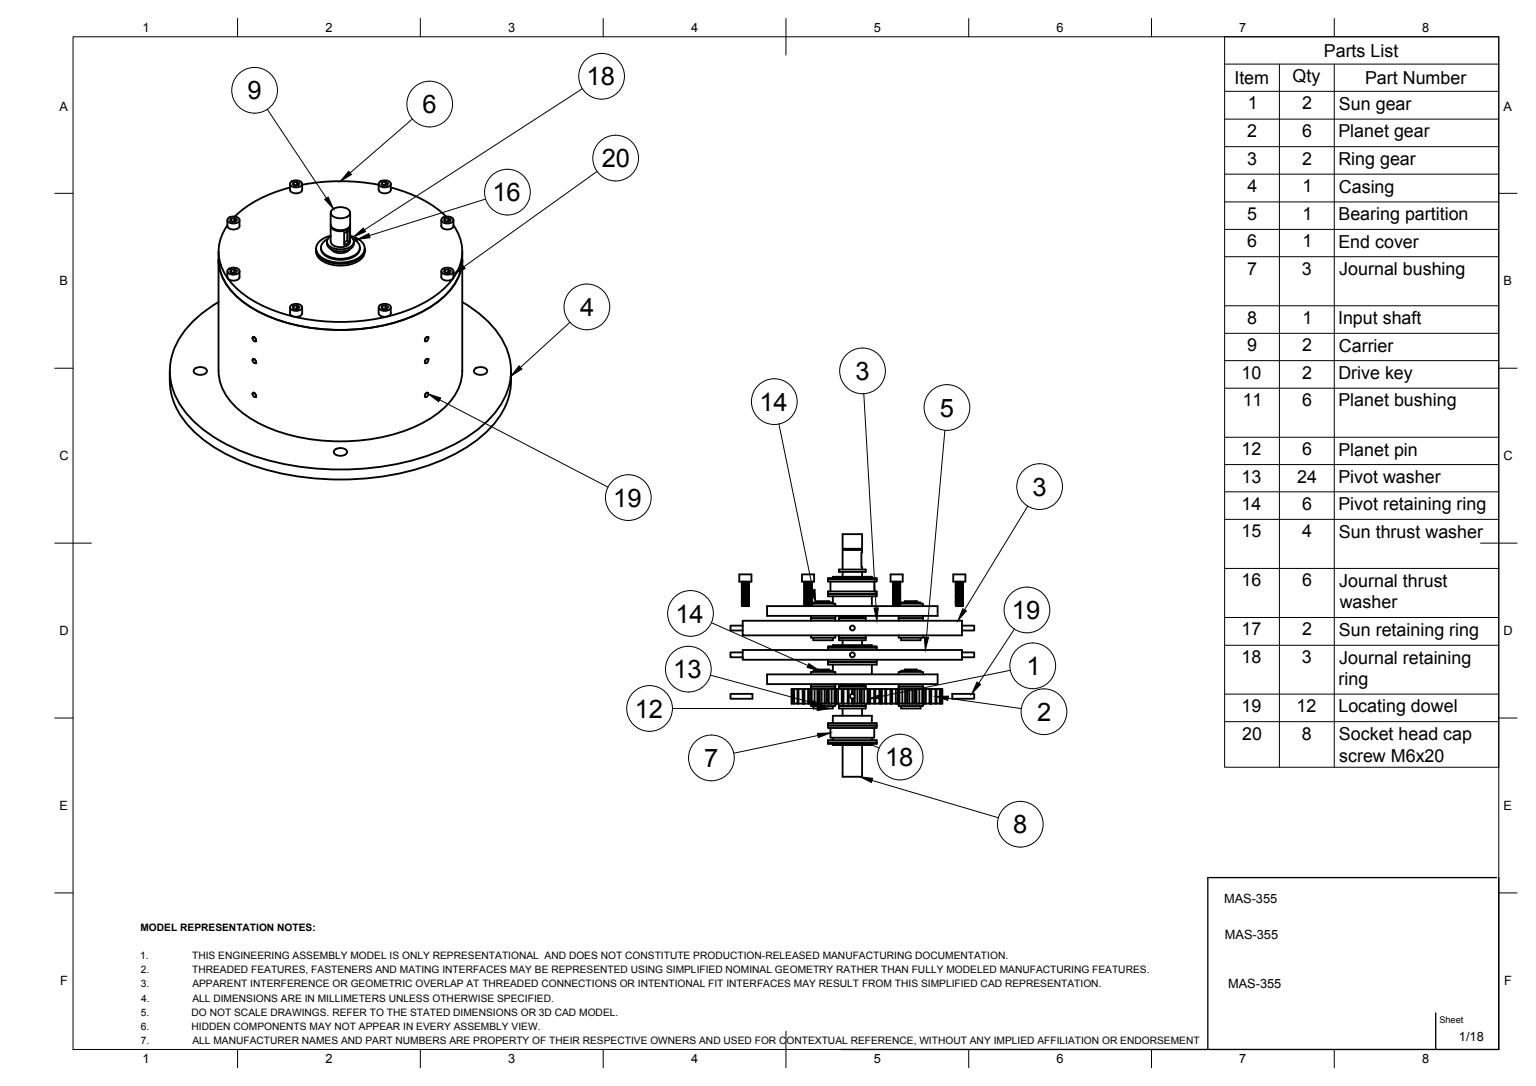
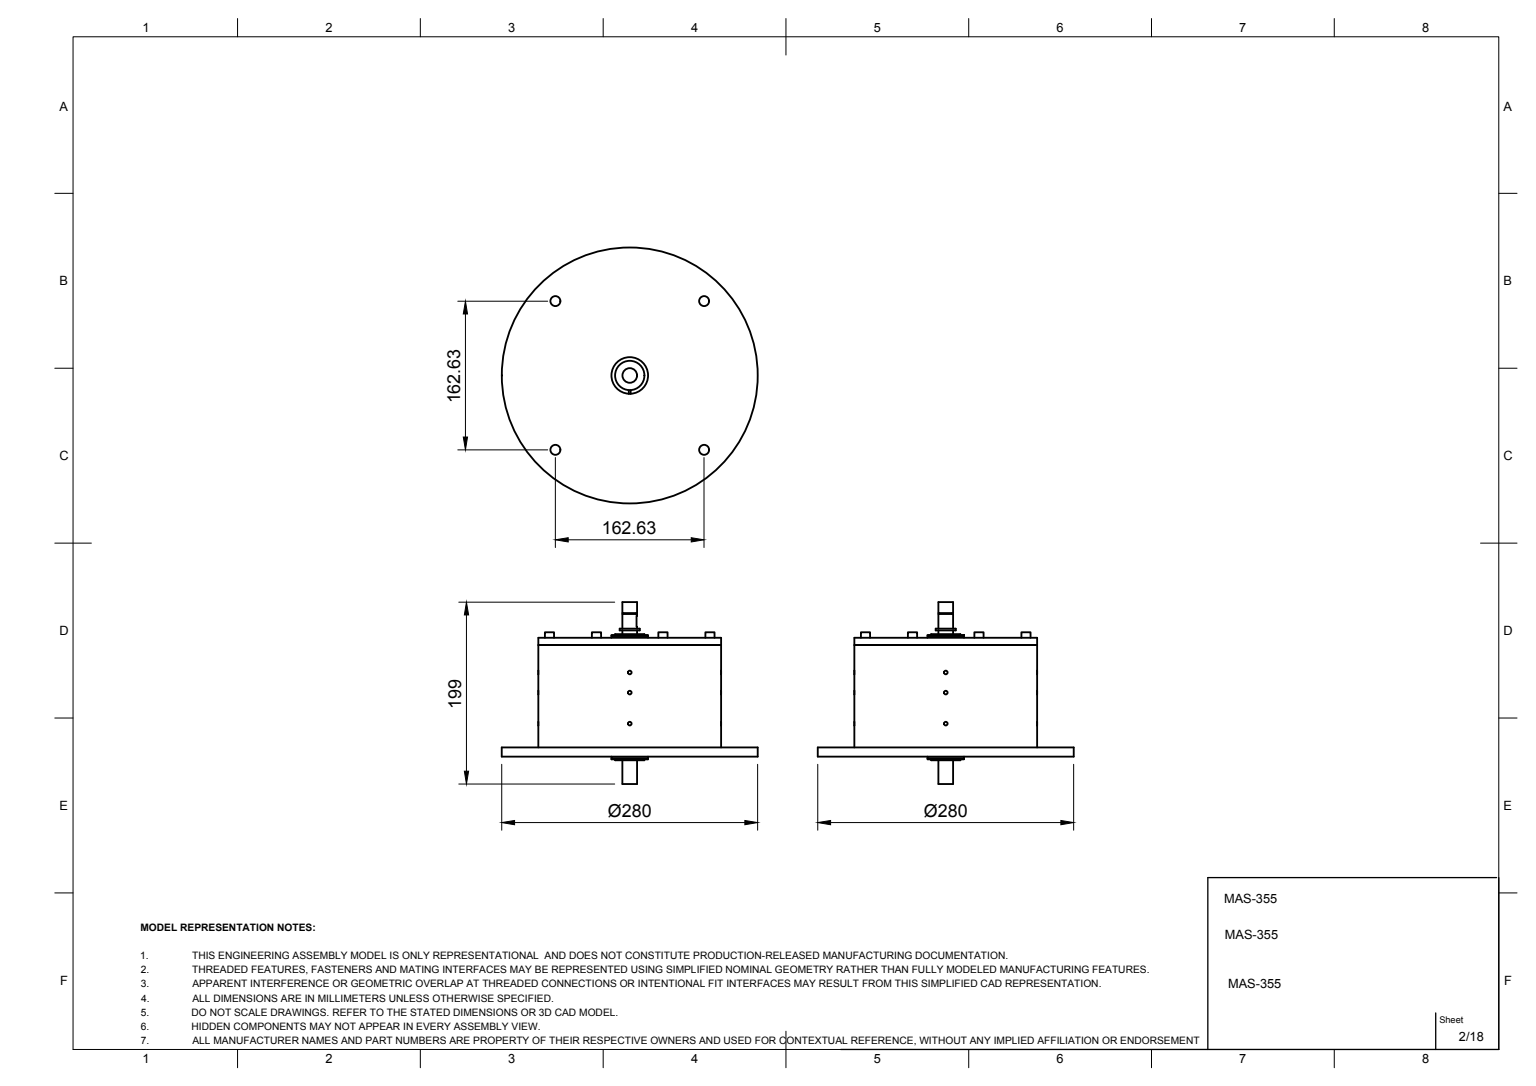
ISO-10303-21;
HEADER;
/* Generated by software containing ST-Developer
 * from STEP Tools, Inc. (www.steptools.com) 
 */

FILE_DESCRIPTION(
/* description */ ('Independent two-stage fixed-ring planetary gearbox,24/24/72 teeth,mod
ule2,20deg involutes,three planets per stage,4:1 x4:1=16:1. Native cut
-space/fillet/pattern tooth profiles derived from reusable gear blanks
; shared sun/planet/ring/carrier parts across both stages. Captured br
onze-journal input/carriers, headed retained planet pins, keyed inters
tage drive and modular keyed output interface. Native ideal gear links
; no torque, precision grade, production backlash/fits, lubrication, s
peed or life rating.'),
/* implementation_level */ '2;1');

FILE_NAME(
/* name */ 'MAS-355.step',
/* time_stamp */ '2026-11-08T19:10:00-08:00',
/* author */ (''),
/* organization */ (''),
/* preprocessor_version */ 'ST-DEVELOPER v20.2',
/* originating_system */ 'Autodesk Translation Framework v15.17.0.0',
/* authorisation */ '');

FILE_SCHEMA (('AUTOMOTIVE_DESIGN { 1 0 10303 214 3 1 1 }'));
ENDSEC;

DATA;
#10=MECHANICAL_DESIGN_GEOMETRIC_PRESENTATION_REPRESENTATION('',(#1163,#1164,
#1165,#1166,#1167,#1168,#1169,#1170,#1171,#1172,#1173,#1174,#1175,#1176,
#1177,#1178,#1179,#1180,#1181,#1182),#259224);
#11=ITEM_DEFINED_TRANSFORMATION($,$,#26314,#27236);
#12=ITEM_DEFINED_TRANSFORMATION($,$,#26659,#27237);
#13=ITEM_DEFINED_TRANSFORMATION($,$,#25864,#27238);
#14=ITEM_DEFINED_TRANSFORMATION($,$,#26659,#27239);
#15=ITEM_DEFINED_TRANSFORMATION($,$,#26659,#27240);
#16=ITEM_DEFINED_TRANSFORMATION($,$,#25392,#27241);
#17=ITEM_DEFINED_TRANSFORMATION($,$,#25757,#27242);
#18=ITEM_DEFINED_TRANSFORMATION($,$,#25778,#27243);
#19=ITEM_DEFINED_TRANSFORMATION($,$,#27001,#27244);
#20=ITEM_DEFINED_TRANSFORMATION($,$,#25811,#27245);
#21=ITEM_DEFINED_TRANSFORMATION($,$,#27010,#27246);
#22=ITEM_DEFINED_TRANSFORMATION($,$,#27076,#27247);
#23=ITEM_DEFINED_TRANSFORMATION($,$,#27083,#27248);
#24=ITEM_DEFINED_TRANSFORMATION($,$,#25864,#27249);
#25=ITEM_DEFINED_TRANSFORMATION($,$,#26314,#27250);
#26=ITEM_DEFINED_TRANSFORMATION($,$,#26659,#27251);
#27=ITEM_DEFINED_TRANSFORMATION($,$,#26659,#27252);
#28=ITEM_DEFINED_TRANSFORMATION($,$,#26659,#27253);
#29=ITEM_DEFINED_TRANSFORMATION($,$,#27001,#27254);
#30=ITEM_DEFINED_TRANSFORMATION($,$,#27001,#27255);
#31=ITEM_DEFINED_TRANSFORMATION($,$,#27010,#27256);
#32=ITEM_DEFINED_TRANSFORMATION($,$,#27076,#27257);
#33=ITEM_DEFINED_TRANSFORMATION($,$,#27092,#27258);
#34=ITEM_DEFINED_TRANSFORMATION($,$,#27121,#27259);
#35=ITEM_DEFINED_TRANSFORMATION($,$,#27110,#27260);
#36=ITEM_DEFINED_TRANSFORMATION($,$,#27083,#27261);
#37=ITEM_DEFINED_TRANSFORMATION($,$,#27083,#27262);
#38=ITEM_DEFINED_TRANSFORMATION($,$,#27083,#27263);
#39=ITEM_DEFINED_TRANSFORMATION($,$,#27083,#27264);
#40=ITEM_DEFINED_TRANSFORMATION($,$,#27083,#27265);
#41=ITEM_DEFINED_TRANSFORMATION($,$,#27130,#27266);
#42=ITEM_DEFINED_TRANSFORMATION($,$,#27139,#27267);
#43=ITEM_DEFINED_TRANSFORMATION($,$,#27148,#27268);
#44=ITEM_DEFINED_TRANSFORMATION($,$,#27159,#27269);
#45=ITEM_DEFINED_TRANSFORMATION($,$,#27170,#27270);
#46=ITEM_DEFINED_TRANSFORMATION($,$,#27176,#27271);
#47=ITEM_DEFINED_TRANSFORMATION($,$,#27121,#27272);
#48=ITEM_DEFINED_TRANSFORMATION($,$,#27121,#27273);
#49=ITEM_DEFINED_TRANSFORMATION($,$,#27121,#27274);
#50=ITEM_DEFINED_TRANSFORMATION($,$,#27092,#27275);
#51=ITEM_DEFINED_TRANSFORMATION($,$,#27110,#27276);
#52=ITEM_DEFINED_TRANSFORMATION($,$,#27121,#27277);
#53=ITEM_DEFINED_TRANSFORMATION($,$,#27121,#27278);
#54=ITEM_DEFINED_TRANSFORMATION($,$,#27121,#27279);
#55=ITEM_DEFINED_TRANSFORMATION($,$,#27121,#27280);
#56=ITEM_DEFINED_TRANSFORMATION($,$,#27092,#27281);
#57=ITEM_DEFINED_TRANSFORMATION($,$,#27110,#27282);
#58=ITEM_DEFINED_TRANSFORMATION($,$,#27121,#27283);
#59=ITEM_DEFINED_TRANSFORMATION($,$,#27121,#27284);
#60=ITEM_DEFINED_TRANSFORMATION($,$,#27121,#27285);
#61=ITEM_DEFINED_TRANSFORMATION($,$,#27121,#27286);
#62=ITEM_DEFINED_TRANSFORMATION($,$,#27092,#27287);
#63=ITEM_DEFINED_TRANSFORMATION($,$,#27110,#27288);
#64=ITEM_DEFINED_TRANSFORMATION($,$,#27121,#27289);
#65=ITEM_DEFINED_TRANSFORMATION($,$,#27121,#27290);
#66=ITEM_DEFINED_TRANSFORMATION($,$,#27121,#27291);
#67=ITEM_DEFINED_TRANSFORMATION($,$,#27121,#27292);
#68=ITEM_DEFINED_TRANSFORMATION($,$,#27092,#27293);
#69=ITEM_DEFINED_TRANSFORMATION($,$,#27110,#27294);
#70=ITEM_DEFINED_TRANSFORMATION($,$,#27121,#27295);
#71=ITEM_DEFINED_TRANSFORMATION($,$,#27121,#27296);
#72=ITEM_DEFINED_TRANSFORMATION($,$,#27121,#27297);
#73=ITEM_DEFINED_TRANSFORMATION($,$,#27121,#27298);
#74=ITEM_DEFINED_TRANSFORMATION($,$,#27092,#27299);
#75=ITEM_DEFINED_TRANSFORMATION($,$,#27110,#27300);
#76=ITEM_DEFINED_TRANSFORMATION($,$,#27121,#27301);
#77=ITEM_DEFINED_TRANSFORMATION($,$,#27121,#27302);
#78=ITEM_DEFINED_TRANSFORMATION($,$,#27121,#27303);
#79=ITEM_DEFINED_TRANSFORMATION($,$,#27121,#27304);
#80=ITEM_DEFINED_TRANSFORMATION($,$,#27130,#27305);
#81=ITEM_DEFINED_TRANSFORMATION($,$,#27130,#27306);
#82=ITEM_DEFINED_TRANSFORMATION($,$,#27130,#27307);
#83=ITEM_DEFINED_TRANSFORMATION($,$,#27139,#27308);
#84=ITEM_DEFINED_TRANSFORMATION($,$,#27139,#27309);
#85=ITEM_DEFINED_TRANSFORMATION($,$,#27139,#27310);
#86=ITEM_DEFINED_TRANSFORMATION($,$,#27139,#27311);
#87=ITEM_DEFINED_TRANSFORMATION($,$,#27139,#27312);
#88=ITEM_DEFINED_TRANSFORMATION($,$,#27148,#27313);
#89=ITEM_DEFINED_TRANSFORMATION($,$,#27159,#27314);
#90=ITEM_DEFINED_TRANSFORMATION($,$,#27159,#27315);
#91=ITEM_DEFINED_TRANSFORMATION($,$,#27170,#27316);
#92=ITEM_DEFINED_TRANSFORMATION($,$,#27170,#27317);
#93=ITEM_DEFINED_TRANSFORMATION($,$,#27170,#27318);
#94=ITEM_DEFINED_TRANSFORMATION($,$,#27170,#27319);
#95=ITEM_DEFINED_TRANSFORMATION($,$,#27170,#27320);
#96=ITEM_DEFINED_TRANSFORMATION($,$,#27170,#27321);
#97=ITEM_DEFINED_TRANSFORMATION($,$,#27170,#27322);
#98=ITEM_DEFINED_TRANSFORMATION($,$,#27170,#27323);
#99=ITEM_DEFINED_TRANSFORMATION($,$,#27170,#27324);
#100=ITEM_DEFINED_TRANSFORMATION($,$,#27170,#27325);
#101=ITEM_DEFINED_TRANSFORMATION($,$,#27170,#27326);
#102=ITEM_DEFINED_TRANSFORMATION($,$,#27176,#27327);
#103=ITEM_DEFINED_TRANSFORMATION($,$,#27176,#27328);
#104=ITEM_DEFINED_TRANSFORMATION($,$,#27176,#27329);
#105=ITEM_DEFINED_TRANSFORMATION($,$,#27176,#27330);
#106=ITEM_DEFINED_TRANSFORMATION($,$,#27176,#27331);
#107=ITEM_DEFINED_TRANSFORMATION($,$,#27176,#27332);
#108=ITEM_DEFINED_TRANSFORMATION($,$,#27176,#27333);
#109=(
REPRESENTATION_RELATIONSHIP($,$,#259375,#259369)
REPRESENTATION_RELATIONSHIP_WITH_TRANSFORMATION(#11)
SHAPE_REPRESENTATION_RELATIONSHIP()
);
#110=(
REPRESENTATION_RELATIONSHIP($,$,#259376,#259369)
REPRESENTATION_RELATIONSHIP_WITH_TRANSFORMATION(#12)
SHAPE_REPRESENTATION_RELATIONSHIP()
);
#111=(
REPRESENTATION_RELATIONSHIP($,$,#259374,#259369)
REPRESENTATION_RELATIONSHIP_WITH_TRANSFORMATION(#13)
SHAPE_REPRESENTATION_RELATIONSHIP()
);
#112=(
REPRESENTATION_RELATIONSHIP($,$,#259376,#259369)
REPRESENTATION_RELATIONSHIP_WITH_TRANSFORMATION(#14)
SHAPE_REPRESENTATION_RELATIONSHIP()
);
#113=(
REPRESENTATION_RELATIONSHIP($,$,#259376,#259369)
REPRESENTATION_RELATIONSHIP_WITH_TRANSFORMATION(#15)
SHAPE_REPRESENTATION_RELATIONSHIP()
);
#114=(
REPRESENTATION_RELATIONSHIP($,$,#259370,#259369)
REPRESENTATION_RELATIONSHIP_WITH_TRANSFORMATION(#16)
SHAPE_REPRESENTATION_RELATIONSHIP()
);
#115=(
REPRESENTATION_RELATIONSHIP($,$,#259371,#259369)
REPRESENTATION_RELATIONSHIP_WITH_TRANSFORMATION(#17)
SHAPE_REPRESENTATION_RELATIONSHIP()
);
#116=(
REPRESENTATION_RELATIONSHIP($,$,#259372,#259369)
REPRESENTATION_RELATIONSHIP_WITH_TRANSFORMATION(#18)
SHAPE_REPRESENTATION_RELATIONSHIP()
);
#117=(
REPRESENTATION_RELATIONSHIP($,$,#259377,#259369)
REPRESENTATION_RELATIONSHIP_WITH_TRANSFORMATION(#19)
SHAPE_REPRESENTATION_RELATIONSHIP()
);
#118=(
REPRESENTATION_RELATIONSHIP($,$,#259373,#259369)
REPRESENTATION_RELATIONSHIP_WITH_TRANSFORMATION(#20)
SHAPE_REPRESENTATION_RELATIONSHIP()
);
#119=(
REPRESENTATION_RELATIONSHIP($,$,#259378,#259369)
REPRESENTATION_RELATIONSHIP_WITH_TRANSFORMATION(#21)
SHAPE_REPRESENTATION_RELATIONSHIP()
);
#120=(
REPRESENTATION_RELATIONSHIP($,$,#259379,#259369)
REPRESENTATION_RELATIONSHIP_WITH_TRANSFORMATION(#22)
SHAPE_REPRESENTATION_RELATIONSHIP()
);
#121=(
REPRESENTATION_RELATIONSHIP($,$,#259380,#259369)
REPRESENTATION_RELATIONSHIP_WITH_TRANSFORMATION(#23)
SHAPE_REPRESENTATION_RELATIONSHIP()
);
#122=(
REPRESENTATION_RELATIONSHIP($,$,#259374,#259369)
REPRESENTATION_RELATIONSHIP_WITH_TRANSFORMATION(#24)
SHAPE_REPRESENTATION_RELATIONSHIP()
);
#123=(
REPRESENTATION_RELATIONSHIP($,$,#259375,#259369)
REPRESENTATION_RELATIONSHIP_WITH_TRANSFORMATION(#25)
SHAPE_REPRESENTATION_RELATIONSHIP()
);
#124=(
REPRESENTATION_RELATIONSHIP($,$,#259376,#259369)
REPRESENTATION_RELATIONSHIP_WITH_TRANSFORMATION(#26)
SHAPE_REPRESENTATION_RELATIONSHIP()
);
#125=(
REPRESENTATION_RELATIONSHIP($,$,#259376,#259369)
REPRESENTATION_RELATIONSHIP_WITH_TRANSFORMATION(#27)
SHAPE_REPRESENTATION_RELATIONSHIP()
);
#126=(
REPRESENTATION_RELATIONSHIP($,$,#259376,#259369)
REPRESENTATION_RELATIONSHIP_WITH_TRANSFORMATION(#28)
SHAPE_REPRESENTATION_RELATIONSHIP()
);
#127=(
REPRESENTATION_RELATIONSHIP($,$,#259377,#259369)
REPRESENTATION_RELATIONSHIP_WITH_TRANSFORMATION(#29)
SHAPE_REPRESENTATION_RELATIONSHIP()
);
#128=(
REPRESENTATION_RELATIONSHIP($,$,#259377,#259369)
REPRESENTATION_RELATIONSHIP_WITH_TRANSFORMATION(#30)
SHAPE_REPRESENTATION_RELATIONSHIP()
);
#129=(
REPRESENTATION_RELATIONSHIP($,$,#259378,#259369)
REPRESENTATION_RELATIONSHIP_WITH_TRANSFORMATION(#31)
SHAPE_REPRESENTATION_RELATIONSHIP()
);
#130=(
REPRESENTATION_RELATIONSHIP($,$,#259379,#259369)
REPRESENTATION_RELATIONSHIP_WITH_TRANSFORMATION(#32)
SHAPE_REPRESENTATION_RELATIONSHIP()
);
#131=(
REPRESENTATION_RELATIONSHIP($,$,#259381,#259369)
REPRESENTATION_RELATIONSHIP_WITH_TRANSFORMATION(#33)
SHAPE_REPRESENTATION_RELATIONSHIP()
);
#132=(
REPRESENTATION_RELATIONSHIP($,$,#259383,#259369)
REPRESENTATION_RELATIONSHIP_WITH_TRANSFORMATION(#34)
SHAPE_REPRESENTATION_RELATIONSHIP()
);
#133=(
REPRESENTATION_RELATIONSHIP($,$,#259382,#259369)
REPRESENTATION_RELATIONSHIP_WITH_TRANSFORMATION(#35)
SHAPE_REPRESENTATION_RELATIONSHIP()
);
#134=(
REPRESENTATION_RELATIONSHIP($,$,#259380,#259369)
REPRESENTATION_RELATIONSHIP_WITH_TRANSFORMATION(#36)
SHAPE_REPRESENTATION_RELATIONSHIP()
);
#135=(
REPRESENTATION_RELATIONSHIP($,$,#259380,#259369)
REPRESENTATION_RELATIONSHIP_WITH_TRANSFORMATION(#37)
SHAPE_REPRESENTATION_RELATIONSHIP()
);
#136=(
REPRESENTATION_RELATIONSHIP($,$,#259380,#259369)
REPRESENTATION_RELATIONSHIP_WITH_TRANSFORMATION(#38)
SHAPE_REPRESENTATION_RELATIONSHIP()
);
#137=(
REPRESENTATION_RELATIONSHIP($,$,#259380,#259369)
REPRESENTATION_RELATIONSHIP_WITH_TRANSFORMATION(#39)
SHAPE_REPRESENTATION_RELATIONSHIP()
);
#138=(
REPRESENTATION_RELATIONSHIP($,$,#259380,#259369)
REPRESENTATION_RELATIONSHIP_WITH_TRANSFORMATION(#40)
SHAPE_REPRESENTATION_RELATIONSHIP()
);
#139=(
REPRESENTATION_RELATIONSHIP($,$,#259384,#259369)
REPRESENTATION_RELATIONSHIP_WITH_TRANSFORMATION(#41)
SHAPE_REPRESENTATION_RELATIONSHIP()
);
#140=(
REPRESENTATION_RELATIONSHIP($,$,#259385,#259369)
REPRESENTATION_RELATIONSHIP_WITH_TRANSFORMATION(#42)
SHAPE_REPRESENTATION_RELATIONSHIP()
);
#141=(
REPRESENTATION_RELATIONSHIP($,$,#259386,#259369)
REPRESENTATION_RELATIONSHIP_WITH_TRANSFORMATION(#43)
SHAPE_REPRESENTATION_RELATIONSHIP()
);
#142=(
REPRESENTATION_RELATIONSHIP($,$,#259387,#259369)
REPRESENTATION_RELATIONSHIP_WITH_TRANSFORMATION(#44)
SHAPE_REPRESENTATION_RELATIONSHIP()
);
#143=(
REPRESENTATION_RELATIONSHIP($,$,#259388,#259369)
REPRESENTATION_RELATIONSHIP_WITH_TRANSFORMATION(#45)
SHAPE_REPRESENTATION_RELATIONSHIP()
);
#144=(
REPRESENTATION_RELATIONSHIP($,$,#259389,#259369)
REPRESENTATION_RELATIONSHIP_WITH_TRANSFORMATION(#46)
SHAPE_REPRESENTATION_RELATIONSHIP()
);
#145=(
REPRESENTATION_RELATIONSHIP($,$,#259383,#259369)
REPRESENTATION_RELATIONSHIP_WITH_TRANSFORMATION(#47)
SHAPE_REPRESENTATION_RELATIONSHIP()
);
#146=(
REPRESENTATION_RELATIONSHIP($,$,#259383,#259369)
REPRESENTATION_RELATIONSHIP_WITH_TRANSFORMATION(#48)
SHAPE_REPRESENTATION_RELATIONSHIP()
);
#147=(
REPRESENTATION_RELATIONSHIP($,$,#259383,#259369)
REPRESENTATION_RELATIONSHIP_WITH_TRANSFORMATION(#49)
SHAPE_REPRESENTATION_RELATIONSHIP()
);
#148=(
REPRESENTATION_RELATIONSHIP($,$,#259381,#259369)
REPRESENTATION_RELATIONSHIP_WITH_TRANSFORMATION(#50)
SHAPE_REPRESENTATION_RELATIONSHIP()
);
#149=(
REPRESENTATION_RELATIONSHIP($,$,#259382,#259369)
REPRESENTATION_RELATIONSHIP_WITH_TRANSFORMATION(#51)
SHAPE_REPRESENTATION_RELATIONSHIP()
);
#150=(
REPRESENTATION_RELATIONSHIP($,$,#259383,#259369)
REPRESENTATION_RELATIONSHIP_WITH_TRANSFORMATION(#52)
SHAPE_REPRESENTATION_RELATIONSHIP()
);
#151=(
REPRESENTATION_RELATIONSHIP($,$,#259383,#259369)
REPRESENTATION_RELATIONSHIP_WITH_TRANSFORMATION(#53)
SHAPE_REPRESENTATION_RELATIONSHIP()
);
#152=(
REPRESENTATION_RELATIONSHIP($,$,#259383,#259369)
REPRESENTATION_RELATIONSHIP_WITH_TRANSFORMATION(#54)
SHAPE_REPRESENTATION_RELATIONSHIP()
);
#153=(
REPRESENTATION_RELATIONSHIP($,$,#259383,#259369)
REPRESENTATION_RELATIONSHIP_WITH_TRANSFORMATION(#55)
SHAPE_REPRESENTATION_RELATIONSHIP()
);
#154=(
REPRESENTATION_RELATIONSHIP($,$,#259381,#259369)
REPRESENTATION_RELATIONSHIP_WITH_TRANSFORMATION(#56)
SHAPE_REPRESENTATION_RELATIONSHIP()
);
#155=(
REPRESENTATION_RELATIONSHIP($,$,#259382,#259369)
REPRESENTATION_RELATIONSHIP_WITH_TRANSFORMATION(#57)
SHAPE_REPRESENTATION_RELATIONSHIP()
);
#156=(
REPRESENTATION_RELATIONSHIP($,$,#259383,#259369)
REPRESENTATION_RELATIONSHIP_WITH_TRANSFORMATION(#58)
SHAPE_REPRESENTATION_RELATIONSHIP()
);
#157=(
REPRESENTATION_RELATIONSHIP($,$,#259383,#259369)
REPRESENTATION_RELATIONSHIP_WITH_TRANSFORMATION(#59)
SHAPE_REPRESENTATION_RELATIONSHIP()
);
#158=(
REPRESENTATION_RELATIONSHIP($,$,#259383,#259369)
REPRESENTATION_RELATIONSHIP_WITH_TRANSFORMATION(#60)
SHAPE_REPRESENTATION_RELATIONSHIP()
);
#159=(
REPRESENTATION_RELATIONSHIP($,$,#259383,#259369)
REPRESENTATION_RELATIONSHIP_WITH_TRANSFORMATION(#61)
SHAPE_REPRESENTATION_RELATIONSHIP()
);
#160=(
REPRESENTATION_RELATIONSHIP($,$,#259381,#259369)
REPRESENTATION_RELATIONSHIP_WITH_TRANSFORMATION(#62)
SHAPE_REPRESENTATION_RELATIONSHIP()
);
#161=(
REPRESENTATION_RELATIONSHIP($,$,#259382,#259369)
REPRESENTATION_RELATIONSHIP_WITH_TRANSFORMATION(#63)
SHAPE_REPRESENTATION_RELATIONSHIP()
);
#162=(
REPRESENTATION_RELATIONSHIP($,$,#259383,#259369)
REPRESENTATION_RELATIONSHIP_WITH_TRANSFORMATION(#64)
SHAPE_REPRESENTATION_RELATIONSHIP()
);
#163=(
REPRESENTATION_RELATIONSHIP($,$,#259383,#259369)
REPRESENTATION_RELATIONSHIP_WITH_TRANSFORMATION(#65)
SHAPE_REPRESENTATION_RELATIONSHIP()
);
#164=(
REPRESENTATION_RELATIONSHIP($,$,#259383,#259369)
REPRESENTATION_RELATIONSHIP_WITH_TRANSFORMATION(#66)
SHAPE_REPRESENTATION_RELATIONSHIP()
);
#165=(
REPRESENTATION_RELATIONSHIP($,$,#259383,#259369)
REPRESENTATION_RELATIONSHIP_WITH_TRANSFORMATION(#67)
SHAPE_REPRESENTATION_RELATIONSHIP()
);
#166=(
REPRESENTATION_RELATIONSHIP($,$,#259381,#259369)
REPRESENTATION_RELATIONSHIP_WITH_TRANSFORMATION(#68)
SHAPE_REPRESENTATION_RELATIONSHIP()
);
#167=(
REPRESENTATION_RELATIONSHIP($,$,#259382,#259369)
REPRESENTATION_RELATIONSHIP_WITH_TRANSFORMATION(#69)
SHAPE_REPRESENTATION_RELATIONSHIP()
);
#168=(
REPRESENTATION_RELATIONSHIP($,$,#259383,#259369)
REPRESENTATION_RELATIONSHIP_WITH_TRANSFORMATION(#70)
SHAPE_REPRESENTATION_RELATIONSHIP()
);
#169=(
REPRESENTATION_RELATIONSHIP($,$,#259383,#259369)
REPRESENTATION_RELATIONSHIP_WITH_TRANSFORMATION(#71)
SHAPE_REPRESENTATION_RELATIONSHIP()
);
#170=(
REPRESENTATION_RELATIONSHIP($,$,#259383,#259369)
REPRESENTATION_RELATIONSHIP_WITH_TRANSFORMATION(#72)
SHAPE_REPRESENTATION_RELATIONSHIP()
);
#171=(
REPRESENTATION_RELATIONSHIP($,$,#259383,#259369)
REPRESENTATION_RELATIONSHIP_WITH_TRANSFORMATION(#73)
SHAPE_REPRESENTATION_RELATIONSHIP()
);
#172=(
REPRESENTATION_RELATIONSHIP($,$,#259381,#259369)
REPRESENTATION_RELATIONSHIP_WITH_TRANSFORMATION(#74)
SHAPE_REPRESENTATION_RELATIONSHIP()
);
#173=(
REPRESENTATION_RELATIONSHIP($,$,#259382,#259369)
REPRESENTATION_RELATIONSHIP_WITH_TRANSFORMATION(#75)
SHAPE_REPRESENTATION_RELATIONSHIP()
);
#174=(
REPRESENTATION_RELATIONSHIP($,$,#259383,#259369)
REPRESENTATION_RELATIONSHIP_WITH_TRANSFORMATION(#76)
SHAPE_REPRESENTATION_RELATIONSHIP()
);
#175=(
REPRESENTATION_RELATIONSHIP($,$,#259383,#259369)
REPRESENTATION_RELATIONSHIP_WITH_TRANSFORMATION(#77)
SHAPE_REPRESENTATION_RELATIONSHIP()
);
#176=(
REPRESENTATION_RELATIONSHIP($,$,#259383,#259369)
REPRESENTATION_RELATIONSHIP_WITH_TRANSFORMATION(#78)
SHAPE_REPRESENTATION_RELATIONSHIP()
);
#177=(
REPRESENTATION_RELATIONSHIP($,$,#259383,#259369)
REPRESENTATION_RELATIONSHIP_WITH_TRANSFORMATION(#79)
SHAPE_REPRESENTATION_RELATIONSHIP()
);
#178=(
REPRESENTATION_RELATIONSHIP($,$,#259384,#259369)
REPRESENTATION_RELATIONSHIP_WITH_TRANSFORMATION(#80)
SHAPE_REPRESENTATION_RELATIONSHIP()
);
#179=(
REPRESENTATION_RELATIONSHIP($,$,#259384,#259369)
REPRESENTATION_RELATIONSHIP_WITH_TRANSFORMATION(#81)
SHAPE_REPRESENTATION_RELATIONSHIP()
);
#180=(
REPRESENTATION_RELATIONSHIP($,$,#259384,#259369)
REPRESENTATION_RELATIONSHIP_WITH_TRANSFORMATION(#82)
SHAPE_REPRESENTATION_RELATIONSHIP()
);
#181=(
REPRESENTATION_RELATIONSHIP($,$,#259385,#259369)
REPRESENTATION_RELATIONSHIP_WITH_TRANSFORMATION(#83)
SHAPE_REPRESENTATION_RELATIONSHIP()
);
#182=(
REPRESENTATION_RELATIONSHIP($,$,#259385,#259369)
REPRESENTATION_RELATIONSHIP_WITH_TRANSFORMATION(#84)
SHAPE_REPRESENTATION_RELATIONSHIP()
);
#183=(
REPRESENTATION_RELATIONSHIP($,$,#259385,#259369)
REPRESENTATION_RELATIONSHIP_WITH_TRANSFORMATION(#85)
SHAPE_REPRESENTATION_RELATIONSHIP()
);
#184=(
REPRESENTATION_RELATIONSHIP($,$,#259385,#259369)
REPRESENTATION_RELATIONSHIP_WITH_TRANSFORMATION(#86)
SHAPE_REPRESENTATION_RELATIONSHIP()
);
#185=(
REPRESENTATION_RELATIONSHIP($,$,#259385,#259369)
REPRESENTATION_RELATIONSHIP_WITH_TRANSFORMATION(#87)
SHAPE_REPRESENTATION_RELATIONSHIP()
);
#186=(
REPRESENTATION_RELATIONSHIP($,$,#259386,#259369)
REPRESENTATION_RELATIONSHIP_WITH_TRANSFORMATION(#88)
SHAPE_REPRESENTATION_RELATIONSHIP()
);
#187=(
REPRESENTATION_RELATIONSHIP($,$,#259387,#259369)
REPRESENTATION_RELATIONSHIP_WITH_TRANSFORMATION(#89)
SHAPE_REPRESENTATION_RELATIONSHIP()
);
#188=(
REPRESENTATION_RELATIONSHIP($,$,#259387,#259369)
REPRESENTATION_RELATIONSHIP_WITH_TRANSFORMATION(#90)
SHAPE_REPRESENTATION_RELATIONSHIP()
);
#189=(
REPRESENTATION_RELATIONSHIP($,$,#259388,#259369)
REPRESENTATION_RELATIONSHIP_WITH_TRANSFORMATION(#91)
SHAPE_REPRESENTATION_RELATIONSHIP()
);
#190=(
REPRESENTATION_RELATIONSHIP($,$,#259388,#259369)
REPRESENTATION_RELATIONSHIP_WITH_TRANSFORMATION(#92)
SHAPE_REPRESENTATION_RELATIONSHIP()
);
#191=(
REPRESENTATION_RELATIONSHIP($,$,#259388,#259369)
REPRESENTATION_RELATIONSHIP_WITH_TRANSFORMATION(#93)
SHAPE_REPRESENTATION_RELATIONSHIP()
);
#192=(
REPRESENTATION_RELATIONSHIP($,$,#259388,#259369)
REPRESENTATION_RELATIONSHIP_WITH_TRANSFORMATION(#94)
SHAPE_REPRESENTATION_RELATIONSHIP()
);
#193=(
REPRESENTATION_RELATIONSHIP($,$,#259388,#259369)
REPRESENTATION_RELATIONSHIP_WITH_TRANSFORMATION(#95)
SHAPE_REPRESENTATION_RELATIONSHIP()
);
#194=(
REPRESENTATION_RELATIONSHIP($,$,#259388,#259369)
REPRESENTATION_RELATIONSHIP_WITH_TRANSFORMATION(#96)
SHAPE_REPRESENTATION_RELATIONSHIP()
);
#195=(
REPRESENTATION_RELATIONSHIP($,$,#259388,#259369)
REPRESENTATION_RELATIONSHIP_WITH_TRANSFORMATION(#97)
SHAPE_REPRESENTATION_RELATIONSHIP()
);
#196=(
REPRESENTATION_RELATIONSHIP($,$,#259388,#259369)
REPRESENTATION_RELATIONSHIP_WITH_TRANSFORMATION(#98)
SHAPE_REPRESENTATION_RELATIONSHIP()
);
#197=(
REPRESENTATION_RELATIONSHIP($,$,#259388,#259369)
REPRESENTATION_RELATIONSHIP_WITH_TRANSFORMATION(#99)
SHAPE_REPRESENTATION_RELATIONSHIP()
);
#198=(
REPRESENTATION_RELATIONSHIP($,$,#259388,#259369)
REPRESENTATION_RELATIONSHIP_WITH_TRANSFORMATION(#100)
SHAPE_REPRESENTATION_RELATIONSHIP()
);
#199=(
REPRESENTATION_RELATIONSHIP($,$,#259388,#259369)
REPRESENTATION_RELATIONSHIP_WITH_TRANSFORMATION(#101)
SHAPE_REPRESENTATION_RELATIONSHIP()
);
#200=(
REPRESENTATION_RELATIONSHIP($,$,#259389,#259369)
REPRESENTATION_RELATIONSHIP_WITH_TRANSFORMATION(#102)
SHAPE_REPRESENTATION_RELATIONSHIP()
);
#201=(
REPRESENTATION_RELATIONSHIP($,$,#259389,#259369)
REPRESENTATION_RELATIONSHIP_WITH_TRANSFORMATION(#103)
SHAPE_REPRESENTATION_RELATIONSHIP()
);
#202=(
REPRESENTATION_RELATIONSHIP($,$,#259389,#259369)
REPRESENTATION_RELATIONSHIP_WITH_TRANSFORMATION(#104)
SHAPE_REPRESENTATION_RELATIONSHIP()
);
#203=(
REPRESENTATION_RELATIONSHIP($,$,#259389,#259369)
REPRESENTATION_RELATIONSHIP_WITH_TRANSFORMATION(#105)
SHAPE_REPRESENTATION_RELATIONSHIP()
);
#204=(
REPRESENTATION_RELATIONSHIP($,$,#259389,#259369)
REPRESENTATION_RELATIONSHIP_WITH_TRANSFORMATION(#106)
SHAPE_REPRESENTATION_RELATIONSHIP()
);
#205=(
REPRESENTATION_RELATIONSHIP($,$,#259389,#259369)
REPRESENTATION_RELATIONSHIP_WITH_TRANSFORMATION(#107)
SHAPE_REPRESENTATION_RELATIONSHIP()
);
#206=(
REPRESENTATION_RELATIONSHIP($,$,#259389,#259369)
REPRESENTATION_RELATIONSHIP_WITH_TRANSFORMATION(#108)
SHAPE_REPRESENTATION_RELATIONSHIP()
);
#207=CONTEXT_DEPENDENT_SHAPE_REPRESENTATION(#109,#259271);
#208=CONTEXT_DEPENDENT_SHAPE_REPRESENTATION(#110,#259272);
#209=CONTEXT_DEPENDENT_SHAPE_REPRESENTATION(#111,#259273);
#210=CONTEXT_DEPENDENT_SHAPE_REPRESENTATION(#112,#259274);
#211=CONTEXT_DEPENDENT_SHAPE_REPRESENTATION(#113,#259275);
#212=CONTEXT_DEPENDENT_SHAPE_REPRESENTATION(#114,#259276);
#213=CONTEXT_DEPENDENT_SHAPE_REPRESENTATION(#115,#259277);
#214=CONTEXT_DEPENDENT_SHAPE_REPRESENTATION(#116,#259278);
#215=CONTEXT_DEPENDENT_SHAPE_REPRESENTATION(#117,#259279);
#216=CONTEXT_DEPENDENT_SHAPE_REPRESENTATION(#118,#259280);
#217=CONTEXT_DEPENDENT_SHAPE_REPRESENTATION(#119,#259281);
#218=CONTEXT_DEPENDENT_SHAPE_REPRESENTATION(#120,#259282);
#219=CONTEXT_DEPENDENT_SHAPE_REPRESENTATION(#121,#259283);
#220=CONTEXT_DEPENDENT_SHAPE_REPRESENTATION(#122,#259284);
#221=CONTEXT_DEPENDENT_SHAPE_REPRESENTATION(#123,#259285);
#222=CONTEXT_DEPENDENT_SHAPE_REPRESENTATION(#124,#259286);
#223=CONTEXT_DEPENDENT_SHAPE_REPRESENTATION(#125,#259287);
#224=CONTEXT_DEPENDENT_SHAPE_REPRESENTATION(#126,#259288);
#225=CONTEXT_DEPENDENT_SHAPE_REPRESENTATION(#127,#259289);
#226=CONTEXT_DEPENDENT_SHAPE_REPRESENTATION(#128,#259290);
#227=CONTEXT_DEPENDENT_SHAPE_REPRESENTATION(#129,#259291);
#228=CONTEXT_DEPENDENT_SHAPE_REPRESENTATION(#130,#259292);
#229=CONTEXT_DEPENDENT_SHAPE_REPRESENTATION(#131,#259293);
#230=CONTEXT_DEPENDENT_SHAPE_REPRESENTATION(#132,#259294);
#231=CONTEXT_DEPENDENT_SHAPE_REPRESENTATION(#133,#259295);
#232=CONTEXT_DEPENDENT_SHAPE_REPRESENTATION(#134,#259296);
#233=CONTEXT_DEPENDENT_SHAPE_REPRESENTATION(#135,#259297);
#234=CONTEXT_DEPENDENT_SHAPE_REPRESENTATION(#136,#259298);
#235=CONTEXT_DEPENDENT_SHAPE_REPRESENTATION(#137,#259299);
#236=CONTEXT_DEPENDENT_SHAPE_REPRESENTATION(#138,#259300);
#237=CONTEXT_DEPENDENT_SHAPE_REPRESENTATION(#139,#259301);
#238=CONTEXT_DEPENDENT_SHAPE_REPRESENTATION(#140,#259302);
#239=CONTEXT_DEPENDENT_SHAPE_REPRESENTATION(#141,#259303);
#240=CONTEXT_DEPENDENT_SHAPE_REPRESENTATION(#142,#259304);
#241=CONTEXT_DEPENDENT_SHAPE_REPRESENTATION(#143,#259305);
#242=CONTEXT_DEPENDENT_SHAPE_REPRESENTATION(#144,#259306);
#243=CONTEXT_DEPENDENT_SHAPE_REPRESENTATION(#145,#259307);
#244=CONTEXT_DEPENDENT_SHAPE_REPRESENTATION(#146,#259308);
#245=CONTEXT_DEPENDENT_SHAPE_REPRESENTATION(#147,#259309);
#246=CONTEXT_DEPENDENT_SHAPE_REPRESENTATION(#148,#259310);
#247=CONTEXT_DEPENDENT_SHAPE_REPRESENTATION(#149,#259311);
#248=CONTEXT_DEPENDENT_SHAPE_REPRESENTATION(#150,#259312);
#249=CONTEXT_DEPENDENT_SHAPE_REPRESENTATION(#151,#259313);
#250=CONTEXT_DEPENDENT_SHAPE_REPRESENTATION(#152,#259314);
#251=CONTEXT_DEPENDENT_SHAPE_REPRESENTATION(#153,#259315);
#252=CONTEXT_DEPENDENT_SHAPE_REPRESENTATION(#154,#259316);
#253=CONTEXT_DEPENDENT_SHAPE_REPRESENTATION(#155,#259317);
#254=CONTEXT_DEPENDENT_SHAPE_REPRESENTATION(#156,#259318);
#255=CONTEXT_DEPENDENT_SHAPE_REPRESENTATION(#157,#259319);
#256=CONTEXT_DEPENDENT_SHAPE_REPRESENTATION(#158,#259320);
#257=CONTEXT_DEPENDENT_SHAPE_REPRESENTATION(#159,#259321);
#258=CONTEXT_DEPENDENT_SHAPE_REPRESENTATION(#160,#259322);
#259=CONTEXT_DEPENDENT_SHAPE_REPRESENTATION(#161,#259323);
#260=CONTEXT_DEPENDENT_SHAPE_REPRESENTATION(#162,#259324);
#261=CONTEXT_DEPENDENT_SHAPE_REPRESENTATION(#163,#259325);
#262=CONTEXT_DEPENDENT_SHAPE_REPRESENTATION(#164,#259326);
#263=CONTEXT_DEPENDENT_SHAPE_REPRESENTATION(#165,#259327);
#264=CONTEXT_DEPENDENT_SHAPE_REPRESENTATION(#166,#259328);
#265=CONTEXT_DEPENDENT_SHAPE_REPRESENTATION(#167,#259329);
#266=CONTEXT_DEPENDENT_SHAPE_REPRESENTATION(#168,#259330);
#267=CONTEXT_DEPENDENT_SHAPE_REPRESENTATION(#169,#259331);
#268=CONTEXT_DEPENDENT_SHAPE_REPRESENTATION(#170,#259332);
#269=CONTEXT_DEPENDENT_SHAPE_REPRESENTATION(#171,#259333);
#270=CONTEXT_DEPENDENT_SHAPE_REPRESENTATION(#172,#259334);
#271=CONTEXT_DEPENDENT_SHAPE_REPRESENTATION(#173,#259335);
#272=CONTEXT_DEPENDENT_SHAPE_REPRESENTATION(#174,#259336);
#273=CONTEXT_DEPENDENT_SHAPE_REPRESENTATION(#175,#259337);
#274=CONTEXT_DEPENDENT_SHAPE_REPRESENTATION(#176,#259338);
#275=CONTEXT_DEPENDENT_SHAPE_REPRESENTATION(#177,#259339);
#276=CONTEXT_DEPENDENT_SHAPE_REPRESENTATION(#178,#259340);
#277=CONTEXT_DEPENDENT_SHAPE_REPRESENTATION(#179,#259341);
#278=CONTEXT_DEPENDENT_SHAPE_REPRESENTATION(#180,#259342);
#279=CONTEXT_DEPENDENT_SHAPE_REPRESENTATION(#181,#259343);
#280=CONTEXT_DEPENDENT_SHAPE_REPRESENTATION(#182,#259344);
#281=CONTEXT_DEPENDENT_SHAPE_REPRESENTATION(#183,#259345);
#282=CONTEXT_DEPENDENT_SHAPE_REPRESENTATION(#184,#259346);
#283=CONTEXT_DEPENDENT_SHAPE_REPRESENTATION(#185,#259347);
#284=CONTEXT_DEPENDENT_SHAPE_REPRESENTATION(#186,#259348);
#285=CONTEXT_DEPENDENT_SHAPE_REPRESENTATION(#187,#259349);
#286=CONTEXT_DEPENDENT_SHAPE_REPRESENTATION(#188,#259350);
#287=CONTEXT_DEPENDENT_SHAPE_REPRESENTATION(#189,#259351);
#288=CONTEXT_DEPENDENT_SHAPE_REPRESENTATION(#190,#259352);
#289=CONTEXT_DEPENDENT_SHAPE_REPRESENTATION(#191,#259353);
#290=CONTEXT_DEPENDENT_SHAPE_REPRESENTATION(#192,#259354);
#291=CONTEXT_DEPENDENT_SHAPE_REPRESENTATION(#193,#259355);
#292=CONTEXT_DEPENDENT_SHAPE_REPRESENTATION(#194,#259356);
#293=CONTEXT_DEPENDENT_SHAPE_REPRESENTATION(#195,#259357);
#294=CONTEXT_DEPENDENT_SHAPE_REPRESENTATION(#196,#259358);
#295=CONTEXT_DEPENDENT_SHAPE_REPRESENTATION(#197,#259359);
#296=CONTEXT_DEPENDENT_SHAPE_REPRESENTATION(#198,#259360);
#297=CONTEXT_DEPENDENT_SHAPE_REPRESENTATION(#199,#259361);
#298=CONTEXT_DEPENDENT_SHAPE_REPRESENTATION(#200,#259362);
#299=CONTEXT_DEPENDENT_SHAPE_REPRESENTATION(#201,#259363);
#300=CONTEXT_DEPENDENT_SHAPE_REPRESENTATION(#202,#259364);
#301=CONTEXT_DEPENDENT_SHAPE_REPRESENTATION(#203,#259365);
#302=CONTEXT_DEPENDENT_SHAPE_REPRESENTATION(#204,#259366);
#303=CONTEXT_DEPENDENT_SHAPE_REPRESENTATION(#205,#259367);
#304=CONTEXT_DEPENDENT_SHAPE_REPRESENTATION(#206,#259368);
#305=NEXT_ASSEMBLY_USAGE_OCCURRENCE('Sun gear:1','Sun gear:1',
'Sun gear:1',#259391,#259397,'Sun gear:1');
#306=NEXT_ASSEMBLY_USAGE_OCCURRENCE('Planet gear:1','Planet gear:1',
'Planet gear:1',#259391,#259398,'Planet gear:1');
#307=NEXT_ASSEMBLY_USAGE_OCCURRENCE('Ring gear:1','Ring gear:1',
'Ring gear:1',#259391,#259396,'Ring gear:1');
#308=NEXT_ASSEMBLY_USAGE_OCCURRENCE('Planet gear:2','Planet gear:2',
'Planet gear:2',#259391,#259398,'Planet gear:2');
#309=NEXT_ASSEMBLY_USAGE_OCCURRENCE('Planet gear:3','Planet gear:3',
'Planet gear:3',#259391,#259398,'Planet gear:3');
#310=NEXT_ASSEMBLY_USAGE_OCCURRENCE('Casing:1','Casing:1','Casing:1',#259391,
#259392,'Casing:1');
#311=NEXT_ASSEMBLY_USAGE_OCCURRENCE('Bearing partition:1',
'Bearing partition:1','Bearing partition:1',#259391,#259393,
'Bearing partition:1');
#312=NEXT_ASSEMBLY_USAGE_OCCURRENCE('End cover:1','End cover:1',
'End cover:1',#259391,#259394,'End cover:1');
#313=NEXT_ASSEMBLY_USAGE_OCCURRENCE('Journal bushing:1',
'Journal bushing:1','Journal bushing:1',#259391,#259399,
'Journal bushing:1');
#314=NEXT_ASSEMBLY_USAGE_OCCURRENCE('Input shaft:1','Input shaft:1',
'Input shaft:1',#259391,#259395,'Input shaft:1');
#315=NEXT_ASSEMBLY_USAGE_OCCURRENCE('Carrier:1','Carrier:1','Carrier:1',
#259391,#259400,'Carrier:1');
#316=NEXT_ASSEMBLY_USAGE_OCCURRENCE('Drive key:1','Drive key:1',
'Drive key:1',#259391,#259401,'Drive key:1');
#317=NEXT_ASSEMBLY_USAGE_OCCURRENCE('Planet bushing:1',
'Planet bushing:1','Planet bushing:1',#259391,#259402,
'Planet bushing:1');
#318=NEXT_ASSEMBLY_USAGE_OCCURRENCE('Ring gear:2','Ring gear:2',
'Ring gear:2',#259391,#259396,'Ring gear:2');
#319=NEXT_ASSEMBLY_USAGE_OCCURRENCE('Sun gear:2','Sun gear:2',
'Sun gear:2',#259391,#259397,'Sun gear:2');
#320=NEXT_ASSEMBLY_USAGE_OCCURRENCE('Planet gear:4','Planet gear:4',
'Planet gear:4',#259391,#259398,'Planet gear:4');
#321=NEXT_ASSEMBLY_USAGE_OCCURRENCE('Planet gear:5','Planet gear:5',
'Planet gear:5',#259391,#259398,'Planet gear:5');
#322=NEXT_ASSEMBLY_USAGE_OCCURRENCE('Planet gear:6','Planet gear:6',
'Planet gear:6',#259391,#259398,'Planet gear:6');
#323=NEXT_ASSEMBLY_USAGE_OCCURRENCE('Journal bushing:2',
'Journal bushing:2','Journal bushing:2',#259391,#259399,
'Journal bushing:2');
#324=NEXT_ASSEMBLY_USAGE_OCCURRENCE('Journal bushing:3',
'Journal bushing:3','Journal bushing:3',#259391,#259399,
'Journal bushing:3');
#325=NEXT_ASSEMBLY_USAGE_OCCURRENCE('Carrier:2','Carrier:2','Carrier:2',
#259391,#259400,'Carrier:2');
#326=NEXT_ASSEMBLY_USAGE_OCCURRENCE('Drive key:2','Drive key:2',
'Drive key:2',#259391,#259401,'Drive key:2');
#327=NEXT_ASSEMBLY_USAGE_OCCURRENCE('Planet pin:1','Planet pin:1',
'Planet pin:1',#259391,#259403,'Planet pin:1');
#328=NEXT_ASSEMBLY_USAGE_OCCURRENCE('Pivot washer:1','Pivot washer:1',
'Pivot washer:1',#259391,#259405,'Pivot washer:1');
#329=NEXT_ASSEMBLY_USAGE_OCCURRENCE('Pivot retaining ring:1',
'Pivot retaining ring:1','Pivot retaining ring:1',#259391,#259404,
'Pivot retaining ring:1');
#330=NEXT_ASSEMBLY_USAGE_OCCURRENCE('Planet bushing:2',
'Planet bushing:2','Planet bushing:2',#259391,#259402,
'Planet bushing:2');
#331=NEXT_ASSEMBLY_USAGE_OCCURRENCE('Planet bushing:3',
'Planet bushing:3','Planet bushing:3',#259391,#259402,
'Planet bushing:3');
#332=NEXT_ASSEMBLY_USAGE_OCCURRENCE('Planet bushing:4',
'Planet bushing:4','Planet bushing:4',#259391,#259402,
'Planet bushing:4');
#333=NEXT_ASSEMBLY_USAGE_OCCURRENCE('Planet bushing:5',
'Planet bushing:5','Planet bushing:5',#259391,#259402,
'Planet bushing:5');
#334=NEXT_ASSEMBLY_USAGE_OCCURRENCE('Planet bushing:6',
'Planet bushing:6','Planet bushing:6',#259391,#259402,
'Planet bushing:6');
#335=NEXT_ASSEMBLY_USAGE_OCCURRENCE('Sun thrust washer:1',
'Sun thrust washer:1','Sun thrust washer:1',#259391,#259406,
'Sun thrust washer:1');
#336=NEXT_ASSEMBLY_USAGE_OCCURRENCE('Journal thrust washer:1',
'Journal thrust washer:1','Journal thrust washer:1',#259391,#259407,
'Journal thrust washer:1');
#337=NEXT_ASSEMBLY_USAGE_OCCURRENCE('Sun retaining ring:1',
'Sun retaining ring:1','Sun retaining ring:1',#259391,#259408,
'Sun retaining ring:1');
#338=NEXT_ASSEMBLY_USAGE_OCCURRENCE('Journal retaining ring:1',
'Journal retaining ring:1','Journal retaining ring:1',#259391,#259409,
'Journal retaining ring:1');
#339=NEXT_ASSEMBLY_USAGE_OCCURRENCE('Locating dowel:1',
'Locating dowel:1','Locating dowel:1',#259391,#259410,
'Locating dowel:1');
#340=NEXT_ASSEMBLY_USAGE_OCCURRENCE('Socket head cap screw M6x20:1',
'Socket head cap screw M6x20:1','Socket head cap screw M6x20:1',#259391,
#259411,'Socket head cap screw M6x20:1');
#341=NEXT_ASSEMBLY_USAGE_OCCURRENCE('Pivot washer:2','Pivot washer:2',
'Pivot washer:2',#259391,#259405,'Pivot washer:2');
#342=NEXT_ASSEMBLY_USAGE_OCCURRENCE('Pivot washer:3','Pivot washer:3',
'Pivot washer:3',#259391,#259405,'Pivot washer:3');
#343=NEXT_ASSEMBLY_USAGE_OCCURRENCE('Pivot washer:4','Pivot washer:4',
'Pivot washer:4',#259391,#259405,'Pivot washer:4');
#344=NEXT_ASSEMBLY_USAGE_OCCURRENCE('Planet pin:2','Planet pin:2',
'Planet pin:2',#259391,#259403,'Planet pin:2');
#345=NEXT_ASSEMBLY_USAGE_OCCURRENCE('Pivot retaining ring:2',
'Pivot retaining ring:2','Pivot retaining ring:2',#259391,#259404,
'Pivot retaining ring:2');
#346=NEXT_ASSEMBLY_USAGE_OCCURRENCE('Pivot washer:5','Pivot washer:5',
'Pivot washer:5',#259391,#259405,'Pivot washer:5');
#347=NEXT_ASSEMBLY_USAGE_OCCURRENCE('Pivot washer:6','Pivot washer:6',
'Pivot washer:6',#259391,#259405,'Pivot washer:6');
#348=NEXT_ASSEMBLY_USAGE_OCCURRENCE('Pivot washer:7','Pivot washer:7',
'Pivot washer:7',#259391,#259405,'Pivot washer:7');
#349=NEXT_ASSEMBLY_USAGE_OCCURRENCE('Pivot washer:8','Pivot washer:8',
'Pivot washer:8',#259391,#259405,'Pivot washer:8');
#350=NEXT_ASSEMBLY_USAGE_OCCURRENCE('Planet pin:3','Planet pin:3',
'Planet pin:3',#259391,#259403,'Planet pin:3');
#351=NEXT_ASSEMBLY_USAGE_OCCURRENCE('Pivot retaining ring:3',
'Pivot retaining ring:3','Pivot retaining ring:3',#259391,#259404,
'Pivot retaining ring:3');
#352=NEXT_ASSEMBLY_USAGE_OCCURRENCE('Pivot washer:9','Pivot washer:9',
'Pivot washer:9',#259391,#259405,'Pivot washer:9');
#353=NEXT_ASSEMBLY_USAGE_OCCURRENCE('Pivot washer:10','Pivot washer:10',
'Pivot washer:10',#259391,#259405,'Pivot washer:10');
#354=NEXT_ASSEMBLY_USAGE_OCCURRENCE('Pivot washer:11','Pivot washer:11',
'Pivot washer:11',#259391,#259405,'Pivot washer:11');
#355=NEXT_ASSEMBLY_USAGE_OCCURRENCE('Pivot washer:12','Pivot washer:12',
'Pivot washer:12',#259391,#259405,'Pivot washer:12');
#356=NEXT_ASSEMBLY_USAGE_OCCURRENCE('Planet pin:4','Planet pin:4',
'Planet pin:4',#259391,#259403,'Planet pin:4');
#357=NEXT_ASSEMBLY_USAGE_OCCURRENCE('Pivot retaining ring:4',
'Pivot retaining ring:4','Pivot retaining ring:4',#259391,#259404,
'Pivot retaining ring:4');
#358=NEXT_ASSEMBLY_USAGE_OCCURRENCE('Pivot washer:13','Pivot washer:13',
'Pivot washer:13',#259391,#259405,'Pivot washer:13');
#359=NEXT_ASSEMBLY_USAGE_OCCURRENCE('Pivot washer:14','Pivot washer:14',
'Pivot washer:14',#259391,#259405,'Pivot washer:14');
#360=NEXT_ASSEMBLY_USAGE_OCCURRENCE('Pivot washer:15','Pivot washer:15',
'Pivot washer:15',#259391,#259405,'Pivot washer:15');
#361=NEXT_ASSEMBLY_USAGE_OCCURRENCE('Pivot washer:16','Pivot washer:16',
'Pivot washer:16',#259391,#259405,'Pivot washer:16');
#362=NEXT_ASSEMBLY_USAGE_OCCURRENCE('Planet pin:5','Planet pin:5',
'Planet pin:5',#259391,#259403,'Planet pin:5');
#363=NEXT_ASSEMBLY_USAGE_OCCURRENCE('Pivot retaining ring:5',
'Pivot retaining ring:5','Pivot retaining ring:5',#259391,#259404,
'Pivot retaining ring:5');
#364=NEXT_ASSEMBLY_USAGE_OCCURRENCE('Pivot washer:17','Pivot washer:17',
'Pivot washer:17',#259391,#259405,'Pivot washer:17');
#365=NEXT_ASSEMBLY_USAGE_OCCURRENCE('Pivot washer:18','Pivot washer:18',
'Pivot washer:18',#259391,#259405,'Pivot washer:18');
#366=NEXT_ASSEMBLY_USAGE_OCCURRENCE('Pivot washer:19','Pivot washer:19',
'Pivot washer:19',#259391,#259405,'Pivot washer:19');
#367=NEXT_ASSEMBLY_USAGE_OCCURRENCE('Pivot washer:20','Pivot washer:20',
'Pivot washer:20',#259391,#259405,'Pivot washer:20');
#368=NEXT_ASSEMBLY_USAGE_OCCURRENCE('Planet pin:6','Planet pin:6',
'Planet pin:6',#259391,#259403,'Planet pin:6');
#369=NEXT_ASSEMBLY_USAGE_OCCURRENCE('Pivot retaining ring:6',
'Pivot retaining ring:6','Pivot retaining ring:6',#259391,#259404,
'Pivot retaining ring:6');
#370=NEXT_ASSEMBLY_USAGE_OCCURRENCE('Pivot washer:21','Pivot washer:21',
'Pivot washer:21',#259391,#259405,'Pivot washer:21');
#371=NEXT_ASSEMBLY_USAGE_OCCURRENCE('Pivot washer:22','Pivot washer:22',
'Pivot washer:22',#259391,#259405,'Pivot washer:22');
#372=NEXT_ASSEMBLY_USAGE_OCCURRENCE('Pivot washer:23','Pivot washer:23',
'Pivot washer:23',#259391,#259405,'Pivot washer:23');
#373=NEXT_ASSEMBLY_USAGE_OCCURRENCE('Pivot washer:24','Pivot washer:24',
'Pivot washer:24',#259391,#259405,'Pivot washer:24');
#374=NEXT_ASSEMBLY_USAGE_OCCURRENCE('Sun thrust washer:2',
'Sun thrust washer:2','Sun thrust washer:2',#259391,#259406,
'Sun thrust washer:2');
#375=NEXT_ASSEMBLY_USAGE_OCCURRENCE('Sun thrust washer:3',
'Sun thrust washer:3','Sun thrust washer:3',#259391,#259406,
'Sun thrust washer:3');
#376=NEXT_ASSEMBLY_USAGE_OCCURRENCE('Sun thrust washer:4',
'Sun thrust washer:4','Sun thrust washer:4',#259391,#259406,
'Sun thrust washer:4');
#377=NEXT_ASSEMBLY_USAGE_OCCURRENCE('Journal thrust washer:2',
'Journal thrust washer:2','Journal thrust washer:2',#259391,#259407,
'Journal thrust washer:2');
#378=NEXT_ASSEMBLY_USAGE_OCCURRENCE('Journal thrust washer:3',
'Journal thrust washer:3','Journal thrust washer:3',#259391,#259407,
'Journal thrust washer:3');
#379=NEXT_ASSEMBLY_USAGE_OCCURRENCE('Journal thrust washer:4',
'Journal thrust washer:4','Journal thrust washer:4',#259391,#259407,
'Journal thrust washer:4');
#380=NEXT_ASSEMBLY_USAGE_OCCURRENCE('Journal thrust washer:5',
'Journal thrust washer:5','Journal thrust washer:5',#259391,#259407,
'Journal thrust washer:5');
#381=NEXT_ASSEMBLY_USAGE_OCCURRENCE('Journal thrust washer:6',
'Journal thrust washer:6','Journal thrust washer:6',#259391,#259407,
'Journal thrust washer:6');
#382=NEXT_ASSEMBLY_USAGE_OCCURRENCE('Sun retaining ring:2',
'Sun retaining ring:2','Sun retaining ring:2',#259391,#259408,
'Sun retaining ring:2');
#383=NEXT_ASSEMBLY_USAGE_OCCURRENCE('Journal retaining ring:2',
'Journal retaining ring:2','Journal retaining ring:2',#259391,#259409,
'Journal retaining ring:2');
#384=NEXT_ASSEMBLY_USAGE_OCCURRENCE('Journal retaining ring:3',
'Journal retaining ring:3','Journal retaining ring:3',#259391,#259409,
'Journal retaining ring:3');
#385=NEXT_ASSEMBLY_USAGE_OCCURRENCE('Locating dowel:2',
'Locating dowel:2','Locating dowel:2',#259391,#259410,
'Locating dowel:2');
#386=NEXT_ASSEMBLY_USAGE_OCCURRENCE('Locating dowel:3',
'Locating dowel:3','Locating dowel:3',#259391,#259410,
'Locating dowel:3');
#387=NEXT_ASSEMBLY_USAGE_OCCURRENCE('Locating dowel:4',
'Locating dowel:4','Locating dowel:4',#259391,#259410,
'Locating dowel:4');
#388=NEXT_ASSEMBLY_USAGE_OCCURRENCE('Locating dowel:5',
'Locating dowel:5','Locating dowel:5',#259391,#259410,
'Locating dowel:5');
#389=NEXT_ASSEMBLY_USAGE_OCCURRENCE('Locating dowel:6',
'Locating dowel:6','Locating dowel:6',#259391,#259410,
'Locating dowel:6');
#390=NEXT_ASSEMBLY_USAGE_OCCURRENCE('Locating dowel:7',
'Locating dowel:7','Locating dowel:7',#259391,#259410,
'Locating dowel:7');
#391=NEXT_ASSEMBLY_USAGE_OCCURRENCE('Locating dowel:8',
'Locating dowel:8','Locating dowel:8',#259391,#259410,
'Locating dowel:8');
#392=NEXT_ASSEMBLY_USAGE_OCCURRENCE('Locating dowel:9',
'Locating dowel:9','Locating dowel:9',#259391,#259410,
'Locating dowel:9');
#393=NEXT_ASSEMBLY_USAGE_OCCURRENCE('Locating dowel:10',
'Locating dowel:10','Locating dowel:10',#259391,#259410,
'Locating dowel:10');
#394=NEXT_ASSEMBLY_USAGE_OCCURRENCE('Locating dowel:11',
'Locating dowel:11','Locating dowel:11',#259391,#259410,
'Locating dowel:11');
#395=NEXT_ASSEMBLY_USAGE_OCCURRENCE('Locating dowel:12',
'Locating dowel:12','Locating dowel:12',#259391,#259410,
'Locating dowel:12');
#396=NEXT_ASSEMBLY_USAGE_OCCURRENCE('Socket head cap screw M6x20:2',
'Socket head cap screw M6x20:2','Socket head cap screw M6x20:2',#259391,
#259411,'Socket head cap screw M6x20:2');
#397=NEXT_ASSEMBLY_USAGE_OCCURRENCE('Socket head cap screw M6x20:3',
'Socket head cap screw M6x20:3','Socket head cap screw M6x20:3',#259391,
#259411,'Socket head cap screw M6x20:3');
#398=NEXT_ASSEMBLY_USAGE_OCCURRENCE('Socket head cap screw M6x20:4',
'Socket head cap screw M6x20:4','Socket head cap screw M6x20:4',#259391,
#259411,'Socket head cap screw M6x20:4');
#399=NEXT_ASSEMBLY_USAGE_OCCURRENCE('Socket head cap screw M6x20:5',
'Socket head cap screw M6x20:5','Socket head cap screw M6x20:5',#259391,
#259411,'Socket head cap screw M6x20:5');
#400=NEXT_ASSEMBLY_USAGE_OCCURRENCE('Socket head cap screw M6x20:6',
'Socket head cap screw M6x20:6','Socket head cap screw M6x20:6',#259391,
#259411,'Socket head cap screw M6x20:6');
#401=NEXT_ASSEMBLY_USAGE_OCCURRENCE('Socket head cap screw M6x20:7',
'Socket head cap screw M6x20:7','Socket head cap screw M6x20:7',#259391,
#259411,'Socket head cap screw M6x20:7');
#402=NEXT_ASSEMBLY_USAGE_OCCURRENCE('Socket head cap screw M6x20:8',
'Socket head cap screw M6x20:8','Socket head cap screw M6x20:8',#259391,
#259411,'Socket head cap screw M6x20:8');
#403=(
BOUNDED_CURVE()
B_SPLINE_CURVE(5,(#53033,#53034,#53035,#53036,#53037,#53038,#53039,#53040,
#53041,#53042,#53043,#53044,#53045,#53046,#53047,#53048,#53049,#53050,#53051,
#53052,#53053,#53054,#53055,#53056,#53057,#53058,#53059,#53060,#53061,#53062,
#53063,#53064,#53065,#53066,#53067,#53068,#53069,#53070,#53071,#53072,#53073,
#53074,#53075,#53076,#53077,#53078,#53079,#53080,#53081,#53082,#53083,#53084,
#53085,#53086,#53087,#53088,#53089,#53090,#53091,#53092,#53093,#53094,#53095,
#53096,#53097,#53098,#53099,#53100,#53101,#53102,#53103,#53104,#53105,#53106,
#53107,#53108,#53109,#53110,#53111,#53112,#53113,#53114,#53115,#53116,#53117,
#53118,#53119,#53120,#53121,#53122,#53123,#53124,#53125,#53126,#53127,#53128,
#53129,#53130,#53131,#53132,#53133,#53134,#53135,#53136,#53137,#53138,#53139,
#53140,#53141,#53142,#53143,#53144,#53145,#53146,#53147,#53148,#53149,#53150,
#53151,#53152,#53153,#53154,#53155,#53156,#53157,#53158,#53159,#53160,#53161,
#53162,#53163,#53164,#53165,#53166,#53167,#53168,#53169,#53170,#53171,#53172,
#53173,#53174,#53175,#53176,#53177,#53178,#53179,#53180,#53181,#53182,#53183,
#53184,#53185,#53186,#53187,#53188,#53189,#53190,#53191,#53192,#53193,#53194,
#53195,#53196,#53197,#53198,#53199,#53200,#53201,#53202,#53203,#53204,#53205,
#53206,#53207,#53208,#53209,#53210,#53211,#53212,#53213,#53214,#53215,#53216,
#53217,#53218,#53219,#53220,#53221,#53222,#53223,#53224,#53225,#53226),
 .UNSPECIFIED.,.F.,.F.)
B_SPLINE_CURVE_WITH_KNOTS((6,1,1,1,1,1,1,1,1,1,1,1,1,1,1,1,1,1,1,1,1,1,
1,1,1,1,1,1,1,1,1,1,1,1,1,1,1,1,1,1,1,1,1,1,1,1,1,1,1,1,1,1,1,1,1,1,1,1,
1,1,1,1,1,1,1,1,1,1,1,1,1,1,1,1,1,1,1,1,1,1,1,1,1,1,1,1,1,1,1,1,1,1,1,1,
1,1,1,1,1,1,1,1,1,1,1,1,1,1,1,1,1,1,1,1,1,1,1,1,1,1,1,1,1,1,1,1,1,1,1,1,
1,1,1,1,1,1,1,1,1,1,1,1,1,1,1,1,1,1,1,1,1,1,1,1,1,1,1,1,1,1,1,1,1,1,1,1,
1,1,1,1,1,1,1,1,1,1,1,1,1,1,1,1,1,1,1,1,1,1,1,6),(0.,0.005,0.01,0.015,0.02,
0.025,0.03,0.035,0.04,0.045,0.05,0.055,0.06,0.065,0.07,0.075,0.08,0.085,
0.09,0.095,0.1,0.105,0.11,0.115,0.12,0.125,0.13,0.135,0.14,0.145,0.15,0.155,
0.16,0.165,0.17,0.175,0.18,0.185,0.19,0.195,0.2,0.205,0.21,0.215,0.22,0.225,
0.23,0.235,0.24,0.245,0.25,0.255,0.26,0.265,0.27,0.275,0.28,0.285,0.29,
0.295,0.3,0.305,0.31,0.315,0.32,0.325,0.33,0.335,0.34,0.345,0.35,0.355,
0.36,0.365,0.37,0.375,0.38,0.385,0.39,0.395,0.4,0.405,0.41,0.415,0.42,0.425,
0.43,0.435,0.44,0.445,0.45,0.455,0.46,0.465,0.47,0.475,0.48,0.485,0.49,
0.495,0.5,0.505,0.51,0.515,0.52,0.525,0.53,0.535,0.54,0.545,0.55,0.555,
0.56,0.565,0.57,0.575,0.58,0.585,0.59,0.595,0.6,0.605,0.61,0.615,0.62,0.625,
0.63,0.635,0.64,0.645,0.65,0.655,0.66,0.665,0.67,0.675,0.68,0.685,0.690000000000001,
0.695000000000001,0.700000000000001,0.705000000000001,0.710000000000001,
0.715000000000001,0.720000000000001,0.725000000000001,0.730000000000001,
0.735000000000001,0.740000000000001,0.745000000000001,0.750000000000001,
0.755000000000001,0.760000000000001,0.765000000000001,0.770000000000001,
0.775000000000001,0.780000000000001,0.785000000000001,0.790000000000001,
0.795000000000001,0.800000000000001,0.805000000000001,0.810000000000001,
0.815000000000001,0.820000000000001,0.825000000000001,0.830000000000001,
0.835000000000001,0.840000000000001,0.845000000000001,0.850000000000001,
0.855000000000001,0.860000000000001,0.865000000000001,0.870000000000001,
0.875000000000001,0.880000000000001,0.885000000000001,0.890000000000001,
0.895000000000001,0.900000000000001,0.905000000000001,0.910000000000001,
0.915000000000001,0.920000000000001,0.925000000000001,0.930000000000001,
0.935000000000001,0.940000000000001,0.941429844431396),.UNSPECIFIED.)
CURVE()
GEOMETRIC_REPRESENTATION_ITEM()
RATIONAL_B_SPLINE_CURVE((1.,1.,1.,1.,1.,1.,1.,1.,1.,1.,1.,1.,1.,1.,1.,1.,
1.,1.,1.,1.,1.,1.,1.,1.,1.,1.,1.,1.,1.,1.,1.,1.,1.,1.,1.,1.,1.,1.,1.,1.,
1.,1.,1.,1.,1.,1.,1.,1.,1.,1.,1.,1.,1.,1.,1.,1.,1.,1.,1.,1.,1.,1.,1.,1.,
1.,1.,1.,1.,1.,1.,1.,1.,1.,1.,1.,1.,1.,1.,1.,1.,1.,1.,1.,1.,1.,1.,1.,1.,
1.,1.,1.,1.,1.,1.,1.,1.,1.,1.,1.,1.,1.,1.,1.,1.,1.,1.,1.,1.,1.,1.,1.,1.,
1.,1.,1.,1.,1.,1.,1.,1.,1.,1.,1.,1.,1.,1.,1.,1.,1.,1.,1.,1.,1.,1.,1.,1.,
1.,1.,1.,1.,1.,1.,1.,1.,1.,1.,1.,1.,1.,1.,1.,1.,1.,1.,1.,1.,1.,1.,1.,1.,
1.,1.,1.,1.,1.,1.,1.,1.,1.,1.,1.,1.,1.,1.,1.,1.,1.,1.,1.,1.,1.,1.,1.,1.,
1.,1.,1.,1.,1.,1.,1.,1.,1.,1.))
REPRESENTATION_ITEM('')
);
#404=(
BOUNDED_CURVE()
B_SPLINE_CURVE(5,(#53229,#53230,#53231,#53232,#53233,#53234,#53235,#53236,
#53237,#53238,#53239,#53240,#53241,#53242,#53243,#53244,#53245,#53246,#53247,
#53248,#53249,#53250,#53251,#53252,#53253,#53254,#53255,#53256,#53257,#53258,
#53259,#53260,#53261,#53262,#53263,#53264,#53265,#53266,#53267,#53268,#53269,
#53270,#53271,#53272,#53273,#53274,#53275,#53276,#53277,#53278,#53279,#53280,
#53281,#53282,#53283,#53284,#53285,#53286,#53287,#53288,#53289,#53290,#53291,
#53292,#53293,#53294,#53295,#53296,#53297,#53298,#53299,#53300,#53301,#53302,
#53303,#53304,#53305,#53306,#53307,#53308,#53309,#53310,#53311,#53312,#53313,
#53314,#53315,#53316,#53317,#53318,#53319,#53320,#53321,#53322,#53323,#53324,
#53325,#53326,#53327,#53328,#53329,#53330,#53331,#53332,#53333,#53334,#53335,
#53336,#53337,#53338,#53339,#53340,#53341,#53342,#53343,#53344,#53345,#53346,
#53347,#53348,#53349,#53350,#53351,#53352,#53353,#53354,#53355,#53356,#53357,
#53358,#53359,#53360,#53361,#53362,#53363,#53364,#53365,#53366,#53367,#53368,
#53369,#53370,#53371,#53372,#53373,#53374,#53375,#53376,#53377,#53378,#53379,
#53380,#53381,#53382,#53383,#53384,#53385,#53386,#53387,#53388,#53389,#53390,
#53391,#53392,#53393,#53394,#53395,#53396,#53397,#53398,#53399,#53400,#53401,
#53402,#53403,#53404,#53405,#53406,#53407,#53408,#53409,#53410,#53411,#53412,
#53413,#53414,#53415,#53416,#53417,#53418,#53419,#53420,#53421,#53422),
 .UNSPECIFIED.,.F.,.F.)
B_SPLINE_CURVE_WITH_KNOTS((6,1,1,1,1,1,1,1,1,1,1,1,1,1,1,1,1,1,1,1,1,1,
1,1,1,1,1,1,1,1,1,1,1,1,1,1,1,1,1,1,1,1,1,1,1,1,1,1,1,1,1,1,1,1,1,1,1,1,
1,1,1,1,1,1,1,1,1,1,1,1,1,1,1,1,1,1,1,1,1,1,1,1,1,1,1,1,1,1,1,1,1,1,1,1,
1,1,1,1,1,1,1,1,1,1,1,1,1,1,1,1,1,1,1,1,1,1,1,1,1,1,1,1,1,1,1,1,1,1,1,1,
1,1,1,1,1,1,1,1,1,1,1,1,1,1,1,1,1,1,1,1,1,1,1,1,1,1,1,1,1,1,1,1,1,1,1,1,
1,1,1,1,1,1,1,1,1,1,1,1,1,1,1,1,1,1,1,1,1,1,1,6),(-0.941429844431396,-0.940000000000001,
-0.935000000000001,-0.930000000000001,-0.925000000000001,-0.920000000000001,
-0.915000000000001,-0.910000000000001,-0.905000000000001,-0.900000000000001,
-0.895000000000001,-0.890000000000001,-0.885000000000001,-0.880000000000001,
-0.875000000000001,-0.870000000000001,-0.865000000000001,-0.860000000000001,
-0.855000000000001,-0.850000000000001,-0.845000000000001,-0.840000000000001,
-0.835000000000001,-0.830000000000001,-0.825000000000001,-0.820000000000001,
-0.815000000000001,-0.810000000000001,-0.805000000000001,-0.800000000000001,
-0.795000000000001,-0.790000000000001,-0.785000000000001,-0.780000000000001,
-0.775000000000001,-0.770000000000001,-0.765000000000001,-0.760000000000001,
-0.755000000000001,-0.750000000000001,-0.745000000000001,-0.740000000000001,
-0.735000000000001,-0.730000000000001,-0.725000000000001,-0.720000000000001,
-0.715000000000001,-0.710000000000001,-0.705000000000001,-0.700000000000001,
-0.695000000000001,-0.690000000000001,-0.685,-0.68,-0.675,-0.67,-0.665,
-0.66,-0.655,-0.65,-0.645,-0.64,-0.635,-0.63,-0.625,-0.62,-0.615,-0.61,
-0.605,-0.6,-0.595,-0.59,-0.585,-0.58,-0.575,-0.57,-0.565,-0.56,-0.555,
-0.55,-0.545,-0.54,-0.535,-0.53,-0.525,-0.52,-0.515,-0.51,-0.505,-0.5,-0.495,
-0.49,-0.485,-0.48,-0.475,-0.47,-0.465,-0.46,-0.455,-0.45,-0.445,-0.44,
-0.435,-0.43,-0.425,-0.42,-0.415,-0.41,-0.405,-0.4,-0.395,-0.39,-0.385,
-0.38,-0.375,-0.37,-0.365,-0.36,-0.355,-0.35,-0.345,-0.34,-0.335,-0.33,
-0.325,-0.32,-0.315,-0.31,-0.305,-0.3,-0.295,-0.29,-0.285,-0.28,-0.275,
-0.27,-0.265,-0.26,-0.255,-0.25,-0.245,-0.24,-0.235,-0.23,-0.225,-0.22,
-0.215,-0.21,-0.205,-0.2,-0.195,-0.19,-0.185,-0.18,-0.175,-0.17,-0.165,
-0.16,-0.155,-0.15,-0.145,-0.14,-0.135,-0.13,-0.125,-0.12,-0.115,-0.11,
-0.105,-0.1,-0.095,-0.09,-0.085,-0.08,-0.075,-0.07,-0.065,-0.06,-0.055,
-0.05,-0.045,-0.04,-0.035,-0.03,-0.025,-0.02,-0.015,-0.01,-0.005,0.),
 .UNSPECIFIED.)
CURVE()
GEOMETRIC_REPRESENTATION_ITEM()
RATIONAL_B_SPLINE_CURVE((1.,1.,1.,1.,1.,1.,1.,1.,1.,1.,1.,1.,1.,1.,1.,1.,
1.,1.,1.,1.,1.,1.,1.,1.,1.,1.,1.,1.,1.,1.,1.,1.,1.,1.,1.,1.,1.,1.,1.,1.,
1.,1.,1.,1.,1.,1.,1.,1.,1.,1.,1.,1.,1.,1.,1.,1.,1.,1.,1.,1.,1.,1.,1.,1.,
1.,1.,1.,1.,1.,1.,1.,1.,1.,1.,1.,1.,1.,1.,1.,1.,1.,1.,1.,1.,1.,1.,1.,1.,
1.,1.,1.,1.,1.,1.,1.,1.,1.,1.,1.,1.,1.,1.,1.,1.,1.,1.,1.,1.,1.,1.,1.,1.,
1.,1.,1.,1.,1.,1.,1.,1.,1.,1.,1.,1.,1.,1.,1.,1.,1.,1.,1.,1.,1.,1.,1.,1.,
1.,1.,1.,1.,1.,1.,1.,1.,1.,1.,1.,1.,1.,1.,1.,1.,1.,1.,1.,1.,1.,1.,1.,1.,
1.,1.,1.,1.,1.,1.,1.,1.,1.,1.,1.,1.,1.,1.,1.,1.,1.,1.,1.,1.,1.,1.,1.,1.,
1.,1.,1.,1.,1.,1.,1.,1.,1.,1.))
REPRESENTATION_ITEM('')
);
#405=(
BOUNDED_CURVE()
B_SPLINE_CURVE(5,(#53929,#53930,#53931,#53932,#53933,#53934,#53935,#53936,
#53937,#53938,#53939,#53940,#53941,#53942,#53943,#53944,#53945,#53946,#53947,
#53948,#53949,#53950,#53951,#53952,#53953,#53954,#53955,#53956,#53957,#53958,
#53959,#53960,#53961,#53962,#53963,#53964,#53965,#53966,#53967,#53968,#53969,
#53970,#53971,#53972,#53973,#53974,#53975,#53976,#53977,#53978,#53979,#53980,
#53981,#53982,#53983,#53984,#53985,#53986,#53987,#53988,#53989,#53990,#53991,
#53992,#53993,#53994,#53995,#53996,#53997,#53998,#53999,#54000,#54001,#54002,
#54003,#54004,#54005,#54006,#54007,#54008,#54009,#54010,#54011,#54012,#54013,
#54014,#54015,#54016,#54017,#54018,#54019,#54020,#54021,#54022,#54023,#54024,
#54025,#54026,#54027,#54028,#54029,#54030,#54031,#54032,#54033,#54034,#54035,
#54036,#54037,#54038,#54039,#54040,#54041,#54042,#54043,#54044,#54045,#54046,
#54047,#54048,#54049,#54050,#54051,#54052,#54053,#54054,#54055,#54056,#54057,
#54058,#54059,#54060,#54061,#54062,#54063,#54064,#54065,#54066,#54067,#54068,
#54069,#54070,#54071,#54072,#54073,#54074,#54075,#54076,#54077,#54078,#54079,
#54080,#54081,#54082,#54083,#54084,#54085,#54086,#54087,#54088,#54089,#54090,
#54091,#54092,#54093,#54094,#54095,#54096,#54097,#54098,#54099,#54100,#54101,
#54102,#54103,#54104,#54105,#54106,#54107,#54108,#54109,#54110,#54111,#54112,
#54113,#54114,#54115,#54116,#54117,#54118,#54119,#54120,#54121,#54122),
 .UNSPECIFIED.,.F.,.F.)
B_SPLINE_CURVE_WITH_KNOTS((6,1,1,1,1,1,1,1,1,1,1,1,1,1,1,1,1,1,1,1,1,1,
1,1,1,1,1,1,1,1,1,1,1,1,1,1,1,1,1,1,1,1,1,1,1,1,1,1,1,1,1,1,1,1,1,1,1,1,
1,1,1,1,1,1,1,1,1,1,1,1,1,1,1,1,1,1,1,1,1,1,1,1,1,1,1,1,1,1,1,1,1,1,1,1,
1,1,1,1,1,1,1,1,1,1,1,1,1,1,1,1,1,1,1,1,1,1,1,1,1,1,1,1,1,1,1,1,1,1,1,1,
1,1,1,1,1,1,1,1,1,1,1,1,1,1,1,1,1,1,1,1,1,1,1,1,1,1,1,1,1,1,1,1,1,1,1,1,
1,1,1,1,1,1,1,1,1,1,1,1,1,1,1,1,1,1,1,1,1,1,1,6),(0.,0.005,0.01,0.015,0.02,
0.025,0.03,0.035,0.04,0.045,0.05,0.055,0.06,0.065,0.07,0.075,0.08,0.085,
0.09,0.095,0.1,0.105,0.11,0.115,0.12,0.125,0.13,0.135,0.14,0.145,0.15,0.155,
0.16,0.165,0.17,0.175,0.18,0.185,0.19,0.195,0.2,0.205,0.21,0.215,0.22,0.225,
0.23,0.235,0.24,0.245,0.25,0.255,0.26,0.265,0.27,0.275,0.28,0.285,0.29,
0.295,0.3,0.305,0.31,0.315,0.32,0.325,0.33,0.335,0.34,0.345,0.35,0.355,
0.36,0.365,0.37,0.375,0.38,0.385,0.39,0.395,0.4,0.405,0.41,0.415,0.42,0.425,
0.43,0.435,0.44,0.445,0.45,0.455,0.46,0.465,0.47,0.475,0.48,0.485,0.49,
0.495,0.5,0.505,0.51,0.515,0.52,0.525,0.53,0.535,0.54,0.545,0.55,0.555,
0.56,0.565,0.57,0.575,0.58,0.585,0.59,0.595,0.6,0.605,0.61,0.615,0.62,0.625,
0.63,0.635,0.64,0.645,0.65,0.655,0.66,0.665,0.67,0.675,0.68,0.685,0.690000000000001,
0.695000000000001,0.700000000000001,0.705000000000001,0.710000000000001,
0.715000000000001,0.720000000000001,0.725000000000001,0.730000000000001,
0.735000000000001,0.740000000000001,0.745000000000001,0.750000000000001,
0.755000000000001,0.760000000000001,0.765000000000001,0.770000000000001,
0.775000000000001,0.780000000000001,0.785000000000001,0.790000000000001,
0.795000000000001,0.800000000000001,0.805000000000001,0.810000000000001,
0.815000000000001,0.820000000000001,0.825000000000001,0.830000000000001,
0.835000000000001,0.840000000000001,0.845000000000001,0.850000000000001,
0.855000000000001,0.860000000000001,0.865000000000001,0.870000000000001,
0.875000000000001,0.880000000000001,0.885000000000001,0.890000000000001,
0.895000000000001,0.900000000000001,0.905000000000001,0.910000000000001,
0.915000000000001,0.920000000000001,0.925000000000001,0.930000000000001,
0.935000000000001,0.940000000000001,0.941429844431388),.UNSPECIFIED.)
CURVE()
GEOMETRIC_REPRESENTATION_ITEM()
RATIONAL_B_SPLINE_CURVE((1.,1.,1.,1.,1.,1.,1.,1.,1.,1.,1.,1.,1.,1.,1.,1.,
1.,1.,1.,1.,1.,1.,1.,1.,1.,1.,1.,1.,1.,1.,1.,1.,1.,1.,1.,1.,1.,1.,1.,1.,
1.,1.,1.,1.,1.,1.,1.,1.,1.,1.,1.,1.,1.,1.,1.,1.,1.,1.,1.,1.,1.,1.,1.,1.,
1.,1.,1.,1.,1.,1.,1.,1.,1.,1.,1.,1.,1.,1.,1.,1.,1.,1.,1.,1.,1.,1.,1.,1.,
1.,1.,1.,1.,1.,1.,1.,1.,1.,1.,1.,1.,1.,1.,1.,1.,1.,1.,1.,1.,1.,1.,1.,1.,
1.,1.,1.,1.,1.,1.,1.,1.,1.,1.,1.,1.,1.,1.,1.,1.,1.,1.,1.,1.,1.,1.,1.,1.,
1.,1.,1.,1.,1.,1.,1.,1.,1.,1.,1.,1.,1.,1.,1.,1.,1.,1.,1.,1.,1.,1.,1.,1.,
1.,1.,1.,1.,1.,1.,1.,1.,1.,1.,1.,1.,1.,1.,1.,1.,1.,1.,1.,1.,1.,1.,1.,1.,
1.,1.,1.,1.,1.,1.,1.,1.,1.,1.))
REPRESENTATION_ITEM('')
);
#406=(
BOUNDED_CURVE()
B_SPLINE_CURVE(5,(#54125,#54126,#54127,#54128,#54129,#54130,#54131,#54132,
#54133,#54134,#54135,#54136,#54137,#54138,#54139,#54140,#54141,#54142,#54143,
#54144,#54145,#54146,#54147,#54148,#54149,#54150,#54151,#54152,#54153,#54154,
#54155,#54156,#54157,#54158,#54159,#54160,#54161,#54162,#54163,#54164,#54165,
#54166,#54167,#54168,#54169,#54170,#54171,#54172,#54173,#54174,#54175,#54176,
#54177,#54178,#54179,#54180,#54181,#54182,#54183,#54184,#54185,#54186,#54187,
#54188,#54189,#54190,#54191,#54192,#54193,#54194,#54195,#54196,#54197,#54198,
#54199,#54200,#54201,#54202,#54203,#54204,#54205,#54206,#54207,#54208,#54209,
#54210,#54211,#54212,#54213,#54214,#54215,#54216,#54217,#54218,#54219,#54220,
#54221,#54222,#54223,#54224,#54225,#54226,#54227,#54228,#54229,#54230,#54231,
#54232,#54233,#54234,#54235,#54236,#54237,#54238,#54239,#54240,#54241,#54242,
#54243,#54244,#54245,#54246,#54247,#54248,#54249,#54250,#54251,#54252,#54253,
#54254,#54255,#54256,#54257,#54258,#54259,#54260,#54261,#54262,#54263,#54264,
#54265,#54266,#54267,#54268,#54269,#54270,#54271,#54272,#54273,#54274,#54275,
#54276,#54277,#54278,#54279,#54280,#54281,#54282,#54283,#54284,#54285,#54286,
#54287,#54288,#54289,#54290,#54291,#54292,#54293,#54294,#54295,#54296,#54297,
#54298,#54299,#54300,#54301,#54302,#54303,#54304,#54305,#54306,#54307,#54308,
#54309,#54310,#54311,#54312,#54313,#54314,#54315,#54316,#54317,#54318),
 .UNSPECIFIED.,.F.,.F.)
B_SPLINE_CURVE_WITH_KNOTS((6,1,1,1,1,1,1,1,1,1,1,1,1,1,1,1,1,1,1,1,1,1,
1,1,1,1,1,1,1,1,1,1,1,1,1,1,1,1,1,1,1,1,1,1,1,1,1,1,1,1,1,1,1,1,1,1,1,1,
1,1,1,1,1,1,1,1,1,1,1,1,1,1,1,1,1,1,1,1,1,1,1,1,1,1,1,1,1,1,1,1,1,1,1,1,
1,1,1,1,1,1,1,1,1,1,1,1,1,1,1,1,1,1,1,1,1,1,1,1,1,1,1,1,1,1,1,1,1,1,1,1,
1,1,1,1,1,1,1,1,1,1,1,1,1,1,1,1,1,1,1,1,1,1,1,1,1,1,1,1,1,1,1,1,1,1,1,1,
1,1,1,1,1,1,1,1,1,1,1,1,1,1,1,1,1,1,1,1,1,1,1,6),(-0.941429844431391,-0.940000000000001,
-0.935000000000001,-0.930000000000001,-0.925000000000001,-0.920000000000001,
-0.915000000000001,-0.910000000000001,-0.905000000000001,-0.900000000000001,
-0.895000000000001,-0.890000000000001,-0.885000000000001,-0.880000000000001,
-0.875000000000001,-0.870000000000001,-0.865000000000001,-0.860000000000001,
-0.855000000000001,-0.850000000000001,-0.845000000000001,-0.840000000000001,
-0.835000000000001,-0.830000000000001,-0.825000000000001,-0.820000000000001,
-0.815000000000001,-0.810000000000001,-0.805000000000001,-0.800000000000001,
-0.795000000000001,-0.790000000000001,-0.785000000000001,-0.780000000000001,
-0.775000000000001,-0.770000000000001,-0.765000000000001,-0.760000000000001,
-0.755000000000001,-0.750000000000001,-0.745000000000001,-0.740000000000001,
-0.735000000000001,-0.730000000000001,-0.725000000000001,-0.720000000000001,
-0.715000000000001,-0.710000000000001,-0.705000000000001,-0.700000000000001,
-0.695000000000001,-0.690000000000001,-0.685,-0.68,-0.675,-0.67,-0.665,
-0.66,-0.655,-0.65,-0.645,-0.64,-0.635,-0.63,-0.625,-0.62,-0.615,-0.61,
-0.605,-0.6,-0.595,-0.59,-0.585,-0.58,-0.575,-0.57,-0.565,-0.56,-0.555,
-0.55,-0.545,-0.54,-0.535,-0.53,-0.525,-0.52,-0.515,-0.51,-0.505,-0.5,-0.495,
-0.49,-0.485,-0.48,-0.475,-0.47,-0.465,-0.46,-0.455,-0.45,-0.445,-0.44,
-0.435,-0.43,-0.425,-0.42,-0.415,-0.41,-0.405,-0.4,-0.395,-0.39,-0.385,
-0.38,-0.375,-0.37,-0.365,-0.36,-0.355,-0.35,-0.345,-0.34,-0.335,-0.33,
-0.325,-0.32,-0.315,-0.31,-0.305,-0.3,-0.295,-0.29,-0.285,-0.28,-0.275,
-0.27,-0.265,-0.26,-0.255,-0.25,-0.245,-0.24,-0.235,-0.23,-0.225,-0.22,
-0.215,-0.21,-0.205,-0.2,-0.195,-0.19,-0.185,-0.18,-0.175,-0.17,-0.165,
-0.16,-0.155,-0.15,-0.145,-0.14,-0.135,-0.13,-0.125,-0.12,-0.115,-0.11,
-0.105,-0.1,-0.095,-0.09,-0.085,-0.08,-0.075,-0.07,-0.065,-0.06,-0.055,
-0.05,-0.045,-0.04,-0.035,-0.03,-0.025,-0.02,-0.015,-0.01,-0.005,0.),
 .UNSPECIFIED.)
CURVE()
GEOMETRIC_REPRESENTATION_ITEM()
RATIONAL_B_SPLINE_CURVE((1.,1.,1.,1.,1.,1.,1.,1.,1.,1.,1.,1.,1.,1.,1.,1.,
1.,1.,1.,1.,1.,1.,1.,1.,1.,1.,1.,1.,1.,1.,1.,1.,1.,1.,1.,1.,1.,1.,1.,1.,
1.,1.,1.,1.,1.,1.,1.,1.,1.,1.,1.,1.,1.,1.,1.,1.,1.,1.,1.,1.,1.,1.,1.,1.,
1.,1.,1.,1.,1.,1.,1.,1.,1.,1.,1.,1.,1.,1.,1.,1.,1.,1.,1.,1.,1.,1.,1.,1.,
1.,1.,1.,1.,1.,1.,1.,1.,1.,1.,1.,1.,1.,1.,1.,1.,1.,1.,1.,1.,1.,1.,1.,1.,
1.,1.,1.,1.,1.,1.,1.,1.,1.,1.,1.,1.,1.,1.,1.,1.,1.,1.,1.,1.,1.,1.,1.,1.,
1.,1.,1.,1.,1.,1.,1.,1.,1.,1.,1.,1.,1.,1.,1.,1.,1.,1.,1.,1.,1.,1.,1.,1.,
1.,1.,1.,1.,1.,1.,1.,1.,1.,1.,1.,1.,1.,1.,1.,1.,1.,1.,1.,1.,1.,1.,1.,1.,
1.,1.,1.,1.,1.,1.,1.,1.,1.,1.))
REPRESENTATION_ITEM('')
);
#407=(
BOUNDED_CURVE()
B_SPLINE_CURVE(5,(#54825,#54826,#54827,#54828,#54829,#54830,#54831,#54832,
#54833,#54834,#54835,#54836,#54837,#54838,#54839,#54840,#54841,#54842,#54843,
#54844,#54845,#54846,#54847,#54848,#54849,#54850,#54851,#54852,#54853,#54854,
#54855,#54856,#54857,#54858,#54859,#54860,#54861,#54862,#54863,#54864,#54865,
#54866,#54867,#54868,#54869,#54870,#54871,#54872,#54873,#54874,#54875,#54876,
#54877,#54878,#54879,#54880,#54881,#54882,#54883,#54884,#54885,#54886,#54887,
#54888,#54889,#54890,#54891,#54892,#54893,#54894,#54895,#54896,#54897,#54898,
#54899,#54900,#54901,#54902,#54903,#54904,#54905,#54906,#54907,#54908,#54909,
#54910,#54911,#54912,#54913,#54914,#54915,#54916,#54917,#54918,#54919,#54920,
#54921,#54922,#54923,#54924,#54925,#54926,#54927,#54928,#54929,#54930,#54931,
#54932,#54933,#54934,#54935,#54936,#54937,#54938,#54939,#54940,#54941,#54942,
#54943,#54944,#54945,#54946,#54947,#54948,#54949,#54950,#54951,#54952,#54953,
#54954,#54955,#54956,#54957,#54958,#54959,#54960,#54961,#54962,#54963,#54964,
#54965,#54966,#54967,#54968,#54969,#54970,#54971,#54972,#54973,#54974,#54975,
#54976,#54977,#54978,#54979,#54980,#54981,#54982,#54983,#54984,#54985,#54986,
#54987,#54988,#54989,#54990,#54991,#54992,#54993,#54994,#54995,#54996,#54997,
#54998,#54999,#55000,#55001,#55002,#55003,#55004,#55005,#55006,#55007,#55008,
#55009,#55010,#55011,#55012,#55013,#55014,#55015,#55016,#55017,#55018),
 .UNSPECIFIED.,.F.,.F.)
B_SPLINE_CURVE_WITH_KNOTS((6,1,1,1,1,1,1,1,1,1,1,1,1,1,1,1,1,1,1,1,1,1,
1,1,1,1,1,1,1,1,1,1,1,1,1,1,1,1,1,1,1,1,1,1,1,1,1,1,1,1,1,1,1,1,1,1,1,1,
1,1,1,1,1,1,1,1,1,1,1,1,1,1,1,1,1,1,1,1,1,1,1,1,1,1,1,1,1,1,1,1,1,1,1,1,
1,1,1,1,1,1,1,1,1,1,1,1,1,1,1,1,1,1,1,1,1,1,1,1,1,1,1,1,1,1,1,1,1,1,1,1,
1,1,1,1,1,1,1,1,1,1,1,1,1,1,1,1,1,1,1,1,1,1,1,1,1,1,1,1,1,1,1,1,1,1,1,1,
1,1,1,1,1,1,1,1,1,1,1,1,1,1,1,1,1,1,1,1,1,1,1,6),(0.,0.005,0.01,0.015,0.02,
0.025,0.03,0.035,0.04,0.045,0.05,0.055,0.06,0.065,0.07,0.075,0.08,0.085,
0.09,0.095,0.1,0.105,0.11,0.115,0.12,0.125,0.13,0.135,0.14,0.145,0.15,0.155,
0.16,0.165,0.17,0.175,0.18,0.185,0.19,0.195,0.2,0.205,0.21,0.215,0.22,0.225,
0.23,0.235,0.24,0.245,0.25,0.255,0.26,0.265,0.27,0.275,0.28,0.285,0.29,
0.295,0.3,0.305,0.31,0.315,0.32,0.325,0.33,0.335,0.34,0.345,0.35,0.355,
0.36,0.365,0.37,0.375,0.38,0.385,0.39,0.395,0.4,0.405,0.41,0.415,0.42,0.425,
0.43,0.435,0.44,0.445,0.45,0.455,0.46,0.465,0.47,0.475,0.48,0.485,0.49,
0.495,0.5,0.505,0.51,0.515,0.52,0.525,0.53,0.535,0.54,0.545,0.55,0.555,
0.56,0.565,0.57,0.575,0.58,0.585,0.59,0.595,0.6,0.605,0.61,0.615,0.62,0.625,
0.63,0.635,0.64,0.645,0.65,0.655,0.66,0.665,0.67,0.675,0.68,0.685,0.690000000000001,
0.695000000000001,0.700000000000001,0.705000000000001,0.710000000000001,
0.715000000000001,0.720000000000001,0.725000000000001,0.730000000000001,
0.735000000000001,0.740000000000001,0.745000000000001,0.750000000000001,
0.755000000000001,0.760000000000001,0.765000000000001,0.770000000000001,
0.775000000000001,0.780000000000001,0.785000000000001,0.790000000000001,
0.795000000000001,0.800000000000001,0.805000000000001,0.810000000000001,
0.815000000000001,0.820000000000001,0.825000000000001,0.830000000000001,
0.835000000000001,0.840000000000001,0.845000000000001,0.850000000000001,
0.855000000000001,0.860000000000001,0.865000000000001,0.870000000000001,
0.875000000000001,0.880000000000001,0.885000000000001,0.890000000000001,
0.895000000000001,0.900000000000001,0.905000000000001,0.910000000000001,
0.915000000000001,0.920000000000001,0.925000000000001,0.930000000000001,
0.935000000000001,0.940000000000001,0.941429844431439),.UNSPECIFIED.)
CURVE()
GEOMETRIC_REPRESENTATION_ITEM()
RATIONAL_B_SPLINE_CURVE((1.,1.,1.,1.,1.,1.,1.,1.,1.,1.,1.,1.,1.,1.,1.,1.,
1.,1.,1.,1.,1.,1.,1.,1.,1.,1.,1.,1.,1.,1.,1.,1.,1.,1.,1.,1.,1.,1.,1.,1.,
1.,1.,1.,1.,1.,1.,1.,1.,1.,1.,1.,1.,1.,1.,1.,1.,1.,1.,1.,1.,1.,1.,1.,1.,
1.,1.,1.,1.,1.,1.,1.,1.,1.,1.,1.,1.,1.,1.,1.,1.,1.,1.,1.,1.,1.,1.,1.,1.,
1.,1.,1.,1.,1.,1.,1.,1.,1.,1.,1.,1.,1.,1.,1.,1.,1.,1.,1.,1.,1.,1.,1.,1.,
1.,1.,1.,1.,1.,1.,1.,1.,1.,1.,1.,1.,1.,1.,1.,1.,1.,1.,1.,1.,1.,1.,1.,1.,
1.,1.,1.,1.,1.,1.,1.,1.,1.,1.,1.,1.,1.,1.,1.,1.,1.,1.,1.,1.,1.,1.,1.,1.,
1.,1.,1.,1.,1.,1.,1.,1.,1.,1.,1.,1.,1.,1.,1.,1.,1.,1.,1.,1.,1.,1.,1.,1.,
1.,1.,1.,1.,1.,1.,1.,1.,1.,1.))
REPRESENTATION_ITEM('')
);
#408=(
BOUNDED_CURVE()
B_SPLINE_CURVE(5,(#55021,#55022,#55023,#55024,#55025,#55026,#55027,#55028,
#55029,#55030,#55031,#55032,#55033,#55034,#55035,#55036,#55037,#55038,#55039,
#55040,#55041,#55042,#55043,#55044,#55045,#55046,#55047,#55048,#55049,#55050,
#55051,#55052,#55053,#55054,#55055,#55056,#55057,#55058,#55059,#55060,#55061,
#55062,#55063,#55064,#55065,#55066,#55067,#55068,#55069,#55070,#55071,#55072,
#55073,#55074,#55075,#55076,#55077,#55078,#55079,#55080,#55081,#55082,#55083,
#55084,#55085,#55086,#55087,#55088,#55089,#55090,#55091,#55092,#55093,#55094,
#55095,#55096,#55097,#55098,#55099,#55100,#55101,#55102,#55103,#55104,#55105,
#55106,#55107,#55108,#55109,#55110,#55111,#55112,#55113,#55114,#55115,#55116,
#55117,#55118,#55119,#55120,#55121,#55122,#55123,#55124,#55125,#55126,#55127,
#55128,#55129,#55130,#55131,#55132,#55133,#55134,#55135,#55136,#55137,#55138,
#55139,#55140,#55141,#55142,#55143,#55144,#55145,#55146,#55147,#55148,#55149,
#55150,#55151,#55152,#55153,#55154,#55155,#55156,#55157,#55158,#55159,#55160,
#55161,#55162,#55163,#55164,#55165,#55166,#55167,#55168,#55169,#55170,#55171,
#55172,#55173,#55174,#55175,#55176,#55177,#55178,#55179,#55180,#55181,#55182,
#55183,#55184,#55185,#55186,#55187,#55188,#55189,#55190,#55191,#55192,#55193,
#55194,#55195,#55196,#55197,#55198,#55199,#55200,#55201,#55202,#55203,#55204,
#55205,#55206,#55207,#55208,#55209,#55210,#55211,#55212,#55213,#55214),
 .UNSPECIFIED.,.F.,.F.)
B_SPLINE_CURVE_WITH_KNOTS((6,1,1,1,1,1,1,1,1,1,1,1,1,1,1,1,1,1,1,1,1,1,
1,1,1,1,1,1,1,1,1,1,1,1,1,1,1,1,1,1,1,1,1,1,1,1,1,1,1,1,1,1,1,1,1,1,1,1,
1,1,1,1,1,1,1,1,1,1,1,1,1,1,1,1,1,1,1,1,1,1,1,1,1,1,1,1,1,1,1,1,1,1,1,1,
1,1,1,1,1,1,1,1,1,1,1,1,1,1,1,1,1,1,1,1,1,1,1,1,1,1,1,1,1,1,1,1,1,1,1,1,
1,1,1,1,1,1,1,1,1,1,1,1,1,1,1,1,1,1,1,1,1,1,1,1,1,1,1,1,1,1,1,1,1,1,1,1,
1,1,1,1,1,1,1,1,1,1,1,1,1,1,1,1,1,1,1,1,1,1,1,6),(-0.941429844431442,-0.940000000000001,
-0.935000000000001,-0.930000000000001,-0.925000000000001,-0.920000000000001,
-0.915000000000001,-0.910000000000001,-0.905000000000001,-0.900000000000001,
-0.895000000000001,-0.890000000000001,-0.885000000000001,-0.880000000000001,
-0.875000000000001,-0.870000000000001,-0.865000000000001,-0.860000000000001,
-0.855000000000001,-0.850000000000001,-0.845000000000001,-0.840000000000001,
-0.835000000000001,-0.830000000000001,-0.825000000000001,-0.820000000000001,
-0.815000000000001,-0.810000000000001,-0.805000000000001,-0.800000000000001,
-0.795000000000001,-0.790000000000001,-0.785000000000001,-0.780000000000001,
-0.775000000000001,-0.770000000000001,-0.765000000000001,-0.760000000000001,
-0.755000000000001,-0.750000000000001,-0.745000000000001,-0.740000000000001,
-0.735000000000001,-0.730000000000001,-0.725000000000001,-0.720000000000001,
-0.715000000000001,-0.710000000000001,-0.705000000000001,-0.700000000000001,
-0.695000000000001,-0.690000000000001,-0.685,-0.68,-0.675,-0.67,-0.665,
-0.66,-0.655,-0.65,-0.645,-0.64,-0.635,-0.63,-0.625,-0.62,-0.615,-0.61,
-0.605,-0.6,-0.595,-0.59,-0.585,-0.58,-0.575,-0.57,-0.565,-0.56,-0.555,
-0.55,-0.545,-0.54,-0.535,-0.53,-0.525,-0.52,-0.515,-0.51,-0.505,-0.5,-0.495,
-0.49,-0.485,-0.48,-0.475,-0.47,-0.465,-0.46,-0.455,-0.45,-0.445,-0.44,
-0.435,-0.43,-0.425,-0.42,-0.415,-0.41,-0.405,-0.4,-0.395,-0.39,-0.385,
-0.38,-0.375,-0.37,-0.365,-0.36,-0.355,-0.35,-0.345,-0.34,-0.335,-0.33,
-0.325,-0.32,-0.315,-0.31,-0.305,-0.3,-0.295,-0.29,-0.285,-0.28,-0.275,
-0.27,-0.265,-0.26,-0.255,-0.25,-0.245,-0.24,-0.235,-0.23,-0.225,-0.22,
-0.215,-0.21,-0.205,-0.2,-0.195,-0.19,-0.185,-0.18,-0.175,-0.17,-0.165,
-0.16,-0.155,-0.15,-0.145,-0.14,-0.135,-0.13,-0.125,-0.12,-0.115,-0.11,
-0.105,-0.1,-0.095,-0.09,-0.085,-0.08,-0.075,-0.07,-0.065,-0.06,-0.055,
-0.05,-0.045,-0.04,-0.035,-0.03,-0.025,-0.02,-0.015,-0.01,-0.005,0.),
 .UNSPECIFIED.)
CURVE()
GEOMETRIC_REPRESENTATION_ITEM()
RATIONAL_B_SPLINE_CURVE((1.,1.,1.,1.,1.,1.,1.,1.,1.,1.,1.,1.,1.,1.,1.,1.,
1.,1.,1.,1.,1.,1.,1.,1.,1.,1.,1.,1.,1.,1.,1.,1.,1.,1.,1.,1.,1.,1.,1.,1.,
1.,1.,1.,1.,1.,1.,1.,1.,1.,1.,1.,1.,1.,1.,1.,1.,1.,1.,1.,1.,1.,1.,1.,1.,
1.,1.,1.,1.,1.,1.,1.,1.,1.,1.,1.,1.,1.,1.,1.,1.,1.,1.,1.,1.,1.,1.,1.,1.,
1.,1.,1.,1.,1.,1.,1.,1.,1.,1.,1.,1.,1.,1.,1.,1.,1.,1.,1.,1.,1.,1.,1.,1.,
1.,1.,1.,1.,1.,1.,1.,1.,1.,1.,1.,1.,1.,1.,1.,1.,1.,1.,1.,1.,1.,1.,1.,1.,
1.,1.,1.,1.,1.,1.,1.,1.,1.,1.,1.,1.,1.,1.,1.,1.,1.,1.,1.,1.,1.,1.,1.,1.,
1.,1.,1.,1.,1.,1.,1.,1.,1.,1.,1.,1.,1.,1.,1.,1.,1.,1.,1.,1.,1.,1.,1.,1.,
1.,1.,1.,1.,1.,1.,1.,1.,1.,1.))
REPRESENTATION_ITEM('')
);
#409=(
BOUNDED_CURVE()
B_SPLINE_CURVE(5,(#55721,#55722,#55723,#55724,#55725,#55726,#55727,#55728,
#55729,#55730,#55731,#55732,#55733,#55734,#55735,#55736,#55737,#55738,#55739,
#55740,#55741,#55742,#55743,#55744,#55745,#55746,#55747,#55748,#55749,#55750,
#55751,#55752,#55753,#55754,#55755,#55756,#55757,#55758,#55759,#55760,#55761,
#55762,#55763,#55764,#55765,#55766,#55767,#55768,#55769,#55770,#55771,#55772,
#55773,#55774,#55775,#55776,#55777,#55778,#55779,#55780,#55781,#55782,#55783,
#55784,#55785,#55786,#55787,#55788,#55789,#55790,#55791,#55792,#55793,#55794,
#55795,#55796,#55797,#55798,#55799,#55800,#55801,#55802,#55803,#55804,#55805,
#55806,#55807,#55808,#55809,#55810,#55811,#55812,#55813,#55814,#55815,#55816,
#55817,#55818,#55819,#55820,#55821,#55822,#55823,#55824,#55825,#55826,#55827,
#55828,#55829,#55830,#55831,#55832,#55833,#55834,#55835,#55836,#55837,#55838,
#55839,#55840,#55841,#55842,#55843,#55844,#55845,#55846,#55847,#55848,#55849,
#55850,#55851,#55852,#55853,#55854,#55855,#55856,#55857,#55858,#55859,#55860,
#55861,#55862,#55863,#55864,#55865,#55866,#55867,#55868,#55869,#55870,#55871,
#55872,#55873,#55874,#55875,#55876,#55877,#55878,#55879,#55880,#55881,#55882,
#55883,#55884,#55885,#55886,#55887,#55888,#55889,#55890,#55891,#55892,#55893,
#55894,#55895,#55896,#55897,#55898,#55899,#55900,#55901,#55902,#55903,#55904,
#55905,#55906,#55907,#55908,#55909,#55910,#55911,#55912,#55913,#55914),
 .UNSPECIFIED.,.F.,.F.)
B_SPLINE_CURVE_WITH_KNOTS((6,1,1,1,1,1,1,1,1,1,1,1,1,1,1,1,1,1,1,1,1,1,
1,1,1,1,1,1,1,1,1,1,1,1,1,1,1,1,1,1,1,1,1,1,1,1,1,1,1,1,1,1,1,1,1,1,1,1,
1,1,1,1,1,1,1,1,1,1,1,1,1,1,1,1,1,1,1,1,1,1,1,1,1,1,1,1,1,1,1,1,1,1,1,1,
1,1,1,1,1,1,1,1,1,1,1,1,1,1,1,1,1,1,1,1,1,1,1,1,1,1,1,1,1,1,1,1,1,1,1,1,
1,1,1,1,1,1,1,1,1,1,1,1,1,1,1,1,1,1,1,1,1,1,1,1,1,1,1,1,1,1,1,1,1,1,1,1,
1,1,1,1,1,1,1,1,1,1,1,1,1,1,1,1,1,1,1,1,1,1,1,6),(0.,0.005,0.01,0.015,0.02,
0.025,0.03,0.035,0.04,0.045,0.05,0.055,0.06,0.065,0.07,0.075,0.08,0.085,
0.09,0.095,0.1,0.105,0.11,0.115,0.12,0.125,0.13,0.135,0.14,0.145,0.15,0.155,
0.16,0.165,0.17,0.175,0.18,0.185,0.19,0.195,0.2,0.205,0.21,0.215,0.22,0.225,
0.23,0.235,0.24,0.245,0.25,0.255,0.26,0.265,0.27,0.275,0.28,0.285,0.29,
0.295,0.3,0.305,0.31,0.315,0.32,0.325,0.33,0.335,0.34,0.345,0.35,0.355,
0.36,0.365,0.37,0.375,0.38,0.385,0.39,0.395,0.4,0.405,0.41,0.415,0.42,0.425,
0.43,0.435,0.44,0.445,0.45,0.455,0.46,0.465,0.47,0.475,0.48,0.485,0.49,
0.495,0.5,0.505,0.51,0.515,0.52,0.525,0.53,0.535,0.54,0.545,0.55,0.555,
0.56,0.565,0.57,0.575,0.58,0.585,0.59,0.595,0.6,0.605,0.61,0.615,0.62,0.625,
0.63,0.635,0.64,0.645,0.65,0.655,0.66,0.665,0.67,0.675,0.68,0.685,0.690000000000001,
0.695000000000001,0.700000000000001,0.705000000000001,0.710000000000001,
0.715000000000001,0.720000000000001,0.725000000000001,0.730000000000001,
0.735000000000001,0.740000000000001,0.745000000000001,0.750000000000001,
0.755000000000001,0.760000000000001,0.765000000000001,0.770000000000001,
0.775000000000001,0.780000000000001,0.785000000000001,0.790000000000001,
0.795000000000001,0.800000000000001,0.805000000000001,0.810000000000001,
0.815000000000001,0.820000000000001,0.825000000000001,0.830000000000001,
0.835000000000001,0.840000000000001,0.845000000000001,0.850000000000001,
0.855000000000001,0.860000000000001,0.865000000000001,0.870000000000001,
0.875000000000001,0.880000000000001,0.885000000000001,0.890000000000001,
0.895000000000001,0.900000000000001,0.905000000000001,0.910000000000001,
0.915000000000001,0.920000000000001,0.925000000000001,0.930000000000001,
0.935000000000001,0.940000000000001,0.941429844431425),.UNSPECIFIED.)
CURVE()
GEOMETRIC_REPRESENTATION_ITEM()
RATIONAL_B_SPLINE_CURVE((1.,1.,1.,1.,1.,1.,1.,1.,1.,1.,1.,1.,1.,1.,1.,1.,
1.,1.,1.,1.,1.,1.,1.,1.,1.,1.,1.,1.,1.,1.,1.,1.,1.,1.,1.,1.,1.,1.,1.,1.,
1.,1.,1.,1.,1.,1.,1.,1.,1.,1.,1.,1.,1.,1.,1.,1.,1.,1.,1.,1.,1.,1.,1.,1.,
1.,1.,1.,1.,1.,1.,1.,1.,1.,1.,1.,1.,1.,1.,1.,1.,1.,1.,1.,1.,1.,1.,1.,1.,
1.,1.,1.,1.,1.,1.,1.,1.,1.,1.,1.,1.,1.,1.,1.,1.,1.,1.,1.,1.,1.,1.,1.,1.,
1.,1.,1.,1.,1.,1.,1.,1.,1.,1.,1.,1.,1.,1.,1.,1.,1.,1.,1.,1.,1.,1.,1.,1.,
1.,1.,1.,1.,1.,1.,1.,1.,1.,1.,1.,1.,1.,1.,1.,1.,1.,1.,1.,1.,1.,1.,1.,1.,
1.,1.,1.,1.,1.,1.,1.,1.,1.,1.,1.,1.,1.,1.,1.,1.,1.,1.,1.,1.,1.,1.,1.,1.,
1.,1.,1.,1.,1.,1.,1.,1.,1.,1.))
REPRESENTATION_ITEM('')
);
#410=(
BOUNDED_CURVE()
B_SPLINE_CURVE(5,(#55917,#55918,#55919,#55920,#55921,#55922,#55923,#55924,
#55925,#55926,#55927,#55928,#55929,#55930,#55931,#55932,#55933,#55934,#55935,
#55936,#55937,#55938,#55939,#55940,#55941,#55942,#55943,#55944,#55945,#55946,
#55947,#55948,#55949,#55950,#55951,#55952,#55953,#55954,#55955,#55956,#55957,
#55958,#55959,#55960,#55961,#55962,#55963,#55964,#55965,#55966,#55967,#55968,
#55969,#55970,#55971,#55972,#55973,#55974,#55975,#55976,#55977,#55978,#55979,
#55980,#55981,#55982,#55983,#55984,#55985,#55986,#55987,#55988,#55989,#55990,
#55991,#55992,#55993,#55994,#55995,#55996,#55997,#55998,#55999,#56000,#56001,
#56002,#56003,#56004,#56005,#56006,#56007,#56008,#56009,#56010,#56011,#56012,
#56013,#56014,#56015,#56016,#56017,#56018,#56019,#56020,#56021,#56022,#56023,
#56024,#56025,#56026,#56027,#56028,#56029,#56030,#56031,#56032,#56033,#56034,
#56035,#56036,#56037,#56038,#56039,#56040,#56041,#56042,#56043,#56044,#56045,
#56046,#56047,#56048,#56049,#56050,#56051,#56052,#56053,#56054,#56055,#56056,
#56057,#56058,#56059,#56060,#56061,#56062,#56063,#56064,#56065,#56066,#56067,
#56068,#56069,#56070,#56071,#56072,#56073,#56074,#56075,#56076,#56077,#56078,
#56079,#56080,#56081,#56082,#56083,#56084,#56085,#56086,#56087,#56088,#56089,
#56090,#56091,#56092,#56093,#56094,#56095,#56096,#56097,#56098,#56099,#56100,
#56101,#56102,#56103,#56104,#56105,#56106,#56107,#56108,#56109,#56110),
 .UNSPECIFIED.,.F.,.F.)
B_SPLINE_CURVE_WITH_KNOTS((6,1,1,1,1,1,1,1,1,1,1,1,1,1,1,1,1,1,1,1,1,1,
1,1,1,1,1,1,1,1,1,1,1,1,1,1,1,1,1,1,1,1,1,1,1,1,1,1,1,1,1,1,1,1,1,1,1,1,
1,1,1,1,1,1,1,1,1,1,1,1,1,1,1,1,1,1,1,1,1,1,1,1,1,1,1,1,1,1,1,1,1,1,1,1,
1,1,1,1,1,1,1,1,1,1,1,1,1,1,1,1,1,1,1,1,1,1,1,1,1,1,1,1,1,1,1,1,1,1,1,1,
1,1,1,1,1,1,1,1,1,1,1,1,1,1,1,1,1,1,1,1,1,1,1,1,1,1,1,1,1,1,1,1,1,1,1,1,
1,1,1,1,1,1,1,1,1,1,1,1,1,1,1,1,1,1,1,1,1,1,1,6),(-0.941429844431423,-0.940000000000001,
-0.935000000000001,-0.930000000000001,-0.925000000000001,-0.920000000000001,
-0.915000000000001,-0.910000000000001,-0.905000000000001,-0.900000000000001,
-0.895000000000001,-0.890000000000001,-0.885000000000001,-0.880000000000001,
-0.875000000000001,-0.870000000000001,-0.865000000000001,-0.860000000000001,
-0.855000000000001,-0.850000000000001,-0.845000000000001,-0.840000000000001,
-0.835000000000001,-0.830000000000001,-0.825000000000001,-0.820000000000001,
-0.815000000000001,-0.810000000000001,-0.805000000000001,-0.800000000000001,
-0.795000000000001,-0.790000000000001,-0.785000000000001,-0.780000000000001,
-0.775000000000001,-0.770000000000001,-0.765000000000001,-0.760000000000001,
-0.755000000000001,-0.750000000000001,-0.745000000000001,-0.740000000000001,
-0.735000000000001,-0.730000000000001,-0.725000000000001,-0.720000000000001,
-0.715000000000001,-0.710000000000001,-0.705000000000001,-0.700000000000001,
-0.695000000000001,-0.690000000000001,-0.685,-0.68,-0.675,-0.67,-0.665,
-0.66,-0.655,-0.65,-0.645,-0.64,-0.635,-0.63,-0.625,-0.62,-0.615,-0.61,
-0.605,-0.6,-0.595,-0.59,-0.585,-0.58,-0.575,-0.57,-0.565,-0.56,-0.555,
-0.55,-0.545,-0.54,-0.535,-0.53,-0.525,-0.52,-0.515,-0.51,-0.505,-0.5,-0.495,
-0.49,-0.485,-0.48,-0.475,-0.47,-0.465,-0.46,-0.455,-0.45,-0.445,-0.44,
-0.435,-0.43,-0.425,-0.42,-0.415,-0.41,-0.405,-0.4,-0.395,-0.39,-0.385,
-0.38,-0.375,-0.37,-0.365,-0.36,-0.355,-0.35,-0.345,-0.34,-0.335,-0.33,
-0.325,-0.32,-0.315,-0.31,-0.305,-0.3,-0.295,-0.29,-0.285,-0.28,-0.275,
-0.27,-0.265,-0.26,-0.255,-0.25,-0.245,-0.24,-0.235,-0.23,-0.225,-0.22,
-0.215,-0.21,-0.205,-0.2,-0.195,-0.19,-0.185,-0.18,-0.175,-0.17,-0.165,
-0.16,-0.155,-0.15,-0.145,-0.14,-0.135,-0.13,-0.125,-0.12,-0.115,-0.11,
-0.105,-0.1,-0.095,-0.09,-0.085,-0.08,-0.075,-0.07,-0.065,-0.06,-0.055,
-0.05,-0.045,-0.04,-0.035,-0.03,-0.025,-0.02,-0.015,-0.01,-0.005,0.),
 .UNSPECIFIED.)
CURVE()
GEOMETRIC_REPRESENTATION_ITEM()
RATIONAL_B_SPLINE_CURVE((1.,1.,1.,1.,1.,1.,1.,1.,1.,1.,1.,1.,1.,1.,1.,1.,
1.,1.,1.,1.,1.,1.,1.,1.,1.,1.,1.,1.,1.,1.,1.,1.,1.,1.,1.,1.,1.,1.,1.,1.,
1.,1.,1.,1.,1.,1.,1.,1.,1.,1.,1.,1.,1.,1.,1.,1.,1.,1.,1.,1.,1.,1.,1.,1.,
1.,1.,1.,1.,1.,1.,1.,1.,1.,1.,1.,1.,1.,1.,1.,1.,1.,1.,1.,1.,1.,1.,1.,1.,
1.,1.,1.,1.,1.,1.,1.,1.,1.,1.,1.,1.,1.,1.,1.,1.,1.,1.,1.,1.,1.,1.,1.,1.,
1.,1.,1.,1.,1.,1.,1.,1.,1.,1.,1.,1.,1.,1.,1.,1.,1.,1.,1.,1.,1.,1.,1.,1.,
1.,1.,1.,1.,1.,1.,1.,1.,1.,1.,1.,1.,1.,1.,1.,1.,1.,1.,1.,1.,1.,1.,1.,1.,
1.,1.,1.,1.,1.,1.,1.,1.,1.,1.,1.,1.,1.,1.,1.,1.,1.,1.,1.,1.,1.,1.,1.,1.,
1.,1.,1.,1.,1.,1.,1.,1.,1.,1.))
REPRESENTATION_ITEM('')
);
#411=(
BOUNDED_CURVE()
B_SPLINE_CURVE(5,(#56617,#56618,#56619,#56620,#56621,#56622,#56623,#56624,
#56625,#56626,#56627,#56628,#56629,#56630,#56631,#56632,#56633,#56634,#56635,
#56636,#56637,#56638,#56639,#56640,#56641,#56642,#56643,#56644,#56645,#56646,
#56647,#56648,#56649,#56650,#56651,#56652,#56653,#56654,#56655,#56656,#56657,
#56658,#56659,#56660,#56661,#56662,#56663,#56664,#56665,#56666,#56667,#56668,
#56669,#56670,#56671,#56672,#56673,#56674,#56675,#56676,#56677,#56678,#56679,
#56680,#56681,#56682,#56683,#56684,#56685,#56686,#56687,#56688,#56689,#56690,
#56691,#56692,#56693,#56694,#56695,#56696,#56697,#56698,#56699,#56700,#56701,
#56702,#56703,#56704,#56705,#56706,#56707,#56708,#56709,#56710,#56711,#56712,
#56713,#56714,#56715,#56716,#56717,#56718,#56719,#56720,#56721,#56722,#56723,
#56724,#56725,#56726,#56727,#56728,#56729,#56730,#56731,#56732,#56733,#56734,
#56735,#56736,#56737,#56738,#56739,#56740,#56741,#56742,#56743,#56744,#56745,
#56746,#56747,#56748,#56749,#56750,#56751,#56752,#56753,#56754,#56755,#56756,
#56757,#56758,#56759,#56760,#56761,#56762,#56763,#56764,#56765,#56766,#56767,
#56768,#56769,#56770,#56771,#56772,#56773,#56774,#56775,#56776,#56777,#56778,
#56779,#56780,#56781,#56782,#56783,#56784,#56785,#56786,#56787,#56788,#56789,
#56790,#56791,#56792,#56793,#56794,#56795,#56796,#56797,#56798,#56799,#56800,
#56801,#56802,#56803,#56804,#56805,#56806,#56807,#56808,#56809,#56810),
 .UNSPECIFIED.,.F.,.F.)
B_SPLINE_CURVE_WITH_KNOTS((6,1,1,1,1,1,1,1,1,1,1,1,1,1,1,1,1,1,1,1,1,1,
1,1,1,1,1,1,1,1,1,1,1,1,1,1,1,1,1,1,1,1,1,1,1,1,1,1,1,1,1,1,1,1,1,1,1,1,
1,1,1,1,1,1,1,1,1,1,1,1,1,1,1,1,1,1,1,1,1,1,1,1,1,1,1,1,1,1,1,1,1,1,1,1,
1,1,1,1,1,1,1,1,1,1,1,1,1,1,1,1,1,1,1,1,1,1,1,1,1,1,1,1,1,1,1,1,1,1,1,1,
1,1,1,1,1,1,1,1,1,1,1,1,1,1,1,1,1,1,1,1,1,1,1,1,1,1,1,1,1,1,1,1,1,1,1,1,
1,1,1,1,1,1,1,1,1,1,1,1,1,1,1,1,1,1,1,1,1,1,1,6),(0.,0.005,0.01,0.015,0.02,
0.025,0.03,0.035,0.04,0.045,0.05,0.055,0.06,0.065,0.07,0.075,0.08,0.085,
0.09,0.095,0.1,0.105,0.11,0.115,0.12,0.125,0.13,0.135,0.14,0.145,0.15,0.155,
0.16,0.165,0.17,0.175,0.18,0.185,0.19,0.195,0.2,0.205,0.21,0.215,0.22,0.225,
0.23,0.235,0.24,0.245,0.25,0.255,0.26,0.265,0.27,0.275,0.28,0.285,0.29,
0.295,0.3,0.305,0.31,0.315,0.32,0.325,0.33,0.335,0.34,0.345,0.35,0.355,
0.36,0.365,0.37,0.375,0.38,0.385,0.39,0.395,0.4,0.405,0.41,0.415,0.42,0.425,
0.43,0.435,0.44,0.445,0.45,0.455,0.46,0.465,0.47,0.475,0.48,0.485,0.49,
0.495,0.5,0.505,0.51,0.515,0.52,0.525,0.53,0.535,0.54,0.545,0.55,0.555,
0.56,0.565,0.57,0.575,0.58,0.585,0.59,0.595,0.6,0.605,0.61,0.615,0.62,0.625,
0.63,0.635,0.64,0.645,0.65,0.655,0.66,0.665,0.67,0.675,0.68,0.685,0.690000000000001,
0.695000000000001,0.700000000000001,0.705000000000001,0.710000000000001,
0.715000000000001,0.720000000000001,0.725000000000001,0.730000000000001,
0.735000000000001,0.740000000000001,0.745000000000001,0.750000000000001,
0.755000000000001,0.760000000000001,0.765000000000001,0.770000000000001,
0.775000000000001,0.780000000000001,0.785000000000001,0.790000000000001,
0.795000000000001,0.800000000000001,0.805000000000001,0.810000000000001,
0.815000000000001,0.820000000000001,0.825000000000001,0.830000000000001,
0.835000000000001,0.840000000000001,0.845000000000001,0.850000000000001,
0.855000000000001,0.860000000000001,0.865000000000001,0.870000000000001,
0.875000000000001,0.880000000000001,0.885000000000001,0.890000000000001,
0.895000000000001,0.900000000000001,0.905000000000001,0.910000000000001,
0.915000000000001,0.920000000000001,0.925000000000001,0.930000000000001,
0.935000000000001,0.940000000000001,0.941429844431363),.UNSPECIFIED.)
CURVE()
GEOMETRIC_REPRESENTATION_ITEM()
RATIONAL_B_SPLINE_CURVE((1.,1.,1.,1.,1.,1.,1.,1.,1.,1.,1.,1.,1.,1.,1.,1.,
1.,1.,1.,1.,1.,1.,1.,1.,1.,1.,1.,1.,1.,1.,1.,1.,1.,1.,1.,1.,1.,1.,1.,1.,
1.,1.,1.,1.,1.,1.,1.,1.,1.,1.,1.,1.,1.,1.,1.,1.,1.,1.,1.,1.,1.,1.,1.,1.,
1.,1.,1.,1.,1.,1.,1.,1.,1.,1.,1.,1.,1.,1.,1.,1.,1.,1.,1.,1.,1.,1.,1.,1.,
1.,1.,1.,1.,1.,1.,1.,1.,1.,1.,1.,1.,1.,1.,1.,1.,1.,1.,1.,1.,1.,1.,1.,1.,
1.,1.,1.,1.,1.,1.,1.,1.,1.,1.,1.,1.,1.,1.,1.,1.,1.,1.,1.,1.,1.,1.,1.,1.,
1.,1.,1.,1.,1.,1.,1.,1.,1.,1.,1.,1.,1.,1.,1.,1.,1.,1.,1.,1.,1.,1.,1.,1.,
1.,1.,1.,1.,1.,1.,1.,1.,1.,1.,1.,1.,1.,1.,1.,1.,1.,1.,1.,1.,1.,1.,1.,1.,
1.,1.,1.,1.,1.,1.,1.,1.,1.,1.))
REPRESENTATION_ITEM('')
);
#412=(
BOUNDED_CURVE()
B_SPLINE_CURVE(5,(#56813,#56814,#56815,#56816,#56817,#56818,#56819,#56820,
#56821,#56822,#56823,#56824,#56825,#56826,#56827,#56828,#56829,#56830,#56831,
#56832,#56833,#56834,#56835,#56836,#56837,#56838,#56839,#56840,#56841,#56842,
#56843,#56844,#56845,#56846,#56847,#56848,#56849,#56850,#56851,#56852,#56853,
#56854,#56855,#56856,#56857,#56858,#56859,#56860,#56861,#56862,#56863,#56864,
#56865,#56866,#56867,#56868,#56869,#56870,#56871,#56872,#56873,#56874,#56875,
#56876,#56877,#56878,#56879,#56880,#56881,#56882,#56883,#56884,#56885,#56886,
#56887,#56888,#56889,#56890,#56891,#56892,#56893,#56894,#56895,#56896,#56897,
#56898,#56899,#56900,#56901,#56902,#56903,#56904,#56905,#56906,#56907,#56908,
#56909,#56910,#56911,#56912,#56913,#56914,#56915,#56916,#56917,#56918,#56919,
#56920,#56921,#56922,#56923,#56924,#56925,#56926,#56927,#56928,#56929,#56930,
#56931,#56932,#56933,#56934,#56935,#56936,#56937,#56938,#56939,#56940,#56941,
#56942,#56943,#56944,#56945,#56946,#56947,#56948,#56949,#56950,#56951,#56952,
#56953,#56954,#56955,#56956,#56957,#56958,#56959,#56960,#56961,#56962,#56963,
#56964,#56965,#56966,#56967,#56968,#56969,#56970,#56971,#56972,#56973,#56974,
#56975,#56976,#56977,#56978,#56979,#56980,#56981,#56982,#56983,#56984,#56985,
#56986,#56987,#56988,#56989,#56990,#56991,#56992,#56993,#56994,#56995,#56996,
#56997,#56998,#56999,#57000,#57001,#57002,#57003,#57004,#57005,#57006),
 .UNSPECIFIED.,.F.,.F.)
B_SPLINE_CURVE_WITH_KNOTS((6,1,1,1,1,1,1,1,1,1,1,1,1,1,1,1,1,1,1,1,1,1,
1,1,1,1,1,1,1,1,1,1,1,1,1,1,1,1,1,1,1,1,1,1,1,1,1,1,1,1,1,1,1,1,1,1,1,1,
1,1,1,1,1,1,1,1,1,1,1,1,1,1,1,1,1,1,1,1,1,1,1,1,1,1,1,1,1,1,1,1,1,1,1,1,
1,1,1,1,1,1,1,1,1,1,1,1,1,1,1,1,1,1,1,1,1,1,1,1,1,1,1,1,1,1,1,1,1,1,1,1,
1,1,1,1,1,1,1,1,1,1,1,1,1,1,1,1,1,1,1,1,1,1,1,1,1,1,1,1,1,1,1,1,1,1,1,1,
1,1,1,1,1,1,1,1,1,1,1,1,1,1,1,1,1,1,1,1,1,1,1,6),(-0.941429844431365,-0.940000000000001,
-0.935000000000001,-0.930000000000001,-0.925000000000001,-0.920000000000001,
-0.915000000000001,-0.910000000000001,-0.905000000000001,-0.900000000000001,
-0.895000000000001,-0.890000000000001,-0.885000000000001,-0.880000000000001,
-0.875000000000001,-0.870000000000001,-0.865000000000001,-0.860000000000001,
-0.855000000000001,-0.850000000000001,-0.845000000000001,-0.840000000000001,
-0.835000000000001,-0.830000000000001,-0.825000000000001,-0.820000000000001,
-0.815000000000001,-0.810000000000001,-0.805000000000001,-0.800000000000001,
-0.795000000000001,-0.790000000000001,-0.785000000000001,-0.780000000000001,
-0.775000000000001,-0.770000000000001,-0.765000000000001,-0.760000000000001,
-0.755000000000001,-0.750000000000001,-0.745000000000001,-0.740000000000001,
-0.735000000000001,-0.730000000000001,-0.725000000000001,-0.720000000000001,
-0.715000000000001,-0.710000000000001,-0.705000000000001,-0.700000000000001,
-0.695000000000001,-0.690000000000001,-0.685,-0.68,-0.675,-0.67,-0.665,
-0.66,-0.655,-0.65,-0.645,-0.64,-0.635,-0.63,-0.625,-0.62,-0.615,-0.61,
-0.605,-0.6,-0.595,-0.59,-0.585,-0.58,-0.575,-0.57,-0.565,-0.56,-0.555,
-0.55,-0.545,-0.54,-0.535,-0.53,-0.525,-0.52,-0.515,-0.51,-0.505,-0.5,-0.495,
-0.49,-0.485,-0.48,-0.475,-0.47,-0.465,-0.46,-0.455,-0.45,-0.445,-0.44,
-0.435,-0.43,-0.425,-0.42,-0.415,-0.41,-0.405,-0.4,-0.395,-0.39,-0.385,
-0.38,-0.375,-0.37,-0.365,-0.36,-0.355,-0.35,-0.345,-0.34,-0.335,-0.33,
-0.325,-0.32,-0.315,-0.31,-0.305,-0.3,-0.295,-0.29,-0.285,-0.28,-0.275,
-0.27,-0.265,-0.26,-0.255,-0.25,-0.245,-0.24,-0.235,-0.23,-0.225,-0.22,
-0.215,-0.21,-0.205,-0.2,-0.195,-0.19,-0.185,-0.18,-0.175,-0.17,-0.165,
-0.16,-0.155,-0.15,-0.145,-0.14,-0.135,-0.13,-0.125,-0.12,-0.115,-0.11,
-0.105,-0.1,-0.095,-0.09,-0.085,-0.08,-0.075,-0.07,-0.065,-0.06,-0.055,
-0.05,-0.045,-0.04,-0.035,-0.03,-0.025,-0.02,-0.015,-0.01,-0.005,0.),
 .UNSPECIFIED.)
CURVE()
GEOMETRIC_REPRESENTATION_ITEM()
RATIONAL_B_SPLINE_CURVE((1.,1.,1.,1.,1.,1.,1.,1.,1.,1.,1.,1.,1.,1.,1.,1.,
1.,1.,1.,1.,1.,1.,1.,1.,1.,1.,1.,1.,1.,1.,1.,1.,1.,1.,1.,1.,1.,1.,1.,1.,
1.,1.,1.,1.,1.,1.,1.,1.,1.,1.,1.,1.,1.,1.,1.,1.,1.,1.,1.,1.,1.,1.,1.,1.,
1.,1.,1.,1.,1.,1.,1.,1.,1.,1.,1.,1.,1.,1.,1.,1.,1.,1.,1.,1.,1.,1.,1.,1.,
1.,1.,1.,1.,1.,1.,1.,1.,1.,1.,1.,1.,1.,1.,1.,1.,1.,1.,1.,1.,1.,1.,1.,1.,
1.,1.,1.,1.,1.,1.,1.,1.,1.,1.,1.,1.,1.,1.,1.,1.,1.,1.,1.,1.,1.,1.,1.,1.,
1.,1.,1.,1.,1.,1.,1.,1.,1.,1.,1.,1.,1.,1.,1.,1.,1.,1.,1.,1.,1.,1.,1.,1.,
1.,1.,1.,1.,1.,1.,1.,1.,1.,1.,1.,1.,1.,1.,1.,1.,1.,1.,1.,1.,1.,1.,1.,1.,
1.,1.,1.,1.,1.,1.,1.,1.,1.,1.))
REPRESENTATION_ITEM('')
);
#413=(
BOUNDED_CURVE()
B_SPLINE_CURVE(5,(#57513,#57514,#57515,#57516,#57517,#57518,#57519,#57520,
#57521,#57522,#57523,#57524,#57525,#57526,#57527,#57528,#57529,#57530,#57531,
#57532,#57533,#57534,#57535,#57536,#57537,#57538,#57539,#57540,#57541,#57542,
#57543,#57544,#57545,#57546,#57547,#57548,#57549,#57550,#57551,#57552,#57553,
#57554,#57555,#57556,#57557,#57558,#57559,#57560,#57561,#57562,#57563,#57564,
#57565,#57566,#57567,#57568,#57569,#57570,#57571,#57572,#57573,#57574,#57575,
#57576,#57577,#57578,#57579,#57580,#57581,#57582,#57583,#57584,#57585,#57586,
#57587,#57588,#57589,#57590,#57591,#57592,#57593,#57594,#57595,#57596,#57597,
#57598,#57599,#57600,#57601,#57602,#57603,#57604,#57605,#57606,#57607,#57608,
#57609,#57610,#57611,#57612,#57613,#57614,#57615,#57616,#57617,#57618,#57619,
#57620,#57621,#57622,#57623,#57624,#57625,#57626,#57627,#57628,#57629,#57630,
#57631,#57632,#57633,#57634,#57635,#57636,#57637,#57638,#57639,#57640,#57641,
#57642,#57643,#57644,#57645,#57646,#57647,#57648,#57649,#57650,#57651,#57652,
#57653,#57654,#57655,#57656,#57657,#57658,#57659,#57660,#57661,#57662,#57663,
#57664,#57665,#57666,#57667,#57668,#57669,#57670,#57671,#57672,#57673,#57674,
#57675,#57676,#57677,#57678,#57679,#57680,#57681,#57682,#57683,#57684,#57685,
#57686,#57687,#57688,#57689,#57690,#57691,#57692,#57693,#57694,#57695,#57696,
#57697,#57698,#57699,#57700,#57701,#57702,#57703,#57704,#57705,#57706),
 .UNSPECIFIED.,.F.,.F.)
B_SPLINE_CURVE_WITH_KNOTS((6,1,1,1,1,1,1,1,1,1,1,1,1,1,1,1,1,1,1,1,1,1,
1,1,1,1,1,1,1,1,1,1,1,1,1,1,1,1,1,1,1,1,1,1,1,1,1,1,1,1,1,1,1,1,1,1,1,1,
1,1,1,1,1,1,1,1,1,1,1,1,1,1,1,1,1,1,1,1,1,1,1,1,1,1,1,1,1,1,1,1,1,1,1,1,
1,1,1,1,1,1,1,1,1,1,1,1,1,1,1,1,1,1,1,1,1,1,1,1,1,1,1,1,1,1,1,1,1,1,1,1,
1,1,1,1,1,1,1,1,1,1,1,1,1,1,1,1,1,1,1,1,1,1,1,1,1,1,1,1,1,1,1,1,1,1,1,1,
1,1,1,1,1,1,1,1,1,1,1,1,1,1,1,1,1,1,1,1,1,1,1,6),(0.,0.005,0.01,0.015,0.02,
0.025,0.03,0.035,0.04,0.045,0.05,0.055,0.06,0.065,0.07,0.075,0.08,0.085,
0.09,0.095,0.1,0.105,0.11,0.115,0.12,0.125,0.13,0.135,0.14,0.145,0.15,0.155,
0.16,0.165,0.17,0.175,0.18,0.185,0.19,0.195,0.2,0.205,0.21,0.215,0.22,0.225,
0.23,0.235,0.24,0.245,0.25,0.255,0.26,0.265,0.27,0.275,0.28,0.285,0.29,
0.295,0.3,0.305,0.31,0.315,0.32,0.325,0.33,0.335,0.34,0.345,0.35,0.355,
0.36,0.365,0.37,0.375,0.38,0.385,0.39,0.395,0.4,0.405,0.41,0.415,0.42,0.425,
0.43,0.435,0.44,0.445,0.45,0.455,0.46,0.465,0.47,0.475,0.48,0.485,0.49,
0.495,0.5,0.505,0.51,0.515,0.52,0.525,0.53,0.535,0.54,0.545,0.55,0.555,
0.56,0.565,0.57,0.575,0.58,0.585,0.59,0.595,0.6,0.605,0.61,0.615,0.62,0.625,
0.63,0.635,0.64,0.645,0.65,0.655,0.66,0.665,0.67,0.675,0.68,0.685,0.690000000000001,
0.695000000000001,0.700000000000001,0.705000000000001,0.710000000000001,
0.715000000000001,0.720000000000001,0.725000000000001,0.730000000000001,
0.735000000000001,0.740000000000001,0.745000000000001,0.750000000000001,
0.755000000000001,0.760000000000001,0.765000000000001,0.770000000000001,
0.775000000000001,0.780000000000001,0.785000000000001,0.790000000000001,
0.795000000000001,0.800000000000001,0.805000000000001,0.810000000000001,
0.815000000000001,0.820000000000001,0.825000000000001,0.830000000000001,
0.835000000000001,0.840000000000001,0.845000000000001,0.850000000000001,
0.855000000000001,0.860000000000001,0.865000000000001,0.870000000000001,
0.875000000000001,0.880000000000001,0.885000000000001,0.890000000000001,
0.895000000000001,0.900000000000001,0.905000000000001,0.910000000000001,
0.915000000000001,0.920000000000001,0.925000000000001,0.930000000000001,
0.935000000000001,0.940000000000001,0.941429844431354),.UNSPECIFIED.)
CURVE()
GEOMETRIC_REPRESENTATION_ITEM()
RATIONAL_B_SPLINE_CURVE((1.,1.,1.,1.,1.,1.,1.,1.,1.,1.,1.,1.,1.,1.,1.,1.,
1.,1.,1.,1.,1.,1.,1.,1.,1.,1.,1.,1.,1.,1.,1.,1.,1.,1.,1.,1.,1.,1.,1.,1.,
1.,1.,1.,1.,1.,1.,1.,1.,1.,1.,1.,1.,1.,1.,1.,1.,1.,1.,1.,1.,1.,1.,1.,1.,
1.,1.,1.,1.,1.,1.,1.,1.,1.,1.,1.,1.,1.,1.,1.,1.,1.,1.,1.,1.,1.,1.,1.,1.,
1.,1.,1.,1.,1.,1.,1.,1.,1.,1.,1.,1.,1.,1.,1.,1.,1.,1.,1.,1.,1.,1.,1.,1.,
1.,1.,1.,1.,1.,1.,1.,1.,1.,1.,1.,1.,1.,1.,1.,1.,1.,1.,1.,1.,1.,1.,1.,1.,
1.,1.,1.,1.,1.,1.,1.,1.,1.,1.,1.,1.,1.,1.,1.,1.,1.,1.,1.,1.,1.,1.,1.,1.,
1.,1.,1.,1.,1.,1.,1.,1.,1.,1.,1.,1.,1.,1.,1.,1.,1.,1.,1.,1.,1.,1.,1.,1.,
1.,1.,1.,1.,1.,1.,1.,1.,1.,1.))
REPRESENTATION_ITEM('')
);
#414=(
BOUNDED_CURVE()
B_SPLINE_CURVE(5,(#57709,#57710,#57711,#57712,#57713,#57714,#57715,#57716,
#57717,#57718,#57719,#57720,#57721,#57722,#57723,#57724,#57725,#57726,#57727,
#57728,#57729,#57730,#57731,#57732,#57733,#57734,#57735,#57736,#57737,#57738,
#57739,#57740,#57741,#57742,#57743,#57744,#57745,#57746,#57747,#57748,#57749,
#57750,#57751,#57752,#57753,#57754,#57755,#57756,#57757,#57758,#57759,#57760,
#57761,#57762,#57763,#57764,#57765,#57766,#57767,#57768,#57769,#57770,#57771,
#57772,#57773,#57774,#57775,#57776,#57777,#57778,#57779,#57780,#57781,#57782,
#57783,#57784,#57785,#57786,#57787,#57788,#57789,#57790,#57791,#57792,#57793,
#57794,#57795,#57796,#57797,#57798,#57799,#57800,#57801,#57802,#57803,#57804,
#57805,#57806,#57807,#57808,#57809,#57810,#57811,#57812,#57813,#57814,#57815,
#57816,#57817,#57818,#57819,#57820,#57821,#57822,#57823,#57824,#57825,#57826,
#57827,#57828,#57829,#57830,#57831,#57832,#57833,#57834,#57835,#57836,#57837,
#57838,#57839,#57840,#57841,#57842,#57843,#57844,#57845,#57846,#57847,#57848,
#57849,#57850,#57851,#57852,#57853,#57854,#57855,#57856,#57857,#57858,#57859,
#57860,#57861,#57862,#57863,#57864,#57865,#57866,#57867,#57868,#57869,#57870,
#57871,#57872,#57873,#57874,#57875,#57876,#57877,#57878,#57879,#57880,#57881,
#57882,#57883,#57884,#57885,#57886,#57887,#57888,#57889,#57890,#57891,#57892,
#57893,#57894,#57895,#57896,#57897,#57898,#57899,#57900,#57901,#57902),
 .UNSPECIFIED.,.F.,.F.)
B_SPLINE_CURVE_WITH_KNOTS((6,1,1,1,1,1,1,1,1,1,1,1,1,1,1,1,1,1,1,1,1,1,
1,1,1,1,1,1,1,1,1,1,1,1,1,1,1,1,1,1,1,1,1,1,1,1,1,1,1,1,1,1,1,1,1,1,1,1,
1,1,1,1,1,1,1,1,1,1,1,1,1,1,1,1,1,1,1,1,1,1,1,1,1,1,1,1,1,1,1,1,1,1,1,1,
1,1,1,1,1,1,1,1,1,1,1,1,1,1,1,1,1,1,1,1,1,1,1,1,1,1,1,1,1,1,1,1,1,1,1,1,
1,1,1,1,1,1,1,1,1,1,1,1,1,1,1,1,1,1,1,1,1,1,1,1,1,1,1,1,1,1,1,1,1,1,1,1,
1,1,1,1,1,1,1,1,1,1,1,1,1,1,1,1,1,1,1,1,1,1,1,6),(-0.941429844431354,-0.940000000000001,
-0.935000000000001,-0.930000000000001,-0.925000000000001,-0.920000000000001,
-0.915000000000001,-0.910000000000001,-0.905000000000001,-0.900000000000001,
-0.895000000000001,-0.890000000000001,-0.885000000000001,-0.880000000000001,
-0.875000000000001,-0.870000000000001,-0.865000000000001,-0.860000000000001,
-0.855000000000001,-0.850000000000001,-0.845000000000001,-0.840000000000001,
-0.835000000000001,-0.830000000000001,-0.825000000000001,-0.820000000000001,
-0.815000000000001,-0.810000000000001,-0.805000000000001,-0.800000000000001,
-0.795000000000001,-0.790000000000001,-0.785000000000001,-0.780000000000001,
-0.775000000000001,-0.770000000000001,-0.765000000000001,-0.760000000000001,
-0.755000000000001,-0.750000000000001,-0.745000000000001,-0.740000000000001,
-0.735000000000001,-0.730000000000001,-0.725000000000001,-0.720000000000001,
-0.715000000000001,-0.710000000000001,-0.705000000000001,-0.700000000000001,
-0.695000000000001,-0.690000000000001,-0.685,-0.68,-0.675,-0.67,-0.665,
-0.66,-0.655,-0.65,-0.645,-0.64,-0.635,-0.63,-0.625,-0.62,-0.615,-0.61,
-0.605,-0.6,-0.595,-0.59,-0.585,-0.58,-0.575,-0.57,-0.565,-0.56,-0.555,
-0.55,-0.545,-0.54,-0.535,-0.53,-0.525,-0.52,-0.515,-0.51,-0.505,-0.5,-0.495,
-0.49,-0.485,-0.48,-0.475,-0.47,-0.465,-0.46,-0.455,-0.45,-0.445,-0.44,
-0.435,-0.43,-0.425,-0.42,-0.415,-0.41,-0.405,-0.4,-0.395,-0.39,-0.385,
-0.38,-0.375,-0.37,-0.365,-0.36,-0.355,-0.35,-0.345,-0.34,-0.335,-0.33,
-0.325,-0.32,-0.315,-0.31,-0.305,-0.3,-0.295,-0.29,-0.285,-0.28,-0.275,
-0.27,-0.265,-0.26,-0.255,-0.25,-0.245,-0.24,-0.235,-0.23,-0.225,-0.22,
-0.215,-0.21,-0.205,-0.2,-0.195,-0.19,-0.185,-0.18,-0.175,-0.17,-0.165,
-0.16,-0.155,-0.15,-0.145,-0.14,-0.135,-0.13,-0.125,-0.12,-0.115,-0.11,
-0.105,-0.1,-0.095,-0.09,-0.085,-0.08,-0.075,-0.07,-0.065,-0.06,-0.055,
-0.05,-0.045,-0.04,-0.035,-0.03,-0.025,-0.02,-0.015,-0.01,-0.005,0.),
 .UNSPECIFIED.)
CURVE()
GEOMETRIC_REPRESENTATION_ITEM()
RATIONAL_B_SPLINE_CURVE((1.,1.,1.,1.,1.,1.,1.,1.,1.,1.,1.,1.,1.,1.,1.,1.,
1.,1.,1.,1.,1.,1.,1.,1.,1.,1.,1.,1.,1.,1.,1.,1.,1.,1.,1.,1.,1.,1.,1.,1.,
1.,1.,1.,1.,1.,1.,1.,1.,1.,1.,1.,1.,1.,1.,1.,1.,1.,1.,1.,1.,1.,1.,1.,1.,
1.,1.,1.,1.,1.,1.,1.,1.,1.,1.,1.,1.,1.,1.,1.,1.,1.,1.,1.,1.,1.,1.,1.,1.,
1.,1.,1.,1.,1.,1.,1.,1.,1.,1.,1.,1.,1.,1.,1.,1.,1.,1.,1.,1.,1.,1.,1.,1.,
1.,1.,1.,1.,1.,1.,1.,1.,1.,1.,1.,1.,1.,1.,1.,1.,1.,1.,1.,1.,1.,1.,1.,1.,
1.,1.,1.,1.,1.,1.,1.,1.,1.,1.,1.,1.,1.,1.,1.,1.,1.,1.,1.,1.,1.,1.,1.,1.,
1.,1.,1.,1.,1.,1.,1.,1.,1.,1.,1.,1.,1.,1.,1.,1.,1.,1.,1.,1.,1.,1.,1.,1.,
1.,1.,1.,1.,1.,1.,1.,1.,1.,1.))
REPRESENTATION_ITEM('')
);
#415=(
BOUNDED_CURVE()
B_SPLINE_CURVE(5,(#58409,#58410,#58411,#58412,#58413,#58414,#58415,#58416,
#58417,#58418,#58419,#58420,#58421,#58422,#58423,#58424,#58425,#58426,#58427,
#58428,#58429,#58430,#58431,#58432,#58433,#58434,#58435,#58436,#58437,#58438,
#58439,#58440,#58441,#58442,#58443,#58444,#58445,#58446,#58447,#58448,#58449,
#58450,#58451,#58452,#58453,#58454,#58455,#58456,#58457,#58458,#58459,#58460,
#58461,#58462,#58463,#58464,#58465,#58466,#58467,#58468,#58469,#58470,#58471,
#58472,#58473,#58474,#58475,#58476,#58477,#58478,#58479,#58480,#58481,#58482,
#58483,#58484,#58485,#58486,#58487,#58488,#58489,#58490,#58491,#58492,#58493,
#58494,#58495,#58496,#58497,#58498,#58499,#58500,#58501,#58502,#58503,#58504,
#58505,#58506,#58507,#58508,#58509,#58510,#58511,#58512,#58513,#58514,#58515,
#58516,#58517,#58518,#58519,#58520,#58521,#58522,#58523,#58524,#58525,#58526,
#58527,#58528,#58529,#58530,#58531,#58532,#58533,#58534,#58535,#58536,#58537,
#58538,#58539,#58540,#58541,#58542,#58543,#58544,#58545,#58546,#58547,#58548,
#58549,#58550,#58551,#58552,#58553,#58554,#58555,#58556,#58557,#58558,#58559,
#58560,#58561,#58562,#58563,#58564,#58565,#58566,#58567,#58568,#58569,#58570,
#58571,#58572,#58573,#58574,#58575,#58576,#58577,#58578,#58579,#58580,#58581,
#58582,#58583,#58584,#58585,#58586,#58587,#58588,#58589,#58590,#58591,#58592,
#58593,#58594,#58595,#58596,#58597,#58598,#58599,#58600,#58601,#58602),
 .UNSPECIFIED.,.F.,.F.)
B_SPLINE_CURVE_WITH_KNOTS((6,1,1,1,1,1,1,1,1,1,1,1,1,1,1,1,1,1,1,1,1,1,
1,1,1,1,1,1,1,1,1,1,1,1,1,1,1,1,1,1,1,1,1,1,1,1,1,1,1,1,1,1,1,1,1,1,1,1,
1,1,1,1,1,1,1,1,1,1,1,1,1,1,1,1,1,1,1,1,1,1,1,1,1,1,1,1,1,1,1,1,1,1,1,1,
1,1,1,1,1,1,1,1,1,1,1,1,1,1,1,1,1,1,1,1,1,1,1,1,1,1,1,1,1,1,1,1,1,1,1,1,
1,1,1,1,1,1,1,1,1,1,1,1,1,1,1,1,1,1,1,1,1,1,1,1,1,1,1,1,1,1,1,1,1,1,1,1,
1,1,1,1,1,1,1,1,1,1,1,1,1,1,1,1,1,1,1,1,1,1,1,6),(0.,0.005,0.01,0.015,0.02,
0.025,0.03,0.035,0.04,0.045,0.05,0.055,0.06,0.065,0.07,0.075,0.08,0.085,
0.09,0.095,0.1,0.105,0.11,0.115,0.12,0.125,0.13,0.135,0.14,0.145,0.15,0.155,
0.16,0.165,0.17,0.175,0.18,0.185,0.19,0.195,0.2,0.205,0.21,0.215,0.22,0.225,
0.23,0.235,0.24,0.245,0.25,0.255,0.26,0.265,0.27,0.275,0.28,0.285,0.29,
0.295,0.3,0.305,0.31,0.315,0.32,0.325,0.33,0.335,0.34,0.345,0.35,0.355,
0.36,0.365,0.37,0.375,0.38,0.385,0.39,0.395,0.4,0.405,0.41,0.415,0.42,0.425,
0.43,0.435,0.44,0.445,0.45,0.455,0.46,0.465,0.47,0.475,0.48,0.485,0.49,
0.495,0.5,0.505,0.51,0.515,0.52,0.525,0.53,0.535,0.54,0.545,0.55,0.555,
0.56,0.565,0.57,0.575,0.58,0.585,0.59,0.595,0.6,0.605,0.61,0.615,0.62,0.625,
0.63,0.635,0.64,0.645,0.65,0.655,0.66,0.665,0.67,0.675,0.68,0.685,0.690000000000001,
0.695000000000001,0.700000000000001,0.705000000000001,0.710000000000001,
0.715000000000001,0.720000000000001,0.725000000000001,0.730000000000001,
0.735000000000001,0.740000000000001,0.745000000000001,0.750000000000001,
0.755000000000001,0.760000000000001,0.765000000000001,0.770000000000001,
0.775000000000001,0.780000000000001,0.785000000000001,0.790000000000001,
0.795000000000001,0.800000000000001,0.805000000000001,0.810000000000001,
0.815000000000001,0.820000000000001,0.825000000000001,0.830000000000001,
0.835000000000001,0.840000000000001,0.845000000000001,0.850000000000001,
0.855000000000001,0.860000000000001,0.865000000000001,0.870000000000001,
0.875000000000001,0.880000000000001,0.885000000000001,0.890000000000001,
0.895000000000001,0.900000000000001,0.905000000000001,0.910000000000001,
0.915000000000001,0.920000000000001,0.925000000000001,0.930000000000001,
0.935000000000001,0.940000000000001,0.941429844431335),.UNSPECIFIED.)
CURVE()
GEOMETRIC_REPRESENTATION_ITEM()
RATIONAL_B_SPLINE_CURVE((1.,1.,1.,1.,1.,1.,1.,1.,1.,1.,1.,1.,1.,1.,1.,1.,
1.,1.,1.,1.,1.,1.,1.,1.,1.,1.,1.,1.,1.,1.,1.,1.,1.,1.,1.,1.,1.,1.,1.,1.,
1.,1.,1.,1.,1.,1.,1.,1.,1.,1.,1.,1.,1.,1.,1.,1.,1.,1.,1.,1.,1.,1.,1.,1.,
1.,1.,1.,1.,1.,1.,1.,1.,1.,1.,1.,1.,1.,1.,1.,1.,1.,1.,1.,1.,1.,1.,1.,1.,
1.,1.,1.,1.,1.,1.,1.,1.,1.,1.,1.,1.,1.,1.,1.,1.,1.,1.,1.,1.,1.,1.,1.,1.,
1.,1.,1.,1.,1.,1.,1.,1.,1.,1.,1.,1.,1.,1.,1.,1.,1.,1.,1.,1.,1.,1.,1.,1.,
1.,1.,1.,1.,1.,1.,1.,1.,1.,1.,1.,1.,1.,1.,1.,1.,1.,1.,1.,1.,1.,1.,1.,1.,
1.,1.,1.,1.,1.,1.,1.,1.,1.,1.,1.,1.,1.,1.,1.,1.,1.,1.,1.,1.,1.,1.,1.,1.,
1.,1.,1.,1.,1.,1.,1.,1.,1.,1.))
REPRESENTATION_ITEM('')
);
#416=(
BOUNDED_CURVE()
B_SPLINE_CURVE(5,(#58605,#58606,#58607,#58608,#58609,#58610,#58611,#58612,
#58613,#58614,#58615,#58616,#58617,#58618,#58619,#58620,#58621,#58622,#58623,
#58624,#58625,#58626,#58627,#58628,#58629,#58630,#58631,#58632,#58633,#58634,
#58635,#58636,#58637,#58638,#58639,#58640,#58641,#58642,#58643,#58644,#58645,
#58646,#58647,#58648,#58649,#58650,#58651,#58652,#58653,#58654,#58655,#58656,
#58657,#58658,#58659,#58660,#58661,#58662,#58663,#58664,#58665,#58666,#58667,
#58668,#58669,#58670,#58671,#58672,#58673,#58674,#58675,#58676,#58677,#58678,
#58679,#58680,#58681,#58682,#58683,#58684,#58685,#58686,#58687,#58688,#58689,
#58690,#58691,#58692,#58693,#58694,#58695,#58696,#58697,#58698,#58699,#58700,
#58701,#58702,#58703,#58704,#58705,#58706,#58707,#58708,#58709,#58710,#58711,
#58712,#58713,#58714,#58715,#58716,#58717,#58718,#58719,#58720,#58721,#58722,
#58723,#58724,#58725,#58726,#58727,#58728,#58729,#58730,#58731,#58732,#58733,
#58734,#58735,#58736,#58737,#58738,#58739,#58740,#58741,#58742,#58743,#58744,
#58745,#58746,#58747,#58748,#58749,#58750,#58751,#58752,#58753,#58754,#58755,
#58756,#58757,#58758,#58759,#58760,#58761,#58762,#58763,#58764,#58765,#58766,
#58767,#58768,#58769,#58770,#58771,#58772,#58773,#58774,#58775,#58776,#58777,
#58778,#58779,#58780,#58781,#58782,#58783,#58784,#58785,#58786,#58787,#58788,
#58789,#58790,#58791,#58792,#58793,#58794,#58795,#58796,#58797,#58798),
 .UNSPECIFIED.,.F.,.F.)
B_SPLINE_CURVE_WITH_KNOTS((6,1,1,1,1,1,1,1,1,1,1,1,1,1,1,1,1,1,1,1,1,1,
1,1,1,1,1,1,1,1,1,1,1,1,1,1,1,1,1,1,1,1,1,1,1,1,1,1,1,1,1,1,1,1,1,1,1,1,
1,1,1,1,1,1,1,1,1,1,1,1,1,1,1,1,1,1,1,1,1,1,1,1,1,1,1,1,1,1,1,1,1,1,1,1,
1,1,1,1,1,1,1,1,1,1,1,1,1,1,1,1,1,1,1,1,1,1,1,1,1,1,1,1,1,1,1,1,1,1,1,1,
1,1,1,1,1,1,1,1,1,1,1,1,1,1,1,1,1,1,1,1,1,1,1,1,1,1,1,1,1,1,1,1,1,1,1,1,
1,1,1,1,1,1,1,1,1,1,1,1,1,1,1,1,1,1,1,1,1,1,1,6),(-0.941429844431332,-0.940000000000001,
-0.935000000000001,-0.930000000000001,-0.925000000000001,-0.920000000000001,
-0.915000000000001,-0.910000000000001,-0.905000000000001,-0.900000000000001,
-0.895000000000001,-0.890000000000001,-0.885000000000001,-0.880000000000001,
-0.875000000000001,-0.870000000000001,-0.865000000000001,-0.860000000000001,
-0.855000000000001,-0.850000000000001,-0.845000000000001,-0.840000000000001,
-0.835000000000001,-0.830000000000001,-0.825000000000001,-0.820000000000001,
-0.815000000000001,-0.810000000000001,-0.805000000000001,-0.800000000000001,
-0.795000000000001,-0.790000000000001,-0.785000000000001,-0.780000000000001,
-0.775000000000001,-0.770000000000001,-0.765000000000001,-0.760000000000001,
-0.755000000000001,-0.750000000000001,-0.745000000000001,-0.740000000000001,
-0.735000000000001,-0.730000000000001,-0.725000000000001,-0.720000000000001,
-0.715000000000001,-0.710000000000001,-0.705000000000001,-0.700000000000001,
-0.695000000000001,-0.690000000000001,-0.685,-0.68,-0.675,-0.67,-0.665,
-0.66,-0.655,-0.65,-0.645,-0.64,-0.635,-0.63,-0.625,-0.62,-0.615,-0.61,
-0.605,-0.6,-0.595,-0.59,-0.585,-0.58,-0.575,-0.57,-0.565,-0.56,-0.555,
-0.55,-0.545,-0.54,-0.535,-0.53,-0.525,-0.52,-0.515,-0.51,-0.505,-0.5,-0.495,
-0.49,-0.485,-0.48,-0.475,-0.47,-0.465,-0.46,-0.455,-0.45,-0.445,-0.44,
-0.435,-0.43,-0.425,-0.42,-0.415,-0.41,-0.405,-0.4,-0.395,-0.39,-0.385,
-0.38,-0.375,-0.37,-0.365,-0.36,-0.355,-0.35,-0.345,-0.34,-0.335,-0.33,
-0.325,-0.32,-0.315,-0.31,-0.305,-0.3,-0.295,-0.29,-0.285,-0.28,-0.275,
-0.27,-0.265,-0.26,-0.255,-0.25,-0.245,-0.24,-0.235,-0.23,-0.225,-0.22,
-0.215,-0.21,-0.205,-0.2,-0.195,-0.19,-0.185,-0.18,-0.175,-0.17,-0.165,
-0.16,-0.155,-0.15,-0.145,-0.14,-0.135,-0.13,-0.125,-0.12,-0.115,-0.11,
-0.105,-0.1,-0.095,-0.09,-0.085,-0.08,-0.075,-0.07,-0.065,-0.06,-0.055,
-0.05,-0.045,-0.04,-0.035,-0.03,-0.025,-0.02,-0.015,-0.01,-0.005,0.),
 .UNSPECIFIED.)
CURVE()
GEOMETRIC_REPRESENTATION_ITEM()
RATIONAL_B_SPLINE_CURVE((1.,1.,1.,1.,1.,1.,1.,1.,1.,1.,1.,1.,1.,1.,1.,1.,
1.,1.,1.,1.,1.,1.,1.,1.,1.,1.,1.,1.,1.,1.,1.,1.,1.,1.,1.,1.,1.,1.,1.,1.,
1.,1.,1.,1.,1.,1.,1.,1.,1.,1.,1.,1.,1.,1.,1.,1.,1.,1.,1.,1.,1.,1.,1.,1.,
1.,1.,1.,1.,1.,1.,1.,1.,1.,1.,1.,1.,1.,1.,1.,1.,1.,1.,1.,1.,1.,1.,1.,1.,
1.,1.,1.,1.,1.,1.,1.,1.,1.,1.,1.,1.,1.,1.,1.,1.,1.,1.,1.,1.,1.,1.,1.,1.,
1.,1.,1.,1.,1.,1.,1.,1.,1.,1.,1.,1.,1.,1.,1.,1.,1.,1.,1.,1.,1.,1.,1.,1.,
1.,1.,1.,1.,1.,1.,1.,1.,1.,1.,1.,1.,1.,1.,1.,1.,1.,1.,1.,1.,1.,1.,1.,1.,
1.,1.,1.,1.,1.,1.,1.,1.,1.,1.,1.,1.,1.,1.,1.,1.,1.,1.,1.,1.,1.,1.,1.,1.,
1.,1.,1.,1.,1.,1.,1.,1.,1.,1.))
REPRESENTATION_ITEM('')
);
#417=(
BOUNDED_CURVE()
B_SPLINE_CURVE(5,(#59305,#59306,#59307,#59308,#59309,#59310,#59311,#59312,
#59313,#59314,#59315,#59316,#59317,#59318,#59319,#59320,#59321,#59322,#59323,
#59324,#59325,#59326,#59327,#59328,#59329,#59330,#59331,#59332,#59333,#59334,
#59335,#59336,#59337,#59338,#59339,#59340,#59341,#59342,#59343,#59344,#59345,
#59346,#59347,#59348,#59349,#59350,#59351,#59352,#59353,#59354,#59355,#59356,
#59357,#59358,#59359,#59360,#59361,#59362,#59363,#59364,#59365,#59366,#59367,
#59368,#59369,#59370,#59371,#59372,#59373,#59374,#59375,#59376,#59377,#59378,
#59379,#59380,#59381,#59382,#59383,#59384,#59385,#59386,#59387,#59388,#59389,
#59390,#59391,#59392,#59393,#59394,#59395,#59396,#59397,#59398,#59399,#59400,
#59401,#59402,#59403,#59404,#59405,#59406,#59407,#59408,#59409,#59410,#59411,
#59412,#59413,#59414,#59415,#59416,#59417,#59418,#59419,#59420,#59421,#59422,
#59423,#59424,#59425,#59426,#59427,#59428,#59429,#59430,#59431,#59432,#59433,
#59434,#59435,#59436,#59437,#59438,#59439,#59440,#59441,#59442,#59443,#59444,
#59445,#59446,#59447,#59448,#59449,#59450,#59451,#59452,#59453,#59454,#59455,
#59456,#59457,#59458,#59459,#59460,#59461,#59462,#59463,#59464,#59465,#59466,
#59467,#59468,#59469,#59470,#59471,#59472,#59473,#59474,#59475,#59476,#59477,
#59478,#59479,#59480,#59481,#59482,#59483,#59484,#59485,#59486,#59487,#59488,
#59489,#59490,#59491,#59492,#59493,#59494,#59495,#59496,#59497,#59498),
 .UNSPECIFIED.,.F.,.F.)
B_SPLINE_CURVE_WITH_KNOTS((6,1,1,1,1,1,1,1,1,1,1,1,1,1,1,1,1,1,1,1,1,1,
1,1,1,1,1,1,1,1,1,1,1,1,1,1,1,1,1,1,1,1,1,1,1,1,1,1,1,1,1,1,1,1,1,1,1,1,
1,1,1,1,1,1,1,1,1,1,1,1,1,1,1,1,1,1,1,1,1,1,1,1,1,1,1,1,1,1,1,1,1,1,1,1,
1,1,1,1,1,1,1,1,1,1,1,1,1,1,1,1,1,1,1,1,1,1,1,1,1,1,1,1,1,1,1,1,1,1,1,1,
1,1,1,1,1,1,1,1,1,1,1,1,1,1,1,1,1,1,1,1,1,1,1,1,1,1,1,1,1,1,1,1,1,1,1,1,
1,1,1,1,1,1,1,1,1,1,1,1,1,1,1,1,1,1,1,1,1,1,1,6),(0.,0.005,0.01,0.015,0.02,
0.025,0.03,0.035,0.04,0.045,0.05,0.055,0.06,0.065,0.07,0.075,0.08,0.085,
0.09,0.095,0.1,0.105,0.11,0.115,0.12,0.125,0.13,0.135,0.14,0.145,0.15,0.155,
0.16,0.165,0.17,0.175,0.18,0.185,0.19,0.195,0.2,0.205,0.21,0.215,0.22,0.225,
0.23,0.235,0.24,0.245,0.25,0.255,0.26,0.265,0.27,0.275,0.28,0.285,0.29,
0.295,0.3,0.305,0.31,0.315,0.32,0.325,0.33,0.335,0.34,0.345,0.35,0.355,
0.36,0.365,0.37,0.375,0.38,0.385,0.39,0.395,0.4,0.405,0.41,0.415,0.42,0.425,
0.43,0.435,0.44,0.445,0.45,0.455,0.46,0.465,0.47,0.475,0.48,0.485,0.49,
0.495,0.5,0.505,0.51,0.515,0.52,0.525,0.53,0.535,0.54,0.545,0.55,0.555,
0.56,0.565,0.57,0.575,0.58,0.585,0.59,0.595,0.6,0.605,0.61,0.615,0.62,0.625,
0.63,0.635,0.64,0.645,0.65,0.655,0.66,0.665,0.67,0.675,0.68,0.685,0.690000000000001,
0.695000000000001,0.700000000000001,0.705000000000001,0.710000000000001,
0.715000000000001,0.720000000000001,0.725000000000001,0.730000000000001,
0.735000000000001,0.740000000000001,0.745000000000001,0.750000000000001,
0.755000000000001,0.760000000000001,0.765000000000001,0.770000000000001,
0.775000000000001,0.780000000000001,0.785000000000001,0.790000000000001,
0.795000000000001,0.800000000000001,0.805000000000001,0.810000000000001,
0.815000000000001,0.820000000000001,0.825000000000001,0.830000000000001,
0.835000000000001,0.840000000000001,0.845000000000001,0.850000000000001,
0.855000000000001,0.860000000000001,0.865000000000001,0.870000000000001,
0.875000000000001,0.880000000000001,0.885000000000001,0.890000000000001,
0.895000000000001,0.900000000000001,0.905000000000001,0.910000000000001,
0.915000000000001,0.920000000000001,0.925000000000001,0.930000000000001,
0.935000000000001,0.940000000000001,0.941429844431367),.UNSPECIFIED.)
CURVE()
GEOMETRIC_REPRESENTATION_ITEM()
RATIONAL_B_SPLINE_CURVE((1.,1.,1.,1.,1.,1.,1.,1.,1.,1.,1.,1.,1.,1.,1.,1.,
1.,1.,1.,1.,1.,1.,1.,1.,1.,1.,1.,1.,1.,1.,1.,1.,1.,1.,1.,1.,1.,1.,1.,1.,
1.,1.,1.,1.,1.,1.,1.,1.,1.,1.,1.,1.,1.,1.,1.,1.,1.,1.,1.,1.,1.,1.,1.,1.,
1.,1.,1.,1.,1.,1.,1.,1.,1.,1.,1.,1.,1.,1.,1.,1.,1.,1.,1.,1.,1.,1.,1.,1.,
1.,1.,1.,1.,1.,1.,1.,1.,1.,1.,1.,1.,1.,1.,1.,1.,1.,1.,1.,1.,1.,1.,1.,1.,
1.,1.,1.,1.,1.,1.,1.,1.,1.,1.,1.,1.,1.,1.,1.,1.,1.,1.,1.,1.,1.,1.,1.,1.,
1.,1.,1.,1.,1.,1.,1.,1.,1.,1.,1.,1.,1.,1.,1.,1.,1.,1.,1.,1.,1.,1.,1.,1.,
1.,1.,1.,1.,1.,1.,1.,1.,1.,1.,1.,1.,1.,1.,1.,1.,1.,1.,1.,1.,1.,1.,1.,1.,
1.,1.,1.,1.,1.,1.,1.,1.,1.,1.))
REPRESENTATION_ITEM('')
);
#418=(
BOUNDED_CURVE()
B_SPLINE_CURVE(5,(#59501,#59502,#59503,#59504,#59505,#59506,#59507,#59508,
#59509,#59510,#59511,#59512,#59513,#59514,#59515,#59516,#59517,#59518,#59519,
#59520,#59521,#59522,#59523,#59524,#59525,#59526,#59527,#59528,#59529,#59530,
#59531,#59532,#59533,#59534,#59535,#59536,#59537,#59538,#59539,#59540,#59541,
#59542,#59543,#59544,#59545,#59546,#59547,#59548,#59549,#59550,#59551,#59552,
#59553,#59554,#59555,#59556,#59557,#59558,#59559,#59560,#59561,#59562,#59563,
#59564,#59565,#59566,#59567,#59568,#59569,#59570,#59571,#59572,#59573,#59574,
#59575,#59576,#59577,#59578,#59579,#59580,#59581,#59582,#59583,#59584,#59585,
#59586,#59587,#59588,#59589,#59590,#59591,#59592,#59593,#59594,#59595,#59596,
#59597,#59598,#59599,#59600,#59601,#59602,#59603,#59604,#59605,#59606,#59607,
#59608,#59609,#59610,#59611,#59612,#59613,#59614,#59615,#59616,#59617,#59618,
#59619,#59620,#59621,#59622,#59623,#59624,#59625,#59626,#59627,#59628,#59629,
#59630,#59631,#59632,#59633,#59634,#59635,#59636,#59637,#59638,#59639,#59640,
#59641,#59642,#59643,#59644,#59645,#59646,#59647,#59648,#59649,#59650,#59651,
#59652,#59653,#59654,#59655,#59656,#59657,#59658,#59659,#59660,#59661,#59662,
#59663,#59664,#59665,#59666,#59667,#59668,#59669,#59670,#59671,#59672,#59673,
#59674,#59675,#59676,#59677,#59678,#59679,#59680,#59681,#59682,#59683,#59684,
#59685,#59686,#59687,#59688,#59689,#59690,#59691,#59692,#59693,#59694),
 .UNSPECIFIED.,.F.,.F.)
B_SPLINE_CURVE_WITH_KNOTS((6,1,1,1,1,1,1,1,1,1,1,1,1,1,1,1,1,1,1,1,1,1,
1,1,1,1,1,1,1,1,1,1,1,1,1,1,1,1,1,1,1,1,1,1,1,1,1,1,1,1,1,1,1,1,1,1,1,1,
1,1,1,1,1,1,1,1,1,1,1,1,1,1,1,1,1,1,1,1,1,1,1,1,1,1,1,1,1,1,1,1,1,1,1,1,
1,1,1,1,1,1,1,1,1,1,1,1,1,1,1,1,1,1,1,1,1,1,1,1,1,1,1,1,1,1,1,1,1,1,1,1,
1,1,1,1,1,1,1,1,1,1,1,1,1,1,1,1,1,1,1,1,1,1,1,1,1,1,1,1,1,1,1,1,1,1,1,1,
1,1,1,1,1,1,1,1,1,1,1,1,1,1,1,1,1,1,1,1,1,1,1,6),(-0.941429844431342,-0.940000000000001,
-0.935000000000001,-0.930000000000001,-0.925000000000001,-0.920000000000001,
-0.915000000000001,-0.910000000000001,-0.905000000000001,-0.900000000000001,
-0.895000000000001,-0.890000000000001,-0.885000000000001,-0.880000000000001,
-0.875000000000001,-0.870000000000001,-0.865000000000001,-0.860000000000001,
-0.855000000000001,-0.850000000000001,-0.845000000000001,-0.840000000000001,
-0.835000000000001,-0.830000000000001,-0.825000000000001,-0.820000000000001,
-0.815000000000001,-0.810000000000001,-0.805000000000001,-0.800000000000001,
-0.795000000000001,-0.790000000000001,-0.785000000000001,-0.780000000000001,
-0.775000000000001,-0.770000000000001,-0.765000000000001,-0.760000000000001,
-0.755000000000001,-0.750000000000001,-0.745000000000001,-0.740000000000001,
-0.735000000000001,-0.730000000000001,-0.725000000000001,-0.720000000000001,
-0.715000000000001,-0.710000000000001,-0.705000000000001,-0.700000000000001,
-0.695000000000001,-0.690000000000001,-0.685,-0.68,-0.675,-0.67,-0.665,
-0.66,-0.655,-0.65,-0.645,-0.64,-0.635,-0.63,-0.625,-0.62,-0.615,-0.61,
-0.605,-0.6,-0.595,-0.59,-0.585,-0.58,-0.575,-0.57,-0.565,-0.56,-0.555,
-0.55,-0.545,-0.54,-0.535,-0.53,-0.525,-0.52,-0.515,-0.51,-0.505,-0.5,-0.495,
-0.49,-0.485,-0.48,-0.475,-0.47,-0.465,-0.46,-0.455,-0.45,-0.445,-0.44,
-0.435,-0.43,-0.425,-0.42,-0.415,-0.41,-0.405,-0.4,-0.395,-0.39,-0.385,
-0.38,-0.375,-0.37,-0.365,-0.36,-0.355,-0.35,-0.345,-0.34,-0.335,-0.33,
-0.325,-0.32,-0.315,-0.31,-0.305,-0.3,-0.295,-0.29,-0.285,-0.28,-0.275,
-0.27,-0.265,-0.26,-0.255,-0.25,-0.245,-0.24,-0.235,-0.23,-0.225,-0.22,
-0.215,-0.21,-0.205,-0.2,-0.195,-0.19,-0.185,-0.18,-0.175,-0.17,-0.165,
-0.16,-0.155,-0.15,-0.145,-0.14,-0.135,-0.13,-0.125,-0.12,-0.115,-0.11,
-0.105,-0.1,-0.095,-0.09,-0.085,-0.08,-0.075,-0.07,-0.065,-0.06,-0.055,
-0.05,-0.045,-0.04,-0.035,-0.03,-0.025,-0.02,-0.015,-0.01,-0.005,0.),
 .UNSPECIFIED.)
CURVE()
GEOMETRIC_REPRESENTATION_ITEM()
RATIONAL_B_SPLINE_CURVE((1.,1.,1.,1.,1.,1.,1.,1.,1.,1.,1.,1.,1.,1.,1.,1.,
1.,1.,1.,1.,1.,1.,1.,1.,1.,1.,1.,1.,1.,1.,1.,1.,1.,1.,1.,1.,1.,1.,1.,1.,
1.,1.,1.,1.,1.,1.,1.,1.,1.,1.,1.,1.,1.,1.,1.,1.,1.,1.,1.,1.,1.,1.,1.,1.,
1.,1.,1.,1.,1.,1.,1.,1.,1.,1.,1.,1.,1.,1.,1.,1.,1.,1.,1.,1.,1.,1.,1.,1.,
1.,1.,1.,1.,1.,1.,1.,1.,1.,1.,1.,1.,1.,1.,1.,1.,1.,1.,1.,1.,1.,1.,1.,1.,
1.,1.,1.,1.,1.,1.,1.,1.,1.,1.,1.,1.,1.,1.,1.,1.,1.,1.,1.,1.,1.,1.,1.,1.,
1.,1.,1.,1.,1.,1.,1.,1.,1.,1.,1.,1.,1.,1.,1.,1.,1.,1.,1.,1.,1.,1.,1.,1.,
1.,1.,1.,1.,1.,1.,1.,1.,1.,1.,1.,1.,1.,1.,1.,1.,1.,1.,1.,1.,1.,1.,1.,1.,
1.,1.,1.,1.,1.,1.,1.,1.,1.,1.))
REPRESENTATION_ITEM('')
);
#419=(
BOUNDED_CURVE()
B_SPLINE_CURVE(5,(#60201,#60202,#60203,#60204,#60205,#60206,#60207,#60208,
#60209,#60210,#60211,#60212,#60213,#60214,#60215,#60216,#60217,#60218,#60219,
#60220,#60221,#60222,#60223,#60224,#60225,#60226,#60227,#60228,#60229,#60230,
#60231,#60232,#60233,#60234,#60235,#60236,#60237,#60238,#60239,#60240,#60241,
#60242,#60243,#60244,#60245,#60246,#60247,#60248,#60249,#60250,#60251,#60252,
#60253,#60254,#60255,#60256,#60257,#60258,#60259,#60260,#60261,#60262,#60263,
#60264,#60265,#60266,#60267,#60268,#60269,#60270,#60271,#60272,#60273,#60274,
#60275,#60276,#60277,#60278,#60279,#60280,#60281,#60282,#60283,#60284,#60285,
#60286,#60287,#60288,#60289,#60290,#60291,#60292,#60293,#60294,#60295,#60296,
#60297,#60298,#60299,#60300,#60301,#60302,#60303,#60304,#60305,#60306,#60307,
#60308,#60309,#60310,#60311,#60312,#60313,#60314,#60315,#60316,#60317,#60318,
#60319,#60320,#60321,#60322,#60323,#60324,#60325,#60326,#60327,#60328,#60329,
#60330,#60331,#60332,#60333,#60334,#60335,#60336,#60337,#60338,#60339,#60340,
#60341,#60342,#60343,#60344,#60345,#60346,#60347,#60348,#60349,#60350,#60351,
#60352,#60353,#60354,#60355,#60356,#60357,#60358,#60359,#60360,#60361,#60362,
#60363,#60364,#60365,#60366,#60367,#60368,#60369,#60370,#60371,#60372,#60373,
#60374,#60375,#60376,#60377,#60378,#60379,#60380,#60381,#60382,#60383,#60384,
#60385,#60386,#60387,#60388,#60389,#60390,#60391,#60392,#60393,#60394),
 .UNSPECIFIED.,.F.,.F.)
B_SPLINE_CURVE_WITH_KNOTS((6,1,1,1,1,1,1,1,1,1,1,1,1,1,1,1,1,1,1,1,1,1,
1,1,1,1,1,1,1,1,1,1,1,1,1,1,1,1,1,1,1,1,1,1,1,1,1,1,1,1,1,1,1,1,1,1,1,1,
1,1,1,1,1,1,1,1,1,1,1,1,1,1,1,1,1,1,1,1,1,1,1,1,1,1,1,1,1,1,1,1,1,1,1,1,
1,1,1,1,1,1,1,1,1,1,1,1,1,1,1,1,1,1,1,1,1,1,1,1,1,1,1,1,1,1,1,1,1,1,1,1,
1,1,1,1,1,1,1,1,1,1,1,1,1,1,1,1,1,1,1,1,1,1,1,1,1,1,1,1,1,1,1,1,1,1,1,1,
1,1,1,1,1,1,1,1,1,1,1,1,1,1,1,1,1,1,1,1,1,1,1,6),(0.,0.005,0.01,0.015,0.02,
0.025,0.03,0.035,0.04,0.045,0.05,0.055,0.06,0.065,0.07,0.075,0.08,0.085,
0.09,0.095,0.1,0.105,0.11,0.115,0.12,0.125,0.13,0.135,0.14,0.145,0.15,0.155,
0.16,0.165,0.17,0.175,0.18,0.185,0.19,0.195,0.2,0.205,0.21,0.215,0.22,0.225,
0.23,0.235,0.24,0.245,0.25,0.255,0.26,0.265,0.27,0.275,0.28,0.285,0.29,
0.295,0.3,0.305,0.31,0.315,0.32,0.325,0.33,0.335,0.34,0.345,0.35,0.355,
0.36,0.365,0.37,0.375,0.38,0.385,0.39,0.395,0.4,0.405,0.41,0.415,0.42,0.425,
0.43,0.435,0.44,0.445,0.45,0.455,0.46,0.465,0.47,0.475,0.48,0.485,0.49,
0.495,0.5,0.505,0.51,0.515,0.52,0.525,0.53,0.535,0.54,0.545,0.55,0.555,
0.56,0.565,0.57,0.575,0.58,0.585,0.59,0.595,0.6,0.605,0.61,0.615,0.62,0.625,
0.63,0.635,0.64,0.645,0.65,0.655,0.66,0.665,0.67,0.675,0.68,0.685,0.690000000000001,
0.695000000000001,0.700000000000001,0.705000000000001,0.710000000000001,
0.715000000000001,0.720000000000001,0.725000000000001,0.730000000000001,
0.735000000000001,0.740000000000001,0.745000000000001,0.750000000000001,
0.755000000000001,0.760000000000001,0.765000000000001,0.770000000000001,
0.775000000000001,0.780000000000001,0.785000000000001,0.790000000000001,
0.795000000000001,0.800000000000001,0.805000000000001,0.810000000000001,
0.815000000000001,0.820000000000001,0.825000000000001,0.830000000000001,
0.835000000000001,0.840000000000001,0.845000000000001,0.850000000000001,
0.855000000000001,0.860000000000001,0.865000000000001,0.870000000000001,
0.875000000000001,0.880000000000001,0.885000000000001,0.890000000000001,
0.895000000000001,0.900000000000001,0.905000000000001,0.910000000000001,
0.915000000000001,0.920000000000001,0.925000000000001,0.930000000000001,
0.935000000000001,0.940000000000001,0.941429844431369),.UNSPECIFIED.)
CURVE()
GEOMETRIC_REPRESENTATION_ITEM()
RATIONAL_B_SPLINE_CURVE((1.,1.,1.,1.,1.,1.,1.,1.,1.,1.,1.,1.,1.,1.,1.,1.,
1.,1.,1.,1.,1.,1.,1.,1.,1.,1.,1.,1.,1.,1.,1.,1.,1.,1.,1.,1.,1.,1.,1.,1.,
1.,1.,1.,1.,1.,1.,1.,1.,1.,1.,1.,1.,1.,1.,1.,1.,1.,1.,1.,1.,1.,1.,1.,1.,
1.,1.,1.,1.,1.,1.,1.,1.,1.,1.,1.,1.,1.,1.,1.,1.,1.,1.,1.,1.,1.,1.,1.,1.,
1.,1.,1.,1.,1.,1.,1.,1.,1.,1.,1.,1.,1.,1.,1.,1.,1.,1.,1.,1.,1.,1.,1.,1.,
1.,1.,1.,1.,1.,1.,1.,1.,1.,1.,1.,1.,1.,1.,1.,1.,1.,1.,1.,1.,1.,1.,1.,1.,
1.,1.,1.,1.,1.,1.,1.,1.,1.,1.,1.,1.,1.,1.,1.,1.,1.,1.,1.,1.,1.,1.,1.,1.,
1.,1.,1.,1.,1.,1.,1.,1.,1.,1.,1.,1.,1.,1.,1.,1.,1.,1.,1.,1.,1.,1.,1.,1.,
1.,1.,1.,1.,1.,1.,1.,1.,1.,1.))
REPRESENTATION_ITEM('')
);
#420=(
BOUNDED_CURVE()
B_SPLINE_CURVE(5,(#60397,#60398,#60399,#60400,#60401,#60402,#60403,#60404,
#60405,#60406,#60407,#60408,#60409,#60410,#60411,#60412,#60413,#60414,#60415,
#60416,#60417,#60418,#60419,#60420,#60421,#60422,#60423,#60424,#60425,#60426,
#60427,#60428,#60429,#60430,#60431,#60432,#60433,#60434,#60435,#60436,#60437,
#60438,#60439,#60440,#60441,#60442,#60443,#60444,#60445,#60446,#60447,#60448,
#60449,#60450,#60451,#60452,#60453,#60454,#60455,#60456,#60457,#60458,#60459,
#60460,#60461,#60462,#60463,#60464,#60465,#60466,#60467,#60468,#60469,#60470,
#60471,#60472,#60473,#60474,#60475,#60476,#60477,#60478,#60479,#60480,#60481,
#60482,#60483,#60484,#60485,#60486,#60487,#60488,#60489,#60490,#60491,#60492,
#60493,#60494,#60495,#60496,#60497,#60498,#60499,#60500,#60501,#60502,#60503,
#60504,#60505,#60506,#60507,#60508,#60509,#60510,#60511,#60512,#60513,#60514,
#60515,#60516,#60517,#60518,#60519,#60520,#60521,#60522,#60523,#60524,#60525,
#60526,#60527,#60528,#60529,#60530,#60531,#60532,#60533,#60534,#60535,#60536,
#60537,#60538,#60539,#60540,#60541,#60542,#60543,#60544,#60545,#60546,#60547,
#60548,#60549,#60550,#60551,#60552,#60553,#60554,#60555,#60556,#60557,#60558,
#60559,#60560,#60561,#60562,#60563,#60564,#60565,#60566,#60567,#60568,#60569,
#60570,#60571,#60572,#60573,#60574,#60575,#60576,#60577,#60578,#60579,#60580,
#60581,#60582,#60583,#60584,#60585,#60586,#60587,#60588,#60589,#60590),
 .UNSPECIFIED.,.F.,.F.)
B_SPLINE_CURVE_WITH_KNOTS((6,1,1,1,1,1,1,1,1,1,1,1,1,1,1,1,1,1,1,1,1,1,
1,1,1,1,1,1,1,1,1,1,1,1,1,1,1,1,1,1,1,1,1,1,1,1,1,1,1,1,1,1,1,1,1,1,1,1,
1,1,1,1,1,1,1,1,1,1,1,1,1,1,1,1,1,1,1,1,1,1,1,1,1,1,1,1,1,1,1,1,1,1,1,1,
1,1,1,1,1,1,1,1,1,1,1,1,1,1,1,1,1,1,1,1,1,1,1,1,1,1,1,1,1,1,1,1,1,1,1,1,
1,1,1,1,1,1,1,1,1,1,1,1,1,1,1,1,1,1,1,1,1,1,1,1,1,1,1,1,1,1,1,1,1,1,1,1,
1,1,1,1,1,1,1,1,1,1,1,1,1,1,1,1,1,1,1,1,1,1,1,6),(-0.941429844431369,-0.940000000000001,
-0.935000000000001,-0.930000000000001,-0.925000000000001,-0.920000000000001,
-0.915000000000001,-0.910000000000001,-0.905000000000001,-0.900000000000001,
-0.895000000000001,-0.890000000000001,-0.885000000000001,-0.880000000000001,
-0.875000000000001,-0.870000000000001,-0.865000000000001,-0.860000000000001,
-0.855000000000001,-0.850000000000001,-0.845000000000001,-0.840000000000001,
-0.835000000000001,-0.830000000000001,-0.825000000000001,-0.820000000000001,
-0.815000000000001,-0.810000000000001,-0.805000000000001,-0.800000000000001,
-0.795000000000001,-0.790000000000001,-0.785000000000001,-0.780000000000001,
-0.775000000000001,-0.770000000000001,-0.765000000000001,-0.760000000000001,
-0.755000000000001,-0.750000000000001,-0.745000000000001,-0.740000000000001,
-0.735000000000001,-0.730000000000001,-0.725000000000001,-0.720000000000001,
-0.715000000000001,-0.710000000000001,-0.705000000000001,-0.700000000000001,
-0.695000000000001,-0.690000000000001,-0.685,-0.68,-0.675,-0.67,-0.665,
-0.66,-0.655,-0.65,-0.645,-0.64,-0.635,-0.63,-0.625,-0.62,-0.615,-0.61,
-0.605,-0.6,-0.595,-0.59,-0.585,-0.58,-0.575,-0.57,-0.565,-0.56,-0.555,
-0.55,-0.545,-0.54,-0.535,-0.53,-0.525,-0.52,-0.515,-0.51,-0.505,-0.5,-0.495,
-0.49,-0.485,-0.48,-0.475,-0.47,-0.465,-0.46,-0.455,-0.45,-0.445,-0.44,
-0.435,-0.43,-0.425,-0.42,-0.415,-0.41,-0.405,-0.4,-0.395,-0.39,-0.385,
-0.38,-0.375,-0.37,-0.365,-0.36,-0.355,-0.35,-0.345,-0.34,-0.335,-0.33,
-0.325,-0.32,-0.315,-0.31,-0.305,-0.3,-0.295,-0.29,-0.285,-0.28,-0.275,
-0.27,-0.265,-0.26,-0.255,-0.25,-0.245,-0.24,-0.235,-0.23,-0.225,-0.22,
-0.215,-0.21,-0.205,-0.2,-0.195,-0.19,-0.185,-0.18,-0.175,-0.17,-0.165,
-0.16,-0.155,-0.15,-0.145,-0.14,-0.135,-0.13,-0.125,-0.12,-0.115,-0.11,
-0.105,-0.1,-0.095,-0.09,-0.085,-0.08,-0.075,-0.07,-0.065,-0.06,-0.055,
-0.05,-0.045,-0.04,-0.035,-0.03,-0.025,-0.02,-0.015,-0.01,-0.005,0.),
 .UNSPECIFIED.)
CURVE()
GEOMETRIC_REPRESENTATION_ITEM()
RATIONAL_B_SPLINE_CURVE((1.,1.,1.,1.,1.,1.,1.,1.,1.,1.,1.,1.,1.,1.,1.,1.,
1.,1.,1.,1.,1.,1.,1.,1.,1.,1.,1.,1.,1.,1.,1.,1.,1.,1.,1.,1.,1.,1.,1.,1.,
1.,1.,1.,1.,1.,1.,1.,1.,1.,1.,1.,1.,1.,1.,1.,1.,1.,1.,1.,1.,1.,1.,1.,1.,
1.,1.,1.,1.,1.,1.,1.,1.,1.,1.,1.,1.,1.,1.,1.,1.,1.,1.,1.,1.,1.,1.,1.,1.,
1.,1.,1.,1.,1.,1.,1.,1.,1.,1.,1.,1.,1.,1.,1.,1.,1.,1.,1.,1.,1.,1.,1.,1.,
1.,1.,1.,1.,1.,1.,1.,1.,1.,1.,1.,1.,1.,1.,1.,1.,1.,1.,1.,1.,1.,1.,1.,1.,
1.,1.,1.,1.,1.,1.,1.,1.,1.,1.,1.,1.,1.,1.,1.,1.,1.,1.,1.,1.,1.,1.,1.,1.,
1.,1.,1.,1.,1.,1.,1.,1.,1.,1.,1.,1.,1.,1.,1.,1.,1.,1.,1.,1.,1.,1.,1.,1.,
1.,1.,1.,1.,1.,1.,1.,1.,1.,1.))
REPRESENTATION_ITEM('')
);
#421=(
BOUNDED_CURVE()
B_SPLINE_CURVE(5,(#61097,#61098,#61099,#61100,#61101,#61102,#61103,#61104,
#61105,#61106,#61107,#61108,#61109,#61110,#61111,#61112,#61113,#61114,#61115,
#61116,#61117,#61118,#61119,#61120,#61121,#61122,#61123,#61124,#61125,#61126,
#61127,#61128,#61129,#61130,#61131,#61132,#61133,#61134,#61135,#61136,#61137,
#61138,#61139,#61140,#61141,#61142,#61143,#61144,#61145,#61146,#61147,#61148,
#61149,#61150,#61151,#61152,#61153,#61154,#61155,#61156,#61157,#61158,#61159,
#61160,#61161,#61162,#61163,#61164,#61165,#61166,#61167,#61168,#61169,#61170,
#61171,#61172,#61173,#61174,#61175,#61176,#61177,#61178,#61179,#61180,#61181,
#61182,#61183,#61184,#61185,#61186,#61187,#61188,#61189,#61190,#61191,#61192,
#61193,#61194,#61195,#61196,#61197,#61198,#61199,#61200,#61201,#61202,#61203,
#61204,#61205,#61206,#61207,#61208,#61209,#61210,#61211,#61212,#61213,#61214,
#61215,#61216,#61217,#61218,#61219,#61220,#61221,#61222,#61223,#61224,#61225,
#61226,#61227,#61228,#61229,#61230,#61231,#61232,#61233,#61234,#61235,#61236,
#61237,#61238,#61239,#61240,#61241,#61242,#61243,#61244,#61245,#61246,#61247,
#61248,#61249,#61250,#61251,#61252,#61253,#61254,#61255,#61256,#61257,#61258,
#61259,#61260,#61261,#61262,#61263,#61264,#61265,#61266,#61267,#61268,#61269,
#61270,#61271,#61272,#61273,#61274,#61275,#61276,#61277,#61278,#61279,#61280,
#61281,#61282,#61283,#61284,#61285,#61286,#61287,#61288,#61289,#61290),
 .UNSPECIFIED.,.F.,.F.)
B_SPLINE_CURVE_WITH_KNOTS((6,1,1,1,1,1,1,1,1,1,1,1,1,1,1,1,1,1,1,1,1,1,
1,1,1,1,1,1,1,1,1,1,1,1,1,1,1,1,1,1,1,1,1,1,1,1,1,1,1,1,1,1,1,1,1,1,1,1,
1,1,1,1,1,1,1,1,1,1,1,1,1,1,1,1,1,1,1,1,1,1,1,1,1,1,1,1,1,1,1,1,1,1,1,1,
1,1,1,1,1,1,1,1,1,1,1,1,1,1,1,1,1,1,1,1,1,1,1,1,1,1,1,1,1,1,1,1,1,1,1,1,
1,1,1,1,1,1,1,1,1,1,1,1,1,1,1,1,1,1,1,1,1,1,1,1,1,1,1,1,1,1,1,1,1,1,1,1,
1,1,1,1,1,1,1,1,1,1,1,1,1,1,1,1,1,1,1,1,1,1,1,6),(0.,0.005,0.01,0.015,0.02,
0.025,0.03,0.035,0.04,0.045,0.05,0.055,0.06,0.065,0.07,0.075,0.08,0.085,
0.09,0.095,0.1,0.105,0.11,0.115,0.12,0.125,0.13,0.135,0.14,0.145,0.15,0.155,
0.16,0.165,0.17,0.175,0.18,0.185,0.19,0.195,0.2,0.205,0.21,0.215,0.22,0.225,
0.23,0.235,0.24,0.245,0.25,0.255,0.26,0.265,0.27,0.275,0.28,0.285,0.29,
0.295,0.3,0.305,0.31,0.315,0.32,0.325,0.33,0.335,0.34,0.345,0.35,0.355,
0.36,0.365,0.37,0.375,0.38,0.385,0.39,0.395,0.4,0.405,0.41,0.415,0.42,0.425,
0.43,0.435,0.44,0.445,0.45,0.455,0.46,0.465,0.47,0.475,0.48,0.485,0.49,
0.495,0.5,0.505,0.51,0.515,0.52,0.525,0.53,0.535,0.54,0.545,0.55,0.555,
0.56,0.565,0.57,0.575,0.58,0.585,0.59,0.595,0.6,0.605,0.61,0.615,0.62,0.625,
0.63,0.635,0.64,0.645,0.65,0.655,0.66,0.665,0.67,0.675,0.68,0.685,0.690000000000001,
0.695000000000001,0.700000000000001,0.705000000000001,0.710000000000001,
0.715000000000001,0.720000000000001,0.725000000000001,0.730000000000001,
0.735000000000001,0.740000000000001,0.745000000000001,0.750000000000001,
0.755000000000001,0.760000000000001,0.765000000000001,0.770000000000001,
0.775000000000001,0.780000000000001,0.785000000000001,0.790000000000001,
0.795000000000001,0.800000000000001,0.805000000000001,0.810000000000001,
0.815000000000001,0.820000000000001,0.825000000000001,0.830000000000001,
0.835000000000001,0.840000000000001,0.845000000000001,0.850000000000001,
0.855000000000001,0.860000000000001,0.865000000000001,0.870000000000001,
0.875000000000001,0.880000000000001,0.885000000000001,0.890000000000001,
0.895000000000001,0.900000000000001,0.905000000000001,0.910000000000001,
0.915000000000001,0.920000000000001,0.925000000000001,0.930000000000001,
0.935000000000001,0.940000000000001,0.941429844431463),.UNSPECIFIED.)
CURVE()
GEOMETRIC_REPRESENTATION_ITEM()
RATIONAL_B_SPLINE_CURVE((1.,1.,1.,1.,1.,1.,1.,1.,1.,1.,1.,1.,1.,1.,1.,1.,
1.,1.,1.,1.,1.,1.,1.,1.,1.,1.,1.,1.,1.,1.,1.,1.,1.,1.,1.,1.,1.,1.,1.,1.,
1.,1.,1.,1.,1.,1.,1.,1.,1.,1.,1.,1.,1.,1.,1.,1.,1.,1.,1.,1.,1.,1.,1.,1.,
1.,1.,1.,1.,1.,1.,1.,1.,1.,1.,1.,1.,1.,1.,1.,1.,1.,1.,1.,1.,1.,1.,1.,1.,
1.,1.,1.,1.,1.,1.,1.,1.,1.,1.,1.,1.,1.,1.,1.,1.,1.,1.,1.,1.,1.,1.,1.,1.,
1.,1.,1.,1.,1.,1.,1.,1.,1.,1.,1.,1.,1.,1.,1.,1.,1.,1.,1.,1.,1.,1.,1.,1.,
1.,1.,1.,1.,1.,1.,1.,1.,1.,1.,1.,1.,1.,1.,1.,1.,1.,1.,1.,1.,1.,1.,1.,1.,
1.,1.,1.,1.,1.,1.,1.,1.,1.,1.,1.,1.,1.,1.,1.,1.,1.,1.,1.,1.,1.,1.,1.,1.,
1.,1.,1.,1.,1.,1.,1.,1.,1.,1.))
REPRESENTATION_ITEM('')
);
#422=(
BOUNDED_CURVE()
B_SPLINE_CURVE(5,(#61293,#61294,#61295,#61296,#61297,#61298,#61299,#61300,
#61301,#61302,#61303,#61304,#61305,#61306,#61307,#61308,#61309,#61310,#61311,
#61312,#61313,#61314,#61315,#61316,#61317,#61318,#61319,#61320,#61321,#61322,
#61323,#61324,#61325,#61326,#61327,#61328,#61329,#61330,#61331,#61332,#61333,
#61334,#61335,#61336,#61337,#61338,#61339,#61340,#61341,#61342,#61343,#61344,
#61345,#61346,#61347,#61348,#61349,#61350,#61351,#61352,#61353,#61354,#61355,
#61356,#61357,#61358,#61359,#61360,#61361,#61362,#61363,#61364,#61365,#61366,
#61367,#61368,#61369,#61370,#61371,#61372,#61373,#61374,#61375,#61376,#61377,
#61378,#61379,#61380,#61381,#61382,#61383,#61384,#61385,#61386,#61387,#61388,
#61389,#61390,#61391,#61392,#61393,#61394,#61395,#61396,#61397,#61398,#61399,
#61400,#61401,#61402,#61403,#61404,#61405,#61406,#61407,#61408,#61409,#61410,
#61411,#61412,#61413,#61414,#61415,#61416,#61417,#61418,#61419,#61420,#61421,
#61422,#61423,#61424,#61425,#61426,#61427,#61428,#61429,#61430,#61431,#61432,
#61433,#61434,#61435,#61436,#61437,#61438,#61439,#61440,#61441,#61442,#61443,
#61444,#61445,#61446,#61447,#61448,#61449,#61450,#61451,#61452,#61453,#61454,
#61455,#61456,#61457,#61458,#61459,#61460,#61461,#61462,#61463,#61464,#61465,
#61466,#61467,#61468,#61469,#61470,#61471,#61472,#61473,#61474,#61475,#61476,
#61477,#61478,#61479,#61480,#61481,#61482,#61483,#61484,#61485,#61486),
 .UNSPECIFIED.,.F.,.F.)
B_SPLINE_CURVE_WITH_KNOTS((6,1,1,1,1,1,1,1,1,1,1,1,1,1,1,1,1,1,1,1,1,1,
1,1,1,1,1,1,1,1,1,1,1,1,1,1,1,1,1,1,1,1,1,1,1,1,1,1,1,1,1,1,1,1,1,1,1,1,
1,1,1,1,1,1,1,1,1,1,1,1,1,1,1,1,1,1,1,1,1,1,1,1,1,1,1,1,1,1,1,1,1,1,1,1,
1,1,1,1,1,1,1,1,1,1,1,1,1,1,1,1,1,1,1,1,1,1,1,1,1,1,1,1,1,1,1,1,1,1,1,1,
1,1,1,1,1,1,1,1,1,1,1,1,1,1,1,1,1,1,1,1,1,1,1,1,1,1,1,1,1,1,1,1,1,1,1,1,
1,1,1,1,1,1,1,1,1,1,1,1,1,1,1,1,1,1,1,1,1,1,1,6),(-0.941429844431463,-0.940000000000001,
-0.935000000000001,-0.930000000000001,-0.925000000000001,-0.920000000000001,
-0.915000000000001,-0.910000000000001,-0.905000000000001,-0.900000000000001,
-0.895000000000001,-0.890000000000001,-0.885000000000001,-0.880000000000001,
-0.875000000000001,-0.870000000000001,-0.865000000000001,-0.860000000000001,
-0.855000000000001,-0.850000000000001,-0.845000000000001,-0.840000000000001,
-0.835000000000001,-0.830000000000001,-0.825000000000001,-0.820000000000001,
-0.815000000000001,-0.810000000000001,-0.805000000000001,-0.800000000000001,
-0.795000000000001,-0.790000000000001,-0.785000000000001,-0.780000000000001,
-0.775000000000001,-0.770000000000001,-0.765000000000001,-0.760000000000001,
-0.755000000000001,-0.750000000000001,-0.745000000000001,-0.740000000000001,
-0.735000000000001,-0.730000000000001,-0.725000000000001,-0.720000000000001,
-0.715000000000001,-0.710000000000001,-0.705000000000001,-0.700000000000001,
-0.695000000000001,-0.690000000000001,-0.685,-0.68,-0.675,-0.67,-0.665,
-0.66,-0.655,-0.65,-0.645,-0.64,-0.635,-0.63,-0.625,-0.62,-0.615,-0.61,
-0.605,-0.6,-0.595,-0.59,-0.585,-0.58,-0.575,-0.57,-0.565,-0.56,-0.555,
-0.55,-0.545,-0.54,-0.535,-0.53,-0.525,-0.52,-0.515,-0.51,-0.505,-0.5,-0.495,
-0.49,-0.485,-0.48,-0.475,-0.47,-0.465,-0.46,-0.455,-0.45,-0.445,-0.44,
-0.435,-0.43,-0.425,-0.42,-0.415,-0.41,-0.405,-0.4,-0.395,-0.39,-0.385,
-0.38,-0.375,-0.37,-0.365,-0.36,-0.355,-0.35,-0.345,-0.34,-0.335,-0.33,
-0.325,-0.32,-0.315,-0.31,-0.305,-0.3,-0.295,-0.29,-0.285,-0.28,-0.275,
-0.27,-0.265,-0.26,-0.255,-0.25,-0.245,-0.24,-0.235,-0.23,-0.225,-0.22,
-0.215,-0.21,-0.205,-0.2,-0.195,-0.19,-0.185,-0.18,-0.175,-0.17,-0.165,
-0.16,-0.155,-0.15,-0.145,-0.14,-0.135,-0.13,-0.125,-0.12,-0.115,-0.11,
-0.105,-0.1,-0.095,-0.09,-0.085,-0.08,-0.075,-0.07,-0.065,-0.06,-0.055,
-0.05,-0.045,-0.04,-0.035,-0.03,-0.025,-0.02,-0.015,-0.01,-0.005,0.),
 .UNSPECIFIED.)
CURVE()
GEOMETRIC_REPRESENTATION_ITEM()
RATIONAL_B_SPLINE_CURVE((1.,1.,1.,1.,1.,1.,1.,1.,1.,1.,1.,1.,1.,1.,1.,1.,
1.,1.,1.,1.,1.,1.,1.,1.,1.,1.,1.,1.,1.,1.,1.,1.,1.,1.,1.,1.,1.,1.,1.,1.,
1.,1.,1.,1.,1.,1.,1.,1.,1.,1.,1.,1.,1.,1.,1.,1.,1.,1.,1.,1.,1.,1.,1.,1.,
1.,1.,1.,1.,1.,1.,1.,1.,1.,1.,1.,1.,1.,1.,1.,1.,1.,1.,1.,1.,1.,1.,1.,1.,
1.,1.,1.,1.,1.,1.,1.,1.,1.,1.,1.,1.,1.,1.,1.,1.,1.,1.,1.,1.,1.,1.,1.,1.,
1.,1.,1.,1.,1.,1.,1.,1.,1.,1.,1.,1.,1.,1.,1.,1.,1.,1.,1.,1.,1.,1.,1.,1.,
1.,1.,1.,1.,1.,1.,1.,1.,1.,1.,1.,1.,1.,1.,1.,1.,1.,1.,1.,1.,1.,1.,1.,1.,
1.,1.,1.,1.,1.,1.,1.,1.,1.,1.,1.,1.,1.,1.,1.,1.,1.,1.,1.,1.,1.,1.,1.,1.,
1.,1.,1.,1.,1.,1.,1.,1.,1.,1.))
REPRESENTATION_ITEM('')
);
#423=(
BOUNDED_CURVE()
B_SPLINE_CURVE(5,(#61993,#61994,#61995,#61996,#61997,#61998,#61999,#62000,
#62001,#62002,#62003,#62004,#62005,#62006,#62007,#62008,#62009,#62010,#62011,
#62012,#62013,#62014,#62015,#62016,#62017,#62018,#62019,#62020,#62021,#62022,
#62023,#62024,#62025,#62026,#62027,#62028,#62029,#62030,#62031,#62032,#62033,
#62034,#62035,#62036,#62037,#62038,#62039,#62040,#62041,#62042,#62043,#62044,
#62045,#62046,#62047,#62048,#62049,#62050,#62051,#62052,#62053,#62054,#62055,
#62056,#62057,#62058,#62059,#62060,#62061,#62062,#62063,#62064,#62065,#62066,
#62067,#62068,#62069,#62070,#62071,#62072,#62073,#62074,#62075,#62076,#62077,
#62078,#62079,#62080,#62081,#62082,#62083,#62084,#62085,#62086,#62087,#62088,
#62089,#62090,#62091,#62092,#62093,#62094,#62095,#62096,#62097,#62098,#62099,
#62100,#62101,#62102,#62103,#62104,#62105,#62106,#62107,#62108,#62109,#62110,
#62111,#62112,#62113,#62114,#62115,#62116,#62117,#62118,#62119,#62120,#62121,
#62122,#62123,#62124,#62125,#62126,#62127,#62128,#62129,#62130,#62131,#62132,
#62133,#62134,#62135,#62136,#62137,#62138,#62139,#62140,#62141,#62142,#62143,
#62144,#62145,#62146,#62147,#62148,#62149,#62150,#62151,#62152,#62153,#62154,
#62155,#62156,#62157,#62158,#62159,#62160,#62161,#62162,#62163,#62164,#62165,
#62166,#62167,#62168,#62169,#62170,#62171,#62172,#62173,#62174,#62175,#62176,
#62177,#62178,#62179,#62180,#62181,#62182,#62183,#62184,#62185,#62186),
 .UNSPECIFIED.,.F.,.F.)
B_SPLINE_CURVE_WITH_KNOTS((6,1,1,1,1,1,1,1,1,1,1,1,1,1,1,1,1,1,1,1,1,1,
1,1,1,1,1,1,1,1,1,1,1,1,1,1,1,1,1,1,1,1,1,1,1,1,1,1,1,1,1,1,1,1,1,1,1,1,
1,1,1,1,1,1,1,1,1,1,1,1,1,1,1,1,1,1,1,1,1,1,1,1,1,1,1,1,1,1,1,1,1,1,1,1,
1,1,1,1,1,1,1,1,1,1,1,1,1,1,1,1,1,1,1,1,1,1,1,1,1,1,1,1,1,1,1,1,1,1,1,1,
1,1,1,1,1,1,1,1,1,1,1,1,1,1,1,1,1,1,1,1,1,1,1,1,1,1,1,1,1,1,1,1,1,1,1,1,
1,1,1,1,1,1,1,1,1,1,1,1,1,1,1,1,1,1,1,1,1,1,1,6),(0.,0.005,0.01,0.015,0.02,
0.025,0.03,0.035,0.04,0.045,0.05,0.055,0.06,0.065,0.07,0.075,0.08,0.085,
0.09,0.095,0.1,0.105,0.11,0.115,0.12,0.125,0.13,0.135,0.14,0.145,0.15,0.155,
0.16,0.165,0.17,0.175,0.18,0.185,0.19,0.195,0.2,0.205,0.21,0.215,0.22,0.225,
0.23,0.235,0.24,0.245,0.25,0.255,0.26,0.265,0.27,0.275,0.28,0.285,0.29,
0.295,0.3,0.305,0.31,0.315,0.32,0.325,0.33,0.335,0.34,0.345,0.35,0.355,
0.36,0.365,0.37,0.375,0.38,0.385,0.39,0.395,0.4,0.405,0.41,0.415,0.42,0.425,
0.43,0.435,0.44,0.445,0.45,0.455,0.46,0.465,0.47,0.475,0.48,0.485,0.49,
0.495,0.5,0.505,0.51,0.515,0.52,0.525,0.53,0.535,0.54,0.545,0.55,0.555,
0.56,0.565,0.57,0.575,0.58,0.585,0.59,0.595,0.6,0.605,0.61,0.615,0.62,0.625,
0.63,0.635,0.64,0.645,0.65,0.655,0.66,0.665,0.67,0.675,0.68,0.685,0.690000000000001,
0.695000000000001,0.700000000000001,0.705000000000001,0.710000000000001,
0.715000000000001,0.720000000000001,0.725000000000001,0.730000000000001,
0.735000000000001,0.740000000000001,0.745000000000001,0.750000000000001,
0.755000000000001,0.760000000000001,0.765000000000001,0.770000000000001,
0.775000000000001,0.780000000000001,0.785000000000001,0.790000000000001,
0.795000000000001,0.800000000000001,0.805000000000001,0.810000000000001,
0.815000000000001,0.820000000000001,0.825000000000001,0.830000000000001,
0.835000000000001,0.840000000000001,0.845000000000001,0.850000000000001,
0.855000000000001,0.860000000000001,0.865000000000001,0.870000000000001,
0.875000000000001,0.880000000000001,0.885000000000001,0.890000000000001,
0.895000000000001,0.900000000000001,0.905000000000001,0.910000000000001,
0.915000000000001,0.920000000000001,0.925000000000001,0.930000000000001,
0.935000000000001,0.940000000000001,0.941429844431297),.UNSPECIFIED.)
CURVE()
GEOMETRIC_REPRESENTATION_ITEM()
RATIONAL_B_SPLINE_CURVE((1.,1.,1.,1.,1.,1.,1.,1.,1.,1.,1.,1.,1.,1.,1.,1.,
1.,1.,1.,1.,1.,1.,1.,1.,1.,1.,1.,1.,1.,1.,1.,1.,1.,1.,1.,1.,1.,1.,1.,1.,
1.,1.,1.,1.,1.,1.,1.,1.,1.,1.,1.,1.,1.,1.,1.,1.,1.,1.,1.,1.,1.,1.,1.,1.,
1.,1.,1.,1.,1.,1.,1.,1.,1.,1.,1.,1.,1.,1.,1.,1.,1.,1.,1.,1.,1.,1.,1.,1.,
1.,1.,1.,1.,1.,1.,1.,1.,1.,1.,1.,1.,1.,1.,1.,1.,1.,1.,1.,1.,1.,1.,1.,1.,
1.,1.,1.,1.,1.,1.,1.,1.,1.,1.,1.,1.,1.,1.,1.,1.,1.,1.,1.,1.,1.,1.,1.,1.,
1.,1.,1.,1.,1.,1.,1.,1.,1.,1.,1.,1.,1.,1.,1.,1.,1.,1.,1.,1.,1.,1.,1.,1.,
1.,1.,1.,1.,1.,1.,1.,1.,1.,1.,1.,1.,1.,1.,1.,1.,1.,1.,1.,1.,1.,1.,1.,1.,
1.,1.,1.,1.,1.,1.,1.,1.,1.,1.))
REPRESENTATION_ITEM('')
);
#424=(
BOUNDED_CURVE()
B_SPLINE_CURVE(5,(#62189,#62190,#62191,#62192,#62193,#62194,#62195,#62196,
#62197,#62198,#62199,#62200,#62201,#62202,#62203,#62204,#62205,#62206,#62207,
#62208,#62209,#62210,#62211,#62212,#62213,#62214,#62215,#62216,#62217,#62218,
#62219,#62220,#62221,#62222,#62223,#62224,#62225,#62226,#62227,#62228,#62229,
#62230,#62231,#62232,#62233,#62234,#62235,#62236,#62237,#62238,#62239,#62240,
#62241,#62242,#62243,#62244,#62245,#62246,#62247,#62248,#62249,#62250,#62251,
#62252,#62253,#62254,#62255,#62256,#62257,#62258,#62259,#62260,#62261,#62262,
#62263,#62264,#62265,#62266,#62267,#62268,#62269,#62270,#62271,#62272,#62273,
#62274,#62275,#62276,#62277,#62278,#62279,#62280,#62281,#62282,#62283,#62284,
#62285,#62286,#62287,#62288,#62289,#62290,#62291,#62292,#62293,#62294,#62295,
#62296,#62297,#62298,#62299,#62300,#62301,#62302,#62303,#62304,#62305,#62306,
#62307,#62308,#62309,#62310,#62311,#62312,#62313,#62314,#62315,#62316,#62317,
#62318,#62319,#62320,#62321,#62322,#62323,#62324,#62325,#62326,#62327,#62328,
#62329,#62330,#62331,#62332,#62333,#62334,#62335,#62336,#62337,#62338,#62339,
#62340,#62341,#62342,#62343,#62344,#62345,#62346,#62347,#62348,#62349,#62350,
#62351,#62352,#62353,#62354,#62355,#62356,#62357,#62358,#62359,#62360,#62361,
#62362,#62363,#62364,#62365,#62366,#62367,#62368,#62369,#62370,#62371,#62372,
#62373,#62374,#62375,#62376,#62377,#62378,#62379,#62380,#62381,#62382),
 .UNSPECIFIED.,.F.,.F.)
B_SPLINE_CURVE_WITH_KNOTS((6,1,1,1,1,1,1,1,1,1,1,1,1,1,1,1,1,1,1,1,1,1,
1,1,1,1,1,1,1,1,1,1,1,1,1,1,1,1,1,1,1,1,1,1,1,1,1,1,1,1,1,1,1,1,1,1,1,1,
1,1,1,1,1,1,1,1,1,1,1,1,1,1,1,1,1,1,1,1,1,1,1,1,1,1,1,1,1,1,1,1,1,1,1,1,
1,1,1,1,1,1,1,1,1,1,1,1,1,1,1,1,1,1,1,1,1,1,1,1,1,1,1,1,1,1,1,1,1,1,1,1,
1,1,1,1,1,1,1,1,1,1,1,1,1,1,1,1,1,1,1,1,1,1,1,1,1,1,1,1,1,1,1,1,1,1,1,1,
1,1,1,1,1,1,1,1,1,1,1,1,1,1,1,1,1,1,1,1,1,1,1,6),(-0.941429844431289,-0.940000000000001,
-0.935000000000001,-0.930000000000001,-0.925000000000001,-0.920000000000001,
-0.915000000000001,-0.910000000000001,-0.905000000000001,-0.900000000000001,
-0.895000000000001,-0.890000000000001,-0.885000000000001,-0.880000000000001,
-0.875000000000001,-0.870000000000001,-0.865000000000001,-0.860000000000001,
-0.855000000000001,-0.850000000000001,-0.845000000000001,-0.840000000000001,
-0.835000000000001,-0.830000000000001,-0.825000000000001,-0.820000000000001,
-0.815000000000001,-0.810000000000001,-0.805000000000001,-0.800000000000001,
-0.795000000000001,-0.790000000000001,-0.785000000000001,-0.780000000000001,
-0.775000000000001,-0.770000000000001,-0.765000000000001,-0.760000000000001,
-0.755000000000001,-0.750000000000001,-0.745000000000001,-0.740000000000001,
-0.735000000000001,-0.730000000000001,-0.725000000000001,-0.720000000000001,
-0.715000000000001,-0.710000000000001,-0.705000000000001,-0.700000000000001,
-0.695000000000001,-0.690000000000001,-0.685,-0.68,-0.675,-0.67,-0.665,
-0.66,-0.655,-0.65,-0.645,-0.64,-0.635,-0.63,-0.625,-0.62,-0.615,-0.61,
-0.605,-0.6,-0.595,-0.59,-0.585,-0.58,-0.575,-0.57,-0.565,-0.56,-0.555,
-0.55,-0.545,-0.54,-0.535,-0.53,-0.525,-0.52,-0.515,-0.51,-0.505,-0.5,-0.495,
-0.49,-0.485,-0.48,-0.475,-0.47,-0.465,-0.46,-0.455,-0.45,-0.445,-0.44,
-0.435,-0.43,-0.425,-0.42,-0.415,-0.41,-0.405,-0.4,-0.395,-0.39,-0.385,
-0.38,-0.375,-0.37,-0.365,-0.36,-0.355,-0.35,-0.345,-0.34,-0.335,-0.33,
-0.325,-0.32,-0.315,-0.31,-0.305,-0.3,-0.295,-0.29,-0.285,-0.28,-0.275,
-0.27,-0.265,-0.26,-0.255,-0.25,-0.245,-0.24,-0.235,-0.23,-0.225,-0.22,
-0.215,-0.21,-0.205,-0.2,-0.195,-0.19,-0.185,-0.18,-0.175,-0.17,-0.165,
-0.16,-0.155,-0.15,-0.145,-0.14,-0.135,-0.13,-0.125,-0.12,-0.115,-0.11,
-0.105,-0.1,-0.095,-0.09,-0.085,-0.08,-0.075,-0.07,-0.065,-0.06,-0.055,
-0.05,-0.045,-0.04,-0.035,-0.03,-0.025,-0.02,-0.015,-0.01,-0.005,0.),
 .UNSPECIFIED.)
CURVE()
GEOMETRIC_REPRESENTATION_ITEM()
RATIONAL_B_SPLINE_CURVE((1.,1.,1.,1.,1.,1.,1.,1.,1.,1.,1.,1.,1.,1.,1.,1.,
1.,1.,1.,1.,1.,1.,1.,1.,1.,1.,1.,1.,1.,1.,1.,1.,1.,1.,1.,1.,1.,1.,1.,1.,
1.,1.,1.,1.,1.,1.,1.,1.,1.,1.,1.,1.,1.,1.,1.,1.,1.,1.,1.,1.,1.,1.,1.,1.,
1.,1.,1.,1.,1.,1.,1.,1.,1.,1.,1.,1.,1.,1.,1.,1.,1.,1.,1.,1.,1.,1.,1.,1.,
1.,1.,1.,1.,1.,1.,1.,1.,1.,1.,1.,1.,1.,1.,1.,1.,1.,1.,1.,1.,1.,1.,1.,1.,
1.,1.,1.,1.,1.,1.,1.,1.,1.,1.,1.,1.,1.,1.,1.,1.,1.,1.,1.,1.,1.,1.,1.,1.,
1.,1.,1.,1.,1.,1.,1.,1.,1.,1.,1.,1.,1.,1.,1.,1.,1.,1.,1.,1.,1.,1.,1.,1.,
1.,1.,1.,1.,1.,1.,1.,1.,1.,1.,1.,1.,1.,1.,1.,1.,1.,1.,1.,1.,1.,1.,1.,1.,
1.,1.,1.,1.,1.,1.,1.,1.,1.,1.))
REPRESENTATION_ITEM('')
);
#425=(
BOUNDED_CURVE()
B_SPLINE_CURVE(5,(#62889,#62890,#62891,#62892,#62893,#62894,#62895,#62896,
#62897,#62898,#62899,#62900,#62901,#62902,#62903,#62904,#62905,#62906,#62907,
#62908,#62909,#62910,#62911,#62912,#62913,#62914,#62915,#62916,#62917,#62918,
#62919,#62920,#62921,#62922,#62923,#62924,#62925,#62926,#62927,#62928,#62929,
#62930,#62931,#62932,#62933,#62934,#62935,#62936,#62937,#62938,#62939,#62940,
#62941,#62942,#62943,#62944,#62945,#62946,#62947,#62948,#62949,#62950,#62951,
#62952,#62953,#62954,#62955,#62956,#62957,#62958,#62959,#62960,#62961,#62962,
#62963,#62964,#62965,#62966,#62967,#62968,#62969,#62970,#62971,#62972,#62973,
#62974,#62975,#62976,#62977,#62978,#62979,#62980,#62981,#62982,#62983,#62984,
#62985,#62986,#62987,#62988,#62989,#62990,#62991,#62992,#62993,#62994,#62995,
#62996,#62997,#62998,#62999,#63000,#63001,#63002,#63003,#63004,#63005,#63006,
#63007,#63008,#63009,#63010,#63011,#63012,#63013,#63014,#63015,#63016,#63017,
#63018,#63019,#63020,#63021,#63022,#63023,#63024,#63025,#63026,#63027,#63028,
#63029,#63030,#63031,#63032,#63033,#63034,#63035,#63036,#63037,#63038,#63039,
#63040,#63041,#63042,#63043,#63044,#63045,#63046,#63047,#63048,#63049,#63050,
#63051,#63052,#63053,#63054,#63055,#63056,#63057,#63058,#63059,#63060,#63061,
#63062,#63063,#63064,#63065,#63066,#63067,#63068,#63069,#63070,#63071,#63072,
#63073,#63074,#63075,#63076,#63077,#63078,#63079,#63080,#63081,#63082),
 .UNSPECIFIED.,.F.,.F.)
B_SPLINE_CURVE_WITH_KNOTS((6,1,1,1,1,1,1,1,1,1,1,1,1,1,1,1,1,1,1,1,1,1,
1,1,1,1,1,1,1,1,1,1,1,1,1,1,1,1,1,1,1,1,1,1,1,1,1,1,1,1,1,1,1,1,1,1,1,1,
1,1,1,1,1,1,1,1,1,1,1,1,1,1,1,1,1,1,1,1,1,1,1,1,1,1,1,1,1,1,1,1,1,1,1,1,
1,1,1,1,1,1,1,1,1,1,1,1,1,1,1,1,1,1,1,1,1,1,1,1,1,1,1,1,1,1,1,1,1,1,1,1,
1,1,1,1,1,1,1,1,1,1,1,1,1,1,1,1,1,1,1,1,1,1,1,1,1,1,1,1,1,1,1,1,1,1,1,1,
1,1,1,1,1,1,1,1,1,1,1,1,1,1,1,1,1,1,1,1,1,1,1,6),(0.,0.005,0.01,0.015,0.02,
0.025,0.03,0.035,0.04,0.045,0.05,0.055,0.06,0.065,0.07,0.075,0.08,0.085,
0.09,0.095,0.1,0.105,0.11,0.115,0.12,0.125,0.13,0.135,0.14,0.145,0.15,0.155,
0.16,0.165,0.17,0.175,0.18,0.185,0.19,0.195,0.2,0.205,0.21,0.215,0.22,0.225,
0.23,0.235,0.24,0.245,0.25,0.255,0.26,0.265,0.27,0.275,0.28,0.285,0.29,
0.295,0.3,0.305,0.31,0.315,0.32,0.325,0.33,0.335,0.34,0.345,0.35,0.355,
0.36,0.365,0.37,0.375,0.38,0.385,0.39,0.395,0.4,0.405,0.41,0.415,0.42,0.425,
0.43,0.435,0.44,0.445,0.45,0.455,0.46,0.465,0.47,0.475,0.48,0.485,0.49,
0.495,0.5,0.505,0.51,0.515,0.52,0.525,0.53,0.535,0.54,0.545,0.55,0.555,
0.56,0.565,0.57,0.575,0.58,0.585,0.59,0.595,0.6,0.605,0.61,0.615,0.62,0.625,
0.63,0.635,0.64,0.645,0.65,0.655,0.66,0.665,0.67,0.675,0.68,0.685,0.690000000000001,
0.695000000000001,0.700000000000001,0.705000000000001,0.710000000000001,
0.715000000000001,0.720000000000001,0.725000000000001,0.730000000000001,
0.735000000000001,0.740000000000001,0.745000000000001,0.750000000000001,
0.755000000000001,0.760000000000001,0.765000000000001,0.770000000000001,
0.775000000000001,0.780000000000001,0.785000000000001,0.790000000000001,
0.795000000000001,0.800000000000001,0.805000000000001,0.810000000000001,
0.815000000000001,0.820000000000001,0.825000000000001,0.830000000000001,
0.835000000000001,0.840000000000001,0.845000000000001,0.850000000000001,
0.855000000000001,0.860000000000001,0.865000000000001,0.870000000000001,
0.875000000000001,0.880000000000001,0.885000000000001,0.890000000000001,
0.895000000000001,0.900000000000001,0.905000000000001,0.910000000000001,
0.915000000000001,0.920000000000001,0.925000000000001,0.930000000000001,
0.935000000000001,0.940000000000001,0.941429844431249),.UNSPECIFIED.)
CURVE()
GEOMETRIC_REPRESENTATION_ITEM()
RATIONAL_B_SPLINE_CURVE((1.,1.,1.,1.,1.,1.,1.,1.,1.,1.,1.,1.,1.,1.,1.,1.,
1.,1.,1.,1.,1.,1.,1.,1.,1.,1.,1.,1.,1.,1.,1.,1.,1.,1.,1.,1.,1.,1.,1.,1.,
1.,1.,1.,1.,1.,1.,1.,1.,1.,1.,1.,1.,1.,1.,1.,1.,1.,1.,1.,1.,1.,1.,1.,1.,
1.,1.,1.,1.,1.,1.,1.,1.,1.,1.,1.,1.,1.,1.,1.,1.,1.,1.,1.,1.,1.,1.,1.,1.,
1.,1.,1.,1.,1.,1.,1.,1.,1.,1.,1.,1.,1.,1.,1.,1.,1.,1.,1.,1.,1.,1.,1.,1.,
1.,1.,1.,1.,1.,1.,1.,1.,1.,1.,1.,1.,1.,1.,1.,1.,1.,1.,1.,1.,1.,1.,1.,1.,
1.,1.,1.,1.,1.,1.,1.,1.,1.,1.,1.,1.,1.,1.,1.,1.,1.,1.,1.,1.,1.,1.,1.,1.,
1.,1.,1.,1.,1.,1.,1.,1.,1.,1.,1.,1.,1.,1.,1.,1.,1.,1.,1.,1.,1.,1.,1.,1.,
1.,1.,1.,1.,1.,1.,1.,1.,1.,1.))
REPRESENTATION_ITEM('')
);
#426=(
BOUNDED_CURVE()
B_SPLINE_CURVE(5,(#63085,#63086,#63087,#63088,#63089,#63090,#63091,#63092,
#63093,#63094,#63095,#63096,#63097,#63098,#63099,#63100,#63101,#63102,#63103,
#63104,#63105,#63106,#63107,#63108,#63109,#63110,#63111,#63112,#63113,#63114,
#63115,#63116,#63117,#63118,#63119,#63120,#63121,#63122,#63123,#63124,#63125,
#63126,#63127,#63128,#63129,#63130,#63131,#63132,#63133,#63134,#63135,#63136,
#63137,#63138,#63139,#63140,#63141,#63142,#63143,#63144,#63145,#63146,#63147,
#63148,#63149,#63150,#63151,#63152,#63153,#63154,#63155,#63156,#63157,#63158,
#63159,#63160,#63161,#63162,#63163,#63164,#63165,#63166,#63167,#63168,#63169,
#63170,#63171,#63172,#63173,#63174,#63175,#63176,#63177,#63178,#63179,#63180,
#63181,#63182,#63183,#63184,#63185,#63186,#63187,#63188,#63189,#63190,#63191,
#63192,#63193,#63194,#63195,#63196,#63197,#63198,#63199,#63200,#63201,#63202,
#63203,#63204,#63205,#63206,#63207,#63208,#63209,#63210,#63211,#63212,#63213,
#63214,#63215,#63216,#63217,#63218,#63219,#63220,#63221,#63222,#63223,#63224,
#63225,#63226,#63227,#63228,#63229,#63230,#63231,#63232,#63233,#63234,#63235,
#63236,#63237,#63238,#63239,#63240,#63241,#63242,#63243,#63244,#63245,#63246,
#63247,#63248,#63249,#63250,#63251,#63252,#63253,#63254,#63255,#63256,#63257,
#63258,#63259,#63260,#63261,#63262,#63263,#63264,#63265,#63266,#63267,#63268,
#63269,#63270,#63271,#63272,#63273,#63274,#63275,#63276,#63277,#63278),
 .UNSPECIFIED.,.F.,.F.)
B_SPLINE_CURVE_WITH_KNOTS((6,1,1,1,1,1,1,1,1,1,1,1,1,1,1,1,1,1,1,1,1,1,
1,1,1,1,1,1,1,1,1,1,1,1,1,1,1,1,1,1,1,1,1,1,1,1,1,1,1,1,1,1,1,1,1,1,1,1,
1,1,1,1,1,1,1,1,1,1,1,1,1,1,1,1,1,1,1,1,1,1,1,1,1,1,1,1,1,1,1,1,1,1,1,1,
1,1,1,1,1,1,1,1,1,1,1,1,1,1,1,1,1,1,1,1,1,1,1,1,1,1,1,1,1,1,1,1,1,1,1,1,
1,1,1,1,1,1,1,1,1,1,1,1,1,1,1,1,1,1,1,1,1,1,1,1,1,1,1,1,1,1,1,1,1,1,1,1,
1,1,1,1,1,1,1,1,1,1,1,1,1,1,1,1,1,1,1,1,1,1,1,6),(-0.94142984443124,-0.940000000000001,
-0.935000000000001,-0.930000000000001,-0.925000000000001,-0.920000000000001,
-0.915000000000001,-0.910000000000001,-0.905000000000001,-0.900000000000001,
-0.895000000000001,-0.890000000000001,-0.885000000000001,-0.880000000000001,
-0.875000000000001,-0.870000000000001,-0.865000000000001,-0.860000000000001,
-0.855000000000001,-0.850000000000001,-0.845000000000001,-0.840000000000001,
-0.835000000000001,-0.830000000000001,-0.825000000000001,-0.820000000000001,
-0.815000000000001,-0.810000000000001,-0.805000000000001,-0.800000000000001,
-0.795000000000001,-0.790000000000001,-0.785000000000001,-0.780000000000001,
-0.775000000000001,-0.770000000000001,-0.765000000000001,-0.760000000000001,
-0.755000000000001,-0.750000000000001,-0.745000000000001,-0.740000000000001,
-0.735000000000001,-0.730000000000001,-0.725000000000001,-0.720000000000001,
-0.715000000000001,-0.710000000000001,-0.705000000000001,-0.700000000000001,
-0.695000000000001,-0.690000000000001,-0.685,-0.68,-0.675,-0.67,-0.665,
-0.66,-0.655,-0.65,-0.645,-0.64,-0.635,-0.63,-0.625,-0.62,-0.615,-0.61,
-0.605,-0.6,-0.595,-0.59,-0.585,-0.58,-0.575,-0.57,-0.565,-0.56,-0.555,
-0.55,-0.545,-0.54,-0.535,-0.53,-0.525,-0.52,-0.515,-0.51,-0.505,-0.5,-0.495,
-0.49,-0.485,-0.48,-0.475,-0.47,-0.465,-0.46,-0.455,-0.45,-0.445,-0.44,
-0.435,-0.43,-0.425,-0.42,-0.415,-0.41,-0.405,-0.4,-0.395,-0.39,-0.385,
-0.38,-0.375,-0.37,-0.365,-0.36,-0.355,-0.35,-0.345,-0.34,-0.335,-0.33,
-0.325,-0.32,-0.315,-0.31,-0.305,-0.3,-0.295,-0.29,-0.285,-0.28,-0.275,
-0.27,-0.265,-0.26,-0.255,-0.25,-0.245,-0.24,-0.235,-0.23,-0.225,-0.22,
-0.215,-0.21,-0.205,-0.2,-0.195,-0.19,-0.185,-0.18,-0.175,-0.17,-0.165,
-0.16,-0.155,-0.15,-0.145,-0.14,-0.135,-0.13,-0.125,-0.12,-0.115,-0.11,
-0.105,-0.1,-0.095,-0.09,-0.085,-0.08,-0.075,-0.07,-0.065,-0.06,-0.055,
-0.05,-0.045,-0.04,-0.035,-0.03,-0.025,-0.02,-0.015,-0.01,-0.005,0.),
 .UNSPECIFIED.)
CURVE()
GEOMETRIC_REPRESENTATION_ITEM()
RATIONAL_B_SPLINE_CURVE((1.,1.,1.,1.,1.,1.,1.,1.,1.,1.,1.,1.,1.,1.,1.,1.,
1.,1.,1.,1.,1.,1.,1.,1.,1.,1.,1.,1.,1.,1.,1.,1.,1.,1.,1.,1.,1.,1.,1.,1.,
1.,1.,1.,1.,1.,1.,1.,1.,1.,1.,1.,1.,1.,1.,1.,1.,1.,1.,1.,1.,1.,1.,1.,1.,
1.,1.,1.,1.,1.,1.,1.,1.,1.,1.,1.,1.,1.,1.,1.,1.,1.,1.,1.,1.,1.,1.,1.,1.,
1.,1.,1.,1.,1.,1.,1.,1.,1.,1.,1.,1.,1.,1.,1.,1.,1.,1.,1.,1.,1.,1.,1.,1.,
1.,1.,1.,1.,1.,1.,1.,1.,1.,1.,1.,1.,1.,1.,1.,1.,1.,1.,1.,1.,1.,1.,1.,1.,
1.,1.,1.,1.,1.,1.,1.,1.,1.,1.,1.,1.,1.,1.,1.,1.,1.,1.,1.,1.,1.,1.,1.,1.,
1.,1.,1.,1.,1.,1.,1.,1.,1.,1.,1.,1.,1.,1.,1.,1.,1.,1.,1.,1.,1.,1.,1.,1.,
1.,1.,1.,1.,1.,1.,1.,1.,1.,1.))
REPRESENTATION_ITEM('')
);
#427=(
BOUNDED_CURVE()
B_SPLINE_CURVE(5,(#63785,#63786,#63787,#63788,#63789,#63790,#63791,#63792,
#63793,#63794,#63795,#63796,#63797,#63798,#63799,#63800,#63801,#63802,#63803,
#63804,#63805,#63806,#63807,#63808,#63809,#63810,#63811,#63812,#63813,#63814,
#63815,#63816,#63817,#63818,#63819,#63820,#63821,#63822,#63823,#63824,#63825,
#63826,#63827,#63828,#63829,#63830,#63831,#63832,#63833,#63834,#63835,#63836,
#63837,#63838,#63839,#63840,#63841,#63842,#63843,#63844,#63845,#63846,#63847,
#63848,#63849,#63850,#63851,#63852,#63853,#63854,#63855,#63856,#63857,#63858,
#63859,#63860,#63861,#63862,#63863,#63864,#63865,#63866,#63867,#63868,#63869,
#63870,#63871,#63872,#63873,#63874,#63875,#63876,#63877,#63878,#63879,#63880,
#63881,#63882,#63883,#63884,#63885,#63886,#63887,#63888,#63889,#63890,#63891,
#63892,#63893,#63894,#63895,#63896,#63897,#63898,#63899,#63900,#63901,#63902,
#63903,#63904,#63905,#63906,#63907,#63908,#63909,#63910,#63911,#63912,#63913,
#63914,#63915,#63916,#63917,#63918,#63919,#63920,#63921,#63922,#63923,#63924,
#63925,#63926,#63927,#63928,#63929,#63930,#63931,#63932,#63933,#63934,#63935,
#63936,#63937,#63938,#63939,#63940,#63941,#63942,#63943,#63944,#63945,#63946,
#63947,#63948,#63949,#63950,#63951,#63952,#63953,#63954,#63955,#63956,#63957,
#63958,#63959,#63960,#63961,#63962,#63963,#63964,#63965,#63966,#63967,#63968,
#63969,#63970,#63971,#63972,#63973,#63974,#63975,#63976,#63977,#63978),
 .UNSPECIFIED.,.F.,.F.)
B_SPLINE_CURVE_WITH_KNOTS((6,1,1,1,1,1,1,1,1,1,1,1,1,1,1,1,1,1,1,1,1,1,
1,1,1,1,1,1,1,1,1,1,1,1,1,1,1,1,1,1,1,1,1,1,1,1,1,1,1,1,1,1,1,1,1,1,1,1,
1,1,1,1,1,1,1,1,1,1,1,1,1,1,1,1,1,1,1,1,1,1,1,1,1,1,1,1,1,1,1,1,1,1,1,1,
1,1,1,1,1,1,1,1,1,1,1,1,1,1,1,1,1,1,1,1,1,1,1,1,1,1,1,1,1,1,1,1,1,1,1,1,
1,1,1,1,1,1,1,1,1,1,1,1,1,1,1,1,1,1,1,1,1,1,1,1,1,1,1,1,1,1,1,1,1,1,1,1,
1,1,1,1,1,1,1,1,1,1,1,1,1,1,1,1,1,1,1,1,1,1,1,6),(0.,0.005,0.01,0.015,0.02,
0.025,0.03,0.035,0.04,0.045,0.05,0.055,0.06,0.065,0.07,0.075,0.08,0.085,
0.09,0.095,0.1,0.105,0.11,0.115,0.12,0.125,0.13,0.135,0.14,0.145,0.15,0.155,
0.16,0.165,0.17,0.175,0.18,0.185,0.19,0.195,0.2,0.205,0.21,0.215,0.22,0.225,
0.23,0.235,0.24,0.245,0.25,0.255,0.26,0.265,0.27,0.275,0.28,0.285,0.29,
0.295,0.3,0.305,0.31,0.315,0.32,0.325,0.33,0.335,0.34,0.345,0.35,0.355,
0.36,0.365,0.37,0.375,0.38,0.385,0.39,0.395,0.4,0.405,0.41,0.415,0.42,0.425,
0.43,0.435,0.44,0.445,0.45,0.455,0.46,0.465,0.47,0.475,0.48,0.485,0.49,
0.495,0.5,0.505,0.51,0.515,0.52,0.525,0.53,0.535,0.54,0.545,0.55,0.555,
0.56,0.565,0.57,0.575,0.58,0.585,0.59,0.595,0.6,0.605,0.61,0.615,0.62,0.625,
0.63,0.635,0.64,0.645,0.65,0.655,0.66,0.665,0.67,0.675,0.68,0.685,0.690000000000001,
0.695000000000001,0.700000000000001,0.705000000000001,0.710000000000001,
0.715000000000001,0.720000000000001,0.725000000000001,0.730000000000001,
0.735000000000001,0.740000000000001,0.745000000000001,0.750000000000001,
0.755000000000001,0.760000000000001,0.765000000000001,0.770000000000001,
0.775000000000001,0.780000000000001,0.785000000000001,0.790000000000001,
0.795000000000001,0.800000000000001,0.805000000000001,0.810000000000001,
0.815000000000001,0.820000000000001,0.825000000000001,0.830000000000001,
0.835000000000001,0.840000000000001,0.845000000000001,0.850000000000001,
0.855000000000001,0.860000000000001,0.865000000000001,0.870000000000001,
0.875000000000001,0.880000000000001,0.885000000000001,0.890000000000001,
0.895000000000001,0.900000000000001,0.905000000000001,0.910000000000001,
0.915000000000001,0.920000000000001,0.925000000000001,0.930000000000001,
0.935000000000001,0.940000000000001,0.941429844431314),.UNSPECIFIED.)
CURVE()
GEOMETRIC_REPRESENTATION_ITEM()
RATIONAL_B_SPLINE_CURVE((1.,1.,1.,1.,1.,1.,1.,1.,1.,1.,1.,1.,1.,1.,1.,1.,
1.,1.,1.,1.,1.,1.,1.,1.,1.,1.,1.,1.,1.,1.,1.,1.,1.,1.,1.,1.,1.,1.,1.,1.,
1.,1.,1.,1.,1.,1.,1.,1.,1.,1.,1.,1.,1.,1.,1.,1.,1.,1.,1.,1.,1.,1.,1.,1.,
1.,1.,1.,1.,1.,1.,1.,1.,1.,1.,1.,1.,1.,1.,1.,1.,1.,1.,1.,1.,1.,1.,1.,1.,
1.,1.,1.,1.,1.,1.,1.,1.,1.,1.,1.,1.,1.,1.,1.,1.,1.,1.,1.,1.,1.,1.,1.,1.,
1.,1.,1.,1.,1.,1.,1.,1.,1.,1.,1.,1.,1.,1.,1.,1.,1.,1.,1.,1.,1.,1.,1.,1.,
1.,1.,1.,1.,1.,1.,1.,1.,1.,1.,1.,1.,1.,1.,1.,1.,1.,1.,1.,1.,1.,1.,1.,1.,
1.,1.,1.,1.,1.,1.,1.,1.,1.,1.,1.,1.,1.,1.,1.,1.,1.,1.,1.,1.,1.,1.,1.,1.,
1.,1.,1.,1.,1.,1.,1.,1.,1.,1.))
REPRESENTATION_ITEM('')
);
#428=(
BOUNDED_CURVE()
B_SPLINE_CURVE(5,(#63981,#63982,#63983,#63984,#63985,#63986,#63987,#63988,
#63989,#63990,#63991,#63992,#63993,#63994,#63995,#63996,#63997,#63998,#63999,
#64000,#64001,#64002,#64003,#64004,#64005,#64006,#64007,#64008,#64009,#64010,
#64011,#64012,#64013,#64014,#64015,#64016,#64017,#64018,#64019,#64020,#64021,
#64022,#64023,#64024,#64025,#64026,#64027,#64028,#64029,#64030,#64031,#64032,
#64033,#64034,#64035,#64036,#64037,#64038,#64039,#64040,#64041,#64042,#64043,
#64044,#64045,#64046,#64047,#64048,#64049,#64050,#64051,#64052,#64053,#64054,
#64055,#64056,#64057,#64058,#64059,#64060,#64061,#64062,#64063,#64064,#64065,
#64066,#64067,#64068,#64069,#64070,#64071,#64072,#64073,#64074,#64075,#64076,
#64077,#64078,#64079,#64080,#64081,#64082,#64083,#64084,#64085,#64086,#64087,
#64088,#64089,#64090,#64091,#64092,#64093,#64094,#64095,#64096,#64097,#64098,
#64099,#64100,#64101,#64102,#64103,#64104,#64105,#64106,#64107,#64108,#64109,
#64110,#64111,#64112,#64113,#64114,#64115,#64116,#64117,#64118,#64119,#64120,
#64121,#64122,#64123,#64124,#64125,#64126,#64127,#64128,#64129,#64130,#64131,
#64132,#64133,#64134,#64135,#64136,#64137,#64138,#64139,#64140,#64141,#64142,
#64143,#64144,#64145,#64146,#64147,#64148,#64149,#64150,#64151,#64152,#64153,
#64154,#64155,#64156,#64157,#64158,#64159,#64160,#64161,#64162,#64163,#64164,
#64165,#64166,#64167,#64168,#64169,#64170,#64171,#64172,#64173,#64174),
 .UNSPECIFIED.,.F.,.F.)
B_SPLINE_CURVE_WITH_KNOTS((6,1,1,1,1,1,1,1,1,1,1,1,1,1,1,1,1,1,1,1,1,1,
1,1,1,1,1,1,1,1,1,1,1,1,1,1,1,1,1,1,1,1,1,1,1,1,1,1,1,1,1,1,1,1,1,1,1,1,
1,1,1,1,1,1,1,1,1,1,1,1,1,1,1,1,1,1,1,1,1,1,1,1,1,1,1,1,1,1,1,1,1,1,1,1,
1,1,1,1,1,1,1,1,1,1,1,1,1,1,1,1,1,1,1,1,1,1,1,1,1,1,1,1,1,1,1,1,1,1,1,1,
1,1,1,1,1,1,1,1,1,1,1,1,1,1,1,1,1,1,1,1,1,1,1,1,1,1,1,1,1,1,1,1,1,1,1,1,
1,1,1,1,1,1,1,1,1,1,1,1,1,1,1,1,1,1,1,1,1,1,1,6),(-0.941429844431327,-0.940000000000001,
-0.935000000000001,-0.930000000000001,-0.925000000000001,-0.920000000000001,
-0.915000000000001,-0.910000000000001,-0.905000000000001,-0.900000000000001,
-0.895000000000001,-0.890000000000001,-0.885000000000001,-0.880000000000001,
-0.875000000000001,-0.870000000000001,-0.865000000000001,-0.860000000000001,
-0.855000000000001,-0.850000000000001,-0.845000000000001,-0.840000000000001,
-0.835000000000001,-0.830000000000001,-0.825000000000001,-0.820000000000001,
-0.815000000000001,-0.810000000000001,-0.805000000000001,-0.800000000000001,
-0.795000000000001,-0.790000000000001,-0.785000000000001,-0.780000000000001,
-0.775000000000001,-0.770000000000001,-0.765000000000001,-0.760000000000001,
-0.755000000000001,-0.750000000000001,-0.745000000000001,-0.740000000000001,
-0.735000000000001,-0.730000000000001,-0.725000000000001,-0.720000000000001,
-0.715000000000001,-0.710000000000001,-0.705000000000001,-0.700000000000001,
-0.695000000000001,-0.690000000000001,-0.685,-0.68,-0.675,-0.67,-0.665,
-0.66,-0.655,-0.65,-0.645,-0.64,-0.635,-0.63,-0.625,-0.62,-0.615,-0.61,
-0.605,-0.6,-0.595,-0.59,-0.585,-0.58,-0.575,-0.57,-0.565,-0.56,-0.555,
-0.55,-0.545,-0.54,-0.535,-0.53,-0.525,-0.52,-0.515,-0.51,-0.505,-0.5,-0.495,
-0.49,-0.485,-0.48,-0.475,-0.47,-0.465,-0.46,-0.455,-0.45,-0.445,-0.44,
-0.435,-0.43,-0.425,-0.42,-0.415,-0.41,-0.405,-0.4,-0.395,-0.39,-0.385,
-0.38,-0.375,-0.37,-0.365,-0.36,-0.355,-0.35,-0.345,-0.34,-0.335,-0.33,
-0.325,-0.32,-0.315,-0.31,-0.305,-0.3,-0.295,-0.29,-0.285,-0.28,-0.275,
-0.27,-0.265,-0.26,-0.255,-0.25,-0.245,-0.24,-0.235,-0.23,-0.225,-0.22,
-0.215,-0.21,-0.205,-0.2,-0.195,-0.19,-0.185,-0.18,-0.175,-0.17,-0.165,
-0.16,-0.155,-0.15,-0.145,-0.14,-0.135,-0.13,-0.125,-0.12,-0.115,-0.11,
-0.105,-0.1,-0.095,-0.09,-0.085,-0.08,-0.075,-0.07,-0.065,-0.06,-0.055,
-0.05,-0.045,-0.04,-0.035,-0.03,-0.025,-0.02,-0.015,-0.01,-0.005,0.),
 .UNSPECIFIED.)
CURVE()
GEOMETRIC_REPRESENTATION_ITEM()
RATIONAL_B_SPLINE_CURVE((1.,1.,1.,1.,1.,1.,1.,1.,1.,1.,1.,1.,1.,1.,1.,1.,
1.,1.,1.,1.,1.,1.,1.,1.,1.,1.,1.,1.,1.,1.,1.,1.,1.,1.,1.,1.,1.,1.,1.,1.,
1.,1.,1.,1.,1.,1.,1.,1.,1.,1.,1.,1.,1.,1.,1.,1.,1.,1.,1.,1.,1.,1.,1.,1.,
1.,1.,1.,1.,1.,1.,1.,1.,1.,1.,1.,1.,1.,1.,1.,1.,1.,1.,1.,1.,1.,1.,1.,1.,
1.,1.,1.,1.,1.,1.,1.,1.,1.,1.,1.,1.,1.,1.,1.,1.,1.,1.,1.,1.,1.,1.,1.,1.,
1.,1.,1.,1.,1.,1.,1.,1.,1.,1.,1.,1.,1.,1.,1.,1.,1.,1.,1.,1.,1.,1.,1.,1.,
1.,1.,1.,1.,1.,1.,1.,1.,1.,1.,1.,1.,1.,1.,1.,1.,1.,1.,1.,1.,1.,1.,1.,1.,
1.,1.,1.,1.,1.,1.,1.,1.,1.,1.,1.,1.,1.,1.,1.,1.,1.,1.,1.,1.,1.,1.,1.,1.,
1.,1.,1.,1.,1.,1.,1.,1.,1.,1.))
REPRESENTATION_ITEM('')
);
#429=(
BOUNDED_CURVE()
B_SPLINE_CURVE(5,(#64681,#64682,#64683,#64684,#64685,#64686,#64687,#64688,
#64689,#64690,#64691,#64692,#64693,#64694,#64695,#64696,#64697,#64698,#64699,
#64700,#64701,#64702,#64703,#64704,#64705,#64706,#64707,#64708,#64709,#64710,
#64711,#64712,#64713,#64714,#64715,#64716,#64717,#64718,#64719,#64720,#64721,
#64722,#64723,#64724,#64725,#64726,#64727,#64728,#64729,#64730,#64731,#64732,
#64733,#64734,#64735,#64736,#64737,#64738,#64739,#64740,#64741,#64742,#64743,
#64744,#64745,#64746,#64747,#64748,#64749,#64750,#64751,#64752,#64753,#64754,
#64755,#64756,#64757,#64758,#64759,#64760,#64761,#64762,#64763,#64764,#64765,
#64766,#64767,#64768,#64769,#64770,#64771,#64772,#64773,#64774,#64775,#64776,
#64777,#64778,#64779,#64780,#64781,#64782,#64783,#64784,#64785,#64786,#64787,
#64788,#64789,#64790,#64791,#64792,#64793,#64794,#64795,#64796,#64797,#64798,
#64799,#64800,#64801,#64802,#64803,#64804,#64805,#64806,#64807,#64808,#64809,
#64810,#64811,#64812,#64813,#64814,#64815,#64816,#64817,#64818,#64819,#64820,
#64821,#64822,#64823,#64824,#64825,#64826,#64827,#64828,#64829,#64830,#64831,
#64832,#64833,#64834,#64835,#64836,#64837,#64838,#64839,#64840,#64841,#64842,
#64843,#64844,#64845,#64846,#64847,#64848,#64849,#64850,#64851,#64852,#64853,
#64854,#64855,#64856,#64857,#64858,#64859,#64860,#64861,#64862,#64863,#64864,
#64865,#64866,#64867,#64868,#64869,#64870,#64871,#64872,#64873,#64874),
 .UNSPECIFIED.,.F.,.F.)
B_SPLINE_CURVE_WITH_KNOTS((6,1,1,1,1,1,1,1,1,1,1,1,1,1,1,1,1,1,1,1,1,1,
1,1,1,1,1,1,1,1,1,1,1,1,1,1,1,1,1,1,1,1,1,1,1,1,1,1,1,1,1,1,1,1,1,1,1,1,
1,1,1,1,1,1,1,1,1,1,1,1,1,1,1,1,1,1,1,1,1,1,1,1,1,1,1,1,1,1,1,1,1,1,1,1,
1,1,1,1,1,1,1,1,1,1,1,1,1,1,1,1,1,1,1,1,1,1,1,1,1,1,1,1,1,1,1,1,1,1,1,1,
1,1,1,1,1,1,1,1,1,1,1,1,1,1,1,1,1,1,1,1,1,1,1,1,1,1,1,1,1,1,1,1,1,1,1,1,
1,1,1,1,1,1,1,1,1,1,1,1,1,1,1,1,1,1,1,1,1,1,1,6),(0.,0.005,0.01,0.015,0.02,
0.025,0.03,0.035,0.04,0.045,0.05,0.055,0.06,0.065,0.07,0.075,0.08,0.085,
0.09,0.095,0.1,0.105,0.11,0.115,0.12,0.125,0.13,0.135,0.14,0.145,0.15,0.155,
0.16,0.165,0.17,0.175,0.18,0.185,0.19,0.195,0.2,0.205,0.21,0.215,0.22,0.225,
0.23,0.235,0.24,0.245,0.25,0.255,0.26,0.265,0.27,0.275,0.28,0.285,0.29,
0.295,0.3,0.305,0.31,0.315,0.32,0.325,0.33,0.335,0.34,0.345,0.35,0.355,
0.36,0.365,0.37,0.375,0.38,0.385,0.39,0.395,0.4,0.405,0.41,0.415,0.42,0.425,
0.43,0.435,0.44,0.445,0.45,0.455,0.46,0.465,0.47,0.475,0.48,0.485,0.49,
0.495,0.5,0.505,0.51,0.515,0.52,0.525,0.53,0.535,0.54,0.545,0.55,0.555,
0.56,0.565,0.57,0.575,0.58,0.585,0.59,0.595,0.6,0.605,0.61,0.615,0.62,0.625,
0.63,0.635,0.64,0.645,0.65,0.655,0.66,0.665,0.67,0.675,0.68,0.685,0.690000000000001,
0.695000000000001,0.700000000000001,0.705000000000001,0.710000000000001,
0.715000000000001,0.720000000000001,0.725000000000001,0.730000000000001,
0.735000000000001,0.740000000000001,0.745000000000001,0.750000000000001,
0.755000000000001,0.760000000000001,0.765000000000001,0.770000000000001,
0.775000000000001,0.780000000000001,0.785000000000001,0.790000000000001,
0.795000000000001,0.800000000000001,0.805000000000001,0.810000000000001,
0.815000000000001,0.820000000000001,0.825000000000001,0.830000000000001,
0.835000000000001,0.840000000000001,0.845000000000001,0.850000000000001,
0.855000000000001,0.860000000000001,0.865000000000001,0.870000000000001,
0.875000000000001,0.880000000000001,0.885000000000001,0.890000000000001,
0.895000000000001,0.900000000000001,0.905000000000001,0.910000000000001,
0.915000000000001,0.920000000000001,0.925000000000001,0.930000000000001,
0.935000000000001,0.940000000000001,0.941429844431384),.UNSPECIFIED.)
CURVE()
GEOMETRIC_REPRESENTATION_ITEM()
RATIONAL_B_SPLINE_CURVE((1.,1.,1.,1.,1.,1.,1.,1.,1.,1.,1.,1.,1.,1.,1.,1.,
1.,1.,1.,1.,1.,1.,1.,1.,1.,1.,1.,1.,1.,1.,1.,1.,1.,1.,1.,1.,1.,1.,1.,1.,
1.,1.,1.,1.,1.,1.,1.,1.,1.,1.,1.,1.,1.,1.,1.,1.,1.,1.,1.,1.,1.,1.,1.,1.,
1.,1.,1.,1.,1.,1.,1.,1.,1.,1.,1.,1.,1.,1.,1.,1.,1.,1.,1.,1.,1.,1.,1.,1.,
1.,1.,1.,1.,1.,1.,1.,1.,1.,1.,1.,1.,1.,1.,1.,1.,1.,1.,1.,1.,1.,1.,1.,1.,
1.,1.,1.,1.,1.,1.,1.,1.,1.,1.,1.,1.,1.,1.,1.,1.,1.,1.,1.,1.,1.,1.,1.,1.,
1.,1.,1.,1.,1.,1.,1.,1.,1.,1.,1.,1.,1.,1.,1.,1.,1.,1.,1.,1.,1.,1.,1.,1.,
1.,1.,1.,1.,1.,1.,1.,1.,1.,1.,1.,1.,1.,1.,1.,1.,1.,1.,1.,1.,1.,1.,1.,1.,
1.,1.,1.,1.,1.,1.,1.,1.,1.,1.))
REPRESENTATION_ITEM('')
);
#430=(
BOUNDED_CURVE()
B_SPLINE_CURVE(5,(#64877,#64878,#64879,#64880,#64881,#64882,#64883,#64884,
#64885,#64886,#64887,#64888,#64889,#64890,#64891,#64892,#64893,#64894,#64895,
#64896,#64897,#64898,#64899,#64900,#64901,#64902,#64903,#64904,#64905,#64906,
#64907,#64908,#64909,#64910,#64911,#64912,#64913,#64914,#64915,#64916,#64917,
#64918,#64919,#64920,#64921,#64922,#64923,#64924,#64925,#64926,#64927,#64928,
#64929,#64930,#64931,#64932,#64933,#64934,#64935,#64936,#64937,#64938,#64939,
#64940,#64941,#64942,#64943,#64944,#64945,#64946,#64947,#64948,#64949,#64950,
#64951,#64952,#64953,#64954,#64955,#64956,#64957,#64958,#64959,#64960,#64961,
#64962,#64963,#64964,#64965,#64966,#64967,#64968,#64969,#64970,#64971,#64972,
#64973,#64974,#64975,#64976,#64977,#64978,#64979,#64980,#64981,#64982,#64983,
#64984,#64985,#64986,#64987,#64988,#64989,#64990,#64991,#64992,#64993,#64994,
#64995,#64996,#64997,#64998,#64999,#65000,#65001,#65002,#65003,#65004,#65005,
#65006,#65007,#65008,#65009,#65010,#65011,#65012,#65013,#65014,#65015,#65016,
#65017,#65018,#65019,#65020,#65021,#65022,#65023,#65024,#65025,#65026,#65027,
#65028,#65029,#65030,#65031,#65032,#65033,#65034,#65035,#65036,#65037,#65038,
#65039,#65040,#65041,#65042,#65043,#65044,#65045,#65046,#65047,#65048,#65049,
#65050,#65051,#65052,#65053,#65054,#65055,#65056,#65057,#65058,#65059,#65060,
#65061,#65062,#65063,#65064,#65065,#65066,#65067,#65068,#65069,#65070),
 .UNSPECIFIED.,.F.,.F.)
B_SPLINE_CURVE_WITH_KNOTS((6,1,1,1,1,1,1,1,1,1,1,1,1,1,1,1,1,1,1,1,1,1,
1,1,1,1,1,1,1,1,1,1,1,1,1,1,1,1,1,1,1,1,1,1,1,1,1,1,1,1,1,1,1,1,1,1,1,1,
1,1,1,1,1,1,1,1,1,1,1,1,1,1,1,1,1,1,1,1,1,1,1,1,1,1,1,1,1,1,1,1,1,1,1,1,
1,1,1,1,1,1,1,1,1,1,1,1,1,1,1,1,1,1,1,1,1,1,1,1,1,1,1,1,1,1,1,1,1,1,1,1,
1,1,1,1,1,1,1,1,1,1,1,1,1,1,1,1,1,1,1,1,1,1,1,1,1,1,1,1,1,1,1,1,1,1,1,1,
1,1,1,1,1,1,1,1,1,1,1,1,1,1,1,1,1,1,1,1,1,1,1,6),(-0.941429844431384,-0.940000000000001,
-0.935000000000001,-0.930000000000001,-0.925000000000001,-0.920000000000001,
-0.915000000000001,-0.910000000000001,-0.905000000000001,-0.900000000000001,
-0.895000000000001,-0.890000000000001,-0.885000000000001,-0.880000000000001,
-0.875000000000001,-0.870000000000001,-0.865000000000001,-0.860000000000001,
-0.855000000000001,-0.850000000000001,-0.845000000000001,-0.840000000000001,
-0.835000000000001,-0.830000000000001,-0.825000000000001,-0.820000000000001,
-0.815000000000001,-0.810000000000001,-0.805000000000001,-0.800000000000001,
-0.795000000000001,-0.790000000000001,-0.785000000000001,-0.780000000000001,
-0.775000000000001,-0.770000000000001,-0.765000000000001,-0.760000000000001,
-0.755000000000001,-0.750000000000001,-0.745000000000001,-0.740000000000001,
-0.735000000000001,-0.730000000000001,-0.725000000000001,-0.720000000000001,
-0.715000000000001,-0.710000000000001,-0.705000000000001,-0.700000000000001,
-0.695000000000001,-0.690000000000001,-0.685,-0.68,-0.675,-0.67,-0.665,
-0.66,-0.655,-0.65,-0.645,-0.64,-0.635,-0.63,-0.625,-0.62,-0.615,-0.61,
-0.605,-0.6,-0.595,-0.59,-0.585,-0.58,-0.575,-0.57,-0.565,-0.56,-0.555,
-0.55,-0.545,-0.54,-0.535,-0.53,-0.525,-0.52,-0.515,-0.51,-0.505,-0.5,-0.495,
-0.49,-0.485,-0.48,-0.475,-0.47,-0.465,-0.46,-0.455,-0.45,-0.445,-0.44,
-0.435,-0.43,-0.425,-0.42,-0.415,-0.41,-0.405,-0.4,-0.395,-0.39,-0.385,
-0.38,-0.375,-0.37,-0.365,-0.36,-0.355,-0.35,-0.345,-0.34,-0.335,-0.33,
-0.325,-0.32,-0.315,-0.31,-0.305,-0.3,-0.295,-0.29,-0.285,-0.28,-0.275,
-0.27,-0.265,-0.26,-0.255,-0.25,-0.245,-0.24,-0.235,-0.23,-0.225,-0.22,
-0.215,-0.21,-0.205,-0.2,-0.195,-0.19,-0.185,-0.18,-0.175,-0.17,-0.165,
-0.16,-0.155,-0.15,-0.145,-0.14,-0.135,-0.13,-0.125,-0.12,-0.115,-0.11,
-0.105,-0.1,-0.095,-0.09,-0.085,-0.08,-0.075,-0.07,-0.065,-0.06,-0.055,
-0.05,-0.045,-0.04,-0.035,-0.03,-0.025,-0.02,-0.015,-0.01,-0.005,0.),
 .UNSPECIFIED.)
CURVE()
GEOMETRIC_REPRESENTATION_ITEM()
RATIONAL_B_SPLINE_CURVE((1.,1.,1.,1.,1.,1.,1.,1.,1.,1.,1.,1.,1.,1.,1.,1.,
1.,1.,1.,1.,1.,1.,1.,1.,1.,1.,1.,1.,1.,1.,1.,1.,1.,1.,1.,1.,1.,1.,1.,1.,
1.,1.,1.,1.,1.,1.,1.,1.,1.,1.,1.,1.,1.,1.,1.,1.,1.,1.,1.,1.,1.,1.,1.,1.,
1.,1.,1.,1.,1.,1.,1.,1.,1.,1.,1.,1.,1.,1.,1.,1.,1.,1.,1.,1.,1.,1.,1.,1.,
1.,1.,1.,1.,1.,1.,1.,1.,1.,1.,1.,1.,1.,1.,1.,1.,1.,1.,1.,1.,1.,1.,1.,1.,
1.,1.,1.,1.,1.,1.,1.,1.,1.,1.,1.,1.,1.,1.,1.,1.,1.,1.,1.,1.,1.,1.,1.,1.,
1.,1.,1.,1.,1.,1.,1.,1.,1.,1.,1.,1.,1.,1.,1.,1.,1.,1.,1.,1.,1.,1.,1.,1.,
1.,1.,1.,1.,1.,1.,1.,1.,1.,1.,1.,1.,1.,1.,1.,1.,1.,1.,1.,1.,1.,1.,1.,1.,
1.,1.,1.,1.,1.,1.,1.,1.,1.,1.))
REPRESENTATION_ITEM('')
);
#431=(
BOUNDED_CURVE()
B_SPLINE_CURVE(5,(#65577,#65578,#65579,#65580,#65581,#65582,#65583,#65584,
#65585,#65586,#65587,#65588,#65589,#65590,#65591,#65592,#65593,#65594,#65595,
#65596,#65597,#65598,#65599,#65600,#65601,#65602,#65603,#65604,#65605,#65606,
#65607,#65608,#65609,#65610,#65611,#65612,#65613,#65614,#65615,#65616,#65617,
#65618,#65619,#65620,#65621,#65622,#65623,#65624,#65625,#65626,#65627,#65628,
#65629,#65630,#65631,#65632,#65633,#65634,#65635,#65636,#65637,#65638,#65639,
#65640,#65641,#65642,#65643,#65644,#65645,#65646,#65647,#65648,#65649,#65650,
#65651,#65652,#65653,#65654,#65655,#65656,#65657,#65658,#65659,#65660,#65661,
#65662,#65663,#65664,#65665,#65666,#65667,#65668,#65669,#65670,#65671,#65672,
#65673,#65674,#65675,#65676,#65677,#65678,#65679,#65680,#65681,#65682,#65683,
#65684,#65685,#65686,#65687,#65688,#65689,#65690,#65691,#65692,#65693,#65694,
#65695,#65696,#65697,#65698,#65699,#65700,#65701,#65702,#65703,#65704,#65705,
#65706,#65707,#65708,#65709,#65710,#65711,#65712,#65713,#65714,#65715,#65716,
#65717,#65718,#65719,#65720,#65721,#65722,#65723,#65724,#65725,#65726,#65727,
#65728,#65729,#65730,#65731,#65732,#65733,#65734,#65735,#65736,#65737,#65738,
#65739,#65740,#65741,#65742,#65743,#65744,#65745,#65746,#65747,#65748,#65749,
#65750,#65751,#65752,#65753,#65754,#65755,#65756,#65757,#65758,#65759,#65760,
#65761,#65762,#65763,#65764,#65765,#65766,#65767,#65768,#65769,#65770),
 .UNSPECIFIED.,.F.,.F.)
B_SPLINE_CURVE_WITH_KNOTS((6,1,1,1,1,1,1,1,1,1,1,1,1,1,1,1,1,1,1,1,1,1,
1,1,1,1,1,1,1,1,1,1,1,1,1,1,1,1,1,1,1,1,1,1,1,1,1,1,1,1,1,1,1,1,1,1,1,1,
1,1,1,1,1,1,1,1,1,1,1,1,1,1,1,1,1,1,1,1,1,1,1,1,1,1,1,1,1,1,1,1,1,1,1,1,
1,1,1,1,1,1,1,1,1,1,1,1,1,1,1,1,1,1,1,1,1,1,1,1,1,1,1,1,1,1,1,1,1,1,1,1,
1,1,1,1,1,1,1,1,1,1,1,1,1,1,1,1,1,1,1,1,1,1,1,1,1,1,1,1,1,1,1,1,1,1,1,1,
1,1,1,1,1,1,1,1,1,1,1,1,1,1,1,1,1,1,1,1,1,1,1,6),(0.,0.005,0.01,0.015,0.02,
0.025,0.03,0.035,0.04,0.045,0.05,0.055,0.06,0.065,0.07,0.075,0.08,0.085,
0.09,0.095,0.1,0.105,0.11,0.115,0.12,0.125,0.13,0.135,0.14,0.145,0.15,0.155,
0.16,0.165,0.17,0.175,0.18,0.185,0.19,0.195,0.2,0.205,0.21,0.215,0.22,0.225,
0.23,0.235,0.24,0.245,0.25,0.255,0.26,0.265,0.27,0.275,0.28,0.285,0.29,
0.295,0.3,0.305,0.31,0.315,0.32,0.325,0.33,0.335,0.34,0.345,0.35,0.355,
0.36,0.365,0.37,0.375,0.38,0.385,0.39,0.395,0.4,0.405,0.41,0.415,0.42,0.425,
0.43,0.435,0.44,0.445,0.45,0.455,0.46,0.465,0.47,0.475,0.48,0.485,0.49,
0.495,0.5,0.505,0.51,0.515,0.52,0.525,0.53,0.535,0.54,0.545,0.55,0.555,
0.56,0.565,0.57,0.575,0.58,0.585,0.59,0.595,0.6,0.605,0.61,0.615,0.62,0.625,
0.63,0.635,0.64,0.645,0.65,0.655,0.66,0.665,0.67,0.675,0.68,0.685,0.690000000000001,
0.695000000000001,0.700000000000001,0.705000000000001,0.710000000000001,
0.715000000000001,0.720000000000001,0.725000000000001,0.730000000000001,
0.735000000000001,0.740000000000001,0.745000000000001,0.750000000000001,
0.755000000000001,0.760000000000001,0.765000000000001,0.770000000000001,
0.775000000000001,0.780000000000001,0.785000000000001,0.790000000000001,
0.795000000000001,0.800000000000001,0.805000000000001,0.810000000000001,
0.815000000000001,0.820000000000001,0.825000000000001,0.830000000000001,
0.835000000000001,0.840000000000001,0.845000000000001,0.850000000000001,
0.855000000000001,0.860000000000001,0.865000000000001,0.870000000000001,
0.875000000000001,0.880000000000001,0.885000000000001,0.890000000000001,
0.895000000000001,0.900000000000001,0.905000000000001,0.910000000000001,
0.915000000000001,0.920000000000001,0.925000000000001,0.930000000000001,
0.935000000000001,0.940000000000001,0.941429844431397),.UNSPECIFIED.)
CURVE()
GEOMETRIC_REPRESENTATION_ITEM()
RATIONAL_B_SPLINE_CURVE((1.,1.,1.,1.,1.,1.,1.,1.,1.,1.,1.,1.,1.,1.,1.,1.,
1.,1.,1.,1.,1.,1.,1.,1.,1.,1.,1.,1.,1.,1.,1.,1.,1.,1.,1.,1.,1.,1.,1.,1.,
1.,1.,1.,1.,1.,1.,1.,1.,1.,1.,1.,1.,1.,1.,1.,1.,1.,1.,1.,1.,1.,1.,1.,1.,
1.,1.,1.,1.,1.,1.,1.,1.,1.,1.,1.,1.,1.,1.,1.,1.,1.,1.,1.,1.,1.,1.,1.,1.,
1.,1.,1.,1.,1.,1.,1.,1.,1.,1.,1.,1.,1.,1.,1.,1.,1.,1.,1.,1.,1.,1.,1.,1.,
1.,1.,1.,1.,1.,1.,1.,1.,1.,1.,1.,1.,1.,1.,1.,1.,1.,1.,1.,1.,1.,1.,1.,1.,
1.,1.,1.,1.,1.,1.,1.,1.,1.,1.,1.,1.,1.,1.,1.,1.,1.,1.,1.,1.,1.,1.,1.,1.,
1.,1.,1.,1.,1.,1.,1.,1.,1.,1.,1.,1.,1.,1.,1.,1.,1.,1.,1.,1.,1.,1.,1.,1.,
1.,1.,1.,1.,1.,1.,1.,1.,1.,1.))
REPRESENTATION_ITEM('')
);
#432=(
BOUNDED_CURVE()
B_SPLINE_CURVE(5,(#65773,#65774,#65775,#65776,#65777,#65778,#65779,#65780,
#65781,#65782,#65783,#65784,#65785,#65786,#65787,#65788,#65789,#65790,#65791,
#65792,#65793,#65794,#65795,#65796,#65797,#65798,#65799,#65800,#65801,#65802,
#65803,#65804,#65805,#65806,#65807,#65808,#65809,#65810,#65811,#65812,#65813,
#65814,#65815,#65816,#65817,#65818,#65819,#65820,#65821,#65822,#65823,#65824,
#65825,#65826,#65827,#65828,#65829,#65830,#65831,#65832,#65833,#65834,#65835,
#65836,#65837,#65838,#65839,#65840,#65841,#65842,#65843,#65844,#65845,#65846,
#65847,#65848,#65849,#65850,#65851,#65852,#65853,#65854,#65855,#65856,#65857,
#65858,#65859,#65860,#65861,#65862,#65863,#65864,#65865,#65866,#65867,#65868,
#65869,#65870,#65871,#65872,#65873,#65874,#65875,#65876,#65877,#65878,#65879,
#65880,#65881,#65882,#65883,#65884,#65885,#65886,#65887,#65888,#65889,#65890,
#65891,#65892,#65893,#65894,#65895,#65896,#65897,#65898,#65899,#65900,#65901,
#65902,#65903,#65904,#65905,#65906,#65907,#65908,#65909,#65910,#65911,#65912,
#65913,#65914,#65915,#65916,#65917,#65918,#65919,#65920,#65921,#65922,#65923,
#65924,#65925,#65926,#65927,#65928,#65929,#65930,#65931,#65932,#65933,#65934,
#65935,#65936,#65937,#65938,#65939,#65940,#65941,#65942,#65943,#65944,#65945,
#65946,#65947,#65948,#65949,#65950,#65951,#65952,#65953,#65954,#65955,#65956,
#65957,#65958,#65959,#65960,#65961,#65962,#65963,#65964,#65965,#65966),
 .UNSPECIFIED.,.F.,.F.)
B_SPLINE_CURVE_WITH_KNOTS((6,1,1,1,1,1,1,1,1,1,1,1,1,1,1,1,1,1,1,1,1,1,
1,1,1,1,1,1,1,1,1,1,1,1,1,1,1,1,1,1,1,1,1,1,1,1,1,1,1,1,1,1,1,1,1,1,1,1,
1,1,1,1,1,1,1,1,1,1,1,1,1,1,1,1,1,1,1,1,1,1,1,1,1,1,1,1,1,1,1,1,1,1,1,1,
1,1,1,1,1,1,1,1,1,1,1,1,1,1,1,1,1,1,1,1,1,1,1,1,1,1,1,1,1,1,1,1,1,1,1,1,
1,1,1,1,1,1,1,1,1,1,1,1,1,1,1,1,1,1,1,1,1,1,1,1,1,1,1,1,1,1,1,1,1,1,1,1,
1,1,1,1,1,1,1,1,1,1,1,1,1,1,1,1,1,1,1,1,1,1,1,6),(-0.941429844431399,-0.940000000000001,
-0.935000000000001,-0.930000000000001,-0.925000000000001,-0.920000000000001,
-0.915000000000001,-0.910000000000001,-0.905000000000001,-0.900000000000001,
-0.895000000000001,-0.890000000000001,-0.885000000000001,-0.880000000000001,
-0.875000000000001,-0.870000000000001,-0.865000000000001,-0.860000000000001,
-0.855000000000001,-0.850000000000001,-0.845000000000001,-0.840000000000001,
-0.835000000000001,-0.830000000000001,-0.825000000000001,-0.820000000000001,
-0.815000000000001,-0.810000000000001,-0.805000000000001,-0.800000000000001,
-0.795000000000001,-0.790000000000001,-0.785000000000001,-0.780000000000001,
-0.775000000000001,-0.770000000000001,-0.765000000000001,-0.760000000000001,
-0.755000000000001,-0.750000000000001,-0.745000000000001,-0.740000000000001,
-0.735000000000001,-0.730000000000001,-0.725000000000001,-0.720000000000001,
-0.715000000000001,-0.710000000000001,-0.705000000000001,-0.700000000000001,
-0.695000000000001,-0.690000000000001,-0.685,-0.68,-0.675,-0.67,-0.665,
-0.66,-0.655,-0.65,-0.645,-0.64,-0.635,-0.63,-0.625,-0.62,-0.615,-0.61,
-0.605,-0.6,-0.595,-0.59,-0.585,-0.58,-0.575,-0.57,-0.565,-0.56,-0.555,
-0.55,-0.545,-0.54,-0.535,-0.53,-0.525,-0.52,-0.515,-0.51,-0.505,-0.5,-0.495,
-0.49,-0.485,-0.48,-0.475,-0.47,-0.465,-0.46,-0.455,-0.45,-0.445,-0.44,
-0.435,-0.43,-0.425,-0.42,-0.415,-0.41,-0.405,-0.4,-0.395,-0.39,-0.385,
-0.38,-0.375,-0.37,-0.365,-0.36,-0.355,-0.35,-0.345,-0.34,-0.335,-0.33,
-0.325,-0.32,-0.315,-0.31,-0.305,-0.3,-0.295,-0.29,-0.285,-0.28,-0.275,
-0.27,-0.265,-0.26,-0.255,-0.25,-0.245,-0.24,-0.235,-0.23,-0.225,-0.22,
-0.215,-0.21,-0.205,-0.2,-0.195,-0.19,-0.185,-0.18,-0.175,-0.17,-0.165,
-0.16,-0.155,-0.15,-0.145,-0.14,-0.135,-0.13,-0.125,-0.12,-0.115,-0.11,
-0.105,-0.1,-0.095,-0.09,-0.085,-0.08,-0.075,-0.07,-0.065,-0.06,-0.055,
-0.05,-0.045,-0.04,-0.035,-0.03,-0.025,-0.02,-0.015,-0.01,-0.005,0.),
 .UNSPECIFIED.)
CURVE()
GEOMETRIC_REPRESENTATION_ITEM()
RATIONAL_B_SPLINE_CURVE((1.,1.,1.,1.,1.,1.,1.,1.,1.,1.,1.,1.,1.,1.,1.,1.,
1.,1.,1.,1.,1.,1.,1.,1.,1.,1.,1.,1.,1.,1.,1.,1.,1.,1.,1.,1.,1.,1.,1.,1.,
1.,1.,1.,1.,1.,1.,1.,1.,1.,1.,1.,1.,1.,1.,1.,1.,1.,1.,1.,1.,1.,1.,1.,1.,
1.,1.,1.,1.,1.,1.,1.,1.,1.,1.,1.,1.,1.,1.,1.,1.,1.,1.,1.,1.,1.,1.,1.,1.,
1.,1.,1.,1.,1.,1.,1.,1.,1.,1.,1.,1.,1.,1.,1.,1.,1.,1.,1.,1.,1.,1.,1.,1.,
1.,1.,1.,1.,1.,1.,1.,1.,1.,1.,1.,1.,1.,1.,1.,1.,1.,1.,1.,1.,1.,1.,1.,1.,
1.,1.,1.,1.,1.,1.,1.,1.,1.,1.,1.,1.,1.,1.,1.,1.,1.,1.,1.,1.,1.,1.,1.,1.,
1.,1.,1.,1.,1.,1.,1.,1.,1.,1.,1.,1.,1.,1.,1.,1.,1.,1.,1.,1.,1.,1.,1.,1.,
1.,1.,1.,1.,1.,1.,1.,1.,1.,1.))
REPRESENTATION_ITEM('')
);
#433=(
BOUNDED_CURVE()
B_SPLINE_CURVE(5,(#66473,#66474,#66475,#66476,#66477,#66478,#66479,#66480,
#66481,#66482,#66483,#66484,#66485,#66486,#66487,#66488,#66489,#66490,#66491,
#66492,#66493,#66494,#66495,#66496,#66497,#66498,#66499,#66500,#66501,#66502,
#66503,#66504,#66505,#66506,#66507,#66508,#66509,#66510,#66511,#66512,#66513,
#66514,#66515,#66516,#66517,#66518,#66519,#66520,#66521,#66522,#66523,#66524,
#66525,#66526,#66527,#66528,#66529,#66530,#66531,#66532,#66533,#66534,#66535,
#66536,#66537,#66538,#66539,#66540,#66541,#66542,#66543,#66544,#66545,#66546,
#66547,#66548,#66549,#66550,#66551,#66552,#66553,#66554,#66555,#66556,#66557,
#66558,#66559,#66560,#66561,#66562,#66563,#66564,#66565,#66566,#66567,#66568,
#66569,#66570,#66571,#66572,#66573,#66574,#66575,#66576,#66577,#66578,#66579,
#66580,#66581,#66582,#66583,#66584,#66585,#66586,#66587,#66588,#66589,#66590,
#66591,#66592,#66593,#66594,#66595,#66596,#66597,#66598,#66599,#66600,#66601,
#66602,#66603,#66604,#66605,#66606,#66607,#66608,#66609,#66610,#66611,#66612,
#66613,#66614,#66615,#66616,#66617,#66618,#66619,#66620,#66621,#66622,#66623,
#66624,#66625,#66626,#66627,#66628,#66629,#66630,#66631,#66632,#66633,#66634,
#66635,#66636,#66637,#66638,#66639,#66640,#66641,#66642,#66643,#66644,#66645,
#66646,#66647,#66648,#66649,#66650,#66651,#66652,#66653,#66654,#66655,#66656,
#66657,#66658,#66659,#66660,#66661,#66662,#66663,#66664,#66665,#66666),
 .UNSPECIFIED.,.F.,.F.)
B_SPLINE_CURVE_WITH_KNOTS((6,1,1,1,1,1,1,1,1,1,1,1,1,1,1,1,1,1,1,1,1,1,
1,1,1,1,1,1,1,1,1,1,1,1,1,1,1,1,1,1,1,1,1,1,1,1,1,1,1,1,1,1,1,1,1,1,1,1,
1,1,1,1,1,1,1,1,1,1,1,1,1,1,1,1,1,1,1,1,1,1,1,1,1,1,1,1,1,1,1,1,1,1,1,1,
1,1,1,1,1,1,1,1,1,1,1,1,1,1,1,1,1,1,1,1,1,1,1,1,1,1,1,1,1,1,1,1,1,1,1,1,
1,1,1,1,1,1,1,1,1,1,1,1,1,1,1,1,1,1,1,1,1,1,1,1,1,1,1,1,1,1,1,1,1,1,1,1,
1,1,1,1,1,1,1,1,1,1,1,1,1,1,1,1,1,1,1,1,1,1,1,6),(0.,0.005,0.01,0.015,0.02,
0.025,0.03,0.035,0.04,0.045,0.05,0.055,0.06,0.065,0.07,0.075,0.08,0.085,
0.09,0.095,0.1,0.105,0.11,0.115,0.12,0.125,0.13,0.135,0.14,0.145,0.15,0.155,
0.16,0.165,0.17,0.175,0.18,0.185,0.19,0.195,0.2,0.205,0.21,0.215,0.22,0.225,
0.23,0.235,0.24,0.245,0.25,0.255,0.26,0.265,0.27,0.275,0.28,0.285,0.29,
0.295,0.3,0.305,0.31,0.315,0.32,0.325,0.33,0.335,0.34,0.345,0.35,0.355,
0.36,0.365,0.37,0.375,0.38,0.385,0.39,0.395,0.4,0.405,0.41,0.415,0.42,0.425,
0.43,0.435,0.44,0.445,0.45,0.455,0.46,0.465,0.47,0.475,0.48,0.485,0.49,
0.495,0.5,0.505,0.51,0.515,0.52,0.525,0.53,0.535,0.54,0.545,0.55,0.555,
0.56,0.565,0.57,0.575,0.58,0.585,0.59,0.595,0.6,0.605,0.61,0.615,0.62,0.625,
0.63,0.635,0.64,0.645,0.65,0.655,0.66,0.665,0.67,0.675,0.68,0.685,0.690000000000001,
0.695000000000001,0.700000000000001,0.705000000000001,0.710000000000001,
0.715000000000001,0.720000000000001,0.725000000000001,0.730000000000001,
0.735000000000001,0.740000000000001,0.745000000000001,0.750000000000001,
0.755000000000001,0.760000000000001,0.765000000000001,0.770000000000001,
0.775000000000001,0.780000000000001,0.785000000000001,0.790000000000001,
0.795000000000001,0.800000000000001,0.805000000000001,0.810000000000001,
0.815000000000001,0.820000000000001,0.825000000000001,0.830000000000001,
0.835000000000001,0.840000000000001,0.845000000000001,0.850000000000001,
0.855000000000001,0.860000000000001,0.865000000000001,0.870000000000001,
0.875000000000001,0.880000000000001,0.885000000000001,0.890000000000001,
0.895000000000001,0.900000000000001,0.905000000000001,0.910000000000001,
0.915000000000001,0.920000000000001,0.925000000000001,0.930000000000001,
0.935000000000001,0.940000000000001,0.941429844431383),.UNSPECIFIED.)
CURVE()
GEOMETRIC_REPRESENTATION_ITEM()
RATIONAL_B_SPLINE_CURVE((1.,1.,1.,1.,1.,1.,1.,1.,1.,1.,1.,1.,1.,1.,1.,1.,
1.,1.,1.,1.,1.,1.,1.,1.,1.,1.,1.,1.,1.,1.,1.,1.,1.,1.,1.,1.,1.,1.,1.,1.,
1.,1.,1.,1.,1.,1.,1.,1.,1.,1.,1.,1.,1.,1.,1.,1.,1.,1.,1.,1.,1.,1.,1.,1.,
1.,1.,1.,1.,1.,1.,1.,1.,1.,1.,1.,1.,1.,1.,1.,1.,1.,1.,1.,1.,1.,1.,1.,1.,
1.,1.,1.,1.,1.,1.,1.,1.,1.,1.,1.,1.,1.,1.,1.,1.,1.,1.,1.,1.,1.,1.,1.,1.,
1.,1.,1.,1.,1.,1.,1.,1.,1.,1.,1.,1.,1.,1.,1.,1.,1.,1.,1.,1.,1.,1.,1.,1.,
1.,1.,1.,1.,1.,1.,1.,1.,1.,1.,1.,1.,1.,1.,1.,1.,1.,1.,1.,1.,1.,1.,1.,1.,
1.,1.,1.,1.,1.,1.,1.,1.,1.,1.,1.,1.,1.,1.,1.,1.,1.,1.,1.,1.,1.,1.,1.,1.,
1.,1.,1.,1.,1.,1.,1.,1.,1.,1.))
REPRESENTATION_ITEM('')
);
#434=(
BOUNDED_CURVE()
B_SPLINE_CURVE(5,(#66669,#66670,#66671,#66672,#66673,#66674,#66675,#66676,
#66677,#66678,#66679,#66680,#66681,#66682,#66683,#66684,#66685,#66686,#66687,
#66688,#66689,#66690,#66691,#66692,#66693,#66694,#66695,#66696,#66697,#66698,
#66699,#66700,#66701,#66702,#66703,#66704,#66705,#66706,#66707,#66708,#66709,
#66710,#66711,#66712,#66713,#66714,#66715,#66716,#66717,#66718,#66719,#66720,
#66721,#66722,#66723,#66724,#66725,#66726,#66727,#66728,#66729,#66730,#66731,
#66732,#66733,#66734,#66735,#66736,#66737,#66738,#66739,#66740,#66741,#66742,
#66743,#66744,#66745,#66746,#66747,#66748,#66749,#66750,#66751,#66752,#66753,
#66754,#66755,#66756,#66757,#66758,#66759,#66760,#66761,#66762,#66763,#66764,
#66765,#66766,#66767,#66768,#66769,#66770,#66771,#66772,#66773,#66774,#66775,
#66776,#66777,#66778,#66779,#66780,#66781,#66782,#66783,#66784,#66785,#66786,
#66787,#66788,#66789,#66790,#66791,#66792,#66793,#66794,#66795,#66796,#66797,
#66798,#66799,#66800,#66801,#66802,#66803,#66804,#66805,#66806,#66807,#66808,
#66809,#66810,#66811,#66812,#66813,#66814,#66815,#66816,#66817,#66818,#66819,
#66820,#66821,#66822,#66823,#66824,#66825,#66826,#66827,#66828,#66829,#66830,
#66831,#66832,#66833,#66834,#66835,#66836,#66837,#66838,#66839,#66840,#66841,
#66842,#66843,#66844,#66845,#66846,#66847,#66848,#66849,#66850,#66851,#66852,
#66853,#66854,#66855,#66856,#66857,#66858,#66859,#66860,#66861,#66862),
 .UNSPECIFIED.,.F.,.F.)
B_SPLINE_CURVE_WITH_KNOTS((6,1,1,1,1,1,1,1,1,1,1,1,1,1,1,1,1,1,1,1,1,1,
1,1,1,1,1,1,1,1,1,1,1,1,1,1,1,1,1,1,1,1,1,1,1,1,1,1,1,1,1,1,1,1,1,1,1,1,
1,1,1,1,1,1,1,1,1,1,1,1,1,1,1,1,1,1,1,1,1,1,1,1,1,1,1,1,1,1,1,1,1,1,1,1,
1,1,1,1,1,1,1,1,1,1,1,1,1,1,1,1,1,1,1,1,1,1,1,1,1,1,1,1,1,1,1,1,1,1,1,1,
1,1,1,1,1,1,1,1,1,1,1,1,1,1,1,1,1,1,1,1,1,1,1,1,1,1,1,1,1,1,1,1,1,1,1,1,
1,1,1,1,1,1,1,1,1,1,1,1,1,1,1,1,1,1,1,1,1,1,1,6),(-0.941429844431371,-0.940000000000001,
-0.935000000000001,-0.930000000000001,-0.925000000000001,-0.920000000000001,
-0.915000000000001,-0.910000000000001,-0.905000000000001,-0.900000000000001,
-0.895000000000001,-0.890000000000001,-0.885000000000001,-0.880000000000001,
-0.875000000000001,-0.870000000000001,-0.865000000000001,-0.860000000000001,
-0.855000000000001,-0.850000000000001,-0.845000000000001,-0.840000000000001,
-0.835000000000001,-0.830000000000001,-0.825000000000001,-0.820000000000001,
-0.815000000000001,-0.810000000000001,-0.805000000000001,-0.800000000000001,
-0.795000000000001,-0.790000000000001,-0.785000000000001,-0.780000000000001,
-0.775000000000001,-0.770000000000001,-0.765000000000001,-0.760000000000001,
-0.755000000000001,-0.750000000000001,-0.745000000000001,-0.740000000000001,
-0.735000000000001,-0.730000000000001,-0.725000000000001,-0.720000000000001,
-0.715000000000001,-0.710000000000001,-0.705000000000001,-0.700000000000001,
-0.695000000000001,-0.690000000000001,-0.685,-0.68,-0.675,-0.67,-0.665,
-0.66,-0.655,-0.65,-0.645,-0.64,-0.635,-0.63,-0.625,-0.62,-0.615,-0.61,
-0.605,-0.6,-0.595,-0.59,-0.585,-0.58,-0.575,-0.57,-0.565,-0.56,-0.555,
-0.55,-0.545,-0.54,-0.535,-0.53,-0.525,-0.52,-0.515,-0.51,-0.505,-0.5,-0.495,
-0.49,-0.485,-0.48,-0.475,-0.47,-0.465,-0.46,-0.455,-0.45,-0.445,-0.44,
-0.435,-0.43,-0.425,-0.42,-0.415,-0.41,-0.405,-0.4,-0.395,-0.39,-0.385,
-0.38,-0.375,-0.37,-0.365,-0.36,-0.355,-0.35,-0.345,-0.34,-0.335,-0.33,
-0.325,-0.32,-0.315,-0.31,-0.305,-0.3,-0.295,-0.29,-0.285,-0.28,-0.275,
-0.27,-0.265,-0.26,-0.255,-0.25,-0.245,-0.24,-0.235,-0.23,-0.225,-0.22,
-0.215,-0.21,-0.205,-0.2,-0.195,-0.19,-0.185,-0.18,-0.175,-0.17,-0.165,
-0.16,-0.155,-0.15,-0.145,-0.14,-0.135,-0.13,-0.125,-0.12,-0.115,-0.11,
-0.105,-0.1,-0.095,-0.09,-0.085,-0.08,-0.075,-0.07,-0.065,-0.06,-0.055,
-0.05,-0.045,-0.04,-0.035,-0.03,-0.025,-0.02,-0.015,-0.01,-0.005,0.),
 .UNSPECIFIED.)
CURVE()
GEOMETRIC_REPRESENTATION_ITEM()
RATIONAL_B_SPLINE_CURVE((1.,1.,1.,1.,1.,1.,1.,1.,1.,1.,1.,1.,1.,1.,1.,1.,
1.,1.,1.,1.,1.,1.,1.,1.,1.,1.,1.,1.,1.,1.,1.,1.,1.,1.,1.,1.,1.,1.,1.,1.,
1.,1.,1.,1.,1.,1.,1.,1.,1.,1.,1.,1.,1.,1.,1.,1.,1.,1.,1.,1.,1.,1.,1.,1.,
1.,1.,1.,1.,1.,1.,1.,1.,1.,1.,1.,1.,1.,1.,1.,1.,1.,1.,1.,1.,1.,1.,1.,1.,
1.,1.,1.,1.,1.,1.,1.,1.,1.,1.,1.,1.,1.,1.,1.,1.,1.,1.,1.,1.,1.,1.,1.,1.,
1.,1.,1.,1.,1.,1.,1.,1.,1.,1.,1.,1.,1.,1.,1.,1.,1.,1.,1.,1.,1.,1.,1.,1.,
1.,1.,1.,1.,1.,1.,1.,1.,1.,1.,1.,1.,1.,1.,1.,1.,1.,1.,1.,1.,1.,1.,1.,1.,
1.,1.,1.,1.,1.,1.,1.,1.,1.,1.,1.,1.,1.,1.,1.,1.,1.,1.,1.,1.,1.,1.,1.,1.,
1.,1.,1.,1.,1.,1.,1.,1.,1.,1.))
REPRESENTATION_ITEM('')
);
#435=(
BOUNDED_CURVE()
B_SPLINE_CURVE(5,(#67369,#67370,#67371,#67372,#67373,#67374,#67375,#67376,
#67377,#67378,#67379,#67380,#67381,#67382,#67383,#67384,#67385,#67386,#67387,
#67388,#67389,#67390,#67391,#67392,#67393,#67394,#67395,#67396,#67397,#67398,
#67399,#67400,#67401,#67402,#67403,#67404,#67405,#67406,#67407,#67408,#67409,
#67410,#67411,#67412,#67413,#67414,#67415,#67416,#67417,#67418,#67419,#67420,
#67421,#67422,#67423,#67424,#67425,#67426,#67427,#67428,#67429,#67430,#67431,
#67432,#67433,#67434,#67435,#67436,#67437,#67438,#67439,#67440,#67441,#67442,
#67443,#67444,#67445,#67446,#67447,#67448,#67449,#67450,#67451,#67452,#67453,
#67454,#67455,#67456,#67457,#67458,#67459,#67460,#67461,#67462,#67463,#67464,
#67465,#67466,#67467,#67468,#67469,#67470,#67471,#67472,#67473,#67474,#67475,
#67476,#67477,#67478,#67479,#67480,#67481,#67482,#67483,#67484,#67485,#67486,
#67487,#67488,#67489,#67490,#67491,#67492,#67493,#67494,#67495,#67496,#67497,
#67498,#67499,#67500,#67501,#67502,#67503,#67504,#67505,#67506,#67507,#67508,
#67509,#67510,#67511,#67512,#67513,#67514,#67515,#67516,#67517,#67518,#67519,
#67520,#67521,#67522,#67523,#67524,#67525,#67526,#67527,#67528,#67529,#67530,
#67531,#67532,#67533,#67534,#67535,#67536,#67537,#67538,#67539,#67540,#67541,
#67542,#67543,#67544,#67545,#67546,#67547,#67548,#67549,#67550,#67551,#67552,
#67553,#67554,#67555,#67556,#67557,#67558,#67559,#67560,#67561,#67562),
 .UNSPECIFIED.,.F.,.F.)
B_SPLINE_CURVE_WITH_KNOTS((6,1,1,1,1,1,1,1,1,1,1,1,1,1,1,1,1,1,1,1,1,1,
1,1,1,1,1,1,1,1,1,1,1,1,1,1,1,1,1,1,1,1,1,1,1,1,1,1,1,1,1,1,1,1,1,1,1,1,
1,1,1,1,1,1,1,1,1,1,1,1,1,1,1,1,1,1,1,1,1,1,1,1,1,1,1,1,1,1,1,1,1,1,1,1,
1,1,1,1,1,1,1,1,1,1,1,1,1,1,1,1,1,1,1,1,1,1,1,1,1,1,1,1,1,1,1,1,1,1,1,1,
1,1,1,1,1,1,1,1,1,1,1,1,1,1,1,1,1,1,1,1,1,1,1,1,1,1,1,1,1,1,1,1,1,1,1,1,
1,1,1,1,1,1,1,1,1,1,1,1,1,1,1,1,1,1,1,1,1,1,1,6),(0.,0.005,0.01,0.015,0.02,
0.025,0.03,0.035,0.04,0.045,0.05,0.055,0.06,0.065,0.07,0.075,0.08,0.085,
0.09,0.095,0.1,0.105,0.11,0.115,0.12,0.125,0.13,0.135,0.14,0.145,0.15,0.155,
0.16,0.165,0.17,0.175,0.18,0.185,0.19,0.195,0.2,0.205,0.21,0.215,0.22,0.225,
0.23,0.235,0.24,0.245,0.25,0.255,0.26,0.265,0.27,0.275,0.28,0.285,0.29,
0.295,0.3,0.305,0.31,0.315,0.32,0.325,0.33,0.335,0.34,0.345,0.35,0.355,
0.36,0.365,0.37,0.375,0.38,0.385,0.39,0.395,0.4,0.405,0.41,0.415,0.42,0.425,
0.43,0.435,0.44,0.445,0.45,0.455,0.46,0.465,0.47,0.475,0.48,0.485,0.49,
0.495,0.5,0.505,0.51,0.515,0.52,0.525,0.53,0.535,0.54,0.545,0.55,0.555,
0.56,0.565,0.57,0.575,0.58,0.585,0.59,0.595,0.6,0.605,0.61,0.615,0.62,0.625,
0.63,0.635,0.64,0.645,0.65,0.655,0.66,0.665,0.67,0.675,0.68,0.685,0.690000000000001,
0.695000000000001,0.700000000000001,0.705000000000001,0.710000000000001,
0.715000000000001,0.720000000000001,0.725000000000001,0.730000000000001,
0.735000000000001,0.740000000000001,0.745000000000001,0.750000000000001,
0.755000000000001,0.760000000000001,0.765000000000001,0.770000000000001,
0.775000000000001,0.780000000000001,0.785000000000001,0.790000000000001,
0.795000000000001,0.800000000000001,0.805000000000001,0.810000000000001,
0.815000000000001,0.820000000000001,0.825000000000001,0.830000000000001,
0.835000000000001,0.840000000000001,0.845000000000001,0.850000000000001,
0.855000000000001,0.860000000000001,0.865000000000001,0.870000000000001,
0.875000000000001,0.880000000000001,0.885000000000001,0.890000000000001,
0.895000000000001,0.900000000000001,0.905000000000001,0.910000000000001,
0.915000000000001,0.920000000000001,0.925000000000001,0.930000000000001,
0.935000000000001,0.940000000000001,0.941429844431383),.UNSPECIFIED.)
CURVE()
GEOMETRIC_REPRESENTATION_ITEM()
RATIONAL_B_SPLINE_CURVE((1.,1.,1.,1.,1.,1.,1.,1.,1.,1.,1.,1.,1.,1.,1.,1.,
1.,1.,1.,1.,1.,1.,1.,1.,1.,1.,1.,1.,1.,1.,1.,1.,1.,1.,1.,1.,1.,1.,1.,1.,
1.,1.,1.,1.,1.,1.,1.,1.,1.,1.,1.,1.,1.,1.,1.,1.,1.,1.,1.,1.,1.,1.,1.,1.,
1.,1.,1.,1.,1.,1.,1.,1.,1.,1.,1.,1.,1.,1.,1.,1.,1.,1.,1.,1.,1.,1.,1.,1.,
1.,1.,1.,1.,1.,1.,1.,1.,1.,1.,1.,1.,1.,1.,1.,1.,1.,1.,1.,1.,1.,1.,1.,1.,
1.,1.,1.,1.,1.,1.,1.,1.,1.,1.,1.,1.,1.,1.,1.,1.,1.,1.,1.,1.,1.,1.,1.,1.,
1.,1.,1.,1.,1.,1.,1.,1.,1.,1.,1.,1.,1.,1.,1.,1.,1.,1.,1.,1.,1.,1.,1.,1.,
1.,1.,1.,1.,1.,1.,1.,1.,1.,1.,1.,1.,1.,1.,1.,1.,1.,1.,1.,1.,1.,1.,1.,1.,
1.,1.,1.,1.,1.,1.,1.,1.,1.,1.))
REPRESENTATION_ITEM('')
);
#436=(
BOUNDED_CURVE()
B_SPLINE_CURVE(5,(#67565,#67566,#67567,#67568,#67569,#67570,#67571,#67572,
#67573,#67574,#67575,#67576,#67577,#67578,#67579,#67580,#67581,#67582,#67583,
#67584,#67585,#67586,#67587,#67588,#67589,#67590,#67591,#67592,#67593,#67594,
#67595,#67596,#67597,#67598,#67599,#67600,#67601,#67602,#67603,#67604,#67605,
#67606,#67607,#67608,#67609,#67610,#67611,#67612,#67613,#67614,#67615,#67616,
#67617,#67618,#67619,#67620,#67621,#67622,#67623,#67624,#67625,#67626,#67627,
#67628,#67629,#67630,#67631,#67632,#67633,#67634,#67635,#67636,#67637,#67638,
#67639,#67640,#67641,#67642,#67643,#67644,#67645,#67646,#67647,#67648,#67649,
#67650,#67651,#67652,#67653,#67654,#67655,#67656,#67657,#67658,#67659,#67660,
#67661,#67662,#67663,#67664,#67665,#67666,#67667,#67668,#67669,#67670,#67671,
#67672,#67673,#67674,#67675,#67676,#67677,#67678,#67679,#67680,#67681,#67682,
#67683,#67684,#67685,#67686,#67687,#67688,#67689,#67690,#67691,#67692,#67693,
#67694,#67695,#67696,#67697,#67698,#67699,#67700,#67701,#67702,#67703,#67704,
#67705,#67706,#67707,#67708,#67709,#67710,#67711,#67712,#67713,#67714,#67715,
#67716,#67717,#67718,#67719,#67720,#67721,#67722,#67723,#67724,#67725,#67726,
#67727,#67728,#67729,#67730,#67731,#67732,#67733,#67734,#67735,#67736,#67737,
#67738,#67739,#67740,#67741,#67742,#67743,#67744,#67745,#67746,#67747,#67748,
#67749,#67750,#67751,#67752,#67753,#67754,#67755,#67756,#67757,#67758),
 .UNSPECIFIED.,.F.,.F.)
B_SPLINE_CURVE_WITH_KNOTS((6,1,1,1,1,1,1,1,1,1,1,1,1,1,1,1,1,1,1,1,1,1,
1,1,1,1,1,1,1,1,1,1,1,1,1,1,1,1,1,1,1,1,1,1,1,1,1,1,1,1,1,1,1,1,1,1,1,1,
1,1,1,1,1,1,1,1,1,1,1,1,1,1,1,1,1,1,1,1,1,1,1,1,1,1,1,1,1,1,1,1,1,1,1,1,
1,1,1,1,1,1,1,1,1,1,1,1,1,1,1,1,1,1,1,1,1,1,1,1,1,1,1,1,1,1,1,1,1,1,1,1,
1,1,1,1,1,1,1,1,1,1,1,1,1,1,1,1,1,1,1,1,1,1,1,1,1,1,1,1,1,1,1,1,1,1,1,1,
1,1,1,1,1,1,1,1,1,1,1,1,1,1,1,1,1,1,1,1,1,1,1,6),(-0.941429844431383,-0.940000000000001,
-0.935000000000001,-0.930000000000001,-0.925000000000001,-0.920000000000001,
-0.915000000000001,-0.910000000000001,-0.905000000000001,-0.900000000000001,
-0.895000000000001,-0.890000000000001,-0.885000000000001,-0.880000000000001,
-0.875000000000001,-0.870000000000001,-0.865000000000001,-0.860000000000001,
-0.855000000000001,-0.850000000000001,-0.845000000000001,-0.840000000000001,
-0.835000000000001,-0.830000000000001,-0.825000000000001,-0.820000000000001,
-0.815000000000001,-0.810000000000001,-0.805000000000001,-0.800000000000001,
-0.795000000000001,-0.790000000000001,-0.785000000000001,-0.780000000000001,
-0.775000000000001,-0.770000000000001,-0.765000000000001,-0.760000000000001,
-0.755000000000001,-0.750000000000001,-0.745000000000001,-0.740000000000001,
-0.735000000000001,-0.730000000000001,-0.725000000000001,-0.720000000000001,
-0.715000000000001,-0.710000000000001,-0.705000000000001,-0.700000000000001,
-0.695000000000001,-0.690000000000001,-0.685,-0.68,-0.675,-0.67,-0.665,
-0.66,-0.655,-0.65,-0.645,-0.64,-0.635,-0.63,-0.625,-0.62,-0.615,-0.61,
-0.605,-0.6,-0.595,-0.59,-0.585,-0.58,-0.575,-0.57,-0.565,-0.56,-0.555,
-0.55,-0.545,-0.54,-0.535,-0.53,-0.525,-0.52,-0.515,-0.51,-0.505,-0.5,-0.495,
-0.49,-0.485,-0.48,-0.475,-0.47,-0.465,-0.46,-0.455,-0.45,-0.445,-0.44,
-0.435,-0.43,-0.425,-0.42,-0.415,-0.41,-0.405,-0.4,-0.395,-0.39,-0.385,
-0.38,-0.375,-0.37,-0.365,-0.36,-0.355,-0.35,-0.345,-0.34,-0.335,-0.33,
-0.325,-0.32,-0.315,-0.31,-0.305,-0.3,-0.295,-0.29,-0.285,-0.28,-0.275,
-0.27,-0.265,-0.26,-0.255,-0.25,-0.245,-0.24,-0.235,-0.23,-0.225,-0.22,
-0.215,-0.21,-0.205,-0.2,-0.195,-0.19,-0.185,-0.18,-0.175,-0.17,-0.165,
-0.16,-0.155,-0.15,-0.145,-0.14,-0.135,-0.13,-0.125,-0.12,-0.115,-0.11,
-0.105,-0.1,-0.095,-0.09,-0.085,-0.08,-0.075,-0.07,-0.065,-0.06,-0.055,
-0.05,-0.045,-0.04,-0.035,-0.03,-0.025,-0.02,-0.015,-0.01,-0.005,0.),
 .UNSPECIFIED.)
CURVE()
GEOMETRIC_REPRESENTATION_ITEM()
RATIONAL_B_SPLINE_CURVE((1.,1.,1.,1.,1.,1.,1.,1.,1.,1.,1.,1.,1.,1.,1.,1.,
1.,1.,1.,1.,1.,1.,1.,1.,1.,1.,1.,1.,1.,1.,1.,1.,1.,1.,1.,1.,1.,1.,1.,1.,
1.,1.,1.,1.,1.,1.,1.,1.,1.,1.,1.,1.,1.,1.,1.,1.,1.,1.,1.,1.,1.,1.,1.,1.,
1.,1.,1.,1.,1.,1.,1.,1.,1.,1.,1.,1.,1.,1.,1.,1.,1.,1.,1.,1.,1.,1.,1.,1.,
1.,1.,1.,1.,1.,1.,1.,1.,1.,1.,1.,1.,1.,1.,1.,1.,1.,1.,1.,1.,1.,1.,1.,1.,
1.,1.,1.,1.,1.,1.,1.,1.,1.,1.,1.,1.,1.,1.,1.,1.,1.,1.,1.,1.,1.,1.,1.,1.,
1.,1.,1.,1.,1.,1.,1.,1.,1.,1.,1.,1.,1.,1.,1.,1.,1.,1.,1.,1.,1.,1.,1.,1.,
1.,1.,1.,1.,1.,1.,1.,1.,1.,1.,1.,1.,1.,1.,1.,1.,1.,1.,1.,1.,1.,1.,1.,1.,
1.,1.,1.,1.,1.,1.,1.,1.,1.,1.))
REPRESENTATION_ITEM('')
);
#437=(
BOUNDED_CURVE()
B_SPLINE_CURVE(5,(#68265,#68266,#68267,#68268,#68269,#68270,#68271,#68272,
#68273,#68274,#68275,#68276,#68277,#68278,#68279,#68280,#68281,#68282,#68283,
#68284,#68285,#68286,#68287,#68288,#68289,#68290,#68291,#68292,#68293,#68294,
#68295,#68296,#68297,#68298,#68299,#68300,#68301,#68302,#68303,#68304,#68305,
#68306,#68307,#68308,#68309,#68310,#68311,#68312,#68313,#68314,#68315,#68316,
#68317,#68318,#68319,#68320,#68321,#68322,#68323,#68324,#68325,#68326,#68327,
#68328,#68329,#68330,#68331,#68332,#68333,#68334,#68335,#68336,#68337,#68338,
#68339,#68340,#68341,#68342,#68343,#68344,#68345,#68346,#68347,#68348,#68349,
#68350,#68351,#68352,#68353,#68354,#68355,#68356,#68357,#68358,#68359,#68360,
#68361,#68362,#68363,#68364,#68365,#68366,#68367,#68368,#68369,#68370,#68371,
#68372,#68373,#68374,#68375,#68376,#68377,#68378,#68379,#68380,#68381,#68382,
#68383,#68384,#68385,#68386,#68387,#68388,#68389,#68390,#68391,#68392,#68393,
#68394,#68395,#68396,#68397,#68398,#68399,#68400,#68401,#68402,#68403,#68404,
#68405,#68406,#68407,#68408,#68409,#68410,#68411,#68412,#68413,#68414,#68415,
#68416,#68417,#68418,#68419,#68420,#68421,#68422,#68423,#68424,#68425,#68426,
#68427,#68428,#68429,#68430,#68431,#68432,#68433,#68434,#68435,#68436,#68437,
#68438,#68439,#68440,#68441,#68442,#68443,#68444,#68445,#68446,#68447,#68448,
#68449,#68450,#68451,#68452,#68453,#68454,#68455,#68456,#68457,#68458),
 .UNSPECIFIED.,.F.,.F.)
B_SPLINE_CURVE_WITH_KNOTS((6,1,1,1,1,1,1,1,1,1,1,1,1,1,1,1,1,1,1,1,1,1,
1,1,1,1,1,1,1,1,1,1,1,1,1,1,1,1,1,1,1,1,1,1,1,1,1,1,1,1,1,1,1,1,1,1,1,1,
1,1,1,1,1,1,1,1,1,1,1,1,1,1,1,1,1,1,1,1,1,1,1,1,1,1,1,1,1,1,1,1,1,1,1,1,
1,1,1,1,1,1,1,1,1,1,1,1,1,1,1,1,1,1,1,1,1,1,1,1,1,1,1,1,1,1,1,1,1,1,1,1,
1,1,1,1,1,1,1,1,1,1,1,1,1,1,1,1,1,1,1,1,1,1,1,1,1,1,1,1,1,1,1,1,1,1,1,1,
1,1,1,1,1,1,1,1,1,1,1,1,1,1,1,1,1,1,1,1,1,1,1,6),(0.,0.005,0.01,0.015,0.02,
0.025,0.03,0.035,0.04,0.045,0.05,0.055,0.06,0.065,0.07,0.075,0.08,0.085,
0.09,0.095,0.1,0.105,0.11,0.115,0.12,0.125,0.13,0.135,0.14,0.145,0.15,0.155,
0.16,0.165,0.17,0.175,0.18,0.185,0.19,0.195,0.2,0.205,0.21,0.215,0.22,0.225,
0.23,0.235,0.24,0.245,0.25,0.255,0.26,0.265,0.27,0.275,0.28,0.285,0.29,
0.295,0.3,0.305,0.31,0.315,0.32,0.325,0.33,0.335,0.34,0.345,0.35,0.355,
0.36,0.365,0.37,0.375,0.38,0.385,0.39,0.395,0.4,0.405,0.41,0.415,0.42,0.425,
0.43,0.435,0.44,0.445,0.45,0.455,0.46,0.465,0.47,0.475,0.48,0.485,0.49,
0.495,0.5,0.505,0.51,0.515,0.52,0.525,0.53,0.535,0.54,0.545,0.55,0.555,
0.56,0.565,0.57,0.575,0.58,0.585,0.59,0.595,0.6,0.605,0.61,0.615,0.62,0.625,
0.63,0.635,0.64,0.645,0.65,0.655,0.66,0.665,0.67,0.675,0.68,0.685,0.690000000000001,
0.695000000000001,0.700000000000001,0.705000000000001,0.710000000000001,
0.715000000000001,0.720000000000001,0.725000000000001,0.730000000000001,
0.735000000000001,0.740000000000001,0.745000000000001,0.750000000000001,
0.755000000000001,0.760000000000001,0.765000000000001,0.770000000000001,
0.775000000000001,0.780000000000001,0.785000000000001,0.790000000000001,
0.795000000000001,0.800000000000001,0.805000000000001,0.810000000000001,
0.815000000000001,0.820000000000001,0.825000000000001,0.830000000000001,
0.835000000000001,0.840000000000001,0.845000000000001,0.850000000000001,
0.855000000000001,0.860000000000001,0.865000000000001,0.870000000000001,
0.875000000000001,0.880000000000001,0.885000000000001,0.890000000000001,
0.895000000000001,0.900000000000001,0.905000000000001,0.910000000000001,
0.915000000000001,0.920000000000001,0.925000000000001,0.930000000000001,
0.935000000000001,0.940000000000001,0.941429844431453),.UNSPECIFIED.)
CURVE()
GEOMETRIC_REPRESENTATION_ITEM()
RATIONAL_B_SPLINE_CURVE((1.,1.,1.,1.,1.,1.,1.,1.,1.,1.,1.,1.,1.,1.,1.,1.,
1.,1.,1.,1.,1.,1.,1.,1.,1.,1.,1.,1.,1.,1.,1.,1.,1.,1.,1.,1.,1.,1.,1.,1.,
1.,1.,1.,1.,1.,1.,1.,1.,1.,1.,1.,1.,1.,1.,1.,1.,1.,1.,1.,1.,1.,1.,1.,1.,
1.,1.,1.,1.,1.,1.,1.,1.,1.,1.,1.,1.,1.,1.,1.,1.,1.,1.,1.,1.,1.,1.,1.,1.,
1.,1.,1.,1.,1.,1.,1.,1.,1.,1.,1.,1.,1.,1.,1.,1.,1.,1.,1.,1.,1.,1.,1.,1.,
1.,1.,1.,1.,1.,1.,1.,1.,1.,1.,1.,1.,1.,1.,1.,1.,1.,1.,1.,1.,1.,1.,1.,1.,
1.,1.,1.,1.,1.,1.,1.,1.,1.,1.,1.,1.,1.,1.,1.,1.,1.,1.,1.,1.,1.,1.,1.,1.,
1.,1.,1.,1.,1.,1.,1.,1.,1.,1.,1.,1.,1.,1.,1.,1.,1.,1.,1.,1.,1.,1.,1.,1.,
1.,1.,1.,1.,1.,1.,1.,1.,1.,1.))
REPRESENTATION_ITEM('')
);
#438=(
BOUNDED_CURVE()
B_SPLINE_CURVE(5,(#68461,#68462,#68463,#68464,#68465,#68466,#68467,#68468,
#68469,#68470,#68471,#68472,#68473,#68474,#68475,#68476,#68477,#68478,#68479,
#68480,#68481,#68482,#68483,#68484,#68485,#68486,#68487,#68488,#68489,#68490,
#68491,#68492,#68493,#68494,#68495,#68496,#68497,#68498,#68499,#68500,#68501,
#68502,#68503,#68504,#68505,#68506,#68507,#68508,#68509,#68510,#68511,#68512,
#68513,#68514,#68515,#68516,#68517,#68518,#68519,#68520,#68521,#68522,#68523,
#68524,#68525,#68526,#68527,#68528,#68529,#68530,#68531,#68532,#68533,#68534,
#68535,#68536,#68537,#68538,#68539,#68540,#68541,#68542,#68543,#68544,#68545,
#68546,#68547,#68548,#68549,#68550,#68551,#68552,#68553,#68554,#68555,#68556,
#68557,#68558,#68559,#68560,#68561,#68562,#68563,#68564,#68565,#68566,#68567,
#68568,#68569,#68570,#68571,#68572,#68573,#68574,#68575,#68576,#68577,#68578,
#68579,#68580,#68581,#68582,#68583,#68584,#68585,#68586,#68587,#68588,#68589,
#68590,#68591,#68592,#68593,#68594,#68595,#68596,#68597,#68598,#68599,#68600,
#68601,#68602,#68603,#68604,#68605,#68606,#68607,#68608,#68609,#68610,#68611,
#68612,#68613,#68614,#68615,#68616,#68617,#68618,#68619,#68620,#68621,#68622,
#68623,#68624,#68625,#68626,#68627,#68628,#68629,#68630,#68631,#68632,#68633,
#68634,#68635,#68636,#68637,#68638,#68639,#68640,#68641,#68642,#68643,#68644,
#68645,#68646,#68647,#68648,#68649,#68650,#68651,#68652,#68653,#68654),
 .UNSPECIFIED.,.F.,.F.)
B_SPLINE_CURVE_WITH_KNOTS((6,1,1,1,1,1,1,1,1,1,1,1,1,1,1,1,1,1,1,1,1,1,
1,1,1,1,1,1,1,1,1,1,1,1,1,1,1,1,1,1,1,1,1,1,1,1,1,1,1,1,1,1,1,1,1,1,1,1,
1,1,1,1,1,1,1,1,1,1,1,1,1,1,1,1,1,1,1,1,1,1,1,1,1,1,1,1,1,1,1,1,1,1,1,1,
1,1,1,1,1,1,1,1,1,1,1,1,1,1,1,1,1,1,1,1,1,1,1,1,1,1,1,1,1,1,1,1,1,1,1,1,
1,1,1,1,1,1,1,1,1,1,1,1,1,1,1,1,1,1,1,1,1,1,1,1,1,1,1,1,1,1,1,1,1,1,1,1,
1,1,1,1,1,1,1,1,1,1,1,1,1,1,1,1,1,1,1,1,1,1,1,6),(-0.941429844431454,-0.940000000000001,
-0.935000000000001,-0.930000000000001,-0.925000000000001,-0.920000000000001,
-0.915000000000001,-0.910000000000001,-0.905000000000001,-0.900000000000001,
-0.895000000000001,-0.890000000000001,-0.885000000000001,-0.880000000000001,
-0.875000000000001,-0.870000000000001,-0.865000000000001,-0.860000000000001,
-0.855000000000001,-0.850000000000001,-0.845000000000001,-0.840000000000001,
-0.835000000000001,-0.830000000000001,-0.825000000000001,-0.820000000000001,
-0.815000000000001,-0.810000000000001,-0.805000000000001,-0.800000000000001,
-0.795000000000001,-0.790000000000001,-0.785000000000001,-0.780000000000001,
-0.775000000000001,-0.770000000000001,-0.765000000000001,-0.760000000000001,
-0.755000000000001,-0.750000000000001,-0.745000000000001,-0.740000000000001,
-0.735000000000001,-0.730000000000001,-0.725000000000001,-0.720000000000001,
-0.715000000000001,-0.710000000000001,-0.705000000000001,-0.700000000000001,
-0.695000000000001,-0.690000000000001,-0.685,-0.68,-0.675,-0.67,-0.665,
-0.66,-0.655,-0.65,-0.645,-0.64,-0.635,-0.63,-0.625,-0.62,-0.615,-0.61,
-0.605,-0.6,-0.595,-0.59,-0.585,-0.58,-0.575,-0.57,-0.565,-0.56,-0.555,
-0.55,-0.545,-0.54,-0.535,-0.53,-0.525,-0.52,-0.515,-0.51,-0.505,-0.5,-0.495,
-0.49,-0.485,-0.48,-0.475,-0.47,-0.465,-0.46,-0.455,-0.45,-0.445,-0.44,
-0.435,-0.43,-0.425,-0.42,-0.415,-0.41,-0.405,-0.4,-0.395,-0.39,-0.385,
-0.38,-0.375,-0.37,-0.365,-0.36,-0.355,-0.35,-0.345,-0.34,-0.335,-0.33,
-0.325,-0.32,-0.315,-0.31,-0.305,-0.3,-0.295,-0.29,-0.285,-0.28,-0.275,
-0.27,-0.265,-0.26,-0.255,-0.25,-0.245,-0.24,-0.235,-0.23,-0.225,-0.22,
-0.215,-0.21,-0.205,-0.2,-0.195,-0.19,-0.185,-0.18,-0.175,-0.17,-0.165,
-0.16,-0.155,-0.15,-0.145,-0.14,-0.135,-0.13,-0.125,-0.12,-0.115,-0.11,
-0.105,-0.1,-0.095,-0.09,-0.085,-0.08,-0.075,-0.07,-0.065,-0.06,-0.055,
-0.05,-0.045,-0.04,-0.035,-0.03,-0.025,-0.02,-0.015,-0.01,-0.005,0.),
 .UNSPECIFIED.)
CURVE()
GEOMETRIC_REPRESENTATION_ITEM()
RATIONAL_B_SPLINE_CURVE((1.,1.,1.,1.,1.,1.,1.,1.,1.,1.,1.,1.,1.,1.,1.,1.,
1.,1.,1.,1.,1.,1.,1.,1.,1.,1.,1.,1.,1.,1.,1.,1.,1.,1.,1.,1.,1.,1.,1.,1.,
1.,1.,1.,1.,1.,1.,1.,1.,1.,1.,1.,1.,1.,1.,1.,1.,1.,1.,1.,1.,1.,1.,1.,1.,
1.,1.,1.,1.,1.,1.,1.,1.,1.,1.,1.,1.,1.,1.,1.,1.,1.,1.,1.,1.,1.,1.,1.,1.,
1.,1.,1.,1.,1.,1.,1.,1.,1.,1.,1.,1.,1.,1.,1.,1.,1.,1.,1.,1.,1.,1.,1.,1.,
1.,1.,1.,1.,1.,1.,1.,1.,1.,1.,1.,1.,1.,1.,1.,1.,1.,1.,1.,1.,1.,1.,1.,1.,
1.,1.,1.,1.,1.,1.,1.,1.,1.,1.,1.,1.,1.,1.,1.,1.,1.,1.,1.,1.,1.,1.,1.,1.,
1.,1.,1.,1.,1.,1.,1.,1.,1.,1.,1.,1.,1.,1.,1.,1.,1.,1.,1.,1.,1.,1.,1.,1.,
1.,1.,1.,1.,1.,1.,1.,1.,1.,1.))
REPRESENTATION_ITEM('')
);
#439=(
BOUNDED_CURVE()
B_SPLINE_CURVE(5,(#69161,#69162,#69163,#69164,#69165,#69166,#69167,#69168,
#69169,#69170,#69171,#69172,#69173,#69174,#69175,#69176,#69177,#69178,#69179,
#69180,#69181,#69182,#69183,#69184,#69185,#69186,#69187,#69188,#69189,#69190,
#69191,#69192,#69193,#69194,#69195,#69196,#69197,#69198,#69199,#69200,#69201,
#69202,#69203,#69204,#69205,#69206,#69207,#69208,#69209,#69210,#69211,#69212,
#69213,#69214,#69215,#69216,#69217,#69218,#69219,#69220,#69221,#69222,#69223,
#69224,#69225,#69226,#69227,#69228,#69229,#69230,#69231,#69232,#69233,#69234,
#69235,#69236,#69237,#69238,#69239,#69240,#69241,#69242,#69243,#69244,#69245,
#69246,#69247,#69248,#69249,#69250,#69251,#69252,#69253,#69254,#69255,#69256,
#69257,#69258,#69259,#69260,#69261,#69262,#69263,#69264,#69265,#69266,#69267,
#69268,#69269,#69270,#69271,#69272,#69273,#69274,#69275,#69276,#69277,#69278,
#69279,#69280,#69281,#69282,#69283,#69284,#69285,#69286,#69287,#69288,#69289,
#69290,#69291,#69292,#69293,#69294,#69295,#69296,#69297,#69298,#69299,#69300,
#69301,#69302,#69303,#69304,#69305,#69306,#69307,#69308,#69309,#69310,#69311,
#69312,#69313,#69314,#69315,#69316,#69317,#69318,#69319,#69320,#69321,#69322,
#69323,#69324,#69325,#69326,#69327,#69328,#69329,#69330,#69331,#69332,#69333,
#69334,#69335,#69336,#69337,#69338,#69339,#69340,#69341,#69342,#69343,#69344,
#69345,#69346,#69347,#69348,#69349,#69350,#69351,#69352,#69353,#69354),
 .UNSPECIFIED.,.F.,.F.)
B_SPLINE_CURVE_WITH_KNOTS((6,1,1,1,1,1,1,1,1,1,1,1,1,1,1,1,1,1,1,1,1,1,
1,1,1,1,1,1,1,1,1,1,1,1,1,1,1,1,1,1,1,1,1,1,1,1,1,1,1,1,1,1,1,1,1,1,1,1,
1,1,1,1,1,1,1,1,1,1,1,1,1,1,1,1,1,1,1,1,1,1,1,1,1,1,1,1,1,1,1,1,1,1,1,1,
1,1,1,1,1,1,1,1,1,1,1,1,1,1,1,1,1,1,1,1,1,1,1,1,1,1,1,1,1,1,1,1,1,1,1,1,
1,1,1,1,1,1,1,1,1,1,1,1,1,1,1,1,1,1,1,1,1,1,1,1,1,1,1,1,1,1,1,1,1,1,1,1,
1,1,1,1,1,1,1,1,1,1,1,1,1,1,1,1,1,1,1,1,1,1,1,6),(0.,0.005,0.01,0.015,0.02,
0.025,0.03,0.035,0.04,0.045,0.05,0.055,0.06,0.065,0.07,0.075,0.08,0.085,
0.09,0.095,0.1,0.105,0.11,0.115,0.12,0.125,0.13,0.135,0.14,0.145,0.15,0.155,
0.16,0.165,0.17,0.175,0.18,0.185,0.19,0.195,0.2,0.205,0.21,0.215,0.22,0.225,
0.23,0.235,0.24,0.245,0.25,0.255,0.26,0.265,0.27,0.275,0.28,0.285,0.29,
0.295,0.3,0.305,0.31,0.315,0.32,0.325,0.33,0.335,0.34,0.345,0.35,0.355,
0.36,0.365,0.37,0.375,0.38,0.385,0.39,0.395,0.4,0.405,0.41,0.415,0.42,0.425,
0.43,0.435,0.44,0.445,0.45,0.455,0.46,0.465,0.47,0.475,0.48,0.485,0.49,
0.495,0.5,0.505,0.51,0.515,0.52,0.525,0.53,0.535,0.54,0.545,0.55,0.555,
0.56,0.565,0.57,0.575,0.58,0.585,0.59,0.595,0.6,0.605,0.61,0.615,0.62,0.625,
0.63,0.635,0.64,0.645,0.65,0.655,0.66,0.665,0.67,0.675,0.68,0.685,0.690000000000001,
0.695000000000001,0.700000000000001,0.705000000000001,0.710000000000001,
0.715000000000001,0.720000000000001,0.725000000000001,0.730000000000001,
0.735000000000001,0.740000000000001,0.745000000000001,0.750000000000001,
0.755000000000001,0.760000000000001,0.765000000000001,0.770000000000001,
0.775000000000001,0.780000000000001,0.785000000000001,0.790000000000001,
0.795000000000001,0.800000000000001,0.805000000000001,0.810000000000001,
0.815000000000001,0.820000000000001,0.825000000000001,0.830000000000001,
0.835000000000001,0.840000000000001,0.845000000000001,0.850000000000001,
0.855000000000001,0.860000000000001,0.865000000000001,0.870000000000001,
0.875000000000001,0.880000000000001,0.885000000000001,0.890000000000001,
0.895000000000001,0.900000000000001,0.905000000000001,0.910000000000001,
0.915000000000001,0.920000000000001,0.925000000000001,0.930000000000001,
0.935000000000001,0.940000000000001,0.941429844431382),.UNSPECIFIED.)
CURVE()
GEOMETRIC_REPRESENTATION_ITEM()
RATIONAL_B_SPLINE_CURVE((1.,1.,1.,1.,1.,1.,1.,1.,1.,1.,1.,1.,1.,1.,1.,1.,
1.,1.,1.,1.,1.,1.,1.,1.,1.,1.,1.,1.,1.,1.,1.,1.,1.,1.,1.,1.,1.,1.,1.,1.,
1.,1.,1.,1.,1.,1.,1.,1.,1.,1.,1.,1.,1.,1.,1.,1.,1.,1.,1.,1.,1.,1.,1.,1.,
1.,1.,1.,1.,1.,1.,1.,1.,1.,1.,1.,1.,1.,1.,1.,1.,1.,1.,1.,1.,1.,1.,1.,1.,
1.,1.,1.,1.,1.,1.,1.,1.,1.,1.,1.,1.,1.,1.,1.,1.,1.,1.,1.,1.,1.,1.,1.,1.,
1.,1.,1.,1.,1.,1.,1.,1.,1.,1.,1.,1.,1.,1.,1.,1.,1.,1.,1.,1.,1.,1.,1.,1.,
1.,1.,1.,1.,1.,1.,1.,1.,1.,1.,1.,1.,1.,1.,1.,1.,1.,1.,1.,1.,1.,1.,1.,1.,
1.,1.,1.,1.,1.,1.,1.,1.,1.,1.,1.,1.,1.,1.,1.,1.,1.,1.,1.,1.,1.,1.,1.,1.,
1.,1.,1.,1.,1.,1.,1.,1.,1.,1.))
REPRESENTATION_ITEM('')
);
#440=(
BOUNDED_CURVE()
B_SPLINE_CURVE(5,(#69357,#69358,#69359,#69360,#69361,#69362,#69363,#69364,
#69365,#69366,#69367,#69368,#69369,#69370,#69371,#69372,#69373,#69374,#69375,
#69376,#69377,#69378,#69379,#69380,#69381,#69382,#69383,#69384,#69385,#69386,
#69387,#69388,#69389,#69390,#69391,#69392,#69393,#69394,#69395,#69396,#69397,
#69398,#69399,#69400,#69401,#69402,#69403,#69404,#69405,#69406,#69407,#69408,
#69409,#69410,#69411,#69412,#69413,#69414,#69415,#69416,#69417,#69418,#69419,
#69420,#69421,#69422,#69423,#69424,#69425,#69426,#69427,#69428,#69429,#69430,
#69431,#69432,#69433,#69434,#69435,#69436,#69437,#69438,#69439,#69440,#69441,
#69442,#69443,#69444,#69445,#69446,#69447,#69448,#69449,#69450,#69451,#69452,
#69453,#69454,#69455,#69456,#69457,#69458,#69459,#69460,#69461,#69462,#69463,
#69464,#69465,#69466,#69467,#69468,#69469,#69470,#69471,#69472,#69473,#69474,
#69475,#69476,#69477,#69478,#69479,#69480,#69481,#69482,#69483,#69484,#69485,
#69486,#69487,#69488,#69489,#69490,#69491,#69492,#69493,#69494,#69495,#69496,
#69497,#69498,#69499,#69500,#69501,#69502,#69503,#69504,#69505,#69506,#69507,
#69508,#69509,#69510,#69511,#69512,#69513,#69514,#69515,#69516,#69517,#69518,
#69519,#69520,#69521,#69522,#69523,#69524,#69525,#69526,#69527,#69528,#69529,
#69530,#69531,#69532,#69533,#69534,#69535,#69536,#69537,#69538,#69539,#69540,
#69541,#69542,#69543,#69544,#69545,#69546,#69547,#69548,#69549,#69550),
 .UNSPECIFIED.,.F.,.F.)
B_SPLINE_CURVE_WITH_KNOTS((6,1,1,1,1,1,1,1,1,1,1,1,1,1,1,1,1,1,1,1,1,1,
1,1,1,1,1,1,1,1,1,1,1,1,1,1,1,1,1,1,1,1,1,1,1,1,1,1,1,1,1,1,1,1,1,1,1,1,
1,1,1,1,1,1,1,1,1,1,1,1,1,1,1,1,1,1,1,1,1,1,1,1,1,1,1,1,1,1,1,1,1,1,1,1,
1,1,1,1,1,1,1,1,1,1,1,1,1,1,1,1,1,1,1,1,1,1,1,1,1,1,1,1,1,1,1,1,1,1,1,1,
1,1,1,1,1,1,1,1,1,1,1,1,1,1,1,1,1,1,1,1,1,1,1,1,1,1,1,1,1,1,1,1,1,1,1,1,
1,1,1,1,1,1,1,1,1,1,1,1,1,1,1,1,1,1,1,1,1,1,1,6),(-0.941429844431382,-0.940000000000001,
-0.935000000000001,-0.930000000000001,-0.925000000000001,-0.920000000000001,
-0.915000000000001,-0.910000000000001,-0.905000000000001,-0.900000000000001,
-0.895000000000001,-0.890000000000001,-0.885000000000001,-0.880000000000001,
-0.875000000000001,-0.870000000000001,-0.865000000000001,-0.860000000000001,
-0.855000000000001,-0.850000000000001,-0.845000000000001,-0.840000000000001,
-0.835000000000001,-0.830000000000001,-0.825000000000001,-0.820000000000001,
-0.815000000000001,-0.810000000000001,-0.805000000000001,-0.800000000000001,
-0.795000000000001,-0.790000000000001,-0.785000000000001,-0.780000000000001,
-0.775000000000001,-0.770000000000001,-0.765000000000001,-0.760000000000001,
-0.755000000000001,-0.750000000000001,-0.745000000000001,-0.740000000000001,
-0.735000000000001,-0.730000000000001,-0.725000000000001,-0.720000000000001,
-0.715000000000001,-0.710000000000001,-0.705000000000001,-0.700000000000001,
-0.695000000000001,-0.690000000000001,-0.685,-0.68,-0.675,-0.67,-0.665,
-0.66,-0.655,-0.65,-0.645,-0.64,-0.635,-0.63,-0.625,-0.62,-0.615,-0.61,
-0.605,-0.6,-0.595,-0.59,-0.585,-0.58,-0.575,-0.57,-0.565,-0.56,-0.555,
-0.55,-0.545,-0.54,-0.535,-0.53,-0.525,-0.52,-0.515,-0.51,-0.505,-0.5,-0.495,
-0.49,-0.485,-0.48,-0.475,-0.47,-0.465,-0.46,-0.455,-0.45,-0.445,-0.44,
-0.435,-0.43,-0.425,-0.42,-0.415,-0.41,-0.405,-0.4,-0.395,-0.39,-0.385,
-0.38,-0.375,-0.37,-0.365,-0.36,-0.355,-0.35,-0.345,-0.34,-0.335,-0.33,
-0.325,-0.32,-0.315,-0.31,-0.305,-0.3,-0.295,-0.29,-0.285,-0.28,-0.275,
-0.27,-0.265,-0.26,-0.255,-0.25,-0.245,-0.24,-0.235,-0.23,-0.225,-0.22,
-0.215,-0.21,-0.205,-0.2,-0.195,-0.19,-0.185,-0.18,-0.175,-0.17,-0.165,
-0.16,-0.155,-0.15,-0.145,-0.14,-0.135,-0.13,-0.125,-0.12,-0.115,-0.11,
-0.105,-0.1,-0.095,-0.09,-0.085,-0.08,-0.075,-0.07,-0.065,-0.06,-0.055,
-0.05,-0.045,-0.04,-0.035,-0.03,-0.025,-0.02,-0.015,-0.01,-0.005,0.),
 .UNSPECIFIED.)
CURVE()
GEOMETRIC_REPRESENTATION_ITEM()
RATIONAL_B_SPLINE_CURVE((1.,1.,1.,1.,1.,1.,1.,1.,1.,1.,1.,1.,1.,1.,1.,1.,
1.,1.,1.,1.,1.,1.,1.,1.,1.,1.,1.,1.,1.,1.,1.,1.,1.,1.,1.,1.,1.,1.,1.,1.,
1.,1.,1.,1.,1.,1.,1.,1.,1.,1.,1.,1.,1.,1.,1.,1.,1.,1.,1.,1.,1.,1.,1.,1.,
1.,1.,1.,1.,1.,1.,1.,1.,1.,1.,1.,1.,1.,1.,1.,1.,1.,1.,1.,1.,1.,1.,1.,1.,
1.,1.,1.,1.,1.,1.,1.,1.,1.,1.,1.,1.,1.,1.,1.,1.,1.,1.,1.,1.,1.,1.,1.,1.,
1.,1.,1.,1.,1.,1.,1.,1.,1.,1.,1.,1.,1.,1.,1.,1.,1.,1.,1.,1.,1.,1.,1.,1.,
1.,1.,1.,1.,1.,1.,1.,1.,1.,1.,1.,1.,1.,1.,1.,1.,1.,1.,1.,1.,1.,1.,1.,1.,
1.,1.,1.,1.,1.,1.,1.,1.,1.,1.,1.,1.,1.,1.,1.,1.,1.,1.,1.,1.,1.,1.,1.,1.,
1.,1.,1.,1.,1.,1.,1.,1.,1.,1.))
REPRESENTATION_ITEM('')
);
#441=(
BOUNDED_CURVE()
B_SPLINE_CURVE(5,(#70057,#70058,#70059,#70060,#70061,#70062,#70063,#70064,
#70065,#70066,#70067,#70068,#70069,#70070,#70071,#70072,#70073,#70074,#70075,
#70076,#70077,#70078,#70079,#70080,#70081,#70082,#70083,#70084,#70085,#70086,
#70087,#70088,#70089,#70090,#70091,#70092,#70093,#70094,#70095,#70096,#70097,
#70098,#70099,#70100,#70101,#70102,#70103,#70104,#70105,#70106,#70107,#70108,
#70109,#70110,#70111,#70112,#70113,#70114,#70115,#70116,#70117,#70118,#70119,
#70120,#70121,#70122,#70123,#70124,#70125,#70126,#70127,#70128,#70129,#70130,
#70131,#70132,#70133,#70134,#70135,#70136,#70137,#70138,#70139,#70140,#70141,
#70142,#70143,#70144,#70145,#70146,#70147,#70148,#70149,#70150,#70151,#70152,
#70153,#70154,#70155,#70156,#70157,#70158,#70159,#70160,#70161,#70162,#70163,
#70164,#70165,#70166,#70167,#70168,#70169,#70170,#70171,#70172,#70173,#70174,
#70175,#70176,#70177,#70178,#70179,#70180,#70181,#70182,#70183,#70184,#70185,
#70186,#70187,#70188,#70189,#70190,#70191,#70192,#70193,#70194,#70195,#70196,
#70197,#70198,#70199,#70200,#70201,#70202,#70203,#70204,#70205,#70206,#70207,
#70208,#70209,#70210,#70211,#70212,#70213,#70214,#70215,#70216,#70217,#70218,
#70219,#70220,#70221,#70222,#70223,#70224,#70225,#70226,#70227,#70228,#70229,
#70230,#70231,#70232,#70233,#70234,#70235,#70236,#70237,#70238,#70239,#70240,
#70241,#70242,#70243,#70244,#70245,#70246,#70247,#70248,#70249,#70250),
 .UNSPECIFIED.,.F.,.F.)
B_SPLINE_CURVE_WITH_KNOTS((6,1,1,1,1,1,1,1,1,1,1,1,1,1,1,1,1,1,1,1,1,1,
1,1,1,1,1,1,1,1,1,1,1,1,1,1,1,1,1,1,1,1,1,1,1,1,1,1,1,1,1,1,1,1,1,1,1,1,
1,1,1,1,1,1,1,1,1,1,1,1,1,1,1,1,1,1,1,1,1,1,1,1,1,1,1,1,1,1,1,1,1,1,1,1,
1,1,1,1,1,1,1,1,1,1,1,1,1,1,1,1,1,1,1,1,1,1,1,1,1,1,1,1,1,1,1,1,1,1,1,1,
1,1,1,1,1,1,1,1,1,1,1,1,1,1,1,1,1,1,1,1,1,1,1,1,1,1,1,1,1,1,1,1,1,1,1,1,
1,1,1,1,1,1,1,1,1,1,1,1,1,1,1,1,1,1,1,1,1,1,1,6),(0.,0.005,0.01,0.015,0.02,
0.025,0.03,0.035,0.04,0.045,0.05,0.055,0.06,0.065,0.07,0.075,0.08,0.085,
0.09,0.095,0.1,0.105,0.11,0.115,0.12,0.125,0.13,0.135,0.14,0.145,0.15,0.155,
0.16,0.165,0.17,0.175,0.18,0.185,0.19,0.195,0.2,0.205,0.21,0.215,0.22,0.225,
0.23,0.235,0.24,0.245,0.25,0.255,0.26,0.265,0.27,0.275,0.28,0.285,0.29,
0.295,0.3,0.305,0.31,0.315,0.32,0.325,0.33,0.335,0.34,0.345,0.35,0.355,
0.36,0.365,0.37,0.375,0.38,0.385,0.39,0.395,0.4,0.405,0.41,0.415,0.42,0.425,
0.43,0.435,0.44,0.445,0.45,0.455,0.46,0.465,0.47,0.475,0.48,0.485,0.49,
0.495,0.5,0.505,0.51,0.515,0.52,0.525,0.53,0.535,0.54,0.545,0.55,0.555,
0.56,0.565,0.57,0.575,0.58,0.585,0.59,0.595,0.6,0.605,0.61,0.615,0.62,0.625,
0.63,0.635,0.64,0.645,0.65,0.655,0.66,0.665,0.67,0.675,0.68,0.685,0.690000000000001,
0.695000000000001,0.700000000000001,0.705000000000001,0.710000000000001,
0.715000000000001,0.720000000000001,0.725000000000001,0.730000000000001,
0.735000000000001,0.740000000000001,0.745000000000001,0.750000000000001,
0.755000000000001,0.760000000000001,0.765000000000001,0.770000000000001,
0.775000000000001,0.780000000000001,0.785000000000001,0.790000000000001,
0.795000000000001,0.800000000000001,0.805000000000001,0.810000000000001,
0.815000000000001,0.820000000000001,0.825000000000001,0.830000000000001,
0.835000000000001,0.840000000000001,0.845000000000001,0.850000000000001,
0.855000000000001,0.860000000000001,0.865000000000001,0.870000000000001,
0.875000000000001,0.880000000000001,0.885000000000001,0.890000000000001,
0.895000000000001,0.900000000000001,0.905000000000001,0.910000000000001,
0.915000000000001,0.920000000000001,0.925000000000001,0.930000000000001,
0.935000000000001,0.940000000000001,0.941429844431395),.UNSPECIFIED.)
CURVE()
GEOMETRIC_REPRESENTATION_ITEM()
RATIONAL_B_SPLINE_CURVE((1.,1.,1.,1.,1.,1.,1.,1.,1.,1.,1.,1.,1.,1.,1.,1.,
1.,1.,1.,1.,1.,1.,1.,1.,1.,1.,1.,1.,1.,1.,1.,1.,1.,1.,1.,1.,1.,1.,1.,1.,
1.,1.,1.,1.,1.,1.,1.,1.,1.,1.,1.,1.,1.,1.,1.,1.,1.,1.,1.,1.,1.,1.,1.,1.,
1.,1.,1.,1.,1.,1.,1.,1.,1.,1.,1.,1.,1.,1.,1.,1.,1.,1.,1.,1.,1.,1.,1.,1.,
1.,1.,1.,1.,1.,1.,1.,1.,1.,1.,1.,1.,1.,1.,1.,1.,1.,1.,1.,1.,1.,1.,1.,1.,
1.,1.,1.,1.,1.,1.,1.,1.,1.,1.,1.,1.,1.,1.,1.,1.,1.,1.,1.,1.,1.,1.,1.,1.,
1.,1.,1.,1.,1.,1.,1.,1.,1.,1.,1.,1.,1.,1.,1.,1.,1.,1.,1.,1.,1.,1.,1.,1.,
1.,1.,1.,1.,1.,1.,1.,1.,1.,1.,1.,1.,1.,1.,1.,1.,1.,1.,1.,1.,1.,1.,1.,1.,
1.,1.,1.,1.,1.,1.,1.,1.,1.,1.))
REPRESENTATION_ITEM('')
);
#442=(
BOUNDED_CURVE()
B_SPLINE_CURVE(5,(#70253,#70254,#70255,#70256,#70257,#70258,#70259,#70260,
#70261,#70262,#70263,#70264,#70265,#70266,#70267,#70268,#70269,#70270,#70271,
#70272,#70273,#70274,#70275,#70276,#70277,#70278,#70279,#70280,#70281,#70282,
#70283,#70284,#70285,#70286,#70287,#70288,#70289,#70290,#70291,#70292,#70293,
#70294,#70295,#70296,#70297,#70298,#70299,#70300,#70301,#70302,#70303,#70304,
#70305,#70306,#70307,#70308,#70309,#70310,#70311,#70312,#70313,#70314,#70315,
#70316,#70317,#70318,#70319,#70320,#70321,#70322,#70323,#70324,#70325,#70326,
#70327,#70328,#70329,#70330,#70331,#70332,#70333,#70334,#70335,#70336,#70337,
#70338,#70339,#70340,#70341,#70342,#70343,#70344,#70345,#70346,#70347,#70348,
#70349,#70350,#70351,#70352,#70353,#70354,#70355,#70356,#70357,#70358,#70359,
#70360,#70361,#70362,#70363,#70364,#70365,#70366,#70367,#70368,#70369,#70370,
#70371,#70372,#70373,#70374,#70375,#70376,#70377,#70378,#70379,#70380,#70381,
#70382,#70383,#70384,#70385,#70386,#70387,#70388,#70389,#70390,#70391,#70392,
#70393,#70394,#70395,#70396,#70397,#70398,#70399,#70400,#70401,#70402,#70403,
#70404,#70405,#70406,#70407,#70408,#70409,#70410,#70411,#70412,#70413,#70414,
#70415,#70416,#70417,#70418,#70419,#70420,#70421,#70422,#70423,#70424,#70425,
#70426,#70427,#70428,#70429,#70430,#70431,#70432,#70433,#70434,#70435,#70436,
#70437,#70438,#70439,#70440,#70441,#70442,#70443,#70444,#70445,#70446),
 .UNSPECIFIED.,.F.,.F.)
B_SPLINE_CURVE_WITH_KNOTS((6,1,1,1,1,1,1,1,1,1,1,1,1,1,1,1,1,1,1,1,1,1,
1,1,1,1,1,1,1,1,1,1,1,1,1,1,1,1,1,1,1,1,1,1,1,1,1,1,1,1,1,1,1,1,1,1,1,1,
1,1,1,1,1,1,1,1,1,1,1,1,1,1,1,1,1,1,1,1,1,1,1,1,1,1,1,1,1,1,1,1,1,1,1,1,
1,1,1,1,1,1,1,1,1,1,1,1,1,1,1,1,1,1,1,1,1,1,1,1,1,1,1,1,1,1,1,1,1,1,1,1,
1,1,1,1,1,1,1,1,1,1,1,1,1,1,1,1,1,1,1,1,1,1,1,1,1,1,1,1,1,1,1,1,1,1,1,1,
1,1,1,1,1,1,1,1,1,1,1,1,1,1,1,1,1,1,1,1,1,1,1,6),(-0.941429844431395,-0.940000000000001,
-0.935000000000001,-0.930000000000001,-0.925000000000001,-0.920000000000001,
-0.915000000000001,-0.910000000000001,-0.905000000000001,-0.900000000000001,
-0.895000000000001,-0.890000000000001,-0.885000000000001,-0.880000000000001,
-0.875000000000001,-0.870000000000001,-0.865000000000001,-0.860000000000001,
-0.855000000000001,-0.850000000000001,-0.845000000000001,-0.840000000000001,
-0.835000000000001,-0.830000000000001,-0.825000000000001,-0.820000000000001,
-0.815000000000001,-0.810000000000001,-0.805000000000001,-0.800000000000001,
-0.795000000000001,-0.790000000000001,-0.785000000000001,-0.780000000000001,
-0.775000000000001,-0.770000000000001,-0.765000000000001,-0.760000000000001,
-0.755000000000001,-0.750000000000001,-0.745000000000001,-0.740000000000001,
-0.735000000000001,-0.730000000000001,-0.725000000000001,-0.720000000000001,
-0.715000000000001,-0.710000000000001,-0.705000000000001,-0.700000000000001,
-0.695000000000001,-0.690000000000001,-0.685,-0.68,-0.675,-0.67,-0.665,
-0.66,-0.655,-0.65,-0.645,-0.64,-0.635,-0.63,-0.625,-0.62,-0.615,-0.61,
-0.605,-0.6,-0.595,-0.59,-0.585,-0.58,-0.575,-0.57,-0.565,-0.56,-0.555,
-0.55,-0.545,-0.54,-0.535,-0.53,-0.525,-0.52,-0.515,-0.51,-0.505,-0.5,-0.495,
-0.49,-0.485,-0.48,-0.475,-0.47,-0.465,-0.46,-0.455,-0.45,-0.445,-0.44,
-0.435,-0.43,-0.425,-0.42,-0.415,-0.41,-0.405,-0.4,-0.395,-0.39,-0.385,
-0.38,-0.375,-0.37,-0.365,-0.36,-0.355,-0.35,-0.345,-0.34,-0.335,-0.33,
-0.325,-0.32,-0.315,-0.31,-0.305,-0.3,-0.295,-0.29,-0.285,-0.28,-0.275,
-0.27,-0.265,-0.26,-0.255,-0.25,-0.245,-0.24,-0.235,-0.23,-0.225,-0.22,
-0.215,-0.21,-0.205,-0.2,-0.195,-0.19,-0.185,-0.18,-0.175,-0.17,-0.165,
-0.16,-0.155,-0.15,-0.145,-0.14,-0.135,-0.13,-0.125,-0.12,-0.115,-0.11,
-0.105,-0.1,-0.095,-0.09,-0.085,-0.08,-0.075,-0.07,-0.065,-0.06,-0.055,
-0.05,-0.045,-0.04,-0.035,-0.03,-0.025,-0.02,-0.015,-0.01,-0.005,0.),
 .UNSPECIFIED.)
CURVE()
GEOMETRIC_REPRESENTATION_ITEM()
RATIONAL_B_SPLINE_CURVE((1.,1.,1.,1.,1.,1.,1.,1.,1.,1.,1.,1.,1.,1.,1.,1.,
1.,1.,1.,1.,1.,1.,1.,1.,1.,1.,1.,1.,1.,1.,1.,1.,1.,1.,1.,1.,1.,1.,1.,1.,
1.,1.,1.,1.,1.,1.,1.,1.,1.,1.,1.,1.,1.,1.,1.,1.,1.,1.,1.,1.,1.,1.,1.,1.,
1.,1.,1.,1.,1.,1.,1.,1.,1.,1.,1.,1.,1.,1.,1.,1.,1.,1.,1.,1.,1.,1.,1.,1.,
1.,1.,1.,1.,1.,1.,1.,1.,1.,1.,1.,1.,1.,1.,1.,1.,1.,1.,1.,1.,1.,1.,1.,1.,
1.,1.,1.,1.,1.,1.,1.,1.,1.,1.,1.,1.,1.,1.,1.,1.,1.,1.,1.,1.,1.,1.,1.,1.,
1.,1.,1.,1.,1.,1.,1.,1.,1.,1.,1.,1.,1.,1.,1.,1.,1.,1.,1.,1.,1.,1.,1.,1.,
1.,1.,1.,1.,1.,1.,1.,1.,1.,1.,1.,1.,1.,1.,1.,1.,1.,1.,1.,1.,1.,1.,1.,1.,
1.,1.,1.,1.,1.,1.,1.,1.,1.,1.))
REPRESENTATION_ITEM('')
);
#443=(
BOUNDED_CURVE()
B_SPLINE_CURVE(5,(#70953,#70954,#70955,#70956,#70957,#70958,#70959,#70960,
#70961,#70962,#70963,#70964,#70965,#70966,#70967,#70968,#70969,#70970,#70971,
#70972,#70973,#70974,#70975,#70976,#70977,#70978,#70979,#70980,#70981,#70982,
#70983,#70984,#70985,#70986,#70987,#70988,#70989,#70990,#70991,#70992,#70993,
#70994,#70995,#70996,#70997,#70998,#70999,#71000,#71001,#71002,#71003,#71004,
#71005,#71006,#71007,#71008,#71009,#71010,#71011,#71012,#71013,#71014,#71015,
#71016,#71017,#71018,#71019,#71020,#71021,#71022,#71023,#71024,#71025,#71026,
#71027,#71028,#71029,#71030,#71031,#71032,#71033,#71034,#71035,#71036,#71037,
#71038,#71039,#71040,#71041,#71042,#71043,#71044,#71045,#71046,#71047,#71048,
#71049,#71050,#71051,#71052,#71053,#71054,#71055,#71056,#71057,#71058,#71059,
#71060,#71061,#71062,#71063,#71064,#71065,#71066,#71067,#71068,#71069,#71070,
#71071,#71072,#71073,#71074,#71075,#71076,#71077,#71078,#71079,#71080,#71081,
#71082,#71083,#71084,#71085,#71086,#71087,#71088,#71089,#71090,#71091,#71092,
#71093,#71094,#71095,#71096,#71097,#71098,#71099,#71100,#71101,#71102,#71103,
#71104,#71105,#71106,#71107,#71108,#71109,#71110,#71111,#71112,#71113,#71114,
#71115,#71116,#71117,#71118,#71119,#71120,#71121,#71122,#71123,#71124,#71125,
#71126,#71127,#71128,#71129,#71130,#71131,#71132,#71133,#71134,#71135,#71136,
#71137,#71138,#71139,#71140,#71141,#71142,#71143,#71144,#71145,#71146),
 .UNSPECIFIED.,.F.,.F.)
B_SPLINE_CURVE_WITH_KNOTS((6,1,1,1,1,1,1,1,1,1,1,1,1,1,1,1,1,1,1,1,1,1,
1,1,1,1,1,1,1,1,1,1,1,1,1,1,1,1,1,1,1,1,1,1,1,1,1,1,1,1,1,1,1,1,1,1,1,1,
1,1,1,1,1,1,1,1,1,1,1,1,1,1,1,1,1,1,1,1,1,1,1,1,1,1,1,1,1,1,1,1,1,1,1,1,
1,1,1,1,1,1,1,1,1,1,1,1,1,1,1,1,1,1,1,1,1,1,1,1,1,1,1,1,1,1,1,1,1,1,1,1,
1,1,1,1,1,1,1,1,1,1,1,1,1,1,1,1,1,1,1,1,1,1,1,1,1,1,1,1,1,1,1,1,1,1,1,1,
1,1,1,1,1,1,1,1,1,1,1,1,1,1,1,1,1,1,1,1,1,1,1,6),(0.,0.005,0.01,0.015,0.02,
0.025,0.03,0.035,0.04,0.045,0.05,0.055,0.06,0.065,0.07,0.075,0.08,0.085,
0.09,0.095,0.1,0.105,0.11,0.115,0.12,0.125,0.13,0.135,0.14,0.145,0.15,0.155,
0.16,0.165,0.17,0.175,0.18,0.185,0.19,0.195,0.2,0.205,0.21,0.215,0.22,0.225,
0.23,0.235,0.24,0.245,0.25,0.255,0.26,0.265,0.27,0.275,0.28,0.285,0.29,
0.295,0.3,0.305,0.31,0.315,0.32,0.325,0.33,0.335,0.34,0.345,0.35,0.355,
0.36,0.365,0.37,0.375,0.38,0.385,0.39,0.395,0.4,0.405,0.41,0.415,0.42,0.425,
0.43,0.435,0.44,0.445,0.45,0.455,0.46,0.465,0.47,0.475,0.48,0.485,0.49,
0.495,0.5,0.505,0.51,0.515,0.52,0.525,0.53,0.535,0.54,0.545,0.55,0.555,
0.56,0.565,0.57,0.575,0.58,0.585,0.59,0.595,0.6,0.605,0.61,0.615,0.62,0.625,
0.63,0.635,0.64,0.645,0.65,0.655,0.66,0.665,0.67,0.675,0.68,0.685,0.690000000000001,
0.695000000000001,0.700000000000001,0.705000000000001,0.710000000000001,
0.715000000000001,0.720000000000001,0.725000000000001,0.730000000000001,
0.735000000000001,0.740000000000001,0.745000000000001,0.750000000000001,
0.755000000000001,0.760000000000001,0.765000000000001,0.770000000000001,
0.775000000000001,0.780000000000001,0.785000000000001,0.790000000000001,
0.795000000000001,0.800000000000001,0.805000000000001,0.810000000000001,
0.815000000000001,0.820000000000001,0.825000000000001,0.830000000000001,
0.835000000000001,0.840000000000001,0.845000000000001,0.850000000000001,
0.855000000000001,0.860000000000001,0.865000000000001,0.870000000000001,
0.875000000000001,0.880000000000001,0.885000000000001,0.890000000000001,
0.895000000000001,0.900000000000001,0.905000000000001,0.910000000000001,
0.915000000000001,0.920000000000001,0.925000000000001,0.930000000000001,
0.935000000000001,0.940000000000001,0.941429844431403),.UNSPECIFIED.)
CURVE()
GEOMETRIC_REPRESENTATION_ITEM()
RATIONAL_B_SPLINE_CURVE((1.,1.,1.,1.,1.,1.,1.,1.,1.,1.,1.,1.,1.,1.,1.,1.,
1.,1.,1.,1.,1.,1.,1.,1.,1.,1.,1.,1.,1.,1.,1.,1.,1.,1.,1.,1.,1.,1.,1.,1.,
1.,1.,1.,1.,1.,1.,1.,1.,1.,1.,1.,1.,1.,1.,1.,1.,1.,1.,1.,1.,1.,1.,1.,1.,
1.,1.,1.,1.,1.,1.,1.,1.,1.,1.,1.,1.,1.,1.,1.,1.,1.,1.,1.,1.,1.,1.,1.,1.,
1.,1.,1.,1.,1.,1.,1.,1.,1.,1.,1.,1.,1.,1.,1.,1.,1.,1.,1.,1.,1.,1.,1.,1.,
1.,1.,1.,1.,1.,1.,1.,1.,1.,1.,1.,1.,1.,1.,1.,1.,1.,1.,1.,1.,1.,1.,1.,1.,
1.,1.,1.,1.,1.,1.,1.,1.,1.,1.,1.,1.,1.,1.,1.,1.,1.,1.,1.,1.,1.,1.,1.,1.,
1.,1.,1.,1.,1.,1.,1.,1.,1.,1.,1.,1.,1.,1.,1.,1.,1.,1.,1.,1.,1.,1.,1.,1.,
1.,1.,1.,1.,1.,1.,1.,1.,1.,1.))
REPRESENTATION_ITEM('')
);
#444=(
BOUNDED_CURVE()
B_SPLINE_CURVE(5,(#71149,#71150,#71151,#71152,#71153,#71154,#71155,#71156,
#71157,#71158,#71159,#71160,#71161,#71162,#71163,#71164,#71165,#71166,#71167,
#71168,#71169,#71170,#71171,#71172,#71173,#71174,#71175,#71176,#71177,#71178,
#71179,#71180,#71181,#71182,#71183,#71184,#71185,#71186,#71187,#71188,#71189,
#71190,#71191,#71192,#71193,#71194,#71195,#71196,#71197,#71198,#71199,#71200,
#71201,#71202,#71203,#71204,#71205,#71206,#71207,#71208,#71209,#71210,#71211,
#71212,#71213,#71214,#71215,#71216,#71217,#71218,#71219,#71220,#71221,#71222,
#71223,#71224,#71225,#71226,#71227,#71228,#71229,#71230,#71231,#71232,#71233,
#71234,#71235,#71236,#71237,#71238,#71239,#71240,#71241,#71242,#71243,#71244,
#71245,#71246,#71247,#71248,#71249,#71250,#71251,#71252,#71253,#71254,#71255,
#71256,#71257,#71258,#71259,#71260,#71261,#71262,#71263,#71264,#71265,#71266,
#71267,#71268,#71269,#71270,#71271,#71272,#71273,#71274,#71275,#71276,#71277,
#71278,#71279,#71280,#71281,#71282,#71283,#71284,#71285,#71286,#71287,#71288,
#71289,#71290,#71291,#71292,#71293,#71294,#71295,#71296,#71297,#71298,#71299,
#71300,#71301,#71302,#71303,#71304,#71305,#71306,#71307,#71308,#71309,#71310,
#71311,#71312,#71313,#71314,#71315,#71316,#71317,#71318,#71319,#71320,#71321,
#71322,#71323,#71324,#71325,#71326,#71327,#71328,#71329,#71330,#71331,#71332,
#71333,#71334,#71335,#71336,#71337,#71338,#71339,#71340,#71341,#71342),
 .UNSPECIFIED.,.F.,.F.)
B_SPLINE_CURVE_WITH_KNOTS((6,1,1,1,1,1,1,1,1,1,1,1,1,1,1,1,1,1,1,1,1,1,
1,1,1,1,1,1,1,1,1,1,1,1,1,1,1,1,1,1,1,1,1,1,1,1,1,1,1,1,1,1,1,1,1,1,1,1,
1,1,1,1,1,1,1,1,1,1,1,1,1,1,1,1,1,1,1,1,1,1,1,1,1,1,1,1,1,1,1,1,1,1,1,1,
1,1,1,1,1,1,1,1,1,1,1,1,1,1,1,1,1,1,1,1,1,1,1,1,1,1,1,1,1,1,1,1,1,1,1,1,
1,1,1,1,1,1,1,1,1,1,1,1,1,1,1,1,1,1,1,1,1,1,1,1,1,1,1,1,1,1,1,1,1,1,1,1,
1,1,1,1,1,1,1,1,1,1,1,1,1,1,1,1,1,1,1,1,1,1,1,6),(-0.941429844431403,-0.940000000000001,
-0.935000000000001,-0.930000000000001,-0.925000000000001,-0.920000000000001,
-0.915000000000001,-0.910000000000001,-0.905000000000001,-0.900000000000001,
-0.895000000000001,-0.890000000000001,-0.885000000000001,-0.880000000000001,
-0.875000000000001,-0.870000000000001,-0.865000000000001,-0.860000000000001,
-0.855000000000001,-0.850000000000001,-0.845000000000001,-0.840000000000001,
-0.835000000000001,-0.830000000000001,-0.825000000000001,-0.820000000000001,
-0.815000000000001,-0.810000000000001,-0.805000000000001,-0.800000000000001,
-0.795000000000001,-0.790000000000001,-0.785000000000001,-0.780000000000001,
-0.775000000000001,-0.770000000000001,-0.765000000000001,-0.760000000000001,
-0.755000000000001,-0.750000000000001,-0.745000000000001,-0.740000000000001,
-0.735000000000001,-0.730000000000001,-0.725000000000001,-0.720000000000001,
-0.715000000000001,-0.710000000000001,-0.705000000000001,-0.700000000000001,
-0.695000000000001,-0.690000000000001,-0.685,-0.68,-0.675,-0.67,-0.665,
-0.66,-0.655,-0.65,-0.645,-0.64,-0.635,-0.63,-0.625,-0.62,-0.615,-0.61,
-0.605,-0.6,-0.595,-0.59,-0.585,-0.58,-0.575,-0.57,-0.565,-0.56,-0.555,
-0.55,-0.545,-0.54,-0.535,-0.53,-0.525,-0.52,-0.515,-0.51,-0.505,-0.5,-0.495,
-0.49,-0.485,-0.48,-0.475,-0.47,-0.465,-0.46,-0.455,-0.45,-0.445,-0.44,
-0.435,-0.43,-0.425,-0.42,-0.415,-0.41,-0.405,-0.4,-0.395,-0.39,-0.385,
-0.38,-0.375,-0.37,-0.365,-0.36,-0.355,-0.35,-0.345,-0.34,-0.335,-0.33,
-0.325,-0.32,-0.315,-0.31,-0.305,-0.3,-0.295,-0.29,-0.285,-0.28,-0.275,
-0.27,-0.265,-0.26,-0.255,-0.25,-0.245,-0.24,-0.235,-0.23,-0.225,-0.22,
-0.215,-0.21,-0.205,-0.2,-0.195,-0.19,-0.185,-0.18,-0.175,-0.17,-0.165,
-0.16,-0.155,-0.15,-0.145,-0.14,-0.135,-0.13,-0.125,-0.12,-0.115,-0.11,
-0.105,-0.1,-0.095,-0.09,-0.085,-0.08,-0.075,-0.07,-0.065,-0.06,-0.055,
-0.05,-0.045,-0.04,-0.035,-0.03,-0.025,-0.02,-0.015,-0.01,-0.005,0.),
 .UNSPECIFIED.)
CURVE()
GEOMETRIC_REPRESENTATION_ITEM()
RATIONAL_B_SPLINE_CURVE((1.,1.,1.,1.,1.,1.,1.,1.,1.,1.,1.,1.,1.,1.,1.,1.,
1.,1.,1.,1.,1.,1.,1.,1.,1.,1.,1.,1.,1.,1.,1.,1.,1.,1.,1.,1.,1.,1.,1.,1.,
1.,1.,1.,1.,1.,1.,1.,1.,1.,1.,1.,1.,1.,1.,1.,1.,1.,1.,1.,1.,1.,1.,1.,1.,
1.,1.,1.,1.,1.,1.,1.,1.,1.,1.,1.,1.,1.,1.,1.,1.,1.,1.,1.,1.,1.,1.,1.,1.,
1.,1.,1.,1.,1.,1.,1.,1.,1.,1.,1.,1.,1.,1.,1.,1.,1.,1.,1.,1.,1.,1.,1.,1.,
1.,1.,1.,1.,1.,1.,1.,1.,1.,1.,1.,1.,1.,1.,1.,1.,1.,1.,1.,1.,1.,1.,1.,1.,
1.,1.,1.,1.,1.,1.,1.,1.,1.,1.,1.,1.,1.,1.,1.,1.,1.,1.,1.,1.,1.,1.,1.,1.,
1.,1.,1.,1.,1.,1.,1.,1.,1.,1.,1.,1.,1.,1.,1.,1.,1.,1.,1.,1.,1.,1.,1.,1.,
1.,1.,1.,1.,1.,1.,1.,1.,1.,1.))
REPRESENTATION_ITEM('')
);
#445=(
BOUNDED_CURVE()
B_SPLINE_CURVE(5,(#71849,#71850,#71851,#71852,#71853,#71854,#71855,#71856,
#71857,#71858,#71859,#71860,#71861,#71862,#71863,#71864,#71865,#71866,#71867,
#71868,#71869,#71870,#71871,#71872,#71873,#71874,#71875,#71876,#71877,#71878,
#71879,#71880,#71881,#71882,#71883,#71884,#71885,#71886,#71887,#71888,#71889,
#71890,#71891,#71892,#71893,#71894,#71895,#71896,#71897,#71898,#71899,#71900,
#71901,#71902,#71903,#71904,#71905,#71906,#71907,#71908,#71909,#71910,#71911,
#71912,#71913,#71914,#71915,#71916,#71917,#71918,#71919,#71920,#71921,#71922,
#71923,#71924,#71925,#71926,#71927,#71928,#71929,#71930,#71931,#71932,#71933,
#71934,#71935,#71936,#71937,#71938,#71939,#71940,#71941,#71942,#71943,#71944,
#71945,#71946,#71947,#71948,#71949,#71950,#71951,#71952,#71953,#71954,#71955,
#71956,#71957,#71958,#71959,#71960,#71961,#71962,#71963,#71964,#71965,#71966,
#71967,#71968,#71969,#71970,#71971,#71972,#71973,#71974,#71975,#71976,#71977,
#71978,#71979,#71980,#71981,#71982,#71983,#71984,#71985,#71986,#71987,#71988,
#71989,#71990,#71991,#71992,#71993,#71994,#71995,#71996,#71997,#71998,#71999,
#72000,#72001,#72002,#72003,#72004,#72005,#72006,#72007,#72008,#72009,#72010,
#72011,#72012,#72013,#72014,#72015,#72016,#72017,#72018,#72019,#72020,#72021,
#72022,#72023,#72024,#72025,#72026,#72027,#72028,#72029,#72030,#72031,#72032,
#72033,#72034,#72035,#72036,#72037,#72038,#72039,#72040,#72041,#72042),
 .UNSPECIFIED.,.F.,.F.)
B_SPLINE_CURVE_WITH_KNOTS((6,1,1,1,1,1,1,1,1,1,1,1,1,1,1,1,1,1,1,1,1,1,
1,1,1,1,1,1,1,1,1,1,1,1,1,1,1,1,1,1,1,1,1,1,1,1,1,1,1,1,1,1,1,1,1,1,1,1,
1,1,1,1,1,1,1,1,1,1,1,1,1,1,1,1,1,1,1,1,1,1,1,1,1,1,1,1,1,1,1,1,1,1,1,1,
1,1,1,1,1,1,1,1,1,1,1,1,1,1,1,1,1,1,1,1,1,1,1,1,1,1,1,1,1,1,1,1,1,1,1,1,
1,1,1,1,1,1,1,1,1,1,1,1,1,1,1,1,1,1,1,1,1,1,1,1,1,1,1,1,1,1,1,1,1,1,1,1,
1,1,1,1,1,1,1,1,1,1,1,1,1,1,1,1,1,1,1,1,1,1,1,6),(0.,0.005,0.01,0.015,0.02,
0.025,0.03,0.035,0.04,0.045,0.05,0.055,0.06,0.065,0.07,0.075,0.08,0.085,
0.09,0.095,0.1,0.105,0.11,0.115,0.12,0.125,0.13,0.135,0.14,0.145,0.15,0.155,
0.16,0.165,0.17,0.175,0.18,0.185,0.19,0.195,0.2,0.205,0.21,0.215,0.22,0.225,
0.23,0.235,0.24,0.245,0.25,0.255,0.26,0.265,0.27,0.275,0.28,0.285,0.29,
0.295,0.3,0.305,0.31,0.315,0.32,0.325,0.33,0.335,0.34,0.345,0.35,0.355,
0.36,0.365,0.37,0.375,0.38,0.385,0.39,0.395,0.4,0.405,0.41,0.415,0.42,0.425,
0.43,0.435,0.44,0.445,0.45,0.455,0.46,0.465,0.47,0.475,0.48,0.485,0.49,
0.495,0.5,0.505,0.51,0.515,0.52,0.525,0.53,0.535,0.54,0.545,0.55,0.555,
0.56,0.565,0.57,0.575,0.58,0.585,0.59,0.595,0.6,0.605,0.61,0.615,0.62,0.625,
0.63,0.635,0.64,0.645,0.65,0.655,0.66,0.665,0.67,0.675,0.68,0.685,0.690000000000001,
0.695000000000001,0.700000000000001,0.705000000000001,0.710000000000001,
0.715000000000001,0.720000000000001,0.725000000000001,0.730000000000001,
0.735000000000001,0.740000000000001,0.745000000000001,0.750000000000001,
0.755000000000001,0.760000000000001,0.765000000000001,0.770000000000001,
0.775000000000001,0.780000000000001,0.785000000000001,0.790000000000001,
0.795000000000001,0.800000000000001,0.805000000000001,0.810000000000001,
0.815000000000001,0.820000000000001,0.825000000000001,0.830000000000001,
0.835000000000001,0.840000000000001,0.845000000000001,0.850000000000001,
0.855000000000001,0.860000000000001,0.865000000000001,0.870000000000001,
0.875000000000001,0.880000000000001,0.885000000000001,0.890000000000001,
0.895000000000001,0.900000000000001,0.905000000000001,0.910000000000001,
0.915000000000001,0.920000000000001,0.925000000000001,0.930000000000001,
0.935000000000001,0.940000000000001,0.941429844431412),.UNSPECIFIED.)
CURVE()
GEOMETRIC_REPRESENTATION_ITEM()
RATIONAL_B_SPLINE_CURVE((1.,1.,1.,1.,1.,1.,1.,1.,1.,1.,1.,1.,1.,1.,1.,1.,
1.,1.,1.,1.,1.,1.,1.,1.,1.,1.,1.,1.,1.,1.,1.,1.,1.,1.,1.,1.,1.,1.,1.,1.,
1.,1.,1.,1.,1.,1.,1.,1.,1.,1.,1.,1.,1.,1.,1.,1.,1.,1.,1.,1.,1.,1.,1.,1.,
1.,1.,1.,1.,1.,1.,1.,1.,1.,1.,1.,1.,1.,1.,1.,1.,1.,1.,1.,1.,1.,1.,1.,1.,
1.,1.,1.,1.,1.,1.,1.,1.,1.,1.,1.,1.,1.,1.,1.,1.,1.,1.,1.,1.,1.,1.,1.,1.,
1.,1.,1.,1.,1.,1.,1.,1.,1.,1.,1.,1.,1.,1.,1.,1.,1.,1.,1.,1.,1.,1.,1.,1.,
1.,1.,1.,1.,1.,1.,1.,1.,1.,1.,1.,1.,1.,1.,1.,1.,1.,1.,1.,1.,1.,1.,1.,1.,
1.,1.,1.,1.,1.,1.,1.,1.,1.,1.,1.,1.,1.,1.,1.,1.,1.,1.,1.,1.,1.,1.,1.,1.,
1.,1.,1.,1.,1.,1.,1.,1.,1.,1.))
REPRESENTATION_ITEM('')
);
#446=(
BOUNDED_CURVE()
B_SPLINE_CURVE(5,(#72045,#72046,#72047,#72048,#72049,#72050,#72051,#72052,
#72053,#72054,#72055,#72056,#72057,#72058,#72059,#72060,#72061,#72062,#72063,
#72064,#72065,#72066,#72067,#72068,#72069,#72070,#72071,#72072,#72073,#72074,
#72075,#72076,#72077,#72078,#72079,#72080,#72081,#72082,#72083,#72084,#72085,
#72086,#72087,#72088,#72089,#72090,#72091,#72092,#72093,#72094,#72095,#72096,
#72097,#72098,#72099,#72100,#72101,#72102,#72103,#72104,#72105,#72106,#72107,
#72108,#72109,#72110,#72111,#72112,#72113,#72114,#72115,#72116,#72117,#72118,
#72119,#72120,#72121,#72122,#72123,#72124,#72125,#72126,#72127,#72128,#72129,
#72130,#72131,#72132,#72133,#72134,#72135,#72136,#72137,#72138,#72139,#72140,
#72141,#72142,#72143,#72144,#72145,#72146,#72147,#72148,#72149,#72150,#72151,
#72152,#72153,#72154,#72155,#72156,#72157,#72158,#72159,#72160,#72161,#72162,
#72163,#72164,#72165,#72166,#72167,#72168,#72169,#72170,#72171,#72172,#72173,
#72174,#72175,#72176,#72177,#72178,#72179,#72180,#72181,#72182,#72183,#72184,
#72185,#72186,#72187,#72188,#72189,#72190,#72191,#72192,#72193,#72194,#72195,
#72196,#72197,#72198,#72199,#72200,#72201,#72202,#72203,#72204,#72205,#72206,
#72207,#72208,#72209,#72210,#72211,#72212,#72213,#72214,#72215,#72216,#72217,
#72218,#72219,#72220,#72221,#72222,#72223,#72224,#72225,#72226,#72227,#72228,
#72229,#72230,#72231,#72232,#72233,#72234,#72235,#72236,#72237,#72238),
 .UNSPECIFIED.,.F.,.F.)
B_SPLINE_CURVE_WITH_KNOTS((6,1,1,1,1,1,1,1,1,1,1,1,1,1,1,1,1,1,1,1,1,1,
1,1,1,1,1,1,1,1,1,1,1,1,1,1,1,1,1,1,1,1,1,1,1,1,1,1,1,1,1,1,1,1,1,1,1,1,
1,1,1,1,1,1,1,1,1,1,1,1,1,1,1,1,1,1,1,1,1,1,1,1,1,1,1,1,1,1,1,1,1,1,1,1,
1,1,1,1,1,1,1,1,1,1,1,1,1,1,1,1,1,1,1,1,1,1,1,1,1,1,1,1,1,1,1,1,1,1,1,1,
1,1,1,1,1,1,1,1,1,1,1,1,1,1,1,1,1,1,1,1,1,1,1,1,1,1,1,1,1,1,1,1,1,1,1,1,
1,1,1,1,1,1,1,1,1,1,1,1,1,1,1,1,1,1,1,1,1,1,1,6),(-0.941429844431412,-0.940000000000001,
-0.935000000000001,-0.930000000000001,-0.925000000000001,-0.920000000000001,
-0.915000000000001,-0.910000000000001,-0.905000000000001,-0.900000000000001,
-0.895000000000001,-0.890000000000001,-0.885000000000001,-0.880000000000001,
-0.875000000000001,-0.870000000000001,-0.865000000000001,-0.860000000000001,
-0.855000000000001,-0.850000000000001,-0.845000000000001,-0.840000000000001,
-0.835000000000001,-0.830000000000001,-0.825000000000001,-0.820000000000001,
-0.815000000000001,-0.810000000000001,-0.805000000000001,-0.800000000000001,
-0.795000000000001,-0.790000000000001,-0.785000000000001,-0.780000000000001,
-0.775000000000001,-0.770000000000001,-0.765000000000001,-0.760000000000001,
-0.755000000000001,-0.750000000000001,-0.745000000000001,-0.740000000000001,
-0.735000000000001,-0.730000000000001,-0.725000000000001,-0.720000000000001,
-0.715000000000001,-0.710000000000001,-0.705000000000001,-0.700000000000001,
-0.695000000000001,-0.690000000000001,-0.685,-0.68,-0.675,-0.67,-0.665,
-0.66,-0.655,-0.65,-0.645,-0.64,-0.635,-0.63,-0.625,-0.62,-0.615,-0.61,
-0.605,-0.6,-0.595,-0.59,-0.585,-0.58,-0.575,-0.57,-0.565,-0.56,-0.555,
-0.55,-0.545,-0.54,-0.535,-0.53,-0.525,-0.52,-0.515,-0.51,-0.505,-0.5,-0.495,
-0.49,-0.485,-0.48,-0.475,-0.47,-0.465,-0.46,-0.455,-0.45,-0.445,-0.44,
-0.435,-0.43,-0.425,-0.42,-0.415,-0.41,-0.405,-0.4,-0.395,-0.39,-0.385,
-0.38,-0.375,-0.37,-0.365,-0.36,-0.355,-0.35,-0.345,-0.34,-0.335,-0.33,
-0.325,-0.32,-0.315,-0.31,-0.305,-0.3,-0.295,-0.29,-0.285,-0.28,-0.275,
-0.27,-0.265,-0.26,-0.255,-0.25,-0.245,-0.24,-0.235,-0.23,-0.225,-0.22,
-0.215,-0.21,-0.205,-0.2,-0.195,-0.19,-0.185,-0.18,-0.175,-0.17,-0.165,
-0.16,-0.155,-0.15,-0.145,-0.14,-0.135,-0.13,-0.125,-0.12,-0.115,-0.11,
-0.105,-0.1,-0.095,-0.09,-0.085,-0.08,-0.075,-0.07,-0.065,-0.06,-0.055,
-0.05,-0.045,-0.04,-0.035,-0.03,-0.025,-0.02,-0.015,-0.01,-0.005,0.),
 .UNSPECIFIED.)
CURVE()
GEOMETRIC_REPRESENTATION_ITEM()
RATIONAL_B_SPLINE_CURVE((1.,1.,1.,1.,1.,1.,1.,1.,1.,1.,1.,1.,1.,1.,1.,1.,
1.,1.,1.,1.,1.,1.,1.,1.,1.,1.,1.,1.,1.,1.,1.,1.,1.,1.,1.,1.,1.,1.,1.,1.,
1.,1.,1.,1.,1.,1.,1.,1.,1.,1.,1.,1.,1.,1.,1.,1.,1.,1.,1.,1.,1.,1.,1.,1.,
1.,1.,1.,1.,1.,1.,1.,1.,1.,1.,1.,1.,1.,1.,1.,1.,1.,1.,1.,1.,1.,1.,1.,1.,
1.,1.,1.,1.,1.,1.,1.,1.,1.,1.,1.,1.,1.,1.,1.,1.,1.,1.,1.,1.,1.,1.,1.,1.,
1.,1.,1.,1.,1.,1.,1.,1.,1.,1.,1.,1.,1.,1.,1.,1.,1.,1.,1.,1.,1.,1.,1.,1.,
1.,1.,1.,1.,1.,1.,1.,1.,1.,1.,1.,1.,1.,1.,1.,1.,1.,1.,1.,1.,1.,1.,1.,1.,
1.,1.,1.,1.,1.,1.,1.,1.,1.,1.,1.,1.,1.,1.,1.,1.,1.,1.,1.,1.,1.,1.,1.,1.,
1.,1.,1.,1.,1.,1.,1.,1.,1.,1.))
REPRESENTATION_ITEM('')
);
#447=(
BOUNDED_CURVE()
B_SPLINE_CURVE(5,(#72745,#72746,#72747,#72748,#72749,#72750,#72751,#72752,
#72753,#72754,#72755,#72756,#72757,#72758,#72759,#72760,#72761,#72762,#72763,
#72764,#72765,#72766,#72767,#72768,#72769,#72770,#72771,#72772,#72773,#72774,
#72775,#72776,#72777,#72778,#72779,#72780,#72781,#72782,#72783,#72784,#72785,
#72786,#72787,#72788,#72789,#72790,#72791,#72792,#72793,#72794,#72795,#72796,
#72797,#72798,#72799,#72800,#72801,#72802,#72803,#72804,#72805,#72806,#72807,
#72808,#72809,#72810,#72811,#72812,#72813,#72814,#72815,#72816,#72817,#72818,
#72819,#72820,#72821,#72822,#72823,#72824,#72825,#72826,#72827,#72828,#72829,
#72830,#72831,#72832,#72833,#72834,#72835,#72836,#72837,#72838,#72839,#72840,
#72841,#72842,#72843,#72844,#72845,#72846,#72847,#72848,#72849,#72850,#72851,
#72852,#72853,#72854,#72855,#72856,#72857,#72858,#72859,#72860,#72861,#72862,
#72863,#72864,#72865,#72866,#72867,#72868,#72869,#72870,#72871,#72872,#72873,
#72874,#72875,#72876,#72877,#72878,#72879,#72880,#72881,#72882,#72883,#72884,
#72885,#72886,#72887,#72888,#72889,#72890,#72891,#72892,#72893,#72894,#72895,
#72896,#72897,#72898,#72899,#72900,#72901,#72902,#72903,#72904,#72905,#72906,
#72907,#72908,#72909,#72910,#72911,#72912,#72913,#72914,#72915,#72916,#72917,
#72918,#72919,#72920,#72921,#72922,#72923,#72924,#72925,#72926,#72927,#72928,
#72929,#72930,#72931,#72932,#72933,#72934,#72935,#72936,#72937,#72938),
 .UNSPECIFIED.,.F.,.F.)
B_SPLINE_CURVE_WITH_KNOTS((6,1,1,1,1,1,1,1,1,1,1,1,1,1,1,1,1,1,1,1,1,1,
1,1,1,1,1,1,1,1,1,1,1,1,1,1,1,1,1,1,1,1,1,1,1,1,1,1,1,1,1,1,1,1,1,1,1,1,
1,1,1,1,1,1,1,1,1,1,1,1,1,1,1,1,1,1,1,1,1,1,1,1,1,1,1,1,1,1,1,1,1,1,1,1,
1,1,1,1,1,1,1,1,1,1,1,1,1,1,1,1,1,1,1,1,1,1,1,1,1,1,1,1,1,1,1,1,1,1,1,1,
1,1,1,1,1,1,1,1,1,1,1,1,1,1,1,1,1,1,1,1,1,1,1,1,1,1,1,1,1,1,1,1,1,1,1,1,
1,1,1,1,1,1,1,1,1,1,1,1,1,1,1,1,1,1,1,1,1,1,1,6),(0.,0.005,0.01,0.015,0.02,
0.025,0.03,0.035,0.04,0.045,0.05,0.055,0.06,0.065,0.07,0.075,0.08,0.085,
0.09,0.095,0.1,0.105,0.11,0.115,0.12,0.125,0.13,0.135,0.14,0.145,0.15,0.155,
0.16,0.165,0.17,0.175,0.18,0.185,0.19,0.195,0.2,0.205,0.21,0.215,0.22,0.225,
0.23,0.235,0.24,0.245,0.25,0.255,0.26,0.265,0.27,0.275,0.28,0.285,0.29,
0.295,0.3,0.305,0.31,0.315,0.32,0.325,0.33,0.335,0.34,0.345,0.35,0.355,
0.36,0.365,0.37,0.375,0.38,0.385,0.39,0.395,0.4,0.405,0.41,0.415,0.42,0.425,
0.43,0.435,0.44,0.445,0.45,0.455,0.46,0.465,0.47,0.475,0.48,0.485,0.49,
0.495,0.5,0.505,0.51,0.515,0.52,0.525,0.53,0.535,0.54,0.545,0.55,0.555,
0.56,0.565,0.57,0.575,0.58,0.585,0.59,0.595,0.6,0.605,0.61,0.615,0.62,0.625,
0.63,0.635,0.64,0.645,0.65,0.655,0.66,0.665,0.67,0.675,0.68,0.685,0.690000000000001,
0.695000000000001,0.700000000000001,0.705000000000001,0.710000000000001,
0.715000000000001,0.720000000000001,0.725000000000001,0.730000000000001,
0.735000000000001,0.740000000000001,0.745000000000001,0.750000000000001,
0.755000000000001,0.760000000000001,0.765000000000001,0.770000000000001,
0.775000000000001,0.780000000000001,0.785000000000001,0.790000000000001,
0.795000000000001,0.800000000000001,0.805000000000001,0.810000000000001,
0.815000000000001,0.820000000000001,0.825000000000001,0.830000000000001,
0.835000000000001,0.840000000000001,0.845000000000001,0.850000000000001,
0.855000000000001,0.860000000000001,0.865000000000001,0.870000000000001,
0.875000000000001,0.880000000000001,0.885000000000001,0.890000000000001,
0.895000000000001,0.900000000000001,0.905000000000001,0.910000000000001,
0.915000000000001,0.920000000000001,0.925000000000001,0.930000000000001,
0.935000000000001,0.940000000000001,0.941429844431353),.UNSPECIFIED.)
CURVE()
GEOMETRIC_REPRESENTATION_ITEM()
RATIONAL_B_SPLINE_CURVE((1.,1.,1.,1.,1.,1.,1.,1.,1.,1.,1.,1.,1.,1.,1.,1.,
1.,1.,1.,1.,1.,1.,1.,1.,1.,1.,1.,1.,1.,1.,1.,1.,1.,1.,1.,1.,1.,1.,1.,1.,
1.,1.,1.,1.,1.,1.,1.,1.,1.,1.,1.,1.,1.,1.,1.,1.,1.,1.,1.,1.,1.,1.,1.,1.,
1.,1.,1.,1.,1.,1.,1.,1.,1.,1.,1.,1.,1.,1.,1.,1.,1.,1.,1.,1.,1.,1.,1.,1.,
1.,1.,1.,1.,1.,1.,1.,1.,1.,1.,1.,1.,1.,1.,1.,1.,1.,1.,1.,1.,1.,1.,1.,1.,
1.,1.,1.,1.,1.,1.,1.,1.,1.,1.,1.,1.,1.,1.,1.,1.,1.,1.,1.,1.,1.,1.,1.,1.,
1.,1.,1.,1.,1.,1.,1.,1.,1.,1.,1.,1.,1.,1.,1.,1.,1.,1.,1.,1.,1.,1.,1.,1.,
1.,1.,1.,1.,1.,1.,1.,1.,1.,1.,1.,1.,1.,1.,1.,1.,1.,1.,1.,1.,1.,1.,1.,1.,
1.,1.,1.,1.,1.,1.,1.,1.,1.,1.))
REPRESENTATION_ITEM('')
);
#448=(
BOUNDED_CURVE()
B_SPLINE_CURVE(5,(#72941,#72942,#72943,#72944,#72945,#72946,#72947,#72948,
#72949,#72950,#72951,#72952,#72953,#72954,#72955,#72956,#72957,#72958,#72959,
#72960,#72961,#72962,#72963,#72964,#72965,#72966,#72967,#72968,#72969,#72970,
#72971,#72972,#72973,#72974,#72975,#72976,#72977,#72978,#72979,#72980,#72981,
#72982,#72983,#72984,#72985,#72986,#72987,#72988,#72989,#72990,#72991,#72992,
#72993,#72994,#72995,#72996,#72997,#72998,#72999,#73000,#73001,#73002,#73003,
#73004,#73005,#73006,#73007,#73008,#73009,#73010,#73011,#73012,#73013,#73014,
#73015,#73016,#73017,#73018,#73019,#73020,#73021,#73022,#73023,#73024,#73025,
#73026,#73027,#73028,#73029,#73030,#73031,#73032,#73033,#73034,#73035,#73036,
#73037,#73038,#73039,#73040,#73041,#73042,#73043,#73044,#73045,#73046,#73047,
#73048,#73049,#73050,#73051,#73052,#73053,#73054,#73055,#73056,#73057,#73058,
#73059,#73060,#73061,#73062,#73063,#73064,#73065,#73066,#73067,#73068,#73069,
#73070,#73071,#73072,#73073,#73074,#73075,#73076,#73077,#73078,#73079,#73080,
#73081,#73082,#73083,#73084,#73085,#73086,#73087,#73088,#73089,#73090,#73091,
#73092,#73093,#73094,#73095,#73096,#73097,#73098,#73099,#73100,#73101,#73102,
#73103,#73104,#73105,#73106,#73107,#73108,#73109,#73110,#73111,#73112,#73113,
#73114,#73115,#73116,#73117,#73118,#73119,#73120,#73121,#73122,#73123,#73124,
#73125,#73126,#73127,#73128,#73129,#73130,#73131,#73132,#73133,#73134),
 .UNSPECIFIED.,.F.,.F.)
B_SPLINE_CURVE_WITH_KNOTS((6,1,1,1,1,1,1,1,1,1,1,1,1,1,1,1,1,1,1,1,1,1,
1,1,1,1,1,1,1,1,1,1,1,1,1,1,1,1,1,1,1,1,1,1,1,1,1,1,1,1,1,1,1,1,1,1,1,1,
1,1,1,1,1,1,1,1,1,1,1,1,1,1,1,1,1,1,1,1,1,1,1,1,1,1,1,1,1,1,1,1,1,1,1,1,
1,1,1,1,1,1,1,1,1,1,1,1,1,1,1,1,1,1,1,1,1,1,1,1,1,1,1,1,1,1,1,1,1,1,1,1,
1,1,1,1,1,1,1,1,1,1,1,1,1,1,1,1,1,1,1,1,1,1,1,1,1,1,1,1,1,1,1,1,1,1,1,1,
1,1,1,1,1,1,1,1,1,1,1,1,1,1,1,1,1,1,1,1,1,1,1,6),(-0.941429844431353,-0.940000000000001,
-0.935000000000001,-0.930000000000001,-0.925000000000001,-0.920000000000001,
-0.915000000000001,-0.910000000000001,-0.905000000000001,-0.900000000000001,
-0.895000000000001,-0.890000000000001,-0.885000000000001,-0.880000000000001,
-0.875000000000001,-0.870000000000001,-0.865000000000001,-0.860000000000001,
-0.855000000000001,-0.850000000000001,-0.845000000000001,-0.840000000000001,
-0.835000000000001,-0.830000000000001,-0.825000000000001,-0.820000000000001,
-0.815000000000001,-0.810000000000001,-0.805000000000001,-0.800000000000001,
-0.795000000000001,-0.790000000000001,-0.785000000000001,-0.780000000000001,
-0.775000000000001,-0.770000000000001,-0.765000000000001,-0.760000000000001,
-0.755000000000001,-0.750000000000001,-0.745000000000001,-0.740000000000001,
-0.735000000000001,-0.730000000000001,-0.725000000000001,-0.720000000000001,
-0.715000000000001,-0.710000000000001,-0.705000000000001,-0.700000000000001,
-0.695000000000001,-0.690000000000001,-0.685,-0.68,-0.675,-0.67,-0.665,
-0.66,-0.655,-0.65,-0.645,-0.64,-0.635,-0.63,-0.625,-0.62,-0.615,-0.61,
-0.605,-0.6,-0.595,-0.59,-0.585,-0.58,-0.575,-0.57,-0.565,-0.56,-0.555,
-0.55,-0.545,-0.54,-0.535,-0.53,-0.525,-0.52,-0.515,-0.51,-0.505,-0.5,-0.495,
-0.49,-0.485,-0.48,-0.475,-0.47,-0.465,-0.46,-0.455,-0.45,-0.445,-0.44,
-0.435,-0.43,-0.425,-0.42,-0.415,-0.41,-0.405,-0.4,-0.395,-0.39,-0.385,
-0.38,-0.375,-0.37,-0.365,-0.36,-0.355,-0.35,-0.345,-0.34,-0.335,-0.33,
-0.325,-0.32,-0.315,-0.31,-0.305,-0.3,-0.295,-0.29,-0.285,-0.28,-0.275,
-0.27,-0.265,-0.26,-0.255,-0.25,-0.245,-0.24,-0.235,-0.23,-0.225,-0.22,
-0.215,-0.21,-0.205,-0.2,-0.195,-0.19,-0.185,-0.18,-0.175,-0.17,-0.165,
-0.16,-0.155,-0.15,-0.145,-0.14,-0.135,-0.13,-0.125,-0.12,-0.115,-0.11,
-0.105,-0.1,-0.095,-0.09,-0.085,-0.08,-0.075,-0.07,-0.065,-0.06,-0.055,
-0.05,-0.045,-0.04,-0.035,-0.03,-0.025,-0.02,-0.015,-0.01,-0.005,0.),
 .UNSPECIFIED.)
CURVE()
GEOMETRIC_REPRESENTATION_ITEM()
RATIONAL_B_SPLINE_CURVE((1.,1.,1.,1.,1.,1.,1.,1.,1.,1.,1.,1.,1.,1.,1.,1.,
1.,1.,1.,1.,1.,1.,1.,1.,1.,1.,1.,1.,1.,1.,1.,1.,1.,1.,1.,1.,1.,1.,1.,1.,
1.,1.,1.,1.,1.,1.,1.,1.,1.,1.,1.,1.,1.,1.,1.,1.,1.,1.,1.,1.,1.,1.,1.,1.,
1.,1.,1.,1.,1.,1.,1.,1.,1.,1.,1.,1.,1.,1.,1.,1.,1.,1.,1.,1.,1.,1.,1.,1.,
1.,1.,1.,1.,1.,1.,1.,1.,1.,1.,1.,1.,1.,1.,1.,1.,1.,1.,1.,1.,1.,1.,1.,1.,
1.,1.,1.,1.,1.,1.,1.,1.,1.,1.,1.,1.,1.,1.,1.,1.,1.,1.,1.,1.,1.,1.,1.,1.,
1.,1.,1.,1.,1.,1.,1.,1.,1.,1.,1.,1.,1.,1.,1.,1.,1.,1.,1.,1.,1.,1.,1.,1.,
1.,1.,1.,1.,1.,1.,1.,1.,1.,1.,1.,1.,1.,1.,1.,1.,1.,1.,1.,1.,1.,1.,1.,1.,
1.,1.,1.,1.,1.,1.,1.,1.,1.,1.))
REPRESENTATION_ITEM('')
);
#449=(
BOUNDED_CURVE()
B_SPLINE_CURVE(5,(#73641,#73642,#73643,#73644,#73645,#73646,#73647,#73648,
#73649,#73650,#73651,#73652,#73653,#73654,#73655,#73656,#73657,#73658,#73659,
#73660,#73661,#73662,#73663,#73664,#73665,#73666,#73667,#73668,#73669,#73670,
#73671,#73672,#73673,#73674,#73675,#73676,#73677,#73678,#73679,#73680,#73681,
#73682,#73683,#73684,#73685,#73686,#73687,#73688,#73689,#73690,#73691,#73692,
#73693,#73694,#73695,#73696,#73697,#73698,#73699,#73700,#73701,#73702,#73703,
#73704,#73705,#73706,#73707,#73708,#73709,#73710,#73711,#73712,#73713,#73714,
#73715,#73716,#73717,#73718,#73719,#73720,#73721,#73722,#73723,#73724,#73725,
#73726,#73727,#73728,#73729,#73730,#73731,#73732,#73733,#73734,#73735,#73736,
#73737,#73738,#73739,#73740,#73741,#73742,#73743,#73744,#73745,#73746,#73747,
#73748,#73749,#73750,#73751,#73752,#73753,#73754,#73755,#73756,#73757,#73758,
#73759,#73760,#73761,#73762,#73763,#73764,#73765,#73766,#73767,#73768,#73769,
#73770,#73771,#73772,#73773,#73774,#73775,#73776,#73777,#73778,#73779,#73780,
#73781,#73782,#73783,#73784,#73785,#73786,#73787,#73788,#73789,#73790,#73791,
#73792,#73793,#73794,#73795,#73796,#73797,#73798,#73799,#73800,#73801,#73802,
#73803,#73804,#73805,#73806,#73807,#73808,#73809,#73810,#73811,#73812,#73813,
#73814,#73815,#73816,#73817,#73818,#73819,#73820,#73821,#73822,#73823,#73824,
#73825,#73826,#73827,#73828,#73829,#73830,#73831,#73832,#73833,#73834),
 .UNSPECIFIED.,.F.,.F.)
B_SPLINE_CURVE_WITH_KNOTS((6,1,1,1,1,1,1,1,1,1,1,1,1,1,1,1,1,1,1,1,1,1,
1,1,1,1,1,1,1,1,1,1,1,1,1,1,1,1,1,1,1,1,1,1,1,1,1,1,1,1,1,1,1,1,1,1,1,1,
1,1,1,1,1,1,1,1,1,1,1,1,1,1,1,1,1,1,1,1,1,1,1,1,1,1,1,1,1,1,1,1,1,1,1,1,
1,1,1,1,1,1,1,1,1,1,1,1,1,1,1,1,1,1,1,1,1,1,1,1,1,1,1,1,1,1,1,1,1,1,1,1,
1,1,1,1,1,1,1,1,1,1,1,1,1,1,1,1,1,1,1,1,1,1,1,1,1,1,1,1,1,1,1,1,1,1,1,1,
1,1,1,1,1,1,1,1,1,1,1,1,1,1,1,1,1,1,1,1,1,1,1,6),(0.,0.005,0.01,0.015,0.02,
0.025,0.03,0.035,0.04,0.045,0.05,0.055,0.06,0.065,0.07,0.075,0.08,0.085,
0.09,0.095,0.1,0.105,0.11,0.115,0.12,0.125,0.13,0.135,0.14,0.145,0.15,0.155,
0.16,0.165,0.17,0.175,0.18,0.185,0.19,0.195,0.2,0.205,0.21,0.215,0.22,0.225,
0.23,0.235,0.24,0.245,0.25,0.255,0.26,0.265,0.27,0.275,0.28,0.285,0.29,
0.295,0.3,0.305,0.31,0.315,0.32,0.325,0.33,0.335,0.34,0.345,0.35,0.355,
0.36,0.365,0.37,0.375,0.38,0.385,0.39,0.395,0.4,0.405,0.41,0.415,0.42,0.425,
0.43,0.435,0.44,0.445,0.45,0.455,0.46,0.465,0.47,0.475,0.48,0.485,0.49,
0.495,0.5,0.505,0.51,0.515,0.52,0.525,0.53,0.535,0.54,0.545,0.55,0.555,
0.56,0.565,0.57,0.575,0.58,0.585,0.59,0.595,0.6,0.605,0.61,0.615,0.62,0.625,
0.63,0.635,0.64,0.645,0.65,0.655,0.66,0.665,0.67,0.675,0.68,0.685,0.690000000000001,
0.695000000000001,0.700000000000001,0.705000000000001,0.710000000000001,
0.715000000000001,0.720000000000001,0.725000000000001,0.730000000000001,
0.735000000000001,0.740000000000001,0.745000000000001,0.750000000000001,
0.755000000000001,0.760000000000001,0.765000000000001,0.770000000000001,
0.775000000000001,0.780000000000001,0.785000000000001,0.790000000000001,
0.795000000000001,0.800000000000001,0.805000000000001,0.810000000000001,
0.815000000000001,0.820000000000001,0.825000000000001,0.830000000000001,
0.835000000000001,0.840000000000001,0.845000000000001,0.850000000000001,
0.855000000000001,0.860000000000001,0.865000000000001,0.870000000000001,
0.875000000000001,0.880000000000001,0.885000000000001,0.890000000000001,
0.895000000000001,0.900000000000001,0.905000000000001,0.910000000000001,
0.915000000000001,0.920000000000001,0.925000000000001,0.930000000000001,
0.935000000000001,0.940000000000001,0.941429844431354),.UNSPECIFIED.)
CURVE()
GEOMETRIC_REPRESENTATION_ITEM()
RATIONAL_B_SPLINE_CURVE((1.,1.,1.,1.,1.,1.,1.,1.,1.,1.,1.,1.,1.,1.,1.,1.,
1.,1.,1.,1.,1.,1.,1.,1.,1.,1.,1.,1.,1.,1.,1.,1.,1.,1.,1.,1.,1.,1.,1.,1.,
1.,1.,1.,1.,1.,1.,1.,1.,1.,1.,1.,1.,1.,1.,1.,1.,1.,1.,1.,1.,1.,1.,1.,1.,
1.,1.,1.,1.,1.,1.,1.,1.,1.,1.,1.,1.,1.,1.,1.,1.,1.,1.,1.,1.,1.,1.,1.,1.,
1.,1.,1.,1.,1.,1.,1.,1.,1.,1.,1.,1.,1.,1.,1.,1.,1.,1.,1.,1.,1.,1.,1.,1.,
1.,1.,1.,1.,1.,1.,1.,1.,1.,1.,1.,1.,1.,1.,1.,1.,1.,1.,1.,1.,1.,1.,1.,1.,
1.,1.,1.,1.,1.,1.,1.,1.,1.,1.,1.,1.,1.,1.,1.,1.,1.,1.,1.,1.,1.,1.,1.,1.,
1.,1.,1.,1.,1.,1.,1.,1.,1.,1.,1.,1.,1.,1.,1.,1.,1.,1.,1.,1.,1.,1.,1.,1.,
1.,1.,1.,1.,1.,1.,1.,1.,1.,1.))
REPRESENTATION_ITEM('')
);
#450=(
BOUNDED_CURVE()
B_SPLINE_CURVE(5,(#73837,#73838,#73839,#73840,#73841,#73842,#73843,#73844,
#73845,#73846,#73847,#73848,#73849,#73850,#73851,#73852,#73853,#73854,#73855,
#73856,#73857,#73858,#73859,#73860,#73861,#73862,#73863,#73864,#73865,#73866,
#73867,#73868,#73869,#73870,#73871,#73872,#73873,#73874,#73875,#73876,#73877,
#73878,#73879,#73880,#73881,#73882,#73883,#73884,#73885,#73886,#73887,#73888,
#73889,#73890,#73891,#73892,#73893,#73894,#73895,#73896,#73897,#73898,#73899,
#73900,#73901,#73902,#73903,#73904,#73905,#73906,#73907,#73908,#73909,#73910,
#73911,#73912,#73913,#73914,#73915,#73916,#73917,#73918,#73919,#73920,#73921,
#73922,#73923,#73924,#73925,#73926,#73927,#73928,#73929,#73930,#73931,#73932,
#73933,#73934,#73935,#73936,#73937,#73938,#73939,#73940,#73941,#73942,#73943,
#73944,#73945,#73946,#73947,#73948,#73949,#73950,#73951,#73952,#73953,#73954,
#73955,#73956,#73957,#73958,#73959,#73960,#73961,#73962,#73963,#73964,#73965,
#73966,#73967,#73968,#73969,#73970,#73971,#73972,#73973,#73974,#73975,#73976,
#73977,#73978,#73979,#73980,#73981,#73982,#73983,#73984,#73985,#73986,#73987,
#73988,#73989,#73990,#73991,#73992,#73993,#73994,#73995,#73996,#73997,#73998,
#73999,#74000,#74001,#74002,#74003,#74004,#74005,#74006,#74007,#74008,#74009,
#74010,#74011,#74012,#74013,#74014,#74015,#74016,#74017,#74018,#74019,#74020,
#74021,#74022,#74023,#74024,#74025,#74026,#74027,#74028,#74029,#74030),
 .UNSPECIFIED.,.F.,.F.)
B_SPLINE_CURVE_WITH_KNOTS((6,1,1,1,1,1,1,1,1,1,1,1,1,1,1,1,1,1,1,1,1,1,
1,1,1,1,1,1,1,1,1,1,1,1,1,1,1,1,1,1,1,1,1,1,1,1,1,1,1,1,1,1,1,1,1,1,1,1,
1,1,1,1,1,1,1,1,1,1,1,1,1,1,1,1,1,1,1,1,1,1,1,1,1,1,1,1,1,1,1,1,1,1,1,1,
1,1,1,1,1,1,1,1,1,1,1,1,1,1,1,1,1,1,1,1,1,1,1,1,1,1,1,1,1,1,1,1,1,1,1,1,
1,1,1,1,1,1,1,1,1,1,1,1,1,1,1,1,1,1,1,1,1,1,1,1,1,1,1,1,1,1,1,1,1,1,1,1,
1,1,1,1,1,1,1,1,1,1,1,1,1,1,1,1,1,1,1,1,1,1,1,6),(-0.941429844431354,-0.940000000000001,
-0.935000000000001,-0.930000000000001,-0.925000000000001,-0.920000000000001,
-0.915000000000001,-0.910000000000001,-0.905000000000001,-0.900000000000001,
-0.895000000000001,-0.890000000000001,-0.885000000000001,-0.880000000000001,
-0.875000000000001,-0.870000000000001,-0.865000000000001,-0.860000000000001,
-0.855000000000001,-0.850000000000001,-0.845000000000001,-0.840000000000001,
-0.835000000000001,-0.830000000000001,-0.825000000000001,-0.820000000000001,
-0.815000000000001,-0.810000000000001,-0.805000000000001,-0.800000000000001,
-0.795000000000001,-0.790000000000001,-0.785000000000001,-0.780000000000001,
-0.775000000000001,-0.770000000000001,-0.765000000000001,-0.760000000000001,
-0.755000000000001,-0.750000000000001,-0.745000000000001,-0.740000000000001,
-0.735000000000001,-0.730000000000001,-0.725000000000001,-0.720000000000001,
-0.715000000000001,-0.710000000000001,-0.705000000000001,-0.700000000000001,
-0.695000000000001,-0.690000000000001,-0.685,-0.68,-0.675,-0.67,-0.665,
-0.66,-0.655,-0.65,-0.645,-0.64,-0.635,-0.63,-0.625,-0.62,-0.615,-0.61,
-0.605,-0.6,-0.595,-0.59,-0.585,-0.58,-0.575,-0.57,-0.565,-0.56,-0.555,
-0.55,-0.545,-0.54,-0.535,-0.53,-0.525,-0.52,-0.515,-0.51,-0.505,-0.5,-0.495,
-0.49,-0.485,-0.48,-0.475,-0.47,-0.465,-0.46,-0.455,-0.45,-0.445,-0.44,
-0.435,-0.43,-0.425,-0.42,-0.415,-0.41,-0.405,-0.4,-0.395,-0.39,-0.385,
-0.38,-0.375,-0.37,-0.365,-0.36,-0.355,-0.35,-0.345,-0.34,-0.335,-0.33,
-0.325,-0.32,-0.315,-0.31,-0.305,-0.3,-0.295,-0.29,-0.285,-0.28,-0.275,
-0.27,-0.265,-0.26,-0.255,-0.25,-0.245,-0.24,-0.235,-0.23,-0.225,-0.22,
-0.215,-0.21,-0.205,-0.2,-0.195,-0.19,-0.185,-0.18,-0.175,-0.17,-0.165,
-0.16,-0.155,-0.15,-0.145,-0.14,-0.135,-0.13,-0.125,-0.12,-0.115,-0.11,
-0.105,-0.1,-0.095,-0.09,-0.085,-0.08,-0.075,-0.07,-0.065,-0.06,-0.055,
-0.05,-0.045,-0.04,-0.035,-0.03,-0.025,-0.02,-0.015,-0.01,-0.005,0.),
 .UNSPECIFIED.)
CURVE()
GEOMETRIC_REPRESENTATION_ITEM()
RATIONAL_B_SPLINE_CURVE((1.,1.,1.,1.,1.,1.,1.,1.,1.,1.,1.,1.,1.,1.,1.,1.,
1.,1.,1.,1.,1.,1.,1.,1.,1.,1.,1.,1.,1.,1.,1.,1.,1.,1.,1.,1.,1.,1.,1.,1.,
1.,1.,1.,1.,1.,1.,1.,1.,1.,1.,1.,1.,1.,1.,1.,1.,1.,1.,1.,1.,1.,1.,1.,1.,
1.,1.,1.,1.,1.,1.,1.,1.,1.,1.,1.,1.,1.,1.,1.,1.,1.,1.,1.,1.,1.,1.,1.,1.,
1.,1.,1.,1.,1.,1.,1.,1.,1.,1.,1.,1.,1.,1.,1.,1.,1.,1.,1.,1.,1.,1.,1.,1.,
1.,1.,1.,1.,1.,1.,1.,1.,1.,1.,1.,1.,1.,1.,1.,1.,1.,1.,1.,1.,1.,1.,1.,1.,
1.,1.,1.,1.,1.,1.,1.,1.,1.,1.,1.,1.,1.,1.,1.,1.,1.,1.,1.,1.,1.,1.,1.,1.,
1.,1.,1.,1.,1.,1.,1.,1.,1.,1.,1.,1.,1.,1.,1.,1.,1.,1.,1.,1.,1.,1.,1.,1.,
1.,1.,1.,1.,1.,1.,1.,1.,1.,1.))
REPRESENTATION_ITEM('')
);
#451=(
BOUNDED_CURVE()
B_SPLINE_CURVE(5,(#74537,#74538,#74539,#74540,#74541,#74542,#74543,#74544,
#74545,#74546,#74547,#74548,#74549,#74550,#74551,#74552,#74553,#74554,#74555,
#74556,#74557,#74558,#74559,#74560,#74561,#74562,#74563,#74564,#74565,#74566,
#74567,#74568,#74569,#74570,#74571,#74572,#74573,#74574,#74575,#74576,#74577,
#74578,#74579,#74580,#74581,#74582,#74583,#74584,#74585,#74586,#74587,#74588,
#74589,#74590,#74591,#74592,#74593,#74594,#74595,#74596,#74597,#74598,#74599,
#74600,#74601,#74602,#74603,#74604,#74605,#74606,#74607,#74608,#74609,#74610,
#74611,#74612,#74613,#74614,#74615,#74616,#74617,#74618,#74619,#74620,#74621,
#74622,#74623,#74624,#74625,#74626,#74627,#74628,#74629,#74630,#74631,#74632,
#74633,#74634,#74635,#74636,#74637,#74638,#74639,#74640,#74641,#74642,#74643,
#74644,#74645,#74646,#74647,#74648,#74649,#74650,#74651,#74652,#74653,#74654,
#74655,#74656,#74657,#74658,#74659,#74660,#74661,#74662,#74663,#74664,#74665,
#74666,#74667,#74668,#74669,#74670,#74671,#74672,#74673,#74674,#74675,#74676,
#74677,#74678,#74679,#74680,#74681,#74682,#74683,#74684,#74685,#74686,#74687,
#74688,#74689,#74690,#74691,#74692,#74693,#74694,#74695,#74696,#74697,#74698,
#74699,#74700,#74701,#74702,#74703,#74704,#74705,#74706,#74707,#74708,#74709,
#74710,#74711,#74712,#74713,#74714,#74715,#74716,#74717,#74718,#74719,#74720,
#74721,#74722,#74723,#74724,#74725,#74726,#74727,#74728,#74729,#74730),
 .UNSPECIFIED.,.F.,.F.)
B_SPLINE_CURVE_WITH_KNOTS((6,1,1,1,1,1,1,1,1,1,1,1,1,1,1,1,1,1,1,1,1,1,
1,1,1,1,1,1,1,1,1,1,1,1,1,1,1,1,1,1,1,1,1,1,1,1,1,1,1,1,1,1,1,1,1,1,1,1,
1,1,1,1,1,1,1,1,1,1,1,1,1,1,1,1,1,1,1,1,1,1,1,1,1,1,1,1,1,1,1,1,1,1,1,1,
1,1,1,1,1,1,1,1,1,1,1,1,1,1,1,1,1,1,1,1,1,1,1,1,1,1,1,1,1,1,1,1,1,1,1,1,
1,1,1,1,1,1,1,1,1,1,1,1,1,1,1,1,1,1,1,1,1,1,1,1,1,1,1,1,1,1,1,1,1,1,1,1,
1,1,1,1,1,1,1,1,1,1,1,1,1,1,1,1,1,1,1,1,1,1,1,6),(0.,0.005,0.01,0.015,0.02,
0.025,0.03,0.035,0.04,0.045,0.05,0.055,0.06,0.065,0.07,0.075,0.08,0.085,
0.09,0.095,0.1,0.105,0.11,0.115,0.12,0.125,0.13,0.135,0.14,0.145,0.15,0.155,
0.16,0.165,0.17,0.175,0.18,0.185,0.19,0.195,0.2,0.205,0.21,0.215,0.22,0.225,
0.23,0.235,0.24,0.245,0.25,0.255,0.26,0.265,0.27,0.275,0.28,0.285,0.29,
0.295,0.3,0.305,0.31,0.315,0.32,0.325,0.33,0.335,0.34,0.345,0.35,0.355,
0.36,0.365,0.37,0.375,0.38,0.385,0.39,0.395,0.4,0.405,0.41,0.415,0.42,0.425,
0.43,0.435,0.44,0.445,0.45,0.455,0.46,0.465,0.47,0.475,0.48,0.485,0.49,
0.495,0.5,0.505,0.51,0.515,0.52,0.525,0.53,0.535,0.54,0.545,0.55,0.555,
0.56,0.565,0.57,0.575,0.58,0.585,0.59,0.595,0.6,0.605,0.61,0.615,0.62,0.625,
0.63,0.635,0.64,0.645,0.65,0.655,0.66,0.665,0.67,0.675,0.68,0.685,0.690000000000001,
0.695000000000001,0.700000000000001,0.705000000000001,0.710000000000001,
0.715000000000001,0.720000000000001,0.725000000000001,0.730000000000001,
0.735000000000001,0.740000000000001,0.745000000000001,0.750000000000001,
0.755000000000001,0.760000000000001,0.765000000000001,0.770000000000001,
0.775000000000001,0.780000000000001,0.785000000000001,0.790000000000001,
0.795000000000001,0.800000000000001,0.805000000000001,0.810000000000001,
0.815000000000001,0.820000000000001,0.825000000000001,0.830000000000001,
0.835000000000001,0.840000000000001,0.845000000000001,0.850000000000001,
0.855000000000001,0.860000000000001,0.865000000000001,0.870000000000001,
0.875000000000001,0.880000000000001,0.885000000000001,0.890000000000001,
0.895000000000001,0.900000000000001,0.905000000000001,0.910000000000001,
0.915000000000001,0.920000000000001,0.925000000000001,0.930000000000001,
0.935000000000001,0.940000000000001,0.94142984443138),.UNSPECIFIED.)
CURVE()
GEOMETRIC_REPRESENTATION_ITEM()
RATIONAL_B_SPLINE_CURVE((1.,1.,1.,1.,1.,1.,1.,1.,1.,1.,1.,1.,1.,1.,1.,1.,
1.,1.,1.,1.,1.,1.,1.,1.,1.,1.,1.,1.,1.,1.,1.,1.,1.,1.,1.,1.,1.,1.,1.,1.,
1.,1.,1.,1.,1.,1.,1.,1.,1.,1.,1.,1.,1.,1.,1.,1.,1.,1.,1.,1.,1.,1.,1.,1.,
1.,1.,1.,1.,1.,1.,1.,1.,1.,1.,1.,1.,1.,1.,1.,1.,1.,1.,1.,1.,1.,1.,1.,1.,
1.,1.,1.,1.,1.,1.,1.,1.,1.,1.,1.,1.,1.,1.,1.,1.,1.,1.,1.,1.,1.,1.,1.,1.,
1.,1.,1.,1.,1.,1.,1.,1.,1.,1.,1.,1.,1.,1.,1.,1.,1.,1.,1.,1.,1.,1.,1.,1.,
1.,1.,1.,1.,1.,1.,1.,1.,1.,1.,1.,1.,1.,1.,1.,1.,1.,1.,1.,1.,1.,1.,1.,1.,
1.,1.,1.,1.,1.,1.,1.,1.,1.,1.,1.,1.,1.,1.,1.,1.,1.,1.,1.,1.,1.,1.,1.,1.,
1.,1.,1.,1.,1.,1.,1.,1.,1.,1.))
REPRESENTATION_ITEM('')
);
#452=(
BOUNDED_CURVE()
B_SPLINE_CURVE(5,(#74733,#74734,#74735,#74736,#74737,#74738,#74739,#74740,
#74741,#74742,#74743,#74744,#74745,#74746,#74747,#74748,#74749,#74750,#74751,
#74752,#74753,#74754,#74755,#74756,#74757,#74758,#74759,#74760,#74761,#74762,
#74763,#74764,#74765,#74766,#74767,#74768,#74769,#74770,#74771,#74772,#74773,
#74774,#74775,#74776,#74777,#74778,#74779,#74780,#74781,#74782,#74783,#74784,
#74785,#74786,#74787,#74788,#74789,#74790,#74791,#74792,#74793,#74794,#74795,
#74796,#74797,#74798,#74799,#74800,#74801,#74802,#74803,#74804,#74805,#74806,
#74807,#74808,#74809,#74810,#74811,#74812,#74813,#74814,#74815,#74816,#74817,
#74818,#74819,#74820,#74821,#74822,#74823,#74824,#74825,#74826,#74827,#74828,
#74829,#74830,#74831,#74832,#74833,#74834,#74835,#74836,#74837,#74838,#74839,
#74840,#74841,#74842,#74843,#74844,#74845,#74846,#74847,#74848,#74849,#74850,
#74851,#74852,#74853,#74854,#74855,#74856,#74857,#74858,#74859,#74860,#74861,
#74862,#74863,#74864,#74865,#74866,#74867,#74868,#74869,#74870,#74871,#74872,
#74873,#74874,#74875,#74876,#74877,#74878,#74879,#74880,#74881,#74882,#74883,
#74884,#74885,#74886,#74887,#74888,#74889,#74890,#74891,#74892,#74893,#74894,
#74895,#74896,#74897,#74898,#74899,#74900,#74901,#74902,#74903,#74904,#74905,
#74906,#74907,#74908,#74909,#74910,#74911,#74912,#74913,#74914,#74915,#74916,
#74917,#74918,#74919,#74920,#74921,#74922,#74923,#74924,#74925,#74926),
 .UNSPECIFIED.,.F.,.F.)
B_SPLINE_CURVE_WITH_KNOTS((6,1,1,1,1,1,1,1,1,1,1,1,1,1,1,1,1,1,1,1,1,1,
1,1,1,1,1,1,1,1,1,1,1,1,1,1,1,1,1,1,1,1,1,1,1,1,1,1,1,1,1,1,1,1,1,1,1,1,
1,1,1,1,1,1,1,1,1,1,1,1,1,1,1,1,1,1,1,1,1,1,1,1,1,1,1,1,1,1,1,1,1,1,1,1,
1,1,1,1,1,1,1,1,1,1,1,1,1,1,1,1,1,1,1,1,1,1,1,1,1,1,1,1,1,1,1,1,1,1,1,1,
1,1,1,1,1,1,1,1,1,1,1,1,1,1,1,1,1,1,1,1,1,1,1,1,1,1,1,1,1,1,1,1,1,1,1,1,
1,1,1,1,1,1,1,1,1,1,1,1,1,1,1,1,1,1,1,1,1,1,1,6),(-0.941429844431407,-0.940000000000001,
-0.935000000000001,-0.930000000000001,-0.925000000000001,-0.920000000000001,
-0.915000000000001,-0.910000000000001,-0.905000000000001,-0.900000000000001,
-0.895000000000001,-0.890000000000001,-0.885000000000001,-0.880000000000001,
-0.875000000000001,-0.870000000000001,-0.865000000000001,-0.860000000000001,
-0.855000000000001,-0.850000000000001,-0.845000000000001,-0.840000000000001,
-0.835000000000001,-0.830000000000001,-0.825000000000001,-0.820000000000001,
-0.815000000000001,-0.810000000000001,-0.805000000000001,-0.800000000000001,
-0.795000000000001,-0.790000000000001,-0.785000000000001,-0.780000000000001,
-0.775000000000001,-0.770000000000001,-0.765000000000001,-0.760000000000001,
-0.755000000000001,-0.750000000000001,-0.745000000000001,-0.740000000000001,
-0.735000000000001,-0.730000000000001,-0.725000000000001,-0.720000000000001,
-0.715000000000001,-0.710000000000001,-0.705000000000001,-0.700000000000001,
-0.695000000000001,-0.690000000000001,-0.685,-0.68,-0.675,-0.67,-0.665,
-0.66,-0.655,-0.65,-0.645,-0.64,-0.635,-0.63,-0.625,-0.62,-0.615,-0.61,
-0.605,-0.6,-0.595,-0.59,-0.585,-0.58,-0.575,-0.57,-0.565,-0.56,-0.555,
-0.55,-0.545,-0.54,-0.535,-0.53,-0.525,-0.52,-0.515,-0.51,-0.505,-0.5,-0.495,
-0.49,-0.485,-0.48,-0.475,-0.47,-0.465,-0.46,-0.455,-0.45,-0.445,-0.44,
-0.435,-0.43,-0.425,-0.42,-0.415,-0.41,-0.405,-0.4,-0.395,-0.39,-0.385,
-0.38,-0.375,-0.37,-0.365,-0.36,-0.355,-0.35,-0.345,-0.34,-0.335,-0.33,
-0.325,-0.32,-0.315,-0.31,-0.305,-0.3,-0.295,-0.29,-0.285,-0.28,-0.275,
-0.27,-0.265,-0.26,-0.255,-0.25,-0.245,-0.24,-0.235,-0.23,-0.225,-0.22,
-0.215,-0.21,-0.205,-0.2,-0.195,-0.19,-0.185,-0.18,-0.175,-0.17,-0.165,
-0.16,-0.155,-0.15,-0.145,-0.14,-0.135,-0.13,-0.125,-0.12,-0.115,-0.11,
-0.105,-0.1,-0.095,-0.09,-0.085,-0.08,-0.075,-0.07,-0.065,-0.06,-0.055,
-0.05,-0.045,-0.04,-0.035,-0.03,-0.025,-0.02,-0.015,-0.01,-0.005,0.),
 .UNSPECIFIED.)
CURVE()
GEOMETRIC_REPRESENTATION_ITEM()
RATIONAL_B_SPLINE_CURVE((1.,1.,1.,1.,1.,1.,1.,1.,1.,1.,1.,1.,1.,1.,1.,1.,
1.,1.,1.,1.,1.,1.,1.,1.,1.,1.,1.,1.,1.,1.,1.,1.,1.,1.,1.,1.,1.,1.,1.,1.,
1.,1.,1.,1.,1.,1.,1.,1.,1.,1.,1.,1.,1.,1.,1.,1.,1.,1.,1.,1.,1.,1.,1.,1.,
1.,1.,1.,1.,1.,1.,1.,1.,1.,1.,1.,1.,1.,1.,1.,1.,1.,1.,1.,1.,1.,1.,1.,1.,
1.,1.,1.,1.,1.,1.,1.,1.,1.,1.,1.,1.,1.,1.,1.,1.,1.,1.,1.,1.,1.,1.,1.,1.,
1.,1.,1.,1.,1.,1.,1.,1.,1.,1.,1.,1.,1.,1.,1.,1.,1.,1.,1.,1.,1.,1.,1.,1.,
1.,1.,1.,1.,1.,1.,1.,1.,1.,1.,1.,1.,1.,1.,1.,1.,1.,1.,1.,1.,1.,1.,1.,1.,
1.,1.,1.,1.,1.,1.,1.,1.,1.,1.,1.,1.,1.,1.,1.,1.,1.,1.,1.,1.,1.,1.,1.,1.,
1.,1.,1.,1.,1.,1.,1.,1.,1.,1.))
REPRESENTATION_ITEM('')
);
#453=(
BOUNDED_CURVE()
B_SPLINE_CURVE(5,(#75433,#75434,#75435,#75436,#75437,#75438,#75439,#75440,
#75441,#75442,#75443,#75444,#75445,#75446,#75447,#75448,#75449,#75450,#75451,
#75452,#75453,#75454,#75455,#75456,#75457,#75458,#75459,#75460,#75461,#75462,
#75463,#75464,#75465,#75466,#75467,#75468,#75469,#75470,#75471,#75472,#75473,
#75474,#75475,#75476,#75477,#75478,#75479,#75480,#75481,#75482,#75483,#75484,
#75485,#75486,#75487,#75488,#75489,#75490,#75491,#75492,#75493,#75494,#75495,
#75496,#75497,#75498,#75499,#75500,#75501,#75502,#75503,#75504,#75505,#75506,
#75507,#75508,#75509,#75510,#75511,#75512,#75513,#75514,#75515,#75516,#75517,
#75518,#75519,#75520,#75521,#75522,#75523,#75524,#75525,#75526,#75527,#75528,
#75529,#75530,#75531,#75532,#75533,#75534,#75535,#75536,#75537,#75538,#75539,
#75540,#75541,#75542,#75543,#75544,#75545,#75546,#75547,#75548,#75549,#75550,
#75551,#75552,#75553,#75554,#75555,#75556,#75557,#75558,#75559,#75560,#75561,
#75562,#75563,#75564,#75565,#75566,#75567,#75568,#75569,#75570,#75571,#75572,
#75573,#75574,#75575,#75576,#75577,#75578,#75579,#75580,#75581,#75582,#75583,
#75584,#75585,#75586,#75587,#75588,#75589,#75590,#75591,#75592,#75593,#75594,
#75595,#75596,#75597,#75598,#75599,#75600,#75601,#75602,#75603,#75604,#75605,
#75606,#75607,#75608,#75609,#75610,#75611,#75612,#75613,#75614,#75615,#75616,
#75617,#75618,#75619,#75620,#75621,#75622,#75623,#75624,#75625,#75626),
 .UNSPECIFIED.,.F.,.F.)
B_SPLINE_CURVE_WITH_KNOTS((6,1,1,1,1,1,1,1,1,1,1,1,1,1,1,1,1,1,1,1,1,1,
1,1,1,1,1,1,1,1,1,1,1,1,1,1,1,1,1,1,1,1,1,1,1,1,1,1,1,1,1,1,1,1,1,1,1,1,
1,1,1,1,1,1,1,1,1,1,1,1,1,1,1,1,1,1,1,1,1,1,1,1,1,1,1,1,1,1,1,1,1,1,1,1,
1,1,1,1,1,1,1,1,1,1,1,1,1,1,1,1,1,1,1,1,1,1,1,1,1,1,1,1,1,1,1,1,1,1,1,1,
1,1,1,1,1,1,1,1,1,1,1,1,1,1,1,1,1,1,1,1,1,1,1,1,1,1,1,1,1,1,1,1,1,1,1,1,
1,1,1,1,1,1,1,1,1,1,1,1,1,1,1,1,1,1,1,1,1,1,1,6),(0.,0.005,0.01,0.015,0.02,
0.025,0.03,0.035,0.04,0.045,0.05,0.055,0.06,0.065,0.07,0.075,0.08,0.085,
0.09,0.095,0.1,0.105,0.11,0.115,0.12,0.125,0.13,0.135,0.14,0.145,0.15,0.155,
0.16,0.165,0.17,0.175,0.18,0.185,0.19,0.195,0.2,0.205,0.21,0.215,0.22,0.225,
0.23,0.235,0.24,0.245,0.25,0.255,0.26,0.265,0.27,0.275,0.28,0.285,0.29,
0.295,0.3,0.305,0.31,0.315,0.32,0.325,0.33,0.335,0.34,0.345,0.35,0.355,
0.36,0.365,0.37,0.375,0.38,0.385,0.39,0.395,0.4,0.405,0.41,0.415,0.42,0.425,
0.43,0.435,0.44,0.445,0.45,0.455,0.46,0.465,0.47,0.475,0.48,0.485,0.49,
0.495,0.5,0.505,0.51,0.515,0.52,0.525,0.53,0.535,0.54,0.545,0.55,0.555,
0.56,0.565,0.57,0.575,0.58,0.585,0.59,0.595,0.6,0.605,0.61,0.615,0.62,0.625,
0.63,0.635,0.64,0.645,0.65,0.655,0.66,0.665,0.67,0.675,0.68,0.685,0.690000000000001,
0.695000000000001,0.700000000000001,0.705000000000001,0.710000000000001,
0.715000000000001,0.720000000000001,0.725000000000001,0.730000000000001,
0.735000000000001,0.740000000000001,0.745000000000001,0.750000000000001,
0.755000000000001,0.760000000000001,0.765000000000001,0.770000000000001,
0.775000000000001,0.780000000000001,0.785000000000001,0.790000000000001,
0.795000000000001,0.800000000000001,0.805000000000001,0.810000000000001,
0.815000000000001,0.820000000000001,0.825000000000001,0.830000000000001,
0.835000000000001,0.840000000000001,0.845000000000001,0.850000000000001,
0.855000000000001,0.860000000000001,0.865000000000001,0.870000000000001,
0.875000000000001,0.880000000000001,0.885000000000001,0.890000000000001,
0.895000000000001,0.900000000000001,0.905000000000001,0.910000000000001,
0.915000000000001,0.920000000000001,0.925000000000001,0.930000000000001,
0.935000000000001,0.940000000000001,0.941429844431403),.UNSPECIFIED.)
CURVE()
GEOMETRIC_REPRESENTATION_ITEM()
RATIONAL_B_SPLINE_CURVE((1.,1.,1.,1.,1.,1.,1.,1.,1.,1.,1.,1.,1.,1.,1.,1.,
1.,1.,1.,1.,1.,1.,1.,1.,1.,1.,1.,1.,1.,1.,1.,1.,1.,1.,1.,1.,1.,1.,1.,1.,
1.,1.,1.,1.,1.,1.,1.,1.,1.,1.,1.,1.,1.,1.,1.,1.,1.,1.,1.,1.,1.,1.,1.,1.,
1.,1.,1.,1.,1.,1.,1.,1.,1.,1.,1.,1.,1.,1.,1.,1.,1.,1.,1.,1.,1.,1.,1.,1.,
1.,1.,1.,1.,1.,1.,1.,1.,1.,1.,1.,1.,1.,1.,1.,1.,1.,1.,1.,1.,1.,1.,1.,1.,
1.,1.,1.,1.,1.,1.,1.,1.,1.,1.,1.,1.,1.,1.,1.,1.,1.,1.,1.,1.,1.,1.,1.,1.,
1.,1.,1.,1.,1.,1.,1.,1.,1.,1.,1.,1.,1.,1.,1.,1.,1.,1.,1.,1.,1.,1.,1.,1.,
1.,1.,1.,1.,1.,1.,1.,1.,1.,1.,1.,1.,1.,1.,1.,1.,1.,1.,1.,1.,1.,1.,1.,1.,
1.,1.,1.,1.,1.,1.,1.,1.,1.,1.))
REPRESENTATION_ITEM('')
);
#454=(
BOUNDED_CURVE()
B_SPLINE_CURVE(5,(#75629,#75630,#75631,#75632,#75633,#75634,#75635,#75636,
#75637,#75638,#75639,#75640,#75641,#75642,#75643,#75644,#75645,#75646,#75647,
#75648,#75649,#75650,#75651,#75652,#75653,#75654,#75655,#75656,#75657,#75658,
#75659,#75660,#75661,#75662,#75663,#75664,#75665,#75666,#75667,#75668,#75669,
#75670,#75671,#75672,#75673,#75674,#75675,#75676,#75677,#75678,#75679,#75680,
#75681,#75682,#75683,#75684,#75685,#75686,#75687,#75688,#75689,#75690,#75691,
#75692,#75693,#75694,#75695,#75696,#75697,#75698,#75699,#75700,#75701,#75702,
#75703,#75704,#75705,#75706,#75707,#75708,#75709,#75710,#75711,#75712,#75713,
#75714,#75715,#75716,#75717,#75718,#75719,#75720,#75721,#75722,#75723,#75724,
#75725,#75726,#75727,#75728,#75729,#75730,#75731,#75732,#75733,#75734,#75735,
#75736,#75737,#75738,#75739,#75740,#75741,#75742,#75743,#75744,#75745,#75746,
#75747,#75748,#75749,#75750,#75751,#75752,#75753,#75754,#75755,#75756,#75757,
#75758,#75759,#75760,#75761,#75762,#75763,#75764,#75765,#75766,#75767,#75768,
#75769,#75770,#75771,#75772,#75773,#75774,#75775,#75776,#75777,#75778,#75779,
#75780,#75781,#75782,#75783,#75784,#75785,#75786,#75787,#75788,#75789,#75790,
#75791,#75792,#75793,#75794,#75795,#75796,#75797,#75798,#75799,#75800,#75801,
#75802,#75803,#75804,#75805,#75806,#75807,#75808,#75809,#75810,#75811,#75812,
#75813,#75814,#75815,#75816,#75817,#75818,#75819,#75820,#75821,#75822),
 .UNSPECIFIED.,.F.,.F.)
B_SPLINE_CURVE_WITH_KNOTS((6,1,1,1,1,1,1,1,1,1,1,1,1,1,1,1,1,1,1,1,1,1,
1,1,1,1,1,1,1,1,1,1,1,1,1,1,1,1,1,1,1,1,1,1,1,1,1,1,1,1,1,1,1,1,1,1,1,1,
1,1,1,1,1,1,1,1,1,1,1,1,1,1,1,1,1,1,1,1,1,1,1,1,1,1,1,1,1,1,1,1,1,1,1,1,
1,1,1,1,1,1,1,1,1,1,1,1,1,1,1,1,1,1,1,1,1,1,1,1,1,1,1,1,1,1,1,1,1,1,1,1,
1,1,1,1,1,1,1,1,1,1,1,1,1,1,1,1,1,1,1,1,1,1,1,1,1,1,1,1,1,1,1,1,1,1,1,1,
1,1,1,1,1,1,1,1,1,1,1,1,1,1,1,1,1,1,1,1,1,1,1,6),(-0.941429844431386,-0.940000000000001,
-0.935000000000001,-0.930000000000001,-0.925000000000001,-0.920000000000001,
-0.915000000000001,-0.910000000000001,-0.905000000000001,-0.900000000000001,
-0.895000000000001,-0.890000000000001,-0.885000000000001,-0.880000000000001,
-0.875000000000001,-0.870000000000001,-0.865000000000001,-0.860000000000001,
-0.855000000000001,-0.850000000000001,-0.845000000000001,-0.840000000000001,
-0.835000000000001,-0.830000000000001,-0.825000000000001,-0.820000000000001,
-0.815000000000001,-0.810000000000001,-0.805000000000001,-0.800000000000001,
-0.795000000000001,-0.790000000000001,-0.785000000000001,-0.780000000000001,
-0.775000000000001,-0.770000000000001,-0.765000000000001,-0.760000000000001,
-0.755000000000001,-0.750000000000001,-0.745000000000001,-0.740000000000001,
-0.735000000000001,-0.730000000000001,-0.725000000000001,-0.720000000000001,
-0.715000000000001,-0.710000000000001,-0.705000000000001,-0.700000000000001,
-0.695000000000001,-0.690000000000001,-0.685,-0.68,-0.675,-0.67,-0.665,
-0.66,-0.655,-0.65,-0.645,-0.64,-0.635,-0.63,-0.625,-0.62,-0.615,-0.61,
-0.605,-0.6,-0.595,-0.59,-0.585,-0.58,-0.575,-0.57,-0.565,-0.56,-0.555,
-0.55,-0.545,-0.54,-0.535,-0.53,-0.525,-0.52,-0.515,-0.51,-0.505,-0.5,-0.495,
-0.49,-0.485,-0.48,-0.475,-0.47,-0.465,-0.46,-0.455,-0.45,-0.445,-0.44,
-0.435,-0.43,-0.425,-0.42,-0.415,-0.41,-0.405,-0.4,-0.395,-0.39,-0.385,
-0.38,-0.375,-0.37,-0.365,-0.36,-0.355,-0.35,-0.345,-0.34,-0.335,-0.33,
-0.325,-0.32,-0.315,-0.31,-0.305,-0.3,-0.295,-0.29,-0.285,-0.28,-0.275,
-0.27,-0.265,-0.26,-0.255,-0.25,-0.245,-0.24,-0.235,-0.23,-0.225,-0.22,
-0.215,-0.21,-0.205,-0.2,-0.195,-0.19,-0.185,-0.18,-0.175,-0.17,-0.165,
-0.16,-0.155,-0.15,-0.145,-0.14,-0.135,-0.13,-0.125,-0.12,-0.115,-0.11,
-0.105,-0.1,-0.095,-0.09,-0.085,-0.08,-0.075,-0.07,-0.065,-0.06,-0.055,
-0.05,-0.045,-0.04,-0.035,-0.03,-0.025,-0.02,-0.015,-0.01,-0.005,0.),
 .UNSPECIFIED.)
CURVE()
GEOMETRIC_REPRESENTATION_ITEM()
RATIONAL_B_SPLINE_CURVE((1.,1.,1.,1.,1.,1.,1.,1.,1.,1.,1.,1.,1.,1.,1.,1.,
1.,1.,1.,1.,1.,1.,1.,1.,1.,1.,1.,1.,1.,1.,1.,1.,1.,1.,1.,1.,1.,1.,1.,1.,
1.,1.,1.,1.,1.,1.,1.,1.,1.,1.,1.,1.,1.,1.,1.,1.,1.,1.,1.,1.,1.,1.,1.,1.,
1.,1.,1.,1.,1.,1.,1.,1.,1.,1.,1.,1.,1.,1.,1.,1.,1.,1.,1.,1.,1.,1.,1.,1.,
1.,1.,1.,1.,1.,1.,1.,1.,1.,1.,1.,1.,1.,1.,1.,1.,1.,1.,1.,1.,1.,1.,1.,1.,
1.,1.,1.,1.,1.,1.,1.,1.,1.,1.,1.,1.,1.,1.,1.,1.,1.,1.,1.,1.,1.,1.,1.,1.,
1.,1.,1.,1.,1.,1.,1.,1.,1.,1.,1.,1.,1.,1.,1.,1.,1.,1.,1.,1.,1.,1.,1.,1.,
1.,1.,1.,1.,1.,1.,1.,1.,1.,1.,1.,1.,1.,1.,1.,1.,1.,1.,1.,1.,1.,1.,1.,1.,
1.,1.,1.,1.,1.,1.,1.,1.,1.,1.))
REPRESENTATION_ITEM('')
);
#455=(
BOUNDED_CURVE()
B_SPLINE_CURVE(5,(#76329,#76330,#76331,#76332,#76333,#76334,#76335,#76336,
#76337,#76338,#76339,#76340,#76341,#76342,#76343,#76344,#76345,#76346,#76347,
#76348,#76349,#76350,#76351,#76352,#76353,#76354,#76355,#76356,#76357,#76358,
#76359,#76360,#76361,#76362,#76363,#76364,#76365,#76366,#76367,#76368,#76369,
#76370,#76371,#76372,#76373,#76374,#76375,#76376,#76377,#76378,#76379,#76380,
#76381,#76382,#76383,#76384,#76385,#76386,#76387,#76388,#76389,#76390,#76391,
#76392,#76393,#76394,#76395,#76396,#76397,#76398,#76399,#76400,#76401,#76402,
#76403,#76404,#76405,#76406,#76407,#76408,#76409,#76410,#76411,#76412,#76413,
#76414,#76415,#76416,#76417,#76418,#76419,#76420,#76421,#76422,#76423,#76424,
#76425,#76426,#76427,#76428,#76429,#76430,#76431,#76432,#76433,#76434,#76435,
#76436,#76437,#76438,#76439,#76440,#76441,#76442,#76443,#76444,#76445,#76446,
#76447,#76448,#76449,#76450,#76451,#76452,#76453,#76454,#76455,#76456,#76457,
#76458,#76459,#76460,#76461,#76462,#76463,#76464,#76465,#76466,#76467,#76468,
#76469,#76470,#76471,#76472,#76473,#76474,#76475,#76476,#76477,#76478,#76479,
#76480,#76481,#76482,#76483,#76484,#76485,#76486,#76487,#76488,#76489,#76490,
#76491,#76492,#76493,#76494,#76495,#76496,#76497,#76498,#76499,#76500,#76501,
#76502,#76503,#76504,#76505,#76506,#76507,#76508,#76509,#76510,#76511,#76512,
#76513,#76514,#76515,#76516,#76517,#76518,#76519,#76520,#76521,#76522),
 .UNSPECIFIED.,.F.,.F.)
B_SPLINE_CURVE_WITH_KNOTS((6,1,1,1,1,1,1,1,1,1,1,1,1,1,1,1,1,1,1,1,1,1,
1,1,1,1,1,1,1,1,1,1,1,1,1,1,1,1,1,1,1,1,1,1,1,1,1,1,1,1,1,1,1,1,1,1,1,1,
1,1,1,1,1,1,1,1,1,1,1,1,1,1,1,1,1,1,1,1,1,1,1,1,1,1,1,1,1,1,1,1,1,1,1,1,
1,1,1,1,1,1,1,1,1,1,1,1,1,1,1,1,1,1,1,1,1,1,1,1,1,1,1,1,1,1,1,1,1,1,1,1,
1,1,1,1,1,1,1,1,1,1,1,1,1,1,1,1,1,1,1,1,1,1,1,1,1,1,1,1,1,1,1,1,1,1,1,1,
1,1,1,1,1,1,1,1,1,1,1,1,1,1,1,1,1,1,1,1,1,1,1,6),(0.,0.005,0.01,0.015,0.02,
0.025,0.03,0.035,0.04,0.045,0.05,0.055,0.06,0.065,0.07,0.075,0.08,0.085,
0.09,0.095,0.1,0.105,0.11,0.115,0.12,0.125,0.13,0.135,0.14,0.145,0.15,0.155,
0.16,0.165,0.17,0.175,0.18,0.185,0.19,0.195,0.2,0.205,0.21,0.215,0.22,0.225,
0.23,0.235,0.24,0.245,0.25,0.255,0.26,0.265,0.27,0.275,0.28,0.285,0.29,
0.295,0.3,0.305,0.31,0.315,0.32,0.325,0.33,0.335,0.34,0.345,0.35,0.355,
0.36,0.365,0.37,0.375,0.38,0.385,0.39,0.395,0.4,0.405,0.41,0.415,0.42,0.425,
0.43,0.435,0.44,0.445,0.45,0.455,0.46,0.465,0.47,0.475,0.48,0.485,0.49,
0.495,0.5,0.505,0.51,0.515,0.52,0.525,0.53,0.535,0.54,0.545,0.55,0.555,
0.56,0.565,0.57,0.575,0.58,0.585,0.59,0.595,0.6,0.605,0.61,0.615,0.62,0.625,
0.63,0.635,0.64,0.645,0.65,0.655,0.66,0.665,0.67,0.675,0.68,0.685,0.690000000000001,
0.695000000000001,0.700000000000001,0.705000000000001,0.710000000000001,
0.715000000000001,0.720000000000001,0.725000000000001,0.730000000000001,
0.735000000000001,0.740000000000001,0.745000000000001,0.750000000000001,
0.755000000000001,0.760000000000001,0.765000000000001,0.770000000000001,
0.775000000000001,0.780000000000001,0.785000000000001,0.790000000000001,
0.795000000000001,0.800000000000001,0.805000000000001,0.810000000000001,
0.815000000000001,0.820000000000001,0.825000000000001,0.830000000000001,
0.835000000000001,0.840000000000001,0.845000000000001,0.850000000000001,
0.855000000000001,0.860000000000001,0.865000000000001,0.870000000000001,
0.875000000000001,0.880000000000001,0.885000000000001,0.890000000000001,
0.895000000000001,0.900000000000001,0.905000000000001,0.910000000000001,
0.915000000000001,0.920000000000001,0.925000000000001,0.930000000000001,
0.935000000000001,0.940000000000001,0.941429844431507),.UNSPECIFIED.)
CURVE()
GEOMETRIC_REPRESENTATION_ITEM()
RATIONAL_B_SPLINE_CURVE((1.,1.,1.,1.,1.,1.,1.,1.,1.,1.,1.,1.,1.,1.,1.,1.,
1.,1.,1.,1.,1.,1.,1.,1.,1.,1.,1.,1.,1.,1.,1.,1.,1.,1.,1.,1.,1.,1.,1.,1.,
1.,1.,1.,1.,1.,1.,1.,1.,1.,1.,1.,1.,1.,1.,1.,1.,1.,1.,1.,1.,1.,1.,1.,1.,
1.,1.,1.,1.,1.,1.,1.,1.,1.,1.,1.,1.,1.,1.,1.,1.,1.,1.,1.,1.,1.,1.,1.,1.,
1.,1.,1.,1.,1.,1.,1.,1.,1.,1.,1.,1.,1.,1.,1.,1.,1.,1.,1.,1.,1.,1.,1.,1.,
1.,1.,1.,1.,1.,1.,1.,1.,1.,1.,1.,1.,1.,1.,1.,1.,1.,1.,1.,1.,1.,1.,1.,1.,
1.,1.,1.,1.,1.,1.,1.,1.,1.,1.,1.,1.,1.,1.,1.,1.,1.,1.,1.,1.,1.,1.,1.,1.,
1.,1.,1.,1.,1.,1.,1.,1.,1.,1.,1.,1.,1.,1.,1.,1.,1.,1.,1.,1.,1.,1.,1.,1.,
1.,1.,1.,1.,1.,1.,1.,1.,1.,1.))
REPRESENTATION_ITEM('')
);
#456=(
BOUNDED_CURVE()
B_SPLINE_CURVE(5,(#76525,#76526,#76527,#76528,#76529,#76530,#76531,#76532,
#76533,#76534,#76535,#76536,#76537,#76538,#76539,#76540,#76541,#76542,#76543,
#76544,#76545,#76546,#76547,#76548,#76549,#76550,#76551,#76552,#76553,#76554,
#76555,#76556,#76557,#76558,#76559,#76560,#76561,#76562,#76563,#76564,#76565,
#76566,#76567,#76568,#76569,#76570,#76571,#76572,#76573,#76574,#76575,#76576,
#76577,#76578,#76579,#76580,#76581,#76582,#76583,#76584,#76585,#76586,#76587,
#76588,#76589,#76590,#76591,#76592,#76593,#76594,#76595,#76596,#76597,#76598,
#76599,#76600,#76601,#76602,#76603,#76604,#76605,#76606,#76607,#76608,#76609,
#76610,#76611,#76612,#76613,#76614,#76615,#76616,#76617,#76618,#76619,#76620,
#76621,#76622,#76623,#76624,#76625,#76626,#76627,#76628,#76629,#76630,#76631,
#76632,#76633,#76634,#76635,#76636,#76637,#76638,#76639,#76640,#76641,#76642,
#76643,#76644,#76645,#76646,#76647,#76648,#76649,#76650,#76651,#76652,#76653,
#76654,#76655,#76656,#76657,#76658,#76659,#76660,#76661,#76662,#76663,#76664,
#76665,#76666,#76667,#76668,#76669,#76670,#76671,#76672,#76673,#76674,#76675,
#76676,#76677,#76678,#76679,#76680,#76681,#76682,#76683,#76684,#76685,#76686,
#76687,#76688,#76689,#76690,#76691,#76692,#76693,#76694,#76695,#76696,#76697,
#76698,#76699,#76700,#76701,#76702,#76703,#76704,#76705,#76706,#76707,#76708,
#76709,#76710,#76711,#76712,#76713,#76714,#76715,#76716,#76717,#76718),
 .UNSPECIFIED.,.F.,.F.)
B_SPLINE_CURVE_WITH_KNOTS((6,1,1,1,1,1,1,1,1,1,1,1,1,1,1,1,1,1,1,1,1,1,
1,1,1,1,1,1,1,1,1,1,1,1,1,1,1,1,1,1,1,1,1,1,1,1,1,1,1,1,1,1,1,1,1,1,1,1,
1,1,1,1,1,1,1,1,1,1,1,1,1,1,1,1,1,1,1,1,1,1,1,1,1,1,1,1,1,1,1,1,1,1,1,1,
1,1,1,1,1,1,1,1,1,1,1,1,1,1,1,1,1,1,1,1,1,1,1,1,1,1,1,1,1,1,1,1,1,1,1,1,
1,1,1,1,1,1,1,1,1,1,1,1,1,1,1,1,1,1,1,1,1,1,1,1,1,1,1,1,1,1,1,1,1,1,1,1,
1,1,1,1,1,1,1,1,1,1,1,1,1,1,1,1,1,1,1,1,1,1,1,6),(-0.9414298444315,-0.940000000000001,
-0.935000000000001,-0.930000000000001,-0.925000000000001,-0.920000000000001,
-0.915000000000001,-0.910000000000001,-0.905000000000001,-0.900000000000001,
-0.895000000000001,-0.890000000000001,-0.885000000000001,-0.880000000000001,
-0.875000000000001,-0.870000000000001,-0.865000000000001,-0.860000000000001,
-0.855000000000001,-0.850000000000001,-0.845000000000001,-0.840000000000001,
-0.835000000000001,-0.830000000000001,-0.825000000000001,-0.820000000000001,
-0.815000000000001,-0.810000000000001,-0.805000000000001,-0.800000000000001,
-0.795000000000001,-0.790000000000001,-0.785000000000001,-0.780000000000001,
-0.775000000000001,-0.770000000000001,-0.765000000000001,-0.760000000000001,
-0.755000000000001,-0.750000000000001,-0.745000000000001,-0.740000000000001,
-0.735000000000001,-0.730000000000001,-0.725000000000001,-0.720000000000001,
-0.715000000000001,-0.710000000000001,-0.705000000000001,-0.700000000000001,
-0.695000000000001,-0.690000000000001,-0.685,-0.68,-0.675,-0.67,-0.665,
-0.66,-0.655,-0.65,-0.645,-0.64,-0.635,-0.63,-0.625,-0.62,-0.615,-0.61,
-0.605,-0.6,-0.595,-0.59,-0.585,-0.58,-0.575,-0.57,-0.565,-0.56,-0.555,
-0.55,-0.545,-0.54,-0.535,-0.53,-0.525,-0.52,-0.515,-0.51,-0.505,-0.5,-0.495,
-0.49,-0.485,-0.48,-0.475,-0.47,-0.465,-0.46,-0.455,-0.45,-0.445,-0.44,
-0.435,-0.43,-0.425,-0.42,-0.415,-0.41,-0.405,-0.4,-0.395,-0.39,-0.385,
-0.38,-0.375,-0.37,-0.365,-0.36,-0.355,-0.35,-0.345,-0.34,-0.335,-0.33,
-0.325,-0.32,-0.315,-0.31,-0.305,-0.3,-0.295,-0.29,-0.285,-0.28,-0.275,
-0.27,-0.265,-0.26,-0.255,-0.25,-0.245,-0.24,-0.235,-0.23,-0.225,-0.22,
-0.215,-0.21,-0.205,-0.2,-0.195,-0.19,-0.185,-0.18,-0.175,-0.17,-0.165,
-0.16,-0.155,-0.15,-0.145,-0.14,-0.135,-0.13,-0.125,-0.12,-0.115,-0.11,
-0.105,-0.1,-0.095,-0.09,-0.085,-0.08,-0.075,-0.07,-0.065,-0.06,-0.055,
-0.05,-0.045,-0.04,-0.035,-0.03,-0.025,-0.02,-0.015,-0.01,-0.005,0.),
 .UNSPECIFIED.)
CURVE()
GEOMETRIC_REPRESENTATION_ITEM()
RATIONAL_B_SPLINE_CURVE((1.,1.,1.,1.,1.,1.,1.,1.,1.,1.,1.,1.,1.,1.,1.,1.,
1.,1.,1.,1.,1.,1.,1.,1.,1.,1.,1.,1.,1.,1.,1.,1.,1.,1.,1.,1.,1.,1.,1.,1.,
1.,1.,1.,1.,1.,1.,1.,1.,1.,1.,1.,1.,1.,1.,1.,1.,1.,1.,1.,1.,1.,1.,1.,1.,
1.,1.,1.,1.,1.,1.,1.,1.,1.,1.,1.,1.,1.,1.,1.,1.,1.,1.,1.,1.,1.,1.,1.,1.,
1.,1.,1.,1.,1.,1.,1.,1.,1.,1.,1.,1.,1.,1.,1.,1.,1.,1.,1.,1.,1.,1.,1.,1.,
1.,1.,1.,1.,1.,1.,1.,1.,1.,1.,1.,1.,1.,1.,1.,1.,1.,1.,1.,1.,1.,1.,1.,1.,
1.,1.,1.,1.,1.,1.,1.,1.,1.,1.,1.,1.,1.,1.,1.,1.,1.,1.,1.,1.,1.,1.,1.,1.,
1.,1.,1.,1.,1.,1.,1.,1.,1.,1.,1.,1.,1.,1.,1.,1.,1.,1.,1.,1.,1.,1.,1.,1.,
1.,1.,1.,1.,1.,1.,1.,1.,1.,1.))
REPRESENTATION_ITEM('')
);
#457=(
BOUNDED_CURVE()
B_SPLINE_CURVE(5,(#77225,#77226,#77227,#77228,#77229,#77230,#77231,#77232,
#77233,#77234,#77235,#77236,#77237,#77238,#77239,#77240,#77241,#77242,#77243,
#77244,#77245,#77246,#77247,#77248,#77249,#77250,#77251,#77252,#77253,#77254,
#77255,#77256,#77257,#77258,#77259,#77260,#77261,#77262,#77263,#77264,#77265,
#77266,#77267,#77268,#77269,#77270,#77271,#77272,#77273,#77274,#77275,#77276,
#77277,#77278,#77279,#77280,#77281,#77282,#77283,#77284,#77285,#77286,#77287,
#77288,#77289,#77290,#77291,#77292,#77293,#77294,#77295,#77296,#77297,#77298,
#77299,#77300,#77301,#77302,#77303,#77304,#77305,#77306,#77307,#77308,#77309,
#77310,#77311,#77312,#77313,#77314,#77315,#77316,#77317,#77318,#77319,#77320,
#77321,#77322,#77323,#77324,#77325,#77326,#77327,#77328,#77329,#77330,#77331,
#77332,#77333,#77334,#77335,#77336,#77337,#77338,#77339,#77340,#77341,#77342,
#77343,#77344,#77345,#77346,#77347,#77348,#77349,#77350,#77351,#77352,#77353,
#77354,#77355,#77356,#77357,#77358,#77359,#77360,#77361,#77362,#77363,#77364,
#77365,#77366,#77367,#77368,#77369,#77370,#77371,#77372,#77373,#77374,#77375,
#77376,#77377,#77378,#77379,#77380,#77381,#77382,#77383,#77384,#77385,#77386,
#77387,#77388,#77389,#77390,#77391,#77392,#77393,#77394,#77395,#77396,#77397,
#77398,#77399,#77400,#77401,#77402,#77403,#77404,#77405,#77406,#77407,#77408,
#77409,#77410,#77411,#77412,#77413,#77414,#77415,#77416,#77417,#77418),
 .UNSPECIFIED.,.F.,.F.)
B_SPLINE_CURVE_WITH_KNOTS((6,1,1,1,1,1,1,1,1,1,1,1,1,1,1,1,1,1,1,1,1,1,
1,1,1,1,1,1,1,1,1,1,1,1,1,1,1,1,1,1,1,1,1,1,1,1,1,1,1,1,1,1,1,1,1,1,1,1,
1,1,1,1,1,1,1,1,1,1,1,1,1,1,1,1,1,1,1,1,1,1,1,1,1,1,1,1,1,1,1,1,1,1,1,1,
1,1,1,1,1,1,1,1,1,1,1,1,1,1,1,1,1,1,1,1,1,1,1,1,1,1,1,1,1,1,1,1,1,1,1,1,
1,1,1,1,1,1,1,1,1,1,1,1,1,1,1,1,1,1,1,1,1,1,1,1,1,1,1,1,1,1,1,1,1,1,1,1,
1,1,1,1,1,1,1,1,1,1,1,1,1,1,1,1,1,1,1,1,1,1,1,6),(0.,0.005,0.01,0.015,0.02,
0.025,0.03,0.035,0.04,0.045,0.05,0.055,0.06,0.065,0.07,0.075,0.08,0.085,
0.09,0.095,0.1,0.105,0.11,0.115,0.12,0.125,0.13,0.135,0.14,0.145,0.15,0.155,
0.16,0.165,0.17,0.175,0.18,0.185,0.19,0.195,0.2,0.205,0.21,0.215,0.22,0.225,
0.23,0.235,0.24,0.245,0.25,0.255,0.26,0.265,0.27,0.275,0.28,0.285,0.29,
0.295,0.3,0.305,0.31,0.315,0.32,0.325,0.33,0.335,0.34,0.345,0.35,0.355,
0.36,0.365,0.37,0.375,0.38,0.385,0.39,0.395,0.4,0.405,0.41,0.415,0.42,0.425,
0.43,0.435,0.44,0.445,0.45,0.455,0.46,0.465,0.47,0.475,0.48,0.485,0.49,
0.495,0.5,0.505,0.51,0.515,0.52,0.525,0.53,0.535,0.54,0.545,0.55,0.555,
0.56,0.565,0.57,0.575,0.58,0.585,0.59,0.595,0.6,0.605,0.61,0.615,0.62,0.625,
0.63,0.635,0.64,0.645,0.65,0.655,0.66,0.665,0.67,0.675,0.68,0.685,0.690000000000001,
0.695000000000001,0.700000000000001,0.705000000000001,0.710000000000001,
0.715000000000001,0.720000000000001,0.725000000000001,0.730000000000001,
0.735000000000001,0.740000000000001,0.745000000000001,0.750000000000001,
0.755000000000001,0.760000000000001,0.765000000000001,0.770000000000001,
0.775000000000001,0.780000000000001,0.785000000000001,0.790000000000001,
0.795000000000001,0.800000000000001,0.805000000000001,0.810000000000001,
0.815000000000001,0.820000000000001,0.825000000000001,0.830000000000001,
0.835000000000001,0.840000000000001,0.845000000000001,0.850000000000001,
0.855000000000001,0.860000000000001,0.865000000000001,0.870000000000001,
0.875000000000001,0.880000000000001,0.885000000000001,0.890000000000001,
0.895000000000001,0.900000000000001,0.905000000000001,0.910000000000001,
0.915000000000001,0.920000000000001,0.925000000000001,0.930000000000001,
0.935000000000001,0.940000000000001,0.941429844431311),.UNSPECIFIED.)
CURVE()
GEOMETRIC_REPRESENTATION_ITEM()
RATIONAL_B_SPLINE_CURVE((1.,1.,1.,1.,1.,1.,1.,1.,1.,1.,1.,1.,1.,1.,1.,1.,
1.,1.,1.,1.,1.,1.,1.,1.,1.,1.,1.,1.,1.,1.,1.,1.,1.,1.,1.,1.,1.,1.,1.,1.,
1.,1.,1.,1.,1.,1.,1.,1.,1.,1.,1.,1.,1.,1.,1.,1.,1.,1.,1.,1.,1.,1.,1.,1.,
1.,1.,1.,1.,1.,1.,1.,1.,1.,1.,1.,1.,1.,1.,1.,1.,1.,1.,1.,1.,1.,1.,1.,1.,
1.,1.,1.,1.,1.,1.,1.,1.,1.,1.,1.,1.,1.,1.,1.,1.,1.,1.,1.,1.,1.,1.,1.,1.,
1.,1.,1.,1.,1.,1.,1.,1.,1.,1.,1.,1.,1.,1.,1.,1.,1.,1.,1.,1.,1.,1.,1.,1.,
1.,1.,1.,1.,1.,1.,1.,1.,1.,1.,1.,1.,1.,1.,1.,1.,1.,1.,1.,1.,1.,1.,1.,1.,
1.,1.,1.,1.,1.,1.,1.,1.,1.,1.,1.,1.,1.,1.,1.,1.,1.,1.,1.,1.,1.,1.,1.,1.,
1.,1.,1.,1.,1.,1.,1.,1.,1.,1.))
REPRESENTATION_ITEM('')
);
#458=(
BOUNDED_CURVE()
B_SPLINE_CURVE(5,(#77421,#77422,#77423,#77424,#77425,#77426,#77427,#77428,
#77429,#77430,#77431,#77432,#77433,#77434,#77435,#77436,#77437,#77438,#77439,
#77440,#77441,#77442,#77443,#77444,#77445,#77446,#77447,#77448,#77449,#77450,
#77451,#77452,#77453,#77454,#77455,#77456,#77457,#77458,#77459,#77460,#77461,
#77462,#77463,#77464,#77465,#77466,#77467,#77468,#77469,#77470,#77471,#77472,
#77473,#77474,#77475,#77476,#77477,#77478,#77479,#77480,#77481,#77482,#77483,
#77484,#77485,#77486,#77487,#77488,#77489,#77490,#77491,#77492,#77493,#77494,
#77495,#77496,#77497,#77498,#77499,#77500,#77501,#77502,#77503,#77504,#77505,
#77506,#77507,#77508,#77509,#77510,#77511,#77512,#77513,#77514,#77515,#77516,
#77517,#77518,#77519,#77520,#77521,#77522,#77523,#77524,#77525,#77526,#77527,
#77528,#77529,#77530,#77531,#77532,#77533,#77534,#77535,#77536,#77537,#77538,
#77539,#77540,#77541,#77542,#77543,#77544,#77545,#77546,#77547,#77548,#77549,
#77550,#77551,#77552,#77553,#77554,#77555,#77556,#77557,#77558,#77559,#77560,
#77561,#77562,#77563,#77564,#77565,#77566,#77567,#77568,#77569,#77570,#77571,
#77572,#77573,#77574,#77575,#77576,#77577,#77578,#77579,#77580,#77581,#77582,
#77583,#77584,#77585,#77586,#77587,#77588,#77589,#77590,#77591,#77592,#77593,
#77594,#77595,#77596,#77597,#77598,#77599,#77600,#77601,#77602,#77603,#77604,
#77605,#77606,#77607,#77608,#77609,#77610,#77611,#77612,#77613,#77614),
 .UNSPECIFIED.,.F.,.F.)
B_SPLINE_CURVE_WITH_KNOTS((6,1,1,1,1,1,1,1,1,1,1,1,1,1,1,1,1,1,1,1,1,1,
1,1,1,1,1,1,1,1,1,1,1,1,1,1,1,1,1,1,1,1,1,1,1,1,1,1,1,1,1,1,1,1,1,1,1,1,
1,1,1,1,1,1,1,1,1,1,1,1,1,1,1,1,1,1,1,1,1,1,1,1,1,1,1,1,1,1,1,1,1,1,1,1,
1,1,1,1,1,1,1,1,1,1,1,1,1,1,1,1,1,1,1,1,1,1,1,1,1,1,1,1,1,1,1,1,1,1,1,1,
1,1,1,1,1,1,1,1,1,1,1,1,1,1,1,1,1,1,1,1,1,1,1,1,1,1,1,1,1,1,1,1,1,1,1,1,
1,1,1,1,1,1,1,1,1,1,1,1,1,1,1,1,1,1,1,1,1,1,1,6),(-0.941429844431311,-0.940000000000001,
-0.935000000000001,-0.930000000000001,-0.925000000000001,-0.920000000000001,
-0.915000000000001,-0.910000000000001,-0.905000000000001,-0.900000000000001,
-0.895000000000001,-0.890000000000001,-0.885000000000001,-0.880000000000001,
-0.875000000000001,-0.870000000000001,-0.865000000000001,-0.860000000000001,
-0.855000000000001,-0.850000000000001,-0.845000000000001,-0.840000000000001,
-0.835000000000001,-0.830000000000001,-0.825000000000001,-0.820000000000001,
-0.815000000000001,-0.810000000000001,-0.805000000000001,-0.800000000000001,
-0.795000000000001,-0.790000000000001,-0.785000000000001,-0.780000000000001,
-0.775000000000001,-0.770000000000001,-0.765000000000001,-0.760000000000001,
-0.755000000000001,-0.750000000000001,-0.745000000000001,-0.740000000000001,
-0.735000000000001,-0.730000000000001,-0.725000000000001,-0.720000000000001,
-0.715000000000001,-0.710000000000001,-0.705000000000001,-0.700000000000001,
-0.695000000000001,-0.690000000000001,-0.685,-0.68,-0.675,-0.67,-0.665,
-0.66,-0.655,-0.65,-0.645,-0.64,-0.635,-0.63,-0.625,-0.62,-0.615,-0.61,
-0.605,-0.6,-0.595,-0.59,-0.585,-0.58,-0.575,-0.57,-0.565,-0.56,-0.555,
-0.55,-0.545,-0.54,-0.535,-0.53,-0.525,-0.52,-0.515,-0.51,-0.505,-0.5,-0.495,
-0.49,-0.485,-0.48,-0.475,-0.47,-0.465,-0.46,-0.455,-0.45,-0.445,-0.44,
-0.435,-0.43,-0.425,-0.42,-0.415,-0.41,-0.405,-0.4,-0.395,-0.39,-0.385,
-0.38,-0.375,-0.37,-0.365,-0.36,-0.355,-0.35,-0.345,-0.34,-0.335,-0.33,
-0.325,-0.32,-0.315,-0.31,-0.305,-0.3,-0.295,-0.29,-0.285,-0.28,-0.275,
-0.27,-0.265,-0.26,-0.255,-0.25,-0.245,-0.24,-0.235,-0.23,-0.225,-0.22,
-0.215,-0.21,-0.205,-0.2,-0.195,-0.19,-0.185,-0.18,-0.175,-0.17,-0.165,
-0.16,-0.155,-0.15,-0.145,-0.14,-0.135,-0.13,-0.125,-0.12,-0.115,-0.11,
-0.105,-0.1,-0.095,-0.09,-0.085,-0.08,-0.075,-0.07,-0.065,-0.06,-0.055,
-0.05,-0.045,-0.04,-0.035,-0.03,-0.025,-0.02,-0.015,-0.01,-0.005,0.),
 .UNSPECIFIED.)
CURVE()
GEOMETRIC_REPRESENTATION_ITEM()
RATIONAL_B_SPLINE_CURVE((1.,1.,1.,1.,1.,1.,1.,1.,1.,1.,1.,1.,1.,1.,1.,1.,
1.,1.,1.,1.,1.,1.,1.,1.,1.,1.,1.,1.,1.,1.,1.,1.,1.,1.,1.,1.,1.,1.,1.,1.,
1.,1.,1.,1.,1.,1.,1.,1.,1.,1.,1.,1.,1.,1.,1.,1.,1.,1.,1.,1.,1.,1.,1.,1.,
1.,1.,1.,1.,1.,1.,1.,1.,1.,1.,1.,1.,1.,1.,1.,1.,1.,1.,1.,1.,1.,1.,1.,1.,
1.,1.,1.,1.,1.,1.,1.,1.,1.,1.,1.,1.,1.,1.,1.,1.,1.,1.,1.,1.,1.,1.,1.,1.,
1.,1.,1.,1.,1.,1.,1.,1.,1.,1.,1.,1.,1.,1.,1.,1.,1.,1.,1.,1.,1.,1.,1.,1.,
1.,1.,1.,1.,1.,1.,1.,1.,1.,1.,1.,1.,1.,1.,1.,1.,1.,1.,1.,1.,1.,1.,1.,1.,
1.,1.,1.,1.,1.,1.,1.,1.,1.,1.,1.,1.,1.,1.,1.,1.,1.,1.,1.,1.,1.,1.,1.,1.,
1.,1.,1.,1.,1.,1.,1.,1.,1.,1.))
REPRESENTATION_ITEM('')
);
#459=(
BOUNDED_CURVE()
B_SPLINE_CURVE(5,(#78121,#78122,#78123,#78124,#78125,#78126,#78127,#78128,
#78129,#78130,#78131,#78132,#78133,#78134,#78135,#78136,#78137,#78138,#78139,
#78140,#78141,#78142,#78143,#78144,#78145,#78146,#78147,#78148,#78149,#78150,
#78151,#78152,#78153,#78154,#78155,#78156,#78157,#78158,#78159,#78160,#78161,
#78162,#78163,#78164,#78165,#78166,#78167,#78168,#78169,#78170,#78171,#78172,
#78173,#78174,#78175,#78176,#78177,#78178,#78179,#78180,#78181,#78182,#78183,
#78184,#78185,#78186,#78187,#78188,#78189,#78190,#78191,#78192,#78193,#78194,
#78195,#78196,#78197,#78198,#78199,#78200,#78201,#78202,#78203,#78204,#78205,
#78206,#78207,#78208,#78209,#78210,#78211,#78212,#78213,#78214,#78215,#78216,
#78217,#78218,#78219,#78220,#78221,#78222,#78223,#78224,#78225,#78226,#78227,
#78228,#78229,#78230,#78231,#78232,#78233,#78234,#78235,#78236,#78237,#78238,
#78239,#78240,#78241,#78242,#78243,#78244,#78245,#78246,#78247,#78248,#78249,
#78250,#78251,#78252,#78253,#78254,#78255,#78256,#78257,#78258,#78259,#78260,
#78261,#78262,#78263,#78264,#78265,#78266,#78267,#78268,#78269,#78270,#78271,
#78272,#78273,#78274,#78275,#78276,#78277,#78278,#78279,#78280,#78281,#78282,
#78283,#78284,#78285,#78286,#78287,#78288,#78289,#78290,#78291,#78292,#78293,
#78294,#78295,#78296,#78297,#78298,#78299,#78300,#78301,#78302,#78303,#78304,
#78305,#78306,#78307,#78308,#78309,#78310,#78311,#78312,#78313,#78314),
 .UNSPECIFIED.,.F.,.F.)
B_SPLINE_CURVE_WITH_KNOTS((6,1,1,1,1,1,1,1,1,1,1,1,1,1,1,1,1,1,1,1,1,1,
1,1,1,1,1,1,1,1,1,1,1,1,1,1,1,1,1,1,1,1,1,1,1,1,1,1,1,1,1,1,1,1,1,1,1,1,
1,1,1,1,1,1,1,1,1,1,1,1,1,1,1,1,1,1,1,1,1,1,1,1,1,1,1,1,1,1,1,1,1,1,1,1,
1,1,1,1,1,1,1,1,1,1,1,1,1,1,1,1,1,1,1,1,1,1,1,1,1,1,1,1,1,1,1,1,1,1,1,1,
1,1,1,1,1,1,1,1,1,1,1,1,1,1,1,1,1,1,1,1,1,1,1,1,1,1,1,1,1,1,1,1,1,1,1,1,
1,1,1,1,1,1,1,1,1,1,1,1,1,1,1,1,1,1,1,1,1,1,1,6),(0.,0.005,0.01,0.015,0.02,
0.025,0.03,0.035,0.04,0.045,0.05,0.055,0.06,0.065,0.07,0.075,0.08,0.085,
0.09,0.095,0.1,0.105,0.11,0.115,0.12,0.125,0.13,0.135,0.14,0.145,0.15,0.155,
0.16,0.165,0.17,0.175,0.18,0.185,0.19,0.195,0.2,0.205,0.21,0.215,0.22,0.225,
0.23,0.235,0.24,0.245,0.25,0.255,0.26,0.265,0.27,0.275,0.28,0.285,0.29,
0.295,0.3,0.305,0.31,0.315,0.32,0.325,0.33,0.335,0.34,0.345,0.35,0.355,
0.36,0.365,0.37,0.375,0.38,0.385,0.39,0.395,0.4,0.405,0.41,0.415,0.42,0.425,
0.43,0.435,0.44,0.445,0.45,0.455,0.46,0.465,0.47,0.475,0.48,0.485,0.49,
0.495,0.5,0.505,0.51,0.515,0.52,0.525,0.53,0.535,0.54,0.545,0.55,0.555,
0.56,0.565,0.57,0.575,0.58,0.585,0.59,0.595,0.6,0.605,0.61,0.615,0.62,0.625,
0.63,0.635,0.64,0.645,0.65,0.655,0.66,0.665,0.67,0.675,0.68,0.685,0.690000000000001,
0.695000000000001,0.700000000000001,0.705000000000001,0.710000000000001,
0.715000000000001,0.720000000000001,0.725000000000001,0.730000000000001,
0.735000000000001,0.740000000000001,0.745000000000001,0.750000000000001,
0.755000000000001,0.760000000000001,0.765000000000001,0.770000000000001,
0.775000000000001,0.780000000000001,0.785000000000001,0.790000000000001,
0.795000000000001,0.800000000000001,0.805000000000001,0.810000000000001,
0.815000000000001,0.820000000000001,0.825000000000001,0.830000000000001,
0.835000000000001,0.840000000000001,0.845000000000001,0.850000000000001,
0.855000000000001,0.860000000000001,0.865000000000001,0.870000000000001,
0.875000000000001,0.880000000000001,0.885000000000001,0.890000000000001,
0.895000000000001,0.900000000000001,0.905000000000001,0.910000000000001,
0.915000000000001,0.920000000000001,0.925000000000001,0.930000000000001,
0.935000000000001,0.940000000000001,0.94142984443127),.UNSPECIFIED.)
CURVE()
GEOMETRIC_REPRESENTATION_ITEM()
RATIONAL_B_SPLINE_CURVE((1.,1.,1.,1.,1.,1.,1.,1.,1.,1.,1.,1.,1.,1.,1.,1.,
1.,1.,1.,1.,1.,1.,1.,1.,1.,1.,1.,1.,1.,1.,1.,1.,1.,1.,1.,1.,1.,1.,1.,1.,
1.,1.,1.,1.,1.,1.,1.,1.,1.,1.,1.,1.,1.,1.,1.,1.,1.,1.,1.,1.,1.,1.,1.,1.,
1.,1.,1.,1.,1.,1.,1.,1.,1.,1.,1.,1.,1.,1.,1.,1.,1.,1.,1.,1.,1.,1.,1.,1.,
1.,1.,1.,1.,1.,1.,1.,1.,1.,1.,1.,1.,1.,1.,1.,1.,1.,1.,1.,1.,1.,1.,1.,1.,
1.,1.,1.,1.,1.,1.,1.,1.,1.,1.,1.,1.,1.,1.,1.,1.,1.,1.,1.,1.,1.,1.,1.,1.,
1.,1.,1.,1.,1.,1.,1.,1.,1.,1.,1.,1.,1.,1.,1.,1.,1.,1.,1.,1.,1.,1.,1.,1.,
1.,1.,1.,1.,1.,1.,1.,1.,1.,1.,1.,1.,1.,1.,1.,1.,1.,1.,1.,1.,1.,1.,1.,1.,
1.,1.,1.,1.,1.,1.,1.,1.,1.,1.))
REPRESENTATION_ITEM('')
);
#460=(
BOUNDED_CURVE()
B_SPLINE_CURVE(5,(#78317,#78318,#78319,#78320,#78321,#78322,#78323,#78324,
#78325,#78326,#78327,#78328,#78329,#78330,#78331,#78332,#78333,#78334,#78335,
#78336,#78337,#78338,#78339,#78340,#78341,#78342,#78343,#78344,#78345,#78346,
#78347,#78348,#78349,#78350,#78351,#78352,#78353,#78354,#78355,#78356,#78357,
#78358,#78359,#78360,#78361,#78362,#78363,#78364,#78365,#78366,#78367,#78368,
#78369,#78370,#78371,#78372,#78373,#78374,#78375,#78376,#78377,#78378,#78379,
#78380,#78381,#78382,#78383,#78384,#78385,#78386,#78387,#78388,#78389,#78390,
#78391,#78392,#78393,#78394,#78395,#78396,#78397,#78398,#78399,#78400,#78401,
#78402,#78403,#78404,#78405,#78406,#78407,#78408,#78409,#78410,#78411,#78412,
#78413,#78414,#78415,#78416,#78417,#78418,#78419,#78420,#78421,#78422,#78423,
#78424,#78425,#78426,#78427,#78428,#78429,#78430,#78431,#78432,#78433,#78434,
#78435,#78436,#78437,#78438,#78439,#78440,#78441,#78442,#78443,#78444,#78445,
#78446,#78447,#78448,#78449,#78450,#78451,#78452,#78453,#78454,#78455,#78456,
#78457,#78458,#78459,#78460,#78461,#78462,#78463,#78464,#78465,#78466,#78467,
#78468,#78469,#78470,#78471,#78472,#78473,#78474,#78475,#78476,#78477,#78478,
#78479,#78480,#78481,#78482,#78483,#78484,#78485,#78486,#78487,#78488,#78489,
#78490,#78491,#78492,#78493,#78494,#78495,#78496,#78497,#78498,#78499,#78500,
#78501,#78502,#78503,#78504,#78505,#78506,#78507,#78508,#78509,#78510),
 .UNSPECIFIED.,.F.,.F.)
B_SPLINE_CURVE_WITH_KNOTS((6,1,1,1,1,1,1,1,1,1,1,1,1,1,1,1,1,1,1,1,1,1,
1,1,1,1,1,1,1,1,1,1,1,1,1,1,1,1,1,1,1,1,1,1,1,1,1,1,1,1,1,1,1,1,1,1,1,1,
1,1,1,1,1,1,1,1,1,1,1,1,1,1,1,1,1,1,1,1,1,1,1,1,1,1,1,1,1,1,1,1,1,1,1,1,
1,1,1,1,1,1,1,1,1,1,1,1,1,1,1,1,1,1,1,1,1,1,1,1,1,1,1,1,1,1,1,1,1,1,1,1,
1,1,1,1,1,1,1,1,1,1,1,1,1,1,1,1,1,1,1,1,1,1,1,1,1,1,1,1,1,1,1,1,1,1,1,1,
1,1,1,1,1,1,1,1,1,1,1,1,1,1,1,1,1,1,1,1,1,1,1,6),(-0.941429844431257,-0.940000000000001,
-0.935000000000001,-0.930000000000001,-0.925000000000001,-0.920000000000001,
-0.915000000000001,-0.910000000000001,-0.905000000000001,-0.900000000000001,
-0.895000000000001,-0.890000000000001,-0.885000000000001,-0.880000000000001,
-0.875000000000001,-0.870000000000001,-0.865000000000001,-0.860000000000001,
-0.855000000000001,-0.850000000000001,-0.845000000000001,-0.840000000000001,
-0.835000000000001,-0.830000000000001,-0.825000000000001,-0.820000000000001,
-0.815000000000001,-0.810000000000001,-0.805000000000001,-0.800000000000001,
-0.795000000000001,-0.790000000000001,-0.785000000000001,-0.780000000000001,
-0.775000000000001,-0.770000000000001,-0.765000000000001,-0.760000000000001,
-0.755000000000001,-0.750000000000001,-0.745000000000001,-0.740000000000001,
-0.735000000000001,-0.730000000000001,-0.725000000000001,-0.720000000000001,
-0.715000000000001,-0.710000000000001,-0.705000000000001,-0.700000000000001,
-0.695000000000001,-0.690000000000001,-0.685,-0.68,-0.675,-0.67,-0.665,
-0.66,-0.655,-0.65,-0.645,-0.64,-0.635,-0.63,-0.625,-0.62,-0.615,-0.61,
-0.605,-0.6,-0.595,-0.59,-0.585,-0.58,-0.575,-0.57,-0.565,-0.56,-0.555,
-0.55,-0.545,-0.54,-0.535,-0.53,-0.525,-0.52,-0.515,-0.51,-0.505,-0.5,-0.495,
-0.49,-0.485,-0.48,-0.475,-0.47,-0.465,-0.46,-0.455,-0.45,-0.445,-0.44,
-0.435,-0.43,-0.425,-0.42,-0.415,-0.41,-0.405,-0.4,-0.395,-0.39,-0.385,
-0.38,-0.375,-0.37,-0.365,-0.36,-0.355,-0.35,-0.345,-0.34,-0.335,-0.33,
-0.325,-0.32,-0.315,-0.31,-0.305,-0.3,-0.295,-0.29,-0.285,-0.28,-0.275,
-0.27,-0.265,-0.26,-0.255,-0.25,-0.245,-0.24,-0.235,-0.23,-0.225,-0.22,
-0.215,-0.21,-0.205,-0.2,-0.195,-0.19,-0.185,-0.18,-0.175,-0.17,-0.165,
-0.16,-0.155,-0.15,-0.145,-0.14,-0.135,-0.13,-0.125,-0.12,-0.115,-0.11,
-0.105,-0.1,-0.095,-0.09,-0.085,-0.08,-0.075,-0.07,-0.065,-0.06,-0.055,
-0.05,-0.045,-0.04,-0.035,-0.03,-0.025,-0.02,-0.015,-0.01,-0.005,0.),
 .UNSPECIFIED.)
CURVE()
GEOMETRIC_REPRESENTATION_ITEM()
RATIONAL_B_SPLINE_CURVE((1.,1.,1.,1.,1.,1.,1.,1.,1.,1.,1.,1.,1.,1.,1.,1.,
1.,1.,1.,1.,1.,1.,1.,1.,1.,1.,1.,1.,1.,1.,1.,1.,1.,1.,1.,1.,1.,1.,1.,1.,
1.,1.,1.,1.,1.,1.,1.,1.,1.,1.,1.,1.,1.,1.,1.,1.,1.,1.,1.,1.,1.,1.,1.,1.,
1.,1.,1.,1.,1.,1.,1.,1.,1.,1.,1.,1.,1.,1.,1.,1.,1.,1.,1.,1.,1.,1.,1.,1.,
1.,1.,1.,1.,1.,1.,1.,1.,1.,1.,1.,1.,1.,1.,1.,1.,1.,1.,1.,1.,1.,1.,1.,1.,
1.,1.,1.,1.,1.,1.,1.,1.,1.,1.,1.,1.,1.,1.,1.,1.,1.,1.,1.,1.,1.,1.,1.,1.,
1.,1.,1.,1.,1.,1.,1.,1.,1.,1.,1.,1.,1.,1.,1.,1.,1.,1.,1.,1.,1.,1.,1.,1.,
1.,1.,1.,1.,1.,1.,1.,1.,1.,1.,1.,1.,1.,1.,1.,1.,1.,1.,1.,1.,1.,1.,1.,1.,
1.,1.,1.,1.,1.,1.,1.,1.,1.,1.))
REPRESENTATION_ITEM('')
);
#461=(
BOUNDED_CURVE()
B_SPLINE_CURVE(5,(#79017,#79018,#79019,#79020,#79021,#79022,#79023,#79024,
#79025,#79026,#79027,#79028,#79029,#79030,#79031,#79032,#79033,#79034,#79035,
#79036,#79037,#79038,#79039,#79040,#79041,#79042,#79043,#79044,#79045,#79046,
#79047,#79048,#79049,#79050,#79051,#79052,#79053,#79054,#79055,#79056,#79057,
#79058,#79059,#79060,#79061,#79062,#79063,#79064,#79065,#79066,#79067,#79068,
#79069,#79070,#79071,#79072,#79073,#79074,#79075,#79076,#79077,#79078,#79079,
#79080,#79081,#79082,#79083,#79084,#79085,#79086,#79087,#79088,#79089,#79090,
#79091,#79092,#79093,#79094,#79095,#79096,#79097,#79098,#79099,#79100,#79101,
#79102,#79103,#79104,#79105,#79106,#79107,#79108,#79109,#79110,#79111,#79112,
#79113,#79114,#79115,#79116,#79117,#79118,#79119,#79120,#79121,#79122,#79123,
#79124,#79125,#79126,#79127,#79128,#79129,#79130,#79131,#79132,#79133,#79134,
#79135,#79136,#79137,#79138,#79139,#79140,#79141,#79142,#79143,#79144,#79145,
#79146,#79147,#79148,#79149,#79150,#79151,#79152,#79153,#79154,#79155,#79156,
#79157,#79158,#79159,#79160,#79161,#79162,#79163,#79164,#79165,#79166,#79167,
#79168,#79169,#79170,#79171,#79172,#79173,#79174,#79175,#79176,#79177,#79178,
#79179,#79180,#79181,#79182,#79183,#79184,#79185,#79186,#79187,#79188,#79189,
#79190,#79191,#79192,#79193,#79194,#79195,#79196,#79197,#79198,#79199,#79200,
#79201,#79202,#79203,#79204,#79205,#79206,#79207,#79208,#79209,#79210),
 .UNSPECIFIED.,.F.,.F.)
B_SPLINE_CURVE_WITH_KNOTS((6,1,1,1,1,1,1,1,1,1,1,1,1,1,1,1,1,1,1,1,1,1,
1,1,1,1,1,1,1,1,1,1,1,1,1,1,1,1,1,1,1,1,1,1,1,1,1,1,1,1,1,1,1,1,1,1,1,1,
1,1,1,1,1,1,1,1,1,1,1,1,1,1,1,1,1,1,1,1,1,1,1,1,1,1,1,1,1,1,1,1,1,1,1,1,
1,1,1,1,1,1,1,1,1,1,1,1,1,1,1,1,1,1,1,1,1,1,1,1,1,1,1,1,1,1,1,1,1,1,1,1,
1,1,1,1,1,1,1,1,1,1,1,1,1,1,1,1,1,1,1,1,1,1,1,1,1,1,1,1,1,1,1,1,1,1,1,1,
1,1,1,1,1,1,1,1,1,1,1,1,1,1,1,1,1,1,1,1,1,1,1,6),(0.,0.005,0.01,0.015,0.02,
0.025,0.03,0.035,0.04,0.045,0.05,0.055,0.06,0.065,0.07,0.075,0.08,0.085,
0.09,0.095,0.1,0.105,0.11,0.115,0.12,0.125,0.13,0.135,0.14,0.145,0.15,0.155,
0.16,0.165,0.17,0.175,0.18,0.185,0.19,0.195,0.2,0.205,0.21,0.215,0.22,0.225,
0.23,0.235,0.24,0.245,0.25,0.255,0.26,0.265,0.27,0.275,0.28,0.285,0.29,
0.295,0.3,0.305,0.31,0.315,0.32,0.325,0.33,0.335,0.34,0.345,0.35,0.355,
0.36,0.365,0.37,0.375,0.38,0.385,0.39,0.395,0.4,0.405,0.41,0.415,0.42,0.425,
0.43,0.435,0.44,0.445,0.45,0.455,0.46,0.465,0.47,0.475,0.48,0.485,0.49,
0.495,0.5,0.505,0.51,0.515,0.52,0.525,0.53,0.535,0.54,0.545,0.55,0.555,
0.56,0.565,0.57,0.575,0.58,0.585,0.59,0.595,0.6,0.605,0.61,0.615,0.62,0.625,
0.63,0.635,0.64,0.645,0.65,0.655,0.66,0.665,0.67,0.675,0.68,0.685,0.690000000000001,
0.695000000000001,0.700000000000001,0.705000000000001,0.710000000000001,
0.715000000000001,0.720000000000001,0.725000000000001,0.730000000000001,
0.735000000000001,0.740000000000001,0.745000000000001,0.750000000000001,
0.755000000000001,0.760000000000001,0.765000000000001,0.770000000000001,
0.775000000000001,0.780000000000001,0.785000000000001,0.790000000000001,
0.795000000000001,0.800000000000001,0.805000000000001,0.810000000000001,
0.815000000000001,0.820000000000001,0.825000000000001,0.830000000000001,
0.835000000000001,0.840000000000001,0.845000000000001,0.850000000000001,
0.855000000000001,0.860000000000001,0.865000000000001,0.870000000000001,
0.875000000000001,0.880000000000001,0.885000000000001,0.890000000000001,
0.895000000000001,0.900000000000001,0.905000000000001,0.910000000000001,
0.915000000000001,0.920000000000001,0.925000000000001,0.930000000000001,
0.935000000000001,0.940000000000001,0.941429844431219),.UNSPECIFIED.)
CURVE()
GEOMETRIC_REPRESENTATION_ITEM()
RATIONAL_B_SPLINE_CURVE((1.,1.,1.,1.,1.,1.,1.,1.,1.,1.,1.,1.,1.,1.,1.,1.,
1.,1.,1.,1.,1.,1.,1.,1.,1.,1.,1.,1.,1.,1.,1.,1.,1.,1.,1.,1.,1.,1.,1.,1.,
1.,1.,1.,1.,1.,1.,1.,1.,1.,1.,1.,1.,1.,1.,1.,1.,1.,1.,1.,1.,1.,1.,1.,1.,
1.,1.,1.,1.,1.,1.,1.,1.,1.,1.,1.,1.,1.,1.,1.,1.,1.,1.,1.,1.,1.,1.,1.,1.,
1.,1.,1.,1.,1.,1.,1.,1.,1.,1.,1.,1.,1.,1.,1.,1.,1.,1.,1.,1.,1.,1.,1.,1.,
1.,1.,1.,1.,1.,1.,1.,1.,1.,1.,1.,1.,1.,1.,1.,1.,1.,1.,1.,1.,1.,1.,1.,1.,
1.,1.,1.,1.,1.,1.,1.,1.,1.,1.,1.,1.,1.,1.,1.,1.,1.,1.,1.,1.,1.,1.,1.,1.,
1.,1.,1.,1.,1.,1.,1.,1.,1.,1.,1.,1.,1.,1.,1.,1.,1.,1.,1.,1.,1.,1.,1.,1.,
1.,1.,1.,1.,1.,1.,1.,1.,1.,1.))
REPRESENTATION_ITEM('')
);
#462=(
BOUNDED_CURVE()
B_SPLINE_CURVE(5,(#79213,#79214,#79215,#79216,#79217,#79218,#79219,#79220,
#79221,#79222,#79223,#79224,#79225,#79226,#79227,#79228,#79229,#79230,#79231,
#79232,#79233,#79234,#79235,#79236,#79237,#79238,#79239,#79240,#79241,#79242,
#79243,#79244,#79245,#79246,#79247,#79248,#79249,#79250,#79251,#79252,#79253,
#79254,#79255,#79256,#79257,#79258,#79259,#79260,#79261,#79262,#79263,#79264,
#79265,#79266,#79267,#79268,#79269,#79270,#79271,#79272,#79273,#79274,#79275,
#79276,#79277,#79278,#79279,#79280,#79281,#79282,#79283,#79284,#79285,#79286,
#79287,#79288,#79289,#79290,#79291,#79292,#79293,#79294,#79295,#79296,#79297,
#79298,#79299,#79300,#79301,#79302,#79303,#79304,#79305,#79306,#79307,#79308,
#79309,#79310,#79311,#79312,#79313,#79314,#79315,#79316,#79317,#79318,#79319,
#79320,#79321,#79322,#79323,#79324,#79325,#79326,#79327,#79328,#79329,#79330,
#79331,#79332,#79333,#79334,#79335,#79336,#79337,#79338,#79339,#79340,#79341,
#79342,#79343,#79344,#79345,#79346,#79347,#79348,#79349,#79350,#79351,#79352,
#79353,#79354,#79355,#79356,#79357,#79358,#79359,#79360,#79361,#79362,#79363,
#79364,#79365,#79366,#79367,#79368,#79369,#79370,#79371,#79372,#79373,#79374,
#79375,#79376,#79377,#79378,#79379,#79380,#79381,#79382,#79383,#79384,#79385,
#79386,#79387,#79388,#79389,#79390,#79391,#79392,#79393,#79394,#79395,#79396,
#79397,#79398,#79399,#79400,#79401,#79402,#79403,#79404,#79405,#79406),
 .UNSPECIFIED.,.F.,.F.)
B_SPLINE_CURVE_WITH_KNOTS((6,1,1,1,1,1,1,1,1,1,1,1,1,1,1,1,1,1,1,1,1,1,
1,1,1,1,1,1,1,1,1,1,1,1,1,1,1,1,1,1,1,1,1,1,1,1,1,1,1,1,1,1,1,1,1,1,1,1,
1,1,1,1,1,1,1,1,1,1,1,1,1,1,1,1,1,1,1,1,1,1,1,1,1,1,1,1,1,1,1,1,1,1,1,1,
1,1,1,1,1,1,1,1,1,1,1,1,1,1,1,1,1,1,1,1,1,1,1,1,1,1,1,1,1,1,1,1,1,1,1,1,
1,1,1,1,1,1,1,1,1,1,1,1,1,1,1,1,1,1,1,1,1,1,1,1,1,1,1,1,1,1,1,1,1,1,1,1,
1,1,1,1,1,1,1,1,1,1,1,1,1,1,1,1,1,1,1,1,1,1,1,6),(-0.94142984443126,-0.940000000000001,
-0.935000000000001,-0.930000000000001,-0.925000000000001,-0.920000000000001,
-0.915000000000001,-0.910000000000001,-0.905000000000001,-0.900000000000001,
-0.895000000000001,-0.890000000000001,-0.885000000000001,-0.880000000000001,
-0.875000000000001,-0.870000000000001,-0.865000000000001,-0.860000000000001,
-0.855000000000001,-0.850000000000001,-0.845000000000001,-0.840000000000001,
-0.835000000000001,-0.830000000000001,-0.825000000000001,-0.820000000000001,
-0.815000000000001,-0.810000000000001,-0.805000000000001,-0.800000000000001,
-0.795000000000001,-0.790000000000001,-0.785000000000001,-0.780000000000001,
-0.775000000000001,-0.770000000000001,-0.765000000000001,-0.760000000000001,
-0.755000000000001,-0.750000000000001,-0.745000000000001,-0.740000000000001,
-0.735000000000001,-0.730000000000001,-0.725000000000001,-0.720000000000001,
-0.715000000000001,-0.710000000000001,-0.705000000000001,-0.700000000000001,
-0.695000000000001,-0.690000000000001,-0.685,-0.68,-0.675,-0.67,-0.665,
-0.66,-0.655,-0.65,-0.645,-0.64,-0.635,-0.63,-0.625,-0.62,-0.615,-0.61,
-0.605,-0.6,-0.595,-0.59,-0.585,-0.58,-0.575,-0.57,-0.565,-0.56,-0.555,
-0.55,-0.545,-0.54,-0.535,-0.53,-0.525,-0.52,-0.515,-0.51,-0.505,-0.5,-0.495,
-0.49,-0.485,-0.48,-0.475,-0.47,-0.465,-0.46,-0.455,-0.45,-0.445,-0.44,
-0.435,-0.43,-0.425,-0.42,-0.415,-0.41,-0.405,-0.4,-0.395,-0.39,-0.385,
-0.38,-0.375,-0.37,-0.365,-0.36,-0.355,-0.35,-0.345,-0.34,-0.335,-0.33,
-0.325,-0.32,-0.315,-0.31,-0.305,-0.3,-0.295,-0.29,-0.285,-0.28,-0.275,
-0.27,-0.265,-0.26,-0.255,-0.25,-0.245,-0.24,-0.235,-0.23,-0.225,-0.22,
-0.215,-0.21,-0.205,-0.2,-0.195,-0.19,-0.185,-0.18,-0.175,-0.17,-0.165,
-0.16,-0.155,-0.15,-0.145,-0.14,-0.135,-0.13,-0.125,-0.12,-0.115,-0.11,
-0.105,-0.1,-0.095,-0.09,-0.085,-0.08,-0.075,-0.07,-0.065,-0.06,-0.055,
-0.05,-0.045,-0.04,-0.035,-0.03,-0.025,-0.02,-0.015,-0.01,-0.005,0.),
 .UNSPECIFIED.)
CURVE()
GEOMETRIC_REPRESENTATION_ITEM()
RATIONAL_B_SPLINE_CURVE((1.,1.,1.,1.,1.,1.,1.,1.,1.,1.,1.,1.,1.,1.,1.,1.,
1.,1.,1.,1.,1.,1.,1.,1.,1.,1.,1.,1.,1.,1.,1.,1.,1.,1.,1.,1.,1.,1.,1.,1.,
1.,1.,1.,1.,1.,1.,1.,1.,1.,1.,1.,1.,1.,1.,1.,1.,1.,1.,1.,1.,1.,1.,1.,1.,
1.,1.,1.,1.,1.,1.,1.,1.,1.,1.,1.,1.,1.,1.,1.,1.,1.,1.,1.,1.,1.,1.,1.,1.,
1.,1.,1.,1.,1.,1.,1.,1.,1.,1.,1.,1.,1.,1.,1.,1.,1.,1.,1.,1.,1.,1.,1.,1.,
1.,1.,1.,1.,1.,1.,1.,1.,1.,1.,1.,1.,1.,1.,1.,1.,1.,1.,1.,1.,1.,1.,1.,1.,
1.,1.,1.,1.,1.,1.,1.,1.,1.,1.,1.,1.,1.,1.,1.,1.,1.,1.,1.,1.,1.,1.,1.,1.,
1.,1.,1.,1.,1.,1.,1.,1.,1.,1.,1.,1.,1.,1.,1.,1.,1.,1.,1.,1.,1.,1.,1.,1.,
1.,1.,1.,1.,1.,1.,1.,1.,1.,1.))
REPRESENTATION_ITEM('')
);
#463=(
BOUNDED_CURVE()
B_SPLINE_CURVE(5,(#79913,#79914,#79915,#79916,#79917,#79918,#79919,#79920,
#79921,#79922,#79923,#79924,#79925,#79926,#79927,#79928,#79929,#79930,#79931,
#79932,#79933,#79934,#79935,#79936,#79937,#79938,#79939,#79940,#79941,#79942,
#79943,#79944,#79945,#79946,#79947,#79948,#79949,#79950,#79951,#79952,#79953,
#79954,#79955,#79956,#79957,#79958,#79959,#79960,#79961,#79962,#79963,#79964,
#79965,#79966,#79967,#79968,#79969,#79970,#79971,#79972,#79973,#79974,#79975,
#79976,#79977,#79978,#79979,#79980,#79981,#79982,#79983,#79984,#79985,#79986,
#79987,#79988,#79989,#79990,#79991,#79992,#79993,#79994,#79995,#79996,#79997,
#79998,#79999,#80000,#80001,#80002,#80003,#80004,#80005,#80006,#80007,#80008,
#80009,#80010,#80011,#80012,#80013,#80014,#80015,#80016,#80017,#80018,#80019,
#80020,#80021,#80022,#80023,#80024,#80025,#80026,#80027,#80028,#80029,#80030,
#80031,#80032,#80033,#80034,#80035,#80036,#80037,#80038,#80039,#80040,#80041,
#80042,#80043,#80044,#80045,#80046,#80047,#80048,#80049,#80050,#80051,#80052,
#80053,#80054,#80055,#80056,#80057,#80058,#80059,#80060,#80061,#80062,#80063,
#80064,#80065,#80066,#80067,#80068,#80069,#80070,#80071,#80072,#80073,#80074,
#80075,#80076,#80077,#80078,#80079,#80080,#80081,#80082,#80083,#80084,#80085,
#80086,#80087,#80088,#80089,#80090,#80091,#80092,#80093,#80094,#80095,#80096,
#80097,#80098,#80099,#80100,#80101,#80102,#80103,#80104,#80105,#80106),
 .UNSPECIFIED.,.F.,.F.)
B_SPLINE_CURVE_WITH_KNOTS((6,1,1,1,1,1,1,1,1,1,1,1,1,1,1,1,1,1,1,1,1,1,
1,1,1,1,1,1,1,1,1,1,1,1,1,1,1,1,1,1,1,1,1,1,1,1,1,1,1,1,1,1,1,1,1,1,1,1,
1,1,1,1,1,1,1,1,1,1,1,1,1,1,1,1,1,1,1,1,1,1,1,1,1,1,1,1,1,1,1,1,1,1,1,1,
1,1,1,1,1,1,1,1,1,1,1,1,1,1,1,1,1,1,1,1,1,1,1,1,1,1,1,1,1,1,1,1,1,1,1,1,
1,1,1,1,1,1,1,1,1,1,1,1,1,1,1,1,1,1,1,1,1,1,1,1,1,1,1,1,1,1,1,1,1,1,1,1,
1,1,1,1,1,1,1,1,1,1,1,1,1,1,1,1,1,1,1,1,1,1,1,6),(0.,0.005,0.01,0.015,0.02,
0.025,0.03,0.035,0.04,0.045,0.05,0.055,0.06,0.065,0.07,0.075,0.08,0.085,
0.09,0.095,0.1,0.105,0.11,0.115,0.12,0.125,0.13,0.135,0.14,0.145,0.15,0.155,
0.16,0.165,0.17,0.175,0.18,0.185,0.19,0.195,0.2,0.205,0.21,0.215,0.22,0.225,
0.23,0.235,0.24,0.245,0.25,0.255,0.26,0.265,0.27,0.275,0.28,0.285,0.29,
0.295,0.3,0.305,0.31,0.315,0.32,0.325,0.33,0.335,0.34,0.345,0.35,0.355,
0.36,0.365,0.37,0.375,0.38,0.385,0.39,0.395,0.4,0.405,0.41,0.415,0.42,0.425,
0.43,0.435,0.44,0.445,0.45,0.455,0.46,0.465,0.47,0.475,0.48,0.485,0.49,
0.495,0.5,0.505,0.51,0.515,0.52,0.525,0.53,0.535,0.54,0.545,0.55,0.555,
0.56,0.565,0.57,0.575,0.58,0.585,0.59,0.595,0.6,0.605,0.61,0.615,0.62,0.625,
0.63,0.635,0.64,0.645,0.65,0.655,0.66,0.665,0.67,0.675,0.68,0.685,0.690000000000001,
0.695000000000001,0.700000000000001,0.705000000000001,0.710000000000001,
0.715000000000001,0.720000000000001,0.725000000000001,0.730000000000001,
0.735000000000001,0.740000000000001,0.745000000000001,0.750000000000001,
0.755000000000001,0.760000000000001,0.765000000000001,0.770000000000001,
0.775000000000001,0.780000000000001,0.785000000000001,0.790000000000001,
0.795000000000001,0.800000000000001,0.805000000000001,0.810000000000001,
0.815000000000001,0.820000000000001,0.825000000000001,0.830000000000001,
0.835000000000001,0.840000000000001,0.845000000000001,0.850000000000001,
0.855000000000001,0.860000000000001,0.865000000000001,0.870000000000001,
0.875000000000001,0.880000000000001,0.885000000000001,0.890000000000001,
0.895000000000001,0.900000000000001,0.905000000000001,0.910000000000001,
0.915000000000001,0.920000000000001,0.925000000000001,0.930000000000001,
0.935000000000001,0.940000000000001,0.941429844431402),.UNSPECIFIED.)
CURVE()
GEOMETRIC_REPRESENTATION_ITEM()
RATIONAL_B_SPLINE_CURVE((1.,1.,1.,1.,1.,1.,1.,1.,1.,1.,1.,1.,1.,1.,1.,1.,
1.,1.,1.,1.,1.,1.,1.,1.,1.,1.,1.,1.,1.,1.,1.,1.,1.,1.,1.,1.,1.,1.,1.,1.,
1.,1.,1.,1.,1.,1.,1.,1.,1.,1.,1.,1.,1.,1.,1.,1.,1.,1.,1.,1.,1.,1.,1.,1.,
1.,1.,1.,1.,1.,1.,1.,1.,1.,1.,1.,1.,1.,1.,1.,1.,1.,1.,1.,1.,1.,1.,1.,1.,
1.,1.,1.,1.,1.,1.,1.,1.,1.,1.,1.,1.,1.,1.,1.,1.,1.,1.,1.,1.,1.,1.,1.,1.,
1.,1.,1.,1.,1.,1.,1.,1.,1.,1.,1.,1.,1.,1.,1.,1.,1.,1.,1.,1.,1.,1.,1.,1.,
1.,1.,1.,1.,1.,1.,1.,1.,1.,1.,1.,1.,1.,1.,1.,1.,1.,1.,1.,1.,1.,1.,1.,1.,
1.,1.,1.,1.,1.,1.,1.,1.,1.,1.,1.,1.,1.,1.,1.,1.,1.,1.,1.,1.,1.,1.,1.,1.,
1.,1.,1.,1.,1.,1.,1.,1.,1.,1.))
REPRESENTATION_ITEM('')
);
#464=(
BOUNDED_CURVE()
B_SPLINE_CURVE(5,(#80109,#80110,#80111,#80112,#80113,#80114,#80115,#80116,
#80117,#80118,#80119,#80120,#80121,#80122,#80123,#80124,#80125,#80126,#80127,
#80128,#80129,#80130,#80131,#80132,#80133,#80134,#80135,#80136,#80137,#80138,
#80139,#80140,#80141,#80142,#80143,#80144,#80145,#80146,#80147,#80148,#80149,
#80150,#80151,#80152,#80153,#80154,#80155,#80156,#80157,#80158,#80159,#80160,
#80161,#80162,#80163,#80164,#80165,#80166,#80167,#80168,#80169,#80170,#80171,
#80172,#80173,#80174,#80175,#80176,#80177,#80178,#80179,#80180,#80181,#80182,
#80183,#80184,#80185,#80186,#80187,#80188,#80189,#80190,#80191,#80192,#80193,
#80194,#80195,#80196,#80197,#80198,#80199,#80200,#80201,#80202,#80203,#80204,
#80205,#80206,#80207,#80208,#80209,#80210,#80211,#80212,#80213,#80214,#80215,
#80216,#80217,#80218,#80219,#80220,#80221,#80222,#80223,#80224,#80225,#80226,
#80227,#80228,#80229,#80230,#80231,#80232,#80233,#80234,#80235,#80236,#80237,
#80238,#80239,#80240,#80241,#80242,#80243,#80244,#80245,#80246,#80247,#80248,
#80249,#80250,#80251,#80252,#80253,#80254,#80255,#80256,#80257,#80258,#80259,
#80260,#80261,#80262,#80263,#80264,#80265,#80266,#80267,#80268,#80269,#80270,
#80271,#80272,#80273,#80274,#80275,#80276,#80277,#80278,#80279,#80280,#80281,
#80282,#80283,#80284,#80285,#80286,#80287,#80288,#80289,#80290,#80291,#80292,
#80293,#80294,#80295,#80296,#80297,#80298,#80299,#80300,#80301,#80302),
 .UNSPECIFIED.,.F.,.F.)
B_SPLINE_CURVE_WITH_KNOTS((6,1,1,1,1,1,1,1,1,1,1,1,1,1,1,1,1,1,1,1,1,1,
1,1,1,1,1,1,1,1,1,1,1,1,1,1,1,1,1,1,1,1,1,1,1,1,1,1,1,1,1,1,1,1,1,1,1,1,
1,1,1,1,1,1,1,1,1,1,1,1,1,1,1,1,1,1,1,1,1,1,1,1,1,1,1,1,1,1,1,1,1,1,1,1,
1,1,1,1,1,1,1,1,1,1,1,1,1,1,1,1,1,1,1,1,1,1,1,1,1,1,1,1,1,1,1,1,1,1,1,1,
1,1,1,1,1,1,1,1,1,1,1,1,1,1,1,1,1,1,1,1,1,1,1,1,1,1,1,1,1,1,1,1,1,1,1,1,
1,1,1,1,1,1,1,1,1,1,1,1,1,1,1,1,1,1,1,1,1,1,1,6),(-0.941429844431404,-0.940000000000001,
-0.935000000000001,-0.930000000000001,-0.925000000000001,-0.920000000000001,
-0.915000000000001,-0.910000000000001,-0.905000000000001,-0.900000000000001,
-0.895000000000001,-0.890000000000001,-0.885000000000001,-0.880000000000001,
-0.875000000000001,-0.870000000000001,-0.865000000000001,-0.860000000000001,
-0.855000000000001,-0.850000000000001,-0.845000000000001,-0.840000000000001,
-0.835000000000001,-0.830000000000001,-0.825000000000001,-0.820000000000001,
-0.815000000000001,-0.810000000000001,-0.805000000000001,-0.800000000000001,
-0.795000000000001,-0.790000000000001,-0.785000000000001,-0.780000000000001,
-0.775000000000001,-0.770000000000001,-0.765000000000001,-0.760000000000001,
-0.755000000000001,-0.750000000000001,-0.745000000000001,-0.740000000000001,
-0.735000000000001,-0.730000000000001,-0.725000000000001,-0.720000000000001,
-0.715000000000001,-0.710000000000001,-0.705000000000001,-0.700000000000001,
-0.695000000000001,-0.690000000000001,-0.685,-0.68,-0.675,-0.67,-0.665,
-0.66,-0.655,-0.65,-0.645,-0.64,-0.635,-0.63,-0.625,-0.62,-0.615,-0.61,
-0.605,-0.6,-0.595,-0.59,-0.585,-0.58,-0.575,-0.57,-0.565,-0.56,-0.555,
-0.55,-0.545,-0.54,-0.535,-0.53,-0.525,-0.52,-0.515,-0.51,-0.505,-0.5,-0.495,
-0.49,-0.485,-0.48,-0.475,-0.47,-0.465,-0.46,-0.455,-0.45,-0.445,-0.44,
-0.435,-0.43,-0.425,-0.42,-0.415,-0.41,-0.405,-0.4,-0.395,-0.39,-0.385,
-0.38,-0.375,-0.37,-0.365,-0.36,-0.355,-0.35,-0.345,-0.34,-0.335,-0.33,
-0.325,-0.32,-0.315,-0.31,-0.305,-0.3,-0.295,-0.29,-0.285,-0.28,-0.275,
-0.27,-0.265,-0.26,-0.255,-0.25,-0.245,-0.24,-0.235,-0.23,-0.225,-0.22,
-0.215,-0.21,-0.205,-0.2,-0.195,-0.19,-0.185,-0.18,-0.175,-0.17,-0.165,
-0.16,-0.155,-0.15,-0.145,-0.14,-0.135,-0.13,-0.125,-0.12,-0.115,-0.11,
-0.105,-0.1,-0.095,-0.09,-0.085,-0.08,-0.075,-0.07,-0.065,-0.06,-0.055,
-0.05,-0.045,-0.04,-0.035,-0.03,-0.025,-0.02,-0.015,-0.01,-0.005,0.),
 .UNSPECIFIED.)
CURVE()
GEOMETRIC_REPRESENTATION_ITEM()
RATIONAL_B_SPLINE_CURVE((1.,1.,1.,1.,1.,1.,1.,1.,1.,1.,1.,1.,1.,1.,1.,1.,
1.,1.,1.,1.,1.,1.,1.,1.,1.,1.,1.,1.,1.,1.,1.,1.,1.,1.,1.,1.,1.,1.,1.,1.,
1.,1.,1.,1.,1.,1.,1.,1.,1.,1.,1.,1.,1.,1.,1.,1.,1.,1.,1.,1.,1.,1.,1.,1.,
1.,1.,1.,1.,1.,1.,1.,1.,1.,1.,1.,1.,1.,1.,1.,1.,1.,1.,1.,1.,1.,1.,1.,1.,
1.,1.,1.,1.,1.,1.,1.,1.,1.,1.,1.,1.,1.,1.,1.,1.,1.,1.,1.,1.,1.,1.,1.,1.,
1.,1.,1.,1.,1.,1.,1.,1.,1.,1.,1.,1.,1.,1.,1.,1.,1.,1.,1.,1.,1.,1.,1.,1.,
1.,1.,1.,1.,1.,1.,1.,1.,1.,1.,1.,1.,1.,1.,1.,1.,1.,1.,1.,1.,1.,1.,1.,1.,
1.,1.,1.,1.,1.,1.,1.,1.,1.,1.,1.,1.,1.,1.,1.,1.,1.,1.,1.,1.,1.,1.,1.,1.,
1.,1.,1.,1.,1.,1.,1.,1.,1.,1.))
REPRESENTATION_ITEM('')
);
#465=(
BOUNDED_CURVE()
B_SPLINE_CURVE(5,(#80809,#80810,#80811,#80812,#80813,#80814,#80815,#80816,
#80817,#80818,#80819,#80820,#80821,#80822,#80823,#80824,#80825,#80826,#80827,
#80828,#80829,#80830,#80831,#80832,#80833,#80834,#80835,#80836,#80837,#80838,
#80839,#80840,#80841,#80842,#80843,#80844,#80845,#80846,#80847,#80848,#80849,
#80850,#80851,#80852,#80853,#80854,#80855,#80856,#80857,#80858,#80859,#80860,
#80861,#80862,#80863,#80864,#80865,#80866,#80867,#80868,#80869,#80870,#80871,
#80872,#80873,#80874,#80875,#80876,#80877,#80878,#80879,#80880,#80881,#80882,
#80883,#80884,#80885,#80886,#80887,#80888,#80889,#80890,#80891,#80892,#80893,
#80894,#80895,#80896,#80897,#80898,#80899,#80900,#80901,#80902,#80903,#80904,
#80905,#80906,#80907,#80908,#80909,#80910,#80911,#80912,#80913,#80914,#80915,
#80916,#80917,#80918,#80919,#80920,#80921,#80922,#80923,#80924,#80925,#80926,
#80927,#80928,#80929,#80930,#80931,#80932,#80933,#80934,#80935,#80936,#80937,
#80938,#80939,#80940,#80941,#80942,#80943,#80944,#80945,#80946,#80947,#80948,
#80949,#80950,#80951,#80952,#80953,#80954,#80955,#80956,#80957,#80958,#80959,
#80960,#80961,#80962,#80963,#80964,#80965,#80966,#80967,#80968,#80969,#80970,
#80971,#80972,#80973,#80974,#80975,#80976,#80977,#80978,#80979,#80980,#80981,
#80982,#80983,#80984,#80985,#80986,#80987,#80988,#80989,#80990,#80991,#80992,
#80993,#80994,#80995,#80996,#80997,#80998,#80999,#81000,#81001,#81002),
 .UNSPECIFIED.,.F.,.F.)
B_SPLINE_CURVE_WITH_KNOTS((6,1,1,1,1,1,1,1,1,1,1,1,1,1,1,1,1,1,1,1,1,1,
1,1,1,1,1,1,1,1,1,1,1,1,1,1,1,1,1,1,1,1,1,1,1,1,1,1,1,1,1,1,1,1,1,1,1,1,
1,1,1,1,1,1,1,1,1,1,1,1,1,1,1,1,1,1,1,1,1,1,1,1,1,1,1,1,1,1,1,1,1,1,1,1,
1,1,1,1,1,1,1,1,1,1,1,1,1,1,1,1,1,1,1,1,1,1,1,1,1,1,1,1,1,1,1,1,1,1,1,1,
1,1,1,1,1,1,1,1,1,1,1,1,1,1,1,1,1,1,1,1,1,1,1,1,1,1,1,1,1,1,1,1,1,1,1,1,
1,1,1,1,1,1,1,1,1,1,1,1,1,1,1,1,1,1,1,1,1,1,1,6),(0.,0.005,0.01,0.015,0.02,
0.025,0.03,0.035,0.04,0.045,0.05,0.055,0.06,0.065,0.07,0.075,0.08,0.085,
0.09,0.095,0.1,0.105,0.11,0.115,0.12,0.125,0.13,0.135,0.14,0.145,0.15,0.155,
0.16,0.165,0.17,0.175,0.18,0.185,0.19,0.195,0.2,0.205,0.21,0.215,0.22,0.225,
0.23,0.235,0.24,0.245,0.25,0.255,0.26,0.265,0.27,0.275,0.28,0.285,0.29,
0.295,0.3,0.305,0.31,0.315,0.32,0.325,0.33,0.335,0.34,0.345,0.35,0.355,
0.36,0.365,0.37,0.375,0.38,0.385,0.39,0.395,0.4,0.405,0.41,0.415,0.42,0.425,
0.43,0.435,0.44,0.445,0.45,0.455,0.46,0.465,0.47,0.475,0.48,0.485,0.49,
0.495,0.5,0.505,0.51,0.515,0.52,0.525,0.53,0.535,0.54,0.545,0.55,0.555,
0.56,0.565,0.57,0.575,0.58,0.585,0.59,0.595,0.6,0.605,0.61,0.615,0.62,0.625,
0.63,0.635,0.64,0.645,0.65,0.655,0.66,0.665,0.67,0.675,0.68,0.685,0.690000000000001,
0.695000000000001,0.700000000000001,0.705000000000001,0.710000000000001,
0.715000000000001,0.720000000000001,0.725000000000001,0.730000000000001,
0.735000000000001,0.740000000000001,0.745000000000001,0.750000000000001,
0.755000000000001,0.760000000000001,0.765000000000001,0.770000000000001,
0.775000000000001,0.780000000000001,0.785000000000001,0.790000000000001,
0.795000000000001,0.800000000000001,0.805000000000001,0.810000000000001,
0.815000000000001,0.820000000000001,0.825000000000001,0.830000000000001,
0.835000000000001,0.840000000000001,0.845000000000001,0.850000000000001,
0.855000000000001,0.860000000000001,0.865000000000001,0.870000000000001,
0.875000000000001,0.880000000000001,0.885000000000001,0.890000000000001,
0.895000000000001,0.900000000000001,0.905000000000001,0.910000000000001,
0.915000000000001,0.920000000000001,0.925000000000001,0.930000000000001,
0.935000000000001,0.940000000000001,0.941429844431281),.UNSPECIFIED.)
CURVE()
GEOMETRIC_REPRESENTATION_ITEM()
RATIONAL_B_SPLINE_CURVE((1.,1.,1.,1.,1.,1.,1.,1.,1.,1.,1.,1.,1.,1.,1.,1.,
1.,1.,1.,1.,1.,1.,1.,1.,1.,1.,1.,1.,1.,1.,1.,1.,1.,1.,1.,1.,1.,1.,1.,1.,
1.,1.,1.,1.,1.,1.,1.,1.,1.,1.,1.,1.,1.,1.,1.,1.,1.,1.,1.,1.,1.,1.,1.,1.,
1.,1.,1.,1.,1.,1.,1.,1.,1.,1.,1.,1.,1.,1.,1.,1.,1.,1.,1.,1.,1.,1.,1.,1.,
1.,1.,1.,1.,1.,1.,1.,1.,1.,1.,1.,1.,1.,1.,1.,1.,1.,1.,1.,1.,1.,1.,1.,1.,
1.,1.,1.,1.,1.,1.,1.,1.,1.,1.,1.,1.,1.,1.,1.,1.,1.,1.,1.,1.,1.,1.,1.,1.,
1.,1.,1.,1.,1.,1.,1.,1.,1.,1.,1.,1.,1.,1.,1.,1.,1.,1.,1.,1.,1.,1.,1.,1.,
1.,1.,1.,1.,1.,1.,1.,1.,1.,1.,1.,1.,1.,1.,1.,1.,1.,1.,1.,1.,1.,1.,1.,1.,
1.,1.,1.,1.,1.,1.,1.,1.,1.,1.))
REPRESENTATION_ITEM('')
);
#466=(
BOUNDED_CURVE()
B_SPLINE_CURVE(5,(#81005,#81006,#81007,#81008,#81009,#81010,#81011,#81012,
#81013,#81014,#81015,#81016,#81017,#81018,#81019,#81020,#81021,#81022,#81023,
#81024,#81025,#81026,#81027,#81028,#81029,#81030,#81031,#81032,#81033,#81034,
#81035,#81036,#81037,#81038,#81039,#81040,#81041,#81042,#81043,#81044,#81045,
#81046,#81047,#81048,#81049,#81050,#81051,#81052,#81053,#81054,#81055,#81056,
#81057,#81058,#81059,#81060,#81061,#81062,#81063,#81064,#81065,#81066,#81067,
#81068,#81069,#81070,#81071,#81072,#81073,#81074,#81075,#81076,#81077,#81078,
#81079,#81080,#81081,#81082,#81083,#81084,#81085,#81086,#81087,#81088,#81089,
#81090,#81091,#81092,#81093,#81094,#81095,#81096,#81097,#81098,#81099,#81100,
#81101,#81102,#81103,#81104,#81105,#81106,#81107,#81108,#81109,#81110,#81111,
#81112,#81113,#81114,#81115,#81116,#81117,#81118,#81119,#81120,#81121,#81122,
#81123,#81124,#81125,#81126,#81127,#81128,#81129,#81130,#81131,#81132,#81133,
#81134,#81135,#81136,#81137,#81138,#81139,#81140,#81141,#81142,#81143,#81144,
#81145,#81146,#81147,#81148,#81149,#81150,#81151,#81152,#81153,#81154,#81155,
#81156,#81157,#81158,#81159,#81160,#81161,#81162,#81163,#81164,#81165,#81166,
#81167,#81168,#81169,#81170,#81171,#81172,#81173,#81174,#81175,#81176,#81177,
#81178,#81179,#81180,#81181,#81182,#81183,#81184,#81185,#81186,#81187,#81188,
#81189,#81190,#81191,#81192,#81193,#81194,#81195,#81196,#81197,#81198),
 .UNSPECIFIED.,.F.,.F.)
B_SPLINE_CURVE_WITH_KNOTS((6,1,1,1,1,1,1,1,1,1,1,1,1,1,1,1,1,1,1,1,1,1,
1,1,1,1,1,1,1,1,1,1,1,1,1,1,1,1,1,1,1,1,1,1,1,1,1,1,1,1,1,1,1,1,1,1,1,1,
1,1,1,1,1,1,1,1,1,1,1,1,1,1,1,1,1,1,1,1,1,1,1,1,1,1,1,1,1,1,1,1,1,1,1,1,
1,1,1,1,1,1,1,1,1,1,1,1,1,1,1,1,1,1,1,1,1,1,1,1,1,1,1,1,1,1,1,1,1,1,1,1,
1,1,1,1,1,1,1,1,1,1,1,1,1,1,1,1,1,1,1,1,1,1,1,1,1,1,1,1,1,1,1,1,1,1,1,1,
1,1,1,1,1,1,1,1,1,1,1,1,1,1,1,1,1,1,1,1,1,1,1,6),(-0.941429844431281,-0.940000000000001,
-0.935000000000001,-0.930000000000001,-0.925000000000001,-0.920000000000001,
-0.915000000000001,-0.910000000000001,-0.905000000000001,-0.900000000000001,
-0.895000000000001,-0.890000000000001,-0.885000000000001,-0.880000000000001,
-0.875000000000001,-0.870000000000001,-0.865000000000001,-0.860000000000001,
-0.855000000000001,-0.850000000000001,-0.845000000000001,-0.840000000000001,
-0.835000000000001,-0.830000000000001,-0.825000000000001,-0.820000000000001,
-0.815000000000001,-0.810000000000001,-0.805000000000001,-0.800000000000001,
-0.795000000000001,-0.790000000000001,-0.785000000000001,-0.780000000000001,
-0.775000000000001,-0.770000000000001,-0.765000000000001,-0.760000000000001,
-0.755000000000001,-0.750000000000001,-0.745000000000001,-0.740000000000001,
-0.735000000000001,-0.730000000000001,-0.725000000000001,-0.720000000000001,
-0.715000000000001,-0.710000000000001,-0.705000000000001,-0.700000000000001,
-0.695000000000001,-0.690000000000001,-0.685,-0.68,-0.675,-0.67,-0.665,
-0.66,-0.655,-0.65,-0.645,-0.64,-0.635,-0.63,-0.625,-0.62,-0.615,-0.61,
-0.605,-0.6,-0.595,-0.59,-0.585,-0.58,-0.575,-0.57,-0.565,-0.56,-0.555,
-0.55,-0.545,-0.54,-0.535,-0.53,-0.525,-0.52,-0.515,-0.51,-0.505,-0.5,-0.495,
-0.49,-0.485,-0.48,-0.475,-0.47,-0.465,-0.46,-0.455,-0.45,-0.445,-0.44,
-0.435,-0.43,-0.425,-0.42,-0.415,-0.41,-0.405,-0.4,-0.395,-0.39,-0.385,
-0.38,-0.375,-0.37,-0.365,-0.36,-0.355,-0.35,-0.345,-0.34,-0.335,-0.33,
-0.325,-0.32,-0.315,-0.31,-0.305,-0.3,-0.295,-0.29,-0.285,-0.28,-0.275,
-0.27,-0.265,-0.26,-0.255,-0.25,-0.245,-0.24,-0.235,-0.23,-0.225,-0.22,
-0.215,-0.21,-0.205,-0.2,-0.195,-0.19,-0.185,-0.18,-0.175,-0.17,-0.165,
-0.16,-0.155,-0.15,-0.145,-0.14,-0.135,-0.13,-0.125,-0.12,-0.115,-0.11,
-0.105,-0.1,-0.095,-0.09,-0.085,-0.08,-0.075,-0.07,-0.065,-0.06,-0.055,
-0.05,-0.045,-0.04,-0.035,-0.03,-0.025,-0.02,-0.015,-0.01,-0.005,0.),
 .UNSPECIFIED.)
CURVE()
GEOMETRIC_REPRESENTATION_ITEM()
RATIONAL_B_SPLINE_CURVE((1.,1.,1.,1.,1.,1.,1.,1.,1.,1.,1.,1.,1.,1.,1.,1.,
1.,1.,1.,1.,1.,1.,1.,1.,1.,1.,1.,1.,1.,1.,1.,1.,1.,1.,1.,1.,1.,1.,1.,1.,
1.,1.,1.,1.,1.,1.,1.,1.,1.,1.,1.,1.,1.,1.,1.,1.,1.,1.,1.,1.,1.,1.,1.,1.,
1.,1.,1.,1.,1.,1.,1.,1.,1.,1.,1.,1.,1.,1.,1.,1.,1.,1.,1.,1.,1.,1.,1.,1.,
1.,1.,1.,1.,1.,1.,1.,1.,1.,1.,1.,1.,1.,1.,1.,1.,1.,1.,1.,1.,1.,1.,1.,1.,
1.,1.,1.,1.,1.,1.,1.,1.,1.,1.,1.,1.,1.,1.,1.,1.,1.,1.,1.,1.,1.,1.,1.,1.,
1.,1.,1.,1.,1.,1.,1.,1.,1.,1.,1.,1.,1.,1.,1.,1.,1.,1.,1.,1.,1.,1.,1.,1.,
1.,1.,1.,1.,1.,1.,1.,1.,1.,1.,1.,1.,1.,1.,1.,1.,1.,1.,1.,1.,1.,1.,1.,1.,
1.,1.,1.,1.,1.,1.,1.,1.,1.,1.))
REPRESENTATION_ITEM('')
);
#467=(
BOUNDED_CURVE()
B_SPLINE_CURVE(5,(#81705,#81706,#81707,#81708,#81709,#81710,#81711,#81712,
#81713,#81714,#81715,#81716,#81717,#81718,#81719,#81720,#81721,#81722,#81723,
#81724,#81725,#81726,#81727,#81728,#81729,#81730,#81731,#81732,#81733,#81734,
#81735,#81736,#81737,#81738,#81739,#81740,#81741,#81742,#81743,#81744,#81745,
#81746,#81747,#81748,#81749,#81750,#81751,#81752,#81753,#81754,#81755,#81756,
#81757,#81758,#81759,#81760,#81761,#81762,#81763,#81764,#81765,#81766,#81767,
#81768,#81769,#81770,#81771,#81772,#81773,#81774,#81775,#81776,#81777,#81778,
#81779,#81780,#81781,#81782,#81783,#81784,#81785,#81786,#81787,#81788,#81789,
#81790,#81791,#81792,#81793,#81794,#81795,#81796,#81797,#81798,#81799,#81800,
#81801,#81802,#81803,#81804,#81805,#81806,#81807,#81808,#81809,#81810,#81811,
#81812,#81813,#81814,#81815,#81816,#81817,#81818,#81819,#81820,#81821,#81822,
#81823,#81824,#81825,#81826,#81827,#81828,#81829,#81830,#81831,#81832,#81833,
#81834,#81835,#81836,#81837,#81838,#81839,#81840,#81841,#81842,#81843,#81844,
#81845,#81846,#81847,#81848,#81849,#81850,#81851,#81852,#81853,#81854,#81855,
#81856,#81857,#81858,#81859,#81860,#81861,#81862,#81863,#81864,#81865,#81866,
#81867,#81868,#81869,#81870,#81871,#81872,#81873,#81874,#81875,#81876,#81877,
#81878,#81879,#81880,#81881,#81882,#81883,#81884,#81885,#81886,#81887,#81888,
#81889,#81890,#81891,#81892,#81893,#81894,#81895,#81896,#81897,#81898),
 .UNSPECIFIED.,.F.,.F.)
B_SPLINE_CURVE_WITH_KNOTS((6,1,1,1,1,1,1,1,1,1,1,1,1,1,1,1,1,1,1,1,1,1,
1,1,1,1,1,1,1,1,1,1,1,1,1,1,1,1,1,1,1,1,1,1,1,1,1,1,1,1,1,1,1,1,1,1,1,1,
1,1,1,1,1,1,1,1,1,1,1,1,1,1,1,1,1,1,1,1,1,1,1,1,1,1,1,1,1,1,1,1,1,1,1,1,
1,1,1,1,1,1,1,1,1,1,1,1,1,1,1,1,1,1,1,1,1,1,1,1,1,1,1,1,1,1,1,1,1,1,1,1,
1,1,1,1,1,1,1,1,1,1,1,1,1,1,1,1,1,1,1,1,1,1,1,1,1,1,1,1,1,1,1,1,1,1,1,1,
1,1,1,1,1,1,1,1,1,1,1,1,1,1,1,1,1,1,1,1,1,1,1,6),(0.,0.005,0.01,0.015,0.02,
0.025,0.03,0.035,0.04,0.045,0.05,0.055,0.06,0.065,0.07,0.075,0.08,0.085,
0.09,0.095,0.1,0.105,0.11,0.115,0.12,0.125,0.13,0.135,0.14,0.145,0.15,0.155,
0.16,0.165,0.17,0.175,0.18,0.185,0.19,0.195,0.2,0.205,0.21,0.215,0.22,0.225,
0.23,0.235,0.24,0.245,0.25,0.255,0.26,0.265,0.27,0.275,0.28,0.285,0.29,
0.295,0.3,0.305,0.31,0.315,0.32,0.325,0.33,0.335,0.34,0.345,0.35,0.355,
0.36,0.365,0.37,0.375,0.38,0.385,0.39,0.395,0.4,0.405,0.41,0.415,0.42,0.425,
0.43,0.435,0.44,0.445,0.45,0.455,0.46,0.465,0.47,0.475,0.48,0.485,0.49,
0.495,0.5,0.505,0.51,0.515,0.52,0.525,0.53,0.535,0.54,0.545,0.55,0.555,
0.56,0.565,0.57,0.575,0.58,0.585,0.59,0.595,0.6,0.605,0.61,0.615,0.62,0.625,
0.63,0.635,0.64,0.645,0.65,0.655,0.66,0.665,0.67,0.675,0.68,0.685,0.690000000000001,
0.695000000000001,0.700000000000001,0.705000000000001,0.710000000000001,
0.715000000000001,0.720000000000001,0.725000000000001,0.730000000000001,
0.735000000000001,0.740000000000001,0.745000000000001,0.750000000000001,
0.755000000000001,0.760000000000001,0.765000000000001,0.770000000000001,
0.775000000000001,0.780000000000001,0.785000000000001,0.790000000000001,
0.795000000000001,0.800000000000001,0.805000000000001,0.810000000000001,
0.815000000000001,0.820000000000001,0.825000000000001,0.830000000000001,
0.835000000000001,0.840000000000001,0.845000000000001,0.850000000000001,
0.855000000000001,0.860000000000001,0.865000000000001,0.870000000000001,
0.875000000000001,0.880000000000001,0.885000000000001,0.890000000000001,
0.895000000000001,0.900000000000001,0.905000000000001,0.910000000000001,
0.915000000000001,0.920000000000001,0.925000000000001,0.930000000000001,
0.935000000000001,0.940000000000001,0.941429844431456),.UNSPECIFIED.)
CURVE()
GEOMETRIC_REPRESENTATION_ITEM()
RATIONAL_B_SPLINE_CURVE((1.,1.,1.,1.,1.,1.,1.,1.,1.,1.,1.,1.,1.,1.,1.,1.,
1.,1.,1.,1.,1.,1.,1.,1.,1.,1.,1.,1.,1.,1.,1.,1.,1.,1.,1.,1.,1.,1.,1.,1.,
1.,1.,1.,1.,1.,1.,1.,1.,1.,1.,1.,1.,1.,1.,1.,1.,1.,1.,1.,1.,1.,1.,1.,1.,
1.,1.,1.,1.,1.,1.,1.,1.,1.,1.,1.,1.,1.,1.,1.,1.,1.,1.,1.,1.,1.,1.,1.,1.,
1.,1.,1.,1.,1.,1.,1.,1.,1.,1.,1.,1.,1.,1.,1.,1.,1.,1.,1.,1.,1.,1.,1.,1.,
1.,1.,1.,1.,1.,1.,1.,1.,1.,1.,1.,1.,1.,1.,1.,1.,1.,1.,1.,1.,1.,1.,1.,1.,
1.,1.,1.,1.,1.,1.,1.,1.,1.,1.,1.,1.,1.,1.,1.,1.,1.,1.,1.,1.,1.,1.,1.,1.,
1.,1.,1.,1.,1.,1.,1.,1.,1.,1.,1.,1.,1.,1.,1.,1.,1.,1.,1.,1.,1.,1.,1.,1.,
1.,1.,1.,1.,1.,1.,1.,1.,1.,1.))
REPRESENTATION_ITEM('')
);
#468=(
BOUNDED_CURVE()
B_SPLINE_CURVE(5,(#81901,#81902,#81903,#81904,#81905,#81906,#81907,#81908,
#81909,#81910,#81911,#81912,#81913,#81914,#81915,#81916,#81917,#81918,#81919,
#81920,#81921,#81922,#81923,#81924,#81925,#81926,#81927,#81928,#81929,#81930,
#81931,#81932,#81933,#81934,#81935,#81936,#81937,#81938,#81939,#81940,#81941,
#81942,#81943,#81944,#81945,#81946,#81947,#81948,#81949,#81950,#81951,#81952,
#81953,#81954,#81955,#81956,#81957,#81958,#81959,#81960,#81961,#81962,#81963,
#81964,#81965,#81966,#81967,#81968,#81969,#81970,#81971,#81972,#81973,#81974,
#81975,#81976,#81977,#81978,#81979,#81980,#81981,#81982,#81983,#81984,#81985,
#81986,#81987,#81988,#81989,#81990,#81991,#81992,#81993,#81994,#81995,#81996,
#81997,#81998,#81999,#82000,#82001,#82002,#82003,#82004,#82005,#82006,#82007,
#82008,#82009,#82010,#82011,#82012,#82013,#82014,#82015,#82016,#82017,#82018,
#82019,#82020,#82021,#82022,#82023,#82024,#82025,#82026,#82027,#82028,#82029,
#82030,#82031,#82032,#82033,#82034,#82035,#82036,#82037,#82038,#82039,#82040,
#82041,#82042,#82043,#82044,#82045,#82046,#82047,#82048,#82049,#82050,#82051,
#82052,#82053,#82054,#82055,#82056,#82057,#82058,#82059,#82060,#82061,#82062,
#82063,#82064,#82065,#82066,#82067,#82068,#82069,#82070,#82071,#82072,#82073,
#82074,#82075,#82076,#82077,#82078,#82079,#82080,#82081,#82082,#82083,#82084,
#82085,#82086,#82087,#82088,#82089,#82090,#82091,#82092,#82093,#82094),
 .UNSPECIFIED.,.F.,.F.)
B_SPLINE_CURVE_WITH_KNOTS((6,1,1,1,1,1,1,1,1,1,1,1,1,1,1,1,1,1,1,1,1,1,
1,1,1,1,1,1,1,1,1,1,1,1,1,1,1,1,1,1,1,1,1,1,1,1,1,1,1,1,1,1,1,1,1,1,1,1,
1,1,1,1,1,1,1,1,1,1,1,1,1,1,1,1,1,1,1,1,1,1,1,1,1,1,1,1,1,1,1,1,1,1,1,1,
1,1,1,1,1,1,1,1,1,1,1,1,1,1,1,1,1,1,1,1,1,1,1,1,1,1,1,1,1,1,1,1,1,1,1,1,
1,1,1,1,1,1,1,1,1,1,1,1,1,1,1,1,1,1,1,1,1,1,1,1,1,1,1,1,1,1,1,1,1,1,1,1,
1,1,1,1,1,1,1,1,1,1,1,1,1,1,1,1,1,1,1,1,1,1,1,6),(-0.941429844431454,-0.940000000000001,
-0.935000000000001,-0.930000000000001,-0.925000000000001,-0.920000000000001,
-0.915000000000001,-0.910000000000001,-0.905000000000001,-0.900000000000001,
-0.895000000000001,-0.890000000000001,-0.885000000000001,-0.880000000000001,
-0.875000000000001,-0.870000000000001,-0.865000000000001,-0.860000000000001,
-0.855000000000001,-0.850000000000001,-0.845000000000001,-0.840000000000001,
-0.835000000000001,-0.830000000000001,-0.825000000000001,-0.820000000000001,
-0.815000000000001,-0.810000000000001,-0.805000000000001,-0.800000000000001,
-0.795000000000001,-0.790000000000001,-0.785000000000001,-0.780000000000001,
-0.775000000000001,-0.770000000000001,-0.765000000000001,-0.760000000000001,
-0.755000000000001,-0.750000000000001,-0.745000000000001,-0.740000000000001,
-0.735000000000001,-0.730000000000001,-0.725000000000001,-0.720000000000001,
-0.715000000000001,-0.710000000000001,-0.705000000000001,-0.700000000000001,
-0.695000000000001,-0.690000000000001,-0.685,-0.68,-0.675,-0.67,-0.665,
-0.66,-0.655,-0.65,-0.645,-0.64,-0.635,-0.63,-0.625,-0.62,-0.615,-0.61,
-0.605,-0.6,-0.595,-0.59,-0.585,-0.58,-0.575,-0.57,-0.565,-0.56,-0.555,
-0.55,-0.545,-0.54,-0.535,-0.53,-0.525,-0.52,-0.515,-0.51,-0.505,-0.5,-0.495,
-0.49,-0.485,-0.48,-0.475,-0.47,-0.465,-0.46,-0.455,-0.45,-0.445,-0.44,
-0.435,-0.43,-0.425,-0.42,-0.415,-0.41,-0.405,-0.4,-0.395,-0.39,-0.385,
-0.38,-0.375,-0.37,-0.365,-0.36,-0.355,-0.35,-0.345,-0.34,-0.335,-0.33,
-0.325,-0.32,-0.315,-0.31,-0.305,-0.3,-0.295,-0.29,-0.285,-0.28,-0.275,
-0.27,-0.265,-0.26,-0.255,-0.25,-0.245,-0.24,-0.235,-0.23,-0.225,-0.22,
-0.215,-0.21,-0.205,-0.2,-0.195,-0.19,-0.185,-0.18,-0.175,-0.17,-0.165,
-0.16,-0.155,-0.15,-0.145,-0.14,-0.135,-0.13,-0.125,-0.12,-0.115,-0.11,
-0.105,-0.1,-0.095,-0.09,-0.085,-0.08,-0.075,-0.07,-0.065,-0.06,-0.055,
-0.05,-0.045,-0.04,-0.035,-0.03,-0.025,-0.02,-0.015,-0.01,-0.005,0.),
 .UNSPECIFIED.)
CURVE()
GEOMETRIC_REPRESENTATION_ITEM()
RATIONAL_B_SPLINE_CURVE((1.,1.,1.,1.,1.,1.,1.,1.,1.,1.,1.,1.,1.,1.,1.,1.,
1.,1.,1.,1.,1.,1.,1.,1.,1.,1.,1.,1.,1.,1.,1.,1.,1.,1.,1.,1.,1.,1.,1.,1.,
1.,1.,1.,1.,1.,1.,1.,1.,1.,1.,1.,1.,1.,1.,1.,1.,1.,1.,1.,1.,1.,1.,1.,1.,
1.,1.,1.,1.,1.,1.,1.,1.,1.,1.,1.,1.,1.,1.,1.,1.,1.,1.,1.,1.,1.,1.,1.,1.,
1.,1.,1.,1.,1.,1.,1.,1.,1.,1.,1.,1.,1.,1.,1.,1.,1.,1.,1.,1.,1.,1.,1.,1.,
1.,1.,1.,1.,1.,1.,1.,1.,1.,1.,1.,1.,1.,1.,1.,1.,1.,1.,1.,1.,1.,1.,1.,1.,
1.,1.,1.,1.,1.,1.,1.,1.,1.,1.,1.,1.,1.,1.,1.,1.,1.,1.,1.,1.,1.,1.,1.,1.,
1.,1.,1.,1.,1.,1.,1.,1.,1.,1.,1.,1.,1.,1.,1.,1.,1.,1.,1.,1.,1.,1.,1.,1.,
1.,1.,1.,1.,1.,1.,1.,1.,1.,1.))
REPRESENTATION_ITEM('')
);
#469=(
BOUNDED_CURVE()
B_SPLINE_CURVE(5,(#82601,#82602,#82603,#82604,#82605,#82606,#82607,#82608,
#82609,#82610,#82611,#82612,#82613,#82614,#82615,#82616,#82617,#82618,#82619,
#82620,#82621,#82622,#82623,#82624,#82625,#82626,#82627,#82628,#82629,#82630,
#82631,#82632,#82633,#82634,#82635,#82636,#82637,#82638,#82639,#82640,#82641,
#82642,#82643,#82644,#82645,#82646,#82647,#82648,#82649,#82650,#82651,#82652,
#82653,#82654,#82655,#82656,#82657,#82658,#82659,#82660,#82661,#82662,#82663,
#82664,#82665,#82666,#82667,#82668,#82669,#82670,#82671,#82672,#82673,#82674,
#82675,#82676,#82677,#82678,#82679,#82680,#82681,#82682,#82683,#82684,#82685,
#82686,#82687,#82688,#82689,#82690,#82691,#82692,#82693,#82694,#82695,#82696,
#82697,#82698,#82699,#82700,#82701,#82702,#82703,#82704,#82705,#82706,#82707,
#82708,#82709,#82710,#82711,#82712,#82713,#82714,#82715,#82716,#82717,#82718,
#82719,#82720,#82721,#82722,#82723,#82724,#82725,#82726,#82727,#82728,#82729,
#82730,#82731,#82732,#82733,#82734,#82735,#82736,#82737,#82738,#82739,#82740,
#82741,#82742,#82743,#82744,#82745,#82746,#82747,#82748,#82749,#82750,#82751,
#82752,#82753,#82754,#82755,#82756,#82757,#82758,#82759,#82760,#82761,#82762,
#82763,#82764,#82765,#82766,#82767,#82768,#82769,#82770,#82771,#82772,#82773,
#82774,#82775,#82776,#82777,#82778,#82779,#82780,#82781,#82782,#82783,#82784,
#82785,#82786,#82787,#82788,#82789,#82790,#82791,#82792,#82793,#82794),
 .UNSPECIFIED.,.F.,.F.)
B_SPLINE_CURVE_WITH_KNOTS((6,1,1,1,1,1,1,1,1,1,1,1,1,1,1,1,1,1,1,1,1,1,
1,1,1,1,1,1,1,1,1,1,1,1,1,1,1,1,1,1,1,1,1,1,1,1,1,1,1,1,1,1,1,1,1,1,1,1,
1,1,1,1,1,1,1,1,1,1,1,1,1,1,1,1,1,1,1,1,1,1,1,1,1,1,1,1,1,1,1,1,1,1,1,1,
1,1,1,1,1,1,1,1,1,1,1,1,1,1,1,1,1,1,1,1,1,1,1,1,1,1,1,1,1,1,1,1,1,1,1,1,
1,1,1,1,1,1,1,1,1,1,1,1,1,1,1,1,1,1,1,1,1,1,1,1,1,1,1,1,1,1,1,1,1,1,1,1,
1,1,1,1,1,1,1,1,1,1,1,1,1,1,1,1,1,1,1,1,1,1,1,6),(0.,0.005,0.01,0.015,0.02,
0.025,0.03,0.035,0.04,0.045,0.05,0.055,0.06,0.065,0.07,0.075,0.08,0.085,
0.09,0.095,0.1,0.105,0.11,0.115,0.12,0.125,0.13,0.135,0.14,0.145,0.15,0.155,
0.16,0.165,0.17,0.175,0.18,0.185,0.19,0.195,0.2,0.205,0.21,0.215,0.22,0.225,
0.23,0.235,0.24,0.245,0.25,0.255,0.26,0.265,0.27,0.275,0.28,0.285,0.29,
0.295,0.3,0.305,0.31,0.315,0.32,0.325,0.33,0.335,0.34,0.345,0.35,0.355,
0.36,0.365,0.37,0.375,0.38,0.385,0.39,0.395,0.4,0.405,0.41,0.415,0.42,0.425,
0.43,0.435,0.44,0.445,0.45,0.455,0.46,0.465,0.47,0.475,0.48,0.485,0.49,
0.495,0.5,0.505,0.51,0.515,0.52,0.525,0.53,0.535,0.54,0.545,0.55,0.555,
0.56,0.565,0.57,0.575,0.58,0.585,0.59,0.595,0.6,0.605,0.61,0.615,0.62,0.625,
0.63,0.635,0.64,0.645,0.65,0.655,0.66,0.665,0.67,0.675,0.68,0.685,0.690000000000001,
0.695000000000001,0.700000000000001,0.705000000000001,0.710000000000001,
0.715000000000001,0.720000000000001,0.725000000000001,0.730000000000001,
0.735000000000001,0.740000000000001,0.745000000000001,0.750000000000001,
0.755000000000001,0.760000000000001,0.765000000000001,0.770000000000001,
0.775000000000001,0.780000000000001,0.785000000000001,0.790000000000001,
0.795000000000001,0.800000000000001,0.805000000000001,0.810000000000001,
0.815000000000001,0.820000000000001,0.825000000000001,0.830000000000001,
0.835000000000001,0.840000000000001,0.845000000000001,0.850000000000001,
0.855000000000001,0.860000000000001,0.865000000000001,0.870000000000001,
0.875000000000001,0.880000000000001,0.885000000000001,0.890000000000001,
0.895000000000001,0.900000000000001,0.905000000000001,0.910000000000001,
0.915000000000001,0.920000000000001,0.925000000000001,0.930000000000001,
0.935000000000001,0.940000000000001,0.94142984443149),.UNSPECIFIED.)
CURVE()
GEOMETRIC_REPRESENTATION_ITEM()
RATIONAL_B_SPLINE_CURVE((1.,1.,1.,1.,1.,1.,1.,1.,1.,1.,1.,1.,1.,1.,1.,1.,
1.,1.,1.,1.,1.,1.,1.,1.,1.,1.,1.,1.,1.,1.,1.,1.,1.,1.,1.,1.,1.,1.,1.,1.,
1.,1.,1.,1.,1.,1.,1.,1.,1.,1.,1.,1.,1.,1.,1.,1.,1.,1.,1.,1.,1.,1.,1.,1.,
1.,1.,1.,1.,1.,1.,1.,1.,1.,1.,1.,1.,1.,1.,1.,1.,1.,1.,1.,1.,1.,1.,1.,1.,
1.,1.,1.,1.,1.,1.,1.,1.,1.,1.,1.,1.,1.,1.,1.,1.,1.,1.,1.,1.,1.,1.,1.,1.,
1.,1.,1.,1.,1.,1.,1.,1.,1.,1.,1.,1.,1.,1.,1.,1.,1.,1.,1.,1.,1.,1.,1.,1.,
1.,1.,1.,1.,1.,1.,1.,1.,1.,1.,1.,1.,1.,1.,1.,1.,1.,1.,1.,1.,1.,1.,1.,1.,
1.,1.,1.,1.,1.,1.,1.,1.,1.,1.,1.,1.,1.,1.,1.,1.,1.,1.,1.,1.,1.,1.,1.,1.,
1.,1.,1.,1.,1.,1.,1.,1.,1.,1.))
REPRESENTATION_ITEM('')
);
#470=(
BOUNDED_CURVE()
B_SPLINE_CURVE(5,(#82797,#82798,#82799,#82800,#82801,#82802,#82803,#82804,
#82805,#82806,#82807,#82808,#82809,#82810,#82811,#82812,#82813,#82814,#82815,
#82816,#82817,#82818,#82819,#82820,#82821,#82822,#82823,#82824,#82825,#82826,
#82827,#82828,#82829,#82830,#82831,#82832,#82833,#82834,#82835,#82836,#82837,
#82838,#82839,#82840,#82841,#82842,#82843,#82844,#82845,#82846,#82847,#82848,
#82849,#82850,#82851,#82852,#82853,#82854,#82855,#82856,#82857,#82858,#82859,
#82860,#82861,#82862,#82863,#82864,#82865,#82866,#82867,#82868,#82869,#82870,
#82871,#82872,#82873,#82874,#82875,#82876,#82877,#82878,#82879,#82880,#82881,
#82882,#82883,#82884,#82885,#82886,#82887,#82888,#82889,#82890,#82891,#82892,
#82893,#82894,#82895,#82896,#82897,#82898,#82899,#82900,#82901,#82902,#82903,
#82904,#82905,#82906,#82907,#82908,#82909,#82910,#82911,#82912,#82913,#82914,
#82915,#82916,#82917,#82918,#82919,#82920,#82921,#82922,#82923,#82924,#82925,
#82926,#82927,#82928,#82929,#82930,#82931,#82932,#82933,#82934,#82935,#82936,
#82937,#82938,#82939,#82940,#82941,#82942,#82943,#82944,#82945,#82946,#82947,
#82948,#82949,#82950,#82951,#82952,#82953,#82954,#82955,#82956,#82957,#82958,
#82959,#82960,#82961,#82962,#82963,#82964,#82965,#82966,#82967,#82968,#82969,
#82970,#82971,#82972,#82973,#82974,#82975,#82976,#82977,#82978,#82979,#82980,
#82981,#82982,#82983,#82984,#82985,#82986,#82987,#82988,#82989,#82990),
 .UNSPECIFIED.,.F.,.F.)
B_SPLINE_CURVE_WITH_KNOTS((6,1,1,1,1,1,1,1,1,1,1,1,1,1,1,1,1,1,1,1,1,1,
1,1,1,1,1,1,1,1,1,1,1,1,1,1,1,1,1,1,1,1,1,1,1,1,1,1,1,1,1,1,1,1,1,1,1,1,
1,1,1,1,1,1,1,1,1,1,1,1,1,1,1,1,1,1,1,1,1,1,1,1,1,1,1,1,1,1,1,1,1,1,1,1,
1,1,1,1,1,1,1,1,1,1,1,1,1,1,1,1,1,1,1,1,1,1,1,1,1,1,1,1,1,1,1,1,1,1,1,1,
1,1,1,1,1,1,1,1,1,1,1,1,1,1,1,1,1,1,1,1,1,1,1,1,1,1,1,1,1,1,1,1,1,1,1,1,
1,1,1,1,1,1,1,1,1,1,1,1,1,1,1,1,1,1,1,1,1,1,1,6),(-0.94142984443149,-0.940000000000001,
-0.935000000000001,-0.930000000000001,-0.925000000000001,-0.920000000000001,
-0.915000000000001,-0.910000000000001,-0.905000000000001,-0.900000000000001,
-0.895000000000001,-0.890000000000001,-0.885000000000001,-0.880000000000001,
-0.875000000000001,-0.870000000000001,-0.865000000000001,-0.860000000000001,
-0.855000000000001,-0.850000000000001,-0.845000000000001,-0.840000000000001,
-0.835000000000001,-0.830000000000001,-0.825000000000001,-0.820000000000001,
-0.815000000000001,-0.810000000000001,-0.805000000000001,-0.800000000000001,
-0.795000000000001,-0.790000000000001,-0.785000000000001,-0.780000000000001,
-0.775000000000001,-0.770000000000001,-0.765000000000001,-0.760000000000001,
-0.755000000000001,-0.750000000000001,-0.745000000000001,-0.740000000000001,
-0.735000000000001,-0.730000000000001,-0.725000000000001,-0.720000000000001,
-0.715000000000001,-0.710000000000001,-0.705000000000001,-0.700000000000001,
-0.695000000000001,-0.690000000000001,-0.685,-0.68,-0.675,-0.67,-0.665,
-0.66,-0.655,-0.65,-0.645,-0.64,-0.635,-0.63,-0.625,-0.62,-0.615,-0.61,
-0.605,-0.6,-0.595,-0.59,-0.585,-0.58,-0.575,-0.57,-0.565,-0.56,-0.555,
-0.55,-0.545,-0.54,-0.535,-0.53,-0.525,-0.52,-0.515,-0.51,-0.505,-0.5,-0.495,
-0.49,-0.485,-0.48,-0.475,-0.47,-0.465,-0.46,-0.455,-0.45,-0.445,-0.44,
-0.435,-0.43,-0.425,-0.42,-0.415,-0.41,-0.405,-0.4,-0.395,-0.39,-0.385,
-0.38,-0.375,-0.37,-0.365,-0.36,-0.355,-0.35,-0.345,-0.34,-0.335,-0.33,
-0.325,-0.32,-0.315,-0.31,-0.305,-0.3,-0.295,-0.29,-0.285,-0.28,-0.275,
-0.27,-0.265,-0.26,-0.255,-0.25,-0.245,-0.24,-0.235,-0.23,-0.225,-0.22,
-0.215,-0.21,-0.205,-0.2,-0.195,-0.19,-0.185,-0.18,-0.175,-0.17,-0.165,
-0.16,-0.155,-0.15,-0.145,-0.14,-0.135,-0.13,-0.125,-0.12,-0.115,-0.11,
-0.105,-0.1,-0.095,-0.09,-0.085,-0.08,-0.075,-0.07,-0.065,-0.06,-0.055,
-0.05,-0.045,-0.04,-0.035,-0.03,-0.025,-0.02,-0.015,-0.01,-0.005,0.),
 .UNSPECIFIED.)
CURVE()
GEOMETRIC_REPRESENTATION_ITEM()
RATIONAL_B_SPLINE_CURVE((1.,1.,1.,1.,1.,1.,1.,1.,1.,1.,1.,1.,1.,1.,1.,1.,
1.,1.,1.,1.,1.,1.,1.,1.,1.,1.,1.,1.,1.,1.,1.,1.,1.,1.,1.,1.,1.,1.,1.,1.,
1.,1.,1.,1.,1.,1.,1.,1.,1.,1.,1.,1.,1.,1.,1.,1.,1.,1.,1.,1.,1.,1.,1.,1.,
1.,1.,1.,1.,1.,1.,1.,1.,1.,1.,1.,1.,1.,1.,1.,1.,1.,1.,1.,1.,1.,1.,1.,1.,
1.,1.,1.,1.,1.,1.,1.,1.,1.,1.,1.,1.,1.,1.,1.,1.,1.,1.,1.,1.,1.,1.,1.,1.,
1.,1.,1.,1.,1.,1.,1.,1.,1.,1.,1.,1.,1.,1.,1.,1.,1.,1.,1.,1.,1.,1.,1.,1.,
1.,1.,1.,1.,1.,1.,1.,1.,1.,1.,1.,1.,1.,1.,1.,1.,1.,1.,1.,1.,1.,1.,1.,1.,
1.,1.,1.,1.,1.,1.,1.,1.,1.,1.,1.,1.,1.,1.,1.,1.,1.,1.,1.,1.,1.,1.,1.,1.,
1.,1.,1.,1.,1.,1.,1.,1.,1.,1.))
REPRESENTATION_ITEM('')
);
#471=(
BOUNDED_CURVE()
B_SPLINE_CURVE(5,(#83497,#83498,#83499,#83500,#83501,#83502,#83503,#83504,
#83505,#83506,#83507,#83508,#83509,#83510,#83511,#83512,#83513,#83514,#83515,
#83516,#83517,#83518,#83519,#83520,#83521,#83522,#83523,#83524,#83525,#83526,
#83527,#83528,#83529,#83530,#83531,#83532,#83533,#83534,#83535,#83536,#83537,
#83538,#83539,#83540,#83541,#83542,#83543,#83544,#83545,#83546,#83547,#83548,
#83549,#83550,#83551,#83552,#83553,#83554,#83555,#83556,#83557,#83558,#83559,
#83560,#83561,#83562,#83563,#83564,#83565,#83566,#83567,#83568,#83569,#83570,
#83571,#83572,#83573,#83574,#83575,#83576,#83577,#83578,#83579,#83580,#83581,
#83582,#83583,#83584,#83585,#83586,#83587,#83588,#83589,#83590,#83591,#83592,
#83593,#83594,#83595,#83596,#83597,#83598,#83599,#83600,#83601,#83602,#83603,
#83604,#83605,#83606,#83607,#83608,#83609,#83610,#83611,#83612,#83613,#83614,
#83615,#83616,#83617,#83618,#83619,#83620,#83621,#83622,#83623,#83624,#83625,
#83626,#83627,#83628,#83629,#83630,#83631,#83632,#83633,#83634,#83635,#83636,
#83637,#83638,#83639,#83640,#83641,#83642,#83643,#83644,#83645,#83646,#83647,
#83648,#83649,#83650,#83651,#83652,#83653,#83654,#83655,#83656,#83657,#83658,
#83659,#83660,#83661,#83662,#83663,#83664,#83665,#83666,#83667,#83668,#83669,
#83670,#83671,#83672,#83673,#83674,#83675,#83676,#83677,#83678,#83679,#83680,
#83681,#83682,#83683,#83684,#83685,#83686,#83687,#83688,#83689,#83690),
 .UNSPECIFIED.,.F.,.F.)
B_SPLINE_CURVE_WITH_KNOTS((6,1,1,1,1,1,1,1,1,1,1,1,1,1,1,1,1,1,1,1,1,1,
1,1,1,1,1,1,1,1,1,1,1,1,1,1,1,1,1,1,1,1,1,1,1,1,1,1,1,1,1,1,1,1,1,1,1,1,
1,1,1,1,1,1,1,1,1,1,1,1,1,1,1,1,1,1,1,1,1,1,1,1,1,1,1,1,1,1,1,1,1,1,1,1,
1,1,1,1,1,1,1,1,1,1,1,1,1,1,1,1,1,1,1,1,1,1,1,1,1,1,1,1,1,1,1,1,1,1,1,1,
1,1,1,1,1,1,1,1,1,1,1,1,1,1,1,1,1,1,1,1,1,1,1,1,1,1,1,1,1,1,1,1,1,1,1,1,
1,1,1,1,1,1,1,1,1,1,1,1,1,1,1,1,1,1,1,1,1,1,1,6),(0.,0.005,0.01,0.015,0.02,
0.025,0.03,0.035,0.04,0.045,0.05,0.055,0.06,0.065,0.07,0.075,0.08,0.085,
0.09,0.095,0.1,0.105,0.11,0.115,0.12,0.125,0.13,0.135,0.14,0.145,0.15,0.155,
0.16,0.165,0.17,0.175,0.18,0.185,0.19,0.195,0.2,0.205,0.21,0.215,0.22,0.225,
0.23,0.235,0.24,0.245,0.25,0.255,0.26,0.265,0.27,0.275,0.28,0.285,0.29,
0.295,0.3,0.305,0.31,0.315,0.32,0.325,0.33,0.335,0.34,0.345,0.35,0.355,
0.36,0.365,0.37,0.375,0.38,0.385,0.39,0.395,0.4,0.405,0.41,0.415,0.42,0.425,
0.43,0.435,0.44,0.445,0.45,0.455,0.46,0.465,0.47,0.475,0.48,0.485,0.49,
0.495,0.5,0.505,0.51,0.515,0.52,0.525,0.53,0.535,0.54,0.545,0.55,0.555,
0.56,0.565,0.57,0.575,0.58,0.585,0.59,0.595,0.6,0.605,0.61,0.615,0.62,0.625,
0.63,0.635,0.64,0.645,0.65,0.655,0.66,0.665,0.67,0.675,0.68,0.685,0.690000000000001,
0.695000000000001,0.700000000000001,0.705000000000001,0.710000000000001,
0.715000000000001,0.720000000000001,0.725000000000001,0.730000000000001,
0.735000000000001,0.740000000000001,0.745000000000001,0.750000000000001,
0.755000000000001,0.760000000000001,0.765000000000001,0.770000000000001,
0.775000000000001,0.780000000000001,0.785000000000001,0.790000000000001,
0.795000000000001,0.800000000000001,0.805000000000001,0.810000000000001,
0.815000000000001,0.820000000000001,0.825000000000001,0.830000000000001,
0.835000000000001,0.840000000000001,0.845000000000001,0.850000000000001,
0.855000000000001,0.860000000000001,0.865000000000001,0.870000000000001,
0.875000000000001,0.880000000000001,0.885000000000001,0.890000000000001,
0.895000000000001,0.900000000000001,0.905000000000001,0.910000000000001,
0.915000000000001,0.920000000000001,0.925000000000001,0.930000000000001,
0.935000000000001,0.940000000000001,0.941429844431321),.UNSPECIFIED.)
CURVE()
GEOMETRIC_REPRESENTATION_ITEM()
RATIONAL_B_SPLINE_CURVE((1.,1.,1.,1.,1.,1.,1.,1.,1.,1.,1.,1.,1.,1.,1.,1.,
1.,1.,1.,1.,1.,1.,1.,1.,1.,1.,1.,1.,1.,1.,1.,1.,1.,1.,1.,1.,1.,1.,1.,1.,
1.,1.,1.,1.,1.,1.,1.,1.,1.,1.,1.,1.,1.,1.,1.,1.,1.,1.,1.,1.,1.,1.,1.,1.,
1.,1.,1.,1.,1.,1.,1.,1.,1.,1.,1.,1.,1.,1.,1.,1.,1.,1.,1.,1.,1.,1.,1.,1.,
1.,1.,1.,1.,1.,1.,1.,1.,1.,1.,1.,1.,1.,1.,1.,1.,1.,1.,1.,1.,1.,1.,1.,1.,
1.,1.,1.,1.,1.,1.,1.,1.,1.,1.,1.,1.,1.,1.,1.,1.,1.,1.,1.,1.,1.,1.,1.,1.,
1.,1.,1.,1.,1.,1.,1.,1.,1.,1.,1.,1.,1.,1.,1.,1.,1.,1.,1.,1.,1.,1.,1.,1.,
1.,1.,1.,1.,1.,1.,1.,1.,1.,1.,1.,1.,1.,1.,1.,1.,1.,1.,1.,1.,1.,1.,1.,1.,
1.,1.,1.,1.,1.,1.,1.,1.,1.,1.))
REPRESENTATION_ITEM('')
);
#472=(
BOUNDED_CURVE()
B_SPLINE_CURVE(5,(#83693,#83694,#83695,#83696,#83697,#83698,#83699,#83700,
#83701,#83702,#83703,#83704,#83705,#83706,#83707,#83708,#83709,#83710,#83711,
#83712,#83713,#83714,#83715,#83716,#83717,#83718,#83719,#83720,#83721,#83722,
#83723,#83724,#83725,#83726,#83727,#83728,#83729,#83730,#83731,#83732,#83733,
#83734,#83735,#83736,#83737,#83738,#83739,#83740,#83741,#83742,#83743,#83744,
#83745,#83746,#83747,#83748,#83749,#83750,#83751,#83752,#83753,#83754,#83755,
#83756,#83757,#83758,#83759,#83760,#83761,#83762,#83763,#83764,#83765,#83766,
#83767,#83768,#83769,#83770,#83771,#83772,#83773,#83774,#83775,#83776,#83777,
#83778,#83779,#83780,#83781,#83782,#83783,#83784,#83785,#83786,#83787,#83788,
#83789,#83790,#83791,#83792,#83793,#83794,#83795,#83796,#83797,#83798,#83799,
#83800,#83801,#83802,#83803,#83804,#83805,#83806,#83807,#83808,#83809,#83810,
#83811,#83812,#83813,#83814,#83815,#83816,#83817,#83818,#83819,#83820,#83821,
#83822,#83823,#83824,#83825,#83826,#83827,#83828,#83829,#83830,#83831,#83832,
#83833,#83834,#83835,#83836,#83837,#83838,#83839,#83840,#83841,#83842,#83843,
#83844,#83845,#83846,#83847,#83848,#83849,#83850,#83851,#83852,#83853,#83854,
#83855,#83856,#83857,#83858,#83859,#83860,#83861,#83862,#83863,#83864,#83865,
#83866,#83867,#83868,#83869,#83870,#83871,#83872,#83873,#83874,#83875,#83876,
#83877,#83878,#83879,#83880,#83881,#83882,#83883,#83884,#83885,#83886),
 .UNSPECIFIED.,.F.,.F.)
B_SPLINE_CURVE_WITH_KNOTS((6,1,1,1,1,1,1,1,1,1,1,1,1,1,1,1,1,1,1,1,1,1,
1,1,1,1,1,1,1,1,1,1,1,1,1,1,1,1,1,1,1,1,1,1,1,1,1,1,1,1,1,1,1,1,1,1,1,1,
1,1,1,1,1,1,1,1,1,1,1,1,1,1,1,1,1,1,1,1,1,1,1,1,1,1,1,1,1,1,1,1,1,1,1,1,
1,1,1,1,1,1,1,1,1,1,1,1,1,1,1,1,1,1,1,1,1,1,1,1,1,1,1,1,1,1,1,1,1,1,1,1,
1,1,1,1,1,1,1,1,1,1,1,1,1,1,1,1,1,1,1,1,1,1,1,1,1,1,1,1,1,1,1,1,1,1,1,1,
1,1,1,1,1,1,1,1,1,1,1,1,1,1,1,1,1,1,1,1,1,1,1,6),(-0.94142984443133,-0.940000000000001,
-0.935000000000001,-0.930000000000001,-0.925000000000001,-0.920000000000001,
-0.915000000000001,-0.910000000000001,-0.905000000000001,-0.900000000000001,
-0.895000000000001,-0.890000000000001,-0.885000000000001,-0.880000000000001,
-0.875000000000001,-0.870000000000001,-0.865000000000001,-0.860000000000001,
-0.855000000000001,-0.850000000000001,-0.845000000000001,-0.840000000000001,
-0.835000000000001,-0.830000000000001,-0.825000000000001,-0.820000000000001,
-0.815000000000001,-0.810000000000001,-0.805000000000001,-0.800000000000001,
-0.795000000000001,-0.790000000000001,-0.785000000000001,-0.780000000000001,
-0.775000000000001,-0.770000000000001,-0.765000000000001,-0.760000000000001,
-0.755000000000001,-0.750000000000001,-0.745000000000001,-0.740000000000001,
-0.735000000000001,-0.730000000000001,-0.725000000000001,-0.720000000000001,
-0.715000000000001,-0.710000000000001,-0.705000000000001,-0.700000000000001,
-0.695000000000001,-0.690000000000001,-0.685,-0.68,-0.675,-0.67,-0.665,
-0.66,-0.655,-0.65,-0.645,-0.64,-0.635,-0.63,-0.625,-0.62,-0.615,-0.61,
-0.605,-0.6,-0.595,-0.59,-0.585,-0.58,-0.575,-0.57,-0.565,-0.56,-0.555,
-0.55,-0.545,-0.54,-0.535,-0.53,-0.525,-0.52,-0.515,-0.51,-0.505,-0.5,-0.495,
-0.49,-0.485,-0.48,-0.475,-0.47,-0.465,-0.46,-0.455,-0.45,-0.445,-0.44,
-0.435,-0.43,-0.425,-0.42,-0.415,-0.41,-0.405,-0.4,-0.395,-0.39,-0.385,
-0.38,-0.375,-0.37,-0.365,-0.36,-0.355,-0.35,-0.345,-0.34,-0.335,-0.33,
-0.325,-0.32,-0.315,-0.31,-0.305,-0.3,-0.295,-0.29,-0.285,-0.28,-0.275,
-0.27,-0.265,-0.26,-0.255,-0.25,-0.245,-0.24,-0.235,-0.23,-0.225,-0.22,
-0.215,-0.21,-0.205,-0.2,-0.195,-0.19,-0.185,-0.18,-0.175,-0.17,-0.165,
-0.16,-0.155,-0.15,-0.145,-0.14,-0.135,-0.13,-0.125,-0.12,-0.115,-0.11,
-0.105,-0.1,-0.095,-0.09,-0.085,-0.08,-0.075,-0.07,-0.065,-0.06,-0.055,
-0.05,-0.045,-0.04,-0.035,-0.03,-0.025,-0.02,-0.015,-0.01,-0.005,0.),
 .UNSPECIFIED.)
CURVE()
GEOMETRIC_REPRESENTATION_ITEM()
RATIONAL_B_SPLINE_CURVE((1.,1.,1.,1.,1.,1.,1.,1.,1.,1.,1.,1.,1.,1.,1.,1.,
1.,1.,1.,1.,1.,1.,1.,1.,1.,1.,1.,1.,1.,1.,1.,1.,1.,1.,1.,1.,1.,1.,1.,1.,
1.,1.,1.,1.,1.,1.,1.,1.,1.,1.,1.,1.,1.,1.,1.,1.,1.,1.,1.,1.,1.,1.,1.,1.,
1.,1.,1.,1.,1.,1.,1.,1.,1.,1.,1.,1.,1.,1.,1.,1.,1.,1.,1.,1.,1.,1.,1.,1.,
1.,1.,1.,1.,1.,1.,1.,1.,1.,1.,1.,1.,1.,1.,1.,1.,1.,1.,1.,1.,1.,1.,1.,1.,
1.,1.,1.,1.,1.,1.,1.,1.,1.,1.,1.,1.,1.,1.,1.,1.,1.,1.,1.,1.,1.,1.,1.,1.,
1.,1.,1.,1.,1.,1.,1.,1.,1.,1.,1.,1.,1.,1.,1.,1.,1.,1.,1.,1.,1.,1.,1.,1.,
1.,1.,1.,1.,1.,1.,1.,1.,1.,1.,1.,1.,1.,1.,1.,1.,1.,1.,1.,1.,1.,1.,1.,1.,
1.,1.,1.,1.,1.,1.,1.,1.,1.,1.))
REPRESENTATION_ITEM('')
);
#473=(
BOUNDED_CURVE()
B_SPLINE_CURVE(5,(#84393,#84394,#84395,#84396,#84397,#84398,#84399,#84400,
#84401,#84402,#84403,#84404,#84405,#84406,#84407,#84408,#84409,#84410,#84411,
#84412,#84413,#84414,#84415,#84416,#84417,#84418,#84419,#84420,#84421,#84422,
#84423,#84424,#84425,#84426,#84427,#84428,#84429,#84430,#84431,#84432,#84433,
#84434,#84435,#84436,#84437,#84438,#84439,#84440,#84441,#84442,#84443,#84444,
#84445,#84446,#84447,#84448,#84449,#84450,#84451,#84452,#84453,#84454,#84455,
#84456,#84457,#84458,#84459,#84460,#84461,#84462,#84463,#84464,#84465,#84466,
#84467,#84468,#84469,#84470,#84471,#84472,#84473,#84474,#84475,#84476,#84477,
#84478,#84479,#84480,#84481,#84482,#84483,#84484,#84485,#84486,#84487,#84488,
#84489,#84490,#84491,#84492,#84493,#84494,#84495,#84496,#84497,#84498,#84499,
#84500,#84501,#84502,#84503,#84504,#84505,#84506,#84507,#84508,#84509,#84510,
#84511,#84512,#84513,#84514,#84515,#84516,#84517,#84518,#84519,#84520,#84521,
#84522,#84523,#84524,#84525,#84526,#84527,#84528,#84529,#84530,#84531,#84532,
#84533,#84534,#84535,#84536,#84537,#84538,#84539,#84540,#84541,#84542,#84543,
#84544,#84545,#84546,#84547,#84548,#84549,#84550,#84551,#84552,#84553,#84554,
#84555,#84556,#84557,#84558,#84559,#84560,#84561,#84562,#84563,#84564,#84565,
#84566,#84567,#84568,#84569,#84570,#84571,#84572,#84573,#84574,#84575,#84576,
#84577,#84578,#84579,#84580,#84581,#84582,#84583,#84584,#84585,#84586),
 .UNSPECIFIED.,.F.,.F.)
B_SPLINE_CURVE_WITH_KNOTS((6,1,1,1,1,1,1,1,1,1,1,1,1,1,1,1,1,1,1,1,1,1,
1,1,1,1,1,1,1,1,1,1,1,1,1,1,1,1,1,1,1,1,1,1,1,1,1,1,1,1,1,1,1,1,1,1,1,1,
1,1,1,1,1,1,1,1,1,1,1,1,1,1,1,1,1,1,1,1,1,1,1,1,1,1,1,1,1,1,1,1,1,1,1,1,
1,1,1,1,1,1,1,1,1,1,1,1,1,1,1,1,1,1,1,1,1,1,1,1,1,1,1,1,1,1,1,1,1,1,1,1,
1,1,1,1,1,1,1,1,1,1,1,1,1,1,1,1,1,1,1,1,1,1,1,1,1,1,1,1,1,1,1,1,1,1,1,1,
1,1,1,1,1,1,1,1,1,1,1,1,1,1,1,1,1,1,1,1,1,1,1,6),(0.,0.005,0.01,0.015,0.02,
0.025,0.03,0.035,0.04,0.045,0.05,0.055,0.06,0.065,0.07,0.075,0.08,0.085,
0.09,0.095,0.1,0.105,0.11,0.115,0.12,0.125,0.13,0.135,0.14,0.145,0.15,0.155,
0.16,0.165,0.17,0.175,0.18,0.185,0.19,0.195,0.2,0.205,0.21,0.215,0.22,0.225,
0.23,0.235,0.24,0.245,0.25,0.255,0.26,0.265,0.27,0.275,0.28,0.285,0.29,
0.295,0.3,0.305,0.31,0.315,0.32,0.325,0.33,0.335,0.34,0.345,0.35,0.355,
0.36,0.365,0.37,0.375,0.38,0.385,0.39,0.395,0.4,0.405,0.41,0.415,0.42,0.425,
0.43,0.435,0.44,0.445,0.45,0.455,0.46,0.465,0.47,0.475,0.48,0.485,0.49,
0.495,0.5,0.505,0.51,0.515,0.52,0.525,0.53,0.535,0.54,0.545,0.55,0.555,
0.56,0.565,0.57,0.575,0.58,0.585,0.59,0.595,0.6,0.605,0.61,0.615,0.62,0.625,
0.63,0.635,0.64,0.645,0.65,0.655,0.66,0.665,0.67,0.675,0.68,0.685,0.690000000000001,
0.695000000000001,0.700000000000001,0.705000000000001,0.710000000000001,
0.715000000000001,0.720000000000001,0.725000000000001,0.730000000000001,
0.735000000000001,0.740000000000001,0.745000000000001,0.750000000000001,
0.755000000000001,0.760000000000001,0.765000000000001,0.770000000000001,
0.775000000000001,0.780000000000001,0.785000000000001,0.790000000000001,
0.795000000000001,0.800000000000001,0.805000000000001,0.810000000000001,
0.815000000000001,0.820000000000001,0.825000000000001,0.830000000000001,
0.835000000000001,0.840000000000001,0.845000000000001,0.850000000000001,
0.855000000000001,0.860000000000001,0.865000000000001,0.870000000000001,
0.875000000000001,0.880000000000001,0.885000000000001,0.890000000000001,
0.895000000000001,0.900000000000001,0.905000000000001,0.910000000000001,
0.915000000000001,0.920000000000001,0.925000000000001,0.930000000000001,
0.935000000000001,0.940000000000001,0.941429844431379),.UNSPECIFIED.)
CURVE()
GEOMETRIC_REPRESENTATION_ITEM()
RATIONAL_B_SPLINE_CURVE((1.,1.,1.,1.,1.,1.,1.,1.,1.,1.,1.,1.,1.,1.,1.,1.,
1.,1.,1.,1.,1.,1.,1.,1.,1.,1.,1.,1.,1.,1.,1.,1.,1.,1.,1.,1.,1.,1.,1.,1.,
1.,1.,1.,1.,1.,1.,1.,1.,1.,1.,1.,1.,1.,1.,1.,1.,1.,1.,1.,1.,1.,1.,1.,1.,
1.,1.,1.,1.,1.,1.,1.,1.,1.,1.,1.,1.,1.,1.,1.,1.,1.,1.,1.,1.,1.,1.,1.,1.,
1.,1.,1.,1.,1.,1.,1.,1.,1.,1.,1.,1.,1.,1.,1.,1.,1.,1.,1.,1.,1.,1.,1.,1.,
1.,1.,1.,1.,1.,1.,1.,1.,1.,1.,1.,1.,1.,1.,1.,1.,1.,1.,1.,1.,1.,1.,1.,1.,
1.,1.,1.,1.,1.,1.,1.,1.,1.,1.,1.,1.,1.,1.,1.,1.,1.,1.,1.,1.,1.,1.,1.,1.,
1.,1.,1.,1.,1.,1.,1.,1.,1.,1.,1.,1.,1.,1.,1.,1.,1.,1.,1.,1.,1.,1.,1.,1.,
1.,1.,1.,1.,1.,1.,1.,1.,1.,1.))
REPRESENTATION_ITEM('')
);
#474=(
BOUNDED_CURVE()
B_SPLINE_CURVE(5,(#84589,#84590,#84591,#84592,#84593,#84594,#84595,#84596,
#84597,#84598,#84599,#84600,#84601,#84602,#84603,#84604,#84605,#84606,#84607,
#84608,#84609,#84610,#84611,#84612,#84613,#84614,#84615,#84616,#84617,#84618,
#84619,#84620,#84621,#84622,#84623,#84624,#84625,#84626,#84627,#84628,#84629,
#84630,#84631,#84632,#84633,#84634,#84635,#84636,#84637,#84638,#84639,#84640,
#84641,#84642,#84643,#84644,#84645,#84646,#84647,#84648,#84649,#84650,#84651,
#84652,#84653,#84654,#84655,#84656,#84657,#84658,#84659,#84660,#84661,#84662,
#84663,#84664,#84665,#84666,#84667,#84668,#84669,#84670,#84671,#84672,#84673,
#84674,#84675,#84676,#84677,#84678,#84679,#84680,#84681,#84682,#84683,#84684,
#84685,#84686,#84687,#84688,#84689,#84690,#84691,#84692,#84693,#84694,#84695,
#84696,#84697,#84698,#84699,#84700,#84701,#84702,#84703,#84704,#84705,#84706,
#84707,#84708,#84709,#84710,#84711,#84712,#84713,#84714,#84715,#84716,#84717,
#84718,#84719,#84720,#84721,#84722,#84723,#84724,#84725,#84726,#84727,#84728,
#84729,#84730,#84731,#84732,#84733,#84734,#84735,#84736,#84737,#84738,#84739,
#84740,#84741,#84742,#84743,#84744,#84745,#84746,#84747,#84748,#84749,#84750,
#84751,#84752,#84753,#84754,#84755,#84756,#84757,#84758,#84759,#84760,#84761,
#84762,#84763,#84764,#84765,#84766,#84767,#84768,#84769,#84770,#84771,#84772,
#84773,#84774,#84775,#84776,#84777,#84778,#84779,#84780,#84781,#84782),
 .UNSPECIFIED.,.F.,.F.)
B_SPLINE_CURVE_WITH_KNOTS((6,1,1,1,1,1,1,1,1,1,1,1,1,1,1,1,1,1,1,1,1,1,
1,1,1,1,1,1,1,1,1,1,1,1,1,1,1,1,1,1,1,1,1,1,1,1,1,1,1,1,1,1,1,1,1,1,1,1,
1,1,1,1,1,1,1,1,1,1,1,1,1,1,1,1,1,1,1,1,1,1,1,1,1,1,1,1,1,1,1,1,1,1,1,1,
1,1,1,1,1,1,1,1,1,1,1,1,1,1,1,1,1,1,1,1,1,1,1,1,1,1,1,1,1,1,1,1,1,1,1,1,
1,1,1,1,1,1,1,1,1,1,1,1,1,1,1,1,1,1,1,1,1,1,1,1,1,1,1,1,1,1,1,1,1,1,1,1,
1,1,1,1,1,1,1,1,1,1,1,1,1,1,1,1,1,1,1,1,1,1,1,6),(-0.941429844431374,-0.940000000000001,
-0.935000000000001,-0.930000000000001,-0.925000000000001,-0.920000000000001,
-0.915000000000001,-0.910000000000001,-0.905000000000001,-0.900000000000001,
-0.895000000000001,-0.890000000000001,-0.885000000000001,-0.880000000000001,
-0.875000000000001,-0.870000000000001,-0.865000000000001,-0.860000000000001,
-0.855000000000001,-0.850000000000001,-0.845000000000001,-0.840000000000001,
-0.835000000000001,-0.830000000000001,-0.825000000000001,-0.820000000000001,
-0.815000000000001,-0.810000000000001,-0.805000000000001,-0.800000000000001,
-0.795000000000001,-0.790000000000001,-0.785000000000001,-0.780000000000001,
-0.775000000000001,-0.770000000000001,-0.765000000000001,-0.760000000000001,
-0.755000000000001,-0.750000000000001,-0.745000000000001,-0.740000000000001,
-0.735000000000001,-0.730000000000001,-0.725000000000001,-0.720000000000001,
-0.715000000000001,-0.710000000000001,-0.705000000000001,-0.700000000000001,
-0.695000000000001,-0.690000000000001,-0.685,-0.68,-0.675,-0.67,-0.665,
-0.66,-0.655,-0.65,-0.645,-0.64,-0.635,-0.63,-0.625,-0.62,-0.615,-0.61,
-0.605,-0.6,-0.595,-0.59,-0.585,-0.58,-0.575,-0.57,-0.565,-0.56,-0.555,
-0.55,-0.545,-0.54,-0.535,-0.53,-0.525,-0.52,-0.515,-0.51,-0.505,-0.5,-0.495,
-0.49,-0.485,-0.48,-0.475,-0.47,-0.465,-0.46,-0.455,-0.45,-0.445,-0.44,
-0.435,-0.43,-0.425,-0.42,-0.415,-0.41,-0.405,-0.4,-0.395,-0.39,-0.385,
-0.38,-0.375,-0.37,-0.365,-0.36,-0.355,-0.35,-0.345,-0.34,-0.335,-0.33,
-0.325,-0.32,-0.315,-0.31,-0.305,-0.3,-0.295,-0.29,-0.285,-0.28,-0.275,
-0.27,-0.265,-0.26,-0.255,-0.25,-0.245,-0.24,-0.235,-0.23,-0.225,-0.22,
-0.215,-0.21,-0.205,-0.2,-0.195,-0.19,-0.185,-0.18,-0.175,-0.17,-0.165,
-0.16,-0.155,-0.15,-0.145,-0.14,-0.135,-0.13,-0.125,-0.12,-0.115,-0.11,
-0.105,-0.1,-0.095,-0.09,-0.085,-0.08,-0.075,-0.07,-0.065,-0.06,-0.055,
-0.05,-0.045,-0.04,-0.035,-0.03,-0.025,-0.02,-0.015,-0.01,-0.005,0.),
 .UNSPECIFIED.)
CURVE()
GEOMETRIC_REPRESENTATION_ITEM()
RATIONAL_B_SPLINE_CURVE((1.,1.,1.,1.,1.,1.,1.,1.,1.,1.,1.,1.,1.,1.,1.,1.,
1.,1.,1.,1.,1.,1.,1.,1.,1.,1.,1.,1.,1.,1.,1.,1.,1.,1.,1.,1.,1.,1.,1.,1.,
1.,1.,1.,1.,1.,1.,1.,1.,1.,1.,1.,1.,1.,1.,1.,1.,1.,1.,1.,1.,1.,1.,1.,1.,
1.,1.,1.,1.,1.,1.,1.,1.,1.,1.,1.,1.,1.,1.,1.,1.,1.,1.,1.,1.,1.,1.,1.,1.,
1.,1.,1.,1.,1.,1.,1.,1.,1.,1.,1.,1.,1.,1.,1.,1.,1.,1.,1.,1.,1.,1.,1.,1.,
1.,1.,1.,1.,1.,1.,1.,1.,1.,1.,1.,1.,1.,1.,1.,1.,1.,1.,1.,1.,1.,1.,1.,1.,
1.,1.,1.,1.,1.,1.,1.,1.,1.,1.,1.,1.,1.,1.,1.,1.,1.,1.,1.,1.,1.,1.,1.,1.,
1.,1.,1.,1.,1.,1.,1.,1.,1.,1.,1.,1.,1.,1.,1.,1.,1.,1.,1.,1.,1.,1.,1.,1.,
1.,1.,1.,1.,1.,1.,1.,1.,1.,1.))
REPRESENTATION_ITEM('')
);
#475=(
BOUNDED_CURVE()
B_SPLINE_CURVE(5,(#85289,#85290,#85291,#85292,#85293,#85294,#85295,#85296,
#85297,#85298,#85299,#85300,#85301,#85302,#85303,#85304,#85305,#85306,#85307,
#85308,#85309,#85310,#85311,#85312,#85313,#85314,#85315,#85316,#85317,#85318,
#85319,#85320,#85321,#85322,#85323,#85324,#85325,#85326,#85327,#85328,#85329,
#85330,#85331,#85332,#85333,#85334,#85335,#85336,#85337,#85338,#85339,#85340,
#85341,#85342,#85343,#85344,#85345,#85346,#85347,#85348,#85349,#85350,#85351,
#85352,#85353,#85354,#85355,#85356,#85357,#85358,#85359,#85360,#85361,#85362,
#85363,#85364,#85365,#85366,#85367,#85368,#85369,#85370,#85371,#85372,#85373,
#85374,#85375,#85376,#85377,#85378,#85379,#85380,#85381,#85382,#85383,#85384,
#85385,#85386,#85387,#85388,#85389,#85390,#85391,#85392,#85393,#85394,#85395,
#85396,#85397,#85398,#85399,#85400,#85401,#85402,#85403,#85404,#85405,#85406,
#85407,#85408,#85409,#85410,#85411,#85412,#85413,#85414,#85415,#85416,#85417,
#85418,#85419,#85420,#85421,#85422,#85423,#85424,#85425,#85426,#85427,#85428,
#85429,#85430,#85431,#85432,#85433,#85434,#85435,#85436,#85437,#85438,#85439,
#85440,#85441,#85442,#85443,#85444,#85445,#85446,#85447,#85448,#85449,#85450,
#85451,#85452,#85453,#85454,#85455,#85456,#85457,#85458,#85459,#85460,#85461,
#85462,#85463,#85464,#85465,#85466,#85467,#85468,#85469,#85470,#85471,#85472,
#85473,#85474,#85475,#85476,#85477,#85478,#85479,#85480,#85481,#85482),
 .UNSPECIFIED.,.F.,.F.)
B_SPLINE_CURVE_WITH_KNOTS((6,1,1,1,1,1,1,1,1,1,1,1,1,1,1,1,1,1,1,1,1,1,
1,1,1,1,1,1,1,1,1,1,1,1,1,1,1,1,1,1,1,1,1,1,1,1,1,1,1,1,1,1,1,1,1,1,1,1,
1,1,1,1,1,1,1,1,1,1,1,1,1,1,1,1,1,1,1,1,1,1,1,1,1,1,1,1,1,1,1,1,1,1,1,1,
1,1,1,1,1,1,1,1,1,1,1,1,1,1,1,1,1,1,1,1,1,1,1,1,1,1,1,1,1,1,1,1,1,1,1,1,
1,1,1,1,1,1,1,1,1,1,1,1,1,1,1,1,1,1,1,1,1,1,1,1,1,1,1,1,1,1,1,1,1,1,1,1,
1,1,1,1,1,1,1,1,1,1,1,1,1,1,1,1,1,1,1,1,1,1,1,6),(0.,0.005,0.01,0.015,0.02,
0.025,0.03,0.035,0.04,0.045,0.05,0.055,0.06,0.065,0.07,0.075,0.08,0.085,
0.09,0.095,0.1,0.105,0.11,0.115,0.12,0.125,0.13,0.135,0.14,0.145,0.15,0.155,
0.16,0.165,0.17,0.175,0.18,0.185,0.19,0.195,0.2,0.205,0.21,0.215,0.22,0.225,
0.23,0.235,0.24,0.245,0.25,0.255,0.26,0.265,0.27,0.275,0.28,0.285,0.29,
0.295,0.3,0.305,0.31,0.315,0.32,0.325,0.33,0.335,0.34,0.345,0.35,0.355,
0.36,0.365,0.37,0.375,0.38,0.385,0.39,0.395,0.4,0.405,0.41,0.415,0.42,0.425,
0.43,0.435,0.44,0.445,0.45,0.455,0.46,0.465,0.47,0.475,0.48,0.485,0.49,
0.495,0.5,0.505,0.51,0.515,0.52,0.525,0.53,0.535,0.54,0.545,0.55,0.555,
0.56,0.565,0.57,0.575,0.58,0.585,0.59,0.595,0.6,0.605,0.61,0.615,0.62,0.625,
0.63,0.635,0.64,0.645,0.65,0.655,0.66,0.665,0.67,0.675,0.68,0.685,0.690000000000001,
0.695000000000001,0.700000000000001,0.705000000000001,0.710000000000001,
0.715000000000001,0.720000000000001,0.725000000000001,0.730000000000001,
0.735000000000001,0.740000000000001,0.745000000000001,0.750000000000001,
0.755000000000001,0.760000000000001,0.765000000000001,0.770000000000001,
0.775000000000001,0.780000000000001,0.785000000000001,0.790000000000001,
0.795000000000001,0.800000000000001,0.805000000000001,0.810000000000001,
0.815000000000001,0.820000000000001,0.825000000000001,0.830000000000001,
0.835000000000001,0.840000000000001,0.845000000000001,0.850000000000001,
0.855000000000001,0.860000000000001,0.865000000000001,0.870000000000001,
0.875000000000001,0.880000000000001,0.885000000000001,0.890000000000001,
0.895000000000001,0.900000000000001,0.905000000000001,0.910000000000001,
0.915000000000001,0.920000000000001,0.925000000000001,0.930000000000001,
0.935000000000001,0.940000000000001,0.94142984443142),.UNSPECIFIED.)
CURVE()
GEOMETRIC_REPRESENTATION_ITEM()
RATIONAL_B_SPLINE_CURVE((1.,1.,1.,1.,1.,1.,1.,1.,1.,1.,1.,1.,1.,1.,1.,1.,
1.,1.,1.,1.,1.,1.,1.,1.,1.,1.,1.,1.,1.,1.,1.,1.,1.,1.,1.,1.,1.,1.,1.,1.,
1.,1.,1.,1.,1.,1.,1.,1.,1.,1.,1.,1.,1.,1.,1.,1.,1.,1.,1.,1.,1.,1.,1.,1.,
1.,1.,1.,1.,1.,1.,1.,1.,1.,1.,1.,1.,1.,1.,1.,1.,1.,1.,1.,1.,1.,1.,1.,1.,
1.,1.,1.,1.,1.,1.,1.,1.,1.,1.,1.,1.,1.,1.,1.,1.,1.,1.,1.,1.,1.,1.,1.,1.,
1.,1.,1.,1.,1.,1.,1.,1.,1.,1.,1.,1.,1.,1.,1.,1.,1.,1.,1.,1.,1.,1.,1.,1.,
1.,1.,1.,1.,1.,1.,1.,1.,1.,1.,1.,1.,1.,1.,1.,1.,1.,1.,1.,1.,1.,1.,1.,1.,
1.,1.,1.,1.,1.,1.,1.,1.,1.,1.,1.,1.,1.,1.,1.,1.,1.,1.,1.,1.,1.,1.,1.,1.,
1.,1.,1.,1.,1.,1.,1.,1.,1.,1.))
REPRESENTATION_ITEM('')
);
#476=(
BOUNDED_CURVE()
B_SPLINE_CURVE(5,(#85485,#85486,#85487,#85488,#85489,#85490,#85491,#85492,
#85493,#85494,#85495,#85496,#85497,#85498,#85499,#85500,#85501,#85502,#85503,
#85504,#85505,#85506,#85507,#85508,#85509,#85510,#85511,#85512,#85513,#85514,
#85515,#85516,#85517,#85518,#85519,#85520,#85521,#85522,#85523,#85524,#85525,
#85526,#85527,#85528,#85529,#85530,#85531,#85532,#85533,#85534,#85535,#85536,
#85537,#85538,#85539,#85540,#85541,#85542,#85543,#85544,#85545,#85546,#85547,
#85548,#85549,#85550,#85551,#85552,#85553,#85554,#85555,#85556,#85557,#85558,
#85559,#85560,#85561,#85562,#85563,#85564,#85565,#85566,#85567,#85568,#85569,
#85570,#85571,#85572,#85573,#85574,#85575,#85576,#85577,#85578,#85579,#85580,
#85581,#85582,#85583,#85584,#85585,#85586,#85587,#85588,#85589,#85590,#85591,
#85592,#85593,#85594,#85595,#85596,#85597,#85598,#85599,#85600,#85601,#85602,
#85603,#85604,#85605,#85606,#85607,#85608,#85609,#85610,#85611,#85612,#85613,
#85614,#85615,#85616,#85617,#85618,#85619,#85620,#85621,#85622,#85623,#85624,
#85625,#85626,#85627,#85628,#85629,#85630,#85631,#85632,#85633,#85634,#85635,
#85636,#85637,#85638,#85639,#85640,#85641,#85642,#85643,#85644,#85645,#85646,
#85647,#85648,#85649,#85650,#85651,#85652,#85653,#85654,#85655,#85656,#85657,
#85658,#85659,#85660,#85661,#85662,#85663,#85664,#85665,#85666,#85667,#85668,
#85669,#85670,#85671,#85672,#85673,#85674,#85675,#85676,#85677,#85678),
 .UNSPECIFIED.,.F.,.F.)
B_SPLINE_CURVE_WITH_KNOTS((6,1,1,1,1,1,1,1,1,1,1,1,1,1,1,1,1,1,1,1,1,1,
1,1,1,1,1,1,1,1,1,1,1,1,1,1,1,1,1,1,1,1,1,1,1,1,1,1,1,1,1,1,1,1,1,1,1,1,
1,1,1,1,1,1,1,1,1,1,1,1,1,1,1,1,1,1,1,1,1,1,1,1,1,1,1,1,1,1,1,1,1,1,1,1,
1,1,1,1,1,1,1,1,1,1,1,1,1,1,1,1,1,1,1,1,1,1,1,1,1,1,1,1,1,1,1,1,1,1,1,1,
1,1,1,1,1,1,1,1,1,1,1,1,1,1,1,1,1,1,1,1,1,1,1,1,1,1,1,1,1,1,1,1,1,1,1,1,
1,1,1,1,1,1,1,1,1,1,1,1,1,1,1,1,1,1,1,1,1,1,1,6),(-0.94142984443141,-0.940000000000001,
-0.935000000000001,-0.930000000000001,-0.925000000000001,-0.920000000000001,
-0.915000000000001,-0.910000000000001,-0.905000000000001,-0.900000000000001,
-0.895000000000001,-0.890000000000001,-0.885000000000001,-0.880000000000001,
-0.875000000000001,-0.870000000000001,-0.865000000000001,-0.860000000000001,
-0.855000000000001,-0.850000000000001,-0.845000000000001,-0.840000000000001,
-0.835000000000001,-0.830000000000001,-0.825000000000001,-0.820000000000001,
-0.815000000000001,-0.810000000000001,-0.805000000000001,-0.800000000000001,
-0.795000000000001,-0.790000000000001,-0.785000000000001,-0.780000000000001,
-0.775000000000001,-0.770000000000001,-0.765000000000001,-0.760000000000001,
-0.755000000000001,-0.750000000000001,-0.745000000000001,-0.740000000000001,
-0.735000000000001,-0.730000000000001,-0.725000000000001,-0.720000000000001,
-0.715000000000001,-0.710000000000001,-0.705000000000001,-0.700000000000001,
-0.695000000000001,-0.690000000000001,-0.685,-0.68,-0.675,-0.67,-0.665,
-0.66,-0.655,-0.65,-0.645,-0.64,-0.635,-0.63,-0.625,-0.62,-0.615,-0.61,
-0.605,-0.6,-0.595,-0.59,-0.585,-0.58,-0.575,-0.57,-0.565,-0.56,-0.555,
-0.55,-0.545,-0.54,-0.535,-0.53,-0.525,-0.52,-0.515,-0.51,-0.505,-0.5,-0.495,
-0.49,-0.485,-0.48,-0.475,-0.47,-0.465,-0.46,-0.455,-0.45,-0.445,-0.44,
-0.435,-0.43,-0.425,-0.42,-0.415,-0.41,-0.405,-0.4,-0.395,-0.39,-0.385,
-0.38,-0.375,-0.37,-0.365,-0.36,-0.355,-0.35,-0.345,-0.34,-0.335,-0.33,
-0.325,-0.32,-0.315,-0.31,-0.305,-0.3,-0.295,-0.29,-0.285,-0.28,-0.275,
-0.27,-0.265,-0.26,-0.255,-0.25,-0.245,-0.24,-0.235,-0.23,-0.225,-0.22,
-0.215,-0.21,-0.205,-0.2,-0.195,-0.19,-0.185,-0.18,-0.175,-0.17,-0.165,
-0.16,-0.155,-0.15,-0.145,-0.14,-0.135,-0.13,-0.125,-0.12,-0.115,-0.11,
-0.105,-0.1,-0.095,-0.09,-0.085,-0.08,-0.075,-0.07,-0.065,-0.06,-0.055,
-0.05,-0.045,-0.04,-0.035,-0.03,-0.025,-0.02,-0.015,-0.01,-0.005,0.),
 .UNSPECIFIED.)
CURVE()
GEOMETRIC_REPRESENTATION_ITEM()
RATIONAL_B_SPLINE_CURVE((1.,1.,1.,1.,1.,1.,1.,1.,1.,1.,1.,1.,1.,1.,1.,1.,
1.,1.,1.,1.,1.,1.,1.,1.,1.,1.,1.,1.,1.,1.,1.,1.,1.,1.,1.,1.,1.,1.,1.,1.,
1.,1.,1.,1.,1.,1.,1.,1.,1.,1.,1.,1.,1.,1.,1.,1.,1.,1.,1.,1.,1.,1.,1.,1.,
1.,1.,1.,1.,1.,1.,1.,1.,1.,1.,1.,1.,1.,1.,1.,1.,1.,1.,1.,1.,1.,1.,1.,1.,
1.,1.,1.,1.,1.,1.,1.,1.,1.,1.,1.,1.,1.,1.,1.,1.,1.,1.,1.,1.,1.,1.,1.,1.,
1.,1.,1.,1.,1.,1.,1.,1.,1.,1.,1.,1.,1.,1.,1.,1.,1.,1.,1.,1.,1.,1.,1.,1.,
1.,1.,1.,1.,1.,1.,1.,1.,1.,1.,1.,1.,1.,1.,1.,1.,1.,1.,1.,1.,1.,1.,1.,1.,
1.,1.,1.,1.,1.,1.,1.,1.,1.,1.,1.,1.,1.,1.,1.,1.,1.,1.,1.,1.,1.,1.,1.,1.,
1.,1.,1.,1.,1.,1.,1.,1.,1.,1.))
REPRESENTATION_ITEM('')
);
#477=(
BOUNDED_CURVE()
B_SPLINE_CURVE(5,(#86185,#86186,#86187,#86188,#86189,#86190,#86191,#86192,
#86193,#86194,#86195,#86196,#86197,#86198,#86199,#86200,#86201,#86202,#86203,
#86204,#86205,#86206,#86207,#86208,#86209,#86210,#86211,#86212,#86213,#86214,
#86215,#86216,#86217,#86218,#86219,#86220,#86221,#86222,#86223,#86224,#86225,
#86226,#86227,#86228,#86229,#86230,#86231,#86232,#86233,#86234,#86235,#86236,
#86237,#86238,#86239,#86240,#86241,#86242,#86243,#86244,#86245,#86246,#86247,
#86248,#86249,#86250,#86251,#86252,#86253,#86254,#86255,#86256,#86257,#86258,
#86259,#86260,#86261,#86262,#86263,#86264,#86265,#86266,#86267,#86268,#86269,
#86270,#86271,#86272,#86273,#86274,#86275,#86276,#86277,#86278,#86279,#86280,
#86281,#86282,#86283,#86284,#86285,#86286,#86287,#86288,#86289,#86290,#86291,
#86292,#86293,#86294,#86295,#86296,#86297,#86298,#86299,#86300,#86301,#86302,
#86303,#86304,#86305,#86306,#86307,#86308,#86309,#86310,#86311,#86312,#86313,
#86314,#86315,#86316,#86317,#86318,#86319,#86320,#86321,#86322,#86323,#86324,
#86325,#86326,#86327,#86328,#86329,#86330,#86331,#86332,#86333,#86334,#86335,
#86336,#86337,#86338,#86339,#86340,#86341,#86342,#86343,#86344,#86345,#86346,
#86347,#86348,#86349,#86350,#86351,#86352,#86353,#86354,#86355,#86356,#86357,
#86358,#86359,#86360,#86361,#86362,#86363,#86364,#86365,#86366,#86367,#86368,
#86369,#86370,#86371,#86372,#86373,#86374,#86375,#86376,#86377,#86378),
 .UNSPECIFIED.,.F.,.F.)
B_SPLINE_CURVE_WITH_KNOTS((6,1,1,1,1,1,1,1,1,1,1,1,1,1,1,1,1,1,1,1,1,1,
1,1,1,1,1,1,1,1,1,1,1,1,1,1,1,1,1,1,1,1,1,1,1,1,1,1,1,1,1,1,1,1,1,1,1,1,
1,1,1,1,1,1,1,1,1,1,1,1,1,1,1,1,1,1,1,1,1,1,1,1,1,1,1,1,1,1,1,1,1,1,1,1,
1,1,1,1,1,1,1,1,1,1,1,1,1,1,1,1,1,1,1,1,1,1,1,1,1,1,1,1,1,1,1,1,1,1,1,1,
1,1,1,1,1,1,1,1,1,1,1,1,1,1,1,1,1,1,1,1,1,1,1,1,1,1,1,1,1,1,1,1,1,1,1,1,
1,1,1,1,1,1,1,1,1,1,1,1,1,1,1,1,1,1,1,1,1,1,1,6),(0.,0.005,0.01,0.015,0.02,
0.025,0.03,0.035,0.04,0.045,0.05,0.055,0.06,0.065,0.07,0.075,0.08,0.085,
0.09,0.095,0.1,0.105,0.11,0.115,0.12,0.125,0.13,0.135,0.14,0.145,0.15,0.155,
0.16,0.165,0.17,0.175,0.18,0.185,0.19,0.195,0.2,0.205,0.21,0.215,0.22,0.225,
0.23,0.235,0.24,0.245,0.25,0.255,0.26,0.265,0.27,0.275,0.28,0.285,0.29,
0.295,0.3,0.305,0.31,0.315,0.32,0.325,0.33,0.335,0.34,0.345,0.35,0.355,
0.36,0.365,0.37,0.375,0.38,0.385,0.39,0.395,0.4,0.405,0.41,0.415,0.42,0.425,
0.43,0.435,0.44,0.445,0.45,0.455,0.46,0.465,0.47,0.475,0.48,0.485,0.49,
0.495,0.5,0.505,0.51,0.515,0.52,0.525,0.53,0.535,0.54,0.545,0.55,0.555,
0.56,0.565,0.57,0.575,0.58,0.585,0.59,0.595,0.6,0.605,0.61,0.615,0.62,0.625,
0.63,0.635,0.64,0.645,0.65,0.655,0.66,0.665,0.67,0.675,0.68,0.685,0.690000000000001,
0.695000000000001,0.700000000000001,0.705000000000001,0.710000000000001,
0.715000000000001,0.720000000000001,0.725000000000001,0.730000000000001,
0.735000000000001,0.740000000000001,0.745000000000001,0.750000000000001,
0.755000000000001,0.760000000000001,0.765000000000001,0.770000000000001,
0.775000000000001,0.780000000000001,0.785000000000001,0.790000000000001,
0.795000000000001,0.800000000000001,0.805000000000001,0.810000000000001,
0.815000000000001,0.820000000000001,0.825000000000001,0.830000000000001,
0.835000000000001,0.840000000000001,0.845000000000001,0.850000000000001,
0.855000000000001,0.860000000000001,0.865000000000001,0.870000000000001,
0.875000000000001,0.880000000000001,0.885000000000001,0.890000000000001,
0.895000000000001,0.900000000000001,0.905000000000001,0.910000000000001,
0.915000000000001,0.920000000000001,0.925000000000001,0.930000000000001,
0.935000000000001,0.940000000000001,0.941429844431322),.UNSPECIFIED.)
CURVE()
GEOMETRIC_REPRESENTATION_ITEM()
RATIONAL_B_SPLINE_CURVE((1.,1.,1.,1.,1.,1.,1.,1.,1.,1.,1.,1.,1.,1.,1.,1.,
1.,1.,1.,1.,1.,1.,1.,1.,1.,1.,1.,1.,1.,1.,1.,1.,1.,1.,1.,1.,1.,1.,1.,1.,
1.,1.,1.,1.,1.,1.,1.,1.,1.,1.,1.,1.,1.,1.,1.,1.,1.,1.,1.,1.,1.,1.,1.,1.,
1.,1.,1.,1.,1.,1.,1.,1.,1.,1.,1.,1.,1.,1.,1.,1.,1.,1.,1.,1.,1.,1.,1.,1.,
1.,1.,1.,1.,1.,1.,1.,1.,1.,1.,1.,1.,1.,1.,1.,1.,1.,1.,1.,1.,1.,1.,1.,1.,
1.,1.,1.,1.,1.,1.,1.,1.,1.,1.,1.,1.,1.,1.,1.,1.,1.,1.,1.,1.,1.,1.,1.,1.,
1.,1.,1.,1.,1.,1.,1.,1.,1.,1.,1.,1.,1.,1.,1.,1.,1.,1.,1.,1.,1.,1.,1.,1.,
1.,1.,1.,1.,1.,1.,1.,1.,1.,1.,1.,1.,1.,1.,1.,1.,1.,1.,1.,1.,1.,1.,1.,1.,
1.,1.,1.,1.,1.,1.,1.,1.,1.,1.))
REPRESENTATION_ITEM('')
);
#478=(
BOUNDED_CURVE()
B_SPLINE_CURVE(5,(#86381,#86382,#86383,#86384,#86385,#86386,#86387,#86388,
#86389,#86390,#86391,#86392,#86393,#86394,#86395,#86396,#86397,#86398,#86399,
#86400,#86401,#86402,#86403,#86404,#86405,#86406,#86407,#86408,#86409,#86410,
#86411,#86412,#86413,#86414,#86415,#86416,#86417,#86418,#86419,#86420,#86421,
#86422,#86423,#86424,#86425,#86426,#86427,#86428,#86429,#86430,#86431,#86432,
#86433,#86434,#86435,#86436,#86437,#86438,#86439,#86440,#86441,#86442,#86443,
#86444,#86445,#86446,#86447,#86448,#86449,#86450,#86451,#86452,#86453,#86454,
#86455,#86456,#86457,#86458,#86459,#86460,#86461,#86462,#86463,#86464,#86465,
#86466,#86467,#86468,#86469,#86470,#86471,#86472,#86473,#86474,#86475,#86476,
#86477,#86478,#86479,#86480,#86481,#86482,#86483,#86484,#86485,#86486,#86487,
#86488,#86489,#86490,#86491,#86492,#86493,#86494,#86495,#86496,#86497,#86498,
#86499,#86500,#86501,#86502,#86503,#86504,#86505,#86506,#86507,#86508,#86509,
#86510,#86511,#86512,#86513,#86514,#86515,#86516,#86517,#86518,#86519,#86520,
#86521,#86522,#86523,#86524,#86525,#86526,#86527,#86528,#86529,#86530,#86531,
#86532,#86533,#86534,#86535,#86536,#86537,#86538,#86539,#86540,#86541,#86542,
#86543,#86544,#86545,#86546,#86547,#86548,#86549,#86550,#86551,#86552,#86553,
#86554,#86555,#86556,#86557,#86558,#86559,#86560,#86561,#86562,#86563,#86564,
#86565,#86566,#86567,#86568,#86569,#86570,#86571,#86572,#86573,#86574),
 .UNSPECIFIED.,.F.,.F.)
B_SPLINE_CURVE_WITH_KNOTS((6,1,1,1,1,1,1,1,1,1,1,1,1,1,1,1,1,1,1,1,1,1,
1,1,1,1,1,1,1,1,1,1,1,1,1,1,1,1,1,1,1,1,1,1,1,1,1,1,1,1,1,1,1,1,1,1,1,1,
1,1,1,1,1,1,1,1,1,1,1,1,1,1,1,1,1,1,1,1,1,1,1,1,1,1,1,1,1,1,1,1,1,1,1,1,
1,1,1,1,1,1,1,1,1,1,1,1,1,1,1,1,1,1,1,1,1,1,1,1,1,1,1,1,1,1,1,1,1,1,1,1,
1,1,1,1,1,1,1,1,1,1,1,1,1,1,1,1,1,1,1,1,1,1,1,1,1,1,1,1,1,1,1,1,1,1,1,1,
1,1,1,1,1,1,1,1,1,1,1,1,1,1,1,1,1,1,1,1,1,1,1,6),(-0.941429844431322,-0.940000000000001,
-0.935000000000001,-0.930000000000001,-0.925000000000001,-0.920000000000001,
-0.915000000000001,-0.910000000000001,-0.905000000000001,-0.900000000000001,
-0.895000000000001,-0.890000000000001,-0.885000000000001,-0.880000000000001,
-0.875000000000001,-0.870000000000001,-0.865000000000001,-0.860000000000001,
-0.855000000000001,-0.850000000000001,-0.845000000000001,-0.840000000000001,
-0.835000000000001,-0.830000000000001,-0.825000000000001,-0.820000000000001,
-0.815000000000001,-0.810000000000001,-0.805000000000001,-0.800000000000001,
-0.795000000000001,-0.790000000000001,-0.785000000000001,-0.780000000000001,
-0.775000000000001,-0.770000000000001,-0.765000000000001,-0.760000000000001,
-0.755000000000001,-0.750000000000001,-0.745000000000001,-0.740000000000001,
-0.735000000000001,-0.730000000000001,-0.725000000000001,-0.720000000000001,
-0.715000000000001,-0.710000000000001,-0.705000000000001,-0.700000000000001,
-0.695000000000001,-0.690000000000001,-0.685,-0.68,-0.675,-0.67,-0.665,
-0.66,-0.655,-0.65,-0.645,-0.64,-0.635,-0.63,-0.625,-0.62,-0.615,-0.61,
-0.605,-0.6,-0.595,-0.59,-0.585,-0.58,-0.575,-0.57,-0.565,-0.56,-0.555,
-0.55,-0.545,-0.54,-0.535,-0.53,-0.525,-0.52,-0.515,-0.51,-0.505,-0.5,-0.495,
-0.49,-0.485,-0.48,-0.475,-0.47,-0.465,-0.46,-0.455,-0.45,-0.445,-0.44,
-0.435,-0.43,-0.425,-0.42,-0.415,-0.41,-0.405,-0.4,-0.395,-0.39,-0.385,
-0.38,-0.375,-0.37,-0.365,-0.36,-0.355,-0.35,-0.345,-0.34,-0.335,-0.33,
-0.325,-0.32,-0.315,-0.31,-0.305,-0.3,-0.295,-0.29,-0.285,-0.28,-0.275,
-0.27,-0.265,-0.26,-0.255,-0.25,-0.245,-0.24,-0.235,-0.23,-0.225,-0.22,
-0.215,-0.21,-0.205,-0.2,-0.195,-0.19,-0.185,-0.18,-0.175,-0.17,-0.165,
-0.16,-0.155,-0.15,-0.145,-0.14,-0.135,-0.13,-0.125,-0.12,-0.115,-0.11,
-0.105,-0.1,-0.095,-0.09,-0.085,-0.08,-0.075,-0.07,-0.065,-0.06,-0.055,
-0.05,-0.045,-0.04,-0.035,-0.03,-0.025,-0.02,-0.015,-0.01,-0.005,0.),
 .UNSPECIFIED.)
CURVE()
GEOMETRIC_REPRESENTATION_ITEM()
RATIONAL_B_SPLINE_CURVE((1.,1.,1.,1.,1.,1.,1.,1.,1.,1.,1.,1.,1.,1.,1.,1.,
1.,1.,1.,1.,1.,1.,1.,1.,1.,1.,1.,1.,1.,1.,1.,1.,1.,1.,1.,1.,1.,1.,1.,1.,
1.,1.,1.,1.,1.,1.,1.,1.,1.,1.,1.,1.,1.,1.,1.,1.,1.,1.,1.,1.,1.,1.,1.,1.,
1.,1.,1.,1.,1.,1.,1.,1.,1.,1.,1.,1.,1.,1.,1.,1.,1.,1.,1.,1.,1.,1.,1.,1.,
1.,1.,1.,1.,1.,1.,1.,1.,1.,1.,1.,1.,1.,1.,1.,1.,1.,1.,1.,1.,1.,1.,1.,1.,
1.,1.,1.,1.,1.,1.,1.,1.,1.,1.,1.,1.,1.,1.,1.,1.,1.,1.,1.,1.,1.,1.,1.,1.,
1.,1.,1.,1.,1.,1.,1.,1.,1.,1.,1.,1.,1.,1.,1.,1.,1.,1.,1.,1.,1.,1.,1.,1.,
1.,1.,1.,1.,1.,1.,1.,1.,1.,1.,1.,1.,1.,1.,1.,1.,1.,1.,1.,1.,1.,1.,1.,1.,
1.,1.,1.,1.,1.,1.,1.,1.,1.,1.))
REPRESENTATION_ITEM('')
);
#479=(
BOUNDED_CURVE()
B_SPLINE_CURVE(5,(#87081,#87082,#87083,#87084,#87085,#87086,#87087,#87088,
#87089,#87090,#87091,#87092,#87093,#87094,#87095,#87096,#87097,#87098,#87099,
#87100,#87101,#87102,#87103,#87104,#87105,#87106,#87107,#87108,#87109,#87110,
#87111,#87112,#87113,#87114,#87115,#87116,#87117,#87118,#87119,#87120,#87121,
#87122,#87123,#87124,#87125,#87126,#87127,#87128,#87129,#87130,#87131,#87132,
#87133,#87134,#87135,#87136,#87137,#87138,#87139,#87140,#87141,#87142,#87143,
#87144,#87145,#87146,#87147,#87148,#87149,#87150,#87151,#87152,#87153,#87154,
#87155,#87156,#87157,#87158,#87159,#87160,#87161,#87162,#87163,#87164,#87165,
#87166,#87167,#87168,#87169,#87170,#87171,#87172,#87173,#87174,#87175,#87176,
#87177,#87178,#87179,#87180,#87181,#87182,#87183,#87184,#87185,#87186,#87187,
#87188,#87189,#87190,#87191,#87192,#87193,#87194,#87195,#87196,#87197,#87198,
#87199,#87200,#87201,#87202,#87203,#87204,#87205,#87206,#87207,#87208,#87209,
#87210,#87211,#87212,#87213,#87214,#87215,#87216,#87217,#87218,#87219,#87220,
#87221,#87222,#87223,#87224,#87225,#87226,#87227,#87228,#87229,#87230,#87231,
#87232,#87233,#87234,#87235,#87236,#87237,#87238,#87239,#87240,#87241,#87242,
#87243,#87244,#87245,#87246,#87247,#87248,#87249,#87250,#87251,#87252,#87253,
#87254,#87255,#87256,#87257,#87258,#87259,#87260,#87261,#87262,#87263,#87264,
#87265,#87266,#87267,#87268,#87269,#87270,#87271,#87272,#87273,#87274),
 .UNSPECIFIED.,.F.,.F.)
B_SPLINE_CURVE_WITH_KNOTS((6,1,1,1,1,1,1,1,1,1,1,1,1,1,1,1,1,1,1,1,1,1,
1,1,1,1,1,1,1,1,1,1,1,1,1,1,1,1,1,1,1,1,1,1,1,1,1,1,1,1,1,1,1,1,1,1,1,1,
1,1,1,1,1,1,1,1,1,1,1,1,1,1,1,1,1,1,1,1,1,1,1,1,1,1,1,1,1,1,1,1,1,1,1,1,
1,1,1,1,1,1,1,1,1,1,1,1,1,1,1,1,1,1,1,1,1,1,1,1,1,1,1,1,1,1,1,1,1,1,1,1,
1,1,1,1,1,1,1,1,1,1,1,1,1,1,1,1,1,1,1,1,1,1,1,1,1,1,1,1,1,1,1,1,1,1,1,1,
1,1,1,1,1,1,1,1,1,1,1,1,1,1,1,1,1,1,1,1,1,1,1,6),(0.,0.005,0.01,0.015,0.02,
0.025,0.03,0.035,0.04,0.045,0.05,0.055,0.06,0.065,0.07,0.075,0.08,0.085,
0.09,0.095,0.1,0.105,0.11,0.115,0.12,0.125,0.13,0.135,0.14,0.145,0.15,0.155,
0.16,0.165,0.17,0.175,0.18,0.185,0.19,0.195,0.2,0.205,0.21,0.215,0.22,0.225,
0.23,0.235,0.24,0.245,0.25,0.255,0.26,0.265,0.27,0.275,0.28,0.285,0.29,
0.295,0.3,0.305,0.31,0.315,0.32,0.325,0.33,0.335,0.34,0.345,0.35,0.355,
0.36,0.365,0.37,0.375,0.38,0.385,0.39,0.395,0.4,0.405,0.41,0.415,0.42,0.425,
0.43,0.435,0.44,0.445,0.45,0.455,0.46,0.465,0.47,0.475,0.48,0.485,0.49,
0.495,0.5,0.505,0.51,0.515,0.52,0.525,0.53,0.535,0.54,0.545,0.55,0.555,
0.56,0.565,0.57,0.575,0.58,0.585,0.59,0.595,0.6,0.605,0.61,0.615,0.62,0.625,
0.63,0.635,0.64,0.645,0.65,0.655,0.66,0.665,0.67,0.675,0.68,0.685,0.690000000000001,
0.695000000000001,0.700000000000001,0.705000000000001,0.710000000000001,
0.715000000000001,0.720000000000001,0.725000000000001,0.730000000000001,
0.735000000000001,0.740000000000001,0.745000000000001,0.750000000000001,
0.755000000000001,0.760000000000001,0.765000000000001,0.770000000000001,
0.775000000000001,0.780000000000001,0.785000000000001,0.790000000000001,
0.795000000000001,0.800000000000001,0.805000000000001,0.810000000000001,
0.815000000000001,0.820000000000001,0.825000000000001,0.830000000000001,
0.835000000000001,0.840000000000001,0.845000000000001,0.850000000000001,
0.855000000000001,0.860000000000001,0.865000000000001,0.870000000000001,
0.875000000000001,0.880000000000001,0.885000000000001,0.890000000000001,
0.895000000000001,0.900000000000001,0.905000000000001,0.910000000000001,
0.915000000000001,0.920000000000001,0.925000000000001,0.930000000000001,
0.935000000000001,0.940000000000001,0.941429844431316),.UNSPECIFIED.)
CURVE()
GEOMETRIC_REPRESENTATION_ITEM()
RATIONAL_B_SPLINE_CURVE((1.,1.,1.,1.,1.,1.,1.,1.,1.,1.,1.,1.,1.,1.,1.,1.,
1.,1.,1.,1.,1.,1.,1.,1.,1.,1.,1.,1.,1.,1.,1.,1.,1.,1.,1.,1.,1.,1.,1.,1.,
1.,1.,1.,1.,1.,1.,1.,1.,1.,1.,1.,1.,1.,1.,1.,1.,1.,1.,1.,1.,1.,1.,1.,1.,
1.,1.,1.,1.,1.,1.,1.,1.,1.,1.,1.,1.,1.,1.,1.,1.,1.,1.,1.,1.,1.,1.,1.,1.,
1.,1.,1.,1.,1.,1.,1.,1.,1.,1.,1.,1.,1.,1.,1.,1.,1.,1.,1.,1.,1.,1.,1.,1.,
1.,1.,1.,1.,1.,1.,1.,1.,1.,1.,1.,1.,1.,1.,1.,1.,1.,1.,1.,1.,1.,1.,1.,1.,
1.,1.,1.,1.,1.,1.,1.,1.,1.,1.,1.,1.,1.,1.,1.,1.,1.,1.,1.,1.,1.,1.,1.,1.,
1.,1.,1.,1.,1.,1.,1.,1.,1.,1.,1.,1.,1.,1.,1.,1.,1.,1.,1.,1.,1.,1.,1.,1.,
1.,1.,1.,1.,1.,1.,1.,1.,1.,1.))
REPRESENTATION_ITEM('')
);
#480=(
BOUNDED_CURVE()
B_SPLINE_CURVE(5,(#87277,#87278,#87279,#87280,#87281,#87282,#87283,#87284,
#87285,#87286,#87287,#87288,#87289,#87290,#87291,#87292,#87293,#87294,#87295,
#87296,#87297,#87298,#87299,#87300,#87301,#87302,#87303,#87304,#87305,#87306,
#87307,#87308,#87309,#87310,#87311,#87312,#87313,#87314,#87315,#87316,#87317,
#87318,#87319,#87320,#87321,#87322,#87323,#87324,#87325,#87326,#87327,#87328,
#87329,#87330,#87331,#87332,#87333,#87334,#87335,#87336,#87337,#87338,#87339,
#87340,#87341,#87342,#87343,#87344,#87345,#87346,#87347,#87348,#87349,#87350,
#87351,#87352,#87353,#87354,#87355,#87356,#87357,#87358,#87359,#87360,#87361,
#87362,#87363,#87364,#87365,#87366,#87367,#87368,#87369,#87370,#87371,#87372,
#87373,#87374,#87375,#87376,#87377,#87378,#87379,#87380,#87381,#87382,#87383,
#87384,#87385,#87386,#87387,#87388,#87389,#87390,#87391,#87392,#87393,#87394,
#87395,#87396,#87397,#87398,#87399,#87400,#87401,#87402,#87403,#87404,#87405,
#87406,#87407,#87408,#87409,#87410,#87411,#87412,#87413,#87414,#87415,#87416,
#87417,#87418,#87419,#87420,#87421,#87422,#87423,#87424,#87425,#87426,#87427,
#87428,#87429,#87430,#87431,#87432,#87433,#87434,#87435,#87436,#87437,#87438,
#87439,#87440,#87441,#87442,#87443,#87444,#87445,#87446,#87447,#87448,#87449,
#87450,#87451,#87452,#87453,#87454,#87455,#87456,#87457,#87458,#87459,#87460,
#87461,#87462,#87463,#87464,#87465,#87466,#87467,#87468,#87469,#87470),
 .UNSPECIFIED.,.F.,.F.)
B_SPLINE_CURVE_WITH_KNOTS((6,1,1,1,1,1,1,1,1,1,1,1,1,1,1,1,1,1,1,1,1,1,
1,1,1,1,1,1,1,1,1,1,1,1,1,1,1,1,1,1,1,1,1,1,1,1,1,1,1,1,1,1,1,1,1,1,1,1,
1,1,1,1,1,1,1,1,1,1,1,1,1,1,1,1,1,1,1,1,1,1,1,1,1,1,1,1,1,1,1,1,1,1,1,1,
1,1,1,1,1,1,1,1,1,1,1,1,1,1,1,1,1,1,1,1,1,1,1,1,1,1,1,1,1,1,1,1,1,1,1,1,
1,1,1,1,1,1,1,1,1,1,1,1,1,1,1,1,1,1,1,1,1,1,1,1,1,1,1,1,1,1,1,1,1,1,1,1,
1,1,1,1,1,1,1,1,1,1,1,1,1,1,1,1,1,1,1,1,1,1,1,6),(-0.941429844431316,-0.940000000000001,
-0.935000000000001,-0.930000000000001,-0.925000000000001,-0.920000000000001,
-0.915000000000001,-0.910000000000001,-0.905000000000001,-0.900000000000001,
-0.895000000000001,-0.890000000000001,-0.885000000000001,-0.880000000000001,
-0.875000000000001,-0.870000000000001,-0.865000000000001,-0.860000000000001,
-0.855000000000001,-0.850000000000001,-0.845000000000001,-0.840000000000001,
-0.835000000000001,-0.830000000000001,-0.825000000000001,-0.820000000000001,
-0.815000000000001,-0.810000000000001,-0.805000000000001,-0.800000000000001,
-0.795000000000001,-0.790000000000001,-0.785000000000001,-0.780000000000001,
-0.775000000000001,-0.770000000000001,-0.765000000000001,-0.760000000000001,
-0.755000000000001,-0.750000000000001,-0.745000000000001,-0.740000000000001,
-0.735000000000001,-0.730000000000001,-0.725000000000001,-0.720000000000001,
-0.715000000000001,-0.710000000000001,-0.705000000000001,-0.700000000000001,
-0.695000000000001,-0.690000000000001,-0.685,-0.68,-0.675,-0.67,-0.665,
-0.66,-0.655,-0.65,-0.645,-0.64,-0.635,-0.63,-0.625,-0.62,-0.615,-0.61,
-0.605,-0.6,-0.595,-0.59,-0.585,-0.58,-0.575,-0.57,-0.565,-0.56,-0.555,
-0.55,-0.545,-0.54,-0.535,-0.53,-0.525,-0.52,-0.515,-0.51,-0.505,-0.5,-0.495,
-0.49,-0.485,-0.48,-0.475,-0.47,-0.465,-0.46,-0.455,-0.45,-0.445,-0.44,
-0.435,-0.43,-0.425,-0.42,-0.415,-0.41,-0.405,-0.4,-0.395,-0.39,-0.385,
-0.38,-0.375,-0.37,-0.365,-0.36,-0.355,-0.35,-0.345,-0.34,-0.335,-0.33,
-0.325,-0.32,-0.315,-0.31,-0.305,-0.3,-0.295,-0.29,-0.285,-0.28,-0.275,
-0.27,-0.265,-0.26,-0.255,-0.25,-0.245,-0.24,-0.235,-0.23,-0.225,-0.22,
-0.215,-0.21,-0.205,-0.2,-0.195,-0.19,-0.185,-0.18,-0.175,-0.17,-0.165,
-0.16,-0.155,-0.15,-0.145,-0.14,-0.135,-0.13,-0.125,-0.12,-0.115,-0.11,
-0.105,-0.1,-0.095,-0.09,-0.085,-0.08,-0.075,-0.07,-0.065,-0.06,-0.055,
-0.05,-0.045,-0.04,-0.035,-0.03,-0.025,-0.02,-0.015,-0.01,-0.005,0.),
 .UNSPECIFIED.)
CURVE()
GEOMETRIC_REPRESENTATION_ITEM()
RATIONAL_B_SPLINE_CURVE((1.,1.,1.,1.,1.,1.,1.,1.,1.,1.,1.,1.,1.,1.,1.,1.,
1.,1.,1.,1.,1.,1.,1.,1.,1.,1.,1.,1.,1.,1.,1.,1.,1.,1.,1.,1.,1.,1.,1.,1.,
1.,1.,1.,1.,1.,1.,1.,1.,1.,1.,1.,1.,1.,1.,1.,1.,1.,1.,1.,1.,1.,1.,1.,1.,
1.,1.,1.,1.,1.,1.,1.,1.,1.,1.,1.,1.,1.,1.,1.,1.,1.,1.,1.,1.,1.,1.,1.,1.,
1.,1.,1.,1.,1.,1.,1.,1.,1.,1.,1.,1.,1.,1.,1.,1.,1.,1.,1.,1.,1.,1.,1.,1.,
1.,1.,1.,1.,1.,1.,1.,1.,1.,1.,1.,1.,1.,1.,1.,1.,1.,1.,1.,1.,1.,1.,1.,1.,
1.,1.,1.,1.,1.,1.,1.,1.,1.,1.,1.,1.,1.,1.,1.,1.,1.,1.,1.,1.,1.,1.,1.,1.,
1.,1.,1.,1.,1.,1.,1.,1.,1.,1.,1.,1.,1.,1.,1.,1.,1.,1.,1.,1.,1.,1.,1.,1.,
1.,1.,1.,1.,1.,1.,1.,1.,1.,1.))
REPRESENTATION_ITEM('')
);
#481=(
BOUNDED_CURVE()
B_SPLINE_CURVE(5,(#87977,#87978,#87979,#87980,#87981,#87982,#87983,#87984,
#87985,#87986,#87987,#87988,#87989,#87990,#87991,#87992,#87993,#87994,#87995,
#87996,#87997,#87998,#87999,#88000,#88001,#88002,#88003,#88004,#88005,#88006,
#88007,#88008,#88009,#88010,#88011,#88012,#88013,#88014,#88015,#88016,#88017,
#88018,#88019,#88020,#88021,#88022,#88023,#88024,#88025,#88026,#88027,#88028,
#88029,#88030,#88031,#88032,#88033,#88034,#88035,#88036,#88037,#88038,#88039,
#88040,#88041,#88042,#88043,#88044,#88045,#88046,#88047,#88048,#88049,#88050,
#88051,#88052,#88053,#88054,#88055,#88056,#88057,#88058,#88059,#88060,#88061,
#88062,#88063,#88064,#88065,#88066,#88067,#88068,#88069,#88070,#88071,#88072,
#88073,#88074,#88075,#88076,#88077,#88078,#88079,#88080,#88081,#88082,#88083,
#88084,#88085,#88086,#88087,#88088,#88089,#88090,#88091,#88092,#88093,#88094,
#88095,#88096,#88097,#88098,#88099,#88100,#88101,#88102,#88103,#88104,#88105,
#88106,#88107,#88108,#88109,#88110,#88111,#88112,#88113,#88114,#88115,#88116,
#88117,#88118,#88119,#88120,#88121,#88122,#88123,#88124,#88125,#88126,#88127,
#88128,#88129,#88130,#88131,#88132,#88133,#88134,#88135,#88136,#88137,#88138,
#88139,#88140,#88141,#88142,#88143,#88144,#88145,#88146,#88147,#88148,#88149,
#88150,#88151,#88152,#88153,#88154,#88155,#88156,#88157,#88158,#88159,#88160,
#88161,#88162,#88163,#88164,#88165,#88166,#88167,#88168,#88169,#88170),
 .UNSPECIFIED.,.F.,.F.)
B_SPLINE_CURVE_WITH_KNOTS((6,1,1,1,1,1,1,1,1,1,1,1,1,1,1,1,1,1,1,1,1,1,
1,1,1,1,1,1,1,1,1,1,1,1,1,1,1,1,1,1,1,1,1,1,1,1,1,1,1,1,1,1,1,1,1,1,1,1,
1,1,1,1,1,1,1,1,1,1,1,1,1,1,1,1,1,1,1,1,1,1,1,1,1,1,1,1,1,1,1,1,1,1,1,1,
1,1,1,1,1,1,1,1,1,1,1,1,1,1,1,1,1,1,1,1,1,1,1,1,1,1,1,1,1,1,1,1,1,1,1,1,
1,1,1,1,1,1,1,1,1,1,1,1,1,1,1,1,1,1,1,1,1,1,1,1,1,1,1,1,1,1,1,1,1,1,1,1,
1,1,1,1,1,1,1,1,1,1,1,1,1,1,1,1,1,1,1,1,1,1,1,6),(0.,0.005,0.01,0.015,0.02,
0.025,0.03,0.035,0.04,0.045,0.05,0.055,0.06,0.065,0.07,0.075,0.08,0.085,
0.09,0.095,0.1,0.105,0.11,0.115,0.12,0.125,0.13,0.135,0.14,0.145,0.15,0.155,
0.16,0.165,0.17,0.175,0.18,0.185,0.19,0.195,0.2,0.205,0.21,0.215,0.22,0.225,
0.23,0.235,0.24,0.245,0.25,0.255,0.26,0.265,0.27,0.275,0.28,0.285,0.29,
0.295,0.3,0.305,0.31,0.315,0.32,0.325,0.33,0.335,0.34,0.345,0.35,0.355,
0.36,0.365,0.37,0.375,0.38,0.385,0.39,0.395,0.4,0.405,0.41,0.415,0.42,0.425,
0.43,0.435,0.44,0.445,0.45,0.455,0.46,0.465,0.47,0.475,0.48,0.485,0.49,
0.495,0.5,0.505,0.51,0.515,0.52,0.525,0.53,0.535,0.54,0.545,0.55,0.555,
0.56,0.565,0.57,0.575,0.58,0.585,0.59,0.595,0.6,0.605,0.61,0.615,0.62,0.625,
0.63,0.635,0.64,0.645,0.65,0.655,0.66,0.665,0.67,0.675,0.68,0.685,0.690000000000001,
0.695000000000001,0.700000000000001,0.705000000000001,0.710000000000001,
0.715000000000001,0.720000000000001,0.725000000000001,0.730000000000001,
0.735000000000001,0.740000000000001,0.745000000000001,0.750000000000001,
0.755000000000001,0.760000000000001,0.765000000000001,0.770000000000001,
0.775000000000001,0.780000000000001,0.785000000000001,0.790000000000001,
0.795000000000001,0.800000000000001,0.805000000000001,0.810000000000001,
0.815000000000001,0.820000000000001,0.825000000000001,0.830000000000001,
0.835000000000001,0.840000000000001,0.845000000000001,0.850000000000001,
0.855000000000001,0.860000000000001,0.865000000000001,0.870000000000001,
0.875000000000001,0.880000000000001,0.885000000000001,0.890000000000001,
0.895000000000001,0.900000000000001,0.905000000000001,0.910000000000001,
0.915000000000001,0.920000000000001,0.925000000000001,0.930000000000001,
0.935000000000001,0.940000000000001,0.941429844431396),.UNSPECIFIED.)
CURVE()
GEOMETRIC_REPRESENTATION_ITEM()
RATIONAL_B_SPLINE_CURVE((1.,1.,1.,1.,1.,1.,1.,1.,1.,1.,1.,1.,1.,1.,1.,1.,
1.,1.,1.,1.,1.,1.,1.,1.,1.,1.,1.,1.,1.,1.,1.,1.,1.,1.,1.,1.,1.,1.,1.,1.,
1.,1.,1.,1.,1.,1.,1.,1.,1.,1.,1.,1.,1.,1.,1.,1.,1.,1.,1.,1.,1.,1.,1.,1.,
1.,1.,1.,1.,1.,1.,1.,1.,1.,1.,1.,1.,1.,1.,1.,1.,1.,1.,1.,1.,1.,1.,1.,1.,
1.,1.,1.,1.,1.,1.,1.,1.,1.,1.,1.,1.,1.,1.,1.,1.,1.,1.,1.,1.,1.,1.,1.,1.,
1.,1.,1.,1.,1.,1.,1.,1.,1.,1.,1.,1.,1.,1.,1.,1.,1.,1.,1.,1.,1.,1.,1.,1.,
1.,1.,1.,1.,1.,1.,1.,1.,1.,1.,1.,1.,1.,1.,1.,1.,1.,1.,1.,1.,1.,1.,1.,1.,
1.,1.,1.,1.,1.,1.,1.,1.,1.,1.,1.,1.,1.,1.,1.,1.,1.,1.,1.,1.,1.,1.,1.,1.,
1.,1.,1.,1.,1.,1.,1.,1.,1.,1.))
REPRESENTATION_ITEM('')
);
#482=(
BOUNDED_CURVE()
B_SPLINE_CURVE(5,(#88173,#88174,#88175,#88176,#88177,#88178,#88179,#88180,
#88181,#88182,#88183,#88184,#88185,#88186,#88187,#88188,#88189,#88190,#88191,
#88192,#88193,#88194,#88195,#88196,#88197,#88198,#88199,#88200,#88201,#88202,
#88203,#88204,#88205,#88206,#88207,#88208,#88209,#88210,#88211,#88212,#88213,
#88214,#88215,#88216,#88217,#88218,#88219,#88220,#88221,#88222,#88223,#88224,
#88225,#88226,#88227,#88228,#88229,#88230,#88231,#88232,#88233,#88234,#88235,
#88236,#88237,#88238,#88239,#88240,#88241,#88242,#88243,#88244,#88245,#88246,
#88247,#88248,#88249,#88250,#88251,#88252,#88253,#88254,#88255,#88256,#88257,
#88258,#88259,#88260,#88261,#88262,#88263,#88264,#88265,#88266,#88267,#88268,
#88269,#88270,#88271,#88272,#88273,#88274,#88275,#88276,#88277,#88278,#88279,
#88280,#88281,#88282,#88283,#88284,#88285,#88286,#88287,#88288,#88289,#88290,
#88291,#88292,#88293,#88294,#88295,#88296,#88297,#88298,#88299,#88300,#88301,
#88302,#88303,#88304,#88305,#88306,#88307,#88308,#88309,#88310,#88311,#88312,
#88313,#88314,#88315,#88316,#88317,#88318,#88319,#88320,#88321,#88322,#88323,
#88324,#88325,#88326,#88327,#88328,#88329,#88330,#88331,#88332,#88333,#88334,
#88335,#88336,#88337,#88338,#88339,#88340,#88341,#88342,#88343,#88344,#88345,
#88346,#88347,#88348,#88349,#88350,#88351,#88352,#88353,#88354,#88355,#88356,
#88357,#88358,#88359,#88360,#88361,#88362,#88363,#88364,#88365,#88366),
 .UNSPECIFIED.,.F.,.F.)
B_SPLINE_CURVE_WITH_KNOTS((6,1,1,1,1,1,1,1,1,1,1,1,1,1,1,1,1,1,1,1,1,1,
1,1,1,1,1,1,1,1,1,1,1,1,1,1,1,1,1,1,1,1,1,1,1,1,1,1,1,1,1,1,1,1,1,1,1,1,
1,1,1,1,1,1,1,1,1,1,1,1,1,1,1,1,1,1,1,1,1,1,1,1,1,1,1,1,1,1,1,1,1,1,1,1,
1,1,1,1,1,1,1,1,1,1,1,1,1,1,1,1,1,1,1,1,1,1,1,1,1,1,1,1,1,1,1,1,1,1,1,1,
1,1,1,1,1,1,1,1,1,1,1,1,1,1,1,1,1,1,1,1,1,1,1,1,1,1,1,1,1,1,1,1,1,1,1,1,
1,1,1,1,1,1,1,1,1,1,1,1,1,1,1,1,1,1,1,1,1,1,1,6),(-0.941429844431407,-0.940000000000001,
-0.935000000000001,-0.930000000000001,-0.925000000000001,-0.920000000000001,
-0.915000000000001,-0.910000000000001,-0.905000000000001,-0.900000000000001,
-0.895000000000001,-0.890000000000001,-0.885000000000001,-0.880000000000001,
-0.875000000000001,-0.870000000000001,-0.865000000000001,-0.860000000000001,
-0.855000000000001,-0.850000000000001,-0.845000000000001,-0.840000000000001,
-0.835000000000001,-0.830000000000001,-0.825000000000001,-0.820000000000001,
-0.815000000000001,-0.810000000000001,-0.805000000000001,-0.800000000000001,
-0.795000000000001,-0.790000000000001,-0.785000000000001,-0.780000000000001,
-0.775000000000001,-0.770000000000001,-0.765000000000001,-0.760000000000001,
-0.755000000000001,-0.750000000000001,-0.745000000000001,-0.740000000000001,
-0.735000000000001,-0.730000000000001,-0.725000000000001,-0.720000000000001,
-0.715000000000001,-0.710000000000001,-0.705000000000001,-0.700000000000001,
-0.695000000000001,-0.690000000000001,-0.685,-0.68,-0.675,-0.67,-0.665,
-0.66,-0.655,-0.65,-0.645,-0.64,-0.635,-0.63,-0.625,-0.62,-0.615,-0.61,
-0.605,-0.6,-0.595,-0.59,-0.585,-0.58,-0.575,-0.57,-0.565,-0.56,-0.555,
-0.55,-0.545,-0.54,-0.535,-0.53,-0.525,-0.52,-0.515,-0.51,-0.505,-0.5,-0.495,
-0.49,-0.485,-0.48,-0.475,-0.47,-0.465,-0.46,-0.455,-0.45,-0.445,-0.44,
-0.435,-0.43,-0.425,-0.42,-0.415,-0.41,-0.405,-0.4,-0.395,-0.39,-0.385,
-0.38,-0.375,-0.37,-0.365,-0.36,-0.355,-0.35,-0.345,-0.34,-0.335,-0.33,
-0.325,-0.32,-0.315,-0.31,-0.305,-0.3,-0.295,-0.29,-0.285,-0.28,-0.275,
-0.27,-0.265,-0.26,-0.255,-0.25,-0.245,-0.24,-0.235,-0.23,-0.225,-0.22,
-0.215,-0.21,-0.205,-0.2,-0.195,-0.19,-0.185,-0.18,-0.175,-0.17,-0.165,
-0.16,-0.155,-0.15,-0.145,-0.14,-0.135,-0.13,-0.125,-0.12,-0.115,-0.11,
-0.105,-0.1,-0.095,-0.09,-0.085,-0.08,-0.075,-0.07,-0.065,-0.06,-0.055,
-0.05,-0.045,-0.04,-0.035,-0.03,-0.025,-0.02,-0.015,-0.01,-0.005,0.),
 .UNSPECIFIED.)
CURVE()
GEOMETRIC_REPRESENTATION_ITEM()
RATIONAL_B_SPLINE_CURVE((1.,1.,1.,1.,1.,1.,1.,1.,1.,1.,1.,1.,1.,1.,1.,1.,
1.,1.,1.,1.,1.,1.,1.,1.,1.,1.,1.,1.,1.,1.,1.,1.,1.,1.,1.,1.,1.,1.,1.,1.,
1.,1.,1.,1.,1.,1.,1.,1.,1.,1.,1.,1.,1.,1.,1.,1.,1.,1.,1.,1.,1.,1.,1.,1.,
1.,1.,1.,1.,1.,1.,1.,1.,1.,1.,1.,1.,1.,1.,1.,1.,1.,1.,1.,1.,1.,1.,1.,1.,
1.,1.,1.,1.,1.,1.,1.,1.,1.,1.,1.,1.,1.,1.,1.,1.,1.,1.,1.,1.,1.,1.,1.,1.,
1.,1.,1.,1.,1.,1.,1.,1.,1.,1.,1.,1.,1.,1.,1.,1.,1.,1.,1.,1.,1.,1.,1.,1.,
1.,1.,1.,1.,1.,1.,1.,1.,1.,1.,1.,1.,1.,1.,1.,1.,1.,1.,1.,1.,1.,1.,1.,1.,
1.,1.,1.,1.,1.,1.,1.,1.,1.,1.,1.,1.,1.,1.,1.,1.,1.,1.,1.,1.,1.,1.,1.,1.,
1.,1.,1.,1.,1.,1.,1.,1.,1.,1.))
REPRESENTATION_ITEM('')
);
#483=(
BOUNDED_CURVE()
B_SPLINE_CURVE(5,(#88873,#88874,#88875,#88876,#88877,#88878,#88879,#88880,
#88881,#88882,#88883,#88884,#88885,#88886,#88887,#88888,#88889,#88890,#88891,
#88892,#88893,#88894,#88895,#88896,#88897,#88898,#88899,#88900,#88901,#88902,
#88903,#88904,#88905,#88906,#88907,#88908,#88909,#88910,#88911,#88912,#88913,
#88914,#88915,#88916,#88917,#88918,#88919,#88920,#88921,#88922,#88923,#88924,
#88925,#88926,#88927,#88928,#88929,#88930,#88931,#88932,#88933,#88934,#88935,
#88936,#88937,#88938,#88939,#88940,#88941,#88942,#88943,#88944,#88945,#88946,
#88947,#88948,#88949,#88950,#88951,#88952,#88953,#88954,#88955,#88956,#88957,
#88958,#88959,#88960,#88961,#88962,#88963,#88964,#88965,#88966,#88967,#88968,
#88969,#88970,#88971,#88972,#88973,#88974,#88975,#88976,#88977,#88978,#88979,
#88980,#88981,#88982,#88983,#88984,#88985,#88986,#88987,#88988,#88989,#88990,
#88991,#88992,#88993,#88994,#88995,#88996,#88997,#88998,#88999,#89000,#89001,
#89002,#89003,#89004,#89005,#89006,#89007,#89008,#89009,#89010,#89011,#89012,
#89013,#89014,#89015,#89016,#89017,#89018,#89019,#89020,#89021,#89022,#89023,
#89024,#89025,#89026,#89027,#89028,#89029,#89030,#89031,#89032,#89033,#89034,
#89035,#89036,#89037,#89038,#89039,#89040,#89041,#89042,#89043,#89044,#89045,
#89046,#89047,#89048,#89049,#89050,#89051,#89052,#89053,#89054,#89055,#89056,
#89057,#89058,#89059,#89060,#89061,#89062,#89063,#89064,#89065,#89066),
 .UNSPECIFIED.,.F.,.F.)
B_SPLINE_CURVE_WITH_KNOTS((6,1,1,1,1,1,1,1,1,1,1,1,1,1,1,1,1,1,1,1,1,1,
1,1,1,1,1,1,1,1,1,1,1,1,1,1,1,1,1,1,1,1,1,1,1,1,1,1,1,1,1,1,1,1,1,1,1,1,
1,1,1,1,1,1,1,1,1,1,1,1,1,1,1,1,1,1,1,1,1,1,1,1,1,1,1,1,1,1,1,1,1,1,1,1,
1,1,1,1,1,1,1,1,1,1,1,1,1,1,1,1,1,1,1,1,1,1,1,1,1,1,1,1,1,1,1,1,1,1,1,1,
1,1,1,1,1,1,1,1,1,1,1,1,1,1,1,1,1,1,1,1,1,1,1,1,1,1,1,1,1,1,1,1,1,1,1,1,
1,1,1,1,1,1,1,1,1,1,1,1,1,1,1,1,1,1,1,1,1,1,1,6),(0.,0.005,0.01,0.015,0.02,
0.025,0.03,0.035,0.04,0.045,0.05,0.055,0.06,0.065,0.07,0.075,0.08,0.085,
0.09,0.095,0.1,0.105,0.11,0.115,0.12,0.125,0.13,0.135,0.14,0.145,0.15,0.155,
0.16,0.165,0.17,0.175,0.18,0.185,0.19,0.195,0.2,0.205,0.21,0.215,0.22,0.225,
0.23,0.235,0.24,0.245,0.25,0.255,0.26,0.265,0.27,0.275,0.28,0.285,0.29,
0.295,0.3,0.305,0.31,0.315,0.32,0.325,0.33,0.335,0.34,0.345,0.35,0.355,
0.36,0.365,0.37,0.375,0.38,0.385,0.39,0.395,0.4,0.405,0.41,0.415,0.42,0.425,
0.43,0.435,0.44,0.445,0.45,0.455,0.46,0.465,0.47,0.475,0.48,0.485,0.49,
0.495,0.5,0.505,0.51,0.515,0.52,0.525,0.53,0.535,0.54,0.545,0.55,0.555,
0.56,0.565,0.57,0.575,0.58,0.585,0.59,0.595,0.6,0.605,0.61,0.615,0.62,0.625,
0.63,0.635,0.64,0.645,0.65,0.655,0.66,0.665,0.67,0.675,0.68,0.685,0.690000000000001,
0.695000000000001,0.700000000000001,0.705000000000001,0.710000000000001,
0.715000000000001,0.720000000000001,0.725000000000001,0.730000000000001,
0.735000000000001,0.740000000000001,0.745000000000001,0.750000000000001,
0.755000000000001,0.760000000000001,0.765000000000001,0.770000000000001,
0.775000000000001,0.780000000000001,0.785000000000001,0.790000000000001,
0.795000000000001,0.800000000000001,0.805000000000001,0.810000000000001,
0.815000000000001,0.820000000000001,0.825000000000001,0.830000000000001,
0.835000000000001,0.840000000000001,0.845000000000001,0.850000000000001,
0.855000000000001,0.860000000000001,0.865000000000001,0.870000000000001,
0.875000000000001,0.880000000000001,0.885000000000001,0.890000000000001,
0.895000000000001,0.900000000000001,0.905000000000001,0.910000000000001,
0.915000000000001,0.920000000000001,0.925000000000001,0.930000000000001,
0.935000000000001,0.940000000000001,0.941429844431366),.UNSPECIFIED.)
CURVE()
GEOMETRIC_REPRESENTATION_ITEM()
RATIONAL_B_SPLINE_CURVE((1.,1.,1.,1.,1.,1.,1.,1.,1.,1.,1.,1.,1.,1.,1.,1.,
1.,1.,1.,1.,1.,1.,1.,1.,1.,1.,1.,1.,1.,1.,1.,1.,1.,1.,1.,1.,1.,1.,1.,1.,
1.,1.,1.,1.,1.,1.,1.,1.,1.,1.,1.,1.,1.,1.,1.,1.,1.,1.,1.,1.,1.,1.,1.,1.,
1.,1.,1.,1.,1.,1.,1.,1.,1.,1.,1.,1.,1.,1.,1.,1.,1.,1.,1.,1.,1.,1.,1.,1.,
1.,1.,1.,1.,1.,1.,1.,1.,1.,1.,1.,1.,1.,1.,1.,1.,1.,1.,1.,1.,1.,1.,1.,1.,
1.,1.,1.,1.,1.,1.,1.,1.,1.,1.,1.,1.,1.,1.,1.,1.,1.,1.,1.,1.,1.,1.,1.,1.,
1.,1.,1.,1.,1.,1.,1.,1.,1.,1.,1.,1.,1.,1.,1.,1.,1.,1.,1.,1.,1.,1.,1.,1.,
1.,1.,1.,1.,1.,1.,1.,1.,1.,1.,1.,1.,1.,1.,1.,1.,1.,1.,1.,1.,1.,1.,1.,1.,
1.,1.,1.,1.,1.,1.,1.,1.,1.,1.))
REPRESENTATION_ITEM('')
);
#484=(
BOUNDED_CURVE()
B_SPLINE_CURVE(5,(#89069,#89070,#89071,#89072,#89073,#89074,#89075,#89076,
#89077,#89078,#89079,#89080,#89081,#89082,#89083,#89084,#89085,#89086,#89087,
#89088,#89089,#89090,#89091,#89092,#89093,#89094,#89095,#89096,#89097,#89098,
#89099,#89100,#89101,#89102,#89103,#89104,#89105,#89106,#89107,#89108,#89109,
#89110,#89111,#89112,#89113,#89114,#89115,#89116,#89117,#89118,#89119,#89120,
#89121,#89122,#89123,#89124,#89125,#89126,#89127,#89128,#89129,#89130,#89131,
#89132,#89133,#89134,#89135,#89136,#89137,#89138,#89139,#89140,#89141,#89142,
#89143,#89144,#89145,#89146,#89147,#89148,#89149,#89150,#89151,#89152,#89153,
#89154,#89155,#89156,#89157,#89158,#89159,#89160,#89161,#89162,#89163,#89164,
#89165,#89166,#89167,#89168,#89169,#89170,#89171,#89172,#89173,#89174,#89175,
#89176,#89177,#89178,#89179,#89180,#89181,#89182,#89183,#89184,#89185,#89186,
#89187,#89188,#89189,#89190,#89191,#89192,#89193,#89194,#89195,#89196,#89197,
#89198,#89199,#89200,#89201,#89202,#89203,#89204,#89205,#89206,#89207,#89208,
#89209,#89210,#89211,#89212,#89213,#89214,#89215,#89216,#89217,#89218,#89219,
#89220,#89221,#89222,#89223,#89224,#89225,#89226,#89227,#89228,#89229,#89230,
#89231,#89232,#89233,#89234,#89235,#89236,#89237,#89238,#89239,#89240,#89241,
#89242,#89243,#89244,#89245,#89246,#89247,#89248,#89249,#89250,#89251,#89252,
#89253,#89254,#89255,#89256,#89257,#89258,#89259,#89260,#89261,#89262),
 .UNSPECIFIED.,.F.,.F.)
B_SPLINE_CURVE_WITH_KNOTS((6,1,1,1,1,1,1,1,1,1,1,1,1,1,1,1,1,1,1,1,1,1,
1,1,1,1,1,1,1,1,1,1,1,1,1,1,1,1,1,1,1,1,1,1,1,1,1,1,1,1,1,1,1,1,1,1,1,1,
1,1,1,1,1,1,1,1,1,1,1,1,1,1,1,1,1,1,1,1,1,1,1,1,1,1,1,1,1,1,1,1,1,1,1,1,
1,1,1,1,1,1,1,1,1,1,1,1,1,1,1,1,1,1,1,1,1,1,1,1,1,1,1,1,1,1,1,1,1,1,1,1,
1,1,1,1,1,1,1,1,1,1,1,1,1,1,1,1,1,1,1,1,1,1,1,1,1,1,1,1,1,1,1,1,1,1,1,1,
1,1,1,1,1,1,1,1,1,1,1,1,1,1,1,1,1,1,1,1,1,1,1,6),(-0.941429844431363,-0.940000000000001,
-0.935000000000001,-0.930000000000001,-0.925000000000001,-0.920000000000001,
-0.915000000000001,-0.910000000000001,-0.905000000000001,-0.900000000000001,
-0.895000000000001,-0.890000000000001,-0.885000000000001,-0.880000000000001,
-0.875000000000001,-0.870000000000001,-0.865000000000001,-0.860000000000001,
-0.855000000000001,-0.850000000000001,-0.845000000000001,-0.840000000000001,
-0.835000000000001,-0.830000000000001,-0.825000000000001,-0.820000000000001,
-0.815000000000001,-0.810000000000001,-0.805000000000001,-0.800000000000001,
-0.795000000000001,-0.790000000000001,-0.785000000000001,-0.780000000000001,
-0.775000000000001,-0.770000000000001,-0.765000000000001,-0.760000000000001,
-0.755000000000001,-0.750000000000001,-0.745000000000001,-0.740000000000001,
-0.735000000000001,-0.730000000000001,-0.725000000000001,-0.720000000000001,
-0.715000000000001,-0.710000000000001,-0.705000000000001,-0.700000000000001,
-0.695000000000001,-0.690000000000001,-0.685,-0.68,-0.675,-0.67,-0.665,
-0.66,-0.655,-0.65,-0.645,-0.64,-0.635,-0.63,-0.625,-0.62,-0.615,-0.61,
-0.605,-0.6,-0.595,-0.59,-0.585,-0.58,-0.575,-0.57,-0.565,-0.56,-0.555,
-0.55,-0.545,-0.54,-0.535,-0.53,-0.525,-0.52,-0.515,-0.51,-0.505,-0.5,-0.495,
-0.49,-0.485,-0.48,-0.475,-0.47,-0.465,-0.46,-0.455,-0.45,-0.445,-0.44,
-0.435,-0.43,-0.425,-0.42,-0.415,-0.41,-0.405,-0.4,-0.395,-0.39,-0.385,
-0.38,-0.375,-0.37,-0.365,-0.36,-0.355,-0.35,-0.345,-0.34,-0.335,-0.33,
-0.325,-0.32,-0.315,-0.31,-0.305,-0.3,-0.295,-0.29,-0.285,-0.28,-0.275,
-0.27,-0.265,-0.26,-0.255,-0.25,-0.245,-0.24,-0.235,-0.23,-0.225,-0.22,
-0.215,-0.21,-0.205,-0.2,-0.195,-0.19,-0.185,-0.18,-0.175,-0.17,-0.165,
-0.16,-0.155,-0.15,-0.145,-0.14,-0.135,-0.13,-0.125,-0.12,-0.115,-0.11,
-0.105,-0.1,-0.095,-0.09,-0.085,-0.08,-0.075,-0.07,-0.065,-0.06,-0.055,
-0.05,-0.045,-0.04,-0.035,-0.03,-0.025,-0.02,-0.015,-0.01,-0.005,0.),
 .UNSPECIFIED.)
CURVE()
GEOMETRIC_REPRESENTATION_ITEM()
RATIONAL_B_SPLINE_CURVE((1.,1.,1.,1.,1.,1.,1.,1.,1.,1.,1.,1.,1.,1.,1.,1.,
1.,1.,1.,1.,1.,1.,1.,1.,1.,1.,1.,1.,1.,1.,1.,1.,1.,1.,1.,1.,1.,1.,1.,1.,
1.,1.,1.,1.,1.,1.,1.,1.,1.,1.,1.,1.,1.,1.,1.,1.,1.,1.,1.,1.,1.,1.,1.,1.,
1.,1.,1.,1.,1.,1.,1.,1.,1.,1.,1.,1.,1.,1.,1.,1.,1.,1.,1.,1.,1.,1.,1.,1.,
1.,1.,1.,1.,1.,1.,1.,1.,1.,1.,1.,1.,1.,1.,1.,1.,1.,1.,1.,1.,1.,1.,1.,1.,
1.,1.,1.,1.,1.,1.,1.,1.,1.,1.,1.,1.,1.,1.,1.,1.,1.,1.,1.,1.,1.,1.,1.,1.,
1.,1.,1.,1.,1.,1.,1.,1.,1.,1.,1.,1.,1.,1.,1.,1.,1.,1.,1.,1.,1.,1.,1.,1.,
1.,1.,1.,1.,1.,1.,1.,1.,1.,1.,1.,1.,1.,1.,1.,1.,1.,1.,1.,1.,1.,1.,1.,1.,
1.,1.,1.,1.,1.,1.,1.,1.,1.,1.))
REPRESENTATION_ITEM('')
);
#485=(
BOUNDED_CURVE()
B_SPLINE_CURVE(5,(#89769,#89770,#89771,#89772,#89773,#89774,#89775,#89776,
#89777,#89778,#89779,#89780,#89781,#89782,#89783,#89784,#89785,#89786,#89787,
#89788,#89789,#89790,#89791,#89792,#89793,#89794,#89795,#89796,#89797,#89798,
#89799,#89800,#89801,#89802,#89803,#89804,#89805,#89806,#89807,#89808,#89809,
#89810,#89811,#89812,#89813,#89814,#89815,#89816,#89817,#89818,#89819,#89820,
#89821,#89822,#89823,#89824,#89825,#89826,#89827,#89828,#89829,#89830,#89831,
#89832,#89833,#89834,#89835,#89836,#89837,#89838,#89839,#89840,#89841,#89842,
#89843,#89844,#89845,#89846,#89847,#89848,#89849,#89850,#89851,#89852,#89853,
#89854,#89855,#89856,#89857,#89858,#89859,#89860,#89861,#89862,#89863,#89864,
#89865,#89866,#89867,#89868,#89869,#89870,#89871,#89872,#89873,#89874,#89875,
#89876,#89877,#89878,#89879,#89880,#89881,#89882,#89883,#89884,#89885,#89886,
#89887,#89888,#89889,#89890,#89891,#89892,#89893,#89894,#89895,#89896,#89897,
#89898,#89899,#89900,#89901,#89902,#89903,#89904,#89905,#89906,#89907,#89908,
#89909,#89910,#89911,#89912,#89913,#89914,#89915,#89916,#89917,#89918,#89919,
#89920,#89921,#89922,#89923,#89924,#89925,#89926,#89927,#89928,#89929,#89930,
#89931,#89932,#89933,#89934,#89935,#89936,#89937,#89938,#89939,#89940,#89941,
#89942,#89943,#89944,#89945,#89946,#89947,#89948,#89949,#89950,#89951,#89952,
#89953,#89954,#89955,#89956,#89957,#89958,#89959,#89960,#89961,#89962),
 .UNSPECIFIED.,.F.,.F.)
B_SPLINE_CURVE_WITH_KNOTS((6,1,1,1,1,1,1,1,1,1,1,1,1,1,1,1,1,1,1,1,1,1,
1,1,1,1,1,1,1,1,1,1,1,1,1,1,1,1,1,1,1,1,1,1,1,1,1,1,1,1,1,1,1,1,1,1,1,1,
1,1,1,1,1,1,1,1,1,1,1,1,1,1,1,1,1,1,1,1,1,1,1,1,1,1,1,1,1,1,1,1,1,1,1,1,
1,1,1,1,1,1,1,1,1,1,1,1,1,1,1,1,1,1,1,1,1,1,1,1,1,1,1,1,1,1,1,1,1,1,1,1,
1,1,1,1,1,1,1,1,1,1,1,1,1,1,1,1,1,1,1,1,1,1,1,1,1,1,1,1,1,1,1,1,1,1,1,1,
1,1,1,1,1,1,1,1,1,1,1,1,1,1,1,1,1,1,1,1,1,1,1,6),(0.,0.005,0.01,0.015,0.02,
0.025,0.03,0.035,0.04,0.045,0.05,0.055,0.06,0.065,0.07,0.075,0.08,0.085,
0.09,0.095,0.1,0.105,0.11,0.115,0.12,0.125,0.13,0.135,0.14,0.145,0.15,0.155,
0.16,0.165,0.17,0.175,0.18,0.185,0.19,0.195,0.2,0.205,0.21,0.215,0.22,0.225,
0.23,0.235,0.24,0.245,0.25,0.255,0.26,0.265,0.27,0.275,0.28,0.285,0.29,
0.295,0.3,0.305,0.31,0.315,0.32,0.325,0.33,0.335,0.34,0.345,0.35,0.355,
0.36,0.365,0.37,0.375,0.38,0.385,0.39,0.395,0.4,0.405,0.41,0.415,0.42,0.425,
0.43,0.435,0.44,0.445,0.45,0.455,0.46,0.465,0.47,0.475,0.48,0.485,0.49,
0.495,0.5,0.505,0.51,0.515,0.52,0.525,0.53,0.535,0.54,0.545,0.55,0.555,
0.56,0.565,0.57,0.575,0.58,0.585,0.59,0.595,0.6,0.605,0.61,0.615,0.62,0.625,
0.63,0.635,0.64,0.645,0.65,0.655,0.66,0.665,0.67,0.675,0.68,0.685,0.690000000000001,
0.695000000000001,0.700000000000001,0.705000000000001,0.710000000000001,
0.715000000000001,0.720000000000001,0.725000000000001,0.730000000000001,
0.735000000000001,0.740000000000001,0.745000000000001,0.750000000000001,
0.755000000000001,0.760000000000001,0.765000000000001,0.770000000000001,
0.775000000000001,0.780000000000001,0.785000000000001,0.790000000000001,
0.795000000000001,0.800000000000001,0.805000000000001,0.810000000000001,
0.815000000000001,0.820000000000001,0.825000000000001,0.830000000000001,
0.835000000000001,0.840000000000001,0.845000000000001,0.850000000000001,
0.855000000000001,0.860000000000001,0.865000000000001,0.870000000000001,
0.875000000000001,0.880000000000001,0.885000000000001,0.890000000000001,
0.895000000000001,0.900000000000001,0.905000000000001,0.910000000000001,
0.915000000000001,0.920000000000001,0.925000000000001,0.930000000000001,
0.935000000000001,0.940000000000001,0.941429844431418),.UNSPECIFIED.)
CURVE()
GEOMETRIC_REPRESENTATION_ITEM()
RATIONAL_B_SPLINE_CURVE((1.,1.,1.,1.,1.,1.,1.,1.,1.,1.,1.,1.,1.,1.,1.,1.,
1.,1.,1.,1.,1.,1.,1.,1.,1.,1.,1.,1.,1.,1.,1.,1.,1.,1.,1.,1.,1.,1.,1.,1.,
1.,1.,1.,1.,1.,1.,1.,1.,1.,1.,1.,1.,1.,1.,1.,1.,1.,1.,1.,1.,1.,1.,1.,1.,
1.,1.,1.,1.,1.,1.,1.,1.,1.,1.,1.,1.,1.,1.,1.,1.,1.,1.,1.,1.,1.,1.,1.,1.,
1.,1.,1.,1.,1.,1.,1.,1.,1.,1.,1.,1.,1.,1.,1.,1.,1.,1.,1.,1.,1.,1.,1.,1.,
1.,1.,1.,1.,1.,1.,1.,1.,1.,1.,1.,1.,1.,1.,1.,1.,1.,1.,1.,1.,1.,1.,1.,1.,
1.,1.,1.,1.,1.,1.,1.,1.,1.,1.,1.,1.,1.,1.,1.,1.,1.,1.,1.,1.,1.,1.,1.,1.,
1.,1.,1.,1.,1.,1.,1.,1.,1.,1.,1.,1.,1.,1.,1.,1.,1.,1.,1.,1.,1.,1.,1.,1.,
1.,1.,1.,1.,1.,1.,1.,1.,1.,1.))
REPRESENTATION_ITEM('')
);
#486=(
BOUNDED_CURVE()
B_SPLINE_CURVE(5,(#89965,#89966,#89967,#89968,#89969,#89970,#89971,#89972,
#89973,#89974,#89975,#89976,#89977,#89978,#89979,#89980,#89981,#89982,#89983,
#89984,#89985,#89986,#89987,#89988,#89989,#89990,#89991,#89992,#89993,#89994,
#89995,#89996,#89997,#89998,#89999,#90000,#90001,#90002,#90003,#90004,#90005,
#90006,#90007,#90008,#90009,#90010,#90011,#90012,#90013,#90014,#90015,#90016,
#90017,#90018,#90019,#90020,#90021,#90022,#90023,#90024,#90025,#90026,#90027,
#90028,#90029,#90030,#90031,#90032,#90033,#90034,#90035,#90036,#90037,#90038,
#90039,#90040,#90041,#90042,#90043,#90044,#90045,#90046,#90047,#90048,#90049,
#90050,#90051,#90052,#90053,#90054,#90055,#90056,#90057,#90058,#90059,#90060,
#90061,#90062,#90063,#90064,#90065,#90066,#90067,#90068,#90069,#90070,#90071,
#90072,#90073,#90074,#90075,#90076,#90077,#90078,#90079,#90080,#90081,#90082,
#90083,#90084,#90085,#90086,#90087,#90088,#90089,#90090,#90091,#90092,#90093,
#90094,#90095,#90096,#90097,#90098,#90099,#90100,#90101,#90102,#90103,#90104,
#90105,#90106,#90107,#90108,#90109,#90110,#90111,#90112,#90113,#90114,#90115,
#90116,#90117,#90118,#90119,#90120,#90121,#90122,#90123,#90124,#90125,#90126,
#90127,#90128,#90129,#90130,#90131,#90132,#90133,#90134,#90135,#90136,#90137,
#90138,#90139,#90140,#90141,#90142,#90143,#90144,#90145,#90146,#90147,#90148,
#90149,#90150,#90151,#90152,#90153,#90154,#90155,#90156,#90157,#90158),
 .UNSPECIFIED.,.F.,.F.)
B_SPLINE_CURVE_WITH_KNOTS((6,1,1,1,1,1,1,1,1,1,1,1,1,1,1,1,1,1,1,1,1,1,
1,1,1,1,1,1,1,1,1,1,1,1,1,1,1,1,1,1,1,1,1,1,1,1,1,1,1,1,1,1,1,1,1,1,1,1,
1,1,1,1,1,1,1,1,1,1,1,1,1,1,1,1,1,1,1,1,1,1,1,1,1,1,1,1,1,1,1,1,1,1,1,1,
1,1,1,1,1,1,1,1,1,1,1,1,1,1,1,1,1,1,1,1,1,1,1,1,1,1,1,1,1,1,1,1,1,1,1,1,
1,1,1,1,1,1,1,1,1,1,1,1,1,1,1,1,1,1,1,1,1,1,1,1,1,1,1,1,1,1,1,1,1,1,1,1,
1,1,1,1,1,1,1,1,1,1,1,1,1,1,1,1,1,1,1,1,1,1,1,6),(-0.941429844431415,-0.940000000000001,
-0.935000000000001,-0.930000000000001,-0.925000000000001,-0.920000000000001,
-0.915000000000001,-0.910000000000001,-0.905000000000001,-0.900000000000001,
-0.895000000000001,-0.890000000000001,-0.885000000000001,-0.880000000000001,
-0.875000000000001,-0.870000000000001,-0.865000000000001,-0.860000000000001,
-0.855000000000001,-0.850000000000001,-0.845000000000001,-0.840000000000001,
-0.835000000000001,-0.830000000000001,-0.825000000000001,-0.820000000000001,
-0.815000000000001,-0.810000000000001,-0.805000000000001,-0.800000000000001,
-0.795000000000001,-0.790000000000001,-0.785000000000001,-0.780000000000001,
-0.775000000000001,-0.770000000000001,-0.765000000000001,-0.760000000000001,
-0.755000000000001,-0.750000000000001,-0.745000000000001,-0.740000000000001,
-0.735000000000001,-0.730000000000001,-0.725000000000001,-0.720000000000001,
-0.715000000000001,-0.710000000000001,-0.705000000000001,-0.700000000000001,
-0.695000000000001,-0.690000000000001,-0.685,-0.68,-0.675,-0.67,-0.665,
-0.66,-0.655,-0.65,-0.645,-0.64,-0.635,-0.63,-0.625,-0.62,-0.615,-0.61,
-0.605,-0.6,-0.595,-0.59,-0.585,-0.58,-0.575,-0.57,-0.565,-0.56,-0.555,
-0.55,-0.545,-0.54,-0.535,-0.53,-0.525,-0.52,-0.515,-0.51,-0.505,-0.5,-0.495,
-0.49,-0.485,-0.48,-0.475,-0.47,-0.465,-0.46,-0.455,-0.45,-0.445,-0.44,
-0.435,-0.43,-0.425,-0.42,-0.415,-0.41,-0.405,-0.4,-0.395,-0.39,-0.385,
-0.38,-0.375,-0.37,-0.365,-0.36,-0.355,-0.35,-0.345,-0.34,-0.335,-0.33,
-0.325,-0.32,-0.315,-0.31,-0.305,-0.3,-0.295,-0.29,-0.285,-0.28,-0.275,
-0.27,-0.265,-0.26,-0.255,-0.25,-0.245,-0.24,-0.235,-0.23,-0.225,-0.22,
-0.215,-0.21,-0.205,-0.2,-0.195,-0.19,-0.185,-0.18,-0.175,-0.17,-0.165,
-0.16,-0.155,-0.15,-0.145,-0.14,-0.135,-0.13,-0.125,-0.12,-0.115,-0.11,
-0.105,-0.1,-0.095,-0.09,-0.085,-0.08,-0.075,-0.07,-0.065,-0.06,-0.055,
-0.05,-0.045,-0.04,-0.035,-0.03,-0.025,-0.02,-0.015,-0.01,-0.005,0.),
 .UNSPECIFIED.)
CURVE()
GEOMETRIC_REPRESENTATION_ITEM()
RATIONAL_B_SPLINE_CURVE((1.,1.,1.,1.,1.,1.,1.,1.,1.,1.,1.,1.,1.,1.,1.,1.,
1.,1.,1.,1.,1.,1.,1.,1.,1.,1.,1.,1.,1.,1.,1.,1.,1.,1.,1.,1.,1.,1.,1.,1.,
1.,1.,1.,1.,1.,1.,1.,1.,1.,1.,1.,1.,1.,1.,1.,1.,1.,1.,1.,1.,1.,1.,1.,1.,
1.,1.,1.,1.,1.,1.,1.,1.,1.,1.,1.,1.,1.,1.,1.,1.,1.,1.,1.,1.,1.,1.,1.,1.,
1.,1.,1.,1.,1.,1.,1.,1.,1.,1.,1.,1.,1.,1.,1.,1.,1.,1.,1.,1.,1.,1.,1.,1.,
1.,1.,1.,1.,1.,1.,1.,1.,1.,1.,1.,1.,1.,1.,1.,1.,1.,1.,1.,1.,1.,1.,1.,1.,
1.,1.,1.,1.,1.,1.,1.,1.,1.,1.,1.,1.,1.,1.,1.,1.,1.,1.,1.,1.,1.,1.,1.,1.,
1.,1.,1.,1.,1.,1.,1.,1.,1.,1.,1.,1.,1.,1.,1.,1.,1.,1.,1.,1.,1.,1.,1.,1.,
1.,1.,1.,1.,1.,1.,1.,1.,1.,1.))
REPRESENTATION_ITEM('')
);
#487=(
BOUNDED_CURVE()
B_SPLINE_CURVE(5,(#90665,#90666,#90667,#90668,#90669,#90670,#90671,#90672,
#90673,#90674,#90675,#90676,#90677,#90678,#90679,#90680,#90681,#90682,#90683,
#90684,#90685,#90686,#90687,#90688,#90689,#90690,#90691,#90692,#90693,#90694,
#90695,#90696,#90697,#90698,#90699,#90700,#90701,#90702,#90703,#90704,#90705,
#90706,#90707,#90708,#90709,#90710,#90711,#90712,#90713,#90714,#90715,#90716,
#90717,#90718,#90719,#90720,#90721,#90722,#90723,#90724,#90725,#90726,#90727,
#90728,#90729,#90730,#90731,#90732,#90733,#90734,#90735,#90736,#90737,#90738,
#90739,#90740,#90741,#90742,#90743,#90744,#90745,#90746,#90747,#90748,#90749,
#90750,#90751,#90752,#90753,#90754,#90755,#90756,#90757,#90758,#90759,#90760,
#90761,#90762,#90763,#90764,#90765,#90766,#90767,#90768,#90769,#90770,#90771,
#90772,#90773,#90774,#90775,#90776,#90777,#90778,#90779,#90780,#90781,#90782,
#90783,#90784,#90785,#90786,#90787,#90788,#90789,#90790,#90791,#90792,#90793,
#90794,#90795,#90796,#90797,#90798,#90799,#90800,#90801,#90802,#90803,#90804,
#90805,#90806,#90807,#90808,#90809,#90810,#90811,#90812,#90813,#90814,#90815,
#90816,#90817,#90818,#90819,#90820,#90821,#90822,#90823,#90824,#90825,#90826,
#90827,#90828,#90829,#90830,#90831,#90832,#90833,#90834,#90835,#90836,#90837,
#90838,#90839,#90840,#90841,#90842,#90843,#90844,#90845,#90846,#90847,#90848,
#90849,#90850,#90851,#90852,#90853,#90854,#90855,#90856,#90857,#90858),
 .UNSPECIFIED.,.F.,.F.)
B_SPLINE_CURVE_WITH_KNOTS((6,1,1,1,1,1,1,1,1,1,1,1,1,1,1,1,1,1,1,1,1,1,
1,1,1,1,1,1,1,1,1,1,1,1,1,1,1,1,1,1,1,1,1,1,1,1,1,1,1,1,1,1,1,1,1,1,1,1,
1,1,1,1,1,1,1,1,1,1,1,1,1,1,1,1,1,1,1,1,1,1,1,1,1,1,1,1,1,1,1,1,1,1,1,1,
1,1,1,1,1,1,1,1,1,1,1,1,1,1,1,1,1,1,1,1,1,1,1,1,1,1,1,1,1,1,1,1,1,1,1,1,
1,1,1,1,1,1,1,1,1,1,1,1,1,1,1,1,1,1,1,1,1,1,1,1,1,1,1,1,1,1,1,1,1,1,1,1,
1,1,1,1,1,1,1,1,1,1,1,1,1,1,1,1,1,1,1,1,1,1,1,6),(0.,0.005,0.01,0.015,0.02,
0.025,0.03,0.035,0.04,0.045,0.05,0.055,0.06,0.065,0.07,0.075,0.08,0.085,
0.09,0.095,0.1,0.105,0.11,0.115,0.12,0.125,0.13,0.135,0.14,0.145,0.15,0.155,
0.16,0.165,0.17,0.175,0.18,0.185,0.19,0.195,0.2,0.205,0.21,0.215,0.22,0.225,
0.23,0.235,0.24,0.245,0.25,0.255,0.26,0.265,0.27,0.275,0.28,0.285,0.29,
0.295,0.3,0.305,0.31,0.315,0.32,0.325,0.33,0.335,0.34,0.345,0.35,0.355,
0.36,0.365,0.37,0.375,0.38,0.385,0.39,0.395,0.4,0.405,0.41,0.415,0.42,0.425,
0.43,0.435,0.44,0.445,0.45,0.455,0.46,0.465,0.47,0.475,0.48,0.485,0.49,
0.495,0.5,0.505,0.51,0.515,0.52,0.525,0.53,0.535,0.54,0.545,0.55,0.555,
0.56,0.565,0.57,0.575,0.58,0.585,0.59,0.595,0.6,0.605,0.61,0.615,0.62,0.625,
0.63,0.635,0.64,0.645,0.65,0.655,0.66,0.665,0.67,0.675,0.68,0.685,0.690000000000001,
0.695000000000001,0.700000000000001,0.705000000000001,0.710000000000001,
0.715000000000001,0.720000000000001,0.725000000000001,0.730000000000001,
0.735000000000001,0.740000000000001,0.745000000000001,0.750000000000001,
0.755000000000001,0.760000000000001,0.765000000000001,0.770000000000001,
0.775000000000001,0.780000000000001,0.785000000000001,0.790000000000001,
0.795000000000001,0.800000000000001,0.805000000000001,0.810000000000001,
0.815000000000001,0.820000000000001,0.825000000000001,0.830000000000001,
0.835000000000001,0.840000000000001,0.845000000000001,0.850000000000001,
0.855000000000001,0.860000000000001,0.865000000000001,0.870000000000001,
0.875000000000001,0.880000000000001,0.885000000000001,0.890000000000001,
0.895000000000001,0.900000000000001,0.905000000000001,0.910000000000001,
0.915000000000001,0.920000000000001,0.925000000000001,0.930000000000001,
0.935000000000001,0.940000000000001,0.941429844431454),.UNSPECIFIED.)
CURVE()
GEOMETRIC_REPRESENTATION_ITEM()
RATIONAL_B_SPLINE_CURVE((1.,1.,1.,1.,1.,1.,1.,1.,1.,1.,1.,1.,1.,1.,1.,1.,
1.,1.,1.,1.,1.,1.,1.,1.,1.,1.,1.,1.,1.,1.,1.,1.,1.,1.,1.,1.,1.,1.,1.,1.,
1.,1.,1.,1.,1.,1.,1.,1.,1.,1.,1.,1.,1.,1.,1.,1.,1.,1.,1.,1.,1.,1.,1.,1.,
1.,1.,1.,1.,1.,1.,1.,1.,1.,1.,1.,1.,1.,1.,1.,1.,1.,1.,1.,1.,1.,1.,1.,1.,
1.,1.,1.,1.,1.,1.,1.,1.,1.,1.,1.,1.,1.,1.,1.,1.,1.,1.,1.,1.,1.,1.,1.,1.,
1.,1.,1.,1.,1.,1.,1.,1.,1.,1.,1.,1.,1.,1.,1.,1.,1.,1.,1.,1.,1.,1.,1.,1.,
1.,1.,1.,1.,1.,1.,1.,1.,1.,1.,1.,1.,1.,1.,1.,1.,1.,1.,1.,1.,1.,1.,1.,1.,
1.,1.,1.,1.,1.,1.,1.,1.,1.,1.,1.,1.,1.,1.,1.,1.,1.,1.,1.,1.,1.,1.,1.,1.,
1.,1.,1.,1.,1.,1.,1.,1.,1.,1.))
REPRESENTATION_ITEM('')
);
#488=(
BOUNDED_CURVE()
B_SPLINE_CURVE(5,(#90861,#90862,#90863,#90864,#90865,#90866,#90867,#90868,
#90869,#90870,#90871,#90872,#90873,#90874,#90875,#90876,#90877,#90878,#90879,
#90880,#90881,#90882,#90883,#90884,#90885,#90886,#90887,#90888,#90889,#90890,
#90891,#90892,#90893,#90894,#90895,#90896,#90897,#90898,#90899,#90900,#90901,
#90902,#90903,#90904,#90905,#90906,#90907,#90908,#90909,#90910,#90911,#90912,
#90913,#90914,#90915,#90916,#90917,#90918,#90919,#90920,#90921,#90922,#90923,
#90924,#90925,#90926,#90927,#90928,#90929,#90930,#90931,#90932,#90933,#90934,
#90935,#90936,#90937,#90938,#90939,#90940,#90941,#90942,#90943,#90944,#90945,
#90946,#90947,#90948,#90949,#90950,#90951,#90952,#90953,#90954,#90955,#90956,
#90957,#90958,#90959,#90960,#90961,#90962,#90963,#90964,#90965,#90966,#90967,
#90968,#90969,#90970,#90971,#90972,#90973,#90974,#90975,#90976,#90977,#90978,
#90979,#90980,#90981,#90982,#90983,#90984,#90985,#90986,#90987,#90988,#90989,
#90990,#90991,#90992,#90993,#90994,#90995,#90996,#90997,#90998,#90999,#91000,
#91001,#91002,#91003,#91004,#91005,#91006,#91007,#91008,#91009,#91010,#91011,
#91012,#91013,#91014,#91015,#91016,#91017,#91018,#91019,#91020,#91021,#91022,
#91023,#91024,#91025,#91026,#91027,#91028,#91029,#91030,#91031,#91032,#91033,
#91034,#91035,#91036,#91037,#91038,#91039,#91040,#91041,#91042,#91043,#91044,
#91045,#91046,#91047,#91048,#91049,#91050,#91051,#91052,#91053,#91054),
 .UNSPECIFIED.,.F.,.F.)
B_SPLINE_CURVE_WITH_KNOTS((6,1,1,1,1,1,1,1,1,1,1,1,1,1,1,1,1,1,1,1,1,1,
1,1,1,1,1,1,1,1,1,1,1,1,1,1,1,1,1,1,1,1,1,1,1,1,1,1,1,1,1,1,1,1,1,1,1,1,
1,1,1,1,1,1,1,1,1,1,1,1,1,1,1,1,1,1,1,1,1,1,1,1,1,1,1,1,1,1,1,1,1,1,1,1,
1,1,1,1,1,1,1,1,1,1,1,1,1,1,1,1,1,1,1,1,1,1,1,1,1,1,1,1,1,1,1,1,1,1,1,1,
1,1,1,1,1,1,1,1,1,1,1,1,1,1,1,1,1,1,1,1,1,1,1,1,1,1,1,1,1,1,1,1,1,1,1,1,
1,1,1,1,1,1,1,1,1,1,1,1,1,1,1,1,1,1,1,1,1,1,1,6),(-0.941429844431448,-0.940000000000001,
-0.935000000000001,-0.930000000000001,-0.925000000000001,-0.920000000000001,
-0.915000000000001,-0.910000000000001,-0.905000000000001,-0.900000000000001,
-0.895000000000001,-0.890000000000001,-0.885000000000001,-0.880000000000001,
-0.875000000000001,-0.870000000000001,-0.865000000000001,-0.860000000000001,
-0.855000000000001,-0.850000000000001,-0.845000000000001,-0.840000000000001,
-0.835000000000001,-0.830000000000001,-0.825000000000001,-0.820000000000001,
-0.815000000000001,-0.810000000000001,-0.805000000000001,-0.800000000000001,
-0.795000000000001,-0.790000000000001,-0.785000000000001,-0.780000000000001,
-0.775000000000001,-0.770000000000001,-0.765000000000001,-0.760000000000001,
-0.755000000000001,-0.750000000000001,-0.745000000000001,-0.740000000000001,
-0.735000000000001,-0.730000000000001,-0.725000000000001,-0.720000000000001,
-0.715000000000001,-0.710000000000001,-0.705000000000001,-0.700000000000001,
-0.695000000000001,-0.690000000000001,-0.685,-0.68,-0.675,-0.67,-0.665,
-0.66,-0.655,-0.65,-0.645,-0.64,-0.635,-0.63,-0.625,-0.62,-0.615,-0.61,
-0.605,-0.6,-0.595,-0.59,-0.585,-0.58,-0.575,-0.57,-0.565,-0.56,-0.555,
-0.55,-0.545,-0.54,-0.535,-0.53,-0.525,-0.52,-0.515,-0.51,-0.505,-0.5,-0.495,
-0.49,-0.485,-0.48,-0.475,-0.47,-0.465,-0.46,-0.455,-0.45,-0.445,-0.44,
-0.435,-0.43,-0.425,-0.42,-0.415,-0.41,-0.405,-0.4,-0.395,-0.39,-0.385,
-0.38,-0.375,-0.37,-0.365,-0.36,-0.355,-0.35,-0.345,-0.34,-0.335,-0.33,
-0.325,-0.32,-0.315,-0.31,-0.305,-0.3,-0.295,-0.29,-0.285,-0.28,-0.275,
-0.27,-0.265,-0.26,-0.255,-0.25,-0.245,-0.24,-0.235,-0.23,-0.225,-0.22,
-0.215,-0.21,-0.205,-0.2,-0.195,-0.19,-0.185,-0.18,-0.175,-0.17,-0.165,
-0.16,-0.155,-0.15,-0.145,-0.14,-0.135,-0.13,-0.125,-0.12,-0.115,-0.11,
-0.105,-0.1,-0.095,-0.09,-0.085,-0.08,-0.075,-0.07,-0.065,-0.06,-0.055,
-0.05,-0.045,-0.04,-0.035,-0.03,-0.025,-0.02,-0.015,-0.01,-0.005,0.),
 .UNSPECIFIED.)
CURVE()
GEOMETRIC_REPRESENTATION_ITEM()
RATIONAL_B_SPLINE_CURVE((1.,1.,1.,1.,1.,1.,1.,1.,1.,1.,1.,1.,1.,1.,1.,1.,
1.,1.,1.,1.,1.,1.,1.,1.,1.,1.,1.,1.,1.,1.,1.,1.,1.,1.,1.,1.,1.,1.,1.,1.,
1.,1.,1.,1.,1.,1.,1.,1.,1.,1.,1.,1.,1.,1.,1.,1.,1.,1.,1.,1.,1.,1.,1.,1.,
1.,1.,1.,1.,1.,1.,1.,1.,1.,1.,1.,1.,1.,1.,1.,1.,1.,1.,1.,1.,1.,1.,1.,1.,
1.,1.,1.,1.,1.,1.,1.,1.,1.,1.,1.,1.,1.,1.,1.,1.,1.,1.,1.,1.,1.,1.,1.,1.,
1.,1.,1.,1.,1.,1.,1.,1.,1.,1.,1.,1.,1.,1.,1.,1.,1.,1.,1.,1.,1.,1.,1.,1.,
1.,1.,1.,1.,1.,1.,1.,1.,1.,1.,1.,1.,1.,1.,1.,1.,1.,1.,1.,1.,1.,1.,1.,1.,
1.,1.,1.,1.,1.,1.,1.,1.,1.,1.,1.,1.,1.,1.,1.,1.,1.,1.,1.,1.,1.,1.,1.,1.,
1.,1.,1.,1.,1.,1.,1.,1.,1.,1.))
REPRESENTATION_ITEM('')
);
#489=(
BOUNDED_CURVE()
B_SPLINE_CURVE(5,(#91561,#91562,#91563,#91564,#91565,#91566,#91567,#91568,
#91569,#91570,#91571,#91572,#91573,#91574,#91575,#91576,#91577,#91578,#91579,
#91580,#91581,#91582,#91583,#91584,#91585,#91586,#91587,#91588,#91589,#91590,
#91591,#91592,#91593,#91594,#91595,#91596,#91597,#91598,#91599,#91600,#91601,
#91602,#91603,#91604,#91605,#91606,#91607,#91608,#91609,#91610,#91611,#91612,
#91613,#91614,#91615,#91616,#91617,#91618,#91619,#91620,#91621,#91622,#91623,
#91624,#91625,#91626,#91627,#91628,#91629,#91630,#91631,#91632,#91633,#91634,
#91635,#91636,#91637,#91638,#91639,#91640,#91641,#91642,#91643,#91644,#91645,
#91646,#91647,#91648,#91649,#91650,#91651,#91652,#91653,#91654,#91655,#91656,
#91657,#91658,#91659,#91660,#91661,#91662,#91663,#91664,#91665,#91666,#91667,
#91668,#91669,#91670,#91671,#91672,#91673,#91674,#91675,#91676,#91677,#91678,
#91679,#91680,#91681,#91682,#91683,#91684,#91685,#91686,#91687,#91688,#91689,
#91690,#91691,#91692,#91693,#91694,#91695,#91696,#91697,#91698,#91699,#91700,
#91701,#91702,#91703,#91704,#91705,#91706,#91707,#91708,#91709,#91710,#91711,
#91712,#91713,#91714,#91715,#91716,#91717,#91718,#91719,#91720,#91721,#91722,
#91723,#91724,#91725,#91726,#91727,#91728,#91729,#91730,#91731,#91732,#91733,
#91734,#91735,#91736,#91737,#91738,#91739,#91740,#91741,#91742,#91743,#91744,
#91745,#91746,#91747,#91748,#91749,#91750,#91751,#91752,#91753,#91754),
 .UNSPECIFIED.,.F.,.F.)
B_SPLINE_CURVE_WITH_KNOTS((6,1,1,1,1,1,1,1,1,1,1,1,1,1,1,1,1,1,1,1,1,1,
1,1,1,1,1,1,1,1,1,1,1,1,1,1,1,1,1,1,1,1,1,1,1,1,1,1,1,1,1,1,1,1,1,1,1,1,
1,1,1,1,1,1,1,1,1,1,1,1,1,1,1,1,1,1,1,1,1,1,1,1,1,1,1,1,1,1,1,1,1,1,1,1,
1,1,1,1,1,1,1,1,1,1,1,1,1,1,1,1,1,1,1,1,1,1,1,1,1,1,1,1,1,1,1,1,1,1,1,1,
1,1,1,1,1,1,1,1,1,1,1,1,1,1,1,1,1,1,1,1,1,1,1,1,1,1,1,1,1,1,1,1,1,1,1,1,
1,1,1,1,1,1,1,1,1,1,1,1,1,1,1,1,1,1,1,1,1,1,1,6),(0.,0.005,0.01,0.015,0.02,
0.025,0.03,0.035,0.04,0.045,0.05,0.055,0.06,0.065,0.07,0.075,0.08,0.085,
0.09,0.095,0.1,0.105,0.11,0.115,0.12,0.125,0.13,0.135,0.14,0.145,0.15,0.155,
0.16,0.165,0.17,0.175,0.18,0.185,0.19,0.195,0.2,0.205,0.21,0.215,0.22,0.225,
0.23,0.235,0.24,0.245,0.25,0.255,0.26,0.265,0.27,0.275,0.28,0.285,0.29,
0.295,0.3,0.305,0.31,0.315,0.32,0.325,0.33,0.335,0.34,0.345,0.35,0.355,
0.36,0.365,0.37,0.375,0.38,0.385,0.39,0.395,0.4,0.405,0.41,0.415,0.42,0.425,
0.43,0.435,0.44,0.445,0.45,0.455,0.46,0.465,0.47,0.475,0.48,0.485,0.49,
0.495,0.5,0.505,0.51,0.515,0.52,0.525,0.53,0.535,0.54,0.545,0.55,0.555,
0.56,0.565,0.57,0.575,0.58,0.585,0.59,0.595,0.6,0.605,0.61,0.615,0.62,0.625,
0.63,0.635,0.64,0.645,0.65,0.655,0.66,0.665,0.67,0.675,0.68,0.685,0.690000000000001,
0.695000000000001,0.700000000000001,0.705000000000001,0.710000000000001,
0.715000000000001,0.720000000000001,0.725000000000001,0.730000000000001,
0.735000000000001,0.740000000000001,0.745000000000001,0.750000000000001,
0.755000000000001,0.760000000000001,0.765000000000001,0.770000000000001,
0.775000000000001,0.780000000000001,0.785000000000001,0.790000000000001,
0.795000000000001,0.800000000000001,0.805000000000001,0.810000000000001,
0.815000000000001,0.820000000000001,0.825000000000001,0.830000000000001,
0.835000000000001,0.840000000000001,0.845000000000001,0.850000000000001,
0.855000000000001,0.860000000000001,0.865000000000001,0.870000000000001,
0.875000000000001,0.880000000000001,0.885000000000001,0.890000000000001,
0.895000000000001,0.900000000000001,0.905000000000001,0.910000000000001,
0.915000000000001,0.920000000000001,0.925000000000001,0.930000000000001,
0.935000000000001,0.940000000000001,0.941429844431403),.UNSPECIFIED.)
CURVE()
GEOMETRIC_REPRESENTATION_ITEM()
RATIONAL_B_SPLINE_CURVE((1.,1.,1.,1.,1.,1.,1.,1.,1.,1.,1.,1.,1.,1.,1.,1.,
1.,1.,1.,1.,1.,1.,1.,1.,1.,1.,1.,1.,1.,1.,1.,1.,1.,1.,1.,1.,1.,1.,1.,1.,
1.,1.,1.,1.,1.,1.,1.,1.,1.,1.,1.,1.,1.,1.,1.,1.,1.,1.,1.,1.,1.,1.,1.,1.,
1.,1.,1.,1.,1.,1.,1.,1.,1.,1.,1.,1.,1.,1.,1.,1.,1.,1.,1.,1.,1.,1.,1.,1.,
1.,1.,1.,1.,1.,1.,1.,1.,1.,1.,1.,1.,1.,1.,1.,1.,1.,1.,1.,1.,1.,1.,1.,1.,
1.,1.,1.,1.,1.,1.,1.,1.,1.,1.,1.,1.,1.,1.,1.,1.,1.,1.,1.,1.,1.,1.,1.,1.,
1.,1.,1.,1.,1.,1.,1.,1.,1.,1.,1.,1.,1.,1.,1.,1.,1.,1.,1.,1.,1.,1.,1.,1.,
1.,1.,1.,1.,1.,1.,1.,1.,1.,1.,1.,1.,1.,1.,1.,1.,1.,1.,1.,1.,1.,1.,1.,1.,
1.,1.,1.,1.,1.,1.,1.,1.,1.,1.))
REPRESENTATION_ITEM('')
);
#490=(
BOUNDED_CURVE()
B_SPLINE_CURVE(5,(#91757,#91758,#91759,#91760,#91761,#91762,#91763,#91764,
#91765,#91766,#91767,#91768,#91769,#91770,#91771,#91772,#91773,#91774,#91775,
#91776,#91777,#91778,#91779,#91780,#91781,#91782,#91783,#91784,#91785,#91786,
#91787,#91788,#91789,#91790,#91791,#91792,#91793,#91794,#91795,#91796,#91797,
#91798,#91799,#91800,#91801,#91802,#91803,#91804,#91805,#91806,#91807,#91808,
#91809,#91810,#91811,#91812,#91813,#91814,#91815,#91816,#91817,#91818,#91819,
#91820,#91821,#91822,#91823,#91824,#91825,#91826,#91827,#91828,#91829,#91830,
#91831,#91832,#91833,#91834,#91835,#91836,#91837,#91838,#91839,#91840,#91841,
#91842,#91843,#91844,#91845,#91846,#91847,#91848,#91849,#91850,#91851,#91852,
#91853,#91854,#91855,#91856,#91857,#91858,#91859,#91860,#91861,#91862,#91863,
#91864,#91865,#91866,#91867,#91868,#91869,#91870,#91871,#91872,#91873,#91874,
#91875,#91876,#91877,#91878,#91879,#91880,#91881,#91882,#91883,#91884,#91885,
#91886,#91887,#91888,#91889,#91890,#91891,#91892,#91893,#91894,#91895,#91896,
#91897,#91898,#91899,#91900,#91901,#91902,#91903,#91904,#91905,#91906,#91907,
#91908,#91909,#91910,#91911,#91912,#91913,#91914,#91915,#91916,#91917,#91918,
#91919,#91920,#91921,#91922,#91923,#91924,#91925,#91926,#91927,#91928,#91929,
#91930,#91931,#91932,#91933,#91934,#91935,#91936,#91937,#91938,#91939,#91940,
#91941,#91942,#91943,#91944,#91945,#91946,#91947,#91948,#91949,#91950),
 .UNSPECIFIED.,.F.,.F.)
B_SPLINE_CURVE_WITH_KNOTS((6,1,1,1,1,1,1,1,1,1,1,1,1,1,1,1,1,1,1,1,1,1,
1,1,1,1,1,1,1,1,1,1,1,1,1,1,1,1,1,1,1,1,1,1,1,1,1,1,1,1,1,1,1,1,1,1,1,1,
1,1,1,1,1,1,1,1,1,1,1,1,1,1,1,1,1,1,1,1,1,1,1,1,1,1,1,1,1,1,1,1,1,1,1,1,
1,1,1,1,1,1,1,1,1,1,1,1,1,1,1,1,1,1,1,1,1,1,1,1,1,1,1,1,1,1,1,1,1,1,1,1,
1,1,1,1,1,1,1,1,1,1,1,1,1,1,1,1,1,1,1,1,1,1,1,1,1,1,1,1,1,1,1,1,1,1,1,1,
1,1,1,1,1,1,1,1,1,1,1,1,1,1,1,1,1,1,1,1,1,1,1,6),(-0.941429844431386,-0.940000000000001,
-0.935000000000001,-0.930000000000001,-0.925000000000001,-0.920000000000001,
-0.915000000000001,-0.910000000000001,-0.905000000000001,-0.900000000000001,
-0.895000000000001,-0.890000000000001,-0.885000000000001,-0.880000000000001,
-0.875000000000001,-0.870000000000001,-0.865000000000001,-0.860000000000001,
-0.855000000000001,-0.850000000000001,-0.845000000000001,-0.840000000000001,
-0.835000000000001,-0.830000000000001,-0.825000000000001,-0.820000000000001,
-0.815000000000001,-0.810000000000001,-0.805000000000001,-0.800000000000001,
-0.795000000000001,-0.790000000000001,-0.785000000000001,-0.780000000000001,
-0.775000000000001,-0.770000000000001,-0.765000000000001,-0.760000000000001,
-0.755000000000001,-0.750000000000001,-0.745000000000001,-0.740000000000001,
-0.735000000000001,-0.730000000000001,-0.725000000000001,-0.720000000000001,
-0.715000000000001,-0.710000000000001,-0.705000000000001,-0.700000000000001,
-0.695000000000001,-0.690000000000001,-0.685,-0.68,-0.675,-0.67,-0.665,
-0.66,-0.655,-0.65,-0.645,-0.64,-0.635,-0.63,-0.625,-0.62,-0.615,-0.61,
-0.605,-0.6,-0.595,-0.59,-0.585,-0.58,-0.575,-0.57,-0.565,-0.56,-0.555,
-0.55,-0.545,-0.54,-0.535,-0.53,-0.525,-0.52,-0.515,-0.51,-0.505,-0.5,-0.495,
-0.49,-0.485,-0.48,-0.475,-0.47,-0.465,-0.46,-0.455,-0.45,-0.445,-0.44,
-0.435,-0.43,-0.425,-0.42,-0.415,-0.41,-0.405,-0.4,-0.395,-0.39,-0.385,
-0.38,-0.375,-0.37,-0.365,-0.36,-0.355,-0.35,-0.345,-0.34,-0.335,-0.33,
-0.325,-0.32,-0.315,-0.31,-0.305,-0.3,-0.295,-0.29,-0.285,-0.28,-0.275,
-0.27,-0.265,-0.26,-0.255,-0.25,-0.245,-0.24,-0.235,-0.23,-0.225,-0.22,
-0.215,-0.21,-0.205,-0.2,-0.195,-0.19,-0.185,-0.18,-0.175,-0.17,-0.165,
-0.16,-0.155,-0.15,-0.145,-0.14,-0.135,-0.13,-0.125,-0.12,-0.115,-0.11,
-0.105,-0.1,-0.095,-0.09,-0.085,-0.08,-0.075,-0.07,-0.065,-0.06,-0.055,
-0.05,-0.045,-0.04,-0.035,-0.03,-0.025,-0.02,-0.015,-0.01,-0.005,0.),
 .UNSPECIFIED.)
CURVE()
GEOMETRIC_REPRESENTATION_ITEM()
RATIONAL_B_SPLINE_CURVE((1.,1.,1.,1.,1.,1.,1.,1.,1.,1.,1.,1.,1.,1.,1.,1.,
1.,1.,1.,1.,1.,1.,1.,1.,1.,1.,1.,1.,1.,1.,1.,1.,1.,1.,1.,1.,1.,1.,1.,1.,
1.,1.,1.,1.,1.,1.,1.,1.,1.,1.,1.,1.,1.,1.,1.,1.,1.,1.,1.,1.,1.,1.,1.,1.,
1.,1.,1.,1.,1.,1.,1.,1.,1.,1.,1.,1.,1.,1.,1.,1.,1.,1.,1.,1.,1.,1.,1.,1.,
1.,1.,1.,1.,1.,1.,1.,1.,1.,1.,1.,1.,1.,1.,1.,1.,1.,1.,1.,1.,1.,1.,1.,1.,
1.,1.,1.,1.,1.,1.,1.,1.,1.,1.,1.,1.,1.,1.,1.,1.,1.,1.,1.,1.,1.,1.,1.,1.,
1.,1.,1.,1.,1.,1.,1.,1.,1.,1.,1.,1.,1.,1.,1.,1.,1.,1.,1.,1.,1.,1.,1.,1.,
1.,1.,1.,1.,1.,1.,1.,1.,1.,1.,1.,1.,1.,1.,1.,1.,1.,1.,1.,1.,1.,1.,1.,1.,
1.,1.,1.,1.,1.,1.,1.,1.,1.,1.))
REPRESENTATION_ITEM('')
);
#491=(
BOUNDED_CURVE()
B_SPLINE_CURVE(5,(#92457,#92458,#92459,#92460,#92461,#92462,#92463,#92464,
#92465,#92466,#92467,#92468,#92469,#92470,#92471,#92472,#92473,#92474,#92475,
#92476,#92477,#92478,#92479,#92480,#92481,#92482,#92483,#92484,#92485,#92486,
#92487,#92488,#92489,#92490,#92491,#92492,#92493,#92494,#92495,#92496,#92497,
#92498,#92499,#92500,#92501,#92502,#92503,#92504,#92505,#92506,#92507,#92508,
#92509,#92510,#92511,#92512,#92513,#92514,#92515,#92516,#92517,#92518,#92519,
#92520,#92521,#92522,#92523,#92524,#92525,#92526,#92527,#92528,#92529,#92530,
#92531,#92532,#92533,#92534,#92535,#92536,#92537,#92538,#92539,#92540,#92541,
#92542,#92543,#92544,#92545,#92546,#92547,#92548,#92549,#92550,#92551,#92552,
#92553,#92554,#92555,#92556,#92557,#92558,#92559,#92560,#92561,#92562,#92563,
#92564,#92565,#92566,#92567,#92568,#92569,#92570,#92571,#92572,#92573,#92574,
#92575,#92576,#92577,#92578,#92579,#92580,#92581,#92582,#92583,#92584,#92585,
#92586,#92587,#92588,#92589,#92590,#92591,#92592,#92593,#92594,#92595,#92596,
#92597,#92598,#92599,#92600,#92601,#92602,#92603,#92604,#92605,#92606,#92607,
#92608,#92609,#92610,#92611,#92612,#92613,#92614,#92615,#92616,#92617,#92618,
#92619,#92620,#92621,#92622,#92623,#92624,#92625,#92626,#92627,#92628,#92629,
#92630,#92631,#92632,#92633,#92634,#92635,#92636,#92637,#92638,#92639,#92640,
#92641,#92642,#92643,#92644,#92645,#92646,#92647,#92648,#92649,#92650),
 .UNSPECIFIED.,.F.,.F.)
B_SPLINE_CURVE_WITH_KNOTS((6,1,1,1,1,1,1,1,1,1,1,1,1,1,1,1,1,1,1,1,1,1,
1,1,1,1,1,1,1,1,1,1,1,1,1,1,1,1,1,1,1,1,1,1,1,1,1,1,1,1,1,1,1,1,1,1,1,1,
1,1,1,1,1,1,1,1,1,1,1,1,1,1,1,1,1,1,1,1,1,1,1,1,1,1,1,1,1,1,1,1,1,1,1,1,
1,1,1,1,1,1,1,1,1,1,1,1,1,1,1,1,1,1,1,1,1,1,1,1,1,1,1,1,1,1,1,1,1,1,1,1,
1,1,1,1,1,1,1,1,1,1,1,1,1,1,1,1,1,1,1,1,1,1,1,1,1,1,1,1,1,1,1,1,1,1,1,1,
1,1,1,1,1,1,1,1,1,1,1,1,1,1,1,1,1,1,1,1,1,1,1,6),(0.,0.005,0.01,0.015,0.02,
0.025,0.03,0.035,0.04,0.045,0.05,0.055,0.06,0.065,0.07,0.075,0.08,0.085,
0.09,0.095,0.1,0.105,0.11,0.115,0.12,0.125,0.13,0.135,0.14,0.145,0.15,0.155,
0.16,0.165,0.17,0.175,0.18,0.185,0.19,0.195,0.2,0.205,0.21,0.215,0.22,0.225,
0.23,0.235,0.24,0.245,0.25,0.255,0.26,0.265,0.27,0.275,0.28,0.285,0.29,
0.295,0.3,0.305,0.31,0.315,0.32,0.325,0.33,0.335,0.34,0.345,0.35,0.355,
0.36,0.365,0.37,0.375,0.38,0.385,0.39,0.395,0.4,0.405,0.41,0.415,0.42,0.425,
0.43,0.435,0.44,0.445,0.45,0.455,0.46,0.465,0.47,0.475,0.48,0.485,0.49,
0.495,0.5,0.505,0.51,0.515,0.52,0.525,0.53,0.535,0.54,0.545,0.55,0.555,
0.56,0.565,0.57,0.575,0.58,0.585,0.59,0.595,0.6,0.605,0.61,0.615,0.62,0.625,
0.63,0.635,0.64,0.645,0.65,0.655,0.66,0.665,0.67,0.675,0.68,0.685,0.690000000000001,
0.695000000000001,0.700000000000001,0.705000000000001,0.710000000000001,
0.715000000000001,0.720000000000001,0.725000000000001,0.730000000000001,
0.735000000000001,0.740000000000001,0.745000000000001,0.750000000000001,
0.755000000000001,0.760000000000001,0.765000000000001,0.770000000000001,
0.775000000000001,0.780000000000001,0.785000000000001,0.790000000000001,
0.795000000000001,0.800000000000001,0.805000000000001,0.810000000000001,
0.815000000000001,0.820000000000001,0.825000000000001,0.830000000000001,
0.835000000000001,0.840000000000001,0.845000000000001,0.850000000000001,
0.855000000000001,0.860000000000001,0.865000000000001,0.870000000000001,
0.875000000000001,0.880000000000001,0.885000000000001,0.890000000000001,
0.895000000000001,0.900000000000001,0.905000000000001,0.910000000000001,
0.915000000000001,0.920000000000001,0.925000000000001,0.930000000000001,
0.935000000000001,0.940000000000001,0.941429844431541),.UNSPECIFIED.)
CURVE()
GEOMETRIC_REPRESENTATION_ITEM()
RATIONAL_B_SPLINE_CURVE((1.,1.,1.,1.,1.,1.,1.,1.,1.,1.,1.,1.,1.,1.,1.,1.,
1.,1.,1.,1.,1.,1.,1.,1.,1.,1.,1.,1.,1.,1.,1.,1.,1.,1.,1.,1.,1.,1.,1.,1.,
1.,1.,1.,1.,1.,1.,1.,1.,1.,1.,1.,1.,1.,1.,1.,1.,1.,1.,1.,1.,1.,1.,1.,1.,
1.,1.,1.,1.,1.,1.,1.,1.,1.,1.,1.,1.,1.,1.,1.,1.,1.,1.,1.,1.,1.,1.,1.,1.,
1.,1.,1.,1.,1.,1.,1.,1.,1.,1.,1.,1.,1.,1.,1.,1.,1.,1.,1.,1.,1.,1.,1.,1.,
1.,1.,1.,1.,1.,1.,1.,1.,1.,1.,1.,1.,1.,1.,1.,1.,1.,1.,1.,1.,1.,1.,1.,1.,
1.,1.,1.,1.,1.,1.,1.,1.,1.,1.,1.,1.,1.,1.,1.,1.,1.,1.,1.,1.,1.,1.,1.,1.,
1.,1.,1.,1.,1.,1.,1.,1.,1.,1.,1.,1.,1.,1.,1.,1.,1.,1.,1.,1.,1.,1.,1.,1.,
1.,1.,1.,1.,1.,1.,1.,1.,1.,1.))
REPRESENTATION_ITEM('')
);
#492=(
BOUNDED_CURVE()
B_SPLINE_CURVE(5,(#92653,#92654,#92655,#92656,#92657,#92658,#92659,#92660,
#92661,#92662,#92663,#92664,#92665,#92666,#92667,#92668,#92669,#92670,#92671,
#92672,#92673,#92674,#92675,#92676,#92677,#92678,#92679,#92680,#92681,#92682,
#92683,#92684,#92685,#92686,#92687,#92688,#92689,#92690,#92691,#92692,#92693,
#92694,#92695,#92696,#92697,#92698,#92699,#92700,#92701,#92702,#92703,#92704,
#92705,#92706,#92707,#92708,#92709,#92710,#92711,#92712,#92713,#92714,#92715,
#92716,#92717,#92718,#92719,#92720,#92721,#92722,#92723,#92724,#92725,#92726,
#92727,#92728,#92729,#92730,#92731,#92732,#92733,#92734,#92735,#92736,#92737,
#92738,#92739,#92740,#92741,#92742,#92743,#92744,#92745,#92746,#92747,#92748,
#92749,#92750,#92751,#92752,#92753,#92754,#92755,#92756,#92757,#92758,#92759,
#92760,#92761,#92762,#92763,#92764,#92765,#92766,#92767,#92768,#92769,#92770,
#92771,#92772,#92773,#92774,#92775,#92776,#92777,#92778,#92779,#92780,#92781,
#92782,#92783,#92784,#92785,#92786,#92787,#92788,#92789,#92790,#92791,#92792,
#92793,#92794,#92795,#92796,#92797,#92798,#92799,#92800,#92801,#92802,#92803,
#92804,#92805,#92806,#92807,#92808,#92809,#92810,#92811,#92812,#92813,#92814,
#92815,#92816,#92817,#92818,#92819,#92820,#92821,#92822,#92823,#92824,#92825,
#92826,#92827,#92828,#92829,#92830,#92831,#92832,#92833,#92834,#92835,#92836,
#92837,#92838,#92839,#92840,#92841,#92842,#92843,#92844,#92845,#92846),
 .UNSPECIFIED.,.F.,.F.)
B_SPLINE_CURVE_WITH_KNOTS((6,1,1,1,1,1,1,1,1,1,1,1,1,1,1,1,1,1,1,1,1,1,
1,1,1,1,1,1,1,1,1,1,1,1,1,1,1,1,1,1,1,1,1,1,1,1,1,1,1,1,1,1,1,1,1,1,1,1,
1,1,1,1,1,1,1,1,1,1,1,1,1,1,1,1,1,1,1,1,1,1,1,1,1,1,1,1,1,1,1,1,1,1,1,1,
1,1,1,1,1,1,1,1,1,1,1,1,1,1,1,1,1,1,1,1,1,1,1,1,1,1,1,1,1,1,1,1,1,1,1,1,
1,1,1,1,1,1,1,1,1,1,1,1,1,1,1,1,1,1,1,1,1,1,1,1,1,1,1,1,1,1,1,1,1,1,1,1,
1,1,1,1,1,1,1,1,1,1,1,1,1,1,1,1,1,1,1,1,1,1,1,6),(-0.941429844431541,-0.940000000000001,
-0.935000000000001,-0.930000000000001,-0.925000000000001,-0.920000000000001,
-0.915000000000001,-0.910000000000001,-0.905000000000001,-0.900000000000001,
-0.895000000000001,-0.890000000000001,-0.885000000000001,-0.880000000000001,
-0.875000000000001,-0.870000000000001,-0.865000000000001,-0.860000000000001,
-0.855000000000001,-0.850000000000001,-0.845000000000001,-0.840000000000001,
-0.835000000000001,-0.830000000000001,-0.825000000000001,-0.820000000000001,
-0.815000000000001,-0.810000000000001,-0.805000000000001,-0.800000000000001,
-0.795000000000001,-0.790000000000001,-0.785000000000001,-0.780000000000001,
-0.775000000000001,-0.770000000000001,-0.765000000000001,-0.760000000000001,
-0.755000000000001,-0.750000000000001,-0.745000000000001,-0.740000000000001,
-0.735000000000001,-0.730000000000001,-0.725000000000001,-0.720000000000001,
-0.715000000000001,-0.710000000000001,-0.705000000000001,-0.700000000000001,
-0.695000000000001,-0.690000000000001,-0.685,-0.68,-0.675,-0.67,-0.665,
-0.66,-0.655,-0.65,-0.645,-0.64,-0.635,-0.63,-0.625,-0.62,-0.615,-0.61,
-0.605,-0.6,-0.595,-0.59,-0.585,-0.58,-0.575,-0.57,-0.565,-0.56,-0.555,
-0.55,-0.545,-0.54,-0.535,-0.53,-0.525,-0.52,-0.515,-0.51,-0.505,-0.5,-0.495,
-0.49,-0.485,-0.48,-0.475,-0.47,-0.465,-0.46,-0.455,-0.45,-0.445,-0.44,
-0.435,-0.43,-0.425,-0.42,-0.415,-0.41,-0.405,-0.4,-0.395,-0.39,-0.385,
-0.38,-0.375,-0.37,-0.365,-0.36,-0.355,-0.35,-0.345,-0.34,-0.335,-0.33,
-0.325,-0.32,-0.315,-0.31,-0.305,-0.3,-0.295,-0.29,-0.285,-0.28,-0.275,
-0.27,-0.265,-0.26,-0.255,-0.25,-0.245,-0.24,-0.235,-0.23,-0.225,-0.22,
-0.215,-0.21,-0.205,-0.2,-0.195,-0.19,-0.185,-0.18,-0.175,-0.17,-0.165,
-0.16,-0.155,-0.15,-0.145,-0.14,-0.135,-0.13,-0.125,-0.12,-0.115,-0.11,
-0.105,-0.1,-0.095,-0.09,-0.085,-0.08,-0.075,-0.07,-0.065,-0.06,-0.055,
-0.05,-0.045,-0.04,-0.035,-0.03,-0.025,-0.02,-0.015,-0.01,-0.005,0.),
 .UNSPECIFIED.)
CURVE()
GEOMETRIC_REPRESENTATION_ITEM()
RATIONAL_B_SPLINE_CURVE((1.,1.,1.,1.,1.,1.,1.,1.,1.,1.,1.,1.,1.,1.,1.,1.,
1.,1.,1.,1.,1.,1.,1.,1.,1.,1.,1.,1.,1.,1.,1.,1.,1.,1.,1.,1.,1.,1.,1.,1.,
1.,1.,1.,1.,1.,1.,1.,1.,1.,1.,1.,1.,1.,1.,1.,1.,1.,1.,1.,1.,1.,1.,1.,1.,
1.,1.,1.,1.,1.,1.,1.,1.,1.,1.,1.,1.,1.,1.,1.,1.,1.,1.,1.,1.,1.,1.,1.,1.,
1.,1.,1.,1.,1.,1.,1.,1.,1.,1.,1.,1.,1.,1.,1.,1.,1.,1.,1.,1.,1.,1.,1.,1.,
1.,1.,1.,1.,1.,1.,1.,1.,1.,1.,1.,1.,1.,1.,1.,1.,1.,1.,1.,1.,1.,1.,1.,1.,
1.,1.,1.,1.,1.,1.,1.,1.,1.,1.,1.,1.,1.,1.,1.,1.,1.,1.,1.,1.,1.,1.,1.,1.,
1.,1.,1.,1.,1.,1.,1.,1.,1.,1.,1.,1.,1.,1.,1.,1.,1.,1.,1.,1.,1.,1.,1.,1.,
1.,1.,1.,1.,1.,1.,1.,1.,1.,1.))
REPRESENTATION_ITEM('')
);
#493=(
BOUNDED_CURVE()
B_SPLINE_CURVE(5,(#93353,#93354,#93355,#93356,#93357,#93358,#93359,#93360,
#93361,#93362,#93363,#93364,#93365,#93366,#93367,#93368,#93369,#93370,#93371,
#93372,#93373,#93374,#93375,#93376,#93377,#93378,#93379,#93380,#93381,#93382,
#93383,#93384,#93385,#93386,#93387,#93388,#93389,#93390,#93391,#93392,#93393,
#93394,#93395,#93396,#93397,#93398,#93399,#93400,#93401,#93402,#93403,#93404,
#93405,#93406,#93407,#93408,#93409,#93410,#93411,#93412,#93413,#93414,#93415,
#93416,#93417,#93418,#93419,#93420,#93421,#93422,#93423,#93424,#93425,#93426,
#93427,#93428,#93429,#93430,#93431,#93432,#93433,#93434,#93435,#93436,#93437,
#93438,#93439,#93440,#93441,#93442,#93443,#93444,#93445,#93446,#93447,#93448,
#93449,#93450,#93451,#93452,#93453,#93454,#93455,#93456,#93457,#93458,#93459,
#93460,#93461,#93462,#93463,#93464,#93465,#93466,#93467,#93468,#93469,#93470,
#93471,#93472,#93473,#93474,#93475,#93476,#93477,#93478,#93479,#93480,#93481,
#93482,#93483,#93484,#93485,#93486,#93487,#93488,#93489,#93490,#93491,#93492,
#93493,#93494,#93495,#93496,#93497,#93498,#93499,#93500,#93501,#93502,#93503,
#93504,#93505,#93506,#93507,#93508,#93509,#93510,#93511,#93512,#93513,#93514,
#93515,#93516,#93517,#93518,#93519,#93520,#93521,#93522,#93523,#93524,#93525,
#93526,#93527,#93528,#93529,#93530,#93531,#93532,#93533,#93534,#93535,#93536,
#93537,#93538,#93539,#93540,#93541,#93542,#93543,#93544,#93545,#93546),
 .UNSPECIFIED.,.F.,.F.)
B_SPLINE_CURVE_WITH_KNOTS((6,1,1,1,1,1,1,1,1,1,1,1,1,1,1,1,1,1,1,1,1,1,
1,1,1,1,1,1,1,1,1,1,1,1,1,1,1,1,1,1,1,1,1,1,1,1,1,1,1,1,1,1,1,1,1,1,1,1,
1,1,1,1,1,1,1,1,1,1,1,1,1,1,1,1,1,1,1,1,1,1,1,1,1,1,1,1,1,1,1,1,1,1,1,1,
1,1,1,1,1,1,1,1,1,1,1,1,1,1,1,1,1,1,1,1,1,1,1,1,1,1,1,1,1,1,1,1,1,1,1,1,
1,1,1,1,1,1,1,1,1,1,1,1,1,1,1,1,1,1,1,1,1,1,1,1,1,1,1,1,1,1,1,1,1,1,1,1,
1,1,1,1,1,1,1,1,1,1,1,1,1,1,1,1,1,1,1,1,1,1,1,6),(0.,0.005,0.01,0.015,0.02,
0.025,0.03,0.035,0.04,0.045,0.05,0.055,0.06,0.065,0.07,0.075,0.08,0.085,
0.09,0.095,0.1,0.105,0.11,0.115,0.12,0.125,0.13,0.135,0.14,0.145,0.15,0.155,
0.16,0.165,0.17,0.175,0.18,0.185,0.19,0.195,0.2,0.205,0.21,0.215,0.22,0.225,
0.23,0.235,0.24,0.245,0.25,0.255,0.26,0.265,0.27,0.275,0.28,0.285,0.29,
0.295,0.3,0.305,0.31,0.315,0.32,0.325,0.33,0.335,0.34,0.345,0.35,0.355,
0.36,0.365,0.37,0.375,0.38,0.385,0.39,0.395,0.4,0.405,0.41,0.415,0.42,0.425,
0.43,0.435,0.44,0.445,0.45,0.455,0.46,0.465,0.47,0.475,0.48,0.485,0.49,
0.495,0.5,0.505,0.51,0.515,0.52,0.525,0.53,0.535,0.54,0.545,0.55,0.555,
0.56,0.565,0.57,0.575,0.58,0.585,0.59,0.595,0.6,0.605,0.61,0.615,0.62,0.625,
0.63,0.635,0.64,0.645,0.65,0.655,0.66,0.665,0.67,0.675,0.68,0.685,0.690000000000001,
0.695000000000001,0.700000000000001,0.705000000000001,0.710000000000001,
0.715000000000001,0.720000000000001,0.725000000000001,0.730000000000001,
0.735000000000001,0.740000000000001,0.745000000000001,0.750000000000001,
0.755000000000001,0.760000000000001,0.765000000000001,0.770000000000001,
0.775000000000001,0.780000000000001,0.785000000000001,0.790000000000001,
0.795000000000001,0.800000000000001,0.805000000000001,0.810000000000001,
0.815000000000001,0.820000000000001,0.825000000000001,0.830000000000001,
0.835000000000001,0.840000000000001,0.845000000000001,0.850000000000001,
0.855000000000001,0.860000000000001,0.865000000000001,0.870000000000001,
0.875000000000001,0.880000000000001,0.885000000000001,0.890000000000001,
0.895000000000001,0.900000000000001,0.905000000000001,0.910000000000001,
0.915000000000001,0.920000000000001,0.925000000000001,0.930000000000001,
0.935000000000001,0.940000000000001,0.941429844431519),.UNSPECIFIED.)
CURVE()
GEOMETRIC_REPRESENTATION_ITEM()
RATIONAL_B_SPLINE_CURVE((1.,1.,1.,1.,1.,1.,1.,1.,1.,1.,1.,1.,1.,1.,1.,1.,
1.,1.,1.,1.,1.,1.,1.,1.,1.,1.,1.,1.,1.,1.,1.,1.,1.,1.,1.,1.,1.,1.,1.,1.,
1.,1.,1.,1.,1.,1.,1.,1.,1.,1.,1.,1.,1.,1.,1.,1.,1.,1.,1.,1.,1.,1.,1.,1.,
1.,1.,1.,1.,1.,1.,1.,1.,1.,1.,1.,1.,1.,1.,1.,1.,1.,1.,1.,1.,1.,1.,1.,1.,
1.,1.,1.,1.,1.,1.,1.,1.,1.,1.,1.,1.,1.,1.,1.,1.,1.,1.,1.,1.,1.,1.,1.,1.,
1.,1.,1.,1.,1.,1.,1.,1.,1.,1.,1.,1.,1.,1.,1.,1.,1.,1.,1.,1.,1.,1.,1.,1.,
1.,1.,1.,1.,1.,1.,1.,1.,1.,1.,1.,1.,1.,1.,1.,1.,1.,1.,1.,1.,1.,1.,1.,1.,
1.,1.,1.,1.,1.,1.,1.,1.,1.,1.,1.,1.,1.,1.,1.,1.,1.,1.,1.,1.,1.,1.,1.,1.,
1.,1.,1.,1.,1.,1.,1.,1.,1.,1.))
REPRESENTATION_ITEM('')
);
#494=(
BOUNDED_CURVE()
B_SPLINE_CURVE(5,(#93549,#93550,#93551,#93552,#93553,#93554,#93555,#93556,
#93557,#93558,#93559,#93560,#93561,#93562,#93563,#93564,#93565,#93566,#93567,
#93568,#93569,#93570,#93571,#93572,#93573,#93574,#93575,#93576,#93577,#93578,
#93579,#93580,#93581,#93582,#93583,#93584,#93585,#93586,#93587,#93588,#93589,
#93590,#93591,#93592,#93593,#93594,#93595,#93596,#93597,#93598,#93599,#93600,
#93601,#93602,#93603,#93604,#93605,#93606,#93607,#93608,#93609,#93610,#93611,
#93612,#93613,#93614,#93615,#93616,#93617,#93618,#93619,#93620,#93621,#93622,
#93623,#93624,#93625,#93626,#93627,#93628,#93629,#93630,#93631,#93632,#93633,
#93634,#93635,#93636,#93637,#93638,#93639,#93640,#93641,#93642,#93643,#93644,
#93645,#93646,#93647,#93648,#93649,#93650,#93651,#93652,#93653,#93654,#93655,
#93656,#93657,#93658,#93659,#93660,#93661,#93662,#93663,#93664,#93665,#93666,
#93667,#93668,#93669,#93670,#93671,#93672,#93673,#93674,#93675,#93676,#93677,
#93678,#93679,#93680,#93681,#93682,#93683,#93684,#93685,#93686,#93687,#93688,
#93689,#93690,#93691,#93692,#93693,#93694,#93695,#93696,#93697,#93698,#93699,
#93700,#93701,#93702,#93703,#93704,#93705,#93706,#93707,#93708,#93709,#93710,
#93711,#93712,#93713,#93714,#93715,#93716,#93717,#93718,#93719,#93720,#93721,
#93722,#93723,#93724,#93725,#93726,#93727,#93728,#93729,#93730,#93731,#93732,
#93733,#93734,#93735,#93736,#93737,#93738,#93739,#93740,#93741,#93742),
 .UNSPECIFIED.,.F.,.F.)
B_SPLINE_CURVE_WITH_KNOTS((6,1,1,1,1,1,1,1,1,1,1,1,1,1,1,1,1,1,1,1,1,1,
1,1,1,1,1,1,1,1,1,1,1,1,1,1,1,1,1,1,1,1,1,1,1,1,1,1,1,1,1,1,1,1,1,1,1,1,
1,1,1,1,1,1,1,1,1,1,1,1,1,1,1,1,1,1,1,1,1,1,1,1,1,1,1,1,1,1,1,1,1,1,1,1,
1,1,1,1,1,1,1,1,1,1,1,1,1,1,1,1,1,1,1,1,1,1,1,1,1,1,1,1,1,1,1,1,1,1,1,1,
1,1,1,1,1,1,1,1,1,1,1,1,1,1,1,1,1,1,1,1,1,1,1,1,1,1,1,1,1,1,1,1,1,1,1,1,
1,1,1,1,1,1,1,1,1,1,1,1,1,1,1,1,1,1,1,1,1,1,1,6),(-0.941429844431519,-0.940000000000001,
-0.935000000000001,-0.930000000000001,-0.925000000000001,-0.920000000000001,
-0.915000000000001,-0.910000000000001,-0.905000000000001,-0.900000000000001,
-0.895000000000001,-0.890000000000001,-0.885000000000001,-0.880000000000001,
-0.875000000000001,-0.870000000000001,-0.865000000000001,-0.860000000000001,
-0.855000000000001,-0.850000000000001,-0.845000000000001,-0.840000000000001,
-0.835000000000001,-0.830000000000001,-0.825000000000001,-0.820000000000001,
-0.815000000000001,-0.810000000000001,-0.805000000000001,-0.800000000000001,
-0.795000000000001,-0.790000000000001,-0.785000000000001,-0.780000000000001,
-0.775000000000001,-0.770000000000001,-0.765000000000001,-0.760000000000001,
-0.755000000000001,-0.750000000000001,-0.745000000000001,-0.740000000000001,
-0.735000000000001,-0.730000000000001,-0.725000000000001,-0.720000000000001,
-0.715000000000001,-0.710000000000001,-0.705000000000001,-0.700000000000001,
-0.695000000000001,-0.690000000000001,-0.685,-0.68,-0.675,-0.67,-0.665,
-0.66,-0.655,-0.65,-0.645,-0.64,-0.635,-0.63,-0.625,-0.62,-0.615,-0.61,
-0.605,-0.6,-0.595,-0.59,-0.585,-0.58,-0.575,-0.57,-0.565,-0.56,-0.555,
-0.55,-0.545,-0.54,-0.535,-0.53,-0.525,-0.52,-0.515,-0.51,-0.505,-0.5,-0.495,
-0.49,-0.485,-0.48,-0.475,-0.47,-0.465,-0.46,-0.455,-0.45,-0.445,-0.44,
-0.435,-0.43,-0.425,-0.42,-0.415,-0.41,-0.405,-0.4,-0.395,-0.39,-0.385,
-0.38,-0.375,-0.37,-0.365,-0.36,-0.355,-0.35,-0.345,-0.34,-0.335,-0.33,
-0.325,-0.32,-0.315,-0.31,-0.305,-0.3,-0.295,-0.29,-0.285,-0.28,-0.275,
-0.27,-0.265,-0.26,-0.255,-0.25,-0.245,-0.24,-0.235,-0.23,-0.225,-0.22,
-0.215,-0.21,-0.205,-0.2,-0.195,-0.19,-0.185,-0.18,-0.175,-0.17,-0.165,
-0.16,-0.155,-0.15,-0.145,-0.14,-0.135,-0.13,-0.125,-0.12,-0.115,-0.11,
-0.105,-0.1,-0.095,-0.09,-0.085,-0.08,-0.075,-0.07,-0.065,-0.06,-0.055,
-0.05,-0.045,-0.04,-0.035,-0.03,-0.025,-0.02,-0.015,-0.01,-0.005,0.),
 .UNSPECIFIED.)
CURVE()
GEOMETRIC_REPRESENTATION_ITEM()
RATIONAL_B_SPLINE_CURVE((1.,1.,1.,1.,1.,1.,1.,1.,1.,1.,1.,1.,1.,1.,1.,1.,
1.,1.,1.,1.,1.,1.,1.,1.,1.,1.,1.,1.,1.,1.,1.,1.,1.,1.,1.,1.,1.,1.,1.,1.,
1.,1.,1.,1.,1.,1.,1.,1.,1.,1.,1.,1.,1.,1.,1.,1.,1.,1.,1.,1.,1.,1.,1.,1.,
1.,1.,1.,1.,1.,1.,1.,1.,1.,1.,1.,1.,1.,1.,1.,1.,1.,1.,1.,1.,1.,1.,1.,1.,
1.,1.,1.,1.,1.,1.,1.,1.,1.,1.,1.,1.,1.,1.,1.,1.,1.,1.,1.,1.,1.,1.,1.,1.,
1.,1.,1.,1.,1.,1.,1.,1.,1.,1.,1.,1.,1.,1.,1.,1.,1.,1.,1.,1.,1.,1.,1.,1.,
1.,1.,1.,1.,1.,1.,1.,1.,1.,1.,1.,1.,1.,1.,1.,1.,1.,1.,1.,1.,1.,1.,1.,1.,
1.,1.,1.,1.,1.,1.,1.,1.,1.,1.,1.,1.,1.,1.,1.,1.,1.,1.,1.,1.,1.,1.,1.,1.,
1.,1.,1.,1.,1.,1.,1.,1.,1.,1.))
REPRESENTATION_ITEM('')
);
#495=(
BOUNDED_CURVE()
B_SPLINE_CURVE(5,(#94249,#94250,#94251,#94252,#94253,#94254,#94255,#94256,
#94257,#94258,#94259,#94260,#94261,#94262,#94263,#94264,#94265,#94266,#94267,
#94268,#94269,#94270,#94271,#94272,#94273,#94274,#94275,#94276,#94277,#94278,
#94279,#94280,#94281,#94282,#94283,#94284,#94285,#94286,#94287,#94288,#94289,
#94290,#94291,#94292,#94293,#94294,#94295,#94296,#94297,#94298,#94299,#94300,
#94301,#94302,#94303,#94304,#94305,#94306,#94307,#94308,#94309,#94310,#94311,
#94312,#94313,#94314,#94315,#94316,#94317,#94318,#94319,#94320,#94321,#94322,
#94323,#94324,#94325,#94326,#94327,#94328,#94329,#94330,#94331,#94332,#94333,
#94334,#94335,#94336,#94337,#94338,#94339,#94340,#94341,#94342,#94343,#94344,
#94345,#94346,#94347,#94348,#94349,#94350,#94351,#94352,#94353,#94354,#94355,
#94356,#94357,#94358,#94359,#94360,#94361,#94362,#94363,#94364,#94365,#94366,
#94367,#94368,#94369,#94370,#94371,#94372,#94373,#94374,#94375,#94376,#94377,
#94378,#94379,#94380,#94381,#94382,#94383,#94384,#94385,#94386,#94387,#94388,
#94389,#94390,#94391,#94392,#94393,#94394,#94395,#94396,#94397,#94398,#94399,
#94400,#94401,#94402,#94403,#94404,#94405,#94406,#94407,#94408,#94409,#94410,
#94411,#94412,#94413,#94414,#94415,#94416,#94417,#94418,#94419,#94420,#94421,
#94422,#94423,#94424,#94425,#94426,#94427,#94428,#94429,#94430,#94431,#94432,
#94433,#94434,#94435,#94436,#94437,#94438,#94439,#94440,#94441,#94442),
 .UNSPECIFIED.,.F.,.F.)
B_SPLINE_CURVE_WITH_KNOTS((6,1,1,1,1,1,1,1,1,1,1,1,1,1,1,1,1,1,1,1,1,1,
1,1,1,1,1,1,1,1,1,1,1,1,1,1,1,1,1,1,1,1,1,1,1,1,1,1,1,1,1,1,1,1,1,1,1,1,
1,1,1,1,1,1,1,1,1,1,1,1,1,1,1,1,1,1,1,1,1,1,1,1,1,1,1,1,1,1,1,1,1,1,1,1,
1,1,1,1,1,1,1,1,1,1,1,1,1,1,1,1,1,1,1,1,1,1,1,1,1,1,1,1,1,1,1,1,1,1,1,1,
1,1,1,1,1,1,1,1,1,1,1,1,1,1,1,1,1,1,1,1,1,1,1,1,1,1,1,1,1,1,1,1,1,1,1,1,
1,1,1,1,1,1,1,1,1,1,1,1,1,1,1,1,1,1,1,1,1,1,1,6),(0.,0.005,0.01,0.015,0.02,
0.025,0.03,0.035,0.04,0.045,0.05,0.055,0.06,0.065,0.07,0.075,0.08,0.085,
0.09,0.095,0.1,0.105,0.11,0.115,0.12,0.125,0.13,0.135,0.14,0.145,0.15,0.155,
0.16,0.165,0.17,0.175,0.18,0.185,0.19,0.195,0.2,0.205,0.21,0.215,0.22,0.225,
0.23,0.235,0.24,0.245,0.25,0.255,0.26,0.265,0.27,0.275,0.28,0.285,0.29,
0.295,0.3,0.305,0.31,0.315,0.32,0.325,0.33,0.335,0.34,0.345,0.35,0.355,
0.36,0.365,0.37,0.375,0.38,0.385,0.39,0.395,0.4,0.405,0.41,0.415,0.42,0.425,
0.43,0.435,0.44,0.445,0.45,0.455,0.46,0.465,0.47,0.475,0.48,0.485,0.49,
0.495,0.5,0.505,0.51,0.515,0.52,0.525,0.53,0.535,0.54,0.545,0.55,0.555,
0.56,0.565,0.57,0.575,0.58,0.585,0.59,0.595,0.6,0.605,0.61,0.615,0.62,0.625,
0.63,0.635,0.64,0.645,0.65,0.655,0.66,0.665,0.67,0.675,0.68,0.685,0.690000000000001,
0.695000000000001,0.700000000000001,0.705000000000001,0.710000000000001,
0.715000000000001,0.720000000000001,0.725000000000001,0.730000000000001,
0.735000000000001,0.740000000000001,0.745000000000001,0.750000000000001,
0.755000000000001,0.760000000000001,0.765000000000001,0.770000000000001,
0.775000000000001,0.780000000000001,0.785000000000001,0.790000000000001,
0.795000000000001,0.800000000000001,0.805000000000001,0.810000000000001,
0.815000000000001,0.820000000000001,0.825000000000001,0.830000000000001,
0.835000000000001,0.840000000000001,0.845000000000001,0.850000000000001,
0.855000000000001,0.860000000000001,0.865000000000001,0.870000000000001,
0.875000000000001,0.880000000000001,0.885000000000001,0.890000000000001,
0.895000000000001,0.900000000000001,0.905000000000001,0.910000000000001,
0.915000000000001,0.920000000000001,0.925000000000001,0.930000000000001,
0.935000000000001,0.940000000000001,0.94142984443127),.UNSPECIFIED.)
CURVE()
GEOMETRIC_REPRESENTATION_ITEM()
RATIONAL_B_SPLINE_CURVE((1.,1.,1.,1.,1.,1.,1.,1.,1.,1.,1.,1.,1.,1.,1.,1.,
1.,1.,1.,1.,1.,1.,1.,1.,1.,1.,1.,1.,1.,1.,1.,1.,1.,1.,1.,1.,1.,1.,1.,1.,
1.,1.,1.,1.,1.,1.,1.,1.,1.,1.,1.,1.,1.,1.,1.,1.,1.,1.,1.,1.,1.,1.,1.,1.,
1.,1.,1.,1.,1.,1.,1.,1.,1.,1.,1.,1.,1.,1.,1.,1.,1.,1.,1.,1.,1.,1.,1.,1.,
1.,1.,1.,1.,1.,1.,1.,1.,1.,1.,1.,1.,1.,1.,1.,1.,1.,1.,1.,1.,1.,1.,1.,1.,
1.,1.,1.,1.,1.,1.,1.,1.,1.,1.,1.,1.,1.,1.,1.,1.,1.,1.,1.,1.,1.,1.,1.,1.,
1.,1.,1.,1.,1.,1.,1.,1.,1.,1.,1.,1.,1.,1.,1.,1.,1.,1.,1.,1.,1.,1.,1.,1.,
1.,1.,1.,1.,1.,1.,1.,1.,1.,1.,1.,1.,1.,1.,1.,1.,1.,1.,1.,1.,1.,1.,1.,1.,
1.,1.,1.,1.,1.,1.,1.,1.,1.,1.))
REPRESENTATION_ITEM('')
);
#496=(
BOUNDED_CURVE()
B_SPLINE_CURVE(5,(#94445,#94446,#94447,#94448,#94449,#94450,#94451,#94452,
#94453,#94454,#94455,#94456,#94457,#94458,#94459,#94460,#94461,#94462,#94463,
#94464,#94465,#94466,#94467,#94468,#94469,#94470,#94471,#94472,#94473,#94474,
#94475,#94476,#94477,#94478,#94479,#94480,#94481,#94482,#94483,#94484,#94485,
#94486,#94487,#94488,#94489,#94490,#94491,#94492,#94493,#94494,#94495,#94496,
#94497,#94498,#94499,#94500,#94501,#94502,#94503,#94504,#94505,#94506,#94507,
#94508,#94509,#94510,#94511,#94512,#94513,#94514,#94515,#94516,#94517,#94518,
#94519,#94520,#94521,#94522,#94523,#94524,#94525,#94526,#94527,#94528,#94529,
#94530,#94531,#94532,#94533,#94534,#94535,#94536,#94537,#94538,#94539,#94540,
#94541,#94542,#94543,#94544,#94545,#94546,#94547,#94548,#94549,#94550,#94551,
#94552,#94553,#94554,#94555,#94556,#94557,#94558,#94559,#94560,#94561,#94562,
#94563,#94564,#94565,#94566,#94567,#94568,#94569,#94570,#94571,#94572,#94573,
#94574,#94575,#94576,#94577,#94578,#94579,#94580,#94581,#94582,#94583,#94584,
#94585,#94586,#94587,#94588,#94589,#94590,#94591,#94592,#94593,#94594,#94595,
#94596,#94597,#94598,#94599,#94600,#94601,#94602,#94603,#94604,#94605,#94606,
#94607,#94608,#94609,#94610,#94611,#94612,#94613,#94614,#94615,#94616,#94617,
#94618,#94619,#94620,#94621,#94622,#94623,#94624,#94625,#94626,#94627,#94628,
#94629,#94630,#94631,#94632,#94633,#94634,#94635,#94636,#94637,#94638),
 .UNSPECIFIED.,.F.,.F.)
B_SPLINE_CURVE_WITH_KNOTS((6,1,1,1,1,1,1,1,1,1,1,1,1,1,1,1,1,1,1,1,1,1,
1,1,1,1,1,1,1,1,1,1,1,1,1,1,1,1,1,1,1,1,1,1,1,1,1,1,1,1,1,1,1,1,1,1,1,1,
1,1,1,1,1,1,1,1,1,1,1,1,1,1,1,1,1,1,1,1,1,1,1,1,1,1,1,1,1,1,1,1,1,1,1,1,
1,1,1,1,1,1,1,1,1,1,1,1,1,1,1,1,1,1,1,1,1,1,1,1,1,1,1,1,1,1,1,1,1,1,1,1,
1,1,1,1,1,1,1,1,1,1,1,1,1,1,1,1,1,1,1,1,1,1,1,1,1,1,1,1,1,1,1,1,1,1,1,1,
1,1,1,1,1,1,1,1,1,1,1,1,1,1,1,1,1,1,1,1,1,1,1,6),(-0.941429844431257,-0.940000000000001,
-0.935000000000001,-0.930000000000001,-0.925000000000001,-0.920000000000001,
-0.915000000000001,-0.910000000000001,-0.905000000000001,-0.900000000000001,
-0.895000000000001,-0.890000000000001,-0.885000000000001,-0.880000000000001,
-0.875000000000001,-0.870000000000001,-0.865000000000001,-0.860000000000001,
-0.855000000000001,-0.850000000000001,-0.845000000000001,-0.840000000000001,
-0.835000000000001,-0.830000000000001,-0.825000000000001,-0.820000000000001,
-0.815000000000001,-0.810000000000001,-0.805000000000001,-0.800000000000001,
-0.795000000000001,-0.790000000000001,-0.785000000000001,-0.780000000000001,
-0.775000000000001,-0.770000000000001,-0.765000000000001,-0.760000000000001,
-0.755000000000001,-0.750000000000001,-0.745000000000001,-0.740000000000001,
-0.735000000000001,-0.730000000000001,-0.725000000000001,-0.720000000000001,
-0.715000000000001,-0.710000000000001,-0.705000000000001,-0.700000000000001,
-0.695000000000001,-0.690000000000001,-0.685,-0.68,-0.675,-0.67,-0.665,
-0.66,-0.655,-0.65,-0.645,-0.64,-0.635,-0.63,-0.625,-0.62,-0.615,-0.61,
-0.605,-0.6,-0.595,-0.59,-0.585,-0.58,-0.575,-0.57,-0.565,-0.56,-0.555,
-0.55,-0.545,-0.54,-0.535,-0.53,-0.525,-0.52,-0.515,-0.51,-0.505,-0.5,-0.495,
-0.49,-0.485,-0.48,-0.475,-0.47,-0.465,-0.46,-0.455,-0.45,-0.445,-0.44,
-0.435,-0.43,-0.425,-0.42,-0.415,-0.41,-0.405,-0.4,-0.395,-0.39,-0.385,
-0.38,-0.375,-0.37,-0.365,-0.36,-0.355,-0.35,-0.345,-0.34,-0.335,-0.33,
-0.325,-0.32,-0.315,-0.31,-0.305,-0.3,-0.295,-0.29,-0.285,-0.28,-0.275,
-0.27,-0.265,-0.26,-0.255,-0.25,-0.245,-0.24,-0.235,-0.23,-0.225,-0.22,
-0.215,-0.21,-0.205,-0.2,-0.195,-0.19,-0.185,-0.18,-0.175,-0.17,-0.165,
-0.16,-0.155,-0.15,-0.145,-0.14,-0.135,-0.13,-0.125,-0.12,-0.115,-0.11,
-0.105,-0.1,-0.095,-0.09,-0.085,-0.08,-0.075,-0.07,-0.065,-0.06,-0.055,
-0.05,-0.045,-0.04,-0.035,-0.03,-0.025,-0.02,-0.015,-0.01,-0.005,0.),
 .UNSPECIFIED.)
CURVE()
GEOMETRIC_REPRESENTATION_ITEM()
RATIONAL_B_SPLINE_CURVE((1.,1.,1.,1.,1.,1.,1.,1.,1.,1.,1.,1.,1.,1.,1.,1.,
1.,1.,1.,1.,1.,1.,1.,1.,1.,1.,1.,1.,1.,1.,1.,1.,1.,1.,1.,1.,1.,1.,1.,1.,
1.,1.,1.,1.,1.,1.,1.,1.,1.,1.,1.,1.,1.,1.,1.,1.,1.,1.,1.,1.,1.,1.,1.,1.,
1.,1.,1.,1.,1.,1.,1.,1.,1.,1.,1.,1.,1.,1.,1.,1.,1.,1.,1.,1.,1.,1.,1.,1.,
1.,1.,1.,1.,1.,1.,1.,1.,1.,1.,1.,1.,1.,1.,1.,1.,1.,1.,1.,1.,1.,1.,1.,1.,
1.,1.,1.,1.,1.,1.,1.,1.,1.,1.,1.,1.,1.,1.,1.,1.,1.,1.,1.,1.,1.,1.,1.,1.,
1.,1.,1.,1.,1.,1.,1.,1.,1.,1.,1.,1.,1.,1.,1.,1.,1.,1.,1.,1.,1.,1.,1.,1.,
1.,1.,1.,1.,1.,1.,1.,1.,1.,1.,1.,1.,1.,1.,1.,1.,1.,1.,1.,1.,1.,1.,1.,1.,
1.,1.,1.,1.,1.,1.,1.,1.,1.,1.))
REPRESENTATION_ITEM('')
);
#497=(
BOUNDED_CURVE()
B_SPLINE_CURVE(5,(#95145,#95146,#95147,#95148,#95149,#95150,#95151,#95152,
#95153,#95154,#95155,#95156,#95157,#95158,#95159,#95160,#95161,#95162,#95163,
#95164,#95165,#95166,#95167,#95168,#95169,#95170,#95171,#95172,#95173,#95174,
#95175,#95176,#95177,#95178,#95179,#95180,#95181,#95182,#95183,#95184,#95185,
#95186,#95187,#95188,#95189,#95190,#95191,#95192,#95193,#95194,#95195,#95196,
#95197,#95198,#95199,#95200,#95201,#95202,#95203,#95204,#95205,#95206,#95207,
#95208,#95209,#95210,#95211,#95212,#95213,#95214,#95215,#95216,#95217,#95218,
#95219,#95220,#95221,#95222,#95223,#95224,#95225,#95226,#95227,#95228,#95229,
#95230,#95231,#95232,#95233,#95234,#95235,#95236,#95237,#95238,#95239,#95240,
#95241,#95242,#95243,#95244,#95245,#95246,#95247,#95248,#95249,#95250,#95251,
#95252,#95253,#95254,#95255,#95256,#95257,#95258,#95259,#95260,#95261,#95262,
#95263,#95264,#95265,#95266,#95267,#95268,#95269,#95270,#95271,#95272,#95273,
#95274,#95275,#95276,#95277,#95278,#95279,#95280,#95281,#95282,#95283,#95284,
#95285,#95286,#95287,#95288,#95289,#95290,#95291,#95292,#95293,#95294,#95295,
#95296,#95297,#95298,#95299,#95300,#95301,#95302,#95303,#95304,#95305,#95306,
#95307,#95308,#95309,#95310,#95311,#95312,#95313,#95314,#95315,#95316,#95317,
#95318,#95319,#95320,#95321,#95322,#95323,#95324,#95325,#95326,#95327,#95328,
#95329,#95330,#95331,#95332,#95333,#95334,#95335,#95336,#95337,#95338),
 .UNSPECIFIED.,.F.,.F.)
B_SPLINE_CURVE_WITH_KNOTS((6,1,1,1,1,1,1,1,1,1,1,1,1,1,1,1,1,1,1,1,1,1,
1,1,1,1,1,1,1,1,1,1,1,1,1,1,1,1,1,1,1,1,1,1,1,1,1,1,1,1,1,1,1,1,1,1,1,1,
1,1,1,1,1,1,1,1,1,1,1,1,1,1,1,1,1,1,1,1,1,1,1,1,1,1,1,1,1,1,1,1,1,1,1,1,
1,1,1,1,1,1,1,1,1,1,1,1,1,1,1,1,1,1,1,1,1,1,1,1,1,1,1,1,1,1,1,1,1,1,1,1,
1,1,1,1,1,1,1,1,1,1,1,1,1,1,1,1,1,1,1,1,1,1,1,1,1,1,1,1,1,1,1,1,1,1,1,1,
1,1,1,1,1,1,1,1,1,1,1,1,1,1,1,1,1,1,1,1,1,1,1,6),(0.,0.005,0.01,0.015,0.02,
0.025,0.03,0.035,0.04,0.045,0.05,0.055,0.06,0.065,0.07,0.075,0.08,0.085,
0.09,0.095,0.1,0.105,0.11,0.115,0.12,0.125,0.13,0.135,0.14,0.145,0.15,0.155,
0.16,0.165,0.17,0.175,0.18,0.185,0.19,0.195,0.2,0.205,0.21,0.215,0.22,0.225,
0.23,0.235,0.24,0.245,0.25,0.255,0.26,0.265,0.27,0.275,0.28,0.285,0.29,
0.295,0.3,0.305,0.31,0.315,0.32,0.325,0.33,0.335,0.34,0.345,0.35,0.355,
0.36,0.365,0.37,0.375,0.38,0.385,0.39,0.395,0.4,0.405,0.41,0.415,0.42,0.425,
0.43,0.435,0.44,0.445,0.45,0.455,0.46,0.465,0.47,0.475,0.48,0.485,0.49,
0.495,0.5,0.505,0.51,0.515,0.52,0.525,0.53,0.535,0.54,0.545,0.55,0.555,
0.56,0.565,0.57,0.575,0.58,0.585,0.59,0.595,0.6,0.605,0.61,0.615,0.62,0.625,
0.63,0.635,0.64,0.645,0.65,0.655,0.66,0.665,0.67,0.675,0.68,0.685,0.690000000000001,
0.695000000000001,0.700000000000001,0.705000000000001,0.710000000000001,
0.715000000000001,0.720000000000001,0.725000000000001,0.730000000000001,
0.735000000000001,0.740000000000001,0.745000000000001,0.750000000000001,
0.755000000000001,0.760000000000001,0.765000000000001,0.770000000000001,
0.775000000000001,0.780000000000001,0.785000000000001,0.790000000000001,
0.795000000000001,0.800000000000001,0.805000000000001,0.810000000000001,
0.815000000000001,0.820000000000001,0.825000000000001,0.830000000000001,
0.835000000000001,0.840000000000001,0.845000000000001,0.850000000000001,
0.855000000000001,0.860000000000001,0.865000000000001,0.870000000000001,
0.875000000000001,0.880000000000001,0.885000000000001,0.890000000000001,
0.895000000000001,0.900000000000001,0.905000000000001,0.910000000000001,
0.915000000000001,0.920000000000001,0.925000000000001,0.930000000000001,
0.935000000000001,0.940000000000001,0.9414298444314),.UNSPECIFIED.)
CURVE()
GEOMETRIC_REPRESENTATION_ITEM()
RATIONAL_B_SPLINE_CURVE((1.,1.,1.,1.,1.,1.,1.,1.,1.,1.,1.,1.,1.,1.,1.,1.,
1.,1.,1.,1.,1.,1.,1.,1.,1.,1.,1.,1.,1.,1.,1.,1.,1.,1.,1.,1.,1.,1.,1.,1.,
1.,1.,1.,1.,1.,1.,1.,1.,1.,1.,1.,1.,1.,1.,1.,1.,1.,1.,1.,1.,1.,1.,1.,1.,
1.,1.,1.,1.,1.,1.,1.,1.,1.,1.,1.,1.,1.,1.,1.,1.,1.,1.,1.,1.,1.,1.,1.,1.,
1.,1.,1.,1.,1.,1.,1.,1.,1.,1.,1.,1.,1.,1.,1.,1.,1.,1.,1.,1.,1.,1.,1.,1.,
1.,1.,1.,1.,1.,1.,1.,1.,1.,1.,1.,1.,1.,1.,1.,1.,1.,1.,1.,1.,1.,1.,1.,1.,
1.,1.,1.,1.,1.,1.,1.,1.,1.,1.,1.,1.,1.,1.,1.,1.,1.,1.,1.,1.,1.,1.,1.,1.,
1.,1.,1.,1.,1.,1.,1.,1.,1.,1.,1.,1.,1.,1.,1.,1.,1.,1.,1.,1.,1.,1.,1.,1.,
1.,1.,1.,1.,1.,1.,1.,1.,1.,1.))
REPRESENTATION_ITEM('')
);
#498=(
BOUNDED_CURVE()
B_SPLINE_CURVE(5,(#95341,#95342,#95343,#95344,#95345,#95346,#95347,#95348,
#95349,#95350,#95351,#95352,#95353,#95354,#95355,#95356,#95357,#95358,#95359,
#95360,#95361,#95362,#95363,#95364,#95365,#95366,#95367,#95368,#95369,#95370,
#95371,#95372,#95373,#95374,#95375,#95376,#95377,#95378,#95379,#95380,#95381,
#95382,#95383,#95384,#95385,#95386,#95387,#95388,#95389,#95390,#95391,#95392,
#95393,#95394,#95395,#95396,#95397,#95398,#95399,#95400,#95401,#95402,#95403,
#95404,#95405,#95406,#95407,#95408,#95409,#95410,#95411,#95412,#95413,#95414,
#95415,#95416,#95417,#95418,#95419,#95420,#95421,#95422,#95423,#95424,#95425,
#95426,#95427,#95428,#95429,#95430,#95431,#95432,#95433,#95434,#95435,#95436,
#95437,#95438,#95439,#95440,#95441,#95442,#95443,#95444,#95445,#95446,#95447,
#95448,#95449,#95450,#95451,#95452,#95453,#95454,#95455,#95456,#95457,#95458,
#95459,#95460,#95461,#95462,#95463,#95464,#95465,#95466,#95467,#95468,#95469,
#95470,#95471,#95472,#95473,#95474,#95475,#95476,#95477,#95478,#95479,#95480,
#95481,#95482,#95483,#95484,#95485,#95486,#95487,#95488,#95489,#95490,#95491,
#95492,#95493,#95494,#95495,#95496,#95497,#95498,#95499,#95500,#95501,#95502,
#95503,#95504,#95505,#95506,#95507,#95508,#95509,#95510,#95511,#95512,#95513,
#95514,#95515,#95516,#95517,#95518,#95519,#95520,#95521,#95522,#95523,#95524,
#95525,#95526,#95527,#95528,#95529,#95530,#95531,#95532,#95533,#95534),
 .UNSPECIFIED.,.F.,.F.)
B_SPLINE_CURVE_WITH_KNOTS((6,1,1,1,1,1,1,1,1,1,1,1,1,1,1,1,1,1,1,1,1,1,
1,1,1,1,1,1,1,1,1,1,1,1,1,1,1,1,1,1,1,1,1,1,1,1,1,1,1,1,1,1,1,1,1,1,1,1,
1,1,1,1,1,1,1,1,1,1,1,1,1,1,1,1,1,1,1,1,1,1,1,1,1,1,1,1,1,1,1,1,1,1,1,1,
1,1,1,1,1,1,1,1,1,1,1,1,1,1,1,1,1,1,1,1,1,1,1,1,1,1,1,1,1,1,1,1,1,1,1,1,
1,1,1,1,1,1,1,1,1,1,1,1,1,1,1,1,1,1,1,1,1,1,1,1,1,1,1,1,1,1,1,1,1,1,1,1,
1,1,1,1,1,1,1,1,1,1,1,1,1,1,1,1,1,1,1,1,1,1,1,6),(-0.941429844431388,-0.940000000000001,
-0.935000000000001,-0.930000000000001,-0.925000000000001,-0.920000000000001,
-0.915000000000001,-0.910000000000001,-0.905000000000001,-0.900000000000001,
-0.895000000000001,-0.890000000000001,-0.885000000000001,-0.880000000000001,
-0.875000000000001,-0.870000000000001,-0.865000000000001,-0.860000000000001,
-0.855000000000001,-0.850000000000001,-0.845000000000001,-0.840000000000001,
-0.835000000000001,-0.830000000000001,-0.825000000000001,-0.820000000000001,
-0.815000000000001,-0.810000000000001,-0.805000000000001,-0.800000000000001,
-0.795000000000001,-0.790000000000001,-0.785000000000001,-0.780000000000001,
-0.775000000000001,-0.770000000000001,-0.765000000000001,-0.760000000000001,
-0.755000000000001,-0.750000000000001,-0.745000000000001,-0.740000000000001,
-0.735000000000001,-0.730000000000001,-0.725000000000001,-0.720000000000001,
-0.715000000000001,-0.710000000000001,-0.705000000000001,-0.700000000000001,
-0.695000000000001,-0.690000000000001,-0.685,-0.68,-0.675,-0.67,-0.665,
-0.66,-0.655,-0.65,-0.645,-0.64,-0.635,-0.63,-0.625,-0.62,-0.615,-0.61,
-0.605,-0.6,-0.595,-0.59,-0.585,-0.58,-0.575,-0.57,-0.565,-0.56,-0.555,
-0.55,-0.545,-0.54,-0.535,-0.53,-0.525,-0.52,-0.515,-0.51,-0.505,-0.5,-0.495,
-0.49,-0.485,-0.48,-0.475,-0.47,-0.465,-0.46,-0.455,-0.45,-0.445,-0.44,
-0.435,-0.43,-0.425,-0.42,-0.415,-0.41,-0.405,-0.4,-0.395,-0.39,-0.385,
-0.38,-0.375,-0.37,-0.365,-0.36,-0.355,-0.35,-0.345,-0.34,-0.335,-0.33,
-0.325,-0.32,-0.315,-0.31,-0.305,-0.3,-0.295,-0.29,-0.285,-0.28,-0.275,
-0.27,-0.265,-0.26,-0.255,-0.25,-0.245,-0.24,-0.235,-0.23,-0.225,-0.22,
-0.215,-0.21,-0.205,-0.2,-0.195,-0.19,-0.185,-0.18,-0.175,-0.17,-0.165,
-0.16,-0.155,-0.15,-0.145,-0.14,-0.135,-0.13,-0.125,-0.12,-0.115,-0.11,
-0.105,-0.1,-0.095,-0.09,-0.085,-0.08,-0.075,-0.07,-0.065,-0.06,-0.055,
-0.05,-0.045,-0.04,-0.035,-0.03,-0.025,-0.02,-0.015,-0.01,-0.005,0.),
 .UNSPECIFIED.)
CURVE()
GEOMETRIC_REPRESENTATION_ITEM()
RATIONAL_B_SPLINE_CURVE((1.,1.,1.,1.,1.,1.,1.,1.,1.,1.,1.,1.,1.,1.,1.,1.,
1.,1.,1.,1.,1.,1.,1.,1.,1.,1.,1.,1.,1.,1.,1.,1.,1.,1.,1.,1.,1.,1.,1.,1.,
1.,1.,1.,1.,1.,1.,1.,1.,1.,1.,1.,1.,1.,1.,1.,1.,1.,1.,1.,1.,1.,1.,1.,1.,
1.,1.,1.,1.,1.,1.,1.,1.,1.,1.,1.,1.,1.,1.,1.,1.,1.,1.,1.,1.,1.,1.,1.,1.,
1.,1.,1.,1.,1.,1.,1.,1.,1.,1.,1.,1.,1.,1.,1.,1.,1.,1.,1.,1.,1.,1.,1.,1.,
1.,1.,1.,1.,1.,1.,1.,1.,1.,1.,1.,1.,1.,1.,1.,1.,1.,1.,1.,1.,1.,1.,1.,1.,
1.,1.,1.,1.,1.,1.,1.,1.,1.,1.,1.,1.,1.,1.,1.,1.,1.,1.,1.,1.,1.,1.,1.,1.,
1.,1.,1.,1.,1.,1.,1.,1.,1.,1.,1.,1.,1.,1.,1.,1.,1.,1.,1.,1.,1.,1.,1.,1.,
1.,1.,1.,1.,1.,1.,1.,1.,1.,1.))
REPRESENTATION_ITEM('')
);
#499=(
BOUNDED_CURVE()
B_SPLINE_CURVE(5,(#96041,#96042,#96043,#96044,#96045,#96046,#96047,#96048,
#96049,#96050,#96051,#96052,#96053,#96054,#96055,#96056,#96057,#96058,#96059,
#96060,#96061,#96062,#96063,#96064,#96065,#96066,#96067,#96068,#96069,#96070,
#96071,#96072,#96073,#96074,#96075,#96076,#96077,#96078,#96079,#96080,#96081,
#96082,#96083,#96084,#96085,#96086,#96087,#96088,#96089,#96090,#96091,#96092,
#96093,#96094,#96095,#96096,#96097,#96098,#96099,#96100,#96101,#96102,#96103,
#96104,#96105,#96106,#96107,#96108,#96109,#96110,#96111,#96112,#96113,#96114,
#96115,#96116,#96117,#96118,#96119,#96120,#96121,#96122,#96123,#96124,#96125,
#96126,#96127,#96128,#96129,#96130,#96131,#96132,#96133,#96134,#96135,#96136,
#96137,#96138,#96139,#96140,#96141,#96142,#96143,#96144,#96145,#96146,#96147,
#96148,#96149,#96150,#96151,#96152,#96153,#96154,#96155,#96156,#96157,#96158,
#96159,#96160,#96161,#96162,#96163,#96164,#96165,#96166,#96167,#96168,#96169,
#96170,#96171,#96172,#96173,#96174,#96175,#96176,#96177,#96178,#96179,#96180,
#96181,#96182,#96183,#96184,#96185,#96186,#96187,#96188,#96189,#96190,#96191,
#96192,#96193,#96194,#96195,#96196,#96197,#96198,#96199,#96200,#96201,#96202,
#96203,#96204,#96205,#96206,#96207,#96208,#96209,#96210,#96211,#96212,#96213,
#96214,#96215,#96216,#96217,#96218,#96219,#96220,#96221,#96222,#96223,#96224,
#96225,#96226,#96227,#96228,#96229,#96230,#96231,#96232,#96233,#96234),
 .UNSPECIFIED.,.F.,.F.)
B_SPLINE_CURVE_WITH_KNOTS((6,1,1,1,1,1,1,1,1,1,1,1,1,1,1,1,1,1,1,1,1,1,
1,1,1,1,1,1,1,1,1,1,1,1,1,1,1,1,1,1,1,1,1,1,1,1,1,1,1,1,1,1,1,1,1,1,1,1,
1,1,1,1,1,1,1,1,1,1,1,1,1,1,1,1,1,1,1,1,1,1,1,1,1,1,1,1,1,1,1,1,1,1,1,1,
1,1,1,1,1,1,1,1,1,1,1,1,1,1,1,1,1,1,1,1,1,1,1,1,1,1,1,1,1,1,1,1,1,1,1,1,
1,1,1,1,1,1,1,1,1,1,1,1,1,1,1,1,1,1,1,1,1,1,1,1,1,1,1,1,1,1,1,1,1,1,1,1,
1,1,1,1,1,1,1,1,1,1,1,1,1,1,1,1,1,1,1,1,1,1,1,6),(0.,0.005,0.01,0.015,0.02,
0.025,0.03,0.035,0.04,0.045,0.05,0.055,0.06,0.065,0.07,0.075,0.08,0.085,
0.09,0.095,0.1,0.105,0.11,0.115,0.12,0.125,0.13,0.135,0.14,0.145,0.15,0.155,
0.16,0.165,0.17,0.175,0.18,0.185,0.19,0.195,0.2,0.205,0.21,0.215,0.22,0.225,
0.23,0.235,0.24,0.245,0.25,0.255,0.26,0.265,0.27,0.275,0.28,0.285,0.29,
0.295,0.3,0.305,0.31,0.315,0.32,0.325,0.33,0.335,0.34,0.345,0.35,0.355,
0.36,0.365,0.37,0.375,0.38,0.385,0.39,0.395,0.4,0.405,0.41,0.415,0.42,0.425,
0.43,0.435,0.44,0.445,0.45,0.455,0.46,0.465,0.47,0.475,0.48,0.485,0.49,
0.495,0.5,0.505,0.51,0.515,0.52,0.525,0.53,0.535,0.54,0.545,0.55,0.555,
0.56,0.565,0.57,0.575,0.58,0.585,0.59,0.595,0.6,0.605,0.61,0.615,0.62,0.625,
0.63,0.635,0.64,0.645,0.65,0.655,0.66,0.665,0.67,0.675,0.68,0.685,0.690000000000001,
0.695000000000001,0.700000000000001,0.705000000000001,0.710000000000001,
0.715000000000001,0.720000000000001,0.725000000000001,0.730000000000001,
0.735000000000001,0.740000000000001,0.745000000000001,0.750000000000001,
0.755000000000001,0.760000000000001,0.765000000000001,0.770000000000001,
0.775000000000001,0.780000000000001,0.785000000000001,0.790000000000001,
0.795000000000001,0.800000000000001,0.805000000000001,0.810000000000001,
0.815000000000001,0.820000000000001,0.825000000000001,0.830000000000001,
0.835000000000001,0.840000000000001,0.845000000000001,0.850000000000001,
0.855000000000001,0.860000000000001,0.865000000000001,0.870000000000001,
0.875000000000001,0.880000000000001,0.885000000000001,0.890000000000001,
0.895000000000001,0.900000000000001,0.905000000000001,0.910000000000001,
0.915000000000001,0.920000000000001,0.925000000000001,0.930000000000001,
0.935000000000001,0.940000000000001,0.941429844431407),.UNSPECIFIED.)
CURVE()
GEOMETRIC_REPRESENTATION_ITEM()
RATIONAL_B_SPLINE_CURVE((1.,1.,1.,1.,1.,1.,1.,1.,1.,1.,1.,1.,1.,1.,1.,1.,
1.,1.,1.,1.,1.,1.,1.,1.,1.,1.,1.,1.,1.,1.,1.,1.,1.,1.,1.,1.,1.,1.,1.,1.,
1.,1.,1.,1.,1.,1.,1.,1.,1.,1.,1.,1.,1.,1.,1.,1.,1.,1.,1.,1.,1.,1.,1.,1.,
1.,1.,1.,1.,1.,1.,1.,1.,1.,1.,1.,1.,1.,1.,1.,1.,1.,1.,1.,1.,1.,1.,1.,1.,
1.,1.,1.,1.,1.,1.,1.,1.,1.,1.,1.,1.,1.,1.,1.,1.,1.,1.,1.,1.,1.,1.,1.,1.,
1.,1.,1.,1.,1.,1.,1.,1.,1.,1.,1.,1.,1.,1.,1.,1.,1.,1.,1.,1.,1.,1.,1.,1.,
1.,1.,1.,1.,1.,1.,1.,1.,1.,1.,1.,1.,1.,1.,1.,1.,1.,1.,1.,1.,1.,1.,1.,1.,
1.,1.,1.,1.,1.,1.,1.,1.,1.,1.,1.,1.,1.,1.,1.,1.,1.,1.,1.,1.,1.,1.,1.,1.,
1.,1.,1.,1.,1.,1.,1.,1.,1.,1.))
REPRESENTATION_ITEM('')
);
#500=(
BOUNDED_CURVE()
B_SPLINE_CURVE(5,(#96237,#96238,#96239,#96240,#96241,#96242,#96243,#96244,
#96245,#96246,#96247,#96248,#96249,#96250,#96251,#96252,#96253,#96254,#96255,
#96256,#96257,#96258,#96259,#96260,#96261,#96262,#96263,#96264,#96265,#96266,
#96267,#96268,#96269,#96270,#96271,#96272,#96273,#96274,#96275,#96276,#96277,
#96278,#96279,#96280,#96281,#96282,#96283,#96284,#96285,#96286,#96287,#96288,
#96289,#96290,#96291,#96292,#96293,#96294,#96295,#96296,#96297,#96298,#96299,
#96300,#96301,#96302,#96303,#96304,#96305,#96306,#96307,#96308,#96309,#96310,
#96311,#96312,#96313,#96314,#96315,#96316,#96317,#96318,#96319,#96320,#96321,
#96322,#96323,#96324,#96325,#96326,#96327,#96328,#96329,#96330,#96331,#96332,
#96333,#96334,#96335,#96336,#96337,#96338,#96339,#96340,#96341,#96342,#96343,
#96344,#96345,#96346,#96347,#96348,#96349,#96350,#96351,#96352,#96353,#96354,
#96355,#96356,#96357,#96358,#96359,#96360,#96361,#96362,#96363,#96364,#96365,
#96366,#96367,#96368,#96369,#96370,#96371,#96372,#96373,#96374,#96375,#96376,
#96377,#96378,#96379,#96380,#96381,#96382,#96383,#96384,#96385,#96386,#96387,
#96388,#96389,#96390,#96391,#96392,#96393,#96394,#96395,#96396,#96397,#96398,
#96399,#96400,#96401,#96402,#96403,#96404,#96405,#96406,#96407,#96408,#96409,
#96410,#96411,#96412,#96413,#96414,#96415,#96416,#96417,#96418,#96419,#96420,
#96421,#96422,#96423,#96424,#96425,#96426,#96427,#96428,#96429,#96430),
 .UNSPECIFIED.,.F.,.F.)
B_SPLINE_CURVE_WITH_KNOTS((6,1,1,1,1,1,1,1,1,1,1,1,1,1,1,1,1,1,1,1,1,1,
1,1,1,1,1,1,1,1,1,1,1,1,1,1,1,1,1,1,1,1,1,1,1,1,1,1,1,1,1,1,1,1,1,1,1,1,
1,1,1,1,1,1,1,1,1,1,1,1,1,1,1,1,1,1,1,1,1,1,1,1,1,1,1,1,1,1,1,1,1,1,1,1,
1,1,1,1,1,1,1,1,1,1,1,1,1,1,1,1,1,1,1,1,1,1,1,1,1,1,1,1,1,1,1,1,1,1,1,1,
1,1,1,1,1,1,1,1,1,1,1,1,1,1,1,1,1,1,1,1,1,1,1,1,1,1,1,1,1,1,1,1,1,1,1,1,
1,1,1,1,1,1,1,1,1,1,1,1,1,1,1,1,1,1,1,1,1,1,1,6),(-0.941429844431431,-0.940000000000001,
-0.935000000000001,-0.930000000000001,-0.925000000000001,-0.920000000000001,
-0.915000000000001,-0.910000000000001,-0.905000000000001,-0.900000000000001,
-0.895000000000001,-0.890000000000001,-0.885000000000001,-0.880000000000001,
-0.875000000000001,-0.870000000000001,-0.865000000000001,-0.860000000000001,
-0.855000000000001,-0.850000000000001,-0.845000000000001,-0.840000000000001,
-0.835000000000001,-0.830000000000001,-0.825000000000001,-0.820000000000001,
-0.815000000000001,-0.810000000000001,-0.805000000000001,-0.800000000000001,
-0.795000000000001,-0.790000000000001,-0.785000000000001,-0.780000000000001,
-0.775000000000001,-0.770000000000001,-0.765000000000001,-0.760000000000001,
-0.755000000000001,-0.750000000000001,-0.745000000000001,-0.740000000000001,
-0.735000000000001,-0.730000000000001,-0.725000000000001,-0.720000000000001,
-0.715000000000001,-0.710000000000001,-0.705000000000001,-0.700000000000001,
-0.695000000000001,-0.690000000000001,-0.685,-0.68,-0.675,-0.67,-0.665,
-0.66,-0.655,-0.65,-0.645,-0.64,-0.635,-0.63,-0.625,-0.62,-0.615,-0.61,
-0.605,-0.6,-0.595,-0.59,-0.585,-0.58,-0.575,-0.57,-0.565,-0.56,-0.555,
-0.55,-0.545,-0.54,-0.535,-0.53,-0.525,-0.52,-0.515,-0.51,-0.505,-0.5,-0.495,
-0.49,-0.485,-0.48,-0.475,-0.47,-0.465,-0.46,-0.455,-0.45,-0.445,-0.44,
-0.435,-0.43,-0.425,-0.42,-0.415,-0.41,-0.405,-0.4,-0.395,-0.39,-0.385,
-0.38,-0.375,-0.37,-0.365,-0.36,-0.355,-0.35,-0.345,-0.34,-0.335,-0.33,
-0.325,-0.32,-0.315,-0.31,-0.305,-0.3,-0.295,-0.29,-0.285,-0.28,-0.275,
-0.27,-0.265,-0.26,-0.255,-0.25,-0.245,-0.24,-0.235,-0.23,-0.225,-0.22,
-0.215,-0.21,-0.205,-0.2,-0.195,-0.19,-0.185,-0.18,-0.175,-0.17,-0.165,
-0.16,-0.155,-0.15,-0.145,-0.14,-0.135,-0.13,-0.125,-0.12,-0.115,-0.11,
-0.105,-0.1,-0.095,-0.09,-0.085,-0.08,-0.075,-0.07,-0.065,-0.06,-0.055,
-0.05,-0.045,-0.04,-0.035,-0.03,-0.025,-0.02,-0.015,-0.01,-0.005,0.),
 .UNSPECIFIED.)
CURVE()
GEOMETRIC_REPRESENTATION_ITEM()
RATIONAL_B_SPLINE_CURVE((1.,1.,1.,1.,1.,1.,1.,1.,1.,1.,1.,1.,1.,1.,1.,1.,
1.,1.,1.,1.,1.,1.,1.,1.,1.,1.,1.,1.,1.,1.,1.,1.,1.,1.,1.,1.,1.,1.,1.,1.,
1.,1.,1.,1.,1.,1.,1.,1.,1.,1.,1.,1.,1.,1.,1.,1.,1.,1.,1.,1.,1.,1.,1.,1.,
1.,1.,1.,1.,1.,1.,1.,1.,1.,1.,1.,1.,1.,1.,1.,1.,1.,1.,1.,1.,1.,1.,1.,1.,
1.,1.,1.,1.,1.,1.,1.,1.,1.,1.,1.,1.,1.,1.,1.,1.,1.,1.,1.,1.,1.,1.,1.,1.,
1.,1.,1.,1.,1.,1.,1.,1.,1.,1.,1.,1.,1.,1.,1.,1.,1.,1.,1.,1.,1.,1.,1.,1.,
1.,1.,1.,1.,1.,1.,1.,1.,1.,1.,1.,1.,1.,1.,1.,1.,1.,1.,1.,1.,1.,1.,1.,1.,
1.,1.,1.,1.,1.,1.,1.,1.,1.,1.,1.,1.,1.,1.,1.,1.,1.,1.,1.,1.,1.,1.,1.,1.,
1.,1.,1.,1.,1.,1.,1.,1.,1.,1.))
REPRESENTATION_ITEM('')
);
#501=(
BOUNDED_CURVE()
B_SPLINE_CURVE(5,(#96937,#96938,#96939,#96940,#96941,#96942,#96943,#96944,
#96945,#96946,#96947,#96948,#96949,#96950,#96951,#96952,#96953,#96954,#96955,
#96956,#96957,#96958,#96959,#96960,#96961,#96962,#96963,#96964,#96965,#96966,
#96967,#96968,#96969,#96970,#96971,#96972,#96973,#96974,#96975,#96976,#96977,
#96978,#96979,#96980,#96981,#96982,#96983,#96984,#96985,#96986,#96987,#96988,
#96989,#96990,#96991,#96992,#96993,#96994,#96995,#96996,#96997,#96998,#96999,
#97000,#97001,#97002,#97003,#97004,#97005,#97006,#97007,#97008,#97009,#97010,
#97011,#97012,#97013,#97014,#97015,#97016,#97017,#97018,#97019,#97020,#97021,
#97022,#97023,#97024,#97025,#97026,#97027,#97028,#97029,#97030,#97031,#97032,
#97033,#97034,#97035,#97036,#97037,#97038,#97039,#97040,#97041,#97042,#97043,
#97044,#97045,#97046,#97047,#97048,#97049,#97050,#97051,#97052,#97053,#97054,
#97055,#97056,#97057,#97058,#97059,#97060,#97061,#97062,#97063,#97064,#97065,
#97066,#97067,#97068,#97069,#97070,#97071,#97072,#97073,#97074,#97075,#97076,
#97077,#97078,#97079,#97080,#97081,#97082,#97083,#97084,#97085,#97086,#97087,
#97088,#97089,#97090,#97091,#97092,#97093,#97094,#97095,#97096,#97097,#97098,
#97099,#97100,#97101,#97102,#97103,#97104,#97105,#97106,#97107,#97108,#97109,
#97110,#97111,#97112,#97113,#97114,#97115,#97116,#97117,#97118,#97119,#97120,
#97121,#97122,#97123,#97124,#97125,#97126,#97127,#97128,#97129,#97130),
 .UNSPECIFIED.,.F.,.F.)
B_SPLINE_CURVE_WITH_KNOTS((6,1,1,1,1,1,1,1,1,1,1,1,1,1,1,1,1,1,1,1,1,1,
1,1,1,1,1,1,1,1,1,1,1,1,1,1,1,1,1,1,1,1,1,1,1,1,1,1,1,1,1,1,1,1,1,1,1,1,
1,1,1,1,1,1,1,1,1,1,1,1,1,1,1,1,1,1,1,1,1,1,1,1,1,1,1,1,1,1,1,1,1,1,1,1,
1,1,1,1,1,1,1,1,1,1,1,1,1,1,1,1,1,1,1,1,1,1,1,1,1,1,1,1,1,1,1,1,1,1,1,1,
1,1,1,1,1,1,1,1,1,1,1,1,1,1,1,1,1,1,1,1,1,1,1,1,1,1,1,1,1,1,1,1,1,1,1,1,
1,1,1,1,1,1,1,1,1,1,1,1,1,1,1,1,1,1,1,1,1,1,1,6),(0.,0.005,0.01,0.015,0.02,
0.025,0.03,0.035,0.04,0.045,0.05,0.055,0.06,0.065,0.07,0.075,0.08,0.085,
0.09,0.095,0.1,0.105,0.11,0.115,0.12,0.125,0.13,0.135,0.14,0.145,0.15,0.155,
0.16,0.165,0.17,0.175,0.18,0.185,0.19,0.195,0.2,0.205,0.21,0.215,0.22,0.225,
0.23,0.235,0.24,0.245,0.25,0.255,0.26,0.265,0.27,0.275,0.28,0.285,0.29,
0.295,0.3,0.305,0.31,0.315,0.32,0.325,0.33,0.335,0.34,0.345,0.35,0.355,
0.36,0.365,0.37,0.375,0.38,0.385,0.39,0.395,0.4,0.405,0.41,0.415,0.42,0.425,
0.43,0.435,0.44,0.445,0.45,0.455,0.46,0.465,0.47,0.475,0.48,0.485,0.49,
0.495,0.5,0.505,0.51,0.515,0.52,0.525,0.53,0.535,0.54,0.545,0.55,0.555,
0.56,0.565,0.57,0.575,0.58,0.585,0.59,0.595,0.6,0.605,0.61,0.615,0.62,0.625,
0.63,0.635,0.64,0.645,0.65,0.655,0.66,0.665,0.67,0.675,0.68,0.685,0.690000000000001,
0.695000000000001,0.700000000000001,0.705000000000001,0.710000000000001,
0.715000000000001,0.720000000000001,0.725000000000001,0.730000000000001,
0.735000000000001,0.740000000000001,0.745000000000001,0.750000000000001,
0.755000000000001,0.760000000000001,0.765000000000001,0.770000000000001,
0.775000000000001,0.780000000000001,0.785000000000001,0.790000000000001,
0.795000000000001,0.800000000000001,0.805000000000001,0.810000000000001,
0.815000000000001,0.820000000000001,0.825000000000001,0.830000000000001,
0.835000000000001,0.840000000000001,0.845000000000001,0.850000000000001,
0.855000000000001,0.860000000000001,0.865000000000001,0.870000000000001,
0.875000000000001,0.880000000000001,0.885000000000001,0.890000000000001,
0.895000000000001,0.900000000000001,0.905000000000001,0.910000000000001,
0.915000000000001,0.920000000000001,0.925000000000001,0.930000000000001,
0.935000000000001,0.940000000000001,0.941429844431522),.UNSPECIFIED.)
CURVE()
GEOMETRIC_REPRESENTATION_ITEM()
RATIONAL_B_SPLINE_CURVE((1.,1.,1.,1.,1.,1.,1.,1.,1.,1.,1.,1.,1.,1.,1.,1.,
1.,1.,1.,1.,1.,1.,1.,1.,1.,1.,1.,1.,1.,1.,1.,1.,1.,1.,1.,1.,1.,1.,1.,1.,
1.,1.,1.,1.,1.,1.,1.,1.,1.,1.,1.,1.,1.,1.,1.,1.,1.,1.,1.,1.,1.,1.,1.,1.,
1.,1.,1.,1.,1.,1.,1.,1.,1.,1.,1.,1.,1.,1.,1.,1.,1.,1.,1.,1.,1.,1.,1.,1.,
1.,1.,1.,1.,1.,1.,1.,1.,1.,1.,1.,1.,1.,1.,1.,1.,1.,1.,1.,1.,1.,1.,1.,1.,
1.,1.,1.,1.,1.,1.,1.,1.,1.,1.,1.,1.,1.,1.,1.,1.,1.,1.,1.,1.,1.,1.,1.,1.,
1.,1.,1.,1.,1.,1.,1.,1.,1.,1.,1.,1.,1.,1.,1.,1.,1.,1.,1.,1.,1.,1.,1.,1.,
1.,1.,1.,1.,1.,1.,1.,1.,1.,1.,1.,1.,1.,1.,1.,1.,1.,1.,1.,1.,1.,1.,1.,1.,
1.,1.,1.,1.,1.,1.,1.,1.,1.,1.))
REPRESENTATION_ITEM('')
);
#502=(
BOUNDED_CURVE()
B_SPLINE_CURVE(5,(#97133,#97134,#97135,#97136,#97137,#97138,#97139,#97140,
#97141,#97142,#97143,#97144,#97145,#97146,#97147,#97148,#97149,#97150,#97151,
#97152,#97153,#97154,#97155,#97156,#97157,#97158,#97159,#97160,#97161,#97162,
#97163,#97164,#97165,#97166,#97167,#97168,#97169,#97170,#97171,#97172,#97173,
#97174,#97175,#97176,#97177,#97178,#97179,#97180,#97181,#97182,#97183,#97184,
#97185,#97186,#97187,#97188,#97189,#97190,#97191,#97192,#97193,#97194,#97195,
#97196,#97197,#97198,#97199,#97200,#97201,#97202,#97203,#97204,#97205,#97206,
#97207,#97208,#97209,#97210,#97211,#97212,#97213,#97214,#97215,#97216,#97217,
#97218,#97219,#97220,#97221,#97222,#97223,#97224,#97225,#97226,#97227,#97228,
#97229,#97230,#97231,#97232,#97233,#97234,#97235,#97236,#97237,#97238,#97239,
#97240,#97241,#97242,#97243,#97244,#97245,#97246,#97247,#97248,#97249,#97250,
#97251,#97252,#97253,#97254,#97255,#97256,#97257,#97258,#97259,#97260,#97261,
#97262,#97263,#97264,#97265,#97266,#97267,#97268,#97269,#97270,#97271,#97272,
#97273,#97274,#97275,#97276,#97277,#97278,#97279,#97280,#97281,#97282,#97283,
#97284,#97285,#97286,#97287,#97288,#97289,#97290,#97291,#97292,#97293,#97294,
#97295,#97296,#97297,#97298,#97299,#97300,#97301,#97302,#97303,#97304,#97305,
#97306,#97307,#97308,#97309,#97310,#97311,#97312,#97313,#97314,#97315,#97316,
#97317,#97318,#97319,#97320,#97321,#97322,#97323,#97324,#97325,#97326),
 .UNSPECIFIED.,.F.,.F.)
B_SPLINE_CURVE_WITH_KNOTS((6,1,1,1,1,1,1,1,1,1,1,1,1,1,1,1,1,1,1,1,1,1,
1,1,1,1,1,1,1,1,1,1,1,1,1,1,1,1,1,1,1,1,1,1,1,1,1,1,1,1,1,1,1,1,1,1,1,1,
1,1,1,1,1,1,1,1,1,1,1,1,1,1,1,1,1,1,1,1,1,1,1,1,1,1,1,1,1,1,1,1,1,1,1,1,
1,1,1,1,1,1,1,1,1,1,1,1,1,1,1,1,1,1,1,1,1,1,1,1,1,1,1,1,1,1,1,1,1,1,1,1,
1,1,1,1,1,1,1,1,1,1,1,1,1,1,1,1,1,1,1,1,1,1,1,1,1,1,1,1,1,1,1,1,1,1,1,1,
1,1,1,1,1,1,1,1,1,1,1,1,1,1,1,1,1,1,1,1,1,1,1,6),(-0.941429844431529,-0.940000000000001,
-0.935000000000001,-0.930000000000001,-0.925000000000001,-0.920000000000001,
-0.915000000000001,-0.910000000000001,-0.905000000000001,-0.900000000000001,
-0.895000000000001,-0.890000000000001,-0.885000000000001,-0.880000000000001,
-0.875000000000001,-0.870000000000001,-0.865000000000001,-0.860000000000001,
-0.855000000000001,-0.850000000000001,-0.845000000000001,-0.840000000000001,
-0.835000000000001,-0.830000000000001,-0.825000000000001,-0.820000000000001,
-0.815000000000001,-0.810000000000001,-0.805000000000001,-0.800000000000001,
-0.795000000000001,-0.790000000000001,-0.785000000000001,-0.780000000000001,
-0.775000000000001,-0.770000000000001,-0.765000000000001,-0.760000000000001,
-0.755000000000001,-0.750000000000001,-0.745000000000001,-0.740000000000001,
-0.735000000000001,-0.730000000000001,-0.725000000000001,-0.720000000000001,
-0.715000000000001,-0.710000000000001,-0.705000000000001,-0.700000000000001,
-0.695000000000001,-0.690000000000001,-0.685,-0.68,-0.675,-0.67,-0.665,
-0.66,-0.655,-0.65,-0.645,-0.64,-0.635,-0.63,-0.625,-0.62,-0.615,-0.61,
-0.605,-0.6,-0.595,-0.59,-0.585,-0.58,-0.575,-0.57,-0.565,-0.56,-0.555,
-0.55,-0.545,-0.54,-0.535,-0.53,-0.525,-0.52,-0.515,-0.51,-0.505,-0.5,-0.495,
-0.49,-0.485,-0.48,-0.475,-0.47,-0.465,-0.46,-0.455,-0.45,-0.445,-0.44,
-0.435,-0.43,-0.425,-0.42,-0.415,-0.41,-0.405,-0.4,-0.395,-0.39,-0.385,
-0.38,-0.375,-0.37,-0.365,-0.36,-0.355,-0.35,-0.345,-0.34,-0.335,-0.33,
-0.325,-0.32,-0.315,-0.31,-0.305,-0.3,-0.295,-0.29,-0.285,-0.28,-0.275,
-0.27,-0.265,-0.26,-0.255,-0.25,-0.245,-0.24,-0.235,-0.23,-0.225,-0.22,
-0.215,-0.21,-0.205,-0.2,-0.195,-0.19,-0.185,-0.18,-0.175,-0.17,-0.165,
-0.16,-0.155,-0.15,-0.145,-0.14,-0.135,-0.13,-0.125,-0.12,-0.115,-0.11,
-0.105,-0.1,-0.095,-0.09,-0.085,-0.08,-0.075,-0.07,-0.065,-0.06,-0.055,
-0.05,-0.045,-0.04,-0.035,-0.03,-0.025,-0.02,-0.015,-0.01,-0.005,0.),
 .UNSPECIFIED.)
CURVE()
GEOMETRIC_REPRESENTATION_ITEM()
RATIONAL_B_SPLINE_CURVE((1.,1.,1.,1.,1.,1.,1.,1.,1.,1.,1.,1.,1.,1.,1.,1.,
1.,1.,1.,1.,1.,1.,1.,1.,1.,1.,1.,1.,1.,1.,1.,1.,1.,1.,1.,1.,1.,1.,1.,1.,
1.,1.,1.,1.,1.,1.,1.,1.,1.,1.,1.,1.,1.,1.,1.,1.,1.,1.,1.,1.,1.,1.,1.,1.,
1.,1.,1.,1.,1.,1.,1.,1.,1.,1.,1.,1.,1.,1.,1.,1.,1.,1.,1.,1.,1.,1.,1.,1.,
1.,1.,1.,1.,1.,1.,1.,1.,1.,1.,1.,1.,1.,1.,1.,1.,1.,1.,1.,1.,1.,1.,1.,1.,
1.,1.,1.,1.,1.,1.,1.,1.,1.,1.,1.,1.,1.,1.,1.,1.,1.,1.,1.,1.,1.,1.,1.,1.,
1.,1.,1.,1.,1.,1.,1.,1.,1.,1.,1.,1.,1.,1.,1.,1.,1.,1.,1.,1.,1.,1.,1.,1.,
1.,1.,1.,1.,1.,1.,1.,1.,1.,1.,1.,1.,1.,1.,1.,1.,1.,1.,1.,1.,1.,1.,1.,1.,
1.,1.,1.,1.,1.,1.,1.,1.,1.,1.))
REPRESENTATION_ITEM('')
);
#503=(
BOUNDED_CURVE()
B_SPLINE_CURVE(5,(#97833,#97834,#97835,#97836,#97837,#97838,#97839,#97840,
#97841,#97842,#97843,#97844,#97845,#97846,#97847,#97848,#97849,#97850,#97851,
#97852,#97853,#97854,#97855,#97856,#97857,#97858,#97859,#97860,#97861,#97862,
#97863,#97864,#97865,#97866,#97867,#97868,#97869,#97870,#97871,#97872,#97873,
#97874,#97875,#97876,#97877,#97878,#97879,#97880,#97881,#97882,#97883,#97884,
#97885,#97886,#97887,#97888,#97889,#97890,#97891,#97892,#97893,#97894,#97895,
#97896,#97897,#97898,#97899,#97900,#97901,#97902,#97903,#97904,#97905,#97906,
#97907,#97908,#97909,#97910,#97911,#97912,#97913,#97914,#97915,#97916,#97917,
#97918,#97919,#97920,#97921,#97922,#97923,#97924,#97925,#97926,#97927,#97928,
#97929,#97930,#97931,#97932,#97933,#97934,#97935,#97936,#97937,#97938,#97939,
#97940,#97941,#97942,#97943,#97944,#97945,#97946,#97947,#97948,#97949,#97950,
#97951,#97952,#97953,#97954,#97955,#97956,#97957,#97958,#97959,#97960,#97961,
#97962,#97963,#97964,#97965,#97966,#97967,#97968,#97969,#97970,#97971,#97972,
#97973,#97974,#97975,#97976,#97977,#97978,#97979,#97980,#97981,#97982,#97983,
#97984,#97985,#97986,#97987,#97988,#97989,#97990,#97991,#97992,#97993,#97994,
#97995,#97996,#97997,#97998,#97999,#98000,#98001,#98002,#98003,#98004,#98005,
#98006,#98007,#98008,#98009,#98010,#98011,#98012,#98013,#98014,#98015,#98016,
#98017,#98018,#98019,#98020,#98021,#98022,#98023,#98024,#98025,#98026),
 .UNSPECIFIED.,.F.,.F.)
B_SPLINE_CURVE_WITH_KNOTS((6,1,1,1,1,1,1,1,1,1,1,1,1,1,1,1,1,1,1,1,1,1,
1,1,1,1,1,1,1,1,1,1,1,1,1,1,1,1,1,1,1,1,1,1,1,1,1,1,1,1,1,1,1,1,1,1,1,1,
1,1,1,1,1,1,1,1,1,1,1,1,1,1,1,1,1,1,1,1,1,1,1,1,1,1,1,1,1,1,1,1,1,1,1,1,
1,1,1,1,1,1,1,1,1,1,1,1,1,1,1,1,1,1,1,1,1,1,1,1,1,1,1,1,1,1,1,1,1,1,1,1,
1,1,1,1,1,1,1,1,1,1,1,1,1,1,1,1,1,1,1,1,1,1,1,1,1,1,1,1,1,1,1,1,1,1,1,1,
1,1,1,1,1,1,1,1,1,1,1,1,1,1,1,1,1,1,1,1,1,1,1,6),(0.,0.005,0.01,0.015,0.02,
0.025,0.03,0.035,0.04,0.045,0.05,0.055,0.06,0.065,0.07,0.075,0.08,0.085,
0.09,0.095,0.1,0.105,0.11,0.115,0.12,0.125,0.13,0.135,0.14,0.145,0.15,0.155,
0.16,0.165,0.17,0.175,0.18,0.185,0.19,0.195,0.2,0.205,0.21,0.215,0.22,0.225,
0.23,0.235,0.24,0.245,0.25,0.255,0.26,0.265,0.27,0.275,0.28,0.285,0.29,
0.295,0.3,0.305,0.31,0.315,0.32,0.325,0.33,0.335,0.34,0.345,0.35,0.355,
0.36,0.365,0.37,0.375,0.38,0.385,0.39,0.395,0.4,0.405,0.41,0.415,0.42,0.425,
0.43,0.435,0.44,0.445,0.45,0.455,0.46,0.465,0.47,0.475,0.48,0.485,0.49,
0.495,0.5,0.505,0.51,0.515,0.52,0.525,0.53,0.535,0.54,0.545,0.55,0.555,
0.56,0.565,0.57,0.575,0.58,0.585,0.59,0.595,0.6,0.605,0.61,0.615,0.62,0.625,
0.63,0.635,0.64,0.645,0.65,0.655,0.66,0.665,0.67,0.675,0.68,0.685,0.690000000000001,
0.695000000000001,0.700000000000001,0.705000000000001,0.710000000000001,
0.715000000000001,0.720000000000001,0.725000000000001,0.730000000000001,
0.735000000000001,0.740000000000001,0.745000000000001,0.750000000000001,
0.755000000000001,0.760000000000001,0.765000000000001,0.770000000000001,
0.775000000000001,0.780000000000001,0.785000000000001,0.790000000000001,
0.795000000000001,0.800000000000001,0.805000000000001,0.810000000000001,
0.815000000000001,0.820000000000001,0.825000000000001,0.830000000000001,
0.835000000000001,0.840000000000001,0.845000000000001,0.850000000000001,
0.855000000000001,0.860000000000001,0.865000000000001,0.870000000000001,
0.875000000000001,0.880000000000001,0.885000000000001,0.890000000000001,
0.895000000000001,0.900000000000001,0.905000000000001,0.910000000000001,
0.915000000000001,0.920000000000001,0.925000000000001,0.930000000000001,
0.935000000000001,0.940000000000001,0.941429844431384),.UNSPECIFIED.)
CURVE()
GEOMETRIC_REPRESENTATION_ITEM()
RATIONAL_B_SPLINE_CURVE((1.,1.,1.,1.,1.,1.,1.,1.,1.,1.,1.,1.,1.,1.,1.,1.,
1.,1.,1.,1.,1.,1.,1.,1.,1.,1.,1.,1.,1.,1.,1.,1.,1.,1.,1.,1.,1.,1.,1.,1.,
1.,1.,1.,1.,1.,1.,1.,1.,1.,1.,1.,1.,1.,1.,1.,1.,1.,1.,1.,1.,1.,1.,1.,1.,
1.,1.,1.,1.,1.,1.,1.,1.,1.,1.,1.,1.,1.,1.,1.,1.,1.,1.,1.,1.,1.,1.,1.,1.,
1.,1.,1.,1.,1.,1.,1.,1.,1.,1.,1.,1.,1.,1.,1.,1.,1.,1.,1.,1.,1.,1.,1.,1.,
1.,1.,1.,1.,1.,1.,1.,1.,1.,1.,1.,1.,1.,1.,1.,1.,1.,1.,1.,1.,1.,1.,1.,1.,
1.,1.,1.,1.,1.,1.,1.,1.,1.,1.,1.,1.,1.,1.,1.,1.,1.,1.,1.,1.,1.,1.,1.,1.,
1.,1.,1.,1.,1.,1.,1.,1.,1.,1.,1.,1.,1.,1.,1.,1.,1.,1.,1.,1.,1.,1.,1.,1.,
1.,1.,1.,1.,1.,1.,1.,1.,1.,1.))
REPRESENTATION_ITEM('')
);
#504=(
BOUNDED_CURVE()
B_SPLINE_CURVE(5,(#98029,#98030,#98031,#98032,#98033,#98034,#98035,#98036,
#98037,#98038,#98039,#98040,#98041,#98042,#98043,#98044,#98045,#98046,#98047,
#98048,#98049,#98050,#98051,#98052,#98053,#98054,#98055,#98056,#98057,#98058,
#98059,#98060,#98061,#98062,#98063,#98064,#98065,#98066,#98067,#98068,#98069,
#98070,#98071,#98072,#98073,#98074,#98075,#98076,#98077,#98078,#98079,#98080,
#98081,#98082,#98083,#98084,#98085,#98086,#98087,#98088,#98089,#98090,#98091,
#98092,#98093,#98094,#98095,#98096,#98097,#98098,#98099,#98100,#98101,#98102,
#98103,#98104,#98105,#98106,#98107,#98108,#98109,#98110,#98111,#98112,#98113,
#98114,#98115,#98116,#98117,#98118,#98119,#98120,#98121,#98122,#98123,#98124,
#98125,#98126,#98127,#98128,#98129,#98130,#98131,#98132,#98133,#98134,#98135,
#98136,#98137,#98138,#98139,#98140,#98141,#98142,#98143,#98144,#98145,#98146,
#98147,#98148,#98149,#98150,#98151,#98152,#98153,#98154,#98155,#98156,#98157,
#98158,#98159,#98160,#98161,#98162,#98163,#98164,#98165,#98166,#98167,#98168,
#98169,#98170,#98171,#98172,#98173,#98174,#98175,#98176,#98177,#98178,#98179,
#98180,#98181,#98182,#98183,#98184,#98185,#98186,#98187,#98188,#98189,#98190,
#98191,#98192,#98193,#98194,#98195,#98196,#98197,#98198,#98199,#98200,#98201,
#98202,#98203,#98204,#98205,#98206,#98207,#98208,#98209,#98210,#98211,#98212,
#98213,#98214,#98215,#98216,#98217,#98218,#98219,#98220,#98221,#98222),
 .UNSPECIFIED.,.F.,.F.)
B_SPLINE_CURVE_WITH_KNOTS((6,1,1,1,1,1,1,1,1,1,1,1,1,1,1,1,1,1,1,1,1,1,
1,1,1,1,1,1,1,1,1,1,1,1,1,1,1,1,1,1,1,1,1,1,1,1,1,1,1,1,1,1,1,1,1,1,1,1,
1,1,1,1,1,1,1,1,1,1,1,1,1,1,1,1,1,1,1,1,1,1,1,1,1,1,1,1,1,1,1,1,1,1,1,1,
1,1,1,1,1,1,1,1,1,1,1,1,1,1,1,1,1,1,1,1,1,1,1,1,1,1,1,1,1,1,1,1,1,1,1,1,
1,1,1,1,1,1,1,1,1,1,1,1,1,1,1,1,1,1,1,1,1,1,1,1,1,1,1,1,1,1,1,1,1,1,1,1,
1,1,1,1,1,1,1,1,1,1,1,1,1,1,1,1,1,1,1,1,1,1,1,6),(-0.941429844431385,-0.940000000000001,
-0.935000000000001,-0.930000000000001,-0.925000000000001,-0.920000000000001,
-0.915000000000001,-0.910000000000001,-0.905000000000001,-0.900000000000001,
-0.895000000000001,-0.890000000000001,-0.885000000000001,-0.880000000000001,
-0.875000000000001,-0.870000000000001,-0.865000000000001,-0.860000000000001,
-0.855000000000001,-0.850000000000001,-0.845000000000001,-0.840000000000001,
-0.835000000000001,-0.830000000000001,-0.825000000000001,-0.820000000000001,
-0.815000000000001,-0.810000000000001,-0.805000000000001,-0.800000000000001,
-0.795000000000001,-0.790000000000001,-0.785000000000001,-0.780000000000001,
-0.775000000000001,-0.770000000000001,-0.765000000000001,-0.760000000000001,
-0.755000000000001,-0.750000000000001,-0.745000000000001,-0.740000000000001,
-0.735000000000001,-0.730000000000001,-0.725000000000001,-0.720000000000001,
-0.715000000000001,-0.710000000000001,-0.705000000000001,-0.700000000000001,
-0.695000000000001,-0.690000000000001,-0.685,-0.68,-0.675,-0.67,-0.665,
-0.66,-0.655,-0.65,-0.645,-0.64,-0.635,-0.63,-0.625,-0.62,-0.615,-0.61,
-0.605,-0.6,-0.595,-0.59,-0.585,-0.58,-0.575,-0.57,-0.565,-0.56,-0.555,
-0.55,-0.545,-0.54,-0.535,-0.53,-0.525,-0.52,-0.515,-0.51,-0.505,-0.5,-0.495,
-0.49,-0.485,-0.48,-0.475,-0.47,-0.465,-0.46,-0.455,-0.45,-0.445,-0.44,
-0.435,-0.43,-0.425,-0.42,-0.415,-0.41,-0.405,-0.4,-0.395,-0.39,-0.385,
-0.38,-0.375,-0.37,-0.365,-0.36,-0.355,-0.35,-0.345,-0.34,-0.335,-0.33,
-0.325,-0.32,-0.315,-0.31,-0.305,-0.3,-0.295,-0.29,-0.285,-0.28,-0.275,
-0.27,-0.265,-0.26,-0.255,-0.25,-0.245,-0.24,-0.235,-0.23,-0.225,-0.22,
-0.215,-0.21,-0.205,-0.2,-0.195,-0.19,-0.185,-0.18,-0.175,-0.17,-0.165,
-0.16,-0.155,-0.15,-0.145,-0.14,-0.135,-0.13,-0.125,-0.12,-0.115,-0.11,
-0.105,-0.1,-0.095,-0.09,-0.085,-0.08,-0.075,-0.07,-0.065,-0.06,-0.055,
-0.05,-0.045,-0.04,-0.035,-0.03,-0.025,-0.02,-0.015,-0.01,-0.005,0.),
 .UNSPECIFIED.)
CURVE()
GEOMETRIC_REPRESENTATION_ITEM()
RATIONAL_B_SPLINE_CURVE((1.,1.,1.,1.,1.,1.,1.,1.,1.,1.,1.,1.,1.,1.,1.,1.,
1.,1.,1.,1.,1.,1.,1.,1.,1.,1.,1.,1.,1.,1.,1.,1.,1.,1.,1.,1.,1.,1.,1.,1.,
1.,1.,1.,1.,1.,1.,1.,1.,1.,1.,1.,1.,1.,1.,1.,1.,1.,1.,1.,1.,1.,1.,1.,1.,
1.,1.,1.,1.,1.,1.,1.,1.,1.,1.,1.,1.,1.,1.,1.,1.,1.,1.,1.,1.,1.,1.,1.,1.,
1.,1.,1.,1.,1.,1.,1.,1.,1.,1.,1.,1.,1.,1.,1.,1.,1.,1.,1.,1.,1.,1.,1.,1.,
1.,1.,1.,1.,1.,1.,1.,1.,1.,1.,1.,1.,1.,1.,1.,1.,1.,1.,1.,1.,1.,1.,1.,1.,
1.,1.,1.,1.,1.,1.,1.,1.,1.,1.,1.,1.,1.,1.,1.,1.,1.,1.,1.,1.,1.,1.,1.,1.,
1.,1.,1.,1.,1.,1.,1.,1.,1.,1.,1.,1.,1.,1.,1.,1.,1.,1.,1.,1.,1.,1.,1.,1.,
1.,1.,1.,1.,1.,1.,1.,1.,1.,1.))
REPRESENTATION_ITEM('')
);
#505=(
BOUNDED_CURVE()
B_SPLINE_CURVE(5,(#98729,#98730,#98731,#98732,#98733,#98734,#98735,#98736,
#98737,#98738,#98739,#98740,#98741,#98742,#98743,#98744,#98745,#98746,#98747,
#98748,#98749,#98750,#98751,#98752,#98753,#98754,#98755,#98756,#98757,#98758,
#98759,#98760,#98761,#98762,#98763,#98764,#98765,#98766,#98767,#98768,#98769,
#98770,#98771,#98772,#98773,#98774,#98775,#98776,#98777,#98778,#98779,#98780,
#98781,#98782,#98783,#98784,#98785,#98786,#98787,#98788,#98789,#98790,#98791,
#98792,#98793,#98794,#98795,#98796,#98797,#98798,#98799,#98800,#98801,#98802,
#98803,#98804,#98805,#98806,#98807,#98808,#98809,#98810,#98811,#98812,#98813,
#98814,#98815,#98816,#98817,#98818,#98819,#98820,#98821,#98822,#98823,#98824,
#98825,#98826,#98827,#98828,#98829,#98830,#98831,#98832,#98833,#98834,#98835,
#98836,#98837,#98838,#98839,#98840,#98841,#98842,#98843,#98844,#98845,#98846,
#98847,#98848,#98849,#98850,#98851,#98852,#98853,#98854,#98855,#98856,#98857,
#98858,#98859,#98860,#98861,#98862,#98863,#98864,#98865,#98866,#98867,#98868,
#98869,#98870,#98871,#98872,#98873,#98874,#98875,#98876,#98877,#98878,#98879,
#98880,#98881,#98882,#98883,#98884,#98885,#98886,#98887,#98888,#98889,#98890,
#98891,#98892,#98893,#98894,#98895,#98896,#98897,#98898,#98899,#98900,#98901,
#98902,#98903,#98904,#98905,#98906,#98907,#98908,#98909,#98910,#98911,#98912,
#98913,#98914,#98915,#98916,#98917,#98918,#98919,#98920,#98921,#98922),
 .UNSPECIFIED.,.F.,.F.)
B_SPLINE_CURVE_WITH_KNOTS((6,1,1,1,1,1,1,1,1,1,1,1,1,1,1,1,1,1,1,1,1,1,
1,1,1,1,1,1,1,1,1,1,1,1,1,1,1,1,1,1,1,1,1,1,1,1,1,1,1,1,1,1,1,1,1,1,1,1,
1,1,1,1,1,1,1,1,1,1,1,1,1,1,1,1,1,1,1,1,1,1,1,1,1,1,1,1,1,1,1,1,1,1,1,1,
1,1,1,1,1,1,1,1,1,1,1,1,1,1,1,1,1,1,1,1,1,1,1,1,1,1,1,1,1,1,1,1,1,1,1,1,
1,1,1,1,1,1,1,1,1,1,1,1,1,1,1,1,1,1,1,1,1,1,1,1,1,1,1,1,1,1,1,1,1,1,1,1,
1,1,1,1,1,1,1,1,1,1,1,1,1,1,1,1,1,1,1,1,1,1,1,6),(0.,0.005,0.01,0.015,0.02,
0.025,0.03,0.035,0.04,0.045,0.05,0.055,0.06,0.065,0.07,0.075,0.08,0.085,
0.09,0.095,0.1,0.105,0.11,0.115,0.12,0.125,0.13,0.135,0.14,0.145,0.15,0.155,
0.16,0.165,0.17,0.175,0.18,0.185,0.19,0.195,0.2,0.205,0.21,0.215,0.22,0.225,
0.23,0.235,0.24,0.245,0.25,0.255,0.26,0.265,0.27,0.275,0.28,0.285,0.29,
0.295,0.3,0.305,0.31,0.315,0.32,0.325,0.33,0.335,0.34,0.345,0.35,0.355,
0.36,0.365,0.37,0.375,0.38,0.385,0.39,0.395,0.4,0.405,0.41,0.415,0.42,0.425,
0.43,0.435,0.44,0.445,0.45,0.455,0.46,0.465,0.47,0.475,0.48,0.485,0.49,
0.495,0.5,0.505,0.51,0.515,0.52,0.525,0.53,0.535,0.54,0.545,0.55,0.555,
0.56,0.565,0.57,0.575,0.58,0.585,0.59,0.595,0.6,0.605,0.61,0.615,0.62,0.625,
0.63,0.635,0.64,0.645,0.65,0.655,0.66,0.665,0.67,0.675,0.68,0.685,0.690000000000001,
0.695000000000001,0.700000000000001,0.705000000000001,0.710000000000001,
0.715000000000001,0.720000000000001,0.725000000000001,0.730000000000001,
0.735000000000001,0.740000000000001,0.745000000000001,0.750000000000001,
0.755000000000001,0.760000000000001,0.765000000000001,0.770000000000001,
0.775000000000001,0.780000000000001,0.785000000000001,0.790000000000001,
0.795000000000001,0.800000000000001,0.805000000000001,0.810000000000001,
0.815000000000001,0.820000000000001,0.825000000000001,0.830000000000001,
0.835000000000001,0.840000000000001,0.845000000000001,0.850000000000001,
0.855000000000001,0.860000000000001,0.865000000000001,0.870000000000001,
0.875000000000001,0.880000000000001,0.885000000000001,0.890000000000001,
0.895000000000001,0.900000000000001,0.905000000000001,0.910000000000001,
0.915000000000001,0.920000000000001,0.925000000000001,0.930000000000001,
0.935000000000001,0.940000000000001,0.941429844431381),.UNSPECIFIED.)
CURVE()
GEOMETRIC_REPRESENTATION_ITEM()
RATIONAL_B_SPLINE_CURVE((1.,1.,1.,1.,1.,1.,1.,1.,1.,1.,1.,1.,1.,1.,1.,1.,
1.,1.,1.,1.,1.,1.,1.,1.,1.,1.,1.,1.,1.,1.,1.,1.,1.,1.,1.,1.,1.,1.,1.,1.,
1.,1.,1.,1.,1.,1.,1.,1.,1.,1.,1.,1.,1.,1.,1.,1.,1.,1.,1.,1.,1.,1.,1.,1.,
1.,1.,1.,1.,1.,1.,1.,1.,1.,1.,1.,1.,1.,1.,1.,1.,1.,1.,1.,1.,1.,1.,1.,1.,
1.,1.,1.,1.,1.,1.,1.,1.,1.,1.,1.,1.,1.,1.,1.,1.,1.,1.,1.,1.,1.,1.,1.,1.,
1.,1.,1.,1.,1.,1.,1.,1.,1.,1.,1.,1.,1.,1.,1.,1.,1.,1.,1.,1.,1.,1.,1.,1.,
1.,1.,1.,1.,1.,1.,1.,1.,1.,1.,1.,1.,1.,1.,1.,1.,1.,1.,1.,1.,1.,1.,1.,1.,
1.,1.,1.,1.,1.,1.,1.,1.,1.,1.,1.,1.,1.,1.,1.,1.,1.,1.,1.,1.,1.,1.,1.,1.,
1.,1.,1.,1.,1.,1.,1.,1.,1.,1.))
REPRESENTATION_ITEM('')
);
#506=(
BOUNDED_CURVE()
B_SPLINE_CURVE(5,(#98925,#98926,#98927,#98928,#98929,#98930,#98931,#98932,
#98933,#98934,#98935,#98936,#98937,#98938,#98939,#98940,#98941,#98942,#98943,
#98944,#98945,#98946,#98947,#98948,#98949,#98950,#98951,#98952,#98953,#98954,
#98955,#98956,#98957,#98958,#98959,#98960,#98961,#98962,#98963,#98964,#98965,
#98966,#98967,#98968,#98969,#98970,#98971,#98972,#98973,#98974,#98975,#98976,
#98977,#98978,#98979,#98980,#98981,#98982,#98983,#98984,#98985,#98986,#98987,
#98988,#98989,#98990,#98991,#98992,#98993,#98994,#98995,#98996,#98997,#98998,
#98999,#99000,#99001,#99002,#99003,#99004,#99005,#99006,#99007,#99008,#99009,
#99010,#99011,#99012,#99013,#99014,#99015,#99016,#99017,#99018,#99019,#99020,
#99021,#99022,#99023,#99024,#99025,#99026,#99027,#99028,#99029,#99030,#99031,
#99032,#99033,#99034,#99035,#99036,#99037,#99038,#99039,#99040,#99041,#99042,
#99043,#99044,#99045,#99046,#99047,#99048,#99049,#99050,#99051,#99052,#99053,
#99054,#99055,#99056,#99057,#99058,#99059,#99060,#99061,#99062,#99063,#99064,
#99065,#99066,#99067,#99068,#99069,#99070,#99071,#99072,#99073,#99074,#99075,
#99076,#99077,#99078,#99079,#99080,#99081,#99082,#99083,#99084,#99085,#99086,
#99087,#99088,#99089,#99090,#99091,#99092,#99093,#99094,#99095,#99096,#99097,
#99098,#99099,#99100,#99101,#99102,#99103,#99104,#99105,#99106,#99107,#99108,
#99109,#99110,#99111,#99112,#99113,#99114,#99115,#99116,#99117,#99118),
 .UNSPECIFIED.,.F.,.F.)
B_SPLINE_CURVE_WITH_KNOTS((6,1,1,1,1,1,1,1,1,1,1,1,1,1,1,1,1,1,1,1,1,1,
1,1,1,1,1,1,1,1,1,1,1,1,1,1,1,1,1,1,1,1,1,1,1,1,1,1,1,1,1,1,1,1,1,1,1,1,
1,1,1,1,1,1,1,1,1,1,1,1,1,1,1,1,1,1,1,1,1,1,1,1,1,1,1,1,1,1,1,1,1,1,1,1,
1,1,1,1,1,1,1,1,1,1,1,1,1,1,1,1,1,1,1,1,1,1,1,1,1,1,1,1,1,1,1,1,1,1,1,1,
1,1,1,1,1,1,1,1,1,1,1,1,1,1,1,1,1,1,1,1,1,1,1,1,1,1,1,1,1,1,1,1,1,1,1,1,
1,1,1,1,1,1,1,1,1,1,1,1,1,1,1,1,1,1,1,1,1,1,1,6),(-0.941429844431409,-0.940000000000001,
-0.935000000000001,-0.930000000000001,-0.925000000000001,-0.920000000000001,
-0.915000000000001,-0.910000000000001,-0.905000000000001,-0.900000000000001,
-0.895000000000001,-0.890000000000001,-0.885000000000001,-0.880000000000001,
-0.875000000000001,-0.870000000000001,-0.865000000000001,-0.860000000000001,
-0.855000000000001,-0.850000000000001,-0.845000000000001,-0.840000000000001,
-0.835000000000001,-0.830000000000001,-0.825000000000001,-0.820000000000001,
-0.815000000000001,-0.810000000000001,-0.805000000000001,-0.800000000000001,
-0.795000000000001,-0.790000000000001,-0.785000000000001,-0.780000000000001,
-0.775000000000001,-0.770000000000001,-0.765000000000001,-0.760000000000001,
-0.755000000000001,-0.750000000000001,-0.745000000000001,-0.740000000000001,
-0.735000000000001,-0.730000000000001,-0.725000000000001,-0.720000000000001,
-0.715000000000001,-0.710000000000001,-0.705000000000001,-0.700000000000001,
-0.695000000000001,-0.690000000000001,-0.685,-0.68,-0.675,-0.67,-0.665,
-0.66,-0.655,-0.65,-0.645,-0.64,-0.635,-0.63,-0.625,-0.62,-0.615,-0.61,
-0.605,-0.6,-0.595,-0.59,-0.585,-0.58,-0.575,-0.57,-0.565,-0.56,-0.555,
-0.55,-0.545,-0.54,-0.535,-0.53,-0.525,-0.52,-0.515,-0.51,-0.505,-0.5,-0.495,
-0.49,-0.485,-0.48,-0.475,-0.47,-0.465,-0.46,-0.455,-0.45,-0.445,-0.44,
-0.435,-0.43,-0.425,-0.42,-0.415,-0.41,-0.405,-0.4,-0.395,-0.39,-0.385,
-0.38,-0.375,-0.37,-0.365,-0.36,-0.355,-0.35,-0.345,-0.34,-0.335,-0.33,
-0.325,-0.32,-0.315,-0.31,-0.305,-0.3,-0.295,-0.29,-0.285,-0.28,-0.275,
-0.27,-0.265,-0.26,-0.255,-0.25,-0.245,-0.24,-0.235,-0.23,-0.225,-0.22,
-0.215,-0.21,-0.205,-0.2,-0.195,-0.19,-0.185,-0.18,-0.175,-0.17,-0.165,
-0.16,-0.155,-0.15,-0.145,-0.14,-0.135,-0.13,-0.125,-0.12,-0.115,-0.11,
-0.105,-0.1,-0.095,-0.09,-0.085,-0.08,-0.075,-0.07,-0.065,-0.06,-0.055,
-0.05,-0.045,-0.04,-0.035,-0.03,-0.025,-0.02,-0.015,-0.01,-0.005,0.),
 .UNSPECIFIED.)
CURVE()
GEOMETRIC_REPRESENTATION_ITEM()
RATIONAL_B_SPLINE_CURVE((1.,1.,1.,1.,1.,1.,1.,1.,1.,1.,1.,1.,1.,1.,1.,1.,
1.,1.,1.,1.,1.,1.,1.,1.,1.,1.,1.,1.,1.,1.,1.,1.,1.,1.,1.,1.,1.,1.,1.,1.,
1.,1.,1.,1.,1.,1.,1.,1.,1.,1.,1.,1.,1.,1.,1.,1.,1.,1.,1.,1.,1.,1.,1.,1.,
1.,1.,1.,1.,1.,1.,1.,1.,1.,1.,1.,1.,1.,1.,1.,1.,1.,1.,1.,1.,1.,1.,1.,1.,
1.,1.,1.,1.,1.,1.,1.,1.,1.,1.,1.,1.,1.,1.,1.,1.,1.,1.,1.,1.,1.,1.,1.,1.,
1.,1.,1.,1.,1.,1.,1.,1.,1.,1.,1.,1.,1.,1.,1.,1.,1.,1.,1.,1.,1.,1.,1.,1.,
1.,1.,1.,1.,1.,1.,1.,1.,1.,1.,1.,1.,1.,1.,1.,1.,1.,1.,1.,1.,1.,1.,1.,1.,
1.,1.,1.,1.,1.,1.,1.,1.,1.,1.,1.,1.,1.,1.,1.,1.,1.,1.,1.,1.,1.,1.,1.,1.,
1.,1.,1.,1.,1.,1.,1.,1.,1.,1.))
REPRESENTATION_ITEM('')
);
#507=(
BOUNDED_CURVE()
B_SPLINE_CURVE(5,(#99625,#99626,#99627,#99628,#99629,#99630,#99631,#99632,
#99633,#99634,#99635,#99636,#99637,#99638,#99639,#99640,#99641,#99642,#99643,
#99644,#99645,#99646,#99647,#99648,#99649,#99650,#99651,#99652,#99653,#99654,
#99655,#99656,#99657,#99658,#99659,#99660,#99661,#99662,#99663,#99664,#99665,
#99666,#99667,#99668,#99669,#99670,#99671,#99672,#99673,#99674,#99675,#99676,
#99677,#99678,#99679,#99680,#99681,#99682,#99683,#99684,#99685,#99686,#99687,
#99688,#99689,#99690,#99691,#99692,#99693,#99694,#99695,#99696,#99697,#99698,
#99699,#99700,#99701,#99702,#99703,#99704,#99705,#99706,#99707,#99708,#99709,
#99710,#99711,#99712,#99713,#99714,#99715,#99716,#99717,#99718,#99719,#99720,
#99721,#99722,#99723,#99724,#99725,#99726,#99727,#99728,#99729,#99730,#99731,
#99732,#99733,#99734,#99735,#99736,#99737,#99738,#99739,#99740,#99741,#99742,
#99743,#99744,#99745,#99746,#99747,#99748,#99749,#99750,#99751,#99752,#99753,
#99754,#99755,#99756,#99757,#99758,#99759,#99760,#99761,#99762,#99763,#99764,
#99765,#99766,#99767,#99768,#99769,#99770,#99771,#99772,#99773,#99774,#99775,
#99776,#99777,#99778,#99779,#99780,#99781,#99782,#99783,#99784,#99785,#99786,
#99787,#99788,#99789,#99790,#99791,#99792,#99793,#99794,#99795,#99796,#99797,
#99798,#99799,#99800,#99801,#99802,#99803,#99804,#99805,#99806,#99807,#99808,
#99809,#99810,#99811,#99812,#99813,#99814,#99815,#99816,#99817,#99818),
 .UNSPECIFIED.,.F.,.F.)
B_SPLINE_CURVE_WITH_KNOTS((6,1,1,1,1,1,1,1,1,1,1,1,1,1,1,1,1,1,1,1,1,1,
1,1,1,1,1,1,1,1,1,1,1,1,1,1,1,1,1,1,1,1,1,1,1,1,1,1,1,1,1,1,1,1,1,1,1,1,
1,1,1,1,1,1,1,1,1,1,1,1,1,1,1,1,1,1,1,1,1,1,1,1,1,1,1,1,1,1,1,1,1,1,1,1,
1,1,1,1,1,1,1,1,1,1,1,1,1,1,1,1,1,1,1,1,1,1,1,1,1,1,1,1,1,1,1,1,1,1,1,1,
1,1,1,1,1,1,1,1,1,1,1,1,1,1,1,1,1,1,1,1,1,1,1,1,1,1,1,1,1,1,1,1,1,1,1,1,
1,1,1,1,1,1,1,1,1,1,1,1,1,1,1,1,1,1,1,1,1,1,1,6),(0.,0.005,0.01,0.015,0.02,
0.025,0.03,0.035,0.04,0.045,0.05,0.055,0.06,0.065,0.07,0.075,0.08,0.085,
0.09,0.095,0.1,0.105,0.11,0.115,0.12,0.125,0.13,0.135,0.14,0.145,0.15,0.155,
0.16,0.165,0.17,0.175,0.18,0.185,0.19,0.195,0.2,0.205,0.21,0.215,0.22,0.225,
0.23,0.235,0.24,0.245,0.25,0.255,0.26,0.265,0.27,0.275,0.28,0.285,0.29,
0.295,0.3,0.305,0.31,0.315,0.32,0.325,0.33,0.335,0.34,0.345,0.35,0.355,
0.36,0.365,0.37,0.375,0.38,0.385,0.39,0.395,0.4,0.405,0.41,0.415,0.42,0.425,
0.43,0.435,0.44,0.445,0.45,0.455,0.46,0.465,0.47,0.475,0.48,0.485,0.49,
0.495,0.5,0.505,0.51,0.515,0.52,0.525,0.53,0.535,0.54,0.545,0.55,0.555,
0.56,0.565,0.57,0.575,0.58,0.585,0.59,0.595,0.6,0.605,0.61,0.615,0.62,0.625,
0.63,0.635,0.64,0.645,0.65,0.655,0.66,0.665,0.67,0.675,0.68,0.685,0.690000000000001,
0.695000000000001,0.700000000000001,0.705000000000001,0.710000000000001,
0.715000000000001,0.720000000000001,0.725000000000001,0.730000000000001,
0.735000000000001,0.740000000000001,0.745000000000001,0.750000000000001,
0.755000000000001,0.760000000000001,0.765000000000001,0.770000000000001,
0.775000000000001,0.780000000000001,0.785000000000001,0.790000000000001,
0.795000000000001,0.800000000000001,0.805000000000001,0.810000000000001,
0.815000000000001,0.820000000000001,0.825000000000001,0.830000000000001,
0.835000000000001,0.840000000000001,0.845000000000001,0.850000000000001,
0.855000000000001,0.860000000000001,0.865000000000001,0.870000000000001,
0.875000000000001,0.880000000000001,0.885000000000001,0.890000000000001,
0.895000000000001,0.900000000000001,0.905000000000001,0.910000000000001,
0.915000000000001,0.920000000000001,0.925000000000001,0.930000000000001,
0.935000000000001,0.940000000000001,0.941429844431327),.UNSPECIFIED.)
CURVE()
GEOMETRIC_REPRESENTATION_ITEM()
RATIONAL_B_SPLINE_CURVE((1.,1.,1.,1.,1.,1.,1.,1.,1.,1.,1.,1.,1.,1.,1.,1.,
1.,1.,1.,1.,1.,1.,1.,1.,1.,1.,1.,1.,1.,1.,1.,1.,1.,1.,1.,1.,1.,1.,1.,1.,
1.,1.,1.,1.,1.,1.,1.,1.,1.,1.,1.,1.,1.,1.,1.,1.,1.,1.,1.,1.,1.,1.,1.,1.,
1.,1.,1.,1.,1.,1.,1.,1.,1.,1.,1.,1.,1.,1.,1.,1.,1.,1.,1.,1.,1.,1.,1.,1.,
1.,1.,1.,1.,1.,1.,1.,1.,1.,1.,1.,1.,1.,1.,1.,1.,1.,1.,1.,1.,1.,1.,1.,1.,
1.,1.,1.,1.,1.,1.,1.,1.,1.,1.,1.,1.,1.,1.,1.,1.,1.,1.,1.,1.,1.,1.,1.,1.,
1.,1.,1.,1.,1.,1.,1.,1.,1.,1.,1.,1.,1.,1.,1.,1.,1.,1.,1.,1.,1.,1.,1.,1.,
1.,1.,1.,1.,1.,1.,1.,1.,1.,1.,1.,1.,1.,1.,1.,1.,1.,1.,1.,1.,1.,1.,1.,1.,
1.,1.,1.,1.,1.,1.,1.,1.,1.,1.))
REPRESENTATION_ITEM('')
);
#508=(
BOUNDED_CURVE()
B_SPLINE_CURVE(5,(#99821,#99822,#99823,#99824,#99825,#99826,#99827,#99828,
#99829,#99830,#99831,#99832,#99833,#99834,#99835,#99836,#99837,#99838,#99839,
#99840,#99841,#99842,#99843,#99844,#99845,#99846,#99847,#99848,#99849,#99850,
#99851,#99852,#99853,#99854,#99855,#99856,#99857,#99858,#99859,#99860,#99861,
#99862,#99863,#99864,#99865,#99866,#99867,#99868,#99869,#99870,#99871,#99872,
#99873,#99874,#99875,#99876,#99877,#99878,#99879,#99880,#99881,#99882,#99883,
#99884,#99885,#99886,#99887,#99888,#99889,#99890,#99891,#99892,#99893,#99894,
#99895,#99896,#99897,#99898,#99899,#99900,#99901,#99902,#99903,#99904,#99905,
#99906,#99907,#99908,#99909,#99910,#99911,#99912,#99913,#99914,#99915,#99916,
#99917,#99918,#99919,#99920,#99921,#99922,#99923,#99924,#99925,#99926,#99927,
#99928,#99929,#99930,#99931,#99932,#99933,#99934,#99935,#99936,#99937,#99938,
#99939,#99940,#99941,#99942,#99943,#99944,#99945,#99946,#99947,#99948,#99949,
#99950,#99951,#99952,#99953,#99954,#99955,#99956,#99957,#99958,#99959,#99960,
#99961,#99962,#99963,#99964,#99965,#99966,#99967,#99968,#99969,#99970,#99971,
#99972,#99973,#99974,#99975,#99976,#99977,#99978,#99979,#99980,#99981,#99982,
#99983,#99984,#99985,#99986,#99987,#99988,#99989,#99990,#99991,#99992,#99993,
#99994,#99995,#99996,#99997,#99998,#99999,#100000,#100001,#100002,#100003,
#100004,#100005,#100006,#100007,#100008,#100009,#100010,#100011,#100012,
#100013,#100014),.UNSPECIFIED.,.F.,.F.)
B_SPLINE_CURVE_WITH_KNOTS((6,1,1,1,1,1,1,1,1,1,1,1,1,1,1,1,1,1,1,1,1,1,
1,1,1,1,1,1,1,1,1,1,1,1,1,1,1,1,1,1,1,1,1,1,1,1,1,1,1,1,1,1,1,1,1,1,1,1,
1,1,1,1,1,1,1,1,1,1,1,1,1,1,1,1,1,1,1,1,1,1,1,1,1,1,1,1,1,1,1,1,1,1,1,1,
1,1,1,1,1,1,1,1,1,1,1,1,1,1,1,1,1,1,1,1,1,1,1,1,1,1,1,1,1,1,1,1,1,1,1,1,
1,1,1,1,1,1,1,1,1,1,1,1,1,1,1,1,1,1,1,1,1,1,1,1,1,1,1,1,1,1,1,1,1,1,1,1,
1,1,1,1,1,1,1,1,1,1,1,1,1,1,1,1,1,1,1,1,1,1,1,6),(-0.941429844431327,-0.940000000000001,
-0.935000000000001,-0.930000000000001,-0.925000000000001,-0.920000000000001,
-0.915000000000001,-0.910000000000001,-0.905000000000001,-0.900000000000001,
-0.895000000000001,-0.890000000000001,-0.885000000000001,-0.880000000000001,
-0.875000000000001,-0.870000000000001,-0.865000000000001,-0.860000000000001,
-0.855000000000001,-0.850000000000001,-0.845000000000001,-0.840000000000001,
-0.835000000000001,-0.830000000000001,-0.825000000000001,-0.820000000000001,
-0.815000000000001,-0.810000000000001,-0.805000000000001,-0.800000000000001,
-0.795000000000001,-0.790000000000001,-0.785000000000001,-0.780000000000001,
-0.775000000000001,-0.770000000000001,-0.765000000000001,-0.760000000000001,
-0.755000000000001,-0.750000000000001,-0.745000000000001,-0.740000000000001,
-0.735000000000001,-0.730000000000001,-0.725000000000001,-0.720000000000001,
-0.715000000000001,-0.710000000000001,-0.705000000000001,-0.700000000000001,
-0.695000000000001,-0.690000000000001,-0.685,-0.68,-0.675,-0.67,-0.665,
-0.66,-0.655,-0.65,-0.645,-0.64,-0.635,-0.63,-0.625,-0.62,-0.615,-0.61,
-0.605,-0.6,-0.595,-0.59,-0.585,-0.58,-0.575,-0.57,-0.565,-0.56,-0.555,
-0.55,-0.545,-0.54,-0.535,-0.53,-0.525,-0.52,-0.515,-0.51,-0.505,-0.5,-0.495,
-0.49,-0.485,-0.48,-0.475,-0.47,-0.465,-0.46,-0.455,-0.45,-0.445,-0.44,
-0.435,-0.43,-0.425,-0.42,-0.415,-0.41,-0.405,-0.4,-0.395,-0.39,-0.385,
-0.38,-0.375,-0.37,-0.365,-0.36,-0.355,-0.35,-0.345,-0.34,-0.335,-0.33,
-0.325,-0.32,-0.315,-0.31,-0.305,-0.3,-0.295,-0.29,-0.285,-0.28,-0.275,
-0.27,-0.265,-0.26,-0.255,-0.25,-0.245,-0.24,-0.235,-0.23,-0.225,-0.22,
-0.215,-0.21,-0.205,-0.2,-0.195,-0.19,-0.185,-0.18,-0.175,-0.17,-0.165,
-0.16,-0.155,-0.15,-0.145,-0.14,-0.135,-0.13,-0.125,-0.12,-0.115,-0.11,
-0.105,-0.1,-0.095,-0.09,-0.085,-0.08,-0.075,-0.07,-0.065,-0.06,-0.055,
-0.05,-0.045,-0.04,-0.035,-0.03,-0.025,-0.02,-0.015,-0.01,-0.005,0.),
 .UNSPECIFIED.)
CURVE()
GEOMETRIC_REPRESENTATION_ITEM()
RATIONAL_B_SPLINE_CURVE((1.,1.,1.,1.,1.,1.,1.,1.,1.,1.,1.,1.,1.,1.,1.,1.,
1.,1.,1.,1.,1.,1.,1.,1.,1.,1.,1.,1.,1.,1.,1.,1.,1.,1.,1.,1.,1.,1.,1.,1.,
1.,1.,1.,1.,1.,1.,1.,1.,1.,1.,1.,1.,1.,1.,1.,1.,1.,1.,1.,1.,1.,1.,1.,1.,
1.,1.,1.,1.,1.,1.,1.,1.,1.,1.,1.,1.,1.,1.,1.,1.,1.,1.,1.,1.,1.,1.,1.,1.,
1.,1.,1.,1.,1.,1.,1.,1.,1.,1.,1.,1.,1.,1.,1.,1.,1.,1.,1.,1.,1.,1.,1.,1.,
1.,1.,1.,1.,1.,1.,1.,1.,1.,1.,1.,1.,1.,1.,1.,1.,1.,1.,1.,1.,1.,1.,1.,1.,
1.,1.,1.,1.,1.,1.,1.,1.,1.,1.,1.,1.,1.,1.,1.,1.,1.,1.,1.,1.,1.,1.,1.,1.,
1.,1.,1.,1.,1.,1.,1.,1.,1.,1.,1.,1.,1.,1.,1.,1.,1.,1.,1.,1.,1.,1.,1.,1.,
1.,1.,1.,1.,1.,1.,1.,1.,1.,1.))
REPRESENTATION_ITEM('')
);
#509=(
BOUNDED_CURVE()
B_SPLINE_CURVE(5,(#100521,#100522,#100523,#100524,#100525,#100526,#100527,
#100528,#100529,#100530,#100531,#100532,#100533,#100534,#100535,#100536,
#100537,#100538,#100539,#100540,#100541,#100542,#100543,#100544,#100545,
#100546,#100547,#100548,#100549,#100550,#100551,#100552,#100553,#100554,
#100555,#100556,#100557,#100558,#100559,#100560,#100561,#100562,#100563,
#100564,#100565,#100566,#100567,#100568,#100569,#100570,#100571,#100572,
#100573,#100574,#100575,#100576,#100577,#100578,#100579,#100580,#100581,
#100582,#100583,#100584,#100585,#100586,#100587,#100588,#100589,#100590,
#100591,#100592,#100593,#100594,#100595,#100596,#100597,#100598,#100599,
#100600,#100601,#100602,#100603,#100604,#100605,#100606,#100607,#100608,
#100609,#100610,#100611,#100612,#100613,#100614,#100615,#100616,#100617,
#100618,#100619,#100620,#100621,#100622,#100623,#100624,#100625,#100626,
#100627,#100628,#100629,#100630,#100631,#100632,#100633,#100634,#100635,
#100636,#100637,#100638,#100639,#100640,#100641,#100642,#100643,#100644,
#100645,#100646,#100647,#100648,#100649,#100650,#100651,#100652,#100653,
#100654,#100655,#100656,#100657,#100658,#100659,#100660,#100661,#100662,
#100663,#100664,#100665,#100666,#100667,#100668,#100669,#100670,#100671,
#100672,#100673,#100674,#100675,#100676,#100677,#100678,#100679,#100680,
#100681,#100682,#100683,#100684,#100685,#100686,#100687,#100688,#100689,
#100690,#100691,#100692,#100693,#100694,#100695,#100696,#100697,#100698,
#100699,#100700,#100701,#100702,#100703,#100704,#100705,#100706,#100707,
#100708,#100709,#100710,#100711,#100712,#100713,#100714),.UNSPECIFIED.,
 .F.,.F.)
B_SPLINE_CURVE_WITH_KNOTS((6,1,1,1,1,1,1,1,1,1,1,1,1,1,1,1,1,1,1,1,1,1,
1,1,1,1,1,1,1,1,1,1,1,1,1,1,1,1,1,1,1,1,1,1,1,1,1,1,1,1,1,1,1,1,1,1,1,1,
1,1,1,1,1,1,1,1,1,1,1,1,1,1,1,1,1,1,1,1,1,1,1,1,1,1,1,1,1,1,1,1,1,1,1,1,
1,1,1,1,1,1,1,1,1,1,1,1,1,1,1,1,1,1,1,1,1,1,1,1,1,1,1,1,1,1,1,1,1,1,1,1,
1,1,1,1,1,1,1,1,1,1,1,1,1,1,1,1,1,1,1,1,1,1,1,1,1,1,1,1,1,1,1,1,1,1,1,1,
1,1,1,1,1,1,1,1,1,1,1,1,1,1,1,1,1,1,1,1,1,1,1,6),(0.,0.005,0.01,0.015,0.02,
0.025,0.03,0.035,0.04,0.045,0.05,0.055,0.06,0.065,0.07,0.075,0.08,0.085,
0.09,0.095,0.1,0.105,0.11,0.115,0.12,0.125,0.13,0.135,0.14,0.145,0.15,0.155,
0.16,0.165,0.17,0.175,0.18,0.185,0.19,0.195,0.2,0.205,0.21,0.215,0.22,0.225,
0.23,0.235,0.24,0.245,0.25,0.255,0.26,0.265,0.27,0.275,0.28,0.285,0.29,
0.295,0.3,0.305,0.31,0.315,0.32,0.325,0.33,0.335,0.34,0.345,0.35,0.355,
0.36,0.365,0.37,0.375,0.38,0.385,0.39,0.395,0.4,0.405,0.41,0.415,0.42,0.425,
0.43,0.435,0.44,0.445,0.45,0.455,0.46,0.465,0.47,0.475,0.48,0.485,0.49,
0.495,0.5,0.505,0.51,0.515,0.52,0.525,0.53,0.535,0.54,0.545,0.55,0.555,
0.56,0.565,0.57,0.575,0.58,0.585,0.59,0.595,0.6,0.605,0.61,0.615,0.62,0.625,
0.63,0.635,0.64,0.645,0.65,0.655,0.66,0.665,0.67,0.675,0.68,0.685,0.690000000000001,
0.695000000000001,0.700000000000001,0.705000000000001,0.710000000000001,
0.715000000000001,0.720000000000001,0.725000000000001,0.730000000000001,
0.735000000000001,0.740000000000001,0.745000000000001,0.750000000000001,
0.755000000000001,0.760000000000001,0.765000000000001,0.770000000000001,
0.775000000000001,0.780000000000001,0.785000000000001,0.790000000000001,
0.795000000000001,0.800000000000001,0.805000000000001,0.810000000000001,
0.815000000000001,0.820000000000001,0.825000000000001,0.830000000000001,
0.835000000000001,0.840000000000001,0.845000000000001,0.850000000000001,
0.855000000000001,0.860000000000001,0.865000000000001,0.870000000000001,
0.875000000000001,0.880000000000001,0.885000000000001,0.890000000000001,
0.895000000000001,0.900000000000001,0.905000000000001,0.910000000000001,
0.915000000000001,0.920000000000001,0.925000000000001,0.930000000000001,
0.935000000000001,0.940000000000001,0.94142984443144),.UNSPECIFIED.)
CURVE()
GEOMETRIC_REPRESENTATION_ITEM()
RATIONAL_B_SPLINE_CURVE((1.,1.,1.,1.,1.,1.,1.,1.,1.,1.,1.,1.,1.,1.,1.,1.,
1.,1.,1.,1.,1.,1.,1.,1.,1.,1.,1.,1.,1.,1.,1.,1.,1.,1.,1.,1.,1.,1.,1.,1.,
1.,1.,1.,1.,1.,1.,1.,1.,1.,1.,1.,1.,1.,1.,1.,1.,1.,1.,1.,1.,1.,1.,1.,1.,
1.,1.,1.,1.,1.,1.,1.,1.,1.,1.,1.,1.,1.,1.,1.,1.,1.,1.,1.,1.,1.,1.,1.,1.,
1.,1.,1.,1.,1.,1.,1.,1.,1.,1.,1.,1.,1.,1.,1.,1.,1.,1.,1.,1.,1.,1.,1.,1.,
1.,1.,1.,1.,1.,1.,1.,1.,1.,1.,1.,1.,1.,1.,1.,1.,1.,1.,1.,1.,1.,1.,1.,1.,
1.,1.,1.,1.,1.,1.,1.,1.,1.,1.,1.,1.,1.,1.,1.,1.,1.,1.,1.,1.,1.,1.,1.,1.,
1.,1.,1.,1.,1.,1.,1.,1.,1.,1.,1.,1.,1.,1.,1.,1.,1.,1.,1.,1.,1.,1.,1.,1.,
1.,1.,1.,1.,1.,1.,1.,1.,1.,1.))
REPRESENTATION_ITEM('')
);
#510=(
BOUNDED_CURVE()
B_SPLINE_CURVE(5,(#100717,#100718,#100719,#100720,#100721,#100722,#100723,
#100724,#100725,#100726,#100727,#100728,#100729,#100730,#100731,#100732,
#100733,#100734,#100735,#100736,#100737,#100738,#100739,#100740,#100741,
#100742,#100743,#100744,#100745,#100746,#100747,#100748,#100749,#100750,
#100751,#100752,#100753,#100754,#100755,#100756,#100757,#100758,#100759,
#100760,#100761,#100762,#100763,#100764,#100765,#100766,#100767,#100768,
#100769,#100770,#100771,#100772,#100773,#100774,#100775,#100776,#100777,
#100778,#100779,#100780,#100781,#100782,#100783,#100784,#100785,#100786,
#100787,#100788,#100789,#100790,#100791,#100792,#100793,#100794,#100795,
#100796,#100797,#100798,#100799,#100800,#100801,#100802,#100803,#100804,
#100805,#100806,#100807,#100808,#100809,#100810,#100811,#100812,#100813,
#100814,#100815,#100816,#100817,#100818,#100819,#100820,#100821,#100822,
#100823,#100824,#100825,#100826,#100827,#100828,#100829,#100830,#100831,
#100832,#100833,#100834,#100835,#100836,#100837,#100838,#100839,#100840,
#100841,#100842,#100843,#100844,#100845,#100846,#100847,#100848,#100849,
#100850,#100851,#100852,#100853,#100854,#100855,#100856,#100857,#100858,
#100859,#100860,#100861,#100862,#100863,#100864,#100865,#100866,#100867,
#100868,#100869,#100870,#100871,#100872,#100873,#100874,#100875,#100876,
#100877,#100878,#100879,#100880,#100881,#100882,#100883,#100884,#100885,
#100886,#100887,#100888,#100889,#100890,#100891,#100892,#100893,#100894,
#100895,#100896,#100897,#100898,#100899,#100900,#100901,#100902,#100903,
#100904,#100905,#100906,#100907,#100908,#100909,#100910),.UNSPECIFIED.,
 .F.,.F.)
B_SPLINE_CURVE_WITH_KNOTS((6,1,1,1,1,1,1,1,1,1,1,1,1,1,1,1,1,1,1,1,1,1,
1,1,1,1,1,1,1,1,1,1,1,1,1,1,1,1,1,1,1,1,1,1,1,1,1,1,1,1,1,1,1,1,1,1,1,1,
1,1,1,1,1,1,1,1,1,1,1,1,1,1,1,1,1,1,1,1,1,1,1,1,1,1,1,1,1,1,1,1,1,1,1,1,
1,1,1,1,1,1,1,1,1,1,1,1,1,1,1,1,1,1,1,1,1,1,1,1,1,1,1,1,1,1,1,1,1,1,1,1,
1,1,1,1,1,1,1,1,1,1,1,1,1,1,1,1,1,1,1,1,1,1,1,1,1,1,1,1,1,1,1,1,1,1,1,1,
1,1,1,1,1,1,1,1,1,1,1,1,1,1,1,1,1,1,1,1,1,1,1,6),(-0.941429844431447,-0.940000000000001,
-0.935000000000001,-0.930000000000001,-0.925000000000001,-0.920000000000001,
-0.915000000000001,-0.910000000000001,-0.905000000000001,-0.900000000000001,
-0.895000000000001,-0.890000000000001,-0.885000000000001,-0.880000000000001,
-0.875000000000001,-0.870000000000001,-0.865000000000001,-0.860000000000001,
-0.855000000000001,-0.850000000000001,-0.845000000000001,-0.840000000000001,
-0.835000000000001,-0.830000000000001,-0.825000000000001,-0.820000000000001,
-0.815000000000001,-0.810000000000001,-0.805000000000001,-0.800000000000001,
-0.795000000000001,-0.790000000000001,-0.785000000000001,-0.780000000000001,
-0.775000000000001,-0.770000000000001,-0.765000000000001,-0.760000000000001,
-0.755000000000001,-0.750000000000001,-0.745000000000001,-0.740000000000001,
-0.735000000000001,-0.730000000000001,-0.725000000000001,-0.720000000000001,
-0.715000000000001,-0.710000000000001,-0.705000000000001,-0.700000000000001,
-0.695000000000001,-0.690000000000001,-0.685,-0.68,-0.675,-0.67,-0.665,
-0.66,-0.655,-0.65,-0.645,-0.64,-0.635,-0.63,-0.625,-0.62,-0.615,-0.61,
-0.605,-0.6,-0.595,-0.59,-0.585,-0.58,-0.575,-0.57,-0.565,-0.56,-0.555,
-0.55,-0.545,-0.54,-0.535,-0.53,-0.525,-0.52,-0.515,-0.51,-0.505,-0.5,-0.495,
-0.49,-0.485,-0.48,-0.475,-0.47,-0.465,-0.46,-0.455,-0.45,-0.445,-0.44,
-0.435,-0.43,-0.425,-0.42,-0.415,-0.41,-0.405,-0.4,-0.395,-0.39,-0.385,
-0.38,-0.375,-0.37,-0.365,-0.36,-0.355,-0.35,-0.345,-0.34,-0.335,-0.33,
-0.325,-0.32,-0.315,-0.31,-0.305,-0.3,-0.295,-0.29,-0.285,-0.28,-0.275,
-0.27,-0.265,-0.26,-0.255,-0.25,-0.245,-0.24,-0.235,-0.23,-0.225,-0.22,
-0.215,-0.21,-0.205,-0.2,-0.195,-0.19,-0.185,-0.18,-0.175,-0.17,-0.165,
-0.16,-0.155,-0.15,-0.145,-0.14,-0.135,-0.13,-0.125,-0.12,-0.115,-0.11,
-0.105,-0.1,-0.095,-0.09,-0.085,-0.08,-0.075,-0.07,-0.065,-0.06,-0.055,
-0.05,-0.045,-0.04,-0.035,-0.03,-0.025,-0.02,-0.015,-0.01,-0.005,0.),
 .UNSPECIFIED.)
CURVE()
GEOMETRIC_REPRESENTATION_ITEM()
RATIONAL_B_SPLINE_CURVE((1.,1.,1.,1.,1.,1.,1.,1.,1.,1.,1.,1.,1.,1.,1.,1.,
1.,1.,1.,1.,1.,1.,1.,1.,1.,1.,1.,1.,1.,1.,1.,1.,1.,1.,1.,1.,1.,1.,1.,1.,
1.,1.,1.,1.,1.,1.,1.,1.,1.,1.,1.,1.,1.,1.,1.,1.,1.,1.,1.,1.,1.,1.,1.,1.,
1.,1.,1.,1.,1.,1.,1.,1.,1.,1.,1.,1.,1.,1.,1.,1.,1.,1.,1.,1.,1.,1.,1.,1.,
1.,1.,1.,1.,1.,1.,1.,1.,1.,1.,1.,1.,1.,1.,1.,1.,1.,1.,1.,1.,1.,1.,1.,1.,
1.,1.,1.,1.,1.,1.,1.,1.,1.,1.,1.,1.,1.,1.,1.,1.,1.,1.,1.,1.,1.,1.,1.,1.,
1.,1.,1.,1.,1.,1.,1.,1.,1.,1.,1.,1.,1.,1.,1.,1.,1.,1.,1.,1.,1.,1.,1.,1.,
1.,1.,1.,1.,1.,1.,1.,1.,1.,1.,1.,1.,1.,1.,1.,1.,1.,1.,1.,1.,1.,1.,1.,1.,
1.,1.,1.,1.,1.,1.,1.,1.,1.,1.))
REPRESENTATION_ITEM('')
);
#511=(
BOUNDED_CURVE()
B_SPLINE_CURVE(5,(#101417,#101418,#101419,#101420,#101421,#101422,#101423,
#101424,#101425,#101426,#101427,#101428,#101429,#101430,#101431,#101432,
#101433,#101434,#101435,#101436,#101437,#101438,#101439,#101440,#101441,
#101442,#101443,#101444,#101445,#101446,#101447,#101448,#101449,#101450,
#101451,#101452,#101453,#101454,#101455,#101456,#101457,#101458,#101459,
#101460,#101461,#101462,#101463,#101464,#101465,#101466,#101467,#101468,
#101469,#101470,#101471,#101472,#101473,#101474,#101475,#101476,#101477,
#101478,#101479,#101480,#101481,#101482,#101483,#101484,#101485,#101486,
#101487,#101488,#101489,#101490,#101491,#101492,#101493,#101494,#101495,
#101496,#101497,#101498,#101499,#101500,#101501,#101502,#101503,#101504,
#101505,#101506,#101507,#101508,#101509,#101510,#101511,#101512,#101513,
#101514,#101515,#101516,#101517,#101518,#101519,#101520,#101521,#101522,
#101523,#101524,#101525,#101526,#101527,#101528,#101529,#101530,#101531,
#101532,#101533,#101534,#101535,#101536,#101537,#101538,#101539,#101540,
#101541,#101542,#101543,#101544,#101545,#101546,#101547,#101548,#101549,
#101550,#101551,#101552,#101553,#101554,#101555,#101556,#101557,#101558,
#101559,#101560,#101561,#101562,#101563,#101564,#101565,#101566,#101567,
#101568,#101569,#101570,#101571,#101572,#101573,#101574,#101575,#101576,
#101577,#101578,#101579,#101580,#101581,#101582,#101583,#101584,#101585,
#101586,#101587,#101588,#101589,#101590,#101591,#101592,#101593,#101594,
#101595,#101596,#101597,#101598,#101599,#101600,#101601,#101602,#101603,
#101604,#101605,#101606,#101607,#101608,#101609,#101610),.UNSPECIFIED.,
 .F.,.F.)
B_SPLINE_CURVE_WITH_KNOTS((6,1,1,1,1,1,1,1,1,1,1,1,1,1,1,1,1,1,1,1,1,1,
1,1,1,1,1,1,1,1,1,1,1,1,1,1,1,1,1,1,1,1,1,1,1,1,1,1,1,1,1,1,1,1,1,1,1,1,
1,1,1,1,1,1,1,1,1,1,1,1,1,1,1,1,1,1,1,1,1,1,1,1,1,1,1,1,1,1,1,1,1,1,1,1,
1,1,1,1,1,1,1,1,1,1,1,1,1,1,1,1,1,1,1,1,1,1,1,1,1,1,1,1,1,1,1,1,1,1,1,1,
1,1,1,1,1,1,1,1,1,1,1,1,1,1,1,1,1,1,1,1,1,1,1,1,1,1,1,1,1,1,1,1,1,1,1,1,
1,1,1,1,1,1,1,1,1,1,1,1,1,1,1,1,1,1,1,1,1,1,1,6),(0.,0.005,0.01,0.015,0.02,
0.025,0.03,0.035,0.04,0.045,0.05,0.055,0.06,0.065,0.07,0.075,0.08,0.085,
0.09,0.095,0.1,0.105,0.11,0.115,0.12,0.125,0.13,0.135,0.14,0.145,0.15,0.155,
0.16,0.165,0.17,0.175,0.18,0.185,0.19,0.195,0.2,0.205,0.21,0.215,0.22,0.225,
0.23,0.235,0.24,0.245,0.25,0.255,0.26,0.265,0.27,0.275,0.28,0.285,0.29,
0.295,0.3,0.305,0.31,0.315,0.32,0.325,0.33,0.335,0.34,0.345,0.35,0.355,
0.36,0.365,0.37,0.375,0.38,0.385,0.39,0.395,0.4,0.405,0.41,0.415,0.42,0.425,
0.43,0.435,0.44,0.445,0.45,0.455,0.46,0.465,0.47,0.475,0.48,0.485,0.49,
0.495,0.5,0.505,0.51,0.515,0.52,0.525,0.53,0.535,0.54,0.545,0.55,0.555,
0.56,0.565,0.57,0.575,0.58,0.585,0.59,0.595,0.6,0.605,0.61,0.615,0.62,0.625,
0.63,0.635,0.64,0.645,0.65,0.655,0.66,0.665,0.67,0.675,0.68,0.685,0.690000000000001,
0.695000000000001,0.700000000000001,0.705000000000001,0.710000000000001,
0.715000000000001,0.720000000000001,0.725000000000001,0.730000000000001,
0.735000000000001,0.740000000000001,0.745000000000001,0.750000000000001,
0.755000000000001,0.760000000000001,0.765000000000001,0.770000000000001,
0.775000000000001,0.780000000000001,0.785000000000001,0.790000000000001,
0.795000000000001,0.800000000000001,0.805000000000001,0.810000000000001,
0.815000000000001,0.820000000000001,0.825000000000001,0.830000000000001,
0.835000000000001,0.840000000000001,0.845000000000001,0.850000000000001,
0.855000000000001,0.860000000000001,0.865000000000001,0.870000000000001,
0.875000000000001,0.880000000000001,0.885000000000001,0.890000000000001,
0.895000000000001,0.900000000000001,0.905000000000001,0.910000000000001,
0.915000000000001,0.920000000000001,0.925000000000001,0.930000000000001,
0.935000000000001,0.940000000000001,0.94142984443143),.UNSPECIFIED.)
CURVE()
GEOMETRIC_REPRESENTATION_ITEM()
RATIONAL_B_SPLINE_CURVE((1.,1.,1.,1.,1.,1.,1.,1.,1.,1.,1.,1.,1.,1.,1.,1.,
1.,1.,1.,1.,1.,1.,1.,1.,1.,1.,1.,1.,1.,1.,1.,1.,1.,1.,1.,1.,1.,1.,1.,1.,
1.,1.,1.,1.,1.,1.,1.,1.,1.,1.,1.,1.,1.,1.,1.,1.,1.,1.,1.,1.,1.,1.,1.,1.,
1.,1.,1.,1.,1.,1.,1.,1.,1.,1.,1.,1.,1.,1.,1.,1.,1.,1.,1.,1.,1.,1.,1.,1.,
1.,1.,1.,1.,1.,1.,1.,1.,1.,1.,1.,1.,1.,1.,1.,1.,1.,1.,1.,1.,1.,1.,1.,1.,
1.,1.,1.,1.,1.,1.,1.,1.,1.,1.,1.,1.,1.,1.,1.,1.,1.,1.,1.,1.,1.,1.,1.,1.,
1.,1.,1.,1.,1.,1.,1.,1.,1.,1.,1.,1.,1.,1.,1.,1.,1.,1.,1.,1.,1.,1.,1.,1.,
1.,1.,1.,1.,1.,1.,1.,1.,1.,1.,1.,1.,1.,1.,1.,1.,1.,1.,1.,1.,1.,1.,1.,1.,
1.,1.,1.,1.,1.,1.,1.,1.,1.,1.))
REPRESENTATION_ITEM('')
);
#512=(
BOUNDED_CURVE()
B_SPLINE_CURVE(5,(#101613,#101614,#101615,#101616,#101617,#101618,#101619,
#101620,#101621,#101622,#101623,#101624,#101625,#101626,#101627,#101628,
#101629,#101630,#101631,#101632,#101633,#101634,#101635,#101636,#101637,
#101638,#101639,#101640,#101641,#101642,#101643,#101644,#101645,#101646,
#101647,#101648,#101649,#101650,#101651,#101652,#101653,#101654,#101655,
#101656,#101657,#101658,#101659,#101660,#101661,#101662,#101663,#101664,
#101665,#101666,#101667,#101668,#101669,#101670,#101671,#101672,#101673,
#101674,#101675,#101676,#101677,#101678,#101679,#101680,#101681,#101682,
#101683,#101684,#101685,#101686,#101687,#101688,#101689,#101690,#101691,
#101692,#101693,#101694,#101695,#101696,#101697,#101698,#101699,#101700,
#101701,#101702,#101703,#101704,#101705,#101706,#101707,#101708,#101709,
#101710,#101711,#101712,#101713,#101714,#101715,#101716,#101717,#101718,
#101719,#101720,#101721,#101722,#101723,#101724,#101725,#101726,#101727,
#101728,#101729,#101730,#101731,#101732,#101733,#101734,#101735,#101736,
#101737,#101738,#101739,#101740,#101741,#101742,#101743,#101744,#101745,
#101746,#101747,#101748,#101749,#101750,#101751,#101752,#101753,#101754,
#101755,#101756,#101757,#101758,#101759,#101760,#101761,#101762,#101763,
#101764,#101765,#101766,#101767,#101768,#101769,#101770,#101771,#101772,
#101773,#101774,#101775,#101776,#101777,#101778,#101779,#101780,#101781,
#101782,#101783,#101784,#101785,#101786,#101787,#101788,#101789,#101790,
#101791,#101792,#101793,#101794,#101795,#101796,#101797,#101798,#101799,
#101800,#101801,#101802,#101803,#101804,#101805,#101806),.UNSPECIFIED.,
 .F.,.F.)
B_SPLINE_CURVE_WITH_KNOTS((6,1,1,1,1,1,1,1,1,1,1,1,1,1,1,1,1,1,1,1,1,1,
1,1,1,1,1,1,1,1,1,1,1,1,1,1,1,1,1,1,1,1,1,1,1,1,1,1,1,1,1,1,1,1,1,1,1,1,
1,1,1,1,1,1,1,1,1,1,1,1,1,1,1,1,1,1,1,1,1,1,1,1,1,1,1,1,1,1,1,1,1,1,1,1,
1,1,1,1,1,1,1,1,1,1,1,1,1,1,1,1,1,1,1,1,1,1,1,1,1,1,1,1,1,1,1,1,1,1,1,1,
1,1,1,1,1,1,1,1,1,1,1,1,1,1,1,1,1,1,1,1,1,1,1,1,1,1,1,1,1,1,1,1,1,1,1,1,
1,1,1,1,1,1,1,1,1,1,1,1,1,1,1,1,1,1,1,1,1,1,1,6),(-0.94142984443143,-0.940000000000001,
-0.935000000000001,-0.930000000000001,-0.925000000000001,-0.920000000000001,
-0.915000000000001,-0.910000000000001,-0.905000000000001,-0.900000000000001,
-0.895000000000001,-0.890000000000001,-0.885000000000001,-0.880000000000001,
-0.875000000000001,-0.870000000000001,-0.865000000000001,-0.860000000000001,
-0.855000000000001,-0.850000000000001,-0.845000000000001,-0.840000000000001,
-0.835000000000001,-0.830000000000001,-0.825000000000001,-0.820000000000001,
-0.815000000000001,-0.810000000000001,-0.805000000000001,-0.800000000000001,
-0.795000000000001,-0.790000000000001,-0.785000000000001,-0.780000000000001,
-0.775000000000001,-0.770000000000001,-0.765000000000001,-0.760000000000001,
-0.755000000000001,-0.750000000000001,-0.745000000000001,-0.740000000000001,
-0.735000000000001,-0.730000000000001,-0.725000000000001,-0.720000000000001,
-0.715000000000001,-0.710000000000001,-0.705000000000001,-0.700000000000001,
-0.695000000000001,-0.690000000000001,-0.685,-0.68,-0.675,-0.67,-0.665,
-0.66,-0.655,-0.65,-0.645,-0.64,-0.635,-0.63,-0.625,-0.62,-0.615,-0.61,
-0.605,-0.6,-0.595,-0.59,-0.585,-0.58,-0.575,-0.57,-0.565,-0.56,-0.555,
-0.55,-0.545,-0.54,-0.535,-0.53,-0.525,-0.52,-0.515,-0.51,-0.505,-0.5,-0.495,
-0.49,-0.485,-0.48,-0.475,-0.47,-0.465,-0.46,-0.455,-0.45,-0.445,-0.44,
-0.435,-0.43,-0.425,-0.42,-0.415,-0.41,-0.405,-0.4,-0.395,-0.39,-0.385,
-0.38,-0.375,-0.37,-0.365,-0.36,-0.355,-0.35,-0.345,-0.34,-0.335,-0.33,
-0.325,-0.32,-0.315,-0.31,-0.305,-0.3,-0.295,-0.29,-0.285,-0.28,-0.275,
-0.27,-0.265,-0.26,-0.255,-0.25,-0.245,-0.24,-0.235,-0.23,-0.225,-0.22,
-0.215,-0.21,-0.205,-0.2,-0.195,-0.19,-0.185,-0.18,-0.175,-0.17,-0.165,
-0.16,-0.155,-0.15,-0.145,-0.14,-0.135,-0.13,-0.125,-0.12,-0.115,-0.11,
-0.105,-0.1,-0.095,-0.09,-0.085,-0.08,-0.075,-0.07,-0.065,-0.06,-0.055,
-0.05,-0.045,-0.04,-0.035,-0.03,-0.025,-0.02,-0.015,-0.01,-0.005,0.),
 .UNSPECIFIED.)
CURVE()
GEOMETRIC_REPRESENTATION_ITEM()
RATIONAL_B_SPLINE_CURVE((1.,1.,1.,1.,1.,1.,1.,1.,1.,1.,1.,1.,1.,1.,1.,1.,
1.,1.,1.,1.,1.,1.,1.,1.,1.,1.,1.,1.,1.,1.,1.,1.,1.,1.,1.,1.,1.,1.,1.,1.,
1.,1.,1.,1.,1.,1.,1.,1.,1.,1.,1.,1.,1.,1.,1.,1.,1.,1.,1.,1.,1.,1.,1.,1.,
1.,1.,1.,1.,1.,1.,1.,1.,1.,1.,1.,1.,1.,1.,1.,1.,1.,1.,1.,1.,1.,1.,1.,1.,
1.,1.,1.,1.,1.,1.,1.,1.,1.,1.,1.,1.,1.,1.,1.,1.,1.,1.,1.,1.,1.,1.,1.,1.,
1.,1.,1.,1.,1.,1.,1.,1.,1.,1.,1.,1.,1.,1.,1.,1.,1.,1.,1.,1.,1.,1.,1.,1.,
1.,1.,1.,1.,1.,1.,1.,1.,1.,1.,1.,1.,1.,1.,1.,1.,1.,1.,1.,1.,1.,1.,1.,1.,
1.,1.,1.,1.,1.,1.,1.,1.,1.,1.,1.,1.,1.,1.,1.,1.,1.,1.,1.,1.,1.,1.,1.,1.,
1.,1.,1.,1.,1.,1.,1.,1.,1.,1.))
REPRESENTATION_ITEM('')
);
#513=(
BOUNDED_CURVE()
B_SPLINE_CURVE(5,(#102313,#102314,#102315,#102316,#102317,#102318,#102319,
#102320,#102321,#102322,#102323,#102324,#102325,#102326,#102327,#102328,
#102329,#102330,#102331,#102332,#102333,#102334,#102335,#102336,#102337,
#102338,#102339,#102340,#102341,#102342,#102343,#102344,#102345,#102346,
#102347,#102348,#102349,#102350,#102351,#102352,#102353,#102354,#102355,
#102356,#102357,#102358,#102359,#102360,#102361,#102362,#102363,#102364,
#102365,#102366,#102367,#102368,#102369,#102370,#102371,#102372,#102373,
#102374,#102375,#102376,#102377,#102378,#102379,#102380,#102381,#102382,
#102383,#102384,#102385,#102386,#102387,#102388,#102389,#102390,#102391,
#102392,#102393,#102394,#102395,#102396,#102397,#102398,#102399,#102400,
#102401,#102402,#102403,#102404,#102405,#102406,#102407,#102408,#102409,
#102410,#102411,#102412,#102413,#102414,#102415,#102416,#102417,#102418,
#102419,#102420,#102421,#102422,#102423,#102424,#102425,#102426,#102427,
#102428,#102429,#102430,#102431,#102432,#102433,#102434,#102435,#102436,
#102437,#102438,#102439,#102440,#102441,#102442,#102443,#102444,#102445,
#102446,#102447,#102448,#102449,#102450,#102451,#102452,#102453,#102454,
#102455,#102456,#102457,#102458,#102459,#102460,#102461,#102462,#102463,
#102464,#102465,#102466,#102467,#102468,#102469,#102470,#102471,#102472,
#102473,#102474,#102475,#102476,#102477,#102478,#102479,#102480,#102481,
#102482,#102483,#102484,#102485,#102486,#102487,#102488,#102489,#102490,
#102491,#102492,#102493,#102494,#102495,#102496,#102497,#102498,#102499,
#102500,#102501,#102502,#102503,#102504,#102505,#102506),.UNSPECIFIED.,
 .F.,.F.)
B_SPLINE_CURVE_WITH_KNOTS((6,1,1,1,1,1,1,1,1,1,1,1,1,1,1,1,1,1,1,1,1,1,
1,1,1,1,1,1,1,1,1,1,1,1,1,1,1,1,1,1,1,1,1,1,1,1,1,1,1,1,1,1,1,1,1,1,1,1,
1,1,1,1,1,1,1,1,1,1,1,1,1,1,1,1,1,1,1,1,1,1,1,1,1,1,1,1,1,1,1,1,1,1,1,1,
1,1,1,1,1,1,1,1,1,1,1,1,1,1,1,1,1,1,1,1,1,1,1,1,1,1,1,1,1,1,1,1,1,1,1,1,
1,1,1,1,1,1,1,1,1,1,1,1,1,1,1,1,1,1,1,1,1,1,1,1,1,1,1,1,1,1,1,1,1,1,1,1,
1,1,1,1,1,1,1,1,1,1,1,1,1,1,1,1,1,1,1,1,1,1,1,6),(0.,0.005,0.01,0.015,0.02,
0.025,0.03,0.035,0.04,0.045,0.05,0.055,0.06,0.065,0.07,0.075,0.08,0.085,
0.09,0.095,0.1,0.105,0.11,0.115,0.12,0.125,0.13,0.135,0.14,0.145,0.15,0.155,
0.16,0.165,0.17,0.175,0.18,0.185,0.19,0.195,0.2,0.205,0.21,0.215,0.22,0.225,
0.23,0.235,0.24,0.245,0.25,0.255,0.26,0.265,0.27,0.275,0.28,0.285,0.29,
0.295,0.3,0.305,0.31,0.315,0.32,0.325,0.33,0.335,0.34,0.345,0.35,0.355,
0.36,0.365,0.37,0.375,0.38,0.385,0.39,0.395,0.4,0.405,0.41,0.415,0.42,0.425,
0.43,0.435,0.44,0.445,0.45,0.455,0.46,0.465,0.47,0.475,0.48,0.485,0.49,
0.495,0.5,0.505,0.51,0.515,0.52,0.525,0.53,0.535,0.54,0.545,0.55,0.555,
0.56,0.565,0.57,0.575,0.58,0.585,0.59,0.595,0.6,0.605,0.61,0.615,0.62,0.625,
0.63,0.635,0.64,0.645,0.65,0.655,0.66,0.665,0.67,0.675,0.68,0.685,0.690000000000001,
0.695000000000001,0.700000000000001,0.705000000000001,0.710000000000001,
0.715000000000001,0.720000000000001,0.725000000000001,0.730000000000001,
0.735000000000001,0.740000000000001,0.745000000000001,0.750000000000001,
0.755000000000001,0.760000000000001,0.765000000000001,0.770000000000001,
0.775000000000001,0.780000000000001,0.785000000000001,0.790000000000001,
0.795000000000001,0.800000000000001,0.805000000000001,0.810000000000001,
0.815000000000001,0.820000000000001,0.825000000000001,0.830000000000001,
0.835000000000001,0.840000000000001,0.845000000000001,0.850000000000001,
0.855000000000001,0.860000000000001,0.865000000000001,0.870000000000001,
0.875000000000001,0.880000000000001,0.885000000000001,0.890000000000001,
0.895000000000001,0.900000000000001,0.905000000000001,0.910000000000001,
0.915000000000001,0.920000000000001,0.925000000000001,0.930000000000001,
0.935000000000001,0.940000000000001,0.941429844431364),.UNSPECIFIED.)
CURVE()
GEOMETRIC_REPRESENTATION_ITEM()
RATIONAL_B_SPLINE_CURVE((1.,1.,1.,1.,1.,1.,1.,1.,1.,1.,1.,1.,1.,1.,1.,1.,
1.,1.,1.,1.,1.,1.,1.,1.,1.,1.,1.,1.,1.,1.,1.,1.,1.,1.,1.,1.,1.,1.,1.,1.,
1.,1.,1.,1.,1.,1.,1.,1.,1.,1.,1.,1.,1.,1.,1.,1.,1.,1.,1.,1.,1.,1.,1.,1.,
1.,1.,1.,1.,1.,1.,1.,1.,1.,1.,1.,1.,1.,1.,1.,1.,1.,1.,1.,1.,1.,1.,1.,1.,
1.,1.,1.,1.,1.,1.,1.,1.,1.,1.,1.,1.,1.,1.,1.,1.,1.,1.,1.,1.,1.,1.,1.,1.,
1.,1.,1.,1.,1.,1.,1.,1.,1.,1.,1.,1.,1.,1.,1.,1.,1.,1.,1.,1.,1.,1.,1.,1.,
1.,1.,1.,1.,1.,1.,1.,1.,1.,1.,1.,1.,1.,1.,1.,1.,1.,1.,1.,1.,1.,1.,1.,1.,
1.,1.,1.,1.,1.,1.,1.,1.,1.,1.,1.,1.,1.,1.,1.,1.,1.,1.,1.,1.,1.,1.,1.,1.,
1.,1.,1.,1.,1.,1.,1.,1.,1.,1.))
REPRESENTATION_ITEM('')
);
#514=(
BOUNDED_CURVE()
B_SPLINE_CURVE(5,(#102509,#102510,#102511,#102512,#102513,#102514,#102515,
#102516,#102517,#102518,#102519,#102520,#102521,#102522,#102523,#102524,
#102525,#102526,#102527,#102528,#102529,#102530,#102531,#102532,#102533,
#102534,#102535,#102536,#102537,#102538,#102539,#102540,#102541,#102542,
#102543,#102544,#102545,#102546,#102547,#102548,#102549,#102550,#102551,
#102552,#102553,#102554,#102555,#102556,#102557,#102558,#102559,#102560,
#102561,#102562,#102563,#102564,#102565,#102566,#102567,#102568,#102569,
#102570,#102571,#102572,#102573,#102574,#102575,#102576,#102577,#102578,
#102579,#102580,#102581,#102582,#102583,#102584,#102585,#102586,#102587,
#102588,#102589,#102590,#102591,#102592,#102593,#102594,#102595,#102596,
#102597,#102598,#102599,#102600,#102601,#102602,#102603,#102604,#102605,
#102606,#102607,#102608,#102609,#102610,#102611,#102612,#102613,#102614,
#102615,#102616,#102617,#102618,#102619,#102620,#102621,#102622,#102623,
#102624,#102625,#102626,#102627,#102628,#102629,#102630,#102631,#102632,
#102633,#102634,#102635,#102636,#102637,#102638,#102639,#102640,#102641,
#102642,#102643,#102644,#102645,#102646,#102647,#102648,#102649,#102650,
#102651,#102652,#102653,#102654,#102655,#102656,#102657,#102658,#102659,
#102660,#102661,#102662,#102663,#102664,#102665,#102666,#102667,#102668,
#102669,#102670,#102671,#102672,#102673,#102674,#102675,#102676,#102677,
#102678,#102679,#102680,#102681,#102682,#102683,#102684,#102685,#102686,
#102687,#102688,#102689,#102690,#102691,#102692,#102693,#102694,#102695,
#102696,#102697,#102698,#102699,#102700,#102701,#102702),.UNSPECIFIED.,
 .F.,.F.)
B_SPLINE_CURVE_WITH_KNOTS((6,1,1,1,1,1,1,1,1,1,1,1,1,1,1,1,1,1,1,1,1,1,
1,1,1,1,1,1,1,1,1,1,1,1,1,1,1,1,1,1,1,1,1,1,1,1,1,1,1,1,1,1,1,1,1,1,1,1,
1,1,1,1,1,1,1,1,1,1,1,1,1,1,1,1,1,1,1,1,1,1,1,1,1,1,1,1,1,1,1,1,1,1,1,1,
1,1,1,1,1,1,1,1,1,1,1,1,1,1,1,1,1,1,1,1,1,1,1,1,1,1,1,1,1,1,1,1,1,1,1,1,
1,1,1,1,1,1,1,1,1,1,1,1,1,1,1,1,1,1,1,1,1,1,1,1,1,1,1,1,1,1,1,1,1,1,1,1,
1,1,1,1,1,1,1,1,1,1,1,1,1,1,1,1,1,1,1,1,1,1,1,6),(-0.941429844431374,-0.940000000000001,
-0.935000000000001,-0.930000000000001,-0.925000000000001,-0.920000000000001,
-0.915000000000001,-0.910000000000001,-0.905000000000001,-0.900000000000001,
-0.895000000000001,-0.890000000000001,-0.885000000000001,-0.880000000000001,
-0.875000000000001,-0.870000000000001,-0.865000000000001,-0.860000000000001,
-0.855000000000001,-0.850000000000001,-0.845000000000001,-0.840000000000001,
-0.835000000000001,-0.830000000000001,-0.825000000000001,-0.820000000000001,
-0.815000000000001,-0.810000000000001,-0.805000000000001,-0.800000000000001,
-0.795000000000001,-0.790000000000001,-0.785000000000001,-0.780000000000001,
-0.775000000000001,-0.770000000000001,-0.765000000000001,-0.760000000000001,
-0.755000000000001,-0.750000000000001,-0.745000000000001,-0.740000000000001,
-0.735000000000001,-0.730000000000001,-0.725000000000001,-0.720000000000001,
-0.715000000000001,-0.710000000000001,-0.705000000000001,-0.700000000000001,
-0.695000000000001,-0.690000000000001,-0.685,-0.68,-0.675,-0.67,-0.665,
-0.66,-0.655,-0.65,-0.645,-0.64,-0.635,-0.63,-0.625,-0.62,-0.615,-0.61,
-0.605,-0.6,-0.595,-0.59,-0.585,-0.58,-0.575,-0.57,-0.565,-0.56,-0.555,
-0.55,-0.545,-0.54,-0.535,-0.53,-0.525,-0.52,-0.515,-0.51,-0.505,-0.5,-0.495,
-0.49,-0.485,-0.48,-0.475,-0.47,-0.465,-0.46,-0.455,-0.45,-0.445,-0.44,
-0.435,-0.43,-0.425,-0.42,-0.415,-0.41,-0.405,-0.4,-0.395,-0.39,-0.385,
-0.38,-0.375,-0.37,-0.365,-0.36,-0.355,-0.35,-0.345,-0.34,-0.335,-0.33,
-0.325,-0.32,-0.315,-0.31,-0.305,-0.3,-0.295,-0.29,-0.285,-0.28,-0.275,
-0.27,-0.265,-0.26,-0.255,-0.25,-0.245,-0.24,-0.235,-0.23,-0.225,-0.22,
-0.215,-0.21,-0.205,-0.2,-0.195,-0.19,-0.185,-0.18,-0.175,-0.17,-0.165,
-0.16,-0.155,-0.15,-0.145,-0.14,-0.135,-0.13,-0.125,-0.12,-0.115,-0.11,
-0.105,-0.1,-0.095,-0.09,-0.085,-0.08,-0.075,-0.07,-0.065,-0.06,-0.055,
-0.05,-0.045,-0.04,-0.035,-0.03,-0.025,-0.02,-0.015,-0.01,-0.005,0.),
 .UNSPECIFIED.)
CURVE()
GEOMETRIC_REPRESENTATION_ITEM()
RATIONAL_B_SPLINE_CURVE((1.,1.,1.,1.,1.,1.,1.,1.,1.,1.,1.,1.,1.,1.,1.,1.,
1.,1.,1.,1.,1.,1.,1.,1.,1.,1.,1.,1.,1.,1.,1.,1.,1.,1.,1.,1.,1.,1.,1.,1.,
1.,1.,1.,1.,1.,1.,1.,1.,1.,1.,1.,1.,1.,1.,1.,1.,1.,1.,1.,1.,1.,1.,1.,1.,
1.,1.,1.,1.,1.,1.,1.,1.,1.,1.,1.,1.,1.,1.,1.,1.,1.,1.,1.,1.,1.,1.,1.,1.,
1.,1.,1.,1.,1.,1.,1.,1.,1.,1.,1.,1.,1.,1.,1.,1.,1.,1.,1.,1.,1.,1.,1.,1.,
1.,1.,1.,1.,1.,1.,1.,1.,1.,1.,1.,1.,1.,1.,1.,1.,1.,1.,1.,1.,1.,1.,1.,1.,
1.,1.,1.,1.,1.,1.,1.,1.,1.,1.,1.,1.,1.,1.,1.,1.,1.,1.,1.,1.,1.,1.,1.,1.,
1.,1.,1.,1.,1.,1.,1.,1.,1.,1.,1.,1.,1.,1.,1.,1.,1.,1.,1.,1.,1.,1.,1.,1.,
1.,1.,1.,1.,1.,1.,1.,1.,1.,1.))
REPRESENTATION_ITEM('')
);
#515=(
BOUNDED_CURVE()
B_SPLINE_CURVE(5,(#103209,#103210,#103211,#103212,#103213,#103214,#103215,
#103216,#103217,#103218,#103219,#103220,#103221,#103222,#103223,#103224,
#103225,#103226,#103227,#103228,#103229,#103230,#103231,#103232,#103233,
#103234,#103235,#103236,#103237,#103238,#103239,#103240,#103241,#103242,
#103243,#103244,#103245,#103246,#103247,#103248,#103249,#103250,#103251,
#103252,#103253,#103254,#103255,#103256,#103257,#103258,#103259,#103260,
#103261,#103262,#103263,#103264,#103265,#103266,#103267,#103268,#103269,
#103270,#103271,#103272,#103273,#103274,#103275,#103276,#103277,#103278,
#103279,#103280,#103281,#103282,#103283,#103284,#103285,#103286,#103287,
#103288,#103289,#103290,#103291,#103292,#103293,#103294,#103295,#103296,
#103297,#103298,#103299,#103300,#103301,#103302,#103303,#103304,#103305,
#103306,#103307,#103308,#103309,#103310,#103311,#103312,#103313,#103314,
#103315,#103316,#103317,#103318,#103319,#103320,#103321,#103322,#103323,
#103324,#103325,#103326,#103327,#103328,#103329,#103330,#103331,#103332,
#103333,#103334,#103335,#103336,#103337,#103338,#103339,#103340,#103341,
#103342,#103343,#103344,#103345,#103346,#103347,#103348,#103349,#103350,
#103351,#103352,#103353,#103354,#103355,#103356,#103357,#103358,#103359,
#103360,#103361,#103362,#103363,#103364,#103365,#103366,#103367,#103368,
#103369,#103370,#103371,#103372,#103373,#103374,#103375,#103376,#103377,
#103378,#103379,#103380,#103381,#103382,#103383,#103384,#103385,#103386,
#103387,#103388,#103389,#103390,#103391,#103392,#103393,#103394,#103395,
#103396,#103397,#103398,#103399,#103400,#103401,#103402),.UNSPECIFIED.,
 .F.,.F.)
B_SPLINE_CURVE_WITH_KNOTS((6,1,1,1,1,1,1,1,1,1,1,1,1,1,1,1,1,1,1,1,1,1,
1,1,1,1,1,1,1,1,1,1,1,1,1,1,1,1,1,1,1,1,1,1,1,1,1,1,1,1,1,1,1,1,1,1,1,1,
1,1,1,1,1,1,1,1,1,1,1,1,1,1,1,1,1,1,1,1,1,1,1,1,1,1,1,1,1,1,1,1,1,1,1,1,
1,1,1,1,1,1,1,1,1,1,1,1,1,1,1,1,1,1,1,1,1,1,1,1,1,1,1,1,1,1,1,1,1,1,1,1,
1,1,1,1,1,1,1,1,1,1,1,1,1,1,1,1,1,1,1,1,1,1,1,1,1,1,1,1,1,1,1,1,1,1,1,1,
1,1,1,1,1,1,1,1,1,1,1,1,1,1,1,1,1,1,1,1,1,1,1,6),(0.,0.005,0.01,0.015,0.02,
0.025,0.03,0.035,0.04,0.045,0.05,0.055,0.06,0.065,0.07,0.075,0.08,0.085,
0.09,0.095,0.1,0.105,0.11,0.115,0.12,0.125,0.13,0.135,0.14,0.145,0.15,0.155,
0.16,0.165,0.17,0.175,0.18,0.185,0.19,0.195,0.2,0.205,0.21,0.215,0.22,0.225,
0.23,0.235,0.24,0.245,0.25,0.255,0.26,0.265,0.27,0.275,0.28,0.285,0.29,
0.295,0.3,0.305,0.31,0.315,0.32,0.325,0.33,0.335,0.34,0.345,0.35,0.355,
0.36,0.365,0.37,0.375,0.38,0.385,0.39,0.395,0.4,0.405,0.41,0.415,0.42,0.425,
0.43,0.435,0.44,0.445,0.45,0.455,0.46,0.465,0.47,0.475,0.48,0.485,0.49,
0.495,0.5,0.505,0.51,0.515,0.52,0.525,0.53,0.535,0.54,0.545,0.55,0.555,
0.56,0.565,0.57,0.575,0.58,0.585,0.59,0.595,0.6,0.605,0.61,0.615,0.62,0.625,
0.63,0.635,0.64,0.645,0.65,0.655,0.66,0.665,0.67,0.675,0.68,0.685,0.690000000000001,
0.695000000000001,0.700000000000001,0.705000000000001,0.710000000000001,
0.715000000000001,0.720000000000001,0.725000000000001,0.730000000000001,
0.735000000000001,0.740000000000001,0.745000000000001,0.750000000000001,
0.755000000000001,0.760000000000001,0.765000000000001,0.770000000000001,
0.775000000000001,0.780000000000001,0.785000000000001,0.790000000000001,
0.795000000000001,0.800000000000001,0.805000000000001,0.810000000000001,
0.815000000000001,0.820000000000001,0.825000000000001,0.830000000000001,
0.835000000000001,0.840000000000001,0.845000000000001,0.850000000000001,
0.855000000000001,0.860000000000001,0.865000000000001,0.870000000000001,
0.875000000000001,0.880000000000001,0.885000000000001,0.890000000000001,
0.895000000000001,0.900000000000001,0.905000000000001,0.910000000000001,
0.915000000000001,0.920000000000001,0.925000000000001,0.930000000000001,
0.935000000000001,0.940000000000001,0.94142984443135),.UNSPECIFIED.)
CURVE()
GEOMETRIC_REPRESENTATION_ITEM()
RATIONAL_B_SPLINE_CURVE((1.,1.,1.,1.,1.,1.,1.,1.,1.,1.,1.,1.,1.,1.,1.,1.,
1.,1.,1.,1.,1.,1.,1.,1.,1.,1.,1.,1.,1.,1.,1.,1.,1.,1.,1.,1.,1.,1.,1.,1.,
1.,1.,1.,1.,1.,1.,1.,1.,1.,1.,1.,1.,1.,1.,1.,1.,1.,1.,1.,1.,1.,1.,1.,1.,
1.,1.,1.,1.,1.,1.,1.,1.,1.,1.,1.,1.,1.,1.,1.,1.,1.,1.,1.,1.,1.,1.,1.,1.,
1.,1.,1.,1.,1.,1.,1.,1.,1.,1.,1.,1.,1.,1.,1.,1.,1.,1.,1.,1.,1.,1.,1.,1.,
1.,1.,1.,1.,1.,1.,1.,1.,1.,1.,1.,1.,1.,1.,1.,1.,1.,1.,1.,1.,1.,1.,1.,1.,
1.,1.,1.,1.,1.,1.,1.,1.,1.,1.,1.,1.,1.,1.,1.,1.,1.,1.,1.,1.,1.,1.,1.,1.,
1.,1.,1.,1.,1.,1.,1.,1.,1.,1.,1.,1.,1.,1.,1.,1.,1.,1.,1.,1.,1.,1.,1.,1.,
1.,1.,1.,1.,1.,1.,1.,1.,1.,1.))
REPRESENTATION_ITEM('')
);
#516=(
BOUNDED_CURVE()
B_SPLINE_CURVE(5,(#103405,#103406,#103407,#103408,#103409,#103410,#103411,
#103412,#103413,#103414,#103415,#103416,#103417,#103418,#103419,#103420,
#103421,#103422,#103423,#103424,#103425,#103426,#103427,#103428,#103429,
#103430,#103431,#103432,#103433,#103434,#103435,#103436,#103437,#103438,
#103439,#103440,#103441,#103442,#103443,#103444,#103445,#103446,#103447,
#103448,#103449,#103450,#103451,#103452,#103453,#103454,#103455,#103456,
#103457,#103458,#103459,#103460,#103461,#103462,#103463,#103464,#103465,
#103466,#103467,#103468,#103469,#103470,#103471,#103472,#103473,#103474,
#103475,#103476,#103477,#103478,#103479,#103480,#103481,#103482,#103483,
#103484,#103485,#103486,#103487,#103488,#103489,#103490,#103491,#103492,
#103493,#103494,#103495,#103496,#103497,#103498,#103499,#103500,#103501,
#103502,#103503,#103504,#103505,#103506,#103507,#103508,#103509,#103510,
#103511,#103512,#103513,#103514,#103515,#103516,#103517,#103518,#103519,
#103520,#103521,#103522,#103523,#103524,#103525,#103526,#103527,#103528,
#103529,#103530,#103531,#103532,#103533,#103534,#103535,#103536,#103537,
#103538,#103539,#103540,#103541,#103542,#103543,#103544,#103545,#103546,
#103547,#103548,#103549,#103550,#103551,#103552,#103553,#103554,#103555,
#103556,#103557,#103558,#103559,#103560,#103561,#103562,#103563,#103564,
#103565,#103566,#103567,#103568,#103569,#103570,#103571,#103572,#103573,
#103574,#103575,#103576,#103577,#103578,#103579,#103580,#103581,#103582,
#103583,#103584,#103585,#103586,#103587,#103588,#103589,#103590,#103591,
#103592,#103593,#103594,#103595,#103596,#103597,#103598),.UNSPECIFIED.,
 .F.,.F.)
B_SPLINE_CURVE_WITH_KNOTS((6,1,1,1,1,1,1,1,1,1,1,1,1,1,1,1,1,1,1,1,1,1,
1,1,1,1,1,1,1,1,1,1,1,1,1,1,1,1,1,1,1,1,1,1,1,1,1,1,1,1,1,1,1,1,1,1,1,1,
1,1,1,1,1,1,1,1,1,1,1,1,1,1,1,1,1,1,1,1,1,1,1,1,1,1,1,1,1,1,1,1,1,1,1,1,
1,1,1,1,1,1,1,1,1,1,1,1,1,1,1,1,1,1,1,1,1,1,1,1,1,1,1,1,1,1,1,1,1,1,1,1,
1,1,1,1,1,1,1,1,1,1,1,1,1,1,1,1,1,1,1,1,1,1,1,1,1,1,1,1,1,1,1,1,1,1,1,1,
1,1,1,1,1,1,1,1,1,1,1,1,1,1,1,1,1,1,1,1,1,1,1,6),(-0.94142984443135,-0.940000000000001,
-0.935000000000001,-0.930000000000001,-0.925000000000001,-0.920000000000001,
-0.915000000000001,-0.910000000000001,-0.905000000000001,-0.900000000000001,
-0.895000000000001,-0.890000000000001,-0.885000000000001,-0.880000000000001,
-0.875000000000001,-0.870000000000001,-0.865000000000001,-0.860000000000001,
-0.855000000000001,-0.850000000000001,-0.845000000000001,-0.840000000000001,
-0.835000000000001,-0.830000000000001,-0.825000000000001,-0.820000000000001,
-0.815000000000001,-0.810000000000001,-0.805000000000001,-0.800000000000001,
-0.795000000000001,-0.790000000000001,-0.785000000000001,-0.780000000000001,
-0.775000000000001,-0.770000000000001,-0.765000000000001,-0.760000000000001,
-0.755000000000001,-0.750000000000001,-0.745000000000001,-0.740000000000001,
-0.735000000000001,-0.730000000000001,-0.725000000000001,-0.720000000000001,
-0.715000000000001,-0.710000000000001,-0.705000000000001,-0.700000000000001,
-0.695000000000001,-0.690000000000001,-0.685,-0.68,-0.675,-0.67,-0.665,
-0.66,-0.655,-0.65,-0.645,-0.64,-0.635,-0.63,-0.625,-0.62,-0.615,-0.61,
-0.605,-0.6,-0.595,-0.59,-0.585,-0.58,-0.575,-0.57,-0.565,-0.56,-0.555,
-0.55,-0.545,-0.54,-0.535,-0.53,-0.525,-0.52,-0.515,-0.51,-0.505,-0.5,-0.495,
-0.49,-0.485,-0.48,-0.475,-0.47,-0.465,-0.46,-0.455,-0.45,-0.445,-0.44,
-0.435,-0.43,-0.425,-0.42,-0.415,-0.41,-0.405,-0.4,-0.395,-0.39,-0.385,
-0.38,-0.375,-0.37,-0.365,-0.36,-0.355,-0.35,-0.345,-0.34,-0.335,-0.33,
-0.325,-0.32,-0.315,-0.31,-0.305,-0.3,-0.295,-0.29,-0.285,-0.28,-0.275,
-0.27,-0.265,-0.26,-0.255,-0.25,-0.245,-0.24,-0.235,-0.23,-0.225,-0.22,
-0.215,-0.21,-0.205,-0.2,-0.195,-0.19,-0.185,-0.18,-0.175,-0.17,-0.165,
-0.16,-0.155,-0.15,-0.145,-0.14,-0.135,-0.13,-0.125,-0.12,-0.115,-0.11,
-0.105,-0.1,-0.095,-0.09,-0.085,-0.08,-0.075,-0.07,-0.065,-0.06,-0.055,
-0.05,-0.045,-0.04,-0.035,-0.03,-0.025,-0.02,-0.015,-0.01,-0.005,0.),
 .UNSPECIFIED.)
CURVE()
GEOMETRIC_REPRESENTATION_ITEM()
RATIONAL_B_SPLINE_CURVE((1.,1.,1.,1.,1.,1.,1.,1.,1.,1.,1.,1.,1.,1.,1.,1.,
1.,1.,1.,1.,1.,1.,1.,1.,1.,1.,1.,1.,1.,1.,1.,1.,1.,1.,1.,1.,1.,1.,1.,1.,
1.,1.,1.,1.,1.,1.,1.,1.,1.,1.,1.,1.,1.,1.,1.,1.,1.,1.,1.,1.,1.,1.,1.,1.,
1.,1.,1.,1.,1.,1.,1.,1.,1.,1.,1.,1.,1.,1.,1.,1.,1.,1.,1.,1.,1.,1.,1.,1.,
1.,1.,1.,1.,1.,1.,1.,1.,1.,1.,1.,1.,1.,1.,1.,1.,1.,1.,1.,1.,1.,1.,1.,1.,
1.,1.,1.,1.,1.,1.,1.,1.,1.,1.,1.,1.,1.,1.,1.,1.,1.,1.,1.,1.,1.,1.,1.,1.,
1.,1.,1.,1.,1.,1.,1.,1.,1.,1.,1.,1.,1.,1.,1.,1.,1.,1.,1.,1.,1.,1.,1.,1.,
1.,1.,1.,1.,1.,1.,1.,1.,1.,1.,1.,1.,1.,1.,1.,1.,1.,1.,1.,1.,1.,1.,1.,1.,
1.,1.,1.,1.,1.,1.,1.,1.,1.,1.))
REPRESENTATION_ITEM('')
);
#517=(
BOUNDED_CURVE()
B_SPLINE_CURVE(5,(#104105,#104106,#104107,#104108,#104109,#104110,#104111,
#104112,#104113,#104114,#104115,#104116,#104117,#104118,#104119,#104120,
#104121,#104122,#104123,#104124,#104125,#104126,#104127,#104128,#104129,
#104130,#104131,#104132,#104133,#104134,#104135,#104136,#104137,#104138,
#104139,#104140,#104141,#104142,#104143,#104144,#104145,#104146,#104147,
#104148,#104149,#104150,#104151,#104152,#104153,#104154,#104155,#104156,
#104157,#104158,#104159,#104160,#104161,#104162,#104163,#104164,#104165,
#104166,#104167,#104168,#104169,#104170,#104171,#104172,#104173,#104174,
#104175,#104176,#104177,#104178,#104179,#104180,#104181,#104182,#104183,
#104184,#104185,#104186,#104187,#104188,#104189,#104190,#104191,#104192,
#104193,#104194,#104195,#104196,#104197,#104198,#104199,#104200,#104201,
#104202,#104203,#104204,#104205,#104206,#104207,#104208,#104209,#104210,
#104211,#104212,#104213,#104214,#104215,#104216,#104217,#104218,#104219,
#104220,#104221,#104222,#104223,#104224,#104225,#104226,#104227,#104228,
#104229,#104230,#104231,#104232,#104233,#104234,#104235,#104236,#104237,
#104238,#104239,#104240,#104241,#104242,#104243,#104244,#104245,#104246,
#104247,#104248,#104249,#104250,#104251,#104252,#104253,#104254,#104255,
#104256,#104257,#104258,#104259,#104260,#104261,#104262,#104263,#104264,
#104265,#104266,#104267,#104268,#104269,#104270,#104271,#104272,#104273,
#104274,#104275,#104276,#104277,#104278,#104279,#104280,#104281,#104282,
#104283,#104284,#104285,#104286,#104287,#104288,#104289,#104290,#104291,
#104292,#104293,#104294,#104295,#104296,#104297,#104298),.UNSPECIFIED.,
 .F.,.F.)
B_SPLINE_CURVE_WITH_KNOTS((6,1,1,1,1,1,1,1,1,1,1,1,1,1,1,1,1,1,1,1,1,1,
1,1,1,1,1,1,1,1,1,1,1,1,1,1,1,1,1,1,1,1,1,1,1,1,1,1,1,1,1,1,1,1,1,1,1,1,
1,1,1,1,1,1,1,1,1,1,1,1,1,1,1,1,1,1,1,1,1,1,1,1,1,1,1,1,1,1,1,1,1,1,1,1,
1,1,1,1,1,1,1,1,1,1,1,1,1,1,1,1,1,1,1,1,1,1,1,1,1,1,1,1,1,1,1,1,1,1,1,1,
1,1,1,1,1,1,1,1,1,1,1,1,1,1,1,1,1,1,1,1,1,1,1,1,1,1,1,1,1,1,1,1,1,1,1,1,
1,1,1,1,1,1,1,1,1,1,1,1,1,1,1,1,1,1,1,1,1,1,1,6),(0.,0.005,0.01,0.015,0.02,
0.025,0.03,0.035,0.04,0.045,0.05,0.055,0.06,0.065,0.07,0.075,0.08,0.085,
0.09,0.095,0.1,0.105,0.11,0.115,0.12,0.125,0.13,0.135,0.14,0.145,0.15,0.155,
0.16,0.165,0.17,0.175,0.18,0.185,0.19,0.195,0.2,0.205,0.21,0.215,0.22,0.225,
0.23,0.235,0.24,0.245,0.25,0.255,0.26,0.265,0.27,0.275,0.28,0.285,0.29,
0.295,0.3,0.305,0.31,0.315,0.32,0.325,0.33,0.335,0.34,0.345,0.35,0.355,
0.36,0.365,0.37,0.375,0.38,0.385,0.39,0.395,0.4,0.405,0.41,0.415,0.42,0.425,
0.43,0.435,0.44,0.445,0.45,0.455,0.46,0.465,0.47,0.475,0.48,0.485,0.49,
0.495,0.5,0.505,0.51,0.515,0.52,0.525,0.53,0.535,0.54,0.545,0.55,0.555,
0.56,0.565,0.57,0.575,0.58,0.585,0.59,0.595,0.6,0.605,0.61,0.615,0.62,0.625,
0.63,0.635,0.64,0.645,0.65,0.655,0.66,0.665,0.67,0.675,0.68,0.685,0.690000000000001,
0.695000000000001,0.700000000000001,0.705000000000001,0.710000000000001,
0.715000000000001,0.720000000000001,0.725000000000001,0.730000000000001,
0.735000000000001,0.740000000000001,0.745000000000001,0.750000000000001,
0.755000000000001,0.760000000000001,0.765000000000001,0.770000000000001,
0.775000000000001,0.780000000000001,0.785000000000001,0.790000000000001,
0.795000000000001,0.800000000000001,0.805000000000001,0.810000000000001,
0.815000000000001,0.820000000000001,0.825000000000001,0.830000000000001,
0.835000000000001,0.840000000000001,0.845000000000001,0.850000000000001,
0.855000000000001,0.860000000000001,0.865000000000001,0.870000000000001,
0.875000000000001,0.880000000000001,0.885000000000001,0.890000000000001,
0.895000000000001,0.900000000000001,0.905000000000001,0.910000000000001,
0.915000000000001,0.920000000000001,0.925000000000001,0.930000000000001,
0.935000000000001,0.940000000000001,0.941429844431347),.UNSPECIFIED.)
CURVE()
GEOMETRIC_REPRESENTATION_ITEM()
RATIONAL_B_SPLINE_CURVE((1.,1.,1.,1.,1.,1.,1.,1.,1.,1.,1.,1.,1.,1.,1.,1.,
1.,1.,1.,1.,1.,1.,1.,1.,1.,1.,1.,1.,1.,1.,1.,1.,1.,1.,1.,1.,1.,1.,1.,1.,
1.,1.,1.,1.,1.,1.,1.,1.,1.,1.,1.,1.,1.,1.,1.,1.,1.,1.,1.,1.,1.,1.,1.,1.,
1.,1.,1.,1.,1.,1.,1.,1.,1.,1.,1.,1.,1.,1.,1.,1.,1.,1.,1.,1.,1.,1.,1.,1.,
1.,1.,1.,1.,1.,1.,1.,1.,1.,1.,1.,1.,1.,1.,1.,1.,1.,1.,1.,1.,1.,1.,1.,1.,
1.,1.,1.,1.,1.,1.,1.,1.,1.,1.,1.,1.,1.,1.,1.,1.,1.,1.,1.,1.,1.,1.,1.,1.,
1.,1.,1.,1.,1.,1.,1.,1.,1.,1.,1.,1.,1.,1.,1.,1.,1.,1.,1.,1.,1.,1.,1.,1.,
1.,1.,1.,1.,1.,1.,1.,1.,1.,1.,1.,1.,1.,1.,1.,1.,1.,1.,1.,1.,1.,1.,1.,1.,
1.,1.,1.,1.,1.,1.,1.,1.,1.,1.))
REPRESENTATION_ITEM('')
);
#518=(
BOUNDED_CURVE()
B_SPLINE_CURVE(5,(#104301,#104302,#104303,#104304,#104305,#104306,#104307,
#104308,#104309,#104310,#104311,#104312,#104313,#104314,#104315,#104316,
#104317,#104318,#104319,#104320,#104321,#104322,#104323,#104324,#104325,
#104326,#104327,#104328,#104329,#104330,#104331,#104332,#104333,#104334,
#104335,#104336,#104337,#104338,#104339,#104340,#104341,#104342,#104343,
#104344,#104345,#104346,#104347,#104348,#104349,#104350,#104351,#104352,
#104353,#104354,#104355,#104356,#104357,#104358,#104359,#104360,#104361,
#104362,#104363,#104364,#104365,#104366,#104367,#104368,#104369,#104370,
#104371,#104372,#104373,#104374,#104375,#104376,#104377,#104378,#104379,
#104380,#104381,#104382,#104383,#104384,#104385,#104386,#104387,#104388,
#104389,#104390,#104391,#104392,#104393,#104394,#104395,#104396,#104397,
#104398,#104399,#104400,#104401,#104402,#104403,#104404,#104405,#104406,
#104407,#104408,#104409,#104410,#104411,#104412,#104413,#104414,#104415,
#104416,#104417,#104418,#104419,#104420,#104421,#104422,#104423,#104424,
#104425,#104426,#104427,#104428,#104429,#104430,#104431,#104432,#104433,
#104434,#104435,#104436,#104437,#104438,#104439,#104440,#104441,#104442,
#104443,#104444,#104445,#104446,#104447,#104448,#104449,#104450,#104451,
#104452,#104453,#104454,#104455,#104456,#104457,#104458,#104459,#104460,
#104461,#104462,#104463,#104464,#104465,#104466,#104467,#104468,#104469,
#104470,#104471,#104472,#104473,#104474,#104475,#104476,#104477,#104478,
#104479,#104480,#104481,#104482,#104483,#104484,#104485,#104486,#104487,
#104488,#104489,#104490,#104491,#104492,#104493,#104494),.UNSPECIFIED.,
 .F.,.F.)
B_SPLINE_CURVE_WITH_KNOTS((6,1,1,1,1,1,1,1,1,1,1,1,1,1,1,1,1,1,1,1,1,1,
1,1,1,1,1,1,1,1,1,1,1,1,1,1,1,1,1,1,1,1,1,1,1,1,1,1,1,1,1,1,1,1,1,1,1,1,
1,1,1,1,1,1,1,1,1,1,1,1,1,1,1,1,1,1,1,1,1,1,1,1,1,1,1,1,1,1,1,1,1,1,1,1,
1,1,1,1,1,1,1,1,1,1,1,1,1,1,1,1,1,1,1,1,1,1,1,1,1,1,1,1,1,1,1,1,1,1,1,1,
1,1,1,1,1,1,1,1,1,1,1,1,1,1,1,1,1,1,1,1,1,1,1,1,1,1,1,1,1,1,1,1,1,1,1,1,
1,1,1,1,1,1,1,1,1,1,1,1,1,1,1,1,1,1,1,1,1,1,1,6),(-0.941429844431341,-0.940000000000001,
-0.935000000000001,-0.930000000000001,-0.925000000000001,-0.920000000000001,
-0.915000000000001,-0.910000000000001,-0.905000000000001,-0.900000000000001,
-0.895000000000001,-0.890000000000001,-0.885000000000001,-0.880000000000001,
-0.875000000000001,-0.870000000000001,-0.865000000000001,-0.860000000000001,
-0.855000000000001,-0.850000000000001,-0.845000000000001,-0.840000000000001,
-0.835000000000001,-0.830000000000001,-0.825000000000001,-0.820000000000001,
-0.815000000000001,-0.810000000000001,-0.805000000000001,-0.800000000000001,
-0.795000000000001,-0.790000000000001,-0.785000000000001,-0.780000000000001,
-0.775000000000001,-0.770000000000001,-0.765000000000001,-0.760000000000001,
-0.755000000000001,-0.750000000000001,-0.745000000000001,-0.740000000000001,
-0.735000000000001,-0.730000000000001,-0.725000000000001,-0.720000000000001,
-0.715000000000001,-0.710000000000001,-0.705000000000001,-0.700000000000001,
-0.695000000000001,-0.690000000000001,-0.685,-0.68,-0.675,-0.67,-0.665,
-0.66,-0.655,-0.65,-0.645,-0.64,-0.635,-0.63,-0.625,-0.62,-0.615,-0.61,
-0.605,-0.6,-0.595,-0.59,-0.585,-0.58,-0.575,-0.57,-0.565,-0.56,-0.555,
-0.55,-0.545,-0.54,-0.535,-0.53,-0.525,-0.52,-0.515,-0.51,-0.505,-0.5,-0.495,
-0.49,-0.485,-0.48,-0.475,-0.47,-0.465,-0.46,-0.455,-0.45,-0.445,-0.44,
-0.435,-0.43,-0.425,-0.42,-0.415,-0.41,-0.405,-0.4,-0.395,-0.39,-0.385,
-0.38,-0.375,-0.37,-0.365,-0.36,-0.355,-0.35,-0.345,-0.34,-0.335,-0.33,
-0.325,-0.32,-0.315,-0.31,-0.305,-0.3,-0.295,-0.29,-0.285,-0.28,-0.275,
-0.27,-0.265,-0.26,-0.255,-0.25,-0.245,-0.24,-0.235,-0.23,-0.225,-0.22,
-0.215,-0.21,-0.205,-0.2,-0.195,-0.19,-0.185,-0.18,-0.175,-0.17,-0.165,
-0.16,-0.155,-0.15,-0.145,-0.14,-0.135,-0.13,-0.125,-0.12,-0.115,-0.11,
-0.105,-0.1,-0.095,-0.09,-0.085,-0.08,-0.075,-0.07,-0.065,-0.06,-0.055,
-0.05,-0.045,-0.04,-0.035,-0.03,-0.025,-0.02,-0.015,-0.01,-0.005,0.),
 .UNSPECIFIED.)
CURVE()
GEOMETRIC_REPRESENTATION_ITEM()
RATIONAL_B_SPLINE_CURVE((1.,1.,1.,1.,1.,1.,1.,1.,1.,1.,1.,1.,1.,1.,1.,1.,
1.,1.,1.,1.,1.,1.,1.,1.,1.,1.,1.,1.,1.,1.,1.,1.,1.,1.,1.,1.,1.,1.,1.,1.,
1.,1.,1.,1.,1.,1.,1.,1.,1.,1.,1.,1.,1.,1.,1.,1.,1.,1.,1.,1.,1.,1.,1.,1.,
1.,1.,1.,1.,1.,1.,1.,1.,1.,1.,1.,1.,1.,1.,1.,1.,1.,1.,1.,1.,1.,1.,1.,1.,
1.,1.,1.,1.,1.,1.,1.,1.,1.,1.,1.,1.,1.,1.,1.,1.,1.,1.,1.,1.,1.,1.,1.,1.,
1.,1.,1.,1.,1.,1.,1.,1.,1.,1.,1.,1.,1.,1.,1.,1.,1.,1.,1.,1.,1.,1.,1.,1.,
1.,1.,1.,1.,1.,1.,1.,1.,1.,1.,1.,1.,1.,1.,1.,1.,1.,1.,1.,1.,1.,1.,1.,1.,
1.,1.,1.,1.,1.,1.,1.,1.,1.,1.,1.,1.,1.,1.,1.,1.,1.,1.,1.,1.,1.,1.,1.,1.,
1.,1.,1.,1.,1.,1.,1.,1.,1.,1.))
REPRESENTATION_ITEM('')
);
#519=(
BOUNDED_CURVE()
B_SPLINE_CURVE(5,(#105001,#105002,#105003,#105004,#105005,#105006,#105007,
#105008,#105009,#105010,#105011,#105012,#105013,#105014,#105015,#105016,
#105017,#105018,#105019,#105020,#105021,#105022,#105023,#105024,#105025,
#105026,#105027,#105028,#105029,#105030,#105031,#105032,#105033,#105034,
#105035,#105036,#105037,#105038,#105039,#105040,#105041,#105042,#105043,
#105044,#105045,#105046,#105047,#105048,#105049,#105050,#105051,#105052,
#105053,#105054,#105055,#105056,#105057,#105058,#105059,#105060,#105061,
#105062,#105063,#105064,#105065,#105066,#105067,#105068,#105069,#105070,
#105071,#105072,#105073,#105074,#105075,#105076,#105077,#105078,#105079,
#105080,#105081,#105082,#105083,#105084,#105085,#105086,#105087,#105088,
#105089,#105090,#105091,#105092,#105093,#105094,#105095,#105096,#105097,
#105098,#105099,#105100,#105101,#105102,#105103,#105104,#105105,#105106,
#105107,#105108,#105109,#105110,#105111,#105112,#105113,#105114,#105115,
#105116,#105117,#105118,#105119,#105120,#105121,#105122,#105123,#105124,
#105125,#105126,#105127,#105128,#105129,#105130,#105131,#105132,#105133,
#105134,#105135,#105136,#105137,#105138,#105139,#105140,#105141,#105142,
#105143,#105144,#105145,#105146,#105147,#105148,#105149,#105150,#105151,
#105152,#105153,#105154,#105155,#105156,#105157,#105158,#105159,#105160,
#105161,#105162,#105163,#105164,#105165,#105166,#105167,#105168,#105169,
#105170,#105171,#105172,#105173,#105174,#105175,#105176,#105177,#105178,
#105179,#105180,#105181,#105182,#105183,#105184,#105185,#105186,#105187,
#105188,#105189,#105190,#105191,#105192,#105193,#105194),.UNSPECIFIED.,
 .F.,.F.)
B_SPLINE_CURVE_WITH_KNOTS((6,1,1,1,1,1,1,1,1,1,1,1,1,1,1,1,1,1,1,1,1,1,
1,1,1,1,1,1,1,1,1,1,1,1,1,1,1,1,1,1,1,1,1,1,1,1,1,1,1,1,1,1,1,1,1,1,1,1,
1,1,1,1,1,1,1,1,1,1,1,1,1,1,1,1,1,1,1,1,1,1,1,1,1,1,1,1,1,1,1,1,1,1,1,1,
1,1,1,1,1,1,1,1,1,1,1,1,1,1,1,1,1,1,1,1,1,1,1,1,1,1,1,1,1,1,1,1,1,1,1,1,
1,1,1,1,1,1,1,1,1,1,1,1,1,1,1,1,1,1,1,1,1,1,1,1,1,1,1,1,1,1,1,1,1,1,1,1,
1,1,1,1,1,1,1,1,1,1,1,1,1,1,1,1,1,1,1,1,1,1,1,6),(0.,0.005,0.01,0.015,0.02,
0.025,0.03,0.035,0.04,0.045,0.05,0.055,0.06,0.065,0.07,0.075,0.08,0.085,
0.09,0.095,0.1,0.105,0.11,0.115,0.12,0.125,0.13,0.135,0.14,0.145,0.15,0.155,
0.16,0.165,0.17,0.175,0.18,0.185,0.19,0.195,0.2,0.205,0.21,0.215,0.22,0.225,
0.23,0.235,0.24,0.245,0.25,0.255,0.26,0.265,0.27,0.275,0.28,0.285,0.29,
0.295,0.3,0.305,0.31,0.315,0.32,0.325,0.33,0.335,0.34,0.345,0.35,0.355,
0.36,0.365,0.37,0.375,0.38,0.385,0.39,0.395,0.4,0.405,0.41,0.415,0.42,0.425,
0.43,0.435,0.44,0.445,0.45,0.455,0.46,0.465,0.47,0.475,0.48,0.485,0.49,
0.495,0.5,0.505,0.51,0.515,0.52,0.525,0.53,0.535,0.54,0.545,0.55,0.555,
0.56,0.565,0.57,0.575,0.58,0.585,0.59,0.595,0.6,0.605,0.61,0.615,0.62,0.625,
0.63,0.635,0.64,0.645,0.65,0.655,0.66,0.665,0.67,0.675,0.68,0.685,0.690000000000001,
0.695000000000001,0.700000000000001,0.705000000000001,0.710000000000001,
0.715000000000001,0.720000000000001,0.725000000000001,0.730000000000001,
0.735000000000001,0.740000000000001,0.745000000000001,0.750000000000001,
0.755000000000001,0.760000000000001,0.765000000000001,0.770000000000001,
0.775000000000001,0.780000000000001,0.785000000000001,0.790000000000001,
0.795000000000001,0.800000000000001,0.805000000000001,0.810000000000001,
0.815000000000001,0.820000000000001,0.825000000000001,0.830000000000001,
0.835000000000001,0.840000000000001,0.845000000000001,0.850000000000001,
0.855000000000001,0.860000000000001,0.865000000000001,0.870000000000001,
0.875000000000001,0.880000000000001,0.885000000000001,0.890000000000001,
0.895000000000001,0.900000000000001,0.905000000000001,0.910000000000001,
0.915000000000001,0.920000000000001,0.925000000000001,0.930000000000001,
0.935000000000001,0.940000000000001,0.941429844431379),.UNSPECIFIED.)
CURVE()
GEOMETRIC_REPRESENTATION_ITEM()
RATIONAL_B_SPLINE_CURVE((1.,1.,1.,1.,1.,1.,1.,1.,1.,1.,1.,1.,1.,1.,1.,1.,
1.,1.,1.,1.,1.,1.,1.,1.,1.,1.,1.,1.,1.,1.,1.,1.,1.,1.,1.,1.,1.,1.,1.,1.,
1.,1.,1.,1.,1.,1.,1.,1.,1.,1.,1.,1.,1.,1.,1.,1.,1.,1.,1.,1.,1.,1.,1.,1.,
1.,1.,1.,1.,1.,1.,1.,1.,1.,1.,1.,1.,1.,1.,1.,1.,1.,1.,1.,1.,1.,1.,1.,1.,
1.,1.,1.,1.,1.,1.,1.,1.,1.,1.,1.,1.,1.,1.,1.,1.,1.,1.,1.,1.,1.,1.,1.,1.,
1.,1.,1.,1.,1.,1.,1.,1.,1.,1.,1.,1.,1.,1.,1.,1.,1.,1.,1.,1.,1.,1.,1.,1.,
1.,1.,1.,1.,1.,1.,1.,1.,1.,1.,1.,1.,1.,1.,1.,1.,1.,1.,1.,1.,1.,1.,1.,1.,
1.,1.,1.,1.,1.,1.,1.,1.,1.,1.,1.,1.,1.,1.,1.,1.,1.,1.,1.,1.,1.,1.,1.,1.,
1.,1.,1.,1.,1.,1.,1.,1.,1.,1.))
REPRESENTATION_ITEM('')
);
#520=(
BOUNDED_CURVE()
B_SPLINE_CURVE(5,(#105197,#105198,#105199,#105200,#105201,#105202,#105203,
#105204,#105205,#105206,#105207,#105208,#105209,#105210,#105211,#105212,
#105213,#105214,#105215,#105216,#105217,#105218,#105219,#105220,#105221,
#105222,#105223,#105224,#105225,#105226,#105227,#105228,#105229,#105230,
#105231,#105232,#105233,#105234,#105235,#105236,#105237,#105238,#105239,
#105240,#105241,#105242,#105243,#105244,#105245,#105246,#105247,#105248,
#105249,#105250,#105251,#105252,#105253,#105254,#105255,#105256,#105257,
#105258,#105259,#105260,#105261,#105262,#105263,#105264,#105265,#105266,
#105267,#105268,#105269,#105270,#105271,#105272,#105273,#105274,#105275,
#105276,#105277,#105278,#105279,#105280,#105281,#105282,#105283,#105284,
#105285,#105286,#105287,#105288,#105289,#105290,#105291,#105292,#105293,
#105294,#105295,#105296,#105297,#105298,#105299,#105300,#105301,#105302,
#105303,#105304,#105305,#105306,#105307,#105308,#105309,#105310,#105311,
#105312,#105313,#105314,#105315,#105316,#105317,#105318,#105319,#105320,
#105321,#105322,#105323,#105324,#105325,#105326,#105327,#105328,#105329,
#105330,#105331,#105332,#105333,#105334,#105335,#105336,#105337,#105338,
#105339,#105340,#105341,#105342,#105343,#105344,#105345,#105346,#105347,
#105348,#105349,#105350,#105351,#105352,#105353,#105354,#105355,#105356,
#105357,#105358,#105359,#105360,#105361,#105362,#105363,#105364,#105365,
#105366,#105367,#105368,#105369,#105370,#105371,#105372,#105373,#105374,
#105375,#105376,#105377,#105378,#105379,#105380,#105381,#105382,#105383,
#105384,#105385,#105386,#105387,#105388,#105389,#105390),.UNSPECIFIED.,
 .F.,.F.)
B_SPLINE_CURVE_WITH_KNOTS((6,1,1,1,1,1,1,1,1,1,1,1,1,1,1,1,1,1,1,1,1,1,
1,1,1,1,1,1,1,1,1,1,1,1,1,1,1,1,1,1,1,1,1,1,1,1,1,1,1,1,1,1,1,1,1,1,1,1,
1,1,1,1,1,1,1,1,1,1,1,1,1,1,1,1,1,1,1,1,1,1,1,1,1,1,1,1,1,1,1,1,1,1,1,1,
1,1,1,1,1,1,1,1,1,1,1,1,1,1,1,1,1,1,1,1,1,1,1,1,1,1,1,1,1,1,1,1,1,1,1,1,
1,1,1,1,1,1,1,1,1,1,1,1,1,1,1,1,1,1,1,1,1,1,1,1,1,1,1,1,1,1,1,1,1,1,1,1,
1,1,1,1,1,1,1,1,1,1,1,1,1,1,1,1,1,1,1,1,1,1,1,6),(-0.941429844431382,-0.940000000000001,
-0.935000000000001,-0.930000000000001,-0.925000000000001,-0.920000000000001,
-0.915000000000001,-0.910000000000001,-0.905000000000001,-0.900000000000001,
-0.895000000000001,-0.890000000000001,-0.885000000000001,-0.880000000000001,
-0.875000000000001,-0.870000000000001,-0.865000000000001,-0.860000000000001,
-0.855000000000001,-0.850000000000001,-0.845000000000001,-0.840000000000001,
-0.835000000000001,-0.830000000000001,-0.825000000000001,-0.820000000000001,
-0.815000000000001,-0.810000000000001,-0.805000000000001,-0.800000000000001,
-0.795000000000001,-0.790000000000001,-0.785000000000001,-0.780000000000001,
-0.775000000000001,-0.770000000000001,-0.765000000000001,-0.760000000000001,
-0.755000000000001,-0.750000000000001,-0.745000000000001,-0.740000000000001,
-0.735000000000001,-0.730000000000001,-0.725000000000001,-0.720000000000001,
-0.715000000000001,-0.710000000000001,-0.705000000000001,-0.700000000000001,
-0.695000000000001,-0.690000000000001,-0.685,-0.68,-0.675,-0.67,-0.665,
-0.66,-0.655,-0.65,-0.645,-0.64,-0.635,-0.63,-0.625,-0.62,-0.615,-0.61,
-0.605,-0.6,-0.595,-0.59,-0.585,-0.58,-0.575,-0.57,-0.565,-0.56,-0.555,
-0.55,-0.545,-0.54,-0.535,-0.53,-0.525,-0.52,-0.515,-0.51,-0.505,-0.5,-0.495,
-0.49,-0.485,-0.48,-0.475,-0.47,-0.465,-0.46,-0.455,-0.45,-0.445,-0.44,
-0.435,-0.43,-0.425,-0.42,-0.415,-0.41,-0.405,-0.4,-0.395,-0.39,-0.385,
-0.38,-0.375,-0.37,-0.365,-0.36,-0.355,-0.35,-0.345,-0.34,-0.335,-0.33,
-0.325,-0.32,-0.315,-0.31,-0.305,-0.3,-0.295,-0.29,-0.285,-0.28,-0.275,
-0.27,-0.265,-0.26,-0.255,-0.25,-0.245,-0.24,-0.235,-0.23,-0.225,-0.22,
-0.215,-0.21,-0.205,-0.2,-0.195,-0.19,-0.185,-0.18,-0.175,-0.17,-0.165,
-0.16,-0.155,-0.15,-0.145,-0.14,-0.135,-0.13,-0.125,-0.12,-0.115,-0.11,
-0.105,-0.1,-0.095,-0.09,-0.085,-0.08,-0.075,-0.07,-0.065,-0.06,-0.055,
-0.05,-0.045,-0.04,-0.035,-0.03,-0.025,-0.02,-0.015,-0.01,-0.005,0.),
 .UNSPECIFIED.)
CURVE()
GEOMETRIC_REPRESENTATION_ITEM()
RATIONAL_B_SPLINE_CURVE((1.,1.,1.,1.,1.,1.,1.,1.,1.,1.,1.,1.,1.,1.,1.,1.,
1.,1.,1.,1.,1.,1.,1.,1.,1.,1.,1.,1.,1.,1.,1.,1.,1.,1.,1.,1.,1.,1.,1.,1.,
1.,1.,1.,1.,1.,1.,1.,1.,1.,1.,1.,1.,1.,1.,1.,1.,1.,1.,1.,1.,1.,1.,1.,1.,
1.,1.,1.,1.,1.,1.,1.,1.,1.,1.,1.,1.,1.,1.,1.,1.,1.,1.,1.,1.,1.,1.,1.,1.,
1.,1.,1.,1.,1.,1.,1.,1.,1.,1.,1.,1.,1.,1.,1.,1.,1.,1.,1.,1.,1.,1.,1.,1.,
1.,1.,1.,1.,1.,1.,1.,1.,1.,1.,1.,1.,1.,1.,1.,1.,1.,1.,1.,1.,1.,1.,1.,1.,
1.,1.,1.,1.,1.,1.,1.,1.,1.,1.,1.,1.,1.,1.,1.,1.,1.,1.,1.,1.,1.,1.,1.,1.,
1.,1.,1.,1.,1.,1.,1.,1.,1.,1.,1.,1.,1.,1.,1.,1.,1.,1.,1.,1.,1.,1.,1.,1.,
1.,1.,1.,1.,1.,1.,1.,1.,1.,1.))
REPRESENTATION_ITEM('')
);
#521=(
BOUNDED_CURVE()
B_SPLINE_CURVE(5,(#105897,#105898,#105899,#105900,#105901,#105902,#105903,
#105904,#105905,#105906,#105907,#105908,#105909,#105910,#105911,#105912,
#105913,#105914,#105915,#105916,#105917,#105918,#105919,#105920,#105921,
#105922,#105923,#105924,#105925,#105926,#105927,#105928,#105929,#105930,
#105931,#105932,#105933,#105934,#105935,#105936,#105937,#105938,#105939,
#105940,#105941,#105942,#105943,#105944,#105945,#105946,#105947,#105948,
#105949,#105950,#105951,#105952,#105953,#105954,#105955,#105956,#105957,
#105958,#105959,#105960,#105961,#105962,#105963,#105964,#105965,#105966,
#105967,#105968,#105969,#105970,#105971,#105972,#105973,#105974,#105975,
#105976,#105977,#105978,#105979,#105980,#105981,#105982,#105983,#105984,
#105985,#105986,#105987,#105988,#105989,#105990,#105991,#105992,#105993,
#105994,#105995,#105996,#105997,#105998,#105999,#106000,#106001,#106002,
#106003,#106004,#106005,#106006,#106007,#106008,#106009,#106010,#106011,
#106012,#106013,#106014,#106015,#106016,#106017,#106018,#106019,#106020,
#106021,#106022,#106023,#106024,#106025,#106026,#106027,#106028,#106029,
#106030,#106031,#106032,#106033,#106034,#106035,#106036,#106037,#106038,
#106039,#106040,#106041,#106042,#106043,#106044,#106045,#106046,#106047,
#106048,#106049,#106050,#106051,#106052,#106053,#106054,#106055,#106056,
#106057,#106058,#106059,#106060,#106061,#106062,#106063,#106064,#106065,
#106066,#106067,#106068,#106069,#106070,#106071,#106072,#106073,#106074,
#106075,#106076,#106077,#106078,#106079,#106080,#106081,#106082,#106083,
#106084,#106085,#106086,#106087,#106088,#106089,#106090),.UNSPECIFIED.,
 .F.,.F.)
B_SPLINE_CURVE_WITH_KNOTS((6,1,1,1,1,1,1,1,1,1,1,1,1,1,1,1,1,1,1,1,1,1,
1,1,1,1,1,1,1,1,1,1,1,1,1,1,1,1,1,1,1,1,1,1,1,1,1,1,1,1,1,1,1,1,1,1,1,1,
1,1,1,1,1,1,1,1,1,1,1,1,1,1,1,1,1,1,1,1,1,1,1,1,1,1,1,1,1,1,1,1,1,1,1,1,
1,1,1,1,1,1,1,1,1,1,1,1,1,1,1,1,1,1,1,1,1,1,1,1,1,1,1,1,1,1,1,1,1,1,1,1,
1,1,1,1,1,1,1,1,1,1,1,1,1,1,1,1,1,1,1,1,1,1,1,1,1,1,1,1,1,1,1,1,1,1,1,1,
1,1,1,1,1,1,1,1,1,1,1,1,1,1,1,1,1,1,1,1,1,1,1,6),(0.,0.005,0.01,0.015,0.02,
0.025,0.03,0.035,0.04,0.045,0.05,0.055,0.06,0.065,0.07,0.075,0.08,0.085,
0.09,0.095,0.1,0.105,0.11,0.115,0.12,0.125,0.13,0.135,0.14,0.145,0.15,0.155,
0.16,0.165,0.17,0.175,0.18,0.185,0.19,0.195,0.2,0.205,0.21,0.215,0.22,0.225,
0.23,0.235,0.24,0.245,0.25,0.255,0.26,0.265,0.27,0.275,0.28,0.285,0.29,
0.295,0.3,0.305,0.31,0.315,0.32,0.325,0.33,0.335,0.34,0.345,0.35,0.355,
0.36,0.365,0.37,0.375,0.38,0.385,0.39,0.395,0.4,0.405,0.41,0.415,0.42,0.425,
0.43,0.435,0.44,0.445,0.45,0.455,0.46,0.465,0.47,0.475,0.48,0.485,0.49,
0.495,0.5,0.505,0.51,0.515,0.52,0.525,0.53,0.535,0.54,0.545,0.55,0.555,
0.56,0.565,0.57,0.575,0.58,0.585,0.59,0.595,0.6,0.605,0.61,0.615,0.62,0.625,
0.63,0.635,0.64,0.645,0.65,0.655,0.66,0.665,0.67,0.675,0.68,0.685,0.690000000000001,
0.695000000000001,0.700000000000001,0.705000000000001,0.710000000000001,
0.715000000000001,0.720000000000001,0.725000000000001,0.730000000000001,
0.735000000000001,0.740000000000001,0.745000000000001,0.750000000000001,
0.755000000000001,0.760000000000001,0.765000000000001,0.770000000000001,
0.775000000000001,0.780000000000001,0.785000000000001,0.790000000000001,
0.795000000000001,0.800000000000001,0.805000000000001,0.810000000000001,
0.815000000000001,0.820000000000001,0.825000000000001,0.830000000000001,
0.835000000000001,0.840000000000001,0.845000000000001,0.850000000000001,
0.855000000000001,0.860000000000001,0.865000000000001,0.870000000000001,
0.875000000000001,0.880000000000001,0.885000000000001,0.890000000000001,
0.895000000000001,0.900000000000001,0.905000000000001,0.910000000000001,
0.915000000000001,0.920000000000001,0.925000000000001,0.930000000000001,
0.935000000000001,0.940000000000001,0.941429844431321),.UNSPECIFIED.)
CURVE()
GEOMETRIC_REPRESENTATION_ITEM()
RATIONAL_B_SPLINE_CURVE((1.,1.,1.,1.,1.,1.,1.,1.,1.,1.,1.,1.,1.,1.,1.,1.,
1.,1.,1.,1.,1.,1.,1.,1.,1.,1.,1.,1.,1.,1.,1.,1.,1.,1.,1.,1.,1.,1.,1.,1.,
1.,1.,1.,1.,1.,1.,1.,1.,1.,1.,1.,1.,1.,1.,1.,1.,1.,1.,1.,1.,1.,1.,1.,1.,
1.,1.,1.,1.,1.,1.,1.,1.,1.,1.,1.,1.,1.,1.,1.,1.,1.,1.,1.,1.,1.,1.,1.,1.,
1.,1.,1.,1.,1.,1.,1.,1.,1.,1.,1.,1.,1.,1.,1.,1.,1.,1.,1.,1.,1.,1.,1.,1.,
1.,1.,1.,1.,1.,1.,1.,1.,1.,1.,1.,1.,1.,1.,1.,1.,1.,1.,1.,1.,1.,1.,1.,1.,
1.,1.,1.,1.,1.,1.,1.,1.,1.,1.,1.,1.,1.,1.,1.,1.,1.,1.,1.,1.,1.,1.,1.,1.,
1.,1.,1.,1.,1.,1.,1.,1.,1.,1.,1.,1.,1.,1.,1.,1.,1.,1.,1.,1.,1.,1.,1.,1.,
1.,1.,1.,1.,1.,1.,1.,1.,1.,1.))
REPRESENTATION_ITEM('')
);
#522=(
BOUNDED_CURVE()
B_SPLINE_CURVE(5,(#106093,#106094,#106095,#106096,#106097,#106098,#106099,
#106100,#106101,#106102,#106103,#106104,#106105,#106106,#106107,#106108,
#106109,#106110,#106111,#106112,#106113,#106114,#106115,#106116,#106117,
#106118,#106119,#106120,#106121,#106122,#106123,#106124,#106125,#106126,
#106127,#106128,#106129,#106130,#106131,#106132,#106133,#106134,#106135,
#106136,#106137,#106138,#106139,#106140,#106141,#106142,#106143,#106144,
#106145,#106146,#106147,#106148,#106149,#106150,#106151,#106152,#106153,
#106154,#106155,#106156,#106157,#106158,#106159,#106160,#106161,#106162,
#106163,#106164,#106165,#106166,#106167,#106168,#106169,#106170,#106171,
#106172,#106173,#106174,#106175,#106176,#106177,#106178,#106179,#106180,
#106181,#106182,#106183,#106184,#106185,#106186,#106187,#106188,#106189,
#106190,#106191,#106192,#106193,#106194,#106195,#106196,#106197,#106198,
#106199,#106200,#106201,#106202,#106203,#106204,#106205,#106206,#106207,
#106208,#106209,#106210,#106211,#106212,#106213,#106214,#106215,#106216,
#106217,#106218,#106219,#106220,#106221,#106222,#106223,#106224,#106225,
#106226,#106227,#106228,#106229,#106230,#106231,#106232,#106233,#106234,
#106235,#106236,#106237,#106238,#106239,#106240,#106241,#106242,#106243,
#106244,#106245,#106246,#106247,#106248,#106249,#106250,#106251,#106252,
#106253,#106254,#106255,#106256,#106257,#106258,#106259,#106260,#106261,
#106262,#106263,#106264,#106265,#106266,#106267,#106268,#106269,#106270,
#106271,#106272,#106273,#106274,#106275,#106276,#106277,#106278,#106279,
#106280,#106281,#106282,#106283,#106284,#106285,#106286),.UNSPECIFIED.,
 .F.,.F.)
B_SPLINE_CURVE_WITH_KNOTS((6,1,1,1,1,1,1,1,1,1,1,1,1,1,1,1,1,1,1,1,1,1,
1,1,1,1,1,1,1,1,1,1,1,1,1,1,1,1,1,1,1,1,1,1,1,1,1,1,1,1,1,1,1,1,1,1,1,1,
1,1,1,1,1,1,1,1,1,1,1,1,1,1,1,1,1,1,1,1,1,1,1,1,1,1,1,1,1,1,1,1,1,1,1,1,
1,1,1,1,1,1,1,1,1,1,1,1,1,1,1,1,1,1,1,1,1,1,1,1,1,1,1,1,1,1,1,1,1,1,1,1,
1,1,1,1,1,1,1,1,1,1,1,1,1,1,1,1,1,1,1,1,1,1,1,1,1,1,1,1,1,1,1,1,1,1,1,1,
1,1,1,1,1,1,1,1,1,1,1,1,1,1,1,1,1,1,1,1,1,1,1,6),(-0.941429844431305,-0.940000000000001,
-0.935000000000001,-0.930000000000001,-0.925000000000001,-0.920000000000001,
-0.915000000000001,-0.910000000000001,-0.905000000000001,-0.900000000000001,
-0.895000000000001,-0.890000000000001,-0.885000000000001,-0.880000000000001,
-0.875000000000001,-0.870000000000001,-0.865000000000001,-0.860000000000001,
-0.855000000000001,-0.850000000000001,-0.845000000000001,-0.840000000000001,
-0.835000000000001,-0.830000000000001,-0.825000000000001,-0.820000000000001,
-0.815000000000001,-0.810000000000001,-0.805000000000001,-0.800000000000001,
-0.795000000000001,-0.790000000000001,-0.785000000000001,-0.780000000000001,
-0.775000000000001,-0.770000000000001,-0.765000000000001,-0.760000000000001,
-0.755000000000001,-0.750000000000001,-0.745000000000001,-0.740000000000001,
-0.735000000000001,-0.730000000000001,-0.725000000000001,-0.720000000000001,
-0.715000000000001,-0.710000000000001,-0.705000000000001,-0.700000000000001,
-0.695000000000001,-0.690000000000001,-0.685,-0.68,-0.675,-0.67,-0.665,
-0.66,-0.655,-0.65,-0.645,-0.64,-0.635,-0.63,-0.625,-0.62,-0.615,-0.61,
-0.605,-0.6,-0.595,-0.59,-0.585,-0.58,-0.575,-0.57,-0.565,-0.56,-0.555,
-0.55,-0.545,-0.54,-0.535,-0.53,-0.525,-0.52,-0.515,-0.51,-0.505,-0.5,-0.495,
-0.49,-0.485,-0.48,-0.475,-0.47,-0.465,-0.46,-0.455,-0.45,-0.445,-0.44,
-0.435,-0.43,-0.425,-0.42,-0.415,-0.41,-0.405,-0.4,-0.395,-0.39,-0.385,
-0.38,-0.375,-0.37,-0.365,-0.36,-0.355,-0.35,-0.345,-0.34,-0.335,-0.33,
-0.325,-0.32,-0.315,-0.31,-0.305,-0.3,-0.295,-0.29,-0.285,-0.28,-0.275,
-0.27,-0.265,-0.26,-0.255,-0.25,-0.245,-0.24,-0.235,-0.23,-0.225,-0.22,
-0.215,-0.21,-0.205,-0.2,-0.195,-0.19,-0.185,-0.18,-0.175,-0.17,-0.165,
-0.16,-0.155,-0.15,-0.145,-0.14,-0.135,-0.13,-0.125,-0.12,-0.115,-0.11,
-0.105,-0.1,-0.095,-0.09,-0.085,-0.08,-0.075,-0.07,-0.065,-0.06,-0.055,
-0.05,-0.045,-0.04,-0.035,-0.03,-0.025,-0.02,-0.015,-0.01,-0.005,0.),
 .UNSPECIFIED.)
CURVE()
GEOMETRIC_REPRESENTATION_ITEM()
RATIONAL_B_SPLINE_CURVE((1.,1.,1.,1.,1.,1.,1.,1.,1.,1.,1.,1.,1.,1.,1.,1.,
1.,1.,1.,1.,1.,1.,1.,1.,1.,1.,1.,1.,1.,1.,1.,1.,1.,1.,1.,1.,1.,1.,1.,1.,
1.,1.,1.,1.,1.,1.,1.,1.,1.,1.,1.,1.,1.,1.,1.,1.,1.,1.,1.,1.,1.,1.,1.,1.,
1.,1.,1.,1.,1.,1.,1.,1.,1.,1.,1.,1.,1.,1.,1.,1.,1.,1.,1.,1.,1.,1.,1.,1.,
1.,1.,1.,1.,1.,1.,1.,1.,1.,1.,1.,1.,1.,1.,1.,1.,1.,1.,1.,1.,1.,1.,1.,1.,
1.,1.,1.,1.,1.,1.,1.,1.,1.,1.,1.,1.,1.,1.,1.,1.,1.,1.,1.,1.,1.,1.,1.,1.,
1.,1.,1.,1.,1.,1.,1.,1.,1.,1.,1.,1.,1.,1.,1.,1.,1.,1.,1.,1.,1.,1.,1.,1.,
1.,1.,1.,1.,1.,1.,1.,1.,1.,1.,1.,1.,1.,1.,1.,1.,1.,1.,1.,1.,1.,1.,1.,1.,
1.,1.,1.,1.,1.,1.,1.,1.,1.,1.))
REPRESENTATION_ITEM('')
);
#523=(
BOUNDED_CURVE()
B_SPLINE_CURVE(5,(#106793,#106794,#106795,#106796,#106797,#106798,#106799,
#106800,#106801,#106802,#106803,#106804,#106805,#106806,#106807,#106808,
#106809,#106810,#106811,#106812,#106813,#106814,#106815,#106816,#106817,
#106818,#106819,#106820,#106821,#106822,#106823,#106824,#106825,#106826,
#106827,#106828,#106829,#106830,#106831,#106832,#106833,#106834,#106835,
#106836,#106837,#106838,#106839,#106840,#106841,#106842,#106843,#106844,
#106845,#106846,#106847,#106848,#106849,#106850,#106851,#106852,#106853,
#106854,#106855,#106856,#106857,#106858,#106859,#106860,#106861,#106862,
#106863,#106864,#106865,#106866,#106867,#106868,#106869,#106870,#106871,
#106872,#106873,#106874,#106875,#106876,#106877,#106878,#106879,#106880,
#106881,#106882,#106883,#106884,#106885,#106886,#106887,#106888,#106889,
#106890,#106891,#106892,#106893,#106894,#106895,#106896,#106897,#106898,
#106899,#106900,#106901,#106902,#106903,#106904,#106905,#106906,#106907,
#106908,#106909,#106910,#106911,#106912,#106913,#106914,#106915,#106916,
#106917,#106918,#106919,#106920,#106921,#106922,#106923,#106924,#106925,
#106926,#106927,#106928,#106929,#106930,#106931,#106932,#106933,#106934,
#106935,#106936,#106937,#106938,#106939,#106940,#106941,#106942,#106943,
#106944,#106945,#106946,#106947,#106948,#106949,#106950,#106951,#106952,
#106953,#106954,#106955,#106956,#106957,#106958,#106959,#106960,#106961,
#106962,#106963,#106964,#106965,#106966,#106967,#106968,#106969,#106970,
#106971,#106972,#106973,#106974,#106975,#106976,#106977,#106978,#106979,
#106980,#106981,#106982,#106983,#106984,#106985,#106986),.UNSPECIFIED.,
 .F.,.F.)
B_SPLINE_CURVE_WITH_KNOTS((6,1,1,1,1,1,1,1,1,1,1,1,1,1,1,1,1,1,1,1,1,1,
1,1,1,1,1,1,1,1,1,1,1,1,1,1,1,1,1,1,1,1,1,1,1,1,1,1,1,1,1,1,1,1,1,1,1,1,
1,1,1,1,1,1,1,1,1,1,1,1,1,1,1,1,1,1,1,1,1,1,1,1,1,1,1,1,1,1,1,1,1,1,1,1,
1,1,1,1,1,1,1,1,1,1,1,1,1,1,1,1,1,1,1,1,1,1,1,1,1,1,1,1,1,1,1,1,1,1,1,1,
1,1,1,1,1,1,1,1,1,1,1,1,1,1,1,1,1,1,1,1,1,1,1,1,1,1,1,1,1,1,1,1,1,1,1,1,
1,1,1,1,1,1,1,1,1,1,1,1,1,1,1,1,1,1,1,1,1,1,1,6),(0.,0.005,0.01,0.015,0.02,
0.025,0.03,0.035,0.04,0.045,0.05,0.055,0.06,0.065,0.07,0.075,0.08,0.085,
0.09,0.095,0.1,0.105,0.11,0.115,0.12,0.125,0.13,0.135,0.14,0.145,0.15,0.155,
0.16,0.165,0.17,0.175,0.18,0.185,0.19,0.195,0.2,0.205,0.21,0.215,0.22,0.225,
0.23,0.235,0.24,0.245,0.25,0.255,0.26,0.265,0.27,0.275,0.28,0.285,0.29,
0.295,0.3,0.305,0.31,0.315,0.32,0.325,0.33,0.335,0.34,0.345,0.35,0.355,
0.36,0.365,0.37,0.375,0.38,0.385,0.39,0.395,0.4,0.405,0.41,0.415,0.42,0.425,
0.43,0.435,0.44,0.445,0.45,0.455,0.46,0.465,0.47,0.475,0.48,0.485,0.49,
0.495,0.5,0.505,0.51,0.515,0.52,0.525,0.53,0.535,0.54,0.545,0.55,0.555,
0.56,0.565,0.57,0.575,0.58,0.585,0.59,0.595,0.6,0.605,0.61,0.615,0.62,0.625,
0.63,0.635,0.64,0.645,0.65,0.655,0.66,0.665,0.67,0.675,0.68,0.685,0.690000000000001,
0.695000000000001,0.700000000000001,0.705000000000001,0.710000000000001,
0.715000000000001,0.720000000000001,0.725000000000001,0.730000000000001,
0.735000000000001,0.740000000000001,0.745000000000001,0.750000000000001,
0.755000000000001,0.760000000000001,0.765000000000001,0.770000000000001,
0.775000000000001,0.780000000000001,0.785000000000001,0.790000000000001,
0.795000000000001,0.800000000000001,0.805000000000001,0.810000000000001,
0.815000000000001,0.820000000000001,0.825000000000001,0.830000000000001,
0.835000000000001,0.840000000000001,0.845000000000001,0.850000000000001,
0.855000000000001,0.860000000000001,0.865000000000001,0.870000000000001,
0.875000000000001,0.880000000000001,0.885000000000001,0.890000000000001,
0.895000000000001,0.900000000000001,0.905000000000001,0.910000000000001,
0.915000000000001,0.920000000000001,0.925000000000001,0.930000000000001,
0.935000000000001,0.940000000000001,0.941429844431252),.UNSPECIFIED.)
CURVE()
GEOMETRIC_REPRESENTATION_ITEM()
RATIONAL_B_SPLINE_CURVE((1.,1.,1.,1.,1.,1.,1.,1.,1.,1.,1.,1.,1.,1.,1.,1.,
1.,1.,1.,1.,1.,1.,1.,1.,1.,1.,1.,1.,1.,1.,1.,1.,1.,1.,1.,1.,1.,1.,1.,1.,
1.,1.,1.,1.,1.,1.,1.,1.,1.,1.,1.,1.,1.,1.,1.,1.,1.,1.,1.,1.,1.,1.,1.,1.,
1.,1.,1.,1.,1.,1.,1.,1.,1.,1.,1.,1.,1.,1.,1.,1.,1.,1.,1.,1.,1.,1.,1.,1.,
1.,1.,1.,1.,1.,1.,1.,1.,1.,1.,1.,1.,1.,1.,1.,1.,1.,1.,1.,1.,1.,1.,1.,1.,
1.,1.,1.,1.,1.,1.,1.,1.,1.,1.,1.,1.,1.,1.,1.,1.,1.,1.,1.,1.,1.,1.,1.,1.,
1.,1.,1.,1.,1.,1.,1.,1.,1.,1.,1.,1.,1.,1.,1.,1.,1.,1.,1.,1.,1.,1.,1.,1.,
1.,1.,1.,1.,1.,1.,1.,1.,1.,1.,1.,1.,1.,1.,1.,1.,1.,1.,1.,1.,1.,1.,1.,1.,
1.,1.,1.,1.,1.,1.,1.,1.,1.,1.))
REPRESENTATION_ITEM('')
);
#524=(
BOUNDED_CURVE()
B_SPLINE_CURVE(5,(#106989,#106990,#106991,#106992,#106993,#106994,#106995,
#106996,#106997,#106998,#106999,#107000,#107001,#107002,#107003,#107004,
#107005,#107006,#107007,#107008,#107009,#107010,#107011,#107012,#107013,
#107014,#107015,#107016,#107017,#107018,#107019,#107020,#107021,#107022,
#107023,#107024,#107025,#107026,#107027,#107028,#107029,#107030,#107031,
#107032,#107033,#107034,#107035,#107036,#107037,#107038,#107039,#107040,
#107041,#107042,#107043,#107044,#107045,#107046,#107047,#107048,#107049,
#107050,#107051,#107052,#107053,#107054,#107055,#107056,#107057,#107058,
#107059,#107060,#107061,#107062,#107063,#107064,#107065,#107066,#107067,
#107068,#107069,#107070,#107071,#107072,#107073,#107074,#107075,#107076,
#107077,#107078,#107079,#107080,#107081,#107082,#107083,#107084,#107085,
#107086,#107087,#107088,#107089,#107090,#107091,#107092,#107093,#107094,
#107095,#107096,#107097,#107098,#107099,#107100,#107101,#107102,#107103,
#107104,#107105,#107106,#107107,#107108,#107109,#107110,#107111,#107112,
#107113,#107114,#107115,#107116,#107117,#107118,#107119,#107120,#107121,
#107122,#107123,#107124,#107125,#107126,#107127,#107128,#107129,#107130,
#107131,#107132,#107133,#107134,#107135,#107136,#107137,#107138,#107139,
#107140,#107141,#107142,#107143,#107144,#107145,#107146,#107147,#107148,
#107149,#107150,#107151,#107152,#107153,#107154,#107155,#107156,#107157,
#107158,#107159,#107160,#107161,#107162,#107163,#107164,#107165,#107166,
#107167,#107168,#107169,#107170,#107171,#107172,#107173,#107174,#107175,
#107176,#107177,#107178,#107179,#107180,#107181,#107182),.UNSPECIFIED.,
 .F.,.F.)
B_SPLINE_CURVE_WITH_KNOTS((6,1,1,1,1,1,1,1,1,1,1,1,1,1,1,1,1,1,1,1,1,1,
1,1,1,1,1,1,1,1,1,1,1,1,1,1,1,1,1,1,1,1,1,1,1,1,1,1,1,1,1,1,1,1,1,1,1,1,
1,1,1,1,1,1,1,1,1,1,1,1,1,1,1,1,1,1,1,1,1,1,1,1,1,1,1,1,1,1,1,1,1,1,1,1,
1,1,1,1,1,1,1,1,1,1,1,1,1,1,1,1,1,1,1,1,1,1,1,1,1,1,1,1,1,1,1,1,1,1,1,1,
1,1,1,1,1,1,1,1,1,1,1,1,1,1,1,1,1,1,1,1,1,1,1,1,1,1,1,1,1,1,1,1,1,1,1,1,
1,1,1,1,1,1,1,1,1,1,1,1,1,1,1,1,1,1,1,1,1,1,1,6),(-0.94142984443125,-0.940000000000001,
-0.935000000000001,-0.930000000000001,-0.925000000000001,-0.920000000000001,
-0.915000000000001,-0.910000000000001,-0.905000000000001,-0.900000000000001,
-0.895000000000001,-0.890000000000001,-0.885000000000001,-0.880000000000001,
-0.875000000000001,-0.870000000000001,-0.865000000000001,-0.860000000000001,
-0.855000000000001,-0.850000000000001,-0.845000000000001,-0.840000000000001,
-0.835000000000001,-0.830000000000001,-0.825000000000001,-0.820000000000001,
-0.815000000000001,-0.810000000000001,-0.805000000000001,-0.800000000000001,
-0.795000000000001,-0.790000000000001,-0.785000000000001,-0.780000000000001,
-0.775000000000001,-0.770000000000001,-0.765000000000001,-0.760000000000001,
-0.755000000000001,-0.750000000000001,-0.745000000000001,-0.740000000000001,
-0.735000000000001,-0.730000000000001,-0.725000000000001,-0.720000000000001,
-0.715000000000001,-0.710000000000001,-0.705000000000001,-0.700000000000001,
-0.695000000000001,-0.690000000000001,-0.685,-0.68,-0.675,-0.67,-0.665,
-0.66,-0.655,-0.65,-0.645,-0.64,-0.635,-0.63,-0.625,-0.62,-0.615,-0.61,
-0.605,-0.6,-0.595,-0.59,-0.585,-0.58,-0.575,-0.57,-0.565,-0.56,-0.555,
-0.55,-0.545,-0.54,-0.535,-0.53,-0.525,-0.52,-0.515,-0.51,-0.505,-0.5,-0.495,
-0.49,-0.485,-0.48,-0.475,-0.47,-0.465,-0.46,-0.455,-0.45,-0.445,-0.44,
-0.435,-0.43,-0.425,-0.42,-0.415,-0.41,-0.405,-0.4,-0.395,-0.39,-0.385,
-0.38,-0.375,-0.37,-0.365,-0.36,-0.355,-0.35,-0.345,-0.34,-0.335,-0.33,
-0.325,-0.32,-0.315,-0.31,-0.305,-0.3,-0.295,-0.29,-0.285,-0.28,-0.275,
-0.27,-0.265,-0.26,-0.255,-0.25,-0.245,-0.24,-0.235,-0.23,-0.225,-0.22,
-0.215,-0.21,-0.205,-0.2,-0.195,-0.19,-0.185,-0.18,-0.175,-0.17,-0.165,
-0.16,-0.155,-0.15,-0.145,-0.14,-0.135,-0.13,-0.125,-0.12,-0.115,-0.11,
-0.105,-0.1,-0.095,-0.09,-0.085,-0.08,-0.075,-0.07,-0.065,-0.06,-0.055,
-0.05,-0.045,-0.04,-0.035,-0.03,-0.025,-0.02,-0.015,-0.01,-0.005,0.),
 .UNSPECIFIED.)
CURVE()
GEOMETRIC_REPRESENTATION_ITEM()
RATIONAL_B_SPLINE_CURVE((1.,1.,1.,1.,1.,1.,1.,1.,1.,1.,1.,1.,1.,1.,1.,1.,
1.,1.,1.,1.,1.,1.,1.,1.,1.,1.,1.,1.,1.,1.,1.,1.,1.,1.,1.,1.,1.,1.,1.,1.,
1.,1.,1.,1.,1.,1.,1.,1.,1.,1.,1.,1.,1.,1.,1.,1.,1.,1.,1.,1.,1.,1.,1.,1.,
1.,1.,1.,1.,1.,1.,1.,1.,1.,1.,1.,1.,1.,1.,1.,1.,1.,1.,1.,1.,1.,1.,1.,1.,
1.,1.,1.,1.,1.,1.,1.,1.,1.,1.,1.,1.,1.,1.,1.,1.,1.,1.,1.,1.,1.,1.,1.,1.,
1.,1.,1.,1.,1.,1.,1.,1.,1.,1.,1.,1.,1.,1.,1.,1.,1.,1.,1.,1.,1.,1.,1.,1.,
1.,1.,1.,1.,1.,1.,1.,1.,1.,1.,1.,1.,1.,1.,1.,1.,1.,1.,1.,1.,1.,1.,1.,1.,
1.,1.,1.,1.,1.,1.,1.,1.,1.,1.,1.,1.,1.,1.,1.,1.,1.,1.,1.,1.,1.,1.,1.,1.,
1.,1.,1.,1.,1.,1.,1.,1.,1.,1.))
REPRESENTATION_ITEM('')
);
#525=(
BOUNDED_CURVE()
B_SPLINE_CURVE(5,(#107689,#107690,#107691,#107692,#107693,#107694,#107695,
#107696,#107697,#107698,#107699,#107700,#107701,#107702,#107703,#107704,
#107705,#107706,#107707,#107708,#107709,#107710,#107711,#107712,#107713,
#107714,#107715,#107716,#107717,#107718,#107719,#107720,#107721,#107722,
#107723,#107724,#107725,#107726,#107727,#107728,#107729,#107730,#107731,
#107732,#107733,#107734,#107735,#107736,#107737,#107738,#107739,#107740,
#107741,#107742,#107743,#107744,#107745,#107746,#107747,#107748,#107749,
#107750,#107751,#107752,#107753,#107754,#107755,#107756,#107757,#107758,
#107759,#107760,#107761,#107762,#107763,#107764,#107765,#107766,#107767,
#107768,#107769,#107770,#107771,#107772,#107773,#107774,#107775,#107776,
#107777,#107778,#107779,#107780,#107781,#107782,#107783,#107784,#107785,
#107786,#107787,#107788,#107789,#107790,#107791,#107792,#107793,#107794,
#107795,#107796,#107797,#107798,#107799,#107800,#107801,#107802,#107803,
#107804,#107805,#107806,#107807,#107808,#107809,#107810,#107811,#107812,
#107813,#107814,#107815,#107816,#107817,#107818,#107819,#107820,#107821,
#107822,#107823,#107824,#107825,#107826,#107827,#107828,#107829,#107830,
#107831,#107832,#107833,#107834,#107835,#107836,#107837,#107838,#107839,
#107840,#107841,#107842,#107843,#107844,#107845,#107846,#107847,#107848,
#107849,#107850,#107851,#107852,#107853,#107854,#107855,#107856,#107857,
#107858,#107859,#107860,#107861,#107862,#107863,#107864,#107865,#107866,
#107867,#107868,#107869,#107870,#107871,#107872,#107873,#107874,#107875,
#107876,#107877,#107878,#107879,#107880,#107881,#107882),.UNSPECIFIED.,
 .F.,.F.)
B_SPLINE_CURVE_WITH_KNOTS((6,1,1,1,1,1,1,1,1,1,1,1,1,1,1,1,1,1,1,1,1,1,
1,1,1,1,1,1,1,1,1,1,1,1,1,1,1,1,1,1,1,1,1,1,1,1,1,1,1,1,1,1,1,1,1,1,1,1,
1,1,1,1,1,1,1,1,1,1,1,1,1,1,1,1,1,1,1,1,1,1,1,1,1,1,1,1,1,1,1,1,1,1,1,1,
1,1,1,1,1,1,1,1,1,1,1,1,1,1,1,1,1,1,1,1,1,1,1,1,1,1,1,1,1,1,1,1,1,1,1,1,
1,1,1,1,1,1,1,1,1,1,1,1,1,1,1,1,1,1,1,1,1,1,1,1,1,1,1,1,1,1,1,1,1,1,1,1,
1,1,1,1,1,1,1,1,1,1,1,1,1,1,1,1,1,1,1,1,1,1,1,6),(0.,0.005,0.01,0.015,0.02,
0.025,0.03,0.035,0.04,0.045,0.05,0.055,0.06,0.065,0.07,0.075,0.08,0.085,
0.09,0.095,0.1,0.105,0.11,0.115,0.12,0.125,0.13,0.135,0.14,0.145,0.15,0.155,
0.16,0.165,0.17,0.175,0.18,0.185,0.19,0.195,0.2,0.205,0.21,0.215,0.22,0.225,
0.23,0.235,0.24,0.245,0.25,0.255,0.26,0.265,0.27,0.275,0.28,0.285,0.29,
0.295,0.3,0.305,0.31,0.315,0.32,0.325,0.33,0.335,0.34,0.345,0.35,0.355,
0.36,0.365,0.37,0.375,0.38,0.385,0.39,0.395,0.4,0.405,0.41,0.415,0.42,0.425,
0.43,0.435,0.44,0.445,0.45,0.455,0.46,0.465,0.47,0.475,0.48,0.485,0.49,
0.495,0.5,0.505,0.51,0.515,0.52,0.525,0.53,0.535,0.54,0.545,0.55,0.555,
0.56,0.565,0.57,0.575,0.58,0.585,0.59,0.595,0.6,0.605,0.61,0.615,0.62,0.625,
0.63,0.635,0.64,0.645,0.65,0.655,0.66,0.665,0.67,0.675,0.68,0.685,0.690000000000001,
0.695000000000001,0.700000000000001,0.705000000000001,0.710000000000001,
0.715000000000001,0.720000000000001,0.725000000000001,0.730000000000001,
0.735000000000001,0.740000000000001,0.745000000000001,0.750000000000001,
0.755000000000001,0.760000000000001,0.765000000000001,0.770000000000001,
0.775000000000001,0.780000000000001,0.785000000000001,0.790000000000001,
0.795000000000001,0.800000000000001,0.805000000000001,0.810000000000001,
0.815000000000001,0.820000000000001,0.825000000000001,0.830000000000001,
0.835000000000001,0.840000000000001,0.845000000000001,0.850000000000001,
0.855000000000001,0.860000000000001,0.865000000000001,0.870000000000001,
0.875000000000001,0.880000000000001,0.885000000000001,0.890000000000001,
0.895000000000001,0.900000000000001,0.905000000000001,0.910000000000001,
0.915000000000001,0.920000000000001,0.925000000000001,0.930000000000001,
0.935000000000001,0.940000000000001,0.941429844431358),.UNSPECIFIED.)
CURVE()
GEOMETRIC_REPRESENTATION_ITEM()
RATIONAL_B_SPLINE_CURVE((1.,1.,1.,1.,1.,1.,1.,1.,1.,1.,1.,1.,1.,1.,1.,1.,
1.,1.,1.,1.,1.,1.,1.,1.,1.,1.,1.,1.,1.,1.,1.,1.,1.,1.,1.,1.,1.,1.,1.,1.,
1.,1.,1.,1.,1.,1.,1.,1.,1.,1.,1.,1.,1.,1.,1.,1.,1.,1.,1.,1.,1.,1.,1.,1.,
1.,1.,1.,1.,1.,1.,1.,1.,1.,1.,1.,1.,1.,1.,1.,1.,1.,1.,1.,1.,1.,1.,1.,1.,
1.,1.,1.,1.,1.,1.,1.,1.,1.,1.,1.,1.,1.,1.,1.,1.,1.,1.,1.,1.,1.,1.,1.,1.,
1.,1.,1.,1.,1.,1.,1.,1.,1.,1.,1.,1.,1.,1.,1.,1.,1.,1.,1.,1.,1.,1.,1.,1.,
1.,1.,1.,1.,1.,1.,1.,1.,1.,1.,1.,1.,1.,1.,1.,1.,1.,1.,1.,1.,1.,1.,1.,1.,
1.,1.,1.,1.,1.,1.,1.,1.,1.,1.,1.,1.,1.,1.,1.,1.,1.,1.,1.,1.,1.,1.,1.,1.,
1.,1.,1.,1.,1.,1.,1.,1.,1.,1.))
REPRESENTATION_ITEM('')
);
#526=(
BOUNDED_CURVE()
B_SPLINE_CURVE(5,(#107885,#107886,#107887,#107888,#107889,#107890,#107891,
#107892,#107893,#107894,#107895,#107896,#107897,#107898,#107899,#107900,
#107901,#107902,#107903,#107904,#107905,#107906,#107907,#107908,#107909,
#107910,#107911,#107912,#107913,#107914,#107915,#107916,#107917,#107918,
#107919,#107920,#107921,#107922,#107923,#107924,#107925,#107926,#107927,
#107928,#107929,#107930,#107931,#107932,#107933,#107934,#107935,#107936,
#107937,#107938,#107939,#107940,#107941,#107942,#107943,#107944,#107945,
#107946,#107947,#107948,#107949,#107950,#107951,#107952,#107953,#107954,
#107955,#107956,#107957,#107958,#107959,#107960,#107961,#107962,#107963,
#107964,#107965,#107966,#107967,#107968,#107969,#107970,#107971,#107972,
#107973,#107974,#107975,#107976,#107977,#107978,#107979,#107980,#107981,
#107982,#107983,#107984,#107985,#107986,#107987,#107988,#107989,#107990,
#107991,#107992,#107993,#107994,#107995,#107996,#107997,#107998,#107999,
#108000,#108001,#108002,#108003,#108004,#108005,#108006,#108007,#108008,
#108009,#108010,#108011,#108012,#108013,#108014,#108015,#108016,#108017,
#108018,#108019,#108020,#108021,#108022,#108023,#108024,#108025,#108026,
#108027,#108028,#108029,#108030,#108031,#108032,#108033,#108034,#108035,
#108036,#108037,#108038,#108039,#108040,#108041,#108042,#108043,#108044,
#108045,#108046,#108047,#108048,#108049,#108050,#108051,#108052,#108053,
#108054,#108055,#108056,#108057,#108058,#108059,#108060,#108061,#108062,
#108063,#108064,#108065,#108066,#108067,#108068,#108069,#108070,#108071,
#108072,#108073,#108074,#108075,#108076,#108077,#108078),.UNSPECIFIED.,
 .F.,.F.)
B_SPLINE_CURVE_WITH_KNOTS((6,1,1,1,1,1,1,1,1,1,1,1,1,1,1,1,1,1,1,1,1,1,
1,1,1,1,1,1,1,1,1,1,1,1,1,1,1,1,1,1,1,1,1,1,1,1,1,1,1,1,1,1,1,1,1,1,1,1,
1,1,1,1,1,1,1,1,1,1,1,1,1,1,1,1,1,1,1,1,1,1,1,1,1,1,1,1,1,1,1,1,1,1,1,1,
1,1,1,1,1,1,1,1,1,1,1,1,1,1,1,1,1,1,1,1,1,1,1,1,1,1,1,1,1,1,1,1,1,1,1,1,
1,1,1,1,1,1,1,1,1,1,1,1,1,1,1,1,1,1,1,1,1,1,1,1,1,1,1,1,1,1,1,1,1,1,1,1,
1,1,1,1,1,1,1,1,1,1,1,1,1,1,1,1,1,1,1,1,1,1,1,6),(-0.941429844431381,-0.940000000000001,
-0.935000000000001,-0.930000000000001,-0.925000000000001,-0.920000000000001,
-0.915000000000001,-0.910000000000001,-0.905000000000001,-0.900000000000001,
-0.895000000000001,-0.890000000000001,-0.885000000000001,-0.880000000000001,
-0.875000000000001,-0.870000000000001,-0.865000000000001,-0.860000000000001,
-0.855000000000001,-0.850000000000001,-0.845000000000001,-0.840000000000001,
-0.835000000000001,-0.830000000000001,-0.825000000000001,-0.820000000000001,
-0.815000000000001,-0.810000000000001,-0.805000000000001,-0.800000000000001,
-0.795000000000001,-0.790000000000001,-0.785000000000001,-0.780000000000001,
-0.775000000000001,-0.770000000000001,-0.765000000000001,-0.760000000000001,
-0.755000000000001,-0.750000000000001,-0.745000000000001,-0.740000000000001,
-0.735000000000001,-0.730000000000001,-0.725000000000001,-0.720000000000001,
-0.715000000000001,-0.710000000000001,-0.705000000000001,-0.700000000000001,
-0.695000000000001,-0.690000000000001,-0.685,-0.68,-0.675,-0.67,-0.665,
-0.66,-0.655,-0.65,-0.645,-0.64,-0.635,-0.63,-0.625,-0.62,-0.615,-0.61,
-0.605,-0.6,-0.595,-0.59,-0.585,-0.58,-0.575,-0.57,-0.565,-0.56,-0.555,
-0.55,-0.545,-0.54,-0.535,-0.53,-0.525,-0.52,-0.515,-0.51,-0.505,-0.5,-0.495,
-0.49,-0.485,-0.48,-0.475,-0.47,-0.465,-0.46,-0.455,-0.45,-0.445,-0.44,
-0.435,-0.43,-0.425,-0.42,-0.415,-0.41,-0.405,-0.4,-0.395,-0.39,-0.385,
-0.38,-0.375,-0.37,-0.365,-0.36,-0.355,-0.35,-0.345,-0.34,-0.335,-0.33,
-0.325,-0.32,-0.315,-0.31,-0.305,-0.3,-0.295,-0.29,-0.285,-0.28,-0.275,
-0.27,-0.265,-0.26,-0.255,-0.25,-0.245,-0.24,-0.235,-0.23,-0.225,-0.22,
-0.215,-0.21,-0.205,-0.2,-0.195,-0.19,-0.185,-0.18,-0.175,-0.17,-0.165,
-0.16,-0.155,-0.15,-0.145,-0.14,-0.135,-0.13,-0.125,-0.12,-0.115,-0.11,
-0.105,-0.1,-0.095,-0.09,-0.085,-0.08,-0.075,-0.07,-0.065,-0.06,-0.055,
-0.05,-0.045,-0.04,-0.035,-0.03,-0.025,-0.02,-0.015,-0.01,-0.005,0.),
 .UNSPECIFIED.)
CURVE()
GEOMETRIC_REPRESENTATION_ITEM()
RATIONAL_B_SPLINE_CURVE((1.,1.,1.,1.,1.,1.,1.,1.,1.,1.,1.,1.,1.,1.,1.,1.,
1.,1.,1.,1.,1.,1.,1.,1.,1.,1.,1.,1.,1.,1.,1.,1.,1.,1.,1.,1.,1.,1.,1.,1.,
1.,1.,1.,1.,1.,1.,1.,1.,1.,1.,1.,1.,1.,1.,1.,1.,1.,1.,1.,1.,1.,1.,1.,1.,
1.,1.,1.,1.,1.,1.,1.,1.,1.,1.,1.,1.,1.,1.,1.,1.,1.,1.,1.,1.,1.,1.,1.,1.,
1.,1.,1.,1.,1.,1.,1.,1.,1.,1.,1.,1.,1.,1.,1.,1.,1.,1.,1.,1.,1.,1.,1.,1.,
1.,1.,1.,1.,1.,1.,1.,1.,1.,1.,1.,1.,1.,1.,1.,1.,1.,1.,1.,1.,1.,1.,1.,1.,
1.,1.,1.,1.,1.,1.,1.,1.,1.,1.,1.,1.,1.,1.,1.,1.,1.,1.,1.,1.,1.,1.,1.,1.,
1.,1.,1.,1.,1.,1.,1.,1.,1.,1.,1.,1.,1.,1.,1.,1.,1.,1.,1.,1.,1.,1.,1.,1.,
1.,1.,1.,1.,1.,1.,1.,1.,1.,1.))
REPRESENTATION_ITEM('')
);
#527=(
BOUNDED_CURVE()
B_SPLINE_CURVE(5,(#108585,#108586,#108587,#108588,#108589,#108590,#108591,
#108592,#108593,#108594,#108595,#108596,#108597,#108598,#108599,#108600,
#108601,#108602,#108603,#108604,#108605,#108606,#108607,#108608,#108609,
#108610,#108611,#108612,#108613,#108614,#108615,#108616,#108617,#108618,
#108619,#108620,#108621,#108622,#108623,#108624,#108625,#108626,#108627,
#108628,#108629,#108630,#108631,#108632,#108633,#108634,#108635,#108636,
#108637,#108638,#108639,#108640,#108641,#108642,#108643,#108644,#108645,
#108646,#108647,#108648,#108649,#108650,#108651,#108652,#108653,#108654,
#108655,#108656,#108657,#108658,#108659,#108660,#108661,#108662,#108663,
#108664,#108665,#108666,#108667,#108668,#108669,#108670,#108671,#108672,
#108673,#108674,#108675,#108676,#108677,#108678,#108679,#108680,#108681,
#108682,#108683,#108684,#108685,#108686,#108687,#108688,#108689,#108690,
#108691,#108692,#108693,#108694,#108695,#108696,#108697,#108698,#108699,
#108700,#108701,#108702,#108703,#108704,#108705,#108706,#108707,#108708,
#108709,#108710,#108711,#108712,#108713,#108714,#108715,#108716,#108717,
#108718,#108719,#108720,#108721,#108722,#108723,#108724,#108725,#108726,
#108727,#108728,#108729,#108730,#108731,#108732,#108733,#108734,#108735,
#108736,#108737,#108738,#108739,#108740,#108741,#108742,#108743,#108744,
#108745,#108746,#108747,#108748,#108749,#108750,#108751,#108752,#108753,
#108754,#108755,#108756,#108757,#108758,#108759,#108760,#108761,#108762,
#108763,#108764,#108765,#108766,#108767,#108768,#108769,#108770,#108771,
#108772,#108773,#108774,#108775,#108776,#108777,#108778),.UNSPECIFIED.,
 .F.,.F.)
B_SPLINE_CURVE_WITH_KNOTS((6,1,1,1,1,1,1,1,1,1,1,1,1,1,1,1,1,1,1,1,1,1,
1,1,1,1,1,1,1,1,1,1,1,1,1,1,1,1,1,1,1,1,1,1,1,1,1,1,1,1,1,1,1,1,1,1,1,1,
1,1,1,1,1,1,1,1,1,1,1,1,1,1,1,1,1,1,1,1,1,1,1,1,1,1,1,1,1,1,1,1,1,1,1,1,
1,1,1,1,1,1,1,1,1,1,1,1,1,1,1,1,1,1,1,1,1,1,1,1,1,1,1,1,1,1,1,1,1,1,1,1,
1,1,1,1,1,1,1,1,1,1,1,1,1,1,1,1,1,1,1,1,1,1,1,1,1,1,1,1,1,1,1,1,1,1,1,1,
1,1,1,1,1,1,1,1,1,1,1,1,1,1,1,1,1,1,1,1,1,1,1,6),(0.,0.005,0.01,0.015,0.02,
0.025,0.03,0.035,0.04,0.045,0.05,0.055,0.06,0.065,0.07,0.075,0.08,0.085,
0.09,0.095,0.1,0.105,0.11,0.115,0.12,0.125,0.13,0.135,0.14,0.145,0.15,0.155,
0.16,0.165,0.17,0.175,0.18,0.185,0.19,0.195,0.2,0.205,0.21,0.215,0.22,0.225,
0.23,0.235,0.24,0.245,0.25,0.255,0.26,0.265,0.27,0.275,0.28,0.285,0.29,
0.295,0.3,0.305,0.31,0.315,0.32,0.325,0.33,0.335,0.34,0.345,0.35,0.355,
0.36,0.365,0.37,0.375,0.38,0.385,0.39,0.395,0.4,0.405,0.41,0.415,0.42,0.425,
0.43,0.435,0.44,0.445,0.45,0.455,0.46,0.465,0.47,0.475,0.48,0.485,0.49,
0.495,0.5,0.505,0.51,0.515,0.52,0.525,0.53,0.535,0.54,0.545,0.55,0.555,
0.56,0.565,0.57,0.575,0.58,0.585,0.59,0.595,0.6,0.605,0.61,0.615,0.62,0.625,
0.63,0.635,0.64,0.645,0.65,0.655,0.66,0.665,0.67,0.675,0.68,0.685,0.690000000000001,
0.695000000000001,0.700000000000001,0.705000000000001,0.710000000000001,
0.715000000000001,0.720000000000001,0.725000000000001,0.730000000000001,
0.735000000000001,0.740000000000001,0.745000000000001,0.750000000000001,
0.755000000000001,0.760000000000001,0.765000000000001,0.770000000000001,
0.775000000000001,0.780000000000001,0.785000000000001,0.790000000000001,
0.795000000000001,0.800000000000001,0.805000000000001,0.810000000000001,
0.815000000000001,0.820000000000001,0.825000000000001,0.830000000000001,
0.835000000000001,0.840000000000001,0.845000000000001,0.850000000000001,
0.855000000000001,0.860000000000001,0.865000000000001,0.870000000000001,
0.875000000000001,0.880000000000001,0.885000000000001,0.890000000000001,
0.895000000000001,0.900000000000001,0.905000000000001,0.910000000000001,
0.915000000000001,0.920000000000001,0.925000000000001,0.930000000000001,
0.935000000000001,0.940000000000001,0.941429844431541),.UNSPECIFIED.)
CURVE()
GEOMETRIC_REPRESENTATION_ITEM()
RATIONAL_B_SPLINE_CURVE((1.,1.,1.,1.,1.,1.,1.,1.,1.,1.,1.,1.,1.,1.,1.,1.,
1.,1.,1.,1.,1.,1.,1.,1.,1.,1.,1.,1.,1.,1.,1.,1.,1.,1.,1.,1.,1.,1.,1.,1.,
1.,1.,1.,1.,1.,1.,1.,1.,1.,1.,1.,1.,1.,1.,1.,1.,1.,1.,1.,1.,1.,1.,1.,1.,
1.,1.,1.,1.,1.,1.,1.,1.,1.,1.,1.,1.,1.,1.,1.,1.,1.,1.,1.,1.,1.,1.,1.,1.,
1.,1.,1.,1.,1.,1.,1.,1.,1.,1.,1.,1.,1.,1.,1.,1.,1.,1.,1.,1.,1.,1.,1.,1.,
1.,1.,1.,1.,1.,1.,1.,1.,1.,1.,1.,1.,1.,1.,1.,1.,1.,1.,1.,1.,1.,1.,1.,1.,
1.,1.,1.,1.,1.,1.,1.,1.,1.,1.,1.,1.,1.,1.,1.,1.,1.,1.,1.,1.,1.,1.,1.,1.,
1.,1.,1.,1.,1.,1.,1.,1.,1.,1.,1.,1.,1.,1.,1.,1.,1.,1.,1.,1.,1.,1.,1.,1.,
1.,1.,1.,1.,1.,1.,1.,1.,1.,1.))
REPRESENTATION_ITEM('')
);
#528=(
BOUNDED_CURVE()
B_SPLINE_CURVE(5,(#108781,#108782,#108783,#108784,#108785,#108786,#108787,
#108788,#108789,#108790,#108791,#108792,#108793,#108794,#108795,#108796,
#108797,#108798,#108799,#108800,#108801,#108802,#108803,#108804,#108805,
#108806,#108807,#108808,#108809,#108810,#108811,#108812,#108813,#108814,
#108815,#108816,#108817,#108818,#108819,#108820,#108821,#108822,#108823,
#108824,#108825,#108826,#108827,#108828,#108829,#108830,#108831,#108832,
#108833,#108834,#108835,#108836,#108837,#108838,#108839,#108840,#108841,
#108842,#108843,#108844,#108845,#108846,#108847,#108848,#108849,#108850,
#108851,#108852,#108853,#108854,#108855,#108856,#108857,#108858,#108859,
#108860,#108861,#108862,#108863,#108864,#108865,#108866,#108867,#108868,
#108869,#108870,#108871,#108872,#108873,#108874,#108875,#108876,#108877,
#108878,#108879,#108880,#108881,#108882,#108883,#108884,#108885,#108886,
#108887,#108888,#108889,#108890,#108891,#108892,#108893,#108894,#108895,
#108896,#108897,#108898,#108899,#108900,#108901,#108902,#108903,#108904,
#108905,#108906,#108907,#108908,#108909,#108910,#108911,#108912,#108913,
#108914,#108915,#108916,#108917,#108918,#108919,#108920,#108921,#108922,
#108923,#108924,#108925,#108926,#108927,#108928,#108929,#108930,#108931,
#108932,#108933,#108934,#108935,#108936,#108937,#108938,#108939,#108940,
#108941,#108942,#108943,#108944,#108945,#108946,#108947,#108948,#108949,
#108950,#108951,#108952,#108953,#108954,#108955,#108956,#108957,#108958,
#108959,#108960,#108961,#108962,#108963,#108964,#108965,#108966,#108967,
#108968,#108969,#108970,#108971,#108972,#108973,#108974),.UNSPECIFIED.,
 .F.,.F.)
B_SPLINE_CURVE_WITH_KNOTS((6,1,1,1,1,1,1,1,1,1,1,1,1,1,1,1,1,1,1,1,1,1,
1,1,1,1,1,1,1,1,1,1,1,1,1,1,1,1,1,1,1,1,1,1,1,1,1,1,1,1,1,1,1,1,1,1,1,1,
1,1,1,1,1,1,1,1,1,1,1,1,1,1,1,1,1,1,1,1,1,1,1,1,1,1,1,1,1,1,1,1,1,1,1,1,
1,1,1,1,1,1,1,1,1,1,1,1,1,1,1,1,1,1,1,1,1,1,1,1,1,1,1,1,1,1,1,1,1,1,1,1,
1,1,1,1,1,1,1,1,1,1,1,1,1,1,1,1,1,1,1,1,1,1,1,1,1,1,1,1,1,1,1,1,1,1,1,1,
1,1,1,1,1,1,1,1,1,1,1,1,1,1,1,1,1,1,1,1,1,1,1,6),(-0.941429844431541,-0.940000000000001,
-0.935000000000001,-0.930000000000001,-0.925000000000001,-0.920000000000001,
-0.915000000000001,-0.910000000000001,-0.905000000000001,-0.900000000000001,
-0.895000000000001,-0.890000000000001,-0.885000000000001,-0.880000000000001,
-0.875000000000001,-0.870000000000001,-0.865000000000001,-0.860000000000001,
-0.855000000000001,-0.850000000000001,-0.845000000000001,-0.840000000000001,
-0.835000000000001,-0.830000000000001,-0.825000000000001,-0.820000000000001,
-0.815000000000001,-0.810000000000001,-0.805000000000001,-0.800000000000001,
-0.795000000000001,-0.790000000000001,-0.785000000000001,-0.780000000000001,
-0.775000000000001,-0.770000000000001,-0.765000000000001,-0.760000000000001,
-0.755000000000001,-0.750000000000001,-0.745000000000001,-0.740000000000001,
-0.735000000000001,-0.730000000000001,-0.725000000000001,-0.720000000000001,
-0.715000000000001,-0.710000000000001,-0.705000000000001,-0.700000000000001,
-0.695000000000001,-0.690000000000001,-0.685,-0.68,-0.675,-0.67,-0.665,
-0.66,-0.655,-0.65,-0.645,-0.64,-0.635,-0.63,-0.625,-0.62,-0.615,-0.61,
-0.605,-0.6,-0.595,-0.59,-0.585,-0.58,-0.575,-0.57,-0.565,-0.56,-0.555,
-0.55,-0.545,-0.54,-0.535,-0.53,-0.525,-0.52,-0.515,-0.51,-0.505,-0.5,-0.495,
-0.49,-0.485,-0.48,-0.475,-0.47,-0.465,-0.46,-0.455,-0.45,-0.445,-0.44,
-0.435,-0.43,-0.425,-0.42,-0.415,-0.41,-0.405,-0.4,-0.395,-0.39,-0.385,
-0.38,-0.375,-0.37,-0.365,-0.36,-0.355,-0.35,-0.345,-0.34,-0.335,-0.33,
-0.325,-0.32,-0.315,-0.31,-0.305,-0.3,-0.295,-0.29,-0.285,-0.28,-0.275,
-0.27,-0.265,-0.26,-0.255,-0.25,-0.245,-0.24,-0.235,-0.23,-0.225,-0.22,
-0.215,-0.21,-0.205,-0.2,-0.195,-0.19,-0.185,-0.18,-0.175,-0.17,-0.165,
-0.16,-0.155,-0.15,-0.145,-0.14,-0.135,-0.13,-0.125,-0.12,-0.115,-0.11,
-0.105,-0.1,-0.095,-0.09,-0.085,-0.08,-0.075,-0.07,-0.065,-0.06,-0.055,
-0.05,-0.045,-0.04,-0.035,-0.03,-0.025,-0.02,-0.015,-0.01,-0.005,0.),
 .UNSPECIFIED.)
CURVE()
GEOMETRIC_REPRESENTATION_ITEM()
RATIONAL_B_SPLINE_CURVE((1.,1.,1.,1.,1.,1.,1.,1.,1.,1.,1.,1.,1.,1.,1.,1.,
1.,1.,1.,1.,1.,1.,1.,1.,1.,1.,1.,1.,1.,1.,1.,1.,1.,1.,1.,1.,1.,1.,1.,1.,
1.,1.,1.,1.,1.,1.,1.,1.,1.,1.,1.,1.,1.,1.,1.,1.,1.,1.,1.,1.,1.,1.,1.,1.,
1.,1.,1.,1.,1.,1.,1.,1.,1.,1.,1.,1.,1.,1.,1.,1.,1.,1.,1.,1.,1.,1.,1.,1.,
1.,1.,1.,1.,1.,1.,1.,1.,1.,1.,1.,1.,1.,1.,1.,1.,1.,1.,1.,1.,1.,1.,1.,1.,
1.,1.,1.,1.,1.,1.,1.,1.,1.,1.,1.,1.,1.,1.,1.,1.,1.,1.,1.,1.,1.,1.,1.,1.,
1.,1.,1.,1.,1.,1.,1.,1.,1.,1.,1.,1.,1.,1.,1.,1.,1.,1.,1.,1.,1.,1.,1.,1.,
1.,1.,1.,1.,1.,1.,1.,1.,1.,1.,1.,1.,1.,1.,1.,1.,1.,1.,1.,1.,1.,1.,1.,1.,
1.,1.,1.,1.,1.,1.,1.,1.,1.,1.))
REPRESENTATION_ITEM('')
);
#529=(
BOUNDED_CURVE()
B_SPLINE_CURVE(5,(#109481,#109482,#109483,#109484,#109485,#109486,#109487,
#109488,#109489,#109490,#109491,#109492,#109493,#109494,#109495,#109496,
#109497,#109498,#109499,#109500,#109501,#109502,#109503,#109504,#109505,
#109506,#109507,#109508,#109509,#109510,#109511,#109512,#109513,#109514,
#109515,#109516,#109517,#109518,#109519,#109520,#109521,#109522,#109523,
#109524,#109525,#109526,#109527,#109528,#109529,#109530,#109531,#109532,
#109533,#109534,#109535,#109536,#109537,#109538,#109539,#109540,#109541,
#109542,#109543,#109544,#109545,#109546,#109547,#109548,#109549,#109550,
#109551,#109552,#109553,#109554,#109555,#109556,#109557,#109558,#109559,
#109560,#109561,#109562,#109563,#109564,#109565,#109566,#109567,#109568,
#109569,#109570,#109571,#109572,#109573,#109574,#109575,#109576,#109577,
#109578,#109579,#109580,#109581,#109582,#109583,#109584,#109585,#109586,
#109587,#109588,#109589,#109590,#109591,#109592,#109593,#109594,#109595,
#109596,#109597,#109598,#109599,#109600,#109601,#109602,#109603,#109604,
#109605,#109606,#109607,#109608,#109609,#109610,#109611,#109612,#109613,
#109614,#109615,#109616,#109617,#109618,#109619,#109620,#109621,#109622,
#109623,#109624,#109625,#109626,#109627,#109628,#109629,#109630,#109631,
#109632,#109633,#109634,#109635,#109636,#109637,#109638,#109639,#109640,
#109641,#109642,#109643,#109644,#109645,#109646,#109647,#109648,#109649,
#109650,#109651,#109652,#109653,#109654,#109655,#109656,#109657,#109658,
#109659,#109660,#109661,#109662,#109663,#109664,#109665,#109666,#109667,
#109668,#109669,#109670,#109671,#109672,#109673,#109674),.UNSPECIFIED.,
 .F.,.F.)
B_SPLINE_CURVE_WITH_KNOTS((6,1,1,1,1,1,1,1,1,1,1,1,1,1,1,1,1,1,1,1,1,1,
1,1,1,1,1,1,1,1,1,1,1,1,1,1,1,1,1,1,1,1,1,1,1,1,1,1,1,1,1,1,1,1,1,1,1,1,
1,1,1,1,1,1,1,1,1,1,1,1,1,1,1,1,1,1,1,1,1,1,1,1,1,1,1,1,1,1,1,1,1,1,1,1,
1,1,1,1,1,1,1,1,1,1,1,1,1,1,1,1,1,1,1,1,1,1,1,1,1,1,1,1,1,1,1,1,1,1,1,1,
1,1,1,1,1,1,1,1,1,1,1,1,1,1,1,1,1,1,1,1,1,1,1,1,1,1,1,1,1,1,1,1,1,1,1,1,
1,1,1,1,1,1,1,1,1,1,1,1,1,1,1,1,1,1,1,1,1,1,1,6),(0.,0.005,0.01,0.015,0.02,
0.025,0.03,0.035,0.04,0.045,0.05,0.055,0.06,0.065,0.07,0.075,0.08,0.085,
0.09,0.095,0.1,0.105,0.11,0.115,0.12,0.125,0.13,0.135,0.14,0.145,0.15,0.155,
0.16,0.165,0.17,0.175,0.18,0.185,0.19,0.195,0.2,0.205,0.21,0.215,0.22,0.225,
0.23,0.235,0.24,0.245,0.25,0.255,0.26,0.265,0.27,0.275,0.28,0.285,0.29,
0.295,0.3,0.305,0.31,0.315,0.32,0.325,0.33,0.335,0.34,0.345,0.35,0.355,
0.36,0.365,0.37,0.375,0.38,0.385,0.39,0.395,0.4,0.405,0.41,0.415,0.42,0.425,
0.43,0.435,0.44,0.445,0.45,0.455,0.46,0.465,0.47,0.475,0.48,0.485,0.49,
0.495,0.5,0.505,0.51,0.515,0.52,0.525,0.53,0.535,0.54,0.545,0.55,0.555,
0.56,0.565,0.57,0.575,0.58,0.585,0.59,0.595,0.6,0.605,0.61,0.615,0.62,0.625,
0.63,0.635,0.64,0.645,0.65,0.655,0.66,0.665,0.67,0.675,0.68,0.685,0.690000000000001,
0.695000000000001,0.700000000000001,0.705000000000001,0.710000000000001,
0.715000000000001,0.720000000000001,0.725000000000001,0.730000000000001,
0.735000000000001,0.740000000000001,0.745000000000001,0.750000000000001,
0.755000000000001,0.760000000000001,0.765000000000001,0.770000000000001,
0.775000000000001,0.780000000000001,0.785000000000001,0.790000000000001,
0.795000000000001,0.800000000000001,0.805000000000001,0.810000000000001,
0.815000000000001,0.820000000000001,0.825000000000001,0.830000000000001,
0.835000000000001,0.840000000000001,0.845000000000001,0.850000000000001,
0.855000000000001,0.860000000000001,0.865000000000001,0.870000000000001,
0.875000000000001,0.880000000000001,0.885000000000001,0.890000000000001,
0.895000000000001,0.900000000000001,0.905000000000001,0.910000000000001,
0.915000000000001,0.920000000000001,0.925000000000001,0.930000000000001,
0.935000000000001,0.940000000000001,0.941429844431311),.UNSPECIFIED.)
CURVE()
GEOMETRIC_REPRESENTATION_ITEM()
RATIONAL_B_SPLINE_CURVE((1.,1.,1.,1.,1.,1.,1.,1.,1.,1.,1.,1.,1.,1.,1.,1.,
1.,1.,1.,1.,1.,1.,1.,1.,1.,1.,1.,1.,1.,1.,1.,1.,1.,1.,1.,1.,1.,1.,1.,1.,
1.,1.,1.,1.,1.,1.,1.,1.,1.,1.,1.,1.,1.,1.,1.,1.,1.,1.,1.,1.,1.,1.,1.,1.,
1.,1.,1.,1.,1.,1.,1.,1.,1.,1.,1.,1.,1.,1.,1.,1.,1.,1.,1.,1.,1.,1.,1.,1.,
1.,1.,1.,1.,1.,1.,1.,1.,1.,1.,1.,1.,1.,1.,1.,1.,1.,1.,1.,1.,1.,1.,1.,1.,
1.,1.,1.,1.,1.,1.,1.,1.,1.,1.,1.,1.,1.,1.,1.,1.,1.,1.,1.,1.,1.,1.,1.,1.,
1.,1.,1.,1.,1.,1.,1.,1.,1.,1.,1.,1.,1.,1.,1.,1.,1.,1.,1.,1.,1.,1.,1.,1.,
1.,1.,1.,1.,1.,1.,1.,1.,1.,1.,1.,1.,1.,1.,1.,1.,1.,1.,1.,1.,1.,1.,1.,1.,
1.,1.,1.,1.,1.,1.,1.,1.,1.,1.))
REPRESENTATION_ITEM('')
);
#530=(
BOUNDED_CURVE()
B_SPLINE_CURVE(5,(#109677,#109678,#109679,#109680,#109681,#109682,#109683,
#109684,#109685,#109686,#109687,#109688,#109689,#109690,#109691,#109692,
#109693,#109694,#109695,#109696,#109697,#109698,#109699,#109700,#109701,
#109702,#109703,#109704,#109705,#109706,#109707,#109708,#109709,#109710,
#109711,#109712,#109713,#109714,#109715,#109716,#109717,#109718,#109719,
#109720,#109721,#109722,#109723,#109724,#109725,#109726,#109727,#109728,
#109729,#109730,#109731,#109732,#109733,#109734,#109735,#109736,#109737,
#109738,#109739,#109740,#109741,#109742,#109743,#109744,#109745,#109746,
#109747,#109748,#109749,#109750,#109751,#109752,#109753,#109754,#109755,
#109756,#109757,#109758,#109759,#109760,#109761,#109762,#109763,#109764,
#109765,#109766,#109767,#109768,#109769,#109770,#109771,#109772,#109773,
#109774,#109775,#109776,#109777,#109778,#109779,#109780,#109781,#109782,
#109783,#109784,#109785,#109786,#109787,#109788,#109789,#109790,#109791,
#109792,#109793,#109794,#109795,#109796,#109797,#109798,#109799,#109800,
#109801,#109802,#109803,#109804,#109805,#109806,#109807,#109808,#109809,
#109810,#109811,#109812,#109813,#109814,#109815,#109816,#109817,#109818,
#109819,#109820,#109821,#109822,#109823,#109824,#109825,#109826,#109827,
#109828,#109829,#109830,#109831,#109832,#109833,#109834,#109835,#109836,
#109837,#109838,#109839,#109840,#109841,#109842,#109843,#109844,#109845,
#109846,#109847,#109848,#109849,#109850,#109851,#109852,#109853,#109854,
#109855,#109856,#109857,#109858,#109859,#109860,#109861,#109862,#109863,
#109864,#109865,#109866,#109867,#109868,#109869,#109870),.UNSPECIFIED.,
 .F.,.F.)
B_SPLINE_CURVE_WITH_KNOTS((6,1,1,1,1,1,1,1,1,1,1,1,1,1,1,1,1,1,1,1,1,1,
1,1,1,1,1,1,1,1,1,1,1,1,1,1,1,1,1,1,1,1,1,1,1,1,1,1,1,1,1,1,1,1,1,1,1,1,
1,1,1,1,1,1,1,1,1,1,1,1,1,1,1,1,1,1,1,1,1,1,1,1,1,1,1,1,1,1,1,1,1,1,1,1,
1,1,1,1,1,1,1,1,1,1,1,1,1,1,1,1,1,1,1,1,1,1,1,1,1,1,1,1,1,1,1,1,1,1,1,1,
1,1,1,1,1,1,1,1,1,1,1,1,1,1,1,1,1,1,1,1,1,1,1,1,1,1,1,1,1,1,1,1,1,1,1,1,
1,1,1,1,1,1,1,1,1,1,1,1,1,1,1,1,1,1,1,1,1,1,1,6),(-0.941429844431311,-0.940000000000001,
-0.935000000000001,-0.930000000000001,-0.925000000000001,-0.920000000000001,
-0.915000000000001,-0.910000000000001,-0.905000000000001,-0.900000000000001,
-0.895000000000001,-0.890000000000001,-0.885000000000001,-0.880000000000001,
-0.875000000000001,-0.870000000000001,-0.865000000000001,-0.860000000000001,
-0.855000000000001,-0.850000000000001,-0.845000000000001,-0.840000000000001,
-0.835000000000001,-0.830000000000001,-0.825000000000001,-0.820000000000001,
-0.815000000000001,-0.810000000000001,-0.805000000000001,-0.800000000000001,
-0.795000000000001,-0.790000000000001,-0.785000000000001,-0.780000000000001,
-0.775000000000001,-0.770000000000001,-0.765000000000001,-0.760000000000001,
-0.755000000000001,-0.750000000000001,-0.745000000000001,-0.740000000000001,
-0.735000000000001,-0.730000000000001,-0.725000000000001,-0.720000000000001,
-0.715000000000001,-0.710000000000001,-0.705000000000001,-0.700000000000001,
-0.695000000000001,-0.690000000000001,-0.685,-0.68,-0.675,-0.67,-0.665,
-0.66,-0.655,-0.65,-0.645,-0.64,-0.635,-0.63,-0.625,-0.62,-0.615,-0.61,
-0.605,-0.6,-0.595,-0.59,-0.585,-0.58,-0.575,-0.57,-0.565,-0.56,-0.555,
-0.55,-0.545,-0.54,-0.535,-0.53,-0.525,-0.52,-0.515,-0.51,-0.505,-0.5,-0.495,
-0.49,-0.485,-0.48,-0.475,-0.47,-0.465,-0.46,-0.455,-0.45,-0.445,-0.44,
-0.435,-0.43,-0.425,-0.42,-0.415,-0.41,-0.405,-0.4,-0.395,-0.39,-0.385,
-0.38,-0.375,-0.37,-0.365,-0.36,-0.355,-0.35,-0.345,-0.34,-0.335,-0.33,
-0.325,-0.32,-0.315,-0.31,-0.305,-0.3,-0.295,-0.29,-0.285,-0.28,-0.275,
-0.27,-0.265,-0.26,-0.255,-0.25,-0.245,-0.24,-0.235,-0.23,-0.225,-0.22,
-0.215,-0.21,-0.205,-0.2,-0.195,-0.19,-0.185,-0.18,-0.175,-0.17,-0.165,
-0.16,-0.155,-0.15,-0.145,-0.14,-0.135,-0.13,-0.125,-0.12,-0.115,-0.11,
-0.105,-0.1,-0.095,-0.09,-0.085,-0.08,-0.075,-0.07,-0.065,-0.06,-0.055,
-0.05,-0.045,-0.04,-0.035,-0.03,-0.025,-0.02,-0.015,-0.01,-0.005,0.),
 .UNSPECIFIED.)
CURVE()
GEOMETRIC_REPRESENTATION_ITEM()
RATIONAL_B_SPLINE_CURVE((1.,1.,1.,1.,1.,1.,1.,1.,1.,1.,1.,1.,1.,1.,1.,1.,
1.,1.,1.,1.,1.,1.,1.,1.,1.,1.,1.,1.,1.,1.,1.,1.,1.,1.,1.,1.,1.,1.,1.,1.,
1.,1.,1.,1.,1.,1.,1.,1.,1.,1.,1.,1.,1.,1.,1.,1.,1.,1.,1.,1.,1.,1.,1.,1.,
1.,1.,1.,1.,1.,1.,1.,1.,1.,1.,1.,1.,1.,1.,1.,1.,1.,1.,1.,1.,1.,1.,1.,1.,
1.,1.,1.,1.,1.,1.,1.,1.,1.,1.,1.,1.,1.,1.,1.,1.,1.,1.,1.,1.,1.,1.,1.,1.,
1.,1.,1.,1.,1.,1.,1.,1.,1.,1.,1.,1.,1.,1.,1.,1.,1.,1.,1.,1.,1.,1.,1.,1.,
1.,1.,1.,1.,1.,1.,1.,1.,1.,1.,1.,1.,1.,1.,1.,1.,1.,1.,1.,1.,1.,1.,1.,1.,
1.,1.,1.,1.,1.,1.,1.,1.,1.,1.,1.,1.,1.,1.,1.,1.,1.,1.,1.,1.,1.,1.,1.,1.,
1.,1.,1.,1.,1.,1.,1.,1.,1.,1.))
REPRESENTATION_ITEM('')
);
#531=(
BOUNDED_CURVE()
B_SPLINE_CURVE(5,(#110377,#110378,#110379,#110380,#110381,#110382,#110383,
#110384,#110385,#110386,#110387,#110388,#110389,#110390,#110391,#110392,
#110393,#110394,#110395,#110396,#110397,#110398,#110399,#110400,#110401,
#110402,#110403,#110404,#110405,#110406,#110407,#110408,#110409,#110410,
#110411,#110412,#110413,#110414,#110415,#110416,#110417,#110418,#110419,
#110420,#110421,#110422,#110423,#110424,#110425,#110426,#110427,#110428,
#110429,#110430,#110431,#110432,#110433,#110434,#110435,#110436,#110437,
#110438,#110439,#110440,#110441,#110442,#110443,#110444,#110445,#110446,
#110447,#110448,#110449,#110450,#110451,#110452,#110453,#110454,#110455,
#110456,#110457,#110458,#110459,#110460,#110461,#110462,#110463,#110464,
#110465,#110466,#110467,#110468,#110469,#110470,#110471,#110472,#110473,
#110474,#110475,#110476,#110477,#110478,#110479,#110480,#110481,#110482,
#110483,#110484,#110485,#110486,#110487,#110488,#110489,#110490,#110491,
#110492,#110493,#110494,#110495,#110496,#110497,#110498,#110499,#110500,
#110501,#110502,#110503,#110504,#110505,#110506,#110507,#110508,#110509,
#110510,#110511,#110512,#110513,#110514,#110515,#110516,#110517,#110518,
#110519,#110520,#110521,#110522,#110523,#110524,#110525,#110526,#110527,
#110528,#110529,#110530,#110531,#110532,#110533,#110534,#110535,#110536,
#110537,#110538,#110539,#110540,#110541,#110542,#110543,#110544,#110545,
#110546,#110547,#110548,#110549,#110550,#110551,#110552,#110553,#110554,
#110555,#110556,#110557,#110558,#110559,#110560,#110561,#110562,#110563,
#110564,#110565,#110566,#110567,#110568,#110569,#110570),.UNSPECIFIED.,
 .F.,.F.)
B_SPLINE_CURVE_WITH_KNOTS((6,1,1,1,1,1,1,1,1,1,1,1,1,1,1,1,1,1,1,1,1,1,
1,1,1,1,1,1,1,1,1,1,1,1,1,1,1,1,1,1,1,1,1,1,1,1,1,1,1,1,1,1,1,1,1,1,1,1,
1,1,1,1,1,1,1,1,1,1,1,1,1,1,1,1,1,1,1,1,1,1,1,1,1,1,1,1,1,1,1,1,1,1,1,1,
1,1,1,1,1,1,1,1,1,1,1,1,1,1,1,1,1,1,1,1,1,1,1,1,1,1,1,1,1,1,1,1,1,1,1,1,
1,1,1,1,1,1,1,1,1,1,1,1,1,1,1,1,1,1,1,1,1,1,1,1,1,1,1,1,1,1,1,1,1,1,1,1,
1,1,1,1,1,1,1,1,1,1,1,1,1,1,1,1,1,1,1,1,1,1,1,6),(0.,0.005,0.01,0.015,0.02,
0.025,0.03,0.035,0.04,0.045,0.05,0.055,0.06,0.065,0.07,0.075,0.08,0.085,
0.09,0.095,0.1,0.105,0.11,0.115,0.12,0.125,0.13,0.135,0.14,0.145,0.15,0.155,
0.16,0.165,0.17,0.175,0.18,0.185,0.19,0.195,0.2,0.205,0.21,0.215,0.22,0.225,
0.23,0.235,0.24,0.245,0.25,0.255,0.26,0.265,0.27,0.275,0.28,0.285,0.29,
0.295,0.3,0.305,0.31,0.315,0.32,0.325,0.33,0.335,0.34,0.345,0.35,0.355,
0.36,0.365,0.37,0.375,0.38,0.385,0.39,0.395,0.4,0.405,0.41,0.415,0.42,0.425,
0.43,0.435,0.44,0.445,0.45,0.455,0.46,0.465,0.47,0.475,0.48,0.485,0.49,
0.495,0.5,0.505,0.51,0.515,0.52,0.525,0.53,0.535,0.54,0.545,0.55,0.555,
0.56,0.565,0.57,0.575,0.58,0.585,0.59,0.595,0.6,0.605,0.61,0.615,0.62,0.625,
0.63,0.635,0.64,0.645,0.65,0.655,0.66,0.665,0.67,0.675,0.68,0.685,0.690000000000001,
0.695000000000001,0.700000000000001,0.705000000000001,0.710000000000001,
0.715000000000001,0.720000000000001,0.725000000000001,0.730000000000001,
0.735000000000001,0.740000000000001,0.745000000000001,0.750000000000001,
0.755000000000001,0.760000000000001,0.765000000000001,0.770000000000001,
0.775000000000001,0.780000000000001,0.785000000000001,0.790000000000001,
0.795000000000001,0.800000000000001,0.805000000000001,0.810000000000001,
0.815000000000001,0.820000000000001,0.825000000000001,0.830000000000001,
0.835000000000001,0.840000000000001,0.845000000000001,0.850000000000001,
0.855000000000001,0.860000000000001,0.865000000000001,0.870000000000001,
0.875000000000001,0.880000000000001,0.885000000000001,0.890000000000001,
0.895000000000001,0.900000000000001,0.905000000000001,0.910000000000001,
0.915000000000001,0.920000000000001,0.925000000000001,0.930000000000001,
0.935000000000001,0.940000000000001,0.941429844431297),.UNSPECIFIED.)
CURVE()
GEOMETRIC_REPRESENTATION_ITEM()
RATIONAL_B_SPLINE_CURVE((1.,1.,1.,1.,1.,1.,1.,1.,1.,1.,1.,1.,1.,1.,1.,1.,
1.,1.,1.,1.,1.,1.,1.,1.,1.,1.,1.,1.,1.,1.,1.,1.,1.,1.,1.,1.,1.,1.,1.,1.,
1.,1.,1.,1.,1.,1.,1.,1.,1.,1.,1.,1.,1.,1.,1.,1.,1.,1.,1.,1.,1.,1.,1.,1.,
1.,1.,1.,1.,1.,1.,1.,1.,1.,1.,1.,1.,1.,1.,1.,1.,1.,1.,1.,1.,1.,1.,1.,1.,
1.,1.,1.,1.,1.,1.,1.,1.,1.,1.,1.,1.,1.,1.,1.,1.,1.,1.,1.,1.,1.,1.,1.,1.,
1.,1.,1.,1.,1.,1.,1.,1.,1.,1.,1.,1.,1.,1.,1.,1.,1.,1.,1.,1.,1.,1.,1.,1.,
1.,1.,1.,1.,1.,1.,1.,1.,1.,1.,1.,1.,1.,1.,1.,1.,1.,1.,1.,1.,1.,1.,1.,1.,
1.,1.,1.,1.,1.,1.,1.,1.,1.,1.,1.,1.,1.,1.,1.,1.,1.,1.,1.,1.,1.,1.,1.,1.,
1.,1.,1.,1.,1.,1.,1.,1.,1.,1.))
REPRESENTATION_ITEM('')
);
#532=(
BOUNDED_CURVE()
B_SPLINE_CURVE(5,(#110573,#110574,#110575,#110576,#110577,#110578,#110579,
#110580,#110581,#110582,#110583,#110584,#110585,#110586,#110587,#110588,
#110589,#110590,#110591,#110592,#110593,#110594,#110595,#110596,#110597,
#110598,#110599,#110600,#110601,#110602,#110603,#110604,#110605,#110606,
#110607,#110608,#110609,#110610,#110611,#110612,#110613,#110614,#110615,
#110616,#110617,#110618,#110619,#110620,#110621,#110622,#110623,#110624,
#110625,#110626,#110627,#110628,#110629,#110630,#110631,#110632,#110633,
#110634,#110635,#110636,#110637,#110638,#110639,#110640,#110641,#110642,
#110643,#110644,#110645,#110646,#110647,#110648,#110649,#110650,#110651,
#110652,#110653,#110654,#110655,#110656,#110657,#110658,#110659,#110660,
#110661,#110662,#110663,#110664,#110665,#110666,#110667,#110668,#110669,
#110670,#110671,#110672,#110673,#110674,#110675,#110676,#110677,#110678,
#110679,#110680,#110681,#110682,#110683,#110684,#110685,#110686,#110687,
#110688,#110689,#110690,#110691,#110692,#110693,#110694,#110695,#110696,
#110697,#110698,#110699,#110700,#110701,#110702,#110703,#110704,#110705,
#110706,#110707,#110708,#110709,#110710,#110711,#110712,#110713,#110714,
#110715,#110716,#110717,#110718,#110719,#110720,#110721,#110722,#110723,
#110724,#110725,#110726,#110727,#110728,#110729,#110730,#110731,#110732,
#110733,#110734,#110735,#110736,#110737,#110738,#110739,#110740,#110741,
#110742,#110743,#110744,#110745,#110746,#110747,#110748,#110749,#110750,
#110751,#110752,#110753,#110754,#110755,#110756,#110757,#110758,#110759,
#110760,#110761,#110762,#110763,#110764,#110765,#110766),.UNSPECIFIED.,
 .F.,.F.)
B_SPLINE_CURVE_WITH_KNOTS((6,1,1,1,1,1,1,1,1,1,1,1,1,1,1,1,1,1,1,1,1,1,
1,1,1,1,1,1,1,1,1,1,1,1,1,1,1,1,1,1,1,1,1,1,1,1,1,1,1,1,1,1,1,1,1,1,1,1,
1,1,1,1,1,1,1,1,1,1,1,1,1,1,1,1,1,1,1,1,1,1,1,1,1,1,1,1,1,1,1,1,1,1,1,1,
1,1,1,1,1,1,1,1,1,1,1,1,1,1,1,1,1,1,1,1,1,1,1,1,1,1,1,1,1,1,1,1,1,1,1,1,
1,1,1,1,1,1,1,1,1,1,1,1,1,1,1,1,1,1,1,1,1,1,1,1,1,1,1,1,1,1,1,1,1,1,1,1,
1,1,1,1,1,1,1,1,1,1,1,1,1,1,1,1,1,1,1,1,1,1,1,6),(-0.941429844431289,-0.940000000000001,
-0.935000000000001,-0.930000000000001,-0.925000000000001,-0.920000000000001,
-0.915000000000001,-0.910000000000001,-0.905000000000001,-0.900000000000001,
-0.895000000000001,-0.890000000000001,-0.885000000000001,-0.880000000000001,
-0.875000000000001,-0.870000000000001,-0.865000000000001,-0.860000000000001,
-0.855000000000001,-0.850000000000001,-0.845000000000001,-0.840000000000001,
-0.835000000000001,-0.830000000000001,-0.825000000000001,-0.820000000000001,
-0.815000000000001,-0.810000000000001,-0.805000000000001,-0.800000000000001,
-0.795000000000001,-0.790000000000001,-0.785000000000001,-0.780000000000001,
-0.775000000000001,-0.770000000000001,-0.765000000000001,-0.760000000000001,
-0.755000000000001,-0.750000000000001,-0.745000000000001,-0.740000000000001,
-0.735000000000001,-0.730000000000001,-0.725000000000001,-0.720000000000001,
-0.715000000000001,-0.710000000000001,-0.705000000000001,-0.700000000000001,
-0.695000000000001,-0.690000000000001,-0.685,-0.68,-0.675,-0.67,-0.665,
-0.66,-0.655,-0.65,-0.645,-0.64,-0.635,-0.63,-0.625,-0.62,-0.615,-0.61,
-0.605,-0.6,-0.595,-0.59,-0.585,-0.58,-0.575,-0.57,-0.565,-0.56,-0.555,
-0.55,-0.545,-0.54,-0.535,-0.53,-0.525,-0.52,-0.515,-0.51,-0.505,-0.5,-0.495,
-0.49,-0.485,-0.48,-0.475,-0.47,-0.465,-0.46,-0.455,-0.45,-0.445,-0.44,
-0.435,-0.43,-0.425,-0.42,-0.415,-0.41,-0.405,-0.4,-0.395,-0.39,-0.385,
-0.38,-0.375,-0.37,-0.365,-0.36,-0.355,-0.35,-0.345,-0.34,-0.335,-0.33,
-0.325,-0.32,-0.315,-0.31,-0.305,-0.3,-0.295,-0.29,-0.285,-0.28,-0.275,
-0.27,-0.265,-0.26,-0.255,-0.25,-0.245,-0.24,-0.235,-0.23,-0.225,-0.22,
-0.215,-0.21,-0.205,-0.2,-0.195,-0.19,-0.185,-0.18,-0.175,-0.17,-0.165,
-0.16,-0.155,-0.15,-0.145,-0.14,-0.135,-0.13,-0.125,-0.12,-0.115,-0.11,
-0.105,-0.1,-0.095,-0.09,-0.085,-0.08,-0.075,-0.07,-0.065,-0.06,-0.055,
-0.05,-0.045,-0.04,-0.035,-0.03,-0.025,-0.02,-0.015,-0.01,-0.005,0.),
 .UNSPECIFIED.)
CURVE()
GEOMETRIC_REPRESENTATION_ITEM()
RATIONAL_B_SPLINE_CURVE((1.,1.,1.,1.,1.,1.,1.,1.,1.,1.,1.,1.,1.,1.,1.,1.,
1.,1.,1.,1.,1.,1.,1.,1.,1.,1.,1.,1.,1.,1.,1.,1.,1.,1.,1.,1.,1.,1.,1.,1.,
1.,1.,1.,1.,1.,1.,1.,1.,1.,1.,1.,1.,1.,1.,1.,1.,1.,1.,1.,1.,1.,1.,1.,1.,
1.,1.,1.,1.,1.,1.,1.,1.,1.,1.,1.,1.,1.,1.,1.,1.,1.,1.,1.,1.,1.,1.,1.,1.,
1.,1.,1.,1.,1.,1.,1.,1.,1.,1.,1.,1.,1.,1.,1.,1.,1.,1.,1.,1.,1.,1.,1.,1.,
1.,1.,1.,1.,1.,1.,1.,1.,1.,1.,1.,1.,1.,1.,1.,1.,1.,1.,1.,1.,1.,1.,1.,1.,
1.,1.,1.,1.,1.,1.,1.,1.,1.,1.,1.,1.,1.,1.,1.,1.,1.,1.,1.,1.,1.,1.,1.,1.,
1.,1.,1.,1.,1.,1.,1.,1.,1.,1.,1.,1.,1.,1.,1.,1.,1.,1.,1.,1.,1.,1.,1.,1.,
1.,1.,1.,1.,1.,1.,1.,1.,1.,1.))
REPRESENTATION_ITEM('')
);
#533=(
BOUNDED_CURVE()
B_SPLINE_CURVE(5,(#111273,#111274,#111275,#111276,#111277,#111278,#111279,
#111280,#111281,#111282,#111283,#111284,#111285,#111286,#111287,#111288,
#111289,#111290,#111291,#111292,#111293,#111294,#111295,#111296,#111297,
#111298,#111299,#111300,#111301,#111302,#111303,#111304,#111305,#111306,
#111307,#111308,#111309,#111310,#111311,#111312,#111313,#111314,#111315,
#111316,#111317,#111318,#111319,#111320,#111321,#111322,#111323,#111324,
#111325,#111326,#111327,#111328,#111329,#111330,#111331,#111332,#111333,
#111334,#111335,#111336,#111337,#111338,#111339,#111340,#111341,#111342,
#111343,#111344,#111345,#111346,#111347,#111348,#111349,#111350,#111351,
#111352,#111353,#111354,#111355,#111356,#111357,#111358,#111359,#111360,
#111361,#111362,#111363,#111364,#111365,#111366,#111367,#111368,#111369,
#111370,#111371,#111372,#111373,#111374,#111375,#111376,#111377,#111378,
#111379,#111380,#111381,#111382,#111383,#111384,#111385,#111386,#111387,
#111388,#111389,#111390,#111391,#111392,#111393,#111394,#111395,#111396,
#111397,#111398,#111399,#111400,#111401,#111402,#111403,#111404,#111405,
#111406,#111407,#111408,#111409,#111410,#111411,#111412,#111413,#111414,
#111415,#111416,#111417,#111418,#111419,#111420,#111421,#111422,#111423,
#111424,#111425,#111426,#111427,#111428,#111429,#111430,#111431,#111432,
#111433,#111434,#111435,#111436,#111437,#111438,#111439,#111440,#111441,
#111442,#111443,#111444,#111445,#111446,#111447,#111448,#111449,#111450,
#111451,#111452,#111453,#111454,#111455,#111456,#111457,#111458,#111459,
#111460,#111461,#111462,#111463,#111464,#111465,#111466),.UNSPECIFIED.,
 .F.,.F.)
B_SPLINE_CURVE_WITH_KNOTS((6,1,1,1,1,1,1,1,1,1,1,1,1,1,1,1,1,1,1,1,1,1,
1,1,1,1,1,1,1,1,1,1,1,1,1,1,1,1,1,1,1,1,1,1,1,1,1,1,1,1,1,1,1,1,1,1,1,1,
1,1,1,1,1,1,1,1,1,1,1,1,1,1,1,1,1,1,1,1,1,1,1,1,1,1,1,1,1,1,1,1,1,1,1,1,
1,1,1,1,1,1,1,1,1,1,1,1,1,1,1,1,1,1,1,1,1,1,1,1,1,1,1,1,1,1,1,1,1,1,1,1,
1,1,1,1,1,1,1,1,1,1,1,1,1,1,1,1,1,1,1,1,1,1,1,1,1,1,1,1,1,1,1,1,1,1,1,1,
1,1,1,1,1,1,1,1,1,1,1,1,1,1,1,1,1,1,1,1,1,1,1,6),(0.,0.005,0.01,0.015,0.02,
0.025,0.03,0.035,0.04,0.045,0.05,0.055,0.06,0.065,0.07,0.075,0.08,0.085,
0.09,0.095,0.1,0.105,0.11,0.115,0.12,0.125,0.13,0.135,0.14,0.145,0.15,0.155,
0.16,0.165,0.17,0.175,0.18,0.185,0.19,0.195,0.2,0.205,0.21,0.215,0.22,0.225,
0.23,0.235,0.24,0.245,0.25,0.255,0.26,0.265,0.27,0.275,0.28,0.285,0.29,
0.295,0.3,0.305,0.31,0.315,0.32,0.325,0.33,0.335,0.34,0.345,0.35,0.355,
0.36,0.365,0.37,0.375,0.38,0.385,0.39,0.395,0.4,0.405,0.41,0.415,0.42,0.425,
0.43,0.435,0.44,0.445,0.45,0.455,0.46,0.465,0.47,0.475,0.48,0.485,0.49,
0.495,0.5,0.505,0.51,0.515,0.52,0.525,0.53,0.535,0.54,0.545,0.55,0.555,
0.56,0.565,0.57,0.575,0.58,0.585,0.59,0.595,0.6,0.605,0.61,0.615,0.62,0.625,
0.63,0.635,0.64,0.645,0.65,0.655,0.66,0.665,0.67,0.675,0.68,0.685,0.690000000000001,
0.695000000000001,0.700000000000001,0.705000000000001,0.710000000000001,
0.715000000000001,0.720000000000001,0.725000000000001,0.730000000000001,
0.735000000000001,0.740000000000001,0.745000000000001,0.750000000000001,
0.755000000000001,0.760000000000001,0.765000000000001,0.770000000000001,
0.775000000000001,0.780000000000001,0.785000000000001,0.790000000000001,
0.795000000000001,0.800000000000001,0.805000000000001,0.810000000000001,
0.815000000000001,0.820000000000001,0.825000000000001,0.830000000000001,
0.835000000000001,0.840000000000001,0.845000000000001,0.850000000000001,
0.855000000000001,0.860000000000001,0.865000000000001,0.870000000000001,
0.875000000000001,0.880000000000001,0.885000000000001,0.890000000000001,
0.895000000000001,0.900000000000001,0.905000000000001,0.910000000000001,
0.915000000000001,0.920000000000001,0.925000000000001,0.930000000000001,
0.935000000000001,0.940000000000001,0.941429844431415),.UNSPECIFIED.)
CURVE()
GEOMETRIC_REPRESENTATION_ITEM()
RATIONAL_B_SPLINE_CURVE((1.,1.,1.,1.,1.,1.,1.,1.,1.,1.,1.,1.,1.,1.,1.,1.,
1.,1.,1.,1.,1.,1.,1.,1.,1.,1.,1.,1.,1.,1.,1.,1.,1.,1.,1.,1.,1.,1.,1.,1.,
1.,1.,1.,1.,1.,1.,1.,1.,1.,1.,1.,1.,1.,1.,1.,1.,1.,1.,1.,1.,1.,1.,1.,1.,
1.,1.,1.,1.,1.,1.,1.,1.,1.,1.,1.,1.,1.,1.,1.,1.,1.,1.,1.,1.,1.,1.,1.,1.,
1.,1.,1.,1.,1.,1.,1.,1.,1.,1.,1.,1.,1.,1.,1.,1.,1.,1.,1.,1.,1.,1.,1.,1.,
1.,1.,1.,1.,1.,1.,1.,1.,1.,1.,1.,1.,1.,1.,1.,1.,1.,1.,1.,1.,1.,1.,1.,1.,
1.,1.,1.,1.,1.,1.,1.,1.,1.,1.,1.,1.,1.,1.,1.,1.,1.,1.,1.,1.,1.,1.,1.,1.,
1.,1.,1.,1.,1.,1.,1.,1.,1.,1.,1.,1.,1.,1.,1.,1.,1.,1.,1.,1.,1.,1.,1.,1.,
1.,1.,1.,1.,1.,1.,1.,1.,1.,1.))
REPRESENTATION_ITEM('')
);
#534=(
BOUNDED_CURVE()
B_SPLINE_CURVE(5,(#111469,#111470,#111471,#111472,#111473,#111474,#111475,
#111476,#111477,#111478,#111479,#111480,#111481,#111482,#111483,#111484,
#111485,#111486,#111487,#111488,#111489,#111490,#111491,#111492,#111493,
#111494,#111495,#111496,#111497,#111498,#111499,#111500,#111501,#111502,
#111503,#111504,#111505,#111506,#111507,#111508,#111509,#111510,#111511,
#111512,#111513,#111514,#111515,#111516,#111517,#111518,#111519,#111520,
#111521,#111522,#111523,#111524,#111525,#111526,#111527,#111528,#111529,
#111530,#111531,#111532,#111533,#111534,#111535,#111536,#111537,#111538,
#111539,#111540,#111541,#111542,#111543,#111544,#111545,#111546,#111547,
#111548,#111549,#111550,#111551,#111552,#111553,#111554,#111555,#111556,
#111557,#111558,#111559,#111560,#111561,#111562,#111563,#111564,#111565,
#111566,#111567,#111568,#111569,#111570,#111571,#111572,#111573,#111574,
#111575,#111576,#111577,#111578,#111579,#111580,#111581,#111582,#111583,
#111584,#111585,#111586,#111587,#111588,#111589,#111590,#111591,#111592,
#111593,#111594,#111595,#111596,#111597,#111598,#111599,#111600,#111601,
#111602,#111603,#111604,#111605,#111606,#111607,#111608,#111609,#111610,
#111611,#111612,#111613,#111614,#111615,#111616,#111617,#111618,#111619,
#111620,#111621,#111622,#111623,#111624,#111625,#111626,#111627,#111628,
#111629,#111630,#111631,#111632,#111633,#111634,#111635,#111636,#111637,
#111638,#111639,#111640,#111641,#111642,#111643,#111644,#111645,#111646,
#111647,#111648,#111649,#111650,#111651,#111652,#111653,#111654,#111655,
#111656,#111657,#111658,#111659,#111660,#111661,#111662),.UNSPECIFIED.,
 .F.,.F.)
B_SPLINE_CURVE_WITH_KNOTS((6,1,1,1,1,1,1,1,1,1,1,1,1,1,1,1,1,1,1,1,1,1,
1,1,1,1,1,1,1,1,1,1,1,1,1,1,1,1,1,1,1,1,1,1,1,1,1,1,1,1,1,1,1,1,1,1,1,1,
1,1,1,1,1,1,1,1,1,1,1,1,1,1,1,1,1,1,1,1,1,1,1,1,1,1,1,1,1,1,1,1,1,1,1,1,
1,1,1,1,1,1,1,1,1,1,1,1,1,1,1,1,1,1,1,1,1,1,1,1,1,1,1,1,1,1,1,1,1,1,1,1,
1,1,1,1,1,1,1,1,1,1,1,1,1,1,1,1,1,1,1,1,1,1,1,1,1,1,1,1,1,1,1,1,1,1,1,1,
1,1,1,1,1,1,1,1,1,1,1,1,1,1,1,1,1,1,1,1,1,1,1,6),(-0.941429844431415,-0.940000000000001,
-0.935000000000001,-0.930000000000001,-0.925000000000001,-0.920000000000001,
-0.915000000000001,-0.910000000000001,-0.905000000000001,-0.900000000000001,
-0.895000000000001,-0.890000000000001,-0.885000000000001,-0.880000000000001,
-0.875000000000001,-0.870000000000001,-0.865000000000001,-0.860000000000001,
-0.855000000000001,-0.850000000000001,-0.845000000000001,-0.840000000000001,
-0.835000000000001,-0.830000000000001,-0.825000000000001,-0.820000000000001,
-0.815000000000001,-0.810000000000001,-0.805000000000001,-0.800000000000001,
-0.795000000000001,-0.790000000000001,-0.785000000000001,-0.780000000000001,
-0.775000000000001,-0.770000000000001,-0.765000000000001,-0.760000000000001,
-0.755000000000001,-0.750000000000001,-0.745000000000001,-0.740000000000001,
-0.735000000000001,-0.730000000000001,-0.725000000000001,-0.720000000000001,
-0.715000000000001,-0.710000000000001,-0.705000000000001,-0.700000000000001,
-0.695000000000001,-0.690000000000001,-0.685,-0.68,-0.675,-0.67,-0.665,
-0.66,-0.655,-0.65,-0.645,-0.64,-0.635,-0.63,-0.625,-0.62,-0.615,-0.61,
-0.605,-0.6,-0.595,-0.59,-0.585,-0.58,-0.575,-0.57,-0.565,-0.56,-0.555,
-0.55,-0.545,-0.54,-0.535,-0.53,-0.525,-0.52,-0.515,-0.51,-0.505,-0.5,-0.495,
-0.49,-0.485,-0.48,-0.475,-0.47,-0.465,-0.46,-0.455,-0.45,-0.445,-0.44,
-0.435,-0.43,-0.425,-0.42,-0.415,-0.41,-0.405,-0.4,-0.395,-0.39,-0.385,
-0.38,-0.375,-0.37,-0.365,-0.36,-0.355,-0.35,-0.345,-0.34,-0.335,-0.33,
-0.325,-0.32,-0.315,-0.31,-0.305,-0.3,-0.295,-0.29,-0.285,-0.28,-0.275,
-0.27,-0.265,-0.26,-0.255,-0.25,-0.245,-0.24,-0.235,-0.23,-0.225,-0.22,
-0.215,-0.21,-0.205,-0.2,-0.195,-0.19,-0.185,-0.18,-0.175,-0.17,-0.165,
-0.16,-0.155,-0.15,-0.145,-0.14,-0.135,-0.13,-0.125,-0.12,-0.115,-0.11,
-0.105,-0.1,-0.095,-0.09,-0.085,-0.08,-0.075,-0.07,-0.065,-0.06,-0.055,
-0.05,-0.045,-0.04,-0.035,-0.03,-0.025,-0.02,-0.015,-0.01,-0.005,0.),
 .UNSPECIFIED.)
CURVE()
GEOMETRIC_REPRESENTATION_ITEM()
RATIONAL_B_SPLINE_CURVE((1.,1.,1.,1.,1.,1.,1.,1.,1.,1.,1.,1.,1.,1.,1.,1.,
1.,1.,1.,1.,1.,1.,1.,1.,1.,1.,1.,1.,1.,1.,1.,1.,1.,1.,1.,1.,1.,1.,1.,1.,
1.,1.,1.,1.,1.,1.,1.,1.,1.,1.,1.,1.,1.,1.,1.,1.,1.,1.,1.,1.,1.,1.,1.,1.,
1.,1.,1.,1.,1.,1.,1.,1.,1.,1.,1.,1.,1.,1.,1.,1.,1.,1.,1.,1.,1.,1.,1.,1.,
1.,1.,1.,1.,1.,1.,1.,1.,1.,1.,1.,1.,1.,1.,1.,1.,1.,1.,1.,1.,1.,1.,1.,1.,
1.,1.,1.,1.,1.,1.,1.,1.,1.,1.,1.,1.,1.,1.,1.,1.,1.,1.,1.,1.,1.,1.,1.,1.,
1.,1.,1.,1.,1.,1.,1.,1.,1.,1.,1.,1.,1.,1.,1.,1.,1.,1.,1.,1.,1.,1.,1.,1.,
1.,1.,1.,1.,1.,1.,1.,1.,1.,1.,1.,1.,1.,1.,1.,1.,1.,1.,1.,1.,1.,1.,1.,1.,
1.,1.,1.,1.,1.,1.,1.,1.,1.,1.))
REPRESENTATION_ITEM('')
);
#535=(
BOUNDED_CURVE()
B_SPLINE_CURVE(5,(#112169,#112170,#112171,#112172,#112173,#112174,#112175,
#112176,#112177,#112178,#112179,#112180,#112181,#112182,#112183,#112184,
#112185,#112186,#112187,#112188,#112189,#112190,#112191,#112192,#112193,
#112194,#112195,#112196,#112197,#112198,#112199,#112200,#112201,#112202,
#112203,#112204,#112205,#112206,#112207,#112208,#112209,#112210,#112211,
#112212,#112213,#112214,#112215,#112216,#112217,#112218,#112219,#112220,
#112221,#112222,#112223,#112224,#112225,#112226,#112227,#112228,#112229,
#112230,#112231,#112232,#112233,#112234,#112235,#112236,#112237,#112238,
#112239,#112240,#112241,#112242,#112243,#112244,#112245,#112246,#112247,
#112248,#112249,#112250,#112251,#112252,#112253,#112254,#112255,#112256,
#112257,#112258,#112259,#112260,#112261,#112262,#112263,#112264,#112265,
#112266,#112267,#112268,#112269,#112270,#112271,#112272,#112273,#112274,
#112275,#112276,#112277,#112278,#112279,#112280,#112281,#112282,#112283,
#112284,#112285,#112286,#112287,#112288,#112289,#112290,#112291,#112292,
#112293,#112294,#112295,#112296,#112297,#112298,#112299,#112300,#112301,
#112302,#112303,#112304,#112305,#112306,#112307,#112308,#112309,#112310,
#112311,#112312,#112313,#112314,#112315,#112316,#112317,#112318,#112319,
#112320,#112321,#112322,#112323,#112324,#112325,#112326,#112327,#112328,
#112329,#112330,#112331,#112332,#112333,#112334,#112335,#112336,#112337,
#112338,#112339,#112340,#112341,#112342,#112343,#112344,#112345,#112346,
#112347,#112348,#112349,#112350,#112351,#112352,#112353,#112354,#112355,
#112356,#112357,#112358,#112359,#112360,#112361,#112362),.UNSPECIFIED.,
 .F.,.F.)
B_SPLINE_CURVE_WITH_KNOTS((6,1,1,1,1,1,1,1,1,1,1,1,1,1,1,1,1,1,1,1,1,1,
1,1,1,1,1,1,1,1,1,1,1,1,1,1,1,1,1,1,1,1,1,1,1,1,1,1,1,1,1,1,1,1,1,1,1,1,
1,1,1,1,1,1,1,1,1,1,1,1,1,1,1,1,1,1,1,1,1,1,1,1,1,1,1,1,1,1,1,1,1,1,1,1,
1,1,1,1,1,1,1,1,1,1,1,1,1,1,1,1,1,1,1,1,1,1,1,1,1,1,1,1,1,1,1,1,1,1,1,1,
1,1,1,1,1,1,1,1,1,1,1,1,1,1,1,1,1,1,1,1,1,1,1,1,1,1,1,1,1,1,1,1,1,1,1,1,
1,1,1,1,1,1,1,1,1,1,1,1,1,1,1,1,1,1,1,1,1,1,1,6),(0.,0.005,0.01,0.015,0.02,
0.025,0.03,0.035,0.04,0.045,0.05,0.055,0.06,0.065,0.07,0.075,0.08,0.085,
0.09,0.095,0.1,0.105,0.11,0.115,0.12,0.125,0.13,0.135,0.14,0.145,0.15,0.155,
0.16,0.165,0.17,0.175,0.18,0.185,0.19,0.195,0.2,0.205,0.21,0.215,0.22,0.225,
0.23,0.235,0.24,0.245,0.25,0.255,0.26,0.265,0.27,0.275,0.28,0.285,0.29,
0.295,0.3,0.305,0.31,0.315,0.32,0.325,0.33,0.335,0.34,0.345,0.35,0.355,
0.36,0.365,0.37,0.375,0.38,0.385,0.39,0.395,0.4,0.405,0.41,0.415,0.42,0.425,
0.43,0.435,0.44,0.445,0.45,0.455,0.46,0.465,0.47,0.475,0.48,0.485,0.49,
0.495,0.5,0.505,0.51,0.515,0.52,0.525,0.53,0.535,0.54,0.545,0.55,0.555,
0.56,0.565,0.57,0.575,0.58,0.585,0.59,0.595,0.6,0.605,0.61,0.615,0.62,0.625,
0.63,0.635,0.64,0.645,0.65,0.655,0.66,0.665,0.67,0.675,0.68,0.685,0.690000000000001,
0.695000000000001,0.700000000000001,0.705000000000001,0.710000000000001,
0.715000000000001,0.720000000000001,0.725000000000001,0.730000000000001,
0.735000000000001,0.740000000000001,0.745000000000001,0.750000000000001,
0.755000000000001,0.760000000000001,0.765000000000001,0.770000000000001,
0.775000000000001,0.780000000000001,0.785000000000001,0.790000000000001,
0.795000000000001,0.800000000000001,0.805000000000001,0.810000000000001,
0.815000000000001,0.820000000000001,0.825000000000001,0.830000000000001,
0.835000000000001,0.840000000000001,0.845000000000001,0.850000000000001,
0.855000000000001,0.860000000000001,0.865000000000001,0.870000000000001,
0.875000000000001,0.880000000000001,0.885000000000001,0.890000000000001,
0.895000000000001,0.900000000000001,0.905000000000001,0.910000000000001,
0.915000000000001,0.920000000000001,0.925000000000001,0.930000000000001,
0.935000000000001,0.940000000000001,0.941429844431445),.UNSPECIFIED.)
CURVE()
GEOMETRIC_REPRESENTATION_ITEM()
RATIONAL_B_SPLINE_CURVE((1.,1.,1.,1.,1.,1.,1.,1.,1.,1.,1.,1.,1.,1.,1.,1.,
1.,1.,1.,1.,1.,1.,1.,1.,1.,1.,1.,1.,1.,1.,1.,1.,1.,1.,1.,1.,1.,1.,1.,1.,
1.,1.,1.,1.,1.,1.,1.,1.,1.,1.,1.,1.,1.,1.,1.,1.,1.,1.,1.,1.,1.,1.,1.,1.,
1.,1.,1.,1.,1.,1.,1.,1.,1.,1.,1.,1.,1.,1.,1.,1.,1.,1.,1.,1.,1.,1.,1.,1.,
1.,1.,1.,1.,1.,1.,1.,1.,1.,1.,1.,1.,1.,1.,1.,1.,1.,1.,1.,1.,1.,1.,1.,1.,
1.,1.,1.,1.,1.,1.,1.,1.,1.,1.,1.,1.,1.,1.,1.,1.,1.,1.,1.,1.,1.,1.,1.,1.,
1.,1.,1.,1.,1.,1.,1.,1.,1.,1.,1.,1.,1.,1.,1.,1.,1.,1.,1.,1.,1.,1.,1.,1.,
1.,1.,1.,1.,1.,1.,1.,1.,1.,1.,1.,1.,1.,1.,1.,1.,1.,1.,1.,1.,1.,1.,1.,1.,
1.,1.,1.,1.,1.,1.,1.,1.,1.,1.))
REPRESENTATION_ITEM('')
);
#536=(
BOUNDED_CURVE()
B_SPLINE_CURVE(5,(#112365,#112366,#112367,#112368,#112369,#112370,#112371,
#112372,#112373,#112374,#112375,#112376,#112377,#112378,#112379,#112380,
#112381,#112382,#112383,#112384,#112385,#112386,#112387,#112388,#112389,
#112390,#112391,#112392,#112393,#112394,#112395,#112396,#112397,#112398,
#112399,#112400,#112401,#112402,#112403,#112404,#112405,#112406,#112407,
#112408,#112409,#112410,#112411,#112412,#112413,#112414,#112415,#112416,
#112417,#112418,#112419,#112420,#112421,#112422,#112423,#112424,#112425,
#112426,#112427,#112428,#112429,#112430,#112431,#112432,#112433,#112434,
#112435,#112436,#112437,#112438,#112439,#112440,#112441,#112442,#112443,
#112444,#112445,#112446,#112447,#112448,#112449,#112450,#112451,#112452,
#112453,#112454,#112455,#112456,#112457,#112458,#112459,#112460,#112461,
#112462,#112463,#112464,#112465,#112466,#112467,#112468,#112469,#112470,
#112471,#112472,#112473,#112474,#112475,#112476,#112477,#112478,#112479,
#112480,#112481,#112482,#112483,#112484,#112485,#112486,#112487,#112488,
#112489,#112490,#112491,#112492,#112493,#112494,#112495,#112496,#112497,
#112498,#112499,#112500,#112501,#112502,#112503,#112504,#112505,#112506,
#112507,#112508,#112509,#112510,#112511,#112512,#112513,#112514,#112515,
#112516,#112517,#112518,#112519,#112520,#112521,#112522,#112523,#112524,
#112525,#112526,#112527,#112528,#112529,#112530,#112531,#112532,#112533,
#112534,#112535,#112536,#112537,#112538,#112539,#112540,#112541,#112542,
#112543,#112544,#112545,#112546,#112547,#112548,#112549,#112550,#112551,
#112552,#112553,#112554,#112555,#112556,#112557,#112558),.UNSPECIFIED.,
 .F.,.F.)
B_SPLINE_CURVE_WITH_KNOTS((6,1,1,1,1,1,1,1,1,1,1,1,1,1,1,1,1,1,1,1,1,1,
1,1,1,1,1,1,1,1,1,1,1,1,1,1,1,1,1,1,1,1,1,1,1,1,1,1,1,1,1,1,1,1,1,1,1,1,
1,1,1,1,1,1,1,1,1,1,1,1,1,1,1,1,1,1,1,1,1,1,1,1,1,1,1,1,1,1,1,1,1,1,1,1,
1,1,1,1,1,1,1,1,1,1,1,1,1,1,1,1,1,1,1,1,1,1,1,1,1,1,1,1,1,1,1,1,1,1,1,1,
1,1,1,1,1,1,1,1,1,1,1,1,1,1,1,1,1,1,1,1,1,1,1,1,1,1,1,1,1,1,1,1,1,1,1,1,
1,1,1,1,1,1,1,1,1,1,1,1,1,1,1,1,1,1,1,1,1,1,1,6),(-0.941429844431472,-0.940000000000001,
-0.935000000000001,-0.930000000000001,-0.925000000000001,-0.920000000000001,
-0.915000000000001,-0.910000000000001,-0.905000000000001,-0.900000000000001,
-0.895000000000001,-0.890000000000001,-0.885000000000001,-0.880000000000001,
-0.875000000000001,-0.870000000000001,-0.865000000000001,-0.860000000000001,
-0.855000000000001,-0.850000000000001,-0.845000000000001,-0.840000000000001,
-0.835000000000001,-0.830000000000001,-0.825000000000001,-0.820000000000001,
-0.815000000000001,-0.810000000000001,-0.805000000000001,-0.800000000000001,
-0.795000000000001,-0.790000000000001,-0.785000000000001,-0.780000000000001,
-0.775000000000001,-0.770000000000001,-0.765000000000001,-0.760000000000001,
-0.755000000000001,-0.750000000000001,-0.745000000000001,-0.740000000000001,
-0.735000000000001,-0.730000000000001,-0.725000000000001,-0.720000000000001,
-0.715000000000001,-0.710000000000001,-0.705000000000001,-0.700000000000001,
-0.695000000000001,-0.690000000000001,-0.685,-0.68,-0.675,-0.67,-0.665,
-0.66,-0.655,-0.65,-0.645,-0.64,-0.635,-0.63,-0.625,-0.62,-0.615,-0.61,
-0.605,-0.6,-0.595,-0.59,-0.585,-0.58,-0.575,-0.57,-0.565,-0.56,-0.555,
-0.55,-0.545,-0.54,-0.535,-0.53,-0.525,-0.52,-0.515,-0.51,-0.505,-0.5,-0.495,
-0.49,-0.485,-0.48,-0.475,-0.47,-0.465,-0.46,-0.455,-0.45,-0.445,-0.44,
-0.435,-0.43,-0.425,-0.42,-0.415,-0.41,-0.405,-0.4,-0.395,-0.39,-0.385,
-0.38,-0.375,-0.37,-0.365,-0.36,-0.355,-0.35,-0.345,-0.34,-0.335,-0.33,
-0.325,-0.32,-0.315,-0.31,-0.305,-0.3,-0.295,-0.29,-0.285,-0.28,-0.275,
-0.27,-0.265,-0.26,-0.255,-0.25,-0.245,-0.24,-0.235,-0.23,-0.225,-0.22,
-0.215,-0.21,-0.205,-0.2,-0.195,-0.19,-0.185,-0.18,-0.175,-0.17,-0.165,
-0.16,-0.155,-0.15,-0.145,-0.14,-0.135,-0.13,-0.125,-0.12,-0.115,-0.11,
-0.105,-0.1,-0.095,-0.09,-0.085,-0.08,-0.075,-0.07,-0.065,-0.06,-0.055,
-0.05,-0.045,-0.04,-0.035,-0.03,-0.025,-0.02,-0.015,-0.01,-0.005,0.),
 .UNSPECIFIED.)
CURVE()
GEOMETRIC_REPRESENTATION_ITEM()
RATIONAL_B_SPLINE_CURVE((1.,1.,1.,1.,1.,1.,1.,1.,1.,1.,1.,1.,1.,1.,1.,1.,
1.,1.,1.,1.,1.,1.,1.,1.,1.,1.,1.,1.,1.,1.,1.,1.,1.,1.,1.,1.,1.,1.,1.,1.,
1.,1.,1.,1.,1.,1.,1.,1.,1.,1.,1.,1.,1.,1.,1.,1.,1.,1.,1.,1.,1.,1.,1.,1.,
1.,1.,1.,1.,1.,1.,1.,1.,1.,1.,1.,1.,1.,1.,1.,1.,1.,1.,1.,1.,1.,1.,1.,1.,
1.,1.,1.,1.,1.,1.,1.,1.,1.,1.,1.,1.,1.,1.,1.,1.,1.,1.,1.,1.,1.,1.,1.,1.,
1.,1.,1.,1.,1.,1.,1.,1.,1.,1.,1.,1.,1.,1.,1.,1.,1.,1.,1.,1.,1.,1.,1.,1.,
1.,1.,1.,1.,1.,1.,1.,1.,1.,1.,1.,1.,1.,1.,1.,1.,1.,1.,1.,1.,1.,1.,1.,1.,
1.,1.,1.,1.,1.,1.,1.,1.,1.,1.,1.,1.,1.,1.,1.,1.,1.,1.,1.,1.,1.,1.,1.,1.,
1.,1.,1.,1.,1.,1.,1.,1.,1.,1.))
REPRESENTATION_ITEM('')
);
#537=(
BOUNDED_CURVE()
B_SPLINE_CURVE(5,(#113065,#113066,#113067,#113068,#113069,#113070,#113071,
#113072,#113073,#113074,#113075,#113076,#113077,#113078,#113079,#113080,
#113081,#113082,#113083,#113084,#113085,#113086,#113087,#113088,#113089,
#113090,#113091,#113092,#113093,#113094,#113095,#113096,#113097,#113098,
#113099,#113100,#113101,#113102,#113103,#113104,#113105,#113106,#113107,
#113108,#113109,#113110,#113111,#113112,#113113,#113114,#113115,#113116,
#113117,#113118,#113119,#113120,#113121,#113122,#113123,#113124,#113125,
#113126,#113127,#113128,#113129,#113130,#113131,#113132,#113133,#113134,
#113135,#113136,#113137,#113138,#113139,#113140,#113141,#113142,#113143,
#113144,#113145,#113146,#113147,#113148,#113149,#113150,#113151,#113152,
#113153,#113154,#113155,#113156,#113157,#113158,#113159,#113160,#113161,
#113162,#113163,#113164,#113165,#113166,#113167,#113168,#113169,#113170,
#113171,#113172,#113173,#113174,#113175,#113176,#113177,#113178,#113179,
#113180,#113181,#113182,#113183,#113184,#113185,#113186,#113187,#113188,
#113189,#113190,#113191,#113192,#113193,#113194,#113195,#113196,#113197,
#113198,#113199,#113200,#113201,#113202,#113203,#113204,#113205,#113206,
#113207,#113208,#113209,#113210,#113211,#113212,#113213,#113214,#113215,
#113216,#113217,#113218,#113219,#113220,#113221,#113222,#113223,#113224,
#113225,#113226,#113227,#113228,#113229,#113230,#113231,#113232,#113233,
#113234,#113235,#113236,#113237,#113238,#113239,#113240,#113241,#113242,
#113243,#113244,#113245,#113246,#113247,#113248,#113249,#113250,#113251,
#113252,#113253,#113254,#113255,#113256,#113257,#113258),.UNSPECIFIED.,
 .F.,.F.)
B_SPLINE_CURVE_WITH_KNOTS((6,1,1,1,1,1,1,1,1,1,1,1,1,1,1,1,1,1,1,1,1,1,
1,1,1,1,1,1,1,1,1,1,1,1,1,1,1,1,1,1,1,1,1,1,1,1,1,1,1,1,1,1,1,1,1,1,1,1,
1,1,1,1,1,1,1,1,1,1,1,1,1,1,1,1,1,1,1,1,1,1,1,1,1,1,1,1,1,1,1,1,1,1,1,1,
1,1,1,1,1,1,1,1,1,1,1,1,1,1,1,1,1,1,1,1,1,1,1,1,1,1,1,1,1,1,1,1,1,1,1,1,
1,1,1,1,1,1,1,1,1,1,1,1,1,1,1,1,1,1,1,1,1,1,1,1,1,1,1,1,1,1,1,1,1,1,1,1,
1,1,1,1,1,1,1,1,1,1,1,1,1,1,1,1,1,1,1,1,1,1,1,6),(0.,0.005,0.01,0.015,0.02,
0.025,0.03,0.035,0.04,0.045,0.05,0.055,0.06,0.065,0.07,0.075,0.08,0.085,
0.09,0.095,0.1,0.105,0.11,0.115,0.12,0.125,0.13,0.135,0.14,0.145,0.15,0.155,
0.16,0.165,0.17,0.175,0.18,0.185,0.19,0.195,0.2,0.205,0.21,0.215,0.22,0.225,
0.23,0.235,0.24,0.245,0.25,0.255,0.26,0.265,0.27,0.275,0.28,0.285,0.29,
0.295,0.3,0.305,0.31,0.315,0.32,0.325,0.33,0.335,0.34,0.345,0.35,0.355,
0.36,0.365,0.37,0.375,0.38,0.385,0.39,0.395,0.4,0.405,0.41,0.415,0.42,0.425,
0.43,0.435,0.44,0.445,0.45,0.455,0.46,0.465,0.47,0.475,0.48,0.485,0.49,
0.495,0.5,0.505,0.51,0.515,0.52,0.525,0.53,0.535,0.54,0.545,0.55,0.555,
0.56,0.565,0.57,0.575,0.58,0.585,0.59,0.595,0.6,0.605,0.61,0.615,0.62,0.625,
0.63,0.635,0.64,0.645,0.65,0.655,0.66,0.665,0.67,0.675,0.68,0.685,0.690000000000001,
0.695000000000001,0.700000000000001,0.705000000000001,0.710000000000001,
0.715000000000001,0.720000000000001,0.725000000000001,0.730000000000001,
0.735000000000001,0.740000000000001,0.745000000000001,0.750000000000001,
0.755000000000001,0.760000000000001,0.765000000000001,0.770000000000001,
0.775000000000001,0.780000000000001,0.785000000000001,0.790000000000001,
0.795000000000001,0.800000000000001,0.805000000000001,0.810000000000001,
0.815000000000001,0.820000000000001,0.825000000000001,0.830000000000001,
0.835000000000001,0.840000000000001,0.845000000000001,0.850000000000001,
0.855000000000001,0.860000000000001,0.865000000000001,0.870000000000001,
0.875000000000001,0.880000000000001,0.885000000000001,0.890000000000001,
0.895000000000001,0.900000000000001,0.905000000000001,0.910000000000001,
0.915000000000001,0.920000000000001,0.925000000000001,0.930000000000001,
0.935000000000001,0.940000000000001,0.941429844431522),.UNSPECIFIED.)
CURVE()
GEOMETRIC_REPRESENTATION_ITEM()
RATIONAL_B_SPLINE_CURVE((1.,1.,1.,1.,1.,1.,1.,1.,1.,1.,1.,1.,1.,1.,1.,1.,
1.,1.,1.,1.,1.,1.,1.,1.,1.,1.,1.,1.,1.,1.,1.,1.,1.,1.,1.,1.,1.,1.,1.,1.,
1.,1.,1.,1.,1.,1.,1.,1.,1.,1.,1.,1.,1.,1.,1.,1.,1.,1.,1.,1.,1.,1.,1.,1.,
1.,1.,1.,1.,1.,1.,1.,1.,1.,1.,1.,1.,1.,1.,1.,1.,1.,1.,1.,1.,1.,1.,1.,1.,
1.,1.,1.,1.,1.,1.,1.,1.,1.,1.,1.,1.,1.,1.,1.,1.,1.,1.,1.,1.,1.,1.,1.,1.,
1.,1.,1.,1.,1.,1.,1.,1.,1.,1.,1.,1.,1.,1.,1.,1.,1.,1.,1.,1.,1.,1.,1.,1.,
1.,1.,1.,1.,1.,1.,1.,1.,1.,1.,1.,1.,1.,1.,1.,1.,1.,1.,1.,1.,1.,1.,1.,1.,
1.,1.,1.,1.,1.,1.,1.,1.,1.,1.,1.,1.,1.,1.,1.,1.,1.,1.,1.,1.,1.,1.,1.,1.,
1.,1.,1.,1.,1.,1.,1.,1.,1.,1.))
REPRESENTATION_ITEM('')
);
#538=(
BOUNDED_CURVE()
B_SPLINE_CURVE(5,(#113261,#113262,#113263,#113264,#113265,#113266,#113267,
#113268,#113269,#113270,#113271,#113272,#113273,#113274,#113275,#113276,
#113277,#113278,#113279,#113280,#113281,#113282,#113283,#113284,#113285,
#113286,#113287,#113288,#113289,#113290,#113291,#113292,#113293,#113294,
#113295,#113296,#113297,#113298,#113299,#113300,#113301,#113302,#113303,
#113304,#113305,#113306,#113307,#113308,#113309,#113310,#113311,#113312,
#113313,#113314,#113315,#113316,#113317,#113318,#113319,#113320,#113321,
#113322,#113323,#113324,#113325,#113326,#113327,#113328,#113329,#113330,
#113331,#113332,#113333,#113334,#113335,#113336,#113337,#113338,#113339,
#113340,#113341,#113342,#113343,#113344,#113345,#113346,#113347,#113348,
#113349,#113350,#113351,#113352,#113353,#113354,#113355,#113356,#113357,
#113358,#113359,#113360,#113361,#113362,#113363,#113364,#113365,#113366,
#113367,#113368,#113369,#113370,#113371,#113372,#113373,#113374,#113375,
#113376,#113377,#113378,#113379,#113380,#113381,#113382,#113383,#113384,
#113385,#113386,#113387,#113388,#113389,#113390,#113391,#113392,#113393,
#113394,#113395,#113396,#113397,#113398,#113399,#113400,#113401,#113402,
#113403,#113404,#113405,#113406,#113407,#113408,#113409,#113410,#113411,
#113412,#113413,#113414,#113415,#113416,#113417,#113418,#113419,#113420,
#113421,#113422,#113423,#113424,#113425,#113426,#113427,#113428,#113429,
#113430,#113431,#113432,#113433,#113434,#113435,#113436,#113437,#113438,
#113439,#113440,#113441,#113442,#113443,#113444,#113445,#113446,#113447,
#113448,#113449,#113450,#113451,#113452,#113453,#113454),.UNSPECIFIED.,
 .F.,.F.)
B_SPLINE_CURVE_WITH_KNOTS((6,1,1,1,1,1,1,1,1,1,1,1,1,1,1,1,1,1,1,1,1,1,
1,1,1,1,1,1,1,1,1,1,1,1,1,1,1,1,1,1,1,1,1,1,1,1,1,1,1,1,1,1,1,1,1,1,1,1,
1,1,1,1,1,1,1,1,1,1,1,1,1,1,1,1,1,1,1,1,1,1,1,1,1,1,1,1,1,1,1,1,1,1,1,1,
1,1,1,1,1,1,1,1,1,1,1,1,1,1,1,1,1,1,1,1,1,1,1,1,1,1,1,1,1,1,1,1,1,1,1,1,
1,1,1,1,1,1,1,1,1,1,1,1,1,1,1,1,1,1,1,1,1,1,1,1,1,1,1,1,1,1,1,1,1,1,1,1,
1,1,1,1,1,1,1,1,1,1,1,1,1,1,1,1,1,1,1,1,1,1,1,6),(-0.941429844431529,-0.940000000000001,
-0.935000000000001,-0.930000000000001,-0.925000000000001,-0.920000000000001,
-0.915000000000001,-0.910000000000001,-0.905000000000001,-0.900000000000001,
-0.895000000000001,-0.890000000000001,-0.885000000000001,-0.880000000000001,
-0.875000000000001,-0.870000000000001,-0.865000000000001,-0.860000000000001,
-0.855000000000001,-0.850000000000001,-0.845000000000001,-0.840000000000001,
-0.835000000000001,-0.830000000000001,-0.825000000000001,-0.820000000000001,
-0.815000000000001,-0.810000000000001,-0.805000000000001,-0.800000000000001,
-0.795000000000001,-0.790000000000001,-0.785000000000001,-0.780000000000001,
-0.775000000000001,-0.770000000000001,-0.765000000000001,-0.760000000000001,
-0.755000000000001,-0.750000000000001,-0.745000000000001,-0.740000000000001,
-0.735000000000001,-0.730000000000001,-0.725000000000001,-0.720000000000001,
-0.715000000000001,-0.710000000000001,-0.705000000000001,-0.700000000000001,
-0.695000000000001,-0.690000000000001,-0.685,-0.68,-0.675,-0.67,-0.665,
-0.66,-0.655,-0.65,-0.645,-0.64,-0.635,-0.63,-0.625,-0.62,-0.615,-0.61,
-0.605,-0.6,-0.595,-0.59,-0.585,-0.58,-0.575,-0.57,-0.565,-0.56,-0.555,
-0.55,-0.545,-0.54,-0.535,-0.53,-0.525,-0.52,-0.515,-0.51,-0.505,-0.5,-0.495,
-0.49,-0.485,-0.48,-0.475,-0.47,-0.465,-0.46,-0.455,-0.45,-0.445,-0.44,
-0.435,-0.43,-0.425,-0.42,-0.415,-0.41,-0.405,-0.4,-0.395,-0.39,-0.385,
-0.38,-0.375,-0.37,-0.365,-0.36,-0.355,-0.35,-0.345,-0.34,-0.335,-0.33,
-0.325,-0.32,-0.315,-0.31,-0.305,-0.3,-0.295,-0.29,-0.285,-0.28,-0.275,
-0.27,-0.265,-0.26,-0.255,-0.25,-0.245,-0.24,-0.235,-0.23,-0.225,-0.22,
-0.215,-0.21,-0.205,-0.2,-0.195,-0.19,-0.185,-0.18,-0.175,-0.17,-0.165,
-0.16,-0.155,-0.15,-0.145,-0.14,-0.135,-0.13,-0.125,-0.12,-0.115,-0.11,
-0.105,-0.1,-0.095,-0.09,-0.085,-0.08,-0.075,-0.07,-0.065,-0.06,-0.055,
-0.05,-0.045,-0.04,-0.035,-0.03,-0.025,-0.02,-0.015,-0.01,-0.005,0.),
 .UNSPECIFIED.)
CURVE()
GEOMETRIC_REPRESENTATION_ITEM()
RATIONAL_B_SPLINE_CURVE((1.,1.,1.,1.,1.,1.,1.,1.,1.,1.,1.,1.,1.,1.,1.,1.,
1.,1.,1.,1.,1.,1.,1.,1.,1.,1.,1.,1.,1.,1.,1.,1.,1.,1.,1.,1.,1.,1.,1.,1.,
1.,1.,1.,1.,1.,1.,1.,1.,1.,1.,1.,1.,1.,1.,1.,1.,1.,1.,1.,1.,1.,1.,1.,1.,
1.,1.,1.,1.,1.,1.,1.,1.,1.,1.,1.,1.,1.,1.,1.,1.,1.,1.,1.,1.,1.,1.,1.,1.,
1.,1.,1.,1.,1.,1.,1.,1.,1.,1.,1.,1.,1.,1.,1.,1.,1.,1.,1.,1.,1.,1.,1.,1.,
1.,1.,1.,1.,1.,1.,1.,1.,1.,1.,1.,1.,1.,1.,1.,1.,1.,1.,1.,1.,1.,1.,1.,1.,
1.,1.,1.,1.,1.,1.,1.,1.,1.,1.,1.,1.,1.,1.,1.,1.,1.,1.,1.,1.,1.,1.,1.,1.,
1.,1.,1.,1.,1.,1.,1.,1.,1.,1.,1.,1.,1.,1.,1.,1.,1.,1.,1.,1.,1.,1.,1.,1.,
1.,1.,1.,1.,1.,1.,1.,1.,1.,1.))
REPRESENTATION_ITEM('')
);
#539=(
BOUNDED_CURVE()
B_SPLINE_CURVE(5,(#113961,#113962,#113963,#113964,#113965,#113966,#113967,
#113968,#113969,#113970,#113971,#113972,#113973,#113974,#113975,#113976,
#113977,#113978,#113979,#113980,#113981,#113982,#113983,#113984,#113985,
#113986,#113987,#113988,#113989,#113990,#113991,#113992,#113993,#113994,
#113995,#113996,#113997,#113998,#113999,#114000,#114001,#114002,#114003,
#114004,#114005,#114006,#114007,#114008,#114009,#114010,#114011,#114012,
#114013,#114014,#114015,#114016,#114017,#114018,#114019,#114020,#114021,
#114022,#114023,#114024,#114025,#114026,#114027,#114028,#114029,#114030,
#114031,#114032,#114033,#114034,#114035,#114036,#114037,#114038,#114039,
#114040,#114041,#114042,#114043,#114044,#114045,#114046,#114047,#114048,
#114049,#114050,#114051,#114052,#114053,#114054,#114055,#114056,#114057,
#114058,#114059,#114060,#114061,#114062,#114063,#114064,#114065,#114066,
#114067,#114068,#114069,#114070,#114071,#114072,#114073,#114074,#114075,
#114076,#114077,#114078,#114079,#114080,#114081,#114082,#114083,#114084,
#114085,#114086,#114087,#114088,#114089,#114090,#114091,#114092,#114093,
#114094,#114095,#114096,#114097,#114098,#114099,#114100,#114101,#114102,
#114103,#114104,#114105,#114106,#114107,#114108,#114109,#114110,#114111,
#114112,#114113,#114114,#114115,#114116,#114117,#114118,#114119,#114120,
#114121,#114122,#114123,#114124,#114125,#114126,#114127,#114128,#114129,
#114130,#114131,#114132,#114133,#114134,#114135,#114136,#114137,#114138,
#114139,#114140,#114141,#114142,#114143,#114144,#114145,#114146,#114147,
#114148,#114149,#114150,#114151,#114152,#114153,#114154),.UNSPECIFIED.,
 .F.,.F.)
B_SPLINE_CURVE_WITH_KNOTS((6,1,1,1,1,1,1,1,1,1,1,1,1,1,1,1,1,1,1,1,1,1,
1,1,1,1,1,1,1,1,1,1,1,1,1,1,1,1,1,1,1,1,1,1,1,1,1,1,1,1,1,1,1,1,1,1,1,1,
1,1,1,1,1,1,1,1,1,1,1,1,1,1,1,1,1,1,1,1,1,1,1,1,1,1,1,1,1,1,1,1,1,1,1,1,
1,1,1,1,1,1,1,1,1,1,1,1,1,1,1,1,1,1,1,1,1,1,1,1,1,1,1,1,1,1,1,1,1,1,1,1,
1,1,1,1,1,1,1,1,1,1,1,1,1,1,1,1,1,1,1,1,1,1,1,1,1,1,1,1,1,1,1,1,1,1,1,1,
1,1,1,1,1,1,1,1,1,1,1,1,1,1,1,1,1,1,1,1,1,1,1,6),(0.,0.005,0.01,0.015,0.02,
0.025,0.03,0.035,0.04,0.045,0.05,0.055,0.06,0.065,0.07,0.075,0.08,0.085,
0.09,0.095,0.1,0.105,0.11,0.115,0.12,0.125,0.13,0.135,0.14,0.145,0.15,0.155,
0.16,0.165,0.17,0.175,0.18,0.185,0.19,0.195,0.2,0.205,0.21,0.215,0.22,0.225,
0.23,0.235,0.24,0.245,0.25,0.255,0.26,0.265,0.27,0.275,0.28,0.285,0.29,
0.295,0.3,0.305,0.31,0.315,0.32,0.325,0.33,0.335,0.34,0.345,0.35,0.355,
0.36,0.365,0.37,0.375,0.38,0.385,0.39,0.395,0.4,0.405,0.41,0.415,0.42,0.425,
0.43,0.435,0.44,0.445,0.45,0.455,0.46,0.465,0.47,0.475,0.48,0.485,0.49,
0.495,0.5,0.505,0.51,0.515,0.52,0.525,0.53,0.535,0.54,0.545,0.55,0.555,
0.56,0.565,0.57,0.575,0.58,0.585,0.59,0.595,0.6,0.605,0.61,0.615,0.62,0.625,
0.63,0.635,0.64,0.645,0.65,0.655,0.66,0.665,0.67,0.675,0.68,0.685,0.690000000000001,
0.695000000000001,0.700000000000001,0.705000000000001,0.710000000000001,
0.715000000000001,0.720000000000001,0.725000000000001,0.730000000000001,
0.735000000000001,0.740000000000001,0.745000000000001,0.750000000000001,
0.755000000000001,0.760000000000001,0.765000000000001,0.770000000000001,
0.775000000000001,0.780000000000001,0.785000000000001,0.790000000000001,
0.795000000000001,0.800000000000001,0.805000000000001,0.810000000000001,
0.815000000000001,0.820000000000001,0.825000000000001,0.830000000000001,
0.835000000000001,0.840000000000001,0.845000000000001,0.850000000000001,
0.855000000000001,0.860000000000001,0.865000000000001,0.870000000000001,
0.875000000000001,0.880000000000001,0.885000000000001,0.890000000000001,
0.895000000000001,0.900000000000001,0.905000000000001,0.910000000000001,
0.915000000000001,0.920000000000001,0.925000000000001,0.930000000000001,
0.935000000000001,0.940000000000001,0.941429844431397),.UNSPECIFIED.)
CURVE()
GEOMETRIC_REPRESENTATION_ITEM()
RATIONAL_B_SPLINE_CURVE((1.,1.,1.,1.,1.,1.,1.,1.,1.,1.,1.,1.,1.,1.,1.,1.,
1.,1.,1.,1.,1.,1.,1.,1.,1.,1.,1.,1.,1.,1.,1.,1.,1.,1.,1.,1.,1.,1.,1.,1.,
1.,1.,1.,1.,1.,1.,1.,1.,1.,1.,1.,1.,1.,1.,1.,1.,1.,1.,1.,1.,1.,1.,1.,1.,
1.,1.,1.,1.,1.,1.,1.,1.,1.,1.,1.,1.,1.,1.,1.,1.,1.,1.,1.,1.,1.,1.,1.,1.,
1.,1.,1.,1.,1.,1.,1.,1.,1.,1.,1.,1.,1.,1.,1.,1.,1.,1.,1.,1.,1.,1.,1.,1.,
1.,1.,1.,1.,1.,1.,1.,1.,1.,1.,1.,1.,1.,1.,1.,1.,1.,1.,1.,1.,1.,1.,1.,1.,
1.,1.,1.,1.,1.,1.,1.,1.,1.,1.,1.,1.,1.,1.,1.,1.,1.,1.,1.,1.,1.,1.,1.,1.,
1.,1.,1.,1.,1.,1.,1.,1.,1.,1.,1.,1.,1.,1.,1.,1.,1.,1.,1.,1.,1.,1.,1.,1.,
1.,1.,1.,1.,1.,1.,1.,1.,1.,1.))
REPRESENTATION_ITEM('')
);
#540=(
BOUNDED_CURVE()
B_SPLINE_CURVE(5,(#114157,#114158,#114159,#114160,#114161,#114162,#114163,
#114164,#114165,#114166,#114167,#114168,#114169,#114170,#114171,#114172,
#114173,#114174,#114175,#114176,#114177,#114178,#114179,#114180,#114181,
#114182,#114183,#114184,#114185,#114186,#114187,#114188,#114189,#114190,
#114191,#114192,#114193,#114194,#114195,#114196,#114197,#114198,#114199,
#114200,#114201,#114202,#114203,#114204,#114205,#114206,#114207,#114208,
#114209,#114210,#114211,#114212,#114213,#114214,#114215,#114216,#114217,
#114218,#114219,#114220,#114221,#114222,#114223,#114224,#114225,#114226,
#114227,#114228,#114229,#114230,#114231,#114232,#114233,#114234,#114235,
#114236,#114237,#114238,#114239,#114240,#114241,#114242,#114243,#114244,
#114245,#114246,#114247,#114248,#114249,#114250,#114251,#114252,#114253,
#114254,#114255,#114256,#114257,#114258,#114259,#114260,#114261,#114262,
#114263,#114264,#114265,#114266,#114267,#114268,#114269,#114270,#114271,
#114272,#114273,#114274,#114275,#114276,#114277,#114278,#114279,#114280,
#114281,#114282,#114283,#114284,#114285,#114286,#114287,#114288,#114289,
#114290,#114291,#114292,#114293,#114294,#114295,#114296,#114297,#114298,
#114299,#114300,#114301,#114302,#114303,#114304,#114305,#114306,#114307,
#114308,#114309,#114310,#114311,#114312,#114313,#114314,#114315,#114316,
#114317,#114318,#114319,#114320,#114321,#114322,#114323,#114324,#114325,
#114326,#114327,#114328,#114329,#114330,#114331,#114332,#114333,#114334,
#114335,#114336,#114337,#114338,#114339,#114340,#114341,#114342,#114343,
#114344,#114345,#114346,#114347,#114348,#114349,#114350),.UNSPECIFIED.,
 .F.,.F.)
B_SPLINE_CURVE_WITH_KNOTS((6,1,1,1,1,1,1,1,1,1,1,1,1,1,1,1,1,1,1,1,1,1,
1,1,1,1,1,1,1,1,1,1,1,1,1,1,1,1,1,1,1,1,1,1,1,1,1,1,1,1,1,1,1,1,1,1,1,1,
1,1,1,1,1,1,1,1,1,1,1,1,1,1,1,1,1,1,1,1,1,1,1,1,1,1,1,1,1,1,1,1,1,1,1,1,
1,1,1,1,1,1,1,1,1,1,1,1,1,1,1,1,1,1,1,1,1,1,1,1,1,1,1,1,1,1,1,1,1,1,1,1,
1,1,1,1,1,1,1,1,1,1,1,1,1,1,1,1,1,1,1,1,1,1,1,1,1,1,1,1,1,1,1,1,1,1,1,1,
1,1,1,1,1,1,1,1,1,1,1,1,1,1,1,1,1,1,1,1,1,1,1,6),(-0.941429844431401,-0.940000000000001,
-0.935000000000001,-0.930000000000001,-0.925000000000001,-0.920000000000001,
-0.915000000000001,-0.910000000000001,-0.905000000000001,-0.900000000000001,
-0.895000000000001,-0.890000000000001,-0.885000000000001,-0.880000000000001,
-0.875000000000001,-0.870000000000001,-0.865000000000001,-0.860000000000001,
-0.855000000000001,-0.850000000000001,-0.845000000000001,-0.840000000000001,
-0.835000000000001,-0.830000000000001,-0.825000000000001,-0.820000000000001,
-0.815000000000001,-0.810000000000001,-0.805000000000001,-0.800000000000001,
-0.795000000000001,-0.790000000000001,-0.785000000000001,-0.780000000000001,
-0.775000000000001,-0.770000000000001,-0.765000000000001,-0.760000000000001,
-0.755000000000001,-0.750000000000001,-0.745000000000001,-0.740000000000001,
-0.735000000000001,-0.730000000000001,-0.725000000000001,-0.720000000000001,
-0.715000000000001,-0.710000000000001,-0.705000000000001,-0.700000000000001,
-0.695000000000001,-0.690000000000001,-0.685,-0.68,-0.675,-0.67,-0.665,
-0.66,-0.655,-0.65,-0.645,-0.64,-0.635,-0.63,-0.625,-0.62,-0.615,-0.61,
-0.605,-0.6,-0.595,-0.59,-0.585,-0.58,-0.575,-0.57,-0.565,-0.56,-0.555,
-0.55,-0.545,-0.54,-0.535,-0.53,-0.525,-0.52,-0.515,-0.51,-0.505,-0.5,-0.495,
-0.49,-0.485,-0.48,-0.475,-0.47,-0.465,-0.46,-0.455,-0.45,-0.445,-0.44,
-0.435,-0.43,-0.425,-0.42,-0.415,-0.41,-0.405,-0.4,-0.395,-0.39,-0.385,
-0.38,-0.375,-0.37,-0.365,-0.36,-0.355,-0.35,-0.345,-0.34,-0.335,-0.33,
-0.325,-0.32,-0.315,-0.31,-0.305,-0.3,-0.295,-0.29,-0.285,-0.28,-0.275,
-0.27,-0.265,-0.26,-0.255,-0.25,-0.245,-0.24,-0.235,-0.23,-0.225,-0.22,
-0.215,-0.21,-0.205,-0.2,-0.195,-0.19,-0.185,-0.18,-0.175,-0.17,-0.165,
-0.16,-0.155,-0.15,-0.145,-0.14,-0.135,-0.13,-0.125,-0.12,-0.115,-0.11,
-0.105,-0.1,-0.095,-0.09,-0.085,-0.08,-0.075,-0.07,-0.065,-0.06,-0.055,
-0.05,-0.045,-0.04,-0.035,-0.03,-0.025,-0.02,-0.015,-0.01,-0.005,0.),
 .UNSPECIFIED.)
CURVE()
GEOMETRIC_REPRESENTATION_ITEM()
RATIONAL_B_SPLINE_CURVE((1.,1.,1.,1.,1.,1.,1.,1.,1.,1.,1.,1.,1.,1.,1.,1.,
1.,1.,1.,1.,1.,1.,1.,1.,1.,1.,1.,1.,1.,1.,1.,1.,1.,1.,1.,1.,1.,1.,1.,1.,
1.,1.,1.,1.,1.,1.,1.,1.,1.,1.,1.,1.,1.,1.,1.,1.,1.,1.,1.,1.,1.,1.,1.,1.,
1.,1.,1.,1.,1.,1.,1.,1.,1.,1.,1.,1.,1.,1.,1.,1.,1.,1.,1.,1.,1.,1.,1.,1.,
1.,1.,1.,1.,1.,1.,1.,1.,1.,1.,1.,1.,1.,1.,1.,1.,1.,1.,1.,1.,1.,1.,1.,1.,
1.,1.,1.,1.,1.,1.,1.,1.,1.,1.,1.,1.,1.,1.,1.,1.,1.,1.,1.,1.,1.,1.,1.,1.,
1.,1.,1.,1.,1.,1.,1.,1.,1.,1.,1.,1.,1.,1.,1.,1.,1.,1.,1.,1.,1.,1.,1.,1.,
1.,1.,1.,1.,1.,1.,1.,1.,1.,1.,1.,1.,1.,1.,1.,1.,1.,1.,1.,1.,1.,1.,1.,1.,
1.,1.,1.,1.,1.,1.,1.,1.,1.,1.))
REPRESENTATION_ITEM('')
);
#541=(
BOUNDED_CURVE()
B_SPLINE_CURVE(5,(#114857,#114858,#114859,#114860,#114861,#114862,#114863,
#114864,#114865,#114866,#114867,#114868,#114869,#114870,#114871,#114872,
#114873,#114874,#114875,#114876,#114877,#114878,#114879,#114880,#114881,
#114882,#114883,#114884,#114885,#114886,#114887,#114888,#114889,#114890,
#114891,#114892,#114893,#114894,#114895,#114896,#114897,#114898,#114899,
#114900,#114901,#114902,#114903,#114904,#114905,#114906,#114907,#114908,
#114909,#114910,#114911,#114912,#114913,#114914,#114915,#114916,#114917,
#114918,#114919,#114920,#114921,#114922,#114923,#114924,#114925,#114926,
#114927,#114928,#114929,#114930,#114931,#114932,#114933,#114934,#114935,
#114936,#114937,#114938,#114939,#114940,#114941,#114942,#114943,#114944,
#114945,#114946,#114947,#114948,#114949,#114950,#114951,#114952,#114953,
#114954,#114955,#114956,#114957,#114958,#114959,#114960,#114961,#114962,
#114963,#114964,#114965,#114966,#114967,#114968,#114969,#114970,#114971,
#114972,#114973,#114974,#114975,#114976,#114977,#114978,#114979,#114980,
#114981,#114982,#114983,#114984,#114985,#114986,#114987,#114988,#114989,
#114990,#114991,#114992,#114993,#114994,#114995,#114996,#114997,#114998,
#114999,#115000,#115001,#115002,#115003,#115004,#115005,#115006,#115007,
#115008,#115009,#115010,#115011,#115012,#115013,#115014,#115015,#115016,
#115017,#115018,#115019,#115020,#115021,#115022,#115023,#115024,#115025,
#115026,#115027,#115028,#115029,#115030,#115031,#115032,#115033,#115034,
#115035,#115036,#115037,#115038,#115039,#115040,#115041,#115042,#115043,
#115044,#115045,#115046,#115047,#115048,#115049,#115050),.UNSPECIFIED.,
 .F.,.F.)
B_SPLINE_CURVE_WITH_KNOTS((6,1,1,1,1,1,1,1,1,1,1,1,1,1,1,1,1,1,1,1,1,1,
1,1,1,1,1,1,1,1,1,1,1,1,1,1,1,1,1,1,1,1,1,1,1,1,1,1,1,1,1,1,1,1,1,1,1,1,
1,1,1,1,1,1,1,1,1,1,1,1,1,1,1,1,1,1,1,1,1,1,1,1,1,1,1,1,1,1,1,1,1,1,1,1,
1,1,1,1,1,1,1,1,1,1,1,1,1,1,1,1,1,1,1,1,1,1,1,1,1,1,1,1,1,1,1,1,1,1,1,1,
1,1,1,1,1,1,1,1,1,1,1,1,1,1,1,1,1,1,1,1,1,1,1,1,1,1,1,1,1,1,1,1,1,1,1,1,
1,1,1,1,1,1,1,1,1,1,1,1,1,1,1,1,1,1,1,1,1,1,1,6),(0.,0.005,0.01,0.015,0.02,
0.025,0.03,0.035,0.04,0.045,0.05,0.055,0.06,0.065,0.07,0.075,0.08,0.085,
0.09,0.095,0.1,0.105,0.11,0.115,0.12,0.125,0.13,0.135,0.14,0.145,0.15,0.155,
0.16,0.165,0.17,0.175,0.18,0.185,0.19,0.195,0.2,0.205,0.21,0.215,0.22,0.225,
0.23,0.235,0.24,0.245,0.25,0.255,0.26,0.265,0.27,0.275,0.28,0.285,0.29,
0.295,0.3,0.305,0.31,0.315,0.32,0.325,0.33,0.335,0.34,0.345,0.35,0.355,
0.36,0.365,0.37,0.375,0.38,0.385,0.39,0.395,0.4,0.405,0.41,0.415,0.42,0.425,
0.43,0.435,0.44,0.445,0.45,0.455,0.46,0.465,0.47,0.475,0.48,0.485,0.49,
0.495,0.5,0.505,0.51,0.515,0.52,0.525,0.53,0.535,0.54,0.545,0.55,0.555,
0.56,0.565,0.57,0.575,0.58,0.585,0.59,0.595,0.6,0.605,0.61,0.615,0.62,0.625,
0.63,0.635,0.64,0.645,0.65,0.655,0.66,0.665,0.67,0.675,0.68,0.685,0.690000000000001,
0.695000000000001,0.700000000000001,0.705000000000001,0.710000000000001,
0.715000000000001,0.720000000000001,0.725000000000001,0.730000000000001,
0.735000000000001,0.740000000000001,0.745000000000001,0.750000000000001,
0.755000000000001,0.760000000000001,0.765000000000001,0.770000000000001,
0.775000000000001,0.780000000000001,0.785000000000001,0.790000000000001,
0.795000000000001,0.800000000000001,0.805000000000001,0.810000000000001,
0.815000000000001,0.820000000000001,0.825000000000001,0.830000000000001,
0.835000000000001,0.840000000000001,0.845000000000001,0.850000000000001,
0.855000000000001,0.860000000000001,0.865000000000001,0.870000000000001,
0.875000000000001,0.880000000000001,0.885000000000001,0.890000000000001,
0.895000000000001,0.900000000000001,0.905000000000001,0.910000000000001,
0.915000000000001,0.920000000000001,0.925000000000001,0.930000000000001,
0.935000000000001,0.940000000000001,0.94142984443138),.UNSPECIFIED.)
CURVE()
GEOMETRIC_REPRESENTATION_ITEM()
RATIONAL_B_SPLINE_CURVE((1.,1.,1.,1.,1.,1.,1.,1.,1.,1.,1.,1.,1.,1.,1.,1.,
1.,1.,1.,1.,1.,1.,1.,1.,1.,1.,1.,1.,1.,1.,1.,1.,1.,1.,1.,1.,1.,1.,1.,1.,
1.,1.,1.,1.,1.,1.,1.,1.,1.,1.,1.,1.,1.,1.,1.,1.,1.,1.,1.,1.,1.,1.,1.,1.,
1.,1.,1.,1.,1.,1.,1.,1.,1.,1.,1.,1.,1.,1.,1.,1.,1.,1.,1.,1.,1.,1.,1.,1.,
1.,1.,1.,1.,1.,1.,1.,1.,1.,1.,1.,1.,1.,1.,1.,1.,1.,1.,1.,1.,1.,1.,1.,1.,
1.,1.,1.,1.,1.,1.,1.,1.,1.,1.,1.,1.,1.,1.,1.,1.,1.,1.,1.,1.,1.,1.,1.,1.,
1.,1.,1.,1.,1.,1.,1.,1.,1.,1.,1.,1.,1.,1.,1.,1.,1.,1.,1.,1.,1.,1.,1.,1.,
1.,1.,1.,1.,1.,1.,1.,1.,1.,1.,1.,1.,1.,1.,1.,1.,1.,1.,1.,1.,1.,1.,1.,1.,
1.,1.,1.,1.,1.,1.,1.,1.,1.,1.))
REPRESENTATION_ITEM('')
);
#542=(
BOUNDED_CURVE()
B_SPLINE_CURVE(5,(#115053,#115054,#115055,#115056,#115057,#115058,#115059,
#115060,#115061,#115062,#115063,#115064,#115065,#115066,#115067,#115068,
#115069,#115070,#115071,#115072,#115073,#115074,#115075,#115076,#115077,
#115078,#115079,#115080,#115081,#115082,#115083,#115084,#115085,#115086,
#115087,#115088,#115089,#115090,#115091,#115092,#115093,#115094,#115095,
#115096,#115097,#115098,#115099,#115100,#115101,#115102,#115103,#115104,
#115105,#115106,#115107,#115108,#115109,#115110,#115111,#115112,#115113,
#115114,#115115,#115116,#115117,#115118,#115119,#115120,#115121,#115122,
#115123,#115124,#115125,#115126,#115127,#115128,#115129,#115130,#115131,
#115132,#115133,#115134,#115135,#115136,#115137,#115138,#115139,#115140,
#115141,#115142,#115143,#115144,#115145,#115146,#115147,#115148,#115149,
#115150,#115151,#115152,#115153,#115154,#115155,#115156,#115157,#115158,
#115159,#115160,#115161,#115162,#115163,#115164,#115165,#115166,#115167,
#115168,#115169,#115170,#115171,#115172,#115173,#115174,#115175,#115176,
#115177,#115178,#115179,#115180,#115181,#115182,#115183,#115184,#115185,
#115186,#115187,#115188,#115189,#115190,#115191,#115192,#115193,#115194,
#115195,#115196,#115197,#115198,#115199,#115200,#115201,#115202,#115203,
#115204,#115205,#115206,#115207,#115208,#115209,#115210,#115211,#115212,
#115213,#115214,#115215,#115216,#115217,#115218,#115219,#115220,#115221,
#115222,#115223,#115224,#115225,#115226,#115227,#115228,#115229,#115230,
#115231,#115232,#115233,#115234,#115235,#115236,#115237,#115238,#115239,
#115240,#115241,#115242,#115243,#115244,#115245,#115246),.UNSPECIFIED.,
 .F.,.F.)
B_SPLINE_CURVE_WITH_KNOTS((6,1,1,1,1,1,1,1,1,1,1,1,1,1,1,1,1,1,1,1,1,1,
1,1,1,1,1,1,1,1,1,1,1,1,1,1,1,1,1,1,1,1,1,1,1,1,1,1,1,1,1,1,1,1,1,1,1,1,
1,1,1,1,1,1,1,1,1,1,1,1,1,1,1,1,1,1,1,1,1,1,1,1,1,1,1,1,1,1,1,1,1,1,1,1,
1,1,1,1,1,1,1,1,1,1,1,1,1,1,1,1,1,1,1,1,1,1,1,1,1,1,1,1,1,1,1,1,1,1,1,1,
1,1,1,1,1,1,1,1,1,1,1,1,1,1,1,1,1,1,1,1,1,1,1,1,1,1,1,1,1,1,1,1,1,1,1,1,
1,1,1,1,1,1,1,1,1,1,1,1,1,1,1,1,1,1,1,1,1,1,1,6),(-0.941429844431381,-0.940000000000001,
-0.935000000000001,-0.930000000000001,-0.925000000000001,-0.920000000000001,
-0.915000000000001,-0.910000000000001,-0.905000000000001,-0.900000000000001,
-0.895000000000001,-0.890000000000001,-0.885000000000001,-0.880000000000001,
-0.875000000000001,-0.870000000000001,-0.865000000000001,-0.860000000000001,
-0.855000000000001,-0.850000000000001,-0.845000000000001,-0.840000000000001,
-0.835000000000001,-0.830000000000001,-0.825000000000001,-0.820000000000001,
-0.815000000000001,-0.810000000000001,-0.805000000000001,-0.800000000000001,
-0.795000000000001,-0.790000000000001,-0.785000000000001,-0.780000000000001,
-0.775000000000001,-0.770000000000001,-0.765000000000001,-0.760000000000001,
-0.755000000000001,-0.750000000000001,-0.745000000000001,-0.740000000000001,
-0.735000000000001,-0.730000000000001,-0.725000000000001,-0.720000000000001,
-0.715000000000001,-0.710000000000001,-0.705000000000001,-0.700000000000001,
-0.695000000000001,-0.690000000000001,-0.685,-0.68,-0.675,-0.67,-0.665,
-0.66,-0.655,-0.65,-0.645,-0.64,-0.635,-0.63,-0.625,-0.62,-0.615,-0.61,
-0.605,-0.6,-0.595,-0.59,-0.585,-0.58,-0.575,-0.57,-0.565,-0.56,-0.555,
-0.55,-0.545,-0.54,-0.535,-0.53,-0.525,-0.52,-0.515,-0.51,-0.505,-0.5,-0.495,
-0.49,-0.485,-0.48,-0.475,-0.47,-0.465,-0.46,-0.455,-0.45,-0.445,-0.44,
-0.435,-0.43,-0.425,-0.42,-0.415,-0.41,-0.405,-0.4,-0.395,-0.39,-0.385,
-0.38,-0.375,-0.37,-0.365,-0.36,-0.355,-0.35,-0.345,-0.34,-0.335,-0.33,
-0.325,-0.32,-0.315,-0.31,-0.305,-0.3,-0.295,-0.29,-0.285,-0.28,-0.275,
-0.27,-0.265,-0.26,-0.255,-0.25,-0.245,-0.24,-0.235,-0.23,-0.225,-0.22,
-0.215,-0.21,-0.205,-0.2,-0.195,-0.19,-0.185,-0.18,-0.175,-0.17,-0.165,
-0.16,-0.155,-0.15,-0.145,-0.14,-0.135,-0.13,-0.125,-0.12,-0.115,-0.11,
-0.105,-0.1,-0.095,-0.09,-0.085,-0.08,-0.075,-0.07,-0.065,-0.06,-0.055,
-0.05,-0.045,-0.04,-0.035,-0.03,-0.025,-0.02,-0.015,-0.01,-0.005,0.),
 .UNSPECIFIED.)
CURVE()
GEOMETRIC_REPRESENTATION_ITEM()
RATIONAL_B_SPLINE_CURVE((1.,1.,1.,1.,1.,1.,1.,1.,1.,1.,1.,1.,1.,1.,1.,1.,
1.,1.,1.,1.,1.,1.,1.,1.,1.,1.,1.,1.,1.,1.,1.,1.,1.,1.,1.,1.,1.,1.,1.,1.,
1.,1.,1.,1.,1.,1.,1.,1.,1.,1.,1.,1.,1.,1.,1.,1.,1.,1.,1.,1.,1.,1.,1.,1.,
1.,1.,1.,1.,1.,1.,1.,1.,1.,1.,1.,1.,1.,1.,1.,1.,1.,1.,1.,1.,1.,1.,1.,1.,
1.,1.,1.,1.,1.,1.,1.,1.,1.,1.,1.,1.,1.,1.,1.,1.,1.,1.,1.,1.,1.,1.,1.,1.,
1.,1.,1.,1.,1.,1.,1.,1.,1.,1.,1.,1.,1.,1.,1.,1.,1.,1.,1.,1.,1.,1.,1.,1.,
1.,1.,1.,1.,1.,1.,1.,1.,1.,1.,1.,1.,1.,1.,1.,1.,1.,1.,1.,1.,1.,1.,1.,1.,
1.,1.,1.,1.,1.,1.,1.,1.,1.,1.,1.,1.,1.,1.,1.,1.,1.,1.,1.,1.,1.,1.,1.,1.,
1.,1.,1.,1.,1.,1.,1.,1.,1.,1.))
REPRESENTATION_ITEM('')
);
#543=(
BOUNDED_CURVE()
B_SPLINE_CURVE(5,(#115753,#115754,#115755,#115756,#115757,#115758,#115759,
#115760,#115761,#115762,#115763,#115764,#115765,#115766,#115767,#115768,
#115769,#115770,#115771,#115772,#115773,#115774,#115775,#115776,#115777,
#115778,#115779,#115780,#115781,#115782,#115783,#115784,#115785,#115786,
#115787,#115788,#115789,#115790,#115791,#115792,#115793,#115794,#115795,
#115796,#115797,#115798,#115799,#115800,#115801,#115802,#115803,#115804,
#115805,#115806,#115807,#115808,#115809,#115810,#115811,#115812,#115813,
#115814,#115815,#115816,#115817,#115818,#115819,#115820,#115821,#115822,
#115823,#115824,#115825,#115826,#115827,#115828,#115829,#115830,#115831,
#115832,#115833,#115834,#115835,#115836,#115837,#115838,#115839,#115840,
#115841,#115842,#115843,#115844,#115845,#115846,#115847,#115848,#115849,
#115850,#115851,#115852,#115853,#115854,#115855,#115856,#115857,#115858,
#115859,#115860,#115861,#115862,#115863,#115864,#115865,#115866,#115867,
#115868,#115869,#115870,#115871,#115872,#115873,#115874,#115875,#115876,
#115877,#115878,#115879,#115880,#115881,#115882,#115883,#115884,#115885,
#115886,#115887,#115888,#115889,#115890,#115891,#115892,#115893,#115894,
#115895,#115896,#115897,#115898,#115899,#115900,#115901,#115902,#115903,
#115904,#115905,#115906,#115907,#115908,#115909,#115910,#115911,#115912,
#115913,#115914,#115915,#115916,#115917,#115918,#115919,#115920,#115921,
#115922,#115923,#115924,#115925,#115926,#115927,#115928,#115929,#115930,
#115931,#115932,#115933,#115934,#115935,#115936,#115937,#115938,#115939,
#115940,#115941,#115942,#115943,#115944,#115945,#115946),.UNSPECIFIED.,
 .F.,.F.)
B_SPLINE_CURVE_WITH_KNOTS((6,1,1,1,1,1,1,1,1,1,1,1,1,1,1,1,1,1,1,1,1,1,
1,1,1,1,1,1,1,1,1,1,1,1,1,1,1,1,1,1,1,1,1,1,1,1,1,1,1,1,1,1,1,1,1,1,1,1,
1,1,1,1,1,1,1,1,1,1,1,1,1,1,1,1,1,1,1,1,1,1,1,1,1,1,1,1,1,1,1,1,1,1,1,1,
1,1,1,1,1,1,1,1,1,1,1,1,1,1,1,1,1,1,1,1,1,1,1,1,1,1,1,1,1,1,1,1,1,1,1,1,
1,1,1,1,1,1,1,1,1,1,1,1,1,1,1,1,1,1,1,1,1,1,1,1,1,1,1,1,1,1,1,1,1,1,1,1,
1,1,1,1,1,1,1,1,1,1,1,1,1,1,1,1,1,1,1,1,1,1,1,6),(0.,0.005,0.01,0.015,0.02,
0.025,0.03,0.035,0.04,0.045,0.05,0.055,0.06,0.065,0.07,0.075,0.08,0.085,
0.09,0.095,0.1,0.105,0.11,0.115,0.12,0.125,0.13,0.135,0.14,0.145,0.15,0.155,
0.16,0.165,0.17,0.175,0.18,0.185,0.19,0.195,0.2,0.205,0.21,0.215,0.22,0.225,
0.23,0.235,0.24,0.245,0.25,0.255,0.26,0.265,0.27,0.275,0.28,0.285,0.29,
0.295,0.3,0.305,0.31,0.315,0.32,0.325,0.33,0.335,0.34,0.345,0.35,0.355,
0.36,0.365,0.37,0.375,0.38,0.385,0.39,0.395,0.4,0.405,0.41,0.415,0.42,0.425,
0.43,0.435,0.44,0.445,0.45,0.455,0.46,0.465,0.47,0.475,0.48,0.485,0.49,
0.495,0.5,0.505,0.51,0.515,0.52,0.525,0.53,0.535,0.54,0.545,0.55,0.555,
0.56,0.565,0.57,0.575,0.58,0.585,0.59,0.595,0.6,0.605,0.61,0.615,0.62,0.625,
0.63,0.635,0.64,0.645,0.65,0.655,0.66,0.665,0.67,0.675,0.68,0.685,0.690000000000001,
0.695000000000001,0.700000000000001,0.705000000000001,0.710000000000001,
0.715000000000001,0.720000000000001,0.725000000000001,0.730000000000001,
0.735000000000001,0.740000000000001,0.745000000000001,0.750000000000001,
0.755000000000001,0.760000000000001,0.765000000000001,0.770000000000001,
0.775000000000001,0.780000000000001,0.785000000000001,0.790000000000001,
0.795000000000001,0.800000000000001,0.805000000000001,0.810000000000001,
0.815000000000001,0.820000000000001,0.825000000000001,0.830000000000001,
0.835000000000001,0.840000000000001,0.845000000000001,0.850000000000001,
0.855000000000001,0.860000000000001,0.865000000000001,0.870000000000001,
0.875000000000001,0.880000000000001,0.885000000000001,0.890000000000001,
0.895000000000001,0.900000000000001,0.905000000000001,0.910000000000001,
0.915000000000001,0.920000000000001,0.925000000000001,0.930000000000001,
0.935000000000001,0.940000000000001,0.941429844431474),.UNSPECIFIED.)
CURVE()
GEOMETRIC_REPRESENTATION_ITEM()
RATIONAL_B_SPLINE_CURVE((1.,1.,1.,1.,1.,1.,1.,1.,1.,1.,1.,1.,1.,1.,1.,1.,
1.,1.,1.,1.,1.,1.,1.,1.,1.,1.,1.,1.,1.,1.,1.,1.,1.,1.,1.,1.,1.,1.,1.,1.,
1.,1.,1.,1.,1.,1.,1.,1.,1.,1.,1.,1.,1.,1.,1.,1.,1.,1.,1.,1.,1.,1.,1.,1.,
1.,1.,1.,1.,1.,1.,1.,1.,1.,1.,1.,1.,1.,1.,1.,1.,1.,1.,1.,1.,1.,1.,1.,1.,
1.,1.,1.,1.,1.,1.,1.,1.,1.,1.,1.,1.,1.,1.,1.,1.,1.,1.,1.,1.,1.,1.,1.,1.,
1.,1.,1.,1.,1.,1.,1.,1.,1.,1.,1.,1.,1.,1.,1.,1.,1.,1.,1.,1.,1.,1.,1.,1.,
1.,1.,1.,1.,1.,1.,1.,1.,1.,1.,1.,1.,1.,1.,1.,1.,1.,1.,1.,1.,1.,1.,1.,1.,
1.,1.,1.,1.,1.,1.,1.,1.,1.,1.,1.,1.,1.,1.,1.,1.,1.,1.,1.,1.,1.,1.,1.,1.,
1.,1.,1.,1.,1.,1.,1.,1.,1.,1.))
REPRESENTATION_ITEM('')
);
#544=(
BOUNDED_CURVE()
B_SPLINE_CURVE(5,(#115949,#115950,#115951,#115952,#115953,#115954,#115955,
#115956,#115957,#115958,#115959,#115960,#115961,#115962,#115963,#115964,
#115965,#115966,#115967,#115968,#115969,#115970,#115971,#115972,#115973,
#115974,#115975,#115976,#115977,#115978,#115979,#115980,#115981,#115982,
#115983,#115984,#115985,#115986,#115987,#115988,#115989,#115990,#115991,
#115992,#115993,#115994,#115995,#115996,#115997,#115998,#115999,#116000,
#116001,#116002,#116003,#116004,#116005,#116006,#116007,#116008,#116009,
#116010,#116011,#116012,#116013,#116014,#116015,#116016,#116017,#116018,
#116019,#116020,#116021,#116022,#116023,#116024,#116025,#116026,#116027,
#116028,#116029,#116030,#116031,#116032,#116033,#116034,#116035,#116036,
#116037,#116038,#116039,#116040,#116041,#116042,#116043,#116044,#116045,
#116046,#116047,#116048,#116049,#116050,#116051,#116052,#116053,#116054,
#116055,#116056,#116057,#116058,#116059,#116060,#116061,#116062,#116063,
#116064,#116065,#116066,#116067,#116068,#116069,#116070,#116071,#116072,
#116073,#116074,#116075,#116076,#116077,#116078,#116079,#116080,#116081,
#116082,#116083,#116084,#116085,#116086,#116087,#116088,#116089,#116090,
#116091,#116092,#116093,#116094,#116095,#116096,#116097,#116098,#116099,
#116100,#116101,#116102,#116103,#116104,#116105,#116106,#116107,#116108,
#116109,#116110,#116111,#116112,#116113,#116114,#116115,#116116,#116117,
#116118,#116119,#116120,#116121,#116122,#116123,#116124,#116125,#116126,
#116127,#116128,#116129,#116130,#116131,#116132,#116133,#116134,#116135,
#116136,#116137,#116138,#116139,#116140,#116141,#116142),.UNSPECIFIED.,
 .F.,.F.)
B_SPLINE_CURVE_WITH_KNOTS((6,1,1,1,1,1,1,1,1,1,1,1,1,1,1,1,1,1,1,1,1,1,
1,1,1,1,1,1,1,1,1,1,1,1,1,1,1,1,1,1,1,1,1,1,1,1,1,1,1,1,1,1,1,1,1,1,1,1,
1,1,1,1,1,1,1,1,1,1,1,1,1,1,1,1,1,1,1,1,1,1,1,1,1,1,1,1,1,1,1,1,1,1,1,1,
1,1,1,1,1,1,1,1,1,1,1,1,1,1,1,1,1,1,1,1,1,1,1,1,1,1,1,1,1,1,1,1,1,1,1,1,
1,1,1,1,1,1,1,1,1,1,1,1,1,1,1,1,1,1,1,1,1,1,1,1,1,1,1,1,1,1,1,1,1,1,1,1,
1,1,1,1,1,1,1,1,1,1,1,1,1,1,1,1,1,1,1,1,1,1,1,6),(-0.941429844431504,-0.940000000000001,
-0.935000000000001,-0.930000000000001,-0.925000000000001,-0.920000000000001,
-0.915000000000001,-0.910000000000001,-0.905000000000001,-0.900000000000001,
-0.895000000000001,-0.890000000000001,-0.885000000000001,-0.880000000000001,
-0.875000000000001,-0.870000000000001,-0.865000000000001,-0.860000000000001,
-0.855000000000001,-0.850000000000001,-0.845000000000001,-0.840000000000001,
-0.835000000000001,-0.830000000000001,-0.825000000000001,-0.820000000000001,
-0.815000000000001,-0.810000000000001,-0.805000000000001,-0.800000000000001,
-0.795000000000001,-0.790000000000001,-0.785000000000001,-0.780000000000001,
-0.775000000000001,-0.770000000000001,-0.765000000000001,-0.760000000000001,
-0.755000000000001,-0.750000000000001,-0.745000000000001,-0.740000000000001,
-0.735000000000001,-0.730000000000001,-0.725000000000001,-0.720000000000001,
-0.715000000000001,-0.710000000000001,-0.705000000000001,-0.700000000000001,
-0.695000000000001,-0.690000000000001,-0.685,-0.68,-0.675,-0.67,-0.665,
-0.66,-0.655,-0.65,-0.645,-0.64,-0.635,-0.63,-0.625,-0.62,-0.615,-0.61,
-0.605,-0.6,-0.595,-0.59,-0.585,-0.58,-0.575,-0.57,-0.565,-0.56,-0.555,
-0.55,-0.545,-0.54,-0.535,-0.53,-0.525,-0.52,-0.515,-0.51,-0.505,-0.5,-0.495,
-0.49,-0.485,-0.48,-0.475,-0.47,-0.465,-0.46,-0.455,-0.45,-0.445,-0.44,
-0.435,-0.43,-0.425,-0.42,-0.415,-0.41,-0.405,-0.4,-0.395,-0.39,-0.385,
-0.38,-0.375,-0.37,-0.365,-0.36,-0.355,-0.35,-0.345,-0.34,-0.335,-0.33,
-0.325,-0.32,-0.315,-0.31,-0.305,-0.3,-0.295,-0.29,-0.285,-0.28,-0.275,
-0.27,-0.265,-0.26,-0.255,-0.25,-0.245,-0.24,-0.235,-0.23,-0.225,-0.22,
-0.215,-0.21,-0.205,-0.2,-0.195,-0.19,-0.185,-0.18,-0.175,-0.17,-0.165,
-0.16,-0.155,-0.15,-0.145,-0.14,-0.135,-0.13,-0.125,-0.12,-0.115,-0.11,
-0.105,-0.1,-0.095,-0.09,-0.085,-0.08,-0.075,-0.07,-0.065,-0.06,-0.055,
-0.05,-0.045,-0.04,-0.035,-0.03,-0.025,-0.02,-0.015,-0.01,-0.005,0.),
 .UNSPECIFIED.)
CURVE()
GEOMETRIC_REPRESENTATION_ITEM()
RATIONAL_B_SPLINE_CURVE((1.,1.,1.,1.,1.,1.,1.,1.,1.,1.,1.,1.,1.,1.,1.,1.,
1.,1.,1.,1.,1.,1.,1.,1.,1.,1.,1.,1.,1.,1.,1.,1.,1.,1.,1.,1.,1.,1.,1.,1.,
1.,1.,1.,1.,1.,1.,1.,1.,1.,1.,1.,1.,1.,1.,1.,1.,1.,1.,1.,1.,1.,1.,1.,1.,
1.,1.,1.,1.,1.,1.,1.,1.,1.,1.,1.,1.,1.,1.,1.,1.,1.,1.,1.,1.,1.,1.,1.,1.,
1.,1.,1.,1.,1.,1.,1.,1.,1.,1.,1.,1.,1.,1.,1.,1.,1.,1.,1.,1.,1.,1.,1.,1.,
1.,1.,1.,1.,1.,1.,1.,1.,1.,1.,1.,1.,1.,1.,1.,1.,1.,1.,1.,1.,1.,1.,1.,1.,
1.,1.,1.,1.,1.,1.,1.,1.,1.,1.,1.,1.,1.,1.,1.,1.,1.,1.,1.,1.,1.,1.,1.,1.,
1.,1.,1.,1.,1.,1.,1.,1.,1.,1.,1.,1.,1.,1.,1.,1.,1.,1.,1.,1.,1.,1.,1.,1.,
1.,1.,1.,1.,1.,1.,1.,1.,1.,1.))
REPRESENTATION_ITEM('')
);
#545=(
BOUNDED_CURVE()
B_SPLINE_CURVE(5,(#116603,#116604,#116605,#116606,#116607,#116608,#116609,
#116610,#116611,#116612,#116613,#116614,#116615,#116616,#116617,#116618,
#116619,#116620,#116621,#116622,#116623,#116624,#116625,#116626,#116627,
#116628,#116629,#116630,#116631,#116632,#116633,#116634,#116635,#116636,
#116637,#116638,#116639,#116640,#116641,#116642,#116643,#116644,#116645,
#116646,#116647,#116648,#116649,#116650,#116651,#116652,#116653,#116654,
#116655,#116656,#116657,#116658,#116659,#116660,#116661,#116662,#116663,
#116664,#116665,#116666,#116667,#116668,#116669,#116670,#116671,#116672,
#116673,#116674,#116675,#116676,#116677,#116678,#116679,#116680,#116681,
#116682,#116683,#116684,#116685,#116686,#116687,#116688,#116689,#116690,
#116691,#116692,#116693,#116694,#116695,#116696,#116697,#116698,#116699,
#116700,#116701,#116702,#116703,#116704,#116705,#116706,#116707,#116708,
#116709,#116710,#116711,#116712,#116713,#116714,#116715,#116716,#116717,
#116718,#116719,#116720,#116721,#116722,#116723,#116724,#116725,#116726,
#116727,#116728,#116729,#116730,#116731,#116732,#116733,#116734,#116735,
#116736,#116737,#116738,#116739,#116740,#116741,#116742,#116743,#116744,
#116745,#116746,#116747,#116748,#116749,#116750,#116751,#116752,#116753,
#116754,#116755,#116756,#116757,#116758,#116759,#116760,#116761,#116762,
#116763,#116764,#116765,#116766,#116767,#116768,#116769,#116770,#116771,
#116772,#116773,#116774,#116775,#116776,#116777,#116778,#116779,#116780,
#116781,#116782,#116783,#116784,#116785,#116786,#116787,#116788,#116789,
#116790,#116791,#116792,#116793,#116794,#116795,#116796),.UNSPECIFIED.,
 .F.,.F.)
B_SPLINE_CURVE_WITH_KNOTS((6,1,1,1,1,1,1,1,1,1,1,1,1,1,1,1,1,1,1,1,1,1,
1,1,1,1,1,1,1,1,1,1,1,1,1,1,1,1,1,1,1,1,1,1,1,1,1,1,1,1,1,1,1,1,1,1,1,1,
1,1,1,1,1,1,1,1,1,1,1,1,1,1,1,1,1,1,1,1,1,1,1,1,1,1,1,1,1,1,1,1,1,1,1,1,
1,1,1,1,1,1,1,1,1,1,1,1,1,1,1,1,1,1,1,1,1,1,1,1,1,1,1,1,1,1,1,1,1,1,1,1,
1,1,1,1,1,1,1,1,1,1,1,1,1,1,1,1,1,1,1,1,1,1,1,1,1,1,1,1,1,1,1,1,1,1,1,1,
1,1,1,1,1,1,1,1,1,1,1,1,1,1,1,1,1,1,1,1,1,1,1,6),(0.,0.005,0.01,0.015,0.02,
0.025,0.03,0.035,0.04,0.045,0.05,0.055,0.06,0.065,0.07,0.075,0.08,0.085,
0.09,0.095,0.1,0.105,0.11,0.115,0.12,0.125,0.13,0.135,0.14,0.145,0.15,0.155,
0.16,0.165,0.17,0.175,0.18,0.185,0.19,0.195,0.2,0.205,0.21,0.215,0.22,0.225,
0.23,0.235,0.24,0.245,0.25,0.255,0.26,0.265,0.27,0.275,0.28,0.285,0.29,
0.295,0.3,0.305,0.31,0.315,0.32,0.325,0.33,0.335,0.34,0.345,0.35,0.355,
0.36,0.365,0.37,0.375,0.38,0.385,0.39,0.395,0.4,0.405,0.41,0.415,0.42,0.425,
0.43,0.435,0.44,0.445,0.45,0.455,0.46,0.465,0.47,0.475,0.48,0.485,0.49,
0.495,0.5,0.505,0.51,0.515,0.52,0.525,0.53,0.535,0.54,0.545,0.55,0.555,
0.56,0.565,0.57,0.575,0.58,0.585,0.59,0.595,0.6,0.605,0.61,0.615,0.62,0.625,
0.63,0.635,0.64,0.645,0.65,0.655,0.66,0.665,0.67,0.675,0.68,0.685,0.690000000000001,
0.695000000000001,0.700000000000001,0.705000000000001,0.710000000000001,
0.715000000000001,0.720000000000001,0.725000000000001,0.730000000000001,
0.735000000000001,0.740000000000001,0.745000000000001,0.750000000000001,
0.755000000000001,0.760000000000001,0.765000000000001,0.770000000000001,
0.775000000000001,0.780000000000001,0.785000000000001,0.790000000000001,
0.795000000000001,0.800000000000001,0.805000000000001,0.810000000000001,
0.815000000000001,0.820000000000001,0.825000000000001,0.830000000000001,
0.835000000000001,0.840000000000001,0.845000000000001,0.850000000000001,
0.855000000000001,0.860000000000001,0.865000000000001,0.870000000000001,
0.875000000000001,0.880000000000001,0.885000000000001,0.890000000000001,
0.895000000000001,0.900000000000001,0.905000000000001,0.910000000000001,
0.915000000000001,0.920000000000001,0.925000000000001,0.930000000000001,
0.935000000000001,0.940000000000001,0.941429844438054),.UNSPECIFIED.)
CURVE()
GEOMETRIC_REPRESENTATION_ITEM()
RATIONAL_B_SPLINE_CURVE((1.,1.,1.,1.,1.,1.,1.,1.,1.,1.,1.,1.,1.,1.,1.,1.,
1.,1.,1.,1.,1.,1.,1.,1.,1.,1.,1.,1.,1.,1.,1.,1.,1.,1.,1.,1.,1.,1.,1.,1.,
1.,1.,1.,1.,1.,1.,1.,1.,1.,1.,1.,1.,1.,1.,1.,1.,1.,1.,1.,1.,1.,1.,1.,1.,
1.,1.,1.,1.,1.,1.,1.,1.,1.,1.,1.,1.,1.,1.,1.,1.,1.,1.,1.,1.,1.,1.,1.,1.,
1.,1.,1.,1.,1.,1.,1.,1.,1.,1.,1.,1.,1.,1.,1.,1.,1.,1.,1.,1.,1.,1.,1.,1.,
1.,1.,1.,1.,1.,1.,1.,1.,1.,1.,1.,1.,1.,1.,1.,1.,1.,1.,1.,1.,1.,1.,1.,1.,
1.,1.,1.,1.,1.,1.,1.,1.,1.,1.,1.,1.,1.,1.,1.,1.,1.,1.,1.,1.,1.,1.,1.,1.,
1.,1.,1.,1.,1.,1.,1.,1.,1.,1.,1.,1.,1.,1.,1.,1.,1.,1.,1.,1.,1.,1.,1.,1.,
1.,1.,1.,1.,1.,1.,1.,1.,1.,1.))
REPRESENTATION_ITEM('')
);
#546=(
BOUNDED_CURVE()
B_SPLINE_CURVE(5,(#116799,#116800,#116801,#116802,#116803,#116804,#116805,
#116806,#116807,#116808,#116809,#116810,#116811,#116812,#116813,#116814,
#116815,#116816,#116817,#116818,#116819,#116820,#116821,#116822,#116823,
#116824,#116825,#116826,#116827,#116828,#116829,#116830,#116831,#116832,
#116833,#116834,#116835,#116836,#116837,#116838,#116839,#116840,#116841,
#116842,#116843,#116844,#116845,#116846,#116847,#116848,#116849,#116850,
#116851,#116852,#116853,#116854,#116855,#116856,#116857,#116858,#116859,
#116860,#116861,#116862,#116863,#116864,#116865,#116866,#116867,#116868,
#116869,#116870,#116871,#116872,#116873,#116874,#116875,#116876,#116877,
#116878,#116879,#116880,#116881,#116882,#116883,#116884,#116885,#116886,
#116887,#116888,#116889,#116890,#116891,#116892,#116893,#116894,#116895,
#116896,#116897,#116898,#116899,#116900,#116901,#116902,#116903,#116904,
#116905,#116906,#116907,#116908,#116909,#116910,#116911,#116912,#116913,
#116914,#116915,#116916,#116917,#116918,#116919,#116920,#116921,#116922,
#116923,#116924,#116925,#116926,#116927,#116928,#116929,#116930,#116931,
#116932,#116933,#116934,#116935,#116936,#116937,#116938,#116939,#116940,
#116941,#116942,#116943,#116944,#116945,#116946,#116947,#116948,#116949,
#116950,#116951,#116952,#116953,#116954,#116955,#116956,#116957,#116958,
#116959,#116960,#116961,#116962,#116963,#116964,#116965,#116966,#116967,
#116968,#116969,#116970,#116971,#116972,#116973,#116974,#116975,#116976,
#116977,#116978,#116979,#116980,#116981,#116982,#116983,#116984,#116985,
#116986,#116987,#116988,#116989,#116990,#116991,#116992),.UNSPECIFIED.,
 .F.,.F.)
B_SPLINE_CURVE_WITH_KNOTS((6,1,1,1,1,1,1,1,1,1,1,1,1,1,1,1,1,1,1,1,1,1,
1,1,1,1,1,1,1,1,1,1,1,1,1,1,1,1,1,1,1,1,1,1,1,1,1,1,1,1,1,1,1,1,1,1,1,1,
1,1,1,1,1,1,1,1,1,1,1,1,1,1,1,1,1,1,1,1,1,1,1,1,1,1,1,1,1,1,1,1,1,1,1,1,
1,1,1,1,1,1,1,1,1,1,1,1,1,1,1,1,1,1,1,1,1,1,1,1,1,1,1,1,1,1,1,1,1,1,1,1,
1,1,1,1,1,1,1,1,1,1,1,1,1,1,1,1,1,1,1,1,1,1,1,1,1,1,1,1,1,1,1,1,1,1,1,1,
1,1,1,1,1,1,1,1,1,1,1,1,1,1,1,1,1,1,1,1,1,1,1,6),(-0.941429844438061,-0.940000000000001,
-0.935000000000001,-0.930000000000001,-0.925000000000001,-0.920000000000001,
-0.915000000000001,-0.910000000000001,-0.905000000000001,-0.900000000000001,
-0.895000000000001,-0.890000000000001,-0.885000000000001,-0.880000000000001,
-0.875000000000001,-0.870000000000001,-0.865000000000001,-0.860000000000001,
-0.855000000000001,-0.850000000000001,-0.845000000000001,-0.840000000000001,
-0.835000000000001,-0.830000000000001,-0.825000000000001,-0.820000000000001,
-0.815000000000001,-0.810000000000001,-0.805000000000001,-0.800000000000001,
-0.795000000000001,-0.790000000000001,-0.785000000000001,-0.780000000000001,
-0.775000000000001,-0.770000000000001,-0.765000000000001,-0.760000000000001,
-0.755000000000001,-0.750000000000001,-0.745000000000001,-0.740000000000001,
-0.735000000000001,-0.730000000000001,-0.725000000000001,-0.720000000000001,
-0.715000000000001,-0.710000000000001,-0.705000000000001,-0.700000000000001,
-0.695000000000001,-0.690000000000001,-0.685,-0.68,-0.675,-0.67,-0.665,
-0.66,-0.655,-0.65,-0.645,-0.64,-0.635,-0.63,-0.625,-0.62,-0.615,-0.61,
-0.605,-0.6,-0.595,-0.59,-0.585,-0.58,-0.575,-0.57,-0.565,-0.56,-0.555,
-0.55,-0.545,-0.54,-0.535,-0.53,-0.525,-0.52,-0.515,-0.51,-0.505,-0.5,-0.495,
-0.49,-0.485,-0.48,-0.475,-0.47,-0.465,-0.46,-0.455,-0.45,-0.445,-0.44,
-0.435,-0.43,-0.425,-0.42,-0.415,-0.41,-0.405,-0.4,-0.395,-0.39,-0.385,
-0.38,-0.375,-0.37,-0.365,-0.36,-0.355,-0.35,-0.345,-0.34,-0.335,-0.33,
-0.325,-0.32,-0.315,-0.31,-0.305,-0.3,-0.295,-0.29,-0.285,-0.28,-0.275,
-0.27,-0.265,-0.26,-0.255,-0.25,-0.245,-0.24,-0.235,-0.23,-0.225,-0.22,
-0.215,-0.21,-0.205,-0.2,-0.195,-0.19,-0.185,-0.18,-0.175,-0.17,-0.165,
-0.16,-0.155,-0.15,-0.145,-0.14,-0.135,-0.13,-0.125,-0.12,-0.115,-0.11,
-0.105,-0.1,-0.095,-0.09,-0.085,-0.08,-0.075,-0.07,-0.065,-0.06,-0.055,
-0.05,-0.045,-0.04,-0.035,-0.03,-0.025,-0.02,-0.015,-0.01,-0.005,0.),
 .UNSPECIFIED.)
CURVE()
GEOMETRIC_REPRESENTATION_ITEM()
RATIONAL_B_SPLINE_CURVE((1.,1.,1.,1.,1.,1.,1.,1.,1.,1.,1.,1.,1.,1.,1.,1.,
1.,1.,1.,1.,1.,1.,1.,1.,1.,1.,1.,1.,1.,1.,1.,1.,1.,1.,1.,1.,1.,1.,1.,1.,
1.,1.,1.,1.,1.,1.,1.,1.,1.,1.,1.,1.,1.,1.,1.,1.,1.,1.,1.,1.,1.,1.,1.,1.,
1.,1.,1.,1.,1.,1.,1.,1.,1.,1.,1.,1.,1.,1.,1.,1.,1.,1.,1.,1.,1.,1.,1.,1.,
1.,1.,1.,1.,1.,1.,1.,1.,1.,1.,1.,1.,1.,1.,1.,1.,1.,1.,1.,1.,1.,1.,1.,1.,
1.,1.,1.,1.,1.,1.,1.,1.,1.,1.,1.,1.,1.,1.,1.,1.,1.,1.,1.,1.,1.,1.,1.,1.,
1.,1.,1.,1.,1.,1.,1.,1.,1.,1.,1.,1.,1.,1.,1.,1.,1.,1.,1.,1.,1.,1.,1.,1.,
1.,1.,1.,1.,1.,1.,1.,1.,1.,1.,1.,1.,1.,1.,1.,1.,1.,1.,1.,1.,1.,1.,1.,1.,
1.,1.,1.,1.,1.,1.,1.,1.,1.,1.))
REPRESENTATION_ITEM('')
);
#547=(
BOUNDED_CURVE()
B_SPLINE_CURVE(5,(#117404,#117405,#117406,#117407,#117408,#117409,#117410,
#117411,#117412,#117413,#117414,#117415,#117416,#117417,#117418,#117419,
#117420,#117421,#117422,#117423,#117424,#117425,#117426,#117427,#117428,
#117429,#117430,#117431,#117432,#117433,#117434,#117435,#117436,#117437,
#117438,#117439,#117440,#117441,#117442,#117443,#117444,#117445,#117446,
#117447,#117448,#117449,#117450,#117451,#117452,#117453,#117454,#117455,
#117456,#117457,#117458,#117459,#117460,#117461,#117462,#117463,#117464,
#117465,#117466,#117467,#117468,#117469,#117470,#117471,#117472,#117473,
#117474,#117475,#117476,#117477,#117478,#117479,#117480,#117481,#117482,
#117483,#117484,#117485,#117486,#117487,#117488,#117489,#117490,#117491,
#117492,#117493,#117494,#117495,#117496,#117497,#117498,#117499,#117500,
#117501,#117502,#117503,#117504,#117505,#117506,#117507,#117508,#117509,
#117510,#117511,#117512,#117513,#117514,#117515,#117516,#117517,#117518,
#117519,#117520,#117521,#117522,#117523,#117524,#117525,#117526,#117527,
#117528,#117529,#117530,#117531,#117532,#117533,#117534,#117535,#117536,
#117537,#117538,#117539,#117540,#117541,#117542,#117543,#117544,#117545,
#117546,#117547,#117548,#117549,#117550,#117551,#117552,#117553,#117554,
#117555,#117556,#117557,#117558,#117559,#117560,#117561,#117562,#117563,
#117564,#117565,#117566,#117567,#117568,#117569,#117570,#117571,#117572,
#117573,#117574,#117575,#117576,#117577,#117578,#117579,#117580,#117581,
#117582,#117583,#117584,#117585,#117586,#117587,#117588,#117589,#117590,
#117591,#117592,#117593,#117594,#117595,#117596,#117597),.UNSPECIFIED.,
 .F.,.F.)
B_SPLINE_CURVE_WITH_KNOTS((6,1,1,1,1,1,1,1,1,1,1,1,1,1,1,1,1,1,1,1,1,1,
1,1,1,1,1,1,1,1,1,1,1,1,1,1,1,1,1,1,1,1,1,1,1,1,1,1,1,1,1,1,1,1,1,1,1,1,
1,1,1,1,1,1,1,1,1,1,1,1,1,1,1,1,1,1,1,1,1,1,1,1,1,1,1,1,1,1,1,1,1,1,1,1,
1,1,1,1,1,1,1,1,1,1,1,1,1,1,1,1,1,1,1,1,1,1,1,1,1,1,1,1,1,1,1,1,1,1,1,1,
1,1,1,1,1,1,1,1,1,1,1,1,1,1,1,1,1,1,1,1,1,1,1,1,1,1,1,1,1,1,1,1,1,1,1,1,
1,1,1,1,1,1,1,1,1,1,1,1,1,1,1,1,1,1,1,1,1,1,1,6),(0.,0.005,0.01,0.015,0.02,
0.025,0.03,0.035,0.04,0.045,0.05,0.055,0.06,0.065,0.07,0.075,0.08,0.085,
0.09,0.095,0.1,0.105,0.11,0.115,0.12,0.125,0.13,0.135,0.14,0.145,0.15,0.155,
0.16,0.165,0.17,0.175,0.18,0.185,0.19,0.195,0.2,0.205,0.21,0.215,0.22,0.225,
0.23,0.235,0.24,0.245,0.25,0.255,0.26,0.265,0.27,0.275,0.28,0.285,0.29,
0.295,0.3,0.305,0.31,0.315,0.32,0.325,0.33,0.335,0.34,0.345,0.35,0.355,
0.36,0.365,0.37,0.375,0.38,0.385,0.39,0.395,0.4,0.405,0.41,0.415,0.42,0.425,
0.43,0.435,0.44,0.445,0.45,0.455,0.46,0.465,0.47,0.475,0.48,0.485,0.49,
0.495,0.5,0.505,0.51,0.515,0.52,0.525,0.53,0.535,0.54,0.545,0.55,0.555,
0.56,0.565,0.57,0.575,0.58,0.585,0.59,0.595,0.6,0.605,0.61,0.615,0.62,0.625,
0.63,0.635,0.64,0.645,0.65,0.655,0.66,0.665,0.67,0.675,0.68,0.685,0.690000000000001,
0.695000000000001,0.700000000000001,0.705000000000001,0.710000000000001,
0.715000000000001,0.720000000000001,0.725000000000001,0.730000000000001,
0.735000000000001,0.740000000000001,0.745000000000001,0.750000000000001,
0.755000000000001,0.760000000000001,0.765000000000001,0.770000000000001,
0.775000000000001,0.780000000000001,0.785000000000001,0.790000000000001,
0.795000000000001,0.800000000000001,0.805000000000001,0.810000000000001,
0.815000000000001,0.820000000000001,0.825000000000001,0.830000000000001,
0.835000000000001,0.840000000000001,0.845000000000001,0.850000000000001,
0.855000000000001,0.860000000000001,0.865000000000001,0.870000000000001,
0.875000000000001,0.880000000000001,0.885000000000001,0.890000000000001,
0.895000000000001,0.900000000000001,0.905000000000001,0.910000000000001,
0.915000000000001,0.920000000000001,0.925000000000001,0.930000000000001,
0.935000000000001,0.940000000000001,0.9414298444381),.UNSPECIFIED.)
CURVE()
GEOMETRIC_REPRESENTATION_ITEM()
RATIONAL_B_SPLINE_CURVE((1.,1.,1.,1.,1.,1.,1.,1.,1.,1.,1.,1.,1.,1.,1.,1.,
1.,1.,1.,1.,1.,1.,1.,1.,1.,1.,1.,1.,1.,1.,1.,1.,1.,1.,1.,1.,1.,1.,1.,1.,
1.,1.,1.,1.,1.,1.,1.,1.,1.,1.,1.,1.,1.,1.,1.,1.,1.,1.,1.,1.,1.,1.,1.,1.,
1.,1.,1.,1.,1.,1.,1.,1.,1.,1.,1.,1.,1.,1.,1.,1.,1.,1.,1.,1.,1.,1.,1.,1.,
1.,1.,1.,1.,1.,1.,1.,1.,1.,1.,1.,1.,1.,1.,1.,1.,1.,1.,1.,1.,1.,1.,1.,1.,
1.,1.,1.,1.,1.,1.,1.,1.,1.,1.,1.,1.,1.,1.,1.,1.,1.,1.,1.,1.,1.,1.,1.,1.,
1.,1.,1.,1.,1.,1.,1.,1.,1.,1.,1.,1.,1.,1.,1.,1.,1.,1.,1.,1.,1.,1.,1.,1.,
1.,1.,1.,1.,1.,1.,1.,1.,1.,1.,1.,1.,1.,1.,1.,1.,1.,1.,1.,1.,1.,1.,1.,1.,
1.,1.,1.,1.,1.,1.,1.,1.,1.,1.))
REPRESENTATION_ITEM('')
);
#548=(
BOUNDED_CURVE()
B_SPLINE_CURVE(5,(#117600,#117601,#117602,#117603,#117604,#117605,#117606,
#117607,#117608,#117609,#117610,#117611,#117612,#117613,#117614,#117615,
#117616,#117617,#117618,#117619,#117620,#117621,#117622,#117623,#117624,
#117625,#117626,#117627,#117628,#117629,#117630,#117631,#117632,#117633,
#117634,#117635,#117636,#117637,#117638,#117639,#117640,#117641,#117642,
#117643,#117644,#117645,#117646,#117647,#117648,#117649,#117650,#117651,
#117652,#117653,#117654,#117655,#117656,#117657,#117658,#117659,#117660,
#117661,#117662,#117663,#117664,#117665,#117666,#117667,#117668,#117669,
#117670,#117671,#117672,#117673,#117674,#117675,#117676,#117677,#117678,
#117679,#117680,#117681,#117682,#117683,#117684,#117685,#117686,#117687,
#117688,#117689,#117690,#117691,#117692,#117693,#117694,#117695,#117696,
#117697,#117698,#117699,#117700,#117701,#117702,#117703,#117704,#117705,
#117706,#117707,#117708,#117709,#117710,#117711,#117712,#117713,#117714,
#117715,#117716,#117717,#117718,#117719,#117720,#117721,#117722,#117723,
#117724,#117725,#117726,#117727,#117728,#117729,#117730,#117731,#117732,
#117733,#117734,#117735,#117736,#117737,#117738,#117739,#117740,#117741,
#117742,#117743,#117744,#117745,#117746,#117747,#117748,#117749,#117750,
#117751,#117752,#117753,#117754,#117755,#117756,#117757,#117758,#117759,
#117760,#117761,#117762,#117763,#117764,#117765,#117766,#117767,#117768,
#117769,#117770,#117771,#117772,#117773,#117774,#117775,#117776,#117777,
#117778,#117779,#117780,#117781,#117782,#117783,#117784,#117785,#117786,
#117787,#117788,#117789,#117790,#117791,#117792,#117793),.UNSPECIFIED.,
 .F.,.F.)
B_SPLINE_CURVE_WITH_KNOTS((6,1,1,1,1,1,1,1,1,1,1,1,1,1,1,1,1,1,1,1,1,1,
1,1,1,1,1,1,1,1,1,1,1,1,1,1,1,1,1,1,1,1,1,1,1,1,1,1,1,1,1,1,1,1,1,1,1,1,
1,1,1,1,1,1,1,1,1,1,1,1,1,1,1,1,1,1,1,1,1,1,1,1,1,1,1,1,1,1,1,1,1,1,1,1,
1,1,1,1,1,1,1,1,1,1,1,1,1,1,1,1,1,1,1,1,1,1,1,1,1,1,1,1,1,1,1,1,1,1,1,1,
1,1,1,1,1,1,1,1,1,1,1,1,1,1,1,1,1,1,1,1,1,1,1,1,1,1,1,1,1,1,1,1,1,1,1,1,
1,1,1,1,1,1,1,1,1,1,1,1,1,1,1,1,1,1,1,1,1,1,1,6),(-0.941429844438093,-0.940000000000001,
-0.935000000000001,-0.930000000000001,-0.925000000000001,-0.920000000000001,
-0.915000000000001,-0.910000000000001,-0.905000000000001,-0.900000000000001,
-0.895000000000001,-0.890000000000001,-0.885000000000001,-0.880000000000001,
-0.875000000000001,-0.870000000000001,-0.865000000000001,-0.860000000000001,
-0.855000000000001,-0.850000000000001,-0.845000000000001,-0.840000000000001,
-0.835000000000001,-0.830000000000001,-0.825000000000001,-0.820000000000001,
-0.815000000000001,-0.810000000000001,-0.805000000000001,-0.800000000000001,
-0.795000000000001,-0.790000000000001,-0.785000000000001,-0.780000000000001,
-0.775000000000001,-0.770000000000001,-0.765000000000001,-0.760000000000001,
-0.755000000000001,-0.750000000000001,-0.745000000000001,-0.740000000000001,
-0.735000000000001,-0.730000000000001,-0.725000000000001,-0.720000000000001,
-0.715000000000001,-0.710000000000001,-0.705000000000001,-0.700000000000001,
-0.695000000000001,-0.690000000000001,-0.685,-0.68,-0.675,-0.67,-0.665,
-0.66,-0.655,-0.65,-0.645,-0.64,-0.635,-0.63,-0.625,-0.62,-0.615,-0.61,
-0.605,-0.6,-0.595,-0.59,-0.585,-0.58,-0.575,-0.57,-0.565,-0.56,-0.555,
-0.55,-0.545,-0.54,-0.535,-0.53,-0.525,-0.52,-0.515,-0.51,-0.505,-0.5,-0.495,
-0.49,-0.485,-0.48,-0.475,-0.47,-0.465,-0.46,-0.455,-0.45,-0.445,-0.44,
-0.435,-0.43,-0.425,-0.42,-0.415,-0.41,-0.405,-0.4,-0.395,-0.39,-0.385,
-0.38,-0.375,-0.37,-0.365,-0.36,-0.355,-0.35,-0.345,-0.34,-0.335,-0.33,
-0.325,-0.32,-0.315,-0.31,-0.305,-0.3,-0.295,-0.29,-0.285,-0.28,-0.275,
-0.27,-0.265,-0.26,-0.255,-0.25,-0.245,-0.24,-0.235,-0.23,-0.225,-0.22,
-0.215,-0.21,-0.205,-0.2,-0.195,-0.19,-0.185,-0.18,-0.175,-0.17,-0.165,
-0.16,-0.155,-0.15,-0.145,-0.14,-0.135,-0.13,-0.125,-0.12,-0.115,-0.11,
-0.105,-0.1,-0.095,-0.09,-0.085,-0.08,-0.075,-0.07,-0.065,-0.06,-0.055,
-0.05,-0.045,-0.04,-0.035,-0.03,-0.025,-0.02,-0.015,-0.01,-0.005,0.),
 .UNSPECIFIED.)
CURVE()
GEOMETRIC_REPRESENTATION_ITEM()
RATIONAL_B_SPLINE_CURVE((1.,1.,1.,1.,1.,1.,1.,1.,1.,1.,1.,1.,1.,1.,1.,1.,
1.,1.,1.,1.,1.,1.,1.,1.,1.,1.,1.,1.,1.,1.,1.,1.,1.,1.,1.,1.,1.,1.,1.,1.,
1.,1.,1.,1.,1.,1.,1.,1.,1.,1.,1.,1.,1.,1.,1.,1.,1.,1.,1.,1.,1.,1.,1.,1.,
1.,1.,1.,1.,1.,1.,1.,1.,1.,1.,1.,1.,1.,1.,1.,1.,1.,1.,1.,1.,1.,1.,1.,1.,
1.,1.,1.,1.,1.,1.,1.,1.,1.,1.,1.,1.,1.,1.,1.,1.,1.,1.,1.,1.,1.,1.,1.,1.,
1.,1.,1.,1.,1.,1.,1.,1.,1.,1.,1.,1.,1.,1.,1.,1.,1.,1.,1.,1.,1.,1.,1.,1.,
1.,1.,1.,1.,1.,1.,1.,1.,1.,1.,1.,1.,1.,1.,1.,1.,1.,1.,1.,1.,1.,1.,1.,1.,
1.,1.,1.,1.,1.,1.,1.,1.,1.,1.,1.,1.,1.,1.,1.,1.,1.,1.,1.,1.,1.,1.,1.,1.,
1.,1.,1.,1.,1.,1.,1.,1.,1.,1.))
REPRESENTATION_ITEM('')
);
#549=(
BOUNDED_CURVE()
B_SPLINE_CURVE(5,(#118205,#118206,#118207,#118208,#118209,#118210,#118211,
#118212,#118213,#118214,#118215,#118216,#118217,#118218,#118219,#118220,
#118221,#118222,#118223,#118224,#118225,#118226,#118227,#118228,#118229,
#118230,#118231,#118232,#118233,#118234,#118235,#118236,#118237,#118238,
#118239,#118240,#118241,#118242,#118243,#118244,#118245,#118246,#118247,
#118248,#118249,#118250,#118251,#118252,#118253,#118254,#118255,#118256,
#118257,#118258,#118259,#118260,#118261,#118262,#118263,#118264,#118265,
#118266,#118267,#118268,#118269,#118270,#118271,#118272,#118273,#118274,
#118275,#118276,#118277,#118278,#118279,#118280,#118281,#118282,#118283,
#118284,#118285,#118286,#118287,#118288,#118289,#118290,#118291,#118292,
#118293,#118294,#118295,#118296,#118297,#118298,#118299,#118300,#118301,
#118302,#118303,#118304,#118305,#118306,#118307,#118308,#118309,#118310,
#118311,#118312,#118313,#118314,#118315,#118316,#118317,#118318,#118319,
#118320,#118321,#118322,#118323,#118324,#118325,#118326,#118327,#118328,
#118329,#118330,#118331,#118332,#118333,#118334,#118335,#118336,#118337,
#118338,#118339,#118340,#118341,#118342,#118343,#118344,#118345,#118346,
#118347,#118348,#118349,#118350,#118351,#118352,#118353,#118354,#118355,
#118356,#118357,#118358,#118359,#118360,#118361,#118362,#118363,#118364,
#118365,#118366,#118367,#118368,#118369,#118370,#118371,#118372,#118373,
#118374,#118375,#118376,#118377,#118378,#118379,#118380,#118381,#118382,
#118383,#118384,#118385,#118386,#118387,#118388,#118389,#118390,#118391,
#118392,#118393,#118394,#118395,#118396,#118397,#118398),.UNSPECIFIED.,
 .F.,.F.)
B_SPLINE_CURVE_WITH_KNOTS((6,1,1,1,1,1,1,1,1,1,1,1,1,1,1,1,1,1,1,1,1,1,
1,1,1,1,1,1,1,1,1,1,1,1,1,1,1,1,1,1,1,1,1,1,1,1,1,1,1,1,1,1,1,1,1,1,1,1,
1,1,1,1,1,1,1,1,1,1,1,1,1,1,1,1,1,1,1,1,1,1,1,1,1,1,1,1,1,1,1,1,1,1,1,1,
1,1,1,1,1,1,1,1,1,1,1,1,1,1,1,1,1,1,1,1,1,1,1,1,1,1,1,1,1,1,1,1,1,1,1,1,
1,1,1,1,1,1,1,1,1,1,1,1,1,1,1,1,1,1,1,1,1,1,1,1,1,1,1,1,1,1,1,1,1,1,1,1,
1,1,1,1,1,1,1,1,1,1,1,1,1,1,1,1,1,1,1,1,1,1,1,6),(0.,0.005,0.01,0.015,0.02,
0.025,0.03,0.035,0.04,0.045,0.05,0.055,0.06,0.065,0.07,0.075,0.08,0.085,
0.09,0.095,0.1,0.105,0.11,0.115,0.12,0.125,0.13,0.135,0.14,0.145,0.15,0.155,
0.16,0.165,0.17,0.175,0.18,0.185,0.19,0.195,0.2,0.205,0.21,0.215,0.22,0.225,
0.23,0.235,0.24,0.245,0.25,0.255,0.26,0.265,0.27,0.275,0.28,0.285,0.29,
0.295,0.3,0.305,0.31,0.315,0.32,0.325,0.33,0.335,0.34,0.345,0.35,0.355,
0.36,0.365,0.37,0.375,0.38,0.385,0.39,0.395,0.4,0.405,0.41,0.415,0.42,0.425,
0.43,0.435,0.44,0.445,0.45,0.455,0.46,0.465,0.47,0.475,0.48,0.485,0.49,
0.495,0.5,0.505,0.51,0.515,0.52,0.525,0.53,0.535,0.54,0.545,0.55,0.555,
0.56,0.565,0.57,0.575,0.58,0.585,0.59,0.595,0.6,0.605,0.61,0.615,0.62,0.625,
0.63,0.635,0.64,0.645,0.65,0.655,0.66,0.665,0.67,0.675,0.68,0.685,0.690000000000001,
0.695000000000001,0.700000000000001,0.705000000000001,0.710000000000001,
0.715000000000001,0.720000000000001,0.725000000000001,0.730000000000001,
0.735000000000001,0.740000000000001,0.745000000000001,0.750000000000001,
0.755000000000001,0.760000000000001,0.765000000000001,0.770000000000001,
0.775000000000001,0.780000000000001,0.785000000000001,0.790000000000001,
0.795000000000001,0.800000000000001,0.805000000000001,0.810000000000001,
0.815000000000001,0.820000000000001,0.825000000000001,0.830000000000001,
0.835000000000001,0.840000000000001,0.845000000000001,0.850000000000001,
0.855000000000001,0.860000000000001,0.865000000000001,0.870000000000001,
0.875000000000001,0.880000000000001,0.885000000000001,0.890000000000001,
0.895000000000001,0.900000000000001,0.905000000000001,0.910000000000001,
0.915000000000001,0.920000000000001,0.925000000000001,0.930000000000001,
0.935000000000001,0.940000000000001,0.941429844438101),.UNSPECIFIED.)
CURVE()
GEOMETRIC_REPRESENTATION_ITEM()
RATIONAL_B_SPLINE_CURVE((1.,1.,1.,1.,1.,1.,1.,1.,1.,1.,1.,1.,1.,1.,1.,1.,
1.,1.,1.,1.,1.,1.,1.,1.,1.,1.,1.,1.,1.,1.,1.,1.,1.,1.,1.,1.,1.,1.,1.,1.,
1.,1.,1.,1.,1.,1.,1.,1.,1.,1.,1.,1.,1.,1.,1.,1.,1.,1.,1.,1.,1.,1.,1.,1.,
1.,1.,1.,1.,1.,1.,1.,1.,1.,1.,1.,1.,1.,1.,1.,1.,1.,1.,1.,1.,1.,1.,1.,1.,
1.,1.,1.,1.,1.,1.,1.,1.,1.,1.,1.,1.,1.,1.,1.,1.,1.,1.,1.,1.,1.,1.,1.,1.,
1.,1.,1.,1.,1.,1.,1.,1.,1.,1.,1.,1.,1.,1.,1.,1.,1.,1.,1.,1.,1.,1.,1.,1.,
1.,1.,1.,1.,1.,1.,1.,1.,1.,1.,1.,1.,1.,1.,1.,1.,1.,1.,1.,1.,1.,1.,1.,1.,
1.,1.,1.,1.,1.,1.,1.,1.,1.,1.,1.,1.,1.,1.,1.,1.,1.,1.,1.,1.,1.,1.,1.,1.,
1.,1.,1.,1.,1.,1.,1.,1.,1.,1.))
REPRESENTATION_ITEM('')
);
#550=(
BOUNDED_CURVE()
B_SPLINE_CURVE(5,(#118401,#118402,#118403,#118404,#118405,#118406,#118407,
#118408,#118409,#118410,#118411,#118412,#118413,#118414,#118415,#118416,
#118417,#118418,#118419,#118420,#118421,#118422,#118423,#118424,#118425,
#118426,#118427,#118428,#118429,#118430,#118431,#118432,#118433,#118434,
#118435,#118436,#118437,#118438,#118439,#118440,#118441,#118442,#118443,
#118444,#118445,#118446,#118447,#118448,#118449,#118450,#118451,#118452,
#118453,#118454,#118455,#118456,#118457,#118458,#118459,#118460,#118461,
#118462,#118463,#118464,#118465,#118466,#118467,#118468,#118469,#118470,
#118471,#118472,#118473,#118474,#118475,#118476,#118477,#118478,#118479,
#118480,#118481,#118482,#118483,#118484,#118485,#118486,#118487,#118488,
#118489,#118490,#118491,#118492,#118493,#118494,#118495,#118496,#118497,
#118498,#118499,#118500,#118501,#118502,#118503,#118504,#118505,#118506,
#118507,#118508,#118509,#118510,#118511,#118512,#118513,#118514,#118515,
#118516,#118517,#118518,#118519,#118520,#118521,#118522,#118523,#118524,
#118525,#118526,#118527,#118528,#118529,#118530,#118531,#118532,#118533,
#118534,#118535,#118536,#118537,#118538,#118539,#118540,#118541,#118542,
#118543,#118544,#118545,#118546,#118547,#118548,#118549,#118550,#118551,
#118552,#118553,#118554,#118555,#118556,#118557,#118558,#118559,#118560,
#118561,#118562,#118563,#118564,#118565,#118566,#118567,#118568,#118569,
#118570,#118571,#118572,#118573,#118574,#118575,#118576,#118577,#118578,
#118579,#118580,#118581,#118582,#118583,#118584,#118585,#118586,#118587,
#118588,#118589,#118590,#118591,#118592,#118593,#118594),.UNSPECIFIED.,
 .F.,.F.)
B_SPLINE_CURVE_WITH_KNOTS((6,1,1,1,1,1,1,1,1,1,1,1,1,1,1,1,1,1,1,1,1,1,
1,1,1,1,1,1,1,1,1,1,1,1,1,1,1,1,1,1,1,1,1,1,1,1,1,1,1,1,1,1,1,1,1,1,1,1,
1,1,1,1,1,1,1,1,1,1,1,1,1,1,1,1,1,1,1,1,1,1,1,1,1,1,1,1,1,1,1,1,1,1,1,1,
1,1,1,1,1,1,1,1,1,1,1,1,1,1,1,1,1,1,1,1,1,1,1,1,1,1,1,1,1,1,1,1,1,1,1,1,
1,1,1,1,1,1,1,1,1,1,1,1,1,1,1,1,1,1,1,1,1,1,1,1,1,1,1,1,1,1,1,1,1,1,1,1,
1,1,1,1,1,1,1,1,1,1,1,1,1,1,1,1,1,1,1,1,1,1,1,6),(-0.941429844438086,-0.940000000000001,
-0.935000000000001,-0.930000000000001,-0.925000000000001,-0.920000000000001,
-0.915000000000001,-0.910000000000001,-0.905000000000001,-0.900000000000001,
-0.895000000000001,-0.890000000000001,-0.885000000000001,-0.880000000000001,
-0.875000000000001,-0.870000000000001,-0.865000000000001,-0.860000000000001,
-0.855000000000001,-0.850000000000001,-0.845000000000001,-0.840000000000001,
-0.835000000000001,-0.830000000000001,-0.825000000000001,-0.820000000000001,
-0.815000000000001,-0.810000000000001,-0.805000000000001,-0.800000000000001,
-0.795000000000001,-0.790000000000001,-0.785000000000001,-0.780000000000001,
-0.775000000000001,-0.770000000000001,-0.765000000000001,-0.760000000000001,
-0.755000000000001,-0.750000000000001,-0.745000000000001,-0.740000000000001,
-0.735000000000001,-0.730000000000001,-0.725000000000001,-0.720000000000001,
-0.715000000000001,-0.710000000000001,-0.705000000000001,-0.700000000000001,
-0.695000000000001,-0.690000000000001,-0.685,-0.68,-0.675,-0.67,-0.665,
-0.66,-0.655,-0.65,-0.645,-0.64,-0.635,-0.63,-0.625,-0.62,-0.615,-0.61,
-0.605,-0.6,-0.595,-0.59,-0.585,-0.58,-0.575,-0.57,-0.565,-0.56,-0.555,
-0.55,-0.545,-0.54,-0.535,-0.53,-0.525,-0.52,-0.515,-0.51,-0.505,-0.5,-0.495,
-0.49,-0.485,-0.48,-0.475,-0.47,-0.465,-0.46,-0.455,-0.45,-0.445,-0.44,
-0.435,-0.43,-0.425,-0.42,-0.415,-0.41,-0.405,-0.4,-0.395,-0.39,-0.385,
-0.38,-0.375,-0.37,-0.365,-0.36,-0.355,-0.35,-0.345,-0.34,-0.335,-0.33,
-0.325,-0.32,-0.315,-0.31,-0.305,-0.3,-0.295,-0.29,-0.285,-0.28,-0.275,
-0.27,-0.265,-0.26,-0.255,-0.25,-0.245,-0.24,-0.235,-0.23,-0.225,-0.22,
-0.215,-0.21,-0.205,-0.2,-0.195,-0.19,-0.185,-0.18,-0.175,-0.17,-0.165,
-0.16,-0.155,-0.15,-0.145,-0.14,-0.135,-0.13,-0.125,-0.12,-0.115,-0.11,
-0.105,-0.1,-0.095,-0.09,-0.085,-0.08,-0.075,-0.07,-0.065,-0.06,-0.055,
-0.05,-0.045,-0.04,-0.035,-0.03,-0.025,-0.02,-0.015,-0.01,-0.005,0.),
 .UNSPECIFIED.)
CURVE()
GEOMETRIC_REPRESENTATION_ITEM()
RATIONAL_B_SPLINE_CURVE((1.,1.,1.,1.,1.,1.,1.,1.,1.,1.,1.,1.,1.,1.,1.,1.,
1.,1.,1.,1.,1.,1.,1.,1.,1.,1.,1.,1.,1.,1.,1.,1.,1.,1.,1.,1.,1.,1.,1.,1.,
1.,1.,1.,1.,1.,1.,1.,1.,1.,1.,1.,1.,1.,1.,1.,1.,1.,1.,1.,1.,1.,1.,1.,1.,
1.,1.,1.,1.,1.,1.,1.,1.,1.,1.,1.,1.,1.,1.,1.,1.,1.,1.,1.,1.,1.,1.,1.,1.,
1.,1.,1.,1.,1.,1.,1.,1.,1.,1.,1.,1.,1.,1.,1.,1.,1.,1.,1.,1.,1.,1.,1.,1.,
1.,1.,1.,1.,1.,1.,1.,1.,1.,1.,1.,1.,1.,1.,1.,1.,1.,1.,1.,1.,1.,1.,1.,1.,
1.,1.,1.,1.,1.,1.,1.,1.,1.,1.,1.,1.,1.,1.,1.,1.,1.,1.,1.,1.,1.,1.,1.,1.,
1.,1.,1.,1.,1.,1.,1.,1.,1.,1.,1.,1.,1.,1.,1.,1.,1.,1.,1.,1.,1.,1.,1.,1.,
1.,1.,1.,1.,1.,1.,1.,1.,1.,1.))
REPRESENTATION_ITEM('')
);
#551=(
BOUNDED_CURVE()
B_SPLINE_CURVE(5,(#119006,#119007,#119008,#119009,#119010,#119011,#119012,
#119013,#119014,#119015,#119016,#119017,#119018,#119019,#119020,#119021,
#119022,#119023,#119024,#119025,#119026,#119027,#119028,#119029,#119030,
#119031,#119032,#119033,#119034,#119035,#119036,#119037,#119038,#119039,
#119040,#119041,#119042,#119043,#119044,#119045,#119046,#119047,#119048,
#119049,#119050,#119051,#119052,#119053,#119054,#119055,#119056,#119057,
#119058,#119059,#119060,#119061,#119062,#119063,#119064,#119065,#119066,
#119067,#119068,#119069,#119070,#119071,#119072,#119073,#119074,#119075,
#119076,#119077,#119078,#119079,#119080,#119081,#119082,#119083,#119084,
#119085,#119086,#119087,#119088,#119089,#119090,#119091,#119092,#119093,
#119094,#119095,#119096,#119097,#119098,#119099,#119100,#119101,#119102,
#119103,#119104,#119105,#119106,#119107,#119108,#119109,#119110,#119111,
#119112,#119113,#119114,#119115,#119116,#119117,#119118,#119119,#119120,
#119121,#119122,#119123,#119124,#119125,#119126,#119127,#119128,#119129,
#119130,#119131,#119132,#119133,#119134,#119135,#119136,#119137,#119138,
#119139,#119140,#119141,#119142,#119143,#119144,#119145,#119146,#119147,
#119148,#119149,#119150,#119151,#119152,#119153,#119154,#119155,#119156,
#119157,#119158,#119159,#119160,#119161,#119162,#119163,#119164,#119165,
#119166,#119167,#119168,#119169,#119170,#119171,#119172,#119173,#119174,
#119175,#119176,#119177,#119178,#119179,#119180,#119181,#119182,#119183,
#119184,#119185,#119186,#119187,#119188,#119189,#119190,#119191,#119192,
#119193,#119194,#119195,#119196,#119197,#119198,#119199),.UNSPECIFIED.,
 .F.,.F.)
B_SPLINE_CURVE_WITH_KNOTS((6,1,1,1,1,1,1,1,1,1,1,1,1,1,1,1,1,1,1,1,1,1,
1,1,1,1,1,1,1,1,1,1,1,1,1,1,1,1,1,1,1,1,1,1,1,1,1,1,1,1,1,1,1,1,1,1,1,1,
1,1,1,1,1,1,1,1,1,1,1,1,1,1,1,1,1,1,1,1,1,1,1,1,1,1,1,1,1,1,1,1,1,1,1,1,
1,1,1,1,1,1,1,1,1,1,1,1,1,1,1,1,1,1,1,1,1,1,1,1,1,1,1,1,1,1,1,1,1,1,1,1,
1,1,1,1,1,1,1,1,1,1,1,1,1,1,1,1,1,1,1,1,1,1,1,1,1,1,1,1,1,1,1,1,1,1,1,1,
1,1,1,1,1,1,1,1,1,1,1,1,1,1,1,1,1,1,1,1,1,1,1,6),(0.,0.005,0.01,0.015,0.02,
0.025,0.03,0.035,0.04,0.045,0.05,0.055,0.06,0.065,0.07,0.075,0.08,0.085,
0.09,0.095,0.1,0.105,0.11,0.115,0.12,0.125,0.13,0.135,0.14,0.145,0.15,0.155,
0.16,0.165,0.17,0.175,0.18,0.185,0.19,0.195,0.2,0.205,0.21,0.215,0.22,0.225,
0.23,0.235,0.24,0.245,0.25,0.255,0.26,0.265,0.27,0.275,0.28,0.285,0.29,
0.295,0.3,0.305,0.31,0.315,0.32,0.325,0.33,0.335,0.34,0.345,0.35,0.355,
0.36,0.365,0.37,0.375,0.38,0.385,0.39,0.395,0.4,0.405,0.41,0.415,0.42,0.425,
0.43,0.435,0.44,0.445,0.45,0.455,0.46,0.465,0.47,0.475,0.48,0.485,0.49,
0.495,0.5,0.505,0.51,0.515,0.52,0.525,0.53,0.535,0.54,0.545,0.55,0.555,
0.56,0.565,0.57,0.575,0.58,0.585,0.59,0.595,0.6,0.605,0.61,0.615,0.62,0.625,
0.63,0.635,0.64,0.645,0.65,0.655,0.66,0.665,0.67,0.675,0.68,0.685,0.690000000000001,
0.695000000000001,0.700000000000001,0.705000000000001,0.710000000000001,
0.715000000000001,0.720000000000001,0.725000000000001,0.730000000000001,
0.735000000000001,0.740000000000001,0.745000000000001,0.750000000000001,
0.755000000000001,0.760000000000001,0.765000000000001,0.770000000000001,
0.775000000000001,0.780000000000001,0.785000000000001,0.790000000000001,
0.795000000000001,0.800000000000001,0.805000000000001,0.810000000000001,
0.815000000000001,0.820000000000001,0.825000000000001,0.830000000000001,
0.835000000000001,0.840000000000001,0.845000000000001,0.850000000000001,
0.855000000000001,0.860000000000001,0.865000000000001,0.870000000000001,
0.875000000000001,0.880000000000001,0.885000000000001,0.890000000000001,
0.895000000000001,0.900000000000001,0.905000000000001,0.910000000000001,
0.915000000000001,0.920000000000001,0.925000000000001,0.930000000000001,
0.935000000000001,0.940000000000001,0.941429844438003),.UNSPECIFIED.)
CURVE()
GEOMETRIC_REPRESENTATION_ITEM()
RATIONAL_B_SPLINE_CURVE((1.,1.,1.,1.,1.,1.,1.,1.,1.,1.,1.,1.,1.,1.,1.,1.,
1.,1.,1.,1.,1.,1.,1.,1.,1.,1.,1.,1.,1.,1.,1.,1.,1.,1.,1.,1.,1.,1.,1.,1.,
1.,1.,1.,1.,1.,1.,1.,1.,1.,1.,1.,1.,1.,1.,1.,1.,1.,1.,1.,1.,1.,1.,1.,1.,
1.,1.,1.,1.,1.,1.,1.,1.,1.,1.,1.,1.,1.,1.,1.,1.,1.,1.,1.,1.,1.,1.,1.,1.,
1.,1.,1.,1.,1.,1.,1.,1.,1.,1.,1.,1.,1.,1.,1.,1.,1.,1.,1.,1.,1.,1.,1.,1.,
1.,1.,1.,1.,1.,1.,1.,1.,1.,1.,1.,1.,1.,1.,1.,1.,1.,1.,1.,1.,1.,1.,1.,1.,
1.,1.,1.,1.,1.,1.,1.,1.,1.,1.,1.,1.,1.,1.,1.,1.,1.,1.,1.,1.,1.,1.,1.,1.,
1.,1.,1.,1.,1.,1.,1.,1.,1.,1.,1.,1.,1.,1.,1.,1.,1.,1.,1.,1.,1.,1.,1.,1.,
1.,1.,1.,1.,1.,1.,1.,1.,1.,1.))
REPRESENTATION_ITEM('')
);
#552=(
BOUNDED_CURVE()
B_SPLINE_CURVE(5,(#119202,#119203,#119204,#119205,#119206,#119207,#119208,
#119209,#119210,#119211,#119212,#119213,#119214,#119215,#119216,#119217,
#119218,#119219,#119220,#119221,#119222,#119223,#119224,#119225,#119226,
#119227,#119228,#119229,#119230,#119231,#119232,#119233,#119234,#119235,
#119236,#119237,#119238,#119239,#119240,#119241,#119242,#119243,#119244,
#119245,#119246,#119247,#119248,#119249,#119250,#119251,#119252,#119253,
#119254,#119255,#119256,#119257,#119258,#119259,#119260,#119261,#119262,
#119263,#119264,#119265,#119266,#119267,#119268,#119269,#119270,#119271,
#119272,#119273,#119274,#119275,#119276,#119277,#119278,#119279,#119280,
#119281,#119282,#119283,#119284,#119285,#119286,#119287,#119288,#119289,
#119290,#119291,#119292,#119293,#119294,#119295,#119296,#119297,#119298,
#119299,#119300,#119301,#119302,#119303,#119304,#119305,#119306,#119307,
#119308,#119309,#119310,#119311,#119312,#119313,#119314,#119315,#119316,
#119317,#119318,#119319,#119320,#119321,#119322,#119323,#119324,#119325,
#119326,#119327,#119328,#119329,#119330,#119331,#119332,#119333,#119334,
#119335,#119336,#119337,#119338,#119339,#119340,#119341,#119342,#119343,
#119344,#119345,#119346,#119347,#119348,#119349,#119350,#119351,#119352,
#119353,#119354,#119355,#119356,#119357,#119358,#119359,#119360,#119361,
#119362,#119363,#119364,#119365,#119366,#119367,#119368,#119369,#119370,
#119371,#119372,#119373,#119374,#119375,#119376,#119377,#119378,#119379,
#119380,#119381,#119382,#119383,#119384,#119385,#119386,#119387,#119388,
#119389,#119390,#119391,#119392,#119393,#119394,#119395),.UNSPECIFIED.,
 .F.,.F.)
B_SPLINE_CURVE_WITH_KNOTS((6,1,1,1,1,1,1,1,1,1,1,1,1,1,1,1,1,1,1,1,1,1,
1,1,1,1,1,1,1,1,1,1,1,1,1,1,1,1,1,1,1,1,1,1,1,1,1,1,1,1,1,1,1,1,1,1,1,1,
1,1,1,1,1,1,1,1,1,1,1,1,1,1,1,1,1,1,1,1,1,1,1,1,1,1,1,1,1,1,1,1,1,1,1,1,
1,1,1,1,1,1,1,1,1,1,1,1,1,1,1,1,1,1,1,1,1,1,1,1,1,1,1,1,1,1,1,1,1,1,1,1,
1,1,1,1,1,1,1,1,1,1,1,1,1,1,1,1,1,1,1,1,1,1,1,1,1,1,1,1,1,1,1,1,1,1,1,1,
1,1,1,1,1,1,1,1,1,1,1,1,1,1,1,1,1,1,1,1,1,1,1,6),(-0.941429844438003,-0.940000000000001,
-0.935000000000001,-0.930000000000001,-0.925000000000001,-0.920000000000001,
-0.915000000000001,-0.910000000000001,-0.905000000000001,-0.900000000000001,
-0.895000000000001,-0.890000000000001,-0.885000000000001,-0.880000000000001,
-0.875000000000001,-0.870000000000001,-0.865000000000001,-0.860000000000001,
-0.855000000000001,-0.850000000000001,-0.845000000000001,-0.840000000000001,
-0.835000000000001,-0.830000000000001,-0.825000000000001,-0.820000000000001,
-0.815000000000001,-0.810000000000001,-0.805000000000001,-0.800000000000001,
-0.795000000000001,-0.790000000000001,-0.785000000000001,-0.780000000000001,
-0.775000000000001,-0.770000000000001,-0.765000000000001,-0.760000000000001,
-0.755000000000001,-0.750000000000001,-0.745000000000001,-0.740000000000001,
-0.735000000000001,-0.730000000000001,-0.725000000000001,-0.720000000000001,
-0.715000000000001,-0.710000000000001,-0.705000000000001,-0.700000000000001,
-0.695000000000001,-0.690000000000001,-0.685,-0.68,-0.675,-0.67,-0.665,
-0.66,-0.655,-0.65,-0.645,-0.64,-0.635,-0.63,-0.625,-0.62,-0.615,-0.61,
-0.605,-0.6,-0.595,-0.59,-0.585,-0.58,-0.575,-0.57,-0.565,-0.56,-0.555,
-0.55,-0.545,-0.54,-0.535,-0.53,-0.525,-0.52,-0.515,-0.51,-0.505,-0.5,-0.495,
-0.49,-0.485,-0.48,-0.475,-0.47,-0.465,-0.46,-0.455,-0.45,-0.445,-0.44,
-0.435,-0.43,-0.425,-0.42,-0.415,-0.41,-0.405,-0.4,-0.395,-0.39,-0.385,
-0.38,-0.375,-0.37,-0.365,-0.36,-0.355,-0.35,-0.345,-0.34,-0.335,-0.33,
-0.325,-0.32,-0.315,-0.31,-0.305,-0.3,-0.295,-0.29,-0.285,-0.28,-0.275,
-0.27,-0.265,-0.26,-0.255,-0.25,-0.245,-0.24,-0.235,-0.23,-0.225,-0.22,
-0.215,-0.21,-0.205,-0.2,-0.195,-0.19,-0.185,-0.18,-0.175,-0.17,-0.165,
-0.16,-0.155,-0.15,-0.145,-0.14,-0.135,-0.13,-0.125,-0.12,-0.115,-0.11,
-0.105,-0.1,-0.095,-0.09,-0.085,-0.08,-0.075,-0.07,-0.065,-0.06,-0.055,
-0.05,-0.045,-0.04,-0.035,-0.03,-0.025,-0.02,-0.015,-0.01,-0.005,0.),
 .UNSPECIFIED.)
CURVE()
GEOMETRIC_REPRESENTATION_ITEM()
RATIONAL_B_SPLINE_CURVE((1.,1.,1.,1.,1.,1.,1.,1.,1.,1.,1.,1.,1.,1.,1.,1.,
1.,1.,1.,1.,1.,1.,1.,1.,1.,1.,1.,1.,1.,1.,1.,1.,1.,1.,1.,1.,1.,1.,1.,1.,
1.,1.,1.,1.,1.,1.,1.,1.,1.,1.,1.,1.,1.,1.,1.,1.,1.,1.,1.,1.,1.,1.,1.,1.,
1.,1.,1.,1.,1.,1.,1.,1.,1.,1.,1.,1.,1.,1.,1.,1.,1.,1.,1.,1.,1.,1.,1.,1.,
1.,1.,1.,1.,1.,1.,1.,1.,1.,1.,1.,1.,1.,1.,1.,1.,1.,1.,1.,1.,1.,1.,1.,1.,
1.,1.,1.,1.,1.,1.,1.,1.,1.,1.,1.,1.,1.,1.,1.,1.,1.,1.,1.,1.,1.,1.,1.,1.,
1.,1.,1.,1.,1.,1.,1.,1.,1.,1.,1.,1.,1.,1.,1.,1.,1.,1.,1.,1.,1.,1.,1.,1.,
1.,1.,1.,1.,1.,1.,1.,1.,1.,1.,1.,1.,1.,1.,1.,1.,1.,1.,1.,1.,1.,1.,1.,1.,
1.,1.,1.,1.,1.,1.,1.,1.,1.,1.))
REPRESENTATION_ITEM('')
);
#553=(
BOUNDED_CURVE()
B_SPLINE_CURVE(5,(#119807,#119808,#119809,#119810,#119811,#119812,#119813,
#119814,#119815,#119816,#119817,#119818,#119819,#119820,#119821,#119822,
#119823,#119824,#119825,#119826,#119827,#119828,#119829,#119830,#119831,
#119832,#119833,#119834,#119835,#119836,#119837,#119838,#119839,#119840,
#119841,#119842,#119843,#119844,#119845,#119846,#119847,#119848,#119849,
#119850,#119851,#119852,#119853,#119854,#119855,#119856,#119857,#119858,
#119859,#119860,#119861,#119862,#119863,#119864,#119865,#119866,#119867,
#119868,#119869,#119870,#119871,#119872,#119873,#119874,#119875,#119876,
#119877,#119878,#119879,#119880,#119881,#119882,#119883,#119884,#119885,
#119886,#119887,#119888,#119889,#119890,#119891,#119892,#119893,#119894,
#119895,#119896,#119897,#119898,#119899,#119900,#119901,#119902,#119903,
#119904,#119905,#119906,#119907,#119908,#119909,#119910,#119911,#119912,
#119913,#119914,#119915,#119916,#119917,#119918,#119919,#119920,#119921,
#119922,#119923,#119924,#119925,#119926,#119927,#119928,#119929,#119930,
#119931,#119932,#119933,#119934,#119935,#119936,#119937,#119938,#119939,
#119940,#119941,#119942,#119943,#119944,#119945,#119946,#119947,#119948,
#119949,#119950,#119951,#119952,#119953,#119954,#119955,#119956,#119957,
#119958,#119959,#119960,#119961,#119962,#119963,#119964,#119965,#119966,
#119967,#119968,#119969,#119970,#119971,#119972,#119973,#119974,#119975,
#119976,#119977,#119978,#119979,#119980,#119981,#119982,#119983,#119984,
#119985,#119986,#119987,#119988,#119989,#119990,#119991,#119992,#119993,
#119994,#119995,#119996,#119997,#119998,#119999,#120000),.UNSPECIFIED.,
 .F.,.F.)
B_SPLINE_CURVE_WITH_KNOTS((6,1,1,1,1,1,1,1,1,1,1,1,1,1,1,1,1,1,1,1,1,1,
1,1,1,1,1,1,1,1,1,1,1,1,1,1,1,1,1,1,1,1,1,1,1,1,1,1,1,1,1,1,1,1,1,1,1,1,
1,1,1,1,1,1,1,1,1,1,1,1,1,1,1,1,1,1,1,1,1,1,1,1,1,1,1,1,1,1,1,1,1,1,1,1,
1,1,1,1,1,1,1,1,1,1,1,1,1,1,1,1,1,1,1,1,1,1,1,1,1,1,1,1,1,1,1,1,1,1,1,1,
1,1,1,1,1,1,1,1,1,1,1,1,1,1,1,1,1,1,1,1,1,1,1,1,1,1,1,1,1,1,1,1,1,1,1,1,
1,1,1,1,1,1,1,1,1,1,1,1,1,1,1,1,1,1,1,1,1,1,1,6),(0.,0.005,0.01,0.015,0.02,
0.025,0.03,0.035,0.04,0.045,0.05,0.055,0.06,0.065,0.07,0.075,0.08,0.085,
0.09,0.095,0.1,0.105,0.11,0.115,0.12,0.125,0.13,0.135,0.14,0.145,0.15,0.155,
0.16,0.165,0.17,0.175,0.18,0.185,0.19,0.195,0.2,0.205,0.21,0.215,0.22,0.225,
0.23,0.235,0.24,0.245,0.25,0.255,0.26,0.265,0.27,0.275,0.28,0.285,0.29,
0.295,0.3,0.305,0.31,0.315,0.32,0.325,0.33,0.335,0.34,0.345,0.35,0.355,
0.36,0.365,0.37,0.375,0.38,0.385,0.39,0.395,0.4,0.405,0.41,0.415,0.42,0.425,
0.43,0.435,0.44,0.445,0.45,0.455,0.46,0.465,0.47,0.475,0.48,0.485,0.49,
0.495,0.5,0.505,0.51,0.515,0.52,0.525,0.53,0.535,0.54,0.545,0.55,0.555,
0.56,0.565,0.57,0.575,0.58,0.585,0.59,0.595,0.6,0.605,0.61,0.615,0.62,0.625,
0.63,0.635,0.64,0.645,0.65,0.655,0.66,0.665,0.67,0.675,0.68,0.685,0.690000000000001,
0.695000000000001,0.700000000000001,0.705000000000001,0.710000000000001,
0.715000000000001,0.720000000000001,0.725000000000001,0.730000000000001,
0.735000000000001,0.740000000000001,0.745000000000001,0.750000000000001,
0.755000000000001,0.760000000000001,0.765000000000001,0.770000000000001,
0.775000000000001,0.780000000000001,0.785000000000001,0.790000000000001,
0.795000000000001,0.800000000000001,0.805000000000001,0.810000000000001,
0.815000000000001,0.820000000000001,0.825000000000001,0.830000000000001,
0.835000000000001,0.840000000000001,0.845000000000001,0.850000000000001,
0.855000000000001,0.860000000000001,0.865000000000001,0.870000000000001,
0.875000000000001,0.880000000000001,0.885000000000001,0.890000000000001,
0.895000000000001,0.900000000000001,0.905000000000001,0.910000000000001,
0.915000000000001,0.920000000000001,0.925000000000001,0.930000000000001,
0.935000000000001,0.940000000000001,0.941429844437941),.UNSPECIFIED.)
CURVE()
GEOMETRIC_REPRESENTATION_ITEM()
RATIONAL_B_SPLINE_CURVE((1.,1.,1.,1.,1.,1.,1.,1.,1.,1.,1.,1.,1.,1.,1.,1.,
1.,1.,1.,1.,1.,1.,1.,1.,1.,1.,1.,1.,1.,1.,1.,1.,1.,1.,1.,1.,1.,1.,1.,1.,
1.,1.,1.,1.,1.,1.,1.,1.,1.,1.,1.,1.,1.,1.,1.,1.,1.,1.,1.,1.,1.,1.,1.,1.,
1.,1.,1.,1.,1.,1.,1.,1.,1.,1.,1.,1.,1.,1.,1.,1.,1.,1.,1.,1.,1.,1.,1.,1.,
1.,1.,1.,1.,1.,1.,1.,1.,1.,1.,1.,1.,1.,1.,1.,1.,1.,1.,1.,1.,1.,1.,1.,1.,
1.,1.,1.,1.,1.,1.,1.,1.,1.,1.,1.,1.,1.,1.,1.,1.,1.,1.,1.,1.,1.,1.,1.,1.,
1.,1.,1.,1.,1.,1.,1.,1.,1.,1.,1.,1.,1.,1.,1.,1.,1.,1.,1.,1.,1.,1.,1.,1.,
1.,1.,1.,1.,1.,1.,1.,1.,1.,1.,1.,1.,1.,1.,1.,1.,1.,1.,1.,1.,1.,1.,1.,1.,
1.,1.,1.,1.,1.,1.,1.,1.,1.,1.))
REPRESENTATION_ITEM('')
);
#554=(
BOUNDED_CURVE()
B_SPLINE_CURVE(5,(#120003,#120004,#120005,#120006,#120007,#120008,#120009,
#120010,#120011,#120012,#120013,#120014,#120015,#120016,#120017,#120018,
#120019,#120020,#120021,#120022,#120023,#120024,#120025,#120026,#120027,
#120028,#120029,#120030,#120031,#120032,#120033,#120034,#120035,#120036,
#120037,#120038,#120039,#120040,#120041,#120042,#120043,#120044,#120045,
#120046,#120047,#120048,#120049,#120050,#120051,#120052,#120053,#120054,
#120055,#120056,#120057,#120058,#120059,#120060,#120061,#120062,#120063,
#120064,#120065,#120066,#120067,#120068,#120069,#120070,#120071,#120072,
#120073,#120074,#120075,#120076,#120077,#120078,#120079,#120080,#120081,
#120082,#120083,#120084,#120085,#120086,#120087,#120088,#120089,#120090,
#120091,#120092,#120093,#120094,#120095,#120096,#120097,#120098,#120099,
#120100,#120101,#120102,#120103,#120104,#120105,#120106,#120107,#120108,
#120109,#120110,#120111,#120112,#120113,#120114,#120115,#120116,#120117,
#120118,#120119,#120120,#120121,#120122,#120123,#120124,#120125,#120126,
#120127,#120128,#120129,#120130,#120131,#120132,#120133,#120134,#120135,
#120136,#120137,#120138,#120139,#120140,#120141,#120142,#120143,#120144,
#120145,#120146,#120147,#120148,#120149,#120150,#120151,#120152,#120153,
#120154,#120155,#120156,#120157,#120158,#120159,#120160,#120161,#120162,
#120163,#120164,#120165,#120166,#120167,#120168,#120169,#120170,#120171,
#120172,#120173,#120174,#120175,#120176,#120177,#120178,#120179,#120180,
#120181,#120182,#120183,#120184,#120185,#120186,#120187,#120188,#120189,
#120190,#120191,#120192,#120193,#120194,#120195,#120196),.UNSPECIFIED.,
 .F.,.F.)
B_SPLINE_CURVE_WITH_KNOTS((6,1,1,1,1,1,1,1,1,1,1,1,1,1,1,1,1,1,1,1,1,1,
1,1,1,1,1,1,1,1,1,1,1,1,1,1,1,1,1,1,1,1,1,1,1,1,1,1,1,1,1,1,1,1,1,1,1,1,
1,1,1,1,1,1,1,1,1,1,1,1,1,1,1,1,1,1,1,1,1,1,1,1,1,1,1,1,1,1,1,1,1,1,1,1,
1,1,1,1,1,1,1,1,1,1,1,1,1,1,1,1,1,1,1,1,1,1,1,1,1,1,1,1,1,1,1,1,1,1,1,1,
1,1,1,1,1,1,1,1,1,1,1,1,1,1,1,1,1,1,1,1,1,1,1,1,1,1,1,1,1,1,1,1,1,1,1,1,
1,1,1,1,1,1,1,1,1,1,1,1,1,1,1,1,1,1,1,1,1,1,1,6),(-0.941429844437942,-0.940000000000001,
-0.935000000000001,-0.930000000000001,-0.925000000000001,-0.920000000000001,
-0.915000000000001,-0.910000000000001,-0.905000000000001,-0.900000000000001,
-0.895000000000001,-0.890000000000001,-0.885000000000001,-0.880000000000001,
-0.875000000000001,-0.870000000000001,-0.865000000000001,-0.860000000000001,
-0.855000000000001,-0.850000000000001,-0.845000000000001,-0.840000000000001,
-0.835000000000001,-0.830000000000001,-0.825000000000001,-0.820000000000001,
-0.815000000000001,-0.810000000000001,-0.805000000000001,-0.800000000000001,
-0.795000000000001,-0.790000000000001,-0.785000000000001,-0.780000000000001,
-0.775000000000001,-0.770000000000001,-0.765000000000001,-0.760000000000001,
-0.755000000000001,-0.750000000000001,-0.745000000000001,-0.740000000000001,
-0.735000000000001,-0.730000000000001,-0.725000000000001,-0.720000000000001,
-0.715000000000001,-0.710000000000001,-0.705000000000001,-0.700000000000001,
-0.695000000000001,-0.690000000000001,-0.685,-0.68,-0.675,-0.67,-0.665,
-0.66,-0.655,-0.65,-0.645,-0.64,-0.635,-0.63,-0.625,-0.62,-0.615,-0.61,
-0.605,-0.6,-0.595,-0.59,-0.585,-0.58,-0.575,-0.57,-0.565,-0.56,-0.555,
-0.55,-0.545,-0.54,-0.535,-0.53,-0.525,-0.52,-0.515,-0.51,-0.505,-0.5,-0.495,
-0.49,-0.485,-0.48,-0.475,-0.47,-0.465,-0.46,-0.455,-0.45,-0.445,-0.44,
-0.435,-0.43,-0.425,-0.42,-0.415,-0.41,-0.405,-0.4,-0.395,-0.39,-0.385,
-0.38,-0.375,-0.37,-0.365,-0.36,-0.355,-0.35,-0.345,-0.34,-0.335,-0.33,
-0.325,-0.32,-0.315,-0.31,-0.305,-0.3,-0.295,-0.29,-0.285,-0.28,-0.275,
-0.27,-0.265,-0.26,-0.255,-0.25,-0.245,-0.24,-0.235,-0.23,-0.225,-0.22,
-0.215,-0.21,-0.205,-0.2,-0.195,-0.19,-0.185,-0.18,-0.175,-0.17,-0.165,
-0.16,-0.155,-0.15,-0.145,-0.14,-0.135,-0.13,-0.125,-0.12,-0.115,-0.11,
-0.105,-0.1,-0.095,-0.09,-0.085,-0.08,-0.075,-0.07,-0.065,-0.06,-0.055,
-0.05,-0.045,-0.04,-0.035,-0.03,-0.025,-0.02,-0.015,-0.01,-0.005,0.),
 .UNSPECIFIED.)
CURVE()
GEOMETRIC_REPRESENTATION_ITEM()
RATIONAL_B_SPLINE_CURVE((1.,1.,1.,1.,1.,1.,1.,1.,1.,1.,1.,1.,1.,1.,1.,1.,
1.,1.,1.,1.,1.,1.,1.,1.,1.,1.,1.,1.,1.,1.,1.,1.,1.,1.,1.,1.,1.,1.,1.,1.,
1.,1.,1.,1.,1.,1.,1.,1.,1.,1.,1.,1.,1.,1.,1.,1.,1.,1.,1.,1.,1.,1.,1.,1.,
1.,1.,1.,1.,1.,1.,1.,1.,1.,1.,1.,1.,1.,1.,1.,1.,1.,1.,1.,1.,1.,1.,1.,1.,
1.,1.,1.,1.,1.,1.,1.,1.,1.,1.,1.,1.,1.,1.,1.,1.,1.,1.,1.,1.,1.,1.,1.,1.,
1.,1.,1.,1.,1.,1.,1.,1.,1.,1.,1.,1.,1.,1.,1.,1.,1.,1.,1.,1.,1.,1.,1.,1.,
1.,1.,1.,1.,1.,1.,1.,1.,1.,1.,1.,1.,1.,1.,1.,1.,1.,1.,1.,1.,1.,1.,1.,1.,
1.,1.,1.,1.,1.,1.,1.,1.,1.,1.,1.,1.,1.,1.,1.,1.,1.,1.,1.,1.,1.,1.,1.,1.,
1.,1.,1.,1.,1.,1.,1.,1.,1.,1.))
REPRESENTATION_ITEM('')
);
#555=(
BOUNDED_CURVE()
B_SPLINE_CURVE(5,(#120608,#120609,#120610,#120611,#120612,#120613,#120614,
#120615,#120616,#120617,#120618,#120619,#120620,#120621,#120622,#120623,
#120624,#120625,#120626,#120627,#120628,#120629,#120630,#120631,#120632,
#120633,#120634,#120635,#120636,#120637,#120638,#120639,#120640,#120641,
#120642,#120643,#120644,#120645,#120646,#120647,#120648,#120649,#120650,
#120651,#120652,#120653,#120654,#120655,#120656,#120657,#120658,#120659,
#120660,#120661,#120662,#120663,#120664,#120665,#120666,#120667,#120668,
#120669,#120670,#120671,#120672,#120673,#120674,#120675,#120676,#120677,
#120678,#120679,#120680,#120681,#120682,#120683,#120684,#120685,#120686,
#120687,#120688,#120689,#120690,#120691,#120692,#120693,#120694,#120695,
#120696,#120697,#120698,#120699,#120700,#120701,#120702,#120703,#120704,
#120705,#120706,#120707,#120708,#120709,#120710,#120711,#120712,#120713,
#120714,#120715,#120716,#120717,#120718,#120719,#120720,#120721,#120722,
#120723,#120724,#120725,#120726,#120727,#120728,#120729,#120730,#120731,
#120732,#120733,#120734,#120735,#120736,#120737,#120738,#120739,#120740,
#120741,#120742,#120743,#120744,#120745,#120746,#120747,#120748,#120749,
#120750,#120751,#120752,#120753,#120754,#120755,#120756,#120757,#120758,
#120759,#120760,#120761,#120762,#120763,#120764,#120765,#120766,#120767,
#120768,#120769,#120770,#120771,#120772,#120773,#120774,#120775,#120776,
#120777,#120778,#120779,#120780,#120781,#120782,#120783,#120784,#120785,
#120786,#120787,#120788,#120789,#120790,#120791,#120792,#120793,#120794,
#120795,#120796,#120797,#120798,#120799,#120800,#120801),.UNSPECIFIED.,
 .F.,.F.)
B_SPLINE_CURVE_WITH_KNOTS((6,1,1,1,1,1,1,1,1,1,1,1,1,1,1,1,1,1,1,1,1,1,
1,1,1,1,1,1,1,1,1,1,1,1,1,1,1,1,1,1,1,1,1,1,1,1,1,1,1,1,1,1,1,1,1,1,1,1,
1,1,1,1,1,1,1,1,1,1,1,1,1,1,1,1,1,1,1,1,1,1,1,1,1,1,1,1,1,1,1,1,1,1,1,1,
1,1,1,1,1,1,1,1,1,1,1,1,1,1,1,1,1,1,1,1,1,1,1,1,1,1,1,1,1,1,1,1,1,1,1,1,
1,1,1,1,1,1,1,1,1,1,1,1,1,1,1,1,1,1,1,1,1,1,1,1,1,1,1,1,1,1,1,1,1,1,1,1,
1,1,1,1,1,1,1,1,1,1,1,1,1,1,1,1,1,1,1,1,1,1,1,6),(0.,0.005,0.01,0.015,0.02,
0.025,0.03,0.035,0.04,0.045,0.05,0.055,0.06,0.065,0.07,0.075,0.08,0.085,
0.09,0.095,0.1,0.105,0.11,0.115,0.12,0.125,0.13,0.135,0.14,0.145,0.15,0.155,
0.16,0.165,0.17,0.175,0.18,0.185,0.19,0.195,0.2,0.205,0.21,0.215,0.22,0.225,
0.23,0.235,0.24,0.245,0.25,0.255,0.26,0.265,0.27,0.275,0.28,0.285,0.29,
0.295,0.3,0.305,0.31,0.315,0.32,0.325,0.33,0.335,0.34,0.345,0.35,0.355,
0.36,0.365,0.37,0.375,0.38,0.385,0.39,0.395,0.4,0.405,0.41,0.415,0.42,0.425,
0.43,0.435,0.44,0.445,0.45,0.455,0.46,0.465,0.47,0.475,0.48,0.485,0.49,
0.495,0.5,0.505,0.51,0.515,0.52,0.525,0.53,0.535,0.54,0.545,0.55,0.555,
0.56,0.565,0.57,0.575,0.58,0.585,0.59,0.595,0.6,0.605,0.61,0.615,0.62,0.625,
0.63,0.635,0.64,0.645,0.65,0.655,0.66,0.665,0.67,0.675,0.68,0.685,0.690000000000001,
0.695000000000001,0.700000000000001,0.705000000000001,0.710000000000001,
0.715000000000001,0.720000000000001,0.725000000000001,0.730000000000001,
0.735000000000001,0.740000000000001,0.745000000000001,0.750000000000001,
0.755000000000001,0.760000000000001,0.765000000000001,0.770000000000001,
0.775000000000001,0.780000000000001,0.785000000000001,0.790000000000001,
0.795000000000001,0.800000000000001,0.805000000000001,0.810000000000001,
0.815000000000001,0.820000000000001,0.825000000000001,0.830000000000001,
0.835000000000001,0.840000000000001,0.845000000000001,0.850000000000001,
0.855000000000001,0.860000000000001,0.865000000000001,0.870000000000001,
0.875000000000001,0.880000000000001,0.885000000000001,0.890000000000001,
0.895000000000001,0.900000000000001,0.905000000000001,0.910000000000001,
0.915000000000001,0.920000000000001,0.925000000000001,0.930000000000001,
0.935000000000001,0.940000000000001,0.941429844438099),.UNSPECIFIED.)
CURVE()
GEOMETRIC_REPRESENTATION_ITEM()
RATIONAL_B_SPLINE_CURVE((1.,1.,1.,1.,1.,1.,1.,1.,1.,1.,1.,1.,1.,1.,1.,1.,
1.,1.,1.,1.,1.,1.,1.,1.,1.,1.,1.,1.,1.,1.,1.,1.,1.,1.,1.,1.,1.,1.,1.,1.,
1.,1.,1.,1.,1.,1.,1.,1.,1.,1.,1.,1.,1.,1.,1.,1.,1.,1.,1.,1.,1.,1.,1.,1.,
1.,1.,1.,1.,1.,1.,1.,1.,1.,1.,1.,1.,1.,1.,1.,1.,1.,1.,1.,1.,1.,1.,1.,1.,
1.,1.,1.,1.,1.,1.,1.,1.,1.,1.,1.,1.,1.,1.,1.,1.,1.,1.,1.,1.,1.,1.,1.,1.,
1.,1.,1.,1.,1.,1.,1.,1.,1.,1.,1.,1.,1.,1.,1.,1.,1.,1.,1.,1.,1.,1.,1.,1.,
1.,1.,1.,1.,1.,1.,1.,1.,1.,1.,1.,1.,1.,1.,1.,1.,1.,1.,1.,1.,1.,1.,1.,1.,
1.,1.,1.,1.,1.,1.,1.,1.,1.,1.,1.,1.,1.,1.,1.,1.,1.,1.,1.,1.,1.,1.,1.,1.,
1.,1.,1.,1.,1.,1.,1.,1.,1.,1.))
REPRESENTATION_ITEM('')
);
#556=(
BOUNDED_CURVE()
B_SPLINE_CURVE(5,(#120804,#120805,#120806,#120807,#120808,#120809,#120810,
#120811,#120812,#120813,#120814,#120815,#120816,#120817,#120818,#120819,
#120820,#120821,#120822,#120823,#120824,#120825,#120826,#120827,#120828,
#120829,#120830,#120831,#120832,#120833,#120834,#120835,#120836,#120837,
#120838,#120839,#120840,#120841,#120842,#120843,#120844,#120845,#120846,
#120847,#120848,#120849,#120850,#120851,#120852,#120853,#120854,#120855,
#120856,#120857,#120858,#120859,#120860,#120861,#120862,#120863,#120864,
#120865,#120866,#120867,#120868,#120869,#120870,#120871,#120872,#120873,
#120874,#120875,#120876,#120877,#120878,#120879,#120880,#120881,#120882,
#120883,#120884,#120885,#120886,#120887,#120888,#120889,#120890,#120891,
#120892,#120893,#120894,#120895,#120896,#120897,#120898,#120899,#120900,
#120901,#120902,#120903,#120904,#120905,#120906,#120907,#120908,#120909,
#120910,#120911,#120912,#120913,#120914,#120915,#120916,#120917,#120918,
#120919,#120920,#120921,#120922,#120923,#120924,#120925,#120926,#120927,
#120928,#120929,#120930,#120931,#120932,#120933,#120934,#120935,#120936,
#120937,#120938,#120939,#120940,#120941,#120942,#120943,#120944,#120945,
#120946,#120947,#120948,#120949,#120950,#120951,#120952,#120953,#120954,
#120955,#120956,#120957,#120958,#120959,#120960,#120961,#120962,#120963,
#120964,#120965,#120966,#120967,#120968,#120969,#120970,#120971,#120972,
#120973,#120974,#120975,#120976,#120977,#120978,#120979,#120980,#120981,
#120982,#120983,#120984,#120985,#120986,#120987,#120988,#120989,#120990,
#120991,#120992,#120993,#120994,#120995,#120996,#120997),.UNSPECIFIED.,
 .F.,.F.)
B_SPLINE_CURVE_WITH_KNOTS((6,1,1,1,1,1,1,1,1,1,1,1,1,1,1,1,1,1,1,1,1,1,
1,1,1,1,1,1,1,1,1,1,1,1,1,1,1,1,1,1,1,1,1,1,1,1,1,1,1,1,1,1,1,1,1,1,1,1,
1,1,1,1,1,1,1,1,1,1,1,1,1,1,1,1,1,1,1,1,1,1,1,1,1,1,1,1,1,1,1,1,1,1,1,1,
1,1,1,1,1,1,1,1,1,1,1,1,1,1,1,1,1,1,1,1,1,1,1,1,1,1,1,1,1,1,1,1,1,1,1,1,
1,1,1,1,1,1,1,1,1,1,1,1,1,1,1,1,1,1,1,1,1,1,1,1,1,1,1,1,1,1,1,1,1,1,1,1,
1,1,1,1,1,1,1,1,1,1,1,1,1,1,1,1,1,1,1,1,1,1,1,6),(-0.941429844438094,-0.940000000000001,
-0.935000000000001,-0.930000000000001,-0.925000000000001,-0.920000000000001,
-0.915000000000001,-0.910000000000001,-0.905000000000001,-0.900000000000001,
-0.895000000000001,-0.890000000000001,-0.885000000000001,-0.880000000000001,
-0.875000000000001,-0.870000000000001,-0.865000000000001,-0.860000000000001,
-0.855000000000001,-0.850000000000001,-0.845000000000001,-0.840000000000001,
-0.835000000000001,-0.830000000000001,-0.825000000000001,-0.820000000000001,
-0.815000000000001,-0.810000000000001,-0.805000000000001,-0.800000000000001,
-0.795000000000001,-0.790000000000001,-0.785000000000001,-0.780000000000001,
-0.775000000000001,-0.770000000000001,-0.765000000000001,-0.760000000000001,
-0.755000000000001,-0.750000000000001,-0.745000000000001,-0.740000000000001,
-0.735000000000001,-0.730000000000001,-0.725000000000001,-0.720000000000001,
-0.715000000000001,-0.710000000000001,-0.705000000000001,-0.700000000000001,
-0.695000000000001,-0.690000000000001,-0.685,-0.68,-0.675,-0.67,-0.665,
-0.66,-0.655,-0.65,-0.645,-0.64,-0.635,-0.63,-0.625,-0.62,-0.615,-0.61,
-0.605,-0.6,-0.595,-0.59,-0.585,-0.58,-0.575,-0.57,-0.565,-0.56,-0.555,
-0.55,-0.545,-0.54,-0.535,-0.53,-0.525,-0.52,-0.515,-0.51,-0.505,-0.5,-0.495,
-0.49,-0.485,-0.48,-0.475,-0.47,-0.465,-0.46,-0.455,-0.45,-0.445,-0.44,
-0.435,-0.43,-0.425,-0.42,-0.415,-0.41,-0.405,-0.4,-0.395,-0.39,-0.385,
-0.38,-0.375,-0.37,-0.365,-0.36,-0.355,-0.35,-0.345,-0.34,-0.335,-0.33,
-0.325,-0.32,-0.315,-0.31,-0.305,-0.3,-0.295,-0.29,-0.285,-0.28,-0.275,
-0.27,-0.265,-0.26,-0.255,-0.25,-0.245,-0.24,-0.235,-0.23,-0.225,-0.22,
-0.215,-0.21,-0.205,-0.2,-0.195,-0.19,-0.185,-0.18,-0.175,-0.17,-0.165,
-0.16,-0.155,-0.15,-0.145,-0.14,-0.135,-0.13,-0.125,-0.12,-0.115,-0.11,
-0.105,-0.1,-0.095,-0.09,-0.085,-0.08,-0.075,-0.07,-0.065,-0.06,-0.055,
-0.05,-0.045,-0.04,-0.035,-0.03,-0.025,-0.02,-0.015,-0.01,-0.005,0.),
 .UNSPECIFIED.)
CURVE()
GEOMETRIC_REPRESENTATION_ITEM()
RATIONAL_B_SPLINE_CURVE((1.,1.,1.,1.,1.,1.,1.,1.,1.,1.,1.,1.,1.,1.,1.,1.,
1.,1.,1.,1.,1.,1.,1.,1.,1.,1.,1.,1.,1.,1.,1.,1.,1.,1.,1.,1.,1.,1.,1.,1.,
1.,1.,1.,1.,1.,1.,1.,1.,1.,1.,1.,1.,1.,1.,1.,1.,1.,1.,1.,1.,1.,1.,1.,1.,
1.,1.,1.,1.,1.,1.,1.,1.,1.,1.,1.,1.,1.,1.,1.,1.,1.,1.,1.,1.,1.,1.,1.,1.,
1.,1.,1.,1.,1.,1.,1.,1.,1.,1.,1.,1.,1.,1.,1.,1.,1.,1.,1.,1.,1.,1.,1.,1.,
1.,1.,1.,1.,1.,1.,1.,1.,1.,1.,1.,1.,1.,1.,1.,1.,1.,1.,1.,1.,1.,1.,1.,1.,
1.,1.,1.,1.,1.,1.,1.,1.,1.,1.,1.,1.,1.,1.,1.,1.,1.,1.,1.,1.,1.,1.,1.,1.,
1.,1.,1.,1.,1.,1.,1.,1.,1.,1.,1.,1.,1.,1.,1.,1.,1.,1.,1.,1.,1.,1.,1.,1.,
1.,1.,1.,1.,1.,1.,1.,1.,1.,1.))
REPRESENTATION_ITEM('')
);
#557=(
BOUNDED_CURVE()
B_SPLINE_CURVE(5,(#121409,#121410,#121411,#121412,#121413,#121414,#121415,
#121416,#121417,#121418,#121419,#121420,#121421,#121422,#121423,#121424,
#121425,#121426,#121427,#121428,#121429,#121430,#121431,#121432,#121433,
#121434,#121435,#121436,#121437,#121438,#121439,#121440,#121441,#121442,
#121443,#121444,#121445,#121446,#121447,#121448,#121449,#121450,#121451,
#121452,#121453,#121454,#121455,#121456,#121457,#121458,#121459,#121460,
#121461,#121462,#121463,#121464,#121465,#121466,#121467,#121468,#121469,
#121470,#121471,#121472,#121473,#121474,#121475,#121476,#121477,#121478,
#121479,#121480,#121481,#121482,#121483,#121484,#121485,#121486,#121487,
#121488,#121489,#121490,#121491,#121492,#121493,#121494,#121495,#121496,
#121497,#121498,#121499,#121500,#121501,#121502,#121503,#121504,#121505,
#121506,#121507,#121508,#121509,#121510,#121511,#121512,#121513,#121514,
#121515,#121516,#121517,#121518,#121519,#121520,#121521,#121522,#121523,
#121524,#121525,#121526,#121527,#121528,#121529,#121530,#121531,#121532,
#121533,#121534,#121535,#121536,#121537,#121538,#121539,#121540,#121541,
#121542,#121543,#121544,#121545,#121546,#121547,#121548,#121549,#121550,
#121551,#121552,#121553,#121554,#121555,#121556,#121557,#121558,#121559,
#121560,#121561,#121562,#121563,#121564,#121565,#121566,#121567,#121568,
#121569,#121570,#121571,#121572,#121573,#121574,#121575,#121576,#121577,
#121578,#121579,#121580,#121581,#121582,#121583,#121584,#121585,#121586,
#121587,#121588,#121589,#121590,#121591,#121592,#121593,#121594,#121595,
#121596,#121597,#121598,#121599,#121600,#121601,#121602),.UNSPECIFIED.,
 .F.,.F.)
B_SPLINE_CURVE_WITH_KNOTS((6,1,1,1,1,1,1,1,1,1,1,1,1,1,1,1,1,1,1,1,1,1,
1,1,1,1,1,1,1,1,1,1,1,1,1,1,1,1,1,1,1,1,1,1,1,1,1,1,1,1,1,1,1,1,1,1,1,1,
1,1,1,1,1,1,1,1,1,1,1,1,1,1,1,1,1,1,1,1,1,1,1,1,1,1,1,1,1,1,1,1,1,1,1,1,
1,1,1,1,1,1,1,1,1,1,1,1,1,1,1,1,1,1,1,1,1,1,1,1,1,1,1,1,1,1,1,1,1,1,1,1,
1,1,1,1,1,1,1,1,1,1,1,1,1,1,1,1,1,1,1,1,1,1,1,1,1,1,1,1,1,1,1,1,1,1,1,1,
1,1,1,1,1,1,1,1,1,1,1,1,1,1,1,1,1,1,1,1,1,1,1,6),(0.,0.005,0.01,0.015,0.02,
0.025,0.03,0.035,0.04,0.045,0.05,0.055,0.06,0.065,0.07,0.075,0.08,0.085,
0.09,0.095,0.1,0.105,0.11,0.115,0.12,0.125,0.13,0.135,0.14,0.145,0.15,0.155,
0.16,0.165,0.17,0.175,0.18,0.185,0.19,0.195,0.2,0.205,0.21,0.215,0.22,0.225,
0.23,0.235,0.24,0.245,0.25,0.255,0.26,0.265,0.27,0.275,0.28,0.285,0.29,
0.295,0.3,0.305,0.31,0.315,0.32,0.325,0.33,0.335,0.34,0.345,0.35,0.355,
0.36,0.365,0.37,0.375,0.38,0.385,0.39,0.395,0.4,0.405,0.41,0.415,0.42,0.425,
0.43,0.435,0.44,0.445,0.45,0.455,0.46,0.465,0.47,0.475,0.48,0.485,0.49,
0.495,0.5,0.505,0.51,0.515,0.52,0.525,0.53,0.535,0.54,0.545,0.55,0.555,
0.56,0.565,0.57,0.575,0.58,0.585,0.59,0.595,0.6,0.605,0.61,0.615,0.62,0.625,
0.63,0.635,0.64,0.645,0.65,0.655,0.66,0.665,0.67,0.675,0.68,0.685,0.690000000000001,
0.695000000000001,0.700000000000001,0.705000000000001,0.710000000000001,
0.715000000000001,0.720000000000001,0.725000000000001,0.730000000000001,
0.735000000000001,0.740000000000001,0.745000000000001,0.750000000000001,
0.755000000000001,0.760000000000001,0.765000000000001,0.770000000000001,
0.775000000000001,0.780000000000001,0.785000000000001,0.790000000000001,
0.795000000000001,0.800000000000001,0.805000000000001,0.810000000000001,
0.815000000000001,0.820000000000001,0.825000000000001,0.830000000000001,
0.835000000000001,0.840000000000001,0.845000000000001,0.850000000000001,
0.855000000000001,0.860000000000001,0.865000000000001,0.870000000000001,
0.875000000000001,0.880000000000001,0.885000000000001,0.890000000000001,
0.895000000000001,0.900000000000001,0.905000000000001,0.910000000000001,
0.915000000000001,0.920000000000001,0.925000000000001,0.930000000000001,
0.935000000000001,0.940000000000001,0.941429844437999),.UNSPECIFIED.)
CURVE()
GEOMETRIC_REPRESENTATION_ITEM()
RATIONAL_B_SPLINE_CURVE((1.,1.,1.,1.,1.,1.,1.,1.,1.,1.,1.,1.,1.,1.,1.,1.,
1.,1.,1.,1.,1.,1.,1.,1.,1.,1.,1.,1.,1.,1.,1.,1.,1.,1.,1.,1.,1.,1.,1.,1.,
1.,1.,1.,1.,1.,1.,1.,1.,1.,1.,1.,1.,1.,1.,1.,1.,1.,1.,1.,1.,1.,1.,1.,1.,
1.,1.,1.,1.,1.,1.,1.,1.,1.,1.,1.,1.,1.,1.,1.,1.,1.,1.,1.,1.,1.,1.,1.,1.,
1.,1.,1.,1.,1.,1.,1.,1.,1.,1.,1.,1.,1.,1.,1.,1.,1.,1.,1.,1.,1.,1.,1.,1.,
1.,1.,1.,1.,1.,1.,1.,1.,1.,1.,1.,1.,1.,1.,1.,1.,1.,1.,1.,1.,1.,1.,1.,1.,
1.,1.,1.,1.,1.,1.,1.,1.,1.,1.,1.,1.,1.,1.,1.,1.,1.,1.,1.,1.,1.,1.,1.,1.,
1.,1.,1.,1.,1.,1.,1.,1.,1.,1.,1.,1.,1.,1.,1.,1.,1.,1.,1.,1.,1.,1.,1.,1.,
1.,1.,1.,1.,1.,1.,1.,1.,1.,1.))
REPRESENTATION_ITEM('')
);
#558=(
BOUNDED_CURVE()
B_SPLINE_CURVE(5,(#121605,#121606,#121607,#121608,#121609,#121610,#121611,
#121612,#121613,#121614,#121615,#121616,#121617,#121618,#121619,#121620,
#121621,#121622,#121623,#121624,#121625,#121626,#121627,#121628,#121629,
#121630,#121631,#121632,#121633,#121634,#121635,#121636,#121637,#121638,
#121639,#121640,#121641,#121642,#121643,#121644,#121645,#121646,#121647,
#121648,#121649,#121650,#121651,#121652,#121653,#121654,#121655,#121656,
#121657,#121658,#121659,#121660,#121661,#121662,#121663,#121664,#121665,
#121666,#121667,#121668,#121669,#121670,#121671,#121672,#121673,#121674,
#121675,#121676,#121677,#121678,#121679,#121680,#121681,#121682,#121683,
#121684,#121685,#121686,#121687,#121688,#121689,#121690,#121691,#121692,
#121693,#121694,#121695,#121696,#121697,#121698,#121699,#121700,#121701,
#121702,#121703,#121704,#121705,#121706,#121707,#121708,#121709,#121710,
#121711,#121712,#121713,#121714,#121715,#121716,#121717,#121718,#121719,
#121720,#121721,#121722,#121723,#121724,#121725,#121726,#121727,#121728,
#121729,#121730,#121731,#121732,#121733,#121734,#121735,#121736,#121737,
#121738,#121739,#121740,#121741,#121742,#121743,#121744,#121745,#121746,
#121747,#121748,#121749,#121750,#121751,#121752,#121753,#121754,#121755,
#121756,#121757,#121758,#121759,#121760,#121761,#121762,#121763,#121764,
#121765,#121766,#121767,#121768,#121769,#121770,#121771,#121772,#121773,
#121774,#121775,#121776,#121777,#121778,#121779,#121780,#121781,#121782,
#121783,#121784,#121785,#121786,#121787,#121788,#121789,#121790,#121791,
#121792,#121793,#121794,#121795,#121796,#121797,#121798),.UNSPECIFIED.,
 .F.,.F.)
B_SPLINE_CURVE_WITH_KNOTS((6,1,1,1,1,1,1,1,1,1,1,1,1,1,1,1,1,1,1,1,1,1,
1,1,1,1,1,1,1,1,1,1,1,1,1,1,1,1,1,1,1,1,1,1,1,1,1,1,1,1,1,1,1,1,1,1,1,1,
1,1,1,1,1,1,1,1,1,1,1,1,1,1,1,1,1,1,1,1,1,1,1,1,1,1,1,1,1,1,1,1,1,1,1,1,
1,1,1,1,1,1,1,1,1,1,1,1,1,1,1,1,1,1,1,1,1,1,1,1,1,1,1,1,1,1,1,1,1,1,1,1,
1,1,1,1,1,1,1,1,1,1,1,1,1,1,1,1,1,1,1,1,1,1,1,1,1,1,1,1,1,1,1,1,1,1,1,1,
1,1,1,1,1,1,1,1,1,1,1,1,1,1,1,1,1,1,1,1,1,1,1,6),(-0.941429844438006,-0.940000000000001,
-0.935000000000001,-0.930000000000001,-0.925000000000001,-0.920000000000001,
-0.915000000000001,-0.910000000000001,-0.905000000000001,-0.900000000000001,
-0.895000000000001,-0.890000000000001,-0.885000000000001,-0.880000000000001,
-0.875000000000001,-0.870000000000001,-0.865000000000001,-0.860000000000001,
-0.855000000000001,-0.850000000000001,-0.845000000000001,-0.840000000000001,
-0.835000000000001,-0.830000000000001,-0.825000000000001,-0.820000000000001,
-0.815000000000001,-0.810000000000001,-0.805000000000001,-0.800000000000001,
-0.795000000000001,-0.790000000000001,-0.785000000000001,-0.780000000000001,
-0.775000000000001,-0.770000000000001,-0.765000000000001,-0.760000000000001,
-0.755000000000001,-0.750000000000001,-0.745000000000001,-0.740000000000001,
-0.735000000000001,-0.730000000000001,-0.725000000000001,-0.720000000000001,
-0.715000000000001,-0.710000000000001,-0.705000000000001,-0.700000000000001,
-0.695000000000001,-0.690000000000001,-0.685,-0.68,-0.675,-0.67,-0.665,
-0.66,-0.655,-0.65,-0.645,-0.64,-0.635,-0.63,-0.625,-0.62,-0.615,-0.61,
-0.605,-0.6,-0.595,-0.59,-0.585,-0.58,-0.575,-0.57,-0.565,-0.56,-0.555,
-0.55,-0.545,-0.54,-0.535,-0.53,-0.525,-0.52,-0.515,-0.51,-0.505,-0.5,-0.495,
-0.49,-0.485,-0.48,-0.475,-0.47,-0.465,-0.46,-0.455,-0.45,-0.445,-0.44,
-0.435,-0.43,-0.425,-0.42,-0.415,-0.41,-0.405,-0.4,-0.395,-0.39,-0.385,
-0.38,-0.375,-0.37,-0.365,-0.36,-0.355,-0.35,-0.345,-0.34,-0.335,-0.33,
-0.325,-0.32,-0.315,-0.31,-0.305,-0.3,-0.295,-0.29,-0.285,-0.28,-0.275,
-0.27,-0.265,-0.26,-0.255,-0.25,-0.245,-0.24,-0.235,-0.23,-0.225,-0.22,
-0.215,-0.21,-0.205,-0.2,-0.195,-0.19,-0.185,-0.18,-0.175,-0.17,-0.165,
-0.16,-0.155,-0.15,-0.145,-0.14,-0.135,-0.13,-0.125,-0.12,-0.115,-0.11,
-0.105,-0.1,-0.095,-0.09,-0.085,-0.08,-0.075,-0.07,-0.065,-0.06,-0.055,
-0.05,-0.045,-0.04,-0.035,-0.03,-0.025,-0.02,-0.015,-0.01,-0.005,0.),
 .UNSPECIFIED.)
CURVE()
GEOMETRIC_REPRESENTATION_ITEM()
RATIONAL_B_SPLINE_CURVE((1.,1.,1.,1.,1.,1.,1.,1.,1.,1.,1.,1.,1.,1.,1.,1.,
1.,1.,1.,1.,1.,1.,1.,1.,1.,1.,1.,1.,1.,1.,1.,1.,1.,1.,1.,1.,1.,1.,1.,1.,
1.,1.,1.,1.,1.,1.,1.,1.,1.,1.,1.,1.,1.,1.,1.,1.,1.,1.,1.,1.,1.,1.,1.,1.,
1.,1.,1.,1.,1.,1.,1.,1.,1.,1.,1.,1.,1.,1.,1.,1.,1.,1.,1.,1.,1.,1.,1.,1.,
1.,1.,1.,1.,1.,1.,1.,1.,1.,1.,1.,1.,1.,1.,1.,1.,1.,1.,1.,1.,1.,1.,1.,1.,
1.,1.,1.,1.,1.,1.,1.,1.,1.,1.,1.,1.,1.,1.,1.,1.,1.,1.,1.,1.,1.,1.,1.,1.,
1.,1.,1.,1.,1.,1.,1.,1.,1.,1.,1.,1.,1.,1.,1.,1.,1.,1.,1.,1.,1.,1.,1.,1.,
1.,1.,1.,1.,1.,1.,1.,1.,1.,1.,1.,1.,1.,1.,1.,1.,1.,1.,1.,1.,1.,1.,1.,1.,
1.,1.,1.,1.,1.,1.,1.,1.,1.,1.))
REPRESENTATION_ITEM('')
);
#559=(
BOUNDED_CURVE()
B_SPLINE_CURVE(5,(#122210,#122211,#122212,#122213,#122214,#122215,#122216,
#122217,#122218,#122219,#122220,#122221,#122222,#122223,#122224,#122225,
#122226,#122227,#122228,#122229,#122230,#122231,#122232,#122233,#122234,
#122235,#122236,#122237,#122238,#122239,#122240,#122241,#122242,#122243,
#122244,#122245,#122246,#122247,#122248,#122249,#122250,#122251,#122252,
#122253,#122254,#122255,#122256,#122257,#122258,#122259,#122260,#122261,
#122262,#122263,#122264,#122265,#122266,#122267,#122268,#122269,#122270,
#122271,#122272,#122273,#122274,#122275,#122276,#122277,#122278,#122279,
#122280,#122281,#122282,#122283,#122284,#122285,#122286,#122287,#122288,
#122289,#122290,#122291,#122292,#122293,#122294,#122295,#122296,#122297,
#122298,#122299,#122300,#122301,#122302,#122303,#122304,#122305,#122306,
#122307,#122308,#122309,#122310,#122311,#122312,#122313,#122314,#122315,
#122316,#122317,#122318,#122319,#122320,#122321,#122322,#122323,#122324,
#122325,#122326,#122327,#122328,#122329,#122330,#122331,#122332,#122333,
#122334,#122335,#122336,#122337,#122338,#122339,#122340,#122341,#122342,
#122343,#122344,#122345,#122346,#122347,#122348,#122349,#122350,#122351,
#122352,#122353,#122354,#122355,#122356,#122357,#122358,#122359,#122360,
#122361,#122362,#122363,#122364,#122365,#122366,#122367,#122368,#122369,
#122370,#122371,#122372,#122373,#122374,#122375,#122376,#122377,#122378,
#122379,#122380,#122381,#122382,#122383,#122384,#122385,#122386,#122387,
#122388,#122389,#122390,#122391,#122392,#122393,#122394,#122395,#122396,
#122397,#122398,#122399,#122400,#122401,#122402,#122403),.UNSPECIFIED.,
 .F.,.F.)
B_SPLINE_CURVE_WITH_KNOTS((6,1,1,1,1,1,1,1,1,1,1,1,1,1,1,1,1,1,1,1,1,1,
1,1,1,1,1,1,1,1,1,1,1,1,1,1,1,1,1,1,1,1,1,1,1,1,1,1,1,1,1,1,1,1,1,1,1,1,
1,1,1,1,1,1,1,1,1,1,1,1,1,1,1,1,1,1,1,1,1,1,1,1,1,1,1,1,1,1,1,1,1,1,1,1,
1,1,1,1,1,1,1,1,1,1,1,1,1,1,1,1,1,1,1,1,1,1,1,1,1,1,1,1,1,1,1,1,1,1,1,1,
1,1,1,1,1,1,1,1,1,1,1,1,1,1,1,1,1,1,1,1,1,1,1,1,1,1,1,1,1,1,1,1,1,1,1,1,
1,1,1,1,1,1,1,1,1,1,1,1,1,1,1,1,1,1,1,1,1,1,1,6),(0.,0.005,0.01,0.015,0.02,
0.025,0.03,0.035,0.04,0.045,0.05,0.055,0.06,0.065,0.07,0.075,0.08,0.085,
0.09,0.095,0.1,0.105,0.11,0.115,0.12,0.125,0.13,0.135,0.14,0.145,0.15,0.155,
0.16,0.165,0.17,0.175,0.18,0.185,0.19,0.195,0.2,0.205,0.21,0.215,0.22,0.225,
0.23,0.235,0.24,0.245,0.25,0.255,0.26,0.265,0.27,0.275,0.28,0.285,0.29,
0.295,0.3,0.305,0.31,0.315,0.32,0.325,0.33,0.335,0.34,0.345,0.35,0.355,
0.36,0.365,0.37,0.375,0.38,0.385,0.39,0.395,0.4,0.405,0.41,0.415,0.42,0.425,
0.43,0.435,0.44,0.445,0.45,0.455,0.46,0.465,0.47,0.475,0.48,0.485,0.49,
0.495,0.5,0.505,0.51,0.515,0.52,0.525,0.53,0.535,0.54,0.545,0.55,0.555,
0.56,0.565,0.57,0.575,0.58,0.585,0.59,0.595,0.6,0.605,0.61,0.615,0.62,0.625,
0.63,0.635,0.64,0.645,0.65,0.655,0.66,0.665,0.67,0.675,0.68,0.685,0.690000000000001,
0.695000000000001,0.700000000000001,0.705000000000001,0.710000000000001,
0.715000000000001,0.720000000000001,0.725000000000001,0.730000000000001,
0.735000000000001,0.740000000000001,0.745000000000001,0.750000000000001,
0.755000000000001,0.760000000000001,0.765000000000001,0.770000000000001,
0.775000000000001,0.780000000000001,0.785000000000001,0.790000000000001,
0.795000000000001,0.800000000000001,0.805000000000001,0.810000000000001,
0.815000000000001,0.820000000000001,0.825000000000001,0.830000000000001,
0.835000000000001,0.840000000000001,0.845000000000001,0.850000000000001,
0.855000000000001,0.860000000000001,0.865000000000001,0.870000000000001,
0.875000000000001,0.880000000000001,0.885000000000001,0.890000000000001,
0.895000000000001,0.900000000000001,0.905000000000001,0.910000000000001,
0.915000000000001,0.920000000000001,0.925000000000001,0.930000000000001,
0.935000000000001,0.940000000000001,0.94142984443805),.UNSPECIFIED.)
CURVE()
GEOMETRIC_REPRESENTATION_ITEM()
RATIONAL_B_SPLINE_CURVE((1.,1.,1.,1.,1.,1.,1.,1.,1.,1.,1.,1.,1.,1.,1.,1.,
1.,1.,1.,1.,1.,1.,1.,1.,1.,1.,1.,1.,1.,1.,1.,1.,1.,1.,1.,1.,1.,1.,1.,1.,
1.,1.,1.,1.,1.,1.,1.,1.,1.,1.,1.,1.,1.,1.,1.,1.,1.,1.,1.,1.,1.,1.,1.,1.,
1.,1.,1.,1.,1.,1.,1.,1.,1.,1.,1.,1.,1.,1.,1.,1.,1.,1.,1.,1.,1.,1.,1.,1.,
1.,1.,1.,1.,1.,1.,1.,1.,1.,1.,1.,1.,1.,1.,1.,1.,1.,1.,1.,1.,1.,1.,1.,1.,
1.,1.,1.,1.,1.,1.,1.,1.,1.,1.,1.,1.,1.,1.,1.,1.,1.,1.,1.,1.,1.,1.,1.,1.,
1.,1.,1.,1.,1.,1.,1.,1.,1.,1.,1.,1.,1.,1.,1.,1.,1.,1.,1.,1.,1.,1.,1.,1.,
1.,1.,1.,1.,1.,1.,1.,1.,1.,1.,1.,1.,1.,1.,1.,1.,1.,1.,1.,1.,1.,1.,1.,1.,
1.,1.,1.,1.,1.,1.,1.,1.,1.,1.))
REPRESENTATION_ITEM('')
);
#560=(
BOUNDED_CURVE()
B_SPLINE_CURVE(5,(#122406,#122407,#122408,#122409,#122410,#122411,#122412,
#122413,#122414,#122415,#122416,#122417,#122418,#122419,#122420,#122421,
#122422,#122423,#122424,#122425,#122426,#122427,#122428,#122429,#122430,
#122431,#122432,#122433,#122434,#122435,#122436,#122437,#122438,#122439,
#122440,#122441,#122442,#122443,#122444,#122445,#122446,#122447,#122448,
#122449,#122450,#122451,#122452,#122453,#122454,#122455,#122456,#122457,
#122458,#122459,#122460,#122461,#122462,#122463,#122464,#122465,#122466,
#122467,#122468,#122469,#122470,#122471,#122472,#122473,#122474,#122475,
#122476,#122477,#122478,#122479,#122480,#122481,#122482,#122483,#122484,
#122485,#122486,#122487,#122488,#122489,#122490,#122491,#122492,#122493,
#122494,#122495,#122496,#122497,#122498,#122499,#122500,#122501,#122502,
#122503,#122504,#122505,#122506,#122507,#122508,#122509,#122510,#122511,
#122512,#122513,#122514,#122515,#122516,#122517,#122518,#122519,#122520,
#122521,#122522,#122523,#122524,#122525,#122526,#122527,#122528,#122529,
#122530,#122531,#122532,#122533,#122534,#122535,#122536,#122537,#122538,
#122539,#122540,#122541,#122542,#122543,#122544,#122545,#122546,#122547,
#122548,#122549,#122550,#122551,#122552,#122553,#122554,#122555,#122556,
#122557,#122558,#122559,#122560,#122561,#122562,#122563,#122564,#122565,
#122566,#122567,#122568,#122569,#122570,#122571,#122572,#122573,#122574,
#122575,#122576,#122577,#122578,#122579,#122580,#122581,#122582,#122583,
#122584,#122585,#122586,#122587,#122588,#122589,#122590,#122591,#122592,
#122593,#122594,#122595,#122596,#122597,#122598,#122599),.UNSPECIFIED.,
 .F.,.F.)
B_SPLINE_CURVE_WITH_KNOTS((6,1,1,1,1,1,1,1,1,1,1,1,1,1,1,1,1,1,1,1,1,1,
1,1,1,1,1,1,1,1,1,1,1,1,1,1,1,1,1,1,1,1,1,1,1,1,1,1,1,1,1,1,1,1,1,1,1,1,
1,1,1,1,1,1,1,1,1,1,1,1,1,1,1,1,1,1,1,1,1,1,1,1,1,1,1,1,1,1,1,1,1,1,1,1,
1,1,1,1,1,1,1,1,1,1,1,1,1,1,1,1,1,1,1,1,1,1,1,1,1,1,1,1,1,1,1,1,1,1,1,1,
1,1,1,1,1,1,1,1,1,1,1,1,1,1,1,1,1,1,1,1,1,1,1,1,1,1,1,1,1,1,1,1,1,1,1,1,
1,1,1,1,1,1,1,1,1,1,1,1,1,1,1,1,1,1,1,1,1,1,1,6),(-0.941429844438018,-0.940000000000001,
-0.935000000000001,-0.930000000000001,-0.925000000000001,-0.920000000000001,
-0.915000000000001,-0.910000000000001,-0.905000000000001,-0.900000000000001,
-0.895000000000001,-0.890000000000001,-0.885000000000001,-0.880000000000001,
-0.875000000000001,-0.870000000000001,-0.865000000000001,-0.860000000000001,
-0.855000000000001,-0.850000000000001,-0.845000000000001,-0.840000000000001,
-0.835000000000001,-0.830000000000001,-0.825000000000001,-0.820000000000001,
-0.815000000000001,-0.810000000000001,-0.805000000000001,-0.800000000000001,
-0.795000000000001,-0.790000000000001,-0.785000000000001,-0.780000000000001,
-0.775000000000001,-0.770000000000001,-0.765000000000001,-0.760000000000001,
-0.755000000000001,-0.750000000000001,-0.745000000000001,-0.740000000000001,
-0.735000000000001,-0.730000000000001,-0.725000000000001,-0.720000000000001,
-0.715000000000001,-0.710000000000001,-0.705000000000001,-0.700000000000001,
-0.695000000000001,-0.690000000000001,-0.685,-0.68,-0.675,-0.67,-0.665,
-0.66,-0.655,-0.65,-0.645,-0.64,-0.635,-0.63,-0.625,-0.62,-0.615,-0.61,
-0.605,-0.6,-0.595,-0.59,-0.585,-0.58,-0.575,-0.57,-0.565,-0.56,-0.555,
-0.55,-0.545,-0.54,-0.535,-0.53,-0.525,-0.52,-0.515,-0.51,-0.505,-0.5,-0.495,
-0.49,-0.485,-0.48,-0.475,-0.47,-0.465,-0.46,-0.455,-0.45,-0.445,-0.44,
-0.435,-0.43,-0.425,-0.42,-0.415,-0.41,-0.405,-0.4,-0.395,-0.39,-0.385,
-0.38,-0.375,-0.37,-0.365,-0.36,-0.355,-0.35,-0.345,-0.34,-0.335,-0.33,
-0.325,-0.32,-0.315,-0.31,-0.305,-0.3,-0.295,-0.29,-0.285,-0.28,-0.275,
-0.27,-0.265,-0.26,-0.255,-0.25,-0.245,-0.24,-0.235,-0.23,-0.225,-0.22,
-0.215,-0.21,-0.205,-0.2,-0.195,-0.19,-0.185,-0.18,-0.175,-0.17,-0.165,
-0.16,-0.155,-0.15,-0.145,-0.14,-0.135,-0.13,-0.125,-0.12,-0.115,-0.11,
-0.105,-0.1,-0.095,-0.09,-0.085,-0.08,-0.075,-0.07,-0.065,-0.06,-0.055,
-0.05,-0.045,-0.04,-0.035,-0.03,-0.025,-0.02,-0.015,-0.01,-0.005,0.),
 .UNSPECIFIED.)
CURVE()
GEOMETRIC_REPRESENTATION_ITEM()
RATIONAL_B_SPLINE_CURVE((1.,1.,1.,1.,1.,1.,1.,1.,1.,1.,1.,1.,1.,1.,1.,1.,
1.,1.,1.,1.,1.,1.,1.,1.,1.,1.,1.,1.,1.,1.,1.,1.,1.,1.,1.,1.,1.,1.,1.,1.,
1.,1.,1.,1.,1.,1.,1.,1.,1.,1.,1.,1.,1.,1.,1.,1.,1.,1.,1.,1.,1.,1.,1.,1.,
1.,1.,1.,1.,1.,1.,1.,1.,1.,1.,1.,1.,1.,1.,1.,1.,1.,1.,1.,1.,1.,1.,1.,1.,
1.,1.,1.,1.,1.,1.,1.,1.,1.,1.,1.,1.,1.,1.,1.,1.,1.,1.,1.,1.,1.,1.,1.,1.,
1.,1.,1.,1.,1.,1.,1.,1.,1.,1.,1.,1.,1.,1.,1.,1.,1.,1.,1.,1.,1.,1.,1.,1.,
1.,1.,1.,1.,1.,1.,1.,1.,1.,1.,1.,1.,1.,1.,1.,1.,1.,1.,1.,1.,1.,1.,1.,1.,
1.,1.,1.,1.,1.,1.,1.,1.,1.,1.,1.,1.,1.,1.,1.,1.,1.,1.,1.,1.,1.,1.,1.,1.,
1.,1.,1.,1.,1.,1.,1.,1.,1.,1.))
REPRESENTATION_ITEM('')
);
#561=(
BOUNDED_CURVE()
B_SPLINE_CURVE(5,(#123011,#123012,#123013,#123014,#123015,#123016,#123017,
#123018,#123019,#123020,#123021,#123022,#123023,#123024,#123025,#123026,
#123027,#123028,#123029,#123030,#123031,#123032,#123033,#123034,#123035,
#123036,#123037,#123038,#123039,#123040,#123041,#123042,#123043,#123044,
#123045,#123046,#123047,#123048,#123049,#123050,#123051,#123052,#123053,
#123054,#123055,#123056,#123057,#123058,#123059,#123060,#123061,#123062,
#123063,#123064,#123065,#123066,#123067,#123068,#123069,#123070,#123071,
#123072,#123073,#123074,#123075,#123076,#123077,#123078,#123079,#123080,
#123081,#123082,#123083,#123084,#123085,#123086,#123087,#123088,#123089,
#123090,#123091,#123092,#123093,#123094,#123095,#123096,#123097,#123098,
#123099,#123100,#123101,#123102,#123103,#123104,#123105,#123106,#123107,
#123108,#123109,#123110,#123111,#123112,#123113,#123114,#123115,#123116,
#123117,#123118,#123119,#123120,#123121,#123122,#123123,#123124,#123125,
#123126,#123127,#123128,#123129,#123130,#123131,#123132,#123133,#123134,
#123135,#123136,#123137,#123138,#123139,#123140,#123141,#123142,#123143,
#123144,#123145,#123146,#123147,#123148,#123149,#123150,#123151,#123152,
#123153,#123154,#123155,#123156,#123157,#123158,#123159,#123160,#123161,
#123162,#123163,#123164,#123165,#123166,#123167,#123168,#123169,#123170,
#123171,#123172,#123173,#123174,#123175,#123176,#123177,#123178,#123179,
#123180,#123181,#123182,#123183,#123184,#123185,#123186,#123187,#123188,
#123189,#123190,#123191,#123192,#123193,#123194,#123195,#123196,#123197,
#123198,#123199,#123200,#123201,#123202,#123203,#123204),.UNSPECIFIED.,
 .F.,.F.)
B_SPLINE_CURVE_WITH_KNOTS((6,1,1,1,1,1,1,1,1,1,1,1,1,1,1,1,1,1,1,1,1,1,
1,1,1,1,1,1,1,1,1,1,1,1,1,1,1,1,1,1,1,1,1,1,1,1,1,1,1,1,1,1,1,1,1,1,1,1,
1,1,1,1,1,1,1,1,1,1,1,1,1,1,1,1,1,1,1,1,1,1,1,1,1,1,1,1,1,1,1,1,1,1,1,1,
1,1,1,1,1,1,1,1,1,1,1,1,1,1,1,1,1,1,1,1,1,1,1,1,1,1,1,1,1,1,1,1,1,1,1,1,
1,1,1,1,1,1,1,1,1,1,1,1,1,1,1,1,1,1,1,1,1,1,1,1,1,1,1,1,1,1,1,1,1,1,1,1,
1,1,1,1,1,1,1,1,1,1,1,1,1,1,1,1,1,1,1,1,1,1,1,6),(0.,0.005,0.01,0.015,0.02,
0.025,0.03,0.035,0.04,0.045,0.05,0.055,0.06,0.065,0.07,0.075,0.08,0.085,
0.09,0.095,0.1,0.105,0.11,0.115,0.12,0.125,0.13,0.135,0.14,0.145,0.15,0.155,
0.16,0.165,0.17,0.175,0.18,0.185,0.19,0.195,0.2,0.205,0.21,0.215,0.22,0.225,
0.23,0.235,0.24,0.245,0.25,0.255,0.26,0.265,0.27,0.275,0.28,0.285,0.29,
0.295,0.3,0.305,0.31,0.315,0.32,0.325,0.33,0.335,0.34,0.345,0.35,0.355,
0.36,0.365,0.37,0.375,0.38,0.385,0.39,0.395,0.4,0.405,0.41,0.415,0.42,0.425,
0.43,0.435,0.44,0.445,0.45,0.455,0.46,0.465,0.47,0.475,0.48,0.485,0.49,
0.495,0.5,0.505,0.51,0.515,0.52,0.525,0.53,0.535,0.54,0.545,0.55,0.555,
0.56,0.565,0.57,0.575,0.58,0.585,0.59,0.595,0.6,0.605,0.61,0.615,0.62,0.625,
0.63,0.635,0.64,0.645,0.65,0.655,0.66,0.665,0.67,0.675,0.68,0.685,0.690000000000001,
0.695000000000001,0.700000000000001,0.705000000000001,0.710000000000001,
0.715000000000001,0.720000000000001,0.725000000000001,0.730000000000001,
0.735000000000001,0.740000000000001,0.745000000000001,0.750000000000001,
0.755000000000001,0.760000000000001,0.765000000000001,0.770000000000001,
0.775000000000001,0.780000000000001,0.785000000000001,0.790000000000001,
0.795000000000001,0.800000000000001,0.805000000000001,0.810000000000001,
0.815000000000001,0.820000000000001,0.825000000000001,0.830000000000001,
0.835000000000001,0.840000000000001,0.845000000000001,0.850000000000001,
0.855000000000001,0.860000000000001,0.865000000000001,0.870000000000001,
0.875000000000001,0.880000000000001,0.885000000000001,0.890000000000001,
0.895000000000001,0.900000000000001,0.905000000000001,0.910000000000001,
0.915000000000001,0.920000000000001,0.925000000000001,0.930000000000001,
0.935000000000001,0.940000000000001,0.941429844438072),.UNSPECIFIED.)
CURVE()
GEOMETRIC_REPRESENTATION_ITEM()
RATIONAL_B_SPLINE_CURVE((1.,1.,1.,1.,1.,1.,1.,1.,1.,1.,1.,1.,1.,1.,1.,1.,
1.,1.,1.,1.,1.,1.,1.,1.,1.,1.,1.,1.,1.,1.,1.,1.,1.,1.,1.,1.,1.,1.,1.,1.,
1.,1.,1.,1.,1.,1.,1.,1.,1.,1.,1.,1.,1.,1.,1.,1.,1.,1.,1.,1.,1.,1.,1.,1.,
1.,1.,1.,1.,1.,1.,1.,1.,1.,1.,1.,1.,1.,1.,1.,1.,1.,1.,1.,1.,1.,1.,1.,1.,
1.,1.,1.,1.,1.,1.,1.,1.,1.,1.,1.,1.,1.,1.,1.,1.,1.,1.,1.,1.,1.,1.,1.,1.,
1.,1.,1.,1.,1.,1.,1.,1.,1.,1.,1.,1.,1.,1.,1.,1.,1.,1.,1.,1.,1.,1.,1.,1.,
1.,1.,1.,1.,1.,1.,1.,1.,1.,1.,1.,1.,1.,1.,1.,1.,1.,1.,1.,1.,1.,1.,1.,1.,
1.,1.,1.,1.,1.,1.,1.,1.,1.,1.,1.,1.,1.,1.,1.,1.,1.,1.,1.,1.,1.,1.,1.,1.,
1.,1.,1.,1.,1.,1.,1.,1.,1.,1.))
REPRESENTATION_ITEM('')
);
#562=(
BOUNDED_CURVE()
B_SPLINE_CURVE(5,(#123207,#123208,#123209,#123210,#123211,#123212,#123213,
#123214,#123215,#123216,#123217,#123218,#123219,#123220,#123221,#123222,
#123223,#123224,#123225,#123226,#123227,#123228,#123229,#123230,#123231,
#123232,#123233,#123234,#123235,#123236,#123237,#123238,#123239,#123240,
#123241,#123242,#123243,#123244,#123245,#123246,#123247,#123248,#123249,
#123250,#123251,#123252,#123253,#123254,#123255,#123256,#123257,#123258,
#123259,#123260,#123261,#123262,#123263,#123264,#123265,#123266,#123267,
#123268,#123269,#123270,#123271,#123272,#123273,#123274,#123275,#123276,
#123277,#123278,#123279,#123280,#123281,#123282,#123283,#123284,#123285,
#123286,#123287,#123288,#123289,#123290,#123291,#123292,#123293,#123294,
#123295,#123296,#123297,#123298,#123299,#123300,#123301,#123302,#123303,
#123304,#123305,#123306,#123307,#123308,#123309,#123310,#123311,#123312,
#123313,#123314,#123315,#123316,#123317,#123318,#123319,#123320,#123321,
#123322,#123323,#123324,#123325,#123326,#123327,#123328,#123329,#123330,
#123331,#123332,#123333,#123334,#123335,#123336,#123337,#123338,#123339,
#123340,#123341,#123342,#123343,#123344,#123345,#123346,#123347,#123348,
#123349,#123350,#123351,#123352,#123353,#123354,#123355,#123356,#123357,
#123358,#123359,#123360,#123361,#123362,#123363,#123364,#123365,#123366,
#123367,#123368,#123369,#123370,#123371,#123372,#123373,#123374,#123375,
#123376,#123377,#123378,#123379,#123380,#123381,#123382,#123383,#123384,
#123385,#123386,#123387,#123388,#123389,#123390,#123391,#123392,#123393,
#123394,#123395,#123396,#123397,#123398,#123399,#123400),.UNSPECIFIED.,
 .F.,.F.)
B_SPLINE_CURVE_WITH_KNOTS((6,1,1,1,1,1,1,1,1,1,1,1,1,1,1,1,1,1,1,1,1,1,
1,1,1,1,1,1,1,1,1,1,1,1,1,1,1,1,1,1,1,1,1,1,1,1,1,1,1,1,1,1,1,1,1,1,1,1,
1,1,1,1,1,1,1,1,1,1,1,1,1,1,1,1,1,1,1,1,1,1,1,1,1,1,1,1,1,1,1,1,1,1,1,1,
1,1,1,1,1,1,1,1,1,1,1,1,1,1,1,1,1,1,1,1,1,1,1,1,1,1,1,1,1,1,1,1,1,1,1,1,
1,1,1,1,1,1,1,1,1,1,1,1,1,1,1,1,1,1,1,1,1,1,1,1,1,1,1,1,1,1,1,1,1,1,1,1,
1,1,1,1,1,1,1,1,1,1,1,1,1,1,1,1,1,1,1,1,1,1,1,6),(-0.941429844438072,-0.940000000000001,
-0.935000000000001,-0.930000000000001,-0.925000000000001,-0.920000000000001,
-0.915000000000001,-0.910000000000001,-0.905000000000001,-0.900000000000001,
-0.895000000000001,-0.890000000000001,-0.885000000000001,-0.880000000000001,
-0.875000000000001,-0.870000000000001,-0.865000000000001,-0.860000000000001,
-0.855000000000001,-0.850000000000001,-0.845000000000001,-0.840000000000001,
-0.835000000000001,-0.830000000000001,-0.825000000000001,-0.820000000000001,
-0.815000000000001,-0.810000000000001,-0.805000000000001,-0.800000000000001,
-0.795000000000001,-0.790000000000001,-0.785000000000001,-0.780000000000001,
-0.775000000000001,-0.770000000000001,-0.765000000000001,-0.760000000000001,
-0.755000000000001,-0.750000000000001,-0.745000000000001,-0.740000000000001,
-0.735000000000001,-0.730000000000001,-0.725000000000001,-0.720000000000001,
-0.715000000000001,-0.710000000000001,-0.705000000000001,-0.700000000000001,
-0.695000000000001,-0.690000000000001,-0.685,-0.68,-0.675,-0.67,-0.665,
-0.66,-0.655,-0.65,-0.645,-0.64,-0.635,-0.63,-0.625,-0.62,-0.615,-0.61,
-0.605,-0.6,-0.595,-0.59,-0.585,-0.58,-0.575,-0.57,-0.565,-0.56,-0.555,
-0.55,-0.545,-0.54,-0.535,-0.53,-0.525,-0.52,-0.515,-0.51,-0.505,-0.5,-0.495,
-0.49,-0.485,-0.48,-0.475,-0.47,-0.465,-0.46,-0.455,-0.45,-0.445,-0.44,
-0.435,-0.43,-0.425,-0.42,-0.415,-0.41,-0.405,-0.4,-0.395,-0.39,-0.385,
-0.38,-0.375,-0.37,-0.365,-0.36,-0.355,-0.35,-0.345,-0.34,-0.335,-0.33,
-0.325,-0.32,-0.315,-0.31,-0.305,-0.3,-0.295,-0.29,-0.285,-0.28,-0.275,
-0.27,-0.265,-0.26,-0.255,-0.25,-0.245,-0.24,-0.235,-0.23,-0.225,-0.22,
-0.215,-0.21,-0.205,-0.2,-0.195,-0.19,-0.185,-0.18,-0.175,-0.17,-0.165,
-0.16,-0.155,-0.15,-0.145,-0.14,-0.135,-0.13,-0.125,-0.12,-0.115,-0.11,
-0.105,-0.1,-0.095,-0.09,-0.085,-0.08,-0.075,-0.07,-0.065,-0.06,-0.055,
-0.05,-0.045,-0.04,-0.035,-0.03,-0.025,-0.02,-0.015,-0.01,-0.005,0.),
 .UNSPECIFIED.)
CURVE()
GEOMETRIC_REPRESENTATION_ITEM()
RATIONAL_B_SPLINE_CURVE((1.,1.,1.,1.,1.,1.,1.,1.,1.,1.,1.,1.,1.,1.,1.,1.,
1.,1.,1.,1.,1.,1.,1.,1.,1.,1.,1.,1.,1.,1.,1.,1.,1.,1.,1.,1.,1.,1.,1.,1.,
1.,1.,1.,1.,1.,1.,1.,1.,1.,1.,1.,1.,1.,1.,1.,1.,1.,1.,1.,1.,1.,1.,1.,1.,
1.,1.,1.,1.,1.,1.,1.,1.,1.,1.,1.,1.,1.,1.,1.,1.,1.,1.,1.,1.,1.,1.,1.,1.,
1.,1.,1.,1.,1.,1.,1.,1.,1.,1.,1.,1.,1.,1.,1.,1.,1.,1.,1.,1.,1.,1.,1.,1.,
1.,1.,1.,1.,1.,1.,1.,1.,1.,1.,1.,1.,1.,1.,1.,1.,1.,1.,1.,1.,1.,1.,1.,1.,
1.,1.,1.,1.,1.,1.,1.,1.,1.,1.,1.,1.,1.,1.,1.,1.,1.,1.,1.,1.,1.,1.,1.,1.,
1.,1.,1.,1.,1.,1.,1.,1.,1.,1.,1.,1.,1.,1.,1.,1.,1.,1.,1.,1.,1.,1.,1.,1.,
1.,1.,1.,1.,1.,1.,1.,1.,1.,1.))
REPRESENTATION_ITEM('')
);
#563=(
BOUNDED_CURVE()
B_SPLINE_CURVE(5,(#123812,#123813,#123814,#123815,#123816,#123817,#123818,
#123819,#123820,#123821,#123822,#123823,#123824,#123825,#123826,#123827,
#123828,#123829,#123830,#123831,#123832,#123833,#123834,#123835,#123836,
#123837,#123838,#123839,#123840,#123841,#123842,#123843,#123844,#123845,
#123846,#123847,#123848,#123849,#123850,#123851,#123852,#123853,#123854,
#123855,#123856,#123857,#123858,#123859,#123860,#123861,#123862,#123863,
#123864,#123865,#123866,#123867,#123868,#123869,#123870,#123871,#123872,
#123873,#123874,#123875,#123876,#123877,#123878,#123879,#123880,#123881,
#123882,#123883,#123884,#123885,#123886,#123887,#123888,#123889,#123890,
#123891,#123892,#123893,#123894,#123895,#123896,#123897,#123898,#123899,
#123900,#123901,#123902,#123903,#123904,#123905,#123906,#123907,#123908,
#123909,#123910,#123911,#123912,#123913,#123914,#123915,#123916,#123917,
#123918,#123919,#123920,#123921,#123922,#123923,#123924,#123925,#123926,
#123927,#123928,#123929,#123930,#123931,#123932,#123933,#123934,#123935,
#123936,#123937,#123938,#123939,#123940,#123941,#123942,#123943,#123944,
#123945,#123946,#123947,#123948,#123949,#123950,#123951,#123952,#123953,
#123954,#123955,#123956,#123957,#123958,#123959,#123960,#123961,#123962,
#123963,#123964,#123965,#123966,#123967,#123968,#123969,#123970,#123971,
#123972,#123973,#123974,#123975,#123976,#123977,#123978,#123979,#123980,
#123981,#123982,#123983,#123984,#123985,#123986,#123987,#123988,#123989,
#123990,#123991,#123992,#123993,#123994,#123995,#123996,#123997,#123998,
#123999,#124000,#124001,#124002,#124003,#124004,#124005),.UNSPECIFIED.,
 .F.,.F.)
B_SPLINE_CURVE_WITH_KNOTS((6,1,1,1,1,1,1,1,1,1,1,1,1,1,1,1,1,1,1,1,1,1,
1,1,1,1,1,1,1,1,1,1,1,1,1,1,1,1,1,1,1,1,1,1,1,1,1,1,1,1,1,1,1,1,1,1,1,1,
1,1,1,1,1,1,1,1,1,1,1,1,1,1,1,1,1,1,1,1,1,1,1,1,1,1,1,1,1,1,1,1,1,1,1,1,
1,1,1,1,1,1,1,1,1,1,1,1,1,1,1,1,1,1,1,1,1,1,1,1,1,1,1,1,1,1,1,1,1,1,1,1,
1,1,1,1,1,1,1,1,1,1,1,1,1,1,1,1,1,1,1,1,1,1,1,1,1,1,1,1,1,1,1,1,1,1,1,1,
1,1,1,1,1,1,1,1,1,1,1,1,1,1,1,1,1,1,1,1,1,1,1,6),(0.,0.005,0.01,0.015,0.02,
0.025,0.03,0.035,0.04,0.045,0.05,0.055,0.06,0.065,0.07,0.075,0.08,0.085,
0.09,0.095,0.1,0.105,0.11,0.115,0.12,0.125,0.13,0.135,0.14,0.145,0.15,0.155,
0.16,0.165,0.17,0.175,0.18,0.185,0.19,0.195,0.2,0.205,0.21,0.215,0.22,0.225,
0.23,0.235,0.24,0.245,0.25,0.255,0.26,0.265,0.27,0.275,0.28,0.285,0.29,
0.295,0.3,0.305,0.31,0.315,0.32,0.325,0.33,0.335,0.34,0.345,0.35,0.355,
0.36,0.365,0.37,0.375,0.38,0.385,0.39,0.395,0.4,0.405,0.41,0.415,0.42,0.425,
0.43,0.435,0.44,0.445,0.45,0.455,0.46,0.465,0.47,0.475,0.48,0.485,0.49,
0.495,0.5,0.505,0.51,0.515,0.52,0.525,0.53,0.535,0.54,0.545,0.55,0.555,
0.56,0.565,0.57,0.575,0.58,0.585,0.59,0.595,0.6,0.605,0.61,0.615,0.62,0.625,
0.63,0.635,0.64,0.645,0.65,0.655,0.66,0.665,0.67,0.675,0.68,0.685,0.690000000000001,
0.695000000000001,0.700000000000001,0.705000000000001,0.710000000000001,
0.715000000000001,0.720000000000001,0.725000000000001,0.730000000000001,
0.735000000000001,0.740000000000001,0.745000000000001,0.750000000000001,
0.755000000000001,0.760000000000001,0.765000000000001,0.770000000000001,
0.775000000000001,0.780000000000001,0.785000000000001,0.790000000000001,
0.795000000000001,0.800000000000001,0.805000000000001,0.810000000000001,
0.815000000000001,0.820000000000001,0.825000000000001,0.830000000000001,
0.835000000000001,0.840000000000001,0.845000000000001,0.850000000000001,
0.855000000000001,0.860000000000001,0.865000000000001,0.870000000000001,
0.875000000000001,0.880000000000001,0.885000000000001,0.890000000000001,
0.895000000000001,0.900000000000001,0.905000000000001,0.910000000000001,
0.915000000000001,0.920000000000001,0.925000000000001,0.930000000000001,
0.935000000000001,0.940000000000001,0.941429844437997),.UNSPECIFIED.)
CURVE()
GEOMETRIC_REPRESENTATION_ITEM()
RATIONAL_B_SPLINE_CURVE((1.,1.,1.,1.,1.,1.,1.,1.,1.,1.,1.,1.,1.,1.,1.,1.,
1.,1.,1.,1.,1.,1.,1.,1.,1.,1.,1.,1.,1.,1.,1.,1.,1.,1.,1.,1.,1.,1.,1.,1.,
1.,1.,1.,1.,1.,1.,1.,1.,1.,1.,1.,1.,1.,1.,1.,1.,1.,1.,1.,1.,1.,1.,1.,1.,
1.,1.,1.,1.,1.,1.,1.,1.,1.,1.,1.,1.,1.,1.,1.,1.,1.,1.,1.,1.,1.,1.,1.,1.,
1.,1.,1.,1.,1.,1.,1.,1.,1.,1.,1.,1.,1.,1.,1.,1.,1.,1.,1.,1.,1.,1.,1.,1.,
1.,1.,1.,1.,1.,1.,1.,1.,1.,1.,1.,1.,1.,1.,1.,1.,1.,1.,1.,1.,1.,1.,1.,1.,
1.,1.,1.,1.,1.,1.,1.,1.,1.,1.,1.,1.,1.,1.,1.,1.,1.,1.,1.,1.,1.,1.,1.,1.,
1.,1.,1.,1.,1.,1.,1.,1.,1.,1.,1.,1.,1.,1.,1.,1.,1.,1.,1.,1.,1.,1.,1.,1.,
1.,1.,1.,1.,1.,1.,1.,1.,1.,1.))
REPRESENTATION_ITEM('')
);
#564=(
BOUNDED_CURVE()
B_SPLINE_CURVE(5,(#124008,#124009,#124010,#124011,#124012,#124013,#124014,
#124015,#124016,#124017,#124018,#124019,#124020,#124021,#124022,#124023,
#124024,#124025,#124026,#124027,#124028,#124029,#124030,#124031,#124032,
#124033,#124034,#124035,#124036,#124037,#124038,#124039,#124040,#124041,
#124042,#124043,#124044,#124045,#124046,#124047,#124048,#124049,#124050,
#124051,#124052,#124053,#124054,#124055,#124056,#124057,#124058,#124059,
#124060,#124061,#124062,#124063,#124064,#124065,#124066,#124067,#124068,
#124069,#124070,#124071,#124072,#124073,#124074,#124075,#124076,#124077,
#124078,#124079,#124080,#124081,#124082,#124083,#124084,#124085,#124086,
#124087,#124088,#124089,#124090,#124091,#124092,#124093,#124094,#124095,
#124096,#124097,#124098,#124099,#124100,#124101,#124102,#124103,#124104,
#124105,#124106,#124107,#124108,#124109,#124110,#124111,#124112,#124113,
#124114,#124115,#124116,#124117,#124118,#124119,#124120,#124121,#124122,
#124123,#124124,#124125,#124126,#124127,#124128,#124129,#124130,#124131,
#124132,#124133,#124134,#124135,#124136,#124137,#124138,#124139,#124140,
#124141,#124142,#124143,#124144,#124145,#124146,#124147,#124148,#124149,
#124150,#124151,#124152,#124153,#124154,#124155,#124156,#124157,#124158,
#124159,#124160,#124161,#124162,#124163,#124164,#124165,#124166,#124167,
#124168,#124169,#124170,#124171,#124172,#124173,#124174,#124175,#124176,
#124177,#124178,#124179,#124180,#124181,#124182,#124183,#124184,#124185,
#124186,#124187,#124188,#124189,#124190,#124191,#124192,#124193,#124194,
#124195,#124196,#124197,#124198,#124199,#124200,#124201),.UNSPECIFIED.,
 .F.,.F.)
B_SPLINE_CURVE_WITH_KNOTS((6,1,1,1,1,1,1,1,1,1,1,1,1,1,1,1,1,1,1,1,1,1,
1,1,1,1,1,1,1,1,1,1,1,1,1,1,1,1,1,1,1,1,1,1,1,1,1,1,1,1,1,1,1,1,1,1,1,1,
1,1,1,1,1,1,1,1,1,1,1,1,1,1,1,1,1,1,1,1,1,1,1,1,1,1,1,1,1,1,1,1,1,1,1,1,
1,1,1,1,1,1,1,1,1,1,1,1,1,1,1,1,1,1,1,1,1,1,1,1,1,1,1,1,1,1,1,1,1,1,1,1,
1,1,1,1,1,1,1,1,1,1,1,1,1,1,1,1,1,1,1,1,1,1,1,1,1,1,1,1,1,1,1,1,1,1,1,1,
1,1,1,1,1,1,1,1,1,1,1,1,1,1,1,1,1,1,1,1,1,1,1,6),(-0.941429844437994,-0.940000000000001,
-0.935000000000001,-0.930000000000001,-0.925000000000001,-0.920000000000001,
-0.915000000000001,-0.910000000000001,-0.905000000000001,-0.900000000000001,
-0.895000000000001,-0.890000000000001,-0.885000000000001,-0.880000000000001,
-0.875000000000001,-0.870000000000001,-0.865000000000001,-0.860000000000001,
-0.855000000000001,-0.850000000000001,-0.845000000000001,-0.840000000000001,
-0.835000000000001,-0.830000000000001,-0.825000000000001,-0.820000000000001,
-0.815000000000001,-0.810000000000001,-0.805000000000001,-0.800000000000001,
-0.795000000000001,-0.790000000000001,-0.785000000000001,-0.780000000000001,
-0.775000000000001,-0.770000000000001,-0.765000000000001,-0.760000000000001,
-0.755000000000001,-0.750000000000001,-0.745000000000001,-0.740000000000001,
-0.735000000000001,-0.730000000000001,-0.725000000000001,-0.720000000000001,
-0.715000000000001,-0.710000000000001,-0.705000000000001,-0.700000000000001,
-0.695000000000001,-0.690000000000001,-0.685,-0.68,-0.675,-0.67,-0.665,
-0.66,-0.655,-0.65,-0.645,-0.64,-0.635,-0.63,-0.625,-0.62,-0.615,-0.61,
-0.605,-0.6,-0.595,-0.59,-0.585,-0.58,-0.575,-0.57,-0.565,-0.56,-0.555,
-0.55,-0.545,-0.54,-0.535,-0.53,-0.525,-0.52,-0.515,-0.51,-0.505,-0.5,-0.495,
-0.49,-0.485,-0.48,-0.475,-0.47,-0.465,-0.46,-0.455,-0.45,-0.445,-0.44,
-0.435,-0.43,-0.425,-0.42,-0.415,-0.41,-0.405,-0.4,-0.395,-0.39,-0.385,
-0.38,-0.375,-0.37,-0.365,-0.36,-0.355,-0.35,-0.345,-0.34,-0.335,-0.33,
-0.325,-0.32,-0.315,-0.31,-0.305,-0.3,-0.295,-0.29,-0.285,-0.28,-0.275,
-0.27,-0.265,-0.26,-0.255,-0.25,-0.245,-0.24,-0.235,-0.23,-0.225,-0.22,
-0.215,-0.21,-0.205,-0.2,-0.195,-0.19,-0.185,-0.18,-0.175,-0.17,-0.165,
-0.16,-0.155,-0.15,-0.145,-0.14,-0.135,-0.13,-0.125,-0.12,-0.115,-0.11,
-0.105,-0.1,-0.095,-0.09,-0.085,-0.08,-0.075,-0.07,-0.065,-0.06,-0.055,
-0.05,-0.045,-0.04,-0.035,-0.03,-0.025,-0.02,-0.015,-0.01,-0.005,0.),
 .UNSPECIFIED.)
CURVE()
GEOMETRIC_REPRESENTATION_ITEM()
RATIONAL_B_SPLINE_CURVE((1.,1.,1.,1.,1.,1.,1.,1.,1.,1.,1.,1.,1.,1.,1.,1.,
1.,1.,1.,1.,1.,1.,1.,1.,1.,1.,1.,1.,1.,1.,1.,1.,1.,1.,1.,1.,1.,1.,1.,1.,
1.,1.,1.,1.,1.,1.,1.,1.,1.,1.,1.,1.,1.,1.,1.,1.,1.,1.,1.,1.,1.,1.,1.,1.,
1.,1.,1.,1.,1.,1.,1.,1.,1.,1.,1.,1.,1.,1.,1.,1.,1.,1.,1.,1.,1.,1.,1.,1.,
1.,1.,1.,1.,1.,1.,1.,1.,1.,1.,1.,1.,1.,1.,1.,1.,1.,1.,1.,1.,1.,1.,1.,1.,
1.,1.,1.,1.,1.,1.,1.,1.,1.,1.,1.,1.,1.,1.,1.,1.,1.,1.,1.,1.,1.,1.,1.,1.,
1.,1.,1.,1.,1.,1.,1.,1.,1.,1.,1.,1.,1.,1.,1.,1.,1.,1.,1.,1.,1.,1.,1.,1.,
1.,1.,1.,1.,1.,1.,1.,1.,1.,1.,1.,1.,1.,1.,1.,1.,1.,1.,1.,1.,1.,1.,1.,1.,
1.,1.,1.,1.,1.,1.,1.,1.,1.,1.))
REPRESENTATION_ITEM('')
);
#565=(
BOUNDED_CURVE()
B_SPLINE_CURVE(5,(#124613,#124614,#124615,#124616,#124617,#124618,#124619,
#124620,#124621,#124622,#124623,#124624,#124625,#124626,#124627,#124628,
#124629,#124630,#124631,#124632,#124633,#124634,#124635,#124636,#124637,
#124638,#124639,#124640,#124641,#124642,#124643,#124644,#124645,#124646,
#124647,#124648,#124649,#124650,#124651,#124652,#124653,#124654,#124655,
#124656,#124657,#124658,#124659,#124660,#124661,#124662,#124663,#124664,
#124665,#124666,#124667,#124668,#124669,#124670,#124671,#124672,#124673,
#124674,#124675,#124676,#124677,#124678,#124679,#124680,#124681,#124682,
#124683,#124684,#124685,#124686,#124687,#124688,#124689,#124690,#124691,
#124692,#124693,#124694,#124695,#124696,#124697,#124698,#124699,#124700,
#124701,#124702,#124703,#124704,#124705,#124706,#124707,#124708,#124709,
#124710,#124711,#124712,#124713,#124714,#124715,#124716,#124717,#124718,
#124719,#124720,#124721,#124722,#124723,#124724,#124725,#124726,#124727,
#124728,#124729,#124730,#124731,#124732,#124733,#124734,#124735,#124736,
#124737,#124738,#124739,#124740,#124741,#124742,#124743,#124744,#124745,
#124746,#124747,#124748,#124749,#124750,#124751,#124752,#124753,#124754,
#124755,#124756,#124757,#124758,#124759,#124760,#124761,#124762,#124763,
#124764,#124765,#124766,#124767,#124768,#124769,#124770,#124771,#124772,
#124773,#124774,#124775,#124776,#124777,#124778,#124779,#124780,#124781,
#124782,#124783,#124784,#124785,#124786,#124787,#124788,#124789,#124790,
#124791,#124792,#124793,#124794,#124795,#124796,#124797,#124798,#124799,
#124800,#124801,#124802,#124803,#124804,#124805,#124806),.UNSPECIFIED.,
 .F.,.F.)
B_SPLINE_CURVE_WITH_KNOTS((6,1,1,1,1,1,1,1,1,1,1,1,1,1,1,1,1,1,1,1,1,1,
1,1,1,1,1,1,1,1,1,1,1,1,1,1,1,1,1,1,1,1,1,1,1,1,1,1,1,1,1,1,1,1,1,1,1,1,
1,1,1,1,1,1,1,1,1,1,1,1,1,1,1,1,1,1,1,1,1,1,1,1,1,1,1,1,1,1,1,1,1,1,1,1,
1,1,1,1,1,1,1,1,1,1,1,1,1,1,1,1,1,1,1,1,1,1,1,1,1,1,1,1,1,1,1,1,1,1,1,1,
1,1,1,1,1,1,1,1,1,1,1,1,1,1,1,1,1,1,1,1,1,1,1,1,1,1,1,1,1,1,1,1,1,1,1,1,
1,1,1,1,1,1,1,1,1,1,1,1,1,1,1,1,1,1,1,1,1,1,1,6),(0.,0.005,0.01,0.015,0.02,
0.025,0.03,0.035,0.04,0.045,0.05,0.055,0.06,0.065,0.07,0.075,0.08,0.085,
0.09,0.095,0.1,0.105,0.11,0.115,0.12,0.125,0.13,0.135,0.14,0.145,0.15,0.155,
0.16,0.165,0.17,0.175,0.18,0.185,0.19,0.195,0.2,0.205,0.21,0.215,0.22,0.225,
0.23,0.235,0.24,0.245,0.25,0.255,0.26,0.265,0.27,0.275,0.28,0.285,0.29,
0.295,0.3,0.305,0.31,0.315,0.32,0.325,0.33,0.335,0.34,0.345,0.35,0.355,
0.36,0.365,0.37,0.375,0.38,0.385,0.39,0.395,0.4,0.405,0.41,0.415,0.42,0.425,
0.43,0.435,0.44,0.445,0.45,0.455,0.46,0.465,0.47,0.475,0.48,0.485,0.49,
0.495,0.5,0.505,0.51,0.515,0.52,0.525,0.53,0.535,0.54,0.545,0.55,0.555,
0.56,0.565,0.57,0.575,0.58,0.585,0.59,0.595,0.6,0.605,0.61,0.615,0.62,0.625,
0.63,0.635,0.64,0.645,0.65,0.655,0.66,0.665,0.67,0.675,0.68,0.685,0.690000000000001,
0.695000000000001,0.700000000000001,0.705000000000001,0.710000000000001,
0.715000000000001,0.720000000000001,0.725000000000001,0.730000000000001,
0.735000000000001,0.740000000000001,0.745000000000001,0.750000000000001,
0.755000000000001,0.760000000000001,0.765000000000001,0.770000000000001,
0.775000000000001,0.780000000000001,0.785000000000001,0.790000000000001,
0.795000000000001,0.800000000000001,0.805000000000001,0.810000000000001,
0.815000000000001,0.820000000000001,0.825000000000001,0.830000000000001,
0.835000000000001,0.840000000000001,0.845000000000001,0.850000000000001,
0.855000000000001,0.860000000000001,0.865000000000001,0.870000000000001,
0.875000000000001,0.880000000000001,0.885000000000001,0.890000000000001,
0.895000000000001,0.900000000000001,0.905000000000001,0.910000000000001,
0.915000000000001,0.920000000000001,0.925000000000001,0.930000000000001,
0.935000000000001,0.940000000000001,0.941429844438079),.UNSPECIFIED.)
CURVE()
GEOMETRIC_REPRESENTATION_ITEM()
RATIONAL_B_SPLINE_CURVE((1.,1.,1.,1.,1.,1.,1.,1.,1.,1.,1.,1.,1.,1.,1.,1.,
1.,1.,1.,1.,1.,1.,1.,1.,1.,1.,1.,1.,1.,1.,1.,1.,1.,1.,1.,1.,1.,1.,1.,1.,
1.,1.,1.,1.,1.,1.,1.,1.,1.,1.,1.,1.,1.,1.,1.,1.,1.,1.,1.,1.,1.,1.,1.,1.,
1.,1.,1.,1.,1.,1.,1.,1.,1.,1.,1.,1.,1.,1.,1.,1.,1.,1.,1.,1.,1.,1.,1.,1.,
1.,1.,1.,1.,1.,1.,1.,1.,1.,1.,1.,1.,1.,1.,1.,1.,1.,1.,1.,1.,1.,1.,1.,1.,
1.,1.,1.,1.,1.,1.,1.,1.,1.,1.,1.,1.,1.,1.,1.,1.,1.,1.,1.,1.,1.,1.,1.,1.,
1.,1.,1.,1.,1.,1.,1.,1.,1.,1.,1.,1.,1.,1.,1.,1.,1.,1.,1.,1.,1.,1.,1.,1.,
1.,1.,1.,1.,1.,1.,1.,1.,1.,1.,1.,1.,1.,1.,1.,1.,1.,1.,1.,1.,1.,1.,1.,1.,
1.,1.,1.,1.,1.,1.,1.,1.,1.,1.))
REPRESENTATION_ITEM('')
);
#566=(
BOUNDED_CURVE()
B_SPLINE_CURVE(5,(#124809,#124810,#124811,#124812,#124813,#124814,#124815,
#124816,#124817,#124818,#124819,#124820,#124821,#124822,#124823,#124824,
#124825,#124826,#124827,#124828,#124829,#124830,#124831,#124832,#124833,
#124834,#124835,#124836,#124837,#124838,#124839,#124840,#124841,#124842,
#124843,#124844,#124845,#124846,#124847,#124848,#124849,#124850,#124851,
#124852,#124853,#124854,#124855,#124856,#124857,#124858,#124859,#124860,
#124861,#124862,#124863,#124864,#124865,#124866,#124867,#124868,#124869,
#124870,#124871,#124872,#124873,#124874,#124875,#124876,#124877,#124878,
#124879,#124880,#124881,#124882,#124883,#124884,#124885,#124886,#124887,
#124888,#124889,#124890,#124891,#124892,#124893,#124894,#124895,#124896,
#124897,#124898,#124899,#124900,#124901,#124902,#124903,#124904,#124905,
#124906,#124907,#124908,#124909,#124910,#124911,#124912,#124913,#124914,
#124915,#124916,#124917,#124918,#124919,#124920,#124921,#124922,#124923,
#124924,#124925,#124926,#124927,#124928,#124929,#124930,#124931,#124932,
#124933,#124934,#124935,#124936,#124937,#124938,#124939,#124940,#124941,
#124942,#124943,#124944,#124945,#124946,#124947,#124948,#124949,#124950,
#124951,#124952,#124953,#124954,#124955,#124956,#124957,#124958,#124959,
#124960,#124961,#124962,#124963,#124964,#124965,#124966,#124967,#124968,
#124969,#124970,#124971,#124972,#124973,#124974,#124975,#124976,#124977,
#124978,#124979,#124980,#124981,#124982,#124983,#124984,#124985,#124986,
#124987,#124988,#124989,#124990,#124991,#124992,#124993,#124994,#124995,
#124996,#124997,#124998,#124999,#125000,#125001,#125002),.UNSPECIFIED.,
 .F.,.F.)
B_SPLINE_CURVE_WITH_KNOTS((6,1,1,1,1,1,1,1,1,1,1,1,1,1,1,1,1,1,1,1,1,1,
1,1,1,1,1,1,1,1,1,1,1,1,1,1,1,1,1,1,1,1,1,1,1,1,1,1,1,1,1,1,1,1,1,1,1,1,
1,1,1,1,1,1,1,1,1,1,1,1,1,1,1,1,1,1,1,1,1,1,1,1,1,1,1,1,1,1,1,1,1,1,1,1,
1,1,1,1,1,1,1,1,1,1,1,1,1,1,1,1,1,1,1,1,1,1,1,1,1,1,1,1,1,1,1,1,1,1,1,1,
1,1,1,1,1,1,1,1,1,1,1,1,1,1,1,1,1,1,1,1,1,1,1,1,1,1,1,1,1,1,1,1,1,1,1,1,
1,1,1,1,1,1,1,1,1,1,1,1,1,1,1,1,1,1,1,1,1,1,1,6),(-0.941429844438079,-0.940000000000001,
-0.935000000000001,-0.930000000000001,-0.925000000000001,-0.920000000000001,
-0.915000000000001,-0.910000000000001,-0.905000000000001,-0.900000000000001,
-0.895000000000001,-0.890000000000001,-0.885000000000001,-0.880000000000001,
-0.875000000000001,-0.870000000000001,-0.865000000000001,-0.860000000000001,
-0.855000000000001,-0.850000000000001,-0.845000000000001,-0.840000000000001,
-0.835000000000001,-0.830000000000001,-0.825000000000001,-0.820000000000001,
-0.815000000000001,-0.810000000000001,-0.805000000000001,-0.800000000000001,
-0.795000000000001,-0.790000000000001,-0.785000000000001,-0.780000000000001,
-0.775000000000001,-0.770000000000001,-0.765000000000001,-0.760000000000001,
-0.755000000000001,-0.750000000000001,-0.745000000000001,-0.740000000000001,
-0.735000000000001,-0.730000000000001,-0.725000000000001,-0.720000000000001,
-0.715000000000001,-0.710000000000001,-0.705000000000001,-0.700000000000001,
-0.695000000000001,-0.690000000000001,-0.685,-0.68,-0.675,-0.67,-0.665,
-0.66,-0.655,-0.65,-0.645,-0.64,-0.635,-0.63,-0.625,-0.62,-0.615,-0.61,
-0.605,-0.6,-0.595,-0.59,-0.585,-0.58,-0.575,-0.57,-0.565,-0.56,-0.555,
-0.55,-0.545,-0.54,-0.535,-0.53,-0.525,-0.52,-0.515,-0.51,-0.505,-0.5,-0.495,
-0.49,-0.485,-0.48,-0.475,-0.47,-0.465,-0.46,-0.455,-0.45,-0.445,-0.44,
-0.435,-0.43,-0.425,-0.42,-0.415,-0.41,-0.405,-0.4,-0.395,-0.39,-0.385,
-0.38,-0.375,-0.37,-0.365,-0.36,-0.355,-0.35,-0.345,-0.34,-0.335,-0.33,
-0.325,-0.32,-0.315,-0.31,-0.305,-0.3,-0.295,-0.29,-0.285,-0.28,-0.275,
-0.27,-0.265,-0.26,-0.255,-0.25,-0.245,-0.24,-0.235,-0.23,-0.225,-0.22,
-0.215,-0.21,-0.205,-0.2,-0.195,-0.19,-0.185,-0.18,-0.175,-0.17,-0.165,
-0.16,-0.155,-0.15,-0.145,-0.14,-0.135,-0.13,-0.125,-0.12,-0.115,-0.11,
-0.105,-0.1,-0.095,-0.09,-0.085,-0.08,-0.075,-0.07,-0.065,-0.06,-0.055,
-0.05,-0.045,-0.04,-0.035,-0.03,-0.025,-0.02,-0.015,-0.01,-0.005,0.),
 .UNSPECIFIED.)
CURVE()
GEOMETRIC_REPRESENTATION_ITEM()
RATIONAL_B_SPLINE_CURVE((1.,1.,1.,1.,1.,1.,1.,1.,1.,1.,1.,1.,1.,1.,1.,1.,
1.,1.,1.,1.,1.,1.,1.,1.,1.,1.,1.,1.,1.,1.,1.,1.,1.,1.,1.,1.,1.,1.,1.,1.,
1.,1.,1.,1.,1.,1.,1.,1.,1.,1.,1.,1.,1.,1.,1.,1.,1.,1.,1.,1.,1.,1.,1.,1.,
1.,1.,1.,1.,1.,1.,1.,1.,1.,1.,1.,1.,1.,1.,1.,1.,1.,1.,1.,1.,1.,1.,1.,1.,
1.,1.,1.,1.,1.,1.,1.,1.,1.,1.,1.,1.,1.,1.,1.,1.,1.,1.,1.,1.,1.,1.,1.,1.,
1.,1.,1.,1.,1.,1.,1.,1.,1.,1.,1.,1.,1.,1.,1.,1.,1.,1.,1.,1.,1.,1.,1.,1.,
1.,1.,1.,1.,1.,1.,1.,1.,1.,1.,1.,1.,1.,1.,1.,1.,1.,1.,1.,1.,1.,1.,1.,1.,
1.,1.,1.,1.,1.,1.,1.,1.,1.,1.,1.,1.,1.,1.,1.,1.,1.,1.,1.,1.,1.,1.,1.,1.,
1.,1.,1.,1.,1.,1.,1.,1.,1.,1.))
REPRESENTATION_ITEM('')
);
#567=(
BOUNDED_CURVE()
B_SPLINE_CURVE(5,(#125414,#125415,#125416,#125417,#125418,#125419,#125420,
#125421,#125422,#125423,#125424,#125425,#125426,#125427,#125428,#125429,
#125430,#125431,#125432,#125433,#125434,#125435,#125436,#125437,#125438,
#125439,#125440,#125441,#125442,#125443,#125444,#125445,#125446,#125447,
#125448,#125449,#125450,#125451,#125452,#125453,#125454,#125455,#125456,
#125457,#125458,#125459,#125460,#125461,#125462,#125463,#125464,#125465,
#125466,#125467,#125468,#125469,#125470,#125471,#125472,#125473,#125474,
#125475,#125476,#125477,#125478,#125479,#125480,#125481,#125482,#125483,
#125484,#125485,#125486,#125487,#125488,#125489,#125490,#125491,#125492,
#125493,#125494,#125495,#125496,#125497,#125498,#125499,#125500,#125501,
#125502,#125503,#125504,#125505,#125506,#125507,#125508,#125509,#125510,
#125511,#125512,#125513,#125514,#125515,#125516,#125517,#125518,#125519,
#125520,#125521,#125522,#125523,#125524,#125525,#125526,#125527,#125528,
#125529,#125530,#125531,#125532,#125533,#125534,#125535,#125536,#125537,
#125538,#125539,#125540,#125541,#125542,#125543,#125544,#125545,#125546,
#125547,#125548,#125549,#125550,#125551,#125552,#125553,#125554,#125555,
#125556,#125557,#125558,#125559,#125560,#125561,#125562,#125563,#125564,
#125565,#125566,#125567,#125568,#125569,#125570,#125571,#125572,#125573,
#125574,#125575,#125576,#125577,#125578,#125579,#125580,#125581,#125582,
#125583,#125584,#125585,#125586,#125587,#125588,#125589,#125590,#125591,
#125592,#125593,#125594,#125595,#125596,#125597,#125598,#125599,#125600,
#125601,#125602,#125603,#125604,#125605,#125606,#125607),.UNSPECIFIED.,
 .F.,.F.)
B_SPLINE_CURVE_WITH_KNOTS((6,1,1,1,1,1,1,1,1,1,1,1,1,1,1,1,1,1,1,1,1,1,
1,1,1,1,1,1,1,1,1,1,1,1,1,1,1,1,1,1,1,1,1,1,1,1,1,1,1,1,1,1,1,1,1,1,1,1,
1,1,1,1,1,1,1,1,1,1,1,1,1,1,1,1,1,1,1,1,1,1,1,1,1,1,1,1,1,1,1,1,1,1,1,1,
1,1,1,1,1,1,1,1,1,1,1,1,1,1,1,1,1,1,1,1,1,1,1,1,1,1,1,1,1,1,1,1,1,1,1,1,
1,1,1,1,1,1,1,1,1,1,1,1,1,1,1,1,1,1,1,1,1,1,1,1,1,1,1,1,1,1,1,1,1,1,1,1,
1,1,1,1,1,1,1,1,1,1,1,1,1,1,1,1,1,1,1,1,1,1,1,6),(0.,0.005,0.01,0.015,0.02,
0.025,0.03,0.035,0.04,0.045,0.05,0.055,0.06,0.065,0.07,0.075,0.08,0.085,
0.09,0.095,0.1,0.105,0.11,0.115,0.12,0.125,0.13,0.135,0.14,0.145,0.15,0.155,
0.16,0.165,0.17,0.175,0.18,0.185,0.19,0.195,0.2,0.205,0.21,0.215,0.22,0.225,
0.23,0.235,0.24,0.245,0.25,0.255,0.26,0.265,0.27,0.275,0.28,0.285,0.29,
0.295,0.3,0.305,0.31,0.315,0.32,0.325,0.33,0.335,0.34,0.345,0.35,0.355,
0.36,0.365,0.37,0.375,0.38,0.385,0.39,0.395,0.4,0.405,0.41,0.415,0.42,0.425,
0.43,0.435,0.44,0.445,0.45,0.455,0.46,0.465,0.47,0.475,0.48,0.485,0.49,
0.495,0.5,0.505,0.51,0.515,0.52,0.525,0.53,0.535,0.54,0.545,0.55,0.555,
0.56,0.565,0.57,0.575,0.58,0.585,0.59,0.595,0.6,0.605,0.61,0.615,0.62,0.625,
0.63,0.635,0.64,0.645,0.65,0.655,0.66,0.665,0.67,0.675,0.68,0.685,0.690000000000001,
0.695000000000001,0.700000000000001,0.705000000000001,0.710000000000001,
0.715000000000001,0.720000000000001,0.725000000000001,0.730000000000001,
0.735000000000001,0.740000000000001,0.745000000000001,0.750000000000001,
0.755000000000001,0.760000000000001,0.765000000000001,0.770000000000001,
0.775000000000001,0.780000000000001,0.785000000000001,0.790000000000001,
0.795000000000001,0.800000000000001,0.805000000000001,0.810000000000001,
0.815000000000001,0.820000000000001,0.825000000000001,0.830000000000001,
0.835000000000001,0.840000000000001,0.845000000000001,0.850000000000001,
0.855000000000001,0.860000000000001,0.865000000000001,0.870000000000001,
0.875000000000001,0.880000000000001,0.885000000000001,0.890000000000001,
0.895000000000001,0.900000000000001,0.905000000000001,0.910000000000001,
0.915000000000001,0.920000000000001,0.925000000000001,0.930000000000001,
0.935000000000001,0.940000000000001,0.941429844438073),.UNSPECIFIED.)
CURVE()
GEOMETRIC_REPRESENTATION_ITEM()
RATIONAL_B_SPLINE_CURVE((1.,1.,1.,1.,1.,1.,1.,1.,1.,1.,1.,1.,1.,1.,1.,1.,
1.,1.,1.,1.,1.,1.,1.,1.,1.,1.,1.,1.,1.,1.,1.,1.,1.,1.,1.,1.,1.,1.,1.,1.,
1.,1.,1.,1.,1.,1.,1.,1.,1.,1.,1.,1.,1.,1.,1.,1.,1.,1.,1.,1.,1.,1.,1.,1.,
1.,1.,1.,1.,1.,1.,1.,1.,1.,1.,1.,1.,1.,1.,1.,1.,1.,1.,1.,1.,1.,1.,1.,1.,
1.,1.,1.,1.,1.,1.,1.,1.,1.,1.,1.,1.,1.,1.,1.,1.,1.,1.,1.,1.,1.,1.,1.,1.,
1.,1.,1.,1.,1.,1.,1.,1.,1.,1.,1.,1.,1.,1.,1.,1.,1.,1.,1.,1.,1.,1.,1.,1.,
1.,1.,1.,1.,1.,1.,1.,1.,1.,1.,1.,1.,1.,1.,1.,1.,1.,1.,1.,1.,1.,1.,1.,1.,
1.,1.,1.,1.,1.,1.,1.,1.,1.,1.,1.,1.,1.,1.,1.,1.,1.,1.,1.,1.,1.,1.,1.,1.,
1.,1.,1.,1.,1.,1.,1.,1.,1.,1.))
REPRESENTATION_ITEM('')
);
#568=(
BOUNDED_CURVE()
B_SPLINE_CURVE(5,(#125610,#125611,#125612,#125613,#125614,#125615,#125616,
#125617,#125618,#125619,#125620,#125621,#125622,#125623,#125624,#125625,
#125626,#125627,#125628,#125629,#125630,#125631,#125632,#125633,#125634,
#125635,#125636,#125637,#125638,#125639,#125640,#125641,#125642,#125643,
#125644,#125645,#125646,#125647,#125648,#125649,#125650,#125651,#125652,
#125653,#125654,#125655,#125656,#125657,#125658,#125659,#125660,#125661,
#125662,#125663,#125664,#125665,#125666,#125667,#125668,#125669,#125670,
#125671,#125672,#125673,#125674,#125675,#125676,#125677,#125678,#125679,
#125680,#125681,#125682,#125683,#125684,#125685,#125686,#125687,#125688,
#125689,#125690,#125691,#125692,#125693,#125694,#125695,#125696,#125697,
#125698,#125699,#125700,#125701,#125702,#125703,#125704,#125705,#125706,
#125707,#125708,#125709,#125710,#125711,#125712,#125713,#125714,#125715,
#125716,#125717,#125718,#125719,#125720,#125721,#125722,#125723,#125724,
#125725,#125726,#125727,#125728,#125729,#125730,#125731,#125732,#125733,
#125734,#125735,#125736,#125737,#125738,#125739,#125740,#125741,#125742,
#125743,#125744,#125745,#125746,#125747,#125748,#125749,#125750,#125751,
#125752,#125753,#125754,#125755,#125756,#125757,#125758,#125759,#125760,
#125761,#125762,#125763,#125764,#125765,#125766,#125767,#125768,#125769,
#125770,#125771,#125772,#125773,#125774,#125775,#125776,#125777,#125778,
#125779,#125780,#125781,#125782,#125783,#125784,#125785,#125786,#125787,
#125788,#125789,#125790,#125791,#125792,#125793,#125794,#125795,#125796,
#125797,#125798,#125799,#125800,#125801,#125802,#125803),.UNSPECIFIED.,
 .F.,.F.)
B_SPLINE_CURVE_WITH_KNOTS((6,1,1,1,1,1,1,1,1,1,1,1,1,1,1,1,1,1,1,1,1,1,
1,1,1,1,1,1,1,1,1,1,1,1,1,1,1,1,1,1,1,1,1,1,1,1,1,1,1,1,1,1,1,1,1,1,1,1,
1,1,1,1,1,1,1,1,1,1,1,1,1,1,1,1,1,1,1,1,1,1,1,1,1,1,1,1,1,1,1,1,1,1,1,1,
1,1,1,1,1,1,1,1,1,1,1,1,1,1,1,1,1,1,1,1,1,1,1,1,1,1,1,1,1,1,1,1,1,1,1,1,
1,1,1,1,1,1,1,1,1,1,1,1,1,1,1,1,1,1,1,1,1,1,1,1,1,1,1,1,1,1,1,1,1,1,1,1,
1,1,1,1,1,1,1,1,1,1,1,1,1,1,1,1,1,1,1,1,1,1,1,6),(-0.941429844438069,-0.940000000000001,
-0.935000000000001,-0.930000000000001,-0.925000000000001,-0.920000000000001,
-0.915000000000001,-0.910000000000001,-0.905000000000001,-0.900000000000001,
-0.895000000000001,-0.890000000000001,-0.885000000000001,-0.880000000000001,
-0.875000000000001,-0.870000000000001,-0.865000000000001,-0.860000000000001,
-0.855000000000001,-0.850000000000001,-0.845000000000001,-0.840000000000001,
-0.835000000000001,-0.830000000000001,-0.825000000000001,-0.820000000000001,
-0.815000000000001,-0.810000000000001,-0.805000000000001,-0.800000000000001,
-0.795000000000001,-0.790000000000001,-0.785000000000001,-0.780000000000001,
-0.775000000000001,-0.770000000000001,-0.765000000000001,-0.760000000000001,
-0.755000000000001,-0.750000000000001,-0.745000000000001,-0.740000000000001,
-0.735000000000001,-0.730000000000001,-0.725000000000001,-0.720000000000001,
-0.715000000000001,-0.710000000000001,-0.705000000000001,-0.700000000000001,
-0.695000000000001,-0.690000000000001,-0.685,-0.68,-0.675,-0.67,-0.665,
-0.66,-0.655,-0.65,-0.645,-0.64,-0.635,-0.63,-0.625,-0.62,-0.615,-0.61,
-0.605,-0.6,-0.595,-0.59,-0.585,-0.58,-0.575,-0.57,-0.565,-0.56,-0.555,
-0.55,-0.545,-0.54,-0.535,-0.53,-0.525,-0.52,-0.515,-0.51,-0.505,-0.5,-0.495,
-0.49,-0.485,-0.48,-0.475,-0.47,-0.465,-0.46,-0.455,-0.45,-0.445,-0.44,
-0.435,-0.43,-0.425,-0.42,-0.415,-0.41,-0.405,-0.4,-0.395,-0.39,-0.385,
-0.38,-0.375,-0.37,-0.365,-0.36,-0.355,-0.35,-0.345,-0.34,-0.335,-0.33,
-0.325,-0.32,-0.315,-0.31,-0.305,-0.3,-0.295,-0.29,-0.285,-0.28,-0.275,
-0.27,-0.265,-0.26,-0.255,-0.25,-0.245,-0.24,-0.235,-0.23,-0.225,-0.22,
-0.215,-0.21,-0.205,-0.2,-0.195,-0.19,-0.185,-0.18,-0.175,-0.17,-0.165,
-0.16,-0.155,-0.15,-0.145,-0.14,-0.135,-0.13,-0.125,-0.12,-0.115,-0.11,
-0.105,-0.1,-0.095,-0.09,-0.085,-0.08,-0.075,-0.07,-0.065,-0.06,-0.055,
-0.05,-0.045,-0.04,-0.035,-0.03,-0.025,-0.02,-0.015,-0.01,-0.005,0.),
 .UNSPECIFIED.)
CURVE()
GEOMETRIC_REPRESENTATION_ITEM()
RATIONAL_B_SPLINE_CURVE((1.,1.,1.,1.,1.,1.,1.,1.,1.,1.,1.,1.,1.,1.,1.,1.,
1.,1.,1.,1.,1.,1.,1.,1.,1.,1.,1.,1.,1.,1.,1.,1.,1.,1.,1.,1.,1.,1.,1.,1.,
1.,1.,1.,1.,1.,1.,1.,1.,1.,1.,1.,1.,1.,1.,1.,1.,1.,1.,1.,1.,1.,1.,1.,1.,
1.,1.,1.,1.,1.,1.,1.,1.,1.,1.,1.,1.,1.,1.,1.,1.,1.,1.,1.,1.,1.,1.,1.,1.,
1.,1.,1.,1.,1.,1.,1.,1.,1.,1.,1.,1.,1.,1.,1.,1.,1.,1.,1.,1.,1.,1.,1.,1.,
1.,1.,1.,1.,1.,1.,1.,1.,1.,1.,1.,1.,1.,1.,1.,1.,1.,1.,1.,1.,1.,1.,1.,1.,
1.,1.,1.,1.,1.,1.,1.,1.,1.,1.,1.,1.,1.,1.,1.,1.,1.,1.,1.,1.,1.,1.,1.,1.,
1.,1.,1.,1.,1.,1.,1.,1.,1.,1.,1.,1.,1.,1.,1.,1.,1.,1.,1.,1.,1.,1.,1.,1.,
1.,1.,1.,1.,1.,1.,1.,1.,1.,1.))
REPRESENTATION_ITEM('')
);
#569=(
BOUNDED_CURVE()
B_SPLINE_CURVE(5,(#126215,#126216,#126217,#126218,#126219,#126220,#126221,
#126222,#126223,#126224,#126225,#126226,#126227,#126228,#126229,#126230,
#126231,#126232,#126233,#126234,#126235,#126236,#126237,#126238,#126239,
#126240,#126241,#126242,#126243,#126244,#126245,#126246,#126247,#126248,
#126249,#126250,#126251,#126252,#126253,#126254,#126255,#126256,#126257,
#126258,#126259,#126260,#126261,#126262,#126263,#126264,#126265,#126266,
#126267,#126268,#126269,#126270,#126271,#126272,#126273,#126274,#126275,
#126276,#126277,#126278,#126279,#126280,#126281,#126282,#126283,#126284,
#126285,#126286,#126287,#126288,#126289,#126290,#126291,#126292,#126293,
#126294,#126295,#126296,#126297,#126298,#126299,#126300,#126301,#126302,
#126303,#126304,#126305,#126306,#126307,#126308,#126309,#126310,#126311,
#126312,#126313,#126314,#126315,#126316,#126317,#126318,#126319,#126320,
#126321,#126322,#126323,#126324,#126325,#126326,#126327,#126328,#126329,
#126330,#126331,#126332,#126333,#126334,#126335,#126336,#126337,#126338,
#126339,#126340,#126341,#126342,#126343,#126344,#126345,#126346,#126347,
#126348,#126349,#126350,#126351,#126352,#126353,#126354,#126355,#126356,
#126357,#126358,#126359,#126360,#126361,#126362,#126363,#126364,#126365,
#126366,#126367,#126368,#126369,#126370,#126371,#126372,#126373,#126374,
#126375,#126376,#126377,#126378,#126379,#126380,#126381,#126382,#126383,
#126384,#126385,#126386,#126387,#126388,#126389,#126390,#126391,#126392,
#126393,#126394,#126395,#126396,#126397,#126398,#126399,#126400,#126401,
#126402,#126403,#126404,#126405,#126406,#126407,#126408),.UNSPECIFIED.,
 .F.,.F.)
B_SPLINE_CURVE_WITH_KNOTS((6,1,1,1,1,1,1,1,1,1,1,1,1,1,1,1,1,1,1,1,1,1,
1,1,1,1,1,1,1,1,1,1,1,1,1,1,1,1,1,1,1,1,1,1,1,1,1,1,1,1,1,1,1,1,1,1,1,1,
1,1,1,1,1,1,1,1,1,1,1,1,1,1,1,1,1,1,1,1,1,1,1,1,1,1,1,1,1,1,1,1,1,1,1,1,
1,1,1,1,1,1,1,1,1,1,1,1,1,1,1,1,1,1,1,1,1,1,1,1,1,1,1,1,1,1,1,1,1,1,1,1,
1,1,1,1,1,1,1,1,1,1,1,1,1,1,1,1,1,1,1,1,1,1,1,1,1,1,1,1,1,1,1,1,1,1,1,1,
1,1,1,1,1,1,1,1,1,1,1,1,1,1,1,1,1,1,1,1,1,1,1,6),(0.,0.005,0.01,0.015,0.02,
0.025,0.03,0.035,0.04,0.045,0.05,0.055,0.06,0.065,0.07,0.075,0.08,0.085,
0.09,0.095,0.1,0.105,0.11,0.115,0.12,0.125,0.13,0.135,0.14,0.145,0.15,0.155,
0.16,0.165,0.17,0.175,0.18,0.185,0.19,0.195,0.2,0.205,0.21,0.215,0.22,0.225,
0.23,0.235,0.24,0.245,0.25,0.255,0.26,0.265,0.27,0.275,0.28,0.285,0.29,
0.295,0.3,0.305,0.31,0.315,0.32,0.325,0.33,0.335,0.34,0.345,0.35,0.355,
0.36,0.365,0.37,0.375,0.38,0.385,0.39,0.395,0.4,0.405,0.41,0.415,0.42,0.425,
0.43,0.435,0.44,0.445,0.45,0.455,0.46,0.465,0.47,0.475,0.48,0.485,0.49,
0.495,0.5,0.505,0.51,0.515,0.52,0.525,0.53,0.535,0.54,0.545,0.55,0.555,
0.56,0.565,0.57,0.575,0.58,0.585,0.59,0.595,0.6,0.605,0.61,0.615,0.62,0.625,
0.63,0.635,0.64,0.645,0.65,0.655,0.66,0.665,0.67,0.675,0.68,0.685,0.690000000000001,
0.695000000000001,0.700000000000001,0.705000000000001,0.710000000000001,
0.715000000000001,0.720000000000001,0.725000000000001,0.730000000000001,
0.735000000000001,0.740000000000001,0.745000000000001,0.750000000000001,
0.755000000000001,0.760000000000001,0.765000000000001,0.770000000000001,
0.775000000000001,0.780000000000001,0.785000000000001,0.790000000000001,
0.795000000000001,0.800000000000001,0.805000000000001,0.810000000000001,
0.815000000000001,0.820000000000001,0.825000000000001,0.830000000000001,
0.835000000000001,0.840000000000001,0.845000000000001,0.850000000000001,
0.855000000000001,0.860000000000001,0.865000000000001,0.870000000000001,
0.875000000000001,0.880000000000001,0.885000000000001,0.890000000000001,
0.895000000000001,0.900000000000001,0.905000000000001,0.910000000000001,
0.915000000000001,0.920000000000001,0.925000000000001,0.930000000000001,
0.935000000000001,0.940000000000001,0.941429844438209),.UNSPECIFIED.)
CURVE()
GEOMETRIC_REPRESENTATION_ITEM()
RATIONAL_B_SPLINE_CURVE((1.,1.,1.,1.,1.,1.,1.,1.,1.,1.,1.,1.,1.,1.,1.,1.,
1.,1.,1.,1.,1.,1.,1.,1.,1.,1.,1.,1.,1.,1.,1.,1.,1.,1.,1.,1.,1.,1.,1.,1.,
1.,1.,1.,1.,1.,1.,1.,1.,1.,1.,1.,1.,1.,1.,1.,1.,1.,1.,1.,1.,1.,1.,1.,1.,
1.,1.,1.,1.,1.,1.,1.,1.,1.,1.,1.,1.,1.,1.,1.,1.,1.,1.,1.,1.,1.,1.,1.,1.,
1.,1.,1.,1.,1.,1.,1.,1.,1.,1.,1.,1.,1.,1.,1.,1.,1.,1.,1.,1.,1.,1.,1.,1.,
1.,1.,1.,1.,1.,1.,1.,1.,1.,1.,1.,1.,1.,1.,1.,1.,1.,1.,1.,1.,1.,1.,1.,1.,
1.,1.,1.,1.,1.,1.,1.,1.,1.,1.,1.,1.,1.,1.,1.,1.,1.,1.,1.,1.,1.,1.,1.,1.,
1.,1.,1.,1.,1.,1.,1.,1.,1.,1.,1.,1.,1.,1.,1.,1.,1.,1.,1.,1.,1.,1.,1.,1.,
1.,1.,1.,1.,1.,1.,1.,1.,1.,1.))
REPRESENTATION_ITEM('')
);
#570=(
BOUNDED_CURVE()
B_SPLINE_CURVE(5,(#126411,#126412,#126413,#126414,#126415,#126416,#126417,
#126418,#126419,#126420,#126421,#126422,#126423,#126424,#126425,#126426,
#126427,#126428,#126429,#126430,#126431,#126432,#126433,#126434,#126435,
#126436,#126437,#126438,#126439,#126440,#126441,#126442,#126443,#126444,
#126445,#126446,#126447,#126448,#126449,#126450,#126451,#126452,#126453,
#126454,#126455,#126456,#126457,#126458,#126459,#126460,#126461,#126462,
#126463,#126464,#126465,#126466,#126467,#126468,#126469,#126470,#126471,
#126472,#126473,#126474,#126475,#126476,#126477,#126478,#126479,#126480,
#126481,#126482,#126483,#126484,#126485,#126486,#126487,#126488,#126489,
#126490,#126491,#126492,#126493,#126494,#126495,#126496,#126497,#126498,
#126499,#126500,#126501,#126502,#126503,#126504,#126505,#126506,#126507,
#126508,#126509,#126510,#126511,#126512,#126513,#126514,#126515,#126516,
#126517,#126518,#126519,#126520,#126521,#126522,#126523,#126524,#126525,
#126526,#126527,#126528,#126529,#126530,#126531,#126532,#126533,#126534,
#126535,#126536,#126537,#126538,#126539,#126540,#126541,#126542,#126543,
#126544,#126545,#126546,#126547,#126548,#126549,#126550,#126551,#126552,
#126553,#126554,#126555,#126556,#126557,#126558,#126559,#126560,#126561,
#126562,#126563,#126564,#126565,#126566,#126567,#126568,#126569,#126570,
#126571,#126572,#126573,#126574,#126575,#126576,#126577,#126578,#126579,
#126580,#126581,#126582,#126583,#126584,#126585,#126586,#126587,#126588,
#126589,#126590,#126591,#126592,#126593,#126594,#126595,#126596,#126597,
#126598,#126599,#126600,#126601,#126602,#126603,#126604),.UNSPECIFIED.,
 .F.,.F.)
B_SPLINE_CURVE_WITH_KNOTS((6,1,1,1,1,1,1,1,1,1,1,1,1,1,1,1,1,1,1,1,1,1,
1,1,1,1,1,1,1,1,1,1,1,1,1,1,1,1,1,1,1,1,1,1,1,1,1,1,1,1,1,1,1,1,1,1,1,1,
1,1,1,1,1,1,1,1,1,1,1,1,1,1,1,1,1,1,1,1,1,1,1,1,1,1,1,1,1,1,1,1,1,1,1,1,
1,1,1,1,1,1,1,1,1,1,1,1,1,1,1,1,1,1,1,1,1,1,1,1,1,1,1,1,1,1,1,1,1,1,1,1,
1,1,1,1,1,1,1,1,1,1,1,1,1,1,1,1,1,1,1,1,1,1,1,1,1,1,1,1,1,1,1,1,1,1,1,1,
1,1,1,1,1,1,1,1,1,1,1,1,1,1,1,1,1,1,1,1,1,1,1,6),(-0.941429844438221,-0.940000000000001,
-0.935000000000001,-0.930000000000001,-0.925000000000001,-0.920000000000001,
-0.915000000000001,-0.910000000000001,-0.905000000000001,-0.900000000000001,
-0.895000000000001,-0.890000000000001,-0.885000000000001,-0.880000000000001,
-0.875000000000001,-0.870000000000001,-0.865000000000001,-0.860000000000001,
-0.855000000000001,-0.850000000000001,-0.845000000000001,-0.840000000000001,
-0.835000000000001,-0.830000000000001,-0.825000000000001,-0.820000000000001,
-0.815000000000001,-0.810000000000001,-0.805000000000001,-0.800000000000001,
-0.795000000000001,-0.790000000000001,-0.785000000000001,-0.780000000000001,
-0.775000000000001,-0.770000000000001,-0.765000000000001,-0.760000000000001,
-0.755000000000001,-0.750000000000001,-0.745000000000001,-0.740000000000001,
-0.735000000000001,-0.730000000000001,-0.725000000000001,-0.720000000000001,
-0.715000000000001,-0.710000000000001,-0.705000000000001,-0.700000000000001,
-0.695000000000001,-0.690000000000001,-0.685,-0.68,-0.675,-0.67,-0.665,
-0.66,-0.655,-0.65,-0.645,-0.64,-0.635,-0.63,-0.625,-0.62,-0.615,-0.61,
-0.605,-0.6,-0.595,-0.59,-0.585,-0.58,-0.575,-0.57,-0.565,-0.56,-0.555,
-0.55,-0.545,-0.54,-0.535,-0.53,-0.525,-0.52,-0.515,-0.51,-0.505,-0.5,-0.495,
-0.49,-0.485,-0.48,-0.475,-0.47,-0.465,-0.46,-0.455,-0.45,-0.445,-0.44,
-0.435,-0.43,-0.425,-0.42,-0.415,-0.41,-0.405,-0.4,-0.395,-0.39,-0.385,
-0.38,-0.375,-0.37,-0.365,-0.36,-0.355,-0.35,-0.345,-0.34,-0.335,-0.33,
-0.325,-0.32,-0.315,-0.31,-0.305,-0.3,-0.295,-0.29,-0.285,-0.28,-0.275,
-0.27,-0.265,-0.26,-0.255,-0.25,-0.245,-0.24,-0.235,-0.23,-0.225,-0.22,
-0.215,-0.21,-0.205,-0.2,-0.195,-0.19,-0.185,-0.18,-0.175,-0.17,-0.165,
-0.16,-0.155,-0.15,-0.145,-0.14,-0.135,-0.13,-0.125,-0.12,-0.115,-0.11,
-0.105,-0.1,-0.095,-0.09,-0.085,-0.08,-0.075,-0.07,-0.065,-0.06,-0.055,
-0.05,-0.045,-0.04,-0.035,-0.03,-0.025,-0.02,-0.015,-0.01,-0.005,0.),
 .UNSPECIFIED.)
CURVE()
GEOMETRIC_REPRESENTATION_ITEM()
RATIONAL_B_SPLINE_CURVE((1.,1.,1.,1.,1.,1.,1.,1.,1.,1.,1.,1.,1.,1.,1.,1.,
1.,1.,1.,1.,1.,1.,1.,1.,1.,1.,1.,1.,1.,1.,1.,1.,1.,1.,1.,1.,1.,1.,1.,1.,
1.,1.,1.,1.,1.,1.,1.,1.,1.,1.,1.,1.,1.,1.,1.,1.,1.,1.,1.,1.,1.,1.,1.,1.,
1.,1.,1.,1.,1.,1.,1.,1.,1.,1.,1.,1.,1.,1.,1.,1.,1.,1.,1.,1.,1.,1.,1.,1.,
1.,1.,1.,1.,1.,1.,1.,1.,1.,1.,1.,1.,1.,1.,1.,1.,1.,1.,1.,1.,1.,1.,1.,1.,
1.,1.,1.,1.,1.,1.,1.,1.,1.,1.,1.,1.,1.,1.,1.,1.,1.,1.,1.,1.,1.,1.,1.,1.,
1.,1.,1.,1.,1.,1.,1.,1.,1.,1.,1.,1.,1.,1.,1.,1.,1.,1.,1.,1.,1.,1.,1.,1.,
1.,1.,1.,1.,1.,1.,1.,1.,1.,1.,1.,1.,1.,1.,1.,1.,1.,1.,1.,1.,1.,1.,1.,1.,
1.,1.,1.,1.,1.,1.,1.,1.,1.,1.))
REPRESENTATION_ITEM('')
);
#571=(
BOUNDED_CURVE()
B_SPLINE_CURVE(5,(#127016,#127017,#127018,#127019,#127020,#127021,#127022,
#127023,#127024,#127025,#127026,#127027,#127028,#127029,#127030,#127031,
#127032,#127033,#127034,#127035,#127036,#127037,#127038,#127039,#127040,
#127041,#127042,#127043,#127044,#127045,#127046,#127047,#127048,#127049,
#127050,#127051,#127052,#127053,#127054,#127055,#127056,#127057,#127058,
#127059,#127060,#127061,#127062,#127063,#127064,#127065,#127066,#127067,
#127068,#127069,#127070,#127071,#127072,#127073,#127074,#127075,#127076,
#127077,#127078,#127079,#127080,#127081,#127082,#127083,#127084,#127085,
#127086,#127087,#127088,#127089,#127090,#127091,#127092,#127093,#127094,
#127095,#127096,#127097,#127098,#127099,#127100,#127101,#127102,#127103,
#127104,#127105,#127106,#127107,#127108,#127109,#127110,#127111,#127112,
#127113,#127114,#127115,#127116,#127117,#127118,#127119,#127120,#127121,
#127122,#127123,#127124,#127125,#127126,#127127,#127128,#127129,#127130,
#127131,#127132,#127133,#127134,#127135,#127136,#127137,#127138,#127139,
#127140,#127141,#127142,#127143,#127144,#127145,#127146,#127147,#127148,
#127149,#127150,#127151,#127152,#127153,#127154,#127155,#127156,#127157,
#127158,#127159,#127160,#127161,#127162,#127163,#127164,#127165,#127166,
#127167,#127168,#127169,#127170,#127171,#127172,#127173,#127174,#127175,
#127176,#127177,#127178,#127179,#127180,#127181,#127182,#127183,#127184,
#127185,#127186,#127187,#127188,#127189,#127190,#127191,#127192,#127193,
#127194,#127195,#127196,#127197,#127198,#127199,#127200,#127201,#127202,
#127203,#127204,#127205,#127206,#127207,#127208,#127209),.UNSPECIFIED.,
 .F.,.F.)
B_SPLINE_CURVE_WITH_KNOTS((6,1,1,1,1,1,1,1,1,1,1,1,1,1,1,1,1,1,1,1,1,1,
1,1,1,1,1,1,1,1,1,1,1,1,1,1,1,1,1,1,1,1,1,1,1,1,1,1,1,1,1,1,1,1,1,1,1,1,
1,1,1,1,1,1,1,1,1,1,1,1,1,1,1,1,1,1,1,1,1,1,1,1,1,1,1,1,1,1,1,1,1,1,1,1,
1,1,1,1,1,1,1,1,1,1,1,1,1,1,1,1,1,1,1,1,1,1,1,1,1,1,1,1,1,1,1,1,1,1,1,1,
1,1,1,1,1,1,1,1,1,1,1,1,1,1,1,1,1,1,1,1,1,1,1,1,1,1,1,1,1,1,1,1,1,1,1,1,
1,1,1,1,1,1,1,1,1,1,1,1,1,1,1,1,1,1,1,1,1,1,1,6),(0.,0.005,0.01,0.015,0.02,
0.025,0.03,0.035,0.04,0.045,0.05,0.055,0.06,0.065,0.07,0.075,0.08,0.085,
0.09,0.095,0.1,0.105,0.11,0.115,0.12,0.125,0.13,0.135,0.14,0.145,0.15,0.155,
0.16,0.165,0.17,0.175,0.18,0.185,0.19,0.195,0.2,0.205,0.21,0.215,0.22,0.225,
0.23,0.235,0.24,0.245,0.25,0.255,0.26,0.265,0.27,0.275,0.28,0.285,0.29,
0.295,0.3,0.305,0.31,0.315,0.32,0.325,0.33,0.335,0.34,0.345,0.35,0.355,
0.36,0.365,0.37,0.375,0.38,0.385,0.39,0.395,0.4,0.405,0.41,0.415,0.42,0.425,
0.43,0.435,0.44,0.445,0.45,0.455,0.46,0.465,0.47,0.475,0.48,0.485,0.49,
0.495,0.5,0.505,0.51,0.515,0.52,0.525,0.53,0.535,0.54,0.545,0.55,0.555,
0.56,0.565,0.57,0.575,0.58,0.585,0.59,0.595,0.6,0.605,0.61,0.615,0.62,0.625,
0.63,0.635,0.64,0.645,0.65,0.655,0.66,0.665,0.67,0.675,0.68,0.685,0.690000000000001,
0.695000000000001,0.700000000000001,0.705000000000001,0.710000000000001,
0.715000000000001,0.720000000000001,0.725000000000001,0.730000000000001,
0.735000000000001,0.740000000000001,0.745000000000001,0.750000000000001,
0.755000000000001,0.760000000000001,0.765000000000001,0.770000000000001,
0.775000000000001,0.780000000000001,0.785000000000001,0.790000000000001,
0.795000000000001,0.800000000000001,0.805000000000001,0.810000000000001,
0.815000000000001,0.820000000000001,0.825000000000001,0.830000000000001,
0.835000000000001,0.840000000000001,0.845000000000001,0.850000000000001,
0.855000000000001,0.860000000000001,0.865000000000001,0.870000000000001,
0.875000000000001,0.880000000000001,0.885000000000001,0.890000000000001,
0.895000000000001,0.900000000000001,0.905000000000001,0.910000000000001,
0.915000000000001,0.920000000000001,0.925000000000001,0.930000000000001,
0.935000000000001,0.940000000000001,0.941429844438077),.UNSPECIFIED.)
CURVE()
GEOMETRIC_REPRESENTATION_ITEM()
RATIONAL_B_SPLINE_CURVE((1.,1.,1.,1.,1.,1.,1.,1.,1.,1.,1.,1.,1.,1.,1.,1.,
1.,1.,1.,1.,1.,1.,1.,1.,1.,1.,1.,1.,1.,1.,1.,1.,1.,1.,1.,1.,1.,1.,1.,1.,
1.,1.,1.,1.,1.,1.,1.,1.,1.,1.,1.,1.,1.,1.,1.,1.,1.,1.,1.,1.,1.,1.,1.,1.,
1.,1.,1.,1.,1.,1.,1.,1.,1.,1.,1.,1.,1.,1.,1.,1.,1.,1.,1.,1.,1.,1.,1.,1.,
1.,1.,1.,1.,1.,1.,1.,1.,1.,1.,1.,1.,1.,1.,1.,1.,1.,1.,1.,1.,1.,1.,1.,1.,
1.,1.,1.,1.,1.,1.,1.,1.,1.,1.,1.,1.,1.,1.,1.,1.,1.,1.,1.,1.,1.,1.,1.,1.,
1.,1.,1.,1.,1.,1.,1.,1.,1.,1.,1.,1.,1.,1.,1.,1.,1.,1.,1.,1.,1.,1.,1.,1.,
1.,1.,1.,1.,1.,1.,1.,1.,1.,1.,1.,1.,1.,1.,1.,1.,1.,1.,1.,1.,1.,1.,1.,1.,
1.,1.,1.,1.,1.,1.,1.,1.,1.,1.))
REPRESENTATION_ITEM('')
);
#572=(
BOUNDED_CURVE()
B_SPLINE_CURVE(5,(#127212,#127213,#127214,#127215,#127216,#127217,#127218,
#127219,#127220,#127221,#127222,#127223,#127224,#127225,#127226,#127227,
#127228,#127229,#127230,#127231,#127232,#127233,#127234,#127235,#127236,
#127237,#127238,#127239,#127240,#127241,#127242,#127243,#127244,#127245,
#127246,#127247,#127248,#127249,#127250,#127251,#127252,#127253,#127254,
#127255,#127256,#127257,#127258,#127259,#127260,#127261,#127262,#127263,
#127264,#127265,#127266,#127267,#127268,#127269,#127270,#127271,#127272,
#127273,#127274,#127275,#127276,#127277,#127278,#127279,#127280,#127281,
#127282,#127283,#127284,#127285,#127286,#127287,#127288,#127289,#127290,
#127291,#127292,#127293,#127294,#127295,#127296,#127297,#127298,#127299,
#127300,#127301,#127302,#127303,#127304,#127305,#127306,#127307,#127308,
#127309,#127310,#127311,#127312,#127313,#127314,#127315,#127316,#127317,
#127318,#127319,#127320,#127321,#127322,#127323,#127324,#127325,#127326,
#127327,#127328,#127329,#127330,#127331,#127332,#127333,#127334,#127335,
#127336,#127337,#127338,#127339,#127340,#127341,#127342,#127343,#127344,
#127345,#127346,#127347,#127348,#127349,#127350,#127351,#127352,#127353,
#127354,#127355,#127356,#127357,#127358,#127359,#127360,#127361,#127362,
#127363,#127364,#127365,#127366,#127367,#127368,#127369,#127370,#127371,
#127372,#127373,#127374,#127375,#127376,#127377,#127378,#127379,#127380,
#127381,#127382,#127383,#127384,#127385,#127386,#127387,#127388,#127389,
#127390,#127391,#127392,#127393,#127394,#127395,#127396,#127397,#127398,
#127399,#127400,#127401,#127402,#127403,#127404,#127405),.UNSPECIFIED.,
 .F.,.F.)
B_SPLINE_CURVE_WITH_KNOTS((6,1,1,1,1,1,1,1,1,1,1,1,1,1,1,1,1,1,1,1,1,1,
1,1,1,1,1,1,1,1,1,1,1,1,1,1,1,1,1,1,1,1,1,1,1,1,1,1,1,1,1,1,1,1,1,1,1,1,
1,1,1,1,1,1,1,1,1,1,1,1,1,1,1,1,1,1,1,1,1,1,1,1,1,1,1,1,1,1,1,1,1,1,1,1,
1,1,1,1,1,1,1,1,1,1,1,1,1,1,1,1,1,1,1,1,1,1,1,1,1,1,1,1,1,1,1,1,1,1,1,1,
1,1,1,1,1,1,1,1,1,1,1,1,1,1,1,1,1,1,1,1,1,1,1,1,1,1,1,1,1,1,1,1,1,1,1,1,
1,1,1,1,1,1,1,1,1,1,1,1,1,1,1,1,1,1,1,1,1,1,1,6),(-0.941429844438077,-0.940000000000001,
-0.935000000000001,-0.930000000000001,-0.925000000000001,-0.920000000000001,
-0.915000000000001,-0.910000000000001,-0.905000000000001,-0.900000000000001,
-0.895000000000001,-0.890000000000001,-0.885000000000001,-0.880000000000001,
-0.875000000000001,-0.870000000000001,-0.865000000000001,-0.860000000000001,
-0.855000000000001,-0.850000000000001,-0.845000000000001,-0.840000000000001,
-0.835000000000001,-0.830000000000001,-0.825000000000001,-0.820000000000001,
-0.815000000000001,-0.810000000000001,-0.805000000000001,-0.800000000000001,
-0.795000000000001,-0.790000000000001,-0.785000000000001,-0.780000000000001,
-0.775000000000001,-0.770000000000001,-0.765000000000001,-0.760000000000001,
-0.755000000000001,-0.750000000000001,-0.745000000000001,-0.740000000000001,
-0.735000000000001,-0.730000000000001,-0.725000000000001,-0.720000000000001,
-0.715000000000001,-0.710000000000001,-0.705000000000001,-0.700000000000001,
-0.695000000000001,-0.690000000000001,-0.685,-0.68,-0.675,-0.67,-0.665,
-0.66,-0.655,-0.65,-0.645,-0.64,-0.635,-0.63,-0.625,-0.62,-0.615,-0.61,
-0.605,-0.6,-0.595,-0.59,-0.585,-0.58,-0.575,-0.57,-0.565,-0.56,-0.555,
-0.55,-0.545,-0.54,-0.535,-0.53,-0.525,-0.52,-0.515,-0.51,-0.505,-0.5,-0.495,
-0.49,-0.485,-0.48,-0.475,-0.47,-0.465,-0.46,-0.455,-0.45,-0.445,-0.44,
-0.435,-0.43,-0.425,-0.42,-0.415,-0.41,-0.405,-0.4,-0.395,-0.39,-0.385,
-0.38,-0.375,-0.37,-0.365,-0.36,-0.355,-0.35,-0.345,-0.34,-0.335,-0.33,
-0.325,-0.32,-0.315,-0.31,-0.305,-0.3,-0.295,-0.29,-0.285,-0.28,-0.275,
-0.27,-0.265,-0.26,-0.255,-0.25,-0.245,-0.24,-0.235,-0.23,-0.225,-0.22,
-0.215,-0.21,-0.205,-0.2,-0.195,-0.19,-0.185,-0.18,-0.175,-0.17,-0.165,
-0.16,-0.155,-0.15,-0.145,-0.14,-0.135,-0.13,-0.125,-0.12,-0.115,-0.11,
-0.105,-0.1,-0.095,-0.09,-0.085,-0.08,-0.075,-0.07,-0.065,-0.06,-0.055,
-0.05,-0.045,-0.04,-0.035,-0.03,-0.025,-0.02,-0.015,-0.01,-0.005,0.),
 .UNSPECIFIED.)
CURVE()
GEOMETRIC_REPRESENTATION_ITEM()
RATIONAL_B_SPLINE_CURVE((1.,1.,1.,1.,1.,1.,1.,1.,1.,1.,1.,1.,1.,1.,1.,1.,
1.,1.,1.,1.,1.,1.,1.,1.,1.,1.,1.,1.,1.,1.,1.,1.,1.,1.,1.,1.,1.,1.,1.,1.,
1.,1.,1.,1.,1.,1.,1.,1.,1.,1.,1.,1.,1.,1.,1.,1.,1.,1.,1.,1.,1.,1.,1.,1.,
1.,1.,1.,1.,1.,1.,1.,1.,1.,1.,1.,1.,1.,1.,1.,1.,1.,1.,1.,1.,1.,1.,1.,1.,
1.,1.,1.,1.,1.,1.,1.,1.,1.,1.,1.,1.,1.,1.,1.,1.,1.,1.,1.,1.,1.,1.,1.,1.,
1.,1.,1.,1.,1.,1.,1.,1.,1.,1.,1.,1.,1.,1.,1.,1.,1.,1.,1.,1.,1.,1.,1.,1.,
1.,1.,1.,1.,1.,1.,1.,1.,1.,1.,1.,1.,1.,1.,1.,1.,1.,1.,1.,1.,1.,1.,1.,1.,
1.,1.,1.,1.,1.,1.,1.,1.,1.,1.,1.,1.,1.,1.,1.,1.,1.,1.,1.,1.,1.,1.,1.,1.,
1.,1.,1.,1.,1.,1.,1.,1.,1.,1.))
REPRESENTATION_ITEM('')
);
#573=(
BOUNDED_CURVE()
B_SPLINE_CURVE(5,(#127817,#127818,#127819,#127820,#127821,#127822,#127823,
#127824,#127825,#127826,#127827,#127828,#127829,#127830,#127831,#127832,
#127833,#127834,#127835,#127836,#127837,#127838,#127839,#127840,#127841,
#127842,#127843,#127844,#127845,#127846,#127847,#127848,#127849,#127850,
#127851,#127852,#127853,#127854,#127855,#127856,#127857,#127858,#127859,
#127860,#127861,#127862,#127863,#127864,#127865,#127866,#127867,#127868,
#127869,#127870,#127871,#127872,#127873,#127874,#127875,#127876,#127877,
#127878,#127879,#127880,#127881,#127882,#127883,#127884,#127885,#127886,
#127887,#127888,#127889,#127890,#127891,#127892,#127893,#127894,#127895,
#127896,#127897,#127898,#127899,#127900,#127901,#127902,#127903,#127904,
#127905,#127906,#127907,#127908,#127909,#127910,#127911,#127912,#127913,
#127914,#127915,#127916,#127917,#127918,#127919,#127920,#127921,#127922,
#127923,#127924,#127925,#127926,#127927,#127928,#127929,#127930,#127931,
#127932,#127933,#127934,#127935,#127936,#127937,#127938,#127939,#127940,
#127941,#127942,#127943,#127944,#127945,#127946,#127947,#127948,#127949,
#127950,#127951,#127952,#127953,#127954,#127955,#127956,#127957,#127958,
#127959,#127960,#127961,#127962,#127963,#127964,#127965,#127966,#127967,
#127968,#127969,#127970,#127971,#127972,#127973,#127974,#127975,#127976,
#127977,#127978,#127979,#127980,#127981,#127982,#127983,#127984,#127985,
#127986,#127987,#127988,#127989,#127990,#127991,#127992,#127993,#127994,
#127995,#127996,#127997,#127998,#127999,#128000,#128001,#128002,#128003,
#128004,#128005,#128006,#128007,#128008,#128009,#128010),.UNSPECIFIED.,
 .F.,.F.)
B_SPLINE_CURVE_WITH_KNOTS((6,1,1,1,1,1,1,1,1,1,1,1,1,1,1,1,1,1,1,1,1,1,
1,1,1,1,1,1,1,1,1,1,1,1,1,1,1,1,1,1,1,1,1,1,1,1,1,1,1,1,1,1,1,1,1,1,1,1,
1,1,1,1,1,1,1,1,1,1,1,1,1,1,1,1,1,1,1,1,1,1,1,1,1,1,1,1,1,1,1,1,1,1,1,1,
1,1,1,1,1,1,1,1,1,1,1,1,1,1,1,1,1,1,1,1,1,1,1,1,1,1,1,1,1,1,1,1,1,1,1,1,
1,1,1,1,1,1,1,1,1,1,1,1,1,1,1,1,1,1,1,1,1,1,1,1,1,1,1,1,1,1,1,1,1,1,1,1,
1,1,1,1,1,1,1,1,1,1,1,1,1,1,1,1,1,1,1,1,1,1,1,6),(0.,0.005,0.01,0.015,0.02,
0.025,0.03,0.035,0.04,0.045,0.05,0.055,0.06,0.065,0.07,0.075,0.08,0.085,
0.09,0.095,0.1,0.105,0.11,0.115,0.12,0.125,0.13,0.135,0.14,0.145,0.15,0.155,
0.16,0.165,0.17,0.175,0.18,0.185,0.19,0.195,0.2,0.205,0.21,0.215,0.22,0.225,
0.23,0.235,0.24,0.245,0.25,0.255,0.26,0.265,0.27,0.275,0.28,0.285,0.29,
0.295,0.3,0.305,0.31,0.315,0.32,0.325,0.33,0.335,0.34,0.345,0.35,0.355,
0.36,0.365,0.37,0.375,0.38,0.385,0.39,0.395,0.4,0.405,0.41,0.415,0.42,0.425,
0.43,0.435,0.44,0.445,0.45,0.455,0.46,0.465,0.47,0.475,0.48,0.485,0.49,
0.495,0.5,0.505,0.51,0.515,0.52,0.525,0.53,0.535,0.54,0.545,0.55,0.555,
0.56,0.565,0.57,0.575,0.58,0.585,0.59,0.595,0.6,0.605,0.61,0.615,0.62,0.625,
0.63,0.635,0.64,0.645,0.65,0.655,0.66,0.665,0.67,0.675,0.68,0.685,0.690000000000001,
0.695000000000001,0.700000000000001,0.705000000000001,0.710000000000001,
0.715000000000001,0.720000000000001,0.725000000000001,0.730000000000001,
0.735000000000001,0.740000000000001,0.745000000000001,0.750000000000001,
0.755000000000001,0.760000000000001,0.765000000000001,0.770000000000001,
0.775000000000001,0.780000000000001,0.785000000000001,0.790000000000001,
0.795000000000001,0.800000000000001,0.805000000000001,0.810000000000001,
0.815000000000001,0.820000000000001,0.825000000000001,0.830000000000001,
0.835000000000001,0.840000000000001,0.845000000000001,0.850000000000001,
0.855000000000001,0.860000000000001,0.865000000000001,0.870000000000001,
0.875000000000001,0.880000000000001,0.885000000000001,0.890000000000001,
0.895000000000001,0.900000000000001,0.905000000000001,0.910000000000001,
0.915000000000001,0.920000000000001,0.925000000000001,0.930000000000001,
0.935000000000001,0.940000000000001,0.94142984443807),.UNSPECIFIED.)
CURVE()
GEOMETRIC_REPRESENTATION_ITEM()
RATIONAL_B_SPLINE_CURVE((1.,1.,1.,1.,1.,1.,1.,1.,1.,1.,1.,1.,1.,1.,1.,1.,
1.,1.,1.,1.,1.,1.,1.,1.,1.,1.,1.,1.,1.,1.,1.,1.,1.,1.,1.,1.,1.,1.,1.,1.,
1.,1.,1.,1.,1.,1.,1.,1.,1.,1.,1.,1.,1.,1.,1.,1.,1.,1.,1.,1.,1.,1.,1.,1.,
1.,1.,1.,1.,1.,1.,1.,1.,1.,1.,1.,1.,1.,1.,1.,1.,1.,1.,1.,1.,1.,1.,1.,1.,
1.,1.,1.,1.,1.,1.,1.,1.,1.,1.,1.,1.,1.,1.,1.,1.,1.,1.,1.,1.,1.,1.,1.,1.,
1.,1.,1.,1.,1.,1.,1.,1.,1.,1.,1.,1.,1.,1.,1.,1.,1.,1.,1.,1.,1.,1.,1.,1.,
1.,1.,1.,1.,1.,1.,1.,1.,1.,1.,1.,1.,1.,1.,1.,1.,1.,1.,1.,1.,1.,1.,1.,1.,
1.,1.,1.,1.,1.,1.,1.,1.,1.,1.,1.,1.,1.,1.,1.,1.,1.,1.,1.,1.,1.,1.,1.,1.,
1.,1.,1.,1.,1.,1.,1.,1.,1.,1.))
REPRESENTATION_ITEM('')
);
#574=(
BOUNDED_CURVE()
B_SPLINE_CURVE(5,(#128013,#128014,#128015,#128016,#128017,#128018,#128019,
#128020,#128021,#128022,#128023,#128024,#128025,#128026,#128027,#128028,
#128029,#128030,#128031,#128032,#128033,#128034,#128035,#128036,#128037,
#128038,#128039,#128040,#128041,#128042,#128043,#128044,#128045,#128046,
#128047,#128048,#128049,#128050,#128051,#128052,#128053,#128054,#128055,
#128056,#128057,#128058,#128059,#128060,#128061,#128062,#128063,#128064,
#128065,#128066,#128067,#128068,#128069,#128070,#128071,#128072,#128073,
#128074,#128075,#128076,#128077,#128078,#128079,#128080,#128081,#128082,
#128083,#128084,#128085,#128086,#128087,#128088,#128089,#128090,#128091,
#128092,#128093,#128094,#128095,#128096,#128097,#128098,#128099,#128100,
#128101,#128102,#128103,#128104,#128105,#128106,#128107,#128108,#128109,
#128110,#128111,#128112,#128113,#128114,#128115,#128116,#128117,#128118,
#128119,#128120,#128121,#128122,#128123,#128124,#128125,#128126,#128127,
#128128,#128129,#128130,#128131,#128132,#128133,#128134,#128135,#128136,
#128137,#128138,#128139,#128140,#128141,#128142,#128143,#128144,#128145,
#128146,#128147,#128148,#128149,#128150,#128151,#128152,#128153,#128154,
#128155,#128156,#128157,#128158,#128159,#128160,#128161,#128162,#128163,
#128164,#128165,#128166,#128167,#128168,#128169,#128170,#128171,#128172,
#128173,#128174,#128175,#128176,#128177,#128178,#128179,#128180,#128181,
#128182,#128183,#128184,#128185,#128186,#128187,#128188,#128189,#128190,
#128191,#128192,#128193,#128194,#128195,#128196,#128197,#128198,#128199,
#128200,#128201,#128202,#128203,#128204,#128205,#128206),.UNSPECIFIED.,
 .F.,.F.)
B_SPLINE_CURVE_WITH_KNOTS((6,1,1,1,1,1,1,1,1,1,1,1,1,1,1,1,1,1,1,1,1,1,
1,1,1,1,1,1,1,1,1,1,1,1,1,1,1,1,1,1,1,1,1,1,1,1,1,1,1,1,1,1,1,1,1,1,1,1,
1,1,1,1,1,1,1,1,1,1,1,1,1,1,1,1,1,1,1,1,1,1,1,1,1,1,1,1,1,1,1,1,1,1,1,1,
1,1,1,1,1,1,1,1,1,1,1,1,1,1,1,1,1,1,1,1,1,1,1,1,1,1,1,1,1,1,1,1,1,1,1,1,
1,1,1,1,1,1,1,1,1,1,1,1,1,1,1,1,1,1,1,1,1,1,1,1,1,1,1,1,1,1,1,1,1,1,1,1,
1,1,1,1,1,1,1,1,1,1,1,1,1,1,1,1,1,1,1,1,1,1,1,6),(-0.941429844438071,-0.940000000000001,
-0.935000000000001,-0.930000000000001,-0.925000000000001,-0.920000000000001,
-0.915000000000001,-0.910000000000001,-0.905000000000001,-0.900000000000001,
-0.895000000000001,-0.890000000000001,-0.885000000000001,-0.880000000000001,
-0.875000000000001,-0.870000000000001,-0.865000000000001,-0.860000000000001,
-0.855000000000001,-0.850000000000001,-0.845000000000001,-0.840000000000001,
-0.835000000000001,-0.830000000000001,-0.825000000000001,-0.820000000000001,
-0.815000000000001,-0.810000000000001,-0.805000000000001,-0.800000000000001,
-0.795000000000001,-0.790000000000001,-0.785000000000001,-0.780000000000001,
-0.775000000000001,-0.770000000000001,-0.765000000000001,-0.760000000000001,
-0.755000000000001,-0.750000000000001,-0.745000000000001,-0.740000000000001,
-0.735000000000001,-0.730000000000001,-0.725000000000001,-0.720000000000001,
-0.715000000000001,-0.710000000000001,-0.705000000000001,-0.700000000000001,
-0.695000000000001,-0.690000000000001,-0.685,-0.68,-0.675,-0.67,-0.665,
-0.66,-0.655,-0.65,-0.645,-0.64,-0.635,-0.63,-0.625,-0.62,-0.615,-0.61,
-0.605,-0.6,-0.595,-0.59,-0.585,-0.58,-0.575,-0.57,-0.565,-0.56,-0.555,
-0.55,-0.545,-0.54,-0.535,-0.53,-0.525,-0.52,-0.515,-0.51,-0.505,-0.5,-0.495,
-0.49,-0.485,-0.48,-0.475,-0.47,-0.465,-0.46,-0.455,-0.45,-0.445,-0.44,
-0.435,-0.43,-0.425,-0.42,-0.415,-0.41,-0.405,-0.4,-0.395,-0.39,-0.385,
-0.38,-0.375,-0.37,-0.365,-0.36,-0.355,-0.35,-0.345,-0.34,-0.335,-0.33,
-0.325,-0.32,-0.315,-0.31,-0.305,-0.3,-0.295,-0.29,-0.285,-0.28,-0.275,
-0.27,-0.265,-0.26,-0.255,-0.25,-0.245,-0.24,-0.235,-0.23,-0.225,-0.22,
-0.215,-0.21,-0.205,-0.2,-0.195,-0.19,-0.185,-0.18,-0.175,-0.17,-0.165,
-0.16,-0.155,-0.15,-0.145,-0.14,-0.135,-0.13,-0.125,-0.12,-0.115,-0.11,
-0.105,-0.1,-0.095,-0.09,-0.085,-0.08,-0.075,-0.07,-0.065,-0.06,-0.055,
-0.05,-0.045,-0.04,-0.035,-0.03,-0.025,-0.02,-0.015,-0.01,-0.005,0.),
 .UNSPECIFIED.)
CURVE()
GEOMETRIC_REPRESENTATION_ITEM()
RATIONAL_B_SPLINE_CURVE((1.,1.,1.,1.,1.,1.,1.,1.,1.,1.,1.,1.,1.,1.,1.,1.,
1.,1.,1.,1.,1.,1.,1.,1.,1.,1.,1.,1.,1.,1.,1.,1.,1.,1.,1.,1.,1.,1.,1.,1.,
1.,1.,1.,1.,1.,1.,1.,1.,1.,1.,1.,1.,1.,1.,1.,1.,1.,1.,1.,1.,1.,1.,1.,1.,
1.,1.,1.,1.,1.,1.,1.,1.,1.,1.,1.,1.,1.,1.,1.,1.,1.,1.,1.,1.,1.,1.,1.,1.,
1.,1.,1.,1.,1.,1.,1.,1.,1.,1.,1.,1.,1.,1.,1.,1.,1.,1.,1.,1.,1.,1.,1.,1.,
1.,1.,1.,1.,1.,1.,1.,1.,1.,1.,1.,1.,1.,1.,1.,1.,1.,1.,1.,1.,1.,1.,1.,1.,
1.,1.,1.,1.,1.,1.,1.,1.,1.,1.,1.,1.,1.,1.,1.,1.,1.,1.,1.,1.,1.,1.,1.,1.,
1.,1.,1.,1.,1.,1.,1.,1.,1.,1.,1.,1.,1.,1.,1.,1.,1.,1.,1.,1.,1.,1.,1.,1.,
1.,1.,1.,1.,1.,1.,1.,1.,1.,1.))
REPRESENTATION_ITEM('')
);
#575=(
BOUNDED_CURVE()
B_SPLINE_CURVE(5,(#128618,#128619,#128620,#128621,#128622,#128623,#128624,
#128625,#128626,#128627,#128628,#128629,#128630,#128631,#128632,#128633,
#128634,#128635,#128636,#128637,#128638,#128639,#128640,#128641,#128642,
#128643,#128644,#128645,#128646,#128647,#128648,#128649,#128650,#128651,
#128652,#128653,#128654,#128655,#128656,#128657,#128658,#128659,#128660,
#128661,#128662,#128663,#128664,#128665,#128666,#128667,#128668,#128669,
#128670,#128671,#128672,#128673,#128674,#128675,#128676,#128677,#128678,
#128679,#128680,#128681,#128682,#128683,#128684,#128685,#128686,#128687,
#128688,#128689,#128690,#128691,#128692,#128693,#128694,#128695,#128696,
#128697,#128698,#128699,#128700,#128701,#128702,#128703,#128704,#128705,
#128706,#128707,#128708,#128709,#128710,#128711,#128712,#128713,#128714,
#128715,#128716,#128717,#128718,#128719,#128720,#128721,#128722,#128723,
#128724,#128725,#128726,#128727,#128728,#128729,#128730,#128731,#128732,
#128733,#128734,#128735,#128736,#128737,#128738,#128739,#128740,#128741,
#128742,#128743,#128744,#128745,#128746,#128747,#128748,#128749,#128750,
#128751,#128752,#128753,#128754,#128755,#128756,#128757,#128758,#128759,
#128760,#128761,#128762,#128763,#128764,#128765,#128766,#128767,#128768,
#128769,#128770,#128771,#128772,#128773,#128774,#128775,#128776,#128777,
#128778,#128779,#128780,#128781,#128782,#128783,#128784,#128785,#128786,
#128787,#128788,#128789,#128790,#128791,#128792,#128793,#128794,#128795,
#128796,#128797,#128798,#128799,#128800,#128801,#128802,#128803,#128804,
#128805,#128806,#128807,#128808,#128809,#128810,#128811),.UNSPECIFIED.,
 .F.,.F.)
B_SPLINE_CURVE_WITH_KNOTS((6,1,1,1,1,1,1,1,1,1,1,1,1,1,1,1,1,1,1,1,1,1,
1,1,1,1,1,1,1,1,1,1,1,1,1,1,1,1,1,1,1,1,1,1,1,1,1,1,1,1,1,1,1,1,1,1,1,1,
1,1,1,1,1,1,1,1,1,1,1,1,1,1,1,1,1,1,1,1,1,1,1,1,1,1,1,1,1,1,1,1,1,1,1,1,
1,1,1,1,1,1,1,1,1,1,1,1,1,1,1,1,1,1,1,1,1,1,1,1,1,1,1,1,1,1,1,1,1,1,1,1,
1,1,1,1,1,1,1,1,1,1,1,1,1,1,1,1,1,1,1,1,1,1,1,1,1,1,1,1,1,1,1,1,1,1,1,1,
1,1,1,1,1,1,1,1,1,1,1,1,1,1,1,1,1,1,1,1,1,1,1,6),(0.,0.005,0.01,0.015,0.02,
0.025,0.03,0.035,0.04,0.045,0.05,0.055,0.06,0.065,0.07,0.075,0.08,0.085,
0.09,0.095,0.1,0.105,0.11,0.115,0.12,0.125,0.13,0.135,0.14,0.145,0.15,0.155,
0.16,0.165,0.17,0.175,0.18,0.185,0.19,0.195,0.2,0.205,0.21,0.215,0.22,0.225,
0.23,0.235,0.24,0.245,0.25,0.255,0.26,0.265,0.27,0.275,0.28,0.285,0.29,
0.295,0.3,0.305,0.31,0.315,0.32,0.325,0.33,0.335,0.34,0.345,0.35,0.355,
0.36,0.365,0.37,0.375,0.38,0.385,0.39,0.395,0.4,0.405,0.41,0.415,0.42,0.425,
0.43,0.435,0.44,0.445,0.45,0.455,0.46,0.465,0.47,0.475,0.48,0.485,0.49,
0.495,0.5,0.505,0.51,0.515,0.52,0.525,0.53,0.535,0.54,0.545,0.55,0.555,
0.56,0.565,0.57,0.575,0.58,0.585,0.59,0.595,0.6,0.605,0.61,0.615,0.62,0.625,
0.63,0.635,0.64,0.645,0.65,0.655,0.66,0.665,0.67,0.675,0.68,0.685,0.690000000000001,
0.695000000000001,0.700000000000001,0.705000000000001,0.710000000000001,
0.715000000000001,0.720000000000001,0.725000000000001,0.730000000000001,
0.735000000000001,0.740000000000001,0.745000000000001,0.750000000000001,
0.755000000000001,0.760000000000001,0.765000000000001,0.770000000000001,
0.775000000000001,0.780000000000001,0.785000000000001,0.790000000000001,
0.795000000000001,0.800000000000001,0.805000000000001,0.810000000000001,
0.815000000000001,0.820000000000001,0.825000000000001,0.830000000000001,
0.835000000000001,0.840000000000001,0.845000000000001,0.850000000000001,
0.855000000000001,0.860000000000001,0.865000000000001,0.870000000000001,
0.875000000000001,0.880000000000001,0.885000000000001,0.890000000000001,
0.895000000000001,0.900000000000001,0.905000000000001,0.910000000000001,
0.915000000000001,0.920000000000001,0.925000000000001,0.930000000000001,
0.935000000000001,0.940000000000001,0.94142984443807),.UNSPECIFIED.)
CURVE()
GEOMETRIC_REPRESENTATION_ITEM()
RATIONAL_B_SPLINE_CURVE((1.,1.,1.,1.,1.,1.,1.,1.,1.,1.,1.,1.,1.,1.,1.,1.,
1.,1.,1.,1.,1.,1.,1.,1.,1.,1.,1.,1.,1.,1.,1.,1.,1.,1.,1.,1.,1.,1.,1.,1.,
1.,1.,1.,1.,1.,1.,1.,1.,1.,1.,1.,1.,1.,1.,1.,1.,1.,1.,1.,1.,1.,1.,1.,1.,
1.,1.,1.,1.,1.,1.,1.,1.,1.,1.,1.,1.,1.,1.,1.,1.,1.,1.,1.,1.,1.,1.,1.,1.,
1.,1.,1.,1.,1.,1.,1.,1.,1.,1.,1.,1.,1.,1.,1.,1.,1.,1.,1.,1.,1.,1.,1.,1.,
1.,1.,1.,1.,1.,1.,1.,1.,1.,1.,1.,1.,1.,1.,1.,1.,1.,1.,1.,1.,1.,1.,1.,1.,
1.,1.,1.,1.,1.,1.,1.,1.,1.,1.,1.,1.,1.,1.,1.,1.,1.,1.,1.,1.,1.,1.,1.,1.,
1.,1.,1.,1.,1.,1.,1.,1.,1.,1.,1.,1.,1.,1.,1.,1.,1.,1.,1.,1.,1.,1.,1.,1.,
1.,1.,1.,1.,1.,1.,1.,1.,1.,1.))
REPRESENTATION_ITEM('')
);
#576=(
BOUNDED_CURVE()
B_SPLINE_CURVE(5,(#128814,#128815,#128816,#128817,#128818,#128819,#128820,
#128821,#128822,#128823,#128824,#128825,#128826,#128827,#128828,#128829,
#128830,#128831,#128832,#128833,#128834,#128835,#128836,#128837,#128838,
#128839,#128840,#128841,#128842,#128843,#128844,#128845,#128846,#128847,
#128848,#128849,#128850,#128851,#128852,#128853,#128854,#128855,#128856,
#128857,#128858,#128859,#128860,#128861,#128862,#128863,#128864,#128865,
#128866,#128867,#128868,#128869,#128870,#128871,#128872,#128873,#128874,
#128875,#128876,#128877,#128878,#128879,#128880,#128881,#128882,#128883,
#128884,#128885,#128886,#128887,#128888,#128889,#128890,#128891,#128892,
#128893,#128894,#128895,#128896,#128897,#128898,#128899,#128900,#128901,
#128902,#128903,#128904,#128905,#128906,#128907,#128908,#128909,#128910,
#128911,#128912,#128913,#128914,#128915,#128916,#128917,#128918,#128919,
#128920,#128921,#128922,#128923,#128924,#128925,#128926,#128927,#128928,
#128929,#128930,#128931,#128932,#128933,#128934,#128935,#128936,#128937,
#128938,#128939,#128940,#128941,#128942,#128943,#128944,#128945,#128946,
#128947,#128948,#128949,#128950,#128951,#128952,#128953,#128954,#128955,
#128956,#128957,#128958,#128959,#128960,#128961,#128962,#128963,#128964,
#128965,#128966,#128967,#128968,#128969,#128970,#128971,#128972,#128973,
#128974,#128975,#128976,#128977,#128978,#128979,#128980,#128981,#128982,
#128983,#128984,#128985,#128986,#128987,#128988,#128989,#128990,#128991,
#128992,#128993,#128994,#128995,#128996,#128997,#128998,#128999,#129000,
#129001,#129002,#129003,#129004,#129005,#129006,#129007),.UNSPECIFIED.,
 .F.,.F.)
B_SPLINE_CURVE_WITH_KNOTS((6,1,1,1,1,1,1,1,1,1,1,1,1,1,1,1,1,1,1,1,1,1,
1,1,1,1,1,1,1,1,1,1,1,1,1,1,1,1,1,1,1,1,1,1,1,1,1,1,1,1,1,1,1,1,1,1,1,1,
1,1,1,1,1,1,1,1,1,1,1,1,1,1,1,1,1,1,1,1,1,1,1,1,1,1,1,1,1,1,1,1,1,1,1,1,
1,1,1,1,1,1,1,1,1,1,1,1,1,1,1,1,1,1,1,1,1,1,1,1,1,1,1,1,1,1,1,1,1,1,1,1,
1,1,1,1,1,1,1,1,1,1,1,1,1,1,1,1,1,1,1,1,1,1,1,1,1,1,1,1,1,1,1,1,1,1,1,1,
1,1,1,1,1,1,1,1,1,1,1,1,1,1,1,1,1,1,1,1,1,1,1,6),(-0.941429844438076,-0.940000000000001,
-0.935000000000001,-0.930000000000001,-0.925000000000001,-0.920000000000001,
-0.915000000000001,-0.910000000000001,-0.905000000000001,-0.900000000000001,
-0.895000000000001,-0.890000000000001,-0.885000000000001,-0.880000000000001,
-0.875000000000001,-0.870000000000001,-0.865000000000001,-0.860000000000001,
-0.855000000000001,-0.850000000000001,-0.845000000000001,-0.840000000000001,
-0.835000000000001,-0.830000000000001,-0.825000000000001,-0.820000000000001,
-0.815000000000001,-0.810000000000001,-0.805000000000001,-0.800000000000001,
-0.795000000000001,-0.790000000000001,-0.785000000000001,-0.780000000000001,
-0.775000000000001,-0.770000000000001,-0.765000000000001,-0.760000000000001,
-0.755000000000001,-0.750000000000001,-0.745000000000001,-0.740000000000001,
-0.735000000000001,-0.730000000000001,-0.725000000000001,-0.720000000000001,
-0.715000000000001,-0.710000000000001,-0.705000000000001,-0.700000000000001,
-0.695000000000001,-0.690000000000001,-0.685,-0.68,-0.675,-0.67,-0.665,
-0.66,-0.655,-0.65,-0.645,-0.64,-0.635,-0.63,-0.625,-0.62,-0.615,-0.61,
-0.605,-0.6,-0.595,-0.59,-0.585,-0.58,-0.575,-0.57,-0.565,-0.56,-0.555,
-0.55,-0.545,-0.54,-0.535,-0.53,-0.525,-0.52,-0.515,-0.51,-0.505,-0.5,-0.495,
-0.49,-0.485,-0.48,-0.475,-0.47,-0.465,-0.46,-0.455,-0.45,-0.445,-0.44,
-0.435,-0.43,-0.425,-0.42,-0.415,-0.41,-0.405,-0.4,-0.395,-0.39,-0.385,
-0.38,-0.375,-0.37,-0.365,-0.36,-0.355,-0.35,-0.345,-0.34,-0.335,-0.33,
-0.325,-0.32,-0.315,-0.31,-0.305,-0.3,-0.295,-0.29,-0.285,-0.28,-0.275,
-0.27,-0.265,-0.26,-0.255,-0.25,-0.245,-0.24,-0.235,-0.23,-0.225,-0.22,
-0.215,-0.21,-0.205,-0.2,-0.195,-0.19,-0.185,-0.18,-0.175,-0.17,-0.165,
-0.16,-0.155,-0.15,-0.145,-0.14,-0.135,-0.13,-0.125,-0.12,-0.115,-0.11,
-0.105,-0.1,-0.095,-0.09,-0.085,-0.08,-0.075,-0.07,-0.065,-0.06,-0.055,
-0.05,-0.045,-0.04,-0.035,-0.03,-0.025,-0.02,-0.015,-0.01,-0.005,0.),
 .UNSPECIFIED.)
CURVE()
GEOMETRIC_REPRESENTATION_ITEM()
RATIONAL_B_SPLINE_CURVE((1.,1.,1.,1.,1.,1.,1.,1.,1.,1.,1.,1.,1.,1.,1.,1.,
1.,1.,1.,1.,1.,1.,1.,1.,1.,1.,1.,1.,1.,1.,1.,1.,1.,1.,1.,1.,1.,1.,1.,1.,
1.,1.,1.,1.,1.,1.,1.,1.,1.,1.,1.,1.,1.,1.,1.,1.,1.,1.,1.,1.,1.,1.,1.,1.,
1.,1.,1.,1.,1.,1.,1.,1.,1.,1.,1.,1.,1.,1.,1.,1.,1.,1.,1.,1.,1.,1.,1.,1.,
1.,1.,1.,1.,1.,1.,1.,1.,1.,1.,1.,1.,1.,1.,1.,1.,1.,1.,1.,1.,1.,1.,1.,1.,
1.,1.,1.,1.,1.,1.,1.,1.,1.,1.,1.,1.,1.,1.,1.,1.,1.,1.,1.,1.,1.,1.,1.,1.,
1.,1.,1.,1.,1.,1.,1.,1.,1.,1.,1.,1.,1.,1.,1.,1.,1.,1.,1.,1.,1.,1.,1.,1.,
1.,1.,1.,1.,1.,1.,1.,1.,1.,1.,1.,1.,1.,1.,1.,1.,1.,1.,1.,1.,1.,1.,1.,1.,
1.,1.,1.,1.,1.,1.,1.,1.,1.,1.))
REPRESENTATION_ITEM('')
);
#577=(
BOUNDED_CURVE()
B_SPLINE_CURVE(5,(#129419,#129420,#129421,#129422,#129423,#129424,#129425,
#129426,#129427,#129428,#129429,#129430,#129431,#129432,#129433,#129434,
#129435,#129436,#129437,#129438,#129439,#129440,#129441,#129442,#129443,
#129444,#129445,#129446,#129447,#129448,#129449,#129450,#129451,#129452,
#129453,#129454,#129455,#129456,#129457,#129458,#129459,#129460,#129461,
#129462,#129463,#129464,#129465,#129466,#129467,#129468,#129469,#129470,
#129471,#129472,#129473,#129474,#129475,#129476,#129477,#129478,#129479,
#129480,#129481,#129482,#129483,#129484,#129485,#129486,#129487,#129488,
#129489,#129490,#129491,#129492,#129493,#129494,#129495,#129496,#129497,
#129498,#129499,#129500,#129501,#129502,#129503,#129504,#129505,#129506,
#129507,#129508,#129509,#129510,#129511,#129512,#129513,#129514,#129515,
#129516,#129517,#129518,#129519,#129520,#129521,#129522,#129523,#129524,
#129525,#129526,#129527,#129528,#129529,#129530,#129531,#129532,#129533,
#129534,#129535,#129536,#129537,#129538,#129539,#129540,#129541,#129542,
#129543,#129544,#129545,#129546,#129547,#129548,#129549,#129550,#129551,
#129552,#129553,#129554,#129555,#129556,#129557,#129558,#129559,#129560,
#129561,#129562,#129563,#129564,#129565,#129566,#129567,#129568,#129569,
#129570,#129571,#129572,#129573,#129574,#129575,#129576,#129577,#129578,
#129579,#129580,#129581,#129582,#129583,#129584,#129585,#129586,#129587,
#129588,#129589,#129590,#129591,#129592,#129593,#129594,#129595,#129596,
#129597,#129598,#129599,#129600,#129601,#129602,#129603,#129604,#129605,
#129606,#129607,#129608,#129609,#129610,#129611,#129612),.UNSPECIFIED.,
 .F.,.F.)
B_SPLINE_CURVE_WITH_KNOTS((6,1,1,1,1,1,1,1,1,1,1,1,1,1,1,1,1,1,1,1,1,1,
1,1,1,1,1,1,1,1,1,1,1,1,1,1,1,1,1,1,1,1,1,1,1,1,1,1,1,1,1,1,1,1,1,1,1,1,
1,1,1,1,1,1,1,1,1,1,1,1,1,1,1,1,1,1,1,1,1,1,1,1,1,1,1,1,1,1,1,1,1,1,1,1,
1,1,1,1,1,1,1,1,1,1,1,1,1,1,1,1,1,1,1,1,1,1,1,1,1,1,1,1,1,1,1,1,1,1,1,1,
1,1,1,1,1,1,1,1,1,1,1,1,1,1,1,1,1,1,1,1,1,1,1,1,1,1,1,1,1,1,1,1,1,1,1,1,
1,1,1,1,1,1,1,1,1,1,1,1,1,1,1,1,1,1,1,1,1,1,1,6),(0.,0.005,0.01,0.015,0.02,
0.025,0.03,0.035,0.04,0.045,0.05,0.055,0.06,0.065,0.07,0.075,0.08,0.085,
0.09,0.095,0.1,0.105,0.11,0.115,0.12,0.125,0.13,0.135,0.14,0.145,0.15,0.155,
0.16,0.165,0.17,0.175,0.18,0.185,0.19,0.195,0.2,0.205,0.21,0.215,0.22,0.225,
0.23,0.235,0.24,0.245,0.25,0.255,0.26,0.265,0.27,0.275,0.28,0.285,0.29,
0.295,0.3,0.305,0.31,0.315,0.32,0.325,0.33,0.335,0.34,0.345,0.35,0.355,
0.36,0.365,0.37,0.375,0.38,0.385,0.39,0.395,0.4,0.405,0.41,0.415,0.42,0.425,
0.43,0.435,0.44,0.445,0.45,0.455,0.46,0.465,0.47,0.475,0.48,0.485,0.49,
0.495,0.5,0.505,0.51,0.515,0.52,0.525,0.53,0.535,0.54,0.545,0.55,0.555,
0.56,0.565,0.57,0.575,0.58,0.585,0.59,0.595,0.6,0.605,0.61,0.615,0.62,0.625,
0.63,0.635,0.64,0.645,0.65,0.655,0.66,0.665,0.67,0.675,0.68,0.685,0.690000000000001,
0.695000000000001,0.700000000000001,0.705000000000001,0.710000000000001,
0.715000000000001,0.720000000000001,0.725000000000001,0.730000000000001,
0.735000000000001,0.740000000000001,0.745000000000001,0.750000000000001,
0.755000000000001,0.760000000000001,0.765000000000001,0.770000000000001,
0.775000000000001,0.780000000000001,0.785000000000001,0.790000000000001,
0.795000000000001,0.800000000000001,0.805000000000001,0.810000000000001,
0.815000000000001,0.820000000000001,0.825000000000001,0.830000000000001,
0.835000000000001,0.840000000000001,0.845000000000001,0.850000000000001,
0.855000000000001,0.860000000000001,0.865000000000001,0.870000000000001,
0.875000000000001,0.880000000000001,0.885000000000001,0.890000000000001,
0.895000000000001,0.900000000000001,0.905000000000001,0.910000000000001,
0.915000000000001,0.920000000000001,0.925000000000001,0.930000000000001,
0.935000000000001,0.940000000000001,0.941429844438015),.UNSPECIFIED.)
CURVE()
GEOMETRIC_REPRESENTATION_ITEM()
RATIONAL_B_SPLINE_CURVE((1.,1.,1.,1.,1.,1.,1.,1.,1.,1.,1.,1.,1.,1.,1.,1.,
1.,1.,1.,1.,1.,1.,1.,1.,1.,1.,1.,1.,1.,1.,1.,1.,1.,1.,1.,1.,1.,1.,1.,1.,
1.,1.,1.,1.,1.,1.,1.,1.,1.,1.,1.,1.,1.,1.,1.,1.,1.,1.,1.,1.,1.,1.,1.,1.,
1.,1.,1.,1.,1.,1.,1.,1.,1.,1.,1.,1.,1.,1.,1.,1.,1.,1.,1.,1.,1.,1.,1.,1.,
1.,1.,1.,1.,1.,1.,1.,1.,1.,1.,1.,1.,1.,1.,1.,1.,1.,1.,1.,1.,1.,1.,1.,1.,
1.,1.,1.,1.,1.,1.,1.,1.,1.,1.,1.,1.,1.,1.,1.,1.,1.,1.,1.,1.,1.,1.,1.,1.,
1.,1.,1.,1.,1.,1.,1.,1.,1.,1.,1.,1.,1.,1.,1.,1.,1.,1.,1.,1.,1.,1.,1.,1.,
1.,1.,1.,1.,1.,1.,1.,1.,1.,1.,1.,1.,1.,1.,1.,1.,1.,1.,1.,1.,1.,1.,1.,1.,
1.,1.,1.,1.,1.,1.,1.,1.,1.,1.))
REPRESENTATION_ITEM('')
);
#578=(
BOUNDED_CURVE()
B_SPLINE_CURVE(5,(#129615,#129616,#129617,#129618,#129619,#129620,#129621,
#129622,#129623,#129624,#129625,#129626,#129627,#129628,#129629,#129630,
#129631,#129632,#129633,#129634,#129635,#129636,#129637,#129638,#129639,
#129640,#129641,#129642,#129643,#129644,#129645,#129646,#129647,#129648,
#129649,#129650,#129651,#129652,#129653,#129654,#129655,#129656,#129657,
#129658,#129659,#129660,#129661,#129662,#129663,#129664,#129665,#129666,
#129667,#129668,#129669,#129670,#129671,#129672,#129673,#129674,#129675,
#129676,#129677,#129678,#129679,#129680,#129681,#129682,#129683,#129684,
#129685,#129686,#129687,#129688,#129689,#129690,#129691,#129692,#129693,
#129694,#129695,#129696,#129697,#129698,#129699,#129700,#129701,#129702,
#129703,#129704,#129705,#129706,#129707,#129708,#129709,#129710,#129711,
#129712,#129713,#129714,#129715,#129716,#129717,#129718,#129719,#129720,
#129721,#129722,#129723,#129724,#129725,#129726,#129727,#129728,#129729,
#129730,#129731,#129732,#129733,#129734,#129735,#129736,#129737,#129738,
#129739,#129740,#129741,#129742,#129743,#129744,#129745,#129746,#129747,
#129748,#129749,#129750,#129751,#129752,#129753,#129754,#129755,#129756,
#129757,#129758,#129759,#129760,#129761,#129762,#129763,#129764,#129765,
#129766,#129767,#129768,#129769,#129770,#129771,#129772,#129773,#129774,
#129775,#129776,#129777,#129778,#129779,#129780,#129781,#129782,#129783,
#129784,#129785,#129786,#129787,#129788,#129789,#129790,#129791,#129792,
#129793,#129794,#129795,#129796,#129797,#129798,#129799,#129800,#129801,
#129802,#129803,#129804,#129805,#129806,#129807,#129808),.UNSPECIFIED.,
 .F.,.F.)
B_SPLINE_CURVE_WITH_KNOTS((6,1,1,1,1,1,1,1,1,1,1,1,1,1,1,1,1,1,1,1,1,1,
1,1,1,1,1,1,1,1,1,1,1,1,1,1,1,1,1,1,1,1,1,1,1,1,1,1,1,1,1,1,1,1,1,1,1,1,
1,1,1,1,1,1,1,1,1,1,1,1,1,1,1,1,1,1,1,1,1,1,1,1,1,1,1,1,1,1,1,1,1,1,1,1,
1,1,1,1,1,1,1,1,1,1,1,1,1,1,1,1,1,1,1,1,1,1,1,1,1,1,1,1,1,1,1,1,1,1,1,1,
1,1,1,1,1,1,1,1,1,1,1,1,1,1,1,1,1,1,1,1,1,1,1,1,1,1,1,1,1,1,1,1,1,1,1,1,
1,1,1,1,1,1,1,1,1,1,1,1,1,1,1,1,1,1,1,1,1,1,1,6),(-0.94142984443801,-0.940000000000001,
-0.935000000000001,-0.930000000000001,-0.925000000000001,-0.920000000000001,
-0.915000000000001,-0.910000000000001,-0.905000000000001,-0.900000000000001,
-0.895000000000001,-0.890000000000001,-0.885000000000001,-0.880000000000001,
-0.875000000000001,-0.870000000000001,-0.865000000000001,-0.860000000000001,
-0.855000000000001,-0.850000000000001,-0.845000000000001,-0.840000000000001,
-0.835000000000001,-0.830000000000001,-0.825000000000001,-0.820000000000001,
-0.815000000000001,-0.810000000000001,-0.805000000000001,-0.800000000000001,
-0.795000000000001,-0.790000000000001,-0.785000000000001,-0.780000000000001,
-0.775000000000001,-0.770000000000001,-0.765000000000001,-0.760000000000001,
-0.755000000000001,-0.750000000000001,-0.745000000000001,-0.740000000000001,
-0.735000000000001,-0.730000000000001,-0.725000000000001,-0.720000000000001,
-0.715000000000001,-0.710000000000001,-0.705000000000001,-0.700000000000001,
-0.695000000000001,-0.690000000000001,-0.685,-0.68,-0.675,-0.67,-0.665,
-0.66,-0.655,-0.65,-0.645,-0.64,-0.635,-0.63,-0.625,-0.62,-0.615,-0.61,
-0.605,-0.6,-0.595,-0.59,-0.585,-0.58,-0.575,-0.57,-0.565,-0.56,-0.555,
-0.55,-0.545,-0.54,-0.535,-0.53,-0.525,-0.52,-0.515,-0.51,-0.505,-0.5,-0.495,
-0.49,-0.485,-0.48,-0.475,-0.47,-0.465,-0.46,-0.455,-0.45,-0.445,-0.44,
-0.435,-0.43,-0.425,-0.42,-0.415,-0.41,-0.405,-0.4,-0.395,-0.39,-0.385,
-0.38,-0.375,-0.37,-0.365,-0.36,-0.355,-0.35,-0.345,-0.34,-0.335,-0.33,
-0.325,-0.32,-0.315,-0.31,-0.305,-0.3,-0.295,-0.29,-0.285,-0.28,-0.275,
-0.27,-0.265,-0.26,-0.255,-0.25,-0.245,-0.24,-0.235,-0.23,-0.225,-0.22,
-0.215,-0.21,-0.205,-0.2,-0.195,-0.19,-0.185,-0.18,-0.175,-0.17,-0.165,
-0.16,-0.155,-0.15,-0.145,-0.14,-0.135,-0.13,-0.125,-0.12,-0.115,-0.11,
-0.105,-0.1,-0.095,-0.09,-0.085,-0.08,-0.075,-0.07,-0.065,-0.06,-0.055,
-0.05,-0.045,-0.04,-0.035,-0.03,-0.025,-0.02,-0.015,-0.01,-0.005,0.),
 .UNSPECIFIED.)
CURVE()
GEOMETRIC_REPRESENTATION_ITEM()
RATIONAL_B_SPLINE_CURVE((1.,1.,1.,1.,1.,1.,1.,1.,1.,1.,1.,1.,1.,1.,1.,1.,
1.,1.,1.,1.,1.,1.,1.,1.,1.,1.,1.,1.,1.,1.,1.,1.,1.,1.,1.,1.,1.,1.,1.,1.,
1.,1.,1.,1.,1.,1.,1.,1.,1.,1.,1.,1.,1.,1.,1.,1.,1.,1.,1.,1.,1.,1.,1.,1.,
1.,1.,1.,1.,1.,1.,1.,1.,1.,1.,1.,1.,1.,1.,1.,1.,1.,1.,1.,1.,1.,1.,1.,1.,
1.,1.,1.,1.,1.,1.,1.,1.,1.,1.,1.,1.,1.,1.,1.,1.,1.,1.,1.,1.,1.,1.,1.,1.,
1.,1.,1.,1.,1.,1.,1.,1.,1.,1.,1.,1.,1.,1.,1.,1.,1.,1.,1.,1.,1.,1.,1.,1.,
1.,1.,1.,1.,1.,1.,1.,1.,1.,1.,1.,1.,1.,1.,1.,1.,1.,1.,1.,1.,1.,1.,1.,1.,
1.,1.,1.,1.,1.,1.,1.,1.,1.,1.,1.,1.,1.,1.,1.,1.,1.,1.,1.,1.,1.,1.,1.,1.,
1.,1.,1.,1.,1.,1.,1.,1.,1.,1.))
REPRESENTATION_ITEM('')
);
#579=(
BOUNDED_CURVE()
B_SPLINE_CURVE(5,(#130220,#130221,#130222,#130223,#130224,#130225,#130226,
#130227,#130228,#130229,#130230,#130231,#130232,#130233,#130234,#130235,
#130236,#130237,#130238,#130239,#130240,#130241,#130242,#130243,#130244,
#130245,#130246,#130247,#130248,#130249,#130250,#130251,#130252,#130253,
#130254,#130255,#130256,#130257,#130258,#130259,#130260,#130261,#130262,
#130263,#130264,#130265,#130266,#130267,#130268,#130269,#130270,#130271,
#130272,#130273,#130274,#130275,#130276,#130277,#130278,#130279,#130280,
#130281,#130282,#130283,#130284,#130285,#130286,#130287,#130288,#130289,
#130290,#130291,#130292,#130293,#130294,#130295,#130296,#130297,#130298,
#130299,#130300,#130301,#130302,#130303,#130304,#130305,#130306,#130307,
#130308,#130309,#130310,#130311,#130312,#130313,#130314,#130315,#130316,
#130317,#130318,#130319,#130320,#130321,#130322,#130323,#130324,#130325,
#130326,#130327,#130328,#130329,#130330,#130331,#130332,#130333,#130334,
#130335,#130336,#130337,#130338,#130339,#130340,#130341,#130342,#130343,
#130344,#130345,#130346,#130347,#130348,#130349,#130350,#130351,#130352,
#130353,#130354,#130355,#130356,#130357,#130358,#130359,#130360,#130361,
#130362,#130363,#130364,#130365,#130366,#130367,#130368,#130369,#130370,
#130371,#130372,#130373,#130374,#130375,#130376,#130377,#130378,#130379,
#130380,#130381,#130382,#130383,#130384,#130385,#130386,#130387,#130388,
#130389,#130390,#130391,#130392,#130393,#130394,#130395,#130396,#130397,
#130398,#130399,#130400,#130401,#130402,#130403,#130404,#130405,#130406,
#130407,#130408,#130409,#130410,#130411,#130412,#130413),.UNSPECIFIED.,
 .F.,.F.)
B_SPLINE_CURVE_WITH_KNOTS((6,1,1,1,1,1,1,1,1,1,1,1,1,1,1,1,1,1,1,1,1,1,
1,1,1,1,1,1,1,1,1,1,1,1,1,1,1,1,1,1,1,1,1,1,1,1,1,1,1,1,1,1,1,1,1,1,1,1,
1,1,1,1,1,1,1,1,1,1,1,1,1,1,1,1,1,1,1,1,1,1,1,1,1,1,1,1,1,1,1,1,1,1,1,1,
1,1,1,1,1,1,1,1,1,1,1,1,1,1,1,1,1,1,1,1,1,1,1,1,1,1,1,1,1,1,1,1,1,1,1,1,
1,1,1,1,1,1,1,1,1,1,1,1,1,1,1,1,1,1,1,1,1,1,1,1,1,1,1,1,1,1,1,1,1,1,1,1,
1,1,1,1,1,1,1,1,1,1,1,1,1,1,1,1,1,1,1,1,1,1,1,6),(0.,0.005,0.01,0.015,0.02,
0.025,0.03,0.035,0.04,0.045,0.05,0.055,0.06,0.065,0.07,0.075,0.08,0.085,
0.09,0.095,0.1,0.105,0.11,0.115,0.12,0.125,0.13,0.135,0.14,0.145,0.15,0.155,
0.16,0.165,0.17,0.175,0.18,0.185,0.19,0.195,0.2,0.205,0.21,0.215,0.22,0.225,
0.23,0.235,0.24,0.245,0.25,0.255,0.26,0.265,0.27,0.275,0.28,0.285,0.29,
0.295,0.3,0.305,0.31,0.315,0.32,0.325,0.33,0.335,0.34,0.345,0.35,0.355,
0.36,0.365,0.37,0.375,0.38,0.385,0.39,0.395,0.4,0.405,0.41,0.415,0.42,0.425,
0.43,0.435,0.44,0.445,0.45,0.455,0.46,0.465,0.47,0.475,0.48,0.485,0.49,
0.495,0.5,0.505,0.51,0.515,0.52,0.525,0.53,0.535,0.54,0.545,0.55,0.555,
0.56,0.565,0.57,0.575,0.58,0.585,0.59,0.595,0.6,0.605,0.61,0.615,0.62,0.625,
0.63,0.635,0.64,0.645,0.65,0.655,0.66,0.665,0.67,0.675,0.68,0.685,0.690000000000001,
0.695000000000001,0.700000000000001,0.705000000000001,0.710000000000001,
0.715000000000001,0.720000000000001,0.725000000000001,0.730000000000001,
0.735000000000001,0.740000000000001,0.745000000000001,0.750000000000001,
0.755000000000001,0.760000000000001,0.765000000000001,0.770000000000001,
0.775000000000001,0.780000000000001,0.785000000000001,0.790000000000001,
0.795000000000001,0.800000000000001,0.805000000000001,0.810000000000001,
0.815000000000001,0.820000000000001,0.825000000000001,0.830000000000001,
0.835000000000001,0.840000000000001,0.845000000000001,0.850000000000001,
0.855000000000001,0.860000000000001,0.865000000000001,0.870000000000001,
0.875000000000001,0.880000000000001,0.885000000000001,0.890000000000001,
0.895000000000001,0.900000000000001,0.905000000000001,0.910000000000001,
0.915000000000001,0.920000000000001,0.925000000000001,0.930000000000001,
0.935000000000001,0.940000000000001,0.941429844438042),.UNSPECIFIED.)
CURVE()
GEOMETRIC_REPRESENTATION_ITEM()
RATIONAL_B_SPLINE_CURVE((1.,1.,1.,1.,1.,1.,1.,1.,1.,1.,1.,1.,1.,1.,1.,1.,
1.,1.,1.,1.,1.,1.,1.,1.,1.,1.,1.,1.,1.,1.,1.,1.,1.,1.,1.,1.,1.,1.,1.,1.,
1.,1.,1.,1.,1.,1.,1.,1.,1.,1.,1.,1.,1.,1.,1.,1.,1.,1.,1.,1.,1.,1.,1.,1.,
1.,1.,1.,1.,1.,1.,1.,1.,1.,1.,1.,1.,1.,1.,1.,1.,1.,1.,1.,1.,1.,1.,1.,1.,
1.,1.,1.,1.,1.,1.,1.,1.,1.,1.,1.,1.,1.,1.,1.,1.,1.,1.,1.,1.,1.,1.,1.,1.,
1.,1.,1.,1.,1.,1.,1.,1.,1.,1.,1.,1.,1.,1.,1.,1.,1.,1.,1.,1.,1.,1.,1.,1.,
1.,1.,1.,1.,1.,1.,1.,1.,1.,1.,1.,1.,1.,1.,1.,1.,1.,1.,1.,1.,1.,1.,1.,1.,
1.,1.,1.,1.,1.,1.,1.,1.,1.,1.,1.,1.,1.,1.,1.,1.,1.,1.,1.,1.,1.,1.,1.,1.,
1.,1.,1.,1.,1.,1.,1.,1.,1.,1.))
REPRESENTATION_ITEM('')
);
#580=(
BOUNDED_CURVE()
B_SPLINE_CURVE(5,(#130416,#130417,#130418,#130419,#130420,#130421,#130422,
#130423,#130424,#130425,#130426,#130427,#130428,#130429,#130430,#130431,
#130432,#130433,#130434,#130435,#130436,#130437,#130438,#130439,#130440,
#130441,#130442,#130443,#130444,#130445,#130446,#130447,#130448,#130449,
#130450,#130451,#130452,#130453,#130454,#130455,#130456,#130457,#130458,
#130459,#130460,#130461,#130462,#130463,#130464,#130465,#130466,#130467,
#130468,#130469,#130470,#130471,#130472,#130473,#130474,#130475,#130476,
#130477,#130478,#130479,#130480,#130481,#130482,#130483,#130484,#130485,
#130486,#130487,#130488,#130489,#130490,#130491,#130492,#130493,#130494,
#130495,#130496,#130497,#130498,#130499,#130500,#130501,#130502,#130503,
#130504,#130505,#130506,#130507,#130508,#130509,#130510,#130511,#130512,
#130513,#130514,#130515,#130516,#130517,#130518,#130519,#130520,#130521,
#130522,#130523,#130524,#130525,#130526,#130527,#130528,#130529,#130530,
#130531,#130532,#130533,#130534,#130535,#130536,#130537,#130538,#130539,
#130540,#130541,#130542,#130543,#130544,#130545,#130546,#130547,#130548,
#130549,#130550,#130551,#130552,#130553,#130554,#130555,#130556,#130557,
#130558,#130559,#130560,#130561,#130562,#130563,#130564,#130565,#130566,
#130567,#130568,#130569,#130570,#130571,#130572,#130573,#130574,#130575,
#130576,#130577,#130578,#130579,#130580,#130581,#130582,#130583,#130584,
#130585,#130586,#130587,#130588,#130589,#130590,#130591,#130592,#130593,
#130594,#130595,#130596,#130597,#130598,#130599,#130600,#130601,#130602,
#130603,#130604,#130605,#130606,#130607,#130608,#130609),.UNSPECIFIED.,
 .F.,.F.)
B_SPLINE_CURVE_WITH_KNOTS((6,1,1,1,1,1,1,1,1,1,1,1,1,1,1,1,1,1,1,1,1,1,
1,1,1,1,1,1,1,1,1,1,1,1,1,1,1,1,1,1,1,1,1,1,1,1,1,1,1,1,1,1,1,1,1,1,1,1,
1,1,1,1,1,1,1,1,1,1,1,1,1,1,1,1,1,1,1,1,1,1,1,1,1,1,1,1,1,1,1,1,1,1,1,1,
1,1,1,1,1,1,1,1,1,1,1,1,1,1,1,1,1,1,1,1,1,1,1,1,1,1,1,1,1,1,1,1,1,1,1,1,
1,1,1,1,1,1,1,1,1,1,1,1,1,1,1,1,1,1,1,1,1,1,1,1,1,1,1,1,1,1,1,1,1,1,1,1,
1,1,1,1,1,1,1,1,1,1,1,1,1,1,1,1,1,1,1,1,1,1,1,6),(-0.941429844438034,-0.940000000000001,
-0.935000000000001,-0.930000000000001,-0.925000000000001,-0.920000000000001,
-0.915000000000001,-0.910000000000001,-0.905000000000001,-0.900000000000001,
-0.895000000000001,-0.890000000000001,-0.885000000000001,-0.880000000000001,
-0.875000000000001,-0.870000000000001,-0.865000000000001,-0.860000000000001,
-0.855000000000001,-0.850000000000001,-0.845000000000001,-0.840000000000001,
-0.835000000000001,-0.830000000000001,-0.825000000000001,-0.820000000000001,
-0.815000000000001,-0.810000000000001,-0.805000000000001,-0.800000000000001,
-0.795000000000001,-0.790000000000001,-0.785000000000001,-0.780000000000001,
-0.775000000000001,-0.770000000000001,-0.765000000000001,-0.760000000000001,
-0.755000000000001,-0.750000000000001,-0.745000000000001,-0.740000000000001,
-0.735000000000001,-0.730000000000001,-0.725000000000001,-0.720000000000001,
-0.715000000000001,-0.710000000000001,-0.705000000000001,-0.700000000000001,
-0.695000000000001,-0.690000000000001,-0.685,-0.68,-0.675,-0.67,-0.665,
-0.66,-0.655,-0.65,-0.645,-0.64,-0.635,-0.63,-0.625,-0.62,-0.615,-0.61,
-0.605,-0.6,-0.595,-0.59,-0.585,-0.58,-0.575,-0.57,-0.565,-0.56,-0.555,
-0.55,-0.545,-0.54,-0.535,-0.53,-0.525,-0.52,-0.515,-0.51,-0.505,-0.5,-0.495,
-0.49,-0.485,-0.48,-0.475,-0.47,-0.465,-0.46,-0.455,-0.45,-0.445,-0.44,
-0.435,-0.43,-0.425,-0.42,-0.415,-0.41,-0.405,-0.4,-0.395,-0.39,-0.385,
-0.38,-0.375,-0.37,-0.365,-0.36,-0.355,-0.35,-0.345,-0.34,-0.335,-0.33,
-0.325,-0.32,-0.315,-0.31,-0.305,-0.3,-0.295,-0.29,-0.285,-0.28,-0.275,
-0.27,-0.265,-0.26,-0.255,-0.25,-0.245,-0.24,-0.235,-0.23,-0.225,-0.22,
-0.215,-0.21,-0.205,-0.2,-0.195,-0.19,-0.185,-0.18,-0.175,-0.17,-0.165,
-0.16,-0.155,-0.15,-0.145,-0.14,-0.135,-0.13,-0.125,-0.12,-0.115,-0.11,
-0.105,-0.1,-0.095,-0.09,-0.085,-0.08,-0.075,-0.07,-0.065,-0.06,-0.055,
-0.05,-0.045,-0.04,-0.035,-0.03,-0.025,-0.02,-0.015,-0.01,-0.005,0.),
 .UNSPECIFIED.)
CURVE()
GEOMETRIC_REPRESENTATION_ITEM()
RATIONAL_B_SPLINE_CURVE((1.,1.,1.,1.,1.,1.,1.,1.,1.,1.,1.,1.,1.,1.,1.,1.,
1.,1.,1.,1.,1.,1.,1.,1.,1.,1.,1.,1.,1.,1.,1.,1.,1.,1.,1.,1.,1.,1.,1.,1.,
1.,1.,1.,1.,1.,1.,1.,1.,1.,1.,1.,1.,1.,1.,1.,1.,1.,1.,1.,1.,1.,1.,1.,1.,
1.,1.,1.,1.,1.,1.,1.,1.,1.,1.,1.,1.,1.,1.,1.,1.,1.,1.,1.,1.,1.,1.,1.,1.,
1.,1.,1.,1.,1.,1.,1.,1.,1.,1.,1.,1.,1.,1.,1.,1.,1.,1.,1.,1.,1.,1.,1.,1.,
1.,1.,1.,1.,1.,1.,1.,1.,1.,1.,1.,1.,1.,1.,1.,1.,1.,1.,1.,1.,1.,1.,1.,1.,
1.,1.,1.,1.,1.,1.,1.,1.,1.,1.,1.,1.,1.,1.,1.,1.,1.,1.,1.,1.,1.,1.,1.,1.,
1.,1.,1.,1.,1.,1.,1.,1.,1.,1.,1.,1.,1.,1.,1.,1.,1.,1.,1.,1.,1.,1.,1.,1.,
1.,1.,1.,1.,1.,1.,1.,1.,1.,1.))
REPRESENTATION_ITEM('')
);
#581=(
BOUNDED_CURVE()
B_SPLINE_CURVE(5,(#131021,#131022,#131023,#131024,#131025,#131026,#131027,
#131028,#131029,#131030,#131031,#131032,#131033,#131034,#131035,#131036,
#131037,#131038,#131039,#131040,#131041,#131042,#131043,#131044,#131045,
#131046,#131047,#131048,#131049,#131050,#131051,#131052,#131053,#131054,
#131055,#131056,#131057,#131058,#131059,#131060,#131061,#131062,#131063,
#131064,#131065,#131066,#131067,#131068,#131069,#131070,#131071,#131072,
#131073,#131074,#131075,#131076,#131077,#131078,#131079,#131080,#131081,
#131082,#131083,#131084,#131085,#131086,#131087,#131088,#131089,#131090,
#131091,#131092,#131093,#131094,#131095,#131096,#131097,#131098,#131099,
#131100,#131101,#131102,#131103,#131104,#131105,#131106,#131107,#131108,
#131109,#131110,#131111,#131112,#131113,#131114,#131115,#131116,#131117,
#131118,#131119,#131120,#131121,#131122,#131123,#131124,#131125,#131126,
#131127,#131128,#131129,#131130,#131131,#131132,#131133,#131134,#131135,
#131136,#131137,#131138,#131139,#131140,#131141,#131142,#131143,#131144,
#131145,#131146,#131147,#131148,#131149,#131150,#131151,#131152,#131153,
#131154,#131155,#131156,#131157,#131158,#131159,#131160,#131161,#131162,
#131163,#131164,#131165,#131166,#131167,#131168,#131169,#131170,#131171,
#131172,#131173,#131174,#131175,#131176,#131177,#131178,#131179,#131180,
#131181,#131182,#131183,#131184,#131185,#131186,#131187,#131188,#131189,
#131190,#131191,#131192,#131193,#131194,#131195,#131196,#131197,#131198,
#131199,#131200,#131201,#131202,#131203,#131204,#131205,#131206,#131207,
#131208,#131209,#131210,#131211,#131212,#131213,#131214),.UNSPECIFIED.,
 .F.,.F.)
B_SPLINE_CURVE_WITH_KNOTS((6,1,1,1,1,1,1,1,1,1,1,1,1,1,1,1,1,1,1,1,1,1,
1,1,1,1,1,1,1,1,1,1,1,1,1,1,1,1,1,1,1,1,1,1,1,1,1,1,1,1,1,1,1,1,1,1,1,1,
1,1,1,1,1,1,1,1,1,1,1,1,1,1,1,1,1,1,1,1,1,1,1,1,1,1,1,1,1,1,1,1,1,1,1,1,
1,1,1,1,1,1,1,1,1,1,1,1,1,1,1,1,1,1,1,1,1,1,1,1,1,1,1,1,1,1,1,1,1,1,1,1,
1,1,1,1,1,1,1,1,1,1,1,1,1,1,1,1,1,1,1,1,1,1,1,1,1,1,1,1,1,1,1,1,1,1,1,1,
1,1,1,1,1,1,1,1,1,1,1,1,1,1,1,1,1,1,1,1,1,1,1,6),(0.,0.005,0.01,0.015,0.02,
0.025,0.03,0.035,0.04,0.045,0.05,0.055,0.06,0.065,0.07,0.075,0.08,0.085,
0.09,0.095,0.1,0.105,0.11,0.115,0.12,0.125,0.13,0.135,0.14,0.145,0.15,0.155,
0.16,0.165,0.17,0.175,0.18,0.185,0.19,0.195,0.2,0.205,0.21,0.215,0.22,0.225,
0.23,0.235,0.24,0.245,0.25,0.255,0.26,0.265,0.27,0.275,0.28,0.285,0.29,
0.295,0.3,0.305,0.31,0.315,0.32,0.325,0.33,0.335,0.34,0.345,0.35,0.355,
0.36,0.365,0.37,0.375,0.38,0.385,0.39,0.395,0.4,0.405,0.41,0.415,0.42,0.425,
0.43,0.435,0.44,0.445,0.45,0.455,0.46,0.465,0.47,0.475,0.48,0.485,0.49,
0.495,0.5,0.505,0.51,0.515,0.52,0.525,0.53,0.535,0.54,0.545,0.55,0.555,
0.56,0.565,0.57,0.575,0.58,0.585,0.59,0.595,0.6,0.605,0.61,0.615,0.62,0.625,
0.63,0.635,0.64,0.645,0.65,0.655,0.66,0.665,0.67,0.675,0.68,0.685,0.690000000000001,
0.695000000000001,0.700000000000001,0.705000000000001,0.710000000000001,
0.715000000000001,0.720000000000001,0.725000000000001,0.730000000000001,
0.735000000000001,0.740000000000001,0.745000000000001,0.750000000000001,
0.755000000000001,0.760000000000001,0.765000000000001,0.770000000000001,
0.775000000000001,0.780000000000001,0.785000000000001,0.790000000000001,
0.795000000000001,0.800000000000001,0.805000000000001,0.810000000000001,
0.815000000000001,0.820000000000001,0.825000000000001,0.830000000000001,
0.835000000000001,0.840000000000001,0.845000000000001,0.850000000000001,
0.855000000000001,0.860000000000001,0.865000000000001,0.870000000000001,
0.875000000000001,0.880000000000001,0.885000000000001,0.890000000000001,
0.895000000000001,0.900000000000001,0.905000000000001,0.910000000000001,
0.915000000000001,0.920000000000001,0.925000000000001,0.930000000000001,
0.935000000000001,0.940000000000001,0.94142984443805),.UNSPECIFIED.)
CURVE()
GEOMETRIC_REPRESENTATION_ITEM()
RATIONAL_B_SPLINE_CURVE((1.,1.,1.,1.,1.,1.,1.,1.,1.,1.,1.,1.,1.,1.,1.,1.,
1.,1.,1.,1.,1.,1.,1.,1.,1.,1.,1.,1.,1.,1.,1.,1.,1.,1.,1.,1.,1.,1.,1.,1.,
1.,1.,1.,1.,1.,1.,1.,1.,1.,1.,1.,1.,1.,1.,1.,1.,1.,1.,1.,1.,1.,1.,1.,1.,
1.,1.,1.,1.,1.,1.,1.,1.,1.,1.,1.,1.,1.,1.,1.,1.,1.,1.,1.,1.,1.,1.,1.,1.,
1.,1.,1.,1.,1.,1.,1.,1.,1.,1.,1.,1.,1.,1.,1.,1.,1.,1.,1.,1.,1.,1.,1.,1.,
1.,1.,1.,1.,1.,1.,1.,1.,1.,1.,1.,1.,1.,1.,1.,1.,1.,1.,1.,1.,1.,1.,1.,1.,
1.,1.,1.,1.,1.,1.,1.,1.,1.,1.,1.,1.,1.,1.,1.,1.,1.,1.,1.,1.,1.,1.,1.,1.,
1.,1.,1.,1.,1.,1.,1.,1.,1.,1.,1.,1.,1.,1.,1.,1.,1.,1.,1.,1.,1.,1.,1.,1.,
1.,1.,1.,1.,1.,1.,1.,1.,1.,1.))
REPRESENTATION_ITEM('')
);
#582=(
BOUNDED_CURVE()
B_SPLINE_CURVE(5,(#131217,#131218,#131219,#131220,#131221,#131222,#131223,
#131224,#131225,#131226,#131227,#131228,#131229,#131230,#131231,#131232,
#131233,#131234,#131235,#131236,#131237,#131238,#131239,#131240,#131241,
#131242,#131243,#131244,#131245,#131246,#131247,#131248,#131249,#131250,
#131251,#131252,#131253,#131254,#131255,#131256,#131257,#131258,#131259,
#131260,#131261,#131262,#131263,#131264,#131265,#131266,#131267,#131268,
#131269,#131270,#131271,#131272,#131273,#131274,#131275,#131276,#131277,
#131278,#131279,#131280,#131281,#131282,#131283,#131284,#131285,#131286,
#131287,#131288,#131289,#131290,#131291,#131292,#131293,#131294,#131295,
#131296,#131297,#131298,#131299,#131300,#131301,#131302,#131303,#131304,
#131305,#131306,#131307,#131308,#131309,#131310,#131311,#131312,#131313,
#131314,#131315,#131316,#131317,#131318,#131319,#131320,#131321,#131322,
#131323,#131324,#131325,#131326,#131327,#131328,#131329,#131330,#131331,
#131332,#131333,#131334,#131335,#131336,#131337,#131338,#131339,#131340,
#131341,#131342,#131343,#131344,#131345,#131346,#131347,#131348,#131349,
#131350,#131351,#131352,#131353,#131354,#131355,#131356,#131357,#131358,
#131359,#131360,#131361,#131362,#131363,#131364,#131365,#131366,#131367,
#131368,#131369,#131370,#131371,#131372,#131373,#131374,#131375,#131376,
#131377,#131378,#131379,#131380,#131381,#131382,#131383,#131384,#131385,
#131386,#131387,#131388,#131389,#131390,#131391,#131392,#131393,#131394,
#131395,#131396,#131397,#131398,#131399,#131400,#131401,#131402,#131403,
#131404,#131405,#131406,#131407,#131408,#131409,#131410),.UNSPECIFIED.,
 .F.,.F.)
B_SPLINE_CURVE_WITH_KNOTS((6,1,1,1,1,1,1,1,1,1,1,1,1,1,1,1,1,1,1,1,1,1,
1,1,1,1,1,1,1,1,1,1,1,1,1,1,1,1,1,1,1,1,1,1,1,1,1,1,1,1,1,1,1,1,1,1,1,1,
1,1,1,1,1,1,1,1,1,1,1,1,1,1,1,1,1,1,1,1,1,1,1,1,1,1,1,1,1,1,1,1,1,1,1,1,
1,1,1,1,1,1,1,1,1,1,1,1,1,1,1,1,1,1,1,1,1,1,1,1,1,1,1,1,1,1,1,1,1,1,1,1,
1,1,1,1,1,1,1,1,1,1,1,1,1,1,1,1,1,1,1,1,1,1,1,1,1,1,1,1,1,1,1,1,1,1,1,1,
1,1,1,1,1,1,1,1,1,1,1,1,1,1,1,1,1,1,1,1,1,1,1,6),(-0.941429844438051,-0.940000000000001,
-0.935000000000001,-0.930000000000001,-0.925000000000001,-0.920000000000001,
-0.915000000000001,-0.910000000000001,-0.905000000000001,-0.900000000000001,
-0.895000000000001,-0.890000000000001,-0.885000000000001,-0.880000000000001,
-0.875000000000001,-0.870000000000001,-0.865000000000001,-0.860000000000001,
-0.855000000000001,-0.850000000000001,-0.845000000000001,-0.840000000000001,
-0.835000000000001,-0.830000000000001,-0.825000000000001,-0.820000000000001,
-0.815000000000001,-0.810000000000001,-0.805000000000001,-0.800000000000001,
-0.795000000000001,-0.790000000000001,-0.785000000000001,-0.780000000000001,
-0.775000000000001,-0.770000000000001,-0.765000000000001,-0.760000000000001,
-0.755000000000001,-0.750000000000001,-0.745000000000001,-0.740000000000001,
-0.735000000000001,-0.730000000000001,-0.725000000000001,-0.720000000000001,
-0.715000000000001,-0.710000000000001,-0.705000000000001,-0.700000000000001,
-0.695000000000001,-0.690000000000001,-0.685,-0.68,-0.675,-0.67,-0.665,
-0.66,-0.655,-0.65,-0.645,-0.64,-0.635,-0.63,-0.625,-0.62,-0.615,-0.61,
-0.605,-0.6,-0.595,-0.59,-0.585,-0.58,-0.575,-0.57,-0.565,-0.56,-0.555,
-0.55,-0.545,-0.54,-0.535,-0.53,-0.525,-0.52,-0.515,-0.51,-0.505,-0.5,-0.495,
-0.49,-0.485,-0.48,-0.475,-0.47,-0.465,-0.46,-0.455,-0.45,-0.445,-0.44,
-0.435,-0.43,-0.425,-0.42,-0.415,-0.41,-0.405,-0.4,-0.395,-0.39,-0.385,
-0.38,-0.375,-0.37,-0.365,-0.36,-0.355,-0.35,-0.345,-0.34,-0.335,-0.33,
-0.325,-0.32,-0.315,-0.31,-0.305,-0.3,-0.295,-0.29,-0.285,-0.28,-0.275,
-0.27,-0.265,-0.26,-0.255,-0.25,-0.245,-0.24,-0.235,-0.23,-0.225,-0.22,
-0.215,-0.21,-0.205,-0.2,-0.195,-0.19,-0.185,-0.18,-0.175,-0.17,-0.165,
-0.16,-0.155,-0.15,-0.145,-0.14,-0.135,-0.13,-0.125,-0.12,-0.115,-0.11,
-0.105,-0.1,-0.095,-0.09,-0.085,-0.08,-0.075,-0.07,-0.065,-0.06,-0.055,
-0.05,-0.045,-0.04,-0.035,-0.03,-0.025,-0.02,-0.015,-0.01,-0.005,0.),
 .UNSPECIFIED.)
CURVE()
GEOMETRIC_REPRESENTATION_ITEM()
RATIONAL_B_SPLINE_CURVE((1.,1.,1.,1.,1.,1.,1.,1.,1.,1.,1.,1.,1.,1.,1.,1.,
1.,1.,1.,1.,1.,1.,1.,1.,1.,1.,1.,1.,1.,1.,1.,1.,1.,1.,1.,1.,1.,1.,1.,1.,
1.,1.,1.,1.,1.,1.,1.,1.,1.,1.,1.,1.,1.,1.,1.,1.,1.,1.,1.,1.,1.,1.,1.,1.,
1.,1.,1.,1.,1.,1.,1.,1.,1.,1.,1.,1.,1.,1.,1.,1.,1.,1.,1.,1.,1.,1.,1.,1.,
1.,1.,1.,1.,1.,1.,1.,1.,1.,1.,1.,1.,1.,1.,1.,1.,1.,1.,1.,1.,1.,1.,1.,1.,
1.,1.,1.,1.,1.,1.,1.,1.,1.,1.,1.,1.,1.,1.,1.,1.,1.,1.,1.,1.,1.,1.,1.,1.,
1.,1.,1.,1.,1.,1.,1.,1.,1.,1.,1.,1.,1.,1.,1.,1.,1.,1.,1.,1.,1.,1.,1.,1.,
1.,1.,1.,1.,1.,1.,1.,1.,1.,1.,1.,1.,1.,1.,1.,1.,1.,1.,1.,1.,1.,1.,1.,1.,
1.,1.,1.,1.,1.,1.,1.,1.,1.,1.))
REPRESENTATION_ITEM('')
);
#583=(
BOUNDED_CURVE()
B_SPLINE_CURVE(5,(#131822,#131823,#131824,#131825,#131826,#131827,#131828,
#131829,#131830,#131831,#131832,#131833,#131834,#131835,#131836,#131837,
#131838,#131839,#131840,#131841,#131842,#131843,#131844,#131845,#131846,
#131847,#131848,#131849,#131850,#131851,#131852,#131853,#131854,#131855,
#131856,#131857,#131858,#131859,#131860,#131861,#131862,#131863,#131864,
#131865,#131866,#131867,#131868,#131869,#131870,#131871,#131872,#131873,
#131874,#131875,#131876,#131877,#131878,#131879,#131880,#131881,#131882,
#131883,#131884,#131885,#131886,#131887,#131888,#131889,#131890,#131891,
#131892,#131893,#131894,#131895,#131896,#131897,#131898,#131899,#131900,
#131901,#131902,#131903,#131904,#131905,#131906,#131907,#131908,#131909,
#131910,#131911,#131912,#131913,#131914,#131915,#131916,#131917,#131918,
#131919,#131920,#131921,#131922,#131923,#131924,#131925,#131926,#131927,
#131928,#131929,#131930,#131931,#131932,#131933,#131934,#131935,#131936,
#131937,#131938,#131939,#131940,#131941,#131942,#131943,#131944,#131945,
#131946,#131947,#131948,#131949,#131950,#131951,#131952,#131953,#131954,
#131955,#131956,#131957,#131958,#131959,#131960,#131961,#131962,#131963,
#131964,#131965,#131966,#131967,#131968,#131969,#131970,#131971,#131972,
#131973,#131974,#131975,#131976,#131977,#131978,#131979,#131980,#131981,
#131982,#131983,#131984,#131985,#131986,#131987,#131988,#131989,#131990,
#131991,#131992,#131993,#131994,#131995,#131996,#131997,#131998,#131999,
#132000,#132001,#132002,#132003,#132004,#132005,#132006,#132007,#132008,
#132009,#132010,#132011,#132012,#132013,#132014,#132015),.UNSPECIFIED.,
 .F.,.F.)
B_SPLINE_CURVE_WITH_KNOTS((6,1,1,1,1,1,1,1,1,1,1,1,1,1,1,1,1,1,1,1,1,1,
1,1,1,1,1,1,1,1,1,1,1,1,1,1,1,1,1,1,1,1,1,1,1,1,1,1,1,1,1,1,1,1,1,1,1,1,
1,1,1,1,1,1,1,1,1,1,1,1,1,1,1,1,1,1,1,1,1,1,1,1,1,1,1,1,1,1,1,1,1,1,1,1,
1,1,1,1,1,1,1,1,1,1,1,1,1,1,1,1,1,1,1,1,1,1,1,1,1,1,1,1,1,1,1,1,1,1,1,1,
1,1,1,1,1,1,1,1,1,1,1,1,1,1,1,1,1,1,1,1,1,1,1,1,1,1,1,1,1,1,1,1,1,1,1,1,
1,1,1,1,1,1,1,1,1,1,1,1,1,1,1,1,1,1,1,1,1,1,1,6),(0.,0.005,0.01,0.015,0.02,
0.025,0.03,0.035,0.04,0.045,0.05,0.055,0.06,0.065,0.07,0.075,0.08,0.085,
0.09,0.095,0.1,0.105,0.11,0.115,0.12,0.125,0.13,0.135,0.14,0.145,0.15,0.155,
0.16,0.165,0.17,0.175,0.18,0.185,0.19,0.195,0.2,0.205,0.21,0.215,0.22,0.225,
0.23,0.235,0.24,0.245,0.25,0.255,0.26,0.265,0.27,0.275,0.28,0.285,0.29,
0.295,0.3,0.305,0.31,0.315,0.32,0.325,0.33,0.335,0.34,0.345,0.35,0.355,
0.36,0.365,0.37,0.375,0.38,0.385,0.39,0.395,0.4,0.405,0.41,0.415,0.42,0.425,
0.43,0.435,0.44,0.445,0.45,0.455,0.46,0.465,0.47,0.475,0.48,0.485,0.49,
0.495,0.5,0.505,0.51,0.515,0.52,0.525,0.53,0.535,0.54,0.545,0.55,0.555,
0.56,0.565,0.57,0.575,0.58,0.585,0.59,0.595,0.6,0.605,0.61,0.615,0.62,0.625,
0.63,0.635,0.64,0.645,0.65,0.655,0.66,0.665,0.67,0.675,0.68,0.685,0.690000000000001,
0.695000000000001,0.700000000000001,0.705000000000001,0.710000000000001,
0.715000000000001,0.720000000000001,0.725000000000001,0.730000000000001,
0.735000000000001,0.740000000000001,0.745000000000001,0.750000000000001,
0.755000000000001,0.760000000000001,0.765000000000001,0.770000000000001,
0.775000000000001,0.780000000000001,0.785000000000001,0.790000000000001,
0.795000000000001,0.800000000000001,0.805000000000001,0.810000000000001,
0.815000000000001,0.820000000000001,0.825000000000001,0.830000000000001,
0.835000000000001,0.840000000000001,0.845000000000001,0.850000000000001,
0.855000000000001,0.860000000000001,0.865000000000001,0.870000000000001,
0.875000000000001,0.880000000000001,0.885000000000001,0.890000000000001,
0.895000000000001,0.900000000000001,0.905000000000001,0.910000000000001,
0.915000000000001,0.920000000000001,0.925000000000001,0.930000000000001,
0.935000000000001,0.940000000000001,0.941429844438123),.UNSPECIFIED.)
CURVE()
GEOMETRIC_REPRESENTATION_ITEM()
RATIONAL_B_SPLINE_CURVE((1.,1.,1.,1.,1.,1.,1.,1.,1.,1.,1.,1.,1.,1.,1.,1.,
1.,1.,1.,1.,1.,1.,1.,1.,1.,1.,1.,1.,1.,1.,1.,1.,1.,1.,1.,1.,1.,1.,1.,1.,
1.,1.,1.,1.,1.,1.,1.,1.,1.,1.,1.,1.,1.,1.,1.,1.,1.,1.,1.,1.,1.,1.,1.,1.,
1.,1.,1.,1.,1.,1.,1.,1.,1.,1.,1.,1.,1.,1.,1.,1.,1.,1.,1.,1.,1.,1.,1.,1.,
1.,1.,1.,1.,1.,1.,1.,1.,1.,1.,1.,1.,1.,1.,1.,1.,1.,1.,1.,1.,1.,1.,1.,1.,
1.,1.,1.,1.,1.,1.,1.,1.,1.,1.,1.,1.,1.,1.,1.,1.,1.,1.,1.,1.,1.,1.,1.,1.,
1.,1.,1.,1.,1.,1.,1.,1.,1.,1.,1.,1.,1.,1.,1.,1.,1.,1.,1.,1.,1.,1.,1.,1.,
1.,1.,1.,1.,1.,1.,1.,1.,1.,1.,1.,1.,1.,1.,1.,1.,1.,1.,1.,1.,1.,1.,1.,1.,
1.,1.,1.,1.,1.,1.,1.,1.,1.,1.))
REPRESENTATION_ITEM('')
);
#584=(
BOUNDED_CURVE()
B_SPLINE_CURVE(5,(#132018,#132019,#132020,#132021,#132022,#132023,#132024,
#132025,#132026,#132027,#132028,#132029,#132030,#132031,#132032,#132033,
#132034,#132035,#132036,#132037,#132038,#132039,#132040,#132041,#132042,
#132043,#132044,#132045,#132046,#132047,#132048,#132049,#132050,#132051,
#132052,#132053,#132054,#132055,#132056,#132057,#132058,#132059,#132060,
#132061,#132062,#132063,#132064,#132065,#132066,#132067,#132068,#132069,
#132070,#132071,#132072,#132073,#132074,#132075,#132076,#132077,#132078,
#132079,#132080,#132081,#132082,#132083,#132084,#132085,#132086,#132087,
#132088,#132089,#132090,#132091,#132092,#132093,#132094,#132095,#132096,
#132097,#132098,#132099,#132100,#132101,#132102,#132103,#132104,#132105,
#132106,#132107,#132108,#132109,#132110,#132111,#132112,#132113,#132114,
#132115,#132116,#132117,#132118,#132119,#132120,#132121,#132122,#132123,
#132124,#132125,#132126,#132127,#132128,#132129,#132130,#132131,#132132,
#132133,#132134,#132135,#132136,#132137,#132138,#132139,#132140,#132141,
#132142,#132143,#132144,#132145,#132146,#132147,#132148,#132149,#132150,
#132151,#132152,#132153,#132154,#132155,#132156,#132157,#132158,#132159,
#132160,#132161,#132162,#132163,#132164,#132165,#132166,#132167,#132168,
#132169,#132170,#132171,#132172,#132173,#132174,#132175,#132176,#132177,
#132178,#132179,#132180,#132181,#132182,#132183,#132184,#132185,#132186,
#132187,#132188,#132189,#132190,#132191,#132192,#132193,#132194,#132195,
#132196,#132197,#132198,#132199,#132200,#132201,#132202,#132203,#132204,
#132205,#132206,#132207,#132208,#132209,#132210,#132211),.UNSPECIFIED.,
 .F.,.F.)
B_SPLINE_CURVE_WITH_KNOTS((6,1,1,1,1,1,1,1,1,1,1,1,1,1,1,1,1,1,1,1,1,1,
1,1,1,1,1,1,1,1,1,1,1,1,1,1,1,1,1,1,1,1,1,1,1,1,1,1,1,1,1,1,1,1,1,1,1,1,
1,1,1,1,1,1,1,1,1,1,1,1,1,1,1,1,1,1,1,1,1,1,1,1,1,1,1,1,1,1,1,1,1,1,1,1,
1,1,1,1,1,1,1,1,1,1,1,1,1,1,1,1,1,1,1,1,1,1,1,1,1,1,1,1,1,1,1,1,1,1,1,1,
1,1,1,1,1,1,1,1,1,1,1,1,1,1,1,1,1,1,1,1,1,1,1,1,1,1,1,1,1,1,1,1,1,1,1,1,
1,1,1,1,1,1,1,1,1,1,1,1,1,1,1,1,1,1,1,1,1,1,1,6),(-0.941429844438125,-0.940000000000001,
-0.935000000000001,-0.930000000000001,-0.925000000000001,-0.920000000000001,
-0.915000000000001,-0.910000000000001,-0.905000000000001,-0.900000000000001,
-0.895000000000001,-0.890000000000001,-0.885000000000001,-0.880000000000001,
-0.875000000000001,-0.870000000000001,-0.865000000000001,-0.860000000000001,
-0.855000000000001,-0.850000000000001,-0.845000000000001,-0.840000000000001,
-0.835000000000001,-0.830000000000001,-0.825000000000001,-0.820000000000001,
-0.815000000000001,-0.810000000000001,-0.805000000000001,-0.800000000000001,
-0.795000000000001,-0.790000000000001,-0.785000000000001,-0.780000000000001,
-0.775000000000001,-0.770000000000001,-0.765000000000001,-0.760000000000001,
-0.755000000000001,-0.750000000000001,-0.745000000000001,-0.740000000000001,
-0.735000000000001,-0.730000000000001,-0.725000000000001,-0.720000000000001,
-0.715000000000001,-0.710000000000001,-0.705000000000001,-0.700000000000001,
-0.695000000000001,-0.690000000000001,-0.685,-0.68,-0.675,-0.67,-0.665,
-0.66,-0.655,-0.65,-0.645,-0.64,-0.635,-0.63,-0.625,-0.62,-0.615,-0.61,
-0.605,-0.6,-0.595,-0.59,-0.585,-0.58,-0.575,-0.57,-0.565,-0.56,-0.555,
-0.55,-0.545,-0.54,-0.535,-0.53,-0.525,-0.52,-0.515,-0.51,-0.505,-0.5,-0.495,
-0.49,-0.485,-0.48,-0.475,-0.47,-0.465,-0.46,-0.455,-0.45,-0.445,-0.44,
-0.435,-0.43,-0.425,-0.42,-0.415,-0.41,-0.405,-0.4,-0.395,-0.39,-0.385,
-0.38,-0.375,-0.37,-0.365,-0.36,-0.355,-0.35,-0.345,-0.34,-0.335,-0.33,
-0.325,-0.32,-0.315,-0.31,-0.305,-0.3,-0.295,-0.29,-0.285,-0.28,-0.275,
-0.27,-0.265,-0.26,-0.255,-0.25,-0.245,-0.24,-0.235,-0.23,-0.225,-0.22,
-0.215,-0.21,-0.205,-0.2,-0.195,-0.19,-0.185,-0.18,-0.175,-0.17,-0.165,
-0.16,-0.155,-0.15,-0.145,-0.14,-0.135,-0.13,-0.125,-0.12,-0.115,-0.11,
-0.105,-0.1,-0.095,-0.09,-0.085,-0.08,-0.075,-0.07,-0.065,-0.06,-0.055,
-0.05,-0.045,-0.04,-0.035,-0.03,-0.025,-0.02,-0.015,-0.01,-0.005,0.),
 .UNSPECIFIED.)
CURVE()
GEOMETRIC_REPRESENTATION_ITEM()
RATIONAL_B_SPLINE_CURVE((1.,1.,1.,1.,1.,1.,1.,1.,1.,1.,1.,1.,1.,1.,1.,1.,
1.,1.,1.,1.,1.,1.,1.,1.,1.,1.,1.,1.,1.,1.,1.,1.,1.,1.,1.,1.,1.,1.,1.,1.,
1.,1.,1.,1.,1.,1.,1.,1.,1.,1.,1.,1.,1.,1.,1.,1.,1.,1.,1.,1.,1.,1.,1.,1.,
1.,1.,1.,1.,1.,1.,1.,1.,1.,1.,1.,1.,1.,1.,1.,1.,1.,1.,1.,1.,1.,1.,1.,1.,
1.,1.,1.,1.,1.,1.,1.,1.,1.,1.,1.,1.,1.,1.,1.,1.,1.,1.,1.,1.,1.,1.,1.,1.,
1.,1.,1.,1.,1.,1.,1.,1.,1.,1.,1.,1.,1.,1.,1.,1.,1.,1.,1.,1.,1.,1.,1.,1.,
1.,1.,1.,1.,1.,1.,1.,1.,1.,1.,1.,1.,1.,1.,1.,1.,1.,1.,1.,1.,1.,1.,1.,1.,
1.,1.,1.,1.,1.,1.,1.,1.,1.,1.,1.,1.,1.,1.,1.,1.,1.,1.,1.,1.,1.,1.,1.,1.,
1.,1.,1.,1.,1.,1.,1.,1.,1.,1.))
REPRESENTATION_ITEM('')
);
#585=(
BOUNDED_CURVE()
B_SPLINE_CURVE(5,(#132623,#132624,#132625,#132626,#132627,#132628,#132629,
#132630,#132631,#132632,#132633,#132634,#132635,#132636,#132637,#132638,
#132639,#132640,#132641,#132642,#132643,#132644,#132645,#132646,#132647,
#132648,#132649,#132650,#132651,#132652,#132653,#132654,#132655,#132656,
#132657,#132658,#132659,#132660,#132661,#132662,#132663,#132664,#132665,
#132666,#132667,#132668,#132669,#132670,#132671,#132672,#132673,#132674,
#132675,#132676,#132677,#132678,#132679,#132680,#132681,#132682,#132683,
#132684,#132685,#132686,#132687,#132688,#132689,#132690,#132691,#132692,
#132693,#132694,#132695,#132696,#132697,#132698,#132699,#132700,#132701,
#132702,#132703,#132704,#132705,#132706,#132707,#132708,#132709,#132710,
#132711,#132712,#132713,#132714,#132715,#132716,#132717,#132718,#132719,
#132720,#132721,#132722,#132723,#132724,#132725,#132726,#132727,#132728,
#132729,#132730,#132731,#132732,#132733,#132734,#132735,#132736,#132737,
#132738,#132739,#132740,#132741,#132742,#132743,#132744,#132745,#132746,
#132747,#132748,#132749,#132750,#132751,#132752,#132753,#132754,#132755,
#132756,#132757,#132758,#132759,#132760,#132761,#132762,#132763,#132764,
#132765,#132766,#132767,#132768,#132769,#132770,#132771,#132772,#132773,
#132774,#132775,#132776,#132777,#132778,#132779,#132780,#132781,#132782,
#132783,#132784,#132785,#132786,#132787,#132788,#132789,#132790,#132791,
#132792,#132793,#132794,#132795,#132796,#132797,#132798,#132799,#132800,
#132801,#132802,#132803,#132804,#132805,#132806,#132807,#132808,#132809,
#132810,#132811,#132812,#132813,#132814,#132815,#132816),.UNSPECIFIED.,
 .F.,.F.)
B_SPLINE_CURVE_WITH_KNOTS((6,1,1,1,1,1,1,1,1,1,1,1,1,1,1,1,1,1,1,1,1,1,
1,1,1,1,1,1,1,1,1,1,1,1,1,1,1,1,1,1,1,1,1,1,1,1,1,1,1,1,1,1,1,1,1,1,1,1,
1,1,1,1,1,1,1,1,1,1,1,1,1,1,1,1,1,1,1,1,1,1,1,1,1,1,1,1,1,1,1,1,1,1,1,1,
1,1,1,1,1,1,1,1,1,1,1,1,1,1,1,1,1,1,1,1,1,1,1,1,1,1,1,1,1,1,1,1,1,1,1,1,
1,1,1,1,1,1,1,1,1,1,1,1,1,1,1,1,1,1,1,1,1,1,1,1,1,1,1,1,1,1,1,1,1,1,1,1,
1,1,1,1,1,1,1,1,1,1,1,1,1,1,1,1,1,1,1,1,1,1,1,6),(0.,0.005,0.01,0.015,0.02,
0.025,0.03,0.035,0.04,0.045,0.05,0.055,0.06,0.065,0.07,0.075,0.08,0.085,
0.09,0.095,0.1,0.105,0.11,0.115,0.12,0.125,0.13,0.135,0.14,0.145,0.15,0.155,
0.16,0.165,0.17,0.175,0.18,0.185,0.19,0.195,0.2,0.205,0.21,0.215,0.22,0.225,
0.23,0.235,0.24,0.245,0.25,0.255,0.26,0.265,0.27,0.275,0.28,0.285,0.29,
0.295,0.3,0.305,0.31,0.315,0.32,0.325,0.33,0.335,0.34,0.345,0.35,0.355,
0.36,0.365,0.37,0.375,0.38,0.385,0.39,0.395,0.4,0.405,0.41,0.415,0.42,0.425,
0.43,0.435,0.44,0.445,0.45,0.455,0.46,0.465,0.47,0.475,0.48,0.485,0.49,
0.495,0.5,0.505,0.51,0.515,0.52,0.525,0.53,0.535,0.54,0.545,0.55,0.555,
0.56,0.565,0.57,0.575,0.58,0.585,0.59,0.595,0.6,0.605,0.61,0.615,0.62,0.625,
0.63,0.635,0.64,0.645,0.65,0.655,0.66,0.665,0.67,0.675,0.68,0.685,0.690000000000001,
0.695000000000001,0.700000000000001,0.705000000000001,0.710000000000001,
0.715000000000001,0.720000000000001,0.725000000000001,0.730000000000001,
0.735000000000001,0.740000000000001,0.745000000000001,0.750000000000001,
0.755000000000001,0.760000000000001,0.765000000000001,0.770000000000001,
0.775000000000001,0.780000000000001,0.785000000000001,0.790000000000001,
0.795000000000001,0.800000000000001,0.805000000000001,0.810000000000001,
0.815000000000001,0.820000000000001,0.825000000000001,0.830000000000001,
0.835000000000001,0.840000000000001,0.845000000000001,0.850000000000001,
0.855000000000001,0.860000000000001,0.865000000000001,0.870000000000001,
0.875000000000001,0.880000000000001,0.885000000000001,0.890000000000001,
0.895000000000001,0.900000000000001,0.905000000000001,0.910000000000001,
0.915000000000001,0.920000000000001,0.925000000000001,0.930000000000001,
0.935000000000001,0.940000000000001,0.941429844438013),.UNSPECIFIED.)
CURVE()
GEOMETRIC_REPRESENTATION_ITEM()
RATIONAL_B_SPLINE_CURVE((1.,1.,1.,1.,1.,1.,1.,1.,1.,1.,1.,1.,1.,1.,1.,1.,
1.,1.,1.,1.,1.,1.,1.,1.,1.,1.,1.,1.,1.,1.,1.,1.,1.,1.,1.,1.,1.,1.,1.,1.,
1.,1.,1.,1.,1.,1.,1.,1.,1.,1.,1.,1.,1.,1.,1.,1.,1.,1.,1.,1.,1.,1.,1.,1.,
1.,1.,1.,1.,1.,1.,1.,1.,1.,1.,1.,1.,1.,1.,1.,1.,1.,1.,1.,1.,1.,1.,1.,1.,
1.,1.,1.,1.,1.,1.,1.,1.,1.,1.,1.,1.,1.,1.,1.,1.,1.,1.,1.,1.,1.,1.,1.,1.,
1.,1.,1.,1.,1.,1.,1.,1.,1.,1.,1.,1.,1.,1.,1.,1.,1.,1.,1.,1.,1.,1.,1.,1.,
1.,1.,1.,1.,1.,1.,1.,1.,1.,1.,1.,1.,1.,1.,1.,1.,1.,1.,1.,1.,1.,1.,1.,1.,
1.,1.,1.,1.,1.,1.,1.,1.,1.,1.,1.,1.,1.,1.,1.,1.,1.,1.,1.,1.,1.,1.,1.,1.,
1.,1.,1.,1.,1.,1.,1.,1.,1.,1.))
REPRESENTATION_ITEM('')
);
#586=(
BOUNDED_CURVE()
B_SPLINE_CURVE(5,(#132819,#132820,#132821,#132822,#132823,#132824,#132825,
#132826,#132827,#132828,#132829,#132830,#132831,#132832,#132833,#132834,
#132835,#132836,#132837,#132838,#132839,#132840,#132841,#132842,#132843,
#132844,#132845,#132846,#132847,#132848,#132849,#132850,#132851,#132852,
#132853,#132854,#132855,#132856,#132857,#132858,#132859,#132860,#132861,
#132862,#132863,#132864,#132865,#132866,#132867,#132868,#132869,#132870,
#132871,#132872,#132873,#132874,#132875,#132876,#132877,#132878,#132879,
#132880,#132881,#132882,#132883,#132884,#132885,#132886,#132887,#132888,
#132889,#132890,#132891,#132892,#132893,#132894,#132895,#132896,#132897,
#132898,#132899,#132900,#132901,#132902,#132903,#132904,#132905,#132906,
#132907,#132908,#132909,#132910,#132911,#132912,#132913,#132914,#132915,
#132916,#132917,#132918,#132919,#132920,#132921,#132922,#132923,#132924,
#132925,#132926,#132927,#132928,#132929,#132930,#132931,#132932,#132933,
#132934,#132935,#132936,#132937,#132938,#132939,#132940,#132941,#132942,
#132943,#132944,#132945,#132946,#132947,#132948,#132949,#132950,#132951,
#132952,#132953,#132954,#132955,#132956,#132957,#132958,#132959,#132960,
#132961,#132962,#132963,#132964,#132965,#132966,#132967,#132968,#132969,
#132970,#132971,#132972,#132973,#132974,#132975,#132976,#132977,#132978,
#132979,#132980,#132981,#132982,#132983,#132984,#132985,#132986,#132987,
#132988,#132989,#132990,#132991,#132992,#132993,#132994,#132995,#132996,
#132997,#132998,#132999,#133000,#133001,#133002,#133003,#133004,#133005,
#133006,#133007,#133008,#133009,#133010,#133011,#133012),.UNSPECIFIED.,
 .F.,.F.)
B_SPLINE_CURVE_WITH_KNOTS((6,1,1,1,1,1,1,1,1,1,1,1,1,1,1,1,1,1,1,1,1,1,
1,1,1,1,1,1,1,1,1,1,1,1,1,1,1,1,1,1,1,1,1,1,1,1,1,1,1,1,1,1,1,1,1,1,1,1,
1,1,1,1,1,1,1,1,1,1,1,1,1,1,1,1,1,1,1,1,1,1,1,1,1,1,1,1,1,1,1,1,1,1,1,1,
1,1,1,1,1,1,1,1,1,1,1,1,1,1,1,1,1,1,1,1,1,1,1,1,1,1,1,1,1,1,1,1,1,1,1,1,
1,1,1,1,1,1,1,1,1,1,1,1,1,1,1,1,1,1,1,1,1,1,1,1,1,1,1,1,1,1,1,1,1,1,1,1,
1,1,1,1,1,1,1,1,1,1,1,1,1,1,1,1,1,1,1,1,1,1,1,6),(-0.941429844438012,-0.940000000000001,
-0.935000000000001,-0.930000000000001,-0.925000000000001,-0.920000000000001,
-0.915000000000001,-0.910000000000001,-0.905000000000001,-0.900000000000001,
-0.895000000000001,-0.890000000000001,-0.885000000000001,-0.880000000000001,
-0.875000000000001,-0.870000000000001,-0.865000000000001,-0.860000000000001,
-0.855000000000001,-0.850000000000001,-0.845000000000001,-0.840000000000001,
-0.835000000000001,-0.830000000000001,-0.825000000000001,-0.820000000000001,
-0.815000000000001,-0.810000000000001,-0.805000000000001,-0.800000000000001,
-0.795000000000001,-0.790000000000001,-0.785000000000001,-0.780000000000001,
-0.775000000000001,-0.770000000000001,-0.765000000000001,-0.760000000000001,
-0.755000000000001,-0.750000000000001,-0.745000000000001,-0.740000000000001,
-0.735000000000001,-0.730000000000001,-0.725000000000001,-0.720000000000001,
-0.715000000000001,-0.710000000000001,-0.705000000000001,-0.700000000000001,
-0.695000000000001,-0.690000000000001,-0.685,-0.68,-0.675,-0.67,-0.665,
-0.66,-0.655,-0.65,-0.645,-0.64,-0.635,-0.63,-0.625,-0.62,-0.615,-0.61,
-0.605,-0.6,-0.595,-0.59,-0.585,-0.58,-0.575,-0.57,-0.565,-0.56,-0.555,
-0.55,-0.545,-0.54,-0.535,-0.53,-0.525,-0.52,-0.515,-0.51,-0.505,-0.5,-0.495,
-0.49,-0.485,-0.48,-0.475,-0.47,-0.465,-0.46,-0.455,-0.45,-0.445,-0.44,
-0.435,-0.43,-0.425,-0.42,-0.415,-0.41,-0.405,-0.4,-0.395,-0.39,-0.385,
-0.38,-0.375,-0.37,-0.365,-0.36,-0.355,-0.35,-0.345,-0.34,-0.335,-0.33,
-0.325,-0.32,-0.315,-0.31,-0.305,-0.3,-0.295,-0.29,-0.285,-0.28,-0.275,
-0.27,-0.265,-0.26,-0.255,-0.25,-0.245,-0.24,-0.235,-0.23,-0.225,-0.22,
-0.215,-0.21,-0.205,-0.2,-0.195,-0.19,-0.185,-0.18,-0.175,-0.17,-0.165,
-0.16,-0.155,-0.15,-0.145,-0.14,-0.135,-0.13,-0.125,-0.12,-0.115,-0.11,
-0.105,-0.1,-0.095,-0.09,-0.085,-0.08,-0.075,-0.07,-0.065,-0.06,-0.055,
-0.05,-0.045,-0.04,-0.035,-0.03,-0.025,-0.02,-0.015,-0.01,-0.005,0.),
 .UNSPECIFIED.)
CURVE()
GEOMETRIC_REPRESENTATION_ITEM()
RATIONAL_B_SPLINE_CURVE((1.,1.,1.,1.,1.,1.,1.,1.,1.,1.,1.,1.,1.,1.,1.,1.,
1.,1.,1.,1.,1.,1.,1.,1.,1.,1.,1.,1.,1.,1.,1.,1.,1.,1.,1.,1.,1.,1.,1.,1.,
1.,1.,1.,1.,1.,1.,1.,1.,1.,1.,1.,1.,1.,1.,1.,1.,1.,1.,1.,1.,1.,1.,1.,1.,
1.,1.,1.,1.,1.,1.,1.,1.,1.,1.,1.,1.,1.,1.,1.,1.,1.,1.,1.,1.,1.,1.,1.,1.,
1.,1.,1.,1.,1.,1.,1.,1.,1.,1.,1.,1.,1.,1.,1.,1.,1.,1.,1.,1.,1.,1.,1.,1.,
1.,1.,1.,1.,1.,1.,1.,1.,1.,1.,1.,1.,1.,1.,1.,1.,1.,1.,1.,1.,1.,1.,1.,1.,
1.,1.,1.,1.,1.,1.,1.,1.,1.,1.,1.,1.,1.,1.,1.,1.,1.,1.,1.,1.,1.,1.,1.,1.,
1.,1.,1.,1.,1.,1.,1.,1.,1.,1.,1.,1.,1.,1.,1.,1.,1.,1.,1.,1.,1.,1.,1.,1.,
1.,1.,1.,1.,1.,1.,1.,1.,1.,1.))
REPRESENTATION_ITEM('')
);
#587=(
BOUNDED_CURVE()
B_SPLINE_CURVE(5,(#133424,#133425,#133426,#133427,#133428,#133429,#133430,
#133431,#133432,#133433,#133434,#133435,#133436,#133437,#133438,#133439,
#133440,#133441,#133442,#133443,#133444,#133445,#133446,#133447,#133448,
#133449,#133450,#133451,#133452,#133453,#133454,#133455,#133456,#133457,
#133458,#133459,#133460,#133461,#133462,#133463,#133464,#133465,#133466,
#133467,#133468,#133469,#133470,#133471,#133472,#133473,#133474,#133475,
#133476,#133477,#133478,#133479,#133480,#133481,#133482,#133483,#133484,
#133485,#133486,#133487,#133488,#133489,#133490,#133491,#133492,#133493,
#133494,#133495,#133496,#133497,#133498,#133499,#133500,#133501,#133502,
#133503,#133504,#133505,#133506,#133507,#133508,#133509,#133510,#133511,
#133512,#133513,#133514,#133515,#133516,#133517,#133518,#133519,#133520,
#133521,#133522,#133523,#133524,#133525,#133526,#133527,#133528,#133529,
#133530,#133531,#133532,#133533,#133534,#133535,#133536,#133537,#133538,
#133539,#133540,#133541,#133542,#133543,#133544,#133545,#133546,#133547,
#133548,#133549,#133550,#133551,#133552,#133553,#133554,#133555,#133556,
#133557,#133558,#133559,#133560,#133561,#133562,#133563,#133564,#133565,
#133566,#133567,#133568,#133569,#133570,#133571,#133572,#133573,#133574,
#133575,#133576,#133577,#133578,#133579,#133580,#133581,#133582,#133583,
#133584,#133585,#133586,#133587,#133588,#133589,#133590,#133591,#133592,
#133593,#133594,#133595,#133596,#133597,#133598,#133599,#133600,#133601,
#133602,#133603,#133604,#133605,#133606,#133607,#133608,#133609,#133610,
#133611,#133612,#133613,#133614,#133615,#133616,#133617),.UNSPECIFIED.,
 .F.,.F.)
B_SPLINE_CURVE_WITH_KNOTS((6,1,1,1,1,1,1,1,1,1,1,1,1,1,1,1,1,1,1,1,1,1,
1,1,1,1,1,1,1,1,1,1,1,1,1,1,1,1,1,1,1,1,1,1,1,1,1,1,1,1,1,1,1,1,1,1,1,1,
1,1,1,1,1,1,1,1,1,1,1,1,1,1,1,1,1,1,1,1,1,1,1,1,1,1,1,1,1,1,1,1,1,1,1,1,
1,1,1,1,1,1,1,1,1,1,1,1,1,1,1,1,1,1,1,1,1,1,1,1,1,1,1,1,1,1,1,1,1,1,1,1,
1,1,1,1,1,1,1,1,1,1,1,1,1,1,1,1,1,1,1,1,1,1,1,1,1,1,1,1,1,1,1,1,1,1,1,1,
1,1,1,1,1,1,1,1,1,1,1,1,1,1,1,1,1,1,1,1,1,1,1,6),(0.,0.005,0.01,0.015,0.02,
0.025,0.03,0.035,0.04,0.045,0.05,0.055,0.06,0.065,0.07,0.075,0.08,0.085,
0.09,0.095,0.1,0.105,0.11,0.115,0.12,0.125,0.13,0.135,0.14,0.145,0.15,0.155,
0.16,0.165,0.17,0.175,0.18,0.185,0.19,0.195,0.2,0.205,0.21,0.215,0.22,0.225,
0.23,0.235,0.24,0.245,0.25,0.255,0.26,0.265,0.27,0.275,0.28,0.285,0.29,
0.295,0.3,0.305,0.31,0.315,0.32,0.325,0.33,0.335,0.34,0.345,0.35,0.355,
0.36,0.365,0.37,0.375,0.38,0.385,0.39,0.395,0.4,0.405,0.41,0.415,0.42,0.425,
0.43,0.435,0.44,0.445,0.45,0.455,0.46,0.465,0.47,0.475,0.48,0.485,0.49,
0.495,0.5,0.505,0.51,0.515,0.52,0.525,0.53,0.535,0.54,0.545,0.55,0.555,
0.56,0.565,0.57,0.575,0.58,0.585,0.59,0.595,0.6,0.605,0.61,0.615,0.62,0.625,
0.63,0.635,0.64,0.645,0.65,0.655,0.66,0.665,0.67,0.675,0.68,0.685,0.690000000000001,
0.695000000000001,0.700000000000001,0.705000000000001,0.710000000000001,
0.715000000000001,0.720000000000001,0.725000000000001,0.730000000000001,
0.735000000000001,0.740000000000001,0.745000000000001,0.750000000000001,
0.755000000000001,0.760000000000001,0.765000000000001,0.770000000000001,
0.775000000000001,0.780000000000001,0.785000000000001,0.790000000000001,
0.795000000000001,0.800000000000001,0.805000000000001,0.810000000000001,
0.815000000000001,0.820000000000001,0.825000000000001,0.830000000000001,
0.835000000000001,0.840000000000001,0.845000000000001,0.850000000000001,
0.855000000000001,0.860000000000001,0.865000000000001,0.870000000000001,
0.875000000000001,0.880000000000001,0.885000000000001,0.890000000000001,
0.895000000000001,0.900000000000001,0.905000000000001,0.910000000000001,
0.915000000000001,0.920000000000001,0.925000000000001,0.930000000000001,
0.935000000000001,0.940000000000001,0.941429844438085),.UNSPECIFIED.)
CURVE()
GEOMETRIC_REPRESENTATION_ITEM()
RATIONAL_B_SPLINE_CURVE((1.,1.,1.,1.,1.,1.,1.,1.,1.,1.,1.,1.,1.,1.,1.,1.,
1.,1.,1.,1.,1.,1.,1.,1.,1.,1.,1.,1.,1.,1.,1.,1.,1.,1.,1.,1.,1.,1.,1.,1.,
1.,1.,1.,1.,1.,1.,1.,1.,1.,1.,1.,1.,1.,1.,1.,1.,1.,1.,1.,1.,1.,1.,1.,1.,
1.,1.,1.,1.,1.,1.,1.,1.,1.,1.,1.,1.,1.,1.,1.,1.,1.,1.,1.,1.,1.,1.,1.,1.,
1.,1.,1.,1.,1.,1.,1.,1.,1.,1.,1.,1.,1.,1.,1.,1.,1.,1.,1.,1.,1.,1.,1.,1.,
1.,1.,1.,1.,1.,1.,1.,1.,1.,1.,1.,1.,1.,1.,1.,1.,1.,1.,1.,1.,1.,1.,1.,1.,
1.,1.,1.,1.,1.,1.,1.,1.,1.,1.,1.,1.,1.,1.,1.,1.,1.,1.,1.,1.,1.,1.,1.,1.,
1.,1.,1.,1.,1.,1.,1.,1.,1.,1.,1.,1.,1.,1.,1.,1.,1.,1.,1.,1.,1.,1.,1.,1.,
1.,1.,1.,1.,1.,1.,1.,1.,1.,1.))
REPRESENTATION_ITEM('')
);
#588=(
BOUNDED_CURVE()
B_SPLINE_CURVE(5,(#133620,#133621,#133622,#133623,#133624,#133625,#133626,
#133627,#133628,#133629,#133630,#133631,#133632,#133633,#133634,#133635,
#133636,#133637,#133638,#133639,#133640,#133641,#133642,#133643,#133644,
#133645,#133646,#133647,#133648,#133649,#133650,#133651,#133652,#133653,
#133654,#133655,#133656,#133657,#133658,#133659,#133660,#133661,#133662,
#133663,#133664,#133665,#133666,#133667,#133668,#133669,#133670,#133671,
#133672,#133673,#133674,#133675,#133676,#133677,#133678,#133679,#133680,
#133681,#133682,#133683,#133684,#133685,#133686,#133687,#133688,#133689,
#133690,#133691,#133692,#133693,#133694,#133695,#133696,#133697,#133698,
#133699,#133700,#133701,#133702,#133703,#133704,#133705,#133706,#133707,
#133708,#133709,#133710,#133711,#133712,#133713,#133714,#133715,#133716,
#133717,#133718,#133719,#133720,#133721,#133722,#133723,#133724,#133725,
#133726,#133727,#133728,#133729,#133730,#133731,#133732,#133733,#133734,
#133735,#133736,#133737,#133738,#133739,#133740,#133741,#133742,#133743,
#133744,#133745,#133746,#133747,#133748,#133749,#133750,#133751,#133752,
#133753,#133754,#133755,#133756,#133757,#133758,#133759,#133760,#133761,
#133762,#133763,#133764,#133765,#133766,#133767,#133768,#133769,#133770,
#133771,#133772,#133773,#133774,#133775,#133776,#133777,#133778,#133779,
#133780,#133781,#133782,#133783,#133784,#133785,#133786,#133787,#133788,
#133789,#133790,#133791,#133792,#133793,#133794,#133795,#133796,#133797,
#133798,#133799,#133800,#133801,#133802,#133803,#133804,#133805,#133806,
#133807,#133808,#133809,#133810,#133811,#133812,#133813),.UNSPECIFIED.,
 .F.,.F.)
B_SPLINE_CURVE_WITH_KNOTS((6,1,1,1,1,1,1,1,1,1,1,1,1,1,1,1,1,1,1,1,1,1,
1,1,1,1,1,1,1,1,1,1,1,1,1,1,1,1,1,1,1,1,1,1,1,1,1,1,1,1,1,1,1,1,1,1,1,1,
1,1,1,1,1,1,1,1,1,1,1,1,1,1,1,1,1,1,1,1,1,1,1,1,1,1,1,1,1,1,1,1,1,1,1,1,
1,1,1,1,1,1,1,1,1,1,1,1,1,1,1,1,1,1,1,1,1,1,1,1,1,1,1,1,1,1,1,1,1,1,1,1,
1,1,1,1,1,1,1,1,1,1,1,1,1,1,1,1,1,1,1,1,1,1,1,1,1,1,1,1,1,1,1,1,1,1,1,1,
1,1,1,1,1,1,1,1,1,1,1,1,1,1,1,1,1,1,1,1,1,1,1,6),(-0.941429844438085,-0.940000000000001,
-0.935000000000001,-0.930000000000001,-0.925000000000001,-0.920000000000001,
-0.915000000000001,-0.910000000000001,-0.905000000000001,-0.900000000000001,
-0.895000000000001,-0.890000000000001,-0.885000000000001,-0.880000000000001,
-0.875000000000001,-0.870000000000001,-0.865000000000001,-0.860000000000001,
-0.855000000000001,-0.850000000000001,-0.845000000000001,-0.840000000000001,
-0.835000000000001,-0.830000000000001,-0.825000000000001,-0.820000000000001,
-0.815000000000001,-0.810000000000001,-0.805000000000001,-0.800000000000001,
-0.795000000000001,-0.790000000000001,-0.785000000000001,-0.780000000000001,
-0.775000000000001,-0.770000000000001,-0.765000000000001,-0.760000000000001,
-0.755000000000001,-0.750000000000001,-0.745000000000001,-0.740000000000001,
-0.735000000000001,-0.730000000000001,-0.725000000000001,-0.720000000000001,
-0.715000000000001,-0.710000000000001,-0.705000000000001,-0.700000000000001,
-0.695000000000001,-0.690000000000001,-0.685,-0.68,-0.675,-0.67,-0.665,
-0.66,-0.655,-0.65,-0.645,-0.64,-0.635,-0.63,-0.625,-0.62,-0.615,-0.61,
-0.605,-0.6,-0.595,-0.59,-0.585,-0.58,-0.575,-0.57,-0.565,-0.56,-0.555,
-0.55,-0.545,-0.54,-0.535,-0.53,-0.525,-0.52,-0.515,-0.51,-0.505,-0.5,-0.495,
-0.49,-0.485,-0.48,-0.475,-0.47,-0.465,-0.46,-0.455,-0.45,-0.445,-0.44,
-0.435,-0.43,-0.425,-0.42,-0.415,-0.41,-0.405,-0.4,-0.395,-0.39,-0.385,
-0.38,-0.375,-0.37,-0.365,-0.36,-0.355,-0.35,-0.345,-0.34,-0.335,-0.33,
-0.325,-0.32,-0.315,-0.31,-0.305,-0.3,-0.295,-0.29,-0.285,-0.28,-0.275,
-0.27,-0.265,-0.26,-0.255,-0.25,-0.245,-0.24,-0.235,-0.23,-0.225,-0.22,
-0.215,-0.21,-0.205,-0.2,-0.195,-0.19,-0.185,-0.18,-0.175,-0.17,-0.165,
-0.16,-0.155,-0.15,-0.145,-0.14,-0.135,-0.13,-0.125,-0.12,-0.115,-0.11,
-0.105,-0.1,-0.095,-0.09,-0.085,-0.08,-0.075,-0.07,-0.065,-0.06,-0.055,
-0.05,-0.045,-0.04,-0.035,-0.03,-0.025,-0.02,-0.015,-0.01,-0.005,0.),
 .UNSPECIFIED.)
CURVE()
GEOMETRIC_REPRESENTATION_ITEM()
RATIONAL_B_SPLINE_CURVE((1.,1.,1.,1.,1.,1.,1.,1.,1.,1.,1.,1.,1.,1.,1.,1.,
1.,1.,1.,1.,1.,1.,1.,1.,1.,1.,1.,1.,1.,1.,1.,1.,1.,1.,1.,1.,1.,1.,1.,1.,
1.,1.,1.,1.,1.,1.,1.,1.,1.,1.,1.,1.,1.,1.,1.,1.,1.,1.,1.,1.,1.,1.,1.,1.,
1.,1.,1.,1.,1.,1.,1.,1.,1.,1.,1.,1.,1.,1.,1.,1.,1.,1.,1.,1.,1.,1.,1.,1.,
1.,1.,1.,1.,1.,1.,1.,1.,1.,1.,1.,1.,1.,1.,1.,1.,1.,1.,1.,1.,1.,1.,1.,1.,
1.,1.,1.,1.,1.,1.,1.,1.,1.,1.,1.,1.,1.,1.,1.,1.,1.,1.,1.,1.,1.,1.,1.,1.,
1.,1.,1.,1.,1.,1.,1.,1.,1.,1.,1.,1.,1.,1.,1.,1.,1.,1.,1.,1.,1.,1.,1.,1.,
1.,1.,1.,1.,1.,1.,1.,1.,1.,1.,1.,1.,1.,1.,1.,1.,1.,1.,1.,1.,1.,1.,1.,1.,
1.,1.,1.,1.,1.,1.,1.,1.,1.,1.))
REPRESENTATION_ITEM('')
);
#589=(
BOUNDED_CURVE()
B_SPLINE_CURVE(5,(#134225,#134226,#134227,#134228,#134229,#134230,#134231,
#134232,#134233,#134234,#134235,#134236,#134237,#134238,#134239,#134240,
#134241,#134242,#134243,#134244,#134245,#134246,#134247,#134248,#134249,
#134250,#134251,#134252,#134253,#134254,#134255,#134256,#134257,#134258,
#134259,#134260,#134261,#134262,#134263,#134264,#134265,#134266,#134267,
#134268,#134269,#134270,#134271,#134272,#134273,#134274,#134275,#134276,
#134277,#134278,#134279,#134280,#134281,#134282,#134283,#134284,#134285,
#134286,#134287,#134288,#134289,#134290,#134291,#134292,#134293,#134294,
#134295,#134296,#134297,#134298,#134299,#134300,#134301,#134302,#134303,
#134304,#134305,#134306,#134307,#134308,#134309,#134310,#134311,#134312,
#134313,#134314,#134315,#134316,#134317,#134318,#134319,#134320,#134321,
#134322,#134323,#134324,#134325,#134326,#134327,#134328,#134329,#134330,
#134331,#134332,#134333,#134334,#134335,#134336,#134337,#134338,#134339,
#134340,#134341,#134342,#134343,#134344,#134345,#134346,#134347,#134348,
#134349,#134350,#134351,#134352,#134353,#134354,#134355,#134356,#134357,
#134358,#134359,#134360,#134361,#134362,#134363,#134364,#134365,#134366,
#134367,#134368,#134369,#134370,#134371,#134372,#134373,#134374,#134375,
#134376,#134377,#134378,#134379,#134380,#134381,#134382,#134383,#134384,
#134385,#134386,#134387,#134388,#134389,#134390,#134391,#134392,#134393,
#134394,#134395,#134396,#134397,#134398,#134399,#134400,#134401,#134402,
#134403,#134404,#134405,#134406,#134407,#134408,#134409,#134410,#134411,
#134412,#134413,#134414,#134415,#134416,#134417,#134418),.UNSPECIFIED.,
 .F.,.F.)
B_SPLINE_CURVE_WITH_KNOTS((6,1,1,1,1,1,1,1,1,1,1,1,1,1,1,1,1,1,1,1,1,1,
1,1,1,1,1,1,1,1,1,1,1,1,1,1,1,1,1,1,1,1,1,1,1,1,1,1,1,1,1,1,1,1,1,1,1,1,
1,1,1,1,1,1,1,1,1,1,1,1,1,1,1,1,1,1,1,1,1,1,1,1,1,1,1,1,1,1,1,1,1,1,1,1,
1,1,1,1,1,1,1,1,1,1,1,1,1,1,1,1,1,1,1,1,1,1,1,1,1,1,1,1,1,1,1,1,1,1,1,1,
1,1,1,1,1,1,1,1,1,1,1,1,1,1,1,1,1,1,1,1,1,1,1,1,1,1,1,1,1,1,1,1,1,1,1,1,
1,1,1,1,1,1,1,1,1,1,1,1,1,1,1,1,1,1,1,1,1,1,1,6),(0.,0.005,0.01,0.015,0.02,
0.025,0.03,0.035,0.04,0.045,0.05,0.055,0.06,0.065,0.07,0.075,0.08,0.085,
0.09,0.095,0.1,0.105,0.11,0.115,0.12,0.125,0.13,0.135,0.14,0.145,0.15,0.155,
0.16,0.165,0.17,0.175,0.18,0.185,0.19,0.195,0.2,0.205,0.21,0.215,0.22,0.225,
0.23,0.235,0.24,0.245,0.25,0.255,0.26,0.265,0.27,0.275,0.28,0.285,0.29,
0.295,0.3,0.305,0.31,0.315,0.32,0.325,0.33,0.335,0.34,0.345,0.35,0.355,
0.36,0.365,0.37,0.375,0.38,0.385,0.39,0.395,0.4,0.405,0.41,0.415,0.42,0.425,
0.43,0.435,0.44,0.445,0.45,0.455,0.46,0.465,0.47,0.475,0.48,0.485,0.49,
0.495,0.5,0.505,0.51,0.515,0.52,0.525,0.53,0.535,0.54,0.545,0.55,0.555,
0.56,0.565,0.57,0.575,0.58,0.585,0.59,0.595,0.6,0.605,0.61,0.615,0.62,0.625,
0.63,0.635,0.64,0.645,0.65,0.655,0.66,0.665,0.67,0.675,0.68,0.685,0.690000000000001,
0.695000000000001,0.700000000000001,0.705000000000001,0.710000000000001,
0.715000000000001,0.720000000000001,0.725000000000001,0.730000000000001,
0.735000000000001,0.740000000000001,0.745000000000001,0.750000000000001,
0.755000000000001,0.760000000000001,0.765000000000001,0.770000000000001,
0.775000000000001,0.780000000000001,0.785000000000001,0.790000000000001,
0.795000000000001,0.800000000000001,0.805000000000001,0.810000000000001,
0.815000000000001,0.820000000000001,0.825000000000001,0.830000000000001,
0.835000000000001,0.840000000000001,0.845000000000001,0.850000000000001,
0.855000000000001,0.860000000000001,0.865000000000001,0.870000000000001,
0.875000000000001,0.880000000000001,0.885000000000001,0.890000000000001,
0.895000000000001,0.900000000000001,0.905000000000001,0.910000000000001,
0.915000000000001,0.920000000000001,0.925000000000001,0.930000000000001,
0.935000000000001,0.940000000000001,0.941429844438033),.UNSPECIFIED.)
CURVE()
GEOMETRIC_REPRESENTATION_ITEM()
RATIONAL_B_SPLINE_CURVE((1.,1.,1.,1.,1.,1.,1.,1.,1.,1.,1.,1.,1.,1.,1.,1.,
1.,1.,1.,1.,1.,1.,1.,1.,1.,1.,1.,1.,1.,1.,1.,1.,1.,1.,1.,1.,1.,1.,1.,1.,
1.,1.,1.,1.,1.,1.,1.,1.,1.,1.,1.,1.,1.,1.,1.,1.,1.,1.,1.,1.,1.,1.,1.,1.,
1.,1.,1.,1.,1.,1.,1.,1.,1.,1.,1.,1.,1.,1.,1.,1.,1.,1.,1.,1.,1.,1.,1.,1.,
1.,1.,1.,1.,1.,1.,1.,1.,1.,1.,1.,1.,1.,1.,1.,1.,1.,1.,1.,1.,1.,1.,1.,1.,
1.,1.,1.,1.,1.,1.,1.,1.,1.,1.,1.,1.,1.,1.,1.,1.,1.,1.,1.,1.,1.,1.,1.,1.,
1.,1.,1.,1.,1.,1.,1.,1.,1.,1.,1.,1.,1.,1.,1.,1.,1.,1.,1.,1.,1.,1.,1.,1.,
1.,1.,1.,1.,1.,1.,1.,1.,1.,1.,1.,1.,1.,1.,1.,1.,1.,1.,1.,1.,1.,1.,1.,1.,
1.,1.,1.,1.,1.,1.,1.,1.,1.,1.))
REPRESENTATION_ITEM('')
);
#590=(
BOUNDED_CURVE()
B_SPLINE_CURVE(5,(#134421,#134422,#134423,#134424,#134425,#134426,#134427,
#134428,#134429,#134430,#134431,#134432,#134433,#134434,#134435,#134436,
#134437,#134438,#134439,#134440,#134441,#134442,#134443,#134444,#134445,
#134446,#134447,#134448,#134449,#134450,#134451,#134452,#134453,#134454,
#134455,#134456,#134457,#134458,#134459,#134460,#134461,#134462,#134463,
#134464,#134465,#134466,#134467,#134468,#134469,#134470,#134471,#134472,
#134473,#134474,#134475,#134476,#134477,#134478,#134479,#134480,#134481,
#134482,#134483,#134484,#134485,#134486,#134487,#134488,#134489,#134490,
#134491,#134492,#134493,#134494,#134495,#134496,#134497,#134498,#134499,
#134500,#134501,#134502,#134503,#134504,#134505,#134506,#134507,#134508,
#134509,#134510,#134511,#134512,#134513,#134514,#134515,#134516,#134517,
#134518,#134519,#134520,#134521,#134522,#134523,#134524,#134525,#134526,
#134527,#134528,#134529,#134530,#134531,#134532,#134533,#134534,#134535,
#134536,#134537,#134538,#134539,#134540,#134541,#134542,#134543,#134544,
#134545,#134546,#134547,#134548,#134549,#134550,#134551,#134552,#134553,
#134554,#134555,#134556,#134557,#134558,#134559,#134560,#134561,#134562,
#134563,#134564,#134565,#134566,#134567,#134568,#134569,#134570,#134571,
#134572,#134573,#134574,#134575,#134576,#134577,#134578,#134579,#134580,
#134581,#134582,#134583,#134584,#134585,#134586,#134587,#134588,#134589,
#134590,#134591,#134592,#134593,#134594,#134595,#134596,#134597,#134598,
#134599,#134600,#134601,#134602,#134603,#134604,#134605,#134606,#134607,
#134608,#134609,#134610,#134611,#134612,#134613,#134614),.UNSPECIFIED.,
 .F.,.F.)
B_SPLINE_CURVE_WITH_KNOTS((6,1,1,1,1,1,1,1,1,1,1,1,1,1,1,1,1,1,1,1,1,1,
1,1,1,1,1,1,1,1,1,1,1,1,1,1,1,1,1,1,1,1,1,1,1,1,1,1,1,1,1,1,1,1,1,1,1,1,
1,1,1,1,1,1,1,1,1,1,1,1,1,1,1,1,1,1,1,1,1,1,1,1,1,1,1,1,1,1,1,1,1,1,1,1,
1,1,1,1,1,1,1,1,1,1,1,1,1,1,1,1,1,1,1,1,1,1,1,1,1,1,1,1,1,1,1,1,1,1,1,1,
1,1,1,1,1,1,1,1,1,1,1,1,1,1,1,1,1,1,1,1,1,1,1,1,1,1,1,1,1,1,1,1,1,1,1,1,
1,1,1,1,1,1,1,1,1,1,1,1,1,1,1,1,1,1,1,1,1,1,1,6),(-0.941429844438033,-0.940000000000001,
-0.935000000000001,-0.930000000000001,-0.925000000000001,-0.920000000000001,
-0.915000000000001,-0.910000000000001,-0.905000000000001,-0.900000000000001,
-0.895000000000001,-0.890000000000001,-0.885000000000001,-0.880000000000001,
-0.875000000000001,-0.870000000000001,-0.865000000000001,-0.860000000000001,
-0.855000000000001,-0.850000000000001,-0.845000000000001,-0.840000000000001,
-0.835000000000001,-0.830000000000001,-0.825000000000001,-0.820000000000001,
-0.815000000000001,-0.810000000000001,-0.805000000000001,-0.800000000000001,
-0.795000000000001,-0.790000000000001,-0.785000000000001,-0.780000000000001,
-0.775000000000001,-0.770000000000001,-0.765000000000001,-0.760000000000001,
-0.755000000000001,-0.750000000000001,-0.745000000000001,-0.740000000000001,
-0.735000000000001,-0.730000000000001,-0.725000000000001,-0.720000000000001,
-0.715000000000001,-0.710000000000001,-0.705000000000001,-0.700000000000001,
-0.695000000000001,-0.690000000000001,-0.685,-0.68,-0.675,-0.67,-0.665,
-0.66,-0.655,-0.65,-0.645,-0.64,-0.635,-0.63,-0.625,-0.62,-0.615,-0.61,
-0.605,-0.6,-0.595,-0.59,-0.585,-0.58,-0.575,-0.57,-0.565,-0.56,-0.555,
-0.55,-0.545,-0.54,-0.535,-0.53,-0.525,-0.52,-0.515,-0.51,-0.505,-0.5,-0.495,
-0.49,-0.485,-0.48,-0.475,-0.47,-0.465,-0.46,-0.455,-0.45,-0.445,-0.44,
-0.435,-0.43,-0.425,-0.42,-0.415,-0.41,-0.405,-0.4,-0.395,-0.39,-0.385,
-0.38,-0.375,-0.37,-0.365,-0.36,-0.355,-0.35,-0.345,-0.34,-0.335,-0.33,
-0.325,-0.32,-0.315,-0.31,-0.305,-0.3,-0.295,-0.29,-0.285,-0.28,-0.275,
-0.27,-0.265,-0.26,-0.255,-0.25,-0.245,-0.24,-0.235,-0.23,-0.225,-0.22,
-0.215,-0.21,-0.205,-0.2,-0.195,-0.19,-0.185,-0.18,-0.175,-0.17,-0.165,
-0.16,-0.155,-0.15,-0.145,-0.14,-0.135,-0.13,-0.125,-0.12,-0.115,-0.11,
-0.105,-0.1,-0.095,-0.09,-0.085,-0.08,-0.075,-0.07,-0.065,-0.06,-0.055,
-0.05,-0.045,-0.04,-0.035,-0.03,-0.025,-0.02,-0.015,-0.01,-0.005,0.),
 .UNSPECIFIED.)
CURVE()
GEOMETRIC_REPRESENTATION_ITEM()
RATIONAL_B_SPLINE_CURVE((1.,1.,1.,1.,1.,1.,1.,1.,1.,1.,1.,1.,1.,1.,1.,1.,
1.,1.,1.,1.,1.,1.,1.,1.,1.,1.,1.,1.,1.,1.,1.,1.,1.,1.,1.,1.,1.,1.,1.,1.,
1.,1.,1.,1.,1.,1.,1.,1.,1.,1.,1.,1.,1.,1.,1.,1.,1.,1.,1.,1.,1.,1.,1.,1.,
1.,1.,1.,1.,1.,1.,1.,1.,1.,1.,1.,1.,1.,1.,1.,1.,1.,1.,1.,1.,1.,1.,1.,1.,
1.,1.,1.,1.,1.,1.,1.,1.,1.,1.,1.,1.,1.,1.,1.,1.,1.,1.,1.,1.,1.,1.,1.,1.,
1.,1.,1.,1.,1.,1.,1.,1.,1.,1.,1.,1.,1.,1.,1.,1.,1.,1.,1.,1.,1.,1.,1.,1.,
1.,1.,1.,1.,1.,1.,1.,1.,1.,1.,1.,1.,1.,1.,1.,1.,1.,1.,1.,1.,1.,1.,1.,1.,
1.,1.,1.,1.,1.,1.,1.,1.,1.,1.,1.,1.,1.,1.,1.,1.,1.,1.,1.,1.,1.,1.,1.,1.,
1.,1.,1.,1.,1.,1.,1.,1.,1.,1.))
REPRESENTATION_ITEM('')
);
#591=(
BOUNDED_CURVE()
B_SPLINE_CURVE(5,(#135026,#135027,#135028,#135029,#135030,#135031,#135032,
#135033,#135034,#135035,#135036,#135037,#135038,#135039,#135040,#135041,
#135042,#135043,#135044,#135045,#135046,#135047,#135048,#135049,#135050,
#135051,#135052,#135053,#135054,#135055,#135056,#135057,#135058,#135059,
#135060,#135061,#135062,#135063,#135064,#135065,#135066,#135067,#135068,
#135069,#135070,#135071,#135072,#135073,#135074,#135075,#135076,#135077,
#135078,#135079,#135080,#135081,#135082,#135083,#135084,#135085,#135086,
#135087,#135088,#135089,#135090,#135091,#135092,#135093,#135094,#135095,
#135096,#135097,#135098,#135099,#135100,#135101,#135102,#135103,#135104,
#135105,#135106,#135107,#135108,#135109,#135110,#135111,#135112,#135113,
#135114,#135115,#135116,#135117,#135118,#135119,#135120,#135121,#135122,
#135123,#135124,#135125,#135126,#135127,#135128,#135129,#135130,#135131,
#135132,#135133,#135134,#135135,#135136,#135137,#135138,#135139,#135140,
#135141,#135142,#135143,#135144,#135145,#135146,#135147,#135148,#135149,
#135150,#135151,#135152,#135153,#135154,#135155,#135156,#135157,#135158,
#135159,#135160,#135161,#135162,#135163,#135164,#135165,#135166,#135167,
#135168,#135169,#135170,#135171,#135172,#135173,#135174,#135175,#135176,
#135177,#135178,#135179,#135180,#135181,#135182,#135183,#135184,#135185,
#135186,#135187,#135188,#135189,#135190,#135191,#135192,#135193,#135194,
#135195,#135196,#135197,#135198,#135199,#135200,#135201,#135202,#135203,
#135204,#135205,#135206,#135207,#135208,#135209,#135210,#135211,#135212,
#135213,#135214,#135215,#135216,#135217,#135218,#135219),.UNSPECIFIED.,
 .F.,.F.)
B_SPLINE_CURVE_WITH_KNOTS((6,1,1,1,1,1,1,1,1,1,1,1,1,1,1,1,1,1,1,1,1,1,
1,1,1,1,1,1,1,1,1,1,1,1,1,1,1,1,1,1,1,1,1,1,1,1,1,1,1,1,1,1,1,1,1,1,1,1,
1,1,1,1,1,1,1,1,1,1,1,1,1,1,1,1,1,1,1,1,1,1,1,1,1,1,1,1,1,1,1,1,1,1,1,1,
1,1,1,1,1,1,1,1,1,1,1,1,1,1,1,1,1,1,1,1,1,1,1,1,1,1,1,1,1,1,1,1,1,1,1,1,
1,1,1,1,1,1,1,1,1,1,1,1,1,1,1,1,1,1,1,1,1,1,1,1,1,1,1,1,1,1,1,1,1,1,1,1,
1,1,1,1,1,1,1,1,1,1,1,1,1,1,1,1,1,1,1,1,1,1,1,6),(0.,0.005,0.01,0.015,0.02,
0.025,0.03,0.035,0.04,0.045,0.05,0.055,0.06,0.065,0.07,0.075,0.08,0.085,
0.09,0.095,0.1,0.105,0.11,0.115,0.12,0.125,0.13,0.135,0.14,0.145,0.15,0.155,
0.16,0.165,0.17,0.175,0.18,0.185,0.19,0.195,0.2,0.205,0.21,0.215,0.22,0.225,
0.23,0.235,0.24,0.245,0.25,0.255,0.26,0.265,0.27,0.275,0.28,0.285,0.29,
0.295,0.3,0.305,0.31,0.315,0.32,0.325,0.33,0.335,0.34,0.345,0.35,0.355,
0.36,0.365,0.37,0.375,0.38,0.385,0.39,0.395,0.4,0.405,0.41,0.415,0.42,0.425,
0.43,0.435,0.44,0.445,0.45,0.455,0.46,0.465,0.47,0.475,0.48,0.485,0.49,
0.495,0.5,0.505,0.51,0.515,0.52,0.525,0.53,0.535,0.54,0.545,0.55,0.555,
0.56,0.565,0.57,0.575,0.58,0.585,0.59,0.595,0.6,0.605,0.61,0.615,0.62,0.625,
0.63,0.635,0.64,0.645,0.65,0.655,0.66,0.665,0.67,0.675,0.68,0.685,0.690000000000001,
0.695000000000001,0.700000000000001,0.705000000000001,0.710000000000001,
0.715000000000001,0.720000000000001,0.725000000000001,0.730000000000001,
0.735000000000001,0.740000000000001,0.745000000000001,0.750000000000001,
0.755000000000001,0.760000000000001,0.765000000000001,0.770000000000001,
0.775000000000001,0.780000000000001,0.785000000000001,0.790000000000001,
0.795000000000001,0.800000000000001,0.805000000000001,0.810000000000001,
0.815000000000001,0.820000000000001,0.825000000000001,0.830000000000001,
0.835000000000001,0.840000000000001,0.845000000000001,0.850000000000001,
0.855000000000001,0.860000000000001,0.865000000000001,0.870000000000001,
0.875000000000001,0.880000000000001,0.885000000000001,0.890000000000001,
0.895000000000001,0.900000000000001,0.905000000000001,0.910000000000001,
0.915000000000001,0.920000000000001,0.925000000000001,0.930000000000001,
0.935000000000001,0.940000000000001,0.941429844438099),.UNSPECIFIED.)
CURVE()
GEOMETRIC_REPRESENTATION_ITEM()
RATIONAL_B_SPLINE_CURVE((1.,1.,1.,1.,1.,1.,1.,1.,1.,1.,1.,1.,1.,1.,1.,1.,
1.,1.,1.,1.,1.,1.,1.,1.,1.,1.,1.,1.,1.,1.,1.,1.,1.,1.,1.,1.,1.,1.,1.,1.,
1.,1.,1.,1.,1.,1.,1.,1.,1.,1.,1.,1.,1.,1.,1.,1.,1.,1.,1.,1.,1.,1.,1.,1.,
1.,1.,1.,1.,1.,1.,1.,1.,1.,1.,1.,1.,1.,1.,1.,1.,1.,1.,1.,1.,1.,1.,1.,1.,
1.,1.,1.,1.,1.,1.,1.,1.,1.,1.,1.,1.,1.,1.,1.,1.,1.,1.,1.,1.,1.,1.,1.,1.,
1.,1.,1.,1.,1.,1.,1.,1.,1.,1.,1.,1.,1.,1.,1.,1.,1.,1.,1.,1.,1.,1.,1.,1.,
1.,1.,1.,1.,1.,1.,1.,1.,1.,1.,1.,1.,1.,1.,1.,1.,1.,1.,1.,1.,1.,1.,1.,1.,
1.,1.,1.,1.,1.,1.,1.,1.,1.,1.,1.,1.,1.,1.,1.,1.,1.,1.,1.,1.,1.,1.,1.,1.,
1.,1.,1.,1.,1.,1.,1.,1.,1.,1.))
REPRESENTATION_ITEM('')
);
#592=(
BOUNDED_CURVE()
B_SPLINE_CURVE(5,(#135222,#135223,#135224,#135225,#135226,#135227,#135228,
#135229,#135230,#135231,#135232,#135233,#135234,#135235,#135236,#135237,
#135238,#135239,#135240,#135241,#135242,#135243,#135244,#135245,#135246,
#135247,#135248,#135249,#135250,#135251,#135252,#135253,#135254,#135255,
#135256,#135257,#135258,#135259,#135260,#135261,#135262,#135263,#135264,
#135265,#135266,#135267,#135268,#135269,#135270,#135271,#135272,#135273,
#135274,#135275,#135276,#135277,#135278,#135279,#135280,#135281,#135282,
#135283,#135284,#135285,#135286,#135287,#135288,#135289,#135290,#135291,
#135292,#135293,#135294,#135295,#135296,#135297,#135298,#135299,#135300,
#135301,#135302,#135303,#135304,#135305,#135306,#135307,#135308,#135309,
#135310,#135311,#135312,#135313,#135314,#135315,#135316,#135317,#135318,
#135319,#135320,#135321,#135322,#135323,#135324,#135325,#135326,#135327,
#135328,#135329,#135330,#135331,#135332,#135333,#135334,#135335,#135336,
#135337,#135338,#135339,#135340,#135341,#135342,#135343,#135344,#135345,
#135346,#135347,#135348,#135349,#135350,#135351,#135352,#135353,#135354,
#135355,#135356,#135357,#135358,#135359,#135360,#135361,#135362,#135363,
#135364,#135365,#135366,#135367,#135368,#135369,#135370,#135371,#135372,
#135373,#135374,#135375,#135376,#135377,#135378,#135379,#135380,#135381,
#135382,#135383,#135384,#135385,#135386,#135387,#135388,#135389,#135390,
#135391,#135392,#135393,#135394,#135395,#135396,#135397,#135398,#135399,
#135400,#135401,#135402,#135403,#135404,#135405,#135406,#135407,#135408,
#135409,#135410,#135411,#135412,#135413,#135414,#135415),.UNSPECIFIED.,
 .F.,.F.)
B_SPLINE_CURVE_WITH_KNOTS((6,1,1,1,1,1,1,1,1,1,1,1,1,1,1,1,1,1,1,1,1,1,
1,1,1,1,1,1,1,1,1,1,1,1,1,1,1,1,1,1,1,1,1,1,1,1,1,1,1,1,1,1,1,1,1,1,1,1,
1,1,1,1,1,1,1,1,1,1,1,1,1,1,1,1,1,1,1,1,1,1,1,1,1,1,1,1,1,1,1,1,1,1,1,1,
1,1,1,1,1,1,1,1,1,1,1,1,1,1,1,1,1,1,1,1,1,1,1,1,1,1,1,1,1,1,1,1,1,1,1,1,
1,1,1,1,1,1,1,1,1,1,1,1,1,1,1,1,1,1,1,1,1,1,1,1,1,1,1,1,1,1,1,1,1,1,1,1,
1,1,1,1,1,1,1,1,1,1,1,1,1,1,1,1,1,1,1,1,1,1,1,6),(-0.941429844438094,-0.940000000000001,
-0.935000000000001,-0.930000000000001,-0.925000000000001,-0.920000000000001,
-0.915000000000001,-0.910000000000001,-0.905000000000001,-0.900000000000001,
-0.895000000000001,-0.890000000000001,-0.885000000000001,-0.880000000000001,
-0.875000000000001,-0.870000000000001,-0.865000000000001,-0.860000000000001,
-0.855000000000001,-0.850000000000001,-0.845000000000001,-0.840000000000001,
-0.835000000000001,-0.830000000000001,-0.825000000000001,-0.820000000000001,
-0.815000000000001,-0.810000000000001,-0.805000000000001,-0.800000000000001,
-0.795000000000001,-0.790000000000001,-0.785000000000001,-0.780000000000001,
-0.775000000000001,-0.770000000000001,-0.765000000000001,-0.760000000000001,
-0.755000000000001,-0.750000000000001,-0.745000000000001,-0.740000000000001,
-0.735000000000001,-0.730000000000001,-0.725000000000001,-0.720000000000001,
-0.715000000000001,-0.710000000000001,-0.705000000000001,-0.700000000000001,
-0.695000000000001,-0.690000000000001,-0.685,-0.68,-0.675,-0.67,-0.665,
-0.66,-0.655,-0.65,-0.645,-0.64,-0.635,-0.63,-0.625,-0.62,-0.615,-0.61,
-0.605,-0.6,-0.595,-0.59,-0.585,-0.58,-0.575,-0.57,-0.565,-0.56,-0.555,
-0.55,-0.545,-0.54,-0.535,-0.53,-0.525,-0.52,-0.515,-0.51,-0.505,-0.5,-0.495,
-0.49,-0.485,-0.48,-0.475,-0.47,-0.465,-0.46,-0.455,-0.45,-0.445,-0.44,
-0.435,-0.43,-0.425,-0.42,-0.415,-0.41,-0.405,-0.4,-0.395,-0.39,-0.385,
-0.38,-0.375,-0.37,-0.365,-0.36,-0.355,-0.35,-0.345,-0.34,-0.335,-0.33,
-0.325,-0.32,-0.315,-0.31,-0.305,-0.3,-0.295,-0.29,-0.285,-0.28,-0.275,
-0.27,-0.265,-0.26,-0.255,-0.25,-0.245,-0.24,-0.235,-0.23,-0.225,-0.22,
-0.215,-0.21,-0.205,-0.2,-0.195,-0.19,-0.185,-0.18,-0.175,-0.17,-0.165,
-0.16,-0.155,-0.15,-0.145,-0.14,-0.135,-0.13,-0.125,-0.12,-0.115,-0.11,
-0.105,-0.1,-0.095,-0.09,-0.085,-0.08,-0.075,-0.07,-0.065,-0.06,-0.055,
-0.05,-0.045,-0.04,-0.035,-0.03,-0.025,-0.02,-0.015,-0.01,-0.005,0.),
 .UNSPECIFIED.)
CURVE()
GEOMETRIC_REPRESENTATION_ITEM()
RATIONAL_B_SPLINE_CURVE((1.,1.,1.,1.,1.,1.,1.,1.,1.,1.,1.,1.,1.,1.,1.,1.,
1.,1.,1.,1.,1.,1.,1.,1.,1.,1.,1.,1.,1.,1.,1.,1.,1.,1.,1.,1.,1.,1.,1.,1.,
1.,1.,1.,1.,1.,1.,1.,1.,1.,1.,1.,1.,1.,1.,1.,1.,1.,1.,1.,1.,1.,1.,1.,1.,
1.,1.,1.,1.,1.,1.,1.,1.,1.,1.,1.,1.,1.,1.,1.,1.,1.,1.,1.,1.,1.,1.,1.,1.,
1.,1.,1.,1.,1.,1.,1.,1.,1.,1.,1.,1.,1.,1.,1.,1.,1.,1.,1.,1.,1.,1.,1.,1.,
1.,1.,1.,1.,1.,1.,1.,1.,1.,1.,1.,1.,1.,1.,1.,1.,1.,1.,1.,1.,1.,1.,1.,1.,
1.,1.,1.,1.,1.,1.,1.,1.,1.,1.,1.,1.,1.,1.,1.,1.,1.,1.,1.,1.,1.,1.,1.,1.,
1.,1.,1.,1.,1.,1.,1.,1.,1.,1.,1.,1.,1.,1.,1.,1.,1.,1.,1.,1.,1.,1.,1.,1.,
1.,1.,1.,1.,1.,1.,1.,1.,1.,1.))
REPRESENTATION_ITEM('')
);
#593=(
BOUNDED_CURVE()
B_SPLINE_CURVE(5,(#135827,#135828,#135829,#135830,#135831,#135832,#135833,
#135834,#135835,#135836,#135837,#135838,#135839,#135840,#135841,#135842,
#135843,#135844,#135845,#135846,#135847,#135848,#135849,#135850,#135851,
#135852,#135853,#135854,#135855,#135856,#135857,#135858,#135859,#135860,
#135861,#135862,#135863,#135864,#135865,#135866,#135867,#135868,#135869,
#135870,#135871,#135872,#135873,#135874,#135875,#135876,#135877,#135878,
#135879,#135880,#135881,#135882,#135883,#135884,#135885,#135886,#135887,
#135888,#135889,#135890,#135891,#135892,#135893,#135894,#135895,#135896,
#135897,#135898,#135899,#135900,#135901,#135902,#135903,#135904,#135905,
#135906,#135907,#135908,#135909,#135910,#135911,#135912,#135913,#135914,
#135915,#135916,#135917,#135918,#135919,#135920,#135921,#135922,#135923,
#135924,#135925,#135926,#135927,#135928,#135929,#135930,#135931,#135932,
#135933,#135934,#135935,#135936,#135937,#135938,#135939,#135940,#135941,
#135942,#135943,#135944,#135945,#135946,#135947,#135948,#135949,#135950,
#135951,#135952,#135953,#135954,#135955,#135956,#135957,#135958,#135959,
#135960,#135961,#135962,#135963,#135964,#135965,#135966,#135967,#135968,
#135969,#135970,#135971,#135972,#135973,#135974,#135975,#135976,#135977,
#135978,#135979,#135980,#135981,#135982,#135983,#135984,#135985,#135986,
#135987,#135988,#135989,#135990,#135991,#135992,#135993,#135994,#135995,
#135996,#135997,#135998,#135999,#136000,#136001,#136002,#136003,#136004,
#136005,#136006,#136007,#136008,#136009,#136010,#136011,#136012,#136013,
#136014,#136015,#136016,#136017,#136018,#136019,#136020),.UNSPECIFIED.,
 .F.,.F.)
B_SPLINE_CURVE_WITH_KNOTS((6,1,1,1,1,1,1,1,1,1,1,1,1,1,1,1,1,1,1,1,1,1,
1,1,1,1,1,1,1,1,1,1,1,1,1,1,1,1,1,1,1,1,1,1,1,1,1,1,1,1,1,1,1,1,1,1,1,1,
1,1,1,1,1,1,1,1,1,1,1,1,1,1,1,1,1,1,1,1,1,1,1,1,1,1,1,1,1,1,1,1,1,1,1,1,
1,1,1,1,1,1,1,1,1,1,1,1,1,1,1,1,1,1,1,1,1,1,1,1,1,1,1,1,1,1,1,1,1,1,1,1,
1,1,1,1,1,1,1,1,1,1,1,1,1,1,1,1,1,1,1,1,1,1,1,1,1,1,1,1,1,1,1,1,1,1,1,1,
1,1,1,1,1,1,1,1,1,1,1,1,1,1,1,1,1,1,1,1,1,1,1,6),(0.,0.005,0.01,0.015,0.02,
0.025,0.03,0.035,0.04,0.045,0.05,0.055,0.06,0.065,0.07,0.075,0.08,0.085,
0.09,0.095,0.1,0.105,0.11,0.115,0.12,0.125,0.13,0.135,0.14,0.145,0.15,0.155,
0.16,0.165,0.17,0.175,0.18,0.185,0.19,0.195,0.2,0.205,0.21,0.215,0.22,0.225,
0.23,0.235,0.24,0.245,0.25,0.255,0.26,0.265,0.27,0.275,0.28,0.285,0.29,
0.295,0.3,0.305,0.31,0.315,0.32,0.325,0.33,0.335,0.34,0.345,0.35,0.355,
0.36,0.365,0.37,0.375,0.38,0.385,0.39,0.395,0.4,0.405,0.41,0.415,0.42,0.425,
0.43,0.435,0.44,0.445,0.45,0.455,0.46,0.465,0.47,0.475,0.48,0.485,0.49,
0.495,0.5,0.505,0.51,0.515,0.52,0.525,0.53,0.535,0.54,0.545,0.55,0.555,
0.56,0.565,0.57,0.575,0.58,0.585,0.59,0.595,0.6,0.605,0.61,0.615,0.62,0.625,
0.63,0.635,0.64,0.645,0.65,0.655,0.66,0.665,0.67,0.675,0.68,0.685,0.690000000000001,
0.695000000000001,0.700000000000001,0.705000000000001,0.710000000000001,
0.715000000000001,0.720000000000001,0.725000000000001,0.730000000000001,
0.735000000000001,0.740000000000001,0.745000000000001,0.750000000000001,
0.755000000000001,0.760000000000001,0.765000000000001,0.770000000000001,
0.775000000000001,0.780000000000001,0.785000000000001,0.790000000000001,
0.795000000000001,0.800000000000001,0.805000000000001,0.810000000000001,
0.815000000000001,0.820000000000001,0.825000000000001,0.830000000000001,
0.835000000000001,0.840000000000001,0.845000000000001,0.850000000000001,
0.855000000000001,0.860000000000001,0.865000000000001,0.870000000000001,
0.875000000000001,0.880000000000001,0.885000000000001,0.890000000000001,
0.895000000000001,0.900000000000001,0.905000000000001,0.910000000000001,
0.915000000000001,0.920000000000001,0.925000000000001,0.930000000000001,
0.935000000000001,0.940000000000001,0.941429844438126),.UNSPECIFIED.)
CURVE()
GEOMETRIC_REPRESENTATION_ITEM()
RATIONAL_B_SPLINE_CURVE((1.,1.,1.,1.,1.,1.,1.,1.,1.,1.,1.,1.,1.,1.,1.,1.,
1.,1.,1.,1.,1.,1.,1.,1.,1.,1.,1.,1.,1.,1.,1.,1.,1.,1.,1.,1.,1.,1.,1.,1.,
1.,1.,1.,1.,1.,1.,1.,1.,1.,1.,1.,1.,1.,1.,1.,1.,1.,1.,1.,1.,1.,1.,1.,1.,
1.,1.,1.,1.,1.,1.,1.,1.,1.,1.,1.,1.,1.,1.,1.,1.,1.,1.,1.,1.,1.,1.,1.,1.,
1.,1.,1.,1.,1.,1.,1.,1.,1.,1.,1.,1.,1.,1.,1.,1.,1.,1.,1.,1.,1.,1.,1.,1.,
1.,1.,1.,1.,1.,1.,1.,1.,1.,1.,1.,1.,1.,1.,1.,1.,1.,1.,1.,1.,1.,1.,1.,1.,
1.,1.,1.,1.,1.,1.,1.,1.,1.,1.,1.,1.,1.,1.,1.,1.,1.,1.,1.,1.,1.,1.,1.,1.,
1.,1.,1.,1.,1.,1.,1.,1.,1.,1.,1.,1.,1.,1.,1.,1.,1.,1.,1.,1.,1.,1.,1.,1.,
1.,1.,1.,1.,1.,1.,1.,1.,1.,1.))
REPRESENTATION_ITEM('')
);
#594=(
BOUNDED_CURVE()
B_SPLINE_CURVE(5,(#136023,#136024,#136025,#136026,#136027,#136028,#136029,
#136030,#136031,#136032,#136033,#136034,#136035,#136036,#136037,#136038,
#136039,#136040,#136041,#136042,#136043,#136044,#136045,#136046,#136047,
#136048,#136049,#136050,#136051,#136052,#136053,#136054,#136055,#136056,
#136057,#136058,#136059,#136060,#136061,#136062,#136063,#136064,#136065,
#136066,#136067,#136068,#136069,#136070,#136071,#136072,#136073,#136074,
#136075,#136076,#136077,#136078,#136079,#136080,#136081,#136082,#136083,
#136084,#136085,#136086,#136087,#136088,#136089,#136090,#136091,#136092,
#136093,#136094,#136095,#136096,#136097,#136098,#136099,#136100,#136101,
#136102,#136103,#136104,#136105,#136106,#136107,#136108,#136109,#136110,
#136111,#136112,#136113,#136114,#136115,#136116,#136117,#136118,#136119,
#136120,#136121,#136122,#136123,#136124,#136125,#136126,#136127,#136128,
#136129,#136130,#136131,#136132,#136133,#136134,#136135,#136136,#136137,
#136138,#136139,#136140,#136141,#136142,#136143,#136144,#136145,#136146,
#136147,#136148,#136149,#136150,#136151,#136152,#136153,#136154,#136155,
#136156,#136157,#136158,#136159,#136160,#136161,#136162,#136163,#136164,
#136165,#136166,#136167,#136168,#136169,#136170,#136171,#136172,#136173,
#136174,#136175,#136176,#136177,#136178,#136179,#136180,#136181,#136182,
#136183,#136184,#136185,#136186,#136187,#136188,#136189,#136190,#136191,
#136192,#136193,#136194,#136195,#136196,#136197,#136198,#136199,#136200,
#136201,#136202,#136203,#136204,#136205,#136206,#136207,#136208,#136209,
#136210,#136211,#136212,#136213,#136214,#136215,#136216),.UNSPECIFIED.,
 .F.,.F.)
B_SPLINE_CURVE_WITH_KNOTS((6,1,1,1,1,1,1,1,1,1,1,1,1,1,1,1,1,1,1,1,1,1,
1,1,1,1,1,1,1,1,1,1,1,1,1,1,1,1,1,1,1,1,1,1,1,1,1,1,1,1,1,1,1,1,1,1,1,1,
1,1,1,1,1,1,1,1,1,1,1,1,1,1,1,1,1,1,1,1,1,1,1,1,1,1,1,1,1,1,1,1,1,1,1,1,
1,1,1,1,1,1,1,1,1,1,1,1,1,1,1,1,1,1,1,1,1,1,1,1,1,1,1,1,1,1,1,1,1,1,1,1,
1,1,1,1,1,1,1,1,1,1,1,1,1,1,1,1,1,1,1,1,1,1,1,1,1,1,1,1,1,1,1,1,1,1,1,1,
1,1,1,1,1,1,1,1,1,1,1,1,1,1,1,1,1,1,1,1,1,1,1,6),(-0.9414298444381,-0.940000000000001,
-0.935000000000001,-0.930000000000001,-0.925000000000001,-0.920000000000001,
-0.915000000000001,-0.910000000000001,-0.905000000000001,-0.900000000000001,
-0.895000000000001,-0.890000000000001,-0.885000000000001,-0.880000000000001,
-0.875000000000001,-0.870000000000001,-0.865000000000001,-0.860000000000001,
-0.855000000000001,-0.850000000000001,-0.845000000000001,-0.840000000000001,
-0.835000000000001,-0.830000000000001,-0.825000000000001,-0.820000000000001,
-0.815000000000001,-0.810000000000001,-0.805000000000001,-0.800000000000001,
-0.795000000000001,-0.790000000000001,-0.785000000000001,-0.780000000000001,
-0.775000000000001,-0.770000000000001,-0.765000000000001,-0.760000000000001,
-0.755000000000001,-0.750000000000001,-0.745000000000001,-0.740000000000001,
-0.735000000000001,-0.730000000000001,-0.725000000000001,-0.720000000000001,
-0.715000000000001,-0.710000000000001,-0.705000000000001,-0.700000000000001,
-0.695000000000001,-0.690000000000001,-0.685,-0.68,-0.675,-0.67,-0.665,
-0.66,-0.655,-0.65,-0.645,-0.64,-0.635,-0.63,-0.625,-0.62,-0.615,-0.61,
-0.605,-0.6,-0.595,-0.59,-0.585,-0.58,-0.575,-0.57,-0.565,-0.56,-0.555,
-0.55,-0.545,-0.54,-0.535,-0.53,-0.525,-0.52,-0.515,-0.51,-0.505,-0.5,-0.495,
-0.49,-0.485,-0.48,-0.475,-0.47,-0.465,-0.46,-0.455,-0.45,-0.445,-0.44,
-0.435,-0.43,-0.425,-0.42,-0.415,-0.41,-0.405,-0.4,-0.395,-0.39,-0.385,
-0.38,-0.375,-0.37,-0.365,-0.36,-0.355,-0.35,-0.345,-0.34,-0.335,-0.33,
-0.325,-0.32,-0.315,-0.31,-0.305,-0.3,-0.295,-0.29,-0.285,-0.28,-0.275,
-0.27,-0.265,-0.26,-0.255,-0.25,-0.245,-0.24,-0.235,-0.23,-0.225,-0.22,
-0.215,-0.21,-0.205,-0.2,-0.195,-0.19,-0.185,-0.18,-0.175,-0.17,-0.165,
-0.16,-0.155,-0.15,-0.145,-0.14,-0.135,-0.13,-0.125,-0.12,-0.115,-0.11,
-0.105,-0.1,-0.095,-0.09,-0.085,-0.08,-0.075,-0.07,-0.065,-0.06,-0.055,
-0.05,-0.045,-0.04,-0.035,-0.03,-0.025,-0.02,-0.015,-0.01,-0.005,0.),
 .UNSPECIFIED.)
CURVE()
GEOMETRIC_REPRESENTATION_ITEM()
RATIONAL_B_SPLINE_CURVE((1.,1.,1.,1.,1.,1.,1.,1.,1.,1.,1.,1.,1.,1.,1.,1.,
1.,1.,1.,1.,1.,1.,1.,1.,1.,1.,1.,1.,1.,1.,1.,1.,1.,1.,1.,1.,1.,1.,1.,1.,
1.,1.,1.,1.,1.,1.,1.,1.,1.,1.,1.,1.,1.,1.,1.,1.,1.,1.,1.,1.,1.,1.,1.,1.,
1.,1.,1.,1.,1.,1.,1.,1.,1.,1.,1.,1.,1.,1.,1.,1.,1.,1.,1.,1.,1.,1.,1.,1.,
1.,1.,1.,1.,1.,1.,1.,1.,1.,1.,1.,1.,1.,1.,1.,1.,1.,1.,1.,1.,1.,1.,1.,1.,
1.,1.,1.,1.,1.,1.,1.,1.,1.,1.,1.,1.,1.,1.,1.,1.,1.,1.,1.,1.,1.,1.,1.,1.,
1.,1.,1.,1.,1.,1.,1.,1.,1.,1.,1.,1.,1.,1.,1.,1.,1.,1.,1.,1.,1.,1.,1.,1.,
1.,1.,1.,1.,1.,1.,1.,1.,1.,1.,1.,1.,1.,1.,1.,1.,1.,1.,1.,1.,1.,1.,1.,1.,
1.,1.,1.,1.,1.,1.,1.,1.,1.,1.))
REPRESENTATION_ITEM('')
);
#595=(
BOUNDED_CURVE()
B_SPLINE_CURVE(5,(#136628,#136629,#136630,#136631,#136632,#136633,#136634,
#136635,#136636,#136637,#136638,#136639,#136640,#136641,#136642,#136643,
#136644,#136645,#136646,#136647,#136648,#136649,#136650,#136651,#136652,
#136653,#136654,#136655,#136656,#136657,#136658,#136659,#136660,#136661,
#136662,#136663,#136664,#136665,#136666,#136667,#136668,#136669,#136670,
#136671,#136672,#136673,#136674,#136675,#136676,#136677,#136678,#136679,
#136680,#136681,#136682,#136683,#136684,#136685,#136686,#136687,#136688,
#136689,#136690,#136691,#136692,#136693,#136694,#136695,#136696,#136697,
#136698,#136699,#136700,#136701,#136702,#136703,#136704,#136705,#136706,
#136707,#136708,#136709,#136710,#136711,#136712,#136713,#136714,#136715,
#136716,#136717,#136718,#136719,#136720,#136721,#136722,#136723,#136724,
#136725,#136726,#136727,#136728,#136729,#136730,#136731,#136732,#136733,
#136734,#136735,#136736,#136737,#136738,#136739,#136740,#136741,#136742,
#136743,#136744,#136745,#136746,#136747,#136748,#136749,#136750,#136751,
#136752,#136753,#136754,#136755,#136756,#136757,#136758,#136759,#136760,
#136761,#136762,#136763,#136764,#136765,#136766,#136767,#136768,#136769,
#136770,#136771,#136772,#136773,#136774,#136775,#136776,#136777,#136778,
#136779,#136780,#136781,#136782,#136783,#136784,#136785,#136786,#136787,
#136788,#136789,#136790,#136791,#136792,#136793,#136794,#136795,#136796,
#136797,#136798,#136799,#136800,#136801,#136802,#136803,#136804,#136805,
#136806,#136807,#136808,#136809,#136810,#136811,#136812,#136813,#136814,
#136815,#136816,#136817,#136818,#136819,#136820,#136821),.UNSPECIFIED.,
 .F.,.F.)
B_SPLINE_CURVE_WITH_KNOTS((6,1,1,1,1,1,1,1,1,1,1,1,1,1,1,1,1,1,1,1,1,1,
1,1,1,1,1,1,1,1,1,1,1,1,1,1,1,1,1,1,1,1,1,1,1,1,1,1,1,1,1,1,1,1,1,1,1,1,
1,1,1,1,1,1,1,1,1,1,1,1,1,1,1,1,1,1,1,1,1,1,1,1,1,1,1,1,1,1,1,1,1,1,1,1,
1,1,1,1,1,1,1,1,1,1,1,1,1,1,1,1,1,1,1,1,1,1,1,1,1,1,1,1,1,1,1,1,1,1,1,1,
1,1,1,1,1,1,1,1,1,1,1,1,1,1,1,1,1,1,1,1,1,1,1,1,1,1,1,1,1,1,1,1,1,1,1,1,
1,1,1,1,1,1,1,1,1,1,1,1,1,1,1,1,1,1,1,1,1,1,1,6),(0.,0.005,0.01,0.015,0.02,
0.025,0.03,0.035,0.04,0.045,0.05,0.055,0.06,0.065,0.07,0.075,0.08,0.085,
0.09,0.095,0.1,0.105,0.11,0.115,0.12,0.125,0.13,0.135,0.14,0.145,0.15,0.155,
0.16,0.165,0.17,0.175,0.18,0.185,0.19,0.195,0.2,0.205,0.21,0.215,0.22,0.225,
0.23,0.235,0.24,0.245,0.25,0.255,0.26,0.265,0.27,0.275,0.28,0.285,0.29,
0.295,0.3,0.305,0.31,0.315,0.32,0.325,0.33,0.335,0.34,0.345,0.35,0.355,
0.36,0.365,0.37,0.375,0.38,0.385,0.39,0.395,0.4,0.405,0.41,0.415,0.42,0.425,
0.43,0.435,0.44,0.445,0.45,0.455,0.46,0.465,0.47,0.475,0.48,0.485,0.49,
0.495,0.5,0.505,0.51,0.515,0.52,0.525,0.53,0.535,0.54,0.545,0.55,0.555,
0.56,0.565,0.57,0.575,0.58,0.585,0.59,0.595,0.6,0.605,0.61,0.615,0.62,0.625,
0.63,0.635,0.64,0.645,0.65,0.655,0.66,0.665,0.67,0.675,0.68,0.685,0.690000000000001,
0.695000000000001,0.700000000000001,0.705000000000001,0.710000000000001,
0.715000000000001,0.720000000000001,0.725000000000001,0.730000000000001,
0.735000000000001,0.740000000000001,0.745000000000001,0.750000000000001,
0.755000000000001,0.760000000000001,0.765000000000001,0.770000000000001,
0.775000000000001,0.780000000000001,0.785000000000001,0.790000000000001,
0.795000000000001,0.800000000000001,0.805000000000001,0.810000000000001,
0.815000000000001,0.820000000000001,0.825000000000001,0.830000000000001,
0.835000000000001,0.840000000000001,0.845000000000001,0.850000000000001,
0.855000000000001,0.860000000000001,0.865000000000001,0.870000000000001,
0.875000000000001,0.880000000000001,0.885000000000001,0.890000000000001,
0.895000000000001,0.900000000000001,0.905000000000001,0.910000000000001,
0.915000000000001,0.920000000000001,0.925000000000001,0.930000000000001,
0.935000000000001,0.940000000000001,0.94142984443805),.UNSPECIFIED.)
CURVE()
GEOMETRIC_REPRESENTATION_ITEM()
RATIONAL_B_SPLINE_CURVE((1.,1.,1.,1.,1.,1.,1.,1.,1.,1.,1.,1.,1.,1.,1.,1.,
1.,1.,1.,1.,1.,1.,1.,1.,1.,1.,1.,1.,1.,1.,1.,1.,1.,1.,1.,1.,1.,1.,1.,1.,
1.,1.,1.,1.,1.,1.,1.,1.,1.,1.,1.,1.,1.,1.,1.,1.,1.,1.,1.,1.,1.,1.,1.,1.,
1.,1.,1.,1.,1.,1.,1.,1.,1.,1.,1.,1.,1.,1.,1.,1.,1.,1.,1.,1.,1.,1.,1.,1.,
1.,1.,1.,1.,1.,1.,1.,1.,1.,1.,1.,1.,1.,1.,1.,1.,1.,1.,1.,1.,1.,1.,1.,1.,
1.,1.,1.,1.,1.,1.,1.,1.,1.,1.,1.,1.,1.,1.,1.,1.,1.,1.,1.,1.,1.,1.,1.,1.,
1.,1.,1.,1.,1.,1.,1.,1.,1.,1.,1.,1.,1.,1.,1.,1.,1.,1.,1.,1.,1.,1.,1.,1.,
1.,1.,1.,1.,1.,1.,1.,1.,1.,1.,1.,1.,1.,1.,1.,1.,1.,1.,1.,1.,1.,1.,1.,1.,
1.,1.,1.,1.,1.,1.,1.,1.,1.,1.))
REPRESENTATION_ITEM('')
);
#596=(
BOUNDED_CURVE()
B_SPLINE_CURVE(5,(#136824,#136825,#136826,#136827,#136828,#136829,#136830,
#136831,#136832,#136833,#136834,#136835,#136836,#136837,#136838,#136839,
#136840,#136841,#136842,#136843,#136844,#136845,#136846,#136847,#136848,
#136849,#136850,#136851,#136852,#136853,#136854,#136855,#136856,#136857,
#136858,#136859,#136860,#136861,#136862,#136863,#136864,#136865,#136866,
#136867,#136868,#136869,#136870,#136871,#136872,#136873,#136874,#136875,
#136876,#136877,#136878,#136879,#136880,#136881,#136882,#136883,#136884,
#136885,#136886,#136887,#136888,#136889,#136890,#136891,#136892,#136893,
#136894,#136895,#136896,#136897,#136898,#136899,#136900,#136901,#136902,
#136903,#136904,#136905,#136906,#136907,#136908,#136909,#136910,#136911,
#136912,#136913,#136914,#136915,#136916,#136917,#136918,#136919,#136920,
#136921,#136922,#136923,#136924,#136925,#136926,#136927,#136928,#136929,
#136930,#136931,#136932,#136933,#136934,#136935,#136936,#136937,#136938,
#136939,#136940,#136941,#136942,#136943,#136944,#136945,#136946,#136947,
#136948,#136949,#136950,#136951,#136952,#136953,#136954,#136955,#136956,
#136957,#136958,#136959,#136960,#136961,#136962,#136963,#136964,#136965,
#136966,#136967,#136968,#136969,#136970,#136971,#136972,#136973,#136974,
#136975,#136976,#136977,#136978,#136979,#136980,#136981,#136982,#136983,
#136984,#136985,#136986,#136987,#136988,#136989,#136990,#136991,#136992,
#136993,#136994,#136995,#136996,#136997,#136998,#136999,#137000,#137001,
#137002,#137003,#137004,#137005,#137006,#137007,#137008,#137009,#137010,
#137011,#137012,#137013,#137014,#137015,#137016,#137017),.UNSPECIFIED.,
 .F.,.F.)
B_SPLINE_CURVE_WITH_KNOTS((6,1,1,1,1,1,1,1,1,1,1,1,1,1,1,1,1,1,1,1,1,1,
1,1,1,1,1,1,1,1,1,1,1,1,1,1,1,1,1,1,1,1,1,1,1,1,1,1,1,1,1,1,1,1,1,1,1,1,
1,1,1,1,1,1,1,1,1,1,1,1,1,1,1,1,1,1,1,1,1,1,1,1,1,1,1,1,1,1,1,1,1,1,1,1,
1,1,1,1,1,1,1,1,1,1,1,1,1,1,1,1,1,1,1,1,1,1,1,1,1,1,1,1,1,1,1,1,1,1,1,1,
1,1,1,1,1,1,1,1,1,1,1,1,1,1,1,1,1,1,1,1,1,1,1,1,1,1,1,1,1,1,1,1,1,1,1,1,
1,1,1,1,1,1,1,1,1,1,1,1,1,1,1,1,1,1,1,1,1,1,1,6),(-0.941429844438045,-0.940000000000001,
-0.935000000000001,-0.930000000000001,-0.925000000000001,-0.920000000000001,
-0.915000000000001,-0.910000000000001,-0.905000000000001,-0.900000000000001,
-0.895000000000001,-0.890000000000001,-0.885000000000001,-0.880000000000001,
-0.875000000000001,-0.870000000000001,-0.865000000000001,-0.860000000000001,
-0.855000000000001,-0.850000000000001,-0.845000000000001,-0.840000000000001,
-0.835000000000001,-0.830000000000001,-0.825000000000001,-0.820000000000001,
-0.815000000000001,-0.810000000000001,-0.805000000000001,-0.800000000000001,
-0.795000000000001,-0.790000000000001,-0.785000000000001,-0.780000000000001,
-0.775000000000001,-0.770000000000001,-0.765000000000001,-0.760000000000001,
-0.755000000000001,-0.750000000000001,-0.745000000000001,-0.740000000000001,
-0.735000000000001,-0.730000000000001,-0.725000000000001,-0.720000000000001,
-0.715000000000001,-0.710000000000001,-0.705000000000001,-0.700000000000001,
-0.695000000000001,-0.690000000000001,-0.685,-0.68,-0.675,-0.67,-0.665,
-0.66,-0.655,-0.65,-0.645,-0.64,-0.635,-0.63,-0.625,-0.62,-0.615,-0.61,
-0.605,-0.6,-0.595,-0.59,-0.585,-0.58,-0.575,-0.57,-0.565,-0.56,-0.555,
-0.55,-0.545,-0.54,-0.535,-0.53,-0.525,-0.52,-0.515,-0.51,-0.505,-0.5,-0.495,
-0.49,-0.485,-0.48,-0.475,-0.47,-0.465,-0.46,-0.455,-0.45,-0.445,-0.44,
-0.435,-0.43,-0.425,-0.42,-0.415,-0.41,-0.405,-0.4,-0.395,-0.39,-0.385,
-0.38,-0.375,-0.37,-0.365,-0.36,-0.355,-0.35,-0.345,-0.34,-0.335,-0.33,
-0.325,-0.32,-0.315,-0.31,-0.305,-0.3,-0.295,-0.29,-0.285,-0.28,-0.275,
-0.27,-0.265,-0.26,-0.255,-0.25,-0.245,-0.24,-0.235,-0.23,-0.225,-0.22,
-0.215,-0.21,-0.205,-0.2,-0.195,-0.19,-0.185,-0.18,-0.175,-0.17,-0.165,
-0.16,-0.155,-0.15,-0.145,-0.14,-0.135,-0.13,-0.125,-0.12,-0.115,-0.11,
-0.105,-0.1,-0.095,-0.09,-0.085,-0.08,-0.075,-0.07,-0.065,-0.06,-0.055,
-0.05,-0.045,-0.04,-0.035,-0.03,-0.025,-0.02,-0.015,-0.01,-0.005,0.),
 .UNSPECIFIED.)
CURVE()
GEOMETRIC_REPRESENTATION_ITEM()
RATIONAL_B_SPLINE_CURVE((1.,1.,1.,1.,1.,1.,1.,1.,1.,1.,1.,1.,1.,1.,1.,1.,
1.,1.,1.,1.,1.,1.,1.,1.,1.,1.,1.,1.,1.,1.,1.,1.,1.,1.,1.,1.,1.,1.,1.,1.,
1.,1.,1.,1.,1.,1.,1.,1.,1.,1.,1.,1.,1.,1.,1.,1.,1.,1.,1.,1.,1.,1.,1.,1.,
1.,1.,1.,1.,1.,1.,1.,1.,1.,1.,1.,1.,1.,1.,1.,1.,1.,1.,1.,1.,1.,1.,1.,1.,
1.,1.,1.,1.,1.,1.,1.,1.,1.,1.,1.,1.,1.,1.,1.,1.,1.,1.,1.,1.,1.,1.,1.,1.,
1.,1.,1.,1.,1.,1.,1.,1.,1.,1.,1.,1.,1.,1.,1.,1.,1.,1.,1.,1.,1.,1.,1.,1.,
1.,1.,1.,1.,1.,1.,1.,1.,1.,1.,1.,1.,1.,1.,1.,1.,1.,1.,1.,1.,1.,1.,1.,1.,
1.,1.,1.,1.,1.,1.,1.,1.,1.,1.,1.,1.,1.,1.,1.,1.,1.,1.,1.,1.,1.,1.,1.,1.,
1.,1.,1.,1.,1.,1.,1.,1.,1.,1.))
REPRESENTATION_ITEM('')
);
#597=(
BOUNDED_CURVE()
B_SPLINE_CURVE(5,(#137429,#137430,#137431,#137432,#137433,#137434,#137435,
#137436,#137437,#137438,#137439,#137440,#137441,#137442,#137443,#137444,
#137445,#137446,#137447,#137448,#137449,#137450,#137451,#137452,#137453,
#137454,#137455,#137456,#137457,#137458,#137459,#137460,#137461,#137462,
#137463,#137464,#137465,#137466,#137467,#137468,#137469,#137470,#137471,
#137472,#137473,#137474,#137475,#137476,#137477,#137478,#137479,#137480,
#137481,#137482,#137483,#137484,#137485,#137486,#137487,#137488,#137489,
#137490,#137491,#137492,#137493,#137494,#137495,#137496,#137497,#137498,
#137499,#137500,#137501,#137502,#137503,#137504,#137505,#137506,#137507,
#137508,#137509,#137510,#137511,#137512,#137513,#137514,#137515,#137516,
#137517,#137518,#137519,#137520,#137521,#137522,#137523,#137524,#137525,
#137526,#137527,#137528,#137529,#137530,#137531,#137532,#137533,#137534,
#137535,#137536,#137537,#137538,#137539,#137540,#137541,#137542,#137543,
#137544,#137545,#137546,#137547,#137548,#137549,#137550,#137551,#137552,
#137553,#137554,#137555,#137556,#137557,#137558,#137559,#137560,#137561,
#137562,#137563,#137564,#137565,#137566,#137567,#137568,#137569,#137570,
#137571,#137572,#137573,#137574,#137575,#137576,#137577,#137578,#137579,
#137580,#137581,#137582,#137583,#137584,#137585,#137586,#137587,#137588,
#137589,#137590,#137591,#137592,#137593,#137594,#137595,#137596,#137597,
#137598,#137599,#137600,#137601,#137602,#137603,#137604,#137605,#137606,
#137607,#137608,#137609,#137610,#137611,#137612,#137613,#137614,#137615,
#137616,#137617,#137618,#137619,#137620,#137621,#137622),.UNSPECIFIED.,
 .F.,.F.)
B_SPLINE_CURVE_WITH_KNOTS((6,1,1,1,1,1,1,1,1,1,1,1,1,1,1,1,1,1,1,1,1,1,
1,1,1,1,1,1,1,1,1,1,1,1,1,1,1,1,1,1,1,1,1,1,1,1,1,1,1,1,1,1,1,1,1,1,1,1,
1,1,1,1,1,1,1,1,1,1,1,1,1,1,1,1,1,1,1,1,1,1,1,1,1,1,1,1,1,1,1,1,1,1,1,1,
1,1,1,1,1,1,1,1,1,1,1,1,1,1,1,1,1,1,1,1,1,1,1,1,1,1,1,1,1,1,1,1,1,1,1,1,
1,1,1,1,1,1,1,1,1,1,1,1,1,1,1,1,1,1,1,1,1,1,1,1,1,1,1,1,1,1,1,1,1,1,1,1,
1,1,1,1,1,1,1,1,1,1,1,1,1,1,1,1,1,1,1,1,1,1,1,6),(0.,0.005,0.01,0.015,0.02,
0.025,0.03,0.035,0.04,0.045,0.05,0.055,0.06,0.065,0.07,0.075,0.08,0.085,
0.09,0.095,0.1,0.105,0.11,0.115,0.12,0.125,0.13,0.135,0.14,0.145,0.15,0.155,
0.16,0.165,0.17,0.175,0.18,0.185,0.19,0.195,0.2,0.205,0.21,0.215,0.22,0.225,
0.23,0.235,0.24,0.245,0.25,0.255,0.26,0.265,0.27,0.275,0.28,0.285,0.29,
0.295,0.3,0.305,0.31,0.315,0.32,0.325,0.33,0.335,0.34,0.345,0.35,0.355,
0.36,0.365,0.37,0.375,0.38,0.385,0.39,0.395,0.4,0.405,0.41,0.415,0.42,0.425,
0.43,0.435,0.44,0.445,0.45,0.455,0.46,0.465,0.47,0.475,0.48,0.485,0.49,
0.495,0.5,0.505,0.51,0.515,0.52,0.525,0.53,0.535,0.54,0.545,0.55,0.555,
0.56,0.565,0.57,0.575,0.58,0.585,0.59,0.595,0.6,0.605,0.61,0.615,0.62,0.625,
0.63,0.635,0.64,0.645,0.65,0.655,0.66,0.665,0.67,0.675,0.68,0.685,0.690000000000001,
0.695000000000001,0.700000000000001,0.705000000000001,0.710000000000001,
0.715000000000001,0.720000000000001,0.725000000000001,0.730000000000001,
0.735000000000001,0.740000000000001,0.745000000000001,0.750000000000001,
0.755000000000001,0.760000000000001,0.765000000000001,0.770000000000001,
0.775000000000001,0.780000000000001,0.785000000000001,0.790000000000001,
0.795000000000001,0.800000000000001,0.805000000000001,0.810000000000001,
0.815000000000001,0.820000000000001,0.825000000000001,0.830000000000001,
0.835000000000001,0.840000000000001,0.845000000000001,0.850000000000001,
0.855000000000001,0.860000000000001,0.865000000000001,0.870000000000001,
0.875000000000001,0.880000000000001,0.885000000000001,0.890000000000001,
0.895000000000001,0.900000000000001,0.905000000000001,0.910000000000001,
0.915000000000001,0.920000000000001,0.925000000000001,0.930000000000001,
0.935000000000001,0.940000000000001,0.941429844437968),.UNSPECIFIED.)
CURVE()
GEOMETRIC_REPRESENTATION_ITEM()
RATIONAL_B_SPLINE_CURVE((1.,1.,1.,1.,1.,1.,1.,1.,1.,1.,1.,1.,1.,1.,1.,1.,
1.,1.,1.,1.,1.,1.,1.,1.,1.,1.,1.,1.,1.,1.,1.,1.,1.,1.,1.,1.,1.,1.,1.,1.,
1.,1.,1.,1.,1.,1.,1.,1.,1.,1.,1.,1.,1.,1.,1.,1.,1.,1.,1.,1.,1.,1.,1.,1.,
1.,1.,1.,1.,1.,1.,1.,1.,1.,1.,1.,1.,1.,1.,1.,1.,1.,1.,1.,1.,1.,1.,1.,1.,
1.,1.,1.,1.,1.,1.,1.,1.,1.,1.,1.,1.,1.,1.,1.,1.,1.,1.,1.,1.,1.,1.,1.,1.,
1.,1.,1.,1.,1.,1.,1.,1.,1.,1.,1.,1.,1.,1.,1.,1.,1.,1.,1.,1.,1.,1.,1.,1.,
1.,1.,1.,1.,1.,1.,1.,1.,1.,1.,1.,1.,1.,1.,1.,1.,1.,1.,1.,1.,1.,1.,1.,1.,
1.,1.,1.,1.,1.,1.,1.,1.,1.,1.,1.,1.,1.,1.,1.,1.,1.,1.,1.,1.,1.,1.,1.,1.,
1.,1.,1.,1.,1.,1.,1.,1.,1.,1.))
REPRESENTATION_ITEM('')
);
#598=(
BOUNDED_CURVE()
B_SPLINE_CURVE(5,(#137625,#137626,#137627,#137628,#137629,#137630,#137631,
#137632,#137633,#137634,#137635,#137636,#137637,#137638,#137639,#137640,
#137641,#137642,#137643,#137644,#137645,#137646,#137647,#137648,#137649,
#137650,#137651,#137652,#137653,#137654,#137655,#137656,#137657,#137658,
#137659,#137660,#137661,#137662,#137663,#137664,#137665,#137666,#137667,
#137668,#137669,#137670,#137671,#137672,#137673,#137674,#137675,#137676,
#137677,#137678,#137679,#137680,#137681,#137682,#137683,#137684,#137685,
#137686,#137687,#137688,#137689,#137690,#137691,#137692,#137693,#137694,
#137695,#137696,#137697,#137698,#137699,#137700,#137701,#137702,#137703,
#137704,#137705,#137706,#137707,#137708,#137709,#137710,#137711,#137712,
#137713,#137714,#137715,#137716,#137717,#137718,#137719,#137720,#137721,
#137722,#137723,#137724,#137725,#137726,#137727,#137728,#137729,#137730,
#137731,#137732,#137733,#137734,#137735,#137736,#137737,#137738,#137739,
#137740,#137741,#137742,#137743,#137744,#137745,#137746,#137747,#137748,
#137749,#137750,#137751,#137752,#137753,#137754,#137755,#137756,#137757,
#137758,#137759,#137760,#137761,#137762,#137763,#137764,#137765,#137766,
#137767,#137768,#137769,#137770,#137771,#137772,#137773,#137774,#137775,
#137776,#137777,#137778,#137779,#137780,#137781,#137782,#137783,#137784,
#137785,#137786,#137787,#137788,#137789,#137790,#137791,#137792,#137793,
#137794,#137795,#137796,#137797,#137798,#137799,#137800,#137801,#137802,
#137803,#137804,#137805,#137806,#137807,#137808,#137809,#137810,#137811,
#137812,#137813,#137814,#137815,#137816,#137817,#137818),.UNSPECIFIED.,
 .F.,.F.)
B_SPLINE_CURVE_WITH_KNOTS((6,1,1,1,1,1,1,1,1,1,1,1,1,1,1,1,1,1,1,1,1,1,
1,1,1,1,1,1,1,1,1,1,1,1,1,1,1,1,1,1,1,1,1,1,1,1,1,1,1,1,1,1,1,1,1,1,1,1,
1,1,1,1,1,1,1,1,1,1,1,1,1,1,1,1,1,1,1,1,1,1,1,1,1,1,1,1,1,1,1,1,1,1,1,1,
1,1,1,1,1,1,1,1,1,1,1,1,1,1,1,1,1,1,1,1,1,1,1,1,1,1,1,1,1,1,1,1,1,1,1,1,
1,1,1,1,1,1,1,1,1,1,1,1,1,1,1,1,1,1,1,1,1,1,1,1,1,1,1,1,1,1,1,1,1,1,1,1,
1,1,1,1,1,1,1,1,1,1,1,1,1,1,1,1,1,1,1,1,1,1,1,6),(-0.941429844437971,-0.940000000000001,
-0.935000000000001,-0.930000000000001,-0.925000000000001,-0.920000000000001,
-0.915000000000001,-0.910000000000001,-0.905000000000001,-0.900000000000001,
-0.895000000000001,-0.890000000000001,-0.885000000000001,-0.880000000000001,
-0.875000000000001,-0.870000000000001,-0.865000000000001,-0.860000000000001,
-0.855000000000001,-0.850000000000001,-0.845000000000001,-0.840000000000001,
-0.835000000000001,-0.830000000000001,-0.825000000000001,-0.820000000000001,
-0.815000000000001,-0.810000000000001,-0.805000000000001,-0.800000000000001,
-0.795000000000001,-0.790000000000001,-0.785000000000001,-0.780000000000001,
-0.775000000000001,-0.770000000000001,-0.765000000000001,-0.760000000000001,
-0.755000000000001,-0.750000000000001,-0.745000000000001,-0.740000000000001,
-0.735000000000001,-0.730000000000001,-0.725000000000001,-0.720000000000001,
-0.715000000000001,-0.710000000000001,-0.705000000000001,-0.700000000000001,
-0.695000000000001,-0.690000000000001,-0.685,-0.68,-0.675,-0.67,-0.665,
-0.66,-0.655,-0.65,-0.645,-0.64,-0.635,-0.63,-0.625,-0.62,-0.615,-0.61,
-0.605,-0.6,-0.595,-0.59,-0.585,-0.58,-0.575,-0.57,-0.565,-0.56,-0.555,
-0.55,-0.545,-0.54,-0.535,-0.53,-0.525,-0.52,-0.515,-0.51,-0.505,-0.5,-0.495,
-0.49,-0.485,-0.48,-0.475,-0.47,-0.465,-0.46,-0.455,-0.45,-0.445,-0.44,
-0.435,-0.43,-0.425,-0.42,-0.415,-0.41,-0.405,-0.4,-0.395,-0.39,-0.385,
-0.38,-0.375,-0.37,-0.365,-0.36,-0.355,-0.35,-0.345,-0.34,-0.335,-0.33,
-0.325,-0.32,-0.315,-0.31,-0.305,-0.3,-0.295,-0.29,-0.285,-0.28,-0.275,
-0.27,-0.265,-0.26,-0.255,-0.25,-0.245,-0.24,-0.235,-0.23,-0.225,-0.22,
-0.215,-0.21,-0.205,-0.2,-0.195,-0.19,-0.185,-0.18,-0.175,-0.17,-0.165,
-0.16,-0.155,-0.15,-0.145,-0.14,-0.135,-0.13,-0.125,-0.12,-0.115,-0.11,
-0.105,-0.1,-0.095,-0.09,-0.085,-0.08,-0.075,-0.07,-0.065,-0.06,-0.055,
-0.05,-0.045,-0.04,-0.035,-0.03,-0.025,-0.02,-0.015,-0.01,-0.005,0.),
 .UNSPECIFIED.)
CURVE()
GEOMETRIC_REPRESENTATION_ITEM()
RATIONAL_B_SPLINE_CURVE((1.,1.,1.,1.,1.,1.,1.,1.,1.,1.,1.,1.,1.,1.,1.,1.,
1.,1.,1.,1.,1.,1.,1.,1.,1.,1.,1.,1.,1.,1.,1.,1.,1.,1.,1.,1.,1.,1.,1.,1.,
1.,1.,1.,1.,1.,1.,1.,1.,1.,1.,1.,1.,1.,1.,1.,1.,1.,1.,1.,1.,1.,1.,1.,1.,
1.,1.,1.,1.,1.,1.,1.,1.,1.,1.,1.,1.,1.,1.,1.,1.,1.,1.,1.,1.,1.,1.,1.,1.,
1.,1.,1.,1.,1.,1.,1.,1.,1.,1.,1.,1.,1.,1.,1.,1.,1.,1.,1.,1.,1.,1.,1.,1.,
1.,1.,1.,1.,1.,1.,1.,1.,1.,1.,1.,1.,1.,1.,1.,1.,1.,1.,1.,1.,1.,1.,1.,1.,
1.,1.,1.,1.,1.,1.,1.,1.,1.,1.,1.,1.,1.,1.,1.,1.,1.,1.,1.,1.,1.,1.,1.,1.,
1.,1.,1.,1.,1.,1.,1.,1.,1.,1.,1.,1.,1.,1.,1.,1.,1.,1.,1.,1.,1.,1.,1.,1.,
1.,1.,1.,1.,1.,1.,1.,1.,1.,1.))
REPRESENTATION_ITEM('')
);
#599=(
BOUNDED_CURVE()
B_SPLINE_CURVE(5,(#138230,#138231,#138232,#138233,#138234,#138235,#138236,
#138237,#138238,#138239,#138240,#138241,#138242,#138243,#138244,#138245,
#138246,#138247,#138248,#138249,#138250,#138251,#138252,#138253,#138254,
#138255,#138256,#138257,#138258,#138259,#138260,#138261,#138262,#138263,
#138264,#138265,#138266,#138267,#138268,#138269,#138270,#138271,#138272,
#138273,#138274,#138275,#138276,#138277,#138278,#138279,#138280,#138281,
#138282,#138283,#138284,#138285,#138286,#138287,#138288,#138289,#138290,
#138291,#138292,#138293,#138294,#138295,#138296,#138297,#138298,#138299,
#138300,#138301,#138302,#138303,#138304,#138305,#138306,#138307,#138308,
#138309,#138310,#138311,#138312,#138313,#138314,#138315,#138316,#138317,
#138318,#138319,#138320,#138321,#138322,#138323,#138324,#138325,#138326,
#138327,#138328,#138329,#138330,#138331,#138332,#138333,#138334,#138335,
#138336,#138337,#138338,#138339,#138340,#138341,#138342,#138343,#138344,
#138345,#138346,#138347,#138348,#138349,#138350,#138351,#138352,#138353,
#138354,#138355,#138356,#138357,#138358,#138359,#138360,#138361,#138362,
#138363,#138364,#138365,#138366,#138367,#138368,#138369,#138370,#138371,
#138372,#138373,#138374,#138375,#138376,#138377,#138378,#138379,#138380,
#138381,#138382,#138383,#138384,#138385,#138386,#138387,#138388,#138389,
#138390,#138391,#138392,#138393,#138394,#138395,#138396,#138397,#138398,
#138399,#138400,#138401,#138402,#138403,#138404,#138405,#138406,#138407,
#138408,#138409,#138410,#138411,#138412,#138413,#138414,#138415,#138416,
#138417,#138418,#138419,#138420,#138421,#138422,#138423),.UNSPECIFIED.,
 .F.,.F.)
B_SPLINE_CURVE_WITH_KNOTS((6,1,1,1,1,1,1,1,1,1,1,1,1,1,1,1,1,1,1,1,1,1,
1,1,1,1,1,1,1,1,1,1,1,1,1,1,1,1,1,1,1,1,1,1,1,1,1,1,1,1,1,1,1,1,1,1,1,1,
1,1,1,1,1,1,1,1,1,1,1,1,1,1,1,1,1,1,1,1,1,1,1,1,1,1,1,1,1,1,1,1,1,1,1,1,
1,1,1,1,1,1,1,1,1,1,1,1,1,1,1,1,1,1,1,1,1,1,1,1,1,1,1,1,1,1,1,1,1,1,1,1,
1,1,1,1,1,1,1,1,1,1,1,1,1,1,1,1,1,1,1,1,1,1,1,1,1,1,1,1,1,1,1,1,1,1,1,1,
1,1,1,1,1,1,1,1,1,1,1,1,1,1,1,1,1,1,1,1,1,1,1,6),(0.,0.005,0.01,0.015,0.02,
0.025,0.03,0.035,0.04,0.045,0.05,0.055,0.06,0.065,0.07,0.075,0.08,0.085,
0.09,0.095,0.1,0.105,0.11,0.115,0.12,0.125,0.13,0.135,0.14,0.145,0.15,0.155,
0.16,0.165,0.17,0.175,0.18,0.185,0.19,0.195,0.2,0.205,0.21,0.215,0.22,0.225,
0.23,0.235,0.24,0.245,0.25,0.255,0.26,0.265,0.27,0.275,0.28,0.285,0.29,
0.295,0.3,0.305,0.31,0.315,0.32,0.325,0.33,0.335,0.34,0.345,0.35,0.355,
0.36,0.365,0.37,0.375,0.38,0.385,0.39,0.395,0.4,0.405,0.41,0.415,0.42,0.425,
0.43,0.435,0.44,0.445,0.45,0.455,0.46,0.465,0.47,0.475,0.48,0.485,0.49,
0.495,0.5,0.505,0.51,0.515,0.52,0.525,0.53,0.535,0.54,0.545,0.55,0.555,
0.56,0.565,0.57,0.575,0.58,0.585,0.59,0.595,0.6,0.605,0.61,0.615,0.62,0.625,
0.63,0.635,0.64,0.645,0.65,0.655,0.66,0.665,0.67,0.675,0.68,0.685,0.690000000000001,
0.695000000000001,0.700000000000001,0.705000000000001,0.710000000000001,
0.715000000000001,0.720000000000001,0.725000000000001,0.730000000000001,
0.735000000000001,0.740000000000001,0.745000000000001,0.750000000000001,
0.755000000000001,0.760000000000001,0.765000000000001,0.770000000000001,
0.775000000000001,0.780000000000001,0.785000000000001,0.790000000000001,
0.795000000000001,0.800000000000001,0.805000000000001,0.810000000000001,
0.815000000000001,0.820000000000001,0.825000000000001,0.830000000000001,
0.835000000000001,0.840000000000001,0.845000000000001,0.850000000000001,
0.855000000000001,0.860000000000001,0.865000000000001,0.870000000000001,
0.875000000000001,0.880000000000001,0.885000000000001,0.890000000000001,
0.895000000000001,0.900000000000001,0.905000000000001,0.910000000000001,
0.915000000000001,0.920000000000001,0.925000000000001,0.930000000000001,
0.935000000000001,0.940000000000001,0.941429844438107),.UNSPECIFIED.)
CURVE()
GEOMETRIC_REPRESENTATION_ITEM()
RATIONAL_B_SPLINE_CURVE((1.,1.,1.,1.,1.,1.,1.,1.,1.,1.,1.,1.,1.,1.,1.,1.,
1.,1.,1.,1.,1.,1.,1.,1.,1.,1.,1.,1.,1.,1.,1.,1.,1.,1.,1.,1.,1.,1.,1.,1.,
1.,1.,1.,1.,1.,1.,1.,1.,1.,1.,1.,1.,1.,1.,1.,1.,1.,1.,1.,1.,1.,1.,1.,1.,
1.,1.,1.,1.,1.,1.,1.,1.,1.,1.,1.,1.,1.,1.,1.,1.,1.,1.,1.,1.,1.,1.,1.,1.,
1.,1.,1.,1.,1.,1.,1.,1.,1.,1.,1.,1.,1.,1.,1.,1.,1.,1.,1.,1.,1.,1.,1.,1.,
1.,1.,1.,1.,1.,1.,1.,1.,1.,1.,1.,1.,1.,1.,1.,1.,1.,1.,1.,1.,1.,1.,1.,1.,
1.,1.,1.,1.,1.,1.,1.,1.,1.,1.,1.,1.,1.,1.,1.,1.,1.,1.,1.,1.,1.,1.,1.,1.,
1.,1.,1.,1.,1.,1.,1.,1.,1.,1.,1.,1.,1.,1.,1.,1.,1.,1.,1.,1.,1.,1.,1.,1.,
1.,1.,1.,1.,1.,1.,1.,1.,1.,1.))
REPRESENTATION_ITEM('')
);
#600=(
BOUNDED_CURVE()
B_SPLINE_CURVE(5,(#138426,#138427,#138428,#138429,#138430,#138431,#138432,
#138433,#138434,#138435,#138436,#138437,#138438,#138439,#138440,#138441,
#138442,#138443,#138444,#138445,#138446,#138447,#138448,#138449,#138450,
#138451,#138452,#138453,#138454,#138455,#138456,#138457,#138458,#138459,
#138460,#138461,#138462,#138463,#138464,#138465,#138466,#138467,#138468,
#138469,#138470,#138471,#138472,#138473,#138474,#138475,#138476,#138477,
#138478,#138479,#138480,#138481,#138482,#138483,#138484,#138485,#138486,
#138487,#138488,#138489,#138490,#138491,#138492,#138493,#138494,#138495,
#138496,#138497,#138498,#138499,#138500,#138501,#138502,#138503,#138504,
#138505,#138506,#138507,#138508,#138509,#138510,#138511,#138512,#138513,
#138514,#138515,#138516,#138517,#138518,#138519,#138520,#138521,#138522,
#138523,#138524,#138525,#138526,#138527,#138528,#138529,#138530,#138531,
#138532,#138533,#138534,#138535,#138536,#138537,#138538,#138539,#138540,
#138541,#138542,#138543,#138544,#138545,#138546,#138547,#138548,#138549,
#138550,#138551,#138552,#138553,#138554,#138555,#138556,#138557,#138558,
#138559,#138560,#138561,#138562,#138563,#138564,#138565,#138566,#138567,
#138568,#138569,#138570,#138571,#138572,#138573,#138574,#138575,#138576,
#138577,#138578,#138579,#138580,#138581,#138582,#138583,#138584,#138585,
#138586,#138587,#138588,#138589,#138590,#138591,#138592,#138593,#138594,
#138595,#138596,#138597,#138598,#138599,#138600,#138601,#138602,#138603,
#138604,#138605,#138606,#138607,#138608,#138609,#138610,#138611,#138612,
#138613,#138614,#138615,#138616,#138617,#138618,#138619),.UNSPECIFIED.,
 .F.,.F.)
B_SPLINE_CURVE_WITH_KNOTS((6,1,1,1,1,1,1,1,1,1,1,1,1,1,1,1,1,1,1,1,1,1,
1,1,1,1,1,1,1,1,1,1,1,1,1,1,1,1,1,1,1,1,1,1,1,1,1,1,1,1,1,1,1,1,1,1,1,1,
1,1,1,1,1,1,1,1,1,1,1,1,1,1,1,1,1,1,1,1,1,1,1,1,1,1,1,1,1,1,1,1,1,1,1,1,
1,1,1,1,1,1,1,1,1,1,1,1,1,1,1,1,1,1,1,1,1,1,1,1,1,1,1,1,1,1,1,1,1,1,1,1,
1,1,1,1,1,1,1,1,1,1,1,1,1,1,1,1,1,1,1,1,1,1,1,1,1,1,1,1,1,1,1,1,1,1,1,1,
1,1,1,1,1,1,1,1,1,1,1,1,1,1,1,1,1,1,1,1,1,1,1,6),(-0.941429844438107,-0.940000000000001,
-0.935000000000001,-0.930000000000001,-0.925000000000001,-0.920000000000001,
-0.915000000000001,-0.910000000000001,-0.905000000000001,-0.900000000000001,
-0.895000000000001,-0.890000000000001,-0.885000000000001,-0.880000000000001,
-0.875000000000001,-0.870000000000001,-0.865000000000001,-0.860000000000001,
-0.855000000000001,-0.850000000000001,-0.845000000000001,-0.840000000000001,
-0.835000000000001,-0.830000000000001,-0.825000000000001,-0.820000000000001,
-0.815000000000001,-0.810000000000001,-0.805000000000001,-0.800000000000001,
-0.795000000000001,-0.790000000000001,-0.785000000000001,-0.780000000000001,
-0.775000000000001,-0.770000000000001,-0.765000000000001,-0.760000000000001,
-0.755000000000001,-0.750000000000001,-0.745000000000001,-0.740000000000001,
-0.735000000000001,-0.730000000000001,-0.725000000000001,-0.720000000000001,
-0.715000000000001,-0.710000000000001,-0.705000000000001,-0.700000000000001,
-0.695000000000001,-0.690000000000001,-0.685,-0.68,-0.675,-0.67,-0.665,
-0.66,-0.655,-0.65,-0.645,-0.64,-0.635,-0.63,-0.625,-0.62,-0.615,-0.61,
-0.605,-0.6,-0.595,-0.59,-0.585,-0.58,-0.575,-0.57,-0.565,-0.56,-0.555,
-0.55,-0.545,-0.54,-0.535,-0.53,-0.525,-0.52,-0.515,-0.51,-0.505,-0.5,-0.495,
-0.49,-0.485,-0.48,-0.475,-0.47,-0.465,-0.46,-0.455,-0.45,-0.445,-0.44,
-0.435,-0.43,-0.425,-0.42,-0.415,-0.41,-0.405,-0.4,-0.395,-0.39,-0.385,
-0.38,-0.375,-0.37,-0.365,-0.36,-0.355,-0.35,-0.345,-0.34,-0.335,-0.33,
-0.325,-0.32,-0.315,-0.31,-0.305,-0.3,-0.295,-0.29,-0.285,-0.28,-0.275,
-0.27,-0.265,-0.26,-0.255,-0.25,-0.245,-0.24,-0.235,-0.23,-0.225,-0.22,
-0.215,-0.21,-0.205,-0.2,-0.195,-0.19,-0.185,-0.18,-0.175,-0.17,-0.165,
-0.16,-0.155,-0.15,-0.145,-0.14,-0.135,-0.13,-0.125,-0.12,-0.115,-0.11,
-0.105,-0.1,-0.095,-0.09,-0.085,-0.08,-0.075,-0.07,-0.065,-0.06,-0.055,
-0.05,-0.045,-0.04,-0.035,-0.03,-0.025,-0.02,-0.015,-0.01,-0.005,0.),
 .UNSPECIFIED.)
CURVE()
GEOMETRIC_REPRESENTATION_ITEM()
RATIONAL_B_SPLINE_CURVE((1.,1.,1.,1.,1.,1.,1.,1.,1.,1.,1.,1.,1.,1.,1.,1.,
1.,1.,1.,1.,1.,1.,1.,1.,1.,1.,1.,1.,1.,1.,1.,1.,1.,1.,1.,1.,1.,1.,1.,1.,
1.,1.,1.,1.,1.,1.,1.,1.,1.,1.,1.,1.,1.,1.,1.,1.,1.,1.,1.,1.,1.,1.,1.,1.,
1.,1.,1.,1.,1.,1.,1.,1.,1.,1.,1.,1.,1.,1.,1.,1.,1.,1.,1.,1.,1.,1.,1.,1.,
1.,1.,1.,1.,1.,1.,1.,1.,1.,1.,1.,1.,1.,1.,1.,1.,1.,1.,1.,1.,1.,1.,1.,1.,
1.,1.,1.,1.,1.,1.,1.,1.,1.,1.,1.,1.,1.,1.,1.,1.,1.,1.,1.,1.,1.,1.,1.,1.,
1.,1.,1.,1.,1.,1.,1.,1.,1.,1.,1.,1.,1.,1.,1.,1.,1.,1.,1.,1.,1.,1.,1.,1.,
1.,1.,1.,1.,1.,1.,1.,1.,1.,1.,1.,1.,1.,1.,1.,1.,1.,1.,1.,1.,1.,1.,1.,1.,
1.,1.,1.,1.,1.,1.,1.,1.,1.,1.))
REPRESENTATION_ITEM('')
);
#601=(
BOUNDED_CURVE()
B_SPLINE_CURVE(5,(#139031,#139032,#139033,#139034,#139035,#139036,#139037,
#139038,#139039,#139040,#139041,#139042,#139043,#139044,#139045,#139046,
#139047,#139048,#139049,#139050,#139051,#139052,#139053,#139054,#139055,
#139056,#139057,#139058,#139059,#139060,#139061,#139062,#139063,#139064,
#139065,#139066,#139067,#139068,#139069,#139070,#139071,#139072,#139073,
#139074,#139075,#139076,#139077,#139078,#139079,#139080,#139081,#139082,
#139083,#139084,#139085,#139086,#139087,#139088,#139089,#139090,#139091,
#139092,#139093,#139094,#139095,#139096,#139097,#139098,#139099,#139100,
#139101,#139102,#139103,#139104,#139105,#139106,#139107,#139108,#139109,
#139110,#139111,#139112,#139113,#139114,#139115,#139116,#139117,#139118,
#139119,#139120,#139121,#139122,#139123,#139124,#139125,#139126,#139127,
#139128,#139129,#139130,#139131,#139132,#139133,#139134,#139135,#139136,
#139137,#139138,#139139,#139140,#139141,#139142,#139143,#139144,#139145,
#139146,#139147,#139148,#139149,#139150,#139151,#139152,#139153,#139154,
#139155,#139156,#139157,#139158,#139159,#139160,#139161,#139162,#139163,
#139164,#139165,#139166,#139167,#139168,#139169,#139170,#139171,#139172,
#139173,#139174,#139175,#139176,#139177,#139178,#139179,#139180,#139181,
#139182,#139183,#139184,#139185,#139186,#139187,#139188,#139189,#139190,
#139191,#139192,#139193,#139194,#139195,#139196,#139197,#139198,#139199,
#139200,#139201,#139202,#139203,#139204,#139205,#139206,#139207,#139208,
#139209,#139210,#139211,#139212,#139213,#139214,#139215,#139216,#139217,
#139218,#139219,#139220,#139221,#139222,#139223,#139224),.UNSPECIFIED.,
 .F.,.F.)
B_SPLINE_CURVE_WITH_KNOTS((6,1,1,1,1,1,1,1,1,1,1,1,1,1,1,1,1,1,1,1,1,1,
1,1,1,1,1,1,1,1,1,1,1,1,1,1,1,1,1,1,1,1,1,1,1,1,1,1,1,1,1,1,1,1,1,1,1,1,
1,1,1,1,1,1,1,1,1,1,1,1,1,1,1,1,1,1,1,1,1,1,1,1,1,1,1,1,1,1,1,1,1,1,1,1,
1,1,1,1,1,1,1,1,1,1,1,1,1,1,1,1,1,1,1,1,1,1,1,1,1,1,1,1,1,1,1,1,1,1,1,1,
1,1,1,1,1,1,1,1,1,1,1,1,1,1,1,1,1,1,1,1,1,1,1,1,1,1,1,1,1,1,1,1,1,1,1,1,
1,1,1,1,1,1,1,1,1,1,1,1,1,1,1,1,1,1,1,1,1,1,1,6),(0.,0.005,0.01,0.015,0.02,
0.025,0.03,0.035,0.04,0.045,0.05,0.055,0.06,0.065,0.07,0.075,0.08,0.085,
0.09,0.095,0.1,0.105,0.11,0.115,0.12,0.125,0.13,0.135,0.14,0.145,0.15,0.155,
0.16,0.165,0.17,0.175,0.18,0.185,0.19,0.195,0.2,0.205,0.21,0.215,0.22,0.225,
0.23,0.235,0.24,0.245,0.25,0.255,0.26,0.265,0.27,0.275,0.28,0.285,0.29,
0.295,0.3,0.305,0.31,0.315,0.32,0.325,0.33,0.335,0.34,0.345,0.35,0.355,
0.36,0.365,0.37,0.375,0.38,0.385,0.39,0.395,0.4,0.405,0.41,0.415,0.42,0.425,
0.43,0.435,0.44,0.445,0.45,0.455,0.46,0.465,0.47,0.475,0.48,0.485,0.49,
0.495,0.5,0.505,0.51,0.515,0.52,0.525,0.53,0.535,0.54,0.545,0.55,0.555,
0.56,0.565,0.57,0.575,0.58,0.585,0.59,0.595,0.6,0.605,0.61,0.615,0.62,0.625,
0.63,0.635,0.64,0.645,0.65,0.655,0.66,0.665,0.67,0.675,0.68,0.685,0.690000000000001,
0.695000000000001,0.700000000000001,0.705000000000001,0.710000000000001,
0.715000000000001,0.720000000000001,0.725000000000001,0.730000000000001,
0.735000000000001,0.740000000000001,0.745000000000001,0.750000000000001,
0.755000000000001,0.760000000000001,0.765000000000001,0.770000000000001,
0.775000000000001,0.780000000000001,0.785000000000001,0.790000000000001,
0.795000000000001,0.800000000000001,0.805000000000001,0.810000000000001,
0.815000000000001,0.820000000000001,0.825000000000001,0.830000000000001,
0.835000000000001,0.840000000000001,0.845000000000001,0.850000000000001,
0.855000000000001,0.860000000000001,0.865000000000001,0.870000000000001,
0.875000000000001,0.880000000000001,0.885000000000001,0.890000000000001,
0.895000000000001,0.900000000000001,0.905000000000001,0.910000000000001,
0.915000000000001,0.920000000000001,0.925000000000001,0.930000000000001,
0.935000000000001,0.940000000000001,0.941429844438169),.UNSPECIFIED.)
CURVE()
GEOMETRIC_REPRESENTATION_ITEM()
RATIONAL_B_SPLINE_CURVE((1.,1.,1.,1.,1.,1.,1.,1.,1.,1.,1.,1.,1.,1.,1.,1.,
1.,1.,1.,1.,1.,1.,1.,1.,1.,1.,1.,1.,1.,1.,1.,1.,1.,1.,1.,1.,1.,1.,1.,1.,
1.,1.,1.,1.,1.,1.,1.,1.,1.,1.,1.,1.,1.,1.,1.,1.,1.,1.,1.,1.,1.,1.,1.,1.,
1.,1.,1.,1.,1.,1.,1.,1.,1.,1.,1.,1.,1.,1.,1.,1.,1.,1.,1.,1.,1.,1.,1.,1.,
1.,1.,1.,1.,1.,1.,1.,1.,1.,1.,1.,1.,1.,1.,1.,1.,1.,1.,1.,1.,1.,1.,1.,1.,
1.,1.,1.,1.,1.,1.,1.,1.,1.,1.,1.,1.,1.,1.,1.,1.,1.,1.,1.,1.,1.,1.,1.,1.,
1.,1.,1.,1.,1.,1.,1.,1.,1.,1.,1.,1.,1.,1.,1.,1.,1.,1.,1.,1.,1.,1.,1.,1.,
1.,1.,1.,1.,1.,1.,1.,1.,1.,1.,1.,1.,1.,1.,1.,1.,1.,1.,1.,1.,1.,1.,1.,1.,
1.,1.,1.,1.,1.,1.,1.,1.,1.,1.))
REPRESENTATION_ITEM('')
);
#602=(
BOUNDED_CURVE()
B_SPLINE_CURVE(5,(#139227,#139228,#139229,#139230,#139231,#139232,#139233,
#139234,#139235,#139236,#139237,#139238,#139239,#139240,#139241,#139242,
#139243,#139244,#139245,#139246,#139247,#139248,#139249,#139250,#139251,
#139252,#139253,#139254,#139255,#139256,#139257,#139258,#139259,#139260,
#139261,#139262,#139263,#139264,#139265,#139266,#139267,#139268,#139269,
#139270,#139271,#139272,#139273,#139274,#139275,#139276,#139277,#139278,
#139279,#139280,#139281,#139282,#139283,#139284,#139285,#139286,#139287,
#139288,#139289,#139290,#139291,#139292,#139293,#139294,#139295,#139296,
#139297,#139298,#139299,#139300,#139301,#139302,#139303,#139304,#139305,
#139306,#139307,#139308,#139309,#139310,#139311,#139312,#139313,#139314,
#139315,#139316,#139317,#139318,#139319,#139320,#139321,#139322,#139323,
#139324,#139325,#139326,#139327,#139328,#139329,#139330,#139331,#139332,
#139333,#139334,#139335,#139336,#139337,#139338,#139339,#139340,#139341,
#139342,#139343,#139344,#139345,#139346,#139347,#139348,#139349,#139350,
#139351,#139352,#139353,#139354,#139355,#139356,#139357,#139358,#139359,
#139360,#139361,#139362,#139363,#139364,#139365,#139366,#139367,#139368,
#139369,#139370,#139371,#139372,#139373,#139374,#139375,#139376,#139377,
#139378,#139379,#139380,#139381,#139382,#139383,#139384,#139385,#139386,
#139387,#139388,#139389,#139390,#139391,#139392,#139393,#139394,#139395,
#139396,#139397,#139398,#139399,#139400,#139401,#139402,#139403,#139404,
#139405,#139406,#139407,#139408,#139409,#139410,#139411,#139412,#139413,
#139414,#139415,#139416,#139417,#139418,#139419,#139420),.UNSPECIFIED.,
 .F.,.F.)
B_SPLINE_CURVE_WITH_KNOTS((6,1,1,1,1,1,1,1,1,1,1,1,1,1,1,1,1,1,1,1,1,1,
1,1,1,1,1,1,1,1,1,1,1,1,1,1,1,1,1,1,1,1,1,1,1,1,1,1,1,1,1,1,1,1,1,1,1,1,
1,1,1,1,1,1,1,1,1,1,1,1,1,1,1,1,1,1,1,1,1,1,1,1,1,1,1,1,1,1,1,1,1,1,1,1,
1,1,1,1,1,1,1,1,1,1,1,1,1,1,1,1,1,1,1,1,1,1,1,1,1,1,1,1,1,1,1,1,1,1,1,1,
1,1,1,1,1,1,1,1,1,1,1,1,1,1,1,1,1,1,1,1,1,1,1,1,1,1,1,1,1,1,1,1,1,1,1,1,
1,1,1,1,1,1,1,1,1,1,1,1,1,1,1,1,1,1,1,1,1,1,1,6),(-0.941429844438167,-0.940000000000001,
-0.935000000000001,-0.930000000000001,-0.925000000000001,-0.920000000000001,
-0.915000000000001,-0.910000000000001,-0.905000000000001,-0.900000000000001,
-0.895000000000001,-0.890000000000001,-0.885000000000001,-0.880000000000001,
-0.875000000000001,-0.870000000000001,-0.865000000000001,-0.860000000000001,
-0.855000000000001,-0.850000000000001,-0.845000000000001,-0.840000000000001,
-0.835000000000001,-0.830000000000001,-0.825000000000001,-0.820000000000001,
-0.815000000000001,-0.810000000000001,-0.805000000000001,-0.800000000000001,
-0.795000000000001,-0.790000000000001,-0.785000000000001,-0.780000000000001,
-0.775000000000001,-0.770000000000001,-0.765000000000001,-0.760000000000001,
-0.755000000000001,-0.750000000000001,-0.745000000000001,-0.740000000000001,
-0.735000000000001,-0.730000000000001,-0.725000000000001,-0.720000000000001,
-0.715000000000001,-0.710000000000001,-0.705000000000001,-0.700000000000001,
-0.695000000000001,-0.690000000000001,-0.685,-0.68,-0.675,-0.67,-0.665,
-0.66,-0.655,-0.65,-0.645,-0.64,-0.635,-0.63,-0.625,-0.62,-0.615,-0.61,
-0.605,-0.6,-0.595,-0.59,-0.585,-0.58,-0.575,-0.57,-0.565,-0.56,-0.555,
-0.55,-0.545,-0.54,-0.535,-0.53,-0.525,-0.52,-0.515,-0.51,-0.505,-0.5,-0.495,
-0.49,-0.485,-0.48,-0.475,-0.47,-0.465,-0.46,-0.455,-0.45,-0.445,-0.44,
-0.435,-0.43,-0.425,-0.42,-0.415,-0.41,-0.405,-0.4,-0.395,-0.39,-0.385,
-0.38,-0.375,-0.37,-0.365,-0.36,-0.355,-0.35,-0.345,-0.34,-0.335,-0.33,
-0.325,-0.32,-0.315,-0.31,-0.305,-0.3,-0.295,-0.29,-0.285,-0.28,-0.275,
-0.27,-0.265,-0.26,-0.255,-0.25,-0.245,-0.24,-0.235,-0.23,-0.225,-0.22,
-0.215,-0.21,-0.205,-0.2,-0.195,-0.19,-0.185,-0.18,-0.175,-0.17,-0.165,
-0.16,-0.155,-0.15,-0.145,-0.14,-0.135,-0.13,-0.125,-0.12,-0.115,-0.11,
-0.105,-0.1,-0.095,-0.09,-0.085,-0.08,-0.075,-0.07,-0.065,-0.06,-0.055,
-0.05,-0.045,-0.04,-0.035,-0.03,-0.025,-0.02,-0.015,-0.01,-0.005,0.),
 .UNSPECIFIED.)
CURVE()
GEOMETRIC_REPRESENTATION_ITEM()
RATIONAL_B_SPLINE_CURVE((1.,1.,1.,1.,1.,1.,1.,1.,1.,1.,1.,1.,1.,1.,1.,1.,
1.,1.,1.,1.,1.,1.,1.,1.,1.,1.,1.,1.,1.,1.,1.,1.,1.,1.,1.,1.,1.,1.,1.,1.,
1.,1.,1.,1.,1.,1.,1.,1.,1.,1.,1.,1.,1.,1.,1.,1.,1.,1.,1.,1.,1.,1.,1.,1.,
1.,1.,1.,1.,1.,1.,1.,1.,1.,1.,1.,1.,1.,1.,1.,1.,1.,1.,1.,1.,1.,1.,1.,1.,
1.,1.,1.,1.,1.,1.,1.,1.,1.,1.,1.,1.,1.,1.,1.,1.,1.,1.,1.,1.,1.,1.,1.,1.,
1.,1.,1.,1.,1.,1.,1.,1.,1.,1.,1.,1.,1.,1.,1.,1.,1.,1.,1.,1.,1.,1.,1.,1.,
1.,1.,1.,1.,1.,1.,1.,1.,1.,1.,1.,1.,1.,1.,1.,1.,1.,1.,1.,1.,1.,1.,1.,1.,
1.,1.,1.,1.,1.,1.,1.,1.,1.,1.,1.,1.,1.,1.,1.,1.,1.,1.,1.,1.,1.,1.,1.,1.,
1.,1.,1.,1.,1.,1.,1.,1.,1.,1.))
REPRESENTATION_ITEM('')
);
#603=(
BOUNDED_CURVE()
B_SPLINE_CURVE(5,(#139832,#139833,#139834,#139835,#139836,#139837,#139838,
#139839,#139840,#139841,#139842,#139843,#139844,#139845,#139846,#139847,
#139848,#139849,#139850,#139851,#139852,#139853,#139854,#139855,#139856,
#139857,#139858,#139859,#139860,#139861,#139862,#139863,#139864,#139865,
#139866,#139867,#139868,#139869,#139870,#139871,#139872,#139873,#139874,
#139875,#139876,#139877,#139878,#139879,#139880,#139881,#139882,#139883,
#139884,#139885,#139886,#139887,#139888,#139889,#139890,#139891,#139892,
#139893,#139894,#139895,#139896,#139897,#139898,#139899,#139900,#139901,
#139902,#139903,#139904,#139905,#139906,#139907,#139908,#139909,#139910,
#139911,#139912,#139913,#139914,#139915,#139916,#139917,#139918,#139919,
#139920,#139921,#139922,#139923,#139924,#139925,#139926,#139927,#139928,
#139929,#139930,#139931,#139932,#139933,#139934,#139935,#139936,#139937,
#139938,#139939,#139940,#139941,#139942,#139943,#139944,#139945,#139946,
#139947,#139948,#139949,#139950,#139951,#139952,#139953,#139954,#139955,
#139956,#139957,#139958,#139959,#139960,#139961,#139962,#139963,#139964,
#139965,#139966,#139967,#139968,#139969,#139970,#139971,#139972,#139973,
#139974,#139975,#139976,#139977,#139978,#139979,#139980,#139981,#139982,
#139983,#139984,#139985,#139986,#139987,#139988,#139989,#139990,#139991,
#139992,#139993,#139994,#139995,#139996,#139997,#139998,#139999,#140000,
#140001,#140002,#140003,#140004,#140005,#140006,#140007,#140008,#140009,
#140010,#140011,#140012,#140013,#140014,#140015,#140016,#140017,#140018,
#140019,#140020,#140021,#140022,#140023,#140024,#140025),.UNSPECIFIED.,
 .F.,.F.)
B_SPLINE_CURVE_WITH_KNOTS((6,1,1,1,1,1,1,1,1,1,1,1,1,1,1,1,1,1,1,1,1,1,
1,1,1,1,1,1,1,1,1,1,1,1,1,1,1,1,1,1,1,1,1,1,1,1,1,1,1,1,1,1,1,1,1,1,1,1,
1,1,1,1,1,1,1,1,1,1,1,1,1,1,1,1,1,1,1,1,1,1,1,1,1,1,1,1,1,1,1,1,1,1,1,1,
1,1,1,1,1,1,1,1,1,1,1,1,1,1,1,1,1,1,1,1,1,1,1,1,1,1,1,1,1,1,1,1,1,1,1,1,
1,1,1,1,1,1,1,1,1,1,1,1,1,1,1,1,1,1,1,1,1,1,1,1,1,1,1,1,1,1,1,1,1,1,1,1,
1,1,1,1,1,1,1,1,1,1,1,1,1,1,1,1,1,1,1,1,1,1,1,6),(0.,0.005,0.01,0.015,0.02,
0.025,0.03,0.035,0.04,0.045,0.05,0.055,0.06,0.065,0.07,0.075,0.08,0.085,
0.09,0.095,0.1,0.105,0.11,0.115,0.12,0.125,0.13,0.135,0.14,0.145,0.15,0.155,
0.16,0.165,0.17,0.175,0.18,0.185,0.19,0.195,0.2,0.205,0.21,0.215,0.22,0.225,
0.23,0.235,0.24,0.245,0.25,0.255,0.26,0.265,0.27,0.275,0.28,0.285,0.29,
0.295,0.3,0.305,0.31,0.315,0.32,0.325,0.33,0.335,0.34,0.345,0.35,0.355,
0.36,0.365,0.37,0.375,0.38,0.385,0.39,0.395,0.4,0.405,0.41,0.415,0.42,0.425,
0.43,0.435,0.44,0.445,0.45,0.455,0.46,0.465,0.47,0.475,0.48,0.485,0.49,
0.495,0.5,0.505,0.51,0.515,0.52,0.525,0.53,0.535,0.54,0.545,0.55,0.555,
0.56,0.565,0.57,0.575,0.58,0.585,0.59,0.595,0.6,0.605,0.61,0.615,0.62,0.625,
0.63,0.635,0.64,0.645,0.65,0.655,0.66,0.665,0.67,0.675,0.68,0.685,0.690000000000001,
0.695000000000001,0.700000000000001,0.705000000000001,0.710000000000001,
0.715000000000001,0.720000000000001,0.725000000000001,0.730000000000001,
0.735000000000001,0.740000000000001,0.745000000000001,0.750000000000001,
0.755000000000001,0.760000000000001,0.765000000000001,0.770000000000001,
0.775000000000001,0.780000000000001,0.785000000000001,0.790000000000001,
0.795000000000001,0.800000000000001,0.805000000000001,0.810000000000001,
0.815000000000001,0.820000000000001,0.825000000000001,0.830000000000001,
0.835000000000001,0.840000000000001,0.845000000000001,0.850000000000001,
0.855000000000001,0.860000000000001,0.865000000000001,0.870000000000001,
0.875000000000001,0.880000000000001,0.885000000000001,0.890000000000001,
0.895000000000001,0.900000000000001,0.905000000000001,0.910000000000001,
0.915000000000001,0.920000000000001,0.925000000000001,0.930000000000001,
0.935000000000001,0.940000000000001,0.941429844438156),.UNSPECIFIED.)
CURVE()
GEOMETRIC_REPRESENTATION_ITEM()
RATIONAL_B_SPLINE_CURVE((1.,1.,1.,1.,1.,1.,1.,1.,1.,1.,1.,1.,1.,1.,1.,1.,
1.,1.,1.,1.,1.,1.,1.,1.,1.,1.,1.,1.,1.,1.,1.,1.,1.,1.,1.,1.,1.,1.,1.,1.,
1.,1.,1.,1.,1.,1.,1.,1.,1.,1.,1.,1.,1.,1.,1.,1.,1.,1.,1.,1.,1.,1.,1.,1.,
1.,1.,1.,1.,1.,1.,1.,1.,1.,1.,1.,1.,1.,1.,1.,1.,1.,1.,1.,1.,1.,1.,1.,1.,
1.,1.,1.,1.,1.,1.,1.,1.,1.,1.,1.,1.,1.,1.,1.,1.,1.,1.,1.,1.,1.,1.,1.,1.,
1.,1.,1.,1.,1.,1.,1.,1.,1.,1.,1.,1.,1.,1.,1.,1.,1.,1.,1.,1.,1.,1.,1.,1.,
1.,1.,1.,1.,1.,1.,1.,1.,1.,1.,1.,1.,1.,1.,1.,1.,1.,1.,1.,1.,1.,1.,1.,1.,
1.,1.,1.,1.,1.,1.,1.,1.,1.,1.,1.,1.,1.,1.,1.,1.,1.,1.,1.,1.,1.,1.,1.,1.,
1.,1.,1.,1.,1.,1.,1.,1.,1.,1.))
REPRESENTATION_ITEM('')
);
#604=(
BOUNDED_CURVE()
B_SPLINE_CURVE(5,(#140028,#140029,#140030,#140031,#140032,#140033,#140034,
#140035,#140036,#140037,#140038,#140039,#140040,#140041,#140042,#140043,
#140044,#140045,#140046,#140047,#140048,#140049,#140050,#140051,#140052,
#140053,#140054,#140055,#140056,#140057,#140058,#140059,#140060,#140061,
#140062,#140063,#140064,#140065,#140066,#140067,#140068,#140069,#140070,
#140071,#140072,#140073,#140074,#140075,#140076,#140077,#140078,#140079,
#140080,#140081,#140082,#140083,#140084,#140085,#140086,#140087,#140088,
#140089,#140090,#140091,#140092,#140093,#140094,#140095,#140096,#140097,
#140098,#140099,#140100,#140101,#140102,#140103,#140104,#140105,#140106,
#140107,#140108,#140109,#140110,#140111,#140112,#140113,#140114,#140115,
#140116,#140117,#140118,#140119,#140120,#140121,#140122,#140123,#140124,
#140125,#140126,#140127,#140128,#140129,#140130,#140131,#140132,#140133,
#140134,#140135,#140136,#140137,#140138,#140139,#140140,#140141,#140142,
#140143,#140144,#140145,#140146,#140147,#140148,#140149,#140150,#140151,
#140152,#140153,#140154,#140155,#140156,#140157,#140158,#140159,#140160,
#140161,#140162,#140163,#140164,#140165,#140166,#140167,#140168,#140169,
#140170,#140171,#140172,#140173,#140174,#140175,#140176,#140177,#140178,
#140179,#140180,#140181,#140182,#140183,#140184,#140185,#140186,#140187,
#140188,#140189,#140190,#140191,#140192,#140193,#140194,#140195,#140196,
#140197,#140198,#140199,#140200,#140201,#140202,#140203,#140204,#140205,
#140206,#140207,#140208,#140209,#140210,#140211,#140212,#140213,#140214,
#140215,#140216,#140217,#140218,#140219,#140220,#140221),.UNSPECIFIED.,
 .F.,.F.)
B_SPLINE_CURVE_WITH_KNOTS((6,1,1,1,1,1,1,1,1,1,1,1,1,1,1,1,1,1,1,1,1,1,
1,1,1,1,1,1,1,1,1,1,1,1,1,1,1,1,1,1,1,1,1,1,1,1,1,1,1,1,1,1,1,1,1,1,1,1,
1,1,1,1,1,1,1,1,1,1,1,1,1,1,1,1,1,1,1,1,1,1,1,1,1,1,1,1,1,1,1,1,1,1,1,1,
1,1,1,1,1,1,1,1,1,1,1,1,1,1,1,1,1,1,1,1,1,1,1,1,1,1,1,1,1,1,1,1,1,1,1,1,
1,1,1,1,1,1,1,1,1,1,1,1,1,1,1,1,1,1,1,1,1,1,1,1,1,1,1,1,1,1,1,1,1,1,1,1,
1,1,1,1,1,1,1,1,1,1,1,1,1,1,1,1,1,1,1,1,1,1,1,6),(-0.941429844438138,-0.940000000000001,
-0.935000000000001,-0.930000000000001,-0.925000000000001,-0.920000000000001,
-0.915000000000001,-0.910000000000001,-0.905000000000001,-0.900000000000001,
-0.895000000000001,-0.890000000000001,-0.885000000000001,-0.880000000000001,
-0.875000000000001,-0.870000000000001,-0.865000000000001,-0.860000000000001,
-0.855000000000001,-0.850000000000001,-0.845000000000001,-0.840000000000001,
-0.835000000000001,-0.830000000000001,-0.825000000000001,-0.820000000000001,
-0.815000000000001,-0.810000000000001,-0.805000000000001,-0.800000000000001,
-0.795000000000001,-0.790000000000001,-0.785000000000001,-0.780000000000001,
-0.775000000000001,-0.770000000000001,-0.765000000000001,-0.760000000000001,
-0.755000000000001,-0.750000000000001,-0.745000000000001,-0.740000000000001,
-0.735000000000001,-0.730000000000001,-0.725000000000001,-0.720000000000001,
-0.715000000000001,-0.710000000000001,-0.705000000000001,-0.700000000000001,
-0.695000000000001,-0.690000000000001,-0.685,-0.68,-0.675,-0.67,-0.665,
-0.66,-0.655,-0.65,-0.645,-0.64,-0.635,-0.63,-0.625,-0.62,-0.615,-0.61,
-0.605,-0.6,-0.595,-0.59,-0.585,-0.58,-0.575,-0.57,-0.565,-0.56,-0.555,
-0.55,-0.545,-0.54,-0.535,-0.53,-0.525,-0.52,-0.515,-0.51,-0.505,-0.5,-0.495,
-0.49,-0.485,-0.48,-0.475,-0.47,-0.465,-0.46,-0.455,-0.45,-0.445,-0.44,
-0.435,-0.43,-0.425,-0.42,-0.415,-0.41,-0.405,-0.4,-0.395,-0.39,-0.385,
-0.38,-0.375,-0.37,-0.365,-0.36,-0.355,-0.35,-0.345,-0.34,-0.335,-0.33,
-0.325,-0.32,-0.315,-0.31,-0.305,-0.3,-0.295,-0.29,-0.285,-0.28,-0.275,
-0.27,-0.265,-0.26,-0.255,-0.25,-0.245,-0.24,-0.235,-0.23,-0.225,-0.22,
-0.215,-0.21,-0.205,-0.2,-0.195,-0.19,-0.185,-0.18,-0.175,-0.17,-0.165,
-0.16,-0.155,-0.15,-0.145,-0.14,-0.135,-0.13,-0.125,-0.12,-0.115,-0.11,
-0.105,-0.1,-0.095,-0.09,-0.085,-0.08,-0.075,-0.07,-0.065,-0.06,-0.055,
-0.05,-0.045,-0.04,-0.035,-0.03,-0.025,-0.02,-0.015,-0.01,-0.005,0.),
 .UNSPECIFIED.)
CURVE()
GEOMETRIC_REPRESENTATION_ITEM()
RATIONAL_B_SPLINE_CURVE((1.,1.,1.,1.,1.,1.,1.,1.,1.,1.,1.,1.,1.,1.,1.,1.,
1.,1.,1.,1.,1.,1.,1.,1.,1.,1.,1.,1.,1.,1.,1.,1.,1.,1.,1.,1.,1.,1.,1.,1.,
1.,1.,1.,1.,1.,1.,1.,1.,1.,1.,1.,1.,1.,1.,1.,1.,1.,1.,1.,1.,1.,1.,1.,1.,
1.,1.,1.,1.,1.,1.,1.,1.,1.,1.,1.,1.,1.,1.,1.,1.,1.,1.,1.,1.,1.,1.,1.,1.,
1.,1.,1.,1.,1.,1.,1.,1.,1.,1.,1.,1.,1.,1.,1.,1.,1.,1.,1.,1.,1.,1.,1.,1.,
1.,1.,1.,1.,1.,1.,1.,1.,1.,1.,1.,1.,1.,1.,1.,1.,1.,1.,1.,1.,1.,1.,1.,1.,
1.,1.,1.,1.,1.,1.,1.,1.,1.,1.,1.,1.,1.,1.,1.,1.,1.,1.,1.,1.,1.,1.,1.,1.,
1.,1.,1.,1.,1.,1.,1.,1.,1.,1.,1.,1.,1.,1.,1.,1.,1.,1.,1.,1.,1.,1.,1.,1.,
1.,1.,1.,1.,1.,1.,1.,1.,1.,1.))
REPRESENTATION_ITEM('')
);
#605=(
BOUNDED_CURVE()
B_SPLINE_CURVE(5,(#140633,#140634,#140635,#140636,#140637,#140638,#140639,
#140640,#140641,#140642,#140643,#140644,#140645,#140646,#140647,#140648,
#140649,#140650,#140651,#140652,#140653,#140654,#140655,#140656,#140657,
#140658,#140659,#140660,#140661,#140662,#140663,#140664,#140665,#140666,
#140667,#140668,#140669,#140670,#140671,#140672,#140673,#140674,#140675,
#140676,#140677,#140678,#140679,#140680,#140681,#140682,#140683,#140684,
#140685,#140686,#140687,#140688,#140689,#140690,#140691,#140692,#140693,
#140694,#140695,#140696,#140697,#140698,#140699,#140700,#140701,#140702,
#140703,#140704,#140705,#140706,#140707,#140708,#140709,#140710,#140711,
#140712,#140713,#140714,#140715,#140716,#140717,#140718,#140719,#140720,
#140721,#140722,#140723,#140724,#140725,#140726,#140727,#140728,#140729,
#140730,#140731,#140732,#140733,#140734,#140735,#140736,#140737,#140738,
#140739,#140740,#140741,#140742,#140743,#140744,#140745,#140746,#140747,
#140748,#140749,#140750,#140751,#140752,#140753,#140754,#140755,#140756,
#140757,#140758,#140759,#140760,#140761,#140762,#140763,#140764,#140765,
#140766,#140767,#140768,#140769,#140770,#140771,#140772,#140773,#140774,
#140775,#140776,#140777,#140778,#140779,#140780,#140781,#140782,#140783,
#140784,#140785,#140786,#140787,#140788,#140789,#140790,#140791,#140792,
#140793,#140794,#140795,#140796,#140797,#140798,#140799,#140800,#140801,
#140802,#140803,#140804,#140805,#140806,#140807,#140808,#140809,#140810,
#140811,#140812,#140813,#140814,#140815,#140816,#140817,#140818,#140819,
#140820,#140821,#140822,#140823,#140824,#140825,#140826),.UNSPECIFIED.,
 .F.,.F.)
B_SPLINE_CURVE_WITH_KNOTS((6,1,1,1,1,1,1,1,1,1,1,1,1,1,1,1,1,1,1,1,1,1,
1,1,1,1,1,1,1,1,1,1,1,1,1,1,1,1,1,1,1,1,1,1,1,1,1,1,1,1,1,1,1,1,1,1,1,1,
1,1,1,1,1,1,1,1,1,1,1,1,1,1,1,1,1,1,1,1,1,1,1,1,1,1,1,1,1,1,1,1,1,1,1,1,
1,1,1,1,1,1,1,1,1,1,1,1,1,1,1,1,1,1,1,1,1,1,1,1,1,1,1,1,1,1,1,1,1,1,1,1,
1,1,1,1,1,1,1,1,1,1,1,1,1,1,1,1,1,1,1,1,1,1,1,1,1,1,1,1,1,1,1,1,1,1,1,1,
1,1,1,1,1,1,1,1,1,1,1,1,1,1,1,1,1,1,1,1,1,1,1,6),(0.,0.005,0.01,0.015,0.02,
0.025,0.03,0.035,0.04,0.045,0.05,0.055,0.06,0.065,0.07,0.075,0.08,0.085,
0.09,0.095,0.1,0.105,0.11,0.115,0.12,0.125,0.13,0.135,0.14,0.145,0.15,0.155,
0.16,0.165,0.17,0.175,0.18,0.185,0.19,0.195,0.2,0.205,0.21,0.215,0.22,0.225,
0.23,0.235,0.24,0.245,0.25,0.255,0.26,0.265,0.27,0.275,0.28,0.285,0.29,
0.295,0.3,0.305,0.31,0.315,0.32,0.325,0.33,0.335,0.34,0.345,0.35,0.355,
0.36,0.365,0.37,0.375,0.38,0.385,0.39,0.395,0.4,0.405,0.41,0.415,0.42,0.425,
0.43,0.435,0.44,0.445,0.45,0.455,0.46,0.465,0.47,0.475,0.48,0.485,0.49,
0.495,0.5,0.505,0.51,0.515,0.52,0.525,0.53,0.535,0.54,0.545,0.55,0.555,
0.56,0.565,0.57,0.575,0.58,0.585,0.59,0.595,0.6,0.605,0.61,0.615,0.62,0.625,
0.63,0.635,0.64,0.645,0.65,0.655,0.66,0.665,0.67,0.675,0.68,0.685,0.690000000000001,
0.695000000000001,0.700000000000001,0.705000000000001,0.710000000000001,
0.715000000000001,0.720000000000001,0.725000000000001,0.730000000000001,
0.735000000000001,0.740000000000001,0.745000000000001,0.750000000000001,
0.755000000000001,0.760000000000001,0.765000000000001,0.770000000000001,
0.775000000000001,0.780000000000001,0.785000000000001,0.790000000000001,
0.795000000000001,0.800000000000001,0.805000000000001,0.810000000000001,
0.815000000000001,0.820000000000001,0.825000000000001,0.830000000000001,
0.835000000000001,0.840000000000001,0.845000000000001,0.850000000000001,
0.855000000000001,0.860000000000001,0.865000000000001,0.870000000000001,
0.875000000000001,0.880000000000001,0.885000000000001,0.890000000000001,
0.895000000000001,0.900000000000001,0.905000000000001,0.910000000000001,
0.915000000000001,0.920000000000001,0.925000000000001,0.930000000000001,
0.935000000000001,0.940000000000001,0.941429844438041),.UNSPECIFIED.)
CURVE()
GEOMETRIC_REPRESENTATION_ITEM()
RATIONAL_B_SPLINE_CURVE((1.,1.,1.,1.,1.,1.,1.,1.,1.,1.,1.,1.,1.,1.,1.,1.,
1.,1.,1.,1.,1.,1.,1.,1.,1.,1.,1.,1.,1.,1.,1.,1.,1.,1.,1.,1.,1.,1.,1.,1.,
1.,1.,1.,1.,1.,1.,1.,1.,1.,1.,1.,1.,1.,1.,1.,1.,1.,1.,1.,1.,1.,1.,1.,1.,
1.,1.,1.,1.,1.,1.,1.,1.,1.,1.,1.,1.,1.,1.,1.,1.,1.,1.,1.,1.,1.,1.,1.,1.,
1.,1.,1.,1.,1.,1.,1.,1.,1.,1.,1.,1.,1.,1.,1.,1.,1.,1.,1.,1.,1.,1.,1.,1.,
1.,1.,1.,1.,1.,1.,1.,1.,1.,1.,1.,1.,1.,1.,1.,1.,1.,1.,1.,1.,1.,1.,1.,1.,
1.,1.,1.,1.,1.,1.,1.,1.,1.,1.,1.,1.,1.,1.,1.,1.,1.,1.,1.,1.,1.,1.,1.,1.,
1.,1.,1.,1.,1.,1.,1.,1.,1.,1.,1.,1.,1.,1.,1.,1.,1.,1.,1.,1.,1.,1.,1.,1.,
1.,1.,1.,1.,1.,1.,1.,1.,1.,1.))
REPRESENTATION_ITEM('')
);
#606=(
BOUNDED_CURVE()
B_SPLINE_CURVE(5,(#140829,#140830,#140831,#140832,#140833,#140834,#140835,
#140836,#140837,#140838,#140839,#140840,#140841,#140842,#140843,#140844,
#140845,#140846,#140847,#140848,#140849,#140850,#140851,#140852,#140853,
#140854,#140855,#140856,#140857,#140858,#140859,#140860,#140861,#140862,
#140863,#140864,#140865,#140866,#140867,#140868,#140869,#140870,#140871,
#140872,#140873,#140874,#140875,#140876,#140877,#140878,#140879,#140880,
#140881,#140882,#140883,#140884,#140885,#140886,#140887,#140888,#140889,
#140890,#140891,#140892,#140893,#140894,#140895,#140896,#140897,#140898,
#140899,#140900,#140901,#140902,#140903,#140904,#140905,#140906,#140907,
#140908,#140909,#140910,#140911,#140912,#140913,#140914,#140915,#140916,
#140917,#140918,#140919,#140920,#140921,#140922,#140923,#140924,#140925,
#140926,#140927,#140928,#140929,#140930,#140931,#140932,#140933,#140934,
#140935,#140936,#140937,#140938,#140939,#140940,#140941,#140942,#140943,
#140944,#140945,#140946,#140947,#140948,#140949,#140950,#140951,#140952,
#140953,#140954,#140955,#140956,#140957,#140958,#140959,#140960,#140961,
#140962,#140963,#140964,#140965,#140966,#140967,#140968,#140969,#140970,
#140971,#140972,#140973,#140974,#140975,#140976,#140977,#140978,#140979,
#140980,#140981,#140982,#140983,#140984,#140985,#140986,#140987,#140988,
#140989,#140990,#140991,#140992,#140993,#140994,#140995,#140996,#140997,
#140998,#140999,#141000,#141001,#141002,#141003,#141004,#141005,#141006,
#141007,#141008,#141009,#141010,#141011,#141012,#141013,#141014,#141015,
#141016,#141017,#141018,#141019,#141020,#141021,#141022),.UNSPECIFIED.,
 .F.,.F.)
B_SPLINE_CURVE_WITH_KNOTS((6,1,1,1,1,1,1,1,1,1,1,1,1,1,1,1,1,1,1,1,1,1,
1,1,1,1,1,1,1,1,1,1,1,1,1,1,1,1,1,1,1,1,1,1,1,1,1,1,1,1,1,1,1,1,1,1,1,1,
1,1,1,1,1,1,1,1,1,1,1,1,1,1,1,1,1,1,1,1,1,1,1,1,1,1,1,1,1,1,1,1,1,1,1,1,
1,1,1,1,1,1,1,1,1,1,1,1,1,1,1,1,1,1,1,1,1,1,1,1,1,1,1,1,1,1,1,1,1,1,1,1,
1,1,1,1,1,1,1,1,1,1,1,1,1,1,1,1,1,1,1,1,1,1,1,1,1,1,1,1,1,1,1,1,1,1,1,1,
1,1,1,1,1,1,1,1,1,1,1,1,1,1,1,1,1,1,1,1,1,1,1,6),(-0.941429844438037,-0.940000000000001,
-0.935000000000001,-0.930000000000001,-0.925000000000001,-0.920000000000001,
-0.915000000000001,-0.910000000000001,-0.905000000000001,-0.900000000000001,
-0.895000000000001,-0.890000000000001,-0.885000000000001,-0.880000000000001,
-0.875000000000001,-0.870000000000001,-0.865000000000001,-0.860000000000001,
-0.855000000000001,-0.850000000000001,-0.845000000000001,-0.840000000000001,
-0.835000000000001,-0.830000000000001,-0.825000000000001,-0.820000000000001,
-0.815000000000001,-0.810000000000001,-0.805000000000001,-0.800000000000001,
-0.795000000000001,-0.790000000000001,-0.785000000000001,-0.780000000000001,
-0.775000000000001,-0.770000000000001,-0.765000000000001,-0.760000000000001,
-0.755000000000001,-0.750000000000001,-0.745000000000001,-0.740000000000001,
-0.735000000000001,-0.730000000000001,-0.725000000000001,-0.720000000000001,
-0.715000000000001,-0.710000000000001,-0.705000000000001,-0.700000000000001,
-0.695000000000001,-0.690000000000001,-0.685,-0.68,-0.675,-0.67,-0.665,
-0.66,-0.655,-0.65,-0.645,-0.64,-0.635,-0.63,-0.625,-0.62,-0.615,-0.61,
-0.605,-0.6,-0.595,-0.59,-0.585,-0.58,-0.575,-0.57,-0.565,-0.56,-0.555,
-0.55,-0.545,-0.54,-0.535,-0.53,-0.525,-0.52,-0.515,-0.51,-0.505,-0.5,-0.495,
-0.49,-0.485,-0.48,-0.475,-0.47,-0.465,-0.46,-0.455,-0.45,-0.445,-0.44,
-0.435,-0.43,-0.425,-0.42,-0.415,-0.41,-0.405,-0.4,-0.395,-0.39,-0.385,
-0.38,-0.375,-0.37,-0.365,-0.36,-0.355,-0.35,-0.345,-0.34,-0.335,-0.33,
-0.325,-0.32,-0.315,-0.31,-0.305,-0.3,-0.295,-0.29,-0.285,-0.28,-0.275,
-0.27,-0.265,-0.26,-0.255,-0.25,-0.245,-0.24,-0.235,-0.23,-0.225,-0.22,
-0.215,-0.21,-0.205,-0.2,-0.195,-0.19,-0.185,-0.18,-0.175,-0.17,-0.165,
-0.16,-0.155,-0.15,-0.145,-0.14,-0.135,-0.13,-0.125,-0.12,-0.115,-0.11,
-0.105,-0.1,-0.095,-0.09,-0.085,-0.08,-0.075,-0.07,-0.065,-0.06,-0.055,
-0.05,-0.045,-0.04,-0.035,-0.03,-0.025,-0.02,-0.015,-0.01,-0.005,0.),
 .UNSPECIFIED.)
CURVE()
GEOMETRIC_REPRESENTATION_ITEM()
RATIONAL_B_SPLINE_CURVE((1.,1.,1.,1.,1.,1.,1.,1.,1.,1.,1.,1.,1.,1.,1.,1.,
1.,1.,1.,1.,1.,1.,1.,1.,1.,1.,1.,1.,1.,1.,1.,1.,1.,1.,1.,1.,1.,1.,1.,1.,
1.,1.,1.,1.,1.,1.,1.,1.,1.,1.,1.,1.,1.,1.,1.,1.,1.,1.,1.,1.,1.,1.,1.,1.,
1.,1.,1.,1.,1.,1.,1.,1.,1.,1.,1.,1.,1.,1.,1.,1.,1.,1.,1.,1.,1.,1.,1.,1.,
1.,1.,1.,1.,1.,1.,1.,1.,1.,1.,1.,1.,1.,1.,1.,1.,1.,1.,1.,1.,1.,1.,1.,1.,
1.,1.,1.,1.,1.,1.,1.,1.,1.,1.,1.,1.,1.,1.,1.,1.,1.,1.,1.,1.,1.,1.,1.,1.,
1.,1.,1.,1.,1.,1.,1.,1.,1.,1.,1.,1.,1.,1.,1.,1.,1.,1.,1.,1.,1.,1.,1.,1.,
1.,1.,1.,1.,1.,1.,1.,1.,1.,1.,1.,1.,1.,1.,1.,1.,1.,1.,1.,1.,1.,1.,1.,1.,
1.,1.,1.,1.,1.,1.,1.,1.,1.,1.))
REPRESENTATION_ITEM('')
);
#607=(
BOUNDED_CURVE()
B_SPLINE_CURVE(5,(#141434,#141435,#141436,#141437,#141438,#141439,#141440,
#141441,#141442,#141443,#141444,#141445,#141446,#141447,#141448,#141449,
#141450,#141451,#141452,#141453,#141454,#141455,#141456,#141457,#141458,
#141459,#141460,#141461,#141462,#141463,#141464,#141465,#141466,#141467,
#141468,#141469,#141470,#141471,#141472,#141473,#141474,#141475,#141476,
#141477,#141478,#141479,#141480,#141481,#141482,#141483,#141484,#141485,
#141486,#141487,#141488,#141489,#141490,#141491,#141492,#141493,#141494,
#141495,#141496,#141497,#141498,#141499,#141500,#141501,#141502,#141503,
#141504,#141505,#141506,#141507,#141508,#141509,#141510,#141511,#141512,
#141513,#141514,#141515,#141516,#141517,#141518,#141519,#141520,#141521,
#141522,#141523,#141524,#141525,#141526,#141527,#141528,#141529,#141530,
#141531,#141532,#141533,#141534,#141535,#141536,#141537,#141538,#141539,
#141540,#141541,#141542,#141543,#141544,#141545,#141546,#141547,#141548,
#141549,#141550,#141551,#141552,#141553,#141554,#141555,#141556,#141557,
#141558,#141559,#141560,#141561,#141562,#141563,#141564,#141565,#141566,
#141567,#141568,#141569,#141570,#141571,#141572,#141573,#141574,#141575,
#141576,#141577,#141578,#141579,#141580,#141581,#141582,#141583,#141584,
#141585,#141586,#141587,#141588,#141589,#141590,#141591,#141592,#141593,
#141594,#141595,#141596,#141597,#141598,#141599,#141600,#141601,#141602,
#141603,#141604,#141605,#141606,#141607,#141608,#141609,#141610,#141611,
#141612,#141613,#141614,#141615,#141616,#141617,#141618,#141619,#141620,
#141621,#141622,#141623,#141624,#141625,#141626,#141627),.UNSPECIFIED.,
 .F.,.F.)
B_SPLINE_CURVE_WITH_KNOTS((6,1,1,1,1,1,1,1,1,1,1,1,1,1,1,1,1,1,1,1,1,1,
1,1,1,1,1,1,1,1,1,1,1,1,1,1,1,1,1,1,1,1,1,1,1,1,1,1,1,1,1,1,1,1,1,1,1,1,
1,1,1,1,1,1,1,1,1,1,1,1,1,1,1,1,1,1,1,1,1,1,1,1,1,1,1,1,1,1,1,1,1,1,1,1,
1,1,1,1,1,1,1,1,1,1,1,1,1,1,1,1,1,1,1,1,1,1,1,1,1,1,1,1,1,1,1,1,1,1,1,1,
1,1,1,1,1,1,1,1,1,1,1,1,1,1,1,1,1,1,1,1,1,1,1,1,1,1,1,1,1,1,1,1,1,1,1,1,
1,1,1,1,1,1,1,1,1,1,1,1,1,1,1,1,1,1,1,1,1,1,1,6),(0.,0.005,0.01,0.015,0.02,
0.025,0.03,0.035,0.04,0.045,0.05,0.055,0.06,0.065,0.07,0.075,0.08,0.085,
0.09,0.095,0.1,0.105,0.11,0.115,0.12,0.125,0.13,0.135,0.14,0.145,0.15,0.155,
0.16,0.165,0.17,0.175,0.18,0.185,0.19,0.195,0.2,0.205,0.21,0.215,0.22,0.225,
0.23,0.235,0.24,0.245,0.25,0.255,0.26,0.265,0.27,0.275,0.28,0.285,0.29,
0.295,0.3,0.305,0.31,0.315,0.32,0.325,0.33,0.335,0.34,0.345,0.35,0.355,
0.36,0.365,0.37,0.375,0.38,0.385,0.39,0.395,0.4,0.405,0.41,0.415,0.42,0.425,
0.43,0.435,0.44,0.445,0.45,0.455,0.46,0.465,0.47,0.475,0.48,0.485,0.49,
0.495,0.5,0.505,0.51,0.515,0.52,0.525,0.53,0.535,0.54,0.545,0.55,0.555,
0.56,0.565,0.57,0.575,0.58,0.585,0.59,0.595,0.6,0.605,0.61,0.615,0.62,0.625,
0.63,0.635,0.64,0.645,0.65,0.655,0.66,0.665,0.67,0.675,0.68,0.685,0.690000000000001,
0.695000000000001,0.700000000000001,0.705000000000001,0.710000000000001,
0.715000000000001,0.720000000000001,0.725000000000001,0.730000000000001,
0.735000000000001,0.740000000000001,0.745000000000001,0.750000000000001,
0.755000000000001,0.760000000000001,0.765000000000001,0.770000000000001,
0.775000000000001,0.780000000000001,0.785000000000001,0.790000000000001,
0.795000000000001,0.800000000000001,0.805000000000001,0.810000000000001,
0.815000000000001,0.820000000000001,0.825000000000001,0.830000000000001,
0.835000000000001,0.840000000000001,0.845000000000001,0.850000000000001,
0.855000000000001,0.860000000000001,0.865000000000001,0.870000000000001,
0.875000000000001,0.880000000000001,0.885000000000001,0.890000000000001,
0.895000000000001,0.900000000000001,0.905000000000001,0.910000000000001,
0.915000000000001,0.920000000000001,0.925000000000001,0.930000000000001,
0.935000000000001,0.940000000000001,0.941429844438043),.UNSPECIFIED.)
CURVE()
GEOMETRIC_REPRESENTATION_ITEM()
RATIONAL_B_SPLINE_CURVE((1.,1.,1.,1.,1.,1.,1.,1.,1.,1.,1.,1.,1.,1.,1.,1.,
1.,1.,1.,1.,1.,1.,1.,1.,1.,1.,1.,1.,1.,1.,1.,1.,1.,1.,1.,1.,1.,1.,1.,1.,
1.,1.,1.,1.,1.,1.,1.,1.,1.,1.,1.,1.,1.,1.,1.,1.,1.,1.,1.,1.,1.,1.,1.,1.,
1.,1.,1.,1.,1.,1.,1.,1.,1.,1.,1.,1.,1.,1.,1.,1.,1.,1.,1.,1.,1.,1.,1.,1.,
1.,1.,1.,1.,1.,1.,1.,1.,1.,1.,1.,1.,1.,1.,1.,1.,1.,1.,1.,1.,1.,1.,1.,1.,
1.,1.,1.,1.,1.,1.,1.,1.,1.,1.,1.,1.,1.,1.,1.,1.,1.,1.,1.,1.,1.,1.,1.,1.,
1.,1.,1.,1.,1.,1.,1.,1.,1.,1.,1.,1.,1.,1.,1.,1.,1.,1.,1.,1.,1.,1.,1.,1.,
1.,1.,1.,1.,1.,1.,1.,1.,1.,1.,1.,1.,1.,1.,1.,1.,1.,1.,1.,1.,1.,1.,1.,1.,
1.,1.,1.,1.,1.,1.,1.,1.,1.,1.))
REPRESENTATION_ITEM('')
);
#608=(
BOUNDED_CURVE()
B_SPLINE_CURVE(5,(#141630,#141631,#141632,#141633,#141634,#141635,#141636,
#141637,#141638,#141639,#141640,#141641,#141642,#141643,#141644,#141645,
#141646,#141647,#141648,#141649,#141650,#141651,#141652,#141653,#141654,
#141655,#141656,#141657,#141658,#141659,#141660,#141661,#141662,#141663,
#141664,#141665,#141666,#141667,#141668,#141669,#141670,#141671,#141672,
#141673,#141674,#141675,#141676,#141677,#141678,#141679,#141680,#141681,
#141682,#141683,#141684,#141685,#141686,#141687,#141688,#141689,#141690,
#141691,#141692,#141693,#141694,#141695,#141696,#141697,#141698,#141699,
#141700,#141701,#141702,#141703,#141704,#141705,#141706,#141707,#141708,
#141709,#141710,#141711,#141712,#141713,#141714,#141715,#141716,#141717,
#141718,#141719,#141720,#141721,#141722,#141723,#141724,#141725,#141726,
#141727,#141728,#141729,#141730,#141731,#141732,#141733,#141734,#141735,
#141736,#141737,#141738,#141739,#141740,#141741,#141742,#141743,#141744,
#141745,#141746,#141747,#141748,#141749,#141750,#141751,#141752,#141753,
#141754,#141755,#141756,#141757,#141758,#141759,#141760,#141761,#141762,
#141763,#141764,#141765,#141766,#141767,#141768,#141769,#141770,#141771,
#141772,#141773,#141774,#141775,#141776,#141777,#141778,#141779,#141780,
#141781,#141782,#141783,#141784,#141785,#141786,#141787,#141788,#141789,
#141790,#141791,#141792,#141793,#141794,#141795,#141796,#141797,#141798,
#141799,#141800,#141801,#141802,#141803,#141804,#141805,#141806,#141807,
#141808,#141809,#141810,#141811,#141812,#141813,#141814,#141815,#141816,
#141817,#141818,#141819,#141820,#141821,#141822,#141823),.UNSPECIFIED.,
 .F.,.F.)
B_SPLINE_CURVE_WITH_KNOTS((6,1,1,1,1,1,1,1,1,1,1,1,1,1,1,1,1,1,1,1,1,1,
1,1,1,1,1,1,1,1,1,1,1,1,1,1,1,1,1,1,1,1,1,1,1,1,1,1,1,1,1,1,1,1,1,1,1,1,
1,1,1,1,1,1,1,1,1,1,1,1,1,1,1,1,1,1,1,1,1,1,1,1,1,1,1,1,1,1,1,1,1,1,1,1,
1,1,1,1,1,1,1,1,1,1,1,1,1,1,1,1,1,1,1,1,1,1,1,1,1,1,1,1,1,1,1,1,1,1,1,1,
1,1,1,1,1,1,1,1,1,1,1,1,1,1,1,1,1,1,1,1,1,1,1,1,1,1,1,1,1,1,1,1,1,1,1,1,
1,1,1,1,1,1,1,1,1,1,1,1,1,1,1,1,1,1,1,1,1,1,1,6),(-0.941429844438047,-0.940000000000001,
-0.935000000000001,-0.930000000000001,-0.925000000000001,-0.920000000000001,
-0.915000000000001,-0.910000000000001,-0.905000000000001,-0.900000000000001,
-0.895000000000001,-0.890000000000001,-0.885000000000001,-0.880000000000001,
-0.875000000000001,-0.870000000000001,-0.865000000000001,-0.860000000000001,
-0.855000000000001,-0.850000000000001,-0.845000000000001,-0.840000000000001,
-0.835000000000001,-0.830000000000001,-0.825000000000001,-0.820000000000001,
-0.815000000000001,-0.810000000000001,-0.805000000000001,-0.800000000000001,
-0.795000000000001,-0.790000000000001,-0.785000000000001,-0.780000000000001,
-0.775000000000001,-0.770000000000001,-0.765000000000001,-0.760000000000001,
-0.755000000000001,-0.750000000000001,-0.745000000000001,-0.740000000000001,
-0.735000000000001,-0.730000000000001,-0.725000000000001,-0.720000000000001,
-0.715000000000001,-0.710000000000001,-0.705000000000001,-0.700000000000001,
-0.695000000000001,-0.690000000000001,-0.685,-0.68,-0.675,-0.67,-0.665,
-0.66,-0.655,-0.65,-0.645,-0.64,-0.635,-0.63,-0.625,-0.62,-0.615,-0.61,
-0.605,-0.6,-0.595,-0.59,-0.585,-0.58,-0.575,-0.57,-0.565,-0.56,-0.555,
-0.55,-0.545,-0.54,-0.535,-0.53,-0.525,-0.52,-0.515,-0.51,-0.505,-0.5,-0.495,
-0.49,-0.485,-0.48,-0.475,-0.47,-0.465,-0.46,-0.455,-0.45,-0.445,-0.44,
-0.435,-0.43,-0.425,-0.42,-0.415,-0.41,-0.405,-0.4,-0.395,-0.39,-0.385,
-0.38,-0.375,-0.37,-0.365,-0.36,-0.355,-0.35,-0.345,-0.34,-0.335,-0.33,
-0.325,-0.32,-0.315,-0.31,-0.305,-0.3,-0.295,-0.29,-0.285,-0.28,-0.275,
-0.27,-0.265,-0.26,-0.255,-0.25,-0.245,-0.24,-0.235,-0.23,-0.225,-0.22,
-0.215,-0.21,-0.205,-0.2,-0.195,-0.19,-0.185,-0.18,-0.175,-0.17,-0.165,
-0.16,-0.155,-0.15,-0.145,-0.14,-0.135,-0.13,-0.125,-0.12,-0.115,-0.11,
-0.105,-0.1,-0.095,-0.09,-0.085,-0.08,-0.075,-0.07,-0.065,-0.06,-0.055,
-0.05,-0.045,-0.04,-0.035,-0.03,-0.025,-0.02,-0.015,-0.01,-0.005,0.),
 .UNSPECIFIED.)
CURVE()
GEOMETRIC_REPRESENTATION_ITEM()
RATIONAL_B_SPLINE_CURVE((1.,1.,1.,1.,1.,1.,1.,1.,1.,1.,1.,1.,1.,1.,1.,1.,
1.,1.,1.,1.,1.,1.,1.,1.,1.,1.,1.,1.,1.,1.,1.,1.,1.,1.,1.,1.,1.,1.,1.,1.,
1.,1.,1.,1.,1.,1.,1.,1.,1.,1.,1.,1.,1.,1.,1.,1.,1.,1.,1.,1.,1.,1.,1.,1.,
1.,1.,1.,1.,1.,1.,1.,1.,1.,1.,1.,1.,1.,1.,1.,1.,1.,1.,1.,1.,1.,1.,1.,1.,
1.,1.,1.,1.,1.,1.,1.,1.,1.,1.,1.,1.,1.,1.,1.,1.,1.,1.,1.,1.,1.,1.,1.,1.,
1.,1.,1.,1.,1.,1.,1.,1.,1.,1.,1.,1.,1.,1.,1.,1.,1.,1.,1.,1.,1.,1.,1.,1.,
1.,1.,1.,1.,1.,1.,1.,1.,1.,1.,1.,1.,1.,1.,1.,1.,1.,1.,1.,1.,1.,1.,1.,1.,
1.,1.,1.,1.,1.,1.,1.,1.,1.,1.,1.,1.,1.,1.,1.,1.,1.,1.,1.,1.,1.,1.,1.,1.,
1.,1.,1.,1.,1.,1.,1.,1.,1.,1.))
REPRESENTATION_ITEM('')
);
#609=(
BOUNDED_CURVE()
B_SPLINE_CURVE(5,(#142235,#142236,#142237,#142238,#142239,#142240,#142241,
#142242,#142243,#142244,#142245,#142246,#142247,#142248,#142249,#142250,
#142251,#142252,#142253,#142254,#142255,#142256,#142257,#142258,#142259,
#142260,#142261,#142262,#142263,#142264,#142265,#142266,#142267,#142268,
#142269,#142270,#142271,#142272,#142273,#142274,#142275,#142276,#142277,
#142278,#142279,#142280,#142281,#142282,#142283,#142284,#142285,#142286,
#142287,#142288,#142289,#142290,#142291,#142292,#142293,#142294,#142295,
#142296,#142297,#142298,#142299,#142300,#142301,#142302,#142303,#142304,
#142305,#142306,#142307,#142308,#142309,#142310,#142311,#142312,#142313,
#142314,#142315,#142316,#142317,#142318,#142319,#142320,#142321,#142322,
#142323,#142324,#142325,#142326,#142327,#142328,#142329,#142330,#142331,
#142332,#142333,#142334,#142335,#142336,#142337,#142338,#142339,#142340,
#142341,#142342,#142343,#142344,#142345,#142346,#142347,#142348,#142349,
#142350,#142351,#142352,#142353,#142354,#142355,#142356,#142357,#142358,
#142359,#142360,#142361,#142362,#142363,#142364,#142365,#142366,#142367,
#142368,#142369,#142370,#142371,#142372,#142373,#142374,#142375,#142376,
#142377,#142378,#142379,#142380,#142381,#142382,#142383,#142384,#142385,
#142386,#142387,#142388,#142389,#142390,#142391,#142392,#142393,#142394,
#142395,#142396,#142397,#142398,#142399,#142400,#142401,#142402,#142403,
#142404,#142405,#142406,#142407,#142408,#142409,#142410,#142411,#142412,
#142413,#142414,#142415,#142416,#142417,#142418,#142419,#142420,#142421,
#142422,#142423,#142424,#142425,#142426,#142427,#142428),.UNSPECIFIED.,
 .F.,.F.)
B_SPLINE_CURVE_WITH_KNOTS((6,1,1,1,1,1,1,1,1,1,1,1,1,1,1,1,1,1,1,1,1,1,
1,1,1,1,1,1,1,1,1,1,1,1,1,1,1,1,1,1,1,1,1,1,1,1,1,1,1,1,1,1,1,1,1,1,1,1,
1,1,1,1,1,1,1,1,1,1,1,1,1,1,1,1,1,1,1,1,1,1,1,1,1,1,1,1,1,1,1,1,1,1,1,1,
1,1,1,1,1,1,1,1,1,1,1,1,1,1,1,1,1,1,1,1,1,1,1,1,1,1,1,1,1,1,1,1,1,1,1,1,
1,1,1,1,1,1,1,1,1,1,1,1,1,1,1,1,1,1,1,1,1,1,1,1,1,1,1,1,1,1,1,1,1,1,1,1,
1,1,1,1,1,1,1,1,1,1,1,1,1,1,1,1,1,1,1,1,1,1,1,6),(0.,0.005,0.01,0.015,0.02,
0.025,0.03,0.035,0.04,0.045,0.05,0.055,0.06,0.065,0.07,0.075,0.08,0.085,
0.09,0.095,0.1,0.105,0.11,0.115,0.12,0.125,0.13,0.135,0.14,0.145,0.15,0.155,
0.16,0.165,0.17,0.175,0.18,0.185,0.19,0.195,0.2,0.205,0.21,0.215,0.22,0.225,
0.23,0.235,0.24,0.245,0.25,0.255,0.26,0.265,0.27,0.275,0.28,0.285,0.29,
0.295,0.3,0.305,0.31,0.315,0.32,0.325,0.33,0.335,0.34,0.345,0.35,0.355,
0.36,0.365,0.37,0.375,0.38,0.385,0.39,0.395,0.4,0.405,0.41,0.415,0.42,0.425,
0.43,0.435,0.44,0.445,0.45,0.455,0.46,0.465,0.47,0.475,0.48,0.485,0.49,
0.495,0.5,0.505,0.51,0.515,0.52,0.525,0.53,0.535,0.54,0.545,0.55,0.555,
0.56,0.565,0.57,0.575,0.58,0.585,0.59,0.595,0.6,0.605,0.61,0.615,0.62,0.625,
0.63,0.635,0.64,0.645,0.65,0.655,0.66,0.665,0.67,0.675,0.68,0.685,0.690000000000001,
0.695000000000001,0.700000000000001,0.705000000000001,0.710000000000001,
0.715000000000001,0.720000000000001,0.725000000000001,0.730000000000001,
0.735000000000001,0.740000000000001,0.745000000000001,0.750000000000001,
0.755000000000001,0.760000000000001,0.765000000000001,0.770000000000001,
0.775000000000001,0.780000000000001,0.785000000000001,0.790000000000001,
0.795000000000001,0.800000000000001,0.805000000000001,0.810000000000001,
0.815000000000001,0.820000000000001,0.825000000000001,0.830000000000001,
0.835000000000001,0.840000000000001,0.845000000000001,0.850000000000001,
0.855000000000001,0.860000000000001,0.865000000000001,0.870000000000001,
0.875000000000001,0.880000000000001,0.885000000000001,0.890000000000001,
0.895000000000001,0.900000000000001,0.905000000000001,0.910000000000001,
0.915000000000001,0.920000000000001,0.925000000000001,0.930000000000001,
0.935000000000001,0.940000000000001,0.94142984443807),.UNSPECIFIED.)
CURVE()
GEOMETRIC_REPRESENTATION_ITEM()
RATIONAL_B_SPLINE_CURVE((1.,1.,1.,1.,1.,1.,1.,1.,1.,1.,1.,1.,1.,1.,1.,1.,
1.,1.,1.,1.,1.,1.,1.,1.,1.,1.,1.,1.,1.,1.,1.,1.,1.,1.,1.,1.,1.,1.,1.,1.,
1.,1.,1.,1.,1.,1.,1.,1.,1.,1.,1.,1.,1.,1.,1.,1.,1.,1.,1.,1.,1.,1.,1.,1.,
1.,1.,1.,1.,1.,1.,1.,1.,1.,1.,1.,1.,1.,1.,1.,1.,1.,1.,1.,1.,1.,1.,1.,1.,
1.,1.,1.,1.,1.,1.,1.,1.,1.,1.,1.,1.,1.,1.,1.,1.,1.,1.,1.,1.,1.,1.,1.,1.,
1.,1.,1.,1.,1.,1.,1.,1.,1.,1.,1.,1.,1.,1.,1.,1.,1.,1.,1.,1.,1.,1.,1.,1.,
1.,1.,1.,1.,1.,1.,1.,1.,1.,1.,1.,1.,1.,1.,1.,1.,1.,1.,1.,1.,1.,1.,1.,1.,
1.,1.,1.,1.,1.,1.,1.,1.,1.,1.,1.,1.,1.,1.,1.,1.,1.,1.,1.,1.,1.,1.,1.,1.,
1.,1.,1.,1.,1.,1.,1.,1.,1.,1.))
REPRESENTATION_ITEM('')
);
#610=(
BOUNDED_CURVE()
B_SPLINE_CURVE(5,(#142431,#142432,#142433,#142434,#142435,#142436,#142437,
#142438,#142439,#142440,#142441,#142442,#142443,#142444,#142445,#142446,
#142447,#142448,#142449,#142450,#142451,#142452,#142453,#142454,#142455,
#142456,#142457,#142458,#142459,#142460,#142461,#142462,#142463,#142464,
#142465,#142466,#142467,#142468,#142469,#142470,#142471,#142472,#142473,
#142474,#142475,#142476,#142477,#142478,#142479,#142480,#142481,#142482,
#142483,#142484,#142485,#142486,#142487,#142488,#142489,#142490,#142491,
#142492,#142493,#142494,#142495,#142496,#142497,#142498,#142499,#142500,
#142501,#142502,#142503,#142504,#142505,#142506,#142507,#142508,#142509,
#142510,#142511,#142512,#142513,#142514,#142515,#142516,#142517,#142518,
#142519,#142520,#142521,#142522,#142523,#142524,#142525,#142526,#142527,
#142528,#142529,#142530,#142531,#142532,#142533,#142534,#142535,#142536,
#142537,#142538,#142539,#142540,#142541,#142542,#142543,#142544,#142545,
#142546,#142547,#142548,#142549,#142550,#142551,#142552,#142553,#142554,
#142555,#142556,#142557,#142558,#142559,#142560,#142561,#142562,#142563,
#142564,#142565,#142566,#142567,#142568,#142569,#142570,#142571,#142572,
#142573,#142574,#142575,#142576,#142577,#142578,#142579,#142580,#142581,
#142582,#142583,#142584,#142585,#142586,#142587,#142588,#142589,#142590,
#142591,#142592,#142593,#142594,#142595,#142596,#142597,#142598,#142599,
#142600,#142601,#142602,#142603,#142604,#142605,#142606,#142607,#142608,
#142609,#142610,#142611,#142612,#142613,#142614,#142615,#142616,#142617,
#142618,#142619,#142620,#142621,#142622,#142623,#142624),.UNSPECIFIED.,
 .F.,.F.)
B_SPLINE_CURVE_WITH_KNOTS((6,1,1,1,1,1,1,1,1,1,1,1,1,1,1,1,1,1,1,1,1,1,
1,1,1,1,1,1,1,1,1,1,1,1,1,1,1,1,1,1,1,1,1,1,1,1,1,1,1,1,1,1,1,1,1,1,1,1,
1,1,1,1,1,1,1,1,1,1,1,1,1,1,1,1,1,1,1,1,1,1,1,1,1,1,1,1,1,1,1,1,1,1,1,1,
1,1,1,1,1,1,1,1,1,1,1,1,1,1,1,1,1,1,1,1,1,1,1,1,1,1,1,1,1,1,1,1,1,1,1,1,
1,1,1,1,1,1,1,1,1,1,1,1,1,1,1,1,1,1,1,1,1,1,1,1,1,1,1,1,1,1,1,1,1,1,1,1,
1,1,1,1,1,1,1,1,1,1,1,1,1,1,1,1,1,1,1,1,1,1,1,6),(-0.94142984443807,-0.940000000000001,
-0.935000000000001,-0.930000000000001,-0.925000000000001,-0.920000000000001,
-0.915000000000001,-0.910000000000001,-0.905000000000001,-0.900000000000001,
-0.895000000000001,-0.890000000000001,-0.885000000000001,-0.880000000000001,
-0.875000000000001,-0.870000000000001,-0.865000000000001,-0.860000000000001,
-0.855000000000001,-0.850000000000001,-0.845000000000001,-0.840000000000001,
-0.835000000000001,-0.830000000000001,-0.825000000000001,-0.820000000000001,
-0.815000000000001,-0.810000000000001,-0.805000000000001,-0.800000000000001,
-0.795000000000001,-0.790000000000001,-0.785000000000001,-0.780000000000001,
-0.775000000000001,-0.770000000000001,-0.765000000000001,-0.760000000000001,
-0.755000000000001,-0.750000000000001,-0.745000000000001,-0.740000000000001,
-0.735000000000001,-0.730000000000001,-0.725000000000001,-0.720000000000001,
-0.715000000000001,-0.710000000000001,-0.705000000000001,-0.700000000000001,
-0.695000000000001,-0.690000000000001,-0.685,-0.68,-0.675,-0.67,-0.665,
-0.66,-0.655,-0.65,-0.645,-0.64,-0.635,-0.63,-0.625,-0.62,-0.615,-0.61,
-0.605,-0.6,-0.595,-0.59,-0.585,-0.58,-0.575,-0.57,-0.565,-0.56,-0.555,
-0.55,-0.545,-0.54,-0.535,-0.53,-0.525,-0.52,-0.515,-0.51,-0.505,-0.5,-0.495,
-0.49,-0.485,-0.48,-0.475,-0.47,-0.465,-0.46,-0.455,-0.45,-0.445,-0.44,
-0.435,-0.43,-0.425,-0.42,-0.415,-0.41,-0.405,-0.4,-0.395,-0.39,-0.385,
-0.38,-0.375,-0.37,-0.365,-0.36,-0.355,-0.35,-0.345,-0.34,-0.335,-0.33,
-0.325,-0.32,-0.315,-0.31,-0.305,-0.3,-0.295,-0.29,-0.285,-0.28,-0.275,
-0.27,-0.265,-0.26,-0.255,-0.25,-0.245,-0.24,-0.235,-0.23,-0.225,-0.22,
-0.215,-0.21,-0.205,-0.2,-0.195,-0.19,-0.185,-0.18,-0.175,-0.17,-0.165,
-0.16,-0.155,-0.15,-0.145,-0.14,-0.135,-0.13,-0.125,-0.12,-0.115,-0.11,
-0.105,-0.1,-0.095,-0.09,-0.085,-0.08,-0.075,-0.07,-0.065,-0.06,-0.055,
-0.05,-0.045,-0.04,-0.035,-0.03,-0.025,-0.02,-0.015,-0.01,-0.005,0.),
 .UNSPECIFIED.)
CURVE()
GEOMETRIC_REPRESENTATION_ITEM()
RATIONAL_B_SPLINE_CURVE((1.,1.,1.,1.,1.,1.,1.,1.,1.,1.,1.,1.,1.,1.,1.,1.,
1.,1.,1.,1.,1.,1.,1.,1.,1.,1.,1.,1.,1.,1.,1.,1.,1.,1.,1.,1.,1.,1.,1.,1.,
1.,1.,1.,1.,1.,1.,1.,1.,1.,1.,1.,1.,1.,1.,1.,1.,1.,1.,1.,1.,1.,1.,1.,1.,
1.,1.,1.,1.,1.,1.,1.,1.,1.,1.,1.,1.,1.,1.,1.,1.,1.,1.,1.,1.,1.,1.,1.,1.,
1.,1.,1.,1.,1.,1.,1.,1.,1.,1.,1.,1.,1.,1.,1.,1.,1.,1.,1.,1.,1.,1.,1.,1.,
1.,1.,1.,1.,1.,1.,1.,1.,1.,1.,1.,1.,1.,1.,1.,1.,1.,1.,1.,1.,1.,1.,1.,1.,
1.,1.,1.,1.,1.,1.,1.,1.,1.,1.,1.,1.,1.,1.,1.,1.,1.,1.,1.,1.,1.,1.,1.,1.,
1.,1.,1.,1.,1.,1.,1.,1.,1.,1.,1.,1.,1.,1.,1.,1.,1.,1.,1.,1.,1.,1.,1.,1.,
1.,1.,1.,1.,1.,1.,1.,1.,1.,1.))
REPRESENTATION_ITEM('')
);
#611=(
BOUNDED_CURVE()
B_SPLINE_CURVE(5,(#143036,#143037,#143038,#143039,#143040,#143041,#143042,
#143043,#143044,#143045,#143046,#143047,#143048,#143049,#143050,#143051,
#143052,#143053,#143054,#143055,#143056,#143057,#143058,#143059,#143060,
#143061,#143062,#143063,#143064,#143065,#143066,#143067,#143068,#143069,
#143070,#143071,#143072,#143073,#143074,#143075,#143076,#143077,#143078,
#143079,#143080,#143081,#143082,#143083,#143084,#143085,#143086,#143087,
#143088,#143089,#143090,#143091,#143092,#143093,#143094,#143095,#143096,
#143097,#143098,#143099,#143100,#143101,#143102,#143103,#143104,#143105,
#143106,#143107,#143108,#143109,#143110,#143111,#143112,#143113,#143114,
#143115,#143116,#143117,#143118,#143119,#143120,#143121,#143122,#143123,
#143124,#143125,#143126,#143127,#143128,#143129,#143130,#143131,#143132,
#143133,#143134,#143135,#143136,#143137,#143138,#143139,#143140,#143141,
#143142,#143143,#143144,#143145,#143146,#143147,#143148,#143149,#143150,
#143151,#143152,#143153,#143154,#143155,#143156,#143157,#143158,#143159,
#143160,#143161,#143162,#143163,#143164,#143165,#143166,#143167,#143168,
#143169,#143170,#143171,#143172,#143173,#143174,#143175,#143176,#143177,
#143178,#143179,#143180,#143181,#143182,#143183,#143184,#143185,#143186,
#143187,#143188,#143189,#143190,#143191,#143192,#143193,#143194,#143195,
#143196,#143197,#143198,#143199,#143200,#143201,#143202,#143203,#143204,
#143205,#143206,#143207,#143208,#143209,#143210,#143211,#143212,#143213,
#143214,#143215,#143216,#143217,#143218,#143219,#143220,#143221,#143222,
#143223,#143224,#143225,#143226,#143227,#143228,#143229),.UNSPECIFIED.,
 .F.,.F.)
B_SPLINE_CURVE_WITH_KNOTS((6,1,1,1,1,1,1,1,1,1,1,1,1,1,1,1,1,1,1,1,1,1,
1,1,1,1,1,1,1,1,1,1,1,1,1,1,1,1,1,1,1,1,1,1,1,1,1,1,1,1,1,1,1,1,1,1,1,1,
1,1,1,1,1,1,1,1,1,1,1,1,1,1,1,1,1,1,1,1,1,1,1,1,1,1,1,1,1,1,1,1,1,1,1,1,
1,1,1,1,1,1,1,1,1,1,1,1,1,1,1,1,1,1,1,1,1,1,1,1,1,1,1,1,1,1,1,1,1,1,1,1,
1,1,1,1,1,1,1,1,1,1,1,1,1,1,1,1,1,1,1,1,1,1,1,1,1,1,1,1,1,1,1,1,1,1,1,1,
1,1,1,1,1,1,1,1,1,1,1,1,1,1,1,1,1,1,1,1,1,1,1,6),(0.,0.005,0.01,0.015,0.02,
0.025,0.03,0.035,0.04,0.045,0.05,0.055,0.06,0.065,0.07,0.075,0.08,0.085,
0.09,0.095,0.1,0.105,0.11,0.115,0.12,0.125,0.13,0.135,0.14,0.145,0.15,0.155,
0.16,0.165,0.17,0.175,0.18,0.185,0.19,0.195,0.2,0.205,0.21,0.215,0.22,0.225,
0.23,0.235,0.24,0.245,0.25,0.255,0.26,0.265,0.27,0.275,0.28,0.285,0.29,
0.295,0.3,0.305,0.31,0.315,0.32,0.325,0.33,0.335,0.34,0.345,0.35,0.355,
0.36,0.365,0.37,0.375,0.38,0.385,0.39,0.395,0.4,0.405,0.41,0.415,0.42,0.425,
0.43,0.435,0.44,0.445,0.45,0.455,0.46,0.465,0.47,0.475,0.48,0.485,0.49,
0.495,0.5,0.505,0.51,0.515,0.52,0.525,0.53,0.535,0.54,0.545,0.55,0.555,
0.56,0.565,0.57,0.575,0.58,0.585,0.59,0.595,0.6,0.605,0.61,0.615,0.62,0.625,
0.63,0.635,0.64,0.645,0.65,0.655,0.66,0.665,0.67,0.675,0.68,0.685,0.690000000000001,
0.695000000000001,0.700000000000001,0.705000000000001,0.710000000000001,
0.715000000000001,0.720000000000001,0.725000000000001,0.730000000000001,
0.735000000000001,0.740000000000001,0.745000000000001,0.750000000000001,
0.755000000000001,0.760000000000001,0.765000000000001,0.770000000000001,
0.775000000000001,0.780000000000001,0.785000000000001,0.790000000000001,
0.795000000000001,0.800000000000001,0.805000000000001,0.810000000000001,
0.815000000000001,0.820000000000001,0.825000000000001,0.830000000000001,
0.835000000000001,0.840000000000001,0.845000000000001,0.850000000000001,
0.855000000000001,0.860000000000001,0.865000000000001,0.870000000000001,
0.875000000000001,0.880000000000001,0.885000000000001,0.890000000000001,
0.895000000000001,0.900000000000001,0.905000000000001,0.910000000000001,
0.915000000000001,0.920000000000001,0.925000000000001,0.930000000000001,
0.935000000000001,0.940000000000001,0.941429844437991),.UNSPECIFIED.)
CURVE()
GEOMETRIC_REPRESENTATION_ITEM()
RATIONAL_B_SPLINE_CURVE((1.,1.,1.,1.,1.,1.,1.,1.,1.,1.,1.,1.,1.,1.,1.,1.,
1.,1.,1.,1.,1.,1.,1.,1.,1.,1.,1.,1.,1.,1.,1.,1.,1.,1.,1.,1.,1.,1.,1.,1.,
1.,1.,1.,1.,1.,1.,1.,1.,1.,1.,1.,1.,1.,1.,1.,1.,1.,1.,1.,1.,1.,1.,1.,1.,
1.,1.,1.,1.,1.,1.,1.,1.,1.,1.,1.,1.,1.,1.,1.,1.,1.,1.,1.,1.,1.,1.,1.,1.,
1.,1.,1.,1.,1.,1.,1.,1.,1.,1.,1.,1.,1.,1.,1.,1.,1.,1.,1.,1.,1.,1.,1.,1.,
1.,1.,1.,1.,1.,1.,1.,1.,1.,1.,1.,1.,1.,1.,1.,1.,1.,1.,1.,1.,1.,1.,1.,1.,
1.,1.,1.,1.,1.,1.,1.,1.,1.,1.,1.,1.,1.,1.,1.,1.,1.,1.,1.,1.,1.,1.,1.,1.,
1.,1.,1.,1.,1.,1.,1.,1.,1.,1.,1.,1.,1.,1.,1.,1.,1.,1.,1.,1.,1.,1.,1.,1.,
1.,1.,1.,1.,1.,1.,1.,1.,1.,1.))
REPRESENTATION_ITEM('')
);
#612=(
BOUNDED_CURVE()
B_SPLINE_CURVE(5,(#143232,#143233,#143234,#143235,#143236,#143237,#143238,
#143239,#143240,#143241,#143242,#143243,#143244,#143245,#143246,#143247,
#143248,#143249,#143250,#143251,#143252,#143253,#143254,#143255,#143256,
#143257,#143258,#143259,#143260,#143261,#143262,#143263,#143264,#143265,
#143266,#143267,#143268,#143269,#143270,#143271,#143272,#143273,#143274,
#143275,#143276,#143277,#143278,#143279,#143280,#143281,#143282,#143283,
#143284,#143285,#143286,#143287,#143288,#143289,#143290,#143291,#143292,
#143293,#143294,#143295,#143296,#143297,#143298,#143299,#143300,#143301,
#143302,#143303,#143304,#143305,#143306,#143307,#143308,#143309,#143310,
#143311,#143312,#143313,#143314,#143315,#143316,#143317,#143318,#143319,
#143320,#143321,#143322,#143323,#143324,#143325,#143326,#143327,#143328,
#143329,#143330,#143331,#143332,#143333,#143334,#143335,#143336,#143337,
#143338,#143339,#143340,#143341,#143342,#143343,#143344,#143345,#143346,
#143347,#143348,#143349,#143350,#143351,#143352,#143353,#143354,#143355,
#143356,#143357,#143358,#143359,#143360,#143361,#143362,#143363,#143364,
#143365,#143366,#143367,#143368,#143369,#143370,#143371,#143372,#143373,
#143374,#143375,#143376,#143377,#143378,#143379,#143380,#143381,#143382,
#143383,#143384,#143385,#143386,#143387,#143388,#143389,#143390,#143391,
#143392,#143393,#143394,#143395,#143396,#143397,#143398,#143399,#143400,
#143401,#143402,#143403,#143404,#143405,#143406,#143407,#143408,#143409,
#143410,#143411,#143412,#143413,#143414,#143415,#143416,#143417,#143418,
#143419,#143420,#143421,#143422,#143423,#143424,#143425),.UNSPECIFIED.,
 .F.,.F.)
B_SPLINE_CURVE_WITH_KNOTS((6,1,1,1,1,1,1,1,1,1,1,1,1,1,1,1,1,1,1,1,1,1,
1,1,1,1,1,1,1,1,1,1,1,1,1,1,1,1,1,1,1,1,1,1,1,1,1,1,1,1,1,1,1,1,1,1,1,1,
1,1,1,1,1,1,1,1,1,1,1,1,1,1,1,1,1,1,1,1,1,1,1,1,1,1,1,1,1,1,1,1,1,1,1,1,
1,1,1,1,1,1,1,1,1,1,1,1,1,1,1,1,1,1,1,1,1,1,1,1,1,1,1,1,1,1,1,1,1,1,1,1,
1,1,1,1,1,1,1,1,1,1,1,1,1,1,1,1,1,1,1,1,1,1,1,1,1,1,1,1,1,1,1,1,1,1,1,1,
1,1,1,1,1,1,1,1,1,1,1,1,1,1,1,1,1,1,1,1,1,1,1,6),(-0.94142984443798,-0.940000000000001,
-0.935000000000001,-0.930000000000001,-0.925000000000001,-0.920000000000001,
-0.915000000000001,-0.910000000000001,-0.905000000000001,-0.900000000000001,
-0.895000000000001,-0.890000000000001,-0.885000000000001,-0.880000000000001,
-0.875000000000001,-0.870000000000001,-0.865000000000001,-0.860000000000001,
-0.855000000000001,-0.850000000000001,-0.845000000000001,-0.840000000000001,
-0.835000000000001,-0.830000000000001,-0.825000000000001,-0.820000000000001,
-0.815000000000001,-0.810000000000001,-0.805000000000001,-0.800000000000001,
-0.795000000000001,-0.790000000000001,-0.785000000000001,-0.780000000000001,
-0.775000000000001,-0.770000000000001,-0.765000000000001,-0.760000000000001,
-0.755000000000001,-0.750000000000001,-0.745000000000001,-0.740000000000001,
-0.735000000000001,-0.730000000000001,-0.725000000000001,-0.720000000000001,
-0.715000000000001,-0.710000000000001,-0.705000000000001,-0.700000000000001,
-0.695000000000001,-0.690000000000001,-0.685,-0.68,-0.675,-0.67,-0.665,
-0.66,-0.655,-0.65,-0.645,-0.64,-0.635,-0.63,-0.625,-0.62,-0.615,-0.61,
-0.605,-0.6,-0.595,-0.59,-0.585,-0.58,-0.575,-0.57,-0.565,-0.56,-0.555,
-0.55,-0.545,-0.54,-0.535,-0.53,-0.525,-0.52,-0.515,-0.51,-0.505,-0.5,-0.495,
-0.49,-0.485,-0.48,-0.475,-0.47,-0.465,-0.46,-0.455,-0.45,-0.445,-0.44,
-0.435,-0.43,-0.425,-0.42,-0.415,-0.41,-0.405,-0.4,-0.395,-0.39,-0.385,
-0.38,-0.375,-0.37,-0.365,-0.36,-0.355,-0.35,-0.345,-0.34,-0.335,-0.33,
-0.325,-0.32,-0.315,-0.31,-0.305,-0.3,-0.295,-0.29,-0.285,-0.28,-0.275,
-0.27,-0.265,-0.26,-0.255,-0.25,-0.245,-0.24,-0.235,-0.23,-0.225,-0.22,
-0.215,-0.21,-0.205,-0.2,-0.195,-0.19,-0.185,-0.18,-0.175,-0.17,-0.165,
-0.16,-0.155,-0.15,-0.145,-0.14,-0.135,-0.13,-0.125,-0.12,-0.115,-0.11,
-0.105,-0.1,-0.095,-0.09,-0.085,-0.08,-0.075,-0.07,-0.065,-0.06,-0.055,
-0.05,-0.045,-0.04,-0.035,-0.03,-0.025,-0.02,-0.015,-0.01,-0.005,0.),
 .UNSPECIFIED.)
CURVE()
GEOMETRIC_REPRESENTATION_ITEM()
RATIONAL_B_SPLINE_CURVE((1.,1.,1.,1.,1.,1.,1.,1.,1.,1.,1.,1.,1.,1.,1.,1.,
1.,1.,1.,1.,1.,1.,1.,1.,1.,1.,1.,1.,1.,1.,1.,1.,1.,1.,1.,1.,1.,1.,1.,1.,
1.,1.,1.,1.,1.,1.,1.,1.,1.,1.,1.,1.,1.,1.,1.,1.,1.,1.,1.,1.,1.,1.,1.,1.,
1.,1.,1.,1.,1.,1.,1.,1.,1.,1.,1.,1.,1.,1.,1.,1.,1.,1.,1.,1.,1.,1.,1.,1.,
1.,1.,1.,1.,1.,1.,1.,1.,1.,1.,1.,1.,1.,1.,1.,1.,1.,1.,1.,1.,1.,1.,1.,1.,
1.,1.,1.,1.,1.,1.,1.,1.,1.,1.,1.,1.,1.,1.,1.,1.,1.,1.,1.,1.,1.,1.,1.,1.,
1.,1.,1.,1.,1.,1.,1.,1.,1.,1.,1.,1.,1.,1.,1.,1.,1.,1.,1.,1.,1.,1.,1.,1.,
1.,1.,1.,1.,1.,1.,1.,1.,1.,1.,1.,1.,1.,1.,1.,1.,1.,1.,1.,1.,1.,1.,1.,1.,
1.,1.,1.,1.,1.,1.,1.,1.,1.,1.))
REPRESENTATION_ITEM('')
);
#613=(
BOUNDED_CURVE()
B_SPLINE_CURVE(5,(#143837,#143838,#143839,#143840,#143841,#143842,#143843,
#143844,#143845,#143846,#143847,#143848,#143849,#143850,#143851,#143852,
#143853,#143854,#143855,#143856,#143857,#143858,#143859,#143860,#143861,
#143862,#143863,#143864,#143865,#143866,#143867,#143868,#143869,#143870,
#143871,#143872,#143873,#143874,#143875,#143876,#143877,#143878,#143879,
#143880,#143881,#143882,#143883,#143884,#143885,#143886,#143887,#143888,
#143889,#143890,#143891,#143892,#143893,#143894,#143895,#143896,#143897,
#143898,#143899,#143900,#143901,#143902,#143903,#143904,#143905,#143906,
#143907,#143908,#143909,#143910,#143911,#143912,#143913,#143914,#143915,
#143916,#143917,#143918,#143919,#143920,#143921,#143922,#143923,#143924,
#143925,#143926,#143927,#143928,#143929,#143930,#143931,#143932,#143933,
#143934,#143935,#143936,#143937,#143938,#143939,#143940,#143941,#143942,
#143943,#143944,#143945,#143946,#143947,#143948,#143949,#143950,#143951,
#143952,#143953,#143954,#143955,#143956,#143957,#143958,#143959,#143960,
#143961,#143962,#143963,#143964,#143965,#143966,#143967,#143968,#143969,
#143970,#143971,#143972,#143973,#143974,#143975,#143976,#143977,#143978,
#143979,#143980,#143981,#143982,#143983,#143984,#143985,#143986,#143987,
#143988,#143989,#143990,#143991,#143992,#143993,#143994,#143995,#143996,
#143997,#143998,#143999,#144000,#144001,#144002,#144003,#144004,#144005,
#144006,#144007,#144008,#144009,#144010,#144011,#144012,#144013,#144014,
#144015,#144016,#144017,#144018,#144019,#144020,#144021,#144022,#144023,
#144024,#144025,#144026,#144027,#144028,#144029,#144030),.UNSPECIFIED.,
 .F.,.F.)
B_SPLINE_CURVE_WITH_KNOTS((6,1,1,1,1,1,1,1,1,1,1,1,1,1,1,1,1,1,1,1,1,1,
1,1,1,1,1,1,1,1,1,1,1,1,1,1,1,1,1,1,1,1,1,1,1,1,1,1,1,1,1,1,1,1,1,1,1,1,
1,1,1,1,1,1,1,1,1,1,1,1,1,1,1,1,1,1,1,1,1,1,1,1,1,1,1,1,1,1,1,1,1,1,1,1,
1,1,1,1,1,1,1,1,1,1,1,1,1,1,1,1,1,1,1,1,1,1,1,1,1,1,1,1,1,1,1,1,1,1,1,1,
1,1,1,1,1,1,1,1,1,1,1,1,1,1,1,1,1,1,1,1,1,1,1,1,1,1,1,1,1,1,1,1,1,1,1,1,
1,1,1,1,1,1,1,1,1,1,1,1,1,1,1,1,1,1,1,1,1,1,1,6),(0.,0.005,0.01,0.015,0.02,
0.025,0.03,0.035,0.04,0.045,0.05,0.055,0.06,0.065,0.07,0.075,0.08,0.085,
0.09,0.095,0.1,0.105,0.11,0.115,0.12,0.125,0.13,0.135,0.14,0.145,0.15,0.155,
0.16,0.165,0.17,0.175,0.18,0.185,0.19,0.195,0.2,0.205,0.21,0.215,0.22,0.225,
0.23,0.235,0.24,0.245,0.25,0.255,0.26,0.265,0.27,0.275,0.28,0.285,0.29,
0.295,0.3,0.305,0.31,0.315,0.32,0.325,0.33,0.335,0.34,0.345,0.35,0.355,
0.36,0.365,0.37,0.375,0.38,0.385,0.39,0.395,0.4,0.405,0.41,0.415,0.42,0.425,
0.43,0.435,0.44,0.445,0.45,0.455,0.46,0.465,0.47,0.475,0.48,0.485,0.49,
0.495,0.5,0.505,0.51,0.515,0.52,0.525,0.53,0.535,0.54,0.545,0.55,0.555,
0.56,0.565,0.57,0.575,0.58,0.585,0.59,0.595,0.6,0.605,0.61,0.615,0.62,0.625,
0.63,0.635,0.64,0.645,0.65,0.655,0.66,0.665,0.67,0.675,0.68,0.685,0.690000000000001,
0.695000000000001,0.700000000000001,0.705000000000001,0.710000000000001,
0.715000000000001,0.720000000000001,0.725000000000001,0.730000000000001,
0.735000000000001,0.740000000000001,0.745000000000001,0.750000000000001,
0.755000000000001,0.760000000000001,0.765000000000001,0.770000000000001,
0.775000000000001,0.780000000000001,0.785000000000001,0.790000000000001,
0.795000000000001,0.800000000000001,0.805000000000001,0.810000000000001,
0.815000000000001,0.820000000000001,0.825000000000001,0.830000000000001,
0.835000000000001,0.840000000000001,0.845000000000001,0.850000000000001,
0.855000000000001,0.860000000000001,0.865000000000001,0.870000000000001,
0.875000000000001,0.880000000000001,0.885000000000001,0.890000000000001,
0.895000000000001,0.900000000000001,0.905000000000001,0.910000000000001,
0.915000000000001,0.920000000000001,0.925000000000001,0.930000000000001,
0.935000000000001,0.940000000000001,0.941429844438089),.UNSPECIFIED.)
CURVE()
GEOMETRIC_REPRESENTATION_ITEM()
RATIONAL_B_SPLINE_CURVE((1.,1.,1.,1.,1.,1.,1.,1.,1.,1.,1.,1.,1.,1.,1.,1.,
1.,1.,1.,1.,1.,1.,1.,1.,1.,1.,1.,1.,1.,1.,1.,1.,1.,1.,1.,1.,1.,1.,1.,1.,
1.,1.,1.,1.,1.,1.,1.,1.,1.,1.,1.,1.,1.,1.,1.,1.,1.,1.,1.,1.,1.,1.,1.,1.,
1.,1.,1.,1.,1.,1.,1.,1.,1.,1.,1.,1.,1.,1.,1.,1.,1.,1.,1.,1.,1.,1.,1.,1.,
1.,1.,1.,1.,1.,1.,1.,1.,1.,1.,1.,1.,1.,1.,1.,1.,1.,1.,1.,1.,1.,1.,1.,1.,
1.,1.,1.,1.,1.,1.,1.,1.,1.,1.,1.,1.,1.,1.,1.,1.,1.,1.,1.,1.,1.,1.,1.,1.,
1.,1.,1.,1.,1.,1.,1.,1.,1.,1.,1.,1.,1.,1.,1.,1.,1.,1.,1.,1.,1.,1.,1.,1.,
1.,1.,1.,1.,1.,1.,1.,1.,1.,1.,1.,1.,1.,1.,1.,1.,1.,1.,1.,1.,1.,1.,1.,1.,
1.,1.,1.,1.,1.,1.,1.,1.,1.,1.))
REPRESENTATION_ITEM('')
);
#614=(
BOUNDED_CURVE()
B_SPLINE_CURVE(5,(#144033,#144034,#144035,#144036,#144037,#144038,#144039,
#144040,#144041,#144042,#144043,#144044,#144045,#144046,#144047,#144048,
#144049,#144050,#144051,#144052,#144053,#144054,#144055,#144056,#144057,
#144058,#144059,#144060,#144061,#144062,#144063,#144064,#144065,#144066,
#144067,#144068,#144069,#144070,#144071,#144072,#144073,#144074,#144075,
#144076,#144077,#144078,#144079,#144080,#144081,#144082,#144083,#144084,
#144085,#144086,#144087,#144088,#144089,#144090,#144091,#144092,#144093,
#144094,#144095,#144096,#144097,#144098,#144099,#144100,#144101,#144102,
#144103,#144104,#144105,#144106,#144107,#144108,#144109,#144110,#144111,
#144112,#144113,#144114,#144115,#144116,#144117,#144118,#144119,#144120,
#144121,#144122,#144123,#144124,#144125,#144126,#144127,#144128,#144129,
#144130,#144131,#144132,#144133,#144134,#144135,#144136,#144137,#144138,
#144139,#144140,#144141,#144142,#144143,#144144,#144145,#144146,#144147,
#144148,#144149,#144150,#144151,#144152,#144153,#144154,#144155,#144156,
#144157,#144158,#144159,#144160,#144161,#144162,#144163,#144164,#144165,
#144166,#144167,#144168,#144169,#144170,#144171,#144172,#144173,#144174,
#144175,#144176,#144177,#144178,#144179,#144180,#144181,#144182,#144183,
#144184,#144185,#144186,#144187,#144188,#144189,#144190,#144191,#144192,
#144193,#144194,#144195,#144196,#144197,#144198,#144199,#144200,#144201,
#144202,#144203,#144204,#144205,#144206,#144207,#144208,#144209,#144210,
#144211,#144212,#144213,#144214,#144215,#144216,#144217,#144218,#144219,
#144220,#144221,#144222,#144223,#144224,#144225,#144226),.UNSPECIFIED.,
 .F.,.F.)
B_SPLINE_CURVE_WITH_KNOTS((6,1,1,1,1,1,1,1,1,1,1,1,1,1,1,1,1,1,1,1,1,1,
1,1,1,1,1,1,1,1,1,1,1,1,1,1,1,1,1,1,1,1,1,1,1,1,1,1,1,1,1,1,1,1,1,1,1,1,
1,1,1,1,1,1,1,1,1,1,1,1,1,1,1,1,1,1,1,1,1,1,1,1,1,1,1,1,1,1,1,1,1,1,1,1,
1,1,1,1,1,1,1,1,1,1,1,1,1,1,1,1,1,1,1,1,1,1,1,1,1,1,1,1,1,1,1,1,1,1,1,1,
1,1,1,1,1,1,1,1,1,1,1,1,1,1,1,1,1,1,1,1,1,1,1,1,1,1,1,1,1,1,1,1,1,1,1,1,
1,1,1,1,1,1,1,1,1,1,1,1,1,1,1,1,1,1,1,1,1,1,1,6),(-0.941429844438087,-0.940000000000001,
-0.935000000000001,-0.930000000000001,-0.925000000000001,-0.920000000000001,
-0.915000000000001,-0.910000000000001,-0.905000000000001,-0.900000000000001,
-0.895000000000001,-0.890000000000001,-0.885000000000001,-0.880000000000001,
-0.875000000000001,-0.870000000000001,-0.865000000000001,-0.860000000000001,
-0.855000000000001,-0.850000000000001,-0.845000000000001,-0.840000000000001,
-0.835000000000001,-0.830000000000001,-0.825000000000001,-0.820000000000001,
-0.815000000000001,-0.810000000000001,-0.805000000000001,-0.800000000000001,
-0.795000000000001,-0.790000000000001,-0.785000000000001,-0.780000000000001,
-0.775000000000001,-0.770000000000001,-0.765000000000001,-0.760000000000001,
-0.755000000000001,-0.750000000000001,-0.745000000000001,-0.740000000000001,
-0.735000000000001,-0.730000000000001,-0.725000000000001,-0.720000000000001,
-0.715000000000001,-0.710000000000001,-0.705000000000001,-0.700000000000001,
-0.695000000000001,-0.690000000000001,-0.685,-0.68,-0.675,-0.67,-0.665,
-0.66,-0.655,-0.65,-0.645,-0.64,-0.635,-0.63,-0.625,-0.62,-0.615,-0.61,
-0.605,-0.6,-0.595,-0.59,-0.585,-0.58,-0.575,-0.57,-0.565,-0.56,-0.555,
-0.55,-0.545,-0.54,-0.535,-0.53,-0.525,-0.52,-0.515,-0.51,-0.505,-0.5,-0.495,
-0.49,-0.485,-0.48,-0.475,-0.47,-0.465,-0.46,-0.455,-0.45,-0.445,-0.44,
-0.435,-0.43,-0.425,-0.42,-0.415,-0.41,-0.405,-0.4,-0.395,-0.39,-0.385,
-0.38,-0.375,-0.37,-0.365,-0.36,-0.355,-0.35,-0.345,-0.34,-0.335,-0.33,
-0.325,-0.32,-0.315,-0.31,-0.305,-0.3,-0.295,-0.29,-0.285,-0.28,-0.275,
-0.27,-0.265,-0.26,-0.255,-0.25,-0.245,-0.24,-0.235,-0.23,-0.225,-0.22,
-0.215,-0.21,-0.205,-0.2,-0.195,-0.19,-0.185,-0.18,-0.175,-0.17,-0.165,
-0.16,-0.155,-0.15,-0.145,-0.14,-0.135,-0.13,-0.125,-0.12,-0.115,-0.11,
-0.105,-0.1,-0.095,-0.09,-0.085,-0.08,-0.075,-0.07,-0.065,-0.06,-0.055,
-0.05,-0.045,-0.04,-0.035,-0.03,-0.025,-0.02,-0.015,-0.01,-0.005,0.),
 .UNSPECIFIED.)
CURVE()
GEOMETRIC_REPRESENTATION_ITEM()
RATIONAL_B_SPLINE_CURVE((1.,1.,1.,1.,1.,1.,1.,1.,1.,1.,1.,1.,1.,1.,1.,1.,
1.,1.,1.,1.,1.,1.,1.,1.,1.,1.,1.,1.,1.,1.,1.,1.,1.,1.,1.,1.,1.,1.,1.,1.,
1.,1.,1.,1.,1.,1.,1.,1.,1.,1.,1.,1.,1.,1.,1.,1.,1.,1.,1.,1.,1.,1.,1.,1.,
1.,1.,1.,1.,1.,1.,1.,1.,1.,1.,1.,1.,1.,1.,1.,1.,1.,1.,1.,1.,1.,1.,1.,1.,
1.,1.,1.,1.,1.,1.,1.,1.,1.,1.,1.,1.,1.,1.,1.,1.,1.,1.,1.,1.,1.,1.,1.,1.,
1.,1.,1.,1.,1.,1.,1.,1.,1.,1.,1.,1.,1.,1.,1.,1.,1.,1.,1.,1.,1.,1.,1.,1.,
1.,1.,1.,1.,1.,1.,1.,1.,1.,1.,1.,1.,1.,1.,1.,1.,1.,1.,1.,1.,1.,1.,1.,1.,
1.,1.,1.,1.,1.,1.,1.,1.,1.,1.,1.,1.,1.,1.,1.,1.,1.,1.,1.,1.,1.,1.,1.,1.,
1.,1.,1.,1.,1.,1.,1.,1.,1.,1.))
REPRESENTATION_ITEM('')
);
#615=(
BOUNDED_CURVE()
B_SPLINE_CURVE(5,(#144638,#144639,#144640,#144641,#144642,#144643,#144644,
#144645,#144646,#144647,#144648,#144649,#144650,#144651,#144652,#144653,
#144654,#144655,#144656,#144657,#144658,#144659,#144660,#144661,#144662,
#144663,#144664,#144665,#144666,#144667,#144668,#144669,#144670,#144671,
#144672,#144673,#144674,#144675,#144676,#144677,#144678,#144679,#144680,
#144681,#144682,#144683,#144684,#144685,#144686,#144687,#144688,#144689,
#144690,#144691,#144692,#144693,#144694,#144695,#144696,#144697,#144698,
#144699,#144700,#144701,#144702,#144703,#144704,#144705,#144706,#144707,
#144708,#144709,#144710,#144711,#144712,#144713,#144714,#144715,#144716,
#144717,#144718,#144719,#144720,#144721,#144722,#144723,#144724,#144725,
#144726,#144727,#144728,#144729,#144730,#144731,#144732,#144733,#144734,
#144735,#144736,#144737,#144738,#144739,#144740,#144741,#144742,#144743,
#144744,#144745,#144746,#144747,#144748,#144749,#144750,#144751,#144752,
#144753,#144754,#144755,#144756,#144757,#144758,#144759,#144760,#144761,
#144762,#144763,#144764,#144765,#144766,#144767,#144768,#144769,#144770,
#144771,#144772,#144773,#144774,#144775,#144776,#144777,#144778,#144779,
#144780,#144781,#144782,#144783,#144784,#144785,#144786,#144787,#144788,
#144789,#144790,#144791,#144792,#144793,#144794,#144795,#144796,#144797,
#144798,#144799,#144800,#144801,#144802,#144803,#144804,#144805,#144806,
#144807,#144808,#144809,#144810,#144811,#144812,#144813,#144814,#144815,
#144816,#144817,#144818,#144819,#144820,#144821,#144822,#144823,#144824,
#144825,#144826,#144827,#144828,#144829,#144830,#144831),.UNSPECIFIED.,
 .F.,.F.)
B_SPLINE_CURVE_WITH_KNOTS((6,1,1,1,1,1,1,1,1,1,1,1,1,1,1,1,1,1,1,1,1,1,
1,1,1,1,1,1,1,1,1,1,1,1,1,1,1,1,1,1,1,1,1,1,1,1,1,1,1,1,1,1,1,1,1,1,1,1,
1,1,1,1,1,1,1,1,1,1,1,1,1,1,1,1,1,1,1,1,1,1,1,1,1,1,1,1,1,1,1,1,1,1,1,1,
1,1,1,1,1,1,1,1,1,1,1,1,1,1,1,1,1,1,1,1,1,1,1,1,1,1,1,1,1,1,1,1,1,1,1,1,
1,1,1,1,1,1,1,1,1,1,1,1,1,1,1,1,1,1,1,1,1,1,1,1,1,1,1,1,1,1,1,1,1,1,1,1,
1,1,1,1,1,1,1,1,1,1,1,1,1,1,1,1,1,1,1,1,1,1,1,6),(0.,0.005,0.01,0.015,0.02,
0.025,0.03,0.035,0.04,0.045,0.05,0.055,0.06,0.065,0.07,0.075,0.08,0.085,
0.09,0.095,0.1,0.105,0.11,0.115,0.12,0.125,0.13,0.135,0.14,0.145,0.15,0.155,
0.16,0.165,0.17,0.175,0.18,0.185,0.19,0.195,0.2,0.205,0.21,0.215,0.22,0.225,
0.23,0.235,0.24,0.245,0.25,0.255,0.26,0.265,0.27,0.275,0.28,0.285,0.29,
0.295,0.3,0.305,0.31,0.315,0.32,0.325,0.33,0.335,0.34,0.345,0.35,0.355,
0.36,0.365,0.37,0.375,0.38,0.385,0.39,0.395,0.4,0.405,0.41,0.415,0.42,0.425,
0.43,0.435,0.44,0.445,0.45,0.455,0.46,0.465,0.47,0.475,0.48,0.485,0.49,
0.495,0.5,0.505,0.51,0.515,0.52,0.525,0.53,0.535,0.54,0.545,0.55,0.555,
0.56,0.565,0.57,0.575,0.58,0.585,0.59,0.595,0.6,0.605,0.61,0.615,0.62,0.625,
0.63,0.635,0.64,0.645,0.65,0.655,0.66,0.665,0.67,0.675,0.68,0.685,0.690000000000001,
0.695000000000001,0.700000000000001,0.705000000000001,0.710000000000001,
0.715000000000001,0.720000000000001,0.725000000000001,0.730000000000001,
0.735000000000001,0.740000000000001,0.745000000000001,0.750000000000001,
0.755000000000001,0.760000000000001,0.765000000000001,0.770000000000001,
0.775000000000001,0.780000000000001,0.785000000000001,0.790000000000001,
0.795000000000001,0.800000000000001,0.805000000000001,0.810000000000001,
0.815000000000001,0.820000000000001,0.825000000000001,0.830000000000001,
0.835000000000001,0.840000000000001,0.845000000000001,0.850000000000001,
0.855000000000001,0.860000000000001,0.865000000000001,0.870000000000001,
0.875000000000001,0.880000000000001,0.885000000000001,0.890000000000001,
0.895000000000001,0.900000000000001,0.905000000000001,0.910000000000001,
0.915000000000001,0.920000000000001,0.925000000000001,0.930000000000001,
0.935000000000001,0.940000000000001,0.94142984443808),.UNSPECIFIED.)
CURVE()
GEOMETRIC_REPRESENTATION_ITEM()
RATIONAL_B_SPLINE_CURVE((1.,1.,1.,1.,1.,1.,1.,1.,1.,1.,1.,1.,1.,1.,1.,1.,
1.,1.,1.,1.,1.,1.,1.,1.,1.,1.,1.,1.,1.,1.,1.,1.,1.,1.,1.,1.,1.,1.,1.,1.,
1.,1.,1.,1.,1.,1.,1.,1.,1.,1.,1.,1.,1.,1.,1.,1.,1.,1.,1.,1.,1.,1.,1.,1.,
1.,1.,1.,1.,1.,1.,1.,1.,1.,1.,1.,1.,1.,1.,1.,1.,1.,1.,1.,1.,1.,1.,1.,1.,
1.,1.,1.,1.,1.,1.,1.,1.,1.,1.,1.,1.,1.,1.,1.,1.,1.,1.,1.,1.,1.,1.,1.,1.,
1.,1.,1.,1.,1.,1.,1.,1.,1.,1.,1.,1.,1.,1.,1.,1.,1.,1.,1.,1.,1.,1.,1.,1.,
1.,1.,1.,1.,1.,1.,1.,1.,1.,1.,1.,1.,1.,1.,1.,1.,1.,1.,1.,1.,1.,1.,1.,1.,
1.,1.,1.,1.,1.,1.,1.,1.,1.,1.,1.,1.,1.,1.,1.,1.,1.,1.,1.,1.,1.,1.,1.,1.,
1.,1.,1.,1.,1.,1.,1.,1.,1.,1.))
REPRESENTATION_ITEM('')
);
#616=(
BOUNDED_CURVE()
B_SPLINE_CURVE(5,(#144834,#144835,#144836,#144837,#144838,#144839,#144840,
#144841,#144842,#144843,#144844,#144845,#144846,#144847,#144848,#144849,
#144850,#144851,#144852,#144853,#144854,#144855,#144856,#144857,#144858,
#144859,#144860,#144861,#144862,#144863,#144864,#144865,#144866,#144867,
#144868,#144869,#144870,#144871,#144872,#144873,#144874,#144875,#144876,
#144877,#144878,#144879,#144880,#144881,#144882,#144883,#144884,#144885,
#144886,#144887,#144888,#144889,#144890,#144891,#144892,#144893,#144894,
#144895,#144896,#144897,#144898,#144899,#144900,#144901,#144902,#144903,
#144904,#144905,#144906,#144907,#144908,#144909,#144910,#144911,#144912,
#144913,#144914,#144915,#144916,#144917,#144918,#144919,#144920,#144921,
#144922,#144923,#144924,#144925,#144926,#144927,#144928,#144929,#144930,
#144931,#144932,#144933,#144934,#144935,#144936,#144937,#144938,#144939,
#144940,#144941,#144942,#144943,#144944,#144945,#144946,#144947,#144948,
#144949,#144950,#144951,#144952,#144953,#144954,#144955,#144956,#144957,
#144958,#144959,#144960,#144961,#144962,#144963,#144964,#144965,#144966,
#144967,#144968,#144969,#144970,#144971,#144972,#144973,#144974,#144975,
#144976,#144977,#144978,#144979,#144980,#144981,#144982,#144983,#144984,
#144985,#144986,#144987,#144988,#144989,#144990,#144991,#144992,#144993,
#144994,#144995,#144996,#144997,#144998,#144999,#145000,#145001,#145002,
#145003,#145004,#145005,#145006,#145007,#145008,#145009,#145010,#145011,
#145012,#145013,#145014,#145015,#145016,#145017,#145018,#145019,#145020,
#145021,#145022,#145023,#145024,#145025,#145026,#145027),.UNSPECIFIED.,
 .F.,.F.)
B_SPLINE_CURVE_WITH_KNOTS((6,1,1,1,1,1,1,1,1,1,1,1,1,1,1,1,1,1,1,1,1,1,
1,1,1,1,1,1,1,1,1,1,1,1,1,1,1,1,1,1,1,1,1,1,1,1,1,1,1,1,1,1,1,1,1,1,1,1,
1,1,1,1,1,1,1,1,1,1,1,1,1,1,1,1,1,1,1,1,1,1,1,1,1,1,1,1,1,1,1,1,1,1,1,1,
1,1,1,1,1,1,1,1,1,1,1,1,1,1,1,1,1,1,1,1,1,1,1,1,1,1,1,1,1,1,1,1,1,1,1,1,
1,1,1,1,1,1,1,1,1,1,1,1,1,1,1,1,1,1,1,1,1,1,1,1,1,1,1,1,1,1,1,1,1,1,1,1,
1,1,1,1,1,1,1,1,1,1,1,1,1,1,1,1,1,1,1,1,1,1,1,6),(-0.941429844438077,-0.940000000000001,
-0.935000000000001,-0.930000000000001,-0.925000000000001,-0.920000000000001,
-0.915000000000001,-0.910000000000001,-0.905000000000001,-0.900000000000001,
-0.895000000000001,-0.890000000000001,-0.885000000000001,-0.880000000000001,
-0.875000000000001,-0.870000000000001,-0.865000000000001,-0.860000000000001,
-0.855000000000001,-0.850000000000001,-0.845000000000001,-0.840000000000001,
-0.835000000000001,-0.830000000000001,-0.825000000000001,-0.820000000000001,
-0.815000000000001,-0.810000000000001,-0.805000000000001,-0.800000000000001,
-0.795000000000001,-0.790000000000001,-0.785000000000001,-0.780000000000001,
-0.775000000000001,-0.770000000000001,-0.765000000000001,-0.760000000000001,
-0.755000000000001,-0.750000000000001,-0.745000000000001,-0.740000000000001,
-0.735000000000001,-0.730000000000001,-0.725000000000001,-0.720000000000001,
-0.715000000000001,-0.710000000000001,-0.705000000000001,-0.700000000000001,
-0.695000000000001,-0.690000000000001,-0.685,-0.68,-0.675,-0.67,-0.665,
-0.66,-0.655,-0.65,-0.645,-0.64,-0.635,-0.63,-0.625,-0.62,-0.615,-0.61,
-0.605,-0.6,-0.595,-0.59,-0.585,-0.58,-0.575,-0.57,-0.565,-0.56,-0.555,
-0.55,-0.545,-0.54,-0.535,-0.53,-0.525,-0.52,-0.515,-0.51,-0.505,-0.5,-0.495,
-0.49,-0.485,-0.48,-0.475,-0.47,-0.465,-0.46,-0.455,-0.45,-0.445,-0.44,
-0.435,-0.43,-0.425,-0.42,-0.415,-0.41,-0.405,-0.4,-0.395,-0.39,-0.385,
-0.38,-0.375,-0.37,-0.365,-0.36,-0.355,-0.35,-0.345,-0.34,-0.335,-0.33,
-0.325,-0.32,-0.315,-0.31,-0.305,-0.3,-0.295,-0.29,-0.285,-0.28,-0.275,
-0.27,-0.265,-0.26,-0.255,-0.25,-0.245,-0.24,-0.235,-0.23,-0.225,-0.22,
-0.215,-0.21,-0.205,-0.2,-0.195,-0.19,-0.185,-0.18,-0.175,-0.17,-0.165,
-0.16,-0.155,-0.15,-0.145,-0.14,-0.135,-0.13,-0.125,-0.12,-0.115,-0.11,
-0.105,-0.1,-0.095,-0.09,-0.085,-0.08,-0.075,-0.07,-0.065,-0.06,-0.055,
-0.05,-0.045,-0.04,-0.035,-0.03,-0.025,-0.02,-0.015,-0.01,-0.005,0.),
 .UNSPECIFIED.)
CURVE()
GEOMETRIC_REPRESENTATION_ITEM()
RATIONAL_B_SPLINE_CURVE((1.,1.,1.,1.,1.,1.,1.,1.,1.,1.,1.,1.,1.,1.,1.,1.,
1.,1.,1.,1.,1.,1.,1.,1.,1.,1.,1.,1.,1.,1.,1.,1.,1.,1.,1.,1.,1.,1.,1.,1.,
1.,1.,1.,1.,1.,1.,1.,1.,1.,1.,1.,1.,1.,1.,1.,1.,1.,1.,1.,1.,1.,1.,1.,1.,
1.,1.,1.,1.,1.,1.,1.,1.,1.,1.,1.,1.,1.,1.,1.,1.,1.,1.,1.,1.,1.,1.,1.,1.,
1.,1.,1.,1.,1.,1.,1.,1.,1.,1.,1.,1.,1.,1.,1.,1.,1.,1.,1.,1.,1.,1.,1.,1.,
1.,1.,1.,1.,1.,1.,1.,1.,1.,1.,1.,1.,1.,1.,1.,1.,1.,1.,1.,1.,1.,1.,1.,1.,
1.,1.,1.,1.,1.,1.,1.,1.,1.,1.,1.,1.,1.,1.,1.,1.,1.,1.,1.,1.,1.,1.,1.,1.,
1.,1.,1.,1.,1.,1.,1.,1.,1.,1.,1.,1.,1.,1.,1.,1.,1.,1.,1.,1.,1.,1.,1.,1.,
1.,1.,1.,1.,1.,1.,1.,1.,1.,1.))
REPRESENTATION_ITEM('')
);
#617=(
BOUNDED_CURVE()
B_SPLINE_CURVE(5,(#145439,#145440,#145441,#145442,#145443,#145444,#145445,
#145446,#145447,#145448,#145449,#145450,#145451,#145452,#145453,#145454,
#145455,#145456,#145457,#145458,#145459,#145460,#145461,#145462,#145463,
#145464,#145465,#145466,#145467,#145468,#145469,#145470,#145471,#145472,
#145473,#145474,#145475,#145476,#145477,#145478,#145479,#145480,#145481,
#145482,#145483,#145484,#145485,#145486,#145487,#145488,#145489,#145490,
#145491,#145492,#145493,#145494,#145495,#145496,#145497,#145498,#145499,
#145500,#145501,#145502,#145503,#145504,#145505,#145506,#145507,#145508,
#145509,#145510,#145511,#145512,#145513,#145514,#145515,#145516,#145517,
#145518,#145519,#145520,#145521,#145522,#145523,#145524,#145525,#145526,
#145527,#145528,#145529,#145530,#145531,#145532,#145533,#145534,#145535,
#145536,#145537,#145538,#145539,#145540,#145541,#145542,#145543,#145544,
#145545,#145546,#145547,#145548,#145549,#145550,#145551,#145552,#145553,
#145554,#145555,#145556,#145557,#145558,#145559,#145560,#145561,#145562,
#145563,#145564,#145565,#145566,#145567,#145568,#145569,#145570,#145571,
#145572,#145573,#145574,#145575,#145576,#145577,#145578,#145579,#145580,
#145581,#145582,#145583,#145584,#145585,#145586,#145587,#145588,#145589,
#145590,#145591,#145592,#145593,#145594,#145595,#145596,#145597,#145598,
#145599,#145600,#145601,#145602,#145603,#145604,#145605,#145606,#145607,
#145608,#145609,#145610,#145611,#145612,#145613,#145614,#145615,#145616,
#145617,#145618,#145619,#145620,#145621,#145622,#145623,#145624,#145625,
#145626,#145627,#145628,#145629,#145630,#145631,#145632),.UNSPECIFIED.,
 .F.,.F.)
B_SPLINE_CURVE_WITH_KNOTS((6,1,1,1,1,1,1,1,1,1,1,1,1,1,1,1,1,1,1,1,1,1,
1,1,1,1,1,1,1,1,1,1,1,1,1,1,1,1,1,1,1,1,1,1,1,1,1,1,1,1,1,1,1,1,1,1,1,1,
1,1,1,1,1,1,1,1,1,1,1,1,1,1,1,1,1,1,1,1,1,1,1,1,1,1,1,1,1,1,1,1,1,1,1,1,
1,1,1,1,1,1,1,1,1,1,1,1,1,1,1,1,1,1,1,1,1,1,1,1,1,1,1,1,1,1,1,1,1,1,1,1,
1,1,1,1,1,1,1,1,1,1,1,1,1,1,1,1,1,1,1,1,1,1,1,1,1,1,1,1,1,1,1,1,1,1,1,1,
1,1,1,1,1,1,1,1,1,1,1,1,1,1,1,1,1,1,1,1,1,1,1,6),(0.,0.005,0.01,0.015,0.02,
0.025,0.03,0.035,0.04,0.045,0.05,0.055,0.06,0.065,0.07,0.075,0.08,0.085,
0.09,0.095,0.1,0.105,0.11,0.115,0.12,0.125,0.13,0.135,0.14,0.145,0.15,0.155,
0.16,0.165,0.17,0.175,0.18,0.185,0.19,0.195,0.2,0.205,0.21,0.215,0.22,0.225,
0.23,0.235,0.24,0.245,0.25,0.255,0.26,0.265,0.27,0.275,0.28,0.285,0.29,
0.295,0.3,0.305,0.31,0.315,0.32,0.325,0.33,0.335,0.34,0.345,0.35,0.355,
0.36,0.365,0.37,0.375,0.38,0.385,0.39,0.395,0.4,0.405,0.41,0.415,0.42,0.425,
0.43,0.435,0.44,0.445,0.45,0.455,0.46,0.465,0.47,0.475,0.48,0.485,0.49,
0.495,0.5,0.505,0.51,0.515,0.52,0.525,0.53,0.535,0.54,0.545,0.55,0.555,
0.56,0.565,0.57,0.575,0.58,0.585,0.59,0.595,0.6,0.605,0.61,0.615,0.62,0.625,
0.63,0.635,0.64,0.645,0.65,0.655,0.66,0.665,0.67,0.675,0.68,0.685,0.690000000000001,
0.695000000000001,0.700000000000001,0.705000000000001,0.710000000000001,
0.715000000000001,0.720000000000001,0.725000000000001,0.730000000000001,
0.735000000000001,0.740000000000001,0.745000000000001,0.750000000000001,
0.755000000000001,0.760000000000001,0.765000000000001,0.770000000000001,
0.775000000000001,0.780000000000001,0.785000000000001,0.790000000000001,
0.795000000000001,0.800000000000001,0.805000000000001,0.810000000000001,
0.815000000000001,0.820000000000001,0.825000000000001,0.830000000000001,
0.835000000000001,0.840000000000001,0.845000000000001,0.850000000000001,
0.855000000000001,0.860000000000001,0.865000000000001,0.870000000000001,
0.875000000000001,0.880000000000001,0.885000000000001,0.890000000000001,
0.895000000000001,0.900000000000001,0.905000000000001,0.910000000000001,
0.915000000000001,0.920000000000001,0.925000000000001,0.930000000000001,
0.935000000000001,0.940000000000001,0.941429844438071),.UNSPECIFIED.)
CURVE()
GEOMETRIC_REPRESENTATION_ITEM()
RATIONAL_B_SPLINE_CURVE((1.,1.,1.,1.,1.,1.,1.,1.,1.,1.,1.,1.,1.,1.,1.,1.,
1.,1.,1.,1.,1.,1.,1.,1.,1.,1.,1.,1.,1.,1.,1.,1.,1.,1.,1.,1.,1.,1.,1.,1.,
1.,1.,1.,1.,1.,1.,1.,1.,1.,1.,1.,1.,1.,1.,1.,1.,1.,1.,1.,1.,1.,1.,1.,1.,
1.,1.,1.,1.,1.,1.,1.,1.,1.,1.,1.,1.,1.,1.,1.,1.,1.,1.,1.,1.,1.,1.,1.,1.,
1.,1.,1.,1.,1.,1.,1.,1.,1.,1.,1.,1.,1.,1.,1.,1.,1.,1.,1.,1.,1.,1.,1.,1.,
1.,1.,1.,1.,1.,1.,1.,1.,1.,1.,1.,1.,1.,1.,1.,1.,1.,1.,1.,1.,1.,1.,1.,1.,
1.,1.,1.,1.,1.,1.,1.,1.,1.,1.,1.,1.,1.,1.,1.,1.,1.,1.,1.,1.,1.,1.,1.,1.,
1.,1.,1.,1.,1.,1.,1.,1.,1.,1.,1.,1.,1.,1.,1.,1.,1.,1.,1.,1.,1.,1.,1.,1.,
1.,1.,1.,1.,1.,1.,1.,1.,1.,1.))
REPRESENTATION_ITEM('')
);
#618=(
BOUNDED_CURVE()
B_SPLINE_CURVE(5,(#145635,#145636,#145637,#145638,#145639,#145640,#145641,
#145642,#145643,#145644,#145645,#145646,#145647,#145648,#145649,#145650,
#145651,#145652,#145653,#145654,#145655,#145656,#145657,#145658,#145659,
#145660,#145661,#145662,#145663,#145664,#145665,#145666,#145667,#145668,
#145669,#145670,#145671,#145672,#145673,#145674,#145675,#145676,#145677,
#145678,#145679,#145680,#145681,#145682,#145683,#145684,#145685,#145686,
#145687,#145688,#145689,#145690,#145691,#145692,#145693,#145694,#145695,
#145696,#145697,#145698,#145699,#145700,#145701,#145702,#145703,#145704,
#145705,#145706,#145707,#145708,#145709,#145710,#145711,#145712,#145713,
#145714,#145715,#145716,#145717,#145718,#145719,#145720,#145721,#145722,
#145723,#145724,#145725,#145726,#145727,#145728,#145729,#145730,#145731,
#145732,#145733,#145734,#145735,#145736,#145737,#145738,#145739,#145740,
#145741,#145742,#145743,#145744,#145745,#145746,#145747,#145748,#145749,
#145750,#145751,#145752,#145753,#145754,#145755,#145756,#145757,#145758,
#145759,#145760,#145761,#145762,#145763,#145764,#145765,#145766,#145767,
#145768,#145769,#145770,#145771,#145772,#145773,#145774,#145775,#145776,
#145777,#145778,#145779,#145780,#145781,#145782,#145783,#145784,#145785,
#145786,#145787,#145788,#145789,#145790,#145791,#145792,#145793,#145794,
#145795,#145796,#145797,#145798,#145799,#145800,#145801,#145802,#145803,
#145804,#145805,#145806,#145807,#145808,#145809,#145810,#145811,#145812,
#145813,#145814,#145815,#145816,#145817,#145818,#145819,#145820,#145821,
#145822,#145823,#145824,#145825,#145826,#145827,#145828),.UNSPECIFIED.,
 .F.,.F.)
B_SPLINE_CURVE_WITH_KNOTS((6,1,1,1,1,1,1,1,1,1,1,1,1,1,1,1,1,1,1,1,1,1,
1,1,1,1,1,1,1,1,1,1,1,1,1,1,1,1,1,1,1,1,1,1,1,1,1,1,1,1,1,1,1,1,1,1,1,1,
1,1,1,1,1,1,1,1,1,1,1,1,1,1,1,1,1,1,1,1,1,1,1,1,1,1,1,1,1,1,1,1,1,1,1,1,
1,1,1,1,1,1,1,1,1,1,1,1,1,1,1,1,1,1,1,1,1,1,1,1,1,1,1,1,1,1,1,1,1,1,1,1,
1,1,1,1,1,1,1,1,1,1,1,1,1,1,1,1,1,1,1,1,1,1,1,1,1,1,1,1,1,1,1,1,1,1,1,1,
1,1,1,1,1,1,1,1,1,1,1,1,1,1,1,1,1,1,1,1,1,1,1,6),(-0.941429844438071,-0.940000000000001,
-0.935000000000001,-0.930000000000001,-0.925000000000001,-0.920000000000001,
-0.915000000000001,-0.910000000000001,-0.905000000000001,-0.900000000000001,
-0.895000000000001,-0.890000000000001,-0.885000000000001,-0.880000000000001,
-0.875000000000001,-0.870000000000001,-0.865000000000001,-0.860000000000001,
-0.855000000000001,-0.850000000000001,-0.845000000000001,-0.840000000000001,
-0.835000000000001,-0.830000000000001,-0.825000000000001,-0.820000000000001,
-0.815000000000001,-0.810000000000001,-0.805000000000001,-0.800000000000001,
-0.795000000000001,-0.790000000000001,-0.785000000000001,-0.780000000000001,
-0.775000000000001,-0.770000000000001,-0.765000000000001,-0.760000000000001,
-0.755000000000001,-0.750000000000001,-0.745000000000001,-0.740000000000001,
-0.735000000000001,-0.730000000000001,-0.725000000000001,-0.720000000000001,
-0.715000000000001,-0.710000000000001,-0.705000000000001,-0.700000000000001,
-0.695000000000001,-0.690000000000001,-0.685,-0.68,-0.675,-0.67,-0.665,
-0.66,-0.655,-0.65,-0.645,-0.64,-0.635,-0.63,-0.625,-0.62,-0.615,-0.61,
-0.605,-0.6,-0.595,-0.59,-0.585,-0.58,-0.575,-0.57,-0.565,-0.56,-0.555,
-0.55,-0.545,-0.54,-0.535,-0.53,-0.525,-0.52,-0.515,-0.51,-0.505,-0.5,-0.495,
-0.49,-0.485,-0.48,-0.475,-0.47,-0.465,-0.46,-0.455,-0.45,-0.445,-0.44,
-0.435,-0.43,-0.425,-0.42,-0.415,-0.41,-0.405,-0.4,-0.395,-0.39,-0.385,
-0.38,-0.375,-0.37,-0.365,-0.36,-0.355,-0.35,-0.345,-0.34,-0.335,-0.33,
-0.325,-0.32,-0.315,-0.31,-0.305,-0.3,-0.295,-0.29,-0.285,-0.28,-0.275,
-0.27,-0.265,-0.26,-0.255,-0.25,-0.245,-0.24,-0.235,-0.23,-0.225,-0.22,
-0.215,-0.21,-0.205,-0.2,-0.195,-0.19,-0.185,-0.18,-0.175,-0.17,-0.165,
-0.16,-0.155,-0.15,-0.145,-0.14,-0.135,-0.13,-0.125,-0.12,-0.115,-0.11,
-0.105,-0.1,-0.095,-0.09,-0.085,-0.08,-0.075,-0.07,-0.065,-0.06,-0.055,
-0.05,-0.045,-0.04,-0.035,-0.03,-0.025,-0.02,-0.015,-0.01,-0.005,0.),
 .UNSPECIFIED.)
CURVE()
GEOMETRIC_REPRESENTATION_ITEM()
RATIONAL_B_SPLINE_CURVE((1.,1.,1.,1.,1.,1.,1.,1.,1.,1.,1.,1.,1.,1.,1.,1.,
1.,1.,1.,1.,1.,1.,1.,1.,1.,1.,1.,1.,1.,1.,1.,1.,1.,1.,1.,1.,1.,1.,1.,1.,
1.,1.,1.,1.,1.,1.,1.,1.,1.,1.,1.,1.,1.,1.,1.,1.,1.,1.,1.,1.,1.,1.,1.,1.,
1.,1.,1.,1.,1.,1.,1.,1.,1.,1.,1.,1.,1.,1.,1.,1.,1.,1.,1.,1.,1.,1.,1.,1.,
1.,1.,1.,1.,1.,1.,1.,1.,1.,1.,1.,1.,1.,1.,1.,1.,1.,1.,1.,1.,1.,1.,1.,1.,
1.,1.,1.,1.,1.,1.,1.,1.,1.,1.,1.,1.,1.,1.,1.,1.,1.,1.,1.,1.,1.,1.,1.,1.,
1.,1.,1.,1.,1.,1.,1.,1.,1.,1.,1.,1.,1.,1.,1.,1.,1.,1.,1.,1.,1.,1.,1.,1.,
1.,1.,1.,1.,1.,1.,1.,1.,1.,1.,1.,1.,1.,1.,1.,1.,1.,1.,1.,1.,1.,1.,1.,1.,
1.,1.,1.,1.,1.,1.,1.,1.,1.,1.))
REPRESENTATION_ITEM('')
);
#619=(
BOUNDED_CURVE()
B_SPLINE_CURVE(5,(#146240,#146241,#146242,#146243,#146244,#146245,#146246,
#146247,#146248,#146249,#146250,#146251,#146252,#146253,#146254,#146255,
#146256,#146257,#146258,#146259,#146260,#146261,#146262,#146263,#146264,
#146265,#146266,#146267,#146268,#146269,#146270,#146271,#146272,#146273,
#146274,#146275,#146276,#146277,#146278,#146279,#146280,#146281,#146282,
#146283,#146284,#146285,#146286,#146287,#146288,#146289,#146290,#146291,
#146292,#146293,#146294,#146295,#146296,#146297,#146298,#146299,#146300,
#146301,#146302,#146303,#146304,#146305,#146306,#146307,#146308,#146309,
#146310,#146311,#146312,#146313,#146314,#146315,#146316,#146317,#146318,
#146319,#146320,#146321,#146322,#146323,#146324,#146325,#146326,#146327,
#146328,#146329,#146330,#146331,#146332,#146333,#146334,#146335,#146336,
#146337,#146338,#146339,#146340,#146341,#146342,#146343,#146344,#146345,
#146346,#146347,#146348,#146349,#146350,#146351,#146352,#146353,#146354,
#146355,#146356,#146357,#146358,#146359,#146360,#146361,#146362,#146363,
#146364,#146365,#146366,#146367,#146368,#146369,#146370,#146371,#146372,
#146373,#146374,#146375,#146376,#146377,#146378,#146379,#146380,#146381,
#146382,#146383,#146384,#146385,#146386,#146387,#146388,#146389,#146390,
#146391,#146392,#146393,#146394,#146395,#146396,#146397,#146398,#146399,
#146400,#146401,#146402,#146403,#146404,#146405,#146406,#146407,#146408,
#146409,#146410,#146411,#146412,#146413,#146414,#146415,#146416,#146417,
#146418,#146419,#146420,#146421,#146422,#146423,#146424,#146425,#146426,
#146427,#146428,#146429,#146430,#146431,#146432,#146433),.UNSPECIFIED.,
 .F.,.F.)
B_SPLINE_CURVE_WITH_KNOTS((6,1,1,1,1,1,1,1,1,1,1,1,1,1,1,1,1,1,1,1,1,1,
1,1,1,1,1,1,1,1,1,1,1,1,1,1,1,1,1,1,1,1,1,1,1,1,1,1,1,1,1,1,1,1,1,1,1,1,
1,1,1,1,1,1,1,1,1,1,1,1,1,1,1,1,1,1,1,1,1,1,1,1,1,1,1,1,1,1,1,1,1,1,1,1,
1,1,1,1,1,1,1,1,1,1,1,1,1,1,1,1,1,1,1,1,1,1,1,1,1,1,1,1,1,1,1,1,1,1,1,1,
1,1,1,1,1,1,1,1,1,1,1,1,1,1,1,1,1,1,1,1,1,1,1,1,1,1,1,1,1,1,1,1,1,1,1,1,
1,1,1,1,1,1,1,1,1,1,1,1,1,1,1,1,1,1,1,1,1,1,1,6),(0.,0.005,0.01,0.015,0.02,
0.025,0.03,0.035,0.04,0.045,0.05,0.055,0.06,0.065,0.07,0.075,0.08,0.085,
0.09,0.095,0.1,0.105,0.11,0.115,0.12,0.125,0.13,0.135,0.14,0.145,0.15,0.155,
0.16,0.165,0.17,0.175,0.18,0.185,0.19,0.195,0.2,0.205,0.21,0.215,0.22,0.225,
0.23,0.235,0.24,0.245,0.25,0.255,0.26,0.265,0.27,0.275,0.28,0.285,0.29,
0.295,0.3,0.305,0.31,0.315,0.32,0.325,0.33,0.335,0.34,0.345,0.35,0.355,
0.36,0.365,0.37,0.375,0.38,0.385,0.39,0.395,0.4,0.405,0.41,0.415,0.42,0.425,
0.43,0.435,0.44,0.445,0.45,0.455,0.46,0.465,0.47,0.475,0.48,0.485,0.49,
0.495,0.5,0.505,0.51,0.515,0.52,0.525,0.53,0.535,0.54,0.545,0.55,0.555,
0.56,0.565,0.57,0.575,0.58,0.585,0.59,0.595,0.6,0.605,0.61,0.615,0.62,0.625,
0.63,0.635,0.64,0.645,0.65,0.655,0.66,0.665,0.67,0.675,0.68,0.685,0.690000000000001,
0.695000000000001,0.700000000000001,0.705000000000001,0.710000000000001,
0.715000000000001,0.720000000000001,0.725000000000001,0.730000000000001,
0.735000000000001,0.740000000000001,0.745000000000001,0.750000000000001,
0.755000000000001,0.760000000000001,0.765000000000001,0.770000000000001,
0.775000000000001,0.780000000000001,0.785000000000001,0.790000000000001,
0.795000000000001,0.800000000000001,0.805000000000001,0.810000000000001,
0.815000000000001,0.820000000000001,0.825000000000001,0.830000000000001,
0.835000000000001,0.840000000000001,0.845000000000001,0.850000000000001,
0.855000000000001,0.860000000000001,0.865000000000001,0.870000000000001,
0.875000000000001,0.880000000000001,0.885000000000001,0.890000000000001,
0.895000000000001,0.900000000000001,0.905000000000001,0.910000000000001,
0.915000000000001,0.920000000000001,0.925000000000001,0.930000000000001,
0.935000000000001,0.940000000000001,0.941429844437995),.UNSPECIFIED.)
CURVE()
GEOMETRIC_REPRESENTATION_ITEM()
RATIONAL_B_SPLINE_CURVE((1.,1.,1.,1.,1.,1.,1.,1.,1.,1.,1.,1.,1.,1.,1.,1.,
1.,1.,1.,1.,1.,1.,1.,1.,1.,1.,1.,1.,1.,1.,1.,1.,1.,1.,1.,1.,1.,1.,1.,1.,
1.,1.,1.,1.,1.,1.,1.,1.,1.,1.,1.,1.,1.,1.,1.,1.,1.,1.,1.,1.,1.,1.,1.,1.,
1.,1.,1.,1.,1.,1.,1.,1.,1.,1.,1.,1.,1.,1.,1.,1.,1.,1.,1.,1.,1.,1.,1.,1.,
1.,1.,1.,1.,1.,1.,1.,1.,1.,1.,1.,1.,1.,1.,1.,1.,1.,1.,1.,1.,1.,1.,1.,1.,
1.,1.,1.,1.,1.,1.,1.,1.,1.,1.,1.,1.,1.,1.,1.,1.,1.,1.,1.,1.,1.,1.,1.,1.,
1.,1.,1.,1.,1.,1.,1.,1.,1.,1.,1.,1.,1.,1.,1.,1.,1.,1.,1.,1.,1.,1.,1.,1.,
1.,1.,1.,1.,1.,1.,1.,1.,1.,1.,1.,1.,1.,1.,1.,1.,1.,1.,1.,1.,1.,1.,1.,1.,
1.,1.,1.,1.,1.,1.,1.,1.,1.,1.))
REPRESENTATION_ITEM('')
);
#620=(
BOUNDED_CURVE()
B_SPLINE_CURVE(5,(#146436,#146437,#146438,#146439,#146440,#146441,#146442,
#146443,#146444,#146445,#146446,#146447,#146448,#146449,#146450,#146451,
#146452,#146453,#146454,#146455,#146456,#146457,#146458,#146459,#146460,
#146461,#146462,#146463,#146464,#146465,#146466,#146467,#146468,#146469,
#146470,#146471,#146472,#146473,#146474,#146475,#146476,#146477,#146478,
#146479,#146480,#146481,#146482,#146483,#146484,#146485,#146486,#146487,
#146488,#146489,#146490,#146491,#146492,#146493,#146494,#146495,#146496,
#146497,#146498,#146499,#146500,#146501,#146502,#146503,#146504,#146505,
#146506,#146507,#146508,#146509,#146510,#146511,#146512,#146513,#146514,
#146515,#146516,#146517,#146518,#146519,#146520,#146521,#146522,#146523,
#146524,#146525,#146526,#146527,#146528,#146529,#146530,#146531,#146532,
#146533,#146534,#146535,#146536,#146537,#146538,#146539,#146540,#146541,
#146542,#146543,#146544,#146545,#146546,#146547,#146548,#146549,#146550,
#146551,#146552,#146553,#146554,#146555,#146556,#146557,#146558,#146559,
#146560,#146561,#146562,#146563,#146564,#146565,#146566,#146567,#146568,
#146569,#146570,#146571,#146572,#146573,#146574,#146575,#146576,#146577,
#146578,#146579,#146580,#146581,#146582,#146583,#146584,#146585,#146586,
#146587,#146588,#146589,#146590,#146591,#146592,#146593,#146594,#146595,
#146596,#146597,#146598,#146599,#146600,#146601,#146602,#146603,#146604,
#146605,#146606,#146607,#146608,#146609,#146610,#146611,#146612,#146613,
#146614,#146615,#146616,#146617,#146618,#146619,#146620,#146621,#146622,
#146623,#146624,#146625,#146626,#146627,#146628,#146629),.UNSPECIFIED.,
 .F.,.F.)
B_SPLINE_CURVE_WITH_KNOTS((6,1,1,1,1,1,1,1,1,1,1,1,1,1,1,1,1,1,1,1,1,1,
1,1,1,1,1,1,1,1,1,1,1,1,1,1,1,1,1,1,1,1,1,1,1,1,1,1,1,1,1,1,1,1,1,1,1,1,
1,1,1,1,1,1,1,1,1,1,1,1,1,1,1,1,1,1,1,1,1,1,1,1,1,1,1,1,1,1,1,1,1,1,1,1,
1,1,1,1,1,1,1,1,1,1,1,1,1,1,1,1,1,1,1,1,1,1,1,1,1,1,1,1,1,1,1,1,1,1,1,1,
1,1,1,1,1,1,1,1,1,1,1,1,1,1,1,1,1,1,1,1,1,1,1,1,1,1,1,1,1,1,1,1,1,1,1,1,
1,1,1,1,1,1,1,1,1,1,1,1,1,1,1,1,1,1,1,1,1,1,1,6),(-0.941429844438002,-0.940000000000001,
-0.935000000000001,-0.930000000000001,-0.925000000000001,-0.920000000000001,
-0.915000000000001,-0.910000000000001,-0.905000000000001,-0.900000000000001,
-0.895000000000001,-0.890000000000001,-0.885000000000001,-0.880000000000001,
-0.875000000000001,-0.870000000000001,-0.865000000000001,-0.860000000000001,
-0.855000000000001,-0.850000000000001,-0.845000000000001,-0.840000000000001,
-0.835000000000001,-0.830000000000001,-0.825000000000001,-0.820000000000001,
-0.815000000000001,-0.810000000000001,-0.805000000000001,-0.800000000000001,
-0.795000000000001,-0.790000000000001,-0.785000000000001,-0.780000000000001,
-0.775000000000001,-0.770000000000001,-0.765000000000001,-0.760000000000001,
-0.755000000000001,-0.750000000000001,-0.745000000000001,-0.740000000000001,
-0.735000000000001,-0.730000000000001,-0.725000000000001,-0.720000000000001,
-0.715000000000001,-0.710000000000001,-0.705000000000001,-0.700000000000001,
-0.695000000000001,-0.690000000000001,-0.685,-0.68,-0.675,-0.67,-0.665,
-0.66,-0.655,-0.65,-0.645,-0.64,-0.635,-0.63,-0.625,-0.62,-0.615,-0.61,
-0.605,-0.6,-0.595,-0.59,-0.585,-0.58,-0.575,-0.57,-0.565,-0.56,-0.555,
-0.55,-0.545,-0.54,-0.535,-0.53,-0.525,-0.52,-0.515,-0.51,-0.505,-0.5,-0.495,
-0.49,-0.485,-0.48,-0.475,-0.47,-0.465,-0.46,-0.455,-0.45,-0.445,-0.44,
-0.435,-0.43,-0.425,-0.42,-0.415,-0.41,-0.405,-0.4,-0.395,-0.39,-0.385,
-0.38,-0.375,-0.37,-0.365,-0.36,-0.355,-0.35,-0.345,-0.34,-0.335,-0.33,
-0.325,-0.32,-0.315,-0.31,-0.305,-0.3,-0.295,-0.29,-0.285,-0.28,-0.275,
-0.27,-0.265,-0.26,-0.255,-0.25,-0.245,-0.24,-0.235,-0.23,-0.225,-0.22,
-0.215,-0.21,-0.205,-0.2,-0.195,-0.19,-0.185,-0.18,-0.175,-0.17,-0.165,
-0.16,-0.155,-0.15,-0.145,-0.14,-0.135,-0.13,-0.125,-0.12,-0.115,-0.11,
-0.105,-0.1,-0.095,-0.09,-0.085,-0.08,-0.075,-0.07,-0.065,-0.06,-0.055,
-0.05,-0.045,-0.04,-0.035,-0.03,-0.025,-0.02,-0.015,-0.01,-0.005,0.),
 .UNSPECIFIED.)
CURVE()
GEOMETRIC_REPRESENTATION_ITEM()
RATIONAL_B_SPLINE_CURVE((1.,1.,1.,1.,1.,1.,1.,1.,1.,1.,1.,1.,1.,1.,1.,1.,
1.,1.,1.,1.,1.,1.,1.,1.,1.,1.,1.,1.,1.,1.,1.,1.,1.,1.,1.,1.,1.,1.,1.,1.,
1.,1.,1.,1.,1.,1.,1.,1.,1.,1.,1.,1.,1.,1.,1.,1.,1.,1.,1.,1.,1.,1.,1.,1.,
1.,1.,1.,1.,1.,1.,1.,1.,1.,1.,1.,1.,1.,1.,1.,1.,1.,1.,1.,1.,1.,1.,1.,1.,
1.,1.,1.,1.,1.,1.,1.,1.,1.,1.,1.,1.,1.,1.,1.,1.,1.,1.,1.,1.,1.,1.,1.,1.,
1.,1.,1.,1.,1.,1.,1.,1.,1.,1.,1.,1.,1.,1.,1.,1.,1.,1.,1.,1.,1.,1.,1.,1.,
1.,1.,1.,1.,1.,1.,1.,1.,1.,1.,1.,1.,1.,1.,1.,1.,1.,1.,1.,1.,1.,1.,1.,1.,
1.,1.,1.,1.,1.,1.,1.,1.,1.,1.,1.,1.,1.,1.,1.,1.,1.,1.,1.,1.,1.,1.,1.,1.,
1.,1.,1.,1.,1.,1.,1.,1.,1.,1.))
REPRESENTATION_ITEM('')
);
#621=(
BOUNDED_CURVE()
B_SPLINE_CURVE(5,(#147041,#147042,#147043,#147044,#147045,#147046,#147047,
#147048,#147049,#147050,#147051,#147052,#147053,#147054,#147055,#147056,
#147057,#147058,#147059,#147060,#147061,#147062,#147063,#147064,#147065,
#147066,#147067,#147068,#147069,#147070,#147071,#147072,#147073,#147074,
#147075,#147076,#147077,#147078,#147079,#147080,#147081,#147082,#147083,
#147084,#147085,#147086,#147087,#147088,#147089,#147090,#147091,#147092,
#147093,#147094,#147095,#147096,#147097,#147098,#147099,#147100,#147101,
#147102,#147103,#147104,#147105,#147106,#147107,#147108,#147109,#147110,
#147111,#147112,#147113,#147114,#147115,#147116,#147117,#147118,#147119,
#147120,#147121,#147122,#147123,#147124,#147125,#147126,#147127,#147128,
#147129,#147130,#147131,#147132,#147133,#147134,#147135,#147136,#147137,
#147138,#147139,#147140,#147141,#147142,#147143,#147144,#147145,#147146,
#147147,#147148,#147149,#147150,#147151,#147152,#147153,#147154,#147155,
#147156,#147157,#147158,#147159,#147160,#147161,#147162,#147163,#147164,
#147165,#147166,#147167,#147168,#147169,#147170,#147171,#147172,#147173,
#147174,#147175,#147176,#147177,#147178,#147179,#147180,#147181,#147182,
#147183,#147184,#147185,#147186,#147187,#147188,#147189,#147190,#147191,
#147192,#147193,#147194,#147195,#147196,#147197,#147198,#147199,#147200,
#147201,#147202,#147203,#147204,#147205,#147206,#147207,#147208,#147209,
#147210,#147211,#147212,#147213,#147214,#147215,#147216,#147217,#147218,
#147219,#147220,#147221,#147222,#147223,#147224,#147225,#147226,#147227,
#147228,#147229,#147230,#147231,#147232,#147233,#147234),.UNSPECIFIED.,
 .F.,.F.)
B_SPLINE_CURVE_WITH_KNOTS((6,1,1,1,1,1,1,1,1,1,1,1,1,1,1,1,1,1,1,1,1,1,
1,1,1,1,1,1,1,1,1,1,1,1,1,1,1,1,1,1,1,1,1,1,1,1,1,1,1,1,1,1,1,1,1,1,1,1,
1,1,1,1,1,1,1,1,1,1,1,1,1,1,1,1,1,1,1,1,1,1,1,1,1,1,1,1,1,1,1,1,1,1,1,1,
1,1,1,1,1,1,1,1,1,1,1,1,1,1,1,1,1,1,1,1,1,1,1,1,1,1,1,1,1,1,1,1,1,1,1,1,
1,1,1,1,1,1,1,1,1,1,1,1,1,1,1,1,1,1,1,1,1,1,1,1,1,1,1,1,1,1,1,1,1,1,1,1,
1,1,1,1,1,1,1,1,1,1,1,1,1,1,1,1,1,1,1,1,1,1,1,6),(0.,0.005,0.01,0.015,0.02,
0.025,0.03,0.035,0.04,0.045,0.05,0.055,0.06,0.065,0.07,0.075,0.08,0.085,
0.09,0.095,0.1,0.105,0.11,0.115,0.12,0.125,0.13,0.135,0.14,0.145,0.15,0.155,
0.16,0.165,0.17,0.175,0.18,0.185,0.19,0.195,0.2,0.205,0.21,0.215,0.22,0.225,
0.23,0.235,0.24,0.245,0.25,0.255,0.26,0.265,0.27,0.275,0.28,0.285,0.29,
0.295,0.3,0.305,0.31,0.315,0.32,0.325,0.33,0.335,0.34,0.345,0.35,0.355,
0.36,0.365,0.37,0.375,0.38,0.385,0.39,0.395,0.4,0.405,0.41,0.415,0.42,0.425,
0.43,0.435,0.44,0.445,0.45,0.455,0.46,0.465,0.47,0.475,0.48,0.485,0.49,
0.495,0.5,0.505,0.51,0.515,0.52,0.525,0.53,0.535,0.54,0.545,0.55,0.555,
0.56,0.565,0.57,0.575,0.58,0.585,0.59,0.595,0.6,0.605,0.61,0.615,0.62,0.625,
0.63,0.635,0.64,0.645,0.65,0.655,0.66,0.665,0.67,0.675,0.68,0.685,0.690000000000001,
0.695000000000001,0.700000000000001,0.705000000000001,0.710000000000001,
0.715000000000001,0.720000000000001,0.725000000000001,0.730000000000001,
0.735000000000001,0.740000000000001,0.745000000000001,0.750000000000001,
0.755000000000001,0.760000000000001,0.765000000000001,0.770000000000001,
0.775000000000001,0.780000000000001,0.785000000000001,0.790000000000001,
0.795000000000001,0.800000000000001,0.805000000000001,0.810000000000001,
0.815000000000001,0.820000000000001,0.825000000000001,0.830000000000001,
0.835000000000001,0.840000000000001,0.845000000000001,0.850000000000001,
0.855000000000001,0.860000000000001,0.865000000000001,0.870000000000001,
0.875000000000001,0.880000000000001,0.885000000000001,0.890000000000001,
0.895000000000001,0.900000000000001,0.905000000000001,0.910000000000001,
0.915000000000001,0.920000000000001,0.925000000000001,0.930000000000001,
0.935000000000001,0.940000000000001,0.941429844437957),.UNSPECIFIED.)
CURVE()
GEOMETRIC_REPRESENTATION_ITEM()
RATIONAL_B_SPLINE_CURVE((1.,1.,1.,1.,1.,1.,1.,1.,1.,1.,1.,1.,1.,1.,1.,1.,
1.,1.,1.,1.,1.,1.,1.,1.,1.,1.,1.,1.,1.,1.,1.,1.,1.,1.,1.,1.,1.,1.,1.,1.,
1.,1.,1.,1.,1.,1.,1.,1.,1.,1.,1.,1.,1.,1.,1.,1.,1.,1.,1.,1.,1.,1.,1.,1.,
1.,1.,1.,1.,1.,1.,1.,1.,1.,1.,1.,1.,1.,1.,1.,1.,1.,1.,1.,1.,1.,1.,1.,1.,
1.,1.,1.,1.,1.,1.,1.,1.,1.,1.,1.,1.,1.,1.,1.,1.,1.,1.,1.,1.,1.,1.,1.,1.,
1.,1.,1.,1.,1.,1.,1.,1.,1.,1.,1.,1.,1.,1.,1.,1.,1.,1.,1.,1.,1.,1.,1.,1.,
1.,1.,1.,1.,1.,1.,1.,1.,1.,1.,1.,1.,1.,1.,1.,1.,1.,1.,1.,1.,1.,1.,1.,1.,
1.,1.,1.,1.,1.,1.,1.,1.,1.,1.,1.,1.,1.,1.,1.,1.,1.,1.,1.,1.,1.,1.,1.,1.,
1.,1.,1.,1.,1.,1.,1.,1.,1.,1.))
REPRESENTATION_ITEM('')
);
#622=(
BOUNDED_CURVE()
B_SPLINE_CURVE(5,(#147237,#147238,#147239,#147240,#147241,#147242,#147243,
#147244,#147245,#147246,#147247,#147248,#147249,#147250,#147251,#147252,
#147253,#147254,#147255,#147256,#147257,#147258,#147259,#147260,#147261,
#147262,#147263,#147264,#147265,#147266,#147267,#147268,#147269,#147270,
#147271,#147272,#147273,#147274,#147275,#147276,#147277,#147278,#147279,
#147280,#147281,#147282,#147283,#147284,#147285,#147286,#147287,#147288,
#147289,#147290,#147291,#147292,#147293,#147294,#147295,#147296,#147297,
#147298,#147299,#147300,#147301,#147302,#147303,#147304,#147305,#147306,
#147307,#147308,#147309,#147310,#147311,#147312,#147313,#147314,#147315,
#147316,#147317,#147318,#147319,#147320,#147321,#147322,#147323,#147324,
#147325,#147326,#147327,#147328,#147329,#147330,#147331,#147332,#147333,
#147334,#147335,#147336,#147337,#147338,#147339,#147340,#147341,#147342,
#147343,#147344,#147345,#147346,#147347,#147348,#147349,#147350,#147351,
#147352,#147353,#147354,#147355,#147356,#147357,#147358,#147359,#147360,
#147361,#147362,#147363,#147364,#147365,#147366,#147367,#147368,#147369,
#147370,#147371,#147372,#147373,#147374,#147375,#147376,#147377,#147378,
#147379,#147380,#147381,#147382,#147383,#147384,#147385,#147386,#147387,
#147388,#147389,#147390,#147391,#147392,#147393,#147394,#147395,#147396,
#147397,#147398,#147399,#147400,#147401,#147402,#147403,#147404,#147405,
#147406,#147407,#147408,#147409,#147410,#147411,#147412,#147413,#147414,
#147415,#147416,#147417,#147418,#147419,#147420,#147421,#147422,#147423,
#147424,#147425,#147426,#147427,#147428,#147429,#147430),.UNSPECIFIED.,
 .F.,.F.)
B_SPLINE_CURVE_WITH_KNOTS((6,1,1,1,1,1,1,1,1,1,1,1,1,1,1,1,1,1,1,1,1,1,
1,1,1,1,1,1,1,1,1,1,1,1,1,1,1,1,1,1,1,1,1,1,1,1,1,1,1,1,1,1,1,1,1,1,1,1,
1,1,1,1,1,1,1,1,1,1,1,1,1,1,1,1,1,1,1,1,1,1,1,1,1,1,1,1,1,1,1,1,1,1,1,1,
1,1,1,1,1,1,1,1,1,1,1,1,1,1,1,1,1,1,1,1,1,1,1,1,1,1,1,1,1,1,1,1,1,1,1,1,
1,1,1,1,1,1,1,1,1,1,1,1,1,1,1,1,1,1,1,1,1,1,1,1,1,1,1,1,1,1,1,1,1,1,1,1,
1,1,1,1,1,1,1,1,1,1,1,1,1,1,1,1,1,1,1,1,1,1,1,6),(-0.94142984443796,-0.940000000000001,
-0.935000000000001,-0.930000000000001,-0.925000000000001,-0.920000000000001,
-0.915000000000001,-0.910000000000001,-0.905000000000001,-0.900000000000001,
-0.895000000000001,-0.890000000000001,-0.885000000000001,-0.880000000000001,
-0.875000000000001,-0.870000000000001,-0.865000000000001,-0.860000000000001,
-0.855000000000001,-0.850000000000001,-0.845000000000001,-0.840000000000001,
-0.835000000000001,-0.830000000000001,-0.825000000000001,-0.820000000000001,
-0.815000000000001,-0.810000000000001,-0.805000000000001,-0.800000000000001,
-0.795000000000001,-0.790000000000001,-0.785000000000001,-0.780000000000001,
-0.775000000000001,-0.770000000000001,-0.765000000000001,-0.760000000000001,
-0.755000000000001,-0.750000000000001,-0.745000000000001,-0.740000000000001,
-0.735000000000001,-0.730000000000001,-0.725000000000001,-0.720000000000001,
-0.715000000000001,-0.710000000000001,-0.705000000000001,-0.700000000000001,
-0.695000000000001,-0.690000000000001,-0.685,-0.68,-0.675,-0.67,-0.665,
-0.66,-0.655,-0.65,-0.645,-0.64,-0.635,-0.63,-0.625,-0.62,-0.615,-0.61,
-0.605,-0.6,-0.595,-0.59,-0.585,-0.58,-0.575,-0.57,-0.565,-0.56,-0.555,
-0.55,-0.545,-0.54,-0.535,-0.53,-0.525,-0.52,-0.515,-0.51,-0.505,-0.5,-0.495,
-0.49,-0.485,-0.48,-0.475,-0.47,-0.465,-0.46,-0.455,-0.45,-0.445,-0.44,
-0.435,-0.43,-0.425,-0.42,-0.415,-0.41,-0.405,-0.4,-0.395,-0.39,-0.385,
-0.38,-0.375,-0.37,-0.365,-0.36,-0.355,-0.35,-0.345,-0.34,-0.335,-0.33,
-0.325,-0.32,-0.315,-0.31,-0.305,-0.3,-0.295,-0.29,-0.285,-0.28,-0.275,
-0.27,-0.265,-0.26,-0.255,-0.25,-0.245,-0.24,-0.235,-0.23,-0.225,-0.22,
-0.215,-0.21,-0.205,-0.2,-0.195,-0.19,-0.185,-0.18,-0.175,-0.17,-0.165,
-0.16,-0.155,-0.15,-0.145,-0.14,-0.135,-0.13,-0.125,-0.12,-0.115,-0.11,
-0.105,-0.1,-0.095,-0.09,-0.085,-0.08,-0.075,-0.07,-0.065,-0.06,-0.055,
-0.05,-0.045,-0.04,-0.035,-0.03,-0.025,-0.02,-0.015,-0.01,-0.005,0.),
 .UNSPECIFIED.)
CURVE()
GEOMETRIC_REPRESENTATION_ITEM()
RATIONAL_B_SPLINE_CURVE((1.,1.,1.,1.,1.,1.,1.,1.,1.,1.,1.,1.,1.,1.,1.,1.,
1.,1.,1.,1.,1.,1.,1.,1.,1.,1.,1.,1.,1.,1.,1.,1.,1.,1.,1.,1.,1.,1.,1.,1.,
1.,1.,1.,1.,1.,1.,1.,1.,1.,1.,1.,1.,1.,1.,1.,1.,1.,1.,1.,1.,1.,1.,1.,1.,
1.,1.,1.,1.,1.,1.,1.,1.,1.,1.,1.,1.,1.,1.,1.,1.,1.,1.,1.,1.,1.,1.,1.,1.,
1.,1.,1.,1.,1.,1.,1.,1.,1.,1.,1.,1.,1.,1.,1.,1.,1.,1.,1.,1.,1.,1.,1.,1.,
1.,1.,1.,1.,1.,1.,1.,1.,1.,1.,1.,1.,1.,1.,1.,1.,1.,1.,1.,1.,1.,1.,1.,1.,
1.,1.,1.,1.,1.,1.,1.,1.,1.,1.,1.,1.,1.,1.,1.,1.,1.,1.,1.,1.,1.,1.,1.,1.,
1.,1.,1.,1.,1.,1.,1.,1.,1.,1.,1.,1.,1.,1.,1.,1.,1.,1.,1.,1.,1.,1.,1.,1.,
1.,1.,1.,1.,1.,1.,1.,1.,1.,1.))
REPRESENTATION_ITEM('')
);
#623=(
BOUNDED_CURVE()
B_SPLINE_CURVE(5,(#147842,#147843,#147844,#147845,#147846,#147847,#147848,
#147849,#147850,#147851,#147852,#147853,#147854,#147855,#147856,#147857,
#147858,#147859,#147860,#147861,#147862,#147863,#147864,#147865,#147866,
#147867,#147868,#147869,#147870,#147871,#147872,#147873,#147874,#147875,
#147876,#147877,#147878,#147879,#147880,#147881,#147882,#147883,#147884,
#147885,#147886,#147887,#147888,#147889,#147890,#147891,#147892,#147893,
#147894,#147895,#147896,#147897,#147898,#147899,#147900,#147901,#147902,
#147903,#147904,#147905,#147906,#147907,#147908,#147909,#147910,#147911,
#147912,#147913,#147914,#147915,#147916,#147917,#147918,#147919,#147920,
#147921,#147922,#147923,#147924,#147925,#147926,#147927,#147928,#147929,
#147930,#147931,#147932,#147933,#147934,#147935,#147936,#147937,#147938,
#147939,#147940,#147941,#147942,#147943,#147944,#147945,#147946,#147947,
#147948,#147949,#147950,#147951,#147952,#147953,#147954,#147955,#147956,
#147957,#147958,#147959,#147960,#147961,#147962,#147963,#147964,#147965,
#147966,#147967,#147968,#147969,#147970,#147971,#147972,#147973,#147974,
#147975,#147976,#147977,#147978,#147979,#147980,#147981,#147982,#147983,
#147984,#147985,#147986,#147987,#147988,#147989,#147990,#147991,#147992,
#147993,#147994,#147995,#147996,#147997,#147998,#147999,#148000,#148001,
#148002,#148003,#148004,#148005,#148006,#148007,#148008,#148009,#148010,
#148011,#148012,#148013,#148014,#148015,#148016,#148017,#148018,#148019,
#148020,#148021,#148022,#148023,#148024,#148025,#148026,#148027,#148028,
#148029,#148030,#148031,#148032,#148033,#148034,#148035),.UNSPECIFIED.,
 .F.,.F.)
B_SPLINE_CURVE_WITH_KNOTS((6,1,1,1,1,1,1,1,1,1,1,1,1,1,1,1,1,1,1,1,1,1,
1,1,1,1,1,1,1,1,1,1,1,1,1,1,1,1,1,1,1,1,1,1,1,1,1,1,1,1,1,1,1,1,1,1,1,1,
1,1,1,1,1,1,1,1,1,1,1,1,1,1,1,1,1,1,1,1,1,1,1,1,1,1,1,1,1,1,1,1,1,1,1,1,
1,1,1,1,1,1,1,1,1,1,1,1,1,1,1,1,1,1,1,1,1,1,1,1,1,1,1,1,1,1,1,1,1,1,1,1,
1,1,1,1,1,1,1,1,1,1,1,1,1,1,1,1,1,1,1,1,1,1,1,1,1,1,1,1,1,1,1,1,1,1,1,1,
1,1,1,1,1,1,1,1,1,1,1,1,1,1,1,1,1,1,1,1,1,1,1,6),(0.,0.005,0.01,0.015,0.02,
0.025,0.03,0.035,0.04,0.045,0.05,0.055,0.06,0.065,0.07,0.075,0.08,0.085,
0.09,0.095,0.1,0.105,0.11,0.115,0.12,0.125,0.13,0.135,0.14,0.145,0.15,0.155,
0.16,0.165,0.17,0.175,0.18,0.185,0.19,0.195,0.2,0.205,0.21,0.215,0.22,0.225,
0.23,0.235,0.24,0.245,0.25,0.255,0.26,0.265,0.27,0.275,0.28,0.285,0.29,
0.295,0.3,0.305,0.31,0.315,0.32,0.325,0.33,0.335,0.34,0.345,0.35,0.355,
0.36,0.365,0.37,0.375,0.38,0.385,0.39,0.395,0.4,0.405,0.41,0.415,0.42,0.425,
0.43,0.435,0.44,0.445,0.45,0.455,0.46,0.465,0.47,0.475,0.48,0.485,0.49,
0.495,0.5,0.505,0.51,0.515,0.52,0.525,0.53,0.535,0.54,0.545,0.55,0.555,
0.56,0.565,0.57,0.575,0.58,0.585,0.59,0.595,0.6,0.605,0.61,0.615,0.62,0.625,
0.63,0.635,0.64,0.645,0.65,0.655,0.66,0.665,0.67,0.675,0.68,0.685,0.690000000000001,
0.695000000000001,0.700000000000001,0.705000000000001,0.710000000000001,
0.715000000000001,0.720000000000001,0.725000000000001,0.730000000000001,
0.735000000000001,0.740000000000001,0.745000000000001,0.750000000000001,
0.755000000000001,0.760000000000001,0.765000000000001,0.770000000000001,
0.775000000000001,0.780000000000001,0.785000000000001,0.790000000000001,
0.795000000000001,0.800000000000001,0.805000000000001,0.810000000000001,
0.815000000000001,0.820000000000001,0.825000000000001,0.830000000000001,
0.835000000000001,0.840000000000001,0.845000000000001,0.850000000000001,
0.855000000000001,0.860000000000001,0.865000000000001,0.870000000000001,
0.875000000000001,0.880000000000001,0.885000000000001,0.890000000000001,
0.895000000000001,0.900000000000001,0.905000000000001,0.910000000000001,
0.915000000000001,0.920000000000001,0.925000000000001,0.930000000000001,
0.935000000000001,0.940000000000001,0.941429844437906),.UNSPECIFIED.)
CURVE()
GEOMETRIC_REPRESENTATION_ITEM()
RATIONAL_B_SPLINE_CURVE((1.,1.,1.,1.,1.,1.,1.,1.,1.,1.,1.,1.,1.,1.,1.,1.,
1.,1.,1.,1.,1.,1.,1.,1.,1.,1.,1.,1.,1.,1.,1.,1.,1.,1.,1.,1.,1.,1.,1.,1.,
1.,1.,1.,1.,1.,1.,1.,1.,1.,1.,1.,1.,1.,1.,1.,1.,1.,1.,1.,1.,1.,1.,1.,1.,
1.,1.,1.,1.,1.,1.,1.,1.,1.,1.,1.,1.,1.,1.,1.,1.,1.,1.,1.,1.,1.,1.,1.,1.,
1.,1.,1.,1.,1.,1.,1.,1.,1.,1.,1.,1.,1.,1.,1.,1.,1.,1.,1.,1.,1.,1.,1.,1.,
1.,1.,1.,1.,1.,1.,1.,1.,1.,1.,1.,1.,1.,1.,1.,1.,1.,1.,1.,1.,1.,1.,1.,1.,
1.,1.,1.,1.,1.,1.,1.,1.,1.,1.,1.,1.,1.,1.,1.,1.,1.,1.,1.,1.,1.,1.,1.,1.,
1.,1.,1.,1.,1.,1.,1.,1.,1.,1.,1.,1.,1.,1.,1.,1.,1.,1.,1.,1.,1.,1.,1.,1.,
1.,1.,1.,1.,1.,1.,1.,1.,1.,1.))
REPRESENTATION_ITEM('')
);
#624=(
BOUNDED_CURVE()
B_SPLINE_CURVE(5,(#148038,#148039,#148040,#148041,#148042,#148043,#148044,
#148045,#148046,#148047,#148048,#148049,#148050,#148051,#148052,#148053,
#148054,#148055,#148056,#148057,#148058,#148059,#148060,#148061,#148062,
#148063,#148064,#148065,#148066,#148067,#148068,#148069,#148070,#148071,
#148072,#148073,#148074,#148075,#148076,#148077,#148078,#148079,#148080,
#148081,#148082,#148083,#148084,#148085,#148086,#148087,#148088,#148089,
#148090,#148091,#148092,#148093,#148094,#148095,#148096,#148097,#148098,
#148099,#148100,#148101,#148102,#148103,#148104,#148105,#148106,#148107,
#148108,#148109,#148110,#148111,#148112,#148113,#148114,#148115,#148116,
#148117,#148118,#148119,#148120,#148121,#148122,#148123,#148124,#148125,
#148126,#148127,#148128,#148129,#148130,#148131,#148132,#148133,#148134,
#148135,#148136,#148137,#148138,#148139,#148140,#148141,#148142,#148143,
#148144,#148145,#148146,#148147,#148148,#148149,#148150,#148151,#148152,
#148153,#148154,#148155,#148156,#148157,#148158,#148159,#148160,#148161,
#148162,#148163,#148164,#148165,#148166,#148167,#148168,#148169,#148170,
#148171,#148172,#148173,#148174,#148175,#148176,#148177,#148178,#148179,
#148180,#148181,#148182,#148183,#148184,#148185,#148186,#148187,#148188,
#148189,#148190,#148191,#148192,#148193,#148194,#148195,#148196,#148197,
#148198,#148199,#148200,#148201,#148202,#148203,#148204,#148205,#148206,
#148207,#148208,#148209,#148210,#148211,#148212,#148213,#148214,#148215,
#148216,#148217,#148218,#148219,#148220,#148221,#148222,#148223,#148224,
#148225,#148226,#148227,#148228,#148229,#148230,#148231),.UNSPECIFIED.,
 .F.,.F.)
B_SPLINE_CURVE_WITH_KNOTS((6,1,1,1,1,1,1,1,1,1,1,1,1,1,1,1,1,1,1,1,1,1,
1,1,1,1,1,1,1,1,1,1,1,1,1,1,1,1,1,1,1,1,1,1,1,1,1,1,1,1,1,1,1,1,1,1,1,1,
1,1,1,1,1,1,1,1,1,1,1,1,1,1,1,1,1,1,1,1,1,1,1,1,1,1,1,1,1,1,1,1,1,1,1,1,
1,1,1,1,1,1,1,1,1,1,1,1,1,1,1,1,1,1,1,1,1,1,1,1,1,1,1,1,1,1,1,1,1,1,1,1,
1,1,1,1,1,1,1,1,1,1,1,1,1,1,1,1,1,1,1,1,1,1,1,1,1,1,1,1,1,1,1,1,1,1,1,1,
1,1,1,1,1,1,1,1,1,1,1,1,1,1,1,1,1,1,1,1,1,1,1,6),(-0.941429844437906,-0.940000000000001,
-0.935000000000001,-0.930000000000001,-0.925000000000001,-0.920000000000001,
-0.915000000000001,-0.910000000000001,-0.905000000000001,-0.900000000000001,
-0.895000000000001,-0.890000000000001,-0.885000000000001,-0.880000000000001,
-0.875000000000001,-0.870000000000001,-0.865000000000001,-0.860000000000001,
-0.855000000000001,-0.850000000000001,-0.845000000000001,-0.840000000000001,
-0.835000000000001,-0.830000000000001,-0.825000000000001,-0.820000000000001,
-0.815000000000001,-0.810000000000001,-0.805000000000001,-0.800000000000001,
-0.795000000000001,-0.790000000000001,-0.785000000000001,-0.780000000000001,
-0.775000000000001,-0.770000000000001,-0.765000000000001,-0.760000000000001,
-0.755000000000001,-0.750000000000001,-0.745000000000001,-0.740000000000001,
-0.735000000000001,-0.730000000000001,-0.725000000000001,-0.720000000000001,
-0.715000000000001,-0.710000000000001,-0.705000000000001,-0.700000000000001,
-0.695000000000001,-0.690000000000001,-0.685,-0.68,-0.675,-0.67,-0.665,
-0.66,-0.655,-0.65,-0.645,-0.64,-0.635,-0.63,-0.625,-0.62,-0.615,-0.61,
-0.605,-0.6,-0.595,-0.59,-0.585,-0.58,-0.575,-0.57,-0.565,-0.56,-0.555,
-0.55,-0.545,-0.54,-0.535,-0.53,-0.525,-0.52,-0.515,-0.51,-0.505,-0.5,-0.495,
-0.49,-0.485,-0.48,-0.475,-0.47,-0.465,-0.46,-0.455,-0.45,-0.445,-0.44,
-0.435,-0.43,-0.425,-0.42,-0.415,-0.41,-0.405,-0.4,-0.395,-0.39,-0.385,
-0.38,-0.375,-0.37,-0.365,-0.36,-0.355,-0.35,-0.345,-0.34,-0.335,-0.33,
-0.325,-0.32,-0.315,-0.31,-0.305,-0.3,-0.295,-0.29,-0.285,-0.28,-0.275,
-0.27,-0.265,-0.26,-0.255,-0.25,-0.245,-0.24,-0.235,-0.23,-0.225,-0.22,
-0.215,-0.21,-0.205,-0.2,-0.195,-0.19,-0.185,-0.18,-0.175,-0.17,-0.165,
-0.16,-0.155,-0.15,-0.145,-0.14,-0.135,-0.13,-0.125,-0.12,-0.115,-0.11,
-0.105,-0.1,-0.095,-0.09,-0.085,-0.08,-0.075,-0.07,-0.065,-0.06,-0.055,
-0.05,-0.045,-0.04,-0.035,-0.03,-0.025,-0.02,-0.015,-0.01,-0.005,0.),
 .UNSPECIFIED.)
CURVE()
GEOMETRIC_REPRESENTATION_ITEM()
RATIONAL_B_SPLINE_CURVE((1.,1.,1.,1.,1.,1.,1.,1.,1.,1.,1.,1.,1.,1.,1.,1.,
1.,1.,1.,1.,1.,1.,1.,1.,1.,1.,1.,1.,1.,1.,1.,1.,1.,1.,1.,1.,1.,1.,1.,1.,
1.,1.,1.,1.,1.,1.,1.,1.,1.,1.,1.,1.,1.,1.,1.,1.,1.,1.,1.,1.,1.,1.,1.,1.,
1.,1.,1.,1.,1.,1.,1.,1.,1.,1.,1.,1.,1.,1.,1.,1.,1.,1.,1.,1.,1.,1.,1.,1.,
1.,1.,1.,1.,1.,1.,1.,1.,1.,1.,1.,1.,1.,1.,1.,1.,1.,1.,1.,1.,1.,1.,1.,1.,
1.,1.,1.,1.,1.,1.,1.,1.,1.,1.,1.,1.,1.,1.,1.,1.,1.,1.,1.,1.,1.,1.,1.,1.,
1.,1.,1.,1.,1.,1.,1.,1.,1.,1.,1.,1.,1.,1.,1.,1.,1.,1.,1.,1.,1.,1.,1.,1.,
1.,1.,1.,1.,1.,1.,1.,1.,1.,1.,1.,1.,1.,1.,1.,1.,1.,1.,1.,1.,1.,1.,1.,1.,
1.,1.,1.,1.,1.,1.,1.,1.,1.,1.))
REPRESENTATION_ITEM('')
);
#625=(
BOUNDED_CURVE()
B_SPLINE_CURVE(5,(#148643,#148644,#148645,#148646,#148647,#148648,#148649,
#148650,#148651,#148652,#148653,#148654,#148655,#148656,#148657,#148658,
#148659,#148660,#148661,#148662,#148663,#148664,#148665,#148666,#148667,
#148668,#148669,#148670,#148671,#148672,#148673,#148674,#148675,#148676,
#148677,#148678,#148679,#148680,#148681,#148682,#148683,#148684,#148685,
#148686,#148687,#148688,#148689,#148690,#148691,#148692,#148693,#148694,
#148695,#148696,#148697,#148698,#148699,#148700,#148701,#148702,#148703,
#148704,#148705,#148706,#148707,#148708,#148709,#148710,#148711,#148712,
#148713,#148714,#148715,#148716,#148717,#148718,#148719,#148720,#148721,
#148722,#148723,#148724,#148725,#148726,#148727,#148728,#148729,#148730,
#148731,#148732,#148733,#148734,#148735,#148736,#148737,#148738,#148739,
#148740,#148741,#148742,#148743,#148744,#148745,#148746,#148747,#148748,
#148749,#148750,#148751,#148752,#148753,#148754,#148755,#148756,#148757,
#148758,#148759,#148760,#148761,#148762,#148763,#148764,#148765,#148766,
#148767,#148768,#148769,#148770,#148771,#148772,#148773,#148774,#148775,
#148776,#148777,#148778,#148779,#148780,#148781,#148782,#148783,#148784,
#148785,#148786,#148787,#148788,#148789,#148790,#148791,#148792,#148793,
#148794,#148795,#148796,#148797,#148798,#148799,#148800,#148801,#148802,
#148803,#148804,#148805,#148806,#148807,#148808,#148809,#148810,#148811,
#148812,#148813,#148814,#148815,#148816,#148817,#148818,#148819,#148820,
#148821,#148822,#148823,#148824,#148825,#148826,#148827,#148828,#148829,
#148830,#148831,#148832,#148833,#148834,#148835,#148836),.UNSPECIFIED.,
 .F.,.F.)
B_SPLINE_CURVE_WITH_KNOTS((6,1,1,1,1,1,1,1,1,1,1,1,1,1,1,1,1,1,1,1,1,1,
1,1,1,1,1,1,1,1,1,1,1,1,1,1,1,1,1,1,1,1,1,1,1,1,1,1,1,1,1,1,1,1,1,1,1,1,
1,1,1,1,1,1,1,1,1,1,1,1,1,1,1,1,1,1,1,1,1,1,1,1,1,1,1,1,1,1,1,1,1,1,1,1,
1,1,1,1,1,1,1,1,1,1,1,1,1,1,1,1,1,1,1,1,1,1,1,1,1,1,1,1,1,1,1,1,1,1,1,1,
1,1,1,1,1,1,1,1,1,1,1,1,1,1,1,1,1,1,1,1,1,1,1,1,1,1,1,1,1,1,1,1,1,1,1,1,
1,1,1,1,1,1,1,1,1,1,1,1,1,1,1,1,1,1,1,1,1,1,1,6),(0.,0.005,0.01,0.015,0.02,
0.025,0.03,0.035,0.04,0.045,0.05,0.055,0.06,0.065,0.07,0.075,0.08,0.085,
0.09,0.095,0.1,0.105,0.11,0.115,0.12,0.125,0.13,0.135,0.14,0.145,0.15,0.155,
0.16,0.165,0.17,0.175,0.18,0.185,0.19,0.195,0.2,0.205,0.21,0.215,0.22,0.225,
0.23,0.235,0.24,0.245,0.25,0.255,0.26,0.265,0.27,0.275,0.28,0.285,0.29,
0.295,0.3,0.305,0.31,0.315,0.32,0.325,0.33,0.335,0.34,0.345,0.35,0.355,
0.36,0.365,0.37,0.375,0.38,0.385,0.39,0.395,0.4,0.405,0.41,0.415,0.42,0.425,
0.43,0.435,0.44,0.445,0.45,0.455,0.46,0.465,0.47,0.475,0.48,0.485,0.49,
0.495,0.5,0.505,0.51,0.515,0.52,0.525,0.53,0.535,0.54,0.545,0.55,0.555,
0.56,0.565,0.57,0.575,0.58,0.585,0.59,0.595,0.6,0.605,0.61,0.615,0.62,0.625,
0.63,0.635,0.64,0.645,0.65,0.655,0.66,0.665,0.67,0.675,0.68,0.685,0.690000000000001,
0.695000000000001,0.700000000000001,0.705000000000001,0.710000000000001,
0.715000000000001,0.720000000000001,0.725000000000001,0.730000000000001,
0.735000000000001,0.740000000000001,0.745000000000001,0.750000000000001,
0.755000000000001,0.760000000000001,0.765000000000001,0.770000000000001,
0.775000000000001,0.780000000000001,0.785000000000001,0.790000000000001,
0.795000000000001,0.800000000000001,0.805000000000001,0.810000000000001,
0.815000000000001,0.820000000000001,0.825000000000001,0.830000000000001,
0.835000000000001,0.840000000000001,0.845000000000001,0.850000000000001,
0.855000000000001,0.860000000000001,0.865000000000001,0.870000000000001,
0.875000000000001,0.880000000000001,0.885000000000001,0.890000000000001,
0.895000000000001,0.900000000000001,0.905000000000001,0.910000000000001,
0.915000000000001,0.920000000000001,0.925000000000001,0.930000000000001,
0.935000000000001,0.940000000000001,0.941429844438009),.UNSPECIFIED.)
CURVE()
GEOMETRIC_REPRESENTATION_ITEM()
RATIONAL_B_SPLINE_CURVE((1.,1.,1.,1.,1.,1.,1.,1.,1.,1.,1.,1.,1.,1.,1.,1.,
1.,1.,1.,1.,1.,1.,1.,1.,1.,1.,1.,1.,1.,1.,1.,1.,1.,1.,1.,1.,1.,1.,1.,1.,
1.,1.,1.,1.,1.,1.,1.,1.,1.,1.,1.,1.,1.,1.,1.,1.,1.,1.,1.,1.,1.,1.,1.,1.,
1.,1.,1.,1.,1.,1.,1.,1.,1.,1.,1.,1.,1.,1.,1.,1.,1.,1.,1.,1.,1.,1.,1.,1.,
1.,1.,1.,1.,1.,1.,1.,1.,1.,1.,1.,1.,1.,1.,1.,1.,1.,1.,1.,1.,1.,1.,1.,1.,
1.,1.,1.,1.,1.,1.,1.,1.,1.,1.,1.,1.,1.,1.,1.,1.,1.,1.,1.,1.,1.,1.,1.,1.,
1.,1.,1.,1.,1.,1.,1.,1.,1.,1.,1.,1.,1.,1.,1.,1.,1.,1.,1.,1.,1.,1.,1.,1.,
1.,1.,1.,1.,1.,1.,1.,1.,1.,1.,1.,1.,1.,1.,1.,1.,1.,1.,1.,1.,1.,1.,1.,1.,
1.,1.,1.,1.,1.,1.,1.,1.,1.,1.))
REPRESENTATION_ITEM('')
);
#626=(
BOUNDED_CURVE()
B_SPLINE_CURVE(5,(#148839,#148840,#148841,#148842,#148843,#148844,#148845,
#148846,#148847,#148848,#148849,#148850,#148851,#148852,#148853,#148854,
#148855,#148856,#148857,#148858,#148859,#148860,#148861,#148862,#148863,
#148864,#148865,#148866,#148867,#148868,#148869,#148870,#148871,#148872,
#148873,#148874,#148875,#148876,#148877,#148878,#148879,#148880,#148881,
#148882,#148883,#148884,#148885,#148886,#148887,#148888,#148889,#148890,
#148891,#148892,#148893,#148894,#148895,#148896,#148897,#148898,#148899,
#148900,#148901,#148902,#148903,#148904,#148905,#148906,#148907,#148908,
#148909,#148910,#148911,#148912,#148913,#148914,#148915,#148916,#148917,
#148918,#148919,#148920,#148921,#148922,#148923,#148924,#148925,#148926,
#148927,#148928,#148929,#148930,#148931,#148932,#148933,#148934,#148935,
#148936,#148937,#148938,#148939,#148940,#148941,#148942,#148943,#148944,
#148945,#148946,#148947,#148948,#148949,#148950,#148951,#148952,#148953,
#148954,#148955,#148956,#148957,#148958,#148959,#148960,#148961,#148962,
#148963,#148964,#148965,#148966,#148967,#148968,#148969,#148970,#148971,
#148972,#148973,#148974,#148975,#148976,#148977,#148978,#148979,#148980,
#148981,#148982,#148983,#148984,#148985,#148986,#148987,#148988,#148989,
#148990,#148991,#148992,#148993,#148994,#148995,#148996,#148997,#148998,
#148999,#149000,#149001,#149002,#149003,#149004,#149005,#149006,#149007,
#149008,#149009,#149010,#149011,#149012,#149013,#149014,#149015,#149016,
#149017,#149018,#149019,#149020,#149021,#149022,#149023,#149024,#149025,
#149026,#149027,#149028,#149029,#149030,#149031,#149032),.UNSPECIFIED.,
 .F.,.F.)
B_SPLINE_CURVE_WITH_KNOTS((6,1,1,1,1,1,1,1,1,1,1,1,1,1,1,1,1,1,1,1,1,1,
1,1,1,1,1,1,1,1,1,1,1,1,1,1,1,1,1,1,1,1,1,1,1,1,1,1,1,1,1,1,1,1,1,1,1,1,
1,1,1,1,1,1,1,1,1,1,1,1,1,1,1,1,1,1,1,1,1,1,1,1,1,1,1,1,1,1,1,1,1,1,1,1,
1,1,1,1,1,1,1,1,1,1,1,1,1,1,1,1,1,1,1,1,1,1,1,1,1,1,1,1,1,1,1,1,1,1,1,1,
1,1,1,1,1,1,1,1,1,1,1,1,1,1,1,1,1,1,1,1,1,1,1,1,1,1,1,1,1,1,1,1,1,1,1,1,
1,1,1,1,1,1,1,1,1,1,1,1,1,1,1,1,1,1,1,1,1,1,1,6),(-0.941429844438009,-0.940000000000001,
-0.935000000000001,-0.930000000000001,-0.925000000000001,-0.920000000000001,
-0.915000000000001,-0.910000000000001,-0.905000000000001,-0.900000000000001,
-0.895000000000001,-0.890000000000001,-0.885000000000001,-0.880000000000001,
-0.875000000000001,-0.870000000000001,-0.865000000000001,-0.860000000000001,
-0.855000000000001,-0.850000000000001,-0.845000000000001,-0.840000000000001,
-0.835000000000001,-0.830000000000001,-0.825000000000001,-0.820000000000001,
-0.815000000000001,-0.810000000000001,-0.805000000000001,-0.800000000000001,
-0.795000000000001,-0.790000000000001,-0.785000000000001,-0.780000000000001,
-0.775000000000001,-0.770000000000001,-0.765000000000001,-0.760000000000001,
-0.755000000000001,-0.750000000000001,-0.745000000000001,-0.740000000000001,
-0.735000000000001,-0.730000000000001,-0.725000000000001,-0.720000000000001,
-0.715000000000001,-0.710000000000001,-0.705000000000001,-0.700000000000001,
-0.695000000000001,-0.690000000000001,-0.685,-0.68,-0.675,-0.67,-0.665,
-0.66,-0.655,-0.65,-0.645,-0.64,-0.635,-0.63,-0.625,-0.62,-0.615,-0.61,
-0.605,-0.6,-0.595,-0.59,-0.585,-0.58,-0.575,-0.57,-0.565,-0.56,-0.555,
-0.55,-0.545,-0.54,-0.535,-0.53,-0.525,-0.52,-0.515,-0.51,-0.505,-0.5,-0.495,
-0.49,-0.485,-0.48,-0.475,-0.47,-0.465,-0.46,-0.455,-0.45,-0.445,-0.44,
-0.435,-0.43,-0.425,-0.42,-0.415,-0.41,-0.405,-0.4,-0.395,-0.39,-0.385,
-0.38,-0.375,-0.37,-0.365,-0.36,-0.355,-0.35,-0.345,-0.34,-0.335,-0.33,
-0.325,-0.32,-0.315,-0.31,-0.305,-0.3,-0.295,-0.29,-0.285,-0.28,-0.275,
-0.27,-0.265,-0.26,-0.255,-0.25,-0.245,-0.24,-0.235,-0.23,-0.225,-0.22,
-0.215,-0.21,-0.205,-0.2,-0.195,-0.19,-0.185,-0.18,-0.175,-0.17,-0.165,
-0.16,-0.155,-0.15,-0.145,-0.14,-0.135,-0.13,-0.125,-0.12,-0.115,-0.11,
-0.105,-0.1,-0.095,-0.09,-0.085,-0.08,-0.075,-0.07,-0.065,-0.06,-0.055,
-0.05,-0.045,-0.04,-0.035,-0.03,-0.025,-0.02,-0.015,-0.01,-0.005,0.),
 .UNSPECIFIED.)
CURVE()
GEOMETRIC_REPRESENTATION_ITEM()
RATIONAL_B_SPLINE_CURVE((1.,1.,1.,1.,1.,1.,1.,1.,1.,1.,1.,1.,1.,1.,1.,1.,
1.,1.,1.,1.,1.,1.,1.,1.,1.,1.,1.,1.,1.,1.,1.,1.,1.,1.,1.,1.,1.,1.,1.,1.,
1.,1.,1.,1.,1.,1.,1.,1.,1.,1.,1.,1.,1.,1.,1.,1.,1.,1.,1.,1.,1.,1.,1.,1.,
1.,1.,1.,1.,1.,1.,1.,1.,1.,1.,1.,1.,1.,1.,1.,1.,1.,1.,1.,1.,1.,1.,1.,1.,
1.,1.,1.,1.,1.,1.,1.,1.,1.,1.,1.,1.,1.,1.,1.,1.,1.,1.,1.,1.,1.,1.,1.,1.,
1.,1.,1.,1.,1.,1.,1.,1.,1.,1.,1.,1.,1.,1.,1.,1.,1.,1.,1.,1.,1.,1.,1.,1.,
1.,1.,1.,1.,1.,1.,1.,1.,1.,1.,1.,1.,1.,1.,1.,1.,1.,1.,1.,1.,1.,1.,1.,1.,
1.,1.,1.,1.,1.,1.,1.,1.,1.,1.,1.,1.,1.,1.,1.,1.,1.,1.,1.,1.,1.,1.,1.,1.,
1.,1.,1.,1.,1.,1.,1.,1.,1.,1.))
REPRESENTATION_ITEM('')
);
#627=(
BOUNDED_CURVE()
B_SPLINE_CURVE(5,(#149444,#149445,#149446,#149447,#149448,#149449,#149450,
#149451,#149452,#149453,#149454,#149455,#149456,#149457,#149458,#149459,
#149460,#149461,#149462,#149463,#149464,#149465,#149466,#149467,#149468,
#149469,#149470,#149471,#149472,#149473,#149474,#149475,#149476,#149477,
#149478,#149479,#149480,#149481,#149482,#149483,#149484,#149485,#149486,
#149487,#149488,#149489,#149490,#149491,#149492,#149493,#149494,#149495,
#149496,#149497,#149498,#149499,#149500,#149501,#149502,#149503,#149504,
#149505,#149506,#149507,#149508,#149509,#149510,#149511,#149512,#149513,
#149514,#149515,#149516,#149517,#149518,#149519,#149520,#149521,#149522,
#149523,#149524,#149525,#149526,#149527,#149528,#149529,#149530,#149531,
#149532,#149533,#149534,#149535,#149536,#149537,#149538,#149539,#149540,
#149541,#149542,#149543,#149544,#149545,#149546,#149547,#149548,#149549,
#149550,#149551,#149552,#149553,#149554,#149555,#149556,#149557,#149558,
#149559,#149560,#149561,#149562,#149563,#149564,#149565,#149566,#149567,
#149568,#149569,#149570,#149571,#149572,#149573,#149574,#149575,#149576,
#149577,#149578,#149579,#149580,#149581,#149582,#149583,#149584,#149585,
#149586,#149587,#149588,#149589,#149590,#149591,#149592,#149593,#149594,
#149595,#149596,#149597,#149598,#149599,#149600,#149601,#149602,#149603,
#149604,#149605,#149606,#149607,#149608,#149609,#149610,#149611,#149612,
#149613,#149614,#149615,#149616,#149617,#149618,#149619,#149620,#149621,
#149622,#149623,#149624,#149625,#149626,#149627,#149628,#149629,#149630,
#149631,#149632,#149633,#149634,#149635,#149636,#149637),.UNSPECIFIED.,
 .F.,.F.)
B_SPLINE_CURVE_WITH_KNOTS((6,1,1,1,1,1,1,1,1,1,1,1,1,1,1,1,1,1,1,1,1,1,
1,1,1,1,1,1,1,1,1,1,1,1,1,1,1,1,1,1,1,1,1,1,1,1,1,1,1,1,1,1,1,1,1,1,1,1,
1,1,1,1,1,1,1,1,1,1,1,1,1,1,1,1,1,1,1,1,1,1,1,1,1,1,1,1,1,1,1,1,1,1,1,1,
1,1,1,1,1,1,1,1,1,1,1,1,1,1,1,1,1,1,1,1,1,1,1,1,1,1,1,1,1,1,1,1,1,1,1,1,
1,1,1,1,1,1,1,1,1,1,1,1,1,1,1,1,1,1,1,1,1,1,1,1,1,1,1,1,1,1,1,1,1,1,1,1,
1,1,1,1,1,1,1,1,1,1,1,1,1,1,1,1,1,1,1,1,1,1,1,6),(0.,0.005,0.01,0.015,0.02,
0.025,0.03,0.035,0.04,0.045,0.05,0.055,0.06,0.065,0.07,0.075,0.08,0.085,
0.09,0.095,0.1,0.105,0.11,0.115,0.12,0.125,0.13,0.135,0.14,0.145,0.15,0.155,
0.16,0.165,0.17,0.175,0.18,0.185,0.19,0.195,0.2,0.205,0.21,0.215,0.22,0.225,
0.23,0.235,0.24,0.245,0.25,0.255,0.26,0.265,0.27,0.275,0.28,0.285,0.29,
0.295,0.3,0.305,0.31,0.315,0.32,0.325,0.33,0.335,0.34,0.345,0.35,0.355,
0.36,0.365,0.37,0.375,0.38,0.385,0.39,0.395,0.4,0.405,0.41,0.415,0.42,0.425,
0.43,0.435,0.44,0.445,0.45,0.455,0.46,0.465,0.47,0.475,0.48,0.485,0.49,
0.495,0.5,0.505,0.51,0.515,0.52,0.525,0.53,0.535,0.54,0.545,0.55,0.555,
0.56,0.565,0.57,0.575,0.58,0.585,0.59,0.595,0.6,0.605,0.61,0.615,0.62,0.625,
0.63,0.635,0.64,0.645,0.65,0.655,0.66,0.665,0.67,0.675,0.68,0.685,0.690000000000001,
0.695000000000001,0.700000000000001,0.705000000000001,0.710000000000001,
0.715000000000001,0.720000000000001,0.725000000000001,0.730000000000001,
0.735000000000001,0.740000000000001,0.745000000000001,0.750000000000001,
0.755000000000001,0.760000000000001,0.765000000000001,0.770000000000001,
0.775000000000001,0.780000000000001,0.785000000000001,0.790000000000001,
0.795000000000001,0.800000000000001,0.805000000000001,0.810000000000001,
0.815000000000001,0.820000000000001,0.825000000000001,0.830000000000001,
0.835000000000001,0.840000000000001,0.845000000000001,0.850000000000001,
0.855000000000001,0.860000000000001,0.865000000000001,0.870000000000001,
0.875000000000001,0.880000000000001,0.885000000000001,0.890000000000001,
0.895000000000001,0.900000000000001,0.905000000000001,0.910000000000001,
0.915000000000001,0.920000000000001,0.925000000000001,0.930000000000001,
0.935000000000001,0.940000000000001,0.941429844438207),.UNSPECIFIED.)
CURVE()
GEOMETRIC_REPRESENTATION_ITEM()
RATIONAL_B_SPLINE_CURVE((1.,1.,1.,1.,1.,1.,1.,1.,1.,1.,1.,1.,1.,1.,1.,1.,
1.,1.,1.,1.,1.,1.,1.,1.,1.,1.,1.,1.,1.,1.,1.,1.,1.,1.,1.,1.,1.,1.,1.,1.,
1.,1.,1.,1.,1.,1.,1.,1.,1.,1.,1.,1.,1.,1.,1.,1.,1.,1.,1.,1.,1.,1.,1.,1.,
1.,1.,1.,1.,1.,1.,1.,1.,1.,1.,1.,1.,1.,1.,1.,1.,1.,1.,1.,1.,1.,1.,1.,1.,
1.,1.,1.,1.,1.,1.,1.,1.,1.,1.,1.,1.,1.,1.,1.,1.,1.,1.,1.,1.,1.,1.,1.,1.,
1.,1.,1.,1.,1.,1.,1.,1.,1.,1.,1.,1.,1.,1.,1.,1.,1.,1.,1.,1.,1.,1.,1.,1.,
1.,1.,1.,1.,1.,1.,1.,1.,1.,1.,1.,1.,1.,1.,1.,1.,1.,1.,1.,1.,1.,1.,1.,1.,
1.,1.,1.,1.,1.,1.,1.,1.,1.,1.,1.,1.,1.,1.,1.,1.,1.,1.,1.,1.,1.,1.,1.,1.,
1.,1.,1.,1.,1.,1.,1.,1.,1.,1.))
REPRESENTATION_ITEM('')
);
#628=(
BOUNDED_CURVE()
B_SPLINE_CURVE(5,(#149640,#149641,#149642,#149643,#149644,#149645,#149646,
#149647,#149648,#149649,#149650,#149651,#149652,#149653,#149654,#149655,
#149656,#149657,#149658,#149659,#149660,#149661,#149662,#149663,#149664,
#149665,#149666,#149667,#149668,#149669,#149670,#149671,#149672,#149673,
#149674,#149675,#149676,#149677,#149678,#149679,#149680,#149681,#149682,
#149683,#149684,#149685,#149686,#149687,#149688,#149689,#149690,#149691,
#149692,#149693,#149694,#149695,#149696,#149697,#149698,#149699,#149700,
#149701,#149702,#149703,#149704,#149705,#149706,#149707,#149708,#149709,
#149710,#149711,#149712,#149713,#149714,#149715,#149716,#149717,#149718,
#149719,#149720,#149721,#149722,#149723,#149724,#149725,#149726,#149727,
#149728,#149729,#149730,#149731,#149732,#149733,#149734,#149735,#149736,
#149737,#149738,#149739,#149740,#149741,#149742,#149743,#149744,#149745,
#149746,#149747,#149748,#149749,#149750,#149751,#149752,#149753,#149754,
#149755,#149756,#149757,#149758,#149759,#149760,#149761,#149762,#149763,
#149764,#149765,#149766,#149767,#149768,#149769,#149770,#149771,#149772,
#149773,#149774,#149775,#149776,#149777,#149778,#149779,#149780,#149781,
#149782,#149783,#149784,#149785,#149786,#149787,#149788,#149789,#149790,
#149791,#149792,#149793,#149794,#149795,#149796,#149797,#149798,#149799,
#149800,#149801,#149802,#149803,#149804,#149805,#149806,#149807,#149808,
#149809,#149810,#149811,#149812,#149813,#149814,#149815,#149816,#149817,
#149818,#149819,#149820,#149821,#149822,#149823,#149824,#149825,#149826,
#149827,#149828,#149829,#149830,#149831,#149832,#149833),.UNSPECIFIED.,
 .F.,.F.)
B_SPLINE_CURVE_WITH_KNOTS((6,1,1,1,1,1,1,1,1,1,1,1,1,1,1,1,1,1,1,1,1,1,
1,1,1,1,1,1,1,1,1,1,1,1,1,1,1,1,1,1,1,1,1,1,1,1,1,1,1,1,1,1,1,1,1,1,1,1,
1,1,1,1,1,1,1,1,1,1,1,1,1,1,1,1,1,1,1,1,1,1,1,1,1,1,1,1,1,1,1,1,1,1,1,1,
1,1,1,1,1,1,1,1,1,1,1,1,1,1,1,1,1,1,1,1,1,1,1,1,1,1,1,1,1,1,1,1,1,1,1,1,
1,1,1,1,1,1,1,1,1,1,1,1,1,1,1,1,1,1,1,1,1,1,1,1,1,1,1,1,1,1,1,1,1,1,1,1,
1,1,1,1,1,1,1,1,1,1,1,1,1,1,1,1,1,1,1,1,1,1,1,6),(-0.941429844438208,-0.940000000000001,
-0.935000000000001,-0.930000000000001,-0.925000000000001,-0.920000000000001,
-0.915000000000001,-0.910000000000001,-0.905000000000001,-0.900000000000001,
-0.895000000000001,-0.890000000000001,-0.885000000000001,-0.880000000000001,
-0.875000000000001,-0.870000000000001,-0.865000000000001,-0.860000000000001,
-0.855000000000001,-0.850000000000001,-0.845000000000001,-0.840000000000001,
-0.835000000000001,-0.830000000000001,-0.825000000000001,-0.820000000000001,
-0.815000000000001,-0.810000000000001,-0.805000000000001,-0.800000000000001,
-0.795000000000001,-0.790000000000001,-0.785000000000001,-0.780000000000001,
-0.775000000000001,-0.770000000000001,-0.765000000000001,-0.760000000000001,
-0.755000000000001,-0.750000000000001,-0.745000000000001,-0.740000000000001,
-0.735000000000001,-0.730000000000001,-0.725000000000001,-0.720000000000001,
-0.715000000000001,-0.710000000000001,-0.705000000000001,-0.700000000000001,
-0.695000000000001,-0.690000000000001,-0.685,-0.68,-0.675,-0.67,-0.665,
-0.66,-0.655,-0.65,-0.645,-0.64,-0.635,-0.63,-0.625,-0.62,-0.615,-0.61,
-0.605,-0.6,-0.595,-0.59,-0.585,-0.58,-0.575,-0.57,-0.565,-0.56,-0.555,
-0.55,-0.545,-0.54,-0.535,-0.53,-0.525,-0.52,-0.515,-0.51,-0.505,-0.5,-0.495,
-0.49,-0.485,-0.48,-0.475,-0.47,-0.465,-0.46,-0.455,-0.45,-0.445,-0.44,
-0.435,-0.43,-0.425,-0.42,-0.415,-0.41,-0.405,-0.4,-0.395,-0.39,-0.385,
-0.38,-0.375,-0.37,-0.365,-0.36,-0.355,-0.35,-0.345,-0.34,-0.335,-0.33,
-0.325,-0.32,-0.315,-0.31,-0.305,-0.3,-0.295,-0.29,-0.285,-0.28,-0.275,
-0.27,-0.265,-0.26,-0.255,-0.25,-0.245,-0.24,-0.235,-0.23,-0.225,-0.22,
-0.215,-0.21,-0.205,-0.2,-0.195,-0.19,-0.185,-0.18,-0.175,-0.17,-0.165,
-0.16,-0.155,-0.15,-0.145,-0.14,-0.135,-0.13,-0.125,-0.12,-0.115,-0.11,
-0.105,-0.1,-0.095,-0.09,-0.085,-0.08,-0.075,-0.07,-0.065,-0.06,-0.055,
-0.05,-0.045,-0.04,-0.035,-0.03,-0.025,-0.02,-0.015,-0.01,-0.005,0.),
 .UNSPECIFIED.)
CURVE()
GEOMETRIC_REPRESENTATION_ITEM()
RATIONAL_B_SPLINE_CURVE((1.,1.,1.,1.,1.,1.,1.,1.,1.,1.,1.,1.,1.,1.,1.,1.,
1.,1.,1.,1.,1.,1.,1.,1.,1.,1.,1.,1.,1.,1.,1.,1.,1.,1.,1.,1.,1.,1.,1.,1.,
1.,1.,1.,1.,1.,1.,1.,1.,1.,1.,1.,1.,1.,1.,1.,1.,1.,1.,1.,1.,1.,1.,1.,1.,
1.,1.,1.,1.,1.,1.,1.,1.,1.,1.,1.,1.,1.,1.,1.,1.,1.,1.,1.,1.,1.,1.,1.,1.,
1.,1.,1.,1.,1.,1.,1.,1.,1.,1.,1.,1.,1.,1.,1.,1.,1.,1.,1.,1.,1.,1.,1.,1.,
1.,1.,1.,1.,1.,1.,1.,1.,1.,1.,1.,1.,1.,1.,1.,1.,1.,1.,1.,1.,1.,1.,1.,1.,
1.,1.,1.,1.,1.,1.,1.,1.,1.,1.,1.,1.,1.,1.,1.,1.,1.,1.,1.,1.,1.,1.,1.,1.,
1.,1.,1.,1.,1.,1.,1.,1.,1.,1.,1.,1.,1.,1.,1.,1.,1.,1.,1.,1.,1.,1.,1.,1.,
1.,1.,1.,1.,1.,1.,1.,1.,1.,1.))
REPRESENTATION_ITEM('')
);
#629=(
BOUNDED_CURVE()
B_SPLINE_CURVE(5,(#150245,#150246,#150247,#150248,#150249,#150250,#150251,
#150252,#150253,#150254,#150255,#150256,#150257,#150258,#150259,#150260,
#150261,#150262,#150263,#150264,#150265,#150266,#150267,#150268,#150269,
#150270,#150271,#150272,#150273,#150274,#150275,#150276,#150277,#150278,
#150279,#150280,#150281,#150282,#150283,#150284,#150285,#150286,#150287,
#150288,#150289,#150290,#150291,#150292,#150293,#150294,#150295,#150296,
#150297,#150298,#150299,#150300,#150301,#150302,#150303,#150304,#150305,
#150306,#150307,#150308,#150309,#150310,#150311,#150312,#150313,#150314,
#150315,#150316,#150317,#150318,#150319,#150320,#150321,#150322,#150323,
#150324,#150325,#150326,#150327,#150328,#150329,#150330,#150331,#150332,
#150333,#150334,#150335,#150336,#150337,#150338,#150339,#150340,#150341,
#150342,#150343,#150344,#150345,#150346,#150347,#150348,#150349,#150350,
#150351,#150352,#150353,#150354,#150355,#150356,#150357,#150358,#150359,
#150360,#150361,#150362,#150363,#150364,#150365,#150366,#150367,#150368,
#150369,#150370,#150371,#150372,#150373,#150374,#150375,#150376,#150377,
#150378,#150379,#150380,#150381,#150382,#150383,#150384,#150385,#150386,
#150387,#150388,#150389,#150390,#150391,#150392,#150393,#150394,#150395,
#150396,#150397,#150398,#150399,#150400,#150401,#150402,#150403,#150404,
#150405,#150406,#150407,#150408,#150409,#150410,#150411,#150412,#150413,
#150414,#150415,#150416,#150417,#150418,#150419,#150420,#150421,#150422,
#150423,#150424,#150425,#150426,#150427,#150428,#150429,#150430,#150431,
#150432,#150433,#150434,#150435,#150436,#150437,#150438),.UNSPECIFIED.,
 .F.,.F.)
B_SPLINE_CURVE_WITH_KNOTS((6,1,1,1,1,1,1,1,1,1,1,1,1,1,1,1,1,1,1,1,1,1,
1,1,1,1,1,1,1,1,1,1,1,1,1,1,1,1,1,1,1,1,1,1,1,1,1,1,1,1,1,1,1,1,1,1,1,1,
1,1,1,1,1,1,1,1,1,1,1,1,1,1,1,1,1,1,1,1,1,1,1,1,1,1,1,1,1,1,1,1,1,1,1,1,
1,1,1,1,1,1,1,1,1,1,1,1,1,1,1,1,1,1,1,1,1,1,1,1,1,1,1,1,1,1,1,1,1,1,1,1,
1,1,1,1,1,1,1,1,1,1,1,1,1,1,1,1,1,1,1,1,1,1,1,1,1,1,1,1,1,1,1,1,1,1,1,1,
1,1,1,1,1,1,1,1,1,1,1,1,1,1,1,1,1,1,1,1,1,1,1,6),(0.,0.005,0.01,0.015,0.02,
0.025,0.03,0.035,0.04,0.045,0.05,0.055,0.06,0.065,0.07,0.075,0.08,0.085,
0.09,0.095,0.1,0.105,0.11,0.115,0.12,0.125,0.13,0.135,0.14,0.145,0.15,0.155,
0.16,0.165,0.17,0.175,0.18,0.185,0.19,0.195,0.2,0.205,0.21,0.215,0.22,0.225,
0.23,0.235,0.24,0.245,0.25,0.255,0.26,0.265,0.27,0.275,0.28,0.285,0.29,
0.295,0.3,0.305,0.31,0.315,0.32,0.325,0.33,0.335,0.34,0.345,0.35,0.355,
0.36,0.365,0.37,0.375,0.38,0.385,0.39,0.395,0.4,0.405,0.41,0.415,0.42,0.425,
0.43,0.435,0.44,0.445,0.45,0.455,0.46,0.465,0.47,0.475,0.48,0.485,0.49,
0.495,0.5,0.505,0.51,0.515,0.52,0.525,0.53,0.535,0.54,0.545,0.55,0.555,
0.56,0.565,0.57,0.575,0.58,0.585,0.59,0.595,0.6,0.605,0.61,0.615,0.62,0.625,
0.63,0.635,0.64,0.645,0.65,0.655,0.66,0.665,0.67,0.675,0.68,0.685,0.690000000000001,
0.695000000000001,0.700000000000001,0.705000000000001,0.710000000000001,
0.715000000000001,0.720000000000001,0.725000000000001,0.730000000000001,
0.735000000000001,0.740000000000001,0.745000000000001,0.750000000000001,
0.755000000000001,0.760000000000001,0.765000000000001,0.770000000000001,
0.775000000000001,0.780000000000001,0.785000000000001,0.790000000000001,
0.795000000000001,0.800000000000001,0.805000000000001,0.810000000000001,
0.815000000000001,0.820000000000001,0.825000000000001,0.830000000000001,
0.835000000000001,0.840000000000001,0.845000000000001,0.850000000000001,
0.855000000000001,0.860000000000001,0.865000000000001,0.870000000000001,
0.875000000000001,0.880000000000001,0.885000000000001,0.890000000000001,
0.895000000000001,0.900000000000001,0.905000000000001,0.910000000000001,
0.915000000000001,0.920000000000001,0.925000000000001,0.930000000000001,
0.935000000000001,0.940000000000001,0.941429844437998),.UNSPECIFIED.)
CURVE()
GEOMETRIC_REPRESENTATION_ITEM()
RATIONAL_B_SPLINE_CURVE((1.,1.,1.,1.,1.,1.,1.,1.,1.,1.,1.,1.,1.,1.,1.,1.,
1.,1.,1.,1.,1.,1.,1.,1.,1.,1.,1.,1.,1.,1.,1.,1.,1.,1.,1.,1.,1.,1.,1.,1.,
1.,1.,1.,1.,1.,1.,1.,1.,1.,1.,1.,1.,1.,1.,1.,1.,1.,1.,1.,1.,1.,1.,1.,1.,
1.,1.,1.,1.,1.,1.,1.,1.,1.,1.,1.,1.,1.,1.,1.,1.,1.,1.,1.,1.,1.,1.,1.,1.,
1.,1.,1.,1.,1.,1.,1.,1.,1.,1.,1.,1.,1.,1.,1.,1.,1.,1.,1.,1.,1.,1.,1.,1.,
1.,1.,1.,1.,1.,1.,1.,1.,1.,1.,1.,1.,1.,1.,1.,1.,1.,1.,1.,1.,1.,1.,1.,1.,
1.,1.,1.,1.,1.,1.,1.,1.,1.,1.,1.,1.,1.,1.,1.,1.,1.,1.,1.,1.,1.,1.,1.,1.,
1.,1.,1.,1.,1.,1.,1.,1.,1.,1.,1.,1.,1.,1.,1.,1.,1.,1.,1.,1.,1.,1.,1.,1.,
1.,1.,1.,1.,1.,1.,1.,1.,1.,1.))
REPRESENTATION_ITEM('')
);
#630=(
BOUNDED_CURVE()
B_SPLINE_CURVE(5,(#150441,#150442,#150443,#150444,#150445,#150446,#150447,
#150448,#150449,#150450,#150451,#150452,#150453,#150454,#150455,#150456,
#150457,#150458,#150459,#150460,#150461,#150462,#150463,#150464,#150465,
#150466,#150467,#150468,#150469,#150470,#150471,#150472,#150473,#150474,
#150475,#150476,#150477,#150478,#150479,#150480,#150481,#150482,#150483,
#150484,#150485,#150486,#150487,#150488,#150489,#150490,#150491,#150492,
#150493,#150494,#150495,#150496,#150497,#150498,#150499,#150500,#150501,
#150502,#150503,#150504,#150505,#150506,#150507,#150508,#150509,#150510,
#150511,#150512,#150513,#150514,#150515,#150516,#150517,#150518,#150519,
#150520,#150521,#150522,#150523,#150524,#150525,#150526,#150527,#150528,
#150529,#150530,#150531,#150532,#150533,#150534,#150535,#150536,#150537,
#150538,#150539,#150540,#150541,#150542,#150543,#150544,#150545,#150546,
#150547,#150548,#150549,#150550,#150551,#150552,#150553,#150554,#150555,
#150556,#150557,#150558,#150559,#150560,#150561,#150562,#150563,#150564,
#150565,#150566,#150567,#150568,#150569,#150570,#150571,#150572,#150573,
#150574,#150575,#150576,#150577,#150578,#150579,#150580,#150581,#150582,
#150583,#150584,#150585,#150586,#150587,#150588,#150589,#150590,#150591,
#150592,#150593,#150594,#150595,#150596,#150597,#150598,#150599,#150600,
#150601,#150602,#150603,#150604,#150605,#150606,#150607,#150608,#150609,
#150610,#150611,#150612,#150613,#150614,#150615,#150616,#150617,#150618,
#150619,#150620,#150621,#150622,#150623,#150624,#150625,#150626,#150627,
#150628,#150629,#150630,#150631,#150632,#150633,#150634),.UNSPECIFIED.,
 .F.,.F.)
B_SPLINE_CURVE_WITH_KNOTS((6,1,1,1,1,1,1,1,1,1,1,1,1,1,1,1,1,1,1,1,1,1,
1,1,1,1,1,1,1,1,1,1,1,1,1,1,1,1,1,1,1,1,1,1,1,1,1,1,1,1,1,1,1,1,1,1,1,1,
1,1,1,1,1,1,1,1,1,1,1,1,1,1,1,1,1,1,1,1,1,1,1,1,1,1,1,1,1,1,1,1,1,1,1,1,
1,1,1,1,1,1,1,1,1,1,1,1,1,1,1,1,1,1,1,1,1,1,1,1,1,1,1,1,1,1,1,1,1,1,1,1,
1,1,1,1,1,1,1,1,1,1,1,1,1,1,1,1,1,1,1,1,1,1,1,1,1,1,1,1,1,1,1,1,1,1,1,1,
1,1,1,1,1,1,1,1,1,1,1,1,1,1,1,1,1,1,1,1,1,1,1,6),(-0.941429844437991,-0.940000000000001,
-0.935000000000001,-0.930000000000001,-0.925000000000001,-0.920000000000001,
-0.915000000000001,-0.910000000000001,-0.905000000000001,-0.900000000000001,
-0.895000000000001,-0.890000000000001,-0.885000000000001,-0.880000000000001,
-0.875000000000001,-0.870000000000001,-0.865000000000001,-0.860000000000001,
-0.855000000000001,-0.850000000000001,-0.845000000000001,-0.840000000000001,
-0.835000000000001,-0.830000000000001,-0.825000000000001,-0.820000000000001,
-0.815000000000001,-0.810000000000001,-0.805000000000001,-0.800000000000001,
-0.795000000000001,-0.790000000000001,-0.785000000000001,-0.780000000000001,
-0.775000000000001,-0.770000000000001,-0.765000000000001,-0.760000000000001,
-0.755000000000001,-0.750000000000001,-0.745000000000001,-0.740000000000001,
-0.735000000000001,-0.730000000000001,-0.725000000000001,-0.720000000000001,
-0.715000000000001,-0.710000000000001,-0.705000000000001,-0.700000000000001,
-0.695000000000001,-0.690000000000001,-0.685,-0.68,-0.675,-0.67,-0.665,
-0.66,-0.655,-0.65,-0.645,-0.64,-0.635,-0.63,-0.625,-0.62,-0.615,-0.61,
-0.605,-0.6,-0.595,-0.59,-0.585,-0.58,-0.575,-0.57,-0.565,-0.56,-0.555,
-0.55,-0.545,-0.54,-0.535,-0.53,-0.525,-0.52,-0.515,-0.51,-0.505,-0.5,-0.495,
-0.49,-0.485,-0.48,-0.475,-0.47,-0.465,-0.46,-0.455,-0.45,-0.445,-0.44,
-0.435,-0.43,-0.425,-0.42,-0.415,-0.41,-0.405,-0.4,-0.395,-0.39,-0.385,
-0.38,-0.375,-0.37,-0.365,-0.36,-0.355,-0.35,-0.345,-0.34,-0.335,-0.33,
-0.325,-0.32,-0.315,-0.31,-0.305,-0.3,-0.295,-0.29,-0.285,-0.28,-0.275,
-0.27,-0.265,-0.26,-0.255,-0.25,-0.245,-0.24,-0.235,-0.23,-0.225,-0.22,
-0.215,-0.21,-0.205,-0.2,-0.195,-0.19,-0.185,-0.18,-0.175,-0.17,-0.165,
-0.16,-0.155,-0.15,-0.145,-0.14,-0.135,-0.13,-0.125,-0.12,-0.115,-0.11,
-0.105,-0.1,-0.095,-0.09,-0.085,-0.08,-0.075,-0.07,-0.065,-0.06,-0.055,
-0.05,-0.045,-0.04,-0.035,-0.03,-0.025,-0.02,-0.015,-0.01,-0.005,0.),
 .UNSPECIFIED.)
CURVE()
GEOMETRIC_REPRESENTATION_ITEM()
RATIONAL_B_SPLINE_CURVE((1.,1.,1.,1.,1.,1.,1.,1.,1.,1.,1.,1.,1.,1.,1.,1.,
1.,1.,1.,1.,1.,1.,1.,1.,1.,1.,1.,1.,1.,1.,1.,1.,1.,1.,1.,1.,1.,1.,1.,1.,
1.,1.,1.,1.,1.,1.,1.,1.,1.,1.,1.,1.,1.,1.,1.,1.,1.,1.,1.,1.,1.,1.,1.,1.,
1.,1.,1.,1.,1.,1.,1.,1.,1.,1.,1.,1.,1.,1.,1.,1.,1.,1.,1.,1.,1.,1.,1.,1.,
1.,1.,1.,1.,1.,1.,1.,1.,1.,1.,1.,1.,1.,1.,1.,1.,1.,1.,1.,1.,1.,1.,1.,1.,
1.,1.,1.,1.,1.,1.,1.,1.,1.,1.,1.,1.,1.,1.,1.,1.,1.,1.,1.,1.,1.,1.,1.,1.,
1.,1.,1.,1.,1.,1.,1.,1.,1.,1.,1.,1.,1.,1.,1.,1.,1.,1.,1.,1.,1.,1.,1.,1.,
1.,1.,1.,1.,1.,1.,1.,1.,1.,1.,1.,1.,1.,1.,1.,1.,1.,1.,1.,1.,1.,1.,1.,1.,
1.,1.,1.,1.,1.,1.,1.,1.,1.,1.))
REPRESENTATION_ITEM('')
);
#631=(
BOUNDED_CURVE()
B_SPLINE_CURVE(5,(#151046,#151047,#151048,#151049,#151050,#151051,#151052,
#151053,#151054,#151055,#151056,#151057,#151058,#151059,#151060,#151061,
#151062,#151063,#151064,#151065,#151066,#151067,#151068,#151069,#151070,
#151071,#151072,#151073,#151074,#151075,#151076,#151077,#151078,#151079,
#151080,#151081,#151082,#151083,#151084,#151085,#151086,#151087,#151088,
#151089,#151090,#151091,#151092,#151093,#151094,#151095,#151096,#151097,
#151098,#151099,#151100,#151101,#151102,#151103,#151104,#151105,#151106,
#151107,#151108,#151109,#151110,#151111,#151112,#151113,#151114,#151115,
#151116,#151117,#151118,#151119,#151120,#151121,#151122,#151123,#151124,
#151125,#151126,#151127,#151128,#151129,#151130,#151131,#151132,#151133,
#151134,#151135,#151136,#151137,#151138,#151139,#151140,#151141,#151142,
#151143,#151144,#151145,#151146,#151147,#151148,#151149,#151150,#151151,
#151152,#151153,#151154,#151155,#151156,#151157,#151158,#151159,#151160,
#151161,#151162,#151163,#151164,#151165,#151166,#151167,#151168,#151169,
#151170,#151171,#151172,#151173,#151174,#151175,#151176,#151177,#151178,
#151179,#151180,#151181,#151182,#151183,#151184,#151185,#151186,#151187,
#151188,#151189,#151190,#151191,#151192,#151193,#151194,#151195,#151196,
#151197,#151198,#151199,#151200,#151201,#151202,#151203,#151204,#151205,
#151206,#151207,#151208,#151209,#151210,#151211,#151212,#151213,#151214,
#151215,#151216,#151217,#151218,#151219,#151220,#151221,#151222,#151223,
#151224,#151225,#151226,#151227,#151228,#151229,#151230,#151231,#151232,
#151233,#151234,#151235,#151236,#151237,#151238,#151239),.UNSPECIFIED.,
 .F.,.F.)
B_SPLINE_CURVE_WITH_KNOTS((6,1,1,1,1,1,1,1,1,1,1,1,1,1,1,1,1,1,1,1,1,1,
1,1,1,1,1,1,1,1,1,1,1,1,1,1,1,1,1,1,1,1,1,1,1,1,1,1,1,1,1,1,1,1,1,1,1,1,
1,1,1,1,1,1,1,1,1,1,1,1,1,1,1,1,1,1,1,1,1,1,1,1,1,1,1,1,1,1,1,1,1,1,1,1,
1,1,1,1,1,1,1,1,1,1,1,1,1,1,1,1,1,1,1,1,1,1,1,1,1,1,1,1,1,1,1,1,1,1,1,1,
1,1,1,1,1,1,1,1,1,1,1,1,1,1,1,1,1,1,1,1,1,1,1,1,1,1,1,1,1,1,1,1,1,1,1,1,
1,1,1,1,1,1,1,1,1,1,1,1,1,1,1,1,1,1,1,1,1,1,1,6),(0.,0.005,0.01,0.015,0.02,
0.025,0.03,0.035,0.04,0.045,0.05,0.055,0.06,0.065,0.07,0.075,0.08,0.085,
0.09,0.095,0.1,0.105,0.11,0.115,0.12,0.125,0.13,0.135,0.14,0.145,0.15,0.155,
0.16,0.165,0.17,0.175,0.18,0.185,0.19,0.195,0.2,0.205,0.21,0.215,0.22,0.225,
0.23,0.235,0.24,0.245,0.25,0.255,0.26,0.265,0.27,0.275,0.28,0.285,0.29,
0.295,0.3,0.305,0.31,0.315,0.32,0.325,0.33,0.335,0.34,0.345,0.35,0.355,
0.36,0.365,0.37,0.375,0.38,0.385,0.39,0.395,0.4,0.405,0.41,0.415,0.42,0.425,
0.43,0.435,0.44,0.445,0.45,0.455,0.46,0.465,0.47,0.475,0.48,0.485,0.49,
0.495,0.5,0.505,0.51,0.515,0.52,0.525,0.53,0.535,0.54,0.545,0.55,0.555,
0.56,0.565,0.57,0.575,0.58,0.585,0.59,0.595,0.6,0.605,0.61,0.615,0.62,0.625,
0.63,0.635,0.64,0.645,0.65,0.655,0.66,0.665,0.67,0.675,0.68,0.685,0.690000000000001,
0.695000000000001,0.700000000000001,0.705000000000001,0.710000000000001,
0.715000000000001,0.720000000000001,0.725000000000001,0.730000000000001,
0.735000000000001,0.740000000000001,0.745000000000001,0.750000000000001,
0.755000000000001,0.760000000000001,0.765000000000001,0.770000000000001,
0.775000000000001,0.780000000000001,0.785000000000001,0.790000000000001,
0.795000000000001,0.800000000000001,0.805000000000001,0.810000000000001,
0.815000000000001,0.820000000000001,0.825000000000001,0.830000000000001,
0.835000000000001,0.840000000000001,0.845000000000001,0.850000000000001,
0.855000000000001,0.860000000000001,0.865000000000001,0.870000000000001,
0.875000000000001,0.880000000000001,0.885000000000001,0.890000000000001,
0.895000000000001,0.900000000000001,0.905000000000001,0.910000000000001,
0.915000000000001,0.920000000000001,0.925000000000001,0.930000000000001,
0.935000000000001,0.940000000000001,0.94142984443805),.UNSPECIFIED.)
CURVE()
GEOMETRIC_REPRESENTATION_ITEM()
RATIONAL_B_SPLINE_CURVE((1.,1.,1.,1.,1.,1.,1.,1.,1.,1.,1.,1.,1.,1.,1.,1.,
1.,1.,1.,1.,1.,1.,1.,1.,1.,1.,1.,1.,1.,1.,1.,1.,1.,1.,1.,1.,1.,1.,1.,1.,
1.,1.,1.,1.,1.,1.,1.,1.,1.,1.,1.,1.,1.,1.,1.,1.,1.,1.,1.,1.,1.,1.,1.,1.,
1.,1.,1.,1.,1.,1.,1.,1.,1.,1.,1.,1.,1.,1.,1.,1.,1.,1.,1.,1.,1.,1.,1.,1.,
1.,1.,1.,1.,1.,1.,1.,1.,1.,1.,1.,1.,1.,1.,1.,1.,1.,1.,1.,1.,1.,1.,1.,1.,
1.,1.,1.,1.,1.,1.,1.,1.,1.,1.,1.,1.,1.,1.,1.,1.,1.,1.,1.,1.,1.,1.,1.,1.,
1.,1.,1.,1.,1.,1.,1.,1.,1.,1.,1.,1.,1.,1.,1.,1.,1.,1.,1.,1.,1.,1.,1.,1.,
1.,1.,1.,1.,1.,1.,1.,1.,1.,1.,1.,1.,1.,1.,1.,1.,1.,1.,1.,1.,1.,1.,1.,1.,
1.,1.,1.,1.,1.,1.,1.,1.,1.,1.))
REPRESENTATION_ITEM('')
);
#632=(
BOUNDED_CURVE()
B_SPLINE_CURVE(5,(#151242,#151243,#151244,#151245,#151246,#151247,#151248,
#151249,#151250,#151251,#151252,#151253,#151254,#151255,#151256,#151257,
#151258,#151259,#151260,#151261,#151262,#151263,#151264,#151265,#151266,
#151267,#151268,#151269,#151270,#151271,#151272,#151273,#151274,#151275,
#151276,#151277,#151278,#151279,#151280,#151281,#151282,#151283,#151284,
#151285,#151286,#151287,#151288,#151289,#151290,#151291,#151292,#151293,
#151294,#151295,#151296,#151297,#151298,#151299,#151300,#151301,#151302,
#151303,#151304,#151305,#151306,#151307,#151308,#151309,#151310,#151311,
#151312,#151313,#151314,#151315,#151316,#151317,#151318,#151319,#151320,
#151321,#151322,#151323,#151324,#151325,#151326,#151327,#151328,#151329,
#151330,#151331,#151332,#151333,#151334,#151335,#151336,#151337,#151338,
#151339,#151340,#151341,#151342,#151343,#151344,#151345,#151346,#151347,
#151348,#151349,#151350,#151351,#151352,#151353,#151354,#151355,#151356,
#151357,#151358,#151359,#151360,#151361,#151362,#151363,#151364,#151365,
#151366,#151367,#151368,#151369,#151370,#151371,#151372,#151373,#151374,
#151375,#151376,#151377,#151378,#151379,#151380,#151381,#151382,#151383,
#151384,#151385,#151386,#151387,#151388,#151389,#151390,#151391,#151392,
#151393,#151394,#151395,#151396,#151397,#151398,#151399,#151400,#151401,
#151402,#151403,#151404,#151405,#151406,#151407,#151408,#151409,#151410,
#151411,#151412,#151413,#151414,#151415,#151416,#151417,#151418,#151419,
#151420,#151421,#151422,#151423,#151424,#151425,#151426,#151427,#151428,
#151429,#151430,#151431,#151432,#151433,#151434,#151435),.UNSPECIFIED.,
 .F.,.F.)
B_SPLINE_CURVE_WITH_KNOTS((6,1,1,1,1,1,1,1,1,1,1,1,1,1,1,1,1,1,1,1,1,1,
1,1,1,1,1,1,1,1,1,1,1,1,1,1,1,1,1,1,1,1,1,1,1,1,1,1,1,1,1,1,1,1,1,1,1,1,
1,1,1,1,1,1,1,1,1,1,1,1,1,1,1,1,1,1,1,1,1,1,1,1,1,1,1,1,1,1,1,1,1,1,1,1,
1,1,1,1,1,1,1,1,1,1,1,1,1,1,1,1,1,1,1,1,1,1,1,1,1,1,1,1,1,1,1,1,1,1,1,1,
1,1,1,1,1,1,1,1,1,1,1,1,1,1,1,1,1,1,1,1,1,1,1,1,1,1,1,1,1,1,1,1,1,1,1,1,
1,1,1,1,1,1,1,1,1,1,1,1,1,1,1,1,1,1,1,1,1,1,1,6),(-0.941429844438045,-0.940000000000001,
-0.935000000000001,-0.930000000000001,-0.925000000000001,-0.920000000000001,
-0.915000000000001,-0.910000000000001,-0.905000000000001,-0.900000000000001,
-0.895000000000001,-0.890000000000001,-0.885000000000001,-0.880000000000001,
-0.875000000000001,-0.870000000000001,-0.865000000000001,-0.860000000000001,
-0.855000000000001,-0.850000000000001,-0.845000000000001,-0.840000000000001,
-0.835000000000001,-0.830000000000001,-0.825000000000001,-0.820000000000001,
-0.815000000000001,-0.810000000000001,-0.805000000000001,-0.800000000000001,
-0.795000000000001,-0.790000000000001,-0.785000000000001,-0.780000000000001,
-0.775000000000001,-0.770000000000001,-0.765000000000001,-0.760000000000001,
-0.755000000000001,-0.750000000000001,-0.745000000000001,-0.740000000000001,
-0.735000000000001,-0.730000000000001,-0.725000000000001,-0.720000000000001,
-0.715000000000001,-0.710000000000001,-0.705000000000001,-0.700000000000001,
-0.695000000000001,-0.690000000000001,-0.685,-0.68,-0.675,-0.67,-0.665,
-0.66,-0.655,-0.65,-0.645,-0.64,-0.635,-0.63,-0.625,-0.62,-0.615,-0.61,
-0.605,-0.6,-0.595,-0.59,-0.585,-0.58,-0.575,-0.57,-0.565,-0.56,-0.555,
-0.55,-0.545,-0.54,-0.535,-0.53,-0.525,-0.52,-0.515,-0.51,-0.505,-0.5,-0.495,
-0.49,-0.485,-0.48,-0.475,-0.47,-0.465,-0.46,-0.455,-0.45,-0.445,-0.44,
-0.435,-0.43,-0.425,-0.42,-0.415,-0.41,-0.405,-0.4,-0.395,-0.39,-0.385,
-0.38,-0.375,-0.37,-0.365,-0.36,-0.355,-0.35,-0.345,-0.34,-0.335,-0.33,
-0.325,-0.32,-0.315,-0.31,-0.305,-0.3,-0.295,-0.29,-0.285,-0.28,-0.275,
-0.27,-0.265,-0.26,-0.255,-0.25,-0.245,-0.24,-0.235,-0.23,-0.225,-0.22,
-0.215,-0.21,-0.205,-0.2,-0.195,-0.19,-0.185,-0.18,-0.175,-0.17,-0.165,
-0.16,-0.155,-0.15,-0.145,-0.14,-0.135,-0.13,-0.125,-0.12,-0.115,-0.11,
-0.105,-0.1,-0.095,-0.09,-0.085,-0.08,-0.075,-0.07,-0.065,-0.06,-0.055,
-0.05,-0.045,-0.04,-0.035,-0.03,-0.025,-0.02,-0.015,-0.01,-0.005,0.),
 .UNSPECIFIED.)
CURVE()
GEOMETRIC_REPRESENTATION_ITEM()
RATIONAL_B_SPLINE_CURVE((1.,1.,1.,1.,1.,1.,1.,1.,1.,1.,1.,1.,1.,1.,1.,1.,
1.,1.,1.,1.,1.,1.,1.,1.,1.,1.,1.,1.,1.,1.,1.,1.,1.,1.,1.,1.,1.,1.,1.,1.,
1.,1.,1.,1.,1.,1.,1.,1.,1.,1.,1.,1.,1.,1.,1.,1.,1.,1.,1.,1.,1.,1.,1.,1.,
1.,1.,1.,1.,1.,1.,1.,1.,1.,1.,1.,1.,1.,1.,1.,1.,1.,1.,1.,1.,1.,1.,1.,1.,
1.,1.,1.,1.,1.,1.,1.,1.,1.,1.,1.,1.,1.,1.,1.,1.,1.,1.,1.,1.,1.,1.,1.,1.,
1.,1.,1.,1.,1.,1.,1.,1.,1.,1.,1.,1.,1.,1.,1.,1.,1.,1.,1.,1.,1.,1.,1.,1.,
1.,1.,1.,1.,1.,1.,1.,1.,1.,1.,1.,1.,1.,1.,1.,1.,1.,1.,1.,1.,1.,1.,1.,1.,
1.,1.,1.,1.,1.,1.,1.,1.,1.,1.,1.,1.,1.,1.,1.,1.,1.,1.,1.,1.,1.,1.,1.,1.,
1.,1.,1.,1.,1.,1.,1.,1.,1.,1.))
REPRESENTATION_ITEM('')
);
#633=(
BOUNDED_CURVE()
B_SPLINE_CURVE(5,(#151847,#151848,#151849,#151850,#151851,#151852,#151853,
#151854,#151855,#151856,#151857,#151858,#151859,#151860,#151861,#151862,
#151863,#151864,#151865,#151866,#151867,#151868,#151869,#151870,#151871,
#151872,#151873,#151874,#151875,#151876,#151877,#151878,#151879,#151880,
#151881,#151882,#151883,#151884,#151885,#151886,#151887,#151888,#151889,
#151890,#151891,#151892,#151893,#151894,#151895,#151896,#151897,#151898,
#151899,#151900,#151901,#151902,#151903,#151904,#151905,#151906,#151907,
#151908,#151909,#151910,#151911,#151912,#151913,#151914,#151915,#151916,
#151917,#151918,#151919,#151920,#151921,#151922,#151923,#151924,#151925,
#151926,#151927,#151928,#151929,#151930,#151931,#151932,#151933,#151934,
#151935,#151936,#151937,#151938,#151939,#151940,#151941,#151942,#151943,
#151944,#151945,#151946,#151947,#151948,#151949,#151950,#151951,#151952,
#151953,#151954,#151955,#151956,#151957,#151958,#151959,#151960,#151961,
#151962,#151963,#151964,#151965,#151966,#151967,#151968,#151969,#151970,
#151971,#151972,#151973,#151974,#151975,#151976,#151977,#151978,#151979,
#151980,#151981,#151982,#151983,#151984,#151985,#151986,#151987,#151988,
#151989,#151990,#151991,#151992,#151993,#151994,#151995,#151996,#151997,
#151998,#151999,#152000,#152001,#152002,#152003,#152004,#152005,#152006,
#152007,#152008,#152009,#152010,#152011,#152012,#152013,#152014,#152015,
#152016,#152017,#152018,#152019,#152020,#152021,#152022,#152023,#152024,
#152025,#152026,#152027,#152028,#152029,#152030,#152031,#152032,#152033,
#152034,#152035,#152036,#152037,#152038,#152039,#152040),.UNSPECIFIED.,
 .F.,.F.)
B_SPLINE_CURVE_WITH_KNOTS((6,1,1,1,1,1,1,1,1,1,1,1,1,1,1,1,1,1,1,1,1,1,
1,1,1,1,1,1,1,1,1,1,1,1,1,1,1,1,1,1,1,1,1,1,1,1,1,1,1,1,1,1,1,1,1,1,1,1,
1,1,1,1,1,1,1,1,1,1,1,1,1,1,1,1,1,1,1,1,1,1,1,1,1,1,1,1,1,1,1,1,1,1,1,1,
1,1,1,1,1,1,1,1,1,1,1,1,1,1,1,1,1,1,1,1,1,1,1,1,1,1,1,1,1,1,1,1,1,1,1,1,
1,1,1,1,1,1,1,1,1,1,1,1,1,1,1,1,1,1,1,1,1,1,1,1,1,1,1,1,1,1,1,1,1,1,1,1,
1,1,1,1,1,1,1,1,1,1,1,1,1,1,1,1,1,1,1,1,1,1,1,6),(0.,0.005,0.01,0.015,0.02,
0.025,0.03,0.035,0.04,0.045,0.05,0.055,0.06,0.065,0.07,0.075,0.08,0.085,
0.09,0.095,0.1,0.105,0.11,0.115,0.12,0.125,0.13,0.135,0.14,0.145,0.15,0.155,
0.16,0.165,0.17,0.175,0.18,0.185,0.19,0.195,0.2,0.205,0.21,0.215,0.22,0.225,
0.23,0.235,0.24,0.245,0.25,0.255,0.26,0.265,0.27,0.275,0.28,0.285,0.29,
0.295,0.3,0.305,0.31,0.315,0.32,0.325,0.33,0.335,0.34,0.345,0.35,0.355,
0.36,0.365,0.37,0.375,0.38,0.385,0.39,0.395,0.4,0.405,0.41,0.415,0.42,0.425,
0.43,0.435,0.44,0.445,0.45,0.455,0.46,0.465,0.47,0.475,0.48,0.485,0.49,
0.495,0.5,0.505,0.51,0.515,0.52,0.525,0.53,0.535,0.54,0.545,0.55,0.555,
0.56,0.565,0.57,0.575,0.58,0.585,0.59,0.595,0.6,0.605,0.61,0.615,0.62,0.625,
0.63,0.635,0.64,0.645,0.65,0.655,0.66,0.665,0.67,0.675,0.68,0.685,0.690000000000001,
0.695000000000001,0.700000000000001,0.705000000000001,0.710000000000001,
0.715000000000001,0.720000000000001,0.725000000000001,0.730000000000001,
0.735000000000001,0.740000000000001,0.745000000000001,0.750000000000001,
0.755000000000001,0.760000000000001,0.765000000000001,0.770000000000001,
0.775000000000001,0.780000000000001,0.785000000000001,0.790000000000001,
0.795000000000001,0.800000000000001,0.805000000000001,0.810000000000001,
0.815000000000001,0.820000000000001,0.825000000000001,0.830000000000001,
0.835000000000001,0.840000000000001,0.845000000000001,0.850000000000001,
0.855000000000001,0.860000000000001,0.865000000000001,0.870000000000001,
0.875000000000001,0.880000000000001,0.885000000000001,0.890000000000001,
0.895000000000001,0.900000000000001,0.905000000000001,0.910000000000001,
0.915000000000001,0.920000000000001,0.925000000000001,0.930000000000001,
0.935000000000001,0.940000000000001,0.94142984443799),.UNSPECIFIED.)
CURVE()
GEOMETRIC_REPRESENTATION_ITEM()
RATIONAL_B_SPLINE_CURVE((1.,1.,1.,1.,1.,1.,1.,1.,1.,1.,1.,1.,1.,1.,1.,1.,
1.,1.,1.,1.,1.,1.,1.,1.,1.,1.,1.,1.,1.,1.,1.,1.,1.,1.,1.,1.,1.,1.,1.,1.,
1.,1.,1.,1.,1.,1.,1.,1.,1.,1.,1.,1.,1.,1.,1.,1.,1.,1.,1.,1.,1.,1.,1.,1.,
1.,1.,1.,1.,1.,1.,1.,1.,1.,1.,1.,1.,1.,1.,1.,1.,1.,1.,1.,1.,1.,1.,1.,1.,
1.,1.,1.,1.,1.,1.,1.,1.,1.,1.,1.,1.,1.,1.,1.,1.,1.,1.,1.,1.,1.,1.,1.,1.,
1.,1.,1.,1.,1.,1.,1.,1.,1.,1.,1.,1.,1.,1.,1.,1.,1.,1.,1.,1.,1.,1.,1.,1.,
1.,1.,1.,1.,1.,1.,1.,1.,1.,1.,1.,1.,1.,1.,1.,1.,1.,1.,1.,1.,1.,1.,1.,1.,
1.,1.,1.,1.,1.,1.,1.,1.,1.,1.,1.,1.,1.,1.,1.,1.,1.,1.,1.,1.,1.,1.,1.,1.,
1.,1.,1.,1.,1.,1.,1.,1.,1.,1.))
REPRESENTATION_ITEM('')
);
#634=(
BOUNDED_CURVE()
B_SPLINE_CURVE(5,(#152043,#152044,#152045,#152046,#152047,#152048,#152049,
#152050,#152051,#152052,#152053,#152054,#152055,#152056,#152057,#152058,
#152059,#152060,#152061,#152062,#152063,#152064,#152065,#152066,#152067,
#152068,#152069,#152070,#152071,#152072,#152073,#152074,#152075,#152076,
#152077,#152078,#152079,#152080,#152081,#152082,#152083,#152084,#152085,
#152086,#152087,#152088,#152089,#152090,#152091,#152092,#152093,#152094,
#152095,#152096,#152097,#152098,#152099,#152100,#152101,#152102,#152103,
#152104,#152105,#152106,#152107,#152108,#152109,#152110,#152111,#152112,
#152113,#152114,#152115,#152116,#152117,#152118,#152119,#152120,#152121,
#152122,#152123,#152124,#152125,#152126,#152127,#152128,#152129,#152130,
#152131,#152132,#152133,#152134,#152135,#152136,#152137,#152138,#152139,
#152140,#152141,#152142,#152143,#152144,#152145,#152146,#152147,#152148,
#152149,#152150,#152151,#152152,#152153,#152154,#152155,#152156,#152157,
#152158,#152159,#152160,#152161,#152162,#152163,#152164,#152165,#152166,
#152167,#152168,#152169,#152170,#152171,#152172,#152173,#152174,#152175,
#152176,#152177,#152178,#152179,#152180,#152181,#152182,#152183,#152184,
#152185,#152186,#152187,#152188,#152189,#152190,#152191,#152192,#152193,
#152194,#152195,#152196,#152197,#152198,#152199,#152200,#152201,#152202,
#152203,#152204,#152205,#152206,#152207,#152208,#152209,#152210,#152211,
#152212,#152213,#152214,#152215,#152216,#152217,#152218,#152219,#152220,
#152221,#152222,#152223,#152224,#152225,#152226,#152227,#152228,#152229,
#152230,#152231,#152232,#152233,#152234,#152235,#152236),.UNSPECIFIED.,
 .F.,.F.)
B_SPLINE_CURVE_WITH_KNOTS((6,1,1,1,1,1,1,1,1,1,1,1,1,1,1,1,1,1,1,1,1,1,
1,1,1,1,1,1,1,1,1,1,1,1,1,1,1,1,1,1,1,1,1,1,1,1,1,1,1,1,1,1,1,1,1,1,1,1,
1,1,1,1,1,1,1,1,1,1,1,1,1,1,1,1,1,1,1,1,1,1,1,1,1,1,1,1,1,1,1,1,1,1,1,1,
1,1,1,1,1,1,1,1,1,1,1,1,1,1,1,1,1,1,1,1,1,1,1,1,1,1,1,1,1,1,1,1,1,1,1,1,
1,1,1,1,1,1,1,1,1,1,1,1,1,1,1,1,1,1,1,1,1,1,1,1,1,1,1,1,1,1,1,1,1,1,1,1,
1,1,1,1,1,1,1,1,1,1,1,1,1,1,1,1,1,1,1,1,1,1,1,6),(-0.941429844437991,-0.940000000000001,
-0.935000000000001,-0.930000000000001,-0.925000000000001,-0.920000000000001,
-0.915000000000001,-0.910000000000001,-0.905000000000001,-0.900000000000001,
-0.895000000000001,-0.890000000000001,-0.885000000000001,-0.880000000000001,
-0.875000000000001,-0.870000000000001,-0.865000000000001,-0.860000000000001,
-0.855000000000001,-0.850000000000001,-0.845000000000001,-0.840000000000001,
-0.835000000000001,-0.830000000000001,-0.825000000000001,-0.820000000000001,
-0.815000000000001,-0.810000000000001,-0.805000000000001,-0.800000000000001,
-0.795000000000001,-0.790000000000001,-0.785000000000001,-0.780000000000001,
-0.775000000000001,-0.770000000000001,-0.765000000000001,-0.760000000000001,
-0.755000000000001,-0.750000000000001,-0.745000000000001,-0.740000000000001,
-0.735000000000001,-0.730000000000001,-0.725000000000001,-0.720000000000001,
-0.715000000000001,-0.710000000000001,-0.705000000000001,-0.700000000000001,
-0.695000000000001,-0.690000000000001,-0.685,-0.68,-0.675,-0.67,-0.665,
-0.66,-0.655,-0.65,-0.645,-0.64,-0.635,-0.63,-0.625,-0.62,-0.615,-0.61,
-0.605,-0.6,-0.595,-0.59,-0.585,-0.58,-0.575,-0.57,-0.565,-0.56,-0.555,
-0.55,-0.545,-0.54,-0.535,-0.53,-0.525,-0.52,-0.515,-0.51,-0.505,-0.5,-0.495,
-0.49,-0.485,-0.48,-0.475,-0.47,-0.465,-0.46,-0.455,-0.45,-0.445,-0.44,
-0.435,-0.43,-0.425,-0.42,-0.415,-0.41,-0.405,-0.4,-0.395,-0.39,-0.385,
-0.38,-0.375,-0.37,-0.365,-0.36,-0.355,-0.35,-0.345,-0.34,-0.335,-0.33,
-0.325,-0.32,-0.315,-0.31,-0.305,-0.3,-0.295,-0.29,-0.285,-0.28,-0.275,
-0.27,-0.265,-0.26,-0.255,-0.25,-0.245,-0.24,-0.235,-0.23,-0.225,-0.22,
-0.215,-0.21,-0.205,-0.2,-0.195,-0.19,-0.185,-0.18,-0.175,-0.17,-0.165,
-0.16,-0.155,-0.15,-0.145,-0.14,-0.135,-0.13,-0.125,-0.12,-0.115,-0.11,
-0.105,-0.1,-0.095,-0.09,-0.085,-0.08,-0.075,-0.07,-0.065,-0.06,-0.055,
-0.05,-0.045,-0.04,-0.035,-0.03,-0.025,-0.02,-0.015,-0.01,-0.005,0.),
 .UNSPECIFIED.)
CURVE()
GEOMETRIC_REPRESENTATION_ITEM()
RATIONAL_B_SPLINE_CURVE((1.,1.,1.,1.,1.,1.,1.,1.,1.,1.,1.,1.,1.,1.,1.,1.,
1.,1.,1.,1.,1.,1.,1.,1.,1.,1.,1.,1.,1.,1.,1.,1.,1.,1.,1.,1.,1.,1.,1.,1.,
1.,1.,1.,1.,1.,1.,1.,1.,1.,1.,1.,1.,1.,1.,1.,1.,1.,1.,1.,1.,1.,1.,1.,1.,
1.,1.,1.,1.,1.,1.,1.,1.,1.,1.,1.,1.,1.,1.,1.,1.,1.,1.,1.,1.,1.,1.,1.,1.,
1.,1.,1.,1.,1.,1.,1.,1.,1.,1.,1.,1.,1.,1.,1.,1.,1.,1.,1.,1.,1.,1.,1.,1.,
1.,1.,1.,1.,1.,1.,1.,1.,1.,1.,1.,1.,1.,1.,1.,1.,1.,1.,1.,1.,1.,1.,1.,1.,
1.,1.,1.,1.,1.,1.,1.,1.,1.,1.,1.,1.,1.,1.,1.,1.,1.,1.,1.,1.,1.,1.,1.,1.,
1.,1.,1.,1.,1.,1.,1.,1.,1.,1.,1.,1.,1.,1.,1.,1.,1.,1.,1.,1.,1.,1.,1.,1.,
1.,1.,1.,1.,1.,1.,1.,1.,1.,1.))
REPRESENTATION_ITEM('')
);
#635=(
BOUNDED_CURVE()
B_SPLINE_CURVE(5,(#152648,#152649,#152650,#152651,#152652,#152653,#152654,
#152655,#152656,#152657,#152658,#152659,#152660,#152661,#152662,#152663,
#152664,#152665,#152666,#152667,#152668,#152669,#152670,#152671,#152672,
#152673,#152674,#152675,#152676,#152677,#152678,#152679,#152680,#152681,
#152682,#152683,#152684,#152685,#152686,#152687,#152688,#152689,#152690,
#152691,#152692,#152693,#152694,#152695,#152696,#152697,#152698,#152699,
#152700,#152701,#152702,#152703,#152704,#152705,#152706,#152707,#152708,
#152709,#152710,#152711,#152712,#152713,#152714,#152715,#152716,#152717,
#152718,#152719,#152720,#152721,#152722,#152723,#152724,#152725,#152726,
#152727,#152728,#152729,#152730,#152731,#152732,#152733,#152734,#152735,
#152736,#152737,#152738,#152739,#152740,#152741,#152742,#152743,#152744,
#152745,#152746,#152747,#152748,#152749,#152750,#152751,#152752,#152753,
#152754,#152755,#152756,#152757,#152758,#152759,#152760,#152761,#152762,
#152763,#152764,#152765,#152766,#152767,#152768,#152769,#152770,#152771,
#152772,#152773,#152774,#152775,#152776,#152777,#152778,#152779,#152780,
#152781,#152782,#152783,#152784,#152785,#152786,#152787,#152788,#152789,
#152790,#152791,#152792,#152793,#152794,#152795,#152796,#152797,#152798,
#152799,#152800,#152801,#152802,#152803,#152804,#152805,#152806,#152807,
#152808,#152809,#152810,#152811,#152812,#152813,#152814,#152815,#152816,
#152817,#152818,#152819,#152820,#152821,#152822,#152823,#152824,#152825,
#152826,#152827,#152828,#152829,#152830,#152831,#152832,#152833,#152834,
#152835,#152836,#152837,#152838,#152839,#152840,#152841),.UNSPECIFIED.,
 .F.,.F.)
B_SPLINE_CURVE_WITH_KNOTS((6,1,1,1,1,1,1,1,1,1,1,1,1,1,1,1,1,1,1,1,1,1,
1,1,1,1,1,1,1,1,1,1,1,1,1,1,1,1,1,1,1,1,1,1,1,1,1,1,1,1,1,1,1,1,1,1,1,1,
1,1,1,1,1,1,1,1,1,1,1,1,1,1,1,1,1,1,1,1,1,1,1,1,1,1,1,1,1,1,1,1,1,1,1,1,
1,1,1,1,1,1,1,1,1,1,1,1,1,1,1,1,1,1,1,1,1,1,1,1,1,1,1,1,1,1,1,1,1,1,1,1,
1,1,1,1,1,1,1,1,1,1,1,1,1,1,1,1,1,1,1,1,1,1,1,1,1,1,1,1,1,1,1,1,1,1,1,1,
1,1,1,1,1,1,1,1,1,1,1,1,1,1,1,1,1,1,1,1,1,1,1,6),(0.,0.005,0.01,0.015,0.02,
0.025,0.03,0.035,0.04,0.045,0.05,0.055,0.06,0.065,0.07,0.075,0.08,0.085,
0.09,0.095,0.1,0.105,0.11,0.115,0.12,0.125,0.13,0.135,0.14,0.145,0.15,0.155,
0.16,0.165,0.17,0.175,0.18,0.185,0.19,0.195,0.2,0.205,0.21,0.215,0.22,0.225,
0.23,0.235,0.24,0.245,0.25,0.255,0.26,0.265,0.27,0.275,0.28,0.285,0.29,
0.295,0.3,0.305,0.31,0.315,0.32,0.325,0.33,0.335,0.34,0.345,0.35,0.355,
0.36,0.365,0.37,0.375,0.38,0.385,0.39,0.395,0.4,0.405,0.41,0.415,0.42,0.425,
0.43,0.435,0.44,0.445,0.45,0.455,0.46,0.465,0.47,0.475,0.48,0.485,0.49,
0.495,0.5,0.505,0.51,0.515,0.52,0.525,0.53,0.535,0.54,0.545,0.55,0.555,
0.56,0.565,0.57,0.575,0.58,0.585,0.59,0.595,0.6,0.605,0.61,0.615,0.62,0.625,
0.63,0.635,0.64,0.645,0.65,0.655,0.66,0.665,0.67,0.675,0.68,0.685,0.690000000000001,
0.695000000000001,0.700000000000001,0.705000000000001,0.710000000000001,
0.715000000000001,0.720000000000001,0.725000000000001,0.730000000000001,
0.735000000000001,0.740000000000001,0.745000000000001,0.750000000000001,
0.755000000000001,0.760000000000001,0.765000000000001,0.770000000000001,
0.775000000000001,0.780000000000001,0.785000000000001,0.790000000000001,
0.795000000000001,0.800000000000001,0.805000000000001,0.810000000000001,
0.815000000000001,0.820000000000001,0.825000000000001,0.830000000000001,
0.835000000000001,0.840000000000001,0.845000000000001,0.850000000000001,
0.855000000000001,0.860000000000001,0.865000000000001,0.870000000000001,
0.875000000000001,0.880000000000001,0.885000000000001,0.890000000000001,
0.895000000000001,0.900000000000001,0.905000000000001,0.910000000000001,
0.915000000000001,0.920000000000001,0.925000000000001,0.930000000000001,
0.935000000000001,0.940000000000001,0.941429844438037),.UNSPECIFIED.)
CURVE()
GEOMETRIC_REPRESENTATION_ITEM()
RATIONAL_B_SPLINE_CURVE((1.,1.,1.,1.,1.,1.,1.,1.,1.,1.,1.,1.,1.,1.,1.,1.,
1.,1.,1.,1.,1.,1.,1.,1.,1.,1.,1.,1.,1.,1.,1.,1.,1.,1.,1.,1.,1.,1.,1.,1.,
1.,1.,1.,1.,1.,1.,1.,1.,1.,1.,1.,1.,1.,1.,1.,1.,1.,1.,1.,1.,1.,1.,1.,1.,
1.,1.,1.,1.,1.,1.,1.,1.,1.,1.,1.,1.,1.,1.,1.,1.,1.,1.,1.,1.,1.,1.,1.,1.,
1.,1.,1.,1.,1.,1.,1.,1.,1.,1.,1.,1.,1.,1.,1.,1.,1.,1.,1.,1.,1.,1.,1.,1.,
1.,1.,1.,1.,1.,1.,1.,1.,1.,1.,1.,1.,1.,1.,1.,1.,1.,1.,1.,1.,1.,1.,1.,1.,
1.,1.,1.,1.,1.,1.,1.,1.,1.,1.,1.,1.,1.,1.,1.,1.,1.,1.,1.,1.,1.,1.,1.,1.,
1.,1.,1.,1.,1.,1.,1.,1.,1.,1.,1.,1.,1.,1.,1.,1.,1.,1.,1.,1.,1.,1.,1.,1.,
1.,1.,1.,1.,1.,1.,1.,1.,1.,1.))
REPRESENTATION_ITEM('')
);
#636=(
BOUNDED_CURVE()
B_SPLINE_CURVE(5,(#152844,#152845,#152846,#152847,#152848,#152849,#152850,
#152851,#152852,#152853,#152854,#152855,#152856,#152857,#152858,#152859,
#152860,#152861,#152862,#152863,#152864,#152865,#152866,#152867,#152868,
#152869,#152870,#152871,#152872,#152873,#152874,#152875,#152876,#152877,
#152878,#152879,#152880,#152881,#152882,#152883,#152884,#152885,#152886,
#152887,#152888,#152889,#152890,#152891,#152892,#152893,#152894,#152895,
#152896,#152897,#152898,#152899,#152900,#152901,#152902,#152903,#152904,
#152905,#152906,#152907,#152908,#152909,#152910,#152911,#152912,#152913,
#152914,#152915,#152916,#152917,#152918,#152919,#152920,#152921,#152922,
#152923,#152924,#152925,#152926,#152927,#152928,#152929,#152930,#152931,
#152932,#152933,#152934,#152935,#152936,#152937,#152938,#152939,#152940,
#152941,#152942,#152943,#152944,#152945,#152946,#152947,#152948,#152949,
#152950,#152951,#152952,#152953,#152954,#152955,#152956,#152957,#152958,
#152959,#152960,#152961,#152962,#152963,#152964,#152965,#152966,#152967,
#152968,#152969,#152970,#152971,#152972,#152973,#152974,#152975,#152976,
#152977,#152978,#152979,#152980,#152981,#152982,#152983,#152984,#152985,
#152986,#152987,#152988,#152989,#152990,#152991,#152992,#152993,#152994,
#152995,#152996,#152997,#152998,#152999,#153000,#153001,#153002,#153003,
#153004,#153005,#153006,#153007,#153008,#153009,#153010,#153011,#153012,
#153013,#153014,#153015,#153016,#153017,#153018,#153019,#153020,#153021,
#153022,#153023,#153024,#153025,#153026,#153027,#153028,#153029,#153030,
#153031,#153032,#153033,#153034,#153035,#153036,#153037),.UNSPECIFIED.,
 .F.,.F.)
B_SPLINE_CURVE_WITH_KNOTS((6,1,1,1,1,1,1,1,1,1,1,1,1,1,1,1,1,1,1,1,1,1,
1,1,1,1,1,1,1,1,1,1,1,1,1,1,1,1,1,1,1,1,1,1,1,1,1,1,1,1,1,1,1,1,1,1,1,1,
1,1,1,1,1,1,1,1,1,1,1,1,1,1,1,1,1,1,1,1,1,1,1,1,1,1,1,1,1,1,1,1,1,1,1,1,
1,1,1,1,1,1,1,1,1,1,1,1,1,1,1,1,1,1,1,1,1,1,1,1,1,1,1,1,1,1,1,1,1,1,1,1,
1,1,1,1,1,1,1,1,1,1,1,1,1,1,1,1,1,1,1,1,1,1,1,1,1,1,1,1,1,1,1,1,1,1,1,1,
1,1,1,1,1,1,1,1,1,1,1,1,1,1,1,1,1,1,1,1,1,1,1,6),(-0.941429844438034,-0.940000000000001,
-0.935000000000001,-0.930000000000001,-0.925000000000001,-0.920000000000001,
-0.915000000000001,-0.910000000000001,-0.905000000000001,-0.900000000000001,
-0.895000000000001,-0.890000000000001,-0.885000000000001,-0.880000000000001,
-0.875000000000001,-0.870000000000001,-0.865000000000001,-0.860000000000001,
-0.855000000000001,-0.850000000000001,-0.845000000000001,-0.840000000000001,
-0.835000000000001,-0.830000000000001,-0.825000000000001,-0.820000000000001,
-0.815000000000001,-0.810000000000001,-0.805000000000001,-0.800000000000001,
-0.795000000000001,-0.790000000000001,-0.785000000000001,-0.780000000000001,
-0.775000000000001,-0.770000000000001,-0.765000000000001,-0.760000000000001,
-0.755000000000001,-0.750000000000001,-0.745000000000001,-0.740000000000001,
-0.735000000000001,-0.730000000000001,-0.725000000000001,-0.720000000000001,
-0.715000000000001,-0.710000000000001,-0.705000000000001,-0.700000000000001,
-0.695000000000001,-0.690000000000001,-0.685,-0.68,-0.675,-0.67,-0.665,
-0.66,-0.655,-0.65,-0.645,-0.64,-0.635,-0.63,-0.625,-0.62,-0.615,-0.61,
-0.605,-0.6,-0.595,-0.59,-0.585,-0.58,-0.575,-0.57,-0.565,-0.56,-0.555,
-0.55,-0.545,-0.54,-0.535,-0.53,-0.525,-0.52,-0.515,-0.51,-0.505,-0.5,-0.495,
-0.49,-0.485,-0.48,-0.475,-0.47,-0.465,-0.46,-0.455,-0.45,-0.445,-0.44,
-0.435,-0.43,-0.425,-0.42,-0.415,-0.41,-0.405,-0.4,-0.395,-0.39,-0.385,
-0.38,-0.375,-0.37,-0.365,-0.36,-0.355,-0.35,-0.345,-0.34,-0.335,-0.33,
-0.325,-0.32,-0.315,-0.31,-0.305,-0.3,-0.295,-0.29,-0.285,-0.28,-0.275,
-0.27,-0.265,-0.26,-0.255,-0.25,-0.245,-0.24,-0.235,-0.23,-0.225,-0.22,
-0.215,-0.21,-0.205,-0.2,-0.195,-0.19,-0.185,-0.18,-0.175,-0.17,-0.165,
-0.16,-0.155,-0.15,-0.145,-0.14,-0.135,-0.13,-0.125,-0.12,-0.115,-0.11,
-0.105,-0.1,-0.095,-0.09,-0.085,-0.08,-0.075,-0.07,-0.065,-0.06,-0.055,
-0.05,-0.045,-0.04,-0.035,-0.03,-0.025,-0.02,-0.015,-0.01,-0.005,0.),
 .UNSPECIFIED.)
CURVE()
GEOMETRIC_REPRESENTATION_ITEM()
RATIONAL_B_SPLINE_CURVE((1.,1.,1.,1.,1.,1.,1.,1.,1.,1.,1.,1.,1.,1.,1.,1.,
1.,1.,1.,1.,1.,1.,1.,1.,1.,1.,1.,1.,1.,1.,1.,1.,1.,1.,1.,1.,1.,1.,1.,1.,
1.,1.,1.,1.,1.,1.,1.,1.,1.,1.,1.,1.,1.,1.,1.,1.,1.,1.,1.,1.,1.,1.,1.,1.,
1.,1.,1.,1.,1.,1.,1.,1.,1.,1.,1.,1.,1.,1.,1.,1.,1.,1.,1.,1.,1.,1.,1.,1.,
1.,1.,1.,1.,1.,1.,1.,1.,1.,1.,1.,1.,1.,1.,1.,1.,1.,1.,1.,1.,1.,1.,1.,1.,
1.,1.,1.,1.,1.,1.,1.,1.,1.,1.,1.,1.,1.,1.,1.,1.,1.,1.,1.,1.,1.,1.,1.,1.,
1.,1.,1.,1.,1.,1.,1.,1.,1.,1.,1.,1.,1.,1.,1.,1.,1.,1.,1.,1.,1.,1.,1.,1.,
1.,1.,1.,1.,1.,1.,1.,1.,1.,1.,1.,1.,1.,1.,1.,1.,1.,1.,1.,1.,1.,1.,1.,1.,
1.,1.,1.,1.,1.,1.,1.,1.,1.,1.))
REPRESENTATION_ITEM('')
);
#637=(
BOUNDED_CURVE()
B_SPLINE_CURVE(5,(#153449,#153450,#153451,#153452,#153453,#153454,#153455,
#153456,#153457,#153458,#153459,#153460,#153461,#153462,#153463,#153464,
#153465,#153466,#153467,#153468,#153469,#153470,#153471,#153472,#153473,
#153474,#153475,#153476,#153477,#153478,#153479,#153480,#153481,#153482,
#153483,#153484,#153485,#153486,#153487,#153488,#153489,#153490,#153491,
#153492,#153493,#153494,#153495,#153496,#153497,#153498,#153499,#153500,
#153501,#153502,#153503,#153504,#153505,#153506,#153507,#153508,#153509,
#153510,#153511,#153512,#153513,#153514,#153515,#153516,#153517,#153518,
#153519,#153520,#153521,#153522,#153523,#153524,#153525,#153526,#153527,
#153528,#153529,#153530,#153531,#153532,#153533,#153534,#153535,#153536,
#153537,#153538,#153539,#153540,#153541,#153542,#153543,#153544,#153545,
#153546,#153547,#153548,#153549,#153550,#153551,#153552,#153553,#153554,
#153555,#153556,#153557,#153558,#153559,#153560,#153561,#153562,#153563,
#153564,#153565,#153566,#153567,#153568,#153569,#153570,#153571,#153572,
#153573,#153574,#153575,#153576,#153577,#153578,#153579,#153580,#153581,
#153582,#153583,#153584,#153585,#153586,#153587,#153588,#153589,#153590,
#153591,#153592,#153593,#153594,#153595,#153596,#153597,#153598,#153599,
#153600,#153601,#153602,#153603,#153604,#153605,#153606,#153607,#153608,
#153609,#153610,#153611,#153612,#153613,#153614,#153615,#153616,#153617,
#153618,#153619,#153620,#153621,#153622,#153623,#153624,#153625,#153626,
#153627,#153628,#153629,#153630,#153631,#153632,#153633,#153634,#153635,
#153636,#153637,#153638,#153639,#153640,#153641,#153642),.UNSPECIFIED.,
 .F.,.F.)
B_SPLINE_CURVE_WITH_KNOTS((6,1,1,1,1,1,1,1,1,1,1,1,1,1,1,1,1,1,1,1,1,1,
1,1,1,1,1,1,1,1,1,1,1,1,1,1,1,1,1,1,1,1,1,1,1,1,1,1,1,1,1,1,1,1,1,1,1,1,
1,1,1,1,1,1,1,1,1,1,1,1,1,1,1,1,1,1,1,1,1,1,1,1,1,1,1,1,1,1,1,1,1,1,1,1,
1,1,1,1,1,1,1,1,1,1,1,1,1,1,1,1,1,1,1,1,1,1,1,1,1,1,1,1,1,1,1,1,1,1,1,1,
1,1,1,1,1,1,1,1,1,1,1,1,1,1,1,1,1,1,1,1,1,1,1,1,1,1,1,1,1,1,1,1,1,1,1,1,
1,1,1,1,1,1,1,1,1,1,1,1,1,1,1,1,1,1,1,1,1,1,1,6),(0.,0.005,0.01,0.015,0.02,
0.025,0.03,0.035,0.04,0.045,0.05,0.055,0.06,0.065,0.07,0.075,0.08,0.085,
0.09,0.095,0.1,0.105,0.11,0.115,0.12,0.125,0.13,0.135,0.14,0.145,0.15,0.155,
0.16,0.165,0.17,0.175,0.18,0.185,0.19,0.195,0.2,0.205,0.21,0.215,0.22,0.225,
0.23,0.235,0.24,0.245,0.25,0.255,0.26,0.265,0.27,0.275,0.28,0.285,0.29,
0.295,0.3,0.305,0.31,0.315,0.32,0.325,0.33,0.335,0.34,0.345,0.35,0.355,
0.36,0.365,0.37,0.375,0.38,0.385,0.39,0.395,0.4,0.405,0.41,0.415,0.42,0.425,
0.43,0.435,0.44,0.445,0.45,0.455,0.46,0.465,0.47,0.475,0.48,0.485,0.49,
0.495,0.5,0.505,0.51,0.515,0.52,0.525,0.53,0.535,0.54,0.545,0.55,0.555,
0.56,0.565,0.57,0.575,0.58,0.585,0.59,0.595,0.6,0.605,0.61,0.615,0.62,0.625,
0.63,0.635,0.64,0.645,0.65,0.655,0.66,0.665,0.67,0.675,0.68,0.685,0.690000000000001,
0.695000000000001,0.700000000000001,0.705000000000001,0.710000000000001,
0.715000000000001,0.720000000000001,0.725000000000001,0.730000000000001,
0.735000000000001,0.740000000000001,0.745000000000001,0.750000000000001,
0.755000000000001,0.760000000000001,0.765000000000001,0.770000000000001,
0.775000000000001,0.780000000000001,0.785000000000001,0.790000000000001,
0.795000000000001,0.800000000000001,0.805000000000001,0.810000000000001,
0.815000000000001,0.820000000000001,0.825000000000001,0.830000000000001,
0.835000000000001,0.840000000000001,0.845000000000001,0.850000000000001,
0.855000000000001,0.860000000000001,0.865000000000001,0.870000000000001,
0.875000000000001,0.880000000000001,0.885000000000001,0.890000000000001,
0.895000000000001,0.900000000000001,0.905000000000001,0.910000000000001,
0.915000000000001,0.920000000000001,0.925000000000001,0.930000000000001,
0.935000000000001,0.940000000000001,0.941429844438169),.UNSPECIFIED.)
CURVE()
GEOMETRIC_REPRESENTATION_ITEM()
RATIONAL_B_SPLINE_CURVE((1.,1.,1.,1.,1.,1.,1.,1.,1.,1.,1.,1.,1.,1.,1.,1.,
1.,1.,1.,1.,1.,1.,1.,1.,1.,1.,1.,1.,1.,1.,1.,1.,1.,1.,1.,1.,1.,1.,1.,1.,
1.,1.,1.,1.,1.,1.,1.,1.,1.,1.,1.,1.,1.,1.,1.,1.,1.,1.,1.,1.,1.,1.,1.,1.,
1.,1.,1.,1.,1.,1.,1.,1.,1.,1.,1.,1.,1.,1.,1.,1.,1.,1.,1.,1.,1.,1.,1.,1.,
1.,1.,1.,1.,1.,1.,1.,1.,1.,1.,1.,1.,1.,1.,1.,1.,1.,1.,1.,1.,1.,1.,1.,1.,
1.,1.,1.,1.,1.,1.,1.,1.,1.,1.,1.,1.,1.,1.,1.,1.,1.,1.,1.,1.,1.,1.,1.,1.,
1.,1.,1.,1.,1.,1.,1.,1.,1.,1.,1.,1.,1.,1.,1.,1.,1.,1.,1.,1.,1.,1.,1.,1.,
1.,1.,1.,1.,1.,1.,1.,1.,1.,1.,1.,1.,1.,1.,1.,1.,1.,1.,1.,1.,1.,1.,1.,1.,
1.,1.,1.,1.,1.,1.,1.,1.,1.,1.))
REPRESENTATION_ITEM('')
);
#638=(
BOUNDED_CURVE()
B_SPLINE_CURVE(5,(#153645,#153646,#153647,#153648,#153649,#153650,#153651,
#153652,#153653,#153654,#153655,#153656,#153657,#153658,#153659,#153660,
#153661,#153662,#153663,#153664,#153665,#153666,#153667,#153668,#153669,
#153670,#153671,#153672,#153673,#153674,#153675,#153676,#153677,#153678,
#153679,#153680,#153681,#153682,#153683,#153684,#153685,#153686,#153687,
#153688,#153689,#153690,#153691,#153692,#153693,#153694,#153695,#153696,
#153697,#153698,#153699,#153700,#153701,#153702,#153703,#153704,#153705,
#153706,#153707,#153708,#153709,#153710,#153711,#153712,#153713,#153714,
#153715,#153716,#153717,#153718,#153719,#153720,#153721,#153722,#153723,
#153724,#153725,#153726,#153727,#153728,#153729,#153730,#153731,#153732,
#153733,#153734,#153735,#153736,#153737,#153738,#153739,#153740,#153741,
#153742,#153743,#153744,#153745,#153746,#153747,#153748,#153749,#153750,
#153751,#153752,#153753,#153754,#153755,#153756,#153757,#153758,#153759,
#153760,#153761,#153762,#153763,#153764,#153765,#153766,#153767,#153768,
#153769,#153770,#153771,#153772,#153773,#153774,#153775,#153776,#153777,
#153778,#153779,#153780,#153781,#153782,#153783,#153784,#153785,#153786,
#153787,#153788,#153789,#153790,#153791,#153792,#153793,#153794,#153795,
#153796,#153797,#153798,#153799,#153800,#153801,#153802,#153803,#153804,
#153805,#153806,#153807,#153808,#153809,#153810,#153811,#153812,#153813,
#153814,#153815,#153816,#153817,#153818,#153819,#153820,#153821,#153822,
#153823,#153824,#153825,#153826,#153827,#153828,#153829,#153830,#153831,
#153832,#153833,#153834,#153835,#153836,#153837,#153838),.UNSPECIFIED.,
 .F.,.F.)
B_SPLINE_CURVE_WITH_KNOTS((6,1,1,1,1,1,1,1,1,1,1,1,1,1,1,1,1,1,1,1,1,1,
1,1,1,1,1,1,1,1,1,1,1,1,1,1,1,1,1,1,1,1,1,1,1,1,1,1,1,1,1,1,1,1,1,1,1,1,
1,1,1,1,1,1,1,1,1,1,1,1,1,1,1,1,1,1,1,1,1,1,1,1,1,1,1,1,1,1,1,1,1,1,1,1,
1,1,1,1,1,1,1,1,1,1,1,1,1,1,1,1,1,1,1,1,1,1,1,1,1,1,1,1,1,1,1,1,1,1,1,1,
1,1,1,1,1,1,1,1,1,1,1,1,1,1,1,1,1,1,1,1,1,1,1,1,1,1,1,1,1,1,1,1,1,1,1,1,
1,1,1,1,1,1,1,1,1,1,1,1,1,1,1,1,1,1,1,1,1,1,1,6),(-0.941429844438167,-0.940000000000001,
-0.935000000000001,-0.930000000000001,-0.925000000000001,-0.920000000000001,
-0.915000000000001,-0.910000000000001,-0.905000000000001,-0.900000000000001,
-0.895000000000001,-0.890000000000001,-0.885000000000001,-0.880000000000001,
-0.875000000000001,-0.870000000000001,-0.865000000000001,-0.860000000000001,
-0.855000000000001,-0.850000000000001,-0.845000000000001,-0.840000000000001,
-0.835000000000001,-0.830000000000001,-0.825000000000001,-0.820000000000001,
-0.815000000000001,-0.810000000000001,-0.805000000000001,-0.800000000000001,
-0.795000000000001,-0.790000000000001,-0.785000000000001,-0.780000000000001,
-0.775000000000001,-0.770000000000001,-0.765000000000001,-0.760000000000001,
-0.755000000000001,-0.750000000000001,-0.745000000000001,-0.740000000000001,
-0.735000000000001,-0.730000000000001,-0.725000000000001,-0.720000000000001,
-0.715000000000001,-0.710000000000001,-0.705000000000001,-0.700000000000001,
-0.695000000000001,-0.690000000000001,-0.685,-0.68,-0.675,-0.67,-0.665,
-0.66,-0.655,-0.65,-0.645,-0.64,-0.635,-0.63,-0.625,-0.62,-0.615,-0.61,
-0.605,-0.6,-0.595,-0.59,-0.585,-0.58,-0.575,-0.57,-0.565,-0.56,-0.555,
-0.55,-0.545,-0.54,-0.535,-0.53,-0.525,-0.52,-0.515,-0.51,-0.505,-0.5,-0.495,
-0.49,-0.485,-0.48,-0.475,-0.47,-0.465,-0.46,-0.455,-0.45,-0.445,-0.44,
-0.435,-0.43,-0.425,-0.42,-0.415,-0.41,-0.405,-0.4,-0.395,-0.39,-0.385,
-0.38,-0.375,-0.37,-0.365,-0.36,-0.355,-0.35,-0.345,-0.34,-0.335,-0.33,
-0.325,-0.32,-0.315,-0.31,-0.305,-0.3,-0.295,-0.29,-0.285,-0.28,-0.275,
-0.27,-0.265,-0.26,-0.255,-0.25,-0.245,-0.24,-0.235,-0.23,-0.225,-0.22,
-0.215,-0.21,-0.205,-0.2,-0.195,-0.19,-0.185,-0.18,-0.175,-0.17,-0.165,
-0.16,-0.155,-0.15,-0.145,-0.14,-0.135,-0.13,-0.125,-0.12,-0.115,-0.11,
-0.105,-0.1,-0.095,-0.09,-0.085,-0.08,-0.075,-0.07,-0.065,-0.06,-0.055,
-0.05,-0.045,-0.04,-0.035,-0.03,-0.025,-0.02,-0.015,-0.01,-0.005,0.),
 .UNSPECIFIED.)
CURVE()
GEOMETRIC_REPRESENTATION_ITEM()
RATIONAL_B_SPLINE_CURVE((1.,1.,1.,1.,1.,1.,1.,1.,1.,1.,1.,1.,1.,1.,1.,1.,
1.,1.,1.,1.,1.,1.,1.,1.,1.,1.,1.,1.,1.,1.,1.,1.,1.,1.,1.,1.,1.,1.,1.,1.,
1.,1.,1.,1.,1.,1.,1.,1.,1.,1.,1.,1.,1.,1.,1.,1.,1.,1.,1.,1.,1.,1.,1.,1.,
1.,1.,1.,1.,1.,1.,1.,1.,1.,1.,1.,1.,1.,1.,1.,1.,1.,1.,1.,1.,1.,1.,1.,1.,
1.,1.,1.,1.,1.,1.,1.,1.,1.,1.,1.,1.,1.,1.,1.,1.,1.,1.,1.,1.,1.,1.,1.,1.,
1.,1.,1.,1.,1.,1.,1.,1.,1.,1.,1.,1.,1.,1.,1.,1.,1.,1.,1.,1.,1.,1.,1.,1.,
1.,1.,1.,1.,1.,1.,1.,1.,1.,1.,1.,1.,1.,1.,1.,1.,1.,1.,1.,1.,1.,1.,1.,1.,
1.,1.,1.,1.,1.,1.,1.,1.,1.,1.,1.,1.,1.,1.,1.,1.,1.,1.,1.,1.,1.,1.,1.,1.,
1.,1.,1.,1.,1.,1.,1.,1.,1.,1.))
REPRESENTATION_ITEM('')
);
#639=(
BOUNDED_CURVE()
B_SPLINE_CURVE(5,(#154250,#154251,#154252,#154253,#154254,#154255,#154256,
#154257,#154258,#154259,#154260,#154261,#154262,#154263,#154264,#154265,
#154266,#154267,#154268,#154269,#154270,#154271,#154272,#154273,#154274,
#154275,#154276,#154277,#154278,#154279,#154280,#154281,#154282,#154283,
#154284,#154285,#154286,#154287,#154288,#154289,#154290,#154291,#154292,
#154293,#154294,#154295,#154296,#154297,#154298,#154299,#154300,#154301,
#154302,#154303,#154304,#154305,#154306,#154307,#154308,#154309,#154310,
#154311,#154312,#154313,#154314,#154315,#154316,#154317,#154318,#154319,
#154320,#154321,#154322,#154323,#154324,#154325,#154326,#154327,#154328,
#154329,#154330,#154331,#154332,#154333,#154334,#154335,#154336,#154337,
#154338,#154339,#154340,#154341,#154342,#154343,#154344,#154345,#154346,
#154347,#154348,#154349,#154350,#154351,#154352,#154353,#154354,#154355,
#154356,#154357,#154358,#154359,#154360,#154361,#154362,#154363,#154364,
#154365,#154366,#154367,#154368,#154369,#154370,#154371,#154372,#154373,
#154374,#154375,#154376,#154377,#154378,#154379,#154380,#154381,#154382,
#154383,#154384,#154385,#154386,#154387,#154388,#154389,#154390,#154391,
#154392,#154393,#154394,#154395,#154396,#154397,#154398,#154399,#154400,
#154401,#154402,#154403,#154404,#154405,#154406,#154407,#154408,#154409,
#154410,#154411,#154412,#154413,#154414,#154415,#154416,#154417,#154418,
#154419,#154420,#154421,#154422,#154423,#154424,#154425,#154426,#154427,
#154428,#154429,#154430,#154431,#154432,#154433,#154434,#154435,#154436,
#154437,#154438,#154439,#154440,#154441,#154442,#154443),.UNSPECIFIED.,
 .F.,.F.)
B_SPLINE_CURVE_WITH_KNOTS((6,1,1,1,1,1,1,1,1,1,1,1,1,1,1,1,1,1,1,1,1,1,
1,1,1,1,1,1,1,1,1,1,1,1,1,1,1,1,1,1,1,1,1,1,1,1,1,1,1,1,1,1,1,1,1,1,1,1,
1,1,1,1,1,1,1,1,1,1,1,1,1,1,1,1,1,1,1,1,1,1,1,1,1,1,1,1,1,1,1,1,1,1,1,1,
1,1,1,1,1,1,1,1,1,1,1,1,1,1,1,1,1,1,1,1,1,1,1,1,1,1,1,1,1,1,1,1,1,1,1,1,
1,1,1,1,1,1,1,1,1,1,1,1,1,1,1,1,1,1,1,1,1,1,1,1,1,1,1,1,1,1,1,1,1,1,1,1,
1,1,1,1,1,1,1,1,1,1,1,1,1,1,1,1,1,1,1,1,1,1,1,6),(0.,0.005,0.01,0.015,0.02,
0.025,0.03,0.035,0.04,0.045,0.05,0.055,0.06,0.065,0.07,0.075,0.08,0.085,
0.09,0.095,0.1,0.105,0.11,0.115,0.12,0.125,0.13,0.135,0.14,0.145,0.15,0.155,
0.16,0.165,0.17,0.175,0.18,0.185,0.19,0.195,0.2,0.205,0.21,0.215,0.22,0.225,
0.23,0.235,0.24,0.245,0.25,0.255,0.26,0.265,0.27,0.275,0.28,0.285,0.29,
0.295,0.3,0.305,0.31,0.315,0.32,0.325,0.33,0.335,0.34,0.345,0.35,0.355,
0.36,0.365,0.37,0.375,0.38,0.385,0.39,0.395,0.4,0.405,0.41,0.415,0.42,0.425,
0.43,0.435,0.44,0.445,0.45,0.455,0.46,0.465,0.47,0.475,0.48,0.485,0.49,
0.495,0.5,0.505,0.51,0.515,0.52,0.525,0.53,0.535,0.54,0.545,0.55,0.555,
0.56,0.565,0.57,0.575,0.58,0.585,0.59,0.595,0.6,0.605,0.61,0.615,0.62,0.625,
0.63,0.635,0.64,0.645,0.65,0.655,0.66,0.665,0.67,0.675,0.68,0.685,0.690000000000001,
0.695000000000001,0.700000000000001,0.705000000000001,0.710000000000001,
0.715000000000001,0.720000000000001,0.725000000000001,0.730000000000001,
0.735000000000001,0.740000000000001,0.745000000000001,0.750000000000001,
0.755000000000001,0.760000000000001,0.765000000000001,0.770000000000001,
0.775000000000001,0.780000000000001,0.785000000000001,0.790000000000001,
0.795000000000001,0.800000000000001,0.805000000000001,0.810000000000001,
0.815000000000001,0.820000000000001,0.825000000000001,0.830000000000001,
0.835000000000001,0.840000000000001,0.845000000000001,0.850000000000001,
0.855000000000001,0.860000000000001,0.865000000000001,0.870000000000001,
0.875000000000001,0.880000000000001,0.885000000000001,0.890000000000001,
0.895000000000001,0.900000000000001,0.905000000000001,0.910000000000001,
0.915000000000001,0.920000000000001,0.925000000000001,0.930000000000001,
0.935000000000001,0.940000000000001,0.941429844437968),.UNSPECIFIED.)
CURVE()
GEOMETRIC_REPRESENTATION_ITEM()
RATIONAL_B_SPLINE_CURVE((1.,1.,1.,1.,1.,1.,1.,1.,1.,1.,1.,1.,1.,1.,1.,1.,
1.,1.,1.,1.,1.,1.,1.,1.,1.,1.,1.,1.,1.,1.,1.,1.,1.,1.,1.,1.,1.,1.,1.,1.,
1.,1.,1.,1.,1.,1.,1.,1.,1.,1.,1.,1.,1.,1.,1.,1.,1.,1.,1.,1.,1.,1.,1.,1.,
1.,1.,1.,1.,1.,1.,1.,1.,1.,1.,1.,1.,1.,1.,1.,1.,1.,1.,1.,1.,1.,1.,1.,1.,
1.,1.,1.,1.,1.,1.,1.,1.,1.,1.,1.,1.,1.,1.,1.,1.,1.,1.,1.,1.,1.,1.,1.,1.,
1.,1.,1.,1.,1.,1.,1.,1.,1.,1.,1.,1.,1.,1.,1.,1.,1.,1.,1.,1.,1.,1.,1.,1.,
1.,1.,1.,1.,1.,1.,1.,1.,1.,1.,1.,1.,1.,1.,1.,1.,1.,1.,1.,1.,1.,1.,1.,1.,
1.,1.,1.,1.,1.,1.,1.,1.,1.,1.,1.,1.,1.,1.,1.,1.,1.,1.,1.,1.,1.,1.,1.,1.,
1.,1.,1.,1.,1.,1.,1.,1.,1.,1.))
REPRESENTATION_ITEM('')
);
#640=(
BOUNDED_CURVE()
B_SPLINE_CURVE(5,(#154446,#154447,#154448,#154449,#154450,#154451,#154452,
#154453,#154454,#154455,#154456,#154457,#154458,#154459,#154460,#154461,
#154462,#154463,#154464,#154465,#154466,#154467,#154468,#154469,#154470,
#154471,#154472,#154473,#154474,#154475,#154476,#154477,#154478,#154479,
#154480,#154481,#154482,#154483,#154484,#154485,#154486,#154487,#154488,
#154489,#154490,#154491,#154492,#154493,#154494,#154495,#154496,#154497,
#154498,#154499,#154500,#154501,#154502,#154503,#154504,#154505,#154506,
#154507,#154508,#154509,#154510,#154511,#154512,#154513,#154514,#154515,
#154516,#154517,#154518,#154519,#154520,#154521,#154522,#154523,#154524,
#154525,#154526,#154527,#154528,#154529,#154530,#154531,#154532,#154533,
#154534,#154535,#154536,#154537,#154538,#154539,#154540,#154541,#154542,
#154543,#154544,#154545,#154546,#154547,#154548,#154549,#154550,#154551,
#154552,#154553,#154554,#154555,#154556,#154557,#154558,#154559,#154560,
#154561,#154562,#154563,#154564,#154565,#154566,#154567,#154568,#154569,
#154570,#154571,#154572,#154573,#154574,#154575,#154576,#154577,#154578,
#154579,#154580,#154581,#154582,#154583,#154584,#154585,#154586,#154587,
#154588,#154589,#154590,#154591,#154592,#154593,#154594,#154595,#154596,
#154597,#154598,#154599,#154600,#154601,#154602,#154603,#154604,#154605,
#154606,#154607,#154608,#154609,#154610,#154611,#154612,#154613,#154614,
#154615,#154616,#154617,#154618,#154619,#154620,#154621,#154622,#154623,
#154624,#154625,#154626,#154627,#154628,#154629,#154630,#154631,#154632,
#154633,#154634,#154635,#154636,#154637,#154638,#154639),.UNSPECIFIED.,
 .F.,.F.)
B_SPLINE_CURVE_WITH_KNOTS((6,1,1,1,1,1,1,1,1,1,1,1,1,1,1,1,1,1,1,1,1,1,
1,1,1,1,1,1,1,1,1,1,1,1,1,1,1,1,1,1,1,1,1,1,1,1,1,1,1,1,1,1,1,1,1,1,1,1,
1,1,1,1,1,1,1,1,1,1,1,1,1,1,1,1,1,1,1,1,1,1,1,1,1,1,1,1,1,1,1,1,1,1,1,1,
1,1,1,1,1,1,1,1,1,1,1,1,1,1,1,1,1,1,1,1,1,1,1,1,1,1,1,1,1,1,1,1,1,1,1,1,
1,1,1,1,1,1,1,1,1,1,1,1,1,1,1,1,1,1,1,1,1,1,1,1,1,1,1,1,1,1,1,1,1,1,1,1,
1,1,1,1,1,1,1,1,1,1,1,1,1,1,1,1,1,1,1,1,1,1,1,6),(-0.94142984443797,-0.940000000000001,
-0.935000000000001,-0.930000000000001,-0.925000000000001,-0.920000000000001,
-0.915000000000001,-0.910000000000001,-0.905000000000001,-0.900000000000001,
-0.895000000000001,-0.890000000000001,-0.885000000000001,-0.880000000000001,
-0.875000000000001,-0.870000000000001,-0.865000000000001,-0.860000000000001,
-0.855000000000001,-0.850000000000001,-0.845000000000001,-0.840000000000001,
-0.835000000000001,-0.830000000000001,-0.825000000000001,-0.820000000000001,
-0.815000000000001,-0.810000000000001,-0.805000000000001,-0.800000000000001,
-0.795000000000001,-0.790000000000001,-0.785000000000001,-0.780000000000001,
-0.775000000000001,-0.770000000000001,-0.765000000000001,-0.760000000000001,
-0.755000000000001,-0.750000000000001,-0.745000000000001,-0.740000000000001,
-0.735000000000001,-0.730000000000001,-0.725000000000001,-0.720000000000001,
-0.715000000000001,-0.710000000000001,-0.705000000000001,-0.700000000000001,
-0.695000000000001,-0.690000000000001,-0.685,-0.68,-0.675,-0.67,-0.665,
-0.66,-0.655,-0.65,-0.645,-0.64,-0.635,-0.63,-0.625,-0.62,-0.615,-0.61,
-0.605,-0.6,-0.595,-0.59,-0.585,-0.58,-0.575,-0.57,-0.565,-0.56,-0.555,
-0.55,-0.545,-0.54,-0.535,-0.53,-0.525,-0.52,-0.515,-0.51,-0.505,-0.5,-0.495,
-0.49,-0.485,-0.48,-0.475,-0.47,-0.465,-0.46,-0.455,-0.45,-0.445,-0.44,
-0.435,-0.43,-0.425,-0.42,-0.415,-0.41,-0.405,-0.4,-0.395,-0.39,-0.385,
-0.38,-0.375,-0.37,-0.365,-0.36,-0.355,-0.35,-0.345,-0.34,-0.335,-0.33,
-0.325,-0.32,-0.315,-0.31,-0.305,-0.3,-0.295,-0.29,-0.285,-0.28,-0.275,
-0.27,-0.265,-0.26,-0.255,-0.25,-0.245,-0.24,-0.235,-0.23,-0.225,-0.22,
-0.215,-0.21,-0.205,-0.2,-0.195,-0.19,-0.185,-0.18,-0.175,-0.17,-0.165,
-0.16,-0.155,-0.15,-0.145,-0.14,-0.135,-0.13,-0.125,-0.12,-0.115,-0.11,
-0.105,-0.1,-0.095,-0.09,-0.085,-0.08,-0.075,-0.07,-0.065,-0.06,-0.055,
-0.05,-0.045,-0.04,-0.035,-0.03,-0.025,-0.02,-0.015,-0.01,-0.005,0.),
 .UNSPECIFIED.)
CURVE()
GEOMETRIC_REPRESENTATION_ITEM()
RATIONAL_B_SPLINE_CURVE((1.,1.,1.,1.,1.,1.,1.,1.,1.,1.,1.,1.,1.,1.,1.,1.,
1.,1.,1.,1.,1.,1.,1.,1.,1.,1.,1.,1.,1.,1.,1.,1.,1.,1.,1.,1.,1.,1.,1.,1.,
1.,1.,1.,1.,1.,1.,1.,1.,1.,1.,1.,1.,1.,1.,1.,1.,1.,1.,1.,1.,1.,1.,1.,1.,
1.,1.,1.,1.,1.,1.,1.,1.,1.,1.,1.,1.,1.,1.,1.,1.,1.,1.,1.,1.,1.,1.,1.,1.,
1.,1.,1.,1.,1.,1.,1.,1.,1.,1.,1.,1.,1.,1.,1.,1.,1.,1.,1.,1.,1.,1.,1.,1.,
1.,1.,1.,1.,1.,1.,1.,1.,1.,1.,1.,1.,1.,1.,1.,1.,1.,1.,1.,1.,1.,1.,1.,1.,
1.,1.,1.,1.,1.,1.,1.,1.,1.,1.,1.,1.,1.,1.,1.,1.,1.,1.,1.,1.,1.,1.,1.,1.,
1.,1.,1.,1.,1.,1.,1.,1.,1.,1.,1.,1.,1.,1.,1.,1.,1.,1.,1.,1.,1.,1.,1.,1.,
1.,1.,1.,1.,1.,1.,1.,1.,1.,1.))
REPRESENTATION_ITEM('')
);
#641=(
BOUNDED_CURVE()
B_SPLINE_CURVE(5,(#155051,#155052,#155053,#155054,#155055,#155056,#155057,
#155058,#155059,#155060,#155061,#155062,#155063,#155064,#155065,#155066,
#155067,#155068,#155069,#155070,#155071,#155072,#155073,#155074,#155075,
#155076,#155077,#155078,#155079,#155080,#155081,#155082,#155083,#155084,
#155085,#155086,#155087,#155088,#155089,#155090,#155091,#155092,#155093,
#155094,#155095,#155096,#155097,#155098,#155099,#155100,#155101,#155102,
#155103,#155104,#155105,#155106,#155107,#155108,#155109,#155110,#155111,
#155112,#155113,#155114,#155115,#155116,#155117,#155118,#155119,#155120,
#155121,#155122,#155123,#155124,#155125,#155126,#155127,#155128,#155129,
#155130,#155131,#155132,#155133,#155134,#155135,#155136,#155137,#155138,
#155139,#155140,#155141,#155142,#155143,#155144,#155145,#155146,#155147,
#155148,#155149,#155150,#155151,#155152,#155153,#155154,#155155,#155156,
#155157,#155158,#155159,#155160,#155161,#155162,#155163,#155164,#155165,
#155166,#155167,#155168,#155169,#155170,#155171,#155172,#155173,#155174,
#155175,#155176,#155177,#155178,#155179,#155180,#155181,#155182,#155183,
#155184,#155185,#155186,#155187,#155188,#155189,#155190,#155191,#155192,
#155193,#155194,#155195,#155196,#155197,#155198,#155199,#155200,#155201,
#155202,#155203,#155204,#155205,#155206,#155207,#155208,#155209,#155210,
#155211,#155212,#155213,#155214,#155215,#155216,#155217,#155218,#155219,
#155220,#155221,#155222,#155223,#155224,#155225,#155226,#155227,#155228,
#155229,#155230,#155231,#155232,#155233,#155234,#155235,#155236,#155237,
#155238,#155239,#155240,#155241,#155242,#155243,#155244),.UNSPECIFIED.,
 .F.,.F.)
B_SPLINE_CURVE_WITH_KNOTS((6,1,1,1,1,1,1,1,1,1,1,1,1,1,1,1,1,1,1,1,1,1,
1,1,1,1,1,1,1,1,1,1,1,1,1,1,1,1,1,1,1,1,1,1,1,1,1,1,1,1,1,1,1,1,1,1,1,1,
1,1,1,1,1,1,1,1,1,1,1,1,1,1,1,1,1,1,1,1,1,1,1,1,1,1,1,1,1,1,1,1,1,1,1,1,
1,1,1,1,1,1,1,1,1,1,1,1,1,1,1,1,1,1,1,1,1,1,1,1,1,1,1,1,1,1,1,1,1,1,1,1,
1,1,1,1,1,1,1,1,1,1,1,1,1,1,1,1,1,1,1,1,1,1,1,1,1,1,1,1,1,1,1,1,1,1,1,1,
1,1,1,1,1,1,1,1,1,1,1,1,1,1,1,1,1,1,1,1,1,1,1,6),(0.,0.005,0.01,0.015,0.02,
0.025,0.03,0.035,0.04,0.045,0.05,0.055,0.06,0.065,0.07,0.075,0.08,0.085,
0.09,0.095,0.1,0.105,0.11,0.115,0.12,0.125,0.13,0.135,0.14,0.145,0.15,0.155,
0.16,0.165,0.17,0.175,0.18,0.185,0.19,0.195,0.2,0.205,0.21,0.215,0.22,0.225,
0.23,0.235,0.24,0.245,0.25,0.255,0.26,0.265,0.27,0.275,0.28,0.285,0.29,
0.295,0.3,0.305,0.31,0.315,0.32,0.325,0.33,0.335,0.34,0.345,0.35,0.355,
0.36,0.365,0.37,0.375,0.38,0.385,0.39,0.395,0.4,0.405,0.41,0.415,0.42,0.425,
0.43,0.435,0.44,0.445,0.45,0.455,0.46,0.465,0.47,0.475,0.48,0.485,0.49,
0.495,0.5,0.505,0.51,0.515,0.52,0.525,0.53,0.535,0.54,0.545,0.55,0.555,
0.56,0.565,0.57,0.575,0.58,0.585,0.59,0.595,0.6,0.605,0.61,0.615,0.62,0.625,
0.63,0.635,0.64,0.645,0.65,0.655,0.66,0.665,0.67,0.675,0.68,0.685,0.690000000000001,
0.695000000000001,0.700000000000001,0.705000000000001,0.710000000000001,
0.715000000000001,0.720000000000001,0.725000000000001,0.730000000000001,
0.735000000000001,0.740000000000001,0.745000000000001,0.750000000000001,
0.755000000000001,0.760000000000001,0.765000000000001,0.770000000000001,
0.775000000000001,0.780000000000001,0.785000000000001,0.790000000000001,
0.795000000000001,0.800000000000001,0.805000000000001,0.810000000000001,
0.815000000000001,0.820000000000001,0.825000000000001,0.830000000000001,
0.835000000000001,0.840000000000001,0.845000000000001,0.850000000000001,
0.855000000000001,0.860000000000001,0.865000000000001,0.870000000000001,
0.875000000000001,0.880000000000001,0.885000000000001,0.890000000000001,
0.895000000000001,0.900000000000001,0.905000000000001,0.910000000000001,
0.915000000000001,0.920000000000001,0.925000000000001,0.930000000000001,
0.935000000000001,0.940000000000001,0.941429844438025),.UNSPECIFIED.)
CURVE()
GEOMETRIC_REPRESENTATION_ITEM()
RATIONAL_B_SPLINE_CURVE((1.,1.,1.,1.,1.,1.,1.,1.,1.,1.,1.,1.,1.,1.,1.,1.,
1.,1.,1.,1.,1.,1.,1.,1.,1.,1.,1.,1.,1.,1.,1.,1.,1.,1.,1.,1.,1.,1.,1.,1.,
1.,1.,1.,1.,1.,1.,1.,1.,1.,1.,1.,1.,1.,1.,1.,1.,1.,1.,1.,1.,1.,1.,1.,1.,
1.,1.,1.,1.,1.,1.,1.,1.,1.,1.,1.,1.,1.,1.,1.,1.,1.,1.,1.,1.,1.,1.,1.,1.,
1.,1.,1.,1.,1.,1.,1.,1.,1.,1.,1.,1.,1.,1.,1.,1.,1.,1.,1.,1.,1.,1.,1.,1.,
1.,1.,1.,1.,1.,1.,1.,1.,1.,1.,1.,1.,1.,1.,1.,1.,1.,1.,1.,1.,1.,1.,1.,1.,
1.,1.,1.,1.,1.,1.,1.,1.,1.,1.,1.,1.,1.,1.,1.,1.,1.,1.,1.,1.,1.,1.,1.,1.,
1.,1.,1.,1.,1.,1.,1.,1.,1.,1.,1.,1.,1.,1.,1.,1.,1.,1.,1.,1.,1.,1.,1.,1.,
1.,1.,1.,1.,1.,1.,1.,1.,1.,1.))
REPRESENTATION_ITEM('')
);
#642=(
BOUNDED_CURVE()
B_SPLINE_CURVE(5,(#155247,#155248,#155249,#155250,#155251,#155252,#155253,
#155254,#155255,#155256,#155257,#155258,#155259,#155260,#155261,#155262,
#155263,#155264,#155265,#155266,#155267,#155268,#155269,#155270,#155271,
#155272,#155273,#155274,#155275,#155276,#155277,#155278,#155279,#155280,
#155281,#155282,#155283,#155284,#155285,#155286,#155287,#155288,#155289,
#155290,#155291,#155292,#155293,#155294,#155295,#155296,#155297,#155298,
#155299,#155300,#155301,#155302,#155303,#155304,#155305,#155306,#155307,
#155308,#155309,#155310,#155311,#155312,#155313,#155314,#155315,#155316,
#155317,#155318,#155319,#155320,#155321,#155322,#155323,#155324,#155325,
#155326,#155327,#155328,#155329,#155330,#155331,#155332,#155333,#155334,
#155335,#155336,#155337,#155338,#155339,#155340,#155341,#155342,#155343,
#155344,#155345,#155346,#155347,#155348,#155349,#155350,#155351,#155352,
#155353,#155354,#155355,#155356,#155357,#155358,#155359,#155360,#155361,
#155362,#155363,#155364,#155365,#155366,#155367,#155368,#155369,#155370,
#155371,#155372,#155373,#155374,#155375,#155376,#155377,#155378,#155379,
#155380,#155381,#155382,#155383,#155384,#155385,#155386,#155387,#155388,
#155389,#155390,#155391,#155392,#155393,#155394,#155395,#155396,#155397,
#155398,#155399,#155400,#155401,#155402,#155403,#155404,#155405,#155406,
#155407,#155408,#155409,#155410,#155411,#155412,#155413,#155414,#155415,
#155416,#155417,#155418,#155419,#155420,#155421,#155422,#155423,#155424,
#155425,#155426,#155427,#155428,#155429,#155430,#155431,#155432,#155433,
#155434,#155435,#155436,#155437,#155438,#155439,#155440),.UNSPECIFIED.,
 .F.,.F.)
B_SPLINE_CURVE_WITH_KNOTS((6,1,1,1,1,1,1,1,1,1,1,1,1,1,1,1,1,1,1,1,1,1,
1,1,1,1,1,1,1,1,1,1,1,1,1,1,1,1,1,1,1,1,1,1,1,1,1,1,1,1,1,1,1,1,1,1,1,1,
1,1,1,1,1,1,1,1,1,1,1,1,1,1,1,1,1,1,1,1,1,1,1,1,1,1,1,1,1,1,1,1,1,1,1,1,
1,1,1,1,1,1,1,1,1,1,1,1,1,1,1,1,1,1,1,1,1,1,1,1,1,1,1,1,1,1,1,1,1,1,1,1,
1,1,1,1,1,1,1,1,1,1,1,1,1,1,1,1,1,1,1,1,1,1,1,1,1,1,1,1,1,1,1,1,1,1,1,1,
1,1,1,1,1,1,1,1,1,1,1,1,1,1,1,1,1,1,1,1,1,1,1,6),(-0.941429844438021,-0.940000000000001,
-0.935000000000001,-0.930000000000001,-0.925000000000001,-0.920000000000001,
-0.915000000000001,-0.910000000000001,-0.905000000000001,-0.900000000000001,
-0.895000000000001,-0.890000000000001,-0.885000000000001,-0.880000000000001,
-0.875000000000001,-0.870000000000001,-0.865000000000001,-0.860000000000001,
-0.855000000000001,-0.850000000000001,-0.845000000000001,-0.840000000000001,
-0.835000000000001,-0.830000000000001,-0.825000000000001,-0.820000000000001,
-0.815000000000001,-0.810000000000001,-0.805000000000001,-0.800000000000001,
-0.795000000000001,-0.790000000000001,-0.785000000000001,-0.780000000000001,
-0.775000000000001,-0.770000000000001,-0.765000000000001,-0.760000000000001,
-0.755000000000001,-0.750000000000001,-0.745000000000001,-0.740000000000001,
-0.735000000000001,-0.730000000000001,-0.725000000000001,-0.720000000000001,
-0.715000000000001,-0.710000000000001,-0.705000000000001,-0.700000000000001,
-0.695000000000001,-0.690000000000001,-0.685,-0.68,-0.675,-0.67,-0.665,
-0.66,-0.655,-0.65,-0.645,-0.64,-0.635,-0.63,-0.625,-0.62,-0.615,-0.61,
-0.605,-0.6,-0.595,-0.59,-0.585,-0.58,-0.575,-0.57,-0.565,-0.56,-0.555,
-0.55,-0.545,-0.54,-0.535,-0.53,-0.525,-0.52,-0.515,-0.51,-0.505,-0.5,-0.495,
-0.49,-0.485,-0.48,-0.475,-0.47,-0.465,-0.46,-0.455,-0.45,-0.445,-0.44,
-0.435,-0.43,-0.425,-0.42,-0.415,-0.41,-0.405,-0.4,-0.395,-0.39,-0.385,
-0.38,-0.375,-0.37,-0.365,-0.36,-0.355,-0.35,-0.345,-0.34,-0.335,-0.33,
-0.325,-0.32,-0.315,-0.31,-0.305,-0.3,-0.295,-0.29,-0.285,-0.28,-0.275,
-0.27,-0.265,-0.26,-0.255,-0.25,-0.245,-0.24,-0.235,-0.23,-0.225,-0.22,
-0.215,-0.21,-0.205,-0.2,-0.195,-0.19,-0.185,-0.18,-0.175,-0.17,-0.165,
-0.16,-0.155,-0.15,-0.145,-0.14,-0.135,-0.13,-0.125,-0.12,-0.115,-0.11,
-0.105,-0.1,-0.095,-0.09,-0.085,-0.08,-0.075,-0.07,-0.065,-0.06,-0.055,
-0.05,-0.045,-0.04,-0.035,-0.03,-0.025,-0.02,-0.015,-0.01,-0.005,0.),
 .UNSPECIFIED.)
CURVE()
GEOMETRIC_REPRESENTATION_ITEM()
RATIONAL_B_SPLINE_CURVE((1.,1.,1.,1.,1.,1.,1.,1.,1.,1.,1.,1.,1.,1.,1.,1.,
1.,1.,1.,1.,1.,1.,1.,1.,1.,1.,1.,1.,1.,1.,1.,1.,1.,1.,1.,1.,1.,1.,1.,1.,
1.,1.,1.,1.,1.,1.,1.,1.,1.,1.,1.,1.,1.,1.,1.,1.,1.,1.,1.,1.,1.,1.,1.,1.,
1.,1.,1.,1.,1.,1.,1.,1.,1.,1.,1.,1.,1.,1.,1.,1.,1.,1.,1.,1.,1.,1.,1.,1.,
1.,1.,1.,1.,1.,1.,1.,1.,1.,1.,1.,1.,1.,1.,1.,1.,1.,1.,1.,1.,1.,1.,1.,1.,
1.,1.,1.,1.,1.,1.,1.,1.,1.,1.,1.,1.,1.,1.,1.,1.,1.,1.,1.,1.,1.,1.,1.,1.,
1.,1.,1.,1.,1.,1.,1.,1.,1.,1.,1.,1.,1.,1.,1.,1.,1.,1.,1.,1.,1.,1.,1.,1.,
1.,1.,1.,1.,1.,1.,1.,1.,1.,1.,1.,1.,1.,1.,1.,1.,1.,1.,1.,1.,1.,1.,1.,1.,
1.,1.,1.,1.,1.,1.,1.,1.,1.,1.))
REPRESENTATION_ITEM('')
);
#643=(
BOUNDED_CURVE()
B_SPLINE_CURVE(5,(#155852,#155853,#155854,#155855,#155856,#155857,#155858,
#155859,#155860,#155861,#155862,#155863,#155864,#155865,#155866,#155867,
#155868,#155869,#155870,#155871,#155872,#155873,#155874,#155875,#155876,
#155877,#155878,#155879,#155880,#155881,#155882,#155883,#155884,#155885,
#155886,#155887,#155888,#155889,#155890,#155891,#155892,#155893,#155894,
#155895,#155896,#155897,#155898,#155899,#155900,#155901,#155902,#155903,
#155904,#155905,#155906,#155907,#155908,#155909,#155910,#155911,#155912,
#155913,#155914,#155915,#155916,#155917,#155918,#155919,#155920,#155921,
#155922,#155923,#155924,#155925,#155926,#155927,#155928,#155929,#155930,
#155931,#155932,#155933,#155934,#155935,#155936,#155937,#155938,#155939,
#155940,#155941,#155942,#155943,#155944,#155945,#155946,#155947,#155948,
#155949,#155950,#155951,#155952,#155953,#155954,#155955,#155956,#155957,
#155958,#155959,#155960,#155961,#155962,#155963,#155964,#155965,#155966,
#155967,#155968,#155969,#155970,#155971,#155972,#155973,#155974,#155975,
#155976,#155977,#155978,#155979,#155980,#155981,#155982,#155983,#155984,
#155985,#155986,#155987,#155988,#155989,#155990,#155991,#155992,#155993,
#155994,#155995,#155996,#155997,#155998,#155999,#156000,#156001,#156002,
#156003,#156004,#156005,#156006,#156007,#156008,#156009,#156010,#156011,
#156012,#156013,#156014,#156015,#156016,#156017,#156018,#156019,#156020,
#156021,#156022,#156023,#156024,#156025,#156026,#156027,#156028,#156029,
#156030,#156031,#156032,#156033,#156034,#156035,#156036,#156037,#156038,
#156039,#156040,#156041,#156042,#156043,#156044,#156045),.UNSPECIFIED.,
 .F.,.F.)
B_SPLINE_CURVE_WITH_KNOTS((6,1,1,1,1,1,1,1,1,1,1,1,1,1,1,1,1,1,1,1,1,1,
1,1,1,1,1,1,1,1,1,1,1,1,1,1,1,1,1,1,1,1,1,1,1,1,1,1,1,1,1,1,1,1,1,1,1,1,
1,1,1,1,1,1,1,1,1,1,1,1,1,1,1,1,1,1,1,1,1,1,1,1,1,1,1,1,1,1,1,1,1,1,1,1,
1,1,1,1,1,1,1,1,1,1,1,1,1,1,1,1,1,1,1,1,1,1,1,1,1,1,1,1,1,1,1,1,1,1,1,1,
1,1,1,1,1,1,1,1,1,1,1,1,1,1,1,1,1,1,1,1,1,1,1,1,1,1,1,1,1,1,1,1,1,1,1,1,
1,1,1,1,1,1,1,1,1,1,1,1,1,1,1,1,1,1,1,1,1,1,1,6),(0.,0.005,0.01,0.015,0.02,
0.025,0.03,0.035,0.04,0.045,0.05,0.055,0.06,0.065,0.07,0.075,0.08,0.085,
0.09,0.095,0.1,0.105,0.11,0.115,0.12,0.125,0.13,0.135,0.14,0.145,0.15,0.155,
0.16,0.165,0.17,0.175,0.18,0.185,0.19,0.195,0.2,0.205,0.21,0.215,0.22,0.225,
0.23,0.235,0.24,0.245,0.25,0.255,0.26,0.265,0.27,0.275,0.28,0.285,0.29,
0.295,0.3,0.305,0.31,0.315,0.32,0.325,0.33,0.335,0.34,0.345,0.35,0.355,
0.36,0.365,0.37,0.375,0.38,0.385,0.39,0.395,0.4,0.405,0.41,0.415,0.42,0.425,
0.43,0.435,0.44,0.445,0.45,0.455,0.46,0.465,0.47,0.475,0.48,0.485,0.49,
0.495,0.5,0.505,0.51,0.515,0.52,0.525,0.53,0.535,0.54,0.545,0.55,0.555,
0.56,0.565,0.57,0.575,0.58,0.585,0.59,0.595,0.6,0.605,0.61,0.615,0.62,0.625,
0.63,0.635,0.64,0.645,0.65,0.655,0.66,0.665,0.67,0.675,0.68,0.685,0.690000000000001,
0.695000000000001,0.700000000000001,0.705000000000001,0.710000000000001,
0.715000000000001,0.720000000000001,0.725000000000001,0.730000000000001,
0.735000000000001,0.740000000000001,0.745000000000001,0.750000000000001,
0.755000000000001,0.760000000000001,0.765000000000001,0.770000000000001,
0.775000000000001,0.780000000000001,0.785000000000001,0.790000000000001,
0.795000000000001,0.800000000000001,0.805000000000001,0.810000000000001,
0.815000000000001,0.820000000000001,0.825000000000001,0.830000000000001,
0.835000000000001,0.840000000000001,0.845000000000001,0.850000000000001,
0.855000000000001,0.860000000000001,0.865000000000001,0.870000000000001,
0.875000000000001,0.880000000000001,0.885000000000001,0.890000000000001,
0.895000000000001,0.900000000000001,0.905000000000001,0.910000000000001,
0.915000000000001,0.920000000000001,0.925000000000001,0.930000000000001,
0.935000000000001,0.940000000000001,0.941429844438046),.UNSPECIFIED.)
CURVE()
GEOMETRIC_REPRESENTATION_ITEM()
RATIONAL_B_SPLINE_CURVE((1.,1.,1.,1.,1.,1.,1.,1.,1.,1.,1.,1.,1.,1.,1.,1.,
1.,1.,1.,1.,1.,1.,1.,1.,1.,1.,1.,1.,1.,1.,1.,1.,1.,1.,1.,1.,1.,1.,1.,1.,
1.,1.,1.,1.,1.,1.,1.,1.,1.,1.,1.,1.,1.,1.,1.,1.,1.,1.,1.,1.,1.,1.,1.,1.,
1.,1.,1.,1.,1.,1.,1.,1.,1.,1.,1.,1.,1.,1.,1.,1.,1.,1.,1.,1.,1.,1.,1.,1.,
1.,1.,1.,1.,1.,1.,1.,1.,1.,1.,1.,1.,1.,1.,1.,1.,1.,1.,1.,1.,1.,1.,1.,1.,
1.,1.,1.,1.,1.,1.,1.,1.,1.,1.,1.,1.,1.,1.,1.,1.,1.,1.,1.,1.,1.,1.,1.,1.,
1.,1.,1.,1.,1.,1.,1.,1.,1.,1.,1.,1.,1.,1.,1.,1.,1.,1.,1.,1.,1.,1.,1.,1.,
1.,1.,1.,1.,1.,1.,1.,1.,1.,1.,1.,1.,1.,1.,1.,1.,1.,1.,1.,1.,1.,1.,1.,1.,
1.,1.,1.,1.,1.,1.,1.,1.,1.,1.))
REPRESENTATION_ITEM('')
);
#644=(
BOUNDED_CURVE()
B_SPLINE_CURVE(5,(#156048,#156049,#156050,#156051,#156052,#156053,#156054,
#156055,#156056,#156057,#156058,#156059,#156060,#156061,#156062,#156063,
#156064,#156065,#156066,#156067,#156068,#156069,#156070,#156071,#156072,
#156073,#156074,#156075,#156076,#156077,#156078,#156079,#156080,#156081,
#156082,#156083,#156084,#156085,#156086,#156087,#156088,#156089,#156090,
#156091,#156092,#156093,#156094,#156095,#156096,#156097,#156098,#156099,
#156100,#156101,#156102,#156103,#156104,#156105,#156106,#156107,#156108,
#156109,#156110,#156111,#156112,#156113,#156114,#156115,#156116,#156117,
#156118,#156119,#156120,#156121,#156122,#156123,#156124,#156125,#156126,
#156127,#156128,#156129,#156130,#156131,#156132,#156133,#156134,#156135,
#156136,#156137,#156138,#156139,#156140,#156141,#156142,#156143,#156144,
#156145,#156146,#156147,#156148,#156149,#156150,#156151,#156152,#156153,
#156154,#156155,#156156,#156157,#156158,#156159,#156160,#156161,#156162,
#156163,#156164,#156165,#156166,#156167,#156168,#156169,#156170,#156171,
#156172,#156173,#156174,#156175,#156176,#156177,#156178,#156179,#156180,
#156181,#156182,#156183,#156184,#156185,#156186,#156187,#156188,#156189,
#156190,#156191,#156192,#156193,#156194,#156195,#156196,#156197,#156198,
#156199,#156200,#156201,#156202,#156203,#156204,#156205,#156206,#156207,
#156208,#156209,#156210,#156211,#156212,#156213,#156214,#156215,#156216,
#156217,#156218,#156219,#156220,#156221,#156222,#156223,#156224,#156225,
#156226,#156227,#156228,#156229,#156230,#156231,#156232,#156233,#156234,
#156235,#156236,#156237,#156238,#156239,#156240,#156241),.UNSPECIFIED.,
 .F.,.F.)
B_SPLINE_CURVE_WITH_KNOTS((6,1,1,1,1,1,1,1,1,1,1,1,1,1,1,1,1,1,1,1,1,1,
1,1,1,1,1,1,1,1,1,1,1,1,1,1,1,1,1,1,1,1,1,1,1,1,1,1,1,1,1,1,1,1,1,1,1,1,
1,1,1,1,1,1,1,1,1,1,1,1,1,1,1,1,1,1,1,1,1,1,1,1,1,1,1,1,1,1,1,1,1,1,1,1,
1,1,1,1,1,1,1,1,1,1,1,1,1,1,1,1,1,1,1,1,1,1,1,1,1,1,1,1,1,1,1,1,1,1,1,1,
1,1,1,1,1,1,1,1,1,1,1,1,1,1,1,1,1,1,1,1,1,1,1,1,1,1,1,1,1,1,1,1,1,1,1,1,
1,1,1,1,1,1,1,1,1,1,1,1,1,1,1,1,1,1,1,1,1,1,1,6),(-0.941429844438047,-0.940000000000001,
-0.935000000000001,-0.930000000000001,-0.925000000000001,-0.920000000000001,
-0.915000000000001,-0.910000000000001,-0.905000000000001,-0.900000000000001,
-0.895000000000001,-0.890000000000001,-0.885000000000001,-0.880000000000001,
-0.875000000000001,-0.870000000000001,-0.865000000000001,-0.860000000000001,
-0.855000000000001,-0.850000000000001,-0.845000000000001,-0.840000000000001,
-0.835000000000001,-0.830000000000001,-0.825000000000001,-0.820000000000001,
-0.815000000000001,-0.810000000000001,-0.805000000000001,-0.800000000000001,
-0.795000000000001,-0.790000000000001,-0.785000000000001,-0.780000000000001,
-0.775000000000001,-0.770000000000001,-0.765000000000001,-0.760000000000001,
-0.755000000000001,-0.750000000000001,-0.745000000000001,-0.740000000000001,
-0.735000000000001,-0.730000000000001,-0.725000000000001,-0.720000000000001,
-0.715000000000001,-0.710000000000001,-0.705000000000001,-0.700000000000001,
-0.695000000000001,-0.690000000000001,-0.685,-0.68,-0.675,-0.67,-0.665,
-0.66,-0.655,-0.65,-0.645,-0.64,-0.635,-0.63,-0.625,-0.62,-0.615,-0.61,
-0.605,-0.6,-0.595,-0.59,-0.585,-0.58,-0.575,-0.57,-0.565,-0.56,-0.555,
-0.55,-0.545,-0.54,-0.535,-0.53,-0.525,-0.52,-0.515,-0.51,-0.505,-0.5,-0.495,
-0.49,-0.485,-0.48,-0.475,-0.47,-0.465,-0.46,-0.455,-0.45,-0.445,-0.44,
-0.435,-0.43,-0.425,-0.42,-0.415,-0.41,-0.405,-0.4,-0.395,-0.39,-0.385,
-0.38,-0.375,-0.37,-0.365,-0.36,-0.355,-0.35,-0.345,-0.34,-0.335,-0.33,
-0.325,-0.32,-0.315,-0.31,-0.305,-0.3,-0.295,-0.29,-0.285,-0.28,-0.275,
-0.27,-0.265,-0.26,-0.255,-0.25,-0.245,-0.24,-0.235,-0.23,-0.225,-0.22,
-0.215,-0.21,-0.205,-0.2,-0.195,-0.19,-0.185,-0.18,-0.175,-0.17,-0.165,
-0.16,-0.155,-0.15,-0.145,-0.14,-0.135,-0.13,-0.125,-0.12,-0.115,-0.11,
-0.105,-0.1,-0.095,-0.09,-0.085,-0.08,-0.075,-0.07,-0.065,-0.06,-0.055,
-0.05,-0.045,-0.04,-0.035,-0.03,-0.025,-0.02,-0.015,-0.01,-0.005,0.),
 .UNSPECIFIED.)
CURVE()
GEOMETRIC_REPRESENTATION_ITEM()
RATIONAL_B_SPLINE_CURVE((1.,1.,1.,1.,1.,1.,1.,1.,1.,1.,1.,1.,1.,1.,1.,1.,
1.,1.,1.,1.,1.,1.,1.,1.,1.,1.,1.,1.,1.,1.,1.,1.,1.,1.,1.,1.,1.,1.,1.,1.,
1.,1.,1.,1.,1.,1.,1.,1.,1.,1.,1.,1.,1.,1.,1.,1.,1.,1.,1.,1.,1.,1.,1.,1.,
1.,1.,1.,1.,1.,1.,1.,1.,1.,1.,1.,1.,1.,1.,1.,1.,1.,1.,1.,1.,1.,1.,1.,1.,
1.,1.,1.,1.,1.,1.,1.,1.,1.,1.,1.,1.,1.,1.,1.,1.,1.,1.,1.,1.,1.,1.,1.,1.,
1.,1.,1.,1.,1.,1.,1.,1.,1.,1.,1.,1.,1.,1.,1.,1.,1.,1.,1.,1.,1.,1.,1.,1.,
1.,1.,1.,1.,1.,1.,1.,1.,1.,1.,1.,1.,1.,1.,1.,1.,1.,1.,1.,1.,1.,1.,1.,1.,
1.,1.,1.,1.,1.,1.,1.,1.,1.,1.,1.,1.,1.,1.,1.,1.,1.,1.,1.,1.,1.,1.,1.,1.,
1.,1.,1.,1.,1.,1.,1.,1.,1.,1.))
REPRESENTATION_ITEM('')
);
#645=(
BOUNDED_CURVE()
B_SPLINE_CURVE(5,(#156653,#156654,#156655,#156656,#156657,#156658,#156659,
#156660,#156661,#156662,#156663,#156664,#156665,#156666,#156667,#156668,
#156669,#156670,#156671,#156672,#156673,#156674,#156675,#156676,#156677,
#156678,#156679,#156680,#156681,#156682,#156683,#156684,#156685,#156686,
#156687,#156688,#156689,#156690,#156691,#156692,#156693,#156694,#156695,
#156696,#156697,#156698,#156699,#156700,#156701,#156702,#156703,#156704,
#156705,#156706,#156707,#156708,#156709,#156710,#156711,#156712,#156713,
#156714,#156715,#156716,#156717,#156718,#156719,#156720,#156721,#156722,
#156723,#156724,#156725,#156726,#156727,#156728,#156729,#156730,#156731,
#156732,#156733,#156734,#156735,#156736,#156737,#156738,#156739,#156740,
#156741,#156742,#156743,#156744,#156745,#156746,#156747,#156748,#156749,
#156750,#156751,#156752,#156753,#156754,#156755,#156756,#156757,#156758,
#156759,#156760,#156761,#156762,#156763,#156764,#156765,#156766,#156767,
#156768,#156769,#156770,#156771,#156772,#156773,#156774,#156775,#156776,
#156777,#156778,#156779,#156780,#156781,#156782,#156783,#156784,#156785,
#156786,#156787,#156788,#156789,#156790,#156791,#156792,#156793,#156794,
#156795,#156796,#156797,#156798,#156799,#156800,#156801,#156802,#156803,
#156804,#156805,#156806,#156807,#156808,#156809,#156810,#156811,#156812,
#156813,#156814,#156815,#156816,#156817,#156818,#156819,#156820,#156821,
#156822,#156823,#156824,#156825,#156826,#156827,#156828,#156829,#156830,
#156831,#156832,#156833,#156834,#156835,#156836,#156837,#156838,#156839,
#156840,#156841,#156842,#156843,#156844,#156845,#156846),.UNSPECIFIED.,
 .F.,.F.)
B_SPLINE_CURVE_WITH_KNOTS((6,1,1,1,1,1,1,1,1,1,1,1,1,1,1,1,1,1,1,1,1,1,
1,1,1,1,1,1,1,1,1,1,1,1,1,1,1,1,1,1,1,1,1,1,1,1,1,1,1,1,1,1,1,1,1,1,1,1,
1,1,1,1,1,1,1,1,1,1,1,1,1,1,1,1,1,1,1,1,1,1,1,1,1,1,1,1,1,1,1,1,1,1,1,1,
1,1,1,1,1,1,1,1,1,1,1,1,1,1,1,1,1,1,1,1,1,1,1,1,1,1,1,1,1,1,1,1,1,1,1,1,
1,1,1,1,1,1,1,1,1,1,1,1,1,1,1,1,1,1,1,1,1,1,1,1,1,1,1,1,1,1,1,1,1,1,1,1,
1,1,1,1,1,1,1,1,1,1,1,1,1,1,1,1,1,1,1,1,1,1,1,6),(0.,0.005,0.01,0.015,0.02,
0.025,0.03,0.035,0.04,0.045,0.05,0.055,0.06,0.065,0.07,0.075,0.08,0.085,
0.09,0.095,0.1,0.105,0.11,0.115,0.12,0.125,0.13,0.135,0.14,0.145,0.15,0.155,
0.16,0.165,0.17,0.175,0.18,0.185,0.19,0.195,0.2,0.205,0.21,0.215,0.22,0.225,
0.23,0.235,0.24,0.245,0.25,0.255,0.26,0.265,0.27,0.275,0.28,0.285,0.29,
0.295,0.3,0.305,0.31,0.315,0.32,0.325,0.33,0.335,0.34,0.345,0.35,0.355,
0.36,0.365,0.37,0.375,0.38,0.385,0.39,0.395,0.4,0.405,0.41,0.415,0.42,0.425,
0.43,0.435,0.44,0.445,0.45,0.455,0.46,0.465,0.47,0.475,0.48,0.485,0.49,
0.495,0.5,0.505,0.51,0.515,0.52,0.525,0.53,0.535,0.54,0.545,0.55,0.555,
0.56,0.565,0.57,0.575,0.58,0.585,0.59,0.595,0.6,0.605,0.61,0.615,0.62,0.625,
0.63,0.635,0.64,0.645,0.65,0.655,0.66,0.665,0.67,0.675,0.68,0.685,0.690000000000001,
0.695000000000001,0.700000000000001,0.705000000000001,0.710000000000001,
0.715000000000001,0.720000000000001,0.725000000000001,0.730000000000001,
0.735000000000001,0.740000000000001,0.745000000000001,0.750000000000001,
0.755000000000001,0.760000000000001,0.765000000000001,0.770000000000001,
0.775000000000001,0.780000000000001,0.785000000000001,0.790000000000001,
0.795000000000001,0.800000000000001,0.805000000000001,0.810000000000001,
0.815000000000001,0.820000000000001,0.825000000000001,0.830000000000001,
0.835000000000001,0.840000000000001,0.845000000000001,0.850000000000001,
0.855000000000001,0.860000000000001,0.865000000000001,0.870000000000001,
0.875000000000001,0.880000000000001,0.885000000000001,0.890000000000001,
0.895000000000001,0.900000000000001,0.905000000000001,0.910000000000001,
0.915000000000001,0.920000000000001,0.925000000000001,0.930000000000001,
0.935000000000001,0.940000000000001,0.94142984443804),.UNSPECIFIED.)
CURVE()
GEOMETRIC_REPRESENTATION_ITEM()
RATIONAL_B_SPLINE_CURVE((1.,1.,1.,1.,1.,1.,1.,1.,1.,1.,1.,1.,1.,1.,1.,1.,
1.,1.,1.,1.,1.,1.,1.,1.,1.,1.,1.,1.,1.,1.,1.,1.,1.,1.,1.,1.,1.,1.,1.,1.,
1.,1.,1.,1.,1.,1.,1.,1.,1.,1.,1.,1.,1.,1.,1.,1.,1.,1.,1.,1.,1.,1.,1.,1.,
1.,1.,1.,1.,1.,1.,1.,1.,1.,1.,1.,1.,1.,1.,1.,1.,1.,1.,1.,1.,1.,1.,1.,1.,
1.,1.,1.,1.,1.,1.,1.,1.,1.,1.,1.,1.,1.,1.,1.,1.,1.,1.,1.,1.,1.,1.,1.,1.,
1.,1.,1.,1.,1.,1.,1.,1.,1.,1.,1.,1.,1.,1.,1.,1.,1.,1.,1.,1.,1.,1.,1.,1.,
1.,1.,1.,1.,1.,1.,1.,1.,1.,1.,1.,1.,1.,1.,1.,1.,1.,1.,1.,1.,1.,1.,1.,1.,
1.,1.,1.,1.,1.,1.,1.,1.,1.,1.,1.,1.,1.,1.,1.,1.,1.,1.,1.,1.,1.,1.,1.,1.,
1.,1.,1.,1.,1.,1.,1.,1.,1.,1.))
REPRESENTATION_ITEM('')
);
#646=(
BOUNDED_CURVE()
B_SPLINE_CURVE(5,(#156849,#156850,#156851,#156852,#156853,#156854,#156855,
#156856,#156857,#156858,#156859,#156860,#156861,#156862,#156863,#156864,
#156865,#156866,#156867,#156868,#156869,#156870,#156871,#156872,#156873,
#156874,#156875,#156876,#156877,#156878,#156879,#156880,#156881,#156882,
#156883,#156884,#156885,#156886,#156887,#156888,#156889,#156890,#156891,
#156892,#156893,#156894,#156895,#156896,#156897,#156898,#156899,#156900,
#156901,#156902,#156903,#156904,#156905,#156906,#156907,#156908,#156909,
#156910,#156911,#156912,#156913,#156914,#156915,#156916,#156917,#156918,
#156919,#156920,#156921,#156922,#156923,#156924,#156925,#156926,#156927,
#156928,#156929,#156930,#156931,#156932,#156933,#156934,#156935,#156936,
#156937,#156938,#156939,#156940,#156941,#156942,#156943,#156944,#156945,
#156946,#156947,#156948,#156949,#156950,#156951,#156952,#156953,#156954,
#156955,#156956,#156957,#156958,#156959,#156960,#156961,#156962,#156963,
#156964,#156965,#156966,#156967,#156968,#156969,#156970,#156971,#156972,
#156973,#156974,#156975,#156976,#156977,#156978,#156979,#156980,#156981,
#156982,#156983,#156984,#156985,#156986,#156987,#156988,#156989,#156990,
#156991,#156992,#156993,#156994,#156995,#156996,#156997,#156998,#156999,
#157000,#157001,#157002,#157003,#157004,#157005,#157006,#157007,#157008,
#157009,#157010,#157011,#157012,#157013,#157014,#157015,#157016,#157017,
#157018,#157019,#157020,#157021,#157022,#157023,#157024,#157025,#157026,
#157027,#157028,#157029,#157030,#157031,#157032,#157033,#157034,#157035,
#157036,#157037,#157038,#157039,#157040,#157041,#157042),.UNSPECIFIED.,
 .F.,.F.)
B_SPLINE_CURVE_WITH_KNOTS((6,1,1,1,1,1,1,1,1,1,1,1,1,1,1,1,1,1,1,1,1,1,
1,1,1,1,1,1,1,1,1,1,1,1,1,1,1,1,1,1,1,1,1,1,1,1,1,1,1,1,1,1,1,1,1,1,1,1,
1,1,1,1,1,1,1,1,1,1,1,1,1,1,1,1,1,1,1,1,1,1,1,1,1,1,1,1,1,1,1,1,1,1,1,1,
1,1,1,1,1,1,1,1,1,1,1,1,1,1,1,1,1,1,1,1,1,1,1,1,1,1,1,1,1,1,1,1,1,1,1,1,
1,1,1,1,1,1,1,1,1,1,1,1,1,1,1,1,1,1,1,1,1,1,1,1,1,1,1,1,1,1,1,1,1,1,1,1,
1,1,1,1,1,1,1,1,1,1,1,1,1,1,1,1,1,1,1,1,1,1,1,6),(-0.94142984443804,-0.940000000000001,
-0.935000000000001,-0.930000000000001,-0.925000000000001,-0.920000000000001,
-0.915000000000001,-0.910000000000001,-0.905000000000001,-0.900000000000001,
-0.895000000000001,-0.890000000000001,-0.885000000000001,-0.880000000000001,
-0.875000000000001,-0.870000000000001,-0.865000000000001,-0.860000000000001,
-0.855000000000001,-0.850000000000001,-0.845000000000001,-0.840000000000001,
-0.835000000000001,-0.830000000000001,-0.825000000000001,-0.820000000000001,
-0.815000000000001,-0.810000000000001,-0.805000000000001,-0.800000000000001,
-0.795000000000001,-0.790000000000001,-0.785000000000001,-0.780000000000001,
-0.775000000000001,-0.770000000000001,-0.765000000000001,-0.760000000000001,
-0.755000000000001,-0.750000000000001,-0.745000000000001,-0.740000000000001,
-0.735000000000001,-0.730000000000001,-0.725000000000001,-0.720000000000001,
-0.715000000000001,-0.710000000000001,-0.705000000000001,-0.700000000000001,
-0.695000000000001,-0.690000000000001,-0.685,-0.68,-0.675,-0.67,-0.665,
-0.66,-0.655,-0.65,-0.645,-0.64,-0.635,-0.63,-0.625,-0.62,-0.615,-0.61,
-0.605,-0.6,-0.595,-0.59,-0.585,-0.58,-0.575,-0.57,-0.565,-0.56,-0.555,
-0.55,-0.545,-0.54,-0.535,-0.53,-0.525,-0.52,-0.515,-0.51,-0.505,-0.5,-0.495,
-0.49,-0.485,-0.48,-0.475,-0.47,-0.465,-0.46,-0.455,-0.45,-0.445,-0.44,
-0.435,-0.43,-0.425,-0.42,-0.415,-0.41,-0.405,-0.4,-0.395,-0.39,-0.385,
-0.38,-0.375,-0.37,-0.365,-0.36,-0.355,-0.35,-0.345,-0.34,-0.335,-0.33,
-0.325,-0.32,-0.315,-0.31,-0.305,-0.3,-0.295,-0.29,-0.285,-0.28,-0.275,
-0.27,-0.265,-0.26,-0.255,-0.25,-0.245,-0.24,-0.235,-0.23,-0.225,-0.22,
-0.215,-0.21,-0.205,-0.2,-0.195,-0.19,-0.185,-0.18,-0.175,-0.17,-0.165,
-0.16,-0.155,-0.15,-0.145,-0.14,-0.135,-0.13,-0.125,-0.12,-0.115,-0.11,
-0.105,-0.1,-0.095,-0.09,-0.085,-0.08,-0.075,-0.07,-0.065,-0.06,-0.055,
-0.05,-0.045,-0.04,-0.035,-0.03,-0.025,-0.02,-0.015,-0.01,-0.005,0.),
 .UNSPECIFIED.)
CURVE()
GEOMETRIC_REPRESENTATION_ITEM()
RATIONAL_B_SPLINE_CURVE((1.,1.,1.,1.,1.,1.,1.,1.,1.,1.,1.,1.,1.,1.,1.,1.,
1.,1.,1.,1.,1.,1.,1.,1.,1.,1.,1.,1.,1.,1.,1.,1.,1.,1.,1.,1.,1.,1.,1.,1.,
1.,1.,1.,1.,1.,1.,1.,1.,1.,1.,1.,1.,1.,1.,1.,1.,1.,1.,1.,1.,1.,1.,1.,1.,
1.,1.,1.,1.,1.,1.,1.,1.,1.,1.,1.,1.,1.,1.,1.,1.,1.,1.,1.,1.,1.,1.,1.,1.,
1.,1.,1.,1.,1.,1.,1.,1.,1.,1.,1.,1.,1.,1.,1.,1.,1.,1.,1.,1.,1.,1.,1.,1.,
1.,1.,1.,1.,1.,1.,1.,1.,1.,1.,1.,1.,1.,1.,1.,1.,1.,1.,1.,1.,1.,1.,1.,1.,
1.,1.,1.,1.,1.,1.,1.,1.,1.,1.,1.,1.,1.,1.,1.,1.,1.,1.,1.,1.,1.,1.,1.,1.,
1.,1.,1.,1.,1.,1.,1.,1.,1.,1.,1.,1.,1.,1.,1.,1.,1.,1.,1.,1.,1.,1.,1.,1.,
1.,1.,1.,1.,1.,1.,1.,1.,1.,1.))
REPRESENTATION_ITEM('')
);
#647=(
BOUNDED_CURVE()
B_SPLINE_CURVE(5,(#157454,#157455,#157456,#157457,#157458,#157459,#157460,
#157461,#157462,#157463,#157464,#157465,#157466,#157467,#157468,#157469,
#157470,#157471,#157472,#157473,#157474,#157475,#157476,#157477,#157478,
#157479,#157480,#157481,#157482,#157483,#157484,#157485,#157486,#157487,
#157488,#157489,#157490,#157491,#157492,#157493,#157494,#157495,#157496,
#157497,#157498,#157499,#157500,#157501,#157502,#157503,#157504,#157505,
#157506,#157507,#157508,#157509,#157510,#157511,#157512,#157513,#157514,
#157515,#157516,#157517,#157518,#157519,#157520,#157521,#157522,#157523,
#157524,#157525,#157526,#157527,#157528,#157529,#157530,#157531,#157532,
#157533,#157534,#157535,#157536,#157537,#157538,#157539,#157540,#157541,
#157542,#157543,#157544,#157545,#157546,#157547,#157548,#157549,#157550,
#157551,#157552,#157553,#157554,#157555,#157556,#157557,#157558,#157559,
#157560,#157561,#157562,#157563,#157564,#157565,#157566,#157567,#157568,
#157569,#157570,#157571,#157572,#157573,#157574,#157575,#157576,#157577,
#157578,#157579,#157580,#157581,#157582,#157583,#157584,#157585,#157586,
#157587,#157588,#157589,#157590,#157591,#157592,#157593,#157594,#157595,
#157596,#157597,#157598,#157599,#157600,#157601,#157602,#157603,#157604,
#157605,#157606,#157607,#157608,#157609,#157610,#157611,#157612,#157613,
#157614,#157615,#157616,#157617,#157618,#157619,#157620,#157621,#157622,
#157623,#157624,#157625,#157626,#157627,#157628,#157629,#157630,#157631,
#157632,#157633,#157634,#157635,#157636,#157637,#157638,#157639,#157640,
#157641,#157642,#157643,#157644,#157645,#157646,#157647),.UNSPECIFIED.,
 .F.,.F.)
B_SPLINE_CURVE_WITH_KNOTS((6,1,1,1,1,1,1,1,1,1,1,1,1,1,1,1,1,1,1,1,1,1,
1,1,1,1,1,1,1,1,1,1,1,1,1,1,1,1,1,1,1,1,1,1,1,1,1,1,1,1,1,1,1,1,1,1,1,1,
1,1,1,1,1,1,1,1,1,1,1,1,1,1,1,1,1,1,1,1,1,1,1,1,1,1,1,1,1,1,1,1,1,1,1,1,
1,1,1,1,1,1,1,1,1,1,1,1,1,1,1,1,1,1,1,1,1,1,1,1,1,1,1,1,1,1,1,1,1,1,1,1,
1,1,1,1,1,1,1,1,1,1,1,1,1,1,1,1,1,1,1,1,1,1,1,1,1,1,1,1,1,1,1,1,1,1,1,1,
1,1,1,1,1,1,1,1,1,1,1,1,1,1,1,1,1,1,1,1,1,1,1,6),(0.,0.005,0.01,0.015,0.02,
0.025,0.03,0.035,0.04,0.045,0.05,0.055,0.06,0.065,0.07,0.075,0.08,0.085,
0.09,0.095,0.1,0.105,0.11,0.115,0.12,0.125,0.13,0.135,0.14,0.145,0.15,0.155,
0.16,0.165,0.17,0.175,0.18,0.185,0.19,0.195,0.2,0.205,0.21,0.215,0.22,0.225,
0.23,0.235,0.24,0.245,0.25,0.255,0.26,0.265,0.27,0.275,0.28,0.285,0.29,
0.295,0.3,0.305,0.31,0.315,0.32,0.325,0.33,0.335,0.34,0.345,0.35,0.355,
0.36,0.365,0.37,0.375,0.38,0.385,0.39,0.395,0.4,0.405,0.41,0.415,0.42,0.425,
0.43,0.435,0.44,0.445,0.45,0.455,0.46,0.465,0.47,0.475,0.48,0.485,0.49,
0.495,0.5,0.505,0.51,0.515,0.52,0.525,0.53,0.535,0.54,0.545,0.55,0.555,
0.56,0.565,0.57,0.575,0.58,0.585,0.59,0.595,0.6,0.605,0.61,0.615,0.62,0.625,
0.63,0.635,0.64,0.645,0.65,0.655,0.66,0.665,0.67,0.675,0.68,0.685,0.690000000000001,
0.695000000000001,0.700000000000001,0.705000000000001,0.710000000000001,
0.715000000000001,0.720000000000001,0.725000000000001,0.730000000000001,
0.735000000000001,0.740000000000001,0.745000000000001,0.750000000000001,
0.755000000000001,0.760000000000001,0.765000000000001,0.770000000000001,
0.775000000000001,0.780000000000001,0.785000000000001,0.790000000000001,
0.795000000000001,0.800000000000001,0.805000000000001,0.810000000000001,
0.815000000000001,0.820000000000001,0.825000000000001,0.830000000000001,
0.835000000000001,0.840000000000001,0.845000000000001,0.850000000000001,
0.855000000000001,0.860000000000001,0.865000000000001,0.870000000000001,
0.875000000000001,0.880000000000001,0.885000000000001,0.890000000000001,
0.895000000000001,0.900000000000001,0.905000000000001,0.910000000000001,
0.915000000000001,0.920000000000001,0.925000000000001,0.930000000000001,
0.935000000000001,0.940000000000001,0.941429844438052),.UNSPECIFIED.)
CURVE()
GEOMETRIC_REPRESENTATION_ITEM()
RATIONAL_B_SPLINE_CURVE((1.,1.,1.,1.,1.,1.,1.,1.,1.,1.,1.,1.,1.,1.,1.,1.,
1.,1.,1.,1.,1.,1.,1.,1.,1.,1.,1.,1.,1.,1.,1.,1.,1.,1.,1.,1.,1.,1.,1.,1.,
1.,1.,1.,1.,1.,1.,1.,1.,1.,1.,1.,1.,1.,1.,1.,1.,1.,1.,1.,1.,1.,1.,1.,1.,
1.,1.,1.,1.,1.,1.,1.,1.,1.,1.,1.,1.,1.,1.,1.,1.,1.,1.,1.,1.,1.,1.,1.,1.,
1.,1.,1.,1.,1.,1.,1.,1.,1.,1.,1.,1.,1.,1.,1.,1.,1.,1.,1.,1.,1.,1.,1.,1.,
1.,1.,1.,1.,1.,1.,1.,1.,1.,1.,1.,1.,1.,1.,1.,1.,1.,1.,1.,1.,1.,1.,1.,1.,
1.,1.,1.,1.,1.,1.,1.,1.,1.,1.,1.,1.,1.,1.,1.,1.,1.,1.,1.,1.,1.,1.,1.,1.,
1.,1.,1.,1.,1.,1.,1.,1.,1.,1.,1.,1.,1.,1.,1.,1.,1.,1.,1.,1.,1.,1.,1.,1.,
1.,1.,1.,1.,1.,1.,1.,1.,1.,1.))
REPRESENTATION_ITEM('')
);
#648=(
BOUNDED_CURVE()
B_SPLINE_CURVE(5,(#157650,#157651,#157652,#157653,#157654,#157655,#157656,
#157657,#157658,#157659,#157660,#157661,#157662,#157663,#157664,#157665,
#157666,#157667,#157668,#157669,#157670,#157671,#157672,#157673,#157674,
#157675,#157676,#157677,#157678,#157679,#157680,#157681,#157682,#157683,
#157684,#157685,#157686,#157687,#157688,#157689,#157690,#157691,#157692,
#157693,#157694,#157695,#157696,#157697,#157698,#157699,#157700,#157701,
#157702,#157703,#157704,#157705,#157706,#157707,#157708,#157709,#157710,
#157711,#157712,#157713,#157714,#157715,#157716,#157717,#157718,#157719,
#157720,#157721,#157722,#157723,#157724,#157725,#157726,#157727,#157728,
#157729,#157730,#157731,#157732,#157733,#157734,#157735,#157736,#157737,
#157738,#157739,#157740,#157741,#157742,#157743,#157744,#157745,#157746,
#157747,#157748,#157749,#157750,#157751,#157752,#157753,#157754,#157755,
#157756,#157757,#157758,#157759,#157760,#157761,#157762,#157763,#157764,
#157765,#157766,#157767,#157768,#157769,#157770,#157771,#157772,#157773,
#157774,#157775,#157776,#157777,#157778,#157779,#157780,#157781,#157782,
#157783,#157784,#157785,#157786,#157787,#157788,#157789,#157790,#157791,
#157792,#157793,#157794,#157795,#157796,#157797,#157798,#157799,#157800,
#157801,#157802,#157803,#157804,#157805,#157806,#157807,#157808,#157809,
#157810,#157811,#157812,#157813,#157814,#157815,#157816,#157817,#157818,
#157819,#157820,#157821,#157822,#157823,#157824,#157825,#157826,#157827,
#157828,#157829,#157830,#157831,#157832,#157833,#157834,#157835,#157836,
#157837,#157838,#157839,#157840,#157841,#157842,#157843),.UNSPECIFIED.,
 .F.,.F.)
B_SPLINE_CURVE_WITH_KNOTS((6,1,1,1,1,1,1,1,1,1,1,1,1,1,1,1,1,1,1,1,1,1,
1,1,1,1,1,1,1,1,1,1,1,1,1,1,1,1,1,1,1,1,1,1,1,1,1,1,1,1,1,1,1,1,1,1,1,1,
1,1,1,1,1,1,1,1,1,1,1,1,1,1,1,1,1,1,1,1,1,1,1,1,1,1,1,1,1,1,1,1,1,1,1,1,
1,1,1,1,1,1,1,1,1,1,1,1,1,1,1,1,1,1,1,1,1,1,1,1,1,1,1,1,1,1,1,1,1,1,1,1,
1,1,1,1,1,1,1,1,1,1,1,1,1,1,1,1,1,1,1,1,1,1,1,1,1,1,1,1,1,1,1,1,1,1,1,1,
1,1,1,1,1,1,1,1,1,1,1,1,1,1,1,1,1,1,1,1,1,1,1,6),(-0.941429844438052,-0.940000000000001,
-0.935000000000001,-0.930000000000001,-0.925000000000001,-0.920000000000001,
-0.915000000000001,-0.910000000000001,-0.905000000000001,-0.900000000000001,
-0.895000000000001,-0.890000000000001,-0.885000000000001,-0.880000000000001,
-0.875000000000001,-0.870000000000001,-0.865000000000001,-0.860000000000001,
-0.855000000000001,-0.850000000000001,-0.845000000000001,-0.840000000000001,
-0.835000000000001,-0.830000000000001,-0.825000000000001,-0.820000000000001,
-0.815000000000001,-0.810000000000001,-0.805000000000001,-0.800000000000001,
-0.795000000000001,-0.790000000000001,-0.785000000000001,-0.780000000000001,
-0.775000000000001,-0.770000000000001,-0.765000000000001,-0.760000000000001,
-0.755000000000001,-0.750000000000001,-0.745000000000001,-0.740000000000001,
-0.735000000000001,-0.730000000000001,-0.725000000000001,-0.720000000000001,
-0.715000000000001,-0.710000000000001,-0.705000000000001,-0.700000000000001,
-0.695000000000001,-0.690000000000001,-0.685,-0.68,-0.675,-0.67,-0.665,
-0.66,-0.655,-0.65,-0.645,-0.64,-0.635,-0.63,-0.625,-0.62,-0.615,-0.61,
-0.605,-0.6,-0.595,-0.59,-0.585,-0.58,-0.575,-0.57,-0.565,-0.56,-0.555,
-0.55,-0.545,-0.54,-0.535,-0.53,-0.525,-0.52,-0.515,-0.51,-0.505,-0.5,-0.495,
-0.49,-0.485,-0.48,-0.475,-0.47,-0.465,-0.46,-0.455,-0.45,-0.445,-0.44,
-0.435,-0.43,-0.425,-0.42,-0.415,-0.41,-0.405,-0.4,-0.395,-0.39,-0.385,
-0.38,-0.375,-0.37,-0.365,-0.36,-0.355,-0.35,-0.345,-0.34,-0.335,-0.33,
-0.325,-0.32,-0.315,-0.31,-0.305,-0.3,-0.295,-0.29,-0.285,-0.28,-0.275,
-0.27,-0.265,-0.26,-0.255,-0.25,-0.245,-0.24,-0.235,-0.23,-0.225,-0.22,
-0.215,-0.21,-0.205,-0.2,-0.195,-0.19,-0.185,-0.18,-0.175,-0.17,-0.165,
-0.16,-0.155,-0.15,-0.145,-0.14,-0.135,-0.13,-0.125,-0.12,-0.115,-0.11,
-0.105,-0.1,-0.095,-0.09,-0.085,-0.08,-0.075,-0.07,-0.065,-0.06,-0.055,
-0.05,-0.045,-0.04,-0.035,-0.03,-0.025,-0.02,-0.015,-0.01,-0.005,0.),
 .UNSPECIFIED.)
CURVE()
GEOMETRIC_REPRESENTATION_ITEM()
RATIONAL_B_SPLINE_CURVE((1.,1.,1.,1.,1.,1.,1.,1.,1.,1.,1.,1.,1.,1.,1.,1.,
1.,1.,1.,1.,1.,1.,1.,1.,1.,1.,1.,1.,1.,1.,1.,1.,1.,1.,1.,1.,1.,1.,1.,1.,
1.,1.,1.,1.,1.,1.,1.,1.,1.,1.,1.,1.,1.,1.,1.,1.,1.,1.,1.,1.,1.,1.,1.,1.,
1.,1.,1.,1.,1.,1.,1.,1.,1.,1.,1.,1.,1.,1.,1.,1.,1.,1.,1.,1.,1.,1.,1.,1.,
1.,1.,1.,1.,1.,1.,1.,1.,1.,1.,1.,1.,1.,1.,1.,1.,1.,1.,1.,1.,1.,1.,1.,1.,
1.,1.,1.,1.,1.,1.,1.,1.,1.,1.,1.,1.,1.,1.,1.,1.,1.,1.,1.,1.,1.,1.,1.,1.,
1.,1.,1.,1.,1.,1.,1.,1.,1.,1.,1.,1.,1.,1.,1.,1.,1.,1.,1.,1.,1.,1.,1.,1.,
1.,1.,1.,1.,1.,1.,1.,1.,1.,1.,1.,1.,1.,1.,1.,1.,1.,1.,1.,1.,1.,1.,1.,1.,
1.,1.,1.,1.,1.,1.,1.,1.,1.,1.))
REPRESENTATION_ITEM('')
);
#649=(
BOUNDED_CURVE()
B_SPLINE_CURVE(5,(#158255,#158256,#158257,#158258,#158259,#158260,#158261,
#158262,#158263,#158264,#158265,#158266,#158267,#158268,#158269,#158270,
#158271,#158272,#158273,#158274,#158275,#158276,#158277,#158278,#158279,
#158280,#158281,#158282,#158283,#158284,#158285,#158286,#158287,#158288,
#158289,#158290,#158291,#158292,#158293,#158294,#158295,#158296,#158297,
#158298,#158299,#158300,#158301,#158302,#158303,#158304,#158305,#158306,
#158307,#158308,#158309,#158310,#158311,#158312,#158313,#158314,#158315,
#158316,#158317,#158318,#158319,#158320,#158321,#158322,#158323,#158324,
#158325,#158326,#158327,#158328,#158329,#158330,#158331,#158332,#158333,
#158334,#158335,#158336,#158337,#158338,#158339,#158340,#158341,#158342,
#158343,#158344,#158345,#158346,#158347,#158348,#158349,#158350,#158351,
#158352,#158353,#158354,#158355,#158356,#158357,#158358,#158359,#158360,
#158361,#158362,#158363,#158364,#158365,#158366,#158367,#158368,#158369,
#158370,#158371,#158372,#158373,#158374,#158375,#158376,#158377,#158378,
#158379,#158380,#158381,#158382,#158383,#158384,#158385,#158386,#158387,
#158388,#158389,#158390,#158391,#158392,#158393,#158394,#158395,#158396,
#158397,#158398,#158399,#158400,#158401,#158402,#158403,#158404,#158405,
#158406,#158407,#158408,#158409,#158410,#158411,#158412,#158413,#158414,
#158415,#158416,#158417,#158418,#158419,#158420,#158421,#158422,#158423,
#158424,#158425,#158426,#158427,#158428,#158429,#158430,#158431,#158432,
#158433,#158434,#158435,#158436,#158437,#158438,#158439,#158440,#158441,
#158442,#158443,#158444,#158445,#158446,#158447,#158448),.UNSPECIFIED.,
 .F.,.F.)
B_SPLINE_CURVE_WITH_KNOTS((6,1,1,1,1,1,1,1,1,1,1,1,1,1,1,1,1,1,1,1,1,1,
1,1,1,1,1,1,1,1,1,1,1,1,1,1,1,1,1,1,1,1,1,1,1,1,1,1,1,1,1,1,1,1,1,1,1,1,
1,1,1,1,1,1,1,1,1,1,1,1,1,1,1,1,1,1,1,1,1,1,1,1,1,1,1,1,1,1,1,1,1,1,1,1,
1,1,1,1,1,1,1,1,1,1,1,1,1,1,1,1,1,1,1,1,1,1,1,1,1,1,1,1,1,1,1,1,1,1,1,1,
1,1,1,1,1,1,1,1,1,1,1,1,1,1,1,1,1,1,1,1,1,1,1,1,1,1,1,1,1,1,1,1,1,1,1,1,
1,1,1,1,1,1,1,1,1,1,1,1,1,1,1,1,1,1,1,1,1,1,1,6),(0.,0.005,0.01,0.015,0.02,
0.025,0.03,0.035,0.04,0.045,0.05,0.055,0.06,0.065,0.07,0.075,0.08,0.085,
0.09,0.095,0.1,0.105,0.11,0.115,0.12,0.125,0.13,0.135,0.14,0.145,0.15,0.155,
0.16,0.165,0.17,0.175,0.18,0.185,0.19,0.195,0.2,0.205,0.21,0.215,0.22,0.225,
0.23,0.235,0.24,0.245,0.25,0.255,0.26,0.265,0.27,0.275,0.28,0.285,0.29,
0.295,0.3,0.305,0.31,0.315,0.32,0.325,0.33,0.335,0.34,0.345,0.35,0.355,
0.36,0.365,0.37,0.375,0.38,0.385,0.39,0.395,0.4,0.405,0.41,0.415,0.42,0.425,
0.43,0.435,0.44,0.445,0.45,0.455,0.46,0.465,0.47,0.475,0.48,0.485,0.49,
0.495,0.5,0.505,0.51,0.515,0.52,0.525,0.53,0.535,0.54,0.545,0.55,0.555,
0.56,0.565,0.57,0.575,0.58,0.585,0.59,0.595,0.6,0.605,0.61,0.615,0.62,0.625,
0.63,0.635,0.64,0.645,0.65,0.655,0.66,0.665,0.67,0.675,0.68,0.685,0.690000000000001,
0.695000000000001,0.700000000000001,0.705000000000001,0.710000000000001,
0.715000000000001,0.720000000000001,0.725000000000001,0.730000000000001,
0.735000000000001,0.740000000000001,0.745000000000001,0.750000000000001,
0.755000000000001,0.760000000000001,0.765000000000001,0.770000000000001,
0.775000000000001,0.780000000000001,0.785000000000001,0.790000000000001,
0.795000000000001,0.800000000000001,0.805000000000001,0.810000000000001,
0.815000000000001,0.820000000000001,0.825000000000001,0.830000000000001,
0.835000000000001,0.840000000000001,0.845000000000001,0.850000000000001,
0.855000000000001,0.860000000000001,0.865000000000001,0.870000000000001,
0.875000000000001,0.880000000000001,0.885000000000001,0.890000000000001,
0.895000000000001,0.900000000000001,0.905000000000001,0.910000000000001,
0.915000000000001,0.920000000000001,0.925000000000001,0.930000000000001,
0.935000000000001,0.940000000000001,0.94142984443803),.UNSPECIFIED.)
CURVE()
GEOMETRIC_REPRESENTATION_ITEM()
RATIONAL_B_SPLINE_CURVE((1.,1.,1.,1.,1.,1.,1.,1.,1.,1.,1.,1.,1.,1.,1.,1.,
1.,1.,1.,1.,1.,1.,1.,1.,1.,1.,1.,1.,1.,1.,1.,1.,1.,1.,1.,1.,1.,1.,1.,1.,
1.,1.,1.,1.,1.,1.,1.,1.,1.,1.,1.,1.,1.,1.,1.,1.,1.,1.,1.,1.,1.,1.,1.,1.,
1.,1.,1.,1.,1.,1.,1.,1.,1.,1.,1.,1.,1.,1.,1.,1.,1.,1.,1.,1.,1.,1.,1.,1.,
1.,1.,1.,1.,1.,1.,1.,1.,1.,1.,1.,1.,1.,1.,1.,1.,1.,1.,1.,1.,1.,1.,1.,1.,
1.,1.,1.,1.,1.,1.,1.,1.,1.,1.,1.,1.,1.,1.,1.,1.,1.,1.,1.,1.,1.,1.,1.,1.,
1.,1.,1.,1.,1.,1.,1.,1.,1.,1.,1.,1.,1.,1.,1.,1.,1.,1.,1.,1.,1.,1.,1.,1.,
1.,1.,1.,1.,1.,1.,1.,1.,1.,1.,1.,1.,1.,1.,1.,1.,1.,1.,1.,1.,1.,1.,1.,1.,
1.,1.,1.,1.,1.,1.,1.,1.,1.,1.))
REPRESENTATION_ITEM('')
);
#650=(
BOUNDED_CURVE()
B_SPLINE_CURVE(5,(#158451,#158452,#158453,#158454,#158455,#158456,#158457,
#158458,#158459,#158460,#158461,#158462,#158463,#158464,#158465,#158466,
#158467,#158468,#158469,#158470,#158471,#158472,#158473,#158474,#158475,
#158476,#158477,#158478,#158479,#158480,#158481,#158482,#158483,#158484,
#158485,#158486,#158487,#158488,#158489,#158490,#158491,#158492,#158493,
#158494,#158495,#158496,#158497,#158498,#158499,#158500,#158501,#158502,
#158503,#158504,#158505,#158506,#158507,#158508,#158509,#158510,#158511,
#158512,#158513,#158514,#158515,#158516,#158517,#158518,#158519,#158520,
#158521,#158522,#158523,#158524,#158525,#158526,#158527,#158528,#158529,
#158530,#158531,#158532,#158533,#158534,#158535,#158536,#158537,#158538,
#158539,#158540,#158541,#158542,#158543,#158544,#158545,#158546,#158547,
#158548,#158549,#158550,#158551,#158552,#158553,#158554,#158555,#158556,
#158557,#158558,#158559,#158560,#158561,#158562,#158563,#158564,#158565,
#158566,#158567,#158568,#158569,#158570,#158571,#158572,#158573,#158574,
#158575,#158576,#158577,#158578,#158579,#158580,#158581,#158582,#158583,
#158584,#158585,#158586,#158587,#158588,#158589,#158590,#158591,#158592,
#158593,#158594,#158595,#158596,#158597,#158598,#158599,#158600,#158601,
#158602,#158603,#158604,#158605,#158606,#158607,#158608,#158609,#158610,
#158611,#158612,#158613,#158614,#158615,#158616,#158617,#158618,#158619,
#158620,#158621,#158622,#158623,#158624,#158625,#158626,#158627,#158628,
#158629,#158630,#158631,#158632,#158633,#158634,#158635,#158636,#158637,
#158638,#158639,#158640,#158641,#158642,#158643,#158644),.UNSPECIFIED.,
 .F.,.F.)
B_SPLINE_CURVE_WITH_KNOTS((6,1,1,1,1,1,1,1,1,1,1,1,1,1,1,1,1,1,1,1,1,1,
1,1,1,1,1,1,1,1,1,1,1,1,1,1,1,1,1,1,1,1,1,1,1,1,1,1,1,1,1,1,1,1,1,1,1,1,
1,1,1,1,1,1,1,1,1,1,1,1,1,1,1,1,1,1,1,1,1,1,1,1,1,1,1,1,1,1,1,1,1,1,1,1,
1,1,1,1,1,1,1,1,1,1,1,1,1,1,1,1,1,1,1,1,1,1,1,1,1,1,1,1,1,1,1,1,1,1,1,1,
1,1,1,1,1,1,1,1,1,1,1,1,1,1,1,1,1,1,1,1,1,1,1,1,1,1,1,1,1,1,1,1,1,1,1,1,
1,1,1,1,1,1,1,1,1,1,1,1,1,1,1,1,1,1,1,1,1,1,1,6),(-0.94142984443803,-0.940000000000001,
-0.935000000000001,-0.930000000000001,-0.925000000000001,-0.920000000000001,
-0.915000000000001,-0.910000000000001,-0.905000000000001,-0.900000000000001,
-0.895000000000001,-0.890000000000001,-0.885000000000001,-0.880000000000001,
-0.875000000000001,-0.870000000000001,-0.865000000000001,-0.860000000000001,
-0.855000000000001,-0.850000000000001,-0.845000000000001,-0.840000000000001,
-0.835000000000001,-0.830000000000001,-0.825000000000001,-0.820000000000001,
-0.815000000000001,-0.810000000000001,-0.805000000000001,-0.800000000000001,
-0.795000000000001,-0.790000000000001,-0.785000000000001,-0.780000000000001,
-0.775000000000001,-0.770000000000001,-0.765000000000001,-0.760000000000001,
-0.755000000000001,-0.750000000000001,-0.745000000000001,-0.740000000000001,
-0.735000000000001,-0.730000000000001,-0.725000000000001,-0.720000000000001,
-0.715000000000001,-0.710000000000001,-0.705000000000001,-0.700000000000001,
-0.695000000000001,-0.690000000000001,-0.685,-0.68,-0.675,-0.67,-0.665,
-0.66,-0.655,-0.65,-0.645,-0.64,-0.635,-0.63,-0.625,-0.62,-0.615,-0.61,
-0.605,-0.6,-0.595,-0.59,-0.585,-0.58,-0.575,-0.57,-0.565,-0.56,-0.555,
-0.55,-0.545,-0.54,-0.535,-0.53,-0.525,-0.52,-0.515,-0.51,-0.505,-0.5,-0.495,
-0.49,-0.485,-0.48,-0.475,-0.47,-0.465,-0.46,-0.455,-0.45,-0.445,-0.44,
-0.435,-0.43,-0.425,-0.42,-0.415,-0.41,-0.405,-0.4,-0.395,-0.39,-0.385,
-0.38,-0.375,-0.37,-0.365,-0.36,-0.355,-0.35,-0.345,-0.34,-0.335,-0.33,
-0.325,-0.32,-0.315,-0.31,-0.305,-0.3,-0.295,-0.29,-0.285,-0.28,-0.275,
-0.27,-0.265,-0.26,-0.255,-0.25,-0.245,-0.24,-0.235,-0.23,-0.225,-0.22,
-0.215,-0.21,-0.205,-0.2,-0.195,-0.19,-0.185,-0.18,-0.175,-0.17,-0.165,
-0.16,-0.155,-0.15,-0.145,-0.14,-0.135,-0.13,-0.125,-0.12,-0.115,-0.11,
-0.105,-0.1,-0.095,-0.09,-0.085,-0.08,-0.075,-0.07,-0.065,-0.06,-0.055,
-0.05,-0.045,-0.04,-0.035,-0.03,-0.025,-0.02,-0.015,-0.01,-0.005,0.),
 .UNSPECIFIED.)
CURVE()
GEOMETRIC_REPRESENTATION_ITEM()
RATIONAL_B_SPLINE_CURVE((1.,1.,1.,1.,1.,1.,1.,1.,1.,1.,1.,1.,1.,1.,1.,1.,
1.,1.,1.,1.,1.,1.,1.,1.,1.,1.,1.,1.,1.,1.,1.,1.,1.,1.,1.,1.,1.,1.,1.,1.,
1.,1.,1.,1.,1.,1.,1.,1.,1.,1.,1.,1.,1.,1.,1.,1.,1.,1.,1.,1.,1.,1.,1.,1.,
1.,1.,1.,1.,1.,1.,1.,1.,1.,1.,1.,1.,1.,1.,1.,1.,1.,1.,1.,1.,1.,1.,1.,1.,
1.,1.,1.,1.,1.,1.,1.,1.,1.,1.,1.,1.,1.,1.,1.,1.,1.,1.,1.,1.,1.,1.,1.,1.,
1.,1.,1.,1.,1.,1.,1.,1.,1.,1.,1.,1.,1.,1.,1.,1.,1.,1.,1.,1.,1.,1.,1.,1.,
1.,1.,1.,1.,1.,1.,1.,1.,1.,1.,1.,1.,1.,1.,1.,1.,1.,1.,1.,1.,1.,1.,1.,1.,
1.,1.,1.,1.,1.,1.,1.,1.,1.,1.,1.,1.,1.,1.,1.,1.,1.,1.,1.,1.,1.,1.,1.,1.,
1.,1.,1.,1.,1.,1.,1.,1.,1.,1.))
REPRESENTATION_ITEM('')
);
#651=(
BOUNDED_CURVE()
B_SPLINE_CURVE(5,(#159056,#159057,#159058,#159059,#159060,#159061,#159062,
#159063,#159064,#159065,#159066,#159067,#159068,#159069,#159070,#159071,
#159072,#159073,#159074,#159075,#159076,#159077,#159078,#159079,#159080,
#159081,#159082,#159083,#159084,#159085,#159086,#159087,#159088,#159089,
#159090,#159091,#159092,#159093,#159094,#159095,#159096,#159097,#159098,
#159099,#159100,#159101,#159102,#159103,#159104,#159105,#159106,#159107,
#159108,#159109,#159110,#159111,#159112,#159113,#159114,#159115,#159116,
#159117,#159118,#159119,#159120,#159121,#159122,#159123,#159124,#159125,
#159126,#159127,#159128,#159129,#159130,#159131,#159132,#159133,#159134,
#159135,#159136,#159137,#159138,#159139,#159140,#159141,#159142,#159143,
#159144,#159145,#159146,#159147,#159148,#159149,#159150,#159151,#159152,
#159153,#159154,#159155,#159156,#159157,#159158,#159159,#159160,#159161,
#159162,#159163,#159164,#159165,#159166,#159167,#159168,#159169,#159170,
#159171,#159172,#159173,#159174,#159175,#159176,#159177,#159178,#159179,
#159180,#159181,#159182,#159183,#159184,#159185,#159186,#159187,#159188,
#159189,#159190,#159191,#159192,#159193,#159194,#159195,#159196,#159197,
#159198,#159199,#159200,#159201,#159202,#159203,#159204,#159205,#159206,
#159207,#159208,#159209,#159210,#159211,#159212,#159213,#159214,#159215,
#159216,#159217,#159218,#159219,#159220,#159221,#159222,#159223,#159224,
#159225,#159226,#159227,#159228,#159229,#159230,#159231,#159232,#159233,
#159234,#159235,#159236,#159237,#159238,#159239,#159240,#159241,#159242,
#159243,#159244,#159245,#159246,#159247,#159248,#159249),.UNSPECIFIED.,
 .F.,.F.)
B_SPLINE_CURVE_WITH_KNOTS((6,1,1,1,1,1,1,1,1,1,1,1,1,1,1,1,1,1,1,1,1,1,
1,1,1,1,1,1,1,1,1,1,1,1,1,1,1,1,1,1,1,1,1,1,1,1,1,1,1,1,1,1,1,1,1,1,1,1,
1,1,1,1,1,1,1,1,1,1,1,1,1,1,1,1,1,1,1,1,1,1,1,1,1,1,1,1,1,1,1,1,1,1,1,1,
1,1,1,1,1,1,1,1,1,1,1,1,1,1,1,1,1,1,1,1,1,1,1,1,1,1,1,1,1,1,1,1,1,1,1,1,
1,1,1,1,1,1,1,1,1,1,1,1,1,1,1,1,1,1,1,1,1,1,1,1,1,1,1,1,1,1,1,1,1,1,1,1,
1,1,1,1,1,1,1,1,1,1,1,1,1,1,1,1,1,1,1,1,1,1,1,6),(0.,0.005,0.01,0.015,0.02,
0.025,0.03,0.035,0.04,0.045,0.05,0.055,0.06,0.065,0.07,0.075,0.08,0.085,
0.09,0.095,0.1,0.105,0.11,0.115,0.12,0.125,0.13,0.135,0.14,0.145,0.15,0.155,
0.16,0.165,0.17,0.175,0.18,0.185,0.19,0.195,0.2,0.205,0.21,0.215,0.22,0.225,
0.23,0.235,0.24,0.245,0.25,0.255,0.26,0.265,0.27,0.275,0.28,0.285,0.29,
0.295,0.3,0.305,0.31,0.315,0.32,0.325,0.33,0.335,0.34,0.345,0.35,0.355,
0.36,0.365,0.37,0.375,0.38,0.385,0.39,0.395,0.4,0.405,0.41,0.415,0.42,0.425,
0.43,0.435,0.44,0.445,0.45,0.455,0.46,0.465,0.47,0.475,0.48,0.485,0.49,
0.495,0.5,0.505,0.51,0.515,0.52,0.525,0.53,0.535,0.54,0.545,0.55,0.555,
0.56,0.565,0.57,0.575,0.58,0.585,0.59,0.595,0.6,0.605,0.61,0.615,0.62,0.625,
0.63,0.635,0.64,0.645,0.65,0.655,0.66,0.665,0.67,0.675,0.68,0.685,0.690000000000001,
0.695000000000001,0.700000000000001,0.705000000000001,0.710000000000001,
0.715000000000001,0.720000000000001,0.725000000000001,0.730000000000001,
0.735000000000001,0.740000000000001,0.745000000000001,0.750000000000001,
0.755000000000001,0.760000000000001,0.765000000000001,0.770000000000001,
0.775000000000001,0.780000000000001,0.785000000000001,0.790000000000001,
0.795000000000001,0.800000000000001,0.805000000000001,0.810000000000001,
0.815000000000001,0.820000000000001,0.825000000000001,0.830000000000001,
0.835000000000001,0.840000000000001,0.845000000000001,0.850000000000001,
0.855000000000001,0.860000000000001,0.865000000000001,0.870000000000001,
0.875000000000001,0.880000000000001,0.885000000000001,0.890000000000001,
0.895000000000001,0.900000000000001,0.905000000000001,0.910000000000001,
0.915000000000001,0.920000000000001,0.925000000000001,0.930000000000001,
0.935000000000001,0.940000000000001,0.94142984443804),.UNSPECIFIED.)
CURVE()
GEOMETRIC_REPRESENTATION_ITEM()
RATIONAL_B_SPLINE_CURVE((1.,1.,1.,1.,1.,1.,1.,1.,1.,1.,1.,1.,1.,1.,1.,1.,
1.,1.,1.,1.,1.,1.,1.,1.,1.,1.,1.,1.,1.,1.,1.,1.,1.,1.,1.,1.,1.,1.,1.,1.,
1.,1.,1.,1.,1.,1.,1.,1.,1.,1.,1.,1.,1.,1.,1.,1.,1.,1.,1.,1.,1.,1.,1.,1.,
1.,1.,1.,1.,1.,1.,1.,1.,1.,1.,1.,1.,1.,1.,1.,1.,1.,1.,1.,1.,1.,1.,1.,1.,
1.,1.,1.,1.,1.,1.,1.,1.,1.,1.,1.,1.,1.,1.,1.,1.,1.,1.,1.,1.,1.,1.,1.,1.,
1.,1.,1.,1.,1.,1.,1.,1.,1.,1.,1.,1.,1.,1.,1.,1.,1.,1.,1.,1.,1.,1.,1.,1.,
1.,1.,1.,1.,1.,1.,1.,1.,1.,1.,1.,1.,1.,1.,1.,1.,1.,1.,1.,1.,1.,1.,1.,1.,
1.,1.,1.,1.,1.,1.,1.,1.,1.,1.,1.,1.,1.,1.,1.,1.,1.,1.,1.,1.,1.,1.,1.,1.,
1.,1.,1.,1.,1.,1.,1.,1.,1.,1.))
REPRESENTATION_ITEM('')
);
#652=(
BOUNDED_CURVE()
B_SPLINE_CURVE(5,(#159252,#159253,#159254,#159255,#159256,#159257,#159258,
#159259,#159260,#159261,#159262,#159263,#159264,#159265,#159266,#159267,
#159268,#159269,#159270,#159271,#159272,#159273,#159274,#159275,#159276,
#159277,#159278,#159279,#159280,#159281,#159282,#159283,#159284,#159285,
#159286,#159287,#159288,#159289,#159290,#159291,#159292,#159293,#159294,
#159295,#159296,#159297,#159298,#159299,#159300,#159301,#159302,#159303,
#159304,#159305,#159306,#159307,#159308,#159309,#159310,#159311,#159312,
#159313,#159314,#159315,#159316,#159317,#159318,#159319,#159320,#159321,
#159322,#159323,#159324,#159325,#159326,#159327,#159328,#159329,#159330,
#159331,#159332,#159333,#159334,#159335,#159336,#159337,#159338,#159339,
#159340,#159341,#159342,#159343,#159344,#159345,#159346,#159347,#159348,
#159349,#159350,#159351,#159352,#159353,#159354,#159355,#159356,#159357,
#159358,#159359,#159360,#159361,#159362,#159363,#159364,#159365,#159366,
#159367,#159368,#159369,#159370,#159371,#159372,#159373,#159374,#159375,
#159376,#159377,#159378,#159379,#159380,#159381,#159382,#159383,#159384,
#159385,#159386,#159387,#159388,#159389,#159390,#159391,#159392,#159393,
#159394,#159395,#159396,#159397,#159398,#159399,#159400,#159401,#159402,
#159403,#159404,#159405,#159406,#159407,#159408,#159409,#159410,#159411,
#159412,#159413,#159414,#159415,#159416,#159417,#159418,#159419,#159420,
#159421,#159422,#159423,#159424,#159425,#159426,#159427,#159428,#159429,
#159430,#159431,#159432,#159433,#159434,#159435,#159436,#159437,#159438,
#159439,#159440,#159441,#159442,#159443,#159444,#159445),.UNSPECIFIED.,
 .F.,.F.)
B_SPLINE_CURVE_WITH_KNOTS((6,1,1,1,1,1,1,1,1,1,1,1,1,1,1,1,1,1,1,1,1,1,
1,1,1,1,1,1,1,1,1,1,1,1,1,1,1,1,1,1,1,1,1,1,1,1,1,1,1,1,1,1,1,1,1,1,1,1,
1,1,1,1,1,1,1,1,1,1,1,1,1,1,1,1,1,1,1,1,1,1,1,1,1,1,1,1,1,1,1,1,1,1,1,1,
1,1,1,1,1,1,1,1,1,1,1,1,1,1,1,1,1,1,1,1,1,1,1,1,1,1,1,1,1,1,1,1,1,1,1,1,
1,1,1,1,1,1,1,1,1,1,1,1,1,1,1,1,1,1,1,1,1,1,1,1,1,1,1,1,1,1,1,1,1,1,1,1,
1,1,1,1,1,1,1,1,1,1,1,1,1,1,1,1,1,1,1,1,1,1,1,6),(-0.941429844438064,-0.940000000000001,
-0.935000000000001,-0.930000000000001,-0.925000000000001,-0.920000000000001,
-0.915000000000001,-0.910000000000001,-0.905000000000001,-0.900000000000001,
-0.895000000000001,-0.890000000000001,-0.885000000000001,-0.880000000000001,
-0.875000000000001,-0.870000000000001,-0.865000000000001,-0.860000000000001,
-0.855000000000001,-0.850000000000001,-0.845000000000001,-0.840000000000001,
-0.835000000000001,-0.830000000000001,-0.825000000000001,-0.820000000000001,
-0.815000000000001,-0.810000000000001,-0.805000000000001,-0.800000000000001,
-0.795000000000001,-0.790000000000001,-0.785000000000001,-0.780000000000001,
-0.775000000000001,-0.770000000000001,-0.765000000000001,-0.760000000000001,
-0.755000000000001,-0.750000000000001,-0.745000000000001,-0.740000000000001,
-0.735000000000001,-0.730000000000001,-0.725000000000001,-0.720000000000001,
-0.715000000000001,-0.710000000000001,-0.705000000000001,-0.700000000000001,
-0.695000000000001,-0.690000000000001,-0.685,-0.68,-0.675,-0.67,-0.665,
-0.66,-0.655,-0.65,-0.645,-0.64,-0.635,-0.63,-0.625,-0.62,-0.615,-0.61,
-0.605,-0.6,-0.595,-0.59,-0.585,-0.58,-0.575,-0.57,-0.565,-0.56,-0.555,
-0.55,-0.545,-0.54,-0.535,-0.53,-0.525,-0.52,-0.515,-0.51,-0.505,-0.5,-0.495,
-0.49,-0.485,-0.48,-0.475,-0.47,-0.465,-0.46,-0.455,-0.45,-0.445,-0.44,
-0.435,-0.43,-0.425,-0.42,-0.415,-0.41,-0.405,-0.4,-0.395,-0.39,-0.385,
-0.38,-0.375,-0.37,-0.365,-0.36,-0.355,-0.35,-0.345,-0.34,-0.335,-0.33,
-0.325,-0.32,-0.315,-0.31,-0.305,-0.3,-0.295,-0.29,-0.285,-0.28,-0.275,
-0.27,-0.265,-0.26,-0.255,-0.25,-0.245,-0.24,-0.235,-0.23,-0.225,-0.22,
-0.215,-0.21,-0.205,-0.2,-0.195,-0.19,-0.185,-0.18,-0.175,-0.17,-0.165,
-0.16,-0.155,-0.15,-0.145,-0.14,-0.135,-0.13,-0.125,-0.12,-0.115,-0.11,
-0.105,-0.1,-0.095,-0.09,-0.085,-0.08,-0.075,-0.07,-0.065,-0.06,-0.055,
-0.05,-0.045,-0.04,-0.035,-0.03,-0.025,-0.02,-0.015,-0.01,-0.005,0.),
 .UNSPECIFIED.)
CURVE()
GEOMETRIC_REPRESENTATION_ITEM()
RATIONAL_B_SPLINE_CURVE((1.,1.,1.,1.,1.,1.,1.,1.,1.,1.,1.,1.,1.,1.,1.,1.,
1.,1.,1.,1.,1.,1.,1.,1.,1.,1.,1.,1.,1.,1.,1.,1.,1.,1.,1.,1.,1.,1.,1.,1.,
1.,1.,1.,1.,1.,1.,1.,1.,1.,1.,1.,1.,1.,1.,1.,1.,1.,1.,1.,1.,1.,1.,1.,1.,
1.,1.,1.,1.,1.,1.,1.,1.,1.,1.,1.,1.,1.,1.,1.,1.,1.,1.,1.,1.,1.,1.,1.,1.,
1.,1.,1.,1.,1.,1.,1.,1.,1.,1.,1.,1.,1.,1.,1.,1.,1.,1.,1.,1.,1.,1.,1.,1.,
1.,1.,1.,1.,1.,1.,1.,1.,1.,1.,1.,1.,1.,1.,1.,1.,1.,1.,1.,1.,1.,1.,1.,1.,
1.,1.,1.,1.,1.,1.,1.,1.,1.,1.,1.,1.,1.,1.,1.,1.,1.,1.,1.,1.,1.,1.,1.,1.,
1.,1.,1.,1.,1.,1.,1.,1.,1.,1.,1.,1.,1.,1.,1.,1.,1.,1.,1.,1.,1.,1.,1.,1.,
1.,1.,1.,1.,1.,1.,1.,1.,1.,1.))
REPRESENTATION_ITEM('')
);
#653=(
BOUNDED_CURVE()
B_SPLINE_CURVE(5,(#159857,#159858,#159859,#159860,#159861,#159862,#159863,
#159864,#159865,#159866,#159867,#159868,#159869,#159870,#159871,#159872,
#159873,#159874,#159875,#159876,#159877,#159878,#159879,#159880,#159881,
#159882,#159883,#159884,#159885,#159886,#159887,#159888,#159889,#159890,
#159891,#159892,#159893,#159894,#159895,#159896,#159897,#159898,#159899,
#159900,#159901,#159902,#159903,#159904,#159905,#159906,#159907,#159908,
#159909,#159910,#159911,#159912,#159913,#159914,#159915,#159916,#159917,
#159918,#159919,#159920,#159921,#159922,#159923,#159924,#159925,#159926,
#159927,#159928,#159929,#159930,#159931,#159932,#159933,#159934,#159935,
#159936,#159937,#159938,#159939,#159940,#159941,#159942,#159943,#159944,
#159945,#159946,#159947,#159948,#159949,#159950,#159951,#159952,#159953,
#159954,#159955,#159956,#159957,#159958,#159959,#159960,#159961,#159962,
#159963,#159964,#159965,#159966,#159967,#159968,#159969,#159970,#159971,
#159972,#159973,#159974,#159975,#159976,#159977,#159978,#159979,#159980,
#159981,#159982,#159983,#159984,#159985,#159986,#159987,#159988,#159989,
#159990,#159991,#159992,#159993,#159994,#159995,#159996,#159997,#159998,
#159999,#160000,#160001,#160002,#160003,#160004,#160005,#160006,#160007,
#160008,#160009,#160010,#160011,#160012,#160013,#160014,#160015,#160016,
#160017,#160018,#160019,#160020,#160021,#160022,#160023,#160024,#160025,
#160026,#160027,#160028,#160029,#160030,#160031,#160032,#160033,#160034,
#160035,#160036,#160037,#160038,#160039,#160040,#160041,#160042,#160043,
#160044,#160045,#160046,#160047,#160048,#160049,#160050),.UNSPECIFIED.,
 .F.,.F.)
B_SPLINE_CURVE_WITH_KNOTS((6,1,1,1,1,1,1,1,1,1,1,1,1,1,1,1,1,1,1,1,1,1,
1,1,1,1,1,1,1,1,1,1,1,1,1,1,1,1,1,1,1,1,1,1,1,1,1,1,1,1,1,1,1,1,1,1,1,1,
1,1,1,1,1,1,1,1,1,1,1,1,1,1,1,1,1,1,1,1,1,1,1,1,1,1,1,1,1,1,1,1,1,1,1,1,
1,1,1,1,1,1,1,1,1,1,1,1,1,1,1,1,1,1,1,1,1,1,1,1,1,1,1,1,1,1,1,1,1,1,1,1,
1,1,1,1,1,1,1,1,1,1,1,1,1,1,1,1,1,1,1,1,1,1,1,1,1,1,1,1,1,1,1,1,1,1,1,1,
1,1,1,1,1,1,1,1,1,1,1,1,1,1,1,1,1,1,1,1,1,1,1,6),(0.,0.005,0.01,0.015,0.02,
0.025,0.03,0.035,0.04,0.045,0.05,0.055,0.06,0.065,0.07,0.075,0.08,0.085,
0.09,0.095,0.1,0.105,0.11,0.115,0.12,0.125,0.13,0.135,0.14,0.145,0.15,0.155,
0.16,0.165,0.17,0.175,0.18,0.185,0.19,0.195,0.2,0.205,0.21,0.215,0.22,0.225,
0.23,0.235,0.24,0.245,0.25,0.255,0.26,0.265,0.27,0.275,0.28,0.285,0.29,
0.295,0.3,0.305,0.31,0.315,0.32,0.325,0.33,0.335,0.34,0.345,0.35,0.355,
0.36,0.365,0.37,0.375,0.38,0.385,0.39,0.395,0.4,0.405,0.41,0.415,0.42,0.425,
0.43,0.435,0.44,0.445,0.45,0.455,0.46,0.465,0.47,0.475,0.48,0.485,0.49,
0.495,0.5,0.505,0.51,0.515,0.52,0.525,0.53,0.535,0.54,0.545,0.55,0.555,
0.56,0.565,0.57,0.575,0.58,0.585,0.59,0.595,0.6,0.605,0.61,0.615,0.62,0.625,
0.63,0.635,0.64,0.645,0.65,0.655,0.66,0.665,0.67,0.675,0.68,0.685,0.690000000000001,
0.695000000000001,0.700000000000001,0.705000000000001,0.710000000000001,
0.715000000000001,0.720000000000001,0.725000000000001,0.730000000000001,
0.735000000000001,0.740000000000001,0.745000000000001,0.750000000000001,
0.755000000000001,0.760000000000001,0.765000000000001,0.770000000000001,
0.775000000000001,0.780000000000001,0.785000000000001,0.790000000000001,
0.795000000000001,0.800000000000001,0.805000000000001,0.810000000000001,
0.815000000000001,0.820000000000001,0.825000000000001,0.830000000000001,
0.835000000000001,0.840000000000001,0.845000000000001,0.850000000000001,
0.855000000000001,0.860000000000001,0.865000000000001,0.870000000000001,
0.875000000000001,0.880000000000001,0.885000000000001,0.890000000000001,
0.895000000000001,0.900000000000001,0.905000000000001,0.910000000000001,
0.915000000000001,0.920000000000001,0.925000000000001,0.930000000000001,
0.935000000000001,0.940000000000001,0.941429844438021),.UNSPECIFIED.)
CURVE()
GEOMETRIC_REPRESENTATION_ITEM()
RATIONAL_B_SPLINE_CURVE((1.,1.,1.,1.,1.,1.,1.,1.,1.,1.,1.,1.,1.,1.,1.,1.,
1.,1.,1.,1.,1.,1.,1.,1.,1.,1.,1.,1.,1.,1.,1.,1.,1.,1.,1.,1.,1.,1.,1.,1.,
1.,1.,1.,1.,1.,1.,1.,1.,1.,1.,1.,1.,1.,1.,1.,1.,1.,1.,1.,1.,1.,1.,1.,1.,
1.,1.,1.,1.,1.,1.,1.,1.,1.,1.,1.,1.,1.,1.,1.,1.,1.,1.,1.,1.,1.,1.,1.,1.,
1.,1.,1.,1.,1.,1.,1.,1.,1.,1.,1.,1.,1.,1.,1.,1.,1.,1.,1.,1.,1.,1.,1.,1.,
1.,1.,1.,1.,1.,1.,1.,1.,1.,1.,1.,1.,1.,1.,1.,1.,1.,1.,1.,1.,1.,1.,1.,1.,
1.,1.,1.,1.,1.,1.,1.,1.,1.,1.,1.,1.,1.,1.,1.,1.,1.,1.,1.,1.,1.,1.,1.,1.,
1.,1.,1.,1.,1.,1.,1.,1.,1.,1.,1.,1.,1.,1.,1.,1.,1.,1.,1.,1.,1.,1.,1.,1.,
1.,1.,1.,1.,1.,1.,1.,1.,1.,1.))
REPRESENTATION_ITEM('')
);
#654=(
BOUNDED_CURVE()
B_SPLINE_CURVE(5,(#160053,#160054,#160055,#160056,#160057,#160058,#160059,
#160060,#160061,#160062,#160063,#160064,#160065,#160066,#160067,#160068,
#160069,#160070,#160071,#160072,#160073,#160074,#160075,#160076,#160077,
#160078,#160079,#160080,#160081,#160082,#160083,#160084,#160085,#160086,
#160087,#160088,#160089,#160090,#160091,#160092,#160093,#160094,#160095,
#160096,#160097,#160098,#160099,#160100,#160101,#160102,#160103,#160104,
#160105,#160106,#160107,#160108,#160109,#160110,#160111,#160112,#160113,
#160114,#160115,#160116,#160117,#160118,#160119,#160120,#160121,#160122,
#160123,#160124,#160125,#160126,#160127,#160128,#160129,#160130,#160131,
#160132,#160133,#160134,#160135,#160136,#160137,#160138,#160139,#160140,
#160141,#160142,#160143,#160144,#160145,#160146,#160147,#160148,#160149,
#160150,#160151,#160152,#160153,#160154,#160155,#160156,#160157,#160158,
#160159,#160160,#160161,#160162,#160163,#160164,#160165,#160166,#160167,
#160168,#160169,#160170,#160171,#160172,#160173,#160174,#160175,#160176,
#160177,#160178,#160179,#160180,#160181,#160182,#160183,#160184,#160185,
#160186,#160187,#160188,#160189,#160190,#160191,#160192,#160193,#160194,
#160195,#160196,#160197,#160198,#160199,#160200,#160201,#160202,#160203,
#160204,#160205,#160206,#160207,#160208,#160209,#160210,#160211,#160212,
#160213,#160214,#160215,#160216,#160217,#160218,#160219,#160220,#160221,
#160222,#160223,#160224,#160225,#160226,#160227,#160228,#160229,#160230,
#160231,#160232,#160233,#160234,#160235,#160236,#160237,#160238,#160239,
#160240,#160241,#160242,#160243,#160244,#160245,#160246),.UNSPECIFIED.,
 .F.,.F.)
B_SPLINE_CURVE_WITH_KNOTS((6,1,1,1,1,1,1,1,1,1,1,1,1,1,1,1,1,1,1,1,1,1,
1,1,1,1,1,1,1,1,1,1,1,1,1,1,1,1,1,1,1,1,1,1,1,1,1,1,1,1,1,1,1,1,1,1,1,1,
1,1,1,1,1,1,1,1,1,1,1,1,1,1,1,1,1,1,1,1,1,1,1,1,1,1,1,1,1,1,1,1,1,1,1,1,
1,1,1,1,1,1,1,1,1,1,1,1,1,1,1,1,1,1,1,1,1,1,1,1,1,1,1,1,1,1,1,1,1,1,1,1,
1,1,1,1,1,1,1,1,1,1,1,1,1,1,1,1,1,1,1,1,1,1,1,1,1,1,1,1,1,1,1,1,1,1,1,1,
1,1,1,1,1,1,1,1,1,1,1,1,1,1,1,1,1,1,1,1,1,1,1,6),(-0.941429844438021,-0.940000000000001,
-0.935000000000001,-0.930000000000001,-0.925000000000001,-0.920000000000001,
-0.915000000000001,-0.910000000000001,-0.905000000000001,-0.900000000000001,
-0.895000000000001,-0.890000000000001,-0.885000000000001,-0.880000000000001,
-0.875000000000001,-0.870000000000001,-0.865000000000001,-0.860000000000001,
-0.855000000000001,-0.850000000000001,-0.845000000000001,-0.840000000000001,
-0.835000000000001,-0.830000000000001,-0.825000000000001,-0.820000000000001,
-0.815000000000001,-0.810000000000001,-0.805000000000001,-0.800000000000001,
-0.795000000000001,-0.790000000000001,-0.785000000000001,-0.780000000000001,
-0.775000000000001,-0.770000000000001,-0.765000000000001,-0.760000000000001,
-0.755000000000001,-0.750000000000001,-0.745000000000001,-0.740000000000001,
-0.735000000000001,-0.730000000000001,-0.725000000000001,-0.720000000000001,
-0.715000000000001,-0.710000000000001,-0.705000000000001,-0.700000000000001,
-0.695000000000001,-0.690000000000001,-0.685,-0.68,-0.675,-0.67,-0.665,
-0.66,-0.655,-0.65,-0.645,-0.64,-0.635,-0.63,-0.625,-0.62,-0.615,-0.61,
-0.605,-0.6,-0.595,-0.59,-0.585,-0.58,-0.575,-0.57,-0.565,-0.56,-0.555,
-0.55,-0.545,-0.54,-0.535,-0.53,-0.525,-0.52,-0.515,-0.51,-0.505,-0.5,-0.495,
-0.49,-0.485,-0.48,-0.475,-0.47,-0.465,-0.46,-0.455,-0.45,-0.445,-0.44,
-0.435,-0.43,-0.425,-0.42,-0.415,-0.41,-0.405,-0.4,-0.395,-0.39,-0.385,
-0.38,-0.375,-0.37,-0.365,-0.36,-0.355,-0.35,-0.345,-0.34,-0.335,-0.33,
-0.325,-0.32,-0.315,-0.31,-0.305,-0.3,-0.295,-0.29,-0.285,-0.28,-0.275,
-0.27,-0.265,-0.26,-0.255,-0.25,-0.245,-0.24,-0.235,-0.23,-0.225,-0.22,
-0.215,-0.21,-0.205,-0.2,-0.195,-0.19,-0.185,-0.18,-0.175,-0.17,-0.165,
-0.16,-0.155,-0.15,-0.145,-0.14,-0.135,-0.13,-0.125,-0.12,-0.115,-0.11,
-0.105,-0.1,-0.095,-0.09,-0.085,-0.08,-0.075,-0.07,-0.065,-0.06,-0.055,
-0.05,-0.045,-0.04,-0.035,-0.03,-0.025,-0.02,-0.015,-0.01,-0.005,0.),
 .UNSPECIFIED.)
CURVE()
GEOMETRIC_REPRESENTATION_ITEM()
RATIONAL_B_SPLINE_CURVE((1.,1.,1.,1.,1.,1.,1.,1.,1.,1.,1.,1.,1.,1.,1.,1.,
1.,1.,1.,1.,1.,1.,1.,1.,1.,1.,1.,1.,1.,1.,1.,1.,1.,1.,1.,1.,1.,1.,1.,1.,
1.,1.,1.,1.,1.,1.,1.,1.,1.,1.,1.,1.,1.,1.,1.,1.,1.,1.,1.,1.,1.,1.,1.,1.,
1.,1.,1.,1.,1.,1.,1.,1.,1.,1.,1.,1.,1.,1.,1.,1.,1.,1.,1.,1.,1.,1.,1.,1.,
1.,1.,1.,1.,1.,1.,1.,1.,1.,1.,1.,1.,1.,1.,1.,1.,1.,1.,1.,1.,1.,1.,1.,1.,
1.,1.,1.,1.,1.,1.,1.,1.,1.,1.,1.,1.,1.,1.,1.,1.,1.,1.,1.,1.,1.,1.,1.,1.,
1.,1.,1.,1.,1.,1.,1.,1.,1.,1.,1.,1.,1.,1.,1.,1.,1.,1.,1.,1.,1.,1.,1.,1.,
1.,1.,1.,1.,1.,1.,1.,1.,1.,1.,1.,1.,1.,1.,1.,1.,1.,1.,1.,1.,1.,1.,1.,1.,
1.,1.,1.,1.,1.,1.,1.,1.,1.,1.))
REPRESENTATION_ITEM('')
);
#655=(
BOUNDED_CURVE()
B_SPLINE_CURVE(5,(#160658,#160659,#160660,#160661,#160662,#160663,#160664,
#160665,#160666,#160667,#160668,#160669,#160670,#160671,#160672,#160673,
#160674,#160675,#160676,#160677,#160678,#160679,#160680,#160681,#160682,
#160683,#160684,#160685,#160686,#160687,#160688,#160689,#160690,#160691,
#160692,#160693,#160694,#160695,#160696,#160697,#160698,#160699,#160700,
#160701,#160702,#160703,#160704,#160705,#160706,#160707,#160708,#160709,
#160710,#160711,#160712,#160713,#160714,#160715,#160716,#160717,#160718,
#160719,#160720,#160721,#160722,#160723,#160724,#160725,#160726,#160727,
#160728,#160729,#160730,#160731,#160732,#160733,#160734,#160735,#160736,
#160737,#160738,#160739,#160740,#160741,#160742,#160743,#160744,#160745,
#160746,#160747,#160748,#160749,#160750,#160751,#160752,#160753,#160754,
#160755,#160756,#160757,#160758,#160759,#160760,#160761,#160762,#160763,
#160764,#160765,#160766,#160767,#160768,#160769,#160770,#160771,#160772,
#160773,#160774,#160775,#160776,#160777,#160778,#160779,#160780,#160781,
#160782,#160783,#160784,#160785,#160786,#160787,#160788,#160789,#160790,
#160791,#160792,#160793,#160794,#160795,#160796,#160797,#160798,#160799,
#160800,#160801,#160802,#160803,#160804,#160805,#160806,#160807,#160808,
#160809,#160810,#160811,#160812,#160813,#160814,#160815,#160816,#160817,
#160818,#160819,#160820,#160821,#160822,#160823,#160824,#160825,#160826,
#160827,#160828,#160829,#160830,#160831,#160832,#160833,#160834,#160835,
#160836,#160837,#160838,#160839,#160840,#160841,#160842,#160843,#160844,
#160845,#160846,#160847,#160848,#160849,#160850,#160851),.UNSPECIFIED.,
 .F.,.F.)
B_SPLINE_CURVE_WITH_KNOTS((6,1,1,1,1,1,1,1,1,1,1,1,1,1,1,1,1,1,1,1,1,1,
1,1,1,1,1,1,1,1,1,1,1,1,1,1,1,1,1,1,1,1,1,1,1,1,1,1,1,1,1,1,1,1,1,1,1,1,
1,1,1,1,1,1,1,1,1,1,1,1,1,1,1,1,1,1,1,1,1,1,1,1,1,1,1,1,1,1,1,1,1,1,1,1,
1,1,1,1,1,1,1,1,1,1,1,1,1,1,1,1,1,1,1,1,1,1,1,1,1,1,1,1,1,1,1,1,1,1,1,1,
1,1,1,1,1,1,1,1,1,1,1,1,1,1,1,1,1,1,1,1,1,1,1,1,1,1,1,1,1,1,1,1,1,1,1,1,
1,1,1,1,1,1,1,1,1,1,1,1,1,1,1,1,1,1,1,1,1,1,1,6),(0.,0.005,0.01,0.015,0.02,
0.025,0.03,0.035,0.04,0.045,0.05,0.055,0.06,0.065,0.07,0.075,0.08,0.085,
0.09,0.095,0.1,0.105,0.11,0.115,0.12,0.125,0.13,0.135,0.14,0.145,0.15,0.155,
0.16,0.165,0.17,0.175,0.18,0.185,0.19,0.195,0.2,0.205,0.21,0.215,0.22,0.225,
0.23,0.235,0.24,0.245,0.25,0.255,0.26,0.265,0.27,0.275,0.28,0.285,0.29,
0.295,0.3,0.305,0.31,0.315,0.32,0.325,0.33,0.335,0.34,0.345,0.35,0.355,
0.36,0.365,0.37,0.375,0.38,0.385,0.39,0.395,0.4,0.405,0.41,0.415,0.42,0.425,
0.43,0.435,0.44,0.445,0.45,0.455,0.46,0.465,0.47,0.475,0.48,0.485,0.49,
0.495,0.5,0.505,0.51,0.515,0.52,0.525,0.53,0.535,0.54,0.545,0.55,0.555,
0.56,0.565,0.57,0.575,0.58,0.585,0.59,0.595,0.6,0.605,0.61,0.615,0.62,0.625,
0.63,0.635,0.64,0.645,0.65,0.655,0.66,0.665,0.67,0.675,0.68,0.685,0.690000000000001,
0.695000000000001,0.700000000000001,0.705000000000001,0.710000000000001,
0.715000000000001,0.720000000000001,0.725000000000001,0.730000000000001,
0.735000000000001,0.740000000000001,0.745000000000001,0.750000000000001,
0.755000000000001,0.760000000000001,0.765000000000001,0.770000000000001,
0.775000000000001,0.780000000000001,0.785000000000001,0.790000000000001,
0.795000000000001,0.800000000000001,0.805000000000001,0.810000000000001,
0.815000000000001,0.820000000000001,0.825000000000001,0.830000000000001,
0.835000000000001,0.840000000000001,0.845000000000001,0.850000000000001,
0.855000000000001,0.860000000000001,0.865000000000001,0.870000000000001,
0.875000000000001,0.880000000000001,0.885000000000001,0.890000000000001,
0.895000000000001,0.900000000000001,0.905000000000001,0.910000000000001,
0.915000000000001,0.920000000000001,0.925000000000001,0.930000000000001,
0.935000000000001,0.940000000000001,0.941429844438003),.UNSPECIFIED.)
CURVE()
GEOMETRIC_REPRESENTATION_ITEM()
RATIONAL_B_SPLINE_CURVE((1.,1.,1.,1.,1.,1.,1.,1.,1.,1.,1.,1.,1.,1.,1.,1.,
1.,1.,1.,1.,1.,1.,1.,1.,1.,1.,1.,1.,1.,1.,1.,1.,1.,1.,1.,1.,1.,1.,1.,1.,
1.,1.,1.,1.,1.,1.,1.,1.,1.,1.,1.,1.,1.,1.,1.,1.,1.,1.,1.,1.,1.,1.,1.,1.,
1.,1.,1.,1.,1.,1.,1.,1.,1.,1.,1.,1.,1.,1.,1.,1.,1.,1.,1.,1.,1.,1.,1.,1.,
1.,1.,1.,1.,1.,1.,1.,1.,1.,1.,1.,1.,1.,1.,1.,1.,1.,1.,1.,1.,1.,1.,1.,1.,
1.,1.,1.,1.,1.,1.,1.,1.,1.,1.,1.,1.,1.,1.,1.,1.,1.,1.,1.,1.,1.,1.,1.,1.,
1.,1.,1.,1.,1.,1.,1.,1.,1.,1.,1.,1.,1.,1.,1.,1.,1.,1.,1.,1.,1.,1.,1.,1.,
1.,1.,1.,1.,1.,1.,1.,1.,1.,1.,1.,1.,1.,1.,1.,1.,1.,1.,1.,1.,1.,1.,1.,1.,
1.,1.,1.,1.,1.,1.,1.,1.,1.,1.))
REPRESENTATION_ITEM('')
);
#656=(
BOUNDED_CURVE()
B_SPLINE_CURVE(5,(#160854,#160855,#160856,#160857,#160858,#160859,#160860,
#160861,#160862,#160863,#160864,#160865,#160866,#160867,#160868,#160869,
#160870,#160871,#160872,#160873,#160874,#160875,#160876,#160877,#160878,
#160879,#160880,#160881,#160882,#160883,#160884,#160885,#160886,#160887,
#160888,#160889,#160890,#160891,#160892,#160893,#160894,#160895,#160896,
#160897,#160898,#160899,#160900,#160901,#160902,#160903,#160904,#160905,
#160906,#160907,#160908,#160909,#160910,#160911,#160912,#160913,#160914,
#160915,#160916,#160917,#160918,#160919,#160920,#160921,#160922,#160923,
#160924,#160925,#160926,#160927,#160928,#160929,#160930,#160931,#160932,
#160933,#160934,#160935,#160936,#160937,#160938,#160939,#160940,#160941,
#160942,#160943,#160944,#160945,#160946,#160947,#160948,#160949,#160950,
#160951,#160952,#160953,#160954,#160955,#160956,#160957,#160958,#160959,
#160960,#160961,#160962,#160963,#160964,#160965,#160966,#160967,#160968,
#160969,#160970,#160971,#160972,#160973,#160974,#160975,#160976,#160977,
#160978,#160979,#160980,#160981,#160982,#160983,#160984,#160985,#160986,
#160987,#160988,#160989,#160990,#160991,#160992,#160993,#160994,#160995,
#160996,#160997,#160998,#160999,#161000,#161001,#161002,#161003,#161004,
#161005,#161006,#161007,#161008,#161009,#161010,#161011,#161012,#161013,
#161014,#161015,#161016,#161017,#161018,#161019,#161020,#161021,#161022,
#161023,#161024,#161025,#161026,#161027,#161028,#161029,#161030,#161031,
#161032,#161033,#161034,#161035,#161036,#161037,#161038,#161039,#161040,
#161041,#161042,#161043,#161044,#161045,#161046,#161047),.UNSPECIFIED.,
 .F.,.F.)
B_SPLINE_CURVE_WITH_KNOTS((6,1,1,1,1,1,1,1,1,1,1,1,1,1,1,1,1,1,1,1,1,1,
1,1,1,1,1,1,1,1,1,1,1,1,1,1,1,1,1,1,1,1,1,1,1,1,1,1,1,1,1,1,1,1,1,1,1,1,
1,1,1,1,1,1,1,1,1,1,1,1,1,1,1,1,1,1,1,1,1,1,1,1,1,1,1,1,1,1,1,1,1,1,1,1,
1,1,1,1,1,1,1,1,1,1,1,1,1,1,1,1,1,1,1,1,1,1,1,1,1,1,1,1,1,1,1,1,1,1,1,1,
1,1,1,1,1,1,1,1,1,1,1,1,1,1,1,1,1,1,1,1,1,1,1,1,1,1,1,1,1,1,1,1,1,1,1,1,
1,1,1,1,1,1,1,1,1,1,1,1,1,1,1,1,1,1,1,1,1,1,1,6),(-0.941429844438005,-0.940000000000001,
-0.935000000000001,-0.930000000000001,-0.925000000000001,-0.920000000000001,
-0.915000000000001,-0.910000000000001,-0.905000000000001,-0.900000000000001,
-0.895000000000001,-0.890000000000001,-0.885000000000001,-0.880000000000001,
-0.875000000000001,-0.870000000000001,-0.865000000000001,-0.860000000000001,
-0.855000000000001,-0.850000000000001,-0.845000000000001,-0.840000000000001,
-0.835000000000001,-0.830000000000001,-0.825000000000001,-0.820000000000001,
-0.815000000000001,-0.810000000000001,-0.805000000000001,-0.800000000000001,
-0.795000000000001,-0.790000000000001,-0.785000000000001,-0.780000000000001,
-0.775000000000001,-0.770000000000001,-0.765000000000001,-0.760000000000001,
-0.755000000000001,-0.750000000000001,-0.745000000000001,-0.740000000000001,
-0.735000000000001,-0.730000000000001,-0.725000000000001,-0.720000000000001,
-0.715000000000001,-0.710000000000001,-0.705000000000001,-0.700000000000001,
-0.695000000000001,-0.690000000000001,-0.685,-0.68,-0.675,-0.67,-0.665,
-0.66,-0.655,-0.65,-0.645,-0.64,-0.635,-0.63,-0.625,-0.62,-0.615,-0.61,
-0.605,-0.6,-0.595,-0.59,-0.585,-0.58,-0.575,-0.57,-0.565,-0.56,-0.555,
-0.55,-0.545,-0.54,-0.535,-0.53,-0.525,-0.52,-0.515,-0.51,-0.505,-0.5,-0.495,
-0.49,-0.485,-0.48,-0.475,-0.47,-0.465,-0.46,-0.455,-0.45,-0.445,-0.44,
-0.435,-0.43,-0.425,-0.42,-0.415,-0.41,-0.405,-0.4,-0.395,-0.39,-0.385,
-0.38,-0.375,-0.37,-0.365,-0.36,-0.355,-0.35,-0.345,-0.34,-0.335,-0.33,
-0.325,-0.32,-0.315,-0.31,-0.305,-0.3,-0.295,-0.29,-0.285,-0.28,-0.275,
-0.27,-0.265,-0.26,-0.255,-0.25,-0.245,-0.24,-0.235,-0.23,-0.225,-0.22,
-0.215,-0.21,-0.205,-0.2,-0.195,-0.19,-0.185,-0.18,-0.175,-0.17,-0.165,
-0.16,-0.155,-0.15,-0.145,-0.14,-0.135,-0.13,-0.125,-0.12,-0.115,-0.11,
-0.105,-0.1,-0.095,-0.09,-0.085,-0.08,-0.075,-0.07,-0.065,-0.06,-0.055,
-0.05,-0.045,-0.04,-0.035,-0.03,-0.025,-0.02,-0.015,-0.01,-0.005,0.),
 .UNSPECIFIED.)
CURVE()
GEOMETRIC_REPRESENTATION_ITEM()
RATIONAL_B_SPLINE_CURVE((1.,1.,1.,1.,1.,1.,1.,1.,1.,1.,1.,1.,1.,1.,1.,1.,
1.,1.,1.,1.,1.,1.,1.,1.,1.,1.,1.,1.,1.,1.,1.,1.,1.,1.,1.,1.,1.,1.,1.,1.,
1.,1.,1.,1.,1.,1.,1.,1.,1.,1.,1.,1.,1.,1.,1.,1.,1.,1.,1.,1.,1.,1.,1.,1.,
1.,1.,1.,1.,1.,1.,1.,1.,1.,1.,1.,1.,1.,1.,1.,1.,1.,1.,1.,1.,1.,1.,1.,1.,
1.,1.,1.,1.,1.,1.,1.,1.,1.,1.,1.,1.,1.,1.,1.,1.,1.,1.,1.,1.,1.,1.,1.,1.,
1.,1.,1.,1.,1.,1.,1.,1.,1.,1.,1.,1.,1.,1.,1.,1.,1.,1.,1.,1.,1.,1.,1.,1.,
1.,1.,1.,1.,1.,1.,1.,1.,1.,1.,1.,1.,1.,1.,1.,1.,1.,1.,1.,1.,1.,1.,1.,1.,
1.,1.,1.,1.,1.,1.,1.,1.,1.,1.,1.,1.,1.,1.,1.,1.,1.,1.,1.,1.,1.,1.,1.,1.,
1.,1.,1.,1.,1.,1.,1.,1.,1.,1.))
REPRESENTATION_ITEM('')
);
#657=(
BOUNDED_CURVE()
B_SPLINE_CURVE(5,(#161459,#161460,#161461,#161462,#161463,#161464,#161465,
#161466,#161467,#161468,#161469,#161470,#161471,#161472,#161473,#161474,
#161475,#161476,#161477,#161478,#161479,#161480,#161481,#161482,#161483,
#161484,#161485,#161486,#161487,#161488,#161489,#161490,#161491,#161492,
#161493,#161494,#161495,#161496,#161497,#161498,#161499,#161500,#161501,
#161502,#161503,#161504,#161505,#161506,#161507,#161508,#161509,#161510,
#161511,#161512,#161513,#161514,#161515,#161516,#161517,#161518,#161519,
#161520,#161521,#161522,#161523,#161524,#161525,#161526,#161527,#161528,
#161529,#161530,#161531,#161532,#161533,#161534,#161535,#161536,#161537,
#161538,#161539,#161540,#161541,#161542,#161543,#161544,#161545,#161546,
#161547,#161548,#161549,#161550,#161551,#161552,#161553,#161554,#161555,
#161556,#161557,#161558,#161559,#161560,#161561,#161562,#161563,#161564,
#161565,#161566,#161567,#161568,#161569,#161570,#161571,#161572,#161573,
#161574,#161575,#161576,#161577,#161578,#161579,#161580,#161581,#161582,
#161583,#161584,#161585,#161586,#161587,#161588,#161589,#161590,#161591,
#161592,#161593,#161594,#161595,#161596,#161597,#161598,#161599,#161600,
#161601,#161602,#161603,#161604,#161605,#161606,#161607,#161608,#161609,
#161610,#161611,#161612,#161613,#161614,#161615,#161616,#161617,#161618,
#161619,#161620,#161621,#161622,#161623,#161624,#161625,#161626,#161627,
#161628,#161629,#161630,#161631,#161632,#161633,#161634,#161635,#161636,
#161637,#161638,#161639,#161640,#161641,#161642,#161643,#161644,#161645,
#161646,#161647,#161648,#161649,#161650,#161651,#161652),.UNSPECIFIED.,
 .F.,.F.)
B_SPLINE_CURVE_WITH_KNOTS((6,1,1,1,1,1,1,1,1,1,1,1,1,1,1,1,1,1,1,1,1,1,
1,1,1,1,1,1,1,1,1,1,1,1,1,1,1,1,1,1,1,1,1,1,1,1,1,1,1,1,1,1,1,1,1,1,1,1,
1,1,1,1,1,1,1,1,1,1,1,1,1,1,1,1,1,1,1,1,1,1,1,1,1,1,1,1,1,1,1,1,1,1,1,1,
1,1,1,1,1,1,1,1,1,1,1,1,1,1,1,1,1,1,1,1,1,1,1,1,1,1,1,1,1,1,1,1,1,1,1,1,
1,1,1,1,1,1,1,1,1,1,1,1,1,1,1,1,1,1,1,1,1,1,1,1,1,1,1,1,1,1,1,1,1,1,1,1,
1,1,1,1,1,1,1,1,1,1,1,1,1,1,1,1,1,1,1,1,1,1,1,6),(0.,0.005,0.01,0.015,0.02,
0.025,0.03,0.035,0.04,0.045,0.05,0.055,0.06,0.065,0.07,0.075,0.08,0.085,
0.09,0.095,0.1,0.105,0.11,0.115,0.12,0.125,0.13,0.135,0.14,0.145,0.15,0.155,
0.16,0.165,0.17,0.175,0.18,0.185,0.19,0.195,0.2,0.205,0.21,0.215,0.22,0.225,
0.23,0.235,0.24,0.245,0.25,0.255,0.26,0.265,0.27,0.275,0.28,0.285,0.29,
0.295,0.3,0.305,0.31,0.315,0.32,0.325,0.33,0.335,0.34,0.345,0.35,0.355,
0.36,0.365,0.37,0.375,0.38,0.385,0.39,0.395,0.4,0.405,0.41,0.415,0.42,0.425,
0.43,0.435,0.44,0.445,0.45,0.455,0.46,0.465,0.47,0.475,0.48,0.485,0.49,
0.495,0.5,0.505,0.51,0.515,0.52,0.525,0.53,0.535,0.54,0.545,0.55,0.555,
0.56,0.565,0.57,0.575,0.58,0.585,0.59,0.595,0.6,0.605,0.61,0.615,0.62,0.625,
0.63,0.635,0.64,0.645,0.65,0.655,0.66,0.665,0.67,0.675,0.68,0.685,0.690000000000001,
0.695000000000001,0.700000000000001,0.705000000000001,0.710000000000001,
0.715000000000001,0.720000000000001,0.725000000000001,0.730000000000001,
0.735000000000001,0.740000000000001,0.745000000000001,0.750000000000001,
0.755000000000001,0.760000000000001,0.765000000000001,0.770000000000001,
0.775000000000001,0.780000000000001,0.785000000000001,0.790000000000001,
0.795000000000001,0.800000000000001,0.805000000000001,0.810000000000001,
0.815000000000001,0.820000000000001,0.825000000000001,0.830000000000001,
0.835000000000001,0.840000000000001,0.845000000000001,0.850000000000001,
0.855000000000001,0.860000000000001,0.865000000000001,0.870000000000001,
0.875000000000001,0.880000000000001,0.885000000000001,0.890000000000001,
0.895000000000001,0.900000000000001,0.905000000000001,0.910000000000001,
0.915000000000001,0.920000000000001,0.925000000000001,0.930000000000001,
0.935000000000001,0.940000000000001,0.941429844438118),.UNSPECIFIED.)
CURVE()
GEOMETRIC_REPRESENTATION_ITEM()
RATIONAL_B_SPLINE_CURVE((1.,1.,1.,1.,1.,1.,1.,1.,1.,1.,1.,1.,1.,1.,1.,1.,
1.,1.,1.,1.,1.,1.,1.,1.,1.,1.,1.,1.,1.,1.,1.,1.,1.,1.,1.,1.,1.,1.,1.,1.,
1.,1.,1.,1.,1.,1.,1.,1.,1.,1.,1.,1.,1.,1.,1.,1.,1.,1.,1.,1.,1.,1.,1.,1.,
1.,1.,1.,1.,1.,1.,1.,1.,1.,1.,1.,1.,1.,1.,1.,1.,1.,1.,1.,1.,1.,1.,1.,1.,
1.,1.,1.,1.,1.,1.,1.,1.,1.,1.,1.,1.,1.,1.,1.,1.,1.,1.,1.,1.,1.,1.,1.,1.,
1.,1.,1.,1.,1.,1.,1.,1.,1.,1.,1.,1.,1.,1.,1.,1.,1.,1.,1.,1.,1.,1.,1.,1.,
1.,1.,1.,1.,1.,1.,1.,1.,1.,1.,1.,1.,1.,1.,1.,1.,1.,1.,1.,1.,1.,1.,1.,1.,
1.,1.,1.,1.,1.,1.,1.,1.,1.,1.,1.,1.,1.,1.,1.,1.,1.,1.,1.,1.,1.,1.,1.,1.,
1.,1.,1.,1.,1.,1.,1.,1.,1.,1.))
REPRESENTATION_ITEM('')
);
#658=(
BOUNDED_CURVE()
B_SPLINE_CURVE(5,(#161655,#161656,#161657,#161658,#161659,#161660,#161661,
#161662,#161663,#161664,#161665,#161666,#161667,#161668,#161669,#161670,
#161671,#161672,#161673,#161674,#161675,#161676,#161677,#161678,#161679,
#161680,#161681,#161682,#161683,#161684,#161685,#161686,#161687,#161688,
#161689,#161690,#161691,#161692,#161693,#161694,#161695,#161696,#161697,
#161698,#161699,#161700,#161701,#161702,#161703,#161704,#161705,#161706,
#161707,#161708,#161709,#161710,#161711,#161712,#161713,#161714,#161715,
#161716,#161717,#161718,#161719,#161720,#161721,#161722,#161723,#161724,
#161725,#161726,#161727,#161728,#161729,#161730,#161731,#161732,#161733,
#161734,#161735,#161736,#161737,#161738,#161739,#161740,#161741,#161742,
#161743,#161744,#161745,#161746,#161747,#161748,#161749,#161750,#161751,
#161752,#161753,#161754,#161755,#161756,#161757,#161758,#161759,#161760,
#161761,#161762,#161763,#161764,#161765,#161766,#161767,#161768,#161769,
#161770,#161771,#161772,#161773,#161774,#161775,#161776,#161777,#161778,
#161779,#161780,#161781,#161782,#161783,#161784,#161785,#161786,#161787,
#161788,#161789,#161790,#161791,#161792,#161793,#161794,#161795,#161796,
#161797,#161798,#161799,#161800,#161801,#161802,#161803,#161804,#161805,
#161806,#161807,#161808,#161809,#161810,#161811,#161812,#161813,#161814,
#161815,#161816,#161817,#161818,#161819,#161820,#161821,#161822,#161823,
#161824,#161825,#161826,#161827,#161828,#161829,#161830,#161831,#161832,
#161833,#161834,#161835,#161836,#161837,#161838,#161839,#161840,#161841,
#161842,#161843,#161844,#161845,#161846,#161847,#161848),.UNSPECIFIED.,
 .F.,.F.)
B_SPLINE_CURVE_WITH_KNOTS((6,1,1,1,1,1,1,1,1,1,1,1,1,1,1,1,1,1,1,1,1,1,
1,1,1,1,1,1,1,1,1,1,1,1,1,1,1,1,1,1,1,1,1,1,1,1,1,1,1,1,1,1,1,1,1,1,1,1,
1,1,1,1,1,1,1,1,1,1,1,1,1,1,1,1,1,1,1,1,1,1,1,1,1,1,1,1,1,1,1,1,1,1,1,1,
1,1,1,1,1,1,1,1,1,1,1,1,1,1,1,1,1,1,1,1,1,1,1,1,1,1,1,1,1,1,1,1,1,1,1,1,
1,1,1,1,1,1,1,1,1,1,1,1,1,1,1,1,1,1,1,1,1,1,1,1,1,1,1,1,1,1,1,1,1,1,1,1,
1,1,1,1,1,1,1,1,1,1,1,1,1,1,1,1,1,1,1,1,1,1,1,6),(-0.941429844438121,-0.940000000000001,
-0.935000000000001,-0.930000000000001,-0.925000000000001,-0.920000000000001,
-0.915000000000001,-0.910000000000001,-0.905000000000001,-0.900000000000001,
-0.895000000000001,-0.890000000000001,-0.885000000000001,-0.880000000000001,
-0.875000000000001,-0.870000000000001,-0.865000000000001,-0.860000000000001,
-0.855000000000001,-0.850000000000001,-0.845000000000001,-0.840000000000001,
-0.835000000000001,-0.830000000000001,-0.825000000000001,-0.820000000000001,
-0.815000000000001,-0.810000000000001,-0.805000000000001,-0.800000000000001,
-0.795000000000001,-0.790000000000001,-0.785000000000001,-0.780000000000001,
-0.775000000000001,-0.770000000000001,-0.765000000000001,-0.760000000000001,
-0.755000000000001,-0.750000000000001,-0.745000000000001,-0.740000000000001,
-0.735000000000001,-0.730000000000001,-0.725000000000001,-0.720000000000001,
-0.715000000000001,-0.710000000000001,-0.705000000000001,-0.700000000000001,
-0.695000000000001,-0.690000000000001,-0.685,-0.68,-0.675,-0.67,-0.665,
-0.66,-0.655,-0.65,-0.645,-0.64,-0.635,-0.63,-0.625,-0.62,-0.615,-0.61,
-0.605,-0.6,-0.595,-0.59,-0.585,-0.58,-0.575,-0.57,-0.565,-0.56,-0.555,
-0.55,-0.545,-0.54,-0.535,-0.53,-0.525,-0.52,-0.515,-0.51,-0.505,-0.5,-0.495,
-0.49,-0.485,-0.48,-0.475,-0.47,-0.465,-0.46,-0.455,-0.45,-0.445,-0.44,
-0.435,-0.43,-0.425,-0.42,-0.415,-0.41,-0.405,-0.4,-0.395,-0.39,-0.385,
-0.38,-0.375,-0.37,-0.365,-0.36,-0.355,-0.35,-0.345,-0.34,-0.335,-0.33,
-0.325,-0.32,-0.315,-0.31,-0.305,-0.3,-0.295,-0.29,-0.285,-0.28,-0.275,
-0.27,-0.265,-0.26,-0.255,-0.25,-0.245,-0.24,-0.235,-0.23,-0.225,-0.22,
-0.215,-0.21,-0.205,-0.2,-0.195,-0.19,-0.185,-0.18,-0.175,-0.17,-0.165,
-0.16,-0.155,-0.15,-0.145,-0.14,-0.135,-0.13,-0.125,-0.12,-0.115,-0.11,
-0.105,-0.1,-0.095,-0.09,-0.085,-0.08,-0.075,-0.07,-0.065,-0.06,-0.055,
-0.05,-0.045,-0.04,-0.035,-0.03,-0.025,-0.02,-0.015,-0.01,-0.005,0.),
 .UNSPECIFIED.)
CURVE()
GEOMETRIC_REPRESENTATION_ITEM()
RATIONAL_B_SPLINE_CURVE((1.,1.,1.,1.,1.,1.,1.,1.,1.,1.,1.,1.,1.,1.,1.,1.,
1.,1.,1.,1.,1.,1.,1.,1.,1.,1.,1.,1.,1.,1.,1.,1.,1.,1.,1.,1.,1.,1.,1.,1.,
1.,1.,1.,1.,1.,1.,1.,1.,1.,1.,1.,1.,1.,1.,1.,1.,1.,1.,1.,1.,1.,1.,1.,1.,
1.,1.,1.,1.,1.,1.,1.,1.,1.,1.,1.,1.,1.,1.,1.,1.,1.,1.,1.,1.,1.,1.,1.,1.,
1.,1.,1.,1.,1.,1.,1.,1.,1.,1.,1.,1.,1.,1.,1.,1.,1.,1.,1.,1.,1.,1.,1.,1.,
1.,1.,1.,1.,1.,1.,1.,1.,1.,1.,1.,1.,1.,1.,1.,1.,1.,1.,1.,1.,1.,1.,1.,1.,
1.,1.,1.,1.,1.,1.,1.,1.,1.,1.,1.,1.,1.,1.,1.,1.,1.,1.,1.,1.,1.,1.,1.,1.,
1.,1.,1.,1.,1.,1.,1.,1.,1.,1.,1.,1.,1.,1.,1.,1.,1.,1.,1.,1.,1.,1.,1.,1.,
1.,1.,1.,1.,1.,1.,1.,1.,1.,1.))
REPRESENTATION_ITEM('')
);
#659=(
BOUNDED_CURVE()
B_SPLINE_CURVE(5,(#162260,#162261,#162262,#162263,#162264,#162265,#162266,
#162267,#162268,#162269,#162270,#162271,#162272,#162273,#162274,#162275,
#162276,#162277,#162278,#162279,#162280,#162281,#162282,#162283,#162284,
#162285,#162286,#162287,#162288,#162289,#162290,#162291,#162292,#162293,
#162294,#162295,#162296,#162297,#162298,#162299,#162300,#162301,#162302,
#162303,#162304,#162305,#162306,#162307,#162308,#162309,#162310,#162311,
#162312,#162313,#162314,#162315,#162316,#162317,#162318,#162319,#162320,
#162321,#162322,#162323,#162324,#162325,#162326,#162327,#162328,#162329,
#162330,#162331,#162332,#162333,#162334,#162335,#162336,#162337,#162338,
#162339,#162340,#162341,#162342,#162343,#162344,#162345,#162346,#162347,
#162348,#162349,#162350,#162351,#162352,#162353,#162354,#162355,#162356,
#162357,#162358,#162359,#162360,#162361,#162362,#162363,#162364,#162365,
#162366,#162367,#162368,#162369,#162370,#162371,#162372,#162373,#162374,
#162375,#162376,#162377,#162378,#162379,#162380,#162381,#162382,#162383,
#162384,#162385,#162386,#162387,#162388,#162389,#162390,#162391,#162392,
#162393,#162394,#162395,#162396,#162397,#162398,#162399,#162400,#162401,
#162402,#162403,#162404,#162405,#162406,#162407,#162408,#162409,#162410,
#162411,#162412,#162413,#162414,#162415,#162416,#162417,#162418,#162419,
#162420,#162421,#162422,#162423,#162424,#162425,#162426,#162427,#162428,
#162429,#162430,#162431,#162432,#162433,#162434,#162435,#162436,#162437,
#162438,#162439,#162440,#162441,#162442,#162443,#162444,#162445,#162446,
#162447,#162448,#162449,#162450,#162451,#162452,#162453),.UNSPECIFIED.,
 .F.,.F.)
B_SPLINE_CURVE_WITH_KNOTS((6,1,1,1,1,1,1,1,1,1,1,1,1,1,1,1,1,1,1,1,1,1,
1,1,1,1,1,1,1,1,1,1,1,1,1,1,1,1,1,1,1,1,1,1,1,1,1,1,1,1,1,1,1,1,1,1,1,1,
1,1,1,1,1,1,1,1,1,1,1,1,1,1,1,1,1,1,1,1,1,1,1,1,1,1,1,1,1,1,1,1,1,1,1,1,
1,1,1,1,1,1,1,1,1,1,1,1,1,1,1,1,1,1,1,1,1,1,1,1,1,1,1,1,1,1,1,1,1,1,1,1,
1,1,1,1,1,1,1,1,1,1,1,1,1,1,1,1,1,1,1,1,1,1,1,1,1,1,1,1,1,1,1,1,1,1,1,1,
1,1,1,1,1,1,1,1,1,1,1,1,1,1,1,1,1,1,1,1,1,1,1,6),(0.,0.005,0.01,0.015,0.02,
0.025,0.03,0.035,0.04,0.045,0.05,0.055,0.06,0.065,0.07,0.075,0.08,0.085,
0.09,0.095,0.1,0.105,0.11,0.115,0.12,0.125,0.13,0.135,0.14,0.145,0.15,0.155,
0.16,0.165,0.17,0.175,0.18,0.185,0.19,0.195,0.2,0.205,0.21,0.215,0.22,0.225,
0.23,0.235,0.24,0.245,0.25,0.255,0.26,0.265,0.27,0.275,0.28,0.285,0.29,
0.295,0.3,0.305,0.31,0.315,0.32,0.325,0.33,0.335,0.34,0.345,0.35,0.355,
0.36,0.365,0.37,0.375,0.38,0.385,0.39,0.395,0.4,0.405,0.41,0.415,0.42,0.425,
0.43,0.435,0.44,0.445,0.45,0.455,0.46,0.465,0.47,0.475,0.48,0.485,0.49,
0.495,0.5,0.505,0.51,0.515,0.52,0.525,0.53,0.535,0.54,0.545,0.55,0.555,
0.56,0.565,0.57,0.575,0.58,0.585,0.59,0.595,0.6,0.605,0.61,0.615,0.62,0.625,
0.63,0.635,0.64,0.645,0.65,0.655,0.66,0.665,0.67,0.675,0.68,0.685,0.690000000000001,
0.695000000000001,0.700000000000001,0.705000000000001,0.710000000000001,
0.715000000000001,0.720000000000001,0.725000000000001,0.730000000000001,
0.735000000000001,0.740000000000001,0.745000000000001,0.750000000000001,
0.755000000000001,0.760000000000001,0.765000000000001,0.770000000000001,
0.775000000000001,0.780000000000001,0.785000000000001,0.790000000000001,
0.795000000000001,0.800000000000001,0.805000000000001,0.810000000000001,
0.815000000000001,0.820000000000001,0.825000000000001,0.830000000000001,
0.835000000000001,0.840000000000001,0.845000000000001,0.850000000000001,
0.855000000000001,0.860000000000001,0.865000000000001,0.870000000000001,
0.875000000000001,0.880000000000001,0.885000000000001,0.890000000000001,
0.895000000000001,0.900000000000001,0.905000000000001,0.910000000000001,
0.915000000000001,0.920000000000001,0.925000000000001,0.930000000000001,
0.935000000000001,0.940000000000001,0.941429844438068),.UNSPECIFIED.)
CURVE()
GEOMETRIC_REPRESENTATION_ITEM()
RATIONAL_B_SPLINE_CURVE((1.,1.,1.,1.,1.,1.,1.,1.,1.,1.,1.,1.,1.,1.,1.,1.,
1.,1.,1.,1.,1.,1.,1.,1.,1.,1.,1.,1.,1.,1.,1.,1.,1.,1.,1.,1.,1.,1.,1.,1.,
1.,1.,1.,1.,1.,1.,1.,1.,1.,1.,1.,1.,1.,1.,1.,1.,1.,1.,1.,1.,1.,1.,1.,1.,
1.,1.,1.,1.,1.,1.,1.,1.,1.,1.,1.,1.,1.,1.,1.,1.,1.,1.,1.,1.,1.,1.,1.,1.,
1.,1.,1.,1.,1.,1.,1.,1.,1.,1.,1.,1.,1.,1.,1.,1.,1.,1.,1.,1.,1.,1.,1.,1.,
1.,1.,1.,1.,1.,1.,1.,1.,1.,1.,1.,1.,1.,1.,1.,1.,1.,1.,1.,1.,1.,1.,1.,1.,
1.,1.,1.,1.,1.,1.,1.,1.,1.,1.,1.,1.,1.,1.,1.,1.,1.,1.,1.,1.,1.,1.,1.,1.,
1.,1.,1.,1.,1.,1.,1.,1.,1.,1.,1.,1.,1.,1.,1.,1.,1.,1.,1.,1.,1.,1.,1.,1.,
1.,1.,1.,1.,1.,1.,1.,1.,1.,1.))
REPRESENTATION_ITEM('')
);
#660=(
BOUNDED_CURVE()
B_SPLINE_CURVE(5,(#162456,#162457,#162458,#162459,#162460,#162461,#162462,
#162463,#162464,#162465,#162466,#162467,#162468,#162469,#162470,#162471,
#162472,#162473,#162474,#162475,#162476,#162477,#162478,#162479,#162480,
#162481,#162482,#162483,#162484,#162485,#162486,#162487,#162488,#162489,
#162490,#162491,#162492,#162493,#162494,#162495,#162496,#162497,#162498,
#162499,#162500,#162501,#162502,#162503,#162504,#162505,#162506,#162507,
#162508,#162509,#162510,#162511,#162512,#162513,#162514,#162515,#162516,
#162517,#162518,#162519,#162520,#162521,#162522,#162523,#162524,#162525,
#162526,#162527,#162528,#162529,#162530,#162531,#162532,#162533,#162534,
#162535,#162536,#162537,#162538,#162539,#162540,#162541,#162542,#162543,
#162544,#162545,#162546,#162547,#162548,#162549,#162550,#162551,#162552,
#162553,#162554,#162555,#162556,#162557,#162558,#162559,#162560,#162561,
#162562,#162563,#162564,#162565,#162566,#162567,#162568,#162569,#162570,
#162571,#162572,#162573,#162574,#162575,#162576,#162577,#162578,#162579,
#162580,#162581,#162582,#162583,#162584,#162585,#162586,#162587,#162588,
#162589,#162590,#162591,#162592,#162593,#162594,#162595,#162596,#162597,
#162598,#162599,#162600,#162601,#162602,#162603,#162604,#162605,#162606,
#162607,#162608,#162609,#162610,#162611,#162612,#162613,#162614,#162615,
#162616,#162617,#162618,#162619,#162620,#162621,#162622,#162623,#162624,
#162625,#162626,#162627,#162628,#162629,#162630,#162631,#162632,#162633,
#162634,#162635,#162636,#162637,#162638,#162639,#162640,#162641,#162642,
#162643,#162644,#162645,#162646,#162647,#162648,#162649),.UNSPECIFIED.,
 .F.,.F.)
B_SPLINE_CURVE_WITH_KNOTS((6,1,1,1,1,1,1,1,1,1,1,1,1,1,1,1,1,1,1,1,1,1,
1,1,1,1,1,1,1,1,1,1,1,1,1,1,1,1,1,1,1,1,1,1,1,1,1,1,1,1,1,1,1,1,1,1,1,1,
1,1,1,1,1,1,1,1,1,1,1,1,1,1,1,1,1,1,1,1,1,1,1,1,1,1,1,1,1,1,1,1,1,1,1,1,
1,1,1,1,1,1,1,1,1,1,1,1,1,1,1,1,1,1,1,1,1,1,1,1,1,1,1,1,1,1,1,1,1,1,1,1,
1,1,1,1,1,1,1,1,1,1,1,1,1,1,1,1,1,1,1,1,1,1,1,1,1,1,1,1,1,1,1,1,1,1,1,1,
1,1,1,1,1,1,1,1,1,1,1,1,1,1,1,1,1,1,1,1,1,1,1,6),(-0.941429844438068,-0.940000000000001,
-0.935000000000001,-0.930000000000001,-0.925000000000001,-0.920000000000001,
-0.915000000000001,-0.910000000000001,-0.905000000000001,-0.900000000000001,
-0.895000000000001,-0.890000000000001,-0.885000000000001,-0.880000000000001,
-0.875000000000001,-0.870000000000001,-0.865000000000001,-0.860000000000001,
-0.855000000000001,-0.850000000000001,-0.845000000000001,-0.840000000000001,
-0.835000000000001,-0.830000000000001,-0.825000000000001,-0.820000000000001,
-0.815000000000001,-0.810000000000001,-0.805000000000001,-0.800000000000001,
-0.795000000000001,-0.790000000000001,-0.785000000000001,-0.780000000000001,
-0.775000000000001,-0.770000000000001,-0.765000000000001,-0.760000000000001,
-0.755000000000001,-0.750000000000001,-0.745000000000001,-0.740000000000001,
-0.735000000000001,-0.730000000000001,-0.725000000000001,-0.720000000000001,
-0.715000000000001,-0.710000000000001,-0.705000000000001,-0.700000000000001,
-0.695000000000001,-0.690000000000001,-0.685,-0.68,-0.675,-0.67,-0.665,
-0.66,-0.655,-0.65,-0.645,-0.64,-0.635,-0.63,-0.625,-0.62,-0.615,-0.61,
-0.605,-0.6,-0.595,-0.59,-0.585,-0.58,-0.575,-0.57,-0.565,-0.56,-0.555,
-0.55,-0.545,-0.54,-0.535,-0.53,-0.525,-0.52,-0.515,-0.51,-0.505,-0.5,-0.495,
-0.49,-0.485,-0.48,-0.475,-0.47,-0.465,-0.46,-0.455,-0.45,-0.445,-0.44,
-0.435,-0.43,-0.425,-0.42,-0.415,-0.41,-0.405,-0.4,-0.395,-0.39,-0.385,
-0.38,-0.375,-0.37,-0.365,-0.36,-0.355,-0.35,-0.345,-0.34,-0.335,-0.33,
-0.325,-0.32,-0.315,-0.31,-0.305,-0.3,-0.295,-0.29,-0.285,-0.28,-0.275,
-0.27,-0.265,-0.26,-0.255,-0.25,-0.245,-0.24,-0.235,-0.23,-0.225,-0.22,
-0.215,-0.21,-0.205,-0.2,-0.195,-0.19,-0.185,-0.18,-0.175,-0.17,-0.165,
-0.16,-0.155,-0.15,-0.145,-0.14,-0.135,-0.13,-0.125,-0.12,-0.115,-0.11,
-0.105,-0.1,-0.095,-0.09,-0.085,-0.08,-0.075,-0.07,-0.065,-0.06,-0.055,
-0.05,-0.045,-0.04,-0.035,-0.03,-0.025,-0.02,-0.015,-0.01,-0.005,0.),
 .UNSPECIFIED.)
CURVE()
GEOMETRIC_REPRESENTATION_ITEM()
RATIONAL_B_SPLINE_CURVE((1.,1.,1.,1.,1.,1.,1.,1.,1.,1.,1.,1.,1.,1.,1.,1.,
1.,1.,1.,1.,1.,1.,1.,1.,1.,1.,1.,1.,1.,1.,1.,1.,1.,1.,1.,1.,1.,1.,1.,1.,
1.,1.,1.,1.,1.,1.,1.,1.,1.,1.,1.,1.,1.,1.,1.,1.,1.,1.,1.,1.,1.,1.,1.,1.,
1.,1.,1.,1.,1.,1.,1.,1.,1.,1.,1.,1.,1.,1.,1.,1.,1.,1.,1.,1.,1.,1.,1.,1.,
1.,1.,1.,1.,1.,1.,1.,1.,1.,1.,1.,1.,1.,1.,1.,1.,1.,1.,1.,1.,1.,1.,1.,1.,
1.,1.,1.,1.,1.,1.,1.,1.,1.,1.,1.,1.,1.,1.,1.,1.,1.,1.,1.,1.,1.,1.,1.,1.,
1.,1.,1.,1.,1.,1.,1.,1.,1.,1.,1.,1.,1.,1.,1.,1.,1.,1.,1.,1.,1.,1.,1.,1.,
1.,1.,1.,1.,1.,1.,1.,1.,1.,1.,1.,1.,1.,1.,1.,1.,1.,1.,1.,1.,1.,1.,1.,1.,
1.,1.,1.,1.,1.,1.,1.,1.,1.,1.))
REPRESENTATION_ITEM('')
);
#661=(
BOUNDED_CURVE()
B_SPLINE_CURVE(5,(#163061,#163062,#163063,#163064,#163065,#163066,#163067,
#163068,#163069,#163070,#163071,#163072,#163073,#163074,#163075,#163076,
#163077,#163078,#163079,#163080,#163081,#163082,#163083,#163084,#163085,
#163086,#163087,#163088,#163089,#163090,#163091,#163092,#163093,#163094,
#163095,#163096,#163097,#163098,#163099,#163100,#163101,#163102,#163103,
#163104,#163105,#163106,#163107,#163108,#163109,#163110,#163111,#163112,
#163113,#163114,#163115,#163116,#163117,#163118,#163119,#163120,#163121,
#163122,#163123,#163124,#163125,#163126,#163127,#163128,#163129,#163130,
#163131,#163132,#163133,#163134,#163135,#163136,#163137,#163138,#163139,
#163140,#163141,#163142,#163143,#163144,#163145,#163146,#163147,#163148,
#163149,#163150,#163151,#163152,#163153,#163154,#163155,#163156,#163157,
#163158,#163159,#163160,#163161,#163162,#163163,#163164,#163165,#163166,
#163167,#163168,#163169,#163170,#163171,#163172,#163173,#163174,#163175,
#163176,#163177,#163178,#163179,#163180,#163181,#163182,#163183,#163184,
#163185,#163186,#163187,#163188,#163189,#163190,#163191,#163192,#163193,
#163194,#163195,#163196,#163197,#163198,#163199,#163200,#163201,#163202,
#163203,#163204,#163205,#163206,#163207,#163208,#163209,#163210,#163211,
#163212,#163213,#163214,#163215,#163216,#163217,#163218,#163219,#163220,
#163221,#163222,#163223,#163224,#163225,#163226,#163227,#163228,#163229,
#163230,#163231,#163232,#163233,#163234,#163235,#163236,#163237,#163238,
#163239,#163240,#163241,#163242,#163243,#163244,#163245,#163246,#163247,
#163248,#163249,#163250,#163251,#163252,#163253,#163254),.UNSPECIFIED.,
 .F.,.F.)
B_SPLINE_CURVE_WITH_KNOTS((6,1,1,1,1,1,1,1,1,1,1,1,1,1,1,1,1,1,1,1,1,1,
1,1,1,1,1,1,1,1,1,1,1,1,1,1,1,1,1,1,1,1,1,1,1,1,1,1,1,1,1,1,1,1,1,1,1,1,
1,1,1,1,1,1,1,1,1,1,1,1,1,1,1,1,1,1,1,1,1,1,1,1,1,1,1,1,1,1,1,1,1,1,1,1,
1,1,1,1,1,1,1,1,1,1,1,1,1,1,1,1,1,1,1,1,1,1,1,1,1,1,1,1,1,1,1,1,1,1,1,1,
1,1,1,1,1,1,1,1,1,1,1,1,1,1,1,1,1,1,1,1,1,1,1,1,1,1,1,1,1,1,1,1,1,1,1,1,
1,1,1,1,1,1,1,1,1,1,1,1,1,1,1,1,1,1,1,1,1,1,1,6),(0.,0.005,0.01,0.015,0.02,
0.025,0.03,0.035,0.04,0.045,0.05,0.055,0.06,0.065,0.07,0.075,0.08,0.085,
0.09,0.095,0.1,0.105,0.11,0.115,0.12,0.125,0.13,0.135,0.14,0.145,0.15,0.155,
0.16,0.165,0.17,0.175,0.18,0.185,0.19,0.195,0.2,0.205,0.21,0.215,0.22,0.225,
0.23,0.235,0.24,0.245,0.25,0.255,0.26,0.265,0.27,0.275,0.28,0.285,0.29,
0.295,0.3,0.305,0.31,0.315,0.32,0.325,0.33,0.335,0.34,0.345,0.35,0.355,
0.36,0.365,0.37,0.375,0.38,0.385,0.39,0.395,0.4,0.405,0.41,0.415,0.42,0.425,
0.43,0.435,0.44,0.445,0.45,0.455,0.46,0.465,0.47,0.475,0.48,0.485,0.49,
0.495,0.5,0.505,0.51,0.515,0.52,0.525,0.53,0.535,0.54,0.545,0.55,0.555,
0.56,0.565,0.57,0.575,0.58,0.585,0.59,0.595,0.6,0.605,0.61,0.615,0.62,0.625,
0.63,0.635,0.64,0.645,0.65,0.655,0.66,0.665,0.67,0.675,0.68,0.685,0.690000000000001,
0.695000000000001,0.700000000000001,0.705000000000001,0.710000000000001,
0.715000000000001,0.720000000000001,0.725000000000001,0.730000000000001,
0.735000000000001,0.740000000000001,0.745000000000001,0.750000000000001,
0.755000000000001,0.760000000000001,0.765000000000001,0.770000000000001,
0.775000000000001,0.780000000000001,0.785000000000001,0.790000000000001,
0.795000000000001,0.800000000000001,0.805000000000001,0.810000000000001,
0.815000000000001,0.820000000000001,0.825000000000001,0.830000000000001,
0.835000000000001,0.840000000000001,0.845000000000001,0.850000000000001,
0.855000000000001,0.860000000000001,0.865000000000001,0.870000000000001,
0.875000000000001,0.880000000000001,0.885000000000001,0.890000000000001,
0.895000000000001,0.900000000000001,0.905000000000001,0.910000000000001,
0.915000000000001,0.920000000000001,0.925000000000001,0.930000000000001,
0.935000000000001,0.940000000000001,0.941429844438002),.UNSPECIFIED.)
CURVE()
GEOMETRIC_REPRESENTATION_ITEM()
RATIONAL_B_SPLINE_CURVE((1.,1.,1.,1.,1.,1.,1.,1.,1.,1.,1.,1.,1.,1.,1.,1.,
1.,1.,1.,1.,1.,1.,1.,1.,1.,1.,1.,1.,1.,1.,1.,1.,1.,1.,1.,1.,1.,1.,1.,1.,
1.,1.,1.,1.,1.,1.,1.,1.,1.,1.,1.,1.,1.,1.,1.,1.,1.,1.,1.,1.,1.,1.,1.,1.,
1.,1.,1.,1.,1.,1.,1.,1.,1.,1.,1.,1.,1.,1.,1.,1.,1.,1.,1.,1.,1.,1.,1.,1.,
1.,1.,1.,1.,1.,1.,1.,1.,1.,1.,1.,1.,1.,1.,1.,1.,1.,1.,1.,1.,1.,1.,1.,1.,
1.,1.,1.,1.,1.,1.,1.,1.,1.,1.,1.,1.,1.,1.,1.,1.,1.,1.,1.,1.,1.,1.,1.,1.,
1.,1.,1.,1.,1.,1.,1.,1.,1.,1.,1.,1.,1.,1.,1.,1.,1.,1.,1.,1.,1.,1.,1.,1.,
1.,1.,1.,1.,1.,1.,1.,1.,1.,1.,1.,1.,1.,1.,1.,1.,1.,1.,1.,1.,1.,1.,1.,1.,
1.,1.,1.,1.,1.,1.,1.,1.,1.,1.))
REPRESENTATION_ITEM('')
);
#662=(
BOUNDED_CURVE()
B_SPLINE_CURVE(5,(#163257,#163258,#163259,#163260,#163261,#163262,#163263,
#163264,#163265,#163266,#163267,#163268,#163269,#163270,#163271,#163272,
#163273,#163274,#163275,#163276,#163277,#163278,#163279,#163280,#163281,
#163282,#163283,#163284,#163285,#163286,#163287,#163288,#163289,#163290,
#163291,#163292,#163293,#163294,#163295,#163296,#163297,#163298,#163299,
#163300,#163301,#163302,#163303,#163304,#163305,#163306,#163307,#163308,
#163309,#163310,#163311,#163312,#163313,#163314,#163315,#163316,#163317,
#163318,#163319,#163320,#163321,#163322,#163323,#163324,#163325,#163326,
#163327,#163328,#163329,#163330,#163331,#163332,#163333,#163334,#163335,
#163336,#163337,#163338,#163339,#163340,#163341,#163342,#163343,#163344,
#163345,#163346,#163347,#163348,#163349,#163350,#163351,#163352,#163353,
#163354,#163355,#163356,#163357,#163358,#163359,#163360,#163361,#163362,
#163363,#163364,#163365,#163366,#163367,#163368,#163369,#163370,#163371,
#163372,#163373,#163374,#163375,#163376,#163377,#163378,#163379,#163380,
#163381,#163382,#163383,#163384,#163385,#163386,#163387,#163388,#163389,
#163390,#163391,#163392,#163393,#163394,#163395,#163396,#163397,#163398,
#163399,#163400,#163401,#163402,#163403,#163404,#163405,#163406,#163407,
#163408,#163409,#163410,#163411,#163412,#163413,#163414,#163415,#163416,
#163417,#163418,#163419,#163420,#163421,#163422,#163423,#163424,#163425,
#163426,#163427,#163428,#163429,#163430,#163431,#163432,#163433,#163434,
#163435,#163436,#163437,#163438,#163439,#163440,#163441,#163442,#163443,
#163444,#163445,#163446,#163447,#163448,#163449,#163450),.UNSPECIFIED.,
 .F.,.F.)
B_SPLINE_CURVE_WITH_KNOTS((6,1,1,1,1,1,1,1,1,1,1,1,1,1,1,1,1,1,1,1,1,1,
1,1,1,1,1,1,1,1,1,1,1,1,1,1,1,1,1,1,1,1,1,1,1,1,1,1,1,1,1,1,1,1,1,1,1,1,
1,1,1,1,1,1,1,1,1,1,1,1,1,1,1,1,1,1,1,1,1,1,1,1,1,1,1,1,1,1,1,1,1,1,1,1,
1,1,1,1,1,1,1,1,1,1,1,1,1,1,1,1,1,1,1,1,1,1,1,1,1,1,1,1,1,1,1,1,1,1,1,1,
1,1,1,1,1,1,1,1,1,1,1,1,1,1,1,1,1,1,1,1,1,1,1,1,1,1,1,1,1,1,1,1,1,1,1,1,
1,1,1,1,1,1,1,1,1,1,1,1,1,1,1,1,1,1,1,1,1,1,1,6),(-0.941429844438003,-0.940000000000001,
-0.935000000000001,-0.930000000000001,-0.925000000000001,-0.920000000000001,
-0.915000000000001,-0.910000000000001,-0.905000000000001,-0.900000000000001,
-0.895000000000001,-0.890000000000001,-0.885000000000001,-0.880000000000001,
-0.875000000000001,-0.870000000000001,-0.865000000000001,-0.860000000000001,
-0.855000000000001,-0.850000000000001,-0.845000000000001,-0.840000000000001,
-0.835000000000001,-0.830000000000001,-0.825000000000001,-0.820000000000001,
-0.815000000000001,-0.810000000000001,-0.805000000000001,-0.800000000000001,
-0.795000000000001,-0.790000000000001,-0.785000000000001,-0.780000000000001,
-0.775000000000001,-0.770000000000001,-0.765000000000001,-0.760000000000001,
-0.755000000000001,-0.750000000000001,-0.745000000000001,-0.740000000000001,
-0.735000000000001,-0.730000000000001,-0.725000000000001,-0.720000000000001,
-0.715000000000001,-0.710000000000001,-0.705000000000001,-0.700000000000001,
-0.695000000000001,-0.690000000000001,-0.685,-0.68,-0.675,-0.67,-0.665,
-0.66,-0.655,-0.65,-0.645,-0.64,-0.635,-0.63,-0.625,-0.62,-0.615,-0.61,
-0.605,-0.6,-0.595,-0.59,-0.585,-0.58,-0.575,-0.57,-0.565,-0.56,-0.555,
-0.55,-0.545,-0.54,-0.535,-0.53,-0.525,-0.52,-0.515,-0.51,-0.505,-0.5,-0.495,
-0.49,-0.485,-0.48,-0.475,-0.47,-0.465,-0.46,-0.455,-0.45,-0.445,-0.44,
-0.435,-0.43,-0.425,-0.42,-0.415,-0.41,-0.405,-0.4,-0.395,-0.39,-0.385,
-0.38,-0.375,-0.37,-0.365,-0.36,-0.355,-0.35,-0.345,-0.34,-0.335,-0.33,
-0.325,-0.32,-0.315,-0.31,-0.305,-0.3,-0.295,-0.29,-0.285,-0.28,-0.275,
-0.27,-0.265,-0.26,-0.255,-0.25,-0.245,-0.24,-0.235,-0.23,-0.225,-0.22,
-0.215,-0.21,-0.205,-0.2,-0.195,-0.19,-0.185,-0.18,-0.175,-0.17,-0.165,
-0.16,-0.155,-0.15,-0.145,-0.14,-0.135,-0.13,-0.125,-0.12,-0.115,-0.11,
-0.105,-0.1,-0.095,-0.09,-0.085,-0.08,-0.075,-0.07,-0.065,-0.06,-0.055,
-0.05,-0.045,-0.04,-0.035,-0.03,-0.025,-0.02,-0.015,-0.01,-0.005,0.),
 .UNSPECIFIED.)
CURVE()
GEOMETRIC_REPRESENTATION_ITEM()
RATIONAL_B_SPLINE_CURVE((1.,1.,1.,1.,1.,1.,1.,1.,1.,1.,1.,1.,1.,1.,1.,1.,
1.,1.,1.,1.,1.,1.,1.,1.,1.,1.,1.,1.,1.,1.,1.,1.,1.,1.,1.,1.,1.,1.,1.,1.,
1.,1.,1.,1.,1.,1.,1.,1.,1.,1.,1.,1.,1.,1.,1.,1.,1.,1.,1.,1.,1.,1.,1.,1.,
1.,1.,1.,1.,1.,1.,1.,1.,1.,1.,1.,1.,1.,1.,1.,1.,1.,1.,1.,1.,1.,1.,1.,1.,
1.,1.,1.,1.,1.,1.,1.,1.,1.,1.,1.,1.,1.,1.,1.,1.,1.,1.,1.,1.,1.,1.,1.,1.,
1.,1.,1.,1.,1.,1.,1.,1.,1.,1.,1.,1.,1.,1.,1.,1.,1.,1.,1.,1.,1.,1.,1.,1.,
1.,1.,1.,1.,1.,1.,1.,1.,1.,1.,1.,1.,1.,1.,1.,1.,1.,1.,1.,1.,1.,1.,1.,1.,
1.,1.,1.,1.,1.,1.,1.,1.,1.,1.,1.,1.,1.,1.,1.,1.,1.,1.,1.,1.,1.,1.,1.,1.,
1.,1.,1.,1.,1.,1.,1.,1.,1.,1.))
REPRESENTATION_ITEM('')
);
#663=(
BOUNDED_CURVE()
B_SPLINE_CURVE(5,(#163862,#163863,#163864,#163865,#163866,#163867,#163868,
#163869,#163870,#163871,#163872,#163873,#163874,#163875,#163876,#163877,
#163878,#163879,#163880,#163881,#163882,#163883,#163884,#163885,#163886,
#163887,#163888,#163889,#163890,#163891,#163892,#163893,#163894,#163895,
#163896,#163897,#163898,#163899,#163900,#163901,#163902,#163903,#163904,
#163905,#163906,#163907,#163908,#163909,#163910,#163911,#163912,#163913,
#163914,#163915,#163916,#163917,#163918,#163919,#163920,#163921,#163922,
#163923,#163924,#163925,#163926,#163927,#163928,#163929,#163930,#163931,
#163932,#163933,#163934,#163935,#163936,#163937,#163938,#163939,#163940,
#163941,#163942,#163943,#163944,#163945,#163946,#163947,#163948,#163949,
#163950,#163951,#163952,#163953,#163954,#163955,#163956,#163957,#163958,
#163959,#163960,#163961,#163962,#163963,#163964,#163965,#163966,#163967,
#163968,#163969,#163970,#163971,#163972,#163973,#163974,#163975,#163976,
#163977,#163978,#163979,#163980,#163981,#163982,#163983,#163984,#163985,
#163986,#163987,#163988,#163989,#163990,#163991,#163992,#163993,#163994,
#163995,#163996,#163997,#163998,#163999,#164000,#164001,#164002,#164003,
#164004,#164005,#164006,#164007,#164008,#164009,#164010,#164011,#164012,
#164013,#164014,#164015,#164016,#164017,#164018,#164019,#164020,#164021,
#164022,#164023,#164024,#164025,#164026,#164027,#164028,#164029,#164030,
#164031,#164032,#164033,#164034,#164035,#164036,#164037,#164038,#164039,
#164040,#164041,#164042,#164043,#164044,#164045,#164046,#164047,#164048,
#164049,#164050,#164051,#164052,#164053,#164054,#164055),.UNSPECIFIED.,
 .F.,.F.)
B_SPLINE_CURVE_WITH_KNOTS((6,1,1,1,1,1,1,1,1,1,1,1,1,1,1,1,1,1,1,1,1,1,
1,1,1,1,1,1,1,1,1,1,1,1,1,1,1,1,1,1,1,1,1,1,1,1,1,1,1,1,1,1,1,1,1,1,1,1,
1,1,1,1,1,1,1,1,1,1,1,1,1,1,1,1,1,1,1,1,1,1,1,1,1,1,1,1,1,1,1,1,1,1,1,1,
1,1,1,1,1,1,1,1,1,1,1,1,1,1,1,1,1,1,1,1,1,1,1,1,1,1,1,1,1,1,1,1,1,1,1,1,
1,1,1,1,1,1,1,1,1,1,1,1,1,1,1,1,1,1,1,1,1,1,1,1,1,1,1,1,1,1,1,1,1,1,1,1,
1,1,1,1,1,1,1,1,1,1,1,1,1,1,1,1,1,1,1,1,1,1,1,6),(0.,0.005,0.01,0.015,0.02,
0.025,0.03,0.035,0.04,0.045,0.05,0.055,0.06,0.065,0.07,0.075,0.08,0.085,
0.09,0.095,0.1,0.105,0.11,0.115,0.12,0.125,0.13,0.135,0.14,0.145,0.15,0.155,
0.16,0.165,0.17,0.175,0.18,0.185,0.19,0.195,0.2,0.205,0.21,0.215,0.22,0.225,
0.23,0.235,0.24,0.245,0.25,0.255,0.26,0.265,0.27,0.275,0.28,0.285,0.29,
0.295,0.3,0.305,0.31,0.315,0.32,0.325,0.33,0.335,0.34,0.345,0.35,0.355,
0.36,0.365,0.37,0.375,0.38,0.385,0.39,0.395,0.4,0.405,0.41,0.415,0.42,0.425,
0.43,0.435,0.44,0.445,0.45,0.455,0.46,0.465,0.47,0.475,0.48,0.485,0.49,
0.495,0.5,0.505,0.51,0.515,0.52,0.525,0.53,0.535,0.54,0.545,0.55,0.555,
0.56,0.565,0.57,0.575,0.58,0.585,0.59,0.595,0.6,0.605,0.61,0.615,0.62,0.625,
0.63,0.635,0.64,0.645,0.65,0.655,0.66,0.665,0.67,0.675,0.68,0.685,0.690000000000001,
0.695000000000001,0.700000000000001,0.705000000000001,0.710000000000001,
0.715000000000001,0.720000000000001,0.725000000000001,0.730000000000001,
0.735000000000001,0.740000000000001,0.745000000000001,0.750000000000001,
0.755000000000001,0.760000000000001,0.765000000000001,0.770000000000001,
0.775000000000001,0.780000000000001,0.785000000000001,0.790000000000001,
0.795000000000001,0.800000000000001,0.805000000000001,0.810000000000001,
0.815000000000001,0.820000000000001,0.825000000000001,0.830000000000001,
0.835000000000001,0.840000000000001,0.845000000000001,0.850000000000001,
0.855000000000001,0.860000000000001,0.865000000000001,0.870000000000001,
0.875000000000001,0.880000000000001,0.885000000000001,0.890000000000001,
0.895000000000001,0.900000000000001,0.905000000000001,0.910000000000001,
0.915000000000001,0.920000000000001,0.925000000000001,0.930000000000001,
0.935000000000001,0.940000000000001,0.941429844437967),.UNSPECIFIED.)
CURVE()
GEOMETRIC_REPRESENTATION_ITEM()
RATIONAL_B_SPLINE_CURVE((1.,1.,1.,1.,1.,1.,1.,1.,1.,1.,1.,1.,1.,1.,1.,1.,
1.,1.,1.,1.,1.,1.,1.,1.,1.,1.,1.,1.,1.,1.,1.,1.,1.,1.,1.,1.,1.,1.,1.,1.,
1.,1.,1.,1.,1.,1.,1.,1.,1.,1.,1.,1.,1.,1.,1.,1.,1.,1.,1.,1.,1.,1.,1.,1.,
1.,1.,1.,1.,1.,1.,1.,1.,1.,1.,1.,1.,1.,1.,1.,1.,1.,1.,1.,1.,1.,1.,1.,1.,
1.,1.,1.,1.,1.,1.,1.,1.,1.,1.,1.,1.,1.,1.,1.,1.,1.,1.,1.,1.,1.,1.,1.,1.,
1.,1.,1.,1.,1.,1.,1.,1.,1.,1.,1.,1.,1.,1.,1.,1.,1.,1.,1.,1.,1.,1.,1.,1.,
1.,1.,1.,1.,1.,1.,1.,1.,1.,1.,1.,1.,1.,1.,1.,1.,1.,1.,1.,1.,1.,1.,1.,1.,
1.,1.,1.,1.,1.,1.,1.,1.,1.,1.,1.,1.,1.,1.,1.,1.,1.,1.,1.,1.,1.,1.,1.,1.,
1.,1.,1.,1.,1.,1.,1.,1.,1.,1.))
REPRESENTATION_ITEM('')
);
#664=(
BOUNDED_CURVE()
B_SPLINE_CURVE(5,(#164058,#164059,#164060,#164061,#164062,#164063,#164064,
#164065,#164066,#164067,#164068,#164069,#164070,#164071,#164072,#164073,
#164074,#164075,#164076,#164077,#164078,#164079,#164080,#164081,#164082,
#164083,#164084,#164085,#164086,#164087,#164088,#164089,#164090,#164091,
#164092,#164093,#164094,#164095,#164096,#164097,#164098,#164099,#164100,
#164101,#164102,#164103,#164104,#164105,#164106,#164107,#164108,#164109,
#164110,#164111,#164112,#164113,#164114,#164115,#164116,#164117,#164118,
#164119,#164120,#164121,#164122,#164123,#164124,#164125,#164126,#164127,
#164128,#164129,#164130,#164131,#164132,#164133,#164134,#164135,#164136,
#164137,#164138,#164139,#164140,#164141,#164142,#164143,#164144,#164145,
#164146,#164147,#164148,#164149,#164150,#164151,#164152,#164153,#164154,
#164155,#164156,#164157,#164158,#164159,#164160,#164161,#164162,#164163,
#164164,#164165,#164166,#164167,#164168,#164169,#164170,#164171,#164172,
#164173,#164174,#164175,#164176,#164177,#164178,#164179,#164180,#164181,
#164182,#164183,#164184,#164185,#164186,#164187,#164188,#164189,#164190,
#164191,#164192,#164193,#164194,#164195,#164196,#164197,#164198,#164199,
#164200,#164201,#164202,#164203,#164204,#164205,#164206,#164207,#164208,
#164209,#164210,#164211,#164212,#164213,#164214,#164215,#164216,#164217,
#164218,#164219,#164220,#164221,#164222,#164223,#164224,#164225,#164226,
#164227,#164228,#164229,#164230,#164231,#164232,#164233,#164234,#164235,
#164236,#164237,#164238,#164239,#164240,#164241,#164242,#164243,#164244,
#164245,#164246,#164247,#164248,#164249,#164250,#164251),.UNSPECIFIED.,
 .F.,.F.)
B_SPLINE_CURVE_WITH_KNOTS((6,1,1,1,1,1,1,1,1,1,1,1,1,1,1,1,1,1,1,1,1,1,
1,1,1,1,1,1,1,1,1,1,1,1,1,1,1,1,1,1,1,1,1,1,1,1,1,1,1,1,1,1,1,1,1,1,1,1,
1,1,1,1,1,1,1,1,1,1,1,1,1,1,1,1,1,1,1,1,1,1,1,1,1,1,1,1,1,1,1,1,1,1,1,1,
1,1,1,1,1,1,1,1,1,1,1,1,1,1,1,1,1,1,1,1,1,1,1,1,1,1,1,1,1,1,1,1,1,1,1,1,
1,1,1,1,1,1,1,1,1,1,1,1,1,1,1,1,1,1,1,1,1,1,1,1,1,1,1,1,1,1,1,1,1,1,1,1,
1,1,1,1,1,1,1,1,1,1,1,1,1,1,1,1,1,1,1,1,1,1,1,6),(-0.941429844437967,-0.940000000000001,
-0.935000000000001,-0.930000000000001,-0.925000000000001,-0.920000000000001,
-0.915000000000001,-0.910000000000001,-0.905000000000001,-0.900000000000001,
-0.895000000000001,-0.890000000000001,-0.885000000000001,-0.880000000000001,
-0.875000000000001,-0.870000000000001,-0.865000000000001,-0.860000000000001,
-0.855000000000001,-0.850000000000001,-0.845000000000001,-0.840000000000001,
-0.835000000000001,-0.830000000000001,-0.825000000000001,-0.820000000000001,
-0.815000000000001,-0.810000000000001,-0.805000000000001,-0.800000000000001,
-0.795000000000001,-0.790000000000001,-0.785000000000001,-0.780000000000001,
-0.775000000000001,-0.770000000000001,-0.765000000000001,-0.760000000000001,
-0.755000000000001,-0.750000000000001,-0.745000000000001,-0.740000000000001,
-0.735000000000001,-0.730000000000001,-0.725000000000001,-0.720000000000001,
-0.715000000000001,-0.710000000000001,-0.705000000000001,-0.700000000000001,
-0.695000000000001,-0.690000000000001,-0.685,-0.68,-0.675,-0.67,-0.665,
-0.66,-0.655,-0.65,-0.645,-0.64,-0.635,-0.63,-0.625,-0.62,-0.615,-0.61,
-0.605,-0.6,-0.595,-0.59,-0.585,-0.58,-0.575,-0.57,-0.565,-0.56,-0.555,
-0.55,-0.545,-0.54,-0.535,-0.53,-0.525,-0.52,-0.515,-0.51,-0.505,-0.5,-0.495,
-0.49,-0.485,-0.48,-0.475,-0.47,-0.465,-0.46,-0.455,-0.45,-0.445,-0.44,
-0.435,-0.43,-0.425,-0.42,-0.415,-0.41,-0.405,-0.4,-0.395,-0.39,-0.385,
-0.38,-0.375,-0.37,-0.365,-0.36,-0.355,-0.35,-0.345,-0.34,-0.335,-0.33,
-0.325,-0.32,-0.315,-0.31,-0.305,-0.3,-0.295,-0.29,-0.285,-0.28,-0.275,
-0.27,-0.265,-0.26,-0.255,-0.25,-0.245,-0.24,-0.235,-0.23,-0.225,-0.22,
-0.215,-0.21,-0.205,-0.2,-0.195,-0.19,-0.185,-0.18,-0.175,-0.17,-0.165,
-0.16,-0.155,-0.15,-0.145,-0.14,-0.135,-0.13,-0.125,-0.12,-0.115,-0.11,
-0.105,-0.1,-0.095,-0.09,-0.085,-0.08,-0.075,-0.07,-0.065,-0.06,-0.055,
-0.05,-0.045,-0.04,-0.035,-0.03,-0.025,-0.02,-0.015,-0.01,-0.005,0.),
 .UNSPECIFIED.)
CURVE()
GEOMETRIC_REPRESENTATION_ITEM()
RATIONAL_B_SPLINE_CURVE((1.,1.,1.,1.,1.,1.,1.,1.,1.,1.,1.,1.,1.,1.,1.,1.,
1.,1.,1.,1.,1.,1.,1.,1.,1.,1.,1.,1.,1.,1.,1.,1.,1.,1.,1.,1.,1.,1.,1.,1.,
1.,1.,1.,1.,1.,1.,1.,1.,1.,1.,1.,1.,1.,1.,1.,1.,1.,1.,1.,1.,1.,1.,1.,1.,
1.,1.,1.,1.,1.,1.,1.,1.,1.,1.,1.,1.,1.,1.,1.,1.,1.,1.,1.,1.,1.,1.,1.,1.,
1.,1.,1.,1.,1.,1.,1.,1.,1.,1.,1.,1.,1.,1.,1.,1.,1.,1.,1.,1.,1.,1.,1.,1.,
1.,1.,1.,1.,1.,1.,1.,1.,1.,1.,1.,1.,1.,1.,1.,1.,1.,1.,1.,1.,1.,1.,1.,1.,
1.,1.,1.,1.,1.,1.,1.,1.,1.,1.,1.,1.,1.,1.,1.,1.,1.,1.,1.,1.,1.,1.,1.,1.,
1.,1.,1.,1.,1.,1.,1.,1.,1.,1.,1.,1.,1.,1.,1.,1.,1.,1.,1.,1.,1.,1.,1.,1.,
1.,1.,1.,1.,1.,1.,1.,1.,1.,1.))
REPRESENTATION_ITEM('')
);
#665=(
BOUNDED_CURVE()
B_SPLINE_CURVE(5,(#164663,#164664,#164665,#164666,#164667,#164668,#164669,
#164670,#164671,#164672,#164673,#164674,#164675,#164676,#164677,#164678,
#164679,#164680,#164681,#164682,#164683,#164684,#164685,#164686,#164687,
#164688,#164689,#164690,#164691,#164692,#164693,#164694,#164695,#164696,
#164697,#164698,#164699,#164700,#164701,#164702,#164703,#164704,#164705,
#164706,#164707,#164708,#164709,#164710,#164711,#164712,#164713,#164714,
#164715,#164716,#164717,#164718,#164719,#164720,#164721,#164722,#164723,
#164724,#164725,#164726,#164727,#164728,#164729,#164730,#164731,#164732,
#164733,#164734,#164735,#164736,#164737,#164738,#164739,#164740,#164741,
#164742,#164743,#164744,#164745,#164746,#164747,#164748,#164749,#164750,
#164751,#164752,#164753,#164754,#164755,#164756,#164757,#164758,#164759,
#164760,#164761,#164762,#164763,#164764,#164765,#164766,#164767,#164768,
#164769,#164770,#164771,#164772,#164773,#164774,#164775,#164776,#164777,
#164778,#164779,#164780,#164781,#164782,#164783,#164784,#164785,#164786,
#164787,#164788,#164789,#164790,#164791,#164792,#164793,#164794,#164795,
#164796,#164797,#164798,#164799,#164800,#164801,#164802,#164803,#164804,
#164805,#164806,#164807,#164808,#164809,#164810,#164811,#164812,#164813,
#164814,#164815,#164816,#164817,#164818,#164819,#164820,#164821,#164822,
#164823,#164824,#164825,#164826,#164827,#164828,#164829,#164830,#164831,
#164832,#164833,#164834,#164835,#164836,#164837,#164838,#164839,#164840,
#164841,#164842,#164843,#164844,#164845,#164846,#164847,#164848,#164849,
#164850,#164851,#164852,#164853,#164854,#164855,#164856),.UNSPECIFIED.,
 .F.,.F.)
B_SPLINE_CURVE_WITH_KNOTS((6,1,1,1,1,1,1,1,1,1,1,1,1,1,1,1,1,1,1,1,1,1,
1,1,1,1,1,1,1,1,1,1,1,1,1,1,1,1,1,1,1,1,1,1,1,1,1,1,1,1,1,1,1,1,1,1,1,1,
1,1,1,1,1,1,1,1,1,1,1,1,1,1,1,1,1,1,1,1,1,1,1,1,1,1,1,1,1,1,1,1,1,1,1,1,
1,1,1,1,1,1,1,1,1,1,1,1,1,1,1,1,1,1,1,1,1,1,1,1,1,1,1,1,1,1,1,1,1,1,1,1,
1,1,1,1,1,1,1,1,1,1,1,1,1,1,1,1,1,1,1,1,1,1,1,1,1,1,1,1,1,1,1,1,1,1,1,1,
1,1,1,1,1,1,1,1,1,1,1,1,1,1,1,1,1,1,1,1,1,1,1,6),(0.,0.005,0.01,0.015,0.02,
0.025,0.03,0.035,0.04,0.045,0.05,0.055,0.06,0.065,0.07,0.075,0.08,0.085,
0.09,0.095,0.1,0.105,0.11,0.115,0.12,0.125,0.13,0.135,0.14,0.145,0.15,0.155,
0.16,0.165,0.17,0.175,0.18,0.185,0.19,0.195,0.2,0.205,0.21,0.215,0.22,0.225,
0.23,0.235,0.24,0.245,0.25,0.255,0.26,0.265,0.27,0.275,0.28,0.285,0.29,
0.295,0.3,0.305,0.31,0.315,0.32,0.325,0.33,0.335,0.34,0.345,0.35,0.355,
0.36,0.365,0.37,0.375,0.38,0.385,0.39,0.395,0.4,0.405,0.41,0.415,0.42,0.425,
0.43,0.435,0.44,0.445,0.45,0.455,0.46,0.465,0.47,0.475,0.48,0.485,0.49,
0.495,0.5,0.505,0.51,0.515,0.52,0.525,0.53,0.535,0.54,0.545,0.55,0.555,
0.56,0.565,0.57,0.575,0.58,0.585,0.59,0.595,0.6,0.605,0.61,0.615,0.62,0.625,
0.63,0.635,0.64,0.645,0.65,0.655,0.66,0.665,0.67,0.675,0.68,0.685,0.690000000000001,
0.695000000000001,0.700000000000001,0.705000000000001,0.710000000000001,
0.715000000000001,0.720000000000001,0.725000000000001,0.730000000000001,
0.735000000000001,0.740000000000001,0.745000000000001,0.750000000000001,
0.755000000000001,0.760000000000001,0.765000000000001,0.770000000000001,
0.775000000000001,0.780000000000001,0.785000000000001,0.790000000000001,
0.795000000000001,0.800000000000001,0.805000000000001,0.810000000000001,
0.815000000000001,0.820000000000001,0.825000000000001,0.830000000000001,
0.835000000000001,0.840000000000001,0.845000000000001,0.850000000000001,
0.855000000000001,0.860000000000001,0.865000000000001,0.870000000000001,
0.875000000000001,0.880000000000001,0.885000000000001,0.890000000000001,
0.895000000000001,0.900000000000001,0.905000000000001,0.910000000000001,
0.915000000000001,0.920000000000001,0.925000000000001,0.930000000000001,
0.935000000000001,0.940000000000001,0.941429844438043),.UNSPECIFIED.)
CURVE()
GEOMETRIC_REPRESENTATION_ITEM()
RATIONAL_B_SPLINE_CURVE((1.,1.,1.,1.,1.,1.,1.,1.,1.,1.,1.,1.,1.,1.,1.,1.,
1.,1.,1.,1.,1.,1.,1.,1.,1.,1.,1.,1.,1.,1.,1.,1.,1.,1.,1.,1.,1.,1.,1.,1.,
1.,1.,1.,1.,1.,1.,1.,1.,1.,1.,1.,1.,1.,1.,1.,1.,1.,1.,1.,1.,1.,1.,1.,1.,
1.,1.,1.,1.,1.,1.,1.,1.,1.,1.,1.,1.,1.,1.,1.,1.,1.,1.,1.,1.,1.,1.,1.,1.,
1.,1.,1.,1.,1.,1.,1.,1.,1.,1.,1.,1.,1.,1.,1.,1.,1.,1.,1.,1.,1.,1.,1.,1.,
1.,1.,1.,1.,1.,1.,1.,1.,1.,1.,1.,1.,1.,1.,1.,1.,1.,1.,1.,1.,1.,1.,1.,1.,
1.,1.,1.,1.,1.,1.,1.,1.,1.,1.,1.,1.,1.,1.,1.,1.,1.,1.,1.,1.,1.,1.,1.,1.,
1.,1.,1.,1.,1.,1.,1.,1.,1.,1.,1.,1.,1.,1.,1.,1.,1.,1.,1.,1.,1.,1.,1.,1.,
1.,1.,1.,1.,1.,1.,1.,1.,1.,1.))
REPRESENTATION_ITEM('')
);
#666=(
BOUNDED_CURVE()
B_SPLINE_CURVE(5,(#164859,#164860,#164861,#164862,#164863,#164864,#164865,
#164866,#164867,#164868,#164869,#164870,#164871,#164872,#164873,#164874,
#164875,#164876,#164877,#164878,#164879,#164880,#164881,#164882,#164883,
#164884,#164885,#164886,#164887,#164888,#164889,#164890,#164891,#164892,
#164893,#164894,#164895,#164896,#164897,#164898,#164899,#164900,#164901,
#164902,#164903,#164904,#164905,#164906,#164907,#164908,#164909,#164910,
#164911,#164912,#164913,#164914,#164915,#164916,#164917,#164918,#164919,
#164920,#164921,#164922,#164923,#164924,#164925,#164926,#164927,#164928,
#164929,#164930,#164931,#164932,#164933,#164934,#164935,#164936,#164937,
#164938,#164939,#164940,#164941,#164942,#164943,#164944,#164945,#164946,
#164947,#164948,#164949,#164950,#164951,#164952,#164953,#164954,#164955,
#164956,#164957,#164958,#164959,#164960,#164961,#164962,#164963,#164964,
#164965,#164966,#164967,#164968,#164969,#164970,#164971,#164972,#164973,
#164974,#164975,#164976,#164977,#164978,#164979,#164980,#164981,#164982,
#164983,#164984,#164985,#164986,#164987,#164988,#164989,#164990,#164991,
#164992,#164993,#164994,#164995,#164996,#164997,#164998,#164999,#165000,
#165001,#165002,#165003,#165004,#165005,#165006,#165007,#165008,#165009,
#165010,#165011,#165012,#165013,#165014,#165015,#165016,#165017,#165018,
#165019,#165020,#165021,#165022,#165023,#165024,#165025,#165026,#165027,
#165028,#165029,#165030,#165031,#165032,#165033,#165034,#165035,#165036,
#165037,#165038,#165039,#165040,#165041,#165042,#165043,#165044,#165045,
#165046,#165047,#165048,#165049,#165050,#165051,#165052),.UNSPECIFIED.,
 .F.,.F.)
B_SPLINE_CURVE_WITH_KNOTS((6,1,1,1,1,1,1,1,1,1,1,1,1,1,1,1,1,1,1,1,1,1,
1,1,1,1,1,1,1,1,1,1,1,1,1,1,1,1,1,1,1,1,1,1,1,1,1,1,1,1,1,1,1,1,1,1,1,1,
1,1,1,1,1,1,1,1,1,1,1,1,1,1,1,1,1,1,1,1,1,1,1,1,1,1,1,1,1,1,1,1,1,1,1,1,
1,1,1,1,1,1,1,1,1,1,1,1,1,1,1,1,1,1,1,1,1,1,1,1,1,1,1,1,1,1,1,1,1,1,1,1,
1,1,1,1,1,1,1,1,1,1,1,1,1,1,1,1,1,1,1,1,1,1,1,1,1,1,1,1,1,1,1,1,1,1,1,1,
1,1,1,1,1,1,1,1,1,1,1,1,1,1,1,1,1,1,1,1,1,1,1,6),(-0.941429844438042,-0.940000000000001,
-0.935000000000001,-0.930000000000001,-0.925000000000001,-0.920000000000001,
-0.915000000000001,-0.910000000000001,-0.905000000000001,-0.900000000000001,
-0.895000000000001,-0.890000000000001,-0.885000000000001,-0.880000000000001,
-0.875000000000001,-0.870000000000001,-0.865000000000001,-0.860000000000001,
-0.855000000000001,-0.850000000000001,-0.845000000000001,-0.840000000000001,
-0.835000000000001,-0.830000000000001,-0.825000000000001,-0.820000000000001,
-0.815000000000001,-0.810000000000001,-0.805000000000001,-0.800000000000001,
-0.795000000000001,-0.790000000000001,-0.785000000000001,-0.780000000000001,
-0.775000000000001,-0.770000000000001,-0.765000000000001,-0.760000000000001,
-0.755000000000001,-0.750000000000001,-0.745000000000001,-0.740000000000001,
-0.735000000000001,-0.730000000000001,-0.725000000000001,-0.720000000000001,
-0.715000000000001,-0.710000000000001,-0.705000000000001,-0.700000000000001,
-0.695000000000001,-0.690000000000001,-0.685,-0.68,-0.675,-0.67,-0.665,
-0.66,-0.655,-0.65,-0.645,-0.64,-0.635,-0.63,-0.625,-0.62,-0.615,-0.61,
-0.605,-0.6,-0.595,-0.59,-0.585,-0.58,-0.575,-0.57,-0.565,-0.56,-0.555,
-0.55,-0.545,-0.54,-0.535,-0.53,-0.525,-0.52,-0.515,-0.51,-0.505,-0.5,-0.495,
-0.49,-0.485,-0.48,-0.475,-0.47,-0.465,-0.46,-0.455,-0.45,-0.445,-0.44,
-0.435,-0.43,-0.425,-0.42,-0.415,-0.41,-0.405,-0.4,-0.395,-0.39,-0.385,
-0.38,-0.375,-0.37,-0.365,-0.36,-0.355,-0.35,-0.345,-0.34,-0.335,-0.33,
-0.325,-0.32,-0.315,-0.31,-0.305,-0.3,-0.295,-0.29,-0.285,-0.28,-0.275,
-0.27,-0.265,-0.26,-0.255,-0.25,-0.245,-0.24,-0.235,-0.23,-0.225,-0.22,
-0.215,-0.21,-0.205,-0.2,-0.195,-0.19,-0.185,-0.18,-0.175,-0.17,-0.165,
-0.16,-0.155,-0.15,-0.145,-0.14,-0.135,-0.13,-0.125,-0.12,-0.115,-0.11,
-0.105,-0.1,-0.095,-0.09,-0.085,-0.08,-0.075,-0.07,-0.065,-0.06,-0.055,
-0.05,-0.045,-0.04,-0.035,-0.03,-0.025,-0.02,-0.015,-0.01,-0.005,0.),
 .UNSPECIFIED.)
CURVE()
GEOMETRIC_REPRESENTATION_ITEM()
RATIONAL_B_SPLINE_CURVE((1.,1.,1.,1.,1.,1.,1.,1.,1.,1.,1.,1.,1.,1.,1.,1.,
1.,1.,1.,1.,1.,1.,1.,1.,1.,1.,1.,1.,1.,1.,1.,1.,1.,1.,1.,1.,1.,1.,1.,1.,
1.,1.,1.,1.,1.,1.,1.,1.,1.,1.,1.,1.,1.,1.,1.,1.,1.,1.,1.,1.,1.,1.,1.,1.,
1.,1.,1.,1.,1.,1.,1.,1.,1.,1.,1.,1.,1.,1.,1.,1.,1.,1.,1.,1.,1.,1.,1.,1.,
1.,1.,1.,1.,1.,1.,1.,1.,1.,1.,1.,1.,1.,1.,1.,1.,1.,1.,1.,1.,1.,1.,1.,1.,
1.,1.,1.,1.,1.,1.,1.,1.,1.,1.,1.,1.,1.,1.,1.,1.,1.,1.,1.,1.,1.,1.,1.,1.,
1.,1.,1.,1.,1.,1.,1.,1.,1.,1.,1.,1.,1.,1.,1.,1.,1.,1.,1.,1.,1.,1.,1.,1.,
1.,1.,1.,1.,1.,1.,1.,1.,1.,1.,1.,1.,1.,1.,1.,1.,1.,1.,1.,1.,1.,1.,1.,1.,
1.,1.,1.,1.,1.,1.,1.,1.,1.,1.))
REPRESENTATION_ITEM('')
);
#667=(
BOUNDED_CURVE()
B_SPLINE_CURVE(5,(#165464,#165465,#165466,#165467,#165468,#165469,#165470,
#165471,#165472,#165473,#165474,#165475,#165476,#165477,#165478,#165479,
#165480,#165481,#165482,#165483,#165484,#165485,#165486,#165487,#165488,
#165489,#165490,#165491,#165492,#165493,#165494,#165495,#165496,#165497,
#165498,#165499,#165500,#165501,#165502,#165503,#165504,#165505,#165506,
#165507,#165508,#165509,#165510,#165511,#165512,#165513,#165514,#165515,
#165516,#165517,#165518,#165519,#165520,#165521,#165522,#165523,#165524,
#165525,#165526,#165527,#165528,#165529,#165530,#165531,#165532,#165533,
#165534,#165535,#165536,#165537,#165538,#165539,#165540,#165541,#165542,
#165543,#165544,#165545,#165546,#165547,#165548,#165549,#165550,#165551,
#165552,#165553,#165554,#165555,#165556,#165557,#165558,#165559,#165560,
#165561,#165562,#165563,#165564,#165565,#165566,#165567,#165568,#165569,
#165570,#165571,#165572,#165573,#165574,#165575,#165576,#165577,#165578,
#165579,#165580,#165581,#165582,#165583,#165584,#165585,#165586,#165587,
#165588,#165589,#165590,#165591,#165592,#165593,#165594,#165595,#165596,
#165597,#165598,#165599,#165600,#165601,#165602,#165603,#165604,#165605,
#165606,#165607,#165608,#165609,#165610,#165611,#165612,#165613,#165614,
#165615,#165616,#165617,#165618,#165619,#165620,#165621,#165622,#165623,
#165624,#165625,#165626,#165627,#165628,#165629,#165630,#165631,#165632,
#165633,#165634,#165635,#165636,#165637,#165638,#165639,#165640,#165641,
#165642,#165643,#165644,#165645,#165646,#165647,#165648,#165649,#165650,
#165651,#165652,#165653,#165654,#165655,#165656,#165657),.UNSPECIFIED.,
 .F.,.F.)
B_SPLINE_CURVE_WITH_KNOTS((6,1,1,1,1,1,1,1,1,1,1,1,1,1,1,1,1,1,1,1,1,1,
1,1,1,1,1,1,1,1,1,1,1,1,1,1,1,1,1,1,1,1,1,1,1,1,1,1,1,1,1,1,1,1,1,1,1,1,
1,1,1,1,1,1,1,1,1,1,1,1,1,1,1,1,1,1,1,1,1,1,1,1,1,1,1,1,1,1,1,1,1,1,1,1,
1,1,1,1,1,1,1,1,1,1,1,1,1,1,1,1,1,1,1,1,1,1,1,1,1,1,1,1,1,1,1,1,1,1,1,1,
1,1,1,1,1,1,1,1,1,1,1,1,1,1,1,1,1,1,1,1,1,1,1,1,1,1,1,1,1,1,1,1,1,1,1,1,
1,1,1,1,1,1,1,1,1,1,1,1,1,1,1,1,1,1,1,1,1,1,1,6),(0.,0.005,0.01,0.015,0.02,
0.025,0.03,0.035,0.04,0.045,0.05,0.055,0.06,0.065,0.07,0.075,0.08,0.085,
0.09,0.095,0.1,0.105,0.11,0.115,0.12,0.125,0.13,0.135,0.14,0.145,0.15,0.155,
0.16,0.165,0.17,0.175,0.18,0.185,0.19,0.195,0.2,0.205,0.21,0.215,0.22,0.225,
0.23,0.235,0.24,0.245,0.25,0.255,0.26,0.265,0.27,0.275,0.28,0.285,0.29,
0.295,0.3,0.305,0.31,0.315,0.32,0.325,0.33,0.335,0.34,0.345,0.35,0.355,
0.36,0.365,0.37,0.375,0.38,0.385,0.39,0.395,0.4,0.405,0.41,0.415,0.42,0.425,
0.43,0.435,0.44,0.445,0.45,0.455,0.46,0.465,0.47,0.475,0.48,0.485,0.49,
0.495,0.5,0.505,0.51,0.515,0.52,0.525,0.53,0.535,0.54,0.545,0.55,0.555,
0.56,0.565,0.57,0.575,0.58,0.585,0.59,0.595,0.6,0.605,0.61,0.615,0.62,0.625,
0.63,0.635,0.64,0.645,0.65,0.655,0.66,0.665,0.67,0.675,0.68,0.685,0.690000000000001,
0.695000000000001,0.700000000000001,0.705000000000001,0.710000000000001,
0.715000000000001,0.720000000000001,0.725000000000001,0.730000000000001,
0.735000000000001,0.740000000000001,0.745000000000001,0.750000000000001,
0.755000000000001,0.760000000000001,0.765000000000001,0.770000000000001,
0.775000000000001,0.780000000000001,0.785000000000001,0.790000000000001,
0.795000000000001,0.800000000000001,0.805000000000001,0.810000000000001,
0.815000000000001,0.820000000000001,0.825000000000001,0.830000000000001,
0.835000000000001,0.840000000000001,0.845000000000001,0.850000000000001,
0.855000000000001,0.860000000000001,0.865000000000001,0.870000000000001,
0.875000000000001,0.880000000000001,0.885000000000001,0.890000000000001,
0.895000000000001,0.900000000000001,0.905000000000001,0.910000000000001,
0.915000000000001,0.920000000000001,0.925000000000001,0.930000000000001,
0.935000000000001,0.940000000000001,0.941429844438172),.UNSPECIFIED.)
CURVE()
GEOMETRIC_REPRESENTATION_ITEM()
RATIONAL_B_SPLINE_CURVE((1.,1.,1.,1.,1.,1.,1.,1.,1.,1.,1.,1.,1.,1.,1.,1.,
1.,1.,1.,1.,1.,1.,1.,1.,1.,1.,1.,1.,1.,1.,1.,1.,1.,1.,1.,1.,1.,1.,1.,1.,
1.,1.,1.,1.,1.,1.,1.,1.,1.,1.,1.,1.,1.,1.,1.,1.,1.,1.,1.,1.,1.,1.,1.,1.,
1.,1.,1.,1.,1.,1.,1.,1.,1.,1.,1.,1.,1.,1.,1.,1.,1.,1.,1.,1.,1.,1.,1.,1.,
1.,1.,1.,1.,1.,1.,1.,1.,1.,1.,1.,1.,1.,1.,1.,1.,1.,1.,1.,1.,1.,1.,1.,1.,
1.,1.,1.,1.,1.,1.,1.,1.,1.,1.,1.,1.,1.,1.,1.,1.,1.,1.,1.,1.,1.,1.,1.,1.,
1.,1.,1.,1.,1.,1.,1.,1.,1.,1.,1.,1.,1.,1.,1.,1.,1.,1.,1.,1.,1.,1.,1.,1.,
1.,1.,1.,1.,1.,1.,1.,1.,1.,1.,1.,1.,1.,1.,1.,1.,1.,1.,1.,1.,1.,1.,1.,1.,
1.,1.,1.,1.,1.,1.,1.,1.,1.,1.))
REPRESENTATION_ITEM('')
);
#668=(
BOUNDED_CURVE()
B_SPLINE_CURVE(5,(#165660,#165661,#165662,#165663,#165664,#165665,#165666,
#165667,#165668,#165669,#165670,#165671,#165672,#165673,#165674,#165675,
#165676,#165677,#165678,#165679,#165680,#165681,#165682,#165683,#165684,
#165685,#165686,#165687,#165688,#165689,#165690,#165691,#165692,#165693,
#165694,#165695,#165696,#165697,#165698,#165699,#165700,#165701,#165702,
#165703,#165704,#165705,#165706,#165707,#165708,#165709,#165710,#165711,
#165712,#165713,#165714,#165715,#165716,#165717,#165718,#165719,#165720,
#165721,#165722,#165723,#165724,#165725,#165726,#165727,#165728,#165729,
#165730,#165731,#165732,#165733,#165734,#165735,#165736,#165737,#165738,
#165739,#165740,#165741,#165742,#165743,#165744,#165745,#165746,#165747,
#165748,#165749,#165750,#165751,#165752,#165753,#165754,#165755,#165756,
#165757,#165758,#165759,#165760,#165761,#165762,#165763,#165764,#165765,
#165766,#165767,#165768,#165769,#165770,#165771,#165772,#165773,#165774,
#165775,#165776,#165777,#165778,#165779,#165780,#165781,#165782,#165783,
#165784,#165785,#165786,#165787,#165788,#165789,#165790,#165791,#165792,
#165793,#165794,#165795,#165796,#165797,#165798,#165799,#165800,#165801,
#165802,#165803,#165804,#165805,#165806,#165807,#165808,#165809,#165810,
#165811,#165812,#165813,#165814,#165815,#165816,#165817,#165818,#165819,
#165820,#165821,#165822,#165823,#165824,#165825,#165826,#165827,#165828,
#165829,#165830,#165831,#165832,#165833,#165834,#165835,#165836,#165837,
#165838,#165839,#165840,#165841,#165842,#165843,#165844,#165845,#165846,
#165847,#165848,#165849,#165850,#165851,#165852,#165853),.UNSPECIFIED.,
 .F.,.F.)
B_SPLINE_CURVE_WITH_KNOTS((6,1,1,1,1,1,1,1,1,1,1,1,1,1,1,1,1,1,1,1,1,1,
1,1,1,1,1,1,1,1,1,1,1,1,1,1,1,1,1,1,1,1,1,1,1,1,1,1,1,1,1,1,1,1,1,1,1,1,
1,1,1,1,1,1,1,1,1,1,1,1,1,1,1,1,1,1,1,1,1,1,1,1,1,1,1,1,1,1,1,1,1,1,1,1,
1,1,1,1,1,1,1,1,1,1,1,1,1,1,1,1,1,1,1,1,1,1,1,1,1,1,1,1,1,1,1,1,1,1,1,1,
1,1,1,1,1,1,1,1,1,1,1,1,1,1,1,1,1,1,1,1,1,1,1,1,1,1,1,1,1,1,1,1,1,1,1,1,
1,1,1,1,1,1,1,1,1,1,1,1,1,1,1,1,1,1,1,1,1,1,1,6),(-0.941429844438172,-0.940000000000001,
-0.935000000000001,-0.930000000000001,-0.925000000000001,-0.920000000000001,
-0.915000000000001,-0.910000000000001,-0.905000000000001,-0.900000000000001,
-0.895000000000001,-0.890000000000001,-0.885000000000001,-0.880000000000001,
-0.875000000000001,-0.870000000000001,-0.865000000000001,-0.860000000000001,
-0.855000000000001,-0.850000000000001,-0.845000000000001,-0.840000000000001,
-0.835000000000001,-0.830000000000001,-0.825000000000001,-0.820000000000001,
-0.815000000000001,-0.810000000000001,-0.805000000000001,-0.800000000000001,
-0.795000000000001,-0.790000000000001,-0.785000000000001,-0.780000000000001,
-0.775000000000001,-0.770000000000001,-0.765000000000001,-0.760000000000001,
-0.755000000000001,-0.750000000000001,-0.745000000000001,-0.740000000000001,
-0.735000000000001,-0.730000000000001,-0.725000000000001,-0.720000000000001,
-0.715000000000001,-0.710000000000001,-0.705000000000001,-0.700000000000001,
-0.695000000000001,-0.690000000000001,-0.685,-0.68,-0.675,-0.67,-0.665,
-0.66,-0.655,-0.65,-0.645,-0.64,-0.635,-0.63,-0.625,-0.62,-0.615,-0.61,
-0.605,-0.6,-0.595,-0.59,-0.585,-0.58,-0.575,-0.57,-0.565,-0.56,-0.555,
-0.55,-0.545,-0.54,-0.535,-0.53,-0.525,-0.52,-0.515,-0.51,-0.505,-0.5,-0.495,
-0.49,-0.485,-0.48,-0.475,-0.47,-0.465,-0.46,-0.455,-0.45,-0.445,-0.44,
-0.435,-0.43,-0.425,-0.42,-0.415,-0.41,-0.405,-0.4,-0.395,-0.39,-0.385,
-0.38,-0.375,-0.37,-0.365,-0.36,-0.355,-0.35,-0.345,-0.34,-0.335,-0.33,
-0.325,-0.32,-0.315,-0.31,-0.305,-0.3,-0.295,-0.29,-0.285,-0.28,-0.275,
-0.27,-0.265,-0.26,-0.255,-0.25,-0.245,-0.24,-0.235,-0.23,-0.225,-0.22,
-0.215,-0.21,-0.205,-0.2,-0.195,-0.19,-0.185,-0.18,-0.175,-0.17,-0.165,
-0.16,-0.155,-0.15,-0.145,-0.14,-0.135,-0.13,-0.125,-0.12,-0.115,-0.11,
-0.105,-0.1,-0.095,-0.09,-0.085,-0.08,-0.075,-0.07,-0.065,-0.06,-0.055,
-0.05,-0.045,-0.04,-0.035,-0.03,-0.025,-0.02,-0.015,-0.01,-0.005,0.),
 .UNSPECIFIED.)
CURVE()
GEOMETRIC_REPRESENTATION_ITEM()
RATIONAL_B_SPLINE_CURVE((1.,1.,1.,1.,1.,1.,1.,1.,1.,1.,1.,1.,1.,1.,1.,1.,
1.,1.,1.,1.,1.,1.,1.,1.,1.,1.,1.,1.,1.,1.,1.,1.,1.,1.,1.,1.,1.,1.,1.,1.,
1.,1.,1.,1.,1.,1.,1.,1.,1.,1.,1.,1.,1.,1.,1.,1.,1.,1.,1.,1.,1.,1.,1.,1.,
1.,1.,1.,1.,1.,1.,1.,1.,1.,1.,1.,1.,1.,1.,1.,1.,1.,1.,1.,1.,1.,1.,1.,1.,
1.,1.,1.,1.,1.,1.,1.,1.,1.,1.,1.,1.,1.,1.,1.,1.,1.,1.,1.,1.,1.,1.,1.,1.,
1.,1.,1.,1.,1.,1.,1.,1.,1.,1.,1.,1.,1.,1.,1.,1.,1.,1.,1.,1.,1.,1.,1.,1.,
1.,1.,1.,1.,1.,1.,1.,1.,1.,1.,1.,1.,1.,1.,1.,1.,1.,1.,1.,1.,1.,1.,1.,1.,
1.,1.,1.,1.,1.,1.,1.,1.,1.,1.,1.,1.,1.,1.,1.,1.,1.,1.,1.,1.,1.,1.,1.,1.,
1.,1.,1.,1.,1.,1.,1.,1.,1.,1.))
REPRESENTATION_ITEM('')
);
#669=(
BOUNDED_CURVE()
B_SPLINE_CURVE(5,(#166265,#166266,#166267,#166268,#166269,#166270,#166271,
#166272,#166273,#166274,#166275,#166276,#166277,#166278,#166279,#166280,
#166281,#166282,#166283,#166284,#166285,#166286,#166287,#166288,#166289,
#166290,#166291,#166292,#166293,#166294,#166295,#166296,#166297,#166298,
#166299,#166300,#166301,#166302,#166303,#166304,#166305,#166306,#166307,
#166308,#166309,#166310,#166311,#166312,#166313,#166314,#166315,#166316,
#166317,#166318,#166319,#166320,#166321,#166322,#166323,#166324,#166325,
#166326,#166327,#166328,#166329,#166330,#166331,#166332,#166333,#166334,
#166335,#166336,#166337,#166338,#166339,#166340,#166341,#166342,#166343,
#166344,#166345,#166346,#166347,#166348,#166349,#166350,#166351,#166352,
#166353,#166354,#166355,#166356,#166357,#166358,#166359,#166360,#166361,
#166362,#166363,#166364,#166365,#166366,#166367,#166368,#166369,#166370,
#166371,#166372,#166373,#166374,#166375,#166376,#166377,#166378,#166379,
#166380,#166381,#166382,#166383,#166384,#166385,#166386,#166387,#166388,
#166389,#166390,#166391,#166392,#166393,#166394,#166395,#166396,#166397,
#166398,#166399,#166400,#166401,#166402,#166403,#166404,#166405,#166406,
#166407,#166408,#166409,#166410,#166411,#166412,#166413,#166414,#166415,
#166416,#166417,#166418,#166419,#166420,#166421,#166422,#166423,#166424,
#166425,#166426,#166427,#166428,#166429,#166430,#166431,#166432,#166433,
#166434,#166435,#166436,#166437,#166438,#166439,#166440,#166441,#166442,
#166443,#166444,#166445,#166446,#166447,#166448,#166449,#166450,#166451,
#166452,#166453,#166454,#166455,#166456,#166457,#166458),.UNSPECIFIED.,
 .F.,.F.)
B_SPLINE_CURVE_WITH_KNOTS((6,1,1,1,1,1,1,1,1,1,1,1,1,1,1,1,1,1,1,1,1,1,
1,1,1,1,1,1,1,1,1,1,1,1,1,1,1,1,1,1,1,1,1,1,1,1,1,1,1,1,1,1,1,1,1,1,1,1,
1,1,1,1,1,1,1,1,1,1,1,1,1,1,1,1,1,1,1,1,1,1,1,1,1,1,1,1,1,1,1,1,1,1,1,1,
1,1,1,1,1,1,1,1,1,1,1,1,1,1,1,1,1,1,1,1,1,1,1,1,1,1,1,1,1,1,1,1,1,1,1,1,
1,1,1,1,1,1,1,1,1,1,1,1,1,1,1,1,1,1,1,1,1,1,1,1,1,1,1,1,1,1,1,1,1,1,1,1,
1,1,1,1,1,1,1,1,1,1,1,1,1,1,1,1,1,1,1,1,1,1,1,6),(0.,0.005,0.01,0.015,0.02,
0.025,0.03,0.035,0.04,0.045,0.05,0.055,0.06,0.065,0.07,0.075,0.08,0.085,
0.09,0.095,0.1,0.105,0.11,0.115,0.12,0.125,0.13,0.135,0.14,0.145,0.15,0.155,
0.16,0.165,0.17,0.175,0.18,0.185,0.19,0.195,0.2,0.205,0.21,0.215,0.22,0.225,
0.23,0.235,0.24,0.245,0.25,0.255,0.26,0.265,0.27,0.275,0.28,0.285,0.29,
0.295,0.3,0.305,0.31,0.315,0.32,0.325,0.33,0.335,0.34,0.345,0.35,0.355,
0.36,0.365,0.37,0.375,0.38,0.385,0.39,0.395,0.4,0.405,0.41,0.415,0.42,0.425,
0.43,0.435,0.44,0.445,0.45,0.455,0.46,0.465,0.47,0.475,0.48,0.485,0.49,
0.495,0.5,0.505,0.51,0.515,0.52,0.525,0.53,0.535,0.54,0.545,0.55,0.555,
0.56,0.565,0.57,0.575,0.58,0.585,0.59,0.595,0.6,0.605,0.61,0.615,0.62,0.625,
0.63,0.635,0.64,0.645,0.65,0.655,0.66,0.665,0.67,0.675,0.68,0.685,0.690000000000001,
0.695000000000001,0.700000000000001,0.705000000000001,0.710000000000001,
0.715000000000001,0.720000000000001,0.725000000000001,0.730000000000001,
0.735000000000001,0.740000000000001,0.745000000000001,0.750000000000001,
0.755000000000001,0.760000000000001,0.765000000000001,0.770000000000001,
0.775000000000001,0.780000000000001,0.785000000000001,0.790000000000001,
0.795000000000001,0.800000000000001,0.805000000000001,0.810000000000001,
0.815000000000001,0.820000000000001,0.825000000000001,0.830000000000001,
0.835000000000001,0.840000000000001,0.845000000000001,0.850000000000001,
0.855000000000001,0.860000000000001,0.865000000000001,0.870000000000001,
0.875000000000001,0.880000000000001,0.885000000000001,0.890000000000001,
0.895000000000001,0.900000000000001,0.905000000000001,0.910000000000001,
0.915000000000001,0.920000000000001,0.925000000000001,0.930000000000001,
0.935000000000001,0.940000000000001,0.94142984443799),.UNSPECIFIED.)
CURVE()
GEOMETRIC_REPRESENTATION_ITEM()
RATIONAL_B_SPLINE_CURVE((1.,1.,1.,1.,1.,1.,1.,1.,1.,1.,1.,1.,1.,1.,1.,1.,
1.,1.,1.,1.,1.,1.,1.,1.,1.,1.,1.,1.,1.,1.,1.,1.,1.,1.,1.,1.,1.,1.,1.,1.,
1.,1.,1.,1.,1.,1.,1.,1.,1.,1.,1.,1.,1.,1.,1.,1.,1.,1.,1.,1.,1.,1.,1.,1.,
1.,1.,1.,1.,1.,1.,1.,1.,1.,1.,1.,1.,1.,1.,1.,1.,1.,1.,1.,1.,1.,1.,1.,1.,
1.,1.,1.,1.,1.,1.,1.,1.,1.,1.,1.,1.,1.,1.,1.,1.,1.,1.,1.,1.,1.,1.,1.,1.,
1.,1.,1.,1.,1.,1.,1.,1.,1.,1.,1.,1.,1.,1.,1.,1.,1.,1.,1.,1.,1.,1.,1.,1.,
1.,1.,1.,1.,1.,1.,1.,1.,1.,1.,1.,1.,1.,1.,1.,1.,1.,1.,1.,1.,1.,1.,1.,1.,
1.,1.,1.,1.,1.,1.,1.,1.,1.,1.,1.,1.,1.,1.,1.,1.,1.,1.,1.,1.,1.,1.,1.,1.,
1.,1.,1.,1.,1.,1.,1.,1.,1.,1.))
REPRESENTATION_ITEM('')
);
#670=(
BOUNDED_CURVE()
B_SPLINE_CURVE(5,(#166461,#166462,#166463,#166464,#166465,#166466,#166467,
#166468,#166469,#166470,#166471,#166472,#166473,#166474,#166475,#166476,
#166477,#166478,#166479,#166480,#166481,#166482,#166483,#166484,#166485,
#166486,#166487,#166488,#166489,#166490,#166491,#166492,#166493,#166494,
#166495,#166496,#166497,#166498,#166499,#166500,#166501,#166502,#166503,
#166504,#166505,#166506,#166507,#166508,#166509,#166510,#166511,#166512,
#166513,#166514,#166515,#166516,#166517,#166518,#166519,#166520,#166521,
#166522,#166523,#166524,#166525,#166526,#166527,#166528,#166529,#166530,
#166531,#166532,#166533,#166534,#166535,#166536,#166537,#166538,#166539,
#166540,#166541,#166542,#166543,#166544,#166545,#166546,#166547,#166548,
#166549,#166550,#166551,#166552,#166553,#166554,#166555,#166556,#166557,
#166558,#166559,#166560,#166561,#166562,#166563,#166564,#166565,#166566,
#166567,#166568,#166569,#166570,#166571,#166572,#166573,#166574,#166575,
#166576,#166577,#166578,#166579,#166580,#166581,#166582,#166583,#166584,
#166585,#166586,#166587,#166588,#166589,#166590,#166591,#166592,#166593,
#166594,#166595,#166596,#166597,#166598,#166599,#166600,#166601,#166602,
#166603,#166604,#166605,#166606,#166607,#166608,#166609,#166610,#166611,
#166612,#166613,#166614,#166615,#166616,#166617,#166618,#166619,#166620,
#166621,#166622,#166623,#166624,#166625,#166626,#166627,#166628,#166629,
#166630,#166631,#166632,#166633,#166634,#166635,#166636,#166637,#166638,
#166639,#166640,#166641,#166642,#166643,#166644,#166645,#166646,#166647,
#166648,#166649,#166650,#166651,#166652,#166653,#166654),.UNSPECIFIED.,
 .F.,.F.)
B_SPLINE_CURVE_WITH_KNOTS((6,1,1,1,1,1,1,1,1,1,1,1,1,1,1,1,1,1,1,1,1,1,
1,1,1,1,1,1,1,1,1,1,1,1,1,1,1,1,1,1,1,1,1,1,1,1,1,1,1,1,1,1,1,1,1,1,1,1,
1,1,1,1,1,1,1,1,1,1,1,1,1,1,1,1,1,1,1,1,1,1,1,1,1,1,1,1,1,1,1,1,1,1,1,1,
1,1,1,1,1,1,1,1,1,1,1,1,1,1,1,1,1,1,1,1,1,1,1,1,1,1,1,1,1,1,1,1,1,1,1,1,
1,1,1,1,1,1,1,1,1,1,1,1,1,1,1,1,1,1,1,1,1,1,1,1,1,1,1,1,1,1,1,1,1,1,1,1,
1,1,1,1,1,1,1,1,1,1,1,1,1,1,1,1,1,1,1,1,1,1,1,6),(-0.941429844437991,-0.940000000000001,
-0.935000000000001,-0.930000000000001,-0.925000000000001,-0.920000000000001,
-0.915000000000001,-0.910000000000001,-0.905000000000001,-0.900000000000001,
-0.895000000000001,-0.890000000000001,-0.885000000000001,-0.880000000000001,
-0.875000000000001,-0.870000000000001,-0.865000000000001,-0.860000000000001,
-0.855000000000001,-0.850000000000001,-0.845000000000001,-0.840000000000001,
-0.835000000000001,-0.830000000000001,-0.825000000000001,-0.820000000000001,
-0.815000000000001,-0.810000000000001,-0.805000000000001,-0.800000000000001,
-0.795000000000001,-0.790000000000001,-0.785000000000001,-0.780000000000001,
-0.775000000000001,-0.770000000000001,-0.765000000000001,-0.760000000000001,
-0.755000000000001,-0.750000000000001,-0.745000000000001,-0.740000000000001,
-0.735000000000001,-0.730000000000001,-0.725000000000001,-0.720000000000001,
-0.715000000000001,-0.710000000000001,-0.705000000000001,-0.700000000000001,
-0.695000000000001,-0.690000000000001,-0.685,-0.68,-0.675,-0.67,-0.665,
-0.66,-0.655,-0.65,-0.645,-0.64,-0.635,-0.63,-0.625,-0.62,-0.615,-0.61,
-0.605,-0.6,-0.595,-0.59,-0.585,-0.58,-0.575,-0.57,-0.565,-0.56,-0.555,
-0.55,-0.545,-0.54,-0.535,-0.53,-0.525,-0.52,-0.515,-0.51,-0.505,-0.5,-0.495,
-0.49,-0.485,-0.48,-0.475,-0.47,-0.465,-0.46,-0.455,-0.45,-0.445,-0.44,
-0.435,-0.43,-0.425,-0.42,-0.415,-0.41,-0.405,-0.4,-0.395,-0.39,-0.385,
-0.38,-0.375,-0.37,-0.365,-0.36,-0.355,-0.35,-0.345,-0.34,-0.335,-0.33,
-0.325,-0.32,-0.315,-0.31,-0.305,-0.3,-0.295,-0.29,-0.285,-0.28,-0.275,
-0.27,-0.265,-0.26,-0.255,-0.25,-0.245,-0.24,-0.235,-0.23,-0.225,-0.22,
-0.215,-0.21,-0.205,-0.2,-0.195,-0.19,-0.185,-0.18,-0.175,-0.17,-0.165,
-0.16,-0.155,-0.15,-0.145,-0.14,-0.135,-0.13,-0.125,-0.12,-0.115,-0.11,
-0.105,-0.1,-0.095,-0.09,-0.085,-0.08,-0.075,-0.07,-0.065,-0.06,-0.055,
-0.05,-0.045,-0.04,-0.035,-0.03,-0.025,-0.02,-0.015,-0.01,-0.005,0.),
 .UNSPECIFIED.)
CURVE()
GEOMETRIC_REPRESENTATION_ITEM()
RATIONAL_B_SPLINE_CURVE((1.,1.,1.,1.,1.,1.,1.,1.,1.,1.,1.,1.,1.,1.,1.,1.,
1.,1.,1.,1.,1.,1.,1.,1.,1.,1.,1.,1.,1.,1.,1.,1.,1.,1.,1.,1.,1.,1.,1.,1.,
1.,1.,1.,1.,1.,1.,1.,1.,1.,1.,1.,1.,1.,1.,1.,1.,1.,1.,1.,1.,1.,1.,1.,1.,
1.,1.,1.,1.,1.,1.,1.,1.,1.,1.,1.,1.,1.,1.,1.,1.,1.,1.,1.,1.,1.,1.,1.,1.,
1.,1.,1.,1.,1.,1.,1.,1.,1.,1.,1.,1.,1.,1.,1.,1.,1.,1.,1.,1.,1.,1.,1.,1.,
1.,1.,1.,1.,1.,1.,1.,1.,1.,1.,1.,1.,1.,1.,1.,1.,1.,1.,1.,1.,1.,1.,1.,1.,
1.,1.,1.,1.,1.,1.,1.,1.,1.,1.,1.,1.,1.,1.,1.,1.,1.,1.,1.,1.,1.,1.,1.,1.,
1.,1.,1.,1.,1.,1.,1.,1.,1.,1.,1.,1.,1.,1.,1.,1.,1.,1.,1.,1.,1.,1.,1.,1.,
1.,1.,1.,1.,1.,1.,1.,1.,1.,1.))
REPRESENTATION_ITEM('')
);
#671=(
BOUNDED_CURVE()
B_SPLINE_CURVE(5,(#167066,#167067,#167068,#167069,#167070,#167071,#167072,
#167073,#167074,#167075,#167076,#167077,#167078,#167079,#167080,#167081,
#167082,#167083,#167084,#167085,#167086,#167087,#167088,#167089,#167090,
#167091,#167092,#167093,#167094,#167095,#167096,#167097,#167098,#167099,
#167100,#167101,#167102,#167103,#167104,#167105,#167106,#167107,#167108,
#167109,#167110,#167111,#167112,#167113,#167114,#167115,#167116,#167117,
#167118,#167119,#167120,#167121,#167122,#167123,#167124,#167125,#167126,
#167127,#167128,#167129,#167130,#167131,#167132,#167133,#167134,#167135,
#167136,#167137,#167138,#167139,#167140,#167141,#167142,#167143,#167144,
#167145,#167146,#167147,#167148,#167149,#167150,#167151,#167152,#167153,
#167154,#167155,#167156,#167157,#167158,#167159,#167160,#167161,#167162,
#167163,#167164,#167165,#167166,#167167,#167168,#167169,#167170,#167171,
#167172,#167173,#167174,#167175,#167176,#167177,#167178,#167179,#167180,
#167181,#167182,#167183,#167184,#167185,#167186,#167187,#167188,#167189,
#167190,#167191,#167192,#167193,#167194,#167195,#167196,#167197,#167198,
#167199,#167200,#167201,#167202,#167203,#167204,#167205,#167206,#167207,
#167208,#167209,#167210,#167211,#167212,#167213,#167214,#167215,#167216,
#167217,#167218,#167219,#167220,#167221,#167222,#167223,#167224,#167225,
#167226,#167227,#167228,#167229,#167230,#167231,#167232,#167233,#167234,
#167235,#167236,#167237,#167238,#167239,#167240,#167241,#167242,#167243,
#167244,#167245,#167246,#167247,#167248,#167249,#167250,#167251,#167252,
#167253,#167254,#167255,#167256,#167257,#167258,#167259),.UNSPECIFIED.,
 .F.,.F.)
B_SPLINE_CURVE_WITH_KNOTS((6,1,1,1,1,1,1,1,1,1,1,1,1,1,1,1,1,1,1,1,1,1,
1,1,1,1,1,1,1,1,1,1,1,1,1,1,1,1,1,1,1,1,1,1,1,1,1,1,1,1,1,1,1,1,1,1,1,1,
1,1,1,1,1,1,1,1,1,1,1,1,1,1,1,1,1,1,1,1,1,1,1,1,1,1,1,1,1,1,1,1,1,1,1,1,
1,1,1,1,1,1,1,1,1,1,1,1,1,1,1,1,1,1,1,1,1,1,1,1,1,1,1,1,1,1,1,1,1,1,1,1,
1,1,1,1,1,1,1,1,1,1,1,1,1,1,1,1,1,1,1,1,1,1,1,1,1,1,1,1,1,1,1,1,1,1,1,1,
1,1,1,1,1,1,1,1,1,1,1,1,1,1,1,1,1,1,1,1,1,1,1,6),(0.,0.005,0.01,0.015,0.02,
0.025,0.03,0.035,0.04,0.045,0.05,0.055,0.06,0.065,0.07,0.075,0.08,0.085,
0.09,0.095,0.1,0.105,0.11,0.115,0.12,0.125,0.13,0.135,0.14,0.145,0.15,0.155,
0.16,0.165,0.17,0.175,0.18,0.185,0.19,0.195,0.2,0.205,0.21,0.215,0.22,0.225,
0.23,0.235,0.24,0.245,0.25,0.255,0.26,0.265,0.27,0.275,0.28,0.285,0.29,
0.295,0.3,0.305,0.31,0.315,0.32,0.325,0.33,0.335,0.34,0.345,0.35,0.355,
0.36,0.365,0.37,0.375,0.38,0.385,0.39,0.395,0.4,0.405,0.41,0.415,0.42,0.425,
0.43,0.435,0.44,0.445,0.45,0.455,0.46,0.465,0.47,0.475,0.48,0.485,0.49,
0.495,0.5,0.505,0.51,0.515,0.52,0.525,0.53,0.535,0.54,0.545,0.55,0.555,
0.56,0.565,0.57,0.575,0.58,0.585,0.59,0.595,0.6,0.605,0.61,0.615,0.62,0.625,
0.63,0.635,0.64,0.645,0.65,0.655,0.66,0.665,0.67,0.675,0.68,0.685,0.690000000000001,
0.695000000000001,0.700000000000001,0.705000000000001,0.710000000000001,
0.715000000000001,0.720000000000001,0.725000000000001,0.730000000000001,
0.735000000000001,0.740000000000001,0.745000000000001,0.750000000000001,
0.755000000000001,0.760000000000001,0.765000000000001,0.770000000000001,
0.775000000000001,0.780000000000001,0.785000000000001,0.790000000000001,
0.795000000000001,0.800000000000001,0.805000000000001,0.810000000000001,
0.815000000000001,0.820000000000001,0.825000000000001,0.830000000000001,
0.835000000000001,0.840000000000001,0.845000000000001,0.850000000000001,
0.855000000000001,0.860000000000001,0.865000000000001,0.870000000000001,
0.875000000000001,0.880000000000001,0.885000000000001,0.890000000000001,
0.895000000000001,0.900000000000001,0.905000000000001,0.910000000000001,
0.915000000000001,0.920000000000001,0.925000000000001,0.930000000000001,
0.935000000000001,0.940000000000001,0.941429844438107),.UNSPECIFIED.)
CURVE()
GEOMETRIC_REPRESENTATION_ITEM()
RATIONAL_B_SPLINE_CURVE((1.,1.,1.,1.,1.,1.,1.,1.,1.,1.,1.,1.,1.,1.,1.,1.,
1.,1.,1.,1.,1.,1.,1.,1.,1.,1.,1.,1.,1.,1.,1.,1.,1.,1.,1.,1.,1.,1.,1.,1.,
1.,1.,1.,1.,1.,1.,1.,1.,1.,1.,1.,1.,1.,1.,1.,1.,1.,1.,1.,1.,1.,1.,1.,1.,
1.,1.,1.,1.,1.,1.,1.,1.,1.,1.,1.,1.,1.,1.,1.,1.,1.,1.,1.,1.,1.,1.,1.,1.,
1.,1.,1.,1.,1.,1.,1.,1.,1.,1.,1.,1.,1.,1.,1.,1.,1.,1.,1.,1.,1.,1.,1.,1.,
1.,1.,1.,1.,1.,1.,1.,1.,1.,1.,1.,1.,1.,1.,1.,1.,1.,1.,1.,1.,1.,1.,1.,1.,
1.,1.,1.,1.,1.,1.,1.,1.,1.,1.,1.,1.,1.,1.,1.,1.,1.,1.,1.,1.,1.,1.,1.,1.,
1.,1.,1.,1.,1.,1.,1.,1.,1.,1.,1.,1.,1.,1.,1.,1.,1.,1.,1.,1.,1.,1.,1.,1.,
1.,1.,1.,1.,1.,1.,1.,1.,1.,1.))
REPRESENTATION_ITEM('')
);
#672=(
BOUNDED_CURVE()
B_SPLINE_CURVE(5,(#167262,#167263,#167264,#167265,#167266,#167267,#167268,
#167269,#167270,#167271,#167272,#167273,#167274,#167275,#167276,#167277,
#167278,#167279,#167280,#167281,#167282,#167283,#167284,#167285,#167286,
#167287,#167288,#167289,#167290,#167291,#167292,#167293,#167294,#167295,
#167296,#167297,#167298,#167299,#167300,#167301,#167302,#167303,#167304,
#167305,#167306,#167307,#167308,#167309,#167310,#167311,#167312,#167313,
#167314,#167315,#167316,#167317,#167318,#167319,#167320,#167321,#167322,
#167323,#167324,#167325,#167326,#167327,#167328,#167329,#167330,#167331,
#167332,#167333,#167334,#167335,#167336,#167337,#167338,#167339,#167340,
#167341,#167342,#167343,#167344,#167345,#167346,#167347,#167348,#167349,
#167350,#167351,#167352,#167353,#167354,#167355,#167356,#167357,#167358,
#167359,#167360,#167361,#167362,#167363,#167364,#167365,#167366,#167367,
#167368,#167369,#167370,#167371,#167372,#167373,#167374,#167375,#167376,
#167377,#167378,#167379,#167380,#167381,#167382,#167383,#167384,#167385,
#167386,#167387,#167388,#167389,#167390,#167391,#167392,#167393,#167394,
#167395,#167396,#167397,#167398,#167399,#167400,#167401,#167402,#167403,
#167404,#167405,#167406,#167407,#167408,#167409,#167410,#167411,#167412,
#167413,#167414,#167415,#167416,#167417,#167418,#167419,#167420,#167421,
#167422,#167423,#167424,#167425,#167426,#167427,#167428,#167429,#167430,
#167431,#167432,#167433,#167434,#167435,#167436,#167437,#167438,#167439,
#167440,#167441,#167442,#167443,#167444,#167445,#167446,#167447,#167448,
#167449,#167450,#167451,#167452,#167453,#167454,#167455),.UNSPECIFIED.,
 .F.,.F.)
B_SPLINE_CURVE_WITH_KNOTS((6,1,1,1,1,1,1,1,1,1,1,1,1,1,1,1,1,1,1,1,1,1,
1,1,1,1,1,1,1,1,1,1,1,1,1,1,1,1,1,1,1,1,1,1,1,1,1,1,1,1,1,1,1,1,1,1,1,1,
1,1,1,1,1,1,1,1,1,1,1,1,1,1,1,1,1,1,1,1,1,1,1,1,1,1,1,1,1,1,1,1,1,1,1,1,
1,1,1,1,1,1,1,1,1,1,1,1,1,1,1,1,1,1,1,1,1,1,1,1,1,1,1,1,1,1,1,1,1,1,1,1,
1,1,1,1,1,1,1,1,1,1,1,1,1,1,1,1,1,1,1,1,1,1,1,1,1,1,1,1,1,1,1,1,1,1,1,1,
1,1,1,1,1,1,1,1,1,1,1,1,1,1,1,1,1,1,1,1,1,1,1,6),(-0.941429844438107,-0.940000000000001,
-0.935000000000001,-0.930000000000001,-0.925000000000001,-0.920000000000001,
-0.915000000000001,-0.910000000000001,-0.905000000000001,-0.900000000000001,
-0.895000000000001,-0.890000000000001,-0.885000000000001,-0.880000000000001,
-0.875000000000001,-0.870000000000001,-0.865000000000001,-0.860000000000001,
-0.855000000000001,-0.850000000000001,-0.845000000000001,-0.840000000000001,
-0.835000000000001,-0.830000000000001,-0.825000000000001,-0.820000000000001,
-0.815000000000001,-0.810000000000001,-0.805000000000001,-0.800000000000001,
-0.795000000000001,-0.790000000000001,-0.785000000000001,-0.780000000000001,
-0.775000000000001,-0.770000000000001,-0.765000000000001,-0.760000000000001,
-0.755000000000001,-0.750000000000001,-0.745000000000001,-0.740000000000001,
-0.735000000000001,-0.730000000000001,-0.725000000000001,-0.720000000000001,
-0.715000000000001,-0.710000000000001,-0.705000000000001,-0.700000000000001,
-0.695000000000001,-0.690000000000001,-0.685,-0.68,-0.675,-0.67,-0.665,
-0.66,-0.655,-0.65,-0.645,-0.64,-0.635,-0.63,-0.625,-0.62,-0.615,-0.61,
-0.605,-0.6,-0.595,-0.59,-0.585,-0.58,-0.575,-0.57,-0.565,-0.56,-0.555,
-0.55,-0.545,-0.54,-0.535,-0.53,-0.525,-0.52,-0.515,-0.51,-0.505,-0.5,-0.495,
-0.49,-0.485,-0.48,-0.475,-0.47,-0.465,-0.46,-0.455,-0.45,-0.445,-0.44,
-0.435,-0.43,-0.425,-0.42,-0.415,-0.41,-0.405,-0.4,-0.395,-0.39,-0.385,
-0.38,-0.375,-0.37,-0.365,-0.36,-0.355,-0.35,-0.345,-0.34,-0.335,-0.33,
-0.325,-0.32,-0.315,-0.31,-0.305,-0.3,-0.295,-0.29,-0.285,-0.28,-0.275,
-0.27,-0.265,-0.26,-0.255,-0.25,-0.245,-0.24,-0.235,-0.23,-0.225,-0.22,
-0.215,-0.21,-0.205,-0.2,-0.195,-0.19,-0.185,-0.18,-0.175,-0.17,-0.165,
-0.16,-0.155,-0.15,-0.145,-0.14,-0.135,-0.13,-0.125,-0.12,-0.115,-0.11,
-0.105,-0.1,-0.095,-0.09,-0.085,-0.08,-0.075,-0.07,-0.065,-0.06,-0.055,
-0.05,-0.045,-0.04,-0.035,-0.03,-0.025,-0.02,-0.015,-0.01,-0.005,0.),
 .UNSPECIFIED.)
CURVE()
GEOMETRIC_REPRESENTATION_ITEM()
RATIONAL_B_SPLINE_CURVE((1.,1.,1.,1.,1.,1.,1.,1.,1.,1.,1.,1.,1.,1.,1.,1.,
1.,1.,1.,1.,1.,1.,1.,1.,1.,1.,1.,1.,1.,1.,1.,1.,1.,1.,1.,1.,1.,1.,1.,1.,
1.,1.,1.,1.,1.,1.,1.,1.,1.,1.,1.,1.,1.,1.,1.,1.,1.,1.,1.,1.,1.,1.,1.,1.,
1.,1.,1.,1.,1.,1.,1.,1.,1.,1.,1.,1.,1.,1.,1.,1.,1.,1.,1.,1.,1.,1.,1.,1.,
1.,1.,1.,1.,1.,1.,1.,1.,1.,1.,1.,1.,1.,1.,1.,1.,1.,1.,1.,1.,1.,1.,1.,1.,
1.,1.,1.,1.,1.,1.,1.,1.,1.,1.,1.,1.,1.,1.,1.,1.,1.,1.,1.,1.,1.,1.,1.,1.,
1.,1.,1.,1.,1.,1.,1.,1.,1.,1.,1.,1.,1.,1.,1.,1.,1.,1.,1.,1.,1.,1.,1.,1.,
1.,1.,1.,1.,1.,1.,1.,1.,1.,1.,1.,1.,1.,1.,1.,1.,1.,1.,1.,1.,1.,1.,1.,1.,
1.,1.,1.,1.,1.,1.,1.,1.,1.,1.))
REPRESENTATION_ITEM('')
);
#673=(
BOUNDED_CURVE()
B_SPLINE_CURVE(5,(#167867,#167868,#167869,#167870,#167871,#167872,#167873,
#167874,#167875,#167876,#167877,#167878,#167879,#167880,#167881,#167882,
#167883,#167884,#167885,#167886,#167887,#167888,#167889,#167890,#167891,
#167892,#167893,#167894,#167895,#167896,#167897,#167898,#167899,#167900,
#167901,#167902,#167903,#167904,#167905,#167906,#167907,#167908,#167909,
#167910,#167911,#167912,#167913,#167914,#167915,#167916,#167917,#167918,
#167919,#167920,#167921,#167922,#167923,#167924,#167925,#167926,#167927,
#167928,#167929,#167930,#167931,#167932,#167933,#167934,#167935,#167936,
#167937,#167938,#167939,#167940,#167941,#167942,#167943,#167944,#167945,
#167946,#167947,#167948,#167949,#167950,#167951,#167952,#167953,#167954,
#167955,#167956,#167957,#167958,#167959,#167960,#167961,#167962,#167963,
#167964,#167965,#167966,#167967,#167968,#167969,#167970,#167971,#167972,
#167973,#167974,#167975,#167976,#167977,#167978,#167979,#167980,#167981,
#167982,#167983,#167984,#167985,#167986,#167987,#167988,#167989,#167990,
#167991,#167992,#167993,#167994,#167995,#167996,#167997,#167998,#167999,
#168000,#168001,#168002,#168003,#168004,#168005,#168006,#168007,#168008,
#168009,#168010,#168011,#168012,#168013,#168014,#168015,#168016,#168017,
#168018,#168019,#168020,#168021,#168022,#168023,#168024,#168025,#168026,
#168027,#168028,#168029,#168030,#168031,#168032,#168033,#168034,#168035,
#168036,#168037,#168038,#168039,#168040,#168041,#168042,#168043,#168044,
#168045,#168046,#168047,#168048,#168049,#168050,#168051,#168052,#168053,
#168054,#168055,#168056,#168057,#168058,#168059,#168060),.UNSPECIFIED.,
 .F.,.F.)
B_SPLINE_CURVE_WITH_KNOTS((6,1,1,1,1,1,1,1,1,1,1,1,1,1,1,1,1,1,1,1,1,1,
1,1,1,1,1,1,1,1,1,1,1,1,1,1,1,1,1,1,1,1,1,1,1,1,1,1,1,1,1,1,1,1,1,1,1,1,
1,1,1,1,1,1,1,1,1,1,1,1,1,1,1,1,1,1,1,1,1,1,1,1,1,1,1,1,1,1,1,1,1,1,1,1,
1,1,1,1,1,1,1,1,1,1,1,1,1,1,1,1,1,1,1,1,1,1,1,1,1,1,1,1,1,1,1,1,1,1,1,1,
1,1,1,1,1,1,1,1,1,1,1,1,1,1,1,1,1,1,1,1,1,1,1,1,1,1,1,1,1,1,1,1,1,1,1,1,
1,1,1,1,1,1,1,1,1,1,1,1,1,1,1,1,1,1,1,1,1,1,1,6),(0.,0.005,0.01,0.015,0.02,
0.025,0.03,0.035,0.04,0.045,0.05,0.055,0.06,0.065,0.07,0.075,0.08,0.085,
0.09,0.095,0.1,0.105,0.11,0.115,0.12,0.125,0.13,0.135,0.14,0.145,0.15,0.155,
0.16,0.165,0.17,0.175,0.18,0.185,0.19,0.195,0.2,0.205,0.21,0.215,0.22,0.225,
0.23,0.235,0.24,0.245,0.25,0.255,0.26,0.265,0.27,0.275,0.28,0.285,0.29,
0.295,0.3,0.305,0.31,0.315,0.32,0.325,0.33,0.335,0.34,0.345,0.35,0.355,
0.36,0.365,0.37,0.375,0.38,0.385,0.39,0.395,0.4,0.405,0.41,0.415,0.42,0.425,
0.43,0.435,0.44,0.445,0.45,0.455,0.46,0.465,0.47,0.475,0.48,0.485,0.49,
0.495,0.5,0.505,0.51,0.515,0.52,0.525,0.53,0.535,0.54,0.545,0.55,0.555,
0.56,0.565,0.57,0.575,0.58,0.585,0.59,0.595,0.6,0.605,0.61,0.615,0.62,0.625,
0.63,0.635,0.64,0.645,0.65,0.655,0.66,0.665,0.67,0.675,0.68,0.685,0.690000000000001,
0.695000000000001,0.700000000000001,0.705000000000001,0.710000000000001,
0.715000000000001,0.720000000000001,0.725000000000001,0.730000000000001,
0.735000000000001,0.740000000000001,0.745000000000001,0.750000000000001,
0.755000000000001,0.760000000000001,0.765000000000001,0.770000000000001,
0.775000000000001,0.780000000000001,0.785000000000001,0.790000000000001,
0.795000000000001,0.800000000000001,0.805000000000001,0.810000000000001,
0.815000000000001,0.820000000000001,0.825000000000001,0.830000000000001,
0.835000000000001,0.840000000000001,0.845000000000001,0.850000000000001,
0.855000000000001,0.860000000000001,0.865000000000001,0.870000000000001,
0.875000000000001,0.880000000000001,0.885000000000001,0.890000000000001,
0.895000000000001,0.900000000000001,0.905000000000001,0.910000000000001,
0.915000000000001,0.920000000000001,0.925000000000001,0.930000000000001,
0.935000000000001,0.940000000000001,0.941429844438079),.UNSPECIFIED.)
CURVE()
GEOMETRIC_REPRESENTATION_ITEM()
RATIONAL_B_SPLINE_CURVE((1.,1.,1.,1.,1.,1.,1.,1.,1.,1.,1.,1.,1.,1.,1.,1.,
1.,1.,1.,1.,1.,1.,1.,1.,1.,1.,1.,1.,1.,1.,1.,1.,1.,1.,1.,1.,1.,1.,1.,1.,
1.,1.,1.,1.,1.,1.,1.,1.,1.,1.,1.,1.,1.,1.,1.,1.,1.,1.,1.,1.,1.,1.,1.,1.,
1.,1.,1.,1.,1.,1.,1.,1.,1.,1.,1.,1.,1.,1.,1.,1.,1.,1.,1.,1.,1.,1.,1.,1.,
1.,1.,1.,1.,1.,1.,1.,1.,1.,1.,1.,1.,1.,1.,1.,1.,1.,1.,1.,1.,1.,1.,1.,1.,
1.,1.,1.,1.,1.,1.,1.,1.,1.,1.,1.,1.,1.,1.,1.,1.,1.,1.,1.,1.,1.,1.,1.,1.,
1.,1.,1.,1.,1.,1.,1.,1.,1.,1.,1.,1.,1.,1.,1.,1.,1.,1.,1.,1.,1.,1.,1.,1.,
1.,1.,1.,1.,1.,1.,1.,1.,1.,1.,1.,1.,1.,1.,1.,1.,1.,1.,1.,1.,1.,1.,1.,1.,
1.,1.,1.,1.,1.,1.,1.,1.,1.,1.))
REPRESENTATION_ITEM('')
);
#674=(
BOUNDED_CURVE()
B_SPLINE_CURVE(5,(#168063,#168064,#168065,#168066,#168067,#168068,#168069,
#168070,#168071,#168072,#168073,#168074,#168075,#168076,#168077,#168078,
#168079,#168080,#168081,#168082,#168083,#168084,#168085,#168086,#168087,
#168088,#168089,#168090,#168091,#168092,#168093,#168094,#168095,#168096,
#168097,#168098,#168099,#168100,#168101,#168102,#168103,#168104,#168105,
#168106,#168107,#168108,#168109,#168110,#168111,#168112,#168113,#168114,
#168115,#168116,#168117,#168118,#168119,#168120,#168121,#168122,#168123,
#168124,#168125,#168126,#168127,#168128,#168129,#168130,#168131,#168132,
#168133,#168134,#168135,#168136,#168137,#168138,#168139,#168140,#168141,
#168142,#168143,#168144,#168145,#168146,#168147,#168148,#168149,#168150,
#168151,#168152,#168153,#168154,#168155,#168156,#168157,#168158,#168159,
#168160,#168161,#168162,#168163,#168164,#168165,#168166,#168167,#168168,
#168169,#168170,#168171,#168172,#168173,#168174,#168175,#168176,#168177,
#168178,#168179,#168180,#168181,#168182,#168183,#168184,#168185,#168186,
#168187,#168188,#168189,#168190,#168191,#168192,#168193,#168194,#168195,
#168196,#168197,#168198,#168199,#168200,#168201,#168202,#168203,#168204,
#168205,#168206,#168207,#168208,#168209,#168210,#168211,#168212,#168213,
#168214,#168215,#168216,#168217,#168218,#168219,#168220,#168221,#168222,
#168223,#168224,#168225,#168226,#168227,#168228,#168229,#168230,#168231,
#168232,#168233,#168234,#168235,#168236,#168237,#168238,#168239,#168240,
#168241,#168242,#168243,#168244,#168245,#168246,#168247,#168248,#168249,
#168250,#168251,#168252,#168253,#168254,#168255,#168256),.UNSPECIFIED.,
 .F.,.F.)
B_SPLINE_CURVE_WITH_KNOTS((6,1,1,1,1,1,1,1,1,1,1,1,1,1,1,1,1,1,1,1,1,1,
1,1,1,1,1,1,1,1,1,1,1,1,1,1,1,1,1,1,1,1,1,1,1,1,1,1,1,1,1,1,1,1,1,1,1,1,
1,1,1,1,1,1,1,1,1,1,1,1,1,1,1,1,1,1,1,1,1,1,1,1,1,1,1,1,1,1,1,1,1,1,1,1,
1,1,1,1,1,1,1,1,1,1,1,1,1,1,1,1,1,1,1,1,1,1,1,1,1,1,1,1,1,1,1,1,1,1,1,1,
1,1,1,1,1,1,1,1,1,1,1,1,1,1,1,1,1,1,1,1,1,1,1,1,1,1,1,1,1,1,1,1,1,1,1,1,
1,1,1,1,1,1,1,1,1,1,1,1,1,1,1,1,1,1,1,1,1,1,1,6),(-0.941429844438079,-0.940000000000001,
-0.935000000000001,-0.930000000000001,-0.925000000000001,-0.920000000000001,
-0.915000000000001,-0.910000000000001,-0.905000000000001,-0.900000000000001,
-0.895000000000001,-0.890000000000001,-0.885000000000001,-0.880000000000001,
-0.875000000000001,-0.870000000000001,-0.865000000000001,-0.860000000000001,
-0.855000000000001,-0.850000000000001,-0.845000000000001,-0.840000000000001,
-0.835000000000001,-0.830000000000001,-0.825000000000001,-0.820000000000001,
-0.815000000000001,-0.810000000000001,-0.805000000000001,-0.800000000000001,
-0.795000000000001,-0.790000000000001,-0.785000000000001,-0.780000000000001,
-0.775000000000001,-0.770000000000001,-0.765000000000001,-0.760000000000001,
-0.755000000000001,-0.750000000000001,-0.745000000000001,-0.740000000000001,
-0.735000000000001,-0.730000000000001,-0.725000000000001,-0.720000000000001,
-0.715000000000001,-0.710000000000001,-0.705000000000001,-0.700000000000001,
-0.695000000000001,-0.690000000000001,-0.685,-0.68,-0.675,-0.67,-0.665,
-0.66,-0.655,-0.65,-0.645,-0.64,-0.635,-0.63,-0.625,-0.62,-0.615,-0.61,
-0.605,-0.6,-0.595,-0.59,-0.585,-0.58,-0.575,-0.57,-0.565,-0.56,-0.555,
-0.55,-0.545,-0.54,-0.535,-0.53,-0.525,-0.52,-0.515,-0.51,-0.505,-0.5,-0.495,
-0.49,-0.485,-0.48,-0.475,-0.47,-0.465,-0.46,-0.455,-0.45,-0.445,-0.44,
-0.435,-0.43,-0.425,-0.42,-0.415,-0.41,-0.405,-0.4,-0.395,-0.39,-0.385,
-0.38,-0.375,-0.37,-0.365,-0.36,-0.355,-0.35,-0.345,-0.34,-0.335,-0.33,
-0.325,-0.32,-0.315,-0.31,-0.305,-0.3,-0.295,-0.29,-0.285,-0.28,-0.275,
-0.27,-0.265,-0.26,-0.255,-0.25,-0.245,-0.24,-0.235,-0.23,-0.225,-0.22,
-0.215,-0.21,-0.205,-0.2,-0.195,-0.19,-0.185,-0.18,-0.175,-0.17,-0.165,
-0.16,-0.155,-0.15,-0.145,-0.14,-0.135,-0.13,-0.125,-0.12,-0.115,-0.11,
-0.105,-0.1,-0.095,-0.09,-0.085,-0.08,-0.075,-0.07,-0.065,-0.06,-0.055,
-0.05,-0.045,-0.04,-0.035,-0.03,-0.025,-0.02,-0.015,-0.01,-0.005,0.),
 .UNSPECIFIED.)
CURVE()
GEOMETRIC_REPRESENTATION_ITEM()
RATIONAL_B_SPLINE_CURVE((1.,1.,1.,1.,1.,1.,1.,1.,1.,1.,1.,1.,1.,1.,1.,1.,
1.,1.,1.,1.,1.,1.,1.,1.,1.,1.,1.,1.,1.,1.,1.,1.,1.,1.,1.,1.,1.,1.,1.,1.,
1.,1.,1.,1.,1.,1.,1.,1.,1.,1.,1.,1.,1.,1.,1.,1.,1.,1.,1.,1.,1.,1.,1.,1.,
1.,1.,1.,1.,1.,1.,1.,1.,1.,1.,1.,1.,1.,1.,1.,1.,1.,1.,1.,1.,1.,1.,1.,1.,
1.,1.,1.,1.,1.,1.,1.,1.,1.,1.,1.,1.,1.,1.,1.,1.,1.,1.,1.,1.,1.,1.,1.,1.,
1.,1.,1.,1.,1.,1.,1.,1.,1.,1.,1.,1.,1.,1.,1.,1.,1.,1.,1.,1.,1.,1.,1.,1.,
1.,1.,1.,1.,1.,1.,1.,1.,1.,1.,1.,1.,1.,1.,1.,1.,1.,1.,1.,1.,1.,1.,1.,1.,
1.,1.,1.,1.,1.,1.,1.,1.,1.,1.,1.,1.,1.,1.,1.,1.,1.,1.,1.,1.,1.,1.,1.,1.,
1.,1.,1.,1.,1.,1.,1.,1.,1.,1.))
REPRESENTATION_ITEM('')
);
#675=(
BOUNDED_CURVE()
B_SPLINE_CURVE(5,(#168668,#168669,#168670,#168671,#168672,#168673,#168674,
#168675,#168676,#168677,#168678,#168679,#168680,#168681,#168682,#168683,
#168684,#168685,#168686,#168687,#168688,#168689,#168690,#168691,#168692,
#168693,#168694,#168695,#168696,#168697,#168698,#168699,#168700,#168701,
#168702,#168703,#168704,#168705,#168706,#168707,#168708,#168709,#168710,
#168711,#168712,#168713,#168714,#168715,#168716,#168717,#168718,#168719,
#168720,#168721,#168722,#168723,#168724,#168725,#168726,#168727,#168728,
#168729,#168730,#168731,#168732,#168733,#168734,#168735,#168736,#168737,
#168738,#168739,#168740,#168741,#168742,#168743,#168744,#168745,#168746,
#168747,#168748,#168749,#168750,#168751,#168752,#168753,#168754,#168755,
#168756,#168757,#168758,#168759,#168760,#168761,#168762,#168763,#168764,
#168765,#168766,#168767,#168768,#168769,#168770,#168771,#168772,#168773,
#168774,#168775,#168776,#168777,#168778,#168779,#168780,#168781,#168782,
#168783,#168784,#168785,#168786,#168787,#168788,#168789,#168790,#168791,
#168792,#168793,#168794,#168795,#168796,#168797,#168798,#168799,#168800,
#168801,#168802,#168803,#168804,#168805,#168806,#168807,#168808,#168809,
#168810,#168811,#168812,#168813,#168814,#168815,#168816,#168817,#168818,
#168819,#168820,#168821,#168822,#168823,#168824,#168825,#168826,#168827,
#168828,#168829,#168830,#168831,#168832,#168833,#168834,#168835,#168836,
#168837,#168838,#168839,#168840,#168841,#168842,#168843,#168844,#168845,
#168846,#168847,#168848,#168849,#168850,#168851,#168852,#168853,#168854,
#168855,#168856,#168857,#168858,#168859,#168860,#168861),.UNSPECIFIED.,
 .F.,.F.)
B_SPLINE_CURVE_WITH_KNOTS((6,1,1,1,1,1,1,1,1,1,1,1,1,1,1,1,1,1,1,1,1,1,
1,1,1,1,1,1,1,1,1,1,1,1,1,1,1,1,1,1,1,1,1,1,1,1,1,1,1,1,1,1,1,1,1,1,1,1,
1,1,1,1,1,1,1,1,1,1,1,1,1,1,1,1,1,1,1,1,1,1,1,1,1,1,1,1,1,1,1,1,1,1,1,1,
1,1,1,1,1,1,1,1,1,1,1,1,1,1,1,1,1,1,1,1,1,1,1,1,1,1,1,1,1,1,1,1,1,1,1,1,
1,1,1,1,1,1,1,1,1,1,1,1,1,1,1,1,1,1,1,1,1,1,1,1,1,1,1,1,1,1,1,1,1,1,1,1,
1,1,1,1,1,1,1,1,1,1,1,1,1,1,1,1,1,1,1,1,1,1,1,6),(0.,0.005,0.01,0.015,0.02,
0.025,0.03,0.035,0.04,0.045,0.05,0.055,0.06,0.065,0.07,0.075,0.08,0.085,
0.09,0.095,0.1,0.105,0.11,0.115,0.12,0.125,0.13,0.135,0.14,0.145,0.15,0.155,
0.16,0.165,0.17,0.175,0.18,0.185,0.19,0.195,0.2,0.205,0.21,0.215,0.22,0.225,
0.23,0.235,0.24,0.245,0.25,0.255,0.26,0.265,0.27,0.275,0.28,0.285,0.29,
0.295,0.3,0.305,0.31,0.315,0.32,0.325,0.33,0.335,0.34,0.345,0.35,0.355,
0.36,0.365,0.37,0.375,0.38,0.385,0.39,0.395,0.4,0.405,0.41,0.415,0.42,0.425,
0.43,0.435,0.44,0.445,0.45,0.455,0.46,0.465,0.47,0.475,0.48,0.485,0.49,
0.495,0.5,0.505,0.51,0.515,0.52,0.525,0.53,0.535,0.54,0.545,0.55,0.555,
0.56,0.565,0.57,0.575,0.58,0.585,0.59,0.595,0.6,0.605,0.61,0.615,0.62,0.625,
0.63,0.635,0.64,0.645,0.65,0.655,0.66,0.665,0.67,0.675,0.68,0.685,0.690000000000001,
0.695000000000001,0.700000000000001,0.705000000000001,0.710000000000001,
0.715000000000001,0.720000000000001,0.725000000000001,0.730000000000001,
0.735000000000001,0.740000000000001,0.745000000000001,0.750000000000001,
0.755000000000001,0.760000000000001,0.765000000000001,0.770000000000001,
0.775000000000001,0.780000000000001,0.785000000000001,0.790000000000001,
0.795000000000001,0.800000000000001,0.805000000000001,0.810000000000001,
0.815000000000001,0.820000000000001,0.825000000000001,0.830000000000001,
0.835000000000001,0.840000000000001,0.845000000000001,0.850000000000001,
0.855000000000001,0.860000000000001,0.865000000000001,0.870000000000001,
0.875000000000001,0.880000000000001,0.885000000000001,0.890000000000001,
0.895000000000001,0.900000000000001,0.905000000000001,0.910000000000001,
0.915000000000001,0.920000000000001,0.925000000000001,0.930000000000001,
0.935000000000001,0.940000000000001,0.941429844438012),.UNSPECIFIED.)
CURVE()
GEOMETRIC_REPRESENTATION_ITEM()
RATIONAL_B_SPLINE_CURVE((1.,1.,1.,1.,1.,1.,1.,1.,1.,1.,1.,1.,1.,1.,1.,1.,
1.,1.,1.,1.,1.,1.,1.,1.,1.,1.,1.,1.,1.,1.,1.,1.,1.,1.,1.,1.,1.,1.,1.,1.,
1.,1.,1.,1.,1.,1.,1.,1.,1.,1.,1.,1.,1.,1.,1.,1.,1.,1.,1.,1.,1.,1.,1.,1.,
1.,1.,1.,1.,1.,1.,1.,1.,1.,1.,1.,1.,1.,1.,1.,1.,1.,1.,1.,1.,1.,1.,1.,1.,
1.,1.,1.,1.,1.,1.,1.,1.,1.,1.,1.,1.,1.,1.,1.,1.,1.,1.,1.,1.,1.,1.,1.,1.,
1.,1.,1.,1.,1.,1.,1.,1.,1.,1.,1.,1.,1.,1.,1.,1.,1.,1.,1.,1.,1.,1.,1.,1.,
1.,1.,1.,1.,1.,1.,1.,1.,1.,1.,1.,1.,1.,1.,1.,1.,1.,1.,1.,1.,1.,1.,1.,1.,
1.,1.,1.,1.,1.,1.,1.,1.,1.,1.,1.,1.,1.,1.,1.,1.,1.,1.,1.,1.,1.,1.,1.,1.,
1.,1.,1.,1.,1.,1.,1.,1.,1.,1.))
REPRESENTATION_ITEM('')
);
#676=(
BOUNDED_CURVE()
B_SPLINE_CURVE(5,(#168864,#168865,#168866,#168867,#168868,#168869,#168870,
#168871,#168872,#168873,#168874,#168875,#168876,#168877,#168878,#168879,
#168880,#168881,#168882,#168883,#168884,#168885,#168886,#168887,#168888,
#168889,#168890,#168891,#168892,#168893,#168894,#168895,#168896,#168897,
#168898,#168899,#168900,#168901,#168902,#168903,#168904,#168905,#168906,
#168907,#168908,#168909,#168910,#168911,#168912,#168913,#168914,#168915,
#168916,#168917,#168918,#168919,#168920,#168921,#168922,#168923,#168924,
#168925,#168926,#168927,#168928,#168929,#168930,#168931,#168932,#168933,
#168934,#168935,#168936,#168937,#168938,#168939,#168940,#168941,#168942,
#168943,#168944,#168945,#168946,#168947,#168948,#168949,#168950,#168951,
#168952,#168953,#168954,#168955,#168956,#168957,#168958,#168959,#168960,
#168961,#168962,#168963,#168964,#168965,#168966,#168967,#168968,#168969,
#168970,#168971,#168972,#168973,#168974,#168975,#168976,#168977,#168978,
#168979,#168980,#168981,#168982,#168983,#168984,#168985,#168986,#168987,
#168988,#168989,#168990,#168991,#168992,#168993,#168994,#168995,#168996,
#168997,#168998,#168999,#169000,#169001,#169002,#169003,#169004,#169005,
#169006,#169007,#169008,#169009,#169010,#169011,#169012,#169013,#169014,
#169015,#169016,#169017,#169018,#169019,#169020,#169021,#169022,#169023,
#169024,#169025,#169026,#169027,#169028,#169029,#169030,#169031,#169032,
#169033,#169034,#169035,#169036,#169037,#169038,#169039,#169040,#169041,
#169042,#169043,#169044,#169045,#169046,#169047,#169048,#169049,#169050,
#169051,#169052,#169053,#169054,#169055,#169056,#169057),.UNSPECIFIED.,
 .F.,.F.)
B_SPLINE_CURVE_WITH_KNOTS((6,1,1,1,1,1,1,1,1,1,1,1,1,1,1,1,1,1,1,1,1,1,
1,1,1,1,1,1,1,1,1,1,1,1,1,1,1,1,1,1,1,1,1,1,1,1,1,1,1,1,1,1,1,1,1,1,1,1,
1,1,1,1,1,1,1,1,1,1,1,1,1,1,1,1,1,1,1,1,1,1,1,1,1,1,1,1,1,1,1,1,1,1,1,1,
1,1,1,1,1,1,1,1,1,1,1,1,1,1,1,1,1,1,1,1,1,1,1,1,1,1,1,1,1,1,1,1,1,1,1,1,
1,1,1,1,1,1,1,1,1,1,1,1,1,1,1,1,1,1,1,1,1,1,1,1,1,1,1,1,1,1,1,1,1,1,1,1,
1,1,1,1,1,1,1,1,1,1,1,1,1,1,1,1,1,1,1,1,1,1,1,6),(-0.941429844438006,-0.940000000000001,
-0.935000000000001,-0.930000000000001,-0.925000000000001,-0.920000000000001,
-0.915000000000001,-0.910000000000001,-0.905000000000001,-0.900000000000001,
-0.895000000000001,-0.890000000000001,-0.885000000000001,-0.880000000000001,
-0.875000000000001,-0.870000000000001,-0.865000000000001,-0.860000000000001,
-0.855000000000001,-0.850000000000001,-0.845000000000001,-0.840000000000001,
-0.835000000000001,-0.830000000000001,-0.825000000000001,-0.820000000000001,
-0.815000000000001,-0.810000000000001,-0.805000000000001,-0.800000000000001,
-0.795000000000001,-0.790000000000001,-0.785000000000001,-0.780000000000001,
-0.775000000000001,-0.770000000000001,-0.765000000000001,-0.760000000000001,
-0.755000000000001,-0.750000000000001,-0.745000000000001,-0.740000000000001,
-0.735000000000001,-0.730000000000001,-0.725000000000001,-0.720000000000001,
-0.715000000000001,-0.710000000000001,-0.705000000000001,-0.700000000000001,
-0.695000000000001,-0.690000000000001,-0.685,-0.68,-0.675,-0.67,-0.665,
-0.66,-0.655,-0.65,-0.645,-0.64,-0.635,-0.63,-0.625,-0.62,-0.615,-0.61,
-0.605,-0.6,-0.595,-0.59,-0.585,-0.58,-0.575,-0.57,-0.565,-0.56,-0.555,
-0.55,-0.545,-0.54,-0.535,-0.53,-0.525,-0.52,-0.515,-0.51,-0.505,-0.5,-0.495,
-0.49,-0.485,-0.48,-0.475,-0.47,-0.465,-0.46,-0.455,-0.45,-0.445,-0.44,
-0.435,-0.43,-0.425,-0.42,-0.415,-0.41,-0.405,-0.4,-0.395,-0.39,-0.385,
-0.38,-0.375,-0.37,-0.365,-0.36,-0.355,-0.35,-0.345,-0.34,-0.335,-0.33,
-0.325,-0.32,-0.315,-0.31,-0.305,-0.3,-0.295,-0.29,-0.285,-0.28,-0.275,
-0.27,-0.265,-0.26,-0.255,-0.25,-0.245,-0.24,-0.235,-0.23,-0.225,-0.22,
-0.215,-0.21,-0.205,-0.2,-0.195,-0.19,-0.185,-0.18,-0.175,-0.17,-0.165,
-0.16,-0.155,-0.15,-0.145,-0.14,-0.135,-0.13,-0.125,-0.12,-0.115,-0.11,
-0.105,-0.1,-0.095,-0.09,-0.085,-0.08,-0.075,-0.07,-0.065,-0.06,-0.055,
-0.05,-0.045,-0.04,-0.035,-0.03,-0.025,-0.02,-0.015,-0.01,-0.005,0.),
 .UNSPECIFIED.)
CURVE()
GEOMETRIC_REPRESENTATION_ITEM()
RATIONAL_B_SPLINE_CURVE((1.,1.,1.,1.,1.,1.,1.,1.,1.,1.,1.,1.,1.,1.,1.,1.,
1.,1.,1.,1.,1.,1.,1.,1.,1.,1.,1.,1.,1.,1.,1.,1.,1.,1.,1.,1.,1.,1.,1.,1.,
1.,1.,1.,1.,1.,1.,1.,1.,1.,1.,1.,1.,1.,1.,1.,1.,1.,1.,1.,1.,1.,1.,1.,1.,
1.,1.,1.,1.,1.,1.,1.,1.,1.,1.,1.,1.,1.,1.,1.,1.,1.,1.,1.,1.,1.,1.,1.,1.,
1.,1.,1.,1.,1.,1.,1.,1.,1.,1.,1.,1.,1.,1.,1.,1.,1.,1.,1.,1.,1.,1.,1.,1.,
1.,1.,1.,1.,1.,1.,1.,1.,1.,1.,1.,1.,1.,1.,1.,1.,1.,1.,1.,1.,1.,1.,1.,1.,
1.,1.,1.,1.,1.,1.,1.,1.,1.,1.,1.,1.,1.,1.,1.,1.,1.,1.,1.,1.,1.,1.,1.,1.,
1.,1.,1.,1.,1.,1.,1.,1.,1.,1.,1.,1.,1.,1.,1.,1.,1.,1.,1.,1.,1.,1.,1.,1.,
1.,1.,1.,1.,1.,1.,1.,1.,1.,1.))
REPRESENTATION_ITEM('')
);
#677=(
BOUNDED_CURVE()
B_SPLINE_CURVE(5,(#169469,#169470,#169471,#169472,#169473,#169474,#169475,
#169476,#169477,#169478,#169479,#169480,#169481,#169482,#169483,#169484,
#169485,#169486,#169487,#169488,#169489,#169490,#169491,#169492,#169493,
#169494,#169495,#169496,#169497,#169498,#169499,#169500,#169501,#169502,
#169503,#169504,#169505,#169506,#169507,#169508,#169509,#169510,#169511,
#169512,#169513,#169514,#169515,#169516,#169517,#169518,#169519,#169520,
#169521,#169522,#169523,#169524,#169525,#169526,#169527,#169528,#169529,
#169530,#169531,#169532,#169533,#169534,#169535,#169536,#169537,#169538,
#169539,#169540,#169541,#169542,#169543,#169544,#169545,#169546,#169547,
#169548,#169549,#169550,#169551,#169552,#169553,#169554,#169555,#169556,
#169557,#169558,#169559,#169560,#169561,#169562,#169563,#169564,#169565,
#169566,#169567,#169568,#169569,#169570,#169571,#169572,#169573,#169574,
#169575,#169576,#169577,#169578,#169579,#169580,#169581,#169582,#169583,
#169584,#169585,#169586,#169587,#169588,#169589,#169590,#169591,#169592,
#169593,#169594,#169595,#169596,#169597,#169598,#169599,#169600,#169601,
#169602,#169603,#169604,#169605,#169606,#169607,#169608,#169609,#169610,
#169611,#169612,#169613,#169614,#169615,#169616,#169617,#169618,#169619,
#169620,#169621,#169622,#169623,#169624,#169625,#169626,#169627,#169628,
#169629,#169630,#169631,#169632,#169633,#169634,#169635,#169636,#169637,
#169638,#169639,#169640,#169641,#169642,#169643,#169644,#169645,#169646,
#169647,#169648,#169649,#169650,#169651,#169652,#169653,#169654,#169655,
#169656,#169657,#169658,#169659,#169660,#169661,#169662),.UNSPECIFIED.,
 .F.,.F.)
B_SPLINE_CURVE_WITH_KNOTS((6,1,1,1,1,1,1,1,1,1,1,1,1,1,1,1,1,1,1,1,1,1,
1,1,1,1,1,1,1,1,1,1,1,1,1,1,1,1,1,1,1,1,1,1,1,1,1,1,1,1,1,1,1,1,1,1,1,1,
1,1,1,1,1,1,1,1,1,1,1,1,1,1,1,1,1,1,1,1,1,1,1,1,1,1,1,1,1,1,1,1,1,1,1,1,
1,1,1,1,1,1,1,1,1,1,1,1,1,1,1,1,1,1,1,1,1,1,1,1,1,1,1,1,1,1,1,1,1,1,1,1,
1,1,1,1,1,1,1,1,1,1,1,1,1,1,1,1,1,1,1,1,1,1,1,1,1,1,1,1,1,1,1,1,1,1,1,1,
1,1,1,1,1,1,1,1,1,1,1,1,1,1,1,1,1,1,1,1,1,1,1,6),(0.,0.005,0.01,0.015,0.02,
0.025,0.03,0.035,0.04,0.045,0.05,0.055,0.06,0.065,0.07,0.075,0.08,0.085,
0.09,0.095,0.1,0.105,0.11,0.115,0.12,0.125,0.13,0.135,0.14,0.145,0.15,0.155,
0.16,0.165,0.17,0.175,0.18,0.185,0.19,0.195,0.2,0.205,0.21,0.215,0.22,0.225,
0.23,0.235,0.24,0.245,0.25,0.255,0.26,0.265,0.27,0.275,0.28,0.285,0.29,
0.295,0.3,0.305,0.31,0.315,0.32,0.325,0.33,0.335,0.34,0.345,0.35,0.355,
0.36,0.365,0.37,0.375,0.38,0.385,0.39,0.395,0.4,0.405,0.41,0.415,0.42,0.425,
0.43,0.435,0.44,0.445,0.45,0.455,0.46,0.465,0.47,0.475,0.48,0.485,0.49,
0.495,0.5,0.505,0.51,0.515,0.52,0.525,0.53,0.535,0.54,0.545,0.55,0.555,
0.56,0.565,0.57,0.575,0.58,0.585,0.59,0.595,0.6,0.605,0.61,0.615,0.62,0.625,
0.63,0.635,0.64,0.645,0.65,0.655,0.66,0.665,0.67,0.675,0.68,0.685,0.690000000000001,
0.695000000000001,0.700000000000001,0.705000000000001,0.710000000000001,
0.715000000000001,0.720000000000001,0.725000000000001,0.730000000000001,
0.735000000000001,0.740000000000001,0.745000000000001,0.750000000000001,
0.755000000000001,0.760000000000001,0.765000000000001,0.770000000000001,
0.775000000000001,0.780000000000001,0.785000000000001,0.790000000000001,
0.795000000000001,0.800000000000001,0.805000000000001,0.810000000000001,
0.815000000000001,0.820000000000001,0.825000000000001,0.830000000000001,
0.835000000000001,0.840000000000001,0.845000000000001,0.850000000000001,
0.855000000000001,0.860000000000001,0.865000000000001,0.870000000000001,
0.875000000000001,0.880000000000001,0.885000000000001,0.890000000000001,
0.895000000000001,0.900000000000001,0.905000000000001,0.910000000000001,
0.915000000000001,0.920000000000001,0.925000000000001,0.930000000000001,
0.935000000000001,0.940000000000001,0.94142984443808),.UNSPECIFIED.)
CURVE()
GEOMETRIC_REPRESENTATION_ITEM()
RATIONAL_B_SPLINE_CURVE((1.,1.,1.,1.,1.,1.,1.,1.,1.,1.,1.,1.,1.,1.,1.,1.,
1.,1.,1.,1.,1.,1.,1.,1.,1.,1.,1.,1.,1.,1.,1.,1.,1.,1.,1.,1.,1.,1.,1.,1.,
1.,1.,1.,1.,1.,1.,1.,1.,1.,1.,1.,1.,1.,1.,1.,1.,1.,1.,1.,1.,1.,1.,1.,1.,
1.,1.,1.,1.,1.,1.,1.,1.,1.,1.,1.,1.,1.,1.,1.,1.,1.,1.,1.,1.,1.,1.,1.,1.,
1.,1.,1.,1.,1.,1.,1.,1.,1.,1.,1.,1.,1.,1.,1.,1.,1.,1.,1.,1.,1.,1.,1.,1.,
1.,1.,1.,1.,1.,1.,1.,1.,1.,1.,1.,1.,1.,1.,1.,1.,1.,1.,1.,1.,1.,1.,1.,1.,
1.,1.,1.,1.,1.,1.,1.,1.,1.,1.,1.,1.,1.,1.,1.,1.,1.,1.,1.,1.,1.,1.,1.,1.,
1.,1.,1.,1.,1.,1.,1.,1.,1.,1.,1.,1.,1.,1.,1.,1.,1.,1.,1.,1.,1.,1.,1.,1.,
1.,1.,1.,1.,1.,1.,1.,1.,1.,1.))
REPRESENTATION_ITEM('')
);
#678=(
BOUNDED_CURVE()
B_SPLINE_CURVE(5,(#169665,#169666,#169667,#169668,#169669,#169670,#169671,
#169672,#169673,#169674,#169675,#169676,#169677,#169678,#169679,#169680,
#169681,#169682,#169683,#169684,#169685,#169686,#169687,#169688,#169689,
#169690,#169691,#169692,#169693,#169694,#169695,#169696,#169697,#169698,
#169699,#169700,#169701,#169702,#169703,#169704,#169705,#169706,#169707,
#169708,#169709,#169710,#169711,#169712,#169713,#169714,#169715,#169716,
#169717,#169718,#169719,#169720,#169721,#169722,#169723,#169724,#169725,
#169726,#169727,#169728,#169729,#169730,#169731,#169732,#169733,#169734,
#169735,#169736,#169737,#169738,#169739,#169740,#169741,#169742,#169743,
#169744,#169745,#169746,#169747,#169748,#169749,#169750,#169751,#169752,
#169753,#169754,#169755,#169756,#169757,#169758,#169759,#169760,#169761,
#169762,#169763,#169764,#169765,#169766,#169767,#169768,#169769,#169770,
#169771,#169772,#169773,#169774,#169775,#169776,#169777,#169778,#169779,
#169780,#169781,#169782,#169783,#169784,#169785,#169786,#169787,#169788,
#169789,#169790,#169791,#169792,#169793,#169794,#169795,#169796,#169797,
#169798,#169799,#169800,#169801,#169802,#169803,#169804,#169805,#169806,
#169807,#169808,#169809,#169810,#169811,#169812,#169813,#169814,#169815,
#169816,#169817,#169818,#169819,#169820,#169821,#169822,#169823,#169824,
#169825,#169826,#169827,#169828,#169829,#169830,#169831,#169832,#169833,
#169834,#169835,#169836,#169837,#169838,#169839,#169840,#169841,#169842,
#169843,#169844,#169845,#169846,#169847,#169848,#169849,#169850,#169851,
#169852,#169853,#169854,#169855,#169856,#169857,#169858),.UNSPECIFIED.,
 .F.,.F.)
B_SPLINE_CURVE_WITH_KNOTS((6,1,1,1,1,1,1,1,1,1,1,1,1,1,1,1,1,1,1,1,1,1,
1,1,1,1,1,1,1,1,1,1,1,1,1,1,1,1,1,1,1,1,1,1,1,1,1,1,1,1,1,1,1,1,1,1,1,1,
1,1,1,1,1,1,1,1,1,1,1,1,1,1,1,1,1,1,1,1,1,1,1,1,1,1,1,1,1,1,1,1,1,1,1,1,
1,1,1,1,1,1,1,1,1,1,1,1,1,1,1,1,1,1,1,1,1,1,1,1,1,1,1,1,1,1,1,1,1,1,1,1,
1,1,1,1,1,1,1,1,1,1,1,1,1,1,1,1,1,1,1,1,1,1,1,1,1,1,1,1,1,1,1,1,1,1,1,1,
1,1,1,1,1,1,1,1,1,1,1,1,1,1,1,1,1,1,1,1,1,1,1,6),(-0.941429844438109,-0.940000000000001,
-0.935000000000001,-0.930000000000001,-0.925000000000001,-0.920000000000001,
-0.915000000000001,-0.910000000000001,-0.905000000000001,-0.900000000000001,
-0.895000000000001,-0.890000000000001,-0.885000000000001,-0.880000000000001,
-0.875000000000001,-0.870000000000001,-0.865000000000001,-0.860000000000001,
-0.855000000000001,-0.850000000000001,-0.845000000000001,-0.840000000000001,
-0.835000000000001,-0.830000000000001,-0.825000000000001,-0.820000000000001,
-0.815000000000001,-0.810000000000001,-0.805000000000001,-0.800000000000001,
-0.795000000000001,-0.790000000000001,-0.785000000000001,-0.780000000000001,
-0.775000000000001,-0.770000000000001,-0.765000000000001,-0.760000000000001,
-0.755000000000001,-0.750000000000001,-0.745000000000001,-0.740000000000001,
-0.735000000000001,-0.730000000000001,-0.725000000000001,-0.720000000000001,
-0.715000000000001,-0.710000000000001,-0.705000000000001,-0.700000000000001,
-0.695000000000001,-0.690000000000001,-0.685,-0.68,-0.675,-0.67,-0.665,
-0.66,-0.655,-0.65,-0.645,-0.64,-0.635,-0.63,-0.625,-0.62,-0.615,-0.61,
-0.605,-0.6,-0.595,-0.59,-0.585,-0.58,-0.575,-0.57,-0.565,-0.56,-0.555,
-0.55,-0.545,-0.54,-0.535,-0.53,-0.525,-0.52,-0.515,-0.51,-0.505,-0.5,-0.495,
-0.49,-0.485,-0.48,-0.475,-0.47,-0.465,-0.46,-0.455,-0.45,-0.445,-0.44,
-0.435,-0.43,-0.425,-0.42,-0.415,-0.41,-0.405,-0.4,-0.395,-0.39,-0.385,
-0.38,-0.375,-0.37,-0.365,-0.36,-0.355,-0.35,-0.345,-0.34,-0.335,-0.33,
-0.325,-0.32,-0.315,-0.31,-0.305,-0.3,-0.295,-0.29,-0.285,-0.28,-0.275,
-0.27,-0.265,-0.26,-0.255,-0.25,-0.245,-0.24,-0.235,-0.23,-0.225,-0.22,
-0.215,-0.21,-0.205,-0.2,-0.195,-0.19,-0.185,-0.18,-0.175,-0.17,-0.165,
-0.16,-0.155,-0.15,-0.145,-0.14,-0.135,-0.13,-0.125,-0.12,-0.115,-0.11,
-0.105,-0.1,-0.095,-0.09,-0.085,-0.08,-0.075,-0.07,-0.065,-0.06,-0.055,
-0.05,-0.045,-0.04,-0.035,-0.03,-0.025,-0.02,-0.015,-0.01,-0.005,0.),
 .UNSPECIFIED.)
CURVE()
GEOMETRIC_REPRESENTATION_ITEM()
RATIONAL_B_SPLINE_CURVE((1.,1.,1.,1.,1.,1.,1.,1.,1.,1.,1.,1.,1.,1.,1.,1.,
1.,1.,1.,1.,1.,1.,1.,1.,1.,1.,1.,1.,1.,1.,1.,1.,1.,1.,1.,1.,1.,1.,1.,1.,
1.,1.,1.,1.,1.,1.,1.,1.,1.,1.,1.,1.,1.,1.,1.,1.,1.,1.,1.,1.,1.,1.,1.,1.,
1.,1.,1.,1.,1.,1.,1.,1.,1.,1.,1.,1.,1.,1.,1.,1.,1.,1.,1.,1.,1.,1.,1.,1.,
1.,1.,1.,1.,1.,1.,1.,1.,1.,1.,1.,1.,1.,1.,1.,1.,1.,1.,1.,1.,1.,1.,1.,1.,
1.,1.,1.,1.,1.,1.,1.,1.,1.,1.,1.,1.,1.,1.,1.,1.,1.,1.,1.,1.,1.,1.,1.,1.,
1.,1.,1.,1.,1.,1.,1.,1.,1.,1.,1.,1.,1.,1.,1.,1.,1.,1.,1.,1.,1.,1.,1.,1.,
1.,1.,1.,1.,1.,1.,1.,1.,1.,1.,1.,1.,1.,1.,1.,1.,1.,1.,1.,1.,1.,1.,1.,1.,
1.,1.,1.,1.,1.,1.,1.,1.,1.,1.))
REPRESENTATION_ITEM('')
);
#679=(
BOUNDED_CURVE()
B_SPLINE_CURVE(5,(#170270,#170271,#170272,#170273,#170274,#170275,#170276,
#170277,#170278,#170279,#170280,#170281,#170282,#170283,#170284,#170285,
#170286,#170287,#170288,#170289,#170290,#170291,#170292,#170293,#170294,
#170295,#170296,#170297,#170298,#170299,#170300,#170301,#170302,#170303,
#170304,#170305,#170306,#170307,#170308,#170309,#170310,#170311,#170312,
#170313,#170314,#170315,#170316,#170317,#170318,#170319,#170320,#170321,
#170322,#170323,#170324,#170325,#170326,#170327,#170328,#170329,#170330,
#170331,#170332,#170333,#170334,#170335,#170336,#170337,#170338,#170339,
#170340,#170341,#170342,#170343,#170344,#170345,#170346,#170347,#170348,
#170349,#170350,#170351,#170352,#170353,#170354,#170355,#170356,#170357,
#170358,#170359,#170360,#170361,#170362,#170363,#170364,#170365,#170366,
#170367,#170368,#170369,#170370,#170371,#170372,#170373,#170374,#170375,
#170376,#170377,#170378,#170379,#170380,#170381,#170382,#170383,#170384,
#170385,#170386,#170387,#170388,#170389,#170390,#170391,#170392,#170393,
#170394,#170395,#170396,#170397,#170398,#170399,#170400,#170401,#170402,
#170403,#170404,#170405,#170406,#170407,#170408,#170409,#170410,#170411,
#170412,#170413,#170414,#170415,#170416,#170417,#170418,#170419,#170420,
#170421,#170422,#170423,#170424,#170425,#170426,#170427,#170428,#170429,
#170430,#170431,#170432,#170433,#170434,#170435,#170436,#170437,#170438,
#170439,#170440,#170441,#170442,#170443,#170444,#170445,#170446,#170447,
#170448,#170449,#170450,#170451,#170452,#170453,#170454,#170455,#170456,
#170457,#170458,#170459,#170460,#170461,#170462,#170463),.UNSPECIFIED.,
 .F.,.F.)
B_SPLINE_CURVE_WITH_KNOTS((6,1,1,1,1,1,1,1,1,1,1,1,1,1,1,1,1,1,1,1,1,1,
1,1,1,1,1,1,1,1,1,1,1,1,1,1,1,1,1,1,1,1,1,1,1,1,1,1,1,1,1,1,1,1,1,1,1,1,
1,1,1,1,1,1,1,1,1,1,1,1,1,1,1,1,1,1,1,1,1,1,1,1,1,1,1,1,1,1,1,1,1,1,1,1,
1,1,1,1,1,1,1,1,1,1,1,1,1,1,1,1,1,1,1,1,1,1,1,1,1,1,1,1,1,1,1,1,1,1,1,1,
1,1,1,1,1,1,1,1,1,1,1,1,1,1,1,1,1,1,1,1,1,1,1,1,1,1,1,1,1,1,1,1,1,1,1,1,
1,1,1,1,1,1,1,1,1,1,1,1,1,1,1,1,1,1,1,1,1,1,1,6),(0.,0.005,0.01,0.015,0.02,
0.025,0.03,0.035,0.04,0.045,0.05,0.055,0.06,0.065,0.07,0.075,0.08,0.085,
0.09,0.095,0.1,0.105,0.11,0.115,0.12,0.125,0.13,0.135,0.14,0.145,0.15,0.155,
0.16,0.165,0.17,0.175,0.18,0.185,0.19,0.195,0.2,0.205,0.21,0.215,0.22,0.225,
0.23,0.235,0.24,0.245,0.25,0.255,0.26,0.265,0.27,0.275,0.28,0.285,0.29,
0.295,0.3,0.305,0.31,0.315,0.32,0.325,0.33,0.335,0.34,0.345,0.35,0.355,
0.36,0.365,0.37,0.375,0.38,0.385,0.39,0.395,0.4,0.405,0.41,0.415,0.42,0.425,
0.43,0.435,0.44,0.445,0.45,0.455,0.46,0.465,0.47,0.475,0.48,0.485,0.49,
0.495,0.5,0.505,0.51,0.515,0.52,0.525,0.53,0.535,0.54,0.545,0.55,0.555,
0.56,0.565,0.57,0.575,0.58,0.585,0.59,0.595,0.6,0.605,0.61,0.615,0.62,0.625,
0.63,0.635,0.64,0.645,0.65,0.655,0.66,0.665,0.67,0.675,0.68,0.685,0.690000000000001,
0.695000000000001,0.700000000000001,0.705000000000001,0.710000000000001,
0.715000000000001,0.720000000000001,0.725000000000001,0.730000000000001,
0.735000000000001,0.740000000000001,0.745000000000001,0.750000000000001,
0.755000000000001,0.760000000000001,0.765000000000001,0.770000000000001,
0.775000000000001,0.780000000000001,0.785000000000001,0.790000000000001,
0.795000000000001,0.800000000000001,0.805000000000001,0.810000000000001,
0.815000000000001,0.820000000000001,0.825000000000001,0.830000000000001,
0.835000000000001,0.840000000000001,0.845000000000001,0.850000000000001,
0.855000000000001,0.860000000000001,0.865000000000001,0.870000000000001,
0.875000000000001,0.880000000000001,0.885000000000001,0.890000000000001,
0.895000000000001,0.900000000000001,0.905000000000001,0.910000000000001,
0.915000000000001,0.920000000000001,0.925000000000001,0.930000000000001,
0.935000000000001,0.940000000000001,0.941429844438046),.UNSPECIFIED.)
CURVE()
GEOMETRIC_REPRESENTATION_ITEM()
RATIONAL_B_SPLINE_CURVE((1.,1.,1.,1.,1.,1.,1.,1.,1.,1.,1.,1.,1.,1.,1.,1.,
1.,1.,1.,1.,1.,1.,1.,1.,1.,1.,1.,1.,1.,1.,1.,1.,1.,1.,1.,1.,1.,1.,1.,1.,
1.,1.,1.,1.,1.,1.,1.,1.,1.,1.,1.,1.,1.,1.,1.,1.,1.,1.,1.,1.,1.,1.,1.,1.,
1.,1.,1.,1.,1.,1.,1.,1.,1.,1.,1.,1.,1.,1.,1.,1.,1.,1.,1.,1.,1.,1.,1.,1.,
1.,1.,1.,1.,1.,1.,1.,1.,1.,1.,1.,1.,1.,1.,1.,1.,1.,1.,1.,1.,1.,1.,1.,1.,
1.,1.,1.,1.,1.,1.,1.,1.,1.,1.,1.,1.,1.,1.,1.,1.,1.,1.,1.,1.,1.,1.,1.,1.,
1.,1.,1.,1.,1.,1.,1.,1.,1.,1.,1.,1.,1.,1.,1.,1.,1.,1.,1.,1.,1.,1.,1.,1.,
1.,1.,1.,1.,1.,1.,1.,1.,1.,1.,1.,1.,1.,1.,1.,1.,1.,1.,1.,1.,1.,1.,1.,1.,
1.,1.,1.,1.,1.,1.,1.,1.,1.,1.))
REPRESENTATION_ITEM('')
);
#680=(
BOUNDED_CURVE()
B_SPLINE_CURVE(5,(#170466,#170467,#170468,#170469,#170470,#170471,#170472,
#170473,#170474,#170475,#170476,#170477,#170478,#170479,#170480,#170481,
#170482,#170483,#170484,#170485,#170486,#170487,#170488,#170489,#170490,
#170491,#170492,#170493,#170494,#170495,#170496,#170497,#170498,#170499,
#170500,#170501,#170502,#170503,#170504,#170505,#170506,#170507,#170508,
#170509,#170510,#170511,#170512,#170513,#170514,#170515,#170516,#170517,
#170518,#170519,#170520,#170521,#170522,#170523,#170524,#170525,#170526,
#170527,#170528,#170529,#170530,#170531,#170532,#170533,#170534,#170535,
#170536,#170537,#170538,#170539,#170540,#170541,#170542,#170543,#170544,
#170545,#170546,#170547,#170548,#170549,#170550,#170551,#170552,#170553,
#170554,#170555,#170556,#170557,#170558,#170559,#170560,#170561,#170562,
#170563,#170564,#170565,#170566,#170567,#170568,#170569,#170570,#170571,
#170572,#170573,#170574,#170575,#170576,#170577,#170578,#170579,#170580,
#170581,#170582,#170583,#170584,#170585,#170586,#170587,#170588,#170589,
#170590,#170591,#170592,#170593,#170594,#170595,#170596,#170597,#170598,
#170599,#170600,#170601,#170602,#170603,#170604,#170605,#170606,#170607,
#170608,#170609,#170610,#170611,#170612,#170613,#170614,#170615,#170616,
#170617,#170618,#170619,#170620,#170621,#170622,#170623,#170624,#170625,
#170626,#170627,#170628,#170629,#170630,#170631,#170632,#170633,#170634,
#170635,#170636,#170637,#170638,#170639,#170640,#170641,#170642,#170643,
#170644,#170645,#170646,#170647,#170648,#170649,#170650,#170651,#170652,
#170653,#170654,#170655,#170656,#170657,#170658,#170659),.UNSPECIFIED.,
 .F.,.F.)
B_SPLINE_CURVE_WITH_KNOTS((6,1,1,1,1,1,1,1,1,1,1,1,1,1,1,1,1,1,1,1,1,1,
1,1,1,1,1,1,1,1,1,1,1,1,1,1,1,1,1,1,1,1,1,1,1,1,1,1,1,1,1,1,1,1,1,1,1,1,
1,1,1,1,1,1,1,1,1,1,1,1,1,1,1,1,1,1,1,1,1,1,1,1,1,1,1,1,1,1,1,1,1,1,1,1,
1,1,1,1,1,1,1,1,1,1,1,1,1,1,1,1,1,1,1,1,1,1,1,1,1,1,1,1,1,1,1,1,1,1,1,1,
1,1,1,1,1,1,1,1,1,1,1,1,1,1,1,1,1,1,1,1,1,1,1,1,1,1,1,1,1,1,1,1,1,1,1,1,
1,1,1,1,1,1,1,1,1,1,1,1,1,1,1,1,1,1,1,1,1,1,1,6),(-0.941429844438047,-0.940000000000001,
-0.935000000000001,-0.930000000000001,-0.925000000000001,-0.920000000000001,
-0.915000000000001,-0.910000000000001,-0.905000000000001,-0.900000000000001,
-0.895000000000001,-0.890000000000001,-0.885000000000001,-0.880000000000001,
-0.875000000000001,-0.870000000000001,-0.865000000000001,-0.860000000000001,
-0.855000000000001,-0.850000000000001,-0.845000000000001,-0.840000000000001,
-0.835000000000001,-0.830000000000001,-0.825000000000001,-0.820000000000001,
-0.815000000000001,-0.810000000000001,-0.805000000000001,-0.800000000000001,
-0.795000000000001,-0.790000000000001,-0.785000000000001,-0.780000000000001,
-0.775000000000001,-0.770000000000001,-0.765000000000001,-0.760000000000001,
-0.755000000000001,-0.750000000000001,-0.745000000000001,-0.740000000000001,
-0.735000000000001,-0.730000000000001,-0.725000000000001,-0.720000000000001,
-0.715000000000001,-0.710000000000001,-0.705000000000001,-0.700000000000001,
-0.695000000000001,-0.690000000000001,-0.685,-0.68,-0.675,-0.67,-0.665,
-0.66,-0.655,-0.65,-0.645,-0.64,-0.635,-0.63,-0.625,-0.62,-0.615,-0.61,
-0.605,-0.6,-0.595,-0.59,-0.585,-0.58,-0.575,-0.57,-0.565,-0.56,-0.555,
-0.55,-0.545,-0.54,-0.535,-0.53,-0.525,-0.52,-0.515,-0.51,-0.505,-0.5,-0.495,
-0.49,-0.485,-0.48,-0.475,-0.47,-0.465,-0.46,-0.455,-0.45,-0.445,-0.44,
-0.435,-0.43,-0.425,-0.42,-0.415,-0.41,-0.405,-0.4,-0.395,-0.39,-0.385,
-0.38,-0.375,-0.37,-0.365,-0.36,-0.355,-0.35,-0.345,-0.34,-0.335,-0.33,
-0.325,-0.32,-0.315,-0.31,-0.305,-0.3,-0.295,-0.29,-0.285,-0.28,-0.275,
-0.27,-0.265,-0.26,-0.255,-0.25,-0.245,-0.24,-0.235,-0.23,-0.225,-0.22,
-0.215,-0.21,-0.205,-0.2,-0.195,-0.19,-0.185,-0.18,-0.175,-0.17,-0.165,
-0.16,-0.155,-0.15,-0.145,-0.14,-0.135,-0.13,-0.125,-0.12,-0.115,-0.11,
-0.105,-0.1,-0.095,-0.09,-0.085,-0.08,-0.075,-0.07,-0.065,-0.06,-0.055,
-0.05,-0.045,-0.04,-0.035,-0.03,-0.025,-0.02,-0.015,-0.01,-0.005,0.),
 .UNSPECIFIED.)
CURVE()
GEOMETRIC_REPRESENTATION_ITEM()
RATIONAL_B_SPLINE_CURVE((1.,1.,1.,1.,1.,1.,1.,1.,1.,1.,1.,1.,1.,1.,1.,1.,
1.,1.,1.,1.,1.,1.,1.,1.,1.,1.,1.,1.,1.,1.,1.,1.,1.,1.,1.,1.,1.,1.,1.,1.,
1.,1.,1.,1.,1.,1.,1.,1.,1.,1.,1.,1.,1.,1.,1.,1.,1.,1.,1.,1.,1.,1.,1.,1.,
1.,1.,1.,1.,1.,1.,1.,1.,1.,1.,1.,1.,1.,1.,1.,1.,1.,1.,1.,1.,1.,1.,1.,1.,
1.,1.,1.,1.,1.,1.,1.,1.,1.,1.,1.,1.,1.,1.,1.,1.,1.,1.,1.,1.,1.,1.,1.,1.,
1.,1.,1.,1.,1.,1.,1.,1.,1.,1.,1.,1.,1.,1.,1.,1.,1.,1.,1.,1.,1.,1.,1.,1.,
1.,1.,1.,1.,1.,1.,1.,1.,1.,1.,1.,1.,1.,1.,1.,1.,1.,1.,1.,1.,1.,1.,1.,1.,
1.,1.,1.,1.,1.,1.,1.,1.,1.,1.,1.,1.,1.,1.,1.,1.,1.,1.,1.,1.,1.,1.,1.,1.,
1.,1.,1.,1.,1.,1.,1.,1.,1.,1.))
REPRESENTATION_ITEM('')
);
#681=(
BOUNDED_CURVE()
B_SPLINE_CURVE(5,(#171071,#171072,#171073,#171074,#171075,#171076,#171077,
#171078,#171079,#171080,#171081,#171082,#171083,#171084,#171085,#171086,
#171087,#171088,#171089,#171090,#171091,#171092,#171093,#171094,#171095,
#171096,#171097,#171098,#171099,#171100,#171101,#171102,#171103,#171104,
#171105,#171106,#171107,#171108,#171109,#171110,#171111,#171112,#171113,
#171114,#171115,#171116,#171117,#171118,#171119,#171120,#171121,#171122,
#171123,#171124,#171125,#171126,#171127,#171128,#171129,#171130,#171131,
#171132,#171133,#171134,#171135,#171136,#171137,#171138,#171139,#171140,
#171141,#171142,#171143,#171144,#171145,#171146,#171147,#171148,#171149,
#171150,#171151,#171152,#171153,#171154,#171155,#171156,#171157,#171158,
#171159,#171160,#171161,#171162,#171163,#171164,#171165,#171166,#171167,
#171168,#171169,#171170,#171171,#171172,#171173,#171174,#171175,#171176,
#171177,#171178,#171179,#171180,#171181,#171182,#171183,#171184,#171185,
#171186,#171187,#171188,#171189,#171190,#171191,#171192,#171193,#171194,
#171195,#171196,#171197,#171198,#171199,#171200,#171201,#171202,#171203,
#171204,#171205,#171206,#171207,#171208,#171209,#171210,#171211,#171212,
#171213,#171214,#171215,#171216,#171217,#171218,#171219,#171220,#171221,
#171222,#171223,#171224,#171225,#171226,#171227,#171228,#171229,#171230,
#171231,#171232,#171233,#171234,#171235,#171236,#171237,#171238,#171239,
#171240,#171241,#171242,#171243,#171244,#171245,#171246,#171247,#171248,
#171249,#171250,#171251,#171252,#171253,#171254,#171255,#171256,#171257,
#171258,#171259,#171260,#171261,#171262,#171263,#171264),.UNSPECIFIED.,
 .F.,.F.)
B_SPLINE_CURVE_WITH_KNOTS((6,1,1,1,1,1,1,1,1,1,1,1,1,1,1,1,1,1,1,1,1,1,
1,1,1,1,1,1,1,1,1,1,1,1,1,1,1,1,1,1,1,1,1,1,1,1,1,1,1,1,1,1,1,1,1,1,1,1,
1,1,1,1,1,1,1,1,1,1,1,1,1,1,1,1,1,1,1,1,1,1,1,1,1,1,1,1,1,1,1,1,1,1,1,1,
1,1,1,1,1,1,1,1,1,1,1,1,1,1,1,1,1,1,1,1,1,1,1,1,1,1,1,1,1,1,1,1,1,1,1,1,
1,1,1,1,1,1,1,1,1,1,1,1,1,1,1,1,1,1,1,1,1,1,1,1,1,1,1,1,1,1,1,1,1,1,1,1,
1,1,1,1,1,1,1,1,1,1,1,1,1,1,1,1,1,1,1,1,1,1,1,6),(0.,0.005,0.01,0.015,0.02,
0.025,0.03,0.035,0.04,0.045,0.05,0.055,0.06,0.065,0.07,0.075,0.08,0.085,
0.09,0.095,0.1,0.105,0.11,0.115,0.12,0.125,0.13,0.135,0.14,0.145,0.15,0.155,
0.16,0.165,0.17,0.175,0.18,0.185,0.19,0.195,0.2,0.205,0.21,0.215,0.22,0.225,
0.23,0.235,0.24,0.245,0.25,0.255,0.26,0.265,0.27,0.275,0.28,0.285,0.29,
0.295,0.3,0.305,0.31,0.315,0.32,0.325,0.33,0.335,0.34,0.345,0.35,0.355,
0.36,0.365,0.37,0.375,0.38,0.385,0.39,0.395,0.4,0.405,0.41,0.415,0.42,0.425,
0.43,0.435,0.44,0.445,0.45,0.455,0.46,0.465,0.47,0.475,0.48,0.485,0.49,
0.495,0.5,0.505,0.51,0.515,0.52,0.525,0.53,0.535,0.54,0.545,0.55,0.555,
0.56,0.565,0.57,0.575,0.58,0.585,0.59,0.595,0.6,0.605,0.61,0.615,0.62,0.625,
0.63,0.635,0.64,0.645,0.65,0.655,0.66,0.665,0.67,0.675,0.68,0.685,0.690000000000001,
0.695000000000001,0.700000000000001,0.705000000000001,0.710000000000001,
0.715000000000001,0.720000000000001,0.725000000000001,0.730000000000001,
0.735000000000001,0.740000000000001,0.745000000000001,0.750000000000001,
0.755000000000001,0.760000000000001,0.765000000000001,0.770000000000001,
0.775000000000001,0.780000000000001,0.785000000000001,0.790000000000001,
0.795000000000001,0.800000000000001,0.805000000000001,0.810000000000001,
0.815000000000001,0.820000000000001,0.825000000000001,0.830000000000001,
0.835000000000001,0.840000000000001,0.845000000000001,0.850000000000001,
0.855000000000001,0.860000000000001,0.865000000000001,0.870000000000001,
0.875000000000001,0.880000000000001,0.885000000000001,0.890000000000001,
0.895000000000001,0.900000000000001,0.905000000000001,0.910000000000001,
0.915000000000001,0.920000000000001,0.925000000000001,0.930000000000001,
0.935000000000001,0.940000000000001,0.94142984443807),.UNSPECIFIED.)
CURVE()
GEOMETRIC_REPRESENTATION_ITEM()
RATIONAL_B_SPLINE_CURVE((1.,1.,1.,1.,1.,1.,1.,1.,1.,1.,1.,1.,1.,1.,1.,1.,
1.,1.,1.,1.,1.,1.,1.,1.,1.,1.,1.,1.,1.,1.,1.,1.,1.,1.,1.,1.,1.,1.,1.,1.,
1.,1.,1.,1.,1.,1.,1.,1.,1.,1.,1.,1.,1.,1.,1.,1.,1.,1.,1.,1.,1.,1.,1.,1.,
1.,1.,1.,1.,1.,1.,1.,1.,1.,1.,1.,1.,1.,1.,1.,1.,1.,1.,1.,1.,1.,1.,1.,1.,
1.,1.,1.,1.,1.,1.,1.,1.,1.,1.,1.,1.,1.,1.,1.,1.,1.,1.,1.,1.,1.,1.,1.,1.,
1.,1.,1.,1.,1.,1.,1.,1.,1.,1.,1.,1.,1.,1.,1.,1.,1.,1.,1.,1.,1.,1.,1.,1.,
1.,1.,1.,1.,1.,1.,1.,1.,1.,1.,1.,1.,1.,1.,1.,1.,1.,1.,1.,1.,1.,1.,1.,1.,
1.,1.,1.,1.,1.,1.,1.,1.,1.,1.,1.,1.,1.,1.,1.,1.,1.,1.,1.,1.,1.,1.,1.,1.,
1.,1.,1.,1.,1.,1.,1.,1.,1.,1.))
REPRESENTATION_ITEM('')
);
#682=(
BOUNDED_CURVE()
B_SPLINE_CURVE(5,(#171267,#171268,#171269,#171270,#171271,#171272,#171273,
#171274,#171275,#171276,#171277,#171278,#171279,#171280,#171281,#171282,
#171283,#171284,#171285,#171286,#171287,#171288,#171289,#171290,#171291,
#171292,#171293,#171294,#171295,#171296,#171297,#171298,#171299,#171300,
#171301,#171302,#171303,#171304,#171305,#171306,#171307,#171308,#171309,
#171310,#171311,#171312,#171313,#171314,#171315,#171316,#171317,#171318,
#171319,#171320,#171321,#171322,#171323,#171324,#171325,#171326,#171327,
#171328,#171329,#171330,#171331,#171332,#171333,#171334,#171335,#171336,
#171337,#171338,#171339,#171340,#171341,#171342,#171343,#171344,#171345,
#171346,#171347,#171348,#171349,#171350,#171351,#171352,#171353,#171354,
#171355,#171356,#171357,#171358,#171359,#171360,#171361,#171362,#171363,
#171364,#171365,#171366,#171367,#171368,#171369,#171370,#171371,#171372,
#171373,#171374,#171375,#171376,#171377,#171378,#171379,#171380,#171381,
#171382,#171383,#171384,#171385,#171386,#171387,#171388,#171389,#171390,
#171391,#171392,#171393,#171394,#171395,#171396,#171397,#171398,#171399,
#171400,#171401,#171402,#171403,#171404,#171405,#171406,#171407,#171408,
#171409,#171410,#171411,#171412,#171413,#171414,#171415,#171416,#171417,
#171418,#171419,#171420,#171421,#171422,#171423,#171424,#171425,#171426,
#171427,#171428,#171429,#171430,#171431,#171432,#171433,#171434,#171435,
#171436,#171437,#171438,#171439,#171440,#171441,#171442,#171443,#171444,
#171445,#171446,#171447,#171448,#171449,#171450,#171451,#171452,#171453,
#171454,#171455,#171456,#171457,#171458,#171459,#171460),.UNSPECIFIED.,
 .F.,.F.)
B_SPLINE_CURVE_WITH_KNOTS((6,1,1,1,1,1,1,1,1,1,1,1,1,1,1,1,1,1,1,1,1,1,
1,1,1,1,1,1,1,1,1,1,1,1,1,1,1,1,1,1,1,1,1,1,1,1,1,1,1,1,1,1,1,1,1,1,1,1,
1,1,1,1,1,1,1,1,1,1,1,1,1,1,1,1,1,1,1,1,1,1,1,1,1,1,1,1,1,1,1,1,1,1,1,1,
1,1,1,1,1,1,1,1,1,1,1,1,1,1,1,1,1,1,1,1,1,1,1,1,1,1,1,1,1,1,1,1,1,1,1,1,
1,1,1,1,1,1,1,1,1,1,1,1,1,1,1,1,1,1,1,1,1,1,1,1,1,1,1,1,1,1,1,1,1,1,1,1,
1,1,1,1,1,1,1,1,1,1,1,1,1,1,1,1,1,1,1,1,1,1,1,6),(-0.941429844438063,-0.940000000000001,
-0.935000000000001,-0.930000000000001,-0.925000000000001,-0.920000000000001,
-0.915000000000001,-0.910000000000001,-0.905000000000001,-0.900000000000001,
-0.895000000000001,-0.890000000000001,-0.885000000000001,-0.880000000000001,
-0.875000000000001,-0.870000000000001,-0.865000000000001,-0.860000000000001,
-0.855000000000001,-0.850000000000001,-0.845000000000001,-0.840000000000001,
-0.835000000000001,-0.830000000000001,-0.825000000000001,-0.820000000000001,
-0.815000000000001,-0.810000000000001,-0.805000000000001,-0.800000000000001,
-0.795000000000001,-0.790000000000001,-0.785000000000001,-0.780000000000001,
-0.775000000000001,-0.770000000000001,-0.765000000000001,-0.760000000000001,
-0.755000000000001,-0.750000000000001,-0.745000000000001,-0.740000000000001,
-0.735000000000001,-0.730000000000001,-0.725000000000001,-0.720000000000001,
-0.715000000000001,-0.710000000000001,-0.705000000000001,-0.700000000000001,
-0.695000000000001,-0.690000000000001,-0.685,-0.68,-0.675,-0.67,-0.665,
-0.66,-0.655,-0.65,-0.645,-0.64,-0.635,-0.63,-0.625,-0.62,-0.615,-0.61,
-0.605,-0.6,-0.595,-0.59,-0.585,-0.58,-0.575,-0.57,-0.565,-0.56,-0.555,
-0.55,-0.545,-0.54,-0.535,-0.53,-0.525,-0.52,-0.515,-0.51,-0.505,-0.5,-0.495,
-0.49,-0.485,-0.48,-0.475,-0.47,-0.465,-0.46,-0.455,-0.45,-0.445,-0.44,
-0.435,-0.43,-0.425,-0.42,-0.415,-0.41,-0.405,-0.4,-0.395,-0.39,-0.385,
-0.38,-0.375,-0.37,-0.365,-0.36,-0.355,-0.35,-0.345,-0.34,-0.335,-0.33,
-0.325,-0.32,-0.315,-0.31,-0.305,-0.3,-0.295,-0.29,-0.285,-0.28,-0.275,
-0.27,-0.265,-0.26,-0.255,-0.25,-0.245,-0.24,-0.235,-0.23,-0.225,-0.22,
-0.215,-0.21,-0.205,-0.2,-0.195,-0.19,-0.185,-0.18,-0.175,-0.17,-0.165,
-0.16,-0.155,-0.15,-0.145,-0.14,-0.135,-0.13,-0.125,-0.12,-0.115,-0.11,
-0.105,-0.1,-0.095,-0.09,-0.085,-0.08,-0.075,-0.07,-0.065,-0.06,-0.055,
-0.05,-0.045,-0.04,-0.035,-0.03,-0.025,-0.02,-0.015,-0.01,-0.005,0.),
 .UNSPECIFIED.)
CURVE()
GEOMETRIC_REPRESENTATION_ITEM()
RATIONAL_B_SPLINE_CURVE((1.,1.,1.,1.,1.,1.,1.,1.,1.,1.,1.,1.,1.,1.,1.,1.,
1.,1.,1.,1.,1.,1.,1.,1.,1.,1.,1.,1.,1.,1.,1.,1.,1.,1.,1.,1.,1.,1.,1.,1.,
1.,1.,1.,1.,1.,1.,1.,1.,1.,1.,1.,1.,1.,1.,1.,1.,1.,1.,1.,1.,1.,1.,1.,1.,
1.,1.,1.,1.,1.,1.,1.,1.,1.,1.,1.,1.,1.,1.,1.,1.,1.,1.,1.,1.,1.,1.,1.,1.,
1.,1.,1.,1.,1.,1.,1.,1.,1.,1.,1.,1.,1.,1.,1.,1.,1.,1.,1.,1.,1.,1.,1.,1.,
1.,1.,1.,1.,1.,1.,1.,1.,1.,1.,1.,1.,1.,1.,1.,1.,1.,1.,1.,1.,1.,1.,1.,1.,
1.,1.,1.,1.,1.,1.,1.,1.,1.,1.,1.,1.,1.,1.,1.,1.,1.,1.,1.,1.,1.,1.,1.,1.,
1.,1.,1.,1.,1.,1.,1.,1.,1.,1.,1.,1.,1.,1.,1.,1.,1.,1.,1.,1.,1.,1.,1.,1.,
1.,1.,1.,1.,1.,1.,1.,1.,1.,1.))
REPRESENTATION_ITEM('')
);
#683=(
BOUNDED_CURVE()
B_SPLINE_CURVE(5,(#171872,#171873,#171874,#171875,#171876,#171877,#171878,
#171879,#171880,#171881,#171882,#171883,#171884,#171885,#171886,#171887,
#171888,#171889,#171890,#171891,#171892,#171893,#171894,#171895,#171896,
#171897,#171898,#171899,#171900,#171901,#171902,#171903,#171904,#171905,
#171906,#171907,#171908,#171909,#171910,#171911,#171912,#171913,#171914,
#171915,#171916,#171917,#171918,#171919,#171920,#171921,#171922,#171923,
#171924,#171925,#171926,#171927,#171928,#171929,#171930,#171931,#171932,
#171933,#171934,#171935,#171936,#171937,#171938,#171939,#171940,#171941,
#171942,#171943,#171944,#171945,#171946,#171947,#171948,#171949,#171950,
#171951,#171952,#171953,#171954,#171955,#171956,#171957,#171958,#171959,
#171960,#171961,#171962,#171963,#171964,#171965,#171966,#171967,#171968,
#171969,#171970,#171971,#171972,#171973,#171974,#171975,#171976,#171977,
#171978,#171979,#171980,#171981,#171982,#171983,#171984,#171985,#171986,
#171987,#171988,#171989,#171990,#171991,#171992,#171993,#171994,#171995,
#171996,#171997,#171998,#171999,#172000,#172001,#172002,#172003,#172004,
#172005,#172006,#172007,#172008,#172009,#172010,#172011,#172012,#172013,
#172014,#172015,#172016,#172017,#172018,#172019,#172020,#172021,#172022,
#172023,#172024,#172025,#172026,#172027,#172028,#172029,#172030,#172031,
#172032,#172033,#172034,#172035,#172036,#172037,#172038,#172039,#172040,
#172041,#172042,#172043,#172044,#172045,#172046,#172047,#172048,#172049,
#172050,#172051,#172052,#172053,#172054,#172055,#172056,#172057,#172058,
#172059,#172060,#172061,#172062,#172063,#172064,#172065),.UNSPECIFIED.,
 .F.,.F.)
B_SPLINE_CURVE_WITH_KNOTS((6,1,1,1,1,1,1,1,1,1,1,1,1,1,1,1,1,1,1,1,1,1,
1,1,1,1,1,1,1,1,1,1,1,1,1,1,1,1,1,1,1,1,1,1,1,1,1,1,1,1,1,1,1,1,1,1,1,1,
1,1,1,1,1,1,1,1,1,1,1,1,1,1,1,1,1,1,1,1,1,1,1,1,1,1,1,1,1,1,1,1,1,1,1,1,
1,1,1,1,1,1,1,1,1,1,1,1,1,1,1,1,1,1,1,1,1,1,1,1,1,1,1,1,1,1,1,1,1,1,1,1,
1,1,1,1,1,1,1,1,1,1,1,1,1,1,1,1,1,1,1,1,1,1,1,1,1,1,1,1,1,1,1,1,1,1,1,1,
1,1,1,1,1,1,1,1,1,1,1,1,1,1,1,1,1,1,1,1,1,1,1,6),(0.,0.005,0.01,0.015,0.02,
0.025,0.03,0.035,0.04,0.045,0.05,0.055,0.06,0.065,0.07,0.075,0.08,0.085,
0.09,0.095,0.1,0.105,0.11,0.115,0.12,0.125,0.13,0.135,0.14,0.145,0.15,0.155,
0.16,0.165,0.17,0.175,0.18,0.185,0.19,0.195,0.2,0.205,0.21,0.215,0.22,0.225,
0.23,0.235,0.24,0.245,0.25,0.255,0.26,0.265,0.27,0.275,0.28,0.285,0.29,
0.295,0.3,0.305,0.31,0.315,0.32,0.325,0.33,0.335,0.34,0.345,0.35,0.355,
0.36,0.365,0.37,0.375,0.38,0.385,0.39,0.395,0.4,0.405,0.41,0.415,0.42,0.425,
0.43,0.435,0.44,0.445,0.45,0.455,0.46,0.465,0.47,0.475,0.48,0.485,0.49,
0.495,0.5,0.505,0.51,0.515,0.52,0.525,0.53,0.535,0.54,0.545,0.55,0.555,
0.56,0.565,0.57,0.575,0.58,0.585,0.59,0.595,0.6,0.605,0.61,0.615,0.62,0.625,
0.63,0.635,0.64,0.645,0.65,0.655,0.66,0.665,0.67,0.675,0.68,0.685,0.690000000000001,
0.695000000000001,0.700000000000001,0.705000000000001,0.710000000000001,
0.715000000000001,0.720000000000001,0.725000000000001,0.730000000000001,
0.735000000000001,0.740000000000001,0.745000000000001,0.750000000000001,
0.755000000000001,0.760000000000001,0.765000000000001,0.770000000000001,
0.775000000000001,0.780000000000001,0.785000000000001,0.790000000000001,
0.795000000000001,0.800000000000001,0.805000000000001,0.810000000000001,
0.815000000000001,0.820000000000001,0.825000000000001,0.830000000000001,
0.835000000000001,0.840000000000001,0.845000000000001,0.850000000000001,
0.855000000000001,0.860000000000001,0.865000000000001,0.870000000000001,
0.875000000000001,0.880000000000001,0.885000000000001,0.890000000000001,
0.895000000000001,0.900000000000001,0.905000000000001,0.910000000000001,
0.915000000000001,0.920000000000001,0.925000000000001,0.930000000000001,
0.935000000000001,0.940000000000001,0.94142984443804),.UNSPECIFIED.)
CURVE()
GEOMETRIC_REPRESENTATION_ITEM()
RATIONAL_B_SPLINE_CURVE((1.,1.,1.,1.,1.,1.,1.,1.,1.,1.,1.,1.,1.,1.,1.,1.,
1.,1.,1.,1.,1.,1.,1.,1.,1.,1.,1.,1.,1.,1.,1.,1.,1.,1.,1.,1.,1.,1.,1.,1.,
1.,1.,1.,1.,1.,1.,1.,1.,1.,1.,1.,1.,1.,1.,1.,1.,1.,1.,1.,1.,1.,1.,1.,1.,
1.,1.,1.,1.,1.,1.,1.,1.,1.,1.,1.,1.,1.,1.,1.,1.,1.,1.,1.,1.,1.,1.,1.,1.,
1.,1.,1.,1.,1.,1.,1.,1.,1.,1.,1.,1.,1.,1.,1.,1.,1.,1.,1.,1.,1.,1.,1.,1.,
1.,1.,1.,1.,1.,1.,1.,1.,1.,1.,1.,1.,1.,1.,1.,1.,1.,1.,1.,1.,1.,1.,1.,1.,
1.,1.,1.,1.,1.,1.,1.,1.,1.,1.,1.,1.,1.,1.,1.,1.,1.,1.,1.,1.,1.,1.,1.,1.,
1.,1.,1.,1.,1.,1.,1.,1.,1.,1.,1.,1.,1.,1.,1.,1.,1.,1.,1.,1.,1.,1.,1.,1.,
1.,1.,1.,1.,1.,1.,1.,1.,1.,1.))
REPRESENTATION_ITEM('')
);
#684=(
BOUNDED_CURVE()
B_SPLINE_CURVE(5,(#172068,#172069,#172070,#172071,#172072,#172073,#172074,
#172075,#172076,#172077,#172078,#172079,#172080,#172081,#172082,#172083,
#172084,#172085,#172086,#172087,#172088,#172089,#172090,#172091,#172092,
#172093,#172094,#172095,#172096,#172097,#172098,#172099,#172100,#172101,
#172102,#172103,#172104,#172105,#172106,#172107,#172108,#172109,#172110,
#172111,#172112,#172113,#172114,#172115,#172116,#172117,#172118,#172119,
#172120,#172121,#172122,#172123,#172124,#172125,#172126,#172127,#172128,
#172129,#172130,#172131,#172132,#172133,#172134,#172135,#172136,#172137,
#172138,#172139,#172140,#172141,#172142,#172143,#172144,#172145,#172146,
#172147,#172148,#172149,#172150,#172151,#172152,#172153,#172154,#172155,
#172156,#172157,#172158,#172159,#172160,#172161,#172162,#172163,#172164,
#172165,#172166,#172167,#172168,#172169,#172170,#172171,#172172,#172173,
#172174,#172175,#172176,#172177,#172178,#172179,#172180,#172181,#172182,
#172183,#172184,#172185,#172186,#172187,#172188,#172189,#172190,#172191,
#172192,#172193,#172194,#172195,#172196,#172197,#172198,#172199,#172200,
#172201,#172202,#172203,#172204,#172205,#172206,#172207,#172208,#172209,
#172210,#172211,#172212,#172213,#172214,#172215,#172216,#172217,#172218,
#172219,#172220,#172221,#172222,#172223,#172224,#172225,#172226,#172227,
#172228,#172229,#172230,#172231,#172232,#172233,#172234,#172235,#172236,
#172237,#172238,#172239,#172240,#172241,#172242,#172243,#172244,#172245,
#172246,#172247,#172248,#172249,#172250,#172251,#172252,#172253,#172254,
#172255,#172256,#172257,#172258,#172259,#172260,#172261),.UNSPECIFIED.,
 .F.,.F.)
B_SPLINE_CURVE_WITH_KNOTS((6,1,1,1,1,1,1,1,1,1,1,1,1,1,1,1,1,1,1,1,1,1,
1,1,1,1,1,1,1,1,1,1,1,1,1,1,1,1,1,1,1,1,1,1,1,1,1,1,1,1,1,1,1,1,1,1,1,1,
1,1,1,1,1,1,1,1,1,1,1,1,1,1,1,1,1,1,1,1,1,1,1,1,1,1,1,1,1,1,1,1,1,1,1,1,
1,1,1,1,1,1,1,1,1,1,1,1,1,1,1,1,1,1,1,1,1,1,1,1,1,1,1,1,1,1,1,1,1,1,1,1,
1,1,1,1,1,1,1,1,1,1,1,1,1,1,1,1,1,1,1,1,1,1,1,1,1,1,1,1,1,1,1,1,1,1,1,1,
1,1,1,1,1,1,1,1,1,1,1,1,1,1,1,1,1,1,1,1,1,1,1,6),(-0.94142984443804,-0.940000000000001,
-0.935000000000001,-0.930000000000001,-0.925000000000001,-0.920000000000001,
-0.915000000000001,-0.910000000000001,-0.905000000000001,-0.900000000000001,
-0.895000000000001,-0.890000000000001,-0.885000000000001,-0.880000000000001,
-0.875000000000001,-0.870000000000001,-0.865000000000001,-0.860000000000001,
-0.855000000000001,-0.850000000000001,-0.845000000000001,-0.840000000000001,
-0.835000000000001,-0.830000000000001,-0.825000000000001,-0.820000000000001,
-0.815000000000001,-0.810000000000001,-0.805000000000001,-0.800000000000001,
-0.795000000000001,-0.790000000000001,-0.785000000000001,-0.780000000000001,
-0.775000000000001,-0.770000000000001,-0.765000000000001,-0.760000000000001,
-0.755000000000001,-0.750000000000001,-0.745000000000001,-0.740000000000001,
-0.735000000000001,-0.730000000000001,-0.725000000000001,-0.720000000000001,
-0.715000000000001,-0.710000000000001,-0.705000000000001,-0.700000000000001,
-0.695000000000001,-0.690000000000001,-0.685,-0.68,-0.675,-0.67,-0.665,
-0.66,-0.655,-0.65,-0.645,-0.64,-0.635,-0.63,-0.625,-0.62,-0.615,-0.61,
-0.605,-0.6,-0.595,-0.59,-0.585,-0.58,-0.575,-0.57,-0.565,-0.56,-0.555,
-0.55,-0.545,-0.54,-0.535,-0.53,-0.525,-0.52,-0.515,-0.51,-0.505,-0.5,-0.495,
-0.49,-0.485,-0.48,-0.475,-0.47,-0.465,-0.46,-0.455,-0.45,-0.445,-0.44,
-0.435,-0.43,-0.425,-0.42,-0.415,-0.41,-0.405,-0.4,-0.395,-0.39,-0.385,
-0.38,-0.375,-0.37,-0.365,-0.36,-0.355,-0.35,-0.345,-0.34,-0.335,-0.33,
-0.325,-0.32,-0.315,-0.31,-0.305,-0.3,-0.295,-0.29,-0.285,-0.28,-0.275,
-0.27,-0.265,-0.26,-0.255,-0.25,-0.245,-0.24,-0.235,-0.23,-0.225,-0.22,
-0.215,-0.21,-0.205,-0.2,-0.195,-0.19,-0.185,-0.18,-0.175,-0.17,-0.165,
-0.16,-0.155,-0.15,-0.145,-0.14,-0.135,-0.13,-0.125,-0.12,-0.115,-0.11,
-0.105,-0.1,-0.095,-0.09,-0.085,-0.08,-0.075,-0.07,-0.065,-0.06,-0.055,
-0.05,-0.045,-0.04,-0.035,-0.03,-0.025,-0.02,-0.015,-0.01,-0.005,0.),
 .UNSPECIFIED.)
CURVE()
GEOMETRIC_REPRESENTATION_ITEM()
RATIONAL_B_SPLINE_CURVE((1.,1.,1.,1.,1.,1.,1.,1.,1.,1.,1.,1.,1.,1.,1.,1.,
1.,1.,1.,1.,1.,1.,1.,1.,1.,1.,1.,1.,1.,1.,1.,1.,1.,1.,1.,1.,1.,1.,1.,1.,
1.,1.,1.,1.,1.,1.,1.,1.,1.,1.,1.,1.,1.,1.,1.,1.,1.,1.,1.,1.,1.,1.,1.,1.,
1.,1.,1.,1.,1.,1.,1.,1.,1.,1.,1.,1.,1.,1.,1.,1.,1.,1.,1.,1.,1.,1.,1.,1.,
1.,1.,1.,1.,1.,1.,1.,1.,1.,1.,1.,1.,1.,1.,1.,1.,1.,1.,1.,1.,1.,1.,1.,1.,
1.,1.,1.,1.,1.,1.,1.,1.,1.,1.,1.,1.,1.,1.,1.,1.,1.,1.,1.,1.,1.,1.,1.,1.,
1.,1.,1.,1.,1.,1.,1.,1.,1.,1.,1.,1.,1.,1.,1.,1.,1.,1.,1.,1.,1.,1.,1.,1.,
1.,1.,1.,1.,1.,1.,1.,1.,1.,1.,1.,1.,1.,1.,1.,1.,1.,1.,1.,1.,1.,1.,1.,1.,
1.,1.,1.,1.,1.,1.,1.,1.,1.,1.))
REPRESENTATION_ITEM('')
);
#685=(
BOUNDED_CURVE()
B_SPLINE_CURVE(5,(#172673,#172674,#172675,#172676,#172677,#172678,#172679,
#172680,#172681,#172682,#172683,#172684,#172685,#172686,#172687,#172688,
#172689,#172690,#172691,#172692,#172693,#172694,#172695,#172696,#172697,
#172698,#172699,#172700,#172701,#172702,#172703,#172704,#172705,#172706,
#172707,#172708,#172709,#172710,#172711,#172712,#172713,#172714,#172715,
#172716,#172717,#172718,#172719,#172720,#172721,#172722,#172723,#172724,
#172725,#172726,#172727,#172728,#172729,#172730,#172731,#172732,#172733,
#172734,#172735,#172736,#172737,#172738,#172739,#172740,#172741,#172742,
#172743,#172744,#172745,#172746,#172747,#172748,#172749,#172750,#172751,
#172752,#172753,#172754,#172755,#172756,#172757,#172758,#172759,#172760,
#172761,#172762,#172763,#172764,#172765,#172766,#172767,#172768,#172769,
#172770,#172771,#172772,#172773,#172774,#172775,#172776,#172777,#172778,
#172779,#172780,#172781,#172782,#172783,#172784,#172785,#172786,#172787,
#172788,#172789,#172790,#172791,#172792,#172793,#172794,#172795,#172796,
#172797,#172798,#172799,#172800,#172801,#172802,#172803,#172804,#172805,
#172806,#172807,#172808,#172809,#172810,#172811,#172812,#172813,#172814,
#172815,#172816,#172817,#172818,#172819,#172820,#172821,#172822,#172823,
#172824,#172825,#172826,#172827,#172828,#172829,#172830,#172831,#172832,
#172833,#172834,#172835,#172836,#172837,#172838,#172839,#172840,#172841,
#172842,#172843,#172844,#172845,#172846,#172847,#172848,#172849,#172850,
#172851,#172852,#172853,#172854,#172855,#172856,#172857,#172858,#172859,
#172860,#172861,#172862,#172863,#172864,#172865,#172866),.UNSPECIFIED.,
 .F.,.F.)
B_SPLINE_CURVE_WITH_KNOTS((6,1,1,1,1,1,1,1,1,1,1,1,1,1,1,1,1,1,1,1,1,1,
1,1,1,1,1,1,1,1,1,1,1,1,1,1,1,1,1,1,1,1,1,1,1,1,1,1,1,1,1,1,1,1,1,1,1,1,
1,1,1,1,1,1,1,1,1,1,1,1,1,1,1,1,1,1,1,1,1,1,1,1,1,1,1,1,1,1,1,1,1,1,1,1,
1,1,1,1,1,1,1,1,1,1,1,1,1,1,1,1,1,1,1,1,1,1,1,1,1,1,1,1,1,1,1,1,1,1,1,1,
1,1,1,1,1,1,1,1,1,1,1,1,1,1,1,1,1,1,1,1,1,1,1,1,1,1,1,1,1,1,1,1,1,1,1,1,
1,1,1,1,1,1,1,1,1,1,1,1,1,1,1,1,1,1,1,1,1,1,1,6),(0.,0.005,0.01,0.015,0.02,
0.025,0.03,0.035,0.04,0.045,0.05,0.055,0.06,0.065,0.07,0.075,0.08,0.085,
0.09,0.095,0.1,0.105,0.11,0.115,0.12,0.125,0.13,0.135,0.14,0.145,0.15,0.155,
0.16,0.165,0.17,0.175,0.18,0.185,0.19,0.195,0.2,0.205,0.21,0.215,0.22,0.225,
0.23,0.235,0.24,0.245,0.25,0.255,0.26,0.265,0.27,0.275,0.28,0.285,0.29,
0.295,0.3,0.305,0.31,0.315,0.32,0.325,0.33,0.335,0.34,0.345,0.35,0.355,
0.36,0.365,0.37,0.375,0.38,0.385,0.39,0.395,0.4,0.405,0.41,0.415,0.42,0.425,
0.43,0.435,0.44,0.445,0.45,0.455,0.46,0.465,0.47,0.475,0.48,0.485,0.49,
0.495,0.5,0.505,0.51,0.515,0.52,0.525,0.53,0.535,0.54,0.545,0.55,0.555,
0.56,0.565,0.57,0.575,0.58,0.585,0.59,0.595,0.6,0.605,0.61,0.615,0.62,0.625,
0.63,0.635,0.64,0.645,0.65,0.655,0.66,0.665,0.67,0.675,0.68,0.685,0.690000000000001,
0.695000000000001,0.700000000000001,0.705000000000001,0.710000000000001,
0.715000000000001,0.720000000000001,0.725000000000001,0.730000000000001,
0.735000000000001,0.740000000000001,0.745000000000001,0.750000000000001,
0.755000000000001,0.760000000000001,0.765000000000001,0.770000000000001,
0.775000000000001,0.780000000000001,0.785000000000001,0.790000000000001,
0.795000000000001,0.800000000000001,0.805000000000001,0.810000000000001,
0.815000000000001,0.820000000000001,0.825000000000001,0.830000000000001,
0.835000000000001,0.840000000000001,0.845000000000001,0.850000000000001,
0.855000000000001,0.860000000000001,0.865000000000001,0.870000000000001,
0.875000000000001,0.880000000000001,0.885000000000001,0.890000000000001,
0.895000000000001,0.900000000000001,0.905000000000001,0.910000000000001,
0.915000000000001,0.920000000000001,0.925000000000001,0.930000000000001,
0.935000000000001,0.940000000000001,0.94142984443804),.UNSPECIFIED.)
CURVE()
GEOMETRIC_REPRESENTATION_ITEM()
RATIONAL_B_SPLINE_CURVE((1.,1.,1.,1.,1.,1.,1.,1.,1.,1.,1.,1.,1.,1.,1.,1.,
1.,1.,1.,1.,1.,1.,1.,1.,1.,1.,1.,1.,1.,1.,1.,1.,1.,1.,1.,1.,1.,1.,1.,1.,
1.,1.,1.,1.,1.,1.,1.,1.,1.,1.,1.,1.,1.,1.,1.,1.,1.,1.,1.,1.,1.,1.,1.,1.,
1.,1.,1.,1.,1.,1.,1.,1.,1.,1.,1.,1.,1.,1.,1.,1.,1.,1.,1.,1.,1.,1.,1.,1.,
1.,1.,1.,1.,1.,1.,1.,1.,1.,1.,1.,1.,1.,1.,1.,1.,1.,1.,1.,1.,1.,1.,1.,1.,
1.,1.,1.,1.,1.,1.,1.,1.,1.,1.,1.,1.,1.,1.,1.,1.,1.,1.,1.,1.,1.,1.,1.,1.,
1.,1.,1.,1.,1.,1.,1.,1.,1.,1.,1.,1.,1.,1.,1.,1.,1.,1.,1.,1.,1.,1.,1.,1.,
1.,1.,1.,1.,1.,1.,1.,1.,1.,1.,1.,1.,1.,1.,1.,1.,1.,1.,1.,1.,1.,1.,1.,1.,
1.,1.,1.,1.,1.,1.,1.,1.,1.,1.))
REPRESENTATION_ITEM('')
);
#686=(
BOUNDED_CURVE()
B_SPLINE_CURVE(5,(#172869,#172870,#172871,#172872,#172873,#172874,#172875,
#172876,#172877,#172878,#172879,#172880,#172881,#172882,#172883,#172884,
#172885,#172886,#172887,#172888,#172889,#172890,#172891,#172892,#172893,
#172894,#172895,#172896,#172897,#172898,#172899,#172900,#172901,#172902,
#172903,#172904,#172905,#172906,#172907,#172908,#172909,#172910,#172911,
#172912,#172913,#172914,#172915,#172916,#172917,#172918,#172919,#172920,
#172921,#172922,#172923,#172924,#172925,#172926,#172927,#172928,#172929,
#172930,#172931,#172932,#172933,#172934,#172935,#172936,#172937,#172938,
#172939,#172940,#172941,#172942,#172943,#172944,#172945,#172946,#172947,
#172948,#172949,#172950,#172951,#172952,#172953,#172954,#172955,#172956,
#172957,#172958,#172959,#172960,#172961,#172962,#172963,#172964,#172965,
#172966,#172967,#172968,#172969,#172970,#172971,#172972,#172973,#172974,
#172975,#172976,#172977,#172978,#172979,#172980,#172981,#172982,#172983,
#172984,#172985,#172986,#172987,#172988,#172989,#172990,#172991,#172992,
#172993,#172994,#172995,#172996,#172997,#172998,#172999,#173000,#173001,
#173002,#173003,#173004,#173005,#173006,#173007,#173008,#173009,#173010,
#173011,#173012,#173013,#173014,#173015,#173016,#173017,#173018,#173019,
#173020,#173021,#173022,#173023,#173024,#173025,#173026,#173027,#173028,
#173029,#173030,#173031,#173032,#173033,#173034,#173035,#173036,#173037,
#173038,#173039,#173040,#173041,#173042,#173043,#173044,#173045,#173046,
#173047,#173048,#173049,#173050,#173051,#173052,#173053,#173054,#173055,
#173056,#173057,#173058,#173059,#173060,#173061,#173062),.UNSPECIFIED.,
 .F.,.F.)
B_SPLINE_CURVE_WITH_KNOTS((6,1,1,1,1,1,1,1,1,1,1,1,1,1,1,1,1,1,1,1,1,1,
1,1,1,1,1,1,1,1,1,1,1,1,1,1,1,1,1,1,1,1,1,1,1,1,1,1,1,1,1,1,1,1,1,1,1,1,
1,1,1,1,1,1,1,1,1,1,1,1,1,1,1,1,1,1,1,1,1,1,1,1,1,1,1,1,1,1,1,1,1,1,1,1,
1,1,1,1,1,1,1,1,1,1,1,1,1,1,1,1,1,1,1,1,1,1,1,1,1,1,1,1,1,1,1,1,1,1,1,1,
1,1,1,1,1,1,1,1,1,1,1,1,1,1,1,1,1,1,1,1,1,1,1,1,1,1,1,1,1,1,1,1,1,1,1,1,
1,1,1,1,1,1,1,1,1,1,1,1,1,1,1,1,1,1,1,1,1,1,1,6),(-0.941429844438057,-0.940000000000001,
-0.935000000000001,-0.930000000000001,-0.925000000000001,-0.920000000000001,
-0.915000000000001,-0.910000000000001,-0.905000000000001,-0.900000000000001,
-0.895000000000001,-0.890000000000001,-0.885000000000001,-0.880000000000001,
-0.875000000000001,-0.870000000000001,-0.865000000000001,-0.860000000000001,
-0.855000000000001,-0.850000000000001,-0.845000000000001,-0.840000000000001,
-0.835000000000001,-0.830000000000001,-0.825000000000001,-0.820000000000001,
-0.815000000000001,-0.810000000000001,-0.805000000000001,-0.800000000000001,
-0.795000000000001,-0.790000000000001,-0.785000000000001,-0.780000000000001,
-0.775000000000001,-0.770000000000001,-0.765000000000001,-0.760000000000001,
-0.755000000000001,-0.750000000000001,-0.745000000000001,-0.740000000000001,
-0.735000000000001,-0.730000000000001,-0.725000000000001,-0.720000000000001,
-0.715000000000001,-0.710000000000001,-0.705000000000001,-0.700000000000001,
-0.695000000000001,-0.690000000000001,-0.685,-0.68,-0.675,-0.67,-0.665,
-0.66,-0.655,-0.65,-0.645,-0.64,-0.635,-0.63,-0.625,-0.62,-0.615,-0.61,
-0.605,-0.6,-0.595,-0.59,-0.585,-0.58,-0.575,-0.57,-0.565,-0.56,-0.555,
-0.55,-0.545,-0.54,-0.535,-0.53,-0.525,-0.52,-0.515,-0.51,-0.505,-0.5,-0.495,
-0.49,-0.485,-0.48,-0.475,-0.47,-0.465,-0.46,-0.455,-0.45,-0.445,-0.44,
-0.435,-0.43,-0.425,-0.42,-0.415,-0.41,-0.405,-0.4,-0.395,-0.39,-0.385,
-0.38,-0.375,-0.37,-0.365,-0.36,-0.355,-0.35,-0.345,-0.34,-0.335,-0.33,
-0.325,-0.32,-0.315,-0.31,-0.305,-0.3,-0.295,-0.29,-0.285,-0.28,-0.275,
-0.27,-0.265,-0.26,-0.255,-0.25,-0.245,-0.24,-0.235,-0.23,-0.225,-0.22,
-0.215,-0.21,-0.205,-0.2,-0.195,-0.19,-0.185,-0.18,-0.175,-0.17,-0.165,
-0.16,-0.155,-0.15,-0.145,-0.14,-0.135,-0.13,-0.125,-0.12,-0.115,-0.11,
-0.105,-0.1,-0.095,-0.09,-0.085,-0.08,-0.075,-0.07,-0.065,-0.06,-0.055,
-0.05,-0.045,-0.04,-0.035,-0.03,-0.025,-0.02,-0.015,-0.01,-0.005,0.),
 .UNSPECIFIED.)
CURVE()
GEOMETRIC_REPRESENTATION_ITEM()
RATIONAL_B_SPLINE_CURVE((1.,1.,1.,1.,1.,1.,1.,1.,1.,1.,1.,1.,1.,1.,1.,1.,
1.,1.,1.,1.,1.,1.,1.,1.,1.,1.,1.,1.,1.,1.,1.,1.,1.,1.,1.,1.,1.,1.,1.,1.,
1.,1.,1.,1.,1.,1.,1.,1.,1.,1.,1.,1.,1.,1.,1.,1.,1.,1.,1.,1.,1.,1.,1.,1.,
1.,1.,1.,1.,1.,1.,1.,1.,1.,1.,1.,1.,1.,1.,1.,1.,1.,1.,1.,1.,1.,1.,1.,1.,
1.,1.,1.,1.,1.,1.,1.,1.,1.,1.,1.,1.,1.,1.,1.,1.,1.,1.,1.,1.,1.,1.,1.,1.,
1.,1.,1.,1.,1.,1.,1.,1.,1.,1.,1.,1.,1.,1.,1.,1.,1.,1.,1.,1.,1.,1.,1.,1.,
1.,1.,1.,1.,1.,1.,1.,1.,1.,1.,1.,1.,1.,1.,1.,1.,1.,1.,1.,1.,1.,1.,1.,1.,
1.,1.,1.,1.,1.,1.,1.,1.,1.,1.,1.,1.,1.,1.,1.,1.,1.,1.,1.,1.,1.,1.,1.,1.,
1.,1.,1.,1.,1.,1.,1.,1.,1.,1.))
REPRESENTATION_ITEM('')
);
#687=(
BOUNDED_CURVE()
B_SPLINE_CURVE(5,(#173738,#173739,#173740,#173741,#173742,#173743,#173744,
#173745,#173746,#173747,#173748,#173749,#173750,#173751,#173752,#173753,
#173754,#173755,#173756,#173757,#173758,#173759,#173760,#173761,#173762,
#173763,#173764,#173765,#173766,#173767,#173768,#173769,#173770,#173771,
#173772,#173773,#173774,#173775,#173776,#173777,#173778,#173779,#173780,
#173781,#173782,#173783,#173784,#173785,#173786,#173787,#173788,#173789,
#173790,#173791,#173792,#173793,#173794,#173795,#173796,#173797,#173798,
#173799,#173800,#173801,#173802,#173803,#173804,#173805,#173806,#173807,
#173808,#173809,#173810,#173811,#173812,#173813,#173814,#173815,#173816,
#173817,#173818,#173819,#173820,#173821,#173822,#173823,#173824,#173825,
#173826,#173827,#173828,#173829,#173830,#173831,#173832,#173833,#173834,
#173835,#173836,#173837,#173838,#173839,#173840,#173841,#173842,#173843,
#173844,#173845,#173846,#173847,#173848,#173849,#173850,#173851,#173852,
#173853,#173854,#173855,#173856,#173857,#173858,#173859,#173860,#173861,
#173862,#173863,#173864,#173865,#173866,#173867,#173868,#173869,#173870,
#173871,#173872,#173873,#173874,#173875,#173876,#173877,#173878,#173879,
#173880,#173881,#173882,#173883,#173884,#173885,#173886,#173887,#173888,
#173889,#173890,#173891,#173892,#173893,#173894,#173895,#173896,#173897,
#173898,#173899,#173900,#173901,#173902,#173903,#173904,#173905,#173906,
#173907,#173908,#173909,#173910,#173911,#173912,#173913,#173914,#173915,
#173916,#173917,#173918,#173919,#173920,#173921,#173922,#173923,#173924,
#173925,#173926,#173927,#173928,#173929,#173930,#173931),.UNSPECIFIED.,
 .F.,.F.)
B_SPLINE_CURVE_WITH_KNOTS((6,1,1,1,1,1,1,1,1,1,1,1,1,1,1,1,1,1,1,1,1,1,
1,1,1,1,1,1,1,1,1,1,1,1,1,1,1,1,1,1,1,1,1,1,1,1,1,1,1,1,1,1,1,1,1,1,1,1,
1,1,1,1,1,1,1,1,1,1,1,1,1,1,1,1,1,1,1,1,1,1,1,1,1,1,1,1,1,1,1,1,1,1,1,1,
1,1,1,1,1,1,1,1,1,1,1,1,1,1,1,1,1,1,1,1,1,1,1,1,1,1,1,1,1,1,1,1,1,1,1,1,
1,1,1,1,1,1,1,1,1,1,1,1,1,1,1,1,1,1,1,1,1,1,1,1,1,1,1,1,1,1,1,1,1,1,1,1,
1,1,1,1,1,1,1,1,1,1,1,1,1,1,1,1,1,1,1,1,1,1,1,6),(0.,0.005,0.01,0.015,0.02,
0.025,0.03,0.035,0.04,0.045,0.05,0.055,0.06,0.065,0.07,0.075,0.08,0.085,
0.09,0.095,0.1,0.105,0.11,0.115,0.12,0.125,0.13,0.135,0.14,0.145,0.15,0.155,
0.16,0.165,0.17,0.175,0.18,0.185,0.19,0.195,0.2,0.205,0.21,0.215,0.22,0.225,
0.23,0.235,0.24,0.245,0.25,0.255,0.26,0.265,0.27,0.275,0.28,0.285,0.29,
0.295,0.3,0.305,0.31,0.315,0.32,0.325,0.33,0.335,0.34,0.345,0.35,0.355,
0.36,0.365,0.37,0.375,0.38,0.385,0.39,0.395,0.4,0.405,0.41,0.415,0.42,0.425,
0.43,0.435,0.44,0.445,0.45,0.455,0.46,0.465,0.47,0.475,0.48,0.485,0.49,
0.495,0.5,0.505,0.51,0.515,0.52,0.525,0.53,0.535,0.54,0.545,0.55,0.555,
0.56,0.565,0.57,0.575,0.58,0.585,0.59,0.595,0.6,0.605,0.61,0.615,0.62,0.625,
0.63,0.635,0.64,0.645,0.65,0.655,0.66,0.665,0.67,0.675,0.68,0.685,0.690000000000001,
0.695000000000001,0.700000000000001,0.705000000000001,0.710000000000001,
0.715000000000001,0.720000000000001,0.725000000000001,0.730000000000001,
0.735000000000001,0.740000000000001,0.745000000000001,0.750000000000001,
0.755000000000001,0.760000000000001,0.765000000000001,0.770000000000001,
0.775000000000001,0.780000000000001,0.785000000000001,0.790000000000001,
0.795000000000001,0.800000000000001,0.805000000000001,0.810000000000001,
0.815000000000001,0.820000000000001,0.825000000000001,0.830000000000001,
0.835000000000001,0.840000000000001,0.845000000000001,0.850000000000001,
0.855000000000001,0.860000000000001,0.865000000000001,0.870000000000001,
0.875000000000001,0.880000000000001,0.885000000000001,0.890000000000001,
0.895000000000001,0.900000000000001,0.905000000000001,0.910000000000001,
0.915000000000001,0.920000000000001,0.925000000000001,0.930000000000001,
0.935000000000001,0.940000000000001,0.941429844431361),.UNSPECIFIED.)
CURVE()
GEOMETRIC_REPRESENTATION_ITEM()
RATIONAL_B_SPLINE_CURVE((1.,1.,1.,1.,1.,1.,1.,1.,1.,1.,1.,1.,1.,1.,1.,1.,
1.,1.,1.,1.,1.,1.,1.,1.,1.,1.,1.,1.,1.,1.,1.,1.,1.,1.,1.,1.,1.,1.,1.,1.,
1.,1.,1.,1.,1.,1.,1.,1.,1.,1.,1.,1.,1.,1.,1.,1.,1.,1.,1.,1.,1.,1.,1.,1.,
1.,1.,1.,1.,1.,1.,1.,1.,1.,1.,1.,1.,1.,1.,1.,1.,1.,1.,1.,1.,1.,1.,1.,1.,
1.,1.,1.,1.,1.,1.,1.,1.,1.,1.,1.,1.,1.,1.,1.,1.,1.,1.,1.,1.,1.,1.,1.,1.,
1.,1.,1.,1.,1.,1.,1.,1.,1.,1.,1.,1.,1.,1.,1.,1.,1.,1.,1.,1.,1.,1.,1.,1.,
1.,1.,1.,1.,1.,1.,1.,1.,1.,1.,1.,1.,1.,1.,1.,1.,1.,1.,1.,1.,1.,1.,1.,1.,
1.,1.,1.,1.,1.,1.,1.,1.,1.,1.,1.,1.,1.,1.,1.,1.,1.,1.,1.,1.,1.,1.,1.,1.,
1.,1.,1.,1.,1.,1.,1.,1.,1.,1.))
REPRESENTATION_ITEM('')
);
#688=(
BOUNDED_CURVE()
B_SPLINE_CURVE(5,(#173932,#173933,#173934,#173935,#173936,#173937,#173938,
#173939,#173940,#173941,#173942,#173943,#173944,#173945,#173946,#173947,
#173948,#173949,#173950,#173951,#173952,#173953,#173954,#173955,#173956,
#173957,#173958,#173959,#173960,#173961,#173962,#173963,#173964,#173965,
#173966,#173967,#173968,#173969,#173970,#173971,#173972,#173973,#173974,
#173975,#173976,#173977,#173978,#173979,#173980,#173981,#173982,#173983,
#173984,#173985,#173986,#173987,#173988,#173989,#173990,#173991,#173992,
#173993,#173994,#173995,#173996,#173997,#173998,#173999,#174000,#174001,
#174002,#174003,#174004,#174005,#174006,#174007,#174008,#174009,#174010,
#174011,#174012,#174013,#174014,#174015,#174016,#174017,#174018,#174019,
#174020,#174021,#174022,#174023,#174024,#174025,#174026,#174027,#174028,
#174029,#174030,#174031,#174032,#174033,#174034,#174035,#174036,#174037,
#174038,#174039,#174040,#174041,#174042,#174043,#174044,#174045,#174046,
#174047,#174048,#174049,#174050,#174051,#174052,#174053,#174054,#174055,
#174056,#174057,#174058,#174059,#174060,#174061,#174062,#174063,#174064,
#174065,#174066,#174067,#174068,#174069,#174070,#174071,#174072,#174073,
#174074,#174075,#174076,#174077,#174078,#174079,#174080,#174081,#174082,
#174083,#174084,#174085,#174086,#174087,#174088,#174089,#174090,#174091,
#174092,#174093,#174094,#174095,#174096,#174097,#174098,#174099,#174100,
#174101,#174102,#174103,#174104,#174105,#174106,#174107,#174108,#174109,
#174110,#174111,#174112,#174113,#174114,#174115,#174116,#174117,#174118,
#174119,#174120,#174121,#174122,#174123,#174124,#174125),.UNSPECIFIED.,
 .F.,.F.)
B_SPLINE_CURVE_WITH_KNOTS((6,1,1,1,1,1,1,1,1,1,1,1,1,1,1,1,1,1,1,1,1,1,
1,1,1,1,1,1,1,1,1,1,1,1,1,1,1,1,1,1,1,1,1,1,1,1,1,1,1,1,1,1,1,1,1,1,1,1,
1,1,1,1,1,1,1,1,1,1,1,1,1,1,1,1,1,1,1,1,1,1,1,1,1,1,1,1,1,1,1,1,1,1,1,1,
1,1,1,1,1,1,1,1,1,1,1,1,1,1,1,1,1,1,1,1,1,1,1,1,1,1,1,1,1,1,1,1,1,1,1,1,
1,1,1,1,1,1,1,1,1,1,1,1,1,1,1,1,1,1,1,1,1,1,1,1,1,1,1,1,1,1,1,1,1,1,1,1,
1,1,1,1,1,1,1,1,1,1,1,1,1,1,1,1,1,1,1,1,1,1,1,6),(-0.941429844431347,-0.940000000000001,
-0.935000000000001,-0.930000000000001,-0.925000000000001,-0.920000000000001,
-0.915000000000001,-0.910000000000001,-0.905000000000001,-0.900000000000001,
-0.895000000000001,-0.890000000000001,-0.885000000000001,-0.880000000000001,
-0.875000000000001,-0.870000000000001,-0.865000000000001,-0.860000000000001,
-0.855000000000001,-0.850000000000001,-0.845000000000001,-0.840000000000001,
-0.835000000000001,-0.830000000000001,-0.825000000000001,-0.820000000000001,
-0.815000000000001,-0.810000000000001,-0.805000000000001,-0.800000000000001,
-0.795000000000001,-0.790000000000001,-0.785000000000001,-0.780000000000001,
-0.775000000000001,-0.770000000000001,-0.765000000000001,-0.760000000000001,
-0.755000000000001,-0.750000000000001,-0.745000000000001,-0.740000000000001,
-0.735000000000001,-0.730000000000001,-0.725000000000001,-0.720000000000001,
-0.715000000000001,-0.710000000000001,-0.705000000000001,-0.700000000000001,
-0.695000000000001,-0.690000000000001,-0.685,-0.68,-0.675,-0.67,-0.665,
-0.66,-0.655,-0.65,-0.645,-0.64,-0.635,-0.63,-0.625,-0.62,-0.615,-0.61,
-0.605,-0.6,-0.595,-0.59,-0.585,-0.58,-0.575,-0.57,-0.565,-0.56,-0.555,
-0.55,-0.545,-0.54,-0.535,-0.53,-0.525,-0.52,-0.515,-0.51,-0.505,-0.5,-0.495,
-0.49,-0.485,-0.48,-0.475,-0.47,-0.465,-0.46,-0.455,-0.45,-0.445,-0.44,
-0.435,-0.43,-0.425,-0.42,-0.415,-0.41,-0.405,-0.4,-0.395,-0.39,-0.385,
-0.38,-0.375,-0.37,-0.365,-0.36,-0.355,-0.35,-0.345,-0.34,-0.335,-0.33,
-0.325,-0.32,-0.315,-0.31,-0.305,-0.3,-0.295,-0.29,-0.285,-0.28,-0.275,
-0.27,-0.265,-0.26,-0.255,-0.25,-0.245,-0.24,-0.235,-0.23,-0.225,-0.22,
-0.215,-0.21,-0.205,-0.2,-0.195,-0.19,-0.185,-0.18,-0.175,-0.17,-0.165,
-0.16,-0.155,-0.15,-0.145,-0.14,-0.135,-0.13,-0.125,-0.12,-0.115,-0.11,
-0.105,-0.1,-0.095,-0.09,-0.085,-0.08,-0.075,-0.07,-0.065,-0.06,-0.055,
-0.05,-0.045,-0.04,-0.035,-0.03,-0.025,-0.02,-0.015,-0.01,-0.005,0.),
 .UNSPECIFIED.)
CURVE()
GEOMETRIC_REPRESENTATION_ITEM()
RATIONAL_B_SPLINE_CURVE((1.,1.,1.,1.,1.,1.,1.,1.,1.,1.,1.,1.,1.,1.,1.,1.,
1.,1.,1.,1.,1.,1.,1.,1.,1.,1.,1.,1.,1.,1.,1.,1.,1.,1.,1.,1.,1.,1.,1.,1.,
1.,1.,1.,1.,1.,1.,1.,1.,1.,1.,1.,1.,1.,1.,1.,1.,1.,1.,1.,1.,1.,1.,1.,1.,
1.,1.,1.,1.,1.,1.,1.,1.,1.,1.,1.,1.,1.,1.,1.,1.,1.,1.,1.,1.,1.,1.,1.,1.,
1.,1.,1.,1.,1.,1.,1.,1.,1.,1.,1.,1.,1.,1.,1.,1.,1.,1.,1.,1.,1.,1.,1.,1.,
1.,1.,1.,1.,1.,1.,1.,1.,1.,1.,1.,1.,1.,1.,1.,1.,1.,1.,1.,1.,1.,1.,1.,1.,
1.,1.,1.,1.,1.,1.,1.,1.,1.,1.,1.,1.,1.,1.,1.,1.,1.,1.,1.,1.,1.,1.,1.,1.,
1.,1.,1.,1.,1.,1.,1.,1.,1.,1.,1.,1.,1.,1.,1.,1.,1.,1.,1.,1.,1.,1.,1.,1.,
1.,1.,1.,1.,1.,1.,1.,1.,1.,1.))
REPRESENTATION_ITEM('')
);
#689=(
BOUNDED_CURVE()
B_SPLINE_CURVE(5,(#174585,#174586,#174587,#174588,#174589,#174590,#174591,
#174592,#174593,#174594,#174595,#174596,#174597,#174598,#174599,#174600,
#174601,#174602,#174603,#174604,#174605,#174606,#174607,#174608,#174609,
#174610,#174611,#174612,#174613,#174614,#174615,#174616,#174617,#174618,
#174619,#174620,#174621,#174622,#174623,#174624,#174625,#174626,#174627,
#174628,#174629,#174630,#174631,#174632,#174633,#174634,#174635,#174636,
#174637,#174638,#174639,#174640,#174641,#174642,#174643,#174644,#174645,
#174646,#174647,#174648,#174649,#174650,#174651,#174652,#174653,#174654,
#174655,#174656,#174657,#174658,#174659,#174660,#174661,#174662,#174663,
#174664,#174665,#174666,#174667,#174668,#174669,#174670,#174671,#174672,
#174673,#174674,#174675,#174676,#174677,#174678,#174679,#174680,#174681,
#174682,#174683,#174684,#174685,#174686,#174687,#174688,#174689,#174690,
#174691,#174692,#174693,#174694,#174695,#174696,#174697,#174698,#174699,
#174700,#174701,#174702,#174703,#174704,#174705,#174706,#174707,#174708,
#174709,#174710,#174711,#174712,#174713,#174714,#174715,#174716,#174717,
#174718,#174719,#174720,#174721,#174722,#174723,#174724,#174725,#174726,
#174727,#174728,#174729,#174730,#174731,#174732,#174733,#174734,#174735,
#174736,#174737,#174738,#174739,#174740,#174741,#174742,#174743,#174744,
#174745,#174746,#174747,#174748,#174749,#174750,#174751,#174752,#174753,
#174754,#174755,#174756,#174757,#174758,#174759,#174760,#174761,#174762,
#174763,#174764,#174765,#174766,#174767,#174768,#174769,#174770,#174771,
#174772,#174773,#174774,#174775,#174776,#174777,#174778),.UNSPECIFIED.,
 .F.,.F.)
B_SPLINE_CURVE_WITH_KNOTS((6,1,1,1,1,1,1,1,1,1,1,1,1,1,1,1,1,1,1,1,1,1,
1,1,1,1,1,1,1,1,1,1,1,1,1,1,1,1,1,1,1,1,1,1,1,1,1,1,1,1,1,1,1,1,1,1,1,1,
1,1,1,1,1,1,1,1,1,1,1,1,1,1,1,1,1,1,1,1,1,1,1,1,1,1,1,1,1,1,1,1,1,1,1,1,
1,1,1,1,1,1,1,1,1,1,1,1,1,1,1,1,1,1,1,1,1,1,1,1,1,1,1,1,1,1,1,1,1,1,1,1,
1,1,1,1,1,1,1,1,1,1,1,1,1,1,1,1,1,1,1,1,1,1,1,1,1,1,1,1,1,1,1,1,1,1,1,1,
1,1,1,1,1,1,1,1,1,1,1,1,1,1,1,1,1,1,1,1,1,1,1,6),(0.,0.005,0.01,0.015,0.02,
0.025,0.03,0.035,0.04,0.045,0.05,0.055,0.06,0.065,0.07,0.075,0.08,0.085,
0.09,0.095,0.1,0.105,0.11,0.115,0.12,0.125,0.13,0.135,0.14,0.145,0.15,0.155,
0.16,0.165,0.17,0.175,0.18,0.185,0.19,0.195,0.2,0.205,0.21,0.215,0.22,0.225,
0.23,0.235,0.24,0.245,0.25,0.255,0.26,0.265,0.27,0.275,0.28,0.285,0.29,
0.295,0.3,0.305,0.31,0.315,0.32,0.325,0.33,0.335,0.34,0.345,0.35,0.355,
0.36,0.365,0.37,0.375,0.38,0.385,0.39,0.395,0.4,0.405,0.41,0.415,0.42,0.425,
0.43,0.435,0.44,0.445,0.45,0.455,0.46,0.465,0.47,0.475,0.48,0.485,0.49,
0.495,0.5,0.505,0.51,0.515,0.52,0.525,0.53,0.535,0.54,0.545,0.55,0.555,
0.56,0.565,0.57,0.575,0.58,0.585,0.59,0.595,0.6,0.605,0.61,0.615,0.62,0.625,
0.63,0.635,0.64,0.645,0.65,0.655,0.66,0.665,0.67,0.675,0.68,0.685,0.690000000000001,
0.695000000000001,0.700000000000001,0.705000000000001,0.710000000000001,
0.715000000000001,0.720000000000001,0.725000000000001,0.730000000000001,
0.735000000000001,0.740000000000001,0.745000000000001,0.750000000000001,
0.755000000000001,0.760000000000001,0.765000000000001,0.770000000000001,
0.775000000000001,0.780000000000001,0.785000000000001,0.790000000000001,
0.795000000000001,0.800000000000001,0.805000000000001,0.810000000000001,
0.815000000000001,0.820000000000001,0.825000000000001,0.830000000000001,
0.835000000000001,0.840000000000001,0.845000000000001,0.850000000000001,
0.855000000000001,0.860000000000001,0.865000000000001,0.870000000000001,
0.875000000000001,0.880000000000001,0.885000000000001,0.890000000000001,
0.895000000000001,0.900000000000001,0.905000000000001,0.910000000000001,
0.915000000000001,0.920000000000001,0.925000000000001,0.930000000000001,
0.935000000000001,0.940000000000001,0.941429844438059),.UNSPECIFIED.)
CURVE()
GEOMETRIC_REPRESENTATION_ITEM()
RATIONAL_B_SPLINE_CURVE((1.,1.,1.,1.,1.,1.,1.,1.,1.,1.,1.,1.,1.,1.,1.,1.,
1.,1.,1.,1.,1.,1.,1.,1.,1.,1.,1.,1.,1.,1.,1.,1.,1.,1.,1.,1.,1.,1.,1.,1.,
1.,1.,1.,1.,1.,1.,1.,1.,1.,1.,1.,1.,1.,1.,1.,1.,1.,1.,1.,1.,1.,1.,1.,1.,
1.,1.,1.,1.,1.,1.,1.,1.,1.,1.,1.,1.,1.,1.,1.,1.,1.,1.,1.,1.,1.,1.,1.,1.,
1.,1.,1.,1.,1.,1.,1.,1.,1.,1.,1.,1.,1.,1.,1.,1.,1.,1.,1.,1.,1.,1.,1.,1.,
1.,1.,1.,1.,1.,1.,1.,1.,1.,1.,1.,1.,1.,1.,1.,1.,1.,1.,1.,1.,1.,1.,1.,1.,
1.,1.,1.,1.,1.,1.,1.,1.,1.,1.,1.,1.,1.,1.,1.,1.,1.,1.,1.,1.,1.,1.,1.,1.,
1.,1.,1.,1.,1.,1.,1.,1.,1.,1.,1.,1.,1.,1.,1.,1.,1.,1.,1.,1.,1.,1.,1.,1.,
1.,1.,1.,1.,1.,1.,1.,1.,1.,1.))
REPRESENTATION_ITEM('')
);
#690=(
BOUNDED_CURVE()
B_SPLINE_CURVE(5,(#174779,#174780,#174781,#174782,#174783,#174784,#174785,
#174786,#174787,#174788,#174789,#174790,#174791,#174792,#174793,#174794,
#174795,#174796,#174797,#174798,#174799,#174800,#174801,#174802,#174803,
#174804,#174805,#174806,#174807,#174808,#174809,#174810,#174811,#174812,
#174813,#174814,#174815,#174816,#174817,#174818,#174819,#174820,#174821,
#174822,#174823,#174824,#174825,#174826,#174827,#174828,#174829,#174830,
#174831,#174832,#174833,#174834,#174835,#174836,#174837,#174838,#174839,
#174840,#174841,#174842,#174843,#174844,#174845,#174846,#174847,#174848,
#174849,#174850,#174851,#174852,#174853,#174854,#174855,#174856,#174857,
#174858,#174859,#174860,#174861,#174862,#174863,#174864,#174865,#174866,
#174867,#174868,#174869,#174870,#174871,#174872,#174873,#174874,#174875,
#174876,#174877,#174878,#174879,#174880,#174881,#174882,#174883,#174884,
#174885,#174886,#174887,#174888,#174889,#174890,#174891,#174892,#174893,
#174894,#174895,#174896,#174897,#174898,#174899,#174900,#174901,#174902,
#174903,#174904,#174905,#174906,#174907,#174908,#174909,#174910,#174911,
#174912,#174913,#174914,#174915,#174916,#174917,#174918,#174919,#174920,
#174921,#174922,#174923,#174924,#174925,#174926,#174927,#174928,#174929,
#174930,#174931,#174932,#174933,#174934,#174935,#174936,#174937,#174938,
#174939,#174940,#174941,#174942,#174943,#174944,#174945,#174946,#174947,
#174948,#174949,#174950,#174951,#174952,#174953,#174954,#174955,#174956,
#174957,#174958,#174959,#174960,#174961,#174962,#174963,#174964,#174965,
#174966,#174967,#174968,#174969,#174970,#174971,#174972),.UNSPECIFIED.,
 .F.,.F.)
B_SPLINE_CURVE_WITH_KNOTS((6,1,1,1,1,1,1,1,1,1,1,1,1,1,1,1,1,1,1,1,1,1,
1,1,1,1,1,1,1,1,1,1,1,1,1,1,1,1,1,1,1,1,1,1,1,1,1,1,1,1,1,1,1,1,1,1,1,1,
1,1,1,1,1,1,1,1,1,1,1,1,1,1,1,1,1,1,1,1,1,1,1,1,1,1,1,1,1,1,1,1,1,1,1,1,
1,1,1,1,1,1,1,1,1,1,1,1,1,1,1,1,1,1,1,1,1,1,1,1,1,1,1,1,1,1,1,1,1,1,1,1,
1,1,1,1,1,1,1,1,1,1,1,1,1,1,1,1,1,1,1,1,1,1,1,1,1,1,1,1,1,1,1,1,1,1,1,1,
1,1,1,1,1,1,1,1,1,1,1,1,1,1,1,1,1,1,1,1,1,1,1,6),(-0.941429844438049,-0.940000000000001,
-0.935000000000001,-0.930000000000001,-0.925000000000001,-0.920000000000001,
-0.915000000000001,-0.910000000000001,-0.905000000000001,-0.900000000000001,
-0.895000000000001,-0.890000000000001,-0.885000000000001,-0.880000000000001,
-0.875000000000001,-0.870000000000001,-0.865000000000001,-0.860000000000001,
-0.855000000000001,-0.850000000000001,-0.845000000000001,-0.840000000000001,
-0.835000000000001,-0.830000000000001,-0.825000000000001,-0.820000000000001,
-0.815000000000001,-0.810000000000001,-0.805000000000001,-0.800000000000001,
-0.795000000000001,-0.790000000000001,-0.785000000000001,-0.780000000000001,
-0.775000000000001,-0.770000000000001,-0.765000000000001,-0.760000000000001,
-0.755000000000001,-0.750000000000001,-0.745000000000001,-0.740000000000001,
-0.735000000000001,-0.730000000000001,-0.725000000000001,-0.720000000000001,
-0.715000000000001,-0.710000000000001,-0.705000000000001,-0.700000000000001,
-0.695000000000001,-0.690000000000001,-0.685,-0.68,-0.675,-0.67,-0.665,
-0.66,-0.655,-0.65,-0.645,-0.64,-0.635,-0.63,-0.625,-0.62,-0.615,-0.61,
-0.605,-0.6,-0.595,-0.59,-0.585,-0.58,-0.575,-0.57,-0.565,-0.56,-0.555,
-0.55,-0.545,-0.54,-0.535,-0.53,-0.525,-0.52,-0.515,-0.51,-0.505,-0.5,-0.495,
-0.49,-0.485,-0.48,-0.475,-0.47,-0.465,-0.46,-0.455,-0.45,-0.445,-0.44,
-0.435,-0.43,-0.425,-0.42,-0.415,-0.41,-0.405,-0.4,-0.395,-0.39,-0.385,
-0.38,-0.375,-0.37,-0.365,-0.36,-0.355,-0.35,-0.345,-0.34,-0.335,-0.33,
-0.325,-0.32,-0.315,-0.31,-0.305,-0.3,-0.295,-0.29,-0.285,-0.28,-0.275,
-0.27,-0.265,-0.26,-0.255,-0.25,-0.245,-0.24,-0.235,-0.23,-0.225,-0.22,
-0.215,-0.21,-0.205,-0.2,-0.195,-0.19,-0.185,-0.18,-0.175,-0.17,-0.165,
-0.16,-0.155,-0.15,-0.145,-0.14,-0.135,-0.13,-0.125,-0.12,-0.115,-0.11,
-0.105,-0.1,-0.095,-0.09,-0.085,-0.08,-0.075,-0.07,-0.065,-0.06,-0.055,
-0.05,-0.045,-0.04,-0.035,-0.03,-0.025,-0.02,-0.015,-0.01,-0.005,0.),
 .UNSPECIFIED.)
CURVE()
GEOMETRIC_REPRESENTATION_ITEM()
RATIONAL_B_SPLINE_CURVE((1.,1.,1.,1.,1.,1.,1.,1.,1.,1.,1.,1.,1.,1.,1.,1.,
1.,1.,1.,1.,1.,1.,1.,1.,1.,1.,1.,1.,1.,1.,1.,1.,1.,1.,1.,1.,1.,1.,1.,1.,
1.,1.,1.,1.,1.,1.,1.,1.,1.,1.,1.,1.,1.,1.,1.,1.,1.,1.,1.,1.,1.,1.,1.,1.,
1.,1.,1.,1.,1.,1.,1.,1.,1.,1.,1.,1.,1.,1.,1.,1.,1.,1.,1.,1.,1.,1.,1.,1.,
1.,1.,1.,1.,1.,1.,1.,1.,1.,1.,1.,1.,1.,1.,1.,1.,1.,1.,1.,1.,1.,1.,1.,1.,
1.,1.,1.,1.,1.,1.,1.,1.,1.,1.,1.,1.,1.,1.,1.,1.,1.,1.,1.,1.,1.,1.,1.,1.,
1.,1.,1.,1.,1.,1.,1.,1.,1.,1.,1.,1.,1.,1.,1.,1.,1.,1.,1.,1.,1.,1.,1.,1.,
1.,1.,1.,1.,1.,1.,1.,1.,1.,1.,1.,1.,1.,1.,1.,1.,1.,1.,1.,1.,1.,1.,1.,1.,
1.,1.,1.,1.,1.,1.,1.,1.,1.,1.))
REPRESENTATION_ITEM('')
);
#691=(
BOUNDED_CURVE()
B_SPLINE_CURVE(5,(#175013,#175014,#175015,#175016,#175017,#175018,#175019,
#175020,#175021,#175022,#175023,#175024,#175025,#175026,#175027,#175028,
#175029,#175030,#175031,#175032,#175033,#175034,#175035,#175036,#175037,
#175038,#175039,#175040,#175041,#175042,#175043,#175044,#175045,#175046,
#175047,#175048,#175049,#175050,#175051,#175052,#175053,#175054,#175055,
#175056,#175057,#175058,#175059,#175060,#175061,#175062,#175063,#175064,
#175065,#175066,#175067,#175068,#175069,#175070,#175071,#175072,#175073,
#175074,#175075,#175076,#175077,#175078,#175079,#175080,#175081,#175082,
#175083,#175084,#175085,#175086,#175087,#175088,#175089,#175090,#175091,
#175092,#175093,#175094,#175095,#175096,#175097,#175098,#175099,#175100,
#175101,#175102,#175103,#175104,#175105,#175106,#175107,#175108,#175109,
#175110,#175111,#175112,#175113,#175114,#175115,#175116,#175117,#175118,
#175119,#175120,#175121,#175122,#175123,#175124,#175125,#175126,#175127,
#175128,#175129,#175130,#175131,#175132,#175133,#175134,#175135,#175136,
#175137,#175138,#175139,#175140,#175141,#175142,#175143,#175144,#175145,
#175146,#175147,#175148,#175149,#175150,#175151,#175152,#175153,#175154,
#175155,#175156,#175157,#175158,#175159,#175160,#175161,#175162,#175163,
#175164,#175165,#175166,#175167,#175168,#175169,#175170,#175171,#175172,
#175173,#175174,#175175,#175176,#175177,#175178,#175179,#175180,#175181,
#175182,#175183,#175184,#175185,#175186,#175187,#175188,#175189,#175190,
#175191,#175192,#175193,#175194,#175195,#175196,#175197,#175198,#175199,
#175200,#175201,#175202,#175203,#175204,#175205,#175206,#175207,#175208,
#175209,#175210,#175211,#175212,#175213,#175214,#175215,#175216,#175217),
 .UNSPECIFIED.,.F.,.F.)
B_SPLINE_CURVE_WITH_KNOTS((6,1,1,1,1,1,1,1,1,1,1,1,1,1,1,1,1,1,1,1,1,1,
1,1,1,1,1,1,1,1,1,1,1,1,1,1,1,1,1,1,1,1,1,1,1,1,1,1,1,1,1,1,1,1,1,1,1,1,
1,1,1,1,1,1,1,1,1,1,1,1,1,1,1,1,1,1,1,1,1,1,1,1,1,1,1,1,1,1,1,1,1,1,1,1,
1,1,1,1,1,1,1,1,1,1,1,1,1,1,1,1,1,1,1,1,1,1,1,1,1,1,1,1,1,1,1,1,1,1,1,1,
1,1,1,1,1,1,1,1,1,1,1,1,1,1,1,1,1,1,1,1,1,1,1,1,1,1,1,1,1,1,1,1,1,1,1,1,
1,1,1,1,1,1,1,1,1,1,1,1,1,1,1,1,1,1,1,1,1,1,1,1,1,1,1,1,1,1,1,1,1,1,6),
(0.,0.005,0.01,0.015,0.02,0.025,0.03,0.035,0.04,0.045,0.05,0.055,0.06,0.065,
0.07,0.075,0.08,0.085,0.09,0.095,0.1,0.105,0.11,0.115,0.12,0.125,0.13,0.135,
0.14,0.145,0.15,0.155,0.16,0.165,0.17,0.175,0.18,0.185,0.19,0.195,0.2,0.205,
0.21,0.215,0.22,0.225,0.23,0.235,0.24,0.245,0.25,0.255,0.26,0.265,0.27,
0.275,0.28,0.285,0.29,0.295,0.3,0.305,0.31,0.315,0.32,0.325,0.33,0.335,
0.34,0.345,0.35,0.355,0.36,0.365,0.37,0.375,0.38,0.385,0.39,0.395,0.4,0.405,
0.41,0.415,0.42,0.425,0.43,0.435,0.44,0.445,0.45,0.455,0.46,0.465,0.47,
0.475,0.48,0.485,0.49,0.495,0.5,0.505,0.51,0.515,0.52,0.525,0.53,0.535,
0.54,0.545,0.55,0.555,0.56,0.565,0.57,0.575,0.58,0.585,0.59,0.595,0.6,0.605,
0.61,0.615,0.62,0.625,0.63,0.635,0.64,0.645,0.65,0.655,0.66,0.665,0.67,
0.675,0.68,0.685,0.690000000000001,0.695000000000001,0.700000000000001,
0.705000000000001,0.710000000000001,0.715000000000001,0.720000000000001,
0.725000000000001,0.730000000000001,0.735000000000001,0.740000000000001,
0.745000000000001,0.750000000000001,0.755000000000001,0.760000000000001,
0.765000000000001,0.770000000000001,0.775000000000001,0.780000000000001,
0.785000000000001,0.790000000000001,0.795000000000001,0.800000000000001,
0.805000000000001,0.810000000000001,0.815000000000001,0.820000000000001,
0.825000000000001,0.830000000000001,0.835000000000001,0.840000000000001,
0.845000000000001,0.850000000000001,0.855000000000001,0.860000000000001,
0.865000000000001,0.870000000000001,0.875000000000001,0.880000000000001,
0.885000000000001,0.890000000000001,0.895000000000001,0.900000000000001,
0.905000000000001,0.910000000000001,0.915000000000001,0.920000000000001,
0.925000000000001,0.930000000000001,0.935000000000001,0.940000000000001,
0.945000000000001,0.950000000000001,0.955000000000001,0.960000000000001,
0.965000000000001,0.970000000000001,0.975000000000001,0.980000000000001,
0.985000000000001,0.990000000000001,0.995000000000001,1.),.UNSPECIFIED.)
CURVE()
GEOMETRIC_REPRESENTATION_ITEM()
RATIONAL_B_SPLINE_CURVE((1.,1.,1.,1.,1.,1.,1.,1.,1.,1.,1.,1.,1.,1.,1.,1.,
1.,1.,1.,1.,1.,1.,1.,1.,1.,1.,1.,1.,1.,1.,1.,1.,1.,1.,1.,1.,1.,1.,1.,1.,
1.,1.,1.,1.,1.,1.,1.,1.,1.,1.,1.,1.,1.,1.,1.,1.,1.,1.,1.,1.,1.,1.,1.,1.,
1.,1.,1.,1.,1.,1.,1.,1.,1.,1.,1.,1.,1.,1.,1.,1.,1.,1.,1.,1.,1.,1.,1.,1.,
1.,1.,1.,1.,1.,1.,1.,1.,1.,1.,1.,1.,1.,1.,1.,1.,1.,1.,1.,1.,1.,1.,1.,1.,
1.,1.,1.,1.,1.,1.,1.,1.,1.,1.,1.,1.,1.,1.,1.,1.,1.,1.,1.,1.,1.,1.,1.,1.,
1.,1.,1.,1.,1.,1.,1.,1.,1.,1.,1.,1.,1.,1.,1.,1.,1.,1.,1.,1.,1.,1.,1.,1.,
1.,1.,1.,1.,1.,1.,1.,1.,1.,1.,1.,1.,1.,1.,1.,1.,1.,1.,1.,1.,1.,1.,1.,1.,
1.,1.,1.,1.,1.,1.,1.,1.,1.,1.,1.,1.,1.,1.,1.,1.,1.,1.,1.,1.,1.))
REPRESENTATION_ITEM('')
);
#692=(
BOUNDED_CURVE()
B_SPLINE_CURVE(5,(#175221,#175222,#175223,#175224,#175225,#175226,#175227,
#175228,#175229,#175230,#175231,#175232,#175233,#175234,#175235,#175236,
#175237,#175238,#175239,#175240,#175241,#175242,#175243,#175244,#175245,
#175246,#175247,#175248,#175249,#175250,#175251,#175252,#175253,#175254,
#175255,#175256,#175257,#175258,#175259,#175260,#175261,#175262,#175263,
#175264,#175265,#175266,#175267,#175268,#175269,#175270,#175271,#175272,
#175273,#175274,#175275,#175276,#175277,#175278,#175279,#175280,#175281,
#175282,#175283,#175284,#175285,#175286,#175287,#175288,#175289,#175290,
#175291,#175292,#175293,#175294,#175295,#175296,#175297,#175298,#175299,
#175300,#175301,#175302,#175303,#175304,#175305,#175306,#175307,#175308,
#175309,#175310,#175311,#175312,#175313,#175314,#175315,#175316,#175317,
#175318,#175319,#175320,#175321,#175322,#175323,#175324,#175325,#175326,
#175327,#175328,#175329,#175330,#175331,#175332,#175333,#175334,#175335,
#175336,#175337,#175338,#175339,#175340,#175341,#175342,#175343,#175344,
#175345,#175346,#175347,#175348,#175349,#175350,#175351,#175352,#175353,
#175354,#175355,#175356,#175357,#175358,#175359,#175360,#175361,#175362,
#175363,#175364,#175365,#175366,#175367,#175368,#175369,#175370,#175371,
#175372,#175373,#175374,#175375,#175376,#175377,#175378,#175379,#175380,
#175381,#175382,#175383,#175384,#175385,#175386,#175387,#175388,#175389,
#175390,#175391,#175392,#175393,#175394,#175395,#175396,#175397,#175398,
#175399,#175400,#175401,#175402,#175403,#175404,#175405,#175406,#175407,
#175408,#175409,#175410,#175411,#175412,#175413,#175414,#175415,#175416,
#175417,#175418,#175419,#175420,#175421,#175422,#175423,#175424,#175425),
 .UNSPECIFIED.,.F.,.F.)
B_SPLINE_CURVE_WITH_KNOTS((6,1,1,1,1,1,1,1,1,1,1,1,1,1,1,1,1,1,1,1,1,1,
1,1,1,1,1,1,1,1,1,1,1,1,1,1,1,1,1,1,1,1,1,1,1,1,1,1,1,1,1,1,1,1,1,1,1,1,
1,1,1,1,1,1,1,1,1,1,1,1,1,1,1,1,1,1,1,1,1,1,1,1,1,1,1,1,1,1,1,1,1,1,1,1,
1,1,1,1,1,1,1,1,1,1,1,1,1,1,1,1,1,1,1,1,1,1,1,1,1,1,1,1,1,1,1,1,1,1,1,1,
1,1,1,1,1,1,1,1,1,1,1,1,1,1,1,1,1,1,1,1,1,1,1,1,1,1,1,1,1,1,1,1,1,1,1,1,
1,1,1,1,1,1,1,1,1,1,1,1,1,1,1,1,1,1,1,1,1,1,1,1,1,1,1,1,1,1,1,1,1,1,6),
(-1.,-0.995000000000001,-0.990000000000001,-0.985000000000001,-0.980000000000001,
-0.975000000000001,-0.970000000000001,-0.965000000000001,-0.960000000000001,
-0.955000000000001,-0.950000000000001,-0.945000000000001,-0.940000000000001,
-0.935000000000001,-0.930000000000001,-0.925000000000001,-0.920000000000001,
-0.915000000000001,-0.910000000000001,-0.905000000000001,-0.900000000000001,
-0.895000000000001,-0.890000000000001,-0.885000000000001,-0.880000000000001,
-0.875000000000001,-0.870000000000001,-0.865000000000001,-0.860000000000001,
-0.855000000000001,-0.850000000000001,-0.845000000000001,-0.840000000000001,
-0.835000000000001,-0.830000000000001,-0.825000000000001,-0.820000000000001,
-0.815000000000001,-0.810000000000001,-0.805000000000001,-0.800000000000001,
-0.795000000000001,-0.790000000000001,-0.785000000000001,-0.780000000000001,
-0.775000000000001,-0.770000000000001,-0.765000000000001,-0.760000000000001,
-0.755000000000001,-0.750000000000001,-0.745000000000001,-0.740000000000001,
-0.735000000000001,-0.730000000000001,-0.725000000000001,-0.720000000000001,
-0.715000000000001,-0.710000000000001,-0.705000000000001,-0.700000000000001,
-0.695000000000001,-0.690000000000001,-0.685,-0.68,-0.675,-0.67,-0.665,
-0.66,-0.655,-0.65,-0.645,-0.64,-0.635,-0.63,-0.625,-0.62,-0.615,-0.61,
-0.605,-0.6,-0.595,-0.59,-0.585,-0.58,-0.575,-0.57,-0.565,-0.56,-0.555,
-0.55,-0.545,-0.54,-0.535,-0.53,-0.525,-0.52,-0.515,-0.51,-0.505,-0.5,-0.495,
-0.49,-0.485,-0.48,-0.475,-0.47,-0.465,-0.46,-0.455,-0.45,-0.445,-0.44,
-0.435,-0.43,-0.425,-0.42,-0.415,-0.41,-0.405,-0.4,-0.395,-0.39,-0.385,
-0.38,-0.375,-0.37,-0.365,-0.36,-0.355,-0.35,-0.345,-0.34,-0.335,-0.33,
-0.325,-0.32,-0.315,-0.31,-0.305,-0.3,-0.295,-0.29,-0.285,-0.28,-0.275,
-0.27,-0.265,-0.26,-0.255,-0.25,-0.245,-0.24,-0.235,-0.23,-0.225,-0.22,
-0.215,-0.21,-0.205,-0.2,-0.195,-0.19,-0.185,-0.18,-0.175,-0.17,-0.165,
-0.16,-0.155,-0.15,-0.145,-0.14,-0.135,-0.13,-0.125,-0.12,-0.115,-0.11,
-0.105,-0.1,-0.095,-0.09,-0.085,-0.08,-0.075,-0.07,-0.065,-0.06,-0.055,
-0.05,-0.045,-0.04,-0.035,-0.03,-0.025,-0.02,-0.015,-0.01,-0.005,0.),
 .UNSPECIFIED.)
CURVE()
GEOMETRIC_REPRESENTATION_ITEM()
RATIONAL_B_SPLINE_CURVE((1.,1.,1.,1.,1.,1.,1.,1.,1.,1.,1.,1.,1.,1.,1.,1.,
1.,1.,1.,1.,1.,1.,1.,1.,1.,1.,1.,1.,1.,1.,1.,1.,1.,1.,1.,1.,1.,1.,1.,1.,
1.,1.,1.,1.,1.,1.,1.,1.,1.,1.,1.,1.,1.,1.,1.,1.,1.,1.,1.,1.,1.,1.,1.,1.,
1.,1.,1.,1.,1.,1.,1.,1.,1.,1.,1.,1.,1.,1.,1.,1.,1.,1.,1.,1.,1.,1.,1.,1.,
1.,1.,1.,1.,1.,1.,1.,1.,1.,1.,1.,1.,1.,1.,1.,1.,1.,1.,1.,1.,1.,1.,1.,1.,
1.,1.,1.,1.,1.,1.,1.,1.,1.,1.,1.,1.,1.,1.,1.,1.,1.,1.,1.,1.,1.,1.,1.,1.,
1.,1.,1.,1.,1.,1.,1.,1.,1.,1.,1.,1.,1.,1.,1.,1.,1.,1.,1.,1.,1.,1.,1.,1.,
1.,1.,1.,1.,1.,1.,1.,1.,1.,1.,1.,1.,1.,1.,1.,1.,1.,1.,1.,1.,1.,1.,1.,1.,
1.,1.,1.,1.,1.,1.,1.,1.,1.,1.,1.,1.,1.,1.,1.,1.,1.,1.,1.,1.,1.))
REPRESENTATION_ITEM('')
);
#693=(
BOUNDED_CURVE()
B_SPLINE_CURVE(5,(#175437,#175438,#175439,#175440,#175441,#175442,#175443,
#175444,#175445,#175446,#175447,#175448,#175449,#175450,#175451,#175452,
#175453,#175454,#175455,#175456,#175457,#175458,#175459,#175460,#175461,
#175462,#175463,#175464,#175465,#175466,#175467,#175468,#175469,#175470,
#175471,#175472,#175473,#175474,#175475,#175476,#175477,#175478,#175479,
#175480,#175481,#175482,#175483,#175484,#175485,#175486,#175487,#175488,
#175489,#175490,#175491,#175492,#175493,#175494,#175495,#175496,#175497,
#175498,#175499,#175500,#175501,#175502,#175503,#175504,#175505,#175506,
#175507,#175508,#175509,#175510,#175511,#175512,#175513,#175514,#175515,
#175516,#175517,#175518,#175519,#175520,#175521,#175522,#175523,#175524,
#175525,#175526,#175527,#175528,#175529,#175530,#175531,#175532,#175533,
#175534,#175535,#175536,#175537,#175538,#175539,#175540,#175541,#175542,
#175543,#175544,#175545,#175546,#175547,#175548,#175549,#175550,#175551,
#175552,#175553,#175554,#175555,#175556,#175557,#175558,#175559,#175560,
#175561,#175562,#175563,#175564,#175565,#175566,#175567,#175568,#175569,
#175570,#175571,#175572,#175573,#175574,#175575,#175576,#175577,#175578,
#175579,#175580,#175581,#175582,#175583,#175584,#175585,#175586,#175587,
#175588,#175589,#175590,#175591,#175592,#175593,#175594,#175595,#175596,
#175597,#175598,#175599,#175600,#175601,#175602,#175603,#175604,#175605,
#175606,#175607,#175608,#175609,#175610,#175611,#175612,#175613,#175614,
#175615,#175616,#175617,#175618,#175619,#175620,#175621,#175622,#175623,
#175624,#175625,#175626,#175627,#175628,#175629,#175630,#175631,#175632,
#175633,#175634,#175635,#175636,#175637,#175638,#175639,#175640,#175641),
 .UNSPECIFIED.,.F.,.F.)
B_SPLINE_CURVE_WITH_KNOTS((6,1,1,1,1,1,1,1,1,1,1,1,1,1,1,1,1,1,1,1,1,1,
1,1,1,1,1,1,1,1,1,1,1,1,1,1,1,1,1,1,1,1,1,1,1,1,1,1,1,1,1,1,1,1,1,1,1,1,
1,1,1,1,1,1,1,1,1,1,1,1,1,1,1,1,1,1,1,1,1,1,1,1,1,1,1,1,1,1,1,1,1,1,1,1,
1,1,1,1,1,1,1,1,1,1,1,1,1,1,1,1,1,1,1,1,1,1,1,1,1,1,1,1,1,1,1,1,1,1,1,1,
1,1,1,1,1,1,1,1,1,1,1,1,1,1,1,1,1,1,1,1,1,1,1,1,1,1,1,1,1,1,1,1,1,1,1,1,
1,1,1,1,1,1,1,1,1,1,1,1,1,1,1,1,1,1,1,1,1,1,1,1,1,1,1,1,1,1,1,1,1,1,6),
(0.,0.005,0.01,0.015,0.02,0.025,0.03,0.035,0.04,0.045,0.05,0.055,0.06,0.065,
0.07,0.075,0.08,0.085,0.09,0.095,0.1,0.105,0.11,0.115,0.12,0.125,0.13,0.135,
0.14,0.145,0.15,0.155,0.16,0.165,0.17,0.175,0.18,0.185,0.19,0.195,0.2,0.205,
0.21,0.215,0.22,0.225,0.23,0.235,0.24,0.245,0.25,0.255,0.26,0.265,0.27,
0.275,0.28,0.285,0.29,0.295,0.3,0.305,0.31,0.315,0.32,0.325,0.33,0.335,
0.34,0.345,0.35,0.355,0.36,0.365,0.37,0.375,0.38,0.385,0.39,0.395,0.4,0.405,
0.41,0.415,0.42,0.425,0.43,0.435,0.44,0.445,0.45,0.455,0.46,0.465,0.47,
0.475,0.48,0.485,0.49,0.495,0.5,0.505,0.51,0.515,0.52,0.525,0.53,0.535,
0.54,0.545,0.55,0.555,0.56,0.565,0.57,0.575,0.58,0.585,0.59,0.595,0.6,0.605,
0.61,0.615,0.62,0.625,0.63,0.635,0.64,0.645,0.65,0.655,0.66,0.665,0.67,
0.675,0.68,0.685,0.690000000000001,0.695000000000001,0.700000000000001,
0.705000000000001,0.710000000000001,0.715000000000001,0.720000000000001,
0.725000000000001,0.730000000000001,0.735000000000001,0.740000000000001,
0.745000000000001,0.750000000000001,0.755000000000001,0.760000000000001,
0.765000000000001,0.770000000000001,0.775000000000001,0.780000000000001,
0.785000000000001,0.790000000000001,0.795000000000001,0.800000000000001,
0.805000000000001,0.810000000000001,0.815000000000001,0.820000000000001,
0.825000000000001,0.830000000000001,0.835000000000001,0.840000000000001,
0.845000000000001,0.850000000000001,0.855000000000001,0.860000000000001,
0.865000000000001,0.870000000000001,0.875000000000001,0.880000000000001,
0.885000000000001,0.890000000000001,0.895000000000001,0.900000000000001,
0.905000000000001,0.910000000000001,0.915000000000001,0.920000000000001,
0.925000000000001,0.930000000000001,0.935000000000001,0.940000000000001,
0.945000000000001,0.950000000000001,0.955000000000001,0.960000000000001,
0.965000000000001,0.970000000000001,0.975000000000001,0.980000000000001,
0.985000000000001,0.990000000000001,0.995000000000001,1.),.UNSPECIFIED.)
CURVE()
GEOMETRIC_REPRESENTATION_ITEM()
RATIONAL_B_SPLINE_CURVE((1.,1.,1.,1.,1.,1.,1.,1.,1.,1.,1.,1.,1.,1.,1.,1.,
1.,1.,1.,1.,1.,1.,1.,1.,1.,1.,1.,1.,1.,1.,1.,1.,1.,1.,1.,1.,1.,1.,1.,1.,
1.,1.,1.,1.,1.,1.,1.,1.,1.,1.,1.,1.,1.,1.,1.,1.,1.,1.,1.,1.,1.,1.,1.,1.,
1.,1.,1.,1.,1.,1.,1.,1.,1.,1.,1.,1.,1.,1.,1.,1.,1.,1.,1.,1.,1.,1.,1.,1.,
1.,1.,1.,1.,1.,1.,1.,1.,1.,1.,1.,1.,1.,1.,1.,1.,1.,1.,1.,1.,1.,1.,1.,1.,
1.,1.,1.,1.,1.,1.,1.,1.,1.,1.,1.,1.,1.,1.,1.,1.,1.,1.,1.,1.,1.,1.,1.,1.,
1.,1.,1.,1.,1.,1.,1.,1.,1.,1.,1.,1.,1.,1.,1.,1.,1.,1.,1.,1.,1.,1.,1.,1.,
1.,1.,1.,1.,1.,1.,1.,1.,1.,1.,1.,1.,1.,1.,1.,1.,1.,1.,1.,1.,1.,1.,1.,1.,
1.,1.,1.,1.,1.,1.,1.,1.,1.,1.,1.,1.,1.,1.,1.,1.,1.,1.,1.,1.,1.))
REPRESENTATION_ITEM('')
);
#694=(
BOUNDED_CURVE()
B_SPLINE_CURVE(5,(#175645,#175646,#175647,#175648,#175649,#175650,#175651,
#175652,#175653,#175654,#175655,#175656,#175657,#175658,#175659,#175660,
#175661,#175662,#175663,#175664,#175665,#175666,#175667,#175668,#175669,
#175670,#175671,#175672,#175673,#175674,#175675,#175676,#175677,#175678,
#175679,#175680,#175681,#175682,#175683,#175684,#175685,#175686,#175687,
#175688,#175689,#175690,#175691,#175692,#175693,#175694,#175695,#175696,
#175697,#175698,#175699,#175700,#175701,#175702,#175703,#175704,#175705,
#175706,#175707,#175708,#175709,#175710,#175711,#175712,#175713,#175714,
#175715,#175716,#175717,#175718,#175719,#175720,#175721,#175722,#175723,
#175724,#175725,#175726,#175727,#175728,#175729,#175730,#175731,#175732,
#175733,#175734,#175735,#175736,#175737,#175738,#175739,#175740,#175741,
#175742,#175743,#175744,#175745,#175746,#175747,#175748,#175749,#175750,
#175751,#175752,#175753,#175754,#175755,#175756,#175757,#175758,#175759,
#175760,#175761,#175762,#175763,#175764,#175765,#175766,#175767,#175768,
#175769,#175770,#175771,#175772,#175773,#175774,#175775,#175776,#175777,
#175778,#175779,#175780,#175781,#175782,#175783,#175784,#175785,#175786,
#175787,#175788,#175789,#175790,#175791,#175792,#175793,#175794,#175795,
#175796,#175797,#175798,#175799,#175800,#175801,#175802,#175803,#175804,
#175805,#175806,#175807,#175808,#175809,#175810,#175811,#175812,#175813,
#175814,#175815,#175816,#175817,#175818,#175819,#175820,#175821,#175822,
#175823,#175824,#175825,#175826,#175827,#175828,#175829,#175830,#175831,
#175832,#175833,#175834,#175835,#175836,#175837,#175838,#175839,#175840,
#175841,#175842,#175843,#175844,#175845,#175846,#175847,#175848,#175849),
 .UNSPECIFIED.,.F.,.F.)
B_SPLINE_CURVE_WITH_KNOTS((6,1,1,1,1,1,1,1,1,1,1,1,1,1,1,1,1,1,1,1,1,1,
1,1,1,1,1,1,1,1,1,1,1,1,1,1,1,1,1,1,1,1,1,1,1,1,1,1,1,1,1,1,1,1,1,1,1,1,
1,1,1,1,1,1,1,1,1,1,1,1,1,1,1,1,1,1,1,1,1,1,1,1,1,1,1,1,1,1,1,1,1,1,1,1,
1,1,1,1,1,1,1,1,1,1,1,1,1,1,1,1,1,1,1,1,1,1,1,1,1,1,1,1,1,1,1,1,1,1,1,1,
1,1,1,1,1,1,1,1,1,1,1,1,1,1,1,1,1,1,1,1,1,1,1,1,1,1,1,1,1,1,1,1,1,1,1,1,
1,1,1,1,1,1,1,1,1,1,1,1,1,1,1,1,1,1,1,1,1,1,1,1,1,1,1,1,1,1,1,1,1,1,6),
(-1.,-0.995000000000001,-0.990000000000001,-0.985000000000001,-0.980000000000001,
-0.975000000000001,-0.970000000000001,-0.965000000000001,-0.960000000000001,
-0.955000000000001,-0.950000000000001,-0.945000000000001,-0.940000000000001,
-0.935000000000001,-0.930000000000001,-0.925000000000001,-0.920000000000001,
-0.915000000000001,-0.910000000000001,-0.905000000000001,-0.900000000000001,
-0.895000000000001,-0.890000000000001,-0.885000000000001,-0.880000000000001,
-0.875000000000001,-0.870000000000001,-0.865000000000001,-0.860000000000001,
-0.855000000000001,-0.850000000000001,-0.845000000000001,-0.840000000000001,
-0.835000000000001,-0.830000000000001,-0.825000000000001,-0.820000000000001,
-0.815000000000001,-0.810000000000001,-0.805000000000001,-0.800000000000001,
-0.795000000000001,-0.790000000000001,-0.785000000000001,-0.780000000000001,
-0.775000000000001,-0.770000000000001,-0.765000000000001,-0.760000000000001,
-0.755000000000001,-0.750000000000001,-0.745000000000001,-0.740000000000001,
-0.735000000000001,-0.730000000000001,-0.725000000000001,-0.720000000000001,
-0.715000000000001,-0.710000000000001,-0.705000000000001,-0.700000000000001,
-0.695000000000001,-0.690000000000001,-0.685,-0.68,-0.675,-0.67,-0.665,
-0.66,-0.655,-0.65,-0.645,-0.64,-0.635,-0.63,-0.625,-0.62,-0.615,-0.61,
-0.605,-0.6,-0.595,-0.59,-0.585,-0.58,-0.575,-0.57,-0.565,-0.56,-0.555,
-0.55,-0.545,-0.54,-0.535,-0.53,-0.525,-0.52,-0.515,-0.51,-0.505,-0.5,-0.495,
-0.49,-0.485,-0.48,-0.475,-0.47,-0.465,-0.46,-0.455,-0.45,-0.445,-0.44,
-0.435,-0.43,-0.425,-0.42,-0.415,-0.41,-0.405,-0.4,-0.395,-0.39,-0.385,
-0.38,-0.375,-0.37,-0.365,-0.36,-0.355,-0.35,-0.345,-0.34,-0.335,-0.33,
-0.325,-0.32,-0.315,-0.31,-0.305,-0.3,-0.295,-0.29,-0.285,-0.28,-0.275,
-0.27,-0.265,-0.26,-0.255,-0.25,-0.245,-0.24,-0.235,-0.23,-0.225,-0.22,
-0.215,-0.21,-0.205,-0.2,-0.195,-0.19,-0.185,-0.18,-0.175,-0.17,-0.165,
-0.16,-0.155,-0.15,-0.145,-0.14,-0.135,-0.13,-0.125,-0.12,-0.115,-0.11,
-0.105,-0.1,-0.095,-0.09,-0.085,-0.08,-0.075,-0.07,-0.065,-0.06,-0.055,
-0.05,-0.045,-0.04,-0.035,-0.03,-0.025,-0.02,-0.015,-0.01,-0.005,0.),
 .UNSPECIFIED.)
CURVE()
GEOMETRIC_REPRESENTATION_ITEM()
RATIONAL_B_SPLINE_CURVE((1.,1.,1.,1.,1.,1.,1.,1.,1.,1.,1.,1.,1.,1.,1.,1.,
1.,1.,1.,1.,1.,1.,1.,1.,1.,1.,1.,1.,1.,1.,1.,1.,1.,1.,1.,1.,1.,1.,1.,1.,
1.,1.,1.,1.,1.,1.,1.,1.,1.,1.,1.,1.,1.,1.,1.,1.,1.,1.,1.,1.,1.,1.,1.,1.,
1.,1.,1.,1.,1.,1.,1.,1.,1.,1.,1.,1.,1.,1.,1.,1.,1.,1.,1.,1.,1.,1.,1.,1.,
1.,1.,1.,1.,1.,1.,1.,1.,1.,1.,1.,1.,1.,1.,1.,1.,1.,1.,1.,1.,1.,1.,1.,1.,
1.,1.,1.,1.,1.,1.,1.,1.,1.,1.,1.,1.,1.,1.,1.,1.,1.,1.,1.,1.,1.,1.,1.,1.,
1.,1.,1.,1.,1.,1.,1.,1.,1.,1.,1.,1.,1.,1.,1.,1.,1.,1.,1.,1.,1.,1.,1.,1.,
1.,1.,1.,1.,1.,1.,1.,1.,1.,1.,1.,1.,1.,1.,1.,1.,1.,1.,1.,1.,1.,1.,1.,1.,
1.,1.,1.,1.,1.,1.,1.,1.,1.,1.,1.,1.,1.,1.,1.,1.,1.,1.,1.,1.,1.))
REPRESENTATION_ITEM('')
);
#695=(
BOUNDED_CURVE()
B_SPLINE_CURVE(5,(#175861,#175862,#175863,#175864,#175865,#175866,#175867,
#175868,#175869,#175870,#175871,#175872,#175873,#175874,#175875,#175876,
#175877,#175878,#175879,#175880,#175881,#175882,#175883,#175884,#175885,
#175886,#175887,#175888,#175889,#175890,#175891,#175892,#175893,#175894,
#175895,#175896,#175897,#175898,#175899,#175900,#175901,#175902,#175903,
#175904,#175905,#175906,#175907,#175908,#175909,#175910,#175911,#175912,
#175913,#175914,#175915,#175916,#175917,#175918,#175919,#175920,#175921,
#175922,#175923,#175924,#175925,#175926,#175927,#175928,#175929,#175930,
#175931,#175932,#175933,#175934,#175935,#175936,#175937,#175938,#175939,
#175940,#175941,#175942,#175943,#175944,#175945,#175946,#175947,#175948,
#175949,#175950,#175951,#175952,#175953,#175954,#175955,#175956,#175957,
#175958,#175959,#175960,#175961,#175962,#175963,#175964,#175965,#175966,
#175967,#175968,#175969,#175970,#175971,#175972,#175973,#175974,#175975,
#175976,#175977,#175978,#175979,#175980,#175981,#175982,#175983,#175984,
#175985,#175986,#175987,#175988,#175989,#175990,#175991,#175992,#175993,
#175994,#175995,#175996,#175997,#175998,#175999,#176000,#176001,#176002,
#176003,#176004,#176005,#176006,#176007,#176008,#176009,#176010,#176011,
#176012,#176013,#176014,#176015,#176016,#176017,#176018,#176019,#176020,
#176021,#176022,#176023,#176024,#176025,#176026,#176027,#176028,#176029,
#176030,#176031,#176032,#176033,#176034,#176035,#176036,#176037,#176038,
#176039,#176040,#176041,#176042,#176043,#176044,#176045,#176046,#176047,
#176048,#176049,#176050,#176051,#176052,#176053,#176054,#176055,#176056,
#176057,#176058,#176059,#176060,#176061,#176062,#176063,#176064,#176065),
 .UNSPECIFIED.,.F.,.F.)
B_SPLINE_CURVE_WITH_KNOTS((6,1,1,1,1,1,1,1,1,1,1,1,1,1,1,1,1,1,1,1,1,1,
1,1,1,1,1,1,1,1,1,1,1,1,1,1,1,1,1,1,1,1,1,1,1,1,1,1,1,1,1,1,1,1,1,1,1,1,
1,1,1,1,1,1,1,1,1,1,1,1,1,1,1,1,1,1,1,1,1,1,1,1,1,1,1,1,1,1,1,1,1,1,1,1,
1,1,1,1,1,1,1,1,1,1,1,1,1,1,1,1,1,1,1,1,1,1,1,1,1,1,1,1,1,1,1,1,1,1,1,1,
1,1,1,1,1,1,1,1,1,1,1,1,1,1,1,1,1,1,1,1,1,1,1,1,1,1,1,1,1,1,1,1,1,1,1,1,
1,1,1,1,1,1,1,1,1,1,1,1,1,1,1,1,1,1,1,1,1,1,1,1,1,1,1,1,1,1,1,1,1,1,6),
(0.,0.005,0.01,0.015,0.02,0.025,0.03,0.035,0.04,0.045,0.05,0.055,0.06,0.065,
0.07,0.075,0.08,0.085,0.09,0.095,0.1,0.105,0.11,0.115,0.12,0.125,0.13,0.135,
0.14,0.145,0.15,0.155,0.16,0.165,0.17,0.175,0.18,0.185,0.19,0.195,0.2,0.205,
0.21,0.215,0.22,0.225,0.23,0.235,0.24,0.245,0.25,0.255,0.26,0.265,0.27,
0.275,0.28,0.285,0.29,0.295,0.3,0.305,0.31,0.315,0.32,0.325,0.33,0.335,
0.34,0.345,0.35,0.355,0.36,0.365,0.37,0.375,0.38,0.385,0.39,0.395,0.4,0.405,
0.41,0.415,0.42,0.425,0.43,0.435,0.44,0.445,0.45,0.455,0.46,0.465,0.47,
0.475,0.48,0.485,0.49,0.495,0.5,0.505,0.51,0.515,0.52,0.525,0.53,0.535,
0.54,0.545,0.55,0.555,0.56,0.565,0.57,0.575,0.58,0.585,0.59,0.595,0.6,0.605,
0.61,0.615,0.62,0.625,0.63,0.635,0.64,0.645,0.65,0.655,0.66,0.665,0.67,
0.675,0.68,0.685,0.690000000000001,0.695000000000001,0.700000000000001,
0.705000000000001,0.710000000000001,0.715000000000001,0.720000000000001,
0.725000000000001,0.730000000000001,0.735000000000001,0.740000000000001,
0.745000000000001,0.750000000000001,0.755000000000001,0.760000000000001,
0.765000000000001,0.770000000000001,0.775000000000001,0.780000000000001,
0.785000000000001,0.790000000000001,0.795000000000001,0.800000000000001,
0.805000000000001,0.810000000000001,0.815000000000001,0.820000000000001,
0.825000000000001,0.830000000000001,0.835000000000001,0.840000000000001,
0.845000000000001,0.850000000000001,0.855000000000001,0.860000000000001,
0.865000000000001,0.870000000000001,0.875000000000001,0.880000000000001,
0.885000000000001,0.890000000000001,0.895000000000001,0.900000000000001,
0.905000000000001,0.910000000000001,0.915000000000001,0.920000000000001,
0.925000000000001,0.930000000000001,0.935000000000001,0.940000000000001,
0.945000000000001,0.950000000000001,0.955000000000001,0.960000000000001,
0.965000000000001,0.970000000000001,0.975000000000001,0.980000000000001,
0.985000000000001,0.990000000000001,0.995000000000001,1.),.UNSPECIFIED.)
CURVE()
GEOMETRIC_REPRESENTATION_ITEM()
RATIONAL_B_SPLINE_CURVE((1.,1.,1.,1.,1.,1.,1.,1.,1.,1.,1.,1.,1.,1.,1.,1.,
1.,1.,1.,1.,1.,1.,1.,1.,1.,1.,1.,1.,1.,1.,1.,1.,1.,1.,1.,1.,1.,1.,1.,1.,
1.,1.,1.,1.,1.,1.,1.,1.,1.,1.,1.,1.,1.,1.,1.,1.,1.,1.,1.,1.,1.,1.,1.,1.,
1.,1.,1.,1.,1.,1.,1.,1.,1.,1.,1.,1.,1.,1.,1.,1.,1.,1.,1.,1.,1.,1.,1.,1.,
1.,1.,1.,1.,1.,1.,1.,1.,1.,1.,1.,1.,1.,1.,1.,1.,1.,1.,1.,1.,1.,1.,1.,1.,
1.,1.,1.,1.,1.,1.,1.,1.,1.,1.,1.,1.,1.,1.,1.,1.,1.,1.,1.,1.,1.,1.,1.,1.,
1.,1.,1.,1.,1.,1.,1.,1.,1.,1.,1.,1.,1.,1.,1.,1.,1.,1.,1.,1.,1.,1.,1.,1.,
1.,1.,1.,1.,1.,1.,1.,1.,1.,1.,1.,1.,1.,1.,1.,1.,1.,1.,1.,1.,1.,1.,1.,1.,
1.,1.,1.,1.,1.,1.,1.,1.,1.,1.,1.,1.,1.,1.,1.,1.,1.,1.,1.,1.,1.))
REPRESENTATION_ITEM('')
);
#696=(
BOUNDED_CURVE()
B_SPLINE_CURVE(5,(#176069,#176070,#176071,#176072,#176073,#176074,#176075,
#176076,#176077,#176078,#176079,#176080,#176081,#176082,#176083,#176084,
#176085,#176086,#176087,#176088,#176089,#176090,#176091,#176092,#176093,
#176094,#176095,#176096,#176097,#176098,#176099,#176100,#176101,#176102,
#176103,#176104,#176105,#176106,#176107,#176108,#176109,#176110,#176111,
#176112,#176113,#176114,#176115,#176116,#176117,#176118,#176119,#176120,
#176121,#176122,#176123,#176124,#176125,#176126,#176127,#176128,#176129,
#176130,#176131,#176132,#176133,#176134,#176135,#176136,#176137,#176138,
#176139,#176140,#176141,#176142,#176143,#176144,#176145,#176146,#176147,
#176148,#176149,#176150,#176151,#176152,#176153,#176154,#176155,#176156,
#176157,#176158,#176159,#176160,#176161,#176162,#176163,#176164,#176165,
#176166,#176167,#176168,#176169,#176170,#176171,#176172,#176173,#176174,
#176175,#176176,#176177,#176178,#176179,#176180,#176181,#176182,#176183,
#176184,#176185,#176186,#176187,#176188,#176189,#176190,#176191,#176192,
#176193,#176194,#176195,#176196,#176197,#176198,#176199,#176200,#176201,
#176202,#176203,#176204,#176205,#176206,#176207,#176208,#176209,#176210,
#176211,#176212,#176213,#176214,#176215,#176216,#176217,#176218,#176219,
#176220,#176221,#176222,#176223,#176224,#176225,#176226,#176227,#176228,
#176229,#176230,#176231,#176232,#176233,#176234,#176235,#176236,#176237,
#176238,#176239,#176240,#176241,#176242,#176243,#176244,#176245,#176246,
#176247,#176248,#176249,#176250,#176251,#176252,#176253,#176254,#176255,
#176256,#176257,#176258,#176259,#176260,#176261,#176262,#176263,#176264,
#176265,#176266,#176267,#176268,#176269,#176270,#176271,#176272,#176273),
 .UNSPECIFIED.,.F.,.F.)
B_SPLINE_CURVE_WITH_KNOTS((6,1,1,1,1,1,1,1,1,1,1,1,1,1,1,1,1,1,1,1,1,1,
1,1,1,1,1,1,1,1,1,1,1,1,1,1,1,1,1,1,1,1,1,1,1,1,1,1,1,1,1,1,1,1,1,1,1,1,
1,1,1,1,1,1,1,1,1,1,1,1,1,1,1,1,1,1,1,1,1,1,1,1,1,1,1,1,1,1,1,1,1,1,1,1,
1,1,1,1,1,1,1,1,1,1,1,1,1,1,1,1,1,1,1,1,1,1,1,1,1,1,1,1,1,1,1,1,1,1,1,1,
1,1,1,1,1,1,1,1,1,1,1,1,1,1,1,1,1,1,1,1,1,1,1,1,1,1,1,1,1,1,1,1,1,1,1,1,
1,1,1,1,1,1,1,1,1,1,1,1,1,1,1,1,1,1,1,1,1,1,1,1,1,1,1,1,1,1,1,1,1,1,6),
(-1.,-0.995000000000001,-0.990000000000001,-0.985000000000001,-0.980000000000001,
-0.975000000000001,-0.970000000000001,-0.965000000000001,-0.960000000000001,
-0.955000000000001,-0.950000000000001,-0.945000000000001,-0.940000000000001,
-0.935000000000001,-0.930000000000001,-0.925000000000001,-0.920000000000001,
-0.915000000000001,-0.910000000000001,-0.905000000000001,-0.900000000000001,
-0.895000000000001,-0.890000000000001,-0.885000000000001,-0.880000000000001,
-0.875000000000001,-0.870000000000001,-0.865000000000001,-0.860000000000001,
-0.855000000000001,-0.850000000000001,-0.845000000000001,-0.840000000000001,
-0.835000000000001,-0.830000000000001,-0.825000000000001,-0.820000000000001,
-0.815000000000001,-0.810000000000001,-0.805000000000001,-0.800000000000001,
-0.795000000000001,-0.790000000000001,-0.785000000000001,-0.780000000000001,
-0.775000000000001,-0.770000000000001,-0.765000000000001,-0.760000000000001,
-0.755000000000001,-0.750000000000001,-0.745000000000001,-0.740000000000001,
-0.735000000000001,-0.730000000000001,-0.725000000000001,-0.720000000000001,
-0.715000000000001,-0.710000000000001,-0.705000000000001,-0.700000000000001,
-0.695000000000001,-0.690000000000001,-0.685,-0.68,-0.675,-0.67,-0.665,
-0.66,-0.655,-0.65,-0.645,-0.64,-0.635,-0.63,-0.625,-0.62,-0.615,-0.61,
-0.605,-0.6,-0.595,-0.59,-0.585,-0.58,-0.575,-0.57,-0.565,-0.56,-0.555,
-0.55,-0.545,-0.54,-0.535,-0.53,-0.525,-0.52,-0.515,-0.51,-0.505,-0.5,-0.495,
-0.49,-0.485,-0.48,-0.475,-0.47,-0.465,-0.46,-0.455,-0.45,-0.445,-0.44,
-0.435,-0.43,-0.425,-0.42,-0.415,-0.41,-0.405,-0.4,-0.395,-0.39,-0.385,
-0.38,-0.375,-0.37,-0.365,-0.36,-0.355,-0.35,-0.345,-0.34,-0.335,-0.33,
-0.325,-0.32,-0.315,-0.31,-0.305,-0.3,-0.295,-0.29,-0.285,-0.28,-0.275,
-0.27,-0.265,-0.26,-0.255,-0.25,-0.245,-0.24,-0.235,-0.23,-0.225,-0.22,
-0.215,-0.21,-0.205,-0.2,-0.195,-0.19,-0.185,-0.18,-0.175,-0.17,-0.165,
-0.16,-0.155,-0.15,-0.145,-0.14,-0.135,-0.13,-0.125,-0.12,-0.115,-0.11,
-0.105,-0.1,-0.095,-0.09,-0.085,-0.08,-0.075,-0.07,-0.065,-0.06,-0.055,
-0.05,-0.045,-0.04,-0.035,-0.03,-0.025,-0.02,-0.015,-0.01,-0.005,0.),
 .UNSPECIFIED.)
CURVE()
GEOMETRIC_REPRESENTATION_ITEM()
RATIONAL_B_SPLINE_CURVE((1.,1.,1.,1.,1.,1.,1.,1.,1.,1.,1.,1.,1.,1.,1.,1.,
1.,1.,1.,1.,1.,1.,1.,1.,1.,1.,1.,1.,1.,1.,1.,1.,1.,1.,1.,1.,1.,1.,1.,1.,
1.,1.,1.,1.,1.,1.,1.,1.,1.,1.,1.,1.,1.,1.,1.,1.,1.,1.,1.,1.,1.,1.,1.,1.,
1.,1.,1.,1.,1.,1.,1.,1.,1.,1.,1.,1.,1.,1.,1.,1.,1.,1.,1.,1.,1.,1.,1.,1.,
1.,1.,1.,1.,1.,1.,1.,1.,1.,1.,1.,1.,1.,1.,1.,1.,1.,1.,1.,1.,1.,1.,1.,1.,
1.,1.,1.,1.,1.,1.,1.,1.,1.,1.,1.,1.,1.,1.,1.,1.,1.,1.,1.,1.,1.,1.,1.,1.,
1.,1.,1.,1.,1.,1.,1.,1.,1.,1.,1.,1.,1.,1.,1.,1.,1.,1.,1.,1.,1.,1.,1.,1.,
1.,1.,1.,1.,1.,1.,1.,1.,1.,1.,1.,1.,1.,1.,1.,1.,1.,1.,1.,1.,1.,1.,1.,1.,
1.,1.,1.,1.,1.,1.,1.,1.,1.,1.,1.,1.,1.,1.,1.,1.,1.,1.,1.,1.,1.))
REPRESENTATION_ITEM('')
);
#697=(
BOUNDED_CURVE()
B_SPLINE_CURVE(5,(#176285,#176286,#176287,#176288,#176289,#176290,#176291,
#176292,#176293,#176294,#176295,#176296,#176297,#176298,#176299,#176300,
#176301,#176302,#176303,#176304,#176305,#176306,#176307,#176308,#176309,
#176310,#176311,#176312,#176313,#176314,#176315,#176316,#176317,#176318,
#176319,#176320,#176321,#176322,#176323,#176324,#176325,#176326,#176327,
#176328,#176329,#176330,#176331,#176332,#176333,#176334,#176335,#176336,
#176337,#176338,#176339,#176340,#176341,#176342,#176343,#176344,#176345,
#176346,#176347,#176348,#176349,#176350,#176351,#176352,#176353,#176354,
#176355,#176356,#176357,#176358,#176359,#176360,#176361,#176362,#176363,
#176364,#176365,#176366,#176367,#176368,#176369,#176370,#176371,#176372,
#176373,#176374,#176375,#176376,#176377,#176378,#176379,#176380,#176381,
#176382,#176383,#176384,#176385,#176386,#176387,#176388,#176389,#176390,
#176391,#176392,#176393,#176394,#176395,#176396,#176397,#176398,#176399,
#176400,#176401,#176402,#176403,#176404,#176405,#176406,#176407,#176408,
#176409,#176410,#176411,#176412,#176413,#176414,#176415,#176416,#176417,
#176418,#176419,#176420,#176421,#176422,#176423,#176424,#176425,#176426,
#176427,#176428,#176429,#176430,#176431,#176432,#176433,#176434,#176435,
#176436,#176437,#176438,#176439,#176440,#176441,#176442,#176443,#176444,
#176445,#176446,#176447,#176448,#176449,#176450,#176451,#176452,#176453,
#176454,#176455,#176456,#176457,#176458,#176459,#176460,#176461,#176462,
#176463,#176464,#176465,#176466,#176467,#176468,#176469,#176470,#176471,
#176472,#176473,#176474,#176475,#176476,#176477,#176478,#176479,#176480,
#176481,#176482,#176483,#176484,#176485,#176486,#176487,#176488,#176489),
 .UNSPECIFIED.,.F.,.F.)
B_SPLINE_CURVE_WITH_KNOTS((6,1,1,1,1,1,1,1,1,1,1,1,1,1,1,1,1,1,1,1,1,1,
1,1,1,1,1,1,1,1,1,1,1,1,1,1,1,1,1,1,1,1,1,1,1,1,1,1,1,1,1,1,1,1,1,1,1,1,
1,1,1,1,1,1,1,1,1,1,1,1,1,1,1,1,1,1,1,1,1,1,1,1,1,1,1,1,1,1,1,1,1,1,1,1,
1,1,1,1,1,1,1,1,1,1,1,1,1,1,1,1,1,1,1,1,1,1,1,1,1,1,1,1,1,1,1,1,1,1,1,1,
1,1,1,1,1,1,1,1,1,1,1,1,1,1,1,1,1,1,1,1,1,1,1,1,1,1,1,1,1,1,1,1,1,1,1,1,
1,1,1,1,1,1,1,1,1,1,1,1,1,1,1,1,1,1,1,1,1,1,1,1,1,1,1,1,1,1,1,1,1,1,6),
(0.,0.005,0.01,0.015,0.02,0.025,0.03,0.035,0.04,0.045,0.05,0.055,0.06,0.065,
0.07,0.075,0.08,0.085,0.09,0.095,0.1,0.105,0.11,0.115,0.12,0.125,0.13,0.135,
0.14,0.145,0.15,0.155,0.16,0.165,0.17,0.175,0.18,0.185,0.19,0.195,0.2,0.205,
0.21,0.215,0.22,0.225,0.23,0.235,0.24,0.245,0.25,0.255,0.26,0.265,0.27,
0.275,0.28,0.285,0.29,0.295,0.3,0.305,0.31,0.315,0.32,0.325,0.33,0.335,
0.34,0.345,0.35,0.355,0.36,0.365,0.37,0.375,0.38,0.385,0.39,0.395,0.4,0.405,
0.41,0.415,0.42,0.425,0.43,0.435,0.44,0.445,0.45,0.455,0.46,0.465,0.47,
0.475,0.48,0.485,0.49,0.495,0.5,0.505,0.51,0.515,0.52,0.525,0.53,0.535,
0.54,0.545,0.55,0.555,0.56,0.565,0.57,0.575,0.58,0.585,0.59,0.595,0.6,0.605,
0.61,0.615,0.62,0.625,0.63,0.635,0.64,0.645,0.65,0.655,0.66,0.665,0.67,
0.675,0.68,0.685,0.690000000000001,0.695000000000001,0.700000000000001,
0.705000000000001,0.710000000000001,0.715000000000001,0.720000000000001,
0.725000000000001,0.730000000000001,0.735000000000001,0.740000000000001,
0.745000000000001,0.750000000000001,0.755000000000001,0.760000000000001,
0.765000000000001,0.770000000000001,0.775000000000001,0.780000000000001,
0.785000000000001,0.790000000000001,0.795000000000001,0.800000000000001,
0.805000000000001,0.810000000000001,0.815000000000001,0.820000000000001,
0.825000000000001,0.830000000000001,0.835000000000001,0.840000000000001,
0.845000000000001,0.850000000000001,0.855000000000001,0.860000000000001,
0.865000000000001,0.870000000000001,0.875000000000001,0.880000000000001,
0.885000000000001,0.890000000000001,0.895000000000001,0.900000000000001,
0.905000000000001,0.910000000000001,0.915000000000001,0.920000000000001,
0.925000000000001,0.930000000000001,0.935000000000001,0.940000000000001,
0.945000000000001,0.950000000000001,0.955000000000001,0.960000000000001,
0.965000000000001,0.970000000000001,0.975000000000001,0.980000000000001,
0.985000000000001,0.990000000000001,0.995000000000001,1.),.UNSPECIFIED.)
CURVE()
GEOMETRIC_REPRESENTATION_ITEM()
RATIONAL_B_SPLINE_CURVE((1.,1.,1.,1.,1.,1.,1.,1.,1.,1.,1.,1.,1.,1.,1.,1.,
1.,1.,1.,1.,1.,1.,1.,1.,1.,1.,1.,1.,1.,1.,1.,1.,1.,1.,1.,1.,1.,1.,1.,1.,
1.,1.,1.,1.,1.,1.,1.,1.,1.,1.,1.,1.,1.,1.,1.,1.,1.,1.,1.,1.,1.,1.,1.,1.,
1.,1.,1.,1.,1.,1.,1.,1.,1.,1.,1.,1.,1.,1.,1.,1.,1.,1.,1.,1.,1.,1.,1.,1.,
1.,1.,1.,1.,1.,1.,1.,1.,1.,1.,1.,1.,1.,1.,1.,1.,1.,1.,1.,1.,1.,1.,1.,1.,
1.,1.,1.,1.,1.,1.,1.,1.,1.,1.,1.,1.,1.,1.,1.,1.,1.,1.,1.,1.,1.,1.,1.,1.,
1.,1.,1.,1.,1.,1.,1.,1.,1.,1.,1.,1.,1.,1.,1.,1.,1.,1.,1.,1.,1.,1.,1.,1.,
1.,1.,1.,1.,1.,1.,1.,1.,1.,1.,1.,1.,1.,1.,1.,1.,1.,1.,1.,1.,1.,1.,1.,1.,
1.,1.,1.,1.,1.,1.,1.,1.,1.,1.,1.,1.,1.,1.,1.,1.,1.,1.,1.,1.,1.))
REPRESENTATION_ITEM('')
);
#698=(
BOUNDED_CURVE()
B_SPLINE_CURVE(5,(#176493,#176494,#176495,#176496,#176497,#176498,#176499,
#176500,#176501,#176502,#176503,#176504,#176505,#176506,#176507,#176508,
#176509,#176510,#176511,#176512,#176513,#176514,#176515,#176516,#176517,
#176518,#176519,#176520,#176521,#176522,#176523,#176524,#176525,#176526,
#176527,#176528,#176529,#176530,#176531,#176532,#176533,#176534,#176535,
#176536,#176537,#176538,#176539,#176540,#176541,#176542,#176543,#176544,
#176545,#176546,#176547,#176548,#176549,#176550,#176551,#176552,#176553,
#176554,#176555,#176556,#176557,#176558,#176559,#176560,#176561,#176562,
#176563,#176564,#176565,#176566,#176567,#176568,#176569,#176570,#176571,
#176572,#176573,#176574,#176575,#176576,#176577,#176578,#176579,#176580,
#176581,#176582,#176583,#176584,#176585,#176586,#176587,#176588,#176589,
#176590,#176591,#176592,#176593,#176594,#176595,#176596,#176597,#176598,
#176599,#176600,#176601,#176602,#176603,#176604,#176605,#176606,#176607,
#176608,#176609,#176610,#176611,#176612,#176613,#176614,#176615,#176616,
#176617,#176618,#176619,#176620,#176621,#176622,#176623,#176624,#176625,
#176626,#176627,#176628,#176629,#176630,#176631,#176632,#176633,#176634,
#176635,#176636,#176637,#176638,#176639,#176640,#176641,#176642,#176643,
#176644,#176645,#176646,#176647,#176648,#176649,#176650,#176651,#176652,
#176653,#176654,#176655,#176656,#176657,#176658,#176659,#176660,#176661,
#176662,#176663,#176664,#176665,#176666,#176667,#176668,#176669,#176670,
#176671,#176672,#176673,#176674,#176675,#176676,#176677,#176678,#176679,
#176680,#176681,#176682,#176683,#176684,#176685,#176686,#176687,#176688,
#176689,#176690,#176691,#176692,#176693,#176694,#176695,#176696,#176697),
 .UNSPECIFIED.,.F.,.F.)
B_SPLINE_CURVE_WITH_KNOTS((6,1,1,1,1,1,1,1,1,1,1,1,1,1,1,1,1,1,1,1,1,1,
1,1,1,1,1,1,1,1,1,1,1,1,1,1,1,1,1,1,1,1,1,1,1,1,1,1,1,1,1,1,1,1,1,1,1,1,
1,1,1,1,1,1,1,1,1,1,1,1,1,1,1,1,1,1,1,1,1,1,1,1,1,1,1,1,1,1,1,1,1,1,1,1,
1,1,1,1,1,1,1,1,1,1,1,1,1,1,1,1,1,1,1,1,1,1,1,1,1,1,1,1,1,1,1,1,1,1,1,1,
1,1,1,1,1,1,1,1,1,1,1,1,1,1,1,1,1,1,1,1,1,1,1,1,1,1,1,1,1,1,1,1,1,1,1,1,
1,1,1,1,1,1,1,1,1,1,1,1,1,1,1,1,1,1,1,1,1,1,1,1,1,1,1,1,1,1,1,1,1,1,6),
(-1.,-0.995000000000001,-0.990000000000001,-0.985000000000001,-0.980000000000001,
-0.975000000000001,-0.970000000000001,-0.965000000000001,-0.960000000000001,
-0.955000000000001,-0.950000000000001,-0.945000000000001,-0.940000000000001,
-0.935000000000001,-0.930000000000001,-0.925000000000001,-0.920000000000001,
-0.915000000000001,-0.910000000000001,-0.905000000000001,-0.900000000000001,
-0.895000000000001,-0.890000000000001,-0.885000000000001,-0.880000000000001,
-0.875000000000001,-0.870000000000001,-0.865000000000001,-0.860000000000001,
-0.855000000000001,-0.850000000000001,-0.845000000000001,-0.840000000000001,
-0.835000000000001,-0.830000000000001,-0.825000000000001,-0.820000000000001,
-0.815000000000001,-0.810000000000001,-0.805000000000001,-0.800000000000001,
-0.795000000000001,-0.790000000000001,-0.785000000000001,-0.780000000000001,
-0.775000000000001,-0.770000000000001,-0.765000000000001,-0.760000000000001,
-0.755000000000001,-0.750000000000001,-0.745000000000001,-0.740000000000001,
-0.735000000000001,-0.730000000000001,-0.725000000000001,-0.720000000000001,
-0.715000000000001,-0.710000000000001,-0.705000000000001,-0.700000000000001,
-0.695000000000001,-0.690000000000001,-0.685,-0.68,-0.675,-0.67,-0.665,
-0.66,-0.655,-0.65,-0.645,-0.64,-0.635,-0.63,-0.625,-0.62,-0.615,-0.61,
-0.605,-0.6,-0.595,-0.59,-0.585,-0.58,-0.575,-0.57,-0.565,-0.56,-0.555,
-0.55,-0.545,-0.54,-0.535,-0.53,-0.525,-0.52,-0.515,-0.51,-0.505,-0.5,-0.495,
-0.49,-0.485,-0.48,-0.475,-0.47,-0.465,-0.46,-0.455,-0.45,-0.445,-0.44,
-0.435,-0.43,-0.425,-0.42,-0.415,-0.41,-0.405,-0.4,-0.395,-0.39,-0.385,
-0.38,-0.375,-0.37,-0.365,-0.36,-0.355,-0.35,-0.345,-0.34,-0.335,-0.33,
-0.325,-0.32,-0.315,-0.31,-0.305,-0.3,-0.295,-0.29,-0.285,-0.28,-0.275,
-0.27,-0.265,-0.26,-0.255,-0.25,-0.245,-0.24,-0.235,-0.23,-0.225,-0.22,
-0.215,-0.21,-0.205,-0.2,-0.195,-0.19,-0.185,-0.18,-0.175,-0.17,-0.165,
-0.16,-0.155,-0.15,-0.145,-0.14,-0.135,-0.13,-0.125,-0.12,-0.115,-0.11,
-0.105,-0.1,-0.095,-0.09,-0.085,-0.08,-0.075,-0.07,-0.065,-0.06,-0.055,
-0.05,-0.045,-0.04,-0.035,-0.03,-0.025,-0.02,-0.015,-0.01,-0.005,0.),
 .UNSPECIFIED.)
CURVE()
GEOMETRIC_REPRESENTATION_ITEM()
RATIONAL_B_SPLINE_CURVE((1.,1.,1.,1.,1.,1.,1.,1.,1.,1.,1.,1.,1.,1.,1.,1.,
1.,1.,1.,1.,1.,1.,1.,1.,1.,1.,1.,1.,1.,1.,1.,1.,1.,1.,1.,1.,1.,1.,1.,1.,
1.,1.,1.,1.,1.,1.,1.,1.,1.,1.,1.,1.,1.,1.,1.,1.,1.,1.,1.,1.,1.,1.,1.,1.,
1.,1.,1.,1.,1.,1.,1.,1.,1.,1.,1.,1.,1.,1.,1.,1.,1.,1.,1.,1.,1.,1.,1.,1.,
1.,1.,1.,1.,1.,1.,1.,1.,1.,1.,1.,1.,1.,1.,1.,1.,1.,1.,1.,1.,1.,1.,1.,1.,
1.,1.,1.,1.,1.,1.,1.,1.,1.,1.,1.,1.,1.,1.,1.,1.,1.,1.,1.,1.,1.,1.,1.,1.,
1.,1.,1.,1.,1.,1.,1.,1.,1.,1.,1.,1.,1.,1.,1.,1.,1.,1.,1.,1.,1.,1.,1.,1.,
1.,1.,1.,1.,1.,1.,1.,1.,1.,1.,1.,1.,1.,1.,1.,1.,1.,1.,1.,1.,1.,1.,1.,1.,
1.,1.,1.,1.,1.,1.,1.,1.,1.,1.,1.,1.,1.,1.,1.,1.,1.,1.,1.,1.,1.))
REPRESENTATION_ITEM('')
);
#699=(
BOUNDED_CURVE()
B_SPLINE_CURVE(5,(#176709,#176710,#176711,#176712,#176713,#176714,#176715,
#176716,#176717,#176718,#176719,#176720,#176721,#176722,#176723,#176724,
#176725,#176726,#176727,#176728,#176729,#176730,#176731,#176732,#176733,
#176734,#176735,#176736,#176737,#176738,#176739,#176740,#176741,#176742,
#176743,#176744,#176745,#176746,#176747,#176748,#176749,#176750,#176751,
#176752,#176753,#176754,#176755,#176756,#176757,#176758,#176759,#176760,
#176761,#176762,#176763,#176764,#176765,#176766,#176767,#176768,#176769,
#176770,#176771,#176772,#176773,#176774,#176775,#176776,#176777,#176778,
#176779,#176780,#176781,#176782,#176783,#176784,#176785,#176786,#176787,
#176788,#176789,#176790,#176791,#176792,#176793,#176794,#176795,#176796,
#176797,#176798,#176799,#176800,#176801,#176802,#176803,#176804,#176805,
#176806,#176807,#176808,#176809,#176810,#176811,#176812,#176813,#176814,
#176815,#176816,#176817,#176818,#176819,#176820,#176821,#176822,#176823,
#176824,#176825,#176826,#176827,#176828,#176829,#176830,#176831,#176832,
#176833,#176834,#176835,#176836,#176837,#176838,#176839,#176840,#176841,
#176842,#176843,#176844,#176845,#176846,#176847,#176848,#176849,#176850,
#176851,#176852,#176853,#176854,#176855,#176856,#176857,#176858,#176859,
#176860,#176861,#176862,#176863,#176864,#176865,#176866,#176867,#176868,
#176869,#176870,#176871,#176872,#176873,#176874,#176875,#176876,#176877,
#176878,#176879,#176880,#176881,#176882,#176883,#176884,#176885,#176886,
#176887,#176888,#176889,#176890,#176891,#176892,#176893,#176894,#176895,
#176896,#176897,#176898,#176899,#176900,#176901,#176902,#176903,#176904,
#176905,#176906,#176907,#176908,#176909,#176910,#176911,#176912,#176913),
 .UNSPECIFIED.,.F.,.F.)
B_SPLINE_CURVE_WITH_KNOTS((6,1,1,1,1,1,1,1,1,1,1,1,1,1,1,1,1,1,1,1,1,1,
1,1,1,1,1,1,1,1,1,1,1,1,1,1,1,1,1,1,1,1,1,1,1,1,1,1,1,1,1,1,1,1,1,1,1,1,
1,1,1,1,1,1,1,1,1,1,1,1,1,1,1,1,1,1,1,1,1,1,1,1,1,1,1,1,1,1,1,1,1,1,1,1,
1,1,1,1,1,1,1,1,1,1,1,1,1,1,1,1,1,1,1,1,1,1,1,1,1,1,1,1,1,1,1,1,1,1,1,1,
1,1,1,1,1,1,1,1,1,1,1,1,1,1,1,1,1,1,1,1,1,1,1,1,1,1,1,1,1,1,1,1,1,1,1,1,
1,1,1,1,1,1,1,1,1,1,1,1,1,1,1,1,1,1,1,1,1,1,1,1,1,1,1,1,1,1,1,1,1,1,6),
(0.,0.005,0.01,0.015,0.02,0.025,0.03,0.035,0.04,0.045,0.05,0.055,0.06,0.065,
0.07,0.075,0.08,0.085,0.09,0.095,0.1,0.105,0.11,0.115,0.12,0.125,0.13,0.135,
0.14,0.145,0.15,0.155,0.16,0.165,0.17,0.175,0.18,0.185,0.19,0.195,0.2,0.205,
0.21,0.215,0.22,0.225,0.23,0.235,0.24,0.245,0.25,0.255,0.26,0.265,0.27,
0.275,0.28,0.285,0.29,0.295,0.3,0.305,0.31,0.315,0.32,0.325,0.33,0.335,
0.34,0.345,0.35,0.355,0.36,0.365,0.37,0.375,0.38,0.385,0.39,0.395,0.4,0.405,
0.41,0.415,0.42,0.425,0.43,0.435,0.44,0.445,0.45,0.455,0.46,0.465,0.47,
0.475,0.48,0.485,0.49,0.495,0.5,0.505,0.51,0.515,0.52,0.525,0.53,0.535,
0.54,0.545,0.55,0.555,0.56,0.565,0.57,0.575,0.58,0.585,0.59,0.595,0.6,0.605,
0.61,0.615,0.62,0.625,0.63,0.635,0.64,0.645,0.65,0.655,0.66,0.665,0.67,
0.675,0.68,0.685,0.690000000000001,0.695000000000001,0.700000000000001,
0.705000000000001,0.710000000000001,0.715000000000001,0.720000000000001,
0.725000000000001,0.730000000000001,0.735000000000001,0.740000000000001,
0.745000000000001,0.750000000000001,0.755000000000001,0.760000000000001,
0.765000000000001,0.770000000000001,0.775000000000001,0.780000000000001,
0.785000000000001,0.790000000000001,0.795000000000001,0.800000000000001,
0.805000000000001,0.810000000000001,0.815000000000001,0.820000000000001,
0.825000000000001,0.830000000000001,0.835000000000001,0.840000000000001,
0.845000000000001,0.850000000000001,0.855000000000001,0.860000000000001,
0.865000000000001,0.870000000000001,0.875000000000001,0.880000000000001,
0.885000000000001,0.890000000000001,0.895000000000001,0.900000000000001,
0.905000000000001,0.910000000000001,0.915000000000001,0.920000000000001,
0.925000000000001,0.930000000000001,0.935000000000001,0.940000000000001,
0.945000000000001,0.950000000000001,0.955000000000001,0.960000000000001,
0.965000000000001,0.970000000000001,0.975000000000001,0.980000000000001,
0.985000000000001,0.990000000000001,0.995000000000001,1.),.UNSPECIFIED.)
CURVE()
GEOMETRIC_REPRESENTATION_ITEM()
RATIONAL_B_SPLINE_CURVE((1.,1.,1.,1.,1.,1.,1.,1.,1.,1.,1.,1.,1.,1.,1.,1.,
1.,1.,1.,1.,1.,1.,1.,1.,1.,1.,1.,1.,1.,1.,1.,1.,1.,1.,1.,1.,1.,1.,1.,1.,
1.,1.,1.,1.,1.,1.,1.,1.,1.,1.,1.,1.,1.,1.,1.,1.,1.,1.,1.,1.,1.,1.,1.,1.,
1.,1.,1.,1.,1.,1.,1.,1.,1.,1.,1.,1.,1.,1.,1.,1.,1.,1.,1.,1.,1.,1.,1.,1.,
1.,1.,1.,1.,1.,1.,1.,1.,1.,1.,1.,1.,1.,1.,1.,1.,1.,1.,1.,1.,1.,1.,1.,1.,
1.,1.,1.,1.,1.,1.,1.,1.,1.,1.,1.,1.,1.,1.,1.,1.,1.,1.,1.,1.,1.,1.,1.,1.,
1.,1.,1.,1.,1.,1.,1.,1.,1.,1.,1.,1.,1.,1.,1.,1.,1.,1.,1.,1.,1.,1.,1.,1.,
1.,1.,1.,1.,1.,1.,1.,1.,1.,1.,1.,1.,1.,1.,1.,1.,1.,1.,1.,1.,1.,1.,1.,1.,
1.,1.,1.,1.,1.,1.,1.,1.,1.,1.,1.,1.,1.,1.,1.,1.,1.,1.,1.,1.,1.))
REPRESENTATION_ITEM('')
);
#700=(
BOUNDED_CURVE()
B_SPLINE_CURVE(5,(#176917,#176918,#176919,#176920,#176921,#176922,#176923,
#176924,#176925,#176926,#176927,#176928,#176929,#176930,#176931,#176932,
#176933,#176934,#176935,#176936,#176937,#176938,#176939,#176940,#176941,
#176942,#176943,#176944,#176945,#176946,#176947,#176948,#176949,#176950,
#176951,#176952,#176953,#176954,#176955,#176956,#176957,#176958,#176959,
#176960,#176961,#176962,#176963,#176964,#176965,#176966,#176967,#176968,
#176969,#176970,#176971,#176972,#176973,#176974,#176975,#176976,#176977,
#176978,#176979,#176980,#176981,#176982,#176983,#176984,#176985,#176986,
#176987,#176988,#176989,#176990,#176991,#176992,#176993,#176994,#176995,
#176996,#176997,#176998,#176999,#177000,#177001,#177002,#177003,#177004,
#177005,#177006,#177007,#177008,#177009,#177010,#177011,#177012,#177013,
#177014,#177015,#177016,#177017,#177018,#177019,#177020,#177021,#177022,
#177023,#177024,#177025,#177026,#177027,#177028,#177029,#177030,#177031,
#177032,#177033,#177034,#177035,#177036,#177037,#177038,#177039,#177040,
#177041,#177042,#177043,#177044,#177045,#177046,#177047,#177048,#177049,
#177050,#177051,#177052,#177053,#177054,#177055,#177056,#177057,#177058,
#177059,#177060,#177061,#177062,#177063,#177064,#177065,#177066,#177067,
#177068,#177069,#177070,#177071,#177072,#177073,#177074,#177075,#177076,
#177077,#177078,#177079,#177080,#177081,#177082,#177083,#177084,#177085,
#177086,#177087,#177088,#177089,#177090,#177091,#177092,#177093,#177094,
#177095,#177096,#177097,#177098,#177099,#177100,#177101,#177102,#177103,
#177104,#177105,#177106,#177107,#177108,#177109,#177110,#177111,#177112,
#177113,#177114,#177115,#177116,#177117,#177118,#177119,#177120,#177121),
 .UNSPECIFIED.,.F.,.F.)
B_SPLINE_CURVE_WITH_KNOTS((6,1,1,1,1,1,1,1,1,1,1,1,1,1,1,1,1,1,1,1,1,1,
1,1,1,1,1,1,1,1,1,1,1,1,1,1,1,1,1,1,1,1,1,1,1,1,1,1,1,1,1,1,1,1,1,1,1,1,
1,1,1,1,1,1,1,1,1,1,1,1,1,1,1,1,1,1,1,1,1,1,1,1,1,1,1,1,1,1,1,1,1,1,1,1,
1,1,1,1,1,1,1,1,1,1,1,1,1,1,1,1,1,1,1,1,1,1,1,1,1,1,1,1,1,1,1,1,1,1,1,1,
1,1,1,1,1,1,1,1,1,1,1,1,1,1,1,1,1,1,1,1,1,1,1,1,1,1,1,1,1,1,1,1,1,1,1,1,
1,1,1,1,1,1,1,1,1,1,1,1,1,1,1,1,1,1,1,1,1,1,1,1,1,1,1,1,1,1,1,1,1,1,6),
(-1.,-0.995000000000001,-0.990000000000001,-0.985000000000001,-0.980000000000001,
-0.975000000000001,-0.970000000000001,-0.965000000000001,-0.960000000000001,
-0.955000000000001,-0.950000000000001,-0.945000000000001,-0.940000000000001,
-0.935000000000001,-0.930000000000001,-0.925000000000001,-0.920000000000001,
-0.915000000000001,-0.910000000000001,-0.905000000000001,-0.900000000000001,
-0.895000000000001,-0.890000000000001,-0.885000000000001,-0.880000000000001,
-0.875000000000001,-0.870000000000001,-0.865000000000001,-0.860000000000001,
-0.855000000000001,-0.850000000000001,-0.845000000000001,-0.840000000000001,
-0.835000000000001,-0.830000000000001,-0.825000000000001,-0.820000000000001,
-0.815000000000001,-0.810000000000001,-0.805000000000001,-0.800000000000001,
-0.795000000000001,-0.790000000000001,-0.785000000000001,-0.780000000000001,
-0.775000000000001,-0.770000000000001,-0.765000000000001,-0.760000000000001,
-0.755000000000001,-0.750000000000001,-0.745000000000001,-0.740000000000001,
-0.735000000000001,-0.730000000000001,-0.725000000000001,-0.720000000000001,
-0.715000000000001,-0.710000000000001,-0.705000000000001,-0.700000000000001,
-0.695000000000001,-0.690000000000001,-0.685,-0.68,-0.675,-0.67,-0.665,
-0.66,-0.655,-0.65,-0.645,-0.64,-0.635,-0.63,-0.625,-0.62,-0.615,-0.61,
-0.605,-0.6,-0.595,-0.59,-0.585,-0.58,-0.575,-0.57,-0.565,-0.56,-0.555,
-0.55,-0.545,-0.54,-0.535,-0.53,-0.525,-0.52,-0.515,-0.51,-0.505,-0.5,-0.495,
-0.49,-0.485,-0.48,-0.475,-0.47,-0.465,-0.46,-0.455,-0.45,-0.445,-0.44,
-0.435,-0.43,-0.425,-0.42,-0.415,-0.41,-0.405,-0.4,-0.395,-0.39,-0.385,
-0.38,-0.375,-0.37,-0.365,-0.36,-0.355,-0.35,-0.345,-0.34,-0.335,-0.33,
-0.325,-0.32,-0.315,-0.31,-0.305,-0.3,-0.295,-0.29,-0.285,-0.28,-0.275,
-0.27,-0.265,-0.26,-0.255,-0.25,-0.245,-0.24,-0.235,-0.23,-0.225,-0.22,
-0.215,-0.21,-0.205,-0.2,-0.195,-0.19,-0.185,-0.18,-0.175,-0.17,-0.165,
-0.16,-0.155,-0.15,-0.145,-0.14,-0.135,-0.13,-0.125,-0.12,-0.115,-0.11,
-0.105,-0.1,-0.095,-0.09,-0.085,-0.08,-0.075,-0.07,-0.065,-0.06,-0.055,
-0.05,-0.045,-0.04,-0.035,-0.03,-0.025,-0.02,-0.015,-0.01,-0.005,0.),
 .UNSPECIFIED.)
CURVE()
GEOMETRIC_REPRESENTATION_ITEM()
RATIONAL_B_SPLINE_CURVE((1.,1.,1.,1.,1.,1.,1.,1.,1.,1.,1.,1.,1.,1.,1.,1.,
1.,1.,1.,1.,1.,1.,1.,1.,1.,1.,1.,1.,1.,1.,1.,1.,1.,1.,1.,1.,1.,1.,1.,1.,
1.,1.,1.,1.,1.,1.,1.,1.,1.,1.,1.,1.,1.,1.,1.,1.,1.,1.,1.,1.,1.,1.,1.,1.,
1.,1.,1.,1.,1.,1.,1.,1.,1.,1.,1.,1.,1.,1.,1.,1.,1.,1.,1.,1.,1.,1.,1.,1.,
1.,1.,1.,1.,1.,1.,1.,1.,1.,1.,1.,1.,1.,1.,1.,1.,1.,1.,1.,1.,1.,1.,1.,1.,
1.,1.,1.,1.,1.,1.,1.,1.,1.,1.,1.,1.,1.,1.,1.,1.,1.,1.,1.,1.,1.,1.,1.,1.,
1.,1.,1.,1.,1.,1.,1.,1.,1.,1.,1.,1.,1.,1.,1.,1.,1.,1.,1.,1.,1.,1.,1.,1.,
1.,1.,1.,1.,1.,1.,1.,1.,1.,1.,1.,1.,1.,1.,1.,1.,1.,1.,1.,1.,1.,1.,1.,1.,
1.,1.,1.,1.,1.,1.,1.,1.,1.,1.,1.,1.,1.,1.,1.,1.,1.,1.,1.,1.,1.))
REPRESENTATION_ITEM('')
);
#701=(
BOUNDED_CURVE()
B_SPLINE_CURVE(5,(#177133,#177134,#177135,#177136,#177137,#177138,#177139,
#177140,#177141,#177142,#177143,#177144,#177145,#177146,#177147,#177148,
#177149,#177150,#177151,#177152,#177153,#177154,#177155,#177156,#177157,
#177158,#177159,#177160,#177161,#177162,#177163,#177164,#177165,#177166,
#177167,#177168,#177169,#177170,#177171,#177172,#177173,#177174,#177175,
#177176,#177177,#177178,#177179,#177180,#177181,#177182,#177183,#177184,
#177185,#177186,#177187,#177188,#177189,#177190,#177191,#177192,#177193,
#177194,#177195,#177196,#177197,#177198,#177199,#177200,#177201,#177202,
#177203,#177204,#177205,#177206,#177207,#177208,#177209,#177210,#177211,
#177212,#177213,#177214,#177215,#177216,#177217,#177218,#177219,#177220,
#177221,#177222,#177223,#177224,#177225,#177226,#177227,#177228,#177229,
#177230,#177231,#177232,#177233,#177234,#177235,#177236,#177237,#177238,
#177239,#177240,#177241,#177242,#177243,#177244,#177245,#177246,#177247,
#177248,#177249,#177250,#177251,#177252,#177253,#177254,#177255,#177256,
#177257,#177258,#177259,#177260,#177261,#177262,#177263,#177264,#177265,
#177266,#177267,#177268,#177269,#177270,#177271,#177272,#177273,#177274,
#177275,#177276,#177277,#177278,#177279,#177280,#177281,#177282,#177283,
#177284,#177285,#177286,#177287,#177288,#177289,#177290,#177291,#177292,
#177293,#177294,#177295,#177296,#177297,#177298,#177299,#177300,#177301,
#177302,#177303,#177304,#177305,#177306,#177307,#177308,#177309,#177310,
#177311,#177312,#177313,#177314,#177315,#177316,#177317,#177318,#177319,
#177320,#177321,#177322,#177323,#177324,#177325,#177326,#177327,#177328,
#177329,#177330,#177331,#177332,#177333,#177334,#177335,#177336,#177337),
 .UNSPECIFIED.,.F.,.F.)
B_SPLINE_CURVE_WITH_KNOTS((6,1,1,1,1,1,1,1,1,1,1,1,1,1,1,1,1,1,1,1,1,1,
1,1,1,1,1,1,1,1,1,1,1,1,1,1,1,1,1,1,1,1,1,1,1,1,1,1,1,1,1,1,1,1,1,1,1,1,
1,1,1,1,1,1,1,1,1,1,1,1,1,1,1,1,1,1,1,1,1,1,1,1,1,1,1,1,1,1,1,1,1,1,1,1,
1,1,1,1,1,1,1,1,1,1,1,1,1,1,1,1,1,1,1,1,1,1,1,1,1,1,1,1,1,1,1,1,1,1,1,1,
1,1,1,1,1,1,1,1,1,1,1,1,1,1,1,1,1,1,1,1,1,1,1,1,1,1,1,1,1,1,1,1,1,1,1,1,
1,1,1,1,1,1,1,1,1,1,1,1,1,1,1,1,1,1,1,1,1,1,1,1,1,1,1,1,1,1,1,1,1,1,6),
(0.,0.005,0.01,0.015,0.02,0.025,0.03,0.035,0.04,0.045,0.05,0.055,0.06,0.065,
0.07,0.075,0.08,0.085,0.09,0.095,0.1,0.105,0.11,0.115,0.12,0.125,0.13,0.135,
0.14,0.145,0.15,0.155,0.16,0.165,0.17,0.175,0.18,0.185,0.19,0.195,0.2,0.205,
0.21,0.215,0.22,0.225,0.23,0.235,0.24,0.245,0.25,0.255,0.26,0.265,0.27,
0.275,0.28,0.285,0.29,0.295,0.3,0.305,0.31,0.315,0.32,0.325,0.33,0.335,
0.34,0.345,0.35,0.355,0.36,0.365,0.37,0.375,0.38,0.385,0.39,0.395,0.4,0.405,
0.41,0.415,0.42,0.425,0.43,0.435,0.44,0.445,0.45,0.455,0.46,0.465,0.47,
0.475,0.48,0.485,0.49,0.495,0.5,0.505,0.51,0.515,0.52,0.525,0.53,0.535,
0.54,0.545,0.55,0.555,0.56,0.565,0.57,0.575,0.58,0.585,0.59,0.595,0.6,0.605,
0.61,0.615,0.62,0.625,0.63,0.635,0.64,0.645,0.65,0.655,0.66,0.665,0.67,
0.675,0.68,0.685,0.690000000000001,0.695000000000001,0.700000000000001,
0.705000000000001,0.710000000000001,0.715000000000001,0.720000000000001,
0.725000000000001,0.730000000000001,0.735000000000001,0.740000000000001,
0.745000000000001,0.750000000000001,0.755000000000001,0.760000000000001,
0.765000000000001,0.770000000000001,0.775000000000001,0.780000000000001,
0.785000000000001,0.790000000000001,0.795000000000001,0.800000000000001,
0.805000000000001,0.810000000000001,0.815000000000001,0.820000000000001,
0.825000000000001,0.830000000000001,0.835000000000001,0.840000000000001,
0.845000000000001,0.850000000000001,0.855000000000001,0.860000000000001,
0.865000000000001,0.870000000000001,0.875000000000001,0.880000000000001,
0.885000000000001,0.890000000000001,0.895000000000001,0.900000000000001,
0.905000000000001,0.910000000000001,0.915000000000001,0.920000000000001,
0.925000000000001,0.930000000000001,0.935000000000001,0.940000000000001,
0.945000000000001,0.950000000000001,0.955000000000001,0.960000000000001,
0.965000000000001,0.970000000000001,0.975000000000001,0.980000000000001,
0.985000000000001,0.990000000000001,0.995000000000001,1.),.UNSPECIFIED.)
CURVE()
GEOMETRIC_REPRESENTATION_ITEM()
RATIONAL_B_SPLINE_CURVE((1.,1.,1.,1.,1.,1.,1.,1.,1.,1.,1.,1.,1.,1.,1.,1.,
1.,1.,1.,1.,1.,1.,1.,1.,1.,1.,1.,1.,1.,1.,1.,1.,1.,1.,1.,1.,1.,1.,1.,1.,
1.,1.,1.,1.,1.,1.,1.,1.,1.,1.,1.,1.,1.,1.,1.,1.,1.,1.,1.,1.,1.,1.,1.,1.,
1.,1.,1.,1.,1.,1.,1.,1.,1.,1.,1.,1.,1.,1.,1.,1.,1.,1.,1.,1.,1.,1.,1.,1.,
1.,1.,1.,1.,1.,1.,1.,1.,1.,1.,1.,1.,1.,1.,1.,1.,1.,1.,1.,1.,1.,1.,1.,1.,
1.,1.,1.,1.,1.,1.,1.,1.,1.,1.,1.,1.,1.,1.,1.,1.,1.,1.,1.,1.,1.,1.,1.,1.,
1.,1.,1.,1.,1.,1.,1.,1.,1.,1.,1.,1.,1.,1.,1.,1.,1.,1.,1.,1.,1.,1.,1.,1.,
1.,1.,1.,1.,1.,1.,1.,1.,1.,1.,1.,1.,1.,1.,1.,1.,1.,1.,1.,1.,1.,1.,1.,1.,
1.,1.,1.,1.,1.,1.,1.,1.,1.,1.,1.,1.,1.,1.,1.,1.,1.,1.,1.,1.,1.))
REPRESENTATION_ITEM('')
);
#702=(
BOUNDED_CURVE()
B_SPLINE_CURVE(5,(#177341,#177342,#177343,#177344,#177345,#177346,#177347,
#177348,#177349,#177350,#177351,#177352,#177353,#177354,#177355,#177356,
#177357,#177358,#177359,#177360,#177361,#177362,#177363,#177364,#177365,
#177366,#177367,#177368,#177369,#177370,#177371,#177372,#177373,#177374,
#177375,#177376,#177377,#177378,#177379,#177380,#177381,#177382,#177383,
#177384,#177385,#177386,#177387,#177388,#177389,#177390,#177391,#177392,
#177393,#177394,#177395,#177396,#177397,#177398,#177399,#177400,#177401,
#177402,#177403,#177404,#177405,#177406,#177407,#177408,#177409,#177410,
#177411,#177412,#177413,#177414,#177415,#177416,#177417,#177418,#177419,
#177420,#177421,#177422,#177423,#177424,#177425,#177426,#177427,#177428,
#177429,#177430,#177431,#177432,#177433,#177434,#177435,#177436,#177437,
#177438,#177439,#177440,#177441,#177442,#177443,#177444,#177445,#177446,
#177447,#177448,#177449,#177450,#177451,#177452,#177453,#177454,#177455,
#177456,#177457,#177458,#177459,#177460,#177461,#177462,#177463,#177464,
#177465,#177466,#177467,#177468,#177469,#177470,#177471,#177472,#177473,
#177474,#177475,#177476,#177477,#177478,#177479,#177480,#177481,#177482,
#177483,#177484,#177485,#177486,#177487,#177488,#177489,#177490,#177491,
#177492,#177493,#177494,#177495,#177496,#177497,#177498,#177499,#177500,
#177501,#177502,#177503,#177504,#177505,#177506,#177507,#177508,#177509,
#177510,#177511,#177512,#177513,#177514,#177515,#177516,#177517,#177518,
#177519,#177520,#177521,#177522,#177523,#177524,#177525,#177526,#177527,
#177528,#177529,#177530,#177531,#177532,#177533,#177534,#177535,#177536,
#177537,#177538,#177539,#177540,#177541,#177542,#177543,#177544,#177545),
 .UNSPECIFIED.,.F.,.F.)
B_SPLINE_CURVE_WITH_KNOTS((6,1,1,1,1,1,1,1,1,1,1,1,1,1,1,1,1,1,1,1,1,1,
1,1,1,1,1,1,1,1,1,1,1,1,1,1,1,1,1,1,1,1,1,1,1,1,1,1,1,1,1,1,1,1,1,1,1,1,
1,1,1,1,1,1,1,1,1,1,1,1,1,1,1,1,1,1,1,1,1,1,1,1,1,1,1,1,1,1,1,1,1,1,1,1,
1,1,1,1,1,1,1,1,1,1,1,1,1,1,1,1,1,1,1,1,1,1,1,1,1,1,1,1,1,1,1,1,1,1,1,1,
1,1,1,1,1,1,1,1,1,1,1,1,1,1,1,1,1,1,1,1,1,1,1,1,1,1,1,1,1,1,1,1,1,1,1,1,
1,1,1,1,1,1,1,1,1,1,1,1,1,1,1,1,1,1,1,1,1,1,1,1,1,1,1,1,1,1,1,1,1,1,6),
(-1.,-0.995000000000001,-0.990000000000001,-0.985000000000001,-0.980000000000001,
-0.975000000000001,-0.970000000000001,-0.965000000000001,-0.960000000000001,
-0.955000000000001,-0.950000000000001,-0.945000000000001,-0.940000000000001,
-0.935000000000001,-0.930000000000001,-0.925000000000001,-0.920000000000001,
-0.915000000000001,-0.910000000000001,-0.905000000000001,-0.900000000000001,
-0.895000000000001,-0.890000000000001,-0.885000000000001,-0.880000000000001,
-0.875000000000001,-0.870000000000001,-0.865000000000001,-0.860000000000001,
-0.855000000000001,-0.850000000000001,-0.845000000000001,-0.840000000000001,
-0.835000000000001,-0.830000000000001,-0.825000000000001,-0.820000000000001,
-0.815000000000001,-0.810000000000001,-0.805000000000001,-0.800000000000001,
-0.795000000000001,-0.790000000000001,-0.785000000000001,-0.780000000000001,
-0.775000000000001,-0.770000000000001,-0.765000000000001,-0.760000000000001,
-0.755000000000001,-0.750000000000001,-0.745000000000001,-0.740000000000001,
-0.735000000000001,-0.730000000000001,-0.725000000000001,-0.720000000000001,
-0.715000000000001,-0.710000000000001,-0.705000000000001,-0.700000000000001,
-0.695000000000001,-0.690000000000001,-0.685,-0.68,-0.675,-0.67,-0.665,
-0.66,-0.655,-0.65,-0.645,-0.64,-0.635,-0.63,-0.625,-0.62,-0.615,-0.61,
-0.605,-0.6,-0.595,-0.59,-0.585,-0.58,-0.575,-0.57,-0.565,-0.56,-0.555,
-0.55,-0.545,-0.54,-0.535,-0.53,-0.525,-0.52,-0.515,-0.51,-0.505,-0.5,-0.495,
-0.49,-0.485,-0.48,-0.475,-0.47,-0.465,-0.46,-0.455,-0.45,-0.445,-0.44,
-0.435,-0.43,-0.425,-0.42,-0.415,-0.41,-0.405,-0.4,-0.395,-0.39,-0.385,
-0.38,-0.375,-0.37,-0.365,-0.36,-0.355,-0.35,-0.345,-0.34,-0.335,-0.33,
-0.325,-0.32,-0.315,-0.31,-0.305,-0.3,-0.295,-0.29,-0.285,-0.28,-0.275,
-0.27,-0.265,-0.26,-0.255,-0.25,-0.245,-0.24,-0.235,-0.23,-0.225,-0.22,
-0.215,-0.21,-0.205,-0.2,-0.195,-0.19,-0.185,-0.18,-0.175,-0.17,-0.165,
-0.16,-0.155,-0.15,-0.145,-0.14,-0.135,-0.13,-0.125,-0.12,-0.115,-0.11,
-0.105,-0.1,-0.095,-0.09,-0.085,-0.08,-0.075,-0.07,-0.065,-0.06,-0.055,
-0.05,-0.045,-0.04,-0.035,-0.03,-0.025,-0.02,-0.015,-0.01,-0.005,0.),
 .UNSPECIFIED.)
CURVE()
GEOMETRIC_REPRESENTATION_ITEM()
RATIONAL_B_SPLINE_CURVE((1.,1.,1.,1.,1.,1.,1.,1.,1.,1.,1.,1.,1.,1.,1.,1.,
1.,1.,1.,1.,1.,1.,1.,1.,1.,1.,1.,1.,1.,1.,1.,1.,1.,1.,1.,1.,1.,1.,1.,1.,
1.,1.,1.,1.,1.,1.,1.,1.,1.,1.,1.,1.,1.,1.,1.,1.,1.,1.,1.,1.,1.,1.,1.,1.,
1.,1.,1.,1.,1.,1.,1.,1.,1.,1.,1.,1.,1.,1.,1.,1.,1.,1.,1.,1.,1.,1.,1.,1.,
1.,1.,1.,1.,1.,1.,1.,1.,1.,1.,1.,1.,1.,1.,1.,1.,1.,1.,1.,1.,1.,1.,1.,1.,
1.,1.,1.,1.,1.,1.,1.,1.,1.,1.,1.,1.,1.,1.,1.,1.,1.,1.,1.,1.,1.,1.,1.,1.,
1.,1.,1.,1.,1.,1.,1.,1.,1.,1.,1.,1.,1.,1.,1.,1.,1.,1.,1.,1.,1.,1.,1.,1.,
1.,1.,1.,1.,1.,1.,1.,1.,1.,1.,1.,1.,1.,1.,1.,1.,1.,1.,1.,1.,1.,1.,1.,1.,
1.,1.,1.,1.,1.,1.,1.,1.,1.,1.,1.,1.,1.,1.,1.,1.,1.,1.,1.,1.,1.))
REPRESENTATION_ITEM('')
);
#703=(
BOUNDED_CURVE()
B_SPLINE_CURVE(5,(#177557,#177558,#177559,#177560,#177561,#177562,#177563,
#177564,#177565,#177566,#177567,#177568,#177569,#177570,#177571,#177572,
#177573,#177574,#177575,#177576,#177577,#177578,#177579,#177580,#177581,
#177582,#177583,#177584,#177585,#177586,#177587,#177588,#177589,#177590,
#177591,#177592,#177593,#177594,#177595,#177596,#177597,#177598,#177599,
#177600,#177601,#177602,#177603,#177604,#177605,#177606,#177607,#177608,
#177609,#177610,#177611,#177612,#177613,#177614,#177615,#177616,#177617,
#177618,#177619,#177620,#177621,#177622,#177623,#177624,#177625,#177626,
#177627,#177628,#177629,#177630,#177631,#177632,#177633,#177634,#177635,
#177636,#177637,#177638,#177639,#177640,#177641,#177642,#177643,#177644,
#177645,#177646,#177647,#177648,#177649,#177650,#177651,#177652,#177653,
#177654,#177655,#177656,#177657,#177658,#177659,#177660,#177661,#177662,
#177663,#177664,#177665,#177666,#177667,#177668,#177669,#177670,#177671,
#177672,#177673,#177674,#177675,#177676,#177677,#177678,#177679,#177680,
#177681,#177682,#177683,#177684,#177685,#177686,#177687,#177688,#177689,
#177690,#177691,#177692,#177693,#177694,#177695,#177696,#177697,#177698,
#177699,#177700,#177701,#177702,#177703,#177704,#177705,#177706,#177707,
#177708,#177709,#177710,#177711,#177712,#177713,#177714,#177715,#177716,
#177717,#177718,#177719,#177720,#177721,#177722,#177723,#177724,#177725,
#177726,#177727,#177728,#177729,#177730,#177731,#177732,#177733,#177734,
#177735,#177736,#177737,#177738,#177739,#177740,#177741,#177742,#177743,
#177744,#177745,#177746,#177747,#177748,#177749,#177750,#177751,#177752,
#177753,#177754,#177755,#177756,#177757,#177758,#177759,#177760,#177761),
 .UNSPECIFIED.,.F.,.F.)
B_SPLINE_CURVE_WITH_KNOTS((6,1,1,1,1,1,1,1,1,1,1,1,1,1,1,1,1,1,1,1,1,1,
1,1,1,1,1,1,1,1,1,1,1,1,1,1,1,1,1,1,1,1,1,1,1,1,1,1,1,1,1,1,1,1,1,1,1,1,
1,1,1,1,1,1,1,1,1,1,1,1,1,1,1,1,1,1,1,1,1,1,1,1,1,1,1,1,1,1,1,1,1,1,1,1,
1,1,1,1,1,1,1,1,1,1,1,1,1,1,1,1,1,1,1,1,1,1,1,1,1,1,1,1,1,1,1,1,1,1,1,1,
1,1,1,1,1,1,1,1,1,1,1,1,1,1,1,1,1,1,1,1,1,1,1,1,1,1,1,1,1,1,1,1,1,1,1,1,
1,1,1,1,1,1,1,1,1,1,1,1,1,1,1,1,1,1,1,1,1,1,1,1,1,1,1,1,1,1,1,1,1,1,6),
(0.,0.005,0.01,0.015,0.02,0.025,0.03,0.035,0.04,0.045,0.05,0.055,0.06,0.065,
0.07,0.075,0.08,0.085,0.09,0.095,0.1,0.105,0.11,0.115,0.12,0.125,0.13,0.135,
0.14,0.145,0.15,0.155,0.16,0.165,0.17,0.175,0.18,0.185,0.19,0.195,0.2,0.205,
0.21,0.215,0.22,0.225,0.23,0.235,0.24,0.245,0.25,0.255,0.26,0.265,0.27,
0.275,0.28,0.285,0.29,0.295,0.3,0.305,0.31,0.315,0.32,0.325,0.33,0.335,
0.34,0.345,0.35,0.355,0.36,0.365,0.37,0.375,0.38,0.385,0.39,0.395,0.4,0.405,
0.41,0.415,0.42,0.425,0.43,0.435,0.44,0.445,0.45,0.455,0.46,0.465,0.47,
0.475,0.48,0.485,0.49,0.495,0.5,0.505,0.51,0.515,0.52,0.525,0.53,0.535,
0.54,0.545,0.55,0.555,0.56,0.565,0.57,0.575,0.58,0.585,0.59,0.595,0.6,0.605,
0.61,0.615,0.62,0.625,0.63,0.635,0.64,0.645,0.65,0.655,0.66,0.665,0.67,
0.675,0.68,0.685,0.690000000000001,0.695000000000001,0.700000000000001,
0.705000000000001,0.710000000000001,0.715000000000001,0.720000000000001,
0.725000000000001,0.730000000000001,0.735000000000001,0.740000000000001,
0.745000000000001,0.750000000000001,0.755000000000001,0.760000000000001,
0.765000000000001,0.770000000000001,0.775000000000001,0.780000000000001,
0.785000000000001,0.790000000000001,0.795000000000001,0.800000000000001,
0.805000000000001,0.810000000000001,0.815000000000001,0.820000000000001,
0.825000000000001,0.830000000000001,0.835000000000001,0.840000000000001,
0.845000000000001,0.850000000000001,0.855000000000001,0.860000000000001,
0.865000000000001,0.870000000000001,0.875000000000001,0.880000000000001,
0.885000000000001,0.890000000000001,0.895000000000001,0.900000000000001,
0.905000000000001,0.910000000000001,0.915000000000001,0.920000000000001,
0.925000000000001,0.930000000000001,0.935000000000001,0.940000000000001,
0.945000000000001,0.950000000000001,0.955000000000001,0.960000000000001,
0.965000000000001,0.970000000000001,0.975000000000001,0.980000000000001,
0.985000000000001,0.990000000000001,0.995000000000001,1.),.UNSPECIFIED.)
CURVE()
GEOMETRIC_REPRESENTATION_ITEM()
RATIONAL_B_SPLINE_CURVE((1.,1.,1.,1.,1.,1.,1.,1.,1.,1.,1.,1.,1.,1.,1.,1.,
1.,1.,1.,1.,1.,1.,1.,1.,1.,1.,1.,1.,1.,1.,1.,1.,1.,1.,1.,1.,1.,1.,1.,1.,
1.,1.,1.,1.,1.,1.,1.,1.,1.,1.,1.,1.,1.,1.,1.,1.,1.,1.,1.,1.,1.,1.,1.,1.,
1.,1.,1.,1.,1.,1.,1.,1.,1.,1.,1.,1.,1.,1.,1.,1.,1.,1.,1.,1.,1.,1.,1.,1.,
1.,1.,1.,1.,1.,1.,1.,1.,1.,1.,1.,1.,1.,1.,1.,1.,1.,1.,1.,1.,1.,1.,1.,1.,
1.,1.,1.,1.,1.,1.,1.,1.,1.,1.,1.,1.,1.,1.,1.,1.,1.,1.,1.,1.,1.,1.,1.,1.,
1.,1.,1.,1.,1.,1.,1.,1.,1.,1.,1.,1.,1.,1.,1.,1.,1.,1.,1.,1.,1.,1.,1.,1.,
1.,1.,1.,1.,1.,1.,1.,1.,1.,1.,1.,1.,1.,1.,1.,1.,1.,1.,1.,1.,1.,1.,1.,1.,
1.,1.,1.,1.,1.,1.,1.,1.,1.,1.,1.,1.,1.,1.,1.,1.,1.,1.,1.,1.,1.))
REPRESENTATION_ITEM('')
);
#704=(
BOUNDED_CURVE()
B_SPLINE_CURVE(5,(#177765,#177766,#177767,#177768,#177769,#177770,#177771,
#177772,#177773,#177774,#177775,#177776,#177777,#177778,#177779,#177780,
#177781,#177782,#177783,#177784,#177785,#177786,#177787,#177788,#177789,
#177790,#177791,#177792,#177793,#177794,#177795,#177796,#177797,#177798,
#177799,#177800,#177801,#177802,#177803,#177804,#177805,#177806,#177807,
#177808,#177809,#177810,#177811,#177812,#177813,#177814,#177815,#177816,
#177817,#177818,#177819,#177820,#177821,#177822,#177823,#177824,#177825,
#177826,#177827,#177828,#177829,#177830,#177831,#177832,#177833,#177834,
#177835,#177836,#177837,#177838,#177839,#177840,#177841,#177842,#177843,
#177844,#177845,#177846,#177847,#177848,#177849,#177850,#177851,#177852,
#177853,#177854,#177855,#177856,#177857,#177858,#177859,#177860,#177861,
#177862,#177863,#177864,#177865,#177866,#177867,#177868,#177869,#177870,
#177871,#177872,#177873,#177874,#177875,#177876,#177877,#177878,#177879,
#177880,#177881,#177882,#177883,#177884,#177885,#177886,#177887,#177888,
#177889,#177890,#177891,#177892,#177893,#177894,#177895,#177896,#177897,
#177898,#177899,#177900,#177901,#177902,#177903,#177904,#177905,#177906,
#177907,#177908,#177909,#177910,#177911,#177912,#177913,#177914,#177915,
#177916,#177917,#177918,#177919,#177920,#177921,#177922,#177923,#177924,
#177925,#177926,#177927,#177928,#177929,#177930,#177931,#177932,#177933,
#177934,#177935,#177936,#177937,#177938,#177939,#177940,#177941,#177942,
#177943,#177944,#177945,#177946,#177947,#177948,#177949,#177950,#177951,
#177952,#177953,#177954,#177955,#177956,#177957,#177958,#177959,#177960,
#177961,#177962,#177963,#177964,#177965,#177966,#177967,#177968,#177969),
 .UNSPECIFIED.,.F.,.F.)
B_SPLINE_CURVE_WITH_KNOTS((6,1,1,1,1,1,1,1,1,1,1,1,1,1,1,1,1,1,1,1,1,1,
1,1,1,1,1,1,1,1,1,1,1,1,1,1,1,1,1,1,1,1,1,1,1,1,1,1,1,1,1,1,1,1,1,1,1,1,
1,1,1,1,1,1,1,1,1,1,1,1,1,1,1,1,1,1,1,1,1,1,1,1,1,1,1,1,1,1,1,1,1,1,1,1,
1,1,1,1,1,1,1,1,1,1,1,1,1,1,1,1,1,1,1,1,1,1,1,1,1,1,1,1,1,1,1,1,1,1,1,1,
1,1,1,1,1,1,1,1,1,1,1,1,1,1,1,1,1,1,1,1,1,1,1,1,1,1,1,1,1,1,1,1,1,1,1,1,
1,1,1,1,1,1,1,1,1,1,1,1,1,1,1,1,1,1,1,1,1,1,1,1,1,1,1,1,1,1,1,1,1,1,6),
(-1.,-0.995000000000001,-0.990000000000001,-0.985000000000001,-0.980000000000001,
-0.975000000000001,-0.970000000000001,-0.965000000000001,-0.960000000000001,
-0.955000000000001,-0.950000000000001,-0.945000000000001,-0.940000000000001,
-0.935000000000001,-0.930000000000001,-0.925000000000001,-0.920000000000001,
-0.915000000000001,-0.910000000000001,-0.905000000000001,-0.900000000000001,
-0.895000000000001,-0.890000000000001,-0.885000000000001,-0.880000000000001,
-0.875000000000001,-0.870000000000001,-0.865000000000001,-0.860000000000001,
-0.855000000000001,-0.850000000000001,-0.845000000000001,-0.840000000000001,
-0.835000000000001,-0.830000000000001,-0.825000000000001,-0.820000000000001,
-0.815000000000001,-0.810000000000001,-0.805000000000001,-0.800000000000001,
-0.795000000000001,-0.790000000000001,-0.785000000000001,-0.780000000000001,
-0.775000000000001,-0.770000000000001,-0.765000000000001,-0.760000000000001,
-0.755000000000001,-0.750000000000001,-0.745000000000001,-0.740000000000001,
-0.735000000000001,-0.730000000000001,-0.725000000000001,-0.720000000000001,
-0.715000000000001,-0.710000000000001,-0.705000000000001,-0.700000000000001,
-0.695000000000001,-0.690000000000001,-0.685,-0.68,-0.675,-0.67,-0.665,
-0.66,-0.655,-0.65,-0.645,-0.64,-0.635,-0.63,-0.625,-0.62,-0.615,-0.61,
-0.605,-0.6,-0.595,-0.59,-0.585,-0.58,-0.575,-0.57,-0.565,-0.56,-0.555,
-0.55,-0.545,-0.54,-0.535,-0.53,-0.525,-0.52,-0.515,-0.51,-0.505,-0.5,-0.495,
-0.49,-0.485,-0.48,-0.475,-0.47,-0.465,-0.46,-0.455,-0.45,-0.445,-0.44,
-0.435,-0.43,-0.425,-0.42,-0.415,-0.41,-0.405,-0.4,-0.395,-0.39,-0.385,
-0.38,-0.375,-0.37,-0.365,-0.36,-0.355,-0.35,-0.345,-0.34,-0.335,-0.33,
-0.325,-0.32,-0.315,-0.31,-0.305,-0.3,-0.295,-0.29,-0.285,-0.28,-0.275,
-0.27,-0.265,-0.26,-0.255,-0.25,-0.245,-0.24,-0.235,-0.23,-0.225,-0.22,
-0.215,-0.21,-0.205,-0.2,-0.195,-0.19,-0.185,-0.18,-0.175,-0.17,-0.165,
-0.16,-0.155,-0.15,-0.145,-0.14,-0.135,-0.13,-0.125,-0.12,-0.115,-0.11,
-0.105,-0.1,-0.095,-0.09,-0.085,-0.08,-0.075,-0.07,-0.065,-0.06,-0.055,
-0.05,-0.045,-0.04,-0.035,-0.03,-0.025,-0.02,-0.015,-0.01,-0.005,0.),
 .UNSPECIFIED.)
CURVE()
GEOMETRIC_REPRESENTATION_ITEM()
RATIONAL_B_SPLINE_CURVE((1.,1.,1.,1.,1.,1.,1.,1.,1.,1.,1.,1.,1.,1.,1.,1.,
1.,1.,1.,1.,1.,1.,1.,1.,1.,1.,1.,1.,1.,1.,1.,1.,1.,1.,1.,1.,1.,1.,1.,1.,
1.,1.,1.,1.,1.,1.,1.,1.,1.,1.,1.,1.,1.,1.,1.,1.,1.,1.,1.,1.,1.,1.,1.,1.,
1.,1.,1.,1.,1.,1.,1.,1.,1.,1.,1.,1.,1.,1.,1.,1.,1.,1.,1.,1.,1.,1.,1.,1.,
1.,1.,1.,1.,1.,1.,1.,1.,1.,1.,1.,1.,1.,1.,1.,1.,1.,1.,1.,1.,1.,1.,1.,1.,
1.,1.,1.,1.,1.,1.,1.,1.,1.,1.,1.,1.,1.,1.,1.,1.,1.,1.,1.,1.,1.,1.,1.,1.,
1.,1.,1.,1.,1.,1.,1.,1.,1.,1.,1.,1.,1.,1.,1.,1.,1.,1.,1.,1.,1.,1.,1.,1.,
1.,1.,1.,1.,1.,1.,1.,1.,1.,1.,1.,1.,1.,1.,1.,1.,1.,1.,1.,1.,1.,1.,1.,1.,
1.,1.,1.,1.,1.,1.,1.,1.,1.,1.,1.,1.,1.,1.,1.,1.,1.,1.,1.,1.,1.))
REPRESENTATION_ITEM('')
);
#705=(
BOUNDED_CURVE()
B_SPLINE_CURVE(5,(#177981,#177982,#177983,#177984,#177985,#177986,#177987,
#177988,#177989,#177990,#177991,#177992,#177993,#177994,#177995,#177996,
#177997,#177998,#177999,#178000,#178001,#178002,#178003,#178004,#178005,
#178006,#178007,#178008,#178009,#178010,#178011,#178012,#178013,#178014,
#178015,#178016,#178017,#178018,#178019,#178020,#178021,#178022,#178023,
#178024,#178025,#178026,#178027,#178028,#178029,#178030,#178031,#178032,
#178033,#178034,#178035,#178036,#178037,#178038,#178039,#178040,#178041,
#178042,#178043,#178044,#178045,#178046,#178047,#178048,#178049,#178050,
#178051,#178052,#178053,#178054,#178055,#178056,#178057,#178058,#178059,
#178060,#178061,#178062,#178063,#178064,#178065,#178066,#178067,#178068,
#178069,#178070,#178071,#178072,#178073,#178074,#178075,#178076,#178077,
#178078,#178079,#178080,#178081,#178082,#178083,#178084,#178085,#178086,
#178087,#178088,#178089,#178090,#178091,#178092,#178093,#178094,#178095,
#178096,#178097,#178098,#178099,#178100,#178101,#178102,#178103,#178104,
#178105,#178106,#178107,#178108,#178109,#178110,#178111,#178112,#178113,
#178114,#178115,#178116,#178117,#178118,#178119,#178120,#178121,#178122,
#178123,#178124,#178125,#178126,#178127,#178128,#178129,#178130,#178131,
#178132,#178133,#178134,#178135,#178136,#178137,#178138,#178139,#178140,
#178141,#178142,#178143,#178144,#178145,#178146,#178147,#178148,#178149,
#178150,#178151,#178152,#178153,#178154,#178155,#178156,#178157,#178158,
#178159,#178160,#178161,#178162,#178163,#178164,#178165,#178166,#178167,
#178168,#178169,#178170,#178171,#178172,#178173,#178174,#178175,#178176,
#178177,#178178,#178179,#178180,#178181,#178182,#178183,#178184,#178185),
 .UNSPECIFIED.,.F.,.F.)
B_SPLINE_CURVE_WITH_KNOTS((6,1,1,1,1,1,1,1,1,1,1,1,1,1,1,1,1,1,1,1,1,1,
1,1,1,1,1,1,1,1,1,1,1,1,1,1,1,1,1,1,1,1,1,1,1,1,1,1,1,1,1,1,1,1,1,1,1,1,
1,1,1,1,1,1,1,1,1,1,1,1,1,1,1,1,1,1,1,1,1,1,1,1,1,1,1,1,1,1,1,1,1,1,1,1,
1,1,1,1,1,1,1,1,1,1,1,1,1,1,1,1,1,1,1,1,1,1,1,1,1,1,1,1,1,1,1,1,1,1,1,1,
1,1,1,1,1,1,1,1,1,1,1,1,1,1,1,1,1,1,1,1,1,1,1,1,1,1,1,1,1,1,1,1,1,1,1,1,
1,1,1,1,1,1,1,1,1,1,1,1,1,1,1,1,1,1,1,1,1,1,1,1,1,1,1,1,1,1,1,1,1,1,6),
(0.,0.005,0.01,0.015,0.02,0.025,0.03,0.035,0.04,0.045,0.05,0.055,0.06,0.065,
0.07,0.075,0.08,0.085,0.09,0.095,0.1,0.105,0.11,0.115,0.12,0.125,0.13,0.135,
0.14,0.145,0.15,0.155,0.16,0.165,0.17,0.175,0.18,0.185,0.19,0.195,0.2,0.205,
0.21,0.215,0.22,0.225,0.23,0.235,0.24,0.245,0.25,0.255,0.26,0.265,0.27,
0.275,0.28,0.285,0.29,0.295,0.3,0.305,0.31,0.315,0.32,0.325,0.33,0.335,
0.34,0.345,0.35,0.355,0.36,0.365,0.37,0.375,0.38,0.385,0.39,0.395,0.4,0.405,
0.41,0.415,0.42,0.425,0.43,0.435,0.44,0.445,0.45,0.455,0.46,0.465,0.47,
0.475,0.48,0.485,0.49,0.495,0.5,0.505,0.51,0.515,0.52,0.525,0.53,0.535,
0.54,0.545,0.55,0.555,0.56,0.565,0.57,0.575,0.58,0.585,0.59,0.595,0.6,0.605,
0.61,0.615,0.62,0.625,0.63,0.635,0.64,0.645,0.65,0.655,0.66,0.665,0.67,
0.675,0.68,0.685,0.690000000000001,0.695000000000001,0.700000000000001,
0.705000000000001,0.710000000000001,0.715000000000001,0.720000000000001,
0.725000000000001,0.730000000000001,0.735000000000001,0.740000000000001,
0.745000000000001,0.750000000000001,0.755000000000001,0.760000000000001,
0.765000000000001,0.770000000000001,0.775000000000001,0.780000000000001,
0.785000000000001,0.790000000000001,0.795000000000001,0.800000000000001,
0.805000000000001,0.810000000000001,0.815000000000001,0.820000000000001,
0.825000000000001,0.830000000000001,0.835000000000001,0.840000000000001,
0.845000000000001,0.850000000000001,0.855000000000001,0.860000000000001,
0.865000000000001,0.870000000000001,0.875000000000001,0.880000000000001,
0.885000000000001,0.890000000000001,0.895000000000001,0.900000000000001,
0.905000000000001,0.910000000000001,0.915000000000001,0.920000000000001,
0.925000000000001,0.930000000000001,0.935000000000001,0.940000000000001,
0.945000000000001,0.950000000000001,0.955000000000001,0.960000000000001,
0.965000000000001,0.970000000000001,0.975000000000001,0.980000000000001,
0.985000000000001,0.990000000000001,0.995000000000001,1.),.UNSPECIFIED.)
CURVE()
GEOMETRIC_REPRESENTATION_ITEM()
RATIONAL_B_SPLINE_CURVE((1.,1.,1.,1.,1.,1.,1.,1.,1.,1.,1.,1.,1.,1.,1.,1.,
1.,1.,1.,1.,1.,1.,1.,1.,1.,1.,1.,1.,1.,1.,1.,1.,1.,1.,1.,1.,1.,1.,1.,1.,
1.,1.,1.,1.,1.,1.,1.,1.,1.,1.,1.,1.,1.,1.,1.,1.,1.,1.,1.,1.,1.,1.,1.,1.,
1.,1.,1.,1.,1.,1.,1.,1.,1.,1.,1.,1.,1.,1.,1.,1.,1.,1.,1.,1.,1.,1.,1.,1.,
1.,1.,1.,1.,1.,1.,1.,1.,1.,1.,1.,1.,1.,1.,1.,1.,1.,1.,1.,1.,1.,1.,1.,1.,
1.,1.,1.,1.,1.,1.,1.,1.,1.,1.,1.,1.,1.,1.,1.,1.,1.,1.,1.,1.,1.,1.,1.,1.,
1.,1.,1.,1.,1.,1.,1.,1.,1.,1.,1.,1.,1.,1.,1.,1.,1.,1.,1.,1.,1.,1.,1.,1.,
1.,1.,1.,1.,1.,1.,1.,1.,1.,1.,1.,1.,1.,1.,1.,1.,1.,1.,1.,1.,1.,1.,1.,1.,
1.,1.,1.,1.,1.,1.,1.,1.,1.,1.,1.,1.,1.,1.,1.,1.,1.,1.,1.,1.,1.))
REPRESENTATION_ITEM('')
);
#706=(
BOUNDED_CURVE()
B_SPLINE_CURVE(5,(#178189,#178190,#178191,#178192,#178193,#178194,#178195,
#178196,#178197,#178198,#178199,#178200,#178201,#178202,#178203,#178204,
#178205,#178206,#178207,#178208,#178209,#178210,#178211,#178212,#178213,
#178214,#178215,#178216,#178217,#178218,#178219,#178220,#178221,#178222,
#178223,#178224,#178225,#178226,#178227,#178228,#178229,#178230,#178231,
#178232,#178233,#178234,#178235,#178236,#178237,#178238,#178239,#178240,
#178241,#178242,#178243,#178244,#178245,#178246,#178247,#178248,#178249,
#178250,#178251,#178252,#178253,#178254,#178255,#178256,#178257,#178258,
#178259,#178260,#178261,#178262,#178263,#178264,#178265,#178266,#178267,
#178268,#178269,#178270,#178271,#178272,#178273,#178274,#178275,#178276,
#178277,#178278,#178279,#178280,#178281,#178282,#178283,#178284,#178285,
#178286,#178287,#178288,#178289,#178290,#178291,#178292,#178293,#178294,
#178295,#178296,#178297,#178298,#178299,#178300,#178301,#178302,#178303,
#178304,#178305,#178306,#178307,#178308,#178309,#178310,#178311,#178312,
#178313,#178314,#178315,#178316,#178317,#178318,#178319,#178320,#178321,
#178322,#178323,#178324,#178325,#178326,#178327,#178328,#178329,#178330,
#178331,#178332,#178333,#178334,#178335,#178336,#178337,#178338,#178339,
#178340,#178341,#178342,#178343,#178344,#178345,#178346,#178347,#178348,
#178349,#178350,#178351,#178352,#178353,#178354,#178355,#178356,#178357,
#178358,#178359,#178360,#178361,#178362,#178363,#178364,#178365,#178366,
#178367,#178368,#178369,#178370,#178371,#178372,#178373,#178374,#178375,
#178376,#178377,#178378,#178379,#178380,#178381,#178382,#178383,#178384,
#178385,#178386,#178387,#178388,#178389,#178390,#178391,#178392,#178393),
 .UNSPECIFIED.,.F.,.F.)
B_SPLINE_CURVE_WITH_KNOTS((6,1,1,1,1,1,1,1,1,1,1,1,1,1,1,1,1,1,1,1,1,1,
1,1,1,1,1,1,1,1,1,1,1,1,1,1,1,1,1,1,1,1,1,1,1,1,1,1,1,1,1,1,1,1,1,1,1,1,
1,1,1,1,1,1,1,1,1,1,1,1,1,1,1,1,1,1,1,1,1,1,1,1,1,1,1,1,1,1,1,1,1,1,1,1,
1,1,1,1,1,1,1,1,1,1,1,1,1,1,1,1,1,1,1,1,1,1,1,1,1,1,1,1,1,1,1,1,1,1,1,1,
1,1,1,1,1,1,1,1,1,1,1,1,1,1,1,1,1,1,1,1,1,1,1,1,1,1,1,1,1,1,1,1,1,1,1,1,
1,1,1,1,1,1,1,1,1,1,1,1,1,1,1,1,1,1,1,1,1,1,1,1,1,1,1,1,1,1,1,1,1,1,6),
(-1.,-0.995000000000001,-0.990000000000001,-0.985000000000001,-0.980000000000001,
-0.975000000000001,-0.970000000000001,-0.965000000000001,-0.960000000000001,
-0.955000000000001,-0.950000000000001,-0.945000000000001,-0.940000000000001,
-0.935000000000001,-0.930000000000001,-0.925000000000001,-0.920000000000001,
-0.915000000000001,-0.910000000000001,-0.905000000000001,-0.900000000000001,
-0.895000000000001,-0.890000000000001,-0.885000000000001,-0.880000000000001,
-0.875000000000001,-0.870000000000001,-0.865000000000001,-0.860000000000001,
-0.855000000000001,-0.850000000000001,-0.845000000000001,-0.840000000000001,
-0.835000000000001,-0.830000000000001,-0.825000000000001,-0.820000000000001,
-0.815000000000001,-0.810000000000001,-0.805000000000001,-0.800000000000001,
-0.795000000000001,-0.790000000000001,-0.785000000000001,-0.780000000000001,
-0.775000000000001,-0.770000000000001,-0.765000000000001,-0.760000000000001,
-0.755000000000001,-0.750000000000001,-0.745000000000001,-0.740000000000001,
-0.735000000000001,-0.730000000000001,-0.725000000000001,-0.720000000000001,
-0.715000000000001,-0.710000000000001,-0.705000000000001,-0.700000000000001,
-0.695000000000001,-0.690000000000001,-0.685,-0.68,-0.675,-0.67,-0.665,
-0.66,-0.655,-0.65,-0.645,-0.64,-0.635,-0.63,-0.625,-0.62,-0.615,-0.61,
-0.605,-0.6,-0.595,-0.59,-0.585,-0.58,-0.575,-0.57,-0.565,-0.56,-0.555,
-0.55,-0.545,-0.54,-0.535,-0.53,-0.525,-0.52,-0.515,-0.51,-0.505,-0.5,-0.495,
-0.49,-0.485,-0.48,-0.475,-0.47,-0.465,-0.46,-0.455,-0.45,-0.445,-0.44,
-0.435,-0.43,-0.425,-0.42,-0.415,-0.41,-0.405,-0.4,-0.395,-0.39,-0.385,
-0.38,-0.375,-0.37,-0.365,-0.36,-0.355,-0.35,-0.345,-0.34,-0.335,-0.33,
-0.325,-0.32,-0.315,-0.31,-0.305,-0.3,-0.295,-0.29,-0.285,-0.28,-0.275,
-0.27,-0.265,-0.26,-0.255,-0.25,-0.245,-0.24,-0.235,-0.23,-0.225,-0.22,
-0.215,-0.21,-0.205,-0.2,-0.195,-0.19,-0.185,-0.18,-0.175,-0.17,-0.165,
-0.16,-0.155,-0.15,-0.145,-0.14,-0.135,-0.13,-0.125,-0.12,-0.115,-0.11,
-0.105,-0.1,-0.095,-0.09,-0.085,-0.08,-0.075,-0.07,-0.065,-0.06,-0.055,
-0.05,-0.045,-0.04,-0.035,-0.03,-0.025,-0.02,-0.015,-0.01,-0.005,0.),
 .UNSPECIFIED.)
CURVE()
GEOMETRIC_REPRESENTATION_ITEM()
RATIONAL_B_SPLINE_CURVE((1.,1.,1.,1.,1.,1.,1.,1.,1.,1.,1.,1.,1.,1.,1.,1.,
1.,1.,1.,1.,1.,1.,1.,1.,1.,1.,1.,1.,1.,1.,1.,1.,1.,1.,1.,1.,1.,1.,1.,1.,
1.,1.,1.,1.,1.,1.,1.,1.,1.,1.,1.,1.,1.,1.,1.,1.,1.,1.,1.,1.,1.,1.,1.,1.,
1.,1.,1.,1.,1.,1.,1.,1.,1.,1.,1.,1.,1.,1.,1.,1.,1.,1.,1.,1.,1.,1.,1.,1.,
1.,1.,1.,1.,1.,1.,1.,1.,1.,1.,1.,1.,1.,1.,1.,1.,1.,1.,1.,1.,1.,1.,1.,1.,
1.,1.,1.,1.,1.,1.,1.,1.,1.,1.,1.,1.,1.,1.,1.,1.,1.,1.,1.,1.,1.,1.,1.,1.,
1.,1.,1.,1.,1.,1.,1.,1.,1.,1.,1.,1.,1.,1.,1.,1.,1.,1.,1.,1.,1.,1.,1.,1.,
1.,1.,1.,1.,1.,1.,1.,1.,1.,1.,1.,1.,1.,1.,1.,1.,1.,1.,1.,1.,1.,1.,1.,1.,
1.,1.,1.,1.,1.,1.,1.,1.,1.,1.,1.,1.,1.,1.,1.,1.,1.,1.,1.,1.,1.))
REPRESENTATION_ITEM('')
);
#707=(
BOUNDED_CURVE()
B_SPLINE_CURVE(5,(#178405,#178406,#178407,#178408,#178409,#178410,#178411,
#178412,#178413,#178414,#178415,#178416,#178417,#178418,#178419,#178420,
#178421,#178422,#178423,#178424,#178425,#178426,#178427,#178428,#178429,
#178430,#178431,#178432,#178433,#178434,#178435,#178436,#178437,#178438,
#178439,#178440,#178441,#178442,#178443,#178444,#178445,#178446,#178447,
#178448,#178449,#178450,#178451,#178452,#178453,#178454,#178455,#178456,
#178457,#178458,#178459,#178460,#178461,#178462,#178463,#178464,#178465,
#178466,#178467,#178468,#178469,#178470,#178471,#178472,#178473,#178474,
#178475,#178476,#178477,#178478,#178479,#178480,#178481,#178482,#178483,
#178484,#178485,#178486,#178487,#178488,#178489,#178490,#178491,#178492,
#178493,#178494,#178495,#178496,#178497,#178498,#178499,#178500,#178501,
#178502,#178503,#178504,#178505,#178506,#178507,#178508,#178509,#178510,
#178511,#178512,#178513,#178514,#178515,#178516,#178517,#178518,#178519,
#178520,#178521,#178522,#178523,#178524,#178525,#178526,#178527,#178528,
#178529,#178530,#178531,#178532,#178533,#178534,#178535,#178536,#178537,
#178538,#178539,#178540,#178541,#178542,#178543,#178544,#178545,#178546,
#178547,#178548,#178549,#178550,#178551,#178552,#178553,#178554,#178555,
#178556,#178557,#178558,#178559,#178560,#178561,#178562,#178563,#178564,
#178565,#178566,#178567,#178568,#178569,#178570,#178571,#178572,#178573,
#178574,#178575,#178576,#178577,#178578,#178579,#178580,#178581,#178582,
#178583,#178584,#178585,#178586,#178587,#178588,#178589,#178590,#178591,
#178592,#178593,#178594,#178595,#178596,#178597,#178598,#178599,#178600,
#178601,#178602,#178603,#178604,#178605,#178606,#178607,#178608,#178609),
 .UNSPECIFIED.,.F.,.F.)
B_SPLINE_CURVE_WITH_KNOTS((6,1,1,1,1,1,1,1,1,1,1,1,1,1,1,1,1,1,1,1,1,1,
1,1,1,1,1,1,1,1,1,1,1,1,1,1,1,1,1,1,1,1,1,1,1,1,1,1,1,1,1,1,1,1,1,1,1,1,
1,1,1,1,1,1,1,1,1,1,1,1,1,1,1,1,1,1,1,1,1,1,1,1,1,1,1,1,1,1,1,1,1,1,1,1,
1,1,1,1,1,1,1,1,1,1,1,1,1,1,1,1,1,1,1,1,1,1,1,1,1,1,1,1,1,1,1,1,1,1,1,1,
1,1,1,1,1,1,1,1,1,1,1,1,1,1,1,1,1,1,1,1,1,1,1,1,1,1,1,1,1,1,1,1,1,1,1,1,
1,1,1,1,1,1,1,1,1,1,1,1,1,1,1,1,1,1,1,1,1,1,1,1,1,1,1,1,1,1,1,1,1,1,6),
(0.,0.005,0.01,0.015,0.02,0.025,0.03,0.035,0.04,0.045,0.05,0.055,0.06,0.065,
0.07,0.075,0.08,0.085,0.09,0.095,0.1,0.105,0.11,0.115,0.12,0.125,0.13,0.135,
0.14,0.145,0.15,0.155,0.16,0.165,0.17,0.175,0.18,0.185,0.19,0.195,0.2,0.205,
0.21,0.215,0.22,0.225,0.23,0.235,0.24,0.245,0.25,0.255,0.26,0.265,0.27,
0.275,0.28,0.285,0.29,0.295,0.3,0.305,0.31,0.315,0.32,0.325,0.33,0.335,
0.34,0.345,0.35,0.355,0.36,0.365,0.37,0.375,0.38,0.385,0.39,0.395,0.4,0.405,
0.41,0.415,0.42,0.425,0.43,0.435,0.44,0.445,0.45,0.455,0.46,0.465,0.47,
0.475,0.48,0.485,0.49,0.495,0.5,0.505,0.51,0.515,0.52,0.525,0.53,0.535,
0.54,0.545,0.55,0.555,0.56,0.565,0.57,0.575,0.58,0.585,0.59,0.595,0.6,0.605,
0.61,0.615,0.62,0.625,0.63,0.635,0.64,0.645,0.65,0.655,0.66,0.665,0.67,
0.675,0.68,0.685,0.690000000000001,0.695000000000001,0.700000000000001,
0.705000000000001,0.710000000000001,0.715000000000001,0.720000000000001,
0.725000000000001,0.730000000000001,0.735000000000001,0.740000000000001,
0.745000000000001,0.750000000000001,0.755000000000001,0.760000000000001,
0.765000000000001,0.770000000000001,0.775000000000001,0.780000000000001,
0.785000000000001,0.790000000000001,0.795000000000001,0.800000000000001,
0.805000000000001,0.810000000000001,0.815000000000001,0.820000000000001,
0.825000000000001,0.830000000000001,0.835000000000001,0.840000000000001,
0.845000000000001,0.850000000000001,0.855000000000001,0.860000000000001,
0.865000000000001,0.870000000000001,0.875000000000001,0.880000000000001,
0.885000000000001,0.890000000000001,0.895000000000001,0.900000000000001,
0.905000000000001,0.910000000000001,0.915000000000001,0.920000000000001,
0.925000000000001,0.930000000000001,0.935000000000001,0.940000000000001,
0.945000000000001,0.950000000000001,0.955000000000001,0.960000000000001,
0.965000000000001,0.970000000000001,0.975000000000001,0.980000000000001,
0.985000000000001,0.990000000000001,0.995000000000001,1.),.UNSPECIFIED.)
CURVE()
GEOMETRIC_REPRESENTATION_ITEM()
RATIONAL_B_SPLINE_CURVE((1.,1.,1.,1.,1.,1.,1.,1.,1.,1.,1.,1.,1.,1.,1.,1.,
1.,1.,1.,1.,1.,1.,1.,1.,1.,1.,1.,1.,1.,1.,1.,1.,1.,1.,1.,1.,1.,1.,1.,1.,
1.,1.,1.,1.,1.,1.,1.,1.,1.,1.,1.,1.,1.,1.,1.,1.,1.,1.,1.,1.,1.,1.,1.,1.,
1.,1.,1.,1.,1.,1.,1.,1.,1.,1.,1.,1.,1.,1.,1.,1.,1.,1.,1.,1.,1.,1.,1.,1.,
1.,1.,1.,1.,1.,1.,1.,1.,1.,1.,1.,1.,1.,1.,1.,1.,1.,1.,1.,1.,1.,1.,1.,1.,
1.,1.,1.,1.,1.,1.,1.,1.,1.,1.,1.,1.,1.,1.,1.,1.,1.,1.,1.,1.,1.,1.,1.,1.,
1.,1.,1.,1.,1.,1.,1.,1.,1.,1.,1.,1.,1.,1.,1.,1.,1.,1.,1.,1.,1.,1.,1.,1.,
1.,1.,1.,1.,1.,1.,1.,1.,1.,1.,1.,1.,1.,1.,1.,1.,1.,1.,1.,1.,1.,1.,1.,1.,
1.,1.,1.,1.,1.,1.,1.,1.,1.,1.,1.,1.,1.,1.,1.,1.,1.,1.,1.,1.,1.))
REPRESENTATION_ITEM('')
);
#708=(
BOUNDED_CURVE()
B_SPLINE_CURVE(5,(#178613,#178614,#178615,#178616,#178617,#178618,#178619,
#178620,#178621,#178622,#178623,#178624,#178625,#178626,#178627,#178628,
#178629,#178630,#178631,#178632,#178633,#178634,#178635,#178636,#178637,
#178638,#178639,#178640,#178641,#178642,#178643,#178644,#178645,#178646,
#178647,#178648,#178649,#178650,#178651,#178652,#178653,#178654,#178655,
#178656,#178657,#178658,#178659,#178660,#178661,#178662,#178663,#178664,
#178665,#178666,#178667,#178668,#178669,#178670,#178671,#178672,#178673,
#178674,#178675,#178676,#178677,#178678,#178679,#178680,#178681,#178682,
#178683,#178684,#178685,#178686,#178687,#178688,#178689,#178690,#178691,
#178692,#178693,#178694,#178695,#178696,#178697,#178698,#178699,#178700,
#178701,#178702,#178703,#178704,#178705,#178706,#178707,#178708,#178709,
#178710,#178711,#178712,#178713,#178714,#178715,#178716,#178717,#178718,
#178719,#178720,#178721,#178722,#178723,#178724,#178725,#178726,#178727,
#178728,#178729,#178730,#178731,#178732,#178733,#178734,#178735,#178736,
#178737,#178738,#178739,#178740,#178741,#178742,#178743,#178744,#178745,
#178746,#178747,#178748,#178749,#178750,#178751,#178752,#178753,#178754,
#178755,#178756,#178757,#178758,#178759,#178760,#178761,#178762,#178763,
#178764,#178765,#178766,#178767,#178768,#178769,#178770,#178771,#178772,
#178773,#178774,#178775,#178776,#178777,#178778,#178779,#178780,#178781,
#178782,#178783,#178784,#178785,#178786,#178787,#178788,#178789,#178790,
#178791,#178792,#178793,#178794,#178795,#178796,#178797,#178798,#178799,
#178800,#178801,#178802,#178803,#178804,#178805,#178806,#178807,#178808,
#178809,#178810,#178811,#178812,#178813,#178814,#178815,#178816,#178817),
 .UNSPECIFIED.,.F.,.F.)
B_SPLINE_CURVE_WITH_KNOTS((6,1,1,1,1,1,1,1,1,1,1,1,1,1,1,1,1,1,1,1,1,1,
1,1,1,1,1,1,1,1,1,1,1,1,1,1,1,1,1,1,1,1,1,1,1,1,1,1,1,1,1,1,1,1,1,1,1,1,
1,1,1,1,1,1,1,1,1,1,1,1,1,1,1,1,1,1,1,1,1,1,1,1,1,1,1,1,1,1,1,1,1,1,1,1,
1,1,1,1,1,1,1,1,1,1,1,1,1,1,1,1,1,1,1,1,1,1,1,1,1,1,1,1,1,1,1,1,1,1,1,1,
1,1,1,1,1,1,1,1,1,1,1,1,1,1,1,1,1,1,1,1,1,1,1,1,1,1,1,1,1,1,1,1,1,1,1,1,
1,1,1,1,1,1,1,1,1,1,1,1,1,1,1,1,1,1,1,1,1,1,1,1,1,1,1,1,1,1,1,1,1,1,6),
(-1.,-0.995000000000001,-0.990000000000001,-0.985000000000001,-0.980000000000001,
-0.975000000000001,-0.970000000000001,-0.965000000000001,-0.960000000000001,
-0.955000000000001,-0.950000000000001,-0.945000000000001,-0.940000000000001,
-0.935000000000001,-0.930000000000001,-0.925000000000001,-0.920000000000001,
-0.915000000000001,-0.910000000000001,-0.905000000000001,-0.900000000000001,
-0.895000000000001,-0.890000000000001,-0.885000000000001,-0.880000000000001,
-0.875000000000001,-0.870000000000001,-0.865000000000001,-0.860000000000001,
-0.855000000000001,-0.850000000000001,-0.845000000000001,-0.840000000000001,
-0.835000000000001,-0.830000000000001,-0.825000000000001,-0.820000000000001,
-0.815000000000001,-0.810000000000001,-0.805000000000001,-0.800000000000001,
-0.795000000000001,-0.790000000000001,-0.785000000000001,-0.780000000000001,
-0.775000000000001,-0.770000000000001,-0.765000000000001,-0.760000000000001,
-0.755000000000001,-0.750000000000001,-0.745000000000001,-0.740000000000001,
-0.735000000000001,-0.730000000000001,-0.725000000000001,-0.720000000000001,
-0.715000000000001,-0.710000000000001,-0.705000000000001,-0.700000000000001,
-0.695000000000001,-0.690000000000001,-0.685,-0.68,-0.675,-0.67,-0.665,
-0.66,-0.655,-0.65,-0.645,-0.64,-0.635,-0.63,-0.625,-0.62,-0.615,-0.61,
-0.605,-0.6,-0.595,-0.59,-0.585,-0.58,-0.575,-0.57,-0.565,-0.56,-0.555,
-0.55,-0.545,-0.54,-0.535,-0.53,-0.525,-0.52,-0.515,-0.51,-0.505,-0.5,-0.495,
-0.49,-0.485,-0.48,-0.475,-0.47,-0.465,-0.46,-0.455,-0.45,-0.445,-0.44,
-0.435,-0.43,-0.425,-0.42,-0.415,-0.41,-0.405,-0.4,-0.395,-0.39,-0.385,
-0.38,-0.375,-0.37,-0.365,-0.36,-0.355,-0.35,-0.345,-0.34,-0.335,-0.33,
-0.325,-0.32,-0.315,-0.31,-0.305,-0.3,-0.295,-0.29,-0.285,-0.28,-0.275,
-0.27,-0.265,-0.26,-0.255,-0.25,-0.245,-0.24,-0.235,-0.23,-0.225,-0.22,
-0.215,-0.21,-0.205,-0.2,-0.195,-0.19,-0.185,-0.18,-0.175,-0.17,-0.165,
-0.16,-0.155,-0.15,-0.145,-0.14,-0.135,-0.13,-0.125,-0.12,-0.115,-0.11,
-0.105,-0.1,-0.095,-0.09,-0.085,-0.08,-0.075,-0.07,-0.065,-0.06,-0.055,
-0.05,-0.045,-0.04,-0.035,-0.03,-0.025,-0.02,-0.015,-0.01,-0.005,0.),
 .UNSPECIFIED.)
CURVE()
GEOMETRIC_REPRESENTATION_ITEM()
RATIONAL_B_SPLINE_CURVE((1.,1.,1.,1.,1.,1.,1.,1.,1.,1.,1.,1.,1.,1.,1.,1.,
1.,1.,1.,1.,1.,1.,1.,1.,1.,1.,1.,1.,1.,1.,1.,1.,1.,1.,1.,1.,1.,1.,1.,1.,
1.,1.,1.,1.,1.,1.,1.,1.,1.,1.,1.,1.,1.,1.,1.,1.,1.,1.,1.,1.,1.,1.,1.,1.,
1.,1.,1.,1.,1.,1.,1.,1.,1.,1.,1.,1.,1.,1.,1.,1.,1.,1.,1.,1.,1.,1.,1.,1.,
1.,1.,1.,1.,1.,1.,1.,1.,1.,1.,1.,1.,1.,1.,1.,1.,1.,1.,1.,1.,1.,1.,1.,1.,
1.,1.,1.,1.,1.,1.,1.,1.,1.,1.,1.,1.,1.,1.,1.,1.,1.,1.,1.,1.,1.,1.,1.,1.,
1.,1.,1.,1.,1.,1.,1.,1.,1.,1.,1.,1.,1.,1.,1.,1.,1.,1.,1.,1.,1.,1.,1.,1.,
1.,1.,1.,1.,1.,1.,1.,1.,1.,1.,1.,1.,1.,1.,1.,1.,1.,1.,1.,1.,1.,1.,1.,1.,
1.,1.,1.,1.,1.,1.,1.,1.,1.,1.,1.,1.,1.,1.,1.,1.,1.,1.,1.,1.,1.))
REPRESENTATION_ITEM('')
);
#709=(
BOUNDED_CURVE()
B_SPLINE_CURVE(5,(#178829,#178830,#178831,#178832,#178833,#178834,#178835,
#178836,#178837,#178838,#178839,#178840,#178841,#178842,#178843,#178844,
#178845,#178846,#178847,#178848,#178849,#178850,#178851,#178852,#178853,
#178854,#178855,#178856,#178857,#178858,#178859,#178860,#178861,#178862,
#178863,#178864,#178865,#178866,#178867,#178868,#178869,#178870,#178871,
#178872,#178873,#178874,#178875,#178876,#178877,#178878,#178879,#178880,
#178881,#178882,#178883,#178884,#178885,#178886,#178887,#178888,#178889,
#178890,#178891,#178892,#178893,#178894,#178895,#178896,#178897,#178898,
#178899,#178900,#178901,#178902,#178903,#178904,#178905,#178906,#178907,
#178908,#178909,#178910,#178911,#178912,#178913,#178914,#178915,#178916,
#178917,#178918,#178919,#178920,#178921,#178922,#178923,#178924,#178925,
#178926,#178927,#178928,#178929,#178930,#178931,#178932,#178933,#178934,
#178935,#178936,#178937,#178938,#178939,#178940,#178941,#178942,#178943,
#178944,#178945,#178946,#178947,#178948,#178949,#178950,#178951,#178952,
#178953,#178954,#178955,#178956,#178957,#178958,#178959,#178960,#178961,
#178962,#178963,#178964,#178965,#178966,#178967,#178968,#178969,#178970,
#178971,#178972,#178973,#178974,#178975,#178976,#178977,#178978,#178979,
#178980,#178981,#178982,#178983,#178984,#178985,#178986,#178987,#178988,
#178989,#178990,#178991,#178992,#178993,#178994,#178995,#178996,#178997,
#178998,#178999,#179000,#179001,#179002,#179003,#179004,#179005,#179006,
#179007,#179008,#179009,#179010,#179011,#179012,#179013,#179014,#179015,
#179016,#179017,#179018,#179019,#179020,#179021,#179022,#179023,#179024,
#179025,#179026,#179027,#179028,#179029,#179030,#179031,#179032,#179033),
 .UNSPECIFIED.,.F.,.F.)
B_SPLINE_CURVE_WITH_KNOTS((6,1,1,1,1,1,1,1,1,1,1,1,1,1,1,1,1,1,1,1,1,1,
1,1,1,1,1,1,1,1,1,1,1,1,1,1,1,1,1,1,1,1,1,1,1,1,1,1,1,1,1,1,1,1,1,1,1,1,
1,1,1,1,1,1,1,1,1,1,1,1,1,1,1,1,1,1,1,1,1,1,1,1,1,1,1,1,1,1,1,1,1,1,1,1,
1,1,1,1,1,1,1,1,1,1,1,1,1,1,1,1,1,1,1,1,1,1,1,1,1,1,1,1,1,1,1,1,1,1,1,1,
1,1,1,1,1,1,1,1,1,1,1,1,1,1,1,1,1,1,1,1,1,1,1,1,1,1,1,1,1,1,1,1,1,1,1,1,
1,1,1,1,1,1,1,1,1,1,1,1,1,1,1,1,1,1,1,1,1,1,1,1,1,1,1,1,1,1,1,1,1,1,6),
(0.,0.005,0.01,0.015,0.02,0.025,0.03,0.035,0.04,0.045,0.05,0.055,0.06,0.065,
0.07,0.075,0.08,0.085,0.09,0.095,0.1,0.105,0.11,0.115,0.12,0.125,0.13,0.135,
0.14,0.145,0.15,0.155,0.16,0.165,0.17,0.175,0.18,0.185,0.19,0.195,0.2,0.205,
0.21,0.215,0.22,0.225,0.23,0.235,0.24,0.245,0.25,0.255,0.26,0.265,0.27,
0.275,0.28,0.285,0.29,0.295,0.3,0.305,0.31,0.315,0.32,0.325,0.33,0.335,
0.34,0.345,0.35,0.355,0.36,0.365,0.37,0.375,0.38,0.385,0.39,0.395,0.4,0.405,
0.41,0.415,0.42,0.425,0.43,0.435,0.44,0.445,0.45,0.455,0.46,0.465,0.47,
0.475,0.48,0.485,0.49,0.495,0.5,0.505,0.51,0.515,0.52,0.525,0.53,0.535,
0.54,0.545,0.55,0.555,0.56,0.565,0.57,0.575,0.58,0.585,0.59,0.595,0.6,0.605,
0.61,0.615,0.62,0.625,0.63,0.635,0.64,0.645,0.65,0.655,0.66,0.665,0.67,
0.675,0.68,0.685,0.690000000000001,0.695000000000001,0.700000000000001,
0.705000000000001,0.710000000000001,0.715000000000001,0.720000000000001,
0.725000000000001,0.730000000000001,0.735000000000001,0.740000000000001,
0.745000000000001,0.750000000000001,0.755000000000001,0.760000000000001,
0.765000000000001,0.770000000000001,0.775000000000001,0.780000000000001,
0.785000000000001,0.790000000000001,0.795000000000001,0.800000000000001,
0.805000000000001,0.810000000000001,0.815000000000001,0.820000000000001,
0.825000000000001,0.830000000000001,0.835000000000001,0.840000000000001,
0.845000000000001,0.850000000000001,0.855000000000001,0.860000000000001,
0.865000000000001,0.870000000000001,0.875000000000001,0.880000000000001,
0.885000000000001,0.890000000000001,0.895000000000001,0.900000000000001,
0.905000000000001,0.910000000000001,0.915000000000001,0.920000000000001,
0.925000000000001,0.930000000000001,0.935000000000001,0.940000000000001,
0.945000000000001,0.950000000000001,0.955000000000001,0.960000000000001,
0.965000000000001,0.970000000000001,0.975000000000001,0.980000000000001,
0.985000000000001,0.990000000000001,0.995000000000001,1.),.UNSPECIFIED.)
CURVE()
GEOMETRIC_REPRESENTATION_ITEM()
RATIONAL_B_SPLINE_CURVE((1.,1.,1.,1.,1.,1.,1.,1.,1.,1.,1.,1.,1.,1.,1.,1.,
1.,1.,1.,1.,1.,1.,1.,1.,1.,1.,1.,1.,1.,1.,1.,1.,1.,1.,1.,1.,1.,1.,1.,1.,
1.,1.,1.,1.,1.,1.,1.,1.,1.,1.,1.,1.,1.,1.,1.,1.,1.,1.,1.,1.,1.,1.,1.,1.,
1.,1.,1.,1.,1.,1.,1.,1.,1.,1.,1.,1.,1.,1.,1.,1.,1.,1.,1.,1.,1.,1.,1.,1.,
1.,1.,1.,1.,1.,1.,1.,1.,1.,1.,1.,1.,1.,1.,1.,1.,1.,1.,1.,1.,1.,1.,1.,1.,
1.,1.,1.,1.,1.,1.,1.,1.,1.,1.,1.,1.,1.,1.,1.,1.,1.,1.,1.,1.,1.,1.,1.,1.,
1.,1.,1.,1.,1.,1.,1.,1.,1.,1.,1.,1.,1.,1.,1.,1.,1.,1.,1.,1.,1.,1.,1.,1.,
1.,1.,1.,1.,1.,1.,1.,1.,1.,1.,1.,1.,1.,1.,1.,1.,1.,1.,1.,1.,1.,1.,1.,1.,
1.,1.,1.,1.,1.,1.,1.,1.,1.,1.,1.,1.,1.,1.,1.,1.,1.,1.,1.,1.,1.))
REPRESENTATION_ITEM('')
);
#710=(
BOUNDED_CURVE()
B_SPLINE_CURVE(5,(#179037,#179038,#179039,#179040,#179041,#179042,#179043,
#179044,#179045,#179046,#179047,#179048,#179049,#179050,#179051,#179052,
#179053,#179054,#179055,#179056,#179057,#179058,#179059,#179060,#179061,
#179062,#179063,#179064,#179065,#179066,#179067,#179068,#179069,#179070,
#179071,#179072,#179073,#179074,#179075,#179076,#179077,#179078,#179079,
#179080,#179081,#179082,#179083,#179084,#179085,#179086,#179087,#179088,
#179089,#179090,#179091,#179092,#179093,#179094,#179095,#179096,#179097,
#179098,#179099,#179100,#179101,#179102,#179103,#179104,#179105,#179106,
#179107,#179108,#179109,#179110,#179111,#179112,#179113,#179114,#179115,
#179116,#179117,#179118,#179119,#179120,#179121,#179122,#179123,#179124,
#179125,#179126,#179127,#179128,#179129,#179130,#179131,#179132,#179133,
#179134,#179135,#179136,#179137,#179138,#179139,#179140,#179141,#179142,
#179143,#179144,#179145,#179146,#179147,#179148,#179149,#179150,#179151,
#179152,#179153,#179154,#179155,#179156,#179157,#179158,#179159,#179160,
#179161,#179162,#179163,#179164,#179165,#179166,#179167,#179168,#179169,
#179170,#179171,#179172,#179173,#179174,#179175,#179176,#179177,#179178,
#179179,#179180,#179181,#179182,#179183,#179184,#179185,#179186,#179187,
#179188,#179189,#179190,#179191,#179192,#179193,#179194,#179195,#179196,
#179197,#179198,#179199,#179200,#179201,#179202,#179203,#179204,#179205,
#179206,#179207,#179208,#179209,#179210,#179211,#179212,#179213,#179214,
#179215,#179216,#179217,#179218,#179219,#179220,#179221,#179222,#179223,
#179224,#179225,#179226,#179227,#179228,#179229,#179230,#179231,#179232,
#179233,#179234,#179235,#179236,#179237,#179238,#179239,#179240,#179241),
 .UNSPECIFIED.,.F.,.F.)
B_SPLINE_CURVE_WITH_KNOTS((6,1,1,1,1,1,1,1,1,1,1,1,1,1,1,1,1,1,1,1,1,1,
1,1,1,1,1,1,1,1,1,1,1,1,1,1,1,1,1,1,1,1,1,1,1,1,1,1,1,1,1,1,1,1,1,1,1,1,
1,1,1,1,1,1,1,1,1,1,1,1,1,1,1,1,1,1,1,1,1,1,1,1,1,1,1,1,1,1,1,1,1,1,1,1,
1,1,1,1,1,1,1,1,1,1,1,1,1,1,1,1,1,1,1,1,1,1,1,1,1,1,1,1,1,1,1,1,1,1,1,1,
1,1,1,1,1,1,1,1,1,1,1,1,1,1,1,1,1,1,1,1,1,1,1,1,1,1,1,1,1,1,1,1,1,1,1,1,
1,1,1,1,1,1,1,1,1,1,1,1,1,1,1,1,1,1,1,1,1,1,1,1,1,1,1,1,1,1,1,1,1,1,6),
(-1.,-0.995000000000001,-0.990000000000001,-0.985000000000001,-0.980000000000001,
-0.975000000000001,-0.970000000000001,-0.965000000000001,-0.960000000000001,
-0.955000000000001,-0.950000000000001,-0.945000000000001,-0.940000000000001,
-0.935000000000001,-0.930000000000001,-0.925000000000001,-0.920000000000001,
-0.915000000000001,-0.910000000000001,-0.905000000000001,-0.900000000000001,
-0.895000000000001,-0.890000000000001,-0.885000000000001,-0.880000000000001,
-0.875000000000001,-0.870000000000001,-0.865000000000001,-0.860000000000001,
-0.855000000000001,-0.850000000000001,-0.845000000000001,-0.840000000000001,
-0.835000000000001,-0.830000000000001,-0.825000000000001,-0.820000000000001,
-0.815000000000001,-0.810000000000001,-0.805000000000001,-0.800000000000001,
-0.795000000000001,-0.790000000000001,-0.785000000000001,-0.780000000000001,
-0.775000000000001,-0.770000000000001,-0.765000000000001,-0.760000000000001,
-0.755000000000001,-0.750000000000001,-0.745000000000001,-0.740000000000001,
-0.735000000000001,-0.730000000000001,-0.725000000000001,-0.720000000000001,
-0.715000000000001,-0.710000000000001,-0.705000000000001,-0.700000000000001,
-0.695000000000001,-0.690000000000001,-0.685,-0.68,-0.675,-0.67,-0.665,
-0.66,-0.655,-0.65,-0.645,-0.64,-0.635,-0.63,-0.625,-0.62,-0.615,-0.61,
-0.605,-0.6,-0.595,-0.59,-0.585,-0.58,-0.575,-0.57,-0.565,-0.56,-0.555,
-0.55,-0.545,-0.54,-0.535,-0.53,-0.525,-0.52,-0.515,-0.51,-0.505,-0.5,-0.495,
-0.49,-0.485,-0.48,-0.475,-0.47,-0.465,-0.46,-0.455,-0.45,-0.445,-0.44,
-0.435,-0.43,-0.425,-0.42,-0.415,-0.41,-0.405,-0.4,-0.395,-0.39,-0.385,
-0.38,-0.375,-0.37,-0.365,-0.36,-0.355,-0.35,-0.345,-0.34,-0.335,-0.33,
-0.325,-0.32,-0.315,-0.31,-0.305,-0.3,-0.295,-0.29,-0.285,-0.28,-0.275,
-0.27,-0.265,-0.26,-0.255,-0.25,-0.245,-0.24,-0.235,-0.23,-0.225,-0.22,
-0.215,-0.21,-0.205,-0.2,-0.195,-0.19,-0.185,-0.18,-0.175,-0.17,-0.165,
-0.16,-0.155,-0.15,-0.145,-0.14,-0.135,-0.13,-0.125,-0.12,-0.115,-0.11,
-0.105,-0.1,-0.095,-0.09,-0.085,-0.08,-0.075,-0.07,-0.065,-0.06,-0.055,
-0.05,-0.045,-0.04,-0.035,-0.03,-0.025,-0.02,-0.015,-0.01,-0.005,0.),
 .UNSPECIFIED.)
CURVE()
GEOMETRIC_REPRESENTATION_ITEM()
RATIONAL_B_SPLINE_CURVE((1.,1.,1.,1.,1.,1.,1.,1.,1.,1.,1.,1.,1.,1.,1.,1.,
1.,1.,1.,1.,1.,1.,1.,1.,1.,1.,1.,1.,1.,1.,1.,1.,1.,1.,1.,1.,1.,1.,1.,1.,
1.,1.,1.,1.,1.,1.,1.,1.,1.,1.,1.,1.,1.,1.,1.,1.,1.,1.,1.,1.,1.,1.,1.,1.,
1.,1.,1.,1.,1.,1.,1.,1.,1.,1.,1.,1.,1.,1.,1.,1.,1.,1.,1.,1.,1.,1.,1.,1.,
1.,1.,1.,1.,1.,1.,1.,1.,1.,1.,1.,1.,1.,1.,1.,1.,1.,1.,1.,1.,1.,1.,1.,1.,
1.,1.,1.,1.,1.,1.,1.,1.,1.,1.,1.,1.,1.,1.,1.,1.,1.,1.,1.,1.,1.,1.,1.,1.,
1.,1.,1.,1.,1.,1.,1.,1.,1.,1.,1.,1.,1.,1.,1.,1.,1.,1.,1.,1.,1.,1.,1.,1.,
1.,1.,1.,1.,1.,1.,1.,1.,1.,1.,1.,1.,1.,1.,1.,1.,1.,1.,1.,1.,1.,1.,1.,1.,
1.,1.,1.,1.,1.,1.,1.,1.,1.,1.,1.,1.,1.,1.,1.,1.,1.,1.,1.,1.,1.))
REPRESENTATION_ITEM('')
);
#711=(
BOUNDED_CURVE()
B_SPLINE_CURVE(5,(#179253,#179254,#179255,#179256,#179257,#179258,#179259,
#179260,#179261,#179262,#179263,#179264,#179265,#179266,#179267,#179268,
#179269,#179270,#179271,#179272,#179273,#179274,#179275,#179276,#179277,
#179278,#179279,#179280,#179281,#179282,#179283,#179284,#179285,#179286,
#179287,#179288,#179289,#179290,#179291,#179292,#179293,#179294,#179295,
#179296,#179297,#179298,#179299,#179300,#179301,#179302,#179303,#179304,
#179305,#179306,#179307,#179308,#179309,#179310,#179311,#179312,#179313,
#179314,#179315,#179316,#179317,#179318,#179319,#179320,#179321,#179322,
#179323,#179324,#179325,#179326,#179327,#179328,#179329,#179330,#179331,
#179332,#179333,#179334,#179335,#179336,#179337,#179338,#179339,#179340,
#179341,#179342,#179343,#179344,#179345,#179346,#179347,#179348,#179349,
#179350,#179351,#179352,#179353,#179354,#179355,#179356,#179357,#179358,
#179359,#179360,#179361,#179362,#179363,#179364,#179365,#179366,#179367,
#179368,#179369,#179370,#179371,#179372,#179373,#179374,#179375,#179376,
#179377,#179378,#179379,#179380,#179381,#179382,#179383,#179384,#179385,
#179386,#179387,#179388,#179389,#179390,#179391,#179392,#179393,#179394,
#179395,#179396,#179397,#179398,#179399,#179400,#179401,#179402,#179403,
#179404,#179405,#179406,#179407,#179408,#179409,#179410,#179411,#179412,
#179413,#179414,#179415,#179416,#179417,#179418,#179419,#179420,#179421,
#179422,#179423,#179424,#179425,#179426,#179427,#179428,#179429,#179430,
#179431,#179432,#179433,#179434,#179435,#179436,#179437,#179438,#179439,
#179440,#179441,#179442,#179443,#179444,#179445,#179446,#179447,#179448,
#179449,#179450,#179451,#179452,#179453,#179454,#179455,#179456,#179457),
 .UNSPECIFIED.,.F.,.F.)
B_SPLINE_CURVE_WITH_KNOTS((6,1,1,1,1,1,1,1,1,1,1,1,1,1,1,1,1,1,1,1,1,1,
1,1,1,1,1,1,1,1,1,1,1,1,1,1,1,1,1,1,1,1,1,1,1,1,1,1,1,1,1,1,1,1,1,1,1,1,
1,1,1,1,1,1,1,1,1,1,1,1,1,1,1,1,1,1,1,1,1,1,1,1,1,1,1,1,1,1,1,1,1,1,1,1,
1,1,1,1,1,1,1,1,1,1,1,1,1,1,1,1,1,1,1,1,1,1,1,1,1,1,1,1,1,1,1,1,1,1,1,1,
1,1,1,1,1,1,1,1,1,1,1,1,1,1,1,1,1,1,1,1,1,1,1,1,1,1,1,1,1,1,1,1,1,1,1,1,
1,1,1,1,1,1,1,1,1,1,1,1,1,1,1,1,1,1,1,1,1,1,1,1,1,1,1,1,1,1,1,1,1,1,6),
(0.,0.005,0.01,0.015,0.02,0.025,0.03,0.035,0.04,0.045,0.05,0.055,0.06,0.065,
0.07,0.075,0.08,0.085,0.09,0.095,0.1,0.105,0.11,0.115,0.12,0.125,0.13,0.135,
0.14,0.145,0.15,0.155,0.16,0.165,0.17,0.175,0.18,0.185,0.19,0.195,0.2,0.205,
0.21,0.215,0.22,0.225,0.23,0.235,0.24,0.245,0.25,0.255,0.26,0.265,0.27,
0.275,0.28,0.285,0.29,0.295,0.3,0.305,0.31,0.315,0.32,0.325,0.33,0.335,
0.34,0.345,0.35,0.355,0.36,0.365,0.37,0.375,0.38,0.385,0.39,0.395,0.4,0.405,
0.41,0.415,0.42,0.425,0.43,0.435,0.44,0.445,0.45,0.455,0.46,0.465,0.47,
0.475,0.48,0.485,0.49,0.495,0.5,0.505,0.51,0.515,0.52,0.525,0.53,0.535,
0.54,0.545,0.55,0.555,0.56,0.565,0.57,0.575,0.58,0.585,0.59,0.595,0.6,0.605,
0.61,0.615,0.62,0.625,0.63,0.635,0.64,0.645,0.65,0.655,0.66,0.665,0.67,
0.675,0.68,0.685,0.690000000000001,0.695000000000001,0.700000000000001,
0.705000000000001,0.710000000000001,0.715000000000001,0.720000000000001,
0.725000000000001,0.730000000000001,0.735000000000001,0.740000000000001,
0.745000000000001,0.750000000000001,0.755000000000001,0.760000000000001,
0.765000000000001,0.770000000000001,0.775000000000001,0.780000000000001,
0.785000000000001,0.790000000000001,0.795000000000001,0.800000000000001,
0.805000000000001,0.810000000000001,0.815000000000001,0.820000000000001,
0.825000000000001,0.830000000000001,0.835000000000001,0.840000000000001,
0.845000000000001,0.850000000000001,0.855000000000001,0.860000000000001,
0.865000000000001,0.870000000000001,0.875000000000001,0.880000000000001,
0.885000000000001,0.890000000000001,0.895000000000001,0.900000000000001,
0.905000000000001,0.910000000000001,0.915000000000001,0.920000000000001,
0.925000000000001,0.930000000000001,0.935000000000001,0.940000000000001,
0.945000000000001,0.950000000000001,0.955000000000001,0.960000000000001,
0.965000000000001,0.970000000000001,0.975000000000001,0.980000000000001,
0.985000000000001,0.990000000000001,0.995000000000001,1.),.UNSPECIFIED.)
CURVE()
GEOMETRIC_REPRESENTATION_ITEM()
RATIONAL_B_SPLINE_CURVE((1.,1.,1.,1.,1.,1.,1.,1.,1.,1.,1.,1.,1.,1.,1.,1.,
1.,1.,1.,1.,1.,1.,1.,1.,1.,1.,1.,1.,1.,1.,1.,1.,1.,1.,1.,1.,1.,1.,1.,1.,
1.,1.,1.,1.,1.,1.,1.,1.,1.,1.,1.,1.,1.,1.,1.,1.,1.,1.,1.,1.,1.,1.,1.,1.,
1.,1.,1.,1.,1.,1.,1.,1.,1.,1.,1.,1.,1.,1.,1.,1.,1.,1.,1.,1.,1.,1.,1.,1.,
1.,1.,1.,1.,1.,1.,1.,1.,1.,1.,1.,1.,1.,1.,1.,1.,1.,1.,1.,1.,1.,1.,1.,1.,
1.,1.,1.,1.,1.,1.,1.,1.,1.,1.,1.,1.,1.,1.,1.,1.,1.,1.,1.,1.,1.,1.,1.,1.,
1.,1.,1.,1.,1.,1.,1.,1.,1.,1.,1.,1.,1.,1.,1.,1.,1.,1.,1.,1.,1.,1.,1.,1.,
1.,1.,1.,1.,1.,1.,1.,1.,1.,1.,1.,1.,1.,1.,1.,1.,1.,1.,1.,1.,1.,1.,1.,1.,
1.,1.,1.,1.,1.,1.,1.,1.,1.,1.,1.,1.,1.,1.,1.,1.,1.,1.,1.,1.,1.))
REPRESENTATION_ITEM('')
);
#712=(
BOUNDED_CURVE()
B_SPLINE_CURVE(5,(#179461,#179462,#179463,#179464,#179465,#179466,#179467,
#179468,#179469,#179470,#179471,#179472,#179473,#179474,#179475,#179476,
#179477,#179478,#179479,#179480,#179481,#179482,#179483,#179484,#179485,
#179486,#179487,#179488,#179489,#179490,#179491,#179492,#179493,#179494,
#179495,#179496,#179497,#179498,#179499,#179500,#179501,#179502,#179503,
#179504,#179505,#179506,#179507,#179508,#179509,#179510,#179511,#179512,
#179513,#179514,#179515,#179516,#179517,#179518,#179519,#179520,#179521,
#179522,#179523,#179524,#179525,#179526,#179527,#179528,#179529,#179530,
#179531,#179532,#179533,#179534,#179535,#179536,#179537,#179538,#179539,
#179540,#179541,#179542,#179543,#179544,#179545,#179546,#179547,#179548,
#179549,#179550,#179551,#179552,#179553,#179554,#179555,#179556,#179557,
#179558,#179559,#179560,#179561,#179562,#179563,#179564,#179565,#179566,
#179567,#179568,#179569,#179570,#179571,#179572,#179573,#179574,#179575,
#179576,#179577,#179578,#179579,#179580,#179581,#179582,#179583,#179584,
#179585,#179586,#179587,#179588,#179589,#179590,#179591,#179592,#179593,
#179594,#179595,#179596,#179597,#179598,#179599,#179600,#179601,#179602,
#179603,#179604,#179605,#179606,#179607,#179608,#179609,#179610,#179611,
#179612,#179613,#179614,#179615,#179616,#179617,#179618,#179619,#179620,
#179621,#179622,#179623,#179624,#179625,#179626,#179627,#179628,#179629,
#179630,#179631,#179632,#179633,#179634,#179635,#179636,#179637,#179638,
#179639,#179640,#179641,#179642,#179643,#179644,#179645,#179646,#179647,
#179648,#179649,#179650,#179651,#179652,#179653,#179654,#179655,#179656,
#179657,#179658,#179659,#179660,#179661,#179662,#179663,#179664,#179665),
 .UNSPECIFIED.,.F.,.F.)
B_SPLINE_CURVE_WITH_KNOTS((6,1,1,1,1,1,1,1,1,1,1,1,1,1,1,1,1,1,1,1,1,1,
1,1,1,1,1,1,1,1,1,1,1,1,1,1,1,1,1,1,1,1,1,1,1,1,1,1,1,1,1,1,1,1,1,1,1,1,
1,1,1,1,1,1,1,1,1,1,1,1,1,1,1,1,1,1,1,1,1,1,1,1,1,1,1,1,1,1,1,1,1,1,1,1,
1,1,1,1,1,1,1,1,1,1,1,1,1,1,1,1,1,1,1,1,1,1,1,1,1,1,1,1,1,1,1,1,1,1,1,1,
1,1,1,1,1,1,1,1,1,1,1,1,1,1,1,1,1,1,1,1,1,1,1,1,1,1,1,1,1,1,1,1,1,1,1,1,
1,1,1,1,1,1,1,1,1,1,1,1,1,1,1,1,1,1,1,1,1,1,1,1,1,1,1,1,1,1,1,1,1,1,6),
(-1.,-0.995000000000001,-0.990000000000001,-0.985000000000001,-0.980000000000001,
-0.975000000000001,-0.970000000000001,-0.965000000000001,-0.960000000000001,
-0.955000000000001,-0.950000000000001,-0.945000000000001,-0.940000000000001,
-0.935000000000001,-0.930000000000001,-0.925000000000001,-0.920000000000001,
-0.915000000000001,-0.910000000000001,-0.905000000000001,-0.900000000000001,
-0.895000000000001,-0.890000000000001,-0.885000000000001,-0.880000000000001,
-0.875000000000001,-0.870000000000001,-0.865000000000001,-0.860000000000001,
-0.855000000000001,-0.850000000000001,-0.845000000000001,-0.840000000000001,
-0.835000000000001,-0.830000000000001,-0.825000000000001,-0.820000000000001,
-0.815000000000001,-0.810000000000001,-0.805000000000001,-0.800000000000001,
-0.795000000000001,-0.790000000000001,-0.785000000000001,-0.780000000000001,
-0.775000000000001,-0.770000000000001,-0.765000000000001,-0.760000000000001,
-0.755000000000001,-0.750000000000001,-0.745000000000001,-0.740000000000001,
-0.735000000000001,-0.730000000000001,-0.725000000000001,-0.720000000000001,
-0.715000000000001,-0.710000000000001,-0.705000000000001,-0.700000000000001,
-0.695000000000001,-0.690000000000001,-0.685,-0.68,-0.675,-0.67,-0.665,
-0.66,-0.655,-0.65,-0.645,-0.64,-0.635,-0.63,-0.625,-0.62,-0.615,-0.61,
-0.605,-0.6,-0.595,-0.59,-0.585,-0.58,-0.575,-0.57,-0.565,-0.56,-0.555,
-0.55,-0.545,-0.54,-0.535,-0.53,-0.525,-0.52,-0.515,-0.51,-0.505,-0.5,-0.495,
-0.49,-0.485,-0.48,-0.475,-0.47,-0.465,-0.46,-0.455,-0.45,-0.445,-0.44,
-0.435,-0.43,-0.425,-0.42,-0.415,-0.41,-0.405,-0.4,-0.395,-0.39,-0.385,
-0.38,-0.375,-0.37,-0.365,-0.36,-0.355,-0.35,-0.345,-0.34,-0.335,-0.33,
-0.325,-0.32,-0.315,-0.31,-0.305,-0.3,-0.295,-0.29,-0.285,-0.28,-0.275,
-0.27,-0.265,-0.26,-0.255,-0.25,-0.245,-0.24,-0.235,-0.23,-0.225,-0.22,
-0.215,-0.21,-0.205,-0.2,-0.195,-0.19,-0.185,-0.18,-0.175,-0.17,-0.165,
-0.16,-0.155,-0.15,-0.145,-0.14,-0.135,-0.13,-0.125,-0.12,-0.115,-0.11,
-0.105,-0.1,-0.095,-0.09,-0.085,-0.08,-0.075,-0.07,-0.065,-0.06,-0.055,
-0.05,-0.045,-0.04,-0.035,-0.03,-0.025,-0.02,-0.015,-0.01,-0.005,0.),
 .UNSPECIFIED.)
CURVE()
GEOMETRIC_REPRESENTATION_ITEM()
RATIONAL_B_SPLINE_CURVE((1.,1.,1.,1.,1.,1.,1.,1.,1.,1.,1.,1.,1.,1.,1.,1.,
1.,1.,1.,1.,1.,1.,1.,1.,1.,1.,1.,1.,1.,1.,1.,1.,1.,1.,1.,1.,1.,1.,1.,1.,
1.,1.,1.,1.,1.,1.,1.,1.,1.,1.,1.,1.,1.,1.,1.,1.,1.,1.,1.,1.,1.,1.,1.,1.,
1.,1.,1.,1.,1.,1.,1.,1.,1.,1.,1.,1.,1.,1.,1.,1.,1.,1.,1.,1.,1.,1.,1.,1.,
1.,1.,1.,1.,1.,1.,1.,1.,1.,1.,1.,1.,1.,1.,1.,1.,1.,1.,1.,1.,1.,1.,1.,1.,
1.,1.,1.,1.,1.,1.,1.,1.,1.,1.,1.,1.,1.,1.,1.,1.,1.,1.,1.,1.,1.,1.,1.,1.,
1.,1.,1.,1.,1.,1.,1.,1.,1.,1.,1.,1.,1.,1.,1.,1.,1.,1.,1.,1.,1.,1.,1.,1.,
1.,1.,1.,1.,1.,1.,1.,1.,1.,1.,1.,1.,1.,1.,1.,1.,1.,1.,1.,1.,1.,1.,1.,1.,
1.,1.,1.,1.,1.,1.,1.,1.,1.,1.,1.,1.,1.,1.,1.,1.,1.,1.,1.,1.,1.))
REPRESENTATION_ITEM('')
);
#713=(
BOUNDED_CURVE()
B_SPLINE_CURVE(5,(#179677,#179678,#179679,#179680,#179681,#179682,#179683,
#179684,#179685,#179686,#179687,#179688,#179689,#179690,#179691,#179692,
#179693,#179694,#179695,#179696,#179697,#179698,#179699,#179700,#179701,
#179702,#179703,#179704,#179705,#179706,#179707,#179708,#179709,#179710,
#179711,#179712,#179713,#179714,#179715,#179716,#179717,#179718,#179719,
#179720,#179721,#179722,#179723,#179724,#179725,#179726,#179727,#179728,
#179729,#179730,#179731,#179732,#179733,#179734,#179735,#179736,#179737,
#179738,#179739,#179740,#179741,#179742,#179743,#179744,#179745,#179746,
#179747,#179748,#179749,#179750,#179751,#179752,#179753,#179754,#179755,
#179756,#179757,#179758,#179759,#179760,#179761,#179762,#179763,#179764,
#179765,#179766,#179767,#179768,#179769,#179770,#179771,#179772,#179773,
#179774,#179775,#179776,#179777,#179778,#179779,#179780,#179781,#179782,
#179783,#179784,#179785,#179786,#179787,#179788,#179789,#179790,#179791,
#179792,#179793,#179794,#179795,#179796,#179797,#179798,#179799,#179800,
#179801,#179802,#179803,#179804,#179805,#179806,#179807,#179808,#179809,
#179810,#179811,#179812,#179813,#179814,#179815,#179816,#179817,#179818,
#179819,#179820,#179821,#179822,#179823,#179824,#179825,#179826,#179827,
#179828,#179829,#179830,#179831,#179832,#179833,#179834,#179835,#179836,
#179837,#179838,#179839,#179840,#179841,#179842,#179843,#179844,#179845,
#179846,#179847,#179848,#179849,#179850,#179851,#179852,#179853,#179854,
#179855,#179856,#179857,#179858,#179859,#179860,#179861,#179862,#179863,
#179864,#179865,#179866,#179867,#179868,#179869,#179870,#179871,#179872,
#179873,#179874,#179875,#179876,#179877,#179878,#179879,#179880,#179881),
 .UNSPECIFIED.,.F.,.F.)
B_SPLINE_CURVE_WITH_KNOTS((6,1,1,1,1,1,1,1,1,1,1,1,1,1,1,1,1,1,1,1,1,1,
1,1,1,1,1,1,1,1,1,1,1,1,1,1,1,1,1,1,1,1,1,1,1,1,1,1,1,1,1,1,1,1,1,1,1,1,
1,1,1,1,1,1,1,1,1,1,1,1,1,1,1,1,1,1,1,1,1,1,1,1,1,1,1,1,1,1,1,1,1,1,1,1,
1,1,1,1,1,1,1,1,1,1,1,1,1,1,1,1,1,1,1,1,1,1,1,1,1,1,1,1,1,1,1,1,1,1,1,1,
1,1,1,1,1,1,1,1,1,1,1,1,1,1,1,1,1,1,1,1,1,1,1,1,1,1,1,1,1,1,1,1,1,1,1,1,
1,1,1,1,1,1,1,1,1,1,1,1,1,1,1,1,1,1,1,1,1,1,1,1,1,1,1,1,1,1,1,1,1,1,6),
(0.,0.005,0.01,0.015,0.02,0.025,0.03,0.035,0.04,0.045,0.05,0.055,0.06,0.065,
0.07,0.075,0.08,0.085,0.09,0.095,0.1,0.105,0.11,0.115,0.12,0.125,0.13,0.135,
0.14,0.145,0.15,0.155,0.16,0.165,0.17,0.175,0.18,0.185,0.19,0.195,0.2,0.205,
0.21,0.215,0.22,0.225,0.23,0.235,0.24,0.245,0.25,0.255,0.26,0.265,0.27,
0.275,0.28,0.285,0.29,0.295,0.3,0.305,0.31,0.315,0.32,0.325,0.33,0.335,
0.34,0.345,0.35,0.355,0.36,0.365,0.37,0.375,0.38,0.385,0.39,0.395,0.4,0.405,
0.41,0.415,0.42,0.425,0.43,0.435,0.44,0.445,0.45,0.455,0.46,0.465,0.47,
0.475,0.48,0.485,0.49,0.495,0.5,0.505,0.51,0.515,0.52,0.525,0.53,0.535,
0.54,0.545,0.55,0.555,0.56,0.565,0.57,0.575,0.58,0.585,0.59,0.595,0.6,0.605,
0.61,0.615,0.62,0.625,0.63,0.635,0.64,0.645,0.65,0.655,0.66,0.665,0.67,
0.675,0.68,0.685,0.690000000000001,0.695000000000001,0.700000000000001,
0.705000000000001,0.710000000000001,0.715000000000001,0.720000000000001,
0.725000000000001,0.730000000000001,0.735000000000001,0.740000000000001,
0.745000000000001,0.750000000000001,0.755000000000001,0.760000000000001,
0.765000000000001,0.770000000000001,0.775000000000001,0.780000000000001,
0.785000000000001,0.790000000000001,0.795000000000001,0.800000000000001,
0.805000000000001,0.810000000000001,0.815000000000001,0.820000000000001,
0.825000000000001,0.830000000000001,0.835000000000001,0.840000000000001,
0.845000000000001,0.850000000000001,0.855000000000001,0.860000000000001,
0.865000000000001,0.870000000000001,0.875000000000001,0.880000000000001,
0.885000000000001,0.890000000000001,0.895000000000001,0.900000000000001,
0.905000000000001,0.910000000000001,0.915000000000001,0.920000000000001,
0.925000000000001,0.930000000000001,0.935000000000001,0.940000000000001,
0.945000000000001,0.950000000000001,0.955000000000001,0.960000000000001,
0.965000000000001,0.970000000000001,0.975000000000001,0.980000000000001,
0.985000000000001,0.990000000000001,0.995000000000001,1.),.UNSPECIFIED.)
CURVE()
GEOMETRIC_REPRESENTATION_ITEM()
RATIONAL_B_SPLINE_CURVE((1.,1.,1.,1.,1.,1.,1.,1.,1.,1.,1.,1.,1.,1.,1.,1.,
1.,1.,1.,1.,1.,1.,1.,1.,1.,1.,1.,1.,1.,1.,1.,1.,1.,1.,1.,1.,1.,1.,1.,1.,
1.,1.,1.,1.,1.,1.,1.,1.,1.,1.,1.,1.,1.,1.,1.,1.,1.,1.,1.,1.,1.,1.,1.,1.,
1.,1.,1.,1.,1.,1.,1.,1.,1.,1.,1.,1.,1.,1.,1.,1.,1.,1.,1.,1.,1.,1.,1.,1.,
1.,1.,1.,1.,1.,1.,1.,1.,1.,1.,1.,1.,1.,1.,1.,1.,1.,1.,1.,1.,1.,1.,1.,1.,
1.,1.,1.,1.,1.,1.,1.,1.,1.,1.,1.,1.,1.,1.,1.,1.,1.,1.,1.,1.,1.,1.,1.,1.,
1.,1.,1.,1.,1.,1.,1.,1.,1.,1.,1.,1.,1.,1.,1.,1.,1.,1.,1.,1.,1.,1.,1.,1.,
1.,1.,1.,1.,1.,1.,1.,1.,1.,1.,1.,1.,1.,1.,1.,1.,1.,1.,1.,1.,1.,1.,1.,1.,
1.,1.,1.,1.,1.,1.,1.,1.,1.,1.,1.,1.,1.,1.,1.,1.,1.,1.,1.,1.,1.))
REPRESENTATION_ITEM('')
);
#714=(
BOUNDED_CURVE()
B_SPLINE_CURVE(5,(#179885,#179886,#179887,#179888,#179889,#179890,#179891,
#179892,#179893,#179894,#179895,#179896,#179897,#179898,#179899,#179900,
#179901,#179902,#179903,#179904,#179905,#179906,#179907,#179908,#179909,
#179910,#179911,#179912,#179913,#179914,#179915,#179916,#179917,#179918,
#179919,#179920,#179921,#179922,#179923,#179924,#179925,#179926,#179927,
#179928,#179929,#179930,#179931,#179932,#179933,#179934,#179935,#179936,
#179937,#179938,#179939,#179940,#179941,#179942,#179943,#179944,#179945,
#179946,#179947,#179948,#179949,#179950,#179951,#179952,#179953,#179954,
#179955,#179956,#179957,#179958,#179959,#179960,#179961,#179962,#179963,
#179964,#179965,#179966,#179967,#179968,#179969,#179970,#179971,#179972,
#179973,#179974,#179975,#179976,#179977,#179978,#179979,#179980,#179981,
#179982,#179983,#179984,#179985,#179986,#179987,#179988,#179989,#179990,
#179991,#179992,#179993,#179994,#179995,#179996,#179997,#179998,#179999,
#180000,#180001,#180002,#180003,#180004,#180005,#180006,#180007,#180008,
#180009,#180010,#180011,#180012,#180013,#180014,#180015,#180016,#180017,
#180018,#180019,#180020,#180021,#180022,#180023,#180024,#180025,#180026,
#180027,#180028,#180029,#180030,#180031,#180032,#180033,#180034,#180035,
#180036,#180037,#180038,#180039,#180040,#180041,#180042,#180043,#180044,
#180045,#180046,#180047,#180048,#180049,#180050,#180051,#180052,#180053,
#180054,#180055,#180056,#180057,#180058,#180059,#180060,#180061,#180062,
#180063,#180064,#180065,#180066,#180067,#180068,#180069,#180070,#180071,
#180072,#180073,#180074,#180075,#180076,#180077,#180078,#180079,#180080,
#180081,#180082,#180083,#180084,#180085,#180086,#180087,#180088,#180089),
 .UNSPECIFIED.,.F.,.F.)
B_SPLINE_CURVE_WITH_KNOTS((6,1,1,1,1,1,1,1,1,1,1,1,1,1,1,1,1,1,1,1,1,1,
1,1,1,1,1,1,1,1,1,1,1,1,1,1,1,1,1,1,1,1,1,1,1,1,1,1,1,1,1,1,1,1,1,1,1,1,
1,1,1,1,1,1,1,1,1,1,1,1,1,1,1,1,1,1,1,1,1,1,1,1,1,1,1,1,1,1,1,1,1,1,1,1,
1,1,1,1,1,1,1,1,1,1,1,1,1,1,1,1,1,1,1,1,1,1,1,1,1,1,1,1,1,1,1,1,1,1,1,1,
1,1,1,1,1,1,1,1,1,1,1,1,1,1,1,1,1,1,1,1,1,1,1,1,1,1,1,1,1,1,1,1,1,1,1,1,
1,1,1,1,1,1,1,1,1,1,1,1,1,1,1,1,1,1,1,1,1,1,1,1,1,1,1,1,1,1,1,1,1,1,6),
(-1.,-0.995000000000001,-0.990000000000001,-0.985000000000001,-0.980000000000001,
-0.975000000000001,-0.970000000000001,-0.965000000000001,-0.960000000000001,
-0.955000000000001,-0.950000000000001,-0.945000000000001,-0.940000000000001,
-0.935000000000001,-0.930000000000001,-0.925000000000001,-0.920000000000001,
-0.915000000000001,-0.910000000000001,-0.905000000000001,-0.900000000000001,
-0.895000000000001,-0.890000000000001,-0.885000000000001,-0.880000000000001,
-0.875000000000001,-0.870000000000001,-0.865000000000001,-0.860000000000001,
-0.855000000000001,-0.850000000000001,-0.845000000000001,-0.840000000000001,
-0.835000000000001,-0.830000000000001,-0.825000000000001,-0.820000000000001,
-0.815000000000001,-0.810000000000001,-0.805000000000001,-0.800000000000001,
-0.795000000000001,-0.790000000000001,-0.785000000000001,-0.780000000000001,
-0.775000000000001,-0.770000000000001,-0.765000000000001,-0.760000000000001,
-0.755000000000001,-0.750000000000001,-0.745000000000001,-0.740000000000001,
-0.735000000000001,-0.730000000000001,-0.725000000000001,-0.720000000000001,
-0.715000000000001,-0.710000000000001,-0.705000000000001,-0.700000000000001,
-0.695000000000001,-0.690000000000001,-0.685,-0.68,-0.675,-0.67,-0.665,
-0.66,-0.655,-0.65,-0.645,-0.64,-0.635,-0.63,-0.625,-0.62,-0.615,-0.61,
-0.605,-0.6,-0.595,-0.59,-0.585,-0.58,-0.575,-0.57,-0.565,-0.56,-0.555,
-0.55,-0.545,-0.54,-0.535,-0.53,-0.525,-0.52,-0.515,-0.51,-0.505,-0.5,-0.495,
-0.49,-0.485,-0.48,-0.475,-0.47,-0.465,-0.46,-0.455,-0.45,-0.445,-0.44,
-0.435,-0.43,-0.425,-0.42,-0.415,-0.41,-0.405,-0.4,-0.395,-0.39,-0.385,
-0.38,-0.375,-0.37,-0.365,-0.36,-0.355,-0.35,-0.345,-0.34,-0.335,-0.33,
-0.325,-0.32,-0.315,-0.31,-0.305,-0.3,-0.295,-0.29,-0.285,-0.28,-0.275,
-0.27,-0.265,-0.26,-0.255,-0.25,-0.245,-0.24,-0.235,-0.23,-0.225,-0.22,
-0.215,-0.21,-0.205,-0.2,-0.195,-0.19,-0.185,-0.18,-0.175,-0.17,-0.165,
-0.16,-0.155,-0.15,-0.145,-0.14,-0.135,-0.13,-0.125,-0.12,-0.115,-0.11,
-0.105,-0.1,-0.095,-0.09,-0.085,-0.08,-0.075,-0.07,-0.065,-0.06,-0.055,
-0.05,-0.045,-0.04,-0.035,-0.03,-0.025,-0.02,-0.015,-0.01,-0.005,0.),
 .UNSPECIFIED.)
CURVE()
GEOMETRIC_REPRESENTATION_ITEM()
RATIONAL_B_SPLINE_CURVE((1.,1.,1.,1.,1.,1.,1.,1.,1.,1.,1.,1.,1.,1.,1.,1.,
1.,1.,1.,1.,1.,1.,1.,1.,1.,1.,1.,1.,1.,1.,1.,1.,1.,1.,1.,1.,1.,1.,1.,1.,
1.,1.,1.,1.,1.,1.,1.,1.,1.,1.,1.,1.,1.,1.,1.,1.,1.,1.,1.,1.,1.,1.,1.,1.,
1.,1.,1.,1.,1.,1.,1.,1.,1.,1.,1.,1.,1.,1.,1.,1.,1.,1.,1.,1.,1.,1.,1.,1.,
1.,1.,1.,1.,1.,1.,1.,1.,1.,1.,1.,1.,1.,1.,1.,1.,1.,1.,1.,1.,1.,1.,1.,1.,
1.,1.,1.,1.,1.,1.,1.,1.,1.,1.,1.,1.,1.,1.,1.,1.,1.,1.,1.,1.,1.,1.,1.,1.,
1.,1.,1.,1.,1.,1.,1.,1.,1.,1.,1.,1.,1.,1.,1.,1.,1.,1.,1.,1.,1.,1.,1.,1.,
1.,1.,1.,1.,1.,1.,1.,1.,1.,1.,1.,1.,1.,1.,1.,1.,1.,1.,1.,1.,1.,1.,1.,1.,
1.,1.,1.,1.,1.,1.,1.,1.,1.,1.,1.,1.,1.,1.,1.,1.,1.,1.,1.,1.,1.))
REPRESENTATION_ITEM('')
);
#715=(
BOUNDED_CURVE()
B_SPLINE_CURVE(5,(#180101,#180102,#180103,#180104,#180105,#180106,#180107,
#180108,#180109,#180110,#180111,#180112,#180113,#180114,#180115,#180116,
#180117,#180118,#180119,#180120,#180121,#180122,#180123,#180124,#180125,
#180126,#180127,#180128,#180129,#180130,#180131,#180132,#180133,#180134,
#180135,#180136,#180137,#180138,#180139,#180140,#180141,#180142,#180143,
#180144,#180145,#180146,#180147,#180148,#180149,#180150,#180151,#180152,
#180153,#180154,#180155,#180156,#180157,#180158,#180159,#180160,#180161,
#180162,#180163,#180164,#180165,#180166,#180167,#180168,#180169,#180170,
#180171,#180172,#180173,#180174,#180175,#180176,#180177,#180178,#180179,
#180180,#180181,#180182,#180183,#180184,#180185,#180186,#180187,#180188,
#180189,#180190,#180191,#180192,#180193,#180194,#180195,#180196,#180197,
#180198,#180199,#180200,#180201,#180202,#180203,#180204,#180205,#180206,
#180207,#180208,#180209,#180210,#180211,#180212,#180213,#180214,#180215,
#180216,#180217,#180218,#180219,#180220,#180221,#180222,#180223,#180224,
#180225,#180226,#180227,#180228,#180229,#180230,#180231,#180232,#180233,
#180234,#180235,#180236,#180237,#180238,#180239,#180240,#180241,#180242,
#180243,#180244,#180245,#180246,#180247,#180248,#180249,#180250,#180251,
#180252,#180253,#180254,#180255,#180256,#180257,#180258,#180259,#180260,
#180261,#180262,#180263,#180264,#180265,#180266,#180267,#180268,#180269,
#180270,#180271,#180272,#180273,#180274,#180275,#180276,#180277,#180278,
#180279,#180280,#180281,#180282,#180283,#180284,#180285,#180286,#180287,
#180288,#180289,#180290,#180291,#180292,#180293,#180294,#180295,#180296,
#180297,#180298,#180299,#180300,#180301,#180302,#180303,#180304,#180305),
 .UNSPECIFIED.,.F.,.F.)
B_SPLINE_CURVE_WITH_KNOTS((6,1,1,1,1,1,1,1,1,1,1,1,1,1,1,1,1,1,1,1,1,1,
1,1,1,1,1,1,1,1,1,1,1,1,1,1,1,1,1,1,1,1,1,1,1,1,1,1,1,1,1,1,1,1,1,1,1,1,
1,1,1,1,1,1,1,1,1,1,1,1,1,1,1,1,1,1,1,1,1,1,1,1,1,1,1,1,1,1,1,1,1,1,1,1,
1,1,1,1,1,1,1,1,1,1,1,1,1,1,1,1,1,1,1,1,1,1,1,1,1,1,1,1,1,1,1,1,1,1,1,1,
1,1,1,1,1,1,1,1,1,1,1,1,1,1,1,1,1,1,1,1,1,1,1,1,1,1,1,1,1,1,1,1,1,1,1,1,
1,1,1,1,1,1,1,1,1,1,1,1,1,1,1,1,1,1,1,1,1,1,1,1,1,1,1,1,1,1,1,1,1,1,6),
(0.,0.005,0.01,0.015,0.02,0.025,0.03,0.035,0.04,0.045,0.05,0.055,0.06,0.065,
0.07,0.075,0.08,0.085,0.09,0.095,0.1,0.105,0.11,0.115,0.12,0.125,0.13,0.135,
0.14,0.145,0.15,0.155,0.16,0.165,0.17,0.175,0.18,0.185,0.19,0.195,0.2,0.205,
0.21,0.215,0.22,0.225,0.23,0.235,0.24,0.245,0.25,0.255,0.26,0.265,0.27,
0.275,0.28,0.285,0.29,0.295,0.3,0.305,0.31,0.315,0.32,0.325,0.33,0.335,
0.34,0.345,0.35,0.355,0.36,0.365,0.37,0.375,0.38,0.385,0.39,0.395,0.4,0.405,
0.41,0.415,0.42,0.425,0.43,0.435,0.44,0.445,0.45,0.455,0.46,0.465,0.47,
0.475,0.48,0.485,0.49,0.495,0.5,0.505,0.51,0.515,0.52,0.525,0.53,0.535,
0.54,0.545,0.55,0.555,0.56,0.565,0.57,0.575,0.58,0.585,0.59,0.595,0.6,0.605,
0.61,0.615,0.62,0.625,0.63,0.635,0.64,0.645,0.65,0.655,0.66,0.665,0.67,
0.675,0.68,0.685,0.690000000000001,0.695000000000001,0.700000000000001,
0.705000000000001,0.710000000000001,0.715000000000001,0.720000000000001,
0.725000000000001,0.730000000000001,0.735000000000001,0.740000000000001,
0.745000000000001,0.750000000000001,0.755000000000001,0.760000000000001,
0.765000000000001,0.770000000000001,0.775000000000001,0.780000000000001,
0.785000000000001,0.790000000000001,0.795000000000001,0.800000000000001,
0.805000000000001,0.810000000000001,0.815000000000001,0.820000000000001,
0.825000000000001,0.830000000000001,0.835000000000001,0.840000000000001,
0.845000000000001,0.850000000000001,0.855000000000001,0.860000000000001,
0.865000000000001,0.870000000000001,0.875000000000001,0.880000000000001,
0.885000000000001,0.890000000000001,0.895000000000001,0.900000000000001,
0.905000000000001,0.910000000000001,0.915000000000001,0.920000000000001,
0.925000000000001,0.930000000000001,0.935000000000001,0.940000000000001,
0.945000000000001,0.950000000000001,0.955000000000001,0.960000000000001,
0.965000000000001,0.970000000000001,0.975000000000001,0.980000000000001,
0.985000000000001,0.990000000000001,0.995000000000001,1.),.UNSPECIFIED.)
CURVE()
GEOMETRIC_REPRESENTATION_ITEM()
RATIONAL_B_SPLINE_CURVE((1.,1.,1.,1.,1.,1.,1.,1.,1.,1.,1.,1.,1.,1.,1.,1.,
1.,1.,1.,1.,1.,1.,1.,1.,1.,1.,1.,1.,1.,1.,1.,1.,1.,1.,1.,1.,1.,1.,1.,1.,
1.,1.,1.,1.,1.,1.,1.,1.,1.,1.,1.,1.,1.,1.,1.,1.,1.,1.,1.,1.,1.,1.,1.,1.,
1.,1.,1.,1.,1.,1.,1.,1.,1.,1.,1.,1.,1.,1.,1.,1.,1.,1.,1.,1.,1.,1.,1.,1.,
1.,1.,1.,1.,1.,1.,1.,1.,1.,1.,1.,1.,1.,1.,1.,1.,1.,1.,1.,1.,1.,1.,1.,1.,
1.,1.,1.,1.,1.,1.,1.,1.,1.,1.,1.,1.,1.,1.,1.,1.,1.,1.,1.,1.,1.,1.,1.,1.,
1.,1.,1.,1.,1.,1.,1.,1.,1.,1.,1.,1.,1.,1.,1.,1.,1.,1.,1.,1.,1.,1.,1.,1.,
1.,1.,1.,1.,1.,1.,1.,1.,1.,1.,1.,1.,1.,1.,1.,1.,1.,1.,1.,1.,1.,1.,1.,1.,
1.,1.,1.,1.,1.,1.,1.,1.,1.,1.,1.,1.,1.,1.,1.,1.,1.,1.,1.,1.,1.))
REPRESENTATION_ITEM('')
);
#716=(
BOUNDED_CURVE()
B_SPLINE_CURVE(5,(#180309,#180310,#180311,#180312,#180313,#180314,#180315,
#180316,#180317,#180318,#180319,#180320,#180321,#180322,#180323,#180324,
#180325,#180326,#180327,#180328,#180329,#180330,#180331,#180332,#180333,
#180334,#180335,#180336,#180337,#180338,#180339,#180340,#180341,#180342,
#180343,#180344,#180345,#180346,#180347,#180348,#180349,#180350,#180351,
#180352,#180353,#180354,#180355,#180356,#180357,#180358,#180359,#180360,
#180361,#180362,#180363,#180364,#180365,#180366,#180367,#180368,#180369,
#180370,#180371,#180372,#180373,#180374,#180375,#180376,#180377,#180378,
#180379,#180380,#180381,#180382,#180383,#180384,#180385,#180386,#180387,
#180388,#180389,#180390,#180391,#180392,#180393,#180394,#180395,#180396,
#180397,#180398,#180399,#180400,#180401,#180402,#180403,#180404,#180405,
#180406,#180407,#180408,#180409,#180410,#180411,#180412,#180413,#180414,
#180415,#180416,#180417,#180418,#180419,#180420,#180421,#180422,#180423,
#180424,#180425,#180426,#180427,#180428,#180429,#180430,#180431,#180432,
#180433,#180434,#180435,#180436,#180437,#180438,#180439,#180440,#180441,
#180442,#180443,#180444,#180445,#180446,#180447,#180448,#180449,#180450,
#180451,#180452,#180453,#180454,#180455,#180456,#180457,#180458,#180459,
#180460,#180461,#180462,#180463,#180464,#180465,#180466,#180467,#180468,
#180469,#180470,#180471,#180472,#180473,#180474,#180475,#180476,#180477,
#180478,#180479,#180480,#180481,#180482,#180483,#180484,#180485,#180486,
#180487,#180488,#180489,#180490,#180491,#180492,#180493,#180494,#180495,
#180496,#180497,#180498,#180499,#180500,#180501,#180502,#180503,#180504,
#180505,#180506,#180507,#180508,#180509,#180510,#180511,#180512,#180513),
 .UNSPECIFIED.,.F.,.F.)
B_SPLINE_CURVE_WITH_KNOTS((6,1,1,1,1,1,1,1,1,1,1,1,1,1,1,1,1,1,1,1,1,1,
1,1,1,1,1,1,1,1,1,1,1,1,1,1,1,1,1,1,1,1,1,1,1,1,1,1,1,1,1,1,1,1,1,1,1,1,
1,1,1,1,1,1,1,1,1,1,1,1,1,1,1,1,1,1,1,1,1,1,1,1,1,1,1,1,1,1,1,1,1,1,1,1,
1,1,1,1,1,1,1,1,1,1,1,1,1,1,1,1,1,1,1,1,1,1,1,1,1,1,1,1,1,1,1,1,1,1,1,1,
1,1,1,1,1,1,1,1,1,1,1,1,1,1,1,1,1,1,1,1,1,1,1,1,1,1,1,1,1,1,1,1,1,1,1,1,
1,1,1,1,1,1,1,1,1,1,1,1,1,1,1,1,1,1,1,1,1,1,1,1,1,1,1,1,1,1,1,1,1,1,6),
(-1.,-0.995000000000001,-0.990000000000001,-0.985000000000001,-0.980000000000001,
-0.975000000000001,-0.970000000000001,-0.965000000000001,-0.960000000000001,
-0.955000000000001,-0.950000000000001,-0.945000000000001,-0.940000000000001,
-0.935000000000001,-0.930000000000001,-0.925000000000001,-0.920000000000001,
-0.915000000000001,-0.910000000000001,-0.905000000000001,-0.900000000000001,
-0.895000000000001,-0.890000000000001,-0.885000000000001,-0.880000000000001,
-0.875000000000001,-0.870000000000001,-0.865000000000001,-0.860000000000001,
-0.855000000000001,-0.850000000000001,-0.845000000000001,-0.840000000000001,
-0.835000000000001,-0.830000000000001,-0.825000000000001,-0.820000000000001,
-0.815000000000001,-0.810000000000001,-0.805000000000001,-0.800000000000001,
-0.795000000000001,-0.790000000000001,-0.785000000000001,-0.780000000000001,
-0.775000000000001,-0.770000000000001,-0.765000000000001,-0.760000000000001,
-0.755000000000001,-0.750000000000001,-0.745000000000001,-0.740000000000001,
-0.735000000000001,-0.730000000000001,-0.725000000000001,-0.720000000000001,
-0.715000000000001,-0.710000000000001,-0.705000000000001,-0.700000000000001,
-0.695000000000001,-0.690000000000001,-0.685,-0.68,-0.675,-0.67,-0.665,
-0.66,-0.655,-0.65,-0.645,-0.64,-0.635,-0.63,-0.625,-0.62,-0.615,-0.61,
-0.605,-0.6,-0.595,-0.59,-0.585,-0.58,-0.575,-0.57,-0.565,-0.56,-0.555,
-0.55,-0.545,-0.54,-0.535,-0.53,-0.525,-0.52,-0.515,-0.51,-0.505,-0.5,-0.495,
-0.49,-0.485,-0.48,-0.475,-0.47,-0.465,-0.46,-0.455,-0.45,-0.445,-0.44,
-0.435,-0.43,-0.425,-0.42,-0.415,-0.41,-0.405,-0.4,-0.395,-0.39,-0.385,
-0.38,-0.375,-0.37,-0.365,-0.36,-0.355,-0.35,-0.345,-0.34,-0.335,-0.33,
-0.325,-0.32,-0.315,-0.31,-0.305,-0.3,-0.295,-0.29,-0.285,-0.28,-0.275,
-0.27,-0.265,-0.26,-0.255,-0.25,-0.245,-0.24,-0.235,-0.23,-0.225,-0.22,
-0.215,-0.21,-0.205,-0.2,-0.195,-0.19,-0.185,-0.18,-0.175,-0.17,-0.165,
-0.16,-0.155,-0.15,-0.145,-0.14,-0.135,-0.13,-0.125,-0.12,-0.115,-0.11,
-0.105,-0.1,-0.095,-0.09,-0.085,-0.08,-0.075,-0.07,-0.065,-0.06,-0.055,
-0.05,-0.045,-0.04,-0.035,-0.03,-0.025,-0.02,-0.015,-0.01,-0.005,0.),
 .UNSPECIFIED.)
CURVE()
GEOMETRIC_REPRESENTATION_ITEM()
RATIONAL_B_SPLINE_CURVE((1.,1.,1.,1.,1.,1.,1.,1.,1.,1.,1.,1.,1.,1.,1.,1.,
1.,1.,1.,1.,1.,1.,1.,1.,1.,1.,1.,1.,1.,1.,1.,1.,1.,1.,1.,1.,1.,1.,1.,1.,
1.,1.,1.,1.,1.,1.,1.,1.,1.,1.,1.,1.,1.,1.,1.,1.,1.,1.,1.,1.,1.,1.,1.,1.,
1.,1.,1.,1.,1.,1.,1.,1.,1.,1.,1.,1.,1.,1.,1.,1.,1.,1.,1.,1.,1.,1.,1.,1.,
1.,1.,1.,1.,1.,1.,1.,1.,1.,1.,1.,1.,1.,1.,1.,1.,1.,1.,1.,1.,1.,1.,1.,1.,
1.,1.,1.,1.,1.,1.,1.,1.,1.,1.,1.,1.,1.,1.,1.,1.,1.,1.,1.,1.,1.,1.,1.,1.,
1.,1.,1.,1.,1.,1.,1.,1.,1.,1.,1.,1.,1.,1.,1.,1.,1.,1.,1.,1.,1.,1.,1.,1.,
1.,1.,1.,1.,1.,1.,1.,1.,1.,1.,1.,1.,1.,1.,1.,1.,1.,1.,1.,1.,1.,1.,1.,1.,
1.,1.,1.,1.,1.,1.,1.,1.,1.,1.,1.,1.,1.,1.,1.,1.,1.,1.,1.,1.,1.))
REPRESENTATION_ITEM('')
);
#717=(
BOUNDED_CURVE()
B_SPLINE_CURVE(5,(#180525,#180526,#180527,#180528,#180529,#180530,#180531,
#180532,#180533,#180534,#180535,#180536,#180537,#180538,#180539,#180540,
#180541,#180542,#180543,#180544,#180545,#180546,#180547,#180548,#180549,
#180550,#180551,#180552,#180553,#180554,#180555,#180556,#180557,#180558,
#180559,#180560,#180561,#180562,#180563,#180564,#180565,#180566,#180567,
#180568,#180569,#180570,#180571,#180572,#180573,#180574,#180575,#180576,
#180577,#180578,#180579,#180580,#180581,#180582,#180583,#180584,#180585,
#180586,#180587,#180588,#180589,#180590,#180591,#180592,#180593,#180594,
#180595,#180596,#180597,#180598,#180599,#180600,#180601,#180602,#180603,
#180604,#180605,#180606,#180607,#180608,#180609,#180610,#180611,#180612,
#180613,#180614,#180615,#180616,#180617,#180618,#180619,#180620,#180621,
#180622,#180623,#180624,#180625,#180626,#180627,#180628,#180629,#180630,
#180631,#180632,#180633,#180634,#180635,#180636,#180637,#180638,#180639,
#180640,#180641,#180642,#180643,#180644,#180645,#180646,#180647,#180648,
#180649,#180650,#180651,#180652,#180653,#180654,#180655,#180656,#180657,
#180658,#180659,#180660,#180661,#180662,#180663,#180664,#180665,#180666,
#180667,#180668,#180669,#180670,#180671,#180672,#180673,#180674,#180675,
#180676,#180677,#180678,#180679,#180680,#180681,#180682,#180683,#180684,
#180685,#180686,#180687,#180688,#180689,#180690,#180691,#180692,#180693,
#180694,#180695,#180696,#180697,#180698,#180699,#180700,#180701,#180702,
#180703,#180704,#180705,#180706,#180707,#180708,#180709,#180710,#180711,
#180712,#180713,#180714,#180715,#180716,#180717,#180718,#180719,#180720,
#180721,#180722,#180723,#180724,#180725,#180726,#180727,#180728,#180729),
 .UNSPECIFIED.,.F.,.F.)
B_SPLINE_CURVE_WITH_KNOTS((6,1,1,1,1,1,1,1,1,1,1,1,1,1,1,1,1,1,1,1,1,1,
1,1,1,1,1,1,1,1,1,1,1,1,1,1,1,1,1,1,1,1,1,1,1,1,1,1,1,1,1,1,1,1,1,1,1,1,
1,1,1,1,1,1,1,1,1,1,1,1,1,1,1,1,1,1,1,1,1,1,1,1,1,1,1,1,1,1,1,1,1,1,1,1,
1,1,1,1,1,1,1,1,1,1,1,1,1,1,1,1,1,1,1,1,1,1,1,1,1,1,1,1,1,1,1,1,1,1,1,1,
1,1,1,1,1,1,1,1,1,1,1,1,1,1,1,1,1,1,1,1,1,1,1,1,1,1,1,1,1,1,1,1,1,1,1,1,
1,1,1,1,1,1,1,1,1,1,1,1,1,1,1,1,1,1,1,1,1,1,1,1,1,1,1,1,1,1,1,1,1,1,6),
(0.,0.005,0.01,0.015,0.02,0.025,0.03,0.035,0.04,0.045,0.05,0.055,0.06,0.065,
0.07,0.075,0.08,0.085,0.09,0.095,0.1,0.105,0.11,0.115,0.12,0.125,0.13,0.135,
0.14,0.145,0.15,0.155,0.16,0.165,0.17,0.175,0.18,0.185,0.19,0.195,0.2,0.205,
0.21,0.215,0.22,0.225,0.23,0.235,0.24,0.245,0.25,0.255,0.26,0.265,0.27,
0.275,0.28,0.285,0.29,0.295,0.3,0.305,0.31,0.315,0.32,0.325,0.33,0.335,
0.34,0.345,0.35,0.355,0.36,0.365,0.37,0.375,0.38,0.385,0.39,0.395,0.4,0.405,
0.41,0.415,0.42,0.425,0.43,0.435,0.44,0.445,0.45,0.455,0.46,0.465,0.47,
0.475,0.48,0.485,0.49,0.495,0.5,0.505,0.51,0.515,0.52,0.525,0.53,0.535,
0.54,0.545,0.55,0.555,0.56,0.565,0.57,0.575,0.58,0.585,0.59,0.595,0.6,0.605,
0.61,0.615,0.62,0.625,0.63,0.635,0.64,0.645,0.65,0.655,0.66,0.665,0.67,
0.675,0.68,0.685,0.690000000000001,0.695000000000001,0.700000000000001,
0.705000000000001,0.710000000000001,0.715000000000001,0.720000000000001,
0.725000000000001,0.730000000000001,0.735000000000001,0.740000000000001,
0.745000000000001,0.750000000000001,0.755000000000001,0.760000000000001,
0.765000000000001,0.770000000000001,0.775000000000001,0.780000000000001,
0.785000000000001,0.790000000000001,0.795000000000001,0.800000000000001,
0.805000000000001,0.810000000000001,0.815000000000001,0.820000000000001,
0.825000000000001,0.830000000000001,0.835000000000001,0.840000000000001,
0.845000000000001,0.850000000000001,0.855000000000001,0.860000000000001,
0.865000000000001,0.870000000000001,0.875000000000001,0.880000000000001,
0.885000000000001,0.890000000000001,0.895000000000001,0.900000000000001,
0.905000000000001,0.910000000000001,0.915000000000001,0.920000000000001,
0.925000000000001,0.930000000000001,0.935000000000001,0.940000000000001,
0.945000000000001,0.950000000000001,0.955000000000001,0.960000000000001,
0.965000000000001,0.970000000000001,0.975000000000001,0.980000000000001,
0.985000000000001,0.990000000000001,0.995000000000001,1.),.UNSPECIFIED.)
CURVE()
GEOMETRIC_REPRESENTATION_ITEM()
RATIONAL_B_SPLINE_CURVE((1.,1.,1.,1.,1.,1.,1.,1.,1.,1.,1.,1.,1.,1.,1.,1.,
1.,1.,1.,1.,1.,1.,1.,1.,1.,1.,1.,1.,1.,1.,1.,1.,1.,1.,1.,1.,1.,1.,1.,1.,
1.,1.,1.,1.,1.,1.,1.,1.,1.,1.,1.,1.,1.,1.,1.,1.,1.,1.,1.,1.,1.,1.,1.,1.,
1.,1.,1.,1.,1.,1.,1.,1.,1.,1.,1.,1.,1.,1.,1.,1.,1.,1.,1.,1.,1.,1.,1.,1.,
1.,1.,1.,1.,1.,1.,1.,1.,1.,1.,1.,1.,1.,1.,1.,1.,1.,1.,1.,1.,1.,1.,1.,1.,
1.,1.,1.,1.,1.,1.,1.,1.,1.,1.,1.,1.,1.,1.,1.,1.,1.,1.,1.,1.,1.,1.,1.,1.,
1.,1.,1.,1.,1.,1.,1.,1.,1.,1.,1.,1.,1.,1.,1.,1.,1.,1.,1.,1.,1.,1.,1.,1.,
1.,1.,1.,1.,1.,1.,1.,1.,1.,1.,1.,1.,1.,1.,1.,1.,1.,1.,1.,1.,1.,1.,1.,1.,
1.,1.,1.,1.,1.,1.,1.,1.,1.,1.,1.,1.,1.,1.,1.,1.,1.,1.,1.,1.,1.))
REPRESENTATION_ITEM('')
);
#718=(
BOUNDED_CURVE()
B_SPLINE_CURVE(5,(#180733,#180734,#180735,#180736,#180737,#180738,#180739,
#180740,#180741,#180742,#180743,#180744,#180745,#180746,#180747,#180748,
#180749,#180750,#180751,#180752,#180753,#180754,#180755,#180756,#180757,
#180758,#180759,#180760,#180761,#180762,#180763,#180764,#180765,#180766,
#180767,#180768,#180769,#180770,#180771,#180772,#180773,#180774,#180775,
#180776,#180777,#180778,#180779,#180780,#180781,#180782,#180783,#180784,
#180785,#180786,#180787,#180788,#180789,#180790,#180791,#180792,#180793,
#180794,#180795,#180796,#180797,#180798,#180799,#180800,#180801,#180802,
#180803,#180804,#180805,#180806,#180807,#180808,#180809,#180810,#180811,
#180812,#180813,#180814,#180815,#180816,#180817,#180818,#180819,#180820,
#180821,#180822,#180823,#180824,#180825,#180826,#180827,#180828,#180829,
#180830,#180831,#180832,#180833,#180834,#180835,#180836,#180837,#180838,
#180839,#180840,#180841,#180842,#180843,#180844,#180845,#180846,#180847,
#180848,#180849,#180850,#180851,#180852,#180853,#180854,#180855,#180856,
#180857,#180858,#180859,#180860,#180861,#180862,#180863,#180864,#180865,
#180866,#180867,#180868,#180869,#180870,#180871,#180872,#180873,#180874,
#180875,#180876,#180877,#180878,#180879,#180880,#180881,#180882,#180883,
#180884,#180885,#180886,#180887,#180888,#180889,#180890,#180891,#180892,
#180893,#180894,#180895,#180896,#180897,#180898,#180899,#180900,#180901,
#180902,#180903,#180904,#180905,#180906,#180907,#180908,#180909,#180910,
#180911,#180912,#180913,#180914,#180915,#180916,#180917,#180918,#180919,
#180920,#180921,#180922,#180923,#180924,#180925,#180926,#180927,#180928,
#180929,#180930,#180931,#180932,#180933,#180934,#180935,#180936,#180937),
 .UNSPECIFIED.,.F.,.F.)
B_SPLINE_CURVE_WITH_KNOTS((6,1,1,1,1,1,1,1,1,1,1,1,1,1,1,1,1,1,1,1,1,1,
1,1,1,1,1,1,1,1,1,1,1,1,1,1,1,1,1,1,1,1,1,1,1,1,1,1,1,1,1,1,1,1,1,1,1,1,
1,1,1,1,1,1,1,1,1,1,1,1,1,1,1,1,1,1,1,1,1,1,1,1,1,1,1,1,1,1,1,1,1,1,1,1,
1,1,1,1,1,1,1,1,1,1,1,1,1,1,1,1,1,1,1,1,1,1,1,1,1,1,1,1,1,1,1,1,1,1,1,1,
1,1,1,1,1,1,1,1,1,1,1,1,1,1,1,1,1,1,1,1,1,1,1,1,1,1,1,1,1,1,1,1,1,1,1,1,
1,1,1,1,1,1,1,1,1,1,1,1,1,1,1,1,1,1,1,1,1,1,1,1,1,1,1,1,1,1,1,1,1,1,6),
(-1.,-0.995000000000001,-0.990000000000001,-0.985000000000001,-0.980000000000001,
-0.975000000000001,-0.970000000000001,-0.965000000000001,-0.960000000000001,
-0.955000000000001,-0.950000000000001,-0.945000000000001,-0.940000000000001,
-0.935000000000001,-0.930000000000001,-0.925000000000001,-0.920000000000001,
-0.915000000000001,-0.910000000000001,-0.905000000000001,-0.900000000000001,
-0.895000000000001,-0.890000000000001,-0.885000000000001,-0.880000000000001,
-0.875000000000001,-0.870000000000001,-0.865000000000001,-0.860000000000001,
-0.855000000000001,-0.850000000000001,-0.845000000000001,-0.840000000000001,
-0.835000000000001,-0.830000000000001,-0.825000000000001,-0.820000000000001,
-0.815000000000001,-0.810000000000001,-0.805000000000001,-0.800000000000001,
-0.795000000000001,-0.790000000000001,-0.785000000000001,-0.780000000000001,
-0.775000000000001,-0.770000000000001,-0.765000000000001,-0.760000000000001,
-0.755000000000001,-0.750000000000001,-0.745000000000001,-0.740000000000001,
-0.735000000000001,-0.730000000000001,-0.725000000000001,-0.720000000000001,
-0.715000000000001,-0.710000000000001,-0.705000000000001,-0.700000000000001,
-0.695000000000001,-0.690000000000001,-0.685,-0.68,-0.675,-0.67,-0.665,
-0.66,-0.655,-0.65,-0.645,-0.64,-0.635,-0.63,-0.625,-0.62,-0.615,-0.61,
-0.605,-0.6,-0.595,-0.59,-0.585,-0.58,-0.575,-0.57,-0.565,-0.56,-0.555,
-0.55,-0.545,-0.54,-0.535,-0.53,-0.525,-0.52,-0.515,-0.51,-0.505,-0.5,-0.495,
-0.49,-0.485,-0.48,-0.475,-0.47,-0.465,-0.46,-0.455,-0.45,-0.445,-0.44,
-0.435,-0.43,-0.425,-0.42,-0.415,-0.41,-0.405,-0.4,-0.395,-0.39,-0.385,
-0.38,-0.375,-0.37,-0.365,-0.36,-0.355,-0.35,-0.345,-0.34,-0.335,-0.33,
-0.325,-0.32,-0.315,-0.31,-0.305,-0.3,-0.295,-0.29,-0.285,-0.28,-0.275,
-0.27,-0.265,-0.26,-0.255,-0.25,-0.245,-0.24,-0.235,-0.23,-0.225,-0.22,
-0.215,-0.21,-0.205,-0.2,-0.195,-0.19,-0.185,-0.18,-0.175,-0.17,-0.165,
-0.16,-0.155,-0.15,-0.145,-0.14,-0.135,-0.13,-0.125,-0.12,-0.115,-0.11,
-0.105,-0.1,-0.095,-0.09,-0.085,-0.08,-0.075,-0.07,-0.065,-0.06,-0.055,
-0.05,-0.045,-0.04,-0.035,-0.03,-0.025,-0.02,-0.015,-0.01,-0.005,0.),
 .UNSPECIFIED.)
CURVE()
GEOMETRIC_REPRESENTATION_ITEM()
RATIONAL_B_SPLINE_CURVE((1.,1.,1.,1.,1.,1.,1.,1.,1.,1.,1.,1.,1.,1.,1.,1.,
1.,1.,1.,1.,1.,1.,1.,1.,1.,1.,1.,1.,1.,1.,1.,1.,1.,1.,1.,1.,1.,1.,1.,1.,
1.,1.,1.,1.,1.,1.,1.,1.,1.,1.,1.,1.,1.,1.,1.,1.,1.,1.,1.,1.,1.,1.,1.,1.,
1.,1.,1.,1.,1.,1.,1.,1.,1.,1.,1.,1.,1.,1.,1.,1.,1.,1.,1.,1.,1.,1.,1.,1.,
1.,1.,1.,1.,1.,1.,1.,1.,1.,1.,1.,1.,1.,1.,1.,1.,1.,1.,1.,1.,1.,1.,1.,1.,
1.,1.,1.,1.,1.,1.,1.,1.,1.,1.,1.,1.,1.,1.,1.,1.,1.,1.,1.,1.,1.,1.,1.,1.,
1.,1.,1.,1.,1.,1.,1.,1.,1.,1.,1.,1.,1.,1.,1.,1.,1.,1.,1.,1.,1.,1.,1.,1.,
1.,1.,1.,1.,1.,1.,1.,1.,1.,1.,1.,1.,1.,1.,1.,1.,1.,1.,1.,1.,1.,1.,1.,1.,
1.,1.,1.,1.,1.,1.,1.,1.,1.,1.,1.,1.,1.,1.,1.,1.,1.,1.,1.,1.,1.))
REPRESENTATION_ITEM('')
);
#719=(
BOUNDED_CURVE()
B_SPLINE_CURVE(5,(#180949,#180950,#180951,#180952,#180953,#180954,#180955,
#180956,#180957,#180958,#180959,#180960,#180961,#180962,#180963,#180964,
#180965,#180966,#180967,#180968,#180969,#180970,#180971,#180972,#180973,
#180974,#180975,#180976,#180977,#180978,#180979,#180980,#180981,#180982,
#180983,#180984,#180985,#180986,#180987,#180988,#180989,#180990,#180991,
#180992,#180993,#180994,#180995,#180996,#180997,#180998,#180999,#181000,
#181001,#181002,#181003,#181004,#181005,#181006,#181007,#181008,#181009,
#181010,#181011,#181012,#181013,#181014,#181015,#181016,#181017,#181018,
#181019,#181020,#181021,#181022,#181023,#181024,#181025,#181026,#181027,
#181028,#181029,#181030,#181031,#181032,#181033,#181034,#181035,#181036,
#181037,#181038,#181039,#181040,#181041,#181042,#181043,#181044,#181045,
#181046,#181047,#181048,#181049,#181050,#181051,#181052,#181053,#181054,
#181055,#181056,#181057,#181058,#181059,#181060,#181061,#181062,#181063,
#181064,#181065,#181066,#181067,#181068,#181069,#181070,#181071,#181072,
#181073,#181074,#181075,#181076,#181077,#181078,#181079,#181080,#181081,
#181082,#181083,#181084,#181085,#181086,#181087,#181088,#181089,#181090,
#181091,#181092,#181093,#181094,#181095,#181096,#181097,#181098,#181099,
#181100,#181101,#181102,#181103,#181104,#181105,#181106,#181107,#181108,
#181109,#181110,#181111,#181112,#181113,#181114,#181115,#181116,#181117,
#181118,#181119,#181120,#181121,#181122,#181123,#181124,#181125,#181126,
#181127,#181128,#181129,#181130,#181131,#181132,#181133,#181134,#181135,
#181136,#181137,#181138,#181139,#181140,#181141,#181142,#181143,#181144,
#181145,#181146,#181147,#181148,#181149,#181150,#181151,#181152,#181153),
 .UNSPECIFIED.,.F.,.F.)
B_SPLINE_CURVE_WITH_KNOTS((6,1,1,1,1,1,1,1,1,1,1,1,1,1,1,1,1,1,1,1,1,1,
1,1,1,1,1,1,1,1,1,1,1,1,1,1,1,1,1,1,1,1,1,1,1,1,1,1,1,1,1,1,1,1,1,1,1,1,
1,1,1,1,1,1,1,1,1,1,1,1,1,1,1,1,1,1,1,1,1,1,1,1,1,1,1,1,1,1,1,1,1,1,1,1,
1,1,1,1,1,1,1,1,1,1,1,1,1,1,1,1,1,1,1,1,1,1,1,1,1,1,1,1,1,1,1,1,1,1,1,1,
1,1,1,1,1,1,1,1,1,1,1,1,1,1,1,1,1,1,1,1,1,1,1,1,1,1,1,1,1,1,1,1,1,1,1,1,
1,1,1,1,1,1,1,1,1,1,1,1,1,1,1,1,1,1,1,1,1,1,1,1,1,1,1,1,1,1,1,1,1,1,6),
(0.,0.005,0.01,0.015,0.02,0.025,0.03,0.035,0.04,0.045,0.05,0.055,0.06,0.065,
0.07,0.075,0.08,0.085,0.09,0.095,0.1,0.105,0.11,0.115,0.12,0.125,0.13,0.135,
0.14,0.145,0.15,0.155,0.16,0.165,0.17,0.175,0.18,0.185,0.19,0.195,0.2,0.205,
0.21,0.215,0.22,0.225,0.23,0.235,0.24,0.245,0.25,0.255,0.26,0.265,0.27,
0.275,0.28,0.285,0.29,0.295,0.3,0.305,0.31,0.315,0.32,0.325,0.33,0.335,
0.34,0.345,0.35,0.355,0.36,0.365,0.37,0.375,0.38,0.385,0.39,0.395,0.4,0.405,
0.41,0.415,0.42,0.425,0.43,0.435,0.44,0.445,0.45,0.455,0.46,0.465,0.47,
0.475,0.48,0.485,0.49,0.495,0.5,0.505,0.51,0.515,0.52,0.525,0.53,0.535,
0.54,0.545,0.55,0.555,0.56,0.565,0.57,0.575,0.58,0.585,0.59,0.595,0.6,0.605,
0.61,0.615,0.62,0.625,0.63,0.635,0.64,0.645,0.65,0.655,0.66,0.665,0.67,
0.675,0.68,0.685,0.690000000000001,0.695000000000001,0.700000000000001,
0.705000000000001,0.710000000000001,0.715000000000001,0.720000000000001,
0.725000000000001,0.730000000000001,0.735000000000001,0.740000000000001,
0.745000000000001,0.750000000000001,0.755000000000001,0.760000000000001,
0.765000000000001,0.770000000000001,0.775000000000001,0.780000000000001,
0.785000000000001,0.790000000000001,0.795000000000001,0.800000000000001,
0.805000000000001,0.810000000000001,0.815000000000001,0.820000000000001,
0.825000000000001,0.830000000000001,0.835000000000001,0.840000000000001,
0.845000000000001,0.850000000000001,0.855000000000001,0.860000000000001,
0.865000000000001,0.870000000000001,0.875000000000001,0.880000000000001,
0.885000000000001,0.890000000000001,0.895000000000001,0.900000000000001,
0.905000000000001,0.910000000000001,0.915000000000001,0.920000000000001,
0.925000000000001,0.930000000000001,0.935000000000001,0.940000000000001,
0.945000000000001,0.950000000000001,0.955000000000001,0.960000000000001,
0.965000000000001,0.970000000000001,0.975000000000001,0.980000000000001,
0.985000000000001,0.990000000000001,0.995000000000001,1.),.UNSPECIFIED.)
CURVE()
GEOMETRIC_REPRESENTATION_ITEM()
RATIONAL_B_SPLINE_CURVE((1.,1.,1.,1.,1.,1.,1.,1.,1.,1.,1.,1.,1.,1.,1.,1.,
1.,1.,1.,1.,1.,1.,1.,1.,1.,1.,1.,1.,1.,1.,1.,1.,1.,1.,1.,1.,1.,1.,1.,1.,
1.,1.,1.,1.,1.,1.,1.,1.,1.,1.,1.,1.,1.,1.,1.,1.,1.,1.,1.,1.,1.,1.,1.,1.,
1.,1.,1.,1.,1.,1.,1.,1.,1.,1.,1.,1.,1.,1.,1.,1.,1.,1.,1.,1.,1.,1.,1.,1.,
1.,1.,1.,1.,1.,1.,1.,1.,1.,1.,1.,1.,1.,1.,1.,1.,1.,1.,1.,1.,1.,1.,1.,1.,
1.,1.,1.,1.,1.,1.,1.,1.,1.,1.,1.,1.,1.,1.,1.,1.,1.,1.,1.,1.,1.,1.,1.,1.,
1.,1.,1.,1.,1.,1.,1.,1.,1.,1.,1.,1.,1.,1.,1.,1.,1.,1.,1.,1.,1.,1.,1.,1.,
1.,1.,1.,1.,1.,1.,1.,1.,1.,1.,1.,1.,1.,1.,1.,1.,1.,1.,1.,1.,1.,1.,1.,1.,
1.,1.,1.,1.,1.,1.,1.,1.,1.,1.,1.,1.,1.,1.,1.,1.,1.,1.,1.,1.,1.))
REPRESENTATION_ITEM('')
);
#720=(
BOUNDED_CURVE()
B_SPLINE_CURVE(5,(#181157,#181158,#181159,#181160,#181161,#181162,#181163,
#181164,#181165,#181166,#181167,#181168,#181169,#181170,#181171,#181172,
#181173,#181174,#181175,#181176,#181177,#181178,#181179,#181180,#181181,
#181182,#181183,#181184,#181185,#181186,#181187,#181188,#181189,#181190,
#181191,#181192,#181193,#181194,#181195,#181196,#181197,#181198,#181199,
#181200,#181201,#181202,#181203,#181204,#181205,#181206,#181207,#181208,
#181209,#181210,#181211,#181212,#181213,#181214,#181215,#181216,#181217,
#181218,#181219,#181220,#181221,#181222,#181223,#181224,#181225,#181226,
#181227,#181228,#181229,#181230,#181231,#181232,#181233,#181234,#181235,
#181236,#181237,#181238,#181239,#181240,#181241,#181242,#181243,#181244,
#181245,#181246,#181247,#181248,#181249,#181250,#181251,#181252,#181253,
#181254,#181255,#181256,#181257,#181258,#181259,#181260,#181261,#181262,
#181263,#181264,#181265,#181266,#181267,#181268,#181269,#181270,#181271,
#181272,#181273,#181274,#181275,#181276,#181277,#181278,#181279,#181280,
#181281,#181282,#181283,#181284,#181285,#181286,#181287,#181288,#181289,
#181290,#181291,#181292,#181293,#181294,#181295,#181296,#181297,#181298,
#181299,#181300,#181301,#181302,#181303,#181304,#181305,#181306,#181307,
#181308,#181309,#181310,#181311,#181312,#181313,#181314,#181315,#181316,
#181317,#181318,#181319,#181320,#181321,#181322,#181323,#181324,#181325,
#181326,#181327,#181328,#181329,#181330,#181331,#181332,#181333,#181334,
#181335,#181336,#181337,#181338,#181339,#181340,#181341,#181342,#181343,
#181344,#181345,#181346,#181347,#181348,#181349,#181350,#181351,#181352,
#181353,#181354,#181355,#181356,#181357,#181358,#181359,#181360,#181361),
 .UNSPECIFIED.,.F.,.F.)
B_SPLINE_CURVE_WITH_KNOTS((6,1,1,1,1,1,1,1,1,1,1,1,1,1,1,1,1,1,1,1,1,1,
1,1,1,1,1,1,1,1,1,1,1,1,1,1,1,1,1,1,1,1,1,1,1,1,1,1,1,1,1,1,1,1,1,1,1,1,
1,1,1,1,1,1,1,1,1,1,1,1,1,1,1,1,1,1,1,1,1,1,1,1,1,1,1,1,1,1,1,1,1,1,1,1,
1,1,1,1,1,1,1,1,1,1,1,1,1,1,1,1,1,1,1,1,1,1,1,1,1,1,1,1,1,1,1,1,1,1,1,1,
1,1,1,1,1,1,1,1,1,1,1,1,1,1,1,1,1,1,1,1,1,1,1,1,1,1,1,1,1,1,1,1,1,1,1,1,
1,1,1,1,1,1,1,1,1,1,1,1,1,1,1,1,1,1,1,1,1,1,1,1,1,1,1,1,1,1,1,1,1,1,6),
(-1.,-0.995000000000001,-0.990000000000001,-0.985000000000001,-0.980000000000001,
-0.975000000000001,-0.970000000000001,-0.965000000000001,-0.960000000000001,
-0.955000000000001,-0.950000000000001,-0.945000000000001,-0.940000000000001,
-0.935000000000001,-0.930000000000001,-0.925000000000001,-0.920000000000001,
-0.915000000000001,-0.910000000000001,-0.905000000000001,-0.900000000000001,
-0.895000000000001,-0.890000000000001,-0.885000000000001,-0.880000000000001,
-0.875000000000001,-0.870000000000001,-0.865000000000001,-0.860000000000001,
-0.855000000000001,-0.850000000000001,-0.845000000000001,-0.840000000000001,
-0.835000000000001,-0.830000000000001,-0.825000000000001,-0.820000000000001,
-0.815000000000001,-0.810000000000001,-0.805000000000001,-0.800000000000001,
-0.795000000000001,-0.790000000000001,-0.785000000000001,-0.780000000000001,
-0.775000000000001,-0.770000000000001,-0.765000000000001,-0.760000000000001,
-0.755000000000001,-0.750000000000001,-0.745000000000001,-0.740000000000001,
-0.735000000000001,-0.730000000000001,-0.725000000000001,-0.720000000000001,
-0.715000000000001,-0.710000000000001,-0.705000000000001,-0.700000000000001,
-0.695000000000001,-0.690000000000001,-0.685,-0.68,-0.675,-0.67,-0.665,
-0.66,-0.655,-0.65,-0.645,-0.64,-0.635,-0.63,-0.625,-0.62,-0.615,-0.61,
-0.605,-0.6,-0.595,-0.59,-0.585,-0.58,-0.575,-0.57,-0.565,-0.56,-0.555,
-0.55,-0.545,-0.54,-0.535,-0.53,-0.525,-0.52,-0.515,-0.51,-0.505,-0.5,-0.495,
-0.49,-0.485,-0.48,-0.475,-0.47,-0.465,-0.46,-0.455,-0.45,-0.445,-0.44,
-0.435,-0.43,-0.425,-0.42,-0.415,-0.41,-0.405,-0.4,-0.395,-0.39,-0.385,
-0.38,-0.375,-0.37,-0.365,-0.36,-0.355,-0.35,-0.345,-0.34,-0.335,-0.33,
-0.325,-0.32,-0.315,-0.31,-0.305,-0.3,-0.295,-0.29,-0.285,-0.28,-0.275,
-0.27,-0.265,-0.26,-0.255,-0.25,-0.245,-0.24,-0.235,-0.23,-0.225,-0.22,
-0.215,-0.21,-0.205,-0.2,-0.195,-0.19,-0.185,-0.18,-0.175,-0.17,-0.165,
-0.16,-0.155,-0.15,-0.145,-0.14,-0.135,-0.13,-0.125,-0.12,-0.115,-0.11,
-0.105,-0.1,-0.095,-0.09,-0.085,-0.08,-0.075,-0.07,-0.065,-0.06,-0.055,
-0.05,-0.045,-0.04,-0.035,-0.03,-0.025,-0.02,-0.015,-0.01,-0.005,0.),
 .UNSPECIFIED.)
CURVE()
GEOMETRIC_REPRESENTATION_ITEM()
RATIONAL_B_SPLINE_CURVE((1.,1.,1.,1.,1.,1.,1.,1.,1.,1.,1.,1.,1.,1.,1.,1.,
1.,1.,1.,1.,1.,1.,1.,1.,1.,1.,1.,1.,1.,1.,1.,1.,1.,1.,1.,1.,1.,1.,1.,1.,
1.,1.,1.,1.,1.,1.,1.,1.,1.,1.,1.,1.,1.,1.,1.,1.,1.,1.,1.,1.,1.,1.,1.,1.,
1.,1.,1.,1.,1.,1.,1.,1.,1.,1.,1.,1.,1.,1.,1.,1.,1.,1.,1.,1.,1.,1.,1.,1.,
1.,1.,1.,1.,1.,1.,1.,1.,1.,1.,1.,1.,1.,1.,1.,1.,1.,1.,1.,1.,1.,1.,1.,1.,
1.,1.,1.,1.,1.,1.,1.,1.,1.,1.,1.,1.,1.,1.,1.,1.,1.,1.,1.,1.,1.,1.,1.,1.,
1.,1.,1.,1.,1.,1.,1.,1.,1.,1.,1.,1.,1.,1.,1.,1.,1.,1.,1.,1.,1.,1.,1.,1.,
1.,1.,1.,1.,1.,1.,1.,1.,1.,1.,1.,1.,1.,1.,1.,1.,1.,1.,1.,1.,1.,1.,1.,1.,
1.,1.,1.,1.,1.,1.,1.,1.,1.,1.,1.,1.,1.,1.,1.,1.,1.,1.,1.,1.,1.))
REPRESENTATION_ITEM('')
);
#721=(
BOUNDED_CURVE()
B_SPLINE_CURVE(5,(#181373,#181374,#181375,#181376,#181377,#181378,#181379,
#181380,#181381,#181382,#181383,#181384,#181385,#181386,#181387,#181388,
#181389,#181390,#181391,#181392,#181393,#181394,#181395,#181396,#181397,
#181398,#181399,#181400,#181401,#181402,#181403,#181404,#181405,#181406,
#181407,#181408,#181409,#181410,#181411,#181412,#181413,#181414,#181415,
#181416,#181417,#181418,#181419,#181420,#181421,#181422,#181423,#181424,
#181425,#181426,#181427,#181428,#181429,#181430,#181431,#181432,#181433,
#181434,#181435,#181436,#181437,#181438,#181439,#181440,#181441,#181442,
#181443,#181444,#181445,#181446,#181447,#181448,#181449,#181450,#181451,
#181452,#181453,#181454,#181455,#181456,#181457,#181458,#181459,#181460,
#181461,#181462,#181463,#181464,#181465,#181466,#181467,#181468,#181469,
#181470,#181471,#181472,#181473,#181474,#181475,#181476,#181477,#181478,
#181479,#181480,#181481,#181482,#181483,#181484,#181485,#181486,#181487,
#181488,#181489,#181490,#181491,#181492,#181493,#181494,#181495,#181496,
#181497,#181498,#181499,#181500,#181501,#181502,#181503,#181504,#181505,
#181506,#181507,#181508,#181509,#181510,#181511,#181512,#181513,#181514,
#181515,#181516,#181517,#181518,#181519,#181520,#181521,#181522,#181523,
#181524,#181525,#181526,#181527,#181528,#181529,#181530,#181531,#181532,
#181533,#181534,#181535,#181536,#181537,#181538,#181539,#181540,#181541,
#181542,#181543,#181544,#181545,#181546,#181547,#181548,#181549,#181550,
#181551,#181552,#181553,#181554,#181555,#181556,#181557,#181558,#181559,
#181560,#181561,#181562,#181563,#181564,#181565,#181566,#181567,#181568,
#181569,#181570,#181571,#181572,#181573,#181574,#181575,#181576,#181577),
 .UNSPECIFIED.,.F.,.F.)
B_SPLINE_CURVE_WITH_KNOTS((6,1,1,1,1,1,1,1,1,1,1,1,1,1,1,1,1,1,1,1,1,1,
1,1,1,1,1,1,1,1,1,1,1,1,1,1,1,1,1,1,1,1,1,1,1,1,1,1,1,1,1,1,1,1,1,1,1,1,
1,1,1,1,1,1,1,1,1,1,1,1,1,1,1,1,1,1,1,1,1,1,1,1,1,1,1,1,1,1,1,1,1,1,1,1,
1,1,1,1,1,1,1,1,1,1,1,1,1,1,1,1,1,1,1,1,1,1,1,1,1,1,1,1,1,1,1,1,1,1,1,1,
1,1,1,1,1,1,1,1,1,1,1,1,1,1,1,1,1,1,1,1,1,1,1,1,1,1,1,1,1,1,1,1,1,1,1,1,
1,1,1,1,1,1,1,1,1,1,1,1,1,1,1,1,1,1,1,1,1,1,1,1,1,1,1,1,1,1,1,1,1,1,6),
(0.,0.005,0.01,0.015,0.02,0.025,0.03,0.035,0.04,0.045,0.05,0.055,0.06,0.065,
0.07,0.075,0.08,0.085,0.09,0.095,0.1,0.105,0.11,0.115,0.12,0.125,0.13,0.135,
0.14,0.145,0.15,0.155,0.16,0.165,0.17,0.175,0.18,0.185,0.19,0.195,0.2,0.205,
0.21,0.215,0.22,0.225,0.23,0.235,0.24,0.245,0.25,0.255,0.26,0.265,0.27,
0.275,0.28,0.285,0.29,0.295,0.3,0.305,0.31,0.315,0.32,0.325,0.33,0.335,
0.34,0.345,0.35,0.355,0.36,0.365,0.37,0.375,0.38,0.385,0.39,0.395,0.4,0.405,
0.41,0.415,0.42,0.425,0.43,0.435,0.44,0.445,0.45,0.455,0.46,0.465,0.47,
0.475,0.48,0.485,0.49,0.495,0.5,0.505,0.51,0.515,0.52,0.525,0.53,0.535,
0.54,0.545,0.55,0.555,0.56,0.565,0.57,0.575,0.58,0.585,0.59,0.595,0.6,0.605,
0.61,0.615,0.62,0.625,0.63,0.635,0.64,0.645,0.65,0.655,0.66,0.665,0.67,
0.675,0.68,0.685,0.690000000000001,0.695000000000001,0.700000000000001,
0.705000000000001,0.710000000000001,0.715000000000001,0.720000000000001,
0.725000000000001,0.730000000000001,0.735000000000001,0.740000000000001,
0.745000000000001,0.750000000000001,0.755000000000001,0.760000000000001,
0.765000000000001,0.770000000000001,0.775000000000001,0.780000000000001,
0.785000000000001,0.790000000000001,0.795000000000001,0.800000000000001,
0.805000000000001,0.810000000000001,0.815000000000001,0.820000000000001,
0.825000000000001,0.830000000000001,0.835000000000001,0.840000000000001,
0.845000000000001,0.850000000000001,0.855000000000001,0.860000000000001,
0.865000000000001,0.870000000000001,0.875000000000001,0.880000000000001,
0.885000000000001,0.890000000000001,0.895000000000001,0.900000000000001,
0.905000000000001,0.910000000000001,0.915000000000001,0.920000000000001,
0.925000000000001,0.930000000000001,0.935000000000001,0.940000000000001,
0.945000000000001,0.950000000000001,0.955000000000001,0.960000000000001,
0.965000000000001,0.970000000000001,0.975000000000001,0.980000000000001,
0.985000000000001,0.990000000000001,0.995000000000001,1.),.UNSPECIFIED.)
CURVE()
GEOMETRIC_REPRESENTATION_ITEM()
RATIONAL_B_SPLINE_CURVE((1.,1.,1.,1.,1.,1.,1.,1.,1.,1.,1.,1.,1.,1.,1.,1.,
1.,1.,1.,1.,1.,1.,1.,1.,1.,1.,1.,1.,1.,1.,1.,1.,1.,1.,1.,1.,1.,1.,1.,1.,
1.,1.,1.,1.,1.,1.,1.,1.,1.,1.,1.,1.,1.,1.,1.,1.,1.,1.,1.,1.,1.,1.,1.,1.,
1.,1.,1.,1.,1.,1.,1.,1.,1.,1.,1.,1.,1.,1.,1.,1.,1.,1.,1.,1.,1.,1.,1.,1.,
1.,1.,1.,1.,1.,1.,1.,1.,1.,1.,1.,1.,1.,1.,1.,1.,1.,1.,1.,1.,1.,1.,1.,1.,
1.,1.,1.,1.,1.,1.,1.,1.,1.,1.,1.,1.,1.,1.,1.,1.,1.,1.,1.,1.,1.,1.,1.,1.,
1.,1.,1.,1.,1.,1.,1.,1.,1.,1.,1.,1.,1.,1.,1.,1.,1.,1.,1.,1.,1.,1.,1.,1.,
1.,1.,1.,1.,1.,1.,1.,1.,1.,1.,1.,1.,1.,1.,1.,1.,1.,1.,1.,1.,1.,1.,1.,1.,
1.,1.,1.,1.,1.,1.,1.,1.,1.,1.,1.,1.,1.,1.,1.,1.,1.,1.,1.,1.,1.))
REPRESENTATION_ITEM('')
);
#722=(
BOUNDED_CURVE()
B_SPLINE_CURVE(5,(#181581,#181582,#181583,#181584,#181585,#181586,#181587,
#181588,#181589,#181590,#181591,#181592,#181593,#181594,#181595,#181596,
#181597,#181598,#181599,#181600,#181601,#181602,#181603,#181604,#181605,
#181606,#181607,#181608,#181609,#181610,#181611,#181612,#181613,#181614,
#181615,#181616,#181617,#181618,#181619,#181620,#181621,#181622,#181623,
#181624,#181625,#181626,#181627,#181628,#181629,#181630,#181631,#181632,
#181633,#181634,#181635,#181636,#181637,#181638,#181639,#181640,#181641,
#181642,#181643,#181644,#181645,#181646,#181647,#181648,#181649,#181650,
#181651,#181652,#181653,#181654,#181655,#181656,#181657,#181658,#181659,
#181660,#181661,#181662,#181663,#181664,#181665,#181666,#181667,#181668,
#181669,#181670,#181671,#181672,#181673,#181674,#181675,#181676,#181677,
#181678,#181679,#181680,#181681,#181682,#181683,#181684,#181685,#181686,
#181687,#181688,#181689,#181690,#181691,#181692,#181693,#181694,#181695,
#181696,#181697,#181698,#181699,#181700,#181701,#181702,#181703,#181704,
#181705,#181706,#181707,#181708,#181709,#181710,#181711,#181712,#181713,
#181714,#181715,#181716,#181717,#181718,#181719,#181720,#181721,#181722,
#181723,#181724,#181725,#181726,#181727,#181728,#181729,#181730,#181731,
#181732,#181733,#181734,#181735,#181736,#181737,#181738,#181739,#181740,
#181741,#181742,#181743,#181744,#181745,#181746,#181747,#181748,#181749,
#181750,#181751,#181752,#181753,#181754,#181755,#181756,#181757,#181758,
#181759,#181760,#181761,#181762,#181763,#181764,#181765,#181766,#181767,
#181768,#181769,#181770,#181771,#181772,#181773,#181774,#181775,#181776,
#181777,#181778,#181779,#181780,#181781,#181782,#181783,#181784,#181785),
 .UNSPECIFIED.,.F.,.F.)
B_SPLINE_CURVE_WITH_KNOTS((6,1,1,1,1,1,1,1,1,1,1,1,1,1,1,1,1,1,1,1,1,1,
1,1,1,1,1,1,1,1,1,1,1,1,1,1,1,1,1,1,1,1,1,1,1,1,1,1,1,1,1,1,1,1,1,1,1,1,
1,1,1,1,1,1,1,1,1,1,1,1,1,1,1,1,1,1,1,1,1,1,1,1,1,1,1,1,1,1,1,1,1,1,1,1,
1,1,1,1,1,1,1,1,1,1,1,1,1,1,1,1,1,1,1,1,1,1,1,1,1,1,1,1,1,1,1,1,1,1,1,1,
1,1,1,1,1,1,1,1,1,1,1,1,1,1,1,1,1,1,1,1,1,1,1,1,1,1,1,1,1,1,1,1,1,1,1,1,
1,1,1,1,1,1,1,1,1,1,1,1,1,1,1,1,1,1,1,1,1,1,1,1,1,1,1,1,1,1,1,1,1,1,6),
(-1.,-0.995000000000001,-0.990000000000001,-0.985000000000001,-0.980000000000001,
-0.975000000000001,-0.970000000000001,-0.965000000000001,-0.960000000000001,
-0.955000000000001,-0.950000000000001,-0.945000000000001,-0.940000000000001,
-0.935000000000001,-0.930000000000001,-0.925000000000001,-0.920000000000001,
-0.915000000000001,-0.910000000000001,-0.905000000000001,-0.900000000000001,
-0.895000000000001,-0.890000000000001,-0.885000000000001,-0.880000000000001,
-0.875000000000001,-0.870000000000001,-0.865000000000001,-0.860000000000001,
-0.855000000000001,-0.850000000000001,-0.845000000000001,-0.840000000000001,
-0.835000000000001,-0.830000000000001,-0.825000000000001,-0.820000000000001,
-0.815000000000001,-0.810000000000001,-0.805000000000001,-0.800000000000001,
-0.795000000000001,-0.790000000000001,-0.785000000000001,-0.780000000000001,
-0.775000000000001,-0.770000000000001,-0.765000000000001,-0.760000000000001,
-0.755000000000001,-0.750000000000001,-0.745000000000001,-0.740000000000001,
-0.735000000000001,-0.730000000000001,-0.725000000000001,-0.720000000000001,
-0.715000000000001,-0.710000000000001,-0.705000000000001,-0.700000000000001,
-0.695000000000001,-0.690000000000001,-0.685,-0.68,-0.675,-0.67,-0.665,
-0.66,-0.655,-0.65,-0.645,-0.64,-0.635,-0.63,-0.625,-0.62,-0.615,-0.61,
-0.605,-0.6,-0.595,-0.59,-0.585,-0.58,-0.575,-0.57,-0.565,-0.56,-0.555,
-0.55,-0.545,-0.54,-0.535,-0.53,-0.525,-0.52,-0.515,-0.51,-0.505,-0.5,-0.495,
-0.49,-0.485,-0.48,-0.475,-0.47,-0.465,-0.46,-0.455,-0.45,-0.445,-0.44,
-0.435,-0.43,-0.425,-0.42,-0.415,-0.41,-0.405,-0.4,-0.395,-0.39,-0.385,
-0.38,-0.375,-0.37,-0.365,-0.36,-0.355,-0.35,-0.345,-0.34,-0.335,-0.33,
-0.325,-0.32,-0.315,-0.31,-0.305,-0.3,-0.295,-0.29,-0.285,-0.28,-0.275,
-0.27,-0.265,-0.26,-0.255,-0.25,-0.245,-0.24,-0.235,-0.23,-0.225,-0.22,
-0.215,-0.21,-0.205,-0.2,-0.195,-0.19,-0.185,-0.18,-0.175,-0.17,-0.165,
-0.16,-0.155,-0.15,-0.145,-0.14,-0.135,-0.13,-0.125,-0.12,-0.115,-0.11,
-0.105,-0.1,-0.095,-0.09,-0.085,-0.08,-0.075,-0.07,-0.065,-0.06,-0.055,
-0.05,-0.045,-0.04,-0.035,-0.03,-0.025,-0.02,-0.015,-0.01,-0.005,0.),
 .UNSPECIFIED.)
CURVE()
GEOMETRIC_REPRESENTATION_ITEM()
RATIONAL_B_SPLINE_CURVE((1.,1.,1.,1.,1.,1.,1.,1.,1.,1.,1.,1.,1.,1.,1.,1.,
1.,1.,1.,1.,1.,1.,1.,1.,1.,1.,1.,1.,1.,1.,1.,1.,1.,1.,1.,1.,1.,1.,1.,1.,
1.,1.,1.,1.,1.,1.,1.,1.,1.,1.,1.,1.,1.,1.,1.,1.,1.,1.,1.,1.,1.,1.,1.,1.,
1.,1.,1.,1.,1.,1.,1.,1.,1.,1.,1.,1.,1.,1.,1.,1.,1.,1.,1.,1.,1.,1.,1.,1.,
1.,1.,1.,1.,1.,1.,1.,1.,1.,1.,1.,1.,1.,1.,1.,1.,1.,1.,1.,1.,1.,1.,1.,1.,
1.,1.,1.,1.,1.,1.,1.,1.,1.,1.,1.,1.,1.,1.,1.,1.,1.,1.,1.,1.,1.,1.,1.,1.,
1.,1.,1.,1.,1.,1.,1.,1.,1.,1.,1.,1.,1.,1.,1.,1.,1.,1.,1.,1.,1.,1.,1.,1.,
1.,1.,1.,1.,1.,1.,1.,1.,1.,1.,1.,1.,1.,1.,1.,1.,1.,1.,1.,1.,1.,1.,1.,1.,
1.,1.,1.,1.,1.,1.,1.,1.,1.,1.,1.,1.,1.,1.,1.,1.,1.,1.,1.,1.,1.))
REPRESENTATION_ITEM('')
);
#723=(
BOUNDED_CURVE()
B_SPLINE_CURVE(5,(#181797,#181798,#181799,#181800,#181801,#181802,#181803,
#181804,#181805,#181806,#181807,#181808,#181809,#181810,#181811,#181812,
#181813,#181814,#181815,#181816,#181817,#181818,#181819,#181820,#181821,
#181822,#181823,#181824,#181825,#181826,#181827,#181828,#181829,#181830,
#181831,#181832,#181833,#181834,#181835,#181836,#181837,#181838,#181839,
#181840,#181841,#181842,#181843,#181844,#181845,#181846,#181847,#181848,
#181849,#181850,#181851,#181852,#181853,#181854,#181855,#181856,#181857,
#181858,#181859,#181860,#181861,#181862,#181863,#181864,#181865,#181866,
#181867,#181868,#181869,#181870,#181871,#181872,#181873,#181874,#181875,
#181876,#181877,#181878,#181879,#181880,#181881,#181882,#181883,#181884,
#181885,#181886,#181887,#181888,#181889,#181890,#181891,#181892,#181893,
#181894,#181895,#181896,#181897,#181898,#181899,#181900,#181901,#181902,
#181903,#181904,#181905,#181906,#181907,#181908,#181909,#181910,#181911,
#181912,#181913,#181914,#181915,#181916,#181917,#181918,#181919,#181920,
#181921,#181922,#181923,#181924,#181925,#181926,#181927,#181928,#181929,
#181930,#181931,#181932,#181933,#181934,#181935,#181936,#181937,#181938,
#181939,#181940,#181941,#181942,#181943,#181944,#181945,#181946,#181947,
#181948,#181949,#181950,#181951,#181952,#181953,#181954,#181955,#181956,
#181957,#181958,#181959,#181960,#181961,#181962,#181963,#181964,#181965,
#181966,#181967,#181968,#181969,#181970,#181971,#181972,#181973,#181974,
#181975,#181976,#181977,#181978,#181979,#181980,#181981,#181982,#181983,
#181984,#181985,#181986,#181987,#181988,#181989,#181990,#181991,#181992,
#181993,#181994,#181995,#181996,#181997,#181998,#181999,#182000,#182001),
 .UNSPECIFIED.,.F.,.F.)
B_SPLINE_CURVE_WITH_KNOTS((6,1,1,1,1,1,1,1,1,1,1,1,1,1,1,1,1,1,1,1,1,1,
1,1,1,1,1,1,1,1,1,1,1,1,1,1,1,1,1,1,1,1,1,1,1,1,1,1,1,1,1,1,1,1,1,1,1,1,
1,1,1,1,1,1,1,1,1,1,1,1,1,1,1,1,1,1,1,1,1,1,1,1,1,1,1,1,1,1,1,1,1,1,1,1,
1,1,1,1,1,1,1,1,1,1,1,1,1,1,1,1,1,1,1,1,1,1,1,1,1,1,1,1,1,1,1,1,1,1,1,1,
1,1,1,1,1,1,1,1,1,1,1,1,1,1,1,1,1,1,1,1,1,1,1,1,1,1,1,1,1,1,1,1,1,1,1,1,
1,1,1,1,1,1,1,1,1,1,1,1,1,1,1,1,1,1,1,1,1,1,1,1,1,1,1,1,1,1,1,1,1,1,6),
(0.,0.005,0.01,0.015,0.02,0.025,0.03,0.035,0.04,0.045,0.05,0.055,0.06,0.065,
0.07,0.075,0.08,0.085,0.09,0.095,0.1,0.105,0.11,0.115,0.12,0.125,0.13,0.135,
0.14,0.145,0.15,0.155,0.16,0.165,0.17,0.175,0.18,0.185,0.19,0.195,0.2,0.205,
0.21,0.215,0.22,0.225,0.23,0.235,0.24,0.245,0.25,0.255,0.26,0.265,0.27,
0.275,0.28,0.285,0.29,0.295,0.3,0.305,0.31,0.315,0.32,0.325,0.33,0.335,
0.34,0.345,0.35,0.355,0.36,0.365,0.37,0.375,0.38,0.385,0.39,0.395,0.4,0.405,
0.41,0.415,0.42,0.425,0.43,0.435,0.44,0.445,0.45,0.455,0.46,0.465,0.47,
0.475,0.48,0.485,0.49,0.495,0.5,0.505,0.51,0.515,0.52,0.525,0.53,0.535,
0.54,0.545,0.55,0.555,0.56,0.565,0.57,0.575,0.58,0.585,0.59,0.595,0.6,0.605,
0.61,0.615,0.62,0.625,0.63,0.635,0.64,0.645,0.65,0.655,0.66,0.665,0.67,
0.675,0.68,0.685,0.690000000000001,0.695000000000001,0.700000000000001,
0.705000000000001,0.710000000000001,0.715000000000001,0.720000000000001,
0.725000000000001,0.730000000000001,0.735000000000001,0.740000000000001,
0.745000000000001,0.750000000000001,0.755000000000001,0.760000000000001,
0.765000000000001,0.770000000000001,0.775000000000001,0.780000000000001,
0.785000000000001,0.790000000000001,0.795000000000001,0.800000000000001,
0.805000000000001,0.810000000000001,0.815000000000001,0.820000000000001,
0.825000000000001,0.830000000000001,0.835000000000001,0.840000000000001,
0.845000000000001,0.850000000000001,0.855000000000001,0.860000000000001,
0.865000000000001,0.870000000000001,0.875000000000001,0.880000000000001,
0.885000000000001,0.890000000000001,0.895000000000001,0.900000000000001,
0.905000000000001,0.910000000000001,0.915000000000001,0.920000000000001,
0.925000000000001,0.930000000000001,0.935000000000001,0.940000000000001,
0.945000000000001,0.950000000000001,0.955000000000001,0.960000000000001,
0.965000000000001,0.970000000000001,0.975000000000001,0.980000000000001,
0.985000000000001,0.990000000000001,0.995000000000001,1.),.UNSPECIFIED.)
CURVE()
GEOMETRIC_REPRESENTATION_ITEM()
RATIONAL_B_SPLINE_CURVE((1.,1.,1.,1.,1.,1.,1.,1.,1.,1.,1.,1.,1.,1.,1.,1.,
1.,1.,1.,1.,1.,1.,1.,1.,1.,1.,1.,1.,1.,1.,1.,1.,1.,1.,1.,1.,1.,1.,1.,1.,
1.,1.,1.,1.,1.,1.,1.,1.,1.,1.,1.,1.,1.,1.,1.,1.,1.,1.,1.,1.,1.,1.,1.,1.,
1.,1.,1.,1.,1.,1.,1.,1.,1.,1.,1.,1.,1.,1.,1.,1.,1.,1.,1.,1.,1.,1.,1.,1.,
1.,1.,1.,1.,1.,1.,1.,1.,1.,1.,1.,1.,1.,1.,1.,1.,1.,1.,1.,1.,1.,1.,1.,1.,
1.,1.,1.,1.,1.,1.,1.,1.,1.,1.,1.,1.,1.,1.,1.,1.,1.,1.,1.,1.,1.,1.,1.,1.,
1.,1.,1.,1.,1.,1.,1.,1.,1.,1.,1.,1.,1.,1.,1.,1.,1.,1.,1.,1.,1.,1.,1.,1.,
1.,1.,1.,1.,1.,1.,1.,1.,1.,1.,1.,1.,1.,1.,1.,1.,1.,1.,1.,1.,1.,1.,1.,1.,
1.,1.,1.,1.,1.,1.,1.,1.,1.,1.,1.,1.,1.,1.,1.,1.,1.,1.,1.,1.,1.))
REPRESENTATION_ITEM('')
);
#724=(
BOUNDED_CURVE()
B_SPLINE_CURVE(5,(#182005,#182006,#182007,#182008,#182009,#182010,#182011,
#182012,#182013,#182014,#182015,#182016,#182017,#182018,#182019,#182020,
#182021,#182022,#182023,#182024,#182025,#182026,#182027,#182028,#182029,
#182030,#182031,#182032,#182033,#182034,#182035,#182036,#182037,#182038,
#182039,#182040,#182041,#182042,#182043,#182044,#182045,#182046,#182047,
#182048,#182049,#182050,#182051,#182052,#182053,#182054,#182055,#182056,
#182057,#182058,#182059,#182060,#182061,#182062,#182063,#182064,#182065,
#182066,#182067,#182068,#182069,#182070,#182071,#182072,#182073,#182074,
#182075,#182076,#182077,#182078,#182079,#182080,#182081,#182082,#182083,
#182084,#182085,#182086,#182087,#182088,#182089,#182090,#182091,#182092,
#182093,#182094,#182095,#182096,#182097,#182098,#182099,#182100,#182101,
#182102,#182103,#182104,#182105,#182106,#182107,#182108,#182109,#182110,
#182111,#182112,#182113,#182114,#182115,#182116,#182117,#182118,#182119,
#182120,#182121,#182122,#182123,#182124,#182125,#182126,#182127,#182128,
#182129,#182130,#182131,#182132,#182133,#182134,#182135,#182136,#182137,
#182138,#182139,#182140,#182141,#182142,#182143,#182144,#182145,#182146,
#182147,#182148,#182149,#182150,#182151,#182152,#182153,#182154,#182155,
#182156,#182157,#182158,#182159,#182160,#182161,#182162,#182163,#182164,
#182165,#182166,#182167,#182168,#182169,#182170,#182171,#182172,#182173,
#182174,#182175,#182176,#182177,#182178,#182179,#182180,#182181,#182182,
#182183,#182184,#182185,#182186,#182187,#182188,#182189,#182190,#182191,
#182192,#182193,#182194,#182195,#182196,#182197,#182198,#182199,#182200,
#182201,#182202,#182203,#182204,#182205,#182206,#182207,#182208,#182209),
 .UNSPECIFIED.,.F.,.F.)
B_SPLINE_CURVE_WITH_KNOTS((6,1,1,1,1,1,1,1,1,1,1,1,1,1,1,1,1,1,1,1,1,1,
1,1,1,1,1,1,1,1,1,1,1,1,1,1,1,1,1,1,1,1,1,1,1,1,1,1,1,1,1,1,1,1,1,1,1,1,
1,1,1,1,1,1,1,1,1,1,1,1,1,1,1,1,1,1,1,1,1,1,1,1,1,1,1,1,1,1,1,1,1,1,1,1,
1,1,1,1,1,1,1,1,1,1,1,1,1,1,1,1,1,1,1,1,1,1,1,1,1,1,1,1,1,1,1,1,1,1,1,1,
1,1,1,1,1,1,1,1,1,1,1,1,1,1,1,1,1,1,1,1,1,1,1,1,1,1,1,1,1,1,1,1,1,1,1,1,
1,1,1,1,1,1,1,1,1,1,1,1,1,1,1,1,1,1,1,1,1,1,1,1,1,1,1,1,1,1,1,1,1,1,6),
(-1.,-0.995000000000001,-0.990000000000001,-0.985000000000001,-0.980000000000001,
-0.975000000000001,-0.970000000000001,-0.965000000000001,-0.960000000000001,
-0.955000000000001,-0.950000000000001,-0.945000000000001,-0.940000000000001,
-0.935000000000001,-0.930000000000001,-0.925000000000001,-0.920000000000001,
-0.915000000000001,-0.910000000000001,-0.905000000000001,-0.900000000000001,
-0.895000000000001,-0.890000000000001,-0.885000000000001,-0.880000000000001,
-0.875000000000001,-0.870000000000001,-0.865000000000001,-0.860000000000001,
-0.855000000000001,-0.850000000000001,-0.845000000000001,-0.840000000000001,
-0.835000000000001,-0.830000000000001,-0.825000000000001,-0.820000000000001,
-0.815000000000001,-0.810000000000001,-0.805000000000001,-0.800000000000001,
-0.795000000000001,-0.790000000000001,-0.785000000000001,-0.780000000000001,
-0.775000000000001,-0.770000000000001,-0.765000000000001,-0.760000000000001,
-0.755000000000001,-0.750000000000001,-0.745000000000001,-0.740000000000001,
-0.735000000000001,-0.730000000000001,-0.725000000000001,-0.720000000000001,
-0.715000000000001,-0.710000000000001,-0.705000000000001,-0.700000000000001,
-0.695000000000001,-0.690000000000001,-0.685,-0.68,-0.675,-0.67,-0.665,
-0.66,-0.655,-0.65,-0.645,-0.64,-0.635,-0.63,-0.625,-0.62,-0.615,-0.61,
-0.605,-0.6,-0.595,-0.59,-0.585,-0.58,-0.575,-0.57,-0.565,-0.56,-0.555,
-0.55,-0.545,-0.54,-0.535,-0.53,-0.525,-0.52,-0.515,-0.51,-0.505,-0.5,-0.495,
-0.49,-0.485,-0.48,-0.475,-0.47,-0.465,-0.46,-0.455,-0.45,-0.445,-0.44,
-0.435,-0.43,-0.425,-0.42,-0.415,-0.41,-0.405,-0.4,-0.395,-0.39,-0.385,
-0.38,-0.375,-0.37,-0.365,-0.36,-0.355,-0.35,-0.345,-0.34,-0.335,-0.33,
-0.325,-0.32,-0.315,-0.31,-0.305,-0.3,-0.295,-0.29,-0.285,-0.28,-0.275,
-0.27,-0.265,-0.26,-0.255,-0.25,-0.245,-0.24,-0.235,-0.23,-0.225,-0.22,
-0.215,-0.21,-0.205,-0.2,-0.195,-0.19,-0.185,-0.18,-0.175,-0.17,-0.165,
-0.16,-0.155,-0.15,-0.145,-0.14,-0.135,-0.13,-0.125,-0.12,-0.115,-0.11,
-0.105,-0.1,-0.095,-0.09,-0.085,-0.08,-0.075,-0.07,-0.065,-0.06,-0.055,
-0.05,-0.045,-0.04,-0.035,-0.03,-0.025,-0.02,-0.015,-0.01,-0.005,0.),
 .UNSPECIFIED.)
CURVE()
GEOMETRIC_REPRESENTATION_ITEM()
RATIONAL_B_SPLINE_CURVE((1.,1.,1.,1.,1.,1.,1.,1.,1.,1.,1.,1.,1.,1.,1.,1.,
1.,1.,1.,1.,1.,1.,1.,1.,1.,1.,1.,1.,1.,1.,1.,1.,1.,1.,1.,1.,1.,1.,1.,1.,
1.,1.,1.,1.,1.,1.,1.,1.,1.,1.,1.,1.,1.,1.,1.,1.,1.,1.,1.,1.,1.,1.,1.,1.,
1.,1.,1.,1.,1.,1.,1.,1.,1.,1.,1.,1.,1.,1.,1.,1.,1.,1.,1.,1.,1.,1.,1.,1.,
1.,1.,1.,1.,1.,1.,1.,1.,1.,1.,1.,1.,1.,1.,1.,1.,1.,1.,1.,1.,1.,1.,1.,1.,
1.,1.,1.,1.,1.,1.,1.,1.,1.,1.,1.,1.,1.,1.,1.,1.,1.,1.,1.,1.,1.,1.,1.,1.,
1.,1.,1.,1.,1.,1.,1.,1.,1.,1.,1.,1.,1.,1.,1.,1.,1.,1.,1.,1.,1.,1.,1.,1.,
1.,1.,1.,1.,1.,1.,1.,1.,1.,1.,1.,1.,1.,1.,1.,1.,1.,1.,1.,1.,1.,1.,1.,1.,
1.,1.,1.,1.,1.,1.,1.,1.,1.,1.,1.,1.,1.,1.,1.,1.,1.,1.,1.,1.,1.))
REPRESENTATION_ITEM('')
);
#725=(
BOUNDED_CURVE()
B_SPLINE_CURVE(5,(#182221,#182222,#182223,#182224,#182225,#182226,#182227,
#182228,#182229,#182230,#182231,#182232,#182233,#182234,#182235,#182236,
#182237,#182238,#182239,#182240,#182241,#182242,#182243,#182244,#182245,
#182246,#182247,#182248,#182249,#182250,#182251,#182252,#182253,#182254,
#182255,#182256,#182257,#182258,#182259,#182260,#182261,#182262,#182263,
#182264,#182265,#182266,#182267,#182268,#182269,#182270,#182271,#182272,
#182273,#182274,#182275,#182276,#182277,#182278,#182279,#182280,#182281,
#182282,#182283,#182284,#182285,#182286,#182287,#182288,#182289,#182290,
#182291,#182292,#182293,#182294,#182295,#182296,#182297,#182298,#182299,
#182300,#182301,#182302,#182303,#182304,#182305,#182306,#182307,#182308,
#182309,#182310,#182311,#182312,#182313,#182314,#182315,#182316,#182317,
#182318,#182319,#182320,#182321,#182322,#182323,#182324,#182325,#182326,
#182327,#182328,#182329,#182330,#182331,#182332,#182333,#182334,#182335,
#182336,#182337,#182338,#182339,#182340,#182341,#182342,#182343,#182344,
#182345,#182346,#182347,#182348,#182349,#182350,#182351,#182352,#182353,
#182354,#182355,#182356,#182357,#182358,#182359,#182360,#182361,#182362,
#182363,#182364,#182365,#182366,#182367,#182368,#182369,#182370,#182371,
#182372,#182373,#182374,#182375,#182376,#182377,#182378,#182379,#182380,
#182381,#182382,#182383,#182384,#182385,#182386,#182387,#182388,#182389,
#182390,#182391,#182392,#182393,#182394,#182395,#182396,#182397,#182398,
#182399,#182400,#182401,#182402,#182403,#182404,#182405,#182406,#182407,
#182408,#182409,#182410,#182411,#182412,#182413,#182414,#182415,#182416,
#182417,#182418,#182419,#182420,#182421,#182422,#182423,#182424,#182425),
 .UNSPECIFIED.,.F.,.F.)
B_SPLINE_CURVE_WITH_KNOTS((6,1,1,1,1,1,1,1,1,1,1,1,1,1,1,1,1,1,1,1,1,1,
1,1,1,1,1,1,1,1,1,1,1,1,1,1,1,1,1,1,1,1,1,1,1,1,1,1,1,1,1,1,1,1,1,1,1,1,
1,1,1,1,1,1,1,1,1,1,1,1,1,1,1,1,1,1,1,1,1,1,1,1,1,1,1,1,1,1,1,1,1,1,1,1,
1,1,1,1,1,1,1,1,1,1,1,1,1,1,1,1,1,1,1,1,1,1,1,1,1,1,1,1,1,1,1,1,1,1,1,1,
1,1,1,1,1,1,1,1,1,1,1,1,1,1,1,1,1,1,1,1,1,1,1,1,1,1,1,1,1,1,1,1,1,1,1,1,
1,1,1,1,1,1,1,1,1,1,1,1,1,1,1,1,1,1,1,1,1,1,1,1,1,1,1,1,1,1,1,1,1,1,6),
(0.,0.005,0.01,0.015,0.02,0.025,0.03,0.035,0.04,0.045,0.05,0.055,0.06,0.065,
0.07,0.075,0.08,0.085,0.09,0.095,0.1,0.105,0.11,0.115,0.12,0.125,0.13,0.135,
0.14,0.145,0.15,0.155,0.16,0.165,0.17,0.175,0.18,0.185,0.19,0.195,0.2,0.205,
0.21,0.215,0.22,0.225,0.23,0.235,0.24,0.245,0.25,0.255,0.26,0.265,0.27,
0.275,0.28,0.285,0.29,0.295,0.3,0.305,0.31,0.315,0.32,0.325,0.33,0.335,
0.34,0.345,0.35,0.355,0.36,0.365,0.37,0.375,0.38,0.385,0.39,0.395,0.4,0.405,
0.41,0.415,0.42,0.425,0.43,0.435,0.44,0.445,0.45,0.455,0.46,0.465,0.47,
0.475,0.48,0.485,0.49,0.495,0.5,0.505,0.51,0.515,0.52,0.525,0.53,0.535,
0.54,0.545,0.55,0.555,0.56,0.565,0.57,0.575,0.58,0.585,0.59,0.595,0.6,0.605,
0.61,0.615,0.62,0.625,0.63,0.635,0.64,0.645,0.65,0.655,0.66,0.665,0.67,
0.675,0.68,0.685,0.690000000000001,0.695000000000001,0.700000000000001,
0.705000000000001,0.710000000000001,0.715000000000001,0.720000000000001,
0.725000000000001,0.730000000000001,0.735000000000001,0.740000000000001,
0.745000000000001,0.750000000000001,0.755000000000001,0.760000000000001,
0.765000000000001,0.770000000000001,0.775000000000001,0.780000000000001,
0.785000000000001,0.790000000000001,0.795000000000001,0.800000000000001,
0.805000000000001,0.810000000000001,0.815000000000001,0.820000000000001,
0.825000000000001,0.830000000000001,0.835000000000001,0.840000000000001,
0.845000000000001,0.850000000000001,0.855000000000001,0.860000000000001,
0.865000000000001,0.870000000000001,0.875000000000001,0.880000000000001,
0.885000000000001,0.890000000000001,0.895000000000001,0.900000000000001,
0.905000000000001,0.910000000000001,0.915000000000001,0.920000000000001,
0.925000000000001,0.930000000000001,0.935000000000001,0.940000000000001,
0.945000000000001,0.950000000000001,0.955000000000001,0.960000000000001,
0.965000000000001,0.970000000000001,0.975000000000001,0.980000000000001,
0.985000000000001,0.990000000000001,0.995000000000001,1.),.UNSPECIFIED.)
CURVE()
GEOMETRIC_REPRESENTATION_ITEM()
RATIONAL_B_SPLINE_CURVE((1.,1.,1.,1.,1.,1.,1.,1.,1.,1.,1.,1.,1.,1.,1.,1.,
1.,1.,1.,1.,1.,1.,1.,1.,1.,1.,1.,1.,1.,1.,1.,1.,1.,1.,1.,1.,1.,1.,1.,1.,
1.,1.,1.,1.,1.,1.,1.,1.,1.,1.,1.,1.,1.,1.,1.,1.,1.,1.,1.,1.,1.,1.,1.,1.,
1.,1.,1.,1.,1.,1.,1.,1.,1.,1.,1.,1.,1.,1.,1.,1.,1.,1.,1.,1.,1.,1.,1.,1.,
1.,1.,1.,1.,1.,1.,1.,1.,1.,1.,1.,1.,1.,1.,1.,1.,1.,1.,1.,1.,1.,1.,1.,1.,
1.,1.,1.,1.,1.,1.,1.,1.,1.,1.,1.,1.,1.,1.,1.,1.,1.,1.,1.,1.,1.,1.,1.,1.,
1.,1.,1.,1.,1.,1.,1.,1.,1.,1.,1.,1.,1.,1.,1.,1.,1.,1.,1.,1.,1.,1.,1.,1.,
1.,1.,1.,1.,1.,1.,1.,1.,1.,1.,1.,1.,1.,1.,1.,1.,1.,1.,1.,1.,1.,1.,1.,1.,
1.,1.,1.,1.,1.,1.,1.,1.,1.,1.,1.,1.,1.,1.,1.,1.,1.,1.,1.,1.,1.))
REPRESENTATION_ITEM('')
);
#726=(
BOUNDED_CURVE()
B_SPLINE_CURVE(5,(#182429,#182430,#182431,#182432,#182433,#182434,#182435,
#182436,#182437,#182438,#182439,#182440,#182441,#182442,#182443,#182444,
#182445,#182446,#182447,#182448,#182449,#182450,#182451,#182452,#182453,
#182454,#182455,#182456,#182457,#182458,#182459,#182460,#182461,#182462,
#182463,#182464,#182465,#182466,#182467,#182468,#182469,#182470,#182471,
#182472,#182473,#182474,#182475,#182476,#182477,#182478,#182479,#182480,
#182481,#182482,#182483,#182484,#182485,#182486,#182487,#182488,#182489,
#182490,#182491,#182492,#182493,#182494,#182495,#182496,#182497,#182498,
#182499,#182500,#182501,#182502,#182503,#182504,#182505,#182506,#182507,
#182508,#182509,#182510,#182511,#182512,#182513,#182514,#182515,#182516,
#182517,#182518,#182519,#182520,#182521,#182522,#182523,#182524,#182525,
#182526,#182527,#182528,#182529,#182530,#182531,#182532,#182533,#182534,
#182535,#182536,#182537,#182538,#182539,#182540,#182541,#182542,#182543,
#182544,#182545,#182546,#182547,#182548,#182549,#182550,#182551,#182552,
#182553,#182554,#182555,#182556,#182557,#182558,#182559,#182560,#182561,
#182562,#182563,#182564,#182565,#182566,#182567,#182568,#182569,#182570,
#182571,#182572,#182573,#182574,#182575,#182576,#182577,#182578,#182579,
#182580,#182581,#182582,#182583,#182584,#182585,#182586,#182587,#182588,
#182589,#182590,#182591,#182592,#182593,#182594,#182595,#182596,#182597,
#182598,#182599,#182600,#182601,#182602,#182603,#182604,#182605,#182606,
#182607,#182608,#182609,#182610,#182611,#182612,#182613,#182614,#182615,
#182616,#182617,#182618,#182619,#182620,#182621,#182622,#182623,#182624,
#182625,#182626,#182627,#182628,#182629,#182630,#182631,#182632,#182633),
 .UNSPECIFIED.,.F.,.F.)
B_SPLINE_CURVE_WITH_KNOTS((6,1,1,1,1,1,1,1,1,1,1,1,1,1,1,1,1,1,1,1,1,1,
1,1,1,1,1,1,1,1,1,1,1,1,1,1,1,1,1,1,1,1,1,1,1,1,1,1,1,1,1,1,1,1,1,1,1,1,
1,1,1,1,1,1,1,1,1,1,1,1,1,1,1,1,1,1,1,1,1,1,1,1,1,1,1,1,1,1,1,1,1,1,1,1,
1,1,1,1,1,1,1,1,1,1,1,1,1,1,1,1,1,1,1,1,1,1,1,1,1,1,1,1,1,1,1,1,1,1,1,1,
1,1,1,1,1,1,1,1,1,1,1,1,1,1,1,1,1,1,1,1,1,1,1,1,1,1,1,1,1,1,1,1,1,1,1,1,
1,1,1,1,1,1,1,1,1,1,1,1,1,1,1,1,1,1,1,1,1,1,1,1,1,1,1,1,1,1,1,1,1,1,6),
(-1.,-0.995000000000001,-0.990000000000001,-0.985000000000001,-0.980000000000001,
-0.975000000000001,-0.970000000000001,-0.965000000000001,-0.960000000000001,
-0.955000000000001,-0.950000000000001,-0.945000000000001,-0.940000000000001,
-0.935000000000001,-0.930000000000001,-0.925000000000001,-0.920000000000001,
-0.915000000000001,-0.910000000000001,-0.905000000000001,-0.900000000000001,
-0.895000000000001,-0.890000000000001,-0.885000000000001,-0.880000000000001,
-0.875000000000001,-0.870000000000001,-0.865000000000001,-0.860000000000001,
-0.855000000000001,-0.850000000000001,-0.845000000000001,-0.840000000000001,
-0.835000000000001,-0.830000000000001,-0.825000000000001,-0.820000000000001,
-0.815000000000001,-0.810000000000001,-0.805000000000001,-0.800000000000001,
-0.795000000000001,-0.790000000000001,-0.785000000000001,-0.780000000000001,
-0.775000000000001,-0.770000000000001,-0.765000000000001,-0.760000000000001,
-0.755000000000001,-0.750000000000001,-0.745000000000001,-0.740000000000001,
-0.735000000000001,-0.730000000000001,-0.725000000000001,-0.720000000000001,
-0.715000000000001,-0.710000000000001,-0.705000000000001,-0.700000000000001,
-0.695000000000001,-0.690000000000001,-0.685,-0.68,-0.675,-0.67,-0.665,
-0.66,-0.655,-0.65,-0.645,-0.64,-0.635,-0.63,-0.625,-0.62,-0.615,-0.61,
-0.605,-0.6,-0.595,-0.59,-0.585,-0.58,-0.575,-0.57,-0.565,-0.56,-0.555,
-0.55,-0.545,-0.54,-0.535,-0.53,-0.525,-0.52,-0.515,-0.51,-0.505,-0.5,-0.495,
-0.49,-0.485,-0.48,-0.475,-0.47,-0.465,-0.46,-0.455,-0.45,-0.445,-0.44,
-0.435,-0.43,-0.425,-0.42,-0.415,-0.41,-0.405,-0.4,-0.395,-0.39,-0.385,
-0.38,-0.375,-0.37,-0.365,-0.36,-0.355,-0.35,-0.345,-0.34,-0.335,-0.33,
-0.325,-0.32,-0.315,-0.31,-0.305,-0.3,-0.295,-0.29,-0.285,-0.28,-0.275,
-0.27,-0.265,-0.26,-0.255,-0.25,-0.245,-0.24,-0.235,-0.23,-0.225,-0.22,
-0.215,-0.21,-0.205,-0.2,-0.195,-0.19,-0.185,-0.18,-0.175,-0.17,-0.165,
-0.16,-0.155,-0.15,-0.145,-0.14,-0.135,-0.13,-0.125,-0.12,-0.115,-0.11,
-0.105,-0.1,-0.095,-0.09,-0.085,-0.08,-0.075,-0.07,-0.065,-0.06,-0.055,
-0.05,-0.045,-0.04,-0.035,-0.03,-0.025,-0.02,-0.015,-0.01,-0.005,0.),
 .UNSPECIFIED.)
CURVE()
GEOMETRIC_REPRESENTATION_ITEM()
RATIONAL_B_SPLINE_CURVE((1.,1.,1.,1.,1.,1.,1.,1.,1.,1.,1.,1.,1.,1.,1.,1.,
1.,1.,1.,1.,1.,1.,1.,1.,1.,1.,1.,1.,1.,1.,1.,1.,1.,1.,1.,1.,1.,1.,1.,1.,
1.,1.,1.,1.,1.,1.,1.,1.,1.,1.,1.,1.,1.,1.,1.,1.,1.,1.,1.,1.,1.,1.,1.,1.,
1.,1.,1.,1.,1.,1.,1.,1.,1.,1.,1.,1.,1.,1.,1.,1.,1.,1.,1.,1.,1.,1.,1.,1.,
1.,1.,1.,1.,1.,1.,1.,1.,1.,1.,1.,1.,1.,1.,1.,1.,1.,1.,1.,1.,1.,1.,1.,1.,
1.,1.,1.,1.,1.,1.,1.,1.,1.,1.,1.,1.,1.,1.,1.,1.,1.,1.,1.,1.,1.,1.,1.,1.,
1.,1.,1.,1.,1.,1.,1.,1.,1.,1.,1.,1.,1.,1.,1.,1.,1.,1.,1.,1.,1.,1.,1.,1.,
1.,1.,1.,1.,1.,1.,1.,1.,1.,1.,1.,1.,1.,1.,1.,1.,1.,1.,1.,1.,1.,1.,1.,1.,
1.,1.,1.,1.,1.,1.,1.,1.,1.,1.,1.,1.,1.,1.,1.,1.,1.,1.,1.,1.,1.))
REPRESENTATION_ITEM('')
);
#727=(
BOUNDED_CURVE()
B_SPLINE_CURVE(5,(#182645,#182646,#182647,#182648,#182649,#182650,#182651,
#182652,#182653,#182654,#182655,#182656,#182657,#182658,#182659,#182660,
#182661,#182662,#182663,#182664,#182665,#182666,#182667,#182668,#182669,
#182670,#182671,#182672,#182673,#182674,#182675,#182676,#182677,#182678,
#182679,#182680,#182681,#182682,#182683,#182684,#182685,#182686,#182687,
#182688,#182689,#182690,#182691,#182692,#182693,#182694,#182695,#182696,
#182697,#182698,#182699,#182700,#182701,#182702,#182703,#182704,#182705,
#182706,#182707,#182708,#182709,#182710,#182711,#182712,#182713,#182714,
#182715,#182716,#182717,#182718,#182719,#182720,#182721,#182722,#182723,
#182724,#182725,#182726,#182727,#182728,#182729,#182730,#182731,#182732,
#182733,#182734,#182735,#182736,#182737,#182738,#182739,#182740,#182741,
#182742,#182743,#182744,#182745,#182746,#182747,#182748,#182749,#182750,
#182751,#182752,#182753,#182754,#182755,#182756,#182757,#182758,#182759,
#182760,#182761,#182762,#182763,#182764,#182765,#182766,#182767,#182768,
#182769,#182770,#182771,#182772,#182773,#182774,#182775,#182776,#182777,
#182778,#182779,#182780,#182781,#182782,#182783,#182784,#182785,#182786,
#182787,#182788,#182789,#182790,#182791,#182792,#182793,#182794,#182795,
#182796,#182797,#182798,#182799,#182800,#182801,#182802,#182803,#182804,
#182805,#182806,#182807,#182808,#182809,#182810,#182811,#182812,#182813,
#182814,#182815,#182816,#182817,#182818,#182819,#182820,#182821,#182822,
#182823,#182824,#182825,#182826,#182827,#182828,#182829,#182830,#182831,
#182832,#182833,#182834,#182835,#182836,#182837,#182838,#182839,#182840,
#182841,#182842,#182843,#182844,#182845,#182846,#182847,#182848,#182849),
 .UNSPECIFIED.,.F.,.F.)
B_SPLINE_CURVE_WITH_KNOTS((6,1,1,1,1,1,1,1,1,1,1,1,1,1,1,1,1,1,1,1,1,1,
1,1,1,1,1,1,1,1,1,1,1,1,1,1,1,1,1,1,1,1,1,1,1,1,1,1,1,1,1,1,1,1,1,1,1,1,
1,1,1,1,1,1,1,1,1,1,1,1,1,1,1,1,1,1,1,1,1,1,1,1,1,1,1,1,1,1,1,1,1,1,1,1,
1,1,1,1,1,1,1,1,1,1,1,1,1,1,1,1,1,1,1,1,1,1,1,1,1,1,1,1,1,1,1,1,1,1,1,1,
1,1,1,1,1,1,1,1,1,1,1,1,1,1,1,1,1,1,1,1,1,1,1,1,1,1,1,1,1,1,1,1,1,1,1,1,
1,1,1,1,1,1,1,1,1,1,1,1,1,1,1,1,1,1,1,1,1,1,1,1,1,1,1,1,1,1,1,1,1,1,6),
(0.,0.005,0.01,0.015,0.02,0.025,0.03,0.035,0.04,0.045,0.05,0.055,0.06,0.065,
0.07,0.075,0.08,0.085,0.09,0.095,0.1,0.105,0.11,0.115,0.12,0.125,0.13,0.135,
0.14,0.145,0.15,0.155,0.16,0.165,0.17,0.175,0.18,0.185,0.19,0.195,0.2,0.205,
0.21,0.215,0.22,0.225,0.23,0.235,0.24,0.245,0.25,0.255,0.26,0.265,0.27,
0.275,0.28,0.285,0.29,0.295,0.3,0.305,0.31,0.315,0.32,0.325,0.33,0.335,
0.34,0.345,0.35,0.355,0.36,0.365,0.37,0.375,0.38,0.385,0.39,0.395,0.4,0.405,
0.41,0.415,0.42,0.425,0.43,0.435,0.44,0.445,0.45,0.455,0.46,0.465,0.47,
0.475,0.48,0.485,0.49,0.495,0.5,0.505,0.51,0.515,0.52,0.525,0.53,0.535,
0.54,0.545,0.55,0.555,0.56,0.565,0.57,0.575,0.58,0.585,0.59,0.595,0.6,0.605,
0.61,0.615,0.62,0.625,0.63,0.635,0.64,0.645,0.65,0.655,0.66,0.665,0.67,
0.675,0.68,0.685,0.690000000000001,0.695000000000001,0.700000000000001,
0.705000000000001,0.710000000000001,0.715000000000001,0.720000000000001,
0.725000000000001,0.730000000000001,0.735000000000001,0.740000000000001,
0.745000000000001,0.750000000000001,0.755000000000001,0.760000000000001,
0.765000000000001,0.770000000000001,0.775000000000001,0.780000000000001,
0.785000000000001,0.790000000000001,0.795000000000001,0.800000000000001,
0.805000000000001,0.810000000000001,0.815000000000001,0.820000000000001,
0.825000000000001,0.830000000000001,0.835000000000001,0.840000000000001,
0.845000000000001,0.850000000000001,0.855000000000001,0.860000000000001,
0.865000000000001,0.870000000000001,0.875000000000001,0.880000000000001,
0.885000000000001,0.890000000000001,0.895000000000001,0.900000000000001,
0.905000000000001,0.910000000000001,0.915000000000001,0.920000000000001,
0.925000000000001,0.930000000000001,0.935000000000001,0.940000000000001,
0.945000000000001,0.950000000000001,0.955000000000001,0.960000000000001,
0.965000000000001,0.970000000000001,0.975000000000001,0.980000000000001,
0.985000000000001,0.990000000000001,0.995000000000001,1.),.UNSPECIFIED.)
CURVE()
GEOMETRIC_REPRESENTATION_ITEM()
RATIONAL_B_SPLINE_CURVE((1.,1.,1.,1.,1.,1.,1.,1.,1.,1.,1.,1.,1.,1.,1.,1.,
1.,1.,1.,1.,1.,1.,1.,1.,1.,1.,1.,1.,1.,1.,1.,1.,1.,1.,1.,1.,1.,1.,1.,1.,
1.,1.,1.,1.,1.,1.,1.,1.,1.,1.,1.,1.,1.,1.,1.,1.,1.,1.,1.,1.,1.,1.,1.,1.,
1.,1.,1.,1.,1.,1.,1.,1.,1.,1.,1.,1.,1.,1.,1.,1.,1.,1.,1.,1.,1.,1.,1.,1.,
1.,1.,1.,1.,1.,1.,1.,1.,1.,1.,1.,1.,1.,1.,1.,1.,1.,1.,1.,1.,1.,1.,1.,1.,
1.,1.,1.,1.,1.,1.,1.,1.,1.,1.,1.,1.,1.,1.,1.,1.,1.,1.,1.,1.,1.,1.,1.,1.,
1.,1.,1.,1.,1.,1.,1.,1.,1.,1.,1.,1.,1.,1.,1.,1.,1.,1.,1.,1.,1.,1.,1.,1.,
1.,1.,1.,1.,1.,1.,1.,1.,1.,1.,1.,1.,1.,1.,1.,1.,1.,1.,1.,1.,1.,1.,1.,1.,
1.,1.,1.,1.,1.,1.,1.,1.,1.,1.,1.,1.,1.,1.,1.,1.,1.,1.,1.,1.,1.))
REPRESENTATION_ITEM('')
);
#728=(
BOUNDED_CURVE()
B_SPLINE_CURVE(5,(#182853,#182854,#182855,#182856,#182857,#182858,#182859,
#182860,#182861,#182862,#182863,#182864,#182865,#182866,#182867,#182868,
#182869,#182870,#182871,#182872,#182873,#182874,#182875,#182876,#182877,
#182878,#182879,#182880,#182881,#182882,#182883,#182884,#182885,#182886,
#182887,#182888,#182889,#182890,#182891,#182892,#182893,#182894,#182895,
#182896,#182897,#182898,#182899,#182900,#182901,#182902,#182903,#182904,
#182905,#182906,#182907,#182908,#182909,#182910,#182911,#182912,#182913,
#182914,#182915,#182916,#182917,#182918,#182919,#182920,#182921,#182922,
#182923,#182924,#182925,#182926,#182927,#182928,#182929,#182930,#182931,
#182932,#182933,#182934,#182935,#182936,#182937,#182938,#182939,#182940,
#182941,#182942,#182943,#182944,#182945,#182946,#182947,#182948,#182949,
#182950,#182951,#182952,#182953,#182954,#182955,#182956,#182957,#182958,
#182959,#182960,#182961,#182962,#182963,#182964,#182965,#182966,#182967,
#182968,#182969,#182970,#182971,#182972,#182973,#182974,#182975,#182976,
#182977,#182978,#182979,#182980,#182981,#182982,#182983,#182984,#182985,
#182986,#182987,#182988,#182989,#182990,#182991,#182992,#182993,#182994,
#182995,#182996,#182997,#182998,#182999,#183000,#183001,#183002,#183003,
#183004,#183005,#183006,#183007,#183008,#183009,#183010,#183011,#183012,
#183013,#183014,#183015,#183016,#183017,#183018,#183019,#183020,#183021,
#183022,#183023,#183024,#183025,#183026,#183027,#183028,#183029,#183030,
#183031,#183032,#183033,#183034,#183035,#183036,#183037,#183038,#183039,
#183040,#183041,#183042,#183043,#183044,#183045,#183046,#183047,#183048,
#183049,#183050,#183051,#183052,#183053,#183054,#183055,#183056,#183057),
 .UNSPECIFIED.,.F.,.F.)
B_SPLINE_CURVE_WITH_KNOTS((6,1,1,1,1,1,1,1,1,1,1,1,1,1,1,1,1,1,1,1,1,1,
1,1,1,1,1,1,1,1,1,1,1,1,1,1,1,1,1,1,1,1,1,1,1,1,1,1,1,1,1,1,1,1,1,1,1,1,
1,1,1,1,1,1,1,1,1,1,1,1,1,1,1,1,1,1,1,1,1,1,1,1,1,1,1,1,1,1,1,1,1,1,1,1,
1,1,1,1,1,1,1,1,1,1,1,1,1,1,1,1,1,1,1,1,1,1,1,1,1,1,1,1,1,1,1,1,1,1,1,1,
1,1,1,1,1,1,1,1,1,1,1,1,1,1,1,1,1,1,1,1,1,1,1,1,1,1,1,1,1,1,1,1,1,1,1,1,
1,1,1,1,1,1,1,1,1,1,1,1,1,1,1,1,1,1,1,1,1,1,1,1,1,1,1,1,1,1,1,1,1,1,6),
(-1.,-0.995000000000001,-0.990000000000001,-0.985000000000001,-0.980000000000001,
-0.975000000000001,-0.970000000000001,-0.965000000000001,-0.960000000000001,
-0.955000000000001,-0.950000000000001,-0.945000000000001,-0.940000000000001,
-0.935000000000001,-0.930000000000001,-0.925000000000001,-0.920000000000001,
-0.915000000000001,-0.910000000000001,-0.905000000000001,-0.900000000000001,
-0.895000000000001,-0.890000000000001,-0.885000000000001,-0.880000000000001,
-0.875000000000001,-0.870000000000001,-0.865000000000001,-0.860000000000001,
-0.855000000000001,-0.850000000000001,-0.845000000000001,-0.840000000000001,
-0.835000000000001,-0.830000000000001,-0.825000000000001,-0.820000000000001,
-0.815000000000001,-0.810000000000001,-0.805000000000001,-0.800000000000001,
-0.795000000000001,-0.790000000000001,-0.785000000000001,-0.780000000000001,
-0.775000000000001,-0.770000000000001,-0.765000000000001,-0.760000000000001,
-0.755000000000001,-0.750000000000001,-0.745000000000001,-0.740000000000001,
-0.735000000000001,-0.730000000000001,-0.725000000000001,-0.720000000000001,
-0.715000000000001,-0.710000000000001,-0.705000000000001,-0.700000000000001,
-0.695000000000001,-0.690000000000001,-0.685,-0.68,-0.675,-0.67,-0.665,
-0.66,-0.655,-0.65,-0.645,-0.64,-0.635,-0.63,-0.625,-0.62,-0.615,-0.61,
-0.605,-0.6,-0.595,-0.59,-0.585,-0.58,-0.575,-0.57,-0.565,-0.56,-0.555,
-0.55,-0.545,-0.54,-0.535,-0.53,-0.525,-0.52,-0.515,-0.51,-0.505,-0.5,-0.495,
-0.49,-0.485,-0.48,-0.475,-0.47,-0.465,-0.46,-0.455,-0.45,-0.445,-0.44,
-0.435,-0.43,-0.425,-0.42,-0.415,-0.41,-0.405,-0.4,-0.395,-0.39,-0.385,
-0.38,-0.375,-0.37,-0.365,-0.36,-0.355,-0.35,-0.345,-0.34,-0.335,-0.33,
-0.325,-0.32,-0.315,-0.31,-0.305,-0.3,-0.295,-0.29,-0.285,-0.28,-0.275,
-0.27,-0.265,-0.26,-0.255,-0.25,-0.245,-0.24,-0.235,-0.23,-0.225,-0.22,
-0.215,-0.21,-0.205,-0.2,-0.195,-0.19,-0.185,-0.18,-0.175,-0.17,-0.165,
-0.16,-0.155,-0.15,-0.145,-0.14,-0.135,-0.13,-0.125,-0.12,-0.115,-0.11,
-0.105,-0.1,-0.095,-0.09,-0.085,-0.08,-0.075,-0.07,-0.065,-0.06,-0.055,
-0.05,-0.045,-0.04,-0.035,-0.03,-0.025,-0.02,-0.015,-0.01,-0.005,0.),
 .UNSPECIFIED.)
CURVE()
GEOMETRIC_REPRESENTATION_ITEM()
RATIONAL_B_SPLINE_CURVE((1.,1.,1.,1.,1.,1.,1.,1.,1.,1.,1.,1.,1.,1.,1.,1.,
1.,1.,1.,1.,1.,1.,1.,1.,1.,1.,1.,1.,1.,1.,1.,1.,1.,1.,1.,1.,1.,1.,1.,1.,
1.,1.,1.,1.,1.,1.,1.,1.,1.,1.,1.,1.,1.,1.,1.,1.,1.,1.,1.,1.,1.,1.,1.,1.,
1.,1.,1.,1.,1.,1.,1.,1.,1.,1.,1.,1.,1.,1.,1.,1.,1.,1.,1.,1.,1.,1.,1.,1.,
1.,1.,1.,1.,1.,1.,1.,1.,1.,1.,1.,1.,1.,1.,1.,1.,1.,1.,1.,1.,1.,1.,1.,1.,
1.,1.,1.,1.,1.,1.,1.,1.,1.,1.,1.,1.,1.,1.,1.,1.,1.,1.,1.,1.,1.,1.,1.,1.,
1.,1.,1.,1.,1.,1.,1.,1.,1.,1.,1.,1.,1.,1.,1.,1.,1.,1.,1.,1.,1.,1.,1.,1.,
1.,1.,1.,1.,1.,1.,1.,1.,1.,1.,1.,1.,1.,1.,1.,1.,1.,1.,1.,1.,1.,1.,1.,1.,
1.,1.,1.,1.,1.,1.,1.,1.,1.,1.,1.,1.,1.,1.,1.,1.,1.,1.,1.,1.,1.))
REPRESENTATION_ITEM('')
);
#729=(
BOUNDED_CURVE()
B_SPLINE_CURVE(5,(#183069,#183070,#183071,#183072,#183073,#183074,#183075,
#183076,#183077,#183078,#183079,#183080,#183081,#183082,#183083,#183084,
#183085,#183086,#183087,#183088,#183089,#183090,#183091,#183092,#183093,
#183094,#183095,#183096,#183097,#183098,#183099,#183100,#183101,#183102,
#183103,#183104,#183105,#183106,#183107,#183108,#183109,#183110,#183111,
#183112,#183113,#183114,#183115,#183116,#183117,#183118,#183119,#183120,
#183121,#183122,#183123,#183124,#183125,#183126,#183127,#183128,#183129,
#183130,#183131,#183132,#183133,#183134,#183135,#183136,#183137,#183138,
#183139,#183140,#183141,#183142,#183143,#183144,#183145,#183146,#183147,
#183148,#183149,#183150,#183151,#183152,#183153,#183154,#183155,#183156,
#183157,#183158,#183159,#183160,#183161,#183162,#183163,#183164,#183165,
#183166,#183167,#183168,#183169,#183170,#183171,#183172,#183173,#183174,
#183175,#183176,#183177,#183178,#183179,#183180,#183181,#183182,#183183,
#183184,#183185,#183186,#183187,#183188,#183189,#183190,#183191,#183192,
#183193,#183194,#183195,#183196,#183197,#183198,#183199,#183200,#183201,
#183202,#183203,#183204,#183205,#183206,#183207,#183208,#183209,#183210,
#183211,#183212,#183213,#183214,#183215,#183216,#183217,#183218,#183219,
#183220,#183221,#183222,#183223,#183224,#183225,#183226,#183227,#183228,
#183229,#183230,#183231,#183232,#183233,#183234,#183235,#183236,#183237,
#183238,#183239,#183240,#183241,#183242,#183243,#183244,#183245,#183246,
#183247,#183248,#183249,#183250,#183251,#183252,#183253,#183254,#183255,
#183256,#183257,#183258,#183259,#183260,#183261,#183262,#183263,#183264,
#183265,#183266,#183267,#183268,#183269,#183270,#183271,#183272,#183273),
 .UNSPECIFIED.,.F.,.F.)
B_SPLINE_CURVE_WITH_KNOTS((6,1,1,1,1,1,1,1,1,1,1,1,1,1,1,1,1,1,1,1,1,1,
1,1,1,1,1,1,1,1,1,1,1,1,1,1,1,1,1,1,1,1,1,1,1,1,1,1,1,1,1,1,1,1,1,1,1,1,
1,1,1,1,1,1,1,1,1,1,1,1,1,1,1,1,1,1,1,1,1,1,1,1,1,1,1,1,1,1,1,1,1,1,1,1,
1,1,1,1,1,1,1,1,1,1,1,1,1,1,1,1,1,1,1,1,1,1,1,1,1,1,1,1,1,1,1,1,1,1,1,1,
1,1,1,1,1,1,1,1,1,1,1,1,1,1,1,1,1,1,1,1,1,1,1,1,1,1,1,1,1,1,1,1,1,1,1,1,
1,1,1,1,1,1,1,1,1,1,1,1,1,1,1,1,1,1,1,1,1,1,1,1,1,1,1,1,1,1,1,1,1,1,6),
(0.,0.005,0.01,0.015,0.02,0.025,0.03,0.035,0.04,0.045,0.05,0.055,0.06,0.065,
0.07,0.075,0.08,0.085,0.09,0.095,0.1,0.105,0.11,0.115,0.12,0.125,0.13,0.135,
0.14,0.145,0.15,0.155,0.16,0.165,0.17,0.175,0.18,0.185,0.19,0.195,0.2,0.205,
0.21,0.215,0.22,0.225,0.23,0.235,0.24,0.245,0.25,0.255,0.26,0.265,0.27,
0.275,0.28,0.285,0.29,0.295,0.3,0.305,0.31,0.315,0.32,0.325,0.33,0.335,
0.34,0.345,0.35,0.355,0.36,0.365,0.37,0.375,0.38,0.385,0.39,0.395,0.4,0.405,
0.41,0.415,0.42,0.425,0.43,0.435,0.44,0.445,0.45,0.455,0.46,0.465,0.47,
0.475,0.48,0.485,0.49,0.495,0.5,0.505,0.51,0.515,0.52,0.525,0.53,0.535,
0.54,0.545,0.55,0.555,0.56,0.565,0.57,0.575,0.58,0.585,0.59,0.595,0.6,0.605,
0.61,0.615,0.62,0.625,0.63,0.635,0.64,0.645,0.65,0.655,0.66,0.665,0.67,
0.675,0.68,0.685,0.690000000000001,0.695000000000001,0.700000000000001,
0.705000000000001,0.710000000000001,0.715000000000001,0.720000000000001,
0.725000000000001,0.730000000000001,0.735000000000001,0.740000000000001,
0.745000000000001,0.750000000000001,0.755000000000001,0.760000000000001,
0.765000000000001,0.770000000000001,0.775000000000001,0.780000000000001,
0.785000000000001,0.790000000000001,0.795000000000001,0.800000000000001,
0.805000000000001,0.810000000000001,0.815000000000001,0.820000000000001,
0.825000000000001,0.830000000000001,0.835000000000001,0.840000000000001,
0.845000000000001,0.850000000000001,0.855000000000001,0.860000000000001,
0.865000000000001,0.870000000000001,0.875000000000001,0.880000000000001,
0.885000000000001,0.890000000000001,0.895000000000001,0.900000000000001,
0.905000000000001,0.910000000000001,0.915000000000001,0.920000000000001,
0.925000000000001,0.930000000000001,0.935000000000001,0.940000000000001,
0.945000000000001,0.950000000000001,0.955000000000001,0.960000000000001,
0.965000000000001,0.970000000000001,0.975000000000001,0.980000000000001,
0.985000000000001,0.990000000000001,0.995000000000001,1.),.UNSPECIFIED.)
CURVE()
GEOMETRIC_REPRESENTATION_ITEM()
RATIONAL_B_SPLINE_CURVE((1.,1.,1.,1.,1.,1.,1.,1.,1.,1.,1.,1.,1.,1.,1.,1.,
1.,1.,1.,1.,1.,1.,1.,1.,1.,1.,1.,1.,1.,1.,1.,1.,1.,1.,1.,1.,1.,1.,1.,1.,
1.,1.,1.,1.,1.,1.,1.,1.,1.,1.,1.,1.,1.,1.,1.,1.,1.,1.,1.,1.,1.,1.,1.,1.,
1.,1.,1.,1.,1.,1.,1.,1.,1.,1.,1.,1.,1.,1.,1.,1.,1.,1.,1.,1.,1.,1.,1.,1.,
1.,1.,1.,1.,1.,1.,1.,1.,1.,1.,1.,1.,1.,1.,1.,1.,1.,1.,1.,1.,1.,1.,1.,1.,
1.,1.,1.,1.,1.,1.,1.,1.,1.,1.,1.,1.,1.,1.,1.,1.,1.,1.,1.,1.,1.,1.,1.,1.,
1.,1.,1.,1.,1.,1.,1.,1.,1.,1.,1.,1.,1.,1.,1.,1.,1.,1.,1.,1.,1.,1.,1.,1.,
1.,1.,1.,1.,1.,1.,1.,1.,1.,1.,1.,1.,1.,1.,1.,1.,1.,1.,1.,1.,1.,1.,1.,1.,
1.,1.,1.,1.,1.,1.,1.,1.,1.,1.,1.,1.,1.,1.,1.,1.,1.,1.,1.,1.,1.))
REPRESENTATION_ITEM('')
);
#730=(
BOUNDED_CURVE()
B_SPLINE_CURVE(5,(#183277,#183278,#183279,#183280,#183281,#183282,#183283,
#183284,#183285,#183286,#183287,#183288,#183289,#183290,#183291,#183292,
#183293,#183294,#183295,#183296,#183297,#183298,#183299,#183300,#183301,
#183302,#183303,#183304,#183305,#183306,#183307,#183308,#183309,#183310,
#183311,#183312,#183313,#183314,#183315,#183316,#183317,#183318,#183319,
#183320,#183321,#183322,#183323,#183324,#183325,#183326,#183327,#183328,
#183329,#183330,#183331,#183332,#183333,#183334,#183335,#183336,#183337,
#183338,#183339,#183340,#183341,#183342,#183343,#183344,#183345,#183346,
#183347,#183348,#183349,#183350,#183351,#183352,#183353,#183354,#183355,
#183356,#183357,#183358,#183359,#183360,#183361,#183362,#183363,#183364,
#183365,#183366,#183367,#183368,#183369,#183370,#183371,#183372,#183373,
#183374,#183375,#183376,#183377,#183378,#183379,#183380,#183381,#183382,
#183383,#183384,#183385,#183386,#183387,#183388,#183389,#183390,#183391,
#183392,#183393,#183394,#183395,#183396,#183397,#183398,#183399,#183400,
#183401,#183402,#183403,#183404,#183405,#183406,#183407,#183408,#183409,
#183410,#183411,#183412,#183413,#183414,#183415,#183416,#183417,#183418,
#183419,#183420,#183421,#183422,#183423,#183424,#183425,#183426,#183427,
#183428,#183429,#183430,#183431,#183432,#183433,#183434,#183435,#183436,
#183437,#183438,#183439,#183440,#183441,#183442,#183443,#183444,#183445,
#183446,#183447,#183448,#183449,#183450,#183451,#183452,#183453,#183454,
#183455,#183456,#183457,#183458,#183459,#183460,#183461,#183462,#183463,
#183464,#183465,#183466,#183467,#183468,#183469,#183470,#183471,#183472,
#183473,#183474,#183475,#183476,#183477,#183478,#183479,#183480,#183481),
 .UNSPECIFIED.,.F.,.F.)
B_SPLINE_CURVE_WITH_KNOTS((6,1,1,1,1,1,1,1,1,1,1,1,1,1,1,1,1,1,1,1,1,1,
1,1,1,1,1,1,1,1,1,1,1,1,1,1,1,1,1,1,1,1,1,1,1,1,1,1,1,1,1,1,1,1,1,1,1,1,
1,1,1,1,1,1,1,1,1,1,1,1,1,1,1,1,1,1,1,1,1,1,1,1,1,1,1,1,1,1,1,1,1,1,1,1,
1,1,1,1,1,1,1,1,1,1,1,1,1,1,1,1,1,1,1,1,1,1,1,1,1,1,1,1,1,1,1,1,1,1,1,1,
1,1,1,1,1,1,1,1,1,1,1,1,1,1,1,1,1,1,1,1,1,1,1,1,1,1,1,1,1,1,1,1,1,1,1,1,
1,1,1,1,1,1,1,1,1,1,1,1,1,1,1,1,1,1,1,1,1,1,1,1,1,1,1,1,1,1,1,1,1,1,6),
(-1.,-0.995000000000001,-0.990000000000001,-0.985000000000001,-0.980000000000001,
-0.975000000000001,-0.970000000000001,-0.965000000000001,-0.960000000000001,
-0.955000000000001,-0.950000000000001,-0.945000000000001,-0.940000000000001,
-0.935000000000001,-0.930000000000001,-0.925000000000001,-0.920000000000001,
-0.915000000000001,-0.910000000000001,-0.905000000000001,-0.900000000000001,
-0.895000000000001,-0.890000000000001,-0.885000000000001,-0.880000000000001,
-0.875000000000001,-0.870000000000001,-0.865000000000001,-0.860000000000001,
-0.855000000000001,-0.850000000000001,-0.845000000000001,-0.840000000000001,
-0.835000000000001,-0.830000000000001,-0.825000000000001,-0.820000000000001,
-0.815000000000001,-0.810000000000001,-0.805000000000001,-0.800000000000001,
-0.795000000000001,-0.790000000000001,-0.785000000000001,-0.780000000000001,
-0.775000000000001,-0.770000000000001,-0.765000000000001,-0.760000000000001,
-0.755000000000001,-0.750000000000001,-0.745000000000001,-0.740000000000001,
-0.735000000000001,-0.730000000000001,-0.725000000000001,-0.720000000000001,
-0.715000000000001,-0.710000000000001,-0.705000000000001,-0.700000000000001,
-0.695000000000001,-0.690000000000001,-0.685,-0.68,-0.675,-0.67,-0.665,
-0.66,-0.655,-0.65,-0.645,-0.64,-0.635,-0.63,-0.625,-0.62,-0.615,-0.61,
-0.605,-0.6,-0.595,-0.59,-0.585,-0.58,-0.575,-0.57,-0.565,-0.56,-0.555,
-0.55,-0.545,-0.54,-0.535,-0.53,-0.525,-0.52,-0.515,-0.51,-0.505,-0.5,-0.495,
-0.49,-0.485,-0.48,-0.475,-0.47,-0.465,-0.46,-0.455,-0.45,-0.445,-0.44,
-0.435,-0.43,-0.425,-0.42,-0.415,-0.41,-0.405,-0.4,-0.395,-0.39,-0.385,
-0.38,-0.375,-0.37,-0.365,-0.36,-0.355,-0.35,-0.345,-0.34,-0.335,-0.33,
-0.325,-0.32,-0.315,-0.31,-0.305,-0.3,-0.295,-0.29,-0.285,-0.28,-0.275,
-0.27,-0.265,-0.26,-0.255,-0.25,-0.245,-0.24,-0.235,-0.23,-0.225,-0.22,
-0.215,-0.21,-0.205,-0.2,-0.195,-0.19,-0.185,-0.18,-0.175,-0.17,-0.165,
-0.16,-0.155,-0.15,-0.145,-0.14,-0.135,-0.13,-0.125,-0.12,-0.115,-0.11,
-0.105,-0.1,-0.095,-0.09,-0.085,-0.08,-0.075,-0.07,-0.065,-0.06,-0.055,
-0.05,-0.045,-0.04,-0.035,-0.03,-0.025,-0.02,-0.015,-0.01,-0.005,0.),
 .UNSPECIFIED.)
CURVE()
GEOMETRIC_REPRESENTATION_ITEM()
RATIONAL_B_SPLINE_CURVE((1.,1.,1.,1.,1.,1.,1.,1.,1.,1.,1.,1.,1.,1.,1.,1.,
1.,1.,1.,1.,1.,1.,1.,1.,1.,1.,1.,1.,1.,1.,1.,1.,1.,1.,1.,1.,1.,1.,1.,1.,
1.,1.,1.,1.,1.,1.,1.,1.,1.,1.,1.,1.,1.,1.,1.,1.,1.,1.,1.,1.,1.,1.,1.,1.,
1.,1.,1.,1.,1.,1.,1.,1.,1.,1.,1.,1.,1.,1.,1.,1.,1.,1.,1.,1.,1.,1.,1.,1.,
1.,1.,1.,1.,1.,1.,1.,1.,1.,1.,1.,1.,1.,1.,1.,1.,1.,1.,1.,1.,1.,1.,1.,1.,
1.,1.,1.,1.,1.,1.,1.,1.,1.,1.,1.,1.,1.,1.,1.,1.,1.,1.,1.,1.,1.,1.,1.,1.,
1.,1.,1.,1.,1.,1.,1.,1.,1.,1.,1.,1.,1.,1.,1.,1.,1.,1.,1.,1.,1.,1.,1.,1.,
1.,1.,1.,1.,1.,1.,1.,1.,1.,1.,1.,1.,1.,1.,1.,1.,1.,1.,1.,1.,1.,1.,1.,1.,
1.,1.,1.,1.,1.,1.,1.,1.,1.,1.,1.,1.,1.,1.,1.,1.,1.,1.,1.,1.,1.))
REPRESENTATION_ITEM('')
);
#731=(
BOUNDED_CURVE()
B_SPLINE_CURVE(5,(#183493,#183494,#183495,#183496,#183497,#183498,#183499,
#183500,#183501,#183502,#183503,#183504,#183505,#183506,#183507,#183508,
#183509,#183510,#183511,#183512,#183513,#183514,#183515,#183516,#183517,
#183518,#183519,#183520,#183521,#183522,#183523,#183524,#183525,#183526,
#183527,#183528,#183529,#183530,#183531,#183532,#183533,#183534,#183535,
#183536,#183537,#183538,#183539,#183540,#183541,#183542,#183543,#183544,
#183545,#183546,#183547,#183548,#183549,#183550,#183551,#183552,#183553,
#183554,#183555,#183556,#183557,#183558,#183559,#183560,#183561,#183562,
#183563,#183564,#183565,#183566,#183567,#183568,#183569,#183570,#183571,
#183572,#183573,#183574,#183575,#183576,#183577,#183578,#183579,#183580,
#183581,#183582,#183583,#183584,#183585,#183586,#183587,#183588,#183589,
#183590,#183591,#183592,#183593,#183594,#183595,#183596,#183597,#183598,
#183599,#183600,#183601,#183602,#183603,#183604,#183605,#183606,#183607,
#183608,#183609,#183610,#183611,#183612,#183613,#183614,#183615,#183616,
#183617,#183618,#183619,#183620,#183621,#183622,#183623,#183624,#183625,
#183626,#183627,#183628,#183629,#183630,#183631,#183632,#183633,#183634,
#183635,#183636,#183637,#183638,#183639,#183640,#183641,#183642,#183643,
#183644,#183645,#183646,#183647,#183648,#183649,#183650,#183651,#183652,
#183653,#183654,#183655,#183656,#183657,#183658,#183659,#183660,#183661,
#183662,#183663,#183664,#183665,#183666,#183667,#183668,#183669,#183670,
#183671,#183672,#183673,#183674,#183675,#183676,#183677,#183678,#183679,
#183680,#183681,#183682,#183683,#183684,#183685,#183686,#183687,#183688,
#183689,#183690,#183691,#183692,#183693,#183694,#183695,#183696,#183697),
 .UNSPECIFIED.,.F.,.F.)
B_SPLINE_CURVE_WITH_KNOTS((6,1,1,1,1,1,1,1,1,1,1,1,1,1,1,1,1,1,1,1,1,1,
1,1,1,1,1,1,1,1,1,1,1,1,1,1,1,1,1,1,1,1,1,1,1,1,1,1,1,1,1,1,1,1,1,1,1,1,
1,1,1,1,1,1,1,1,1,1,1,1,1,1,1,1,1,1,1,1,1,1,1,1,1,1,1,1,1,1,1,1,1,1,1,1,
1,1,1,1,1,1,1,1,1,1,1,1,1,1,1,1,1,1,1,1,1,1,1,1,1,1,1,1,1,1,1,1,1,1,1,1,
1,1,1,1,1,1,1,1,1,1,1,1,1,1,1,1,1,1,1,1,1,1,1,1,1,1,1,1,1,1,1,1,1,1,1,1,
1,1,1,1,1,1,1,1,1,1,1,1,1,1,1,1,1,1,1,1,1,1,1,1,1,1,1,1,1,1,1,1,1,1,6),
(0.,0.005,0.01,0.015,0.02,0.025,0.03,0.035,0.04,0.045,0.05,0.055,0.06,0.065,
0.07,0.075,0.08,0.085,0.09,0.095,0.1,0.105,0.11,0.115,0.12,0.125,0.13,0.135,
0.14,0.145,0.15,0.155,0.16,0.165,0.17,0.175,0.18,0.185,0.19,0.195,0.2,0.205,
0.21,0.215,0.22,0.225,0.23,0.235,0.24,0.245,0.25,0.255,0.26,0.265,0.27,
0.275,0.28,0.285,0.29,0.295,0.3,0.305,0.31,0.315,0.32,0.325,0.33,0.335,
0.34,0.345,0.35,0.355,0.36,0.365,0.37,0.375,0.38,0.385,0.39,0.395,0.4,0.405,
0.41,0.415,0.42,0.425,0.43,0.435,0.44,0.445,0.45,0.455,0.46,0.465,0.47,
0.475,0.48,0.485,0.49,0.495,0.5,0.505,0.51,0.515,0.52,0.525,0.53,0.535,
0.54,0.545,0.55,0.555,0.56,0.565,0.57,0.575,0.58,0.585,0.59,0.595,0.6,0.605,
0.61,0.615,0.62,0.625,0.63,0.635,0.64,0.645,0.65,0.655,0.66,0.665,0.67,
0.675,0.68,0.685,0.690000000000001,0.695000000000001,0.700000000000001,
0.705000000000001,0.710000000000001,0.715000000000001,0.720000000000001,
0.725000000000001,0.730000000000001,0.735000000000001,0.740000000000001,
0.745000000000001,0.750000000000001,0.755000000000001,0.760000000000001,
0.765000000000001,0.770000000000001,0.775000000000001,0.780000000000001,
0.785000000000001,0.790000000000001,0.795000000000001,0.800000000000001,
0.805000000000001,0.810000000000001,0.815000000000001,0.820000000000001,
0.825000000000001,0.830000000000001,0.835000000000001,0.840000000000001,
0.845000000000001,0.850000000000001,0.855000000000001,0.860000000000001,
0.865000000000001,0.870000000000001,0.875000000000001,0.880000000000001,
0.885000000000001,0.890000000000001,0.895000000000001,0.900000000000001,
0.905000000000001,0.910000000000001,0.915000000000001,0.920000000000001,
0.925000000000001,0.930000000000001,0.935000000000001,0.940000000000001,
0.945000000000001,0.950000000000001,0.955000000000001,0.960000000000001,
0.965000000000001,0.970000000000001,0.975000000000001,0.980000000000001,
0.985000000000001,0.990000000000001,0.995000000000001,1.),.UNSPECIFIED.)
CURVE()
GEOMETRIC_REPRESENTATION_ITEM()
RATIONAL_B_SPLINE_CURVE((1.,1.,1.,1.,1.,1.,1.,1.,1.,1.,1.,1.,1.,1.,1.,1.,
1.,1.,1.,1.,1.,1.,1.,1.,1.,1.,1.,1.,1.,1.,1.,1.,1.,1.,1.,1.,1.,1.,1.,1.,
1.,1.,1.,1.,1.,1.,1.,1.,1.,1.,1.,1.,1.,1.,1.,1.,1.,1.,1.,1.,1.,1.,1.,1.,
1.,1.,1.,1.,1.,1.,1.,1.,1.,1.,1.,1.,1.,1.,1.,1.,1.,1.,1.,1.,1.,1.,1.,1.,
1.,1.,1.,1.,1.,1.,1.,1.,1.,1.,1.,1.,1.,1.,1.,1.,1.,1.,1.,1.,1.,1.,1.,1.,
1.,1.,1.,1.,1.,1.,1.,1.,1.,1.,1.,1.,1.,1.,1.,1.,1.,1.,1.,1.,1.,1.,1.,1.,
1.,1.,1.,1.,1.,1.,1.,1.,1.,1.,1.,1.,1.,1.,1.,1.,1.,1.,1.,1.,1.,1.,1.,1.,
1.,1.,1.,1.,1.,1.,1.,1.,1.,1.,1.,1.,1.,1.,1.,1.,1.,1.,1.,1.,1.,1.,1.,1.,
1.,1.,1.,1.,1.,1.,1.,1.,1.,1.,1.,1.,1.,1.,1.,1.,1.,1.,1.,1.,1.))
REPRESENTATION_ITEM('')
);
#732=(
BOUNDED_CURVE()
B_SPLINE_CURVE(5,(#183701,#183702,#183703,#183704,#183705,#183706,#183707,
#183708,#183709,#183710,#183711,#183712,#183713,#183714,#183715,#183716,
#183717,#183718,#183719,#183720,#183721,#183722,#183723,#183724,#183725,
#183726,#183727,#183728,#183729,#183730,#183731,#183732,#183733,#183734,
#183735,#183736,#183737,#183738,#183739,#183740,#183741,#183742,#183743,
#183744,#183745,#183746,#183747,#183748,#183749,#183750,#183751,#183752,
#183753,#183754,#183755,#183756,#183757,#183758,#183759,#183760,#183761,
#183762,#183763,#183764,#183765,#183766,#183767,#183768,#183769,#183770,
#183771,#183772,#183773,#183774,#183775,#183776,#183777,#183778,#183779,
#183780,#183781,#183782,#183783,#183784,#183785,#183786,#183787,#183788,
#183789,#183790,#183791,#183792,#183793,#183794,#183795,#183796,#183797,
#183798,#183799,#183800,#183801,#183802,#183803,#183804,#183805,#183806,
#183807,#183808,#183809,#183810,#183811,#183812,#183813,#183814,#183815,
#183816,#183817,#183818,#183819,#183820,#183821,#183822,#183823,#183824,
#183825,#183826,#183827,#183828,#183829,#183830,#183831,#183832,#183833,
#183834,#183835,#183836,#183837,#183838,#183839,#183840,#183841,#183842,
#183843,#183844,#183845,#183846,#183847,#183848,#183849,#183850,#183851,
#183852,#183853,#183854,#183855,#183856,#183857,#183858,#183859,#183860,
#183861,#183862,#183863,#183864,#183865,#183866,#183867,#183868,#183869,
#183870,#183871,#183872,#183873,#183874,#183875,#183876,#183877,#183878,
#183879,#183880,#183881,#183882,#183883,#183884,#183885,#183886,#183887,
#183888,#183889,#183890,#183891,#183892,#183893,#183894,#183895,#183896,
#183897,#183898,#183899,#183900,#183901,#183902,#183903,#183904,#183905),
 .UNSPECIFIED.,.F.,.F.)
B_SPLINE_CURVE_WITH_KNOTS((6,1,1,1,1,1,1,1,1,1,1,1,1,1,1,1,1,1,1,1,1,1,
1,1,1,1,1,1,1,1,1,1,1,1,1,1,1,1,1,1,1,1,1,1,1,1,1,1,1,1,1,1,1,1,1,1,1,1,
1,1,1,1,1,1,1,1,1,1,1,1,1,1,1,1,1,1,1,1,1,1,1,1,1,1,1,1,1,1,1,1,1,1,1,1,
1,1,1,1,1,1,1,1,1,1,1,1,1,1,1,1,1,1,1,1,1,1,1,1,1,1,1,1,1,1,1,1,1,1,1,1,
1,1,1,1,1,1,1,1,1,1,1,1,1,1,1,1,1,1,1,1,1,1,1,1,1,1,1,1,1,1,1,1,1,1,1,1,
1,1,1,1,1,1,1,1,1,1,1,1,1,1,1,1,1,1,1,1,1,1,1,1,1,1,1,1,1,1,1,1,1,1,6),
(-1.,-0.995000000000001,-0.990000000000001,-0.985000000000001,-0.980000000000001,
-0.975000000000001,-0.970000000000001,-0.965000000000001,-0.960000000000001,
-0.955000000000001,-0.950000000000001,-0.945000000000001,-0.940000000000001,
-0.935000000000001,-0.930000000000001,-0.925000000000001,-0.920000000000001,
-0.915000000000001,-0.910000000000001,-0.905000000000001,-0.900000000000001,
-0.895000000000001,-0.890000000000001,-0.885000000000001,-0.880000000000001,
-0.875000000000001,-0.870000000000001,-0.865000000000001,-0.860000000000001,
-0.855000000000001,-0.850000000000001,-0.845000000000001,-0.840000000000001,
-0.835000000000001,-0.830000000000001,-0.825000000000001,-0.820000000000001,
-0.815000000000001,-0.810000000000001,-0.805000000000001,-0.800000000000001,
-0.795000000000001,-0.790000000000001,-0.785000000000001,-0.780000000000001,
-0.775000000000001,-0.770000000000001,-0.765000000000001,-0.760000000000001,
-0.755000000000001,-0.750000000000001,-0.745000000000001,-0.740000000000001,
-0.735000000000001,-0.730000000000001,-0.725000000000001,-0.720000000000001,
-0.715000000000001,-0.710000000000001,-0.705000000000001,-0.700000000000001,
-0.695000000000001,-0.690000000000001,-0.685,-0.68,-0.675,-0.67,-0.665,
-0.66,-0.655,-0.65,-0.645,-0.64,-0.635,-0.63,-0.625,-0.62,-0.615,-0.61,
-0.605,-0.6,-0.595,-0.59,-0.585,-0.58,-0.575,-0.57,-0.565,-0.56,-0.555,
-0.55,-0.545,-0.54,-0.535,-0.53,-0.525,-0.52,-0.515,-0.51,-0.505,-0.5,-0.495,
-0.49,-0.485,-0.48,-0.475,-0.47,-0.465,-0.46,-0.455,-0.45,-0.445,-0.44,
-0.435,-0.43,-0.425,-0.42,-0.415,-0.41,-0.405,-0.4,-0.395,-0.39,-0.385,
-0.38,-0.375,-0.37,-0.365,-0.36,-0.355,-0.35,-0.345,-0.34,-0.335,-0.33,
-0.325,-0.32,-0.315,-0.31,-0.305,-0.3,-0.295,-0.29,-0.285,-0.28,-0.275,
-0.27,-0.265,-0.26,-0.255,-0.25,-0.245,-0.24,-0.235,-0.23,-0.225,-0.22,
-0.215,-0.21,-0.205,-0.2,-0.195,-0.19,-0.185,-0.18,-0.175,-0.17,-0.165,
-0.16,-0.155,-0.15,-0.145,-0.14,-0.135,-0.13,-0.125,-0.12,-0.115,-0.11,
-0.105,-0.1,-0.095,-0.09,-0.085,-0.08,-0.075,-0.07,-0.065,-0.06,-0.055,
-0.05,-0.045,-0.04,-0.035,-0.03,-0.025,-0.02,-0.015,-0.01,-0.005,0.),
 .UNSPECIFIED.)
CURVE()
GEOMETRIC_REPRESENTATION_ITEM()
RATIONAL_B_SPLINE_CURVE((1.,1.,1.,1.,1.,1.,1.,1.,1.,1.,1.,1.,1.,1.,1.,1.,
1.,1.,1.,1.,1.,1.,1.,1.,1.,1.,1.,1.,1.,1.,1.,1.,1.,1.,1.,1.,1.,1.,1.,1.,
1.,1.,1.,1.,1.,1.,1.,1.,1.,1.,1.,1.,1.,1.,1.,1.,1.,1.,1.,1.,1.,1.,1.,1.,
1.,1.,1.,1.,1.,1.,1.,1.,1.,1.,1.,1.,1.,1.,1.,1.,1.,1.,1.,1.,1.,1.,1.,1.,
1.,1.,1.,1.,1.,1.,1.,1.,1.,1.,1.,1.,1.,1.,1.,1.,1.,1.,1.,1.,1.,1.,1.,1.,
1.,1.,1.,1.,1.,1.,1.,1.,1.,1.,1.,1.,1.,1.,1.,1.,1.,1.,1.,1.,1.,1.,1.,1.,
1.,1.,1.,1.,1.,1.,1.,1.,1.,1.,1.,1.,1.,1.,1.,1.,1.,1.,1.,1.,1.,1.,1.,1.,
1.,1.,1.,1.,1.,1.,1.,1.,1.,1.,1.,1.,1.,1.,1.,1.,1.,1.,1.,1.,1.,1.,1.,1.,
1.,1.,1.,1.,1.,1.,1.,1.,1.,1.,1.,1.,1.,1.,1.,1.,1.,1.,1.,1.,1.))
REPRESENTATION_ITEM('')
);
#733=(
BOUNDED_CURVE()
B_SPLINE_CURVE(5,(#183917,#183918,#183919,#183920,#183921,#183922,#183923,
#183924,#183925,#183926,#183927,#183928,#183929,#183930,#183931,#183932,
#183933,#183934,#183935,#183936,#183937,#183938,#183939,#183940,#183941,
#183942,#183943,#183944,#183945,#183946,#183947,#183948,#183949,#183950,
#183951,#183952,#183953,#183954,#183955,#183956,#183957,#183958,#183959,
#183960,#183961,#183962,#183963,#183964,#183965,#183966,#183967,#183968,
#183969,#183970,#183971,#183972,#183973,#183974,#183975,#183976,#183977,
#183978,#183979,#183980,#183981,#183982,#183983,#183984,#183985,#183986,
#183987,#183988,#183989,#183990,#183991,#183992,#183993,#183994,#183995,
#183996,#183997,#183998,#183999,#184000,#184001,#184002,#184003,#184004,
#184005,#184006,#184007,#184008,#184009,#184010,#184011,#184012,#184013,
#184014,#184015,#184016,#184017,#184018,#184019,#184020,#184021,#184022,
#184023,#184024,#184025,#184026,#184027,#184028,#184029,#184030,#184031,
#184032,#184033,#184034,#184035,#184036,#184037,#184038,#184039,#184040,
#184041,#184042,#184043,#184044,#184045,#184046,#184047,#184048,#184049,
#184050,#184051,#184052,#184053,#184054,#184055,#184056,#184057,#184058,
#184059,#184060,#184061,#184062,#184063,#184064,#184065,#184066,#184067,
#184068,#184069,#184070,#184071,#184072,#184073,#184074,#184075,#184076,
#184077,#184078,#184079,#184080,#184081,#184082,#184083,#184084,#184085,
#184086,#184087,#184088,#184089,#184090,#184091,#184092,#184093,#184094,
#184095,#184096,#184097,#184098,#184099,#184100,#184101,#184102,#184103,
#184104,#184105,#184106,#184107,#184108,#184109,#184110,#184111,#184112,
#184113,#184114,#184115,#184116,#184117,#184118,#184119,#184120,#184121),
 .UNSPECIFIED.,.F.,.F.)
B_SPLINE_CURVE_WITH_KNOTS((6,1,1,1,1,1,1,1,1,1,1,1,1,1,1,1,1,1,1,1,1,1,
1,1,1,1,1,1,1,1,1,1,1,1,1,1,1,1,1,1,1,1,1,1,1,1,1,1,1,1,1,1,1,1,1,1,1,1,
1,1,1,1,1,1,1,1,1,1,1,1,1,1,1,1,1,1,1,1,1,1,1,1,1,1,1,1,1,1,1,1,1,1,1,1,
1,1,1,1,1,1,1,1,1,1,1,1,1,1,1,1,1,1,1,1,1,1,1,1,1,1,1,1,1,1,1,1,1,1,1,1,
1,1,1,1,1,1,1,1,1,1,1,1,1,1,1,1,1,1,1,1,1,1,1,1,1,1,1,1,1,1,1,1,1,1,1,1,
1,1,1,1,1,1,1,1,1,1,1,1,1,1,1,1,1,1,1,1,1,1,1,1,1,1,1,1,1,1,1,1,1,1,6),
(0.,0.005,0.01,0.015,0.02,0.025,0.03,0.035,0.04,0.045,0.05,0.055,0.06,0.065,
0.07,0.075,0.08,0.085,0.09,0.095,0.1,0.105,0.11,0.115,0.12,0.125,0.13,0.135,
0.14,0.145,0.15,0.155,0.16,0.165,0.17,0.175,0.18,0.185,0.19,0.195,0.2,0.205,
0.21,0.215,0.22,0.225,0.23,0.235,0.24,0.245,0.25,0.255,0.26,0.265,0.27,
0.275,0.28,0.285,0.29,0.295,0.3,0.305,0.31,0.315,0.32,0.325,0.33,0.335,
0.34,0.345,0.35,0.355,0.36,0.365,0.37,0.375,0.38,0.385,0.39,0.395,0.4,0.405,
0.41,0.415,0.42,0.425,0.43,0.435,0.44,0.445,0.45,0.455,0.46,0.465,0.47,
0.475,0.48,0.485,0.49,0.495,0.5,0.505,0.51,0.515,0.52,0.525,0.53,0.535,
0.54,0.545,0.55,0.555,0.56,0.565,0.57,0.575,0.58,0.585,0.59,0.595,0.6,0.605,
0.61,0.615,0.62,0.625,0.63,0.635,0.64,0.645,0.65,0.655,0.66,0.665,0.67,
0.675,0.68,0.685,0.690000000000001,0.695000000000001,0.700000000000001,
0.705000000000001,0.710000000000001,0.715000000000001,0.720000000000001,
0.725000000000001,0.730000000000001,0.735000000000001,0.740000000000001,
0.745000000000001,0.750000000000001,0.755000000000001,0.760000000000001,
0.765000000000001,0.770000000000001,0.775000000000001,0.780000000000001,
0.785000000000001,0.790000000000001,0.795000000000001,0.800000000000001,
0.805000000000001,0.810000000000001,0.815000000000001,0.820000000000001,
0.825000000000001,0.830000000000001,0.835000000000001,0.840000000000001,
0.845000000000001,0.850000000000001,0.855000000000001,0.860000000000001,
0.865000000000001,0.870000000000001,0.875000000000001,0.880000000000001,
0.885000000000001,0.890000000000001,0.895000000000001,0.900000000000001,
0.905000000000001,0.910000000000001,0.915000000000001,0.920000000000001,
0.925000000000001,0.930000000000001,0.935000000000001,0.940000000000001,
0.945000000000001,0.950000000000001,0.955000000000001,0.960000000000001,
0.965000000000001,0.970000000000001,0.975000000000001,0.980000000000001,
0.985000000000001,0.990000000000001,0.995000000000001,1.),.UNSPECIFIED.)
CURVE()
GEOMETRIC_REPRESENTATION_ITEM()
RATIONAL_B_SPLINE_CURVE((1.,1.,1.,1.,1.,1.,1.,1.,1.,1.,1.,1.,1.,1.,1.,1.,
1.,1.,1.,1.,1.,1.,1.,1.,1.,1.,1.,1.,1.,1.,1.,1.,1.,1.,1.,1.,1.,1.,1.,1.,
1.,1.,1.,1.,1.,1.,1.,1.,1.,1.,1.,1.,1.,1.,1.,1.,1.,1.,1.,1.,1.,1.,1.,1.,
1.,1.,1.,1.,1.,1.,1.,1.,1.,1.,1.,1.,1.,1.,1.,1.,1.,1.,1.,1.,1.,1.,1.,1.,
1.,1.,1.,1.,1.,1.,1.,1.,1.,1.,1.,1.,1.,1.,1.,1.,1.,1.,1.,1.,1.,1.,1.,1.,
1.,1.,1.,1.,1.,1.,1.,1.,1.,1.,1.,1.,1.,1.,1.,1.,1.,1.,1.,1.,1.,1.,1.,1.,
1.,1.,1.,1.,1.,1.,1.,1.,1.,1.,1.,1.,1.,1.,1.,1.,1.,1.,1.,1.,1.,1.,1.,1.,
1.,1.,1.,1.,1.,1.,1.,1.,1.,1.,1.,1.,1.,1.,1.,1.,1.,1.,1.,1.,1.,1.,1.,1.,
1.,1.,1.,1.,1.,1.,1.,1.,1.,1.,1.,1.,1.,1.,1.,1.,1.,1.,1.,1.,1.))
REPRESENTATION_ITEM('')
);
#734=(
BOUNDED_CURVE()
B_SPLINE_CURVE(5,(#184125,#184126,#184127,#184128,#184129,#184130,#184131,
#184132,#184133,#184134,#184135,#184136,#184137,#184138,#184139,#184140,
#184141,#184142,#184143,#184144,#184145,#184146,#184147,#184148,#184149,
#184150,#184151,#184152,#184153,#184154,#184155,#184156,#184157,#184158,
#184159,#184160,#184161,#184162,#184163,#184164,#184165,#184166,#184167,
#184168,#184169,#184170,#184171,#184172,#184173,#184174,#184175,#184176,
#184177,#184178,#184179,#184180,#184181,#184182,#184183,#184184,#184185,
#184186,#184187,#184188,#184189,#184190,#184191,#184192,#184193,#184194,
#184195,#184196,#184197,#184198,#184199,#184200,#184201,#184202,#184203,
#184204,#184205,#184206,#184207,#184208,#184209,#184210,#184211,#184212,
#184213,#184214,#184215,#184216,#184217,#184218,#184219,#184220,#184221,
#184222,#184223,#184224,#184225,#184226,#184227,#184228,#184229,#184230,
#184231,#184232,#184233,#184234,#184235,#184236,#184237,#184238,#184239,
#184240,#184241,#184242,#184243,#184244,#184245,#184246,#184247,#184248,
#184249,#184250,#184251,#184252,#184253,#184254,#184255,#184256,#184257,
#184258,#184259,#184260,#184261,#184262,#184263,#184264,#184265,#184266,
#184267,#184268,#184269,#184270,#184271,#184272,#184273,#184274,#184275,
#184276,#184277,#184278,#184279,#184280,#184281,#184282,#184283,#184284,
#184285,#184286,#184287,#184288,#184289,#184290,#184291,#184292,#184293,
#184294,#184295,#184296,#184297,#184298,#184299,#184300,#184301,#184302,
#184303,#184304,#184305,#184306,#184307,#184308,#184309,#184310,#184311,
#184312,#184313,#184314,#184315,#184316,#184317,#184318,#184319,#184320,
#184321,#184322,#184323,#184324,#184325,#184326,#184327,#184328,#184329),
 .UNSPECIFIED.,.F.,.F.)
B_SPLINE_CURVE_WITH_KNOTS((6,1,1,1,1,1,1,1,1,1,1,1,1,1,1,1,1,1,1,1,1,1,
1,1,1,1,1,1,1,1,1,1,1,1,1,1,1,1,1,1,1,1,1,1,1,1,1,1,1,1,1,1,1,1,1,1,1,1,
1,1,1,1,1,1,1,1,1,1,1,1,1,1,1,1,1,1,1,1,1,1,1,1,1,1,1,1,1,1,1,1,1,1,1,1,
1,1,1,1,1,1,1,1,1,1,1,1,1,1,1,1,1,1,1,1,1,1,1,1,1,1,1,1,1,1,1,1,1,1,1,1,
1,1,1,1,1,1,1,1,1,1,1,1,1,1,1,1,1,1,1,1,1,1,1,1,1,1,1,1,1,1,1,1,1,1,1,1,
1,1,1,1,1,1,1,1,1,1,1,1,1,1,1,1,1,1,1,1,1,1,1,1,1,1,1,1,1,1,1,1,1,1,6),
(-1.,-0.995000000000001,-0.990000000000001,-0.985000000000001,-0.980000000000001,
-0.975000000000001,-0.970000000000001,-0.965000000000001,-0.960000000000001,
-0.955000000000001,-0.950000000000001,-0.945000000000001,-0.940000000000001,
-0.935000000000001,-0.930000000000001,-0.925000000000001,-0.920000000000001,
-0.915000000000001,-0.910000000000001,-0.905000000000001,-0.900000000000001,
-0.895000000000001,-0.890000000000001,-0.885000000000001,-0.880000000000001,
-0.875000000000001,-0.870000000000001,-0.865000000000001,-0.860000000000001,
-0.855000000000001,-0.850000000000001,-0.845000000000001,-0.840000000000001,
-0.835000000000001,-0.830000000000001,-0.825000000000001,-0.820000000000001,
-0.815000000000001,-0.810000000000001,-0.805000000000001,-0.800000000000001,
-0.795000000000001,-0.790000000000001,-0.785000000000001,-0.780000000000001,
-0.775000000000001,-0.770000000000001,-0.765000000000001,-0.760000000000001,
-0.755000000000001,-0.750000000000001,-0.745000000000001,-0.740000000000001,
-0.735000000000001,-0.730000000000001,-0.725000000000001,-0.720000000000001,
-0.715000000000001,-0.710000000000001,-0.705000000000001,-0.700000000000001,
-0.695000000000001,-0.690000000000001,-0.685,-0.68,-0.675,-0.67,-0.665,
-0.66,-0.655,-0.65,-0.645,-0.64,-0.635,-0.63,-0.625,-0.62,-0.615,-0.61,
-0.605,-0.6,-0.595,-0.59,-0.585,-0.58,-0.575,-0.57,-0.565,-0.56,-0.555,
-0.55,-0.545,-0.54,-0.535,-0.53,-0.525,-0.52,-0.515,-0.51,-0.505,-0.5,-0.495,
-0.49,-0.485,-0.48,-0.475,-0.47,-0.465,-0.46,-0.455,-0.45,-0.445,-0.44,
-0.435,-0.43,-0.425,-0.42,-0.415,-0.41,-0.405,-0.4,-0.395,-0.39,-0.385,
-0.38,-0.375,-0.37,-0.365,-0.36,-0.355,-0.35,-0.345,-0.34,-0.335,-0.33,
-0.325,-0.32,-0.315,-0.31,-0.305,-0.3,-0.295,-0.29,-0.285,-0.28,-0.275,
-0.27,-0.265,-0.26,-0.255,-0.25,-0.245,-0.24,-0.235,-0.23,-0.225,-0.22,
-0.215,-0.21,-0.205,-0.2,-0.195,-0.19,-0.185,-0.18,-0.175,-0.17,-0.165,
-0.16,-0.155,-0.15,-0.145,-0.14,-0.135,-0.13,-0.125,-0.12,-0.115,-0.11,
-0.105,-0.1,-0.095,-0.09,-0.085,-0.08,-0.075,-0.07,-0.065,-0.06,-0.055,
-0.05,-0.045,-0.04,-0.035,-0.03,-0.025,-0.02,-0.015,-0.01,-0.005,0.),
 .UNSPECIFIED.)
CURVE()
GEOMETRIC_REPRESENTATION_ITEM()
RATIONAL_B_SPLINE_CURVE((1.,1.,1.,1.,1.,1.,1.,1.,1.,1.,1.,1.,1.,1.,1.,1.,
1.,1.,1.,1.,1.,1.,1.,1.,1.,1.,1.,1.,1.,1.,1.,1.,1.,1.,1.,1.,1.,1.,1.,1.,
1.,1.,1.,1.,1.,1.,1.,1.,1.,1.,1.,1.,1.,1.,1.,1.,1.,1.,1.,1.,1.,1.,1.,1.,
1.,1.,1.,1.,1.,1.,1.,1.,1.,1.,1.,1.,1.,1.,1.,1.,1.,1.,1.,1.,1.,1.,1.,1.,
1.,1.,1.,1.,1.,1.,1.,1.,1.,1.,1.,1.,1.,1.,1.,1.,1.,1.,1.,1.,1.,1.,1.,1.,
1.,1.,1.,1.,1.,1.,1.,1.,1.,1.,1.,1.,1.,1.,1.,1.,1.,1.,1.,1.,1.,1.,1.,1.,
1.,1.,1.,1.,1.,1.,1.,1.,1.,1.,1.,1.,1.,1.,1.,1.,1.,1.,1.,1.,1.,1.,1.,1.,
1.,1.,1.,1.,1.,1.,1.,1.,1.,1.,1.,1.,1.,1.,1.,1.,1.,1.,1.,1.,1.,1.,1.,1.,
1.,1.,1.,1.,1.,1.,1.,1.,1.,1.,1.,1.,1.,1.,1.,1.,1.,1.,1.,1.,1.))
REPRESENTATION_ITEM('')
);
#735=(
BOUNDED_CURVE()
B_SPLINE_CURVE(5,(#184341,#184342,#184343,#184344,#184345,#184346,#184347,
#184348,#184349,#184350,#184351,#184352,#184353,#184354,#184355,#184356,
#184357,#184358,#184359,#184360,#184361,#184362,#184363,#184364,#184365,
#184366,#184367,#184368,#184369,#184370,#184371,#184372,#184373,#184374,
#184375,#184376,#184377,#184378,#184379,#184380,#184381,#184382,#184383,
#184384,#184385,#184386,#184387,#184388,#184389,#184390,#184391,#184392,
#184393,#184394,#184395,#184396,#184397,#184398,#184399,#184400,#184401,
#184402,#184403,#184404,#184405,#184406,#184407,#184408,#184409,#184410,
#184411,#184412,#184413,#184414,#184415,#184416,#184417,#184418,#184419,
#184420,#184421,#184422,#184423,#184424,#184425,#184426,#184427,#184428,
#184429,#184430,#184431,#184432,#184433,#184434,#184435,#184436,#184437,
#184438,#184439,#184440,#184441,#184442,#184443,#184444,#184445,#184446,
#184447,#184448,#184449,#184450,#184451,#184452,#184453,#184454,#184455,
#184456,#184457,#184458,#184459,#184460,#184461,#184462,#184463,#184464,
#184465,#184466,#184467,#184468,#184469,#184470,#184471,#184472,#184473,
#184474,#184475,#184476,#184477,#184478,#184479,#184480,#184481,#184482,
#184483,#184484,#184485,#184486,#184487,#184488,#184489,#184490,#184491,
#184492,#184493,#184494,#184495,#184496,#184497,#184498,#184499,#184500,
#184501,#184502,#184503,#184504,#184505,#184506,#184507,#184508,#184509,
#184510,#184511,#184512,#184513,#184514,#184515,#184516,#184517,#184518,
#184519,#184520,#184521,#184522,#184523,#184524,#184525,#184526,#184527,
#184528,#184529,#184530,#184531,#184532,#184533,#184534,#184535,#184536,
#184537,#184538,#184539,#184540,#184541,#184542,#184543,#184544,#184545),
 .UNSPECIFIED.,.F.,.F.)
B_SPLINE_CURVE_WITH_KNOTS((6,1,1,1,1,1,1,1,1,1,1,1,1,1,1,1,1,1,1,1,1,1,
1,1,1,1,1,1,1,1,1,1,1,1,1,1,1,1,1,1,1,1,1,1,1,1,1,1,1,1,1,1,1,1,1,1,1,1,
1,1,1,1,1,1,1,1,1,1,1,1,1,1,1,1,1,1,1,1,1,1,1,1,1,1,1,1,1,1,1,1,1,1,1,1,
1,1,1,1,1,1,1,1,1,1,1,1,1,1,1,1,1,1,1,1,1,1,1,1,1,1,1,1,1,1,1,1,1,1,1,1,
1,1,1,1,1,1,1,1,1,1,1,1,1,1,1,1,1,1,1,1,1,1,1,1,1,1,1,1,1,1,1,1,1,1,1,1,
1,1,1,1,1,1,1,1,1,1,1,1,1,1,1,1,1,1,1,1,1,1,1,1,1,1,1,1,1,1,1,1,1,1,6),
(0.,0.005,0.01,0.015,0.02,0.025,0.03,0.035,0.04,0.045,0.05,0.055,0.06,0.065,
0.07,0.075,0.08,0.085,0.09,0.095,0.1,0.105,0.11,0.115,0.12,0.125,0.13,0.135,
0.14,0.145,0.15,0.155,0.16,0.165,0.17,0.175,0.18,0.185,0.19,0.195,0.2,0.205,
0.21,0.215,0.22,0.225,0.23,0.235,0.24,0.245,0.25,0.255,0.26,0.265,0.27,
0.275,0.28,0.285,0.29,0.295,0.3,0.305,0.31,0.315,0.32,0.325,0.33,0.335,
0.34,0.345,0.35,0.355,0.36,0.365,0.37,0.375,0.38,0.385,0.39,0.395,0.4,0.405,
0.41,0.415,0.42,0.425,0.43,0.435,0.44,0.445,0.45,0.455,0.46,0.465,0.47,
0.475,0.48,0.485,0.49,0.495,0.5,0.505,0.51,0.515,0.52,0.525,0.53,0.535,
0.54,0.545,0.55,0.555,0.56,0.565,0.57,0.575,0.58,0.585,0.59,0.595,0.6,0.605,
0.61,0.615,0.62,0.625,0.63,0.635,0.64,0.645,0.65,0.655,0.66,0.665,0.67,
0.675,0.68,0.685,0.690000000000001,0.695000000000001,0.700000000000001,
0.705000000000001,0.710000000000001,0.715000000000001,0.720000000000001,
0.725000000000001,0.730000000000001,0.735000000000001,0.740000000000001,
0.745000000000001,0.750000000000001,0.755000000000001,0.760000000000001,
0.765000000000001,0.770000000000001,0.775000000000001,0.780000000000001,
0.785000000000001,0.790000000000001,0.795000000000001,0.800000000000001,
0.805000000000001,0.810000000000001,0.815000000000001,0.820000000000001,
0.825000000000001,0.830000000000001,0.835000000000001,0.840000000000001,
0.845000000000001,0.850000000000001,0.855000000000001,0.860000000000001,
0.865000000000001,0.870000000000001,0.875000000000001,0.880000000000001,
0.885000000000001,0.890000000000001,0.895000000000001,0.900000000000001,
0.905000000000001,0.910000000000001,0.915000000000001,0.920000000000001,
0.925000000000001,0.930000000000001,0.935000000000001,0.940000000000001,
0.945000000000001,0.950000000000001,0.955000000000001,0.960000000000001,
0.965000000000001,0.970000000000001,0.975000000000001,0.980000000000001,
0.985000000000001,0.990000000000001,0.995000000000001,1.),.UNSPECIFIED.)
CURVE()
GEOMETRIC_REPRESENTATION_ITEM()
RATIONAL_B_SPLINE_CURVE((1.,1.,1.,1.,1.,1.,1.,1.,1.,1.,1.,1.,1.,1.,1.,1.,
1.,1.,1.,1.,1.,1.,1.,1.,1.,1.,1.,1.,1.,1.,1.,1.,1.,1.,1.,1.,1.,1.,1.,1.,
1.,1.,1.,1.,1.,1.,1.,1.,1.,1.,1.,1.,1.,1.,1.,1.,1.,1.,1.,1.,1.,1.,1.,1.,
1.,1.,1.,1.,1.,1.,1.,1.,1.,1.,1.,1.,1.,1.,1.,1.,1.,1.,1.,1.,1.,1.,1.,1.,
1.,1.,1.,1.,1.,1.,1.,1.,1.,1.,1.,1.,1.,1.,1.,1.,1.,1.,1.,1.,1.,1.,1.,1.,
1.,1.,1.,1.,1.,1.,1.,1.,1.,1.,1.,1.,1.,1.,1.,1.,1.,1.,1.,1.,1.,1.,1.,1.,
1.,1.,1.,1.,1.,1.,1.,1.,1.,1.,1.,1.,1.,1.,1.,1.,1.,1.,1.,1.,1.,1.,1.,1.,
1.,1.,1.,1.,1.,1.,1.,1.,1.,1.,1.,1.,1.,1.,1.,1.,1.,1.,1.,1.,1.,1.,1.,1.,
1.,1.,1.,1.,1.,1.,1.,1.,1.,1.,1.,1.,1.,1.,1.,1.,1.,1.,1.,1.,1.))
REPRESENTATION_ITEM('')
);
#736=(
BOUNDED_CURVE()
B_SPLINE_CURVE(5,(#184549,#184550,#184551,#184552,#184553,#184554,#184555,
#184556,#184557,#184558,#184559,#184560,#184561,#184562,#184563,#184564,
#184565,#184566,#184567,#184568,#184569,#184570,#184571,#184572,#184573,
#184574,#184575,#184576,#184577,#184578,#184579,#184580,#184581,#184582,
#184583,#184584,#184585,#184586,#184587,#184588,#184589,#184590,#184591,
#184592,#184593,#184594,#184595,#184596,#184597,#184598,#184599,#184600,
#184601,#184602,#184603,#184604,#184605,#184606,#184607,#184608,#184609,
#184610,#184611,#184612,#184613,#184614,#184615,#184616,#184617,#184618,
#184619,#184620,#184621,#184622,#184623,#184624,#184625,#184626,#184627,
#184628,#184629,#184630,#184631,#184632,#184633,#184634,#184635,#184636,
#184637,#184638,#184639,#184640,#184641,#184642,#184643,#184644,#184645,
#184646,#184647,#184648,#184649,#184650,#184651,#184652,#184653,#184654,
#184655,#184656,#184657,#184658,#184659,#184660,#184661,#184662,#184663,
#184664,#184665,#184666,#184667,#184668,#184669,#184670,#184671,#184672,
#184673,#184674,#184675,#184676,#184677,#184678,#184679,#184680,#184681,
#184682,#184683,#184684,#184685,#184686,#184687,#184688,#184689,#184690,
#184691,#184692,#184693,#184694,#184695,#184696,#184697,#184698,#184699,
#184700,#184701,#184702,#184703,#184704,#184705,#184706,#184707,#184708,
#184709,#184710,#184711,#184712,#184713,#184714,#184715,#184716,#184717,
#184718,#184719,#184720,#184721,#184722,#184723,#184724,#184725,#184726,
#184727,#184728,#184729,#184730,#184731,#184732,#184733,#184734,#184735,
#184736,#184737,#184738,#184739,#184740,#184741,#184742,#184743,#184744,
#184745,#184746,#184747,#184748,#184749,#184750,#184751,#184752,#184753),
 .UNSPECIFIED.,.F.,.F.)
B_SPLINE_CURVE_WITH_KNOTS((6,1,1,1,1,1,1,1,1,1,1,1,1,1,1,1,1,1,1,1,1,1,
1,1,1,1,1,1,1,1,1,1,1,1,1,1,1,1,1,1,1,1,1,1,1,1,1,1,1,1,1,1,1,1,1,1,1,1,
1,1,1,1,1,1,1,1,1,1,1,1,1,1,1,1,1,1,1,1,1,1,1,1,1,1,1,1,1,1,1,1,1,1,1,1,
1,1,1,1,1,1,1,1,1,1,1,1,1,1,1,1,1,1,1,1,1,1,1,1,1,1,1,1,1,1,1,1,1,1,1,1,
1,1,1,1,1,1,1,1,1,1,1,1,1,1,1,1,1,1,1,1,1,1,1,1,1,1,1,1,1,1,1,1,1,1,1,1,
1,1,1,1,1,1,1,1,1,1,1,1,1,1,1,1,1,1,1,1,1,1,1,1,1,1,1,1,1,1,1,1,1,1,6),
(-1.,-0.995000000000001,-0.990000000000001,-0.985000000000001,-0.980000000000001,
-0.975000000000001,-0.970000000000001,-0.965000000000001,-0.960000000000001,
-0.955000000000001,-0.950000000000001,-0.945000000000001,-0.940000000000001,
-0.935000000000001,-0.930000000000001,-0.925000000000001,-0.920000000000001,
-0.915000000000001,-0.910000000000001,-0.905000000000001,-0.900000000000001,
-0.895000000000001,-0.890000000000001,-0.885000000000001,-0.880000000000001,
-0.875000000000001,-0.870000000000001,-0.865000000000001,-0.860000000000001,
-0.855000000000001,-0.850000000000001,-0.845000000000001,-0.840000000000001,
-0.835000000000001,-0.830000000000001,-0.825000000000001,-0.820000000000001,
-0.815000000000001,-0.810000000000001,-0.805000000000001,-0.800000000000001,
-0.795000000000001,-0.790000000000001,-0.785000000000001,-0.780000000000001,
-0.775000000000001,-0.770000000000001,-0.765000000000001,-0.760000000000001,
-0.755000000000001,-0.750000000000001,-0.745000000000001,-0.740000000000001,
-0.735000000000001,-0.730000000000001,-0.725000000000001,-0.720000000000001,
-0.715000000000001,-0.710000000000001,-0.705000000000001,-0.700000000000001,
-0.695000000000001,-0.690000000000001,-0.685,-0.68,-0.675,-0.67,-0.665,
-0.66,-0.655,-0.65,-0.645,-0.64,-0.635,-0.63,-0.625,-0.62,-0.615,-0.61,
-0.605,-0.6,-0.595,-0.59,-0.585,-0.58,-0.575,-0.57,-0.565,-0.56,-0.555,
-0.55,-0.545,-0.54,-0.535,-0.53,-0.525,-0.52,-0.515,-0.51,-0.505,-0.5,-0.495,
-0.49,-0.485,-0.48,-0.475,-0.47,-0.465,-0.46,-0.455,-0.45,-0.445,-0.44,
-0.435,-0.43,-0.425,-0.42,-0.415,-0.41,-0.405,-0.4,-0.395,-0.39,-0.385,
-0.38,-0.375,-0.37,-0.365,-0.36,-0.355,-0.35,-0.345,-0.34,-0.335,-0.33,
-0.325,-0.32,-0.315,-0.31,-0.305,-0.3,-0.295,-0.29,-0.285,-0.28,-0.275,
-0.27,-0.265,-0.26,-0.255,-0.25,-0.245,-0.24,-0.235,-0.23,-0.225,-0.22,
-0.215,-0.21,-0.205,-0.2,-0.195,-0.19,-0.185,-0.18,-0.175,-0.17,-0.165,
-0.16,-0.155,-0.15,-0.145,-0.14,-0.135,-0.13,-0.125,-0.12,-0.115,-0.11,
-0.105,-0.1,-0.095,-0.09,-0.085,-0.08,-0.075,-0.07,-0.065,-0.06,-0.055,
-0.05,-0.045,-0.04,-0.035,-0.03,-0.025,-0.02,-0.015,-0.01,-0.005,0.),
 .UNSPECIFIED.)
CURVE()
GEOMETRIC_REPRESENTATION_ITEM()
RATIONAL_B_SPLINE_CURVE((1.,1.,1.,1.,1.,1.,1.,1.,1.,1.,1.,1.,1.,1.,1.,1.,
1.,1.,1.,1.,1.,1.,1.,1.,1.,1.,1.,1.,1.,1.,1.,1.,1.,1.,1.,1.,1.,1.,1.,1.,
1.,1.,1.,1.,1.,1.,1.,1.,1.,1.,1.,1.,1.,1.,1.,1.,1.,1.,1.,1.,1.,1.,1.,1.,
1.,1.,1.,1.,1.,1.,1.,1.,1.,1.,1.,1.,1.,1.,1.,1.,1.,1.,1.,1.,1.,1.,1.,1.,
1.,1.,1.,1.,1.,1.,1.,1.,1.,1.,1.,1.,1.,1.,1.,1.,1.,1.,1.,1.,1.,1.,1.,1.,
1.,1.,1.,1.,1.,1.,1.,1.,1.,1.,1.,1.,1.,1.,1.,1.,1.,1.,1.,1.,1.,1.,1.,1.,
1.,1.,1.,1.,1.,1.,1.,1.,1.,1.,1.,1.,1.,1.,1.,1.,1.,1.,1.,1.,1.,1.,1.,1.,
1.,1.,1.,1.,1.,1.,1.,1.,1.,1.,1.,1.,1.,1.,1.,1.,1.,1.,1.,1.,1.,1.,1.,1.,
1.,1.,1.,1.,1.,1.,1.,1.,1.,1.,1.,1.,1.,1.,1.,1.,1.,1.,1.,1.,1.))
REPRESENTATION_ITEM('')
);
#737=(
BOUNDED_CURVE()
B_SPLINE_CURVE(5,(#184765,#184766,#184767,#184768,#184769,#184770,#184771,
#184772,#184773,#184774,#184775,#184776,#184777,#184778,#184779,#184780,
#184781,#184782,#184783,#184784,#184785,#184786,#184787,#184788,#184789,
#184790,#184791,#184792,#184793,#184794,#184795,#184796,#184797,#184798,
#184799,#184800,#184801,#184802,#184803,#184804,#184805,#184806,#184807,
#184808,#184809,#184810,#184811,#184812,#184813,#184814,#184815,#184816,
#184817,#184818,#184819,#184820,#184821,#184822,#184823,#184824,#184825,
#184826,#184827,#184828,#184829,#184830,#184831,#184832,#184833,#184834,
#184835,#184836,#184837,#184838,#184839,#184840,#184841,#184842,#184843,
#184844,#184845,#184846,#184847,#184848,#184849,#184850,#184851,#184852,
#184853,#184854,#184855,#184856,#184857,#184858,#184859,#184860,#184861,
#184862,#184863,#184864,#184865,#184866,#184867,#184868,#184869,#184870,
#184871,#184872,#184873,#184874,#184875,#184876,#184877,#184878,#184879,
#184880,#184881,#184882,#184883,#184884,#184885,#184886,#184887,#184888,
#184889,#184890,#184891,#184892,#184893,#184894,#184895,#184896,#184897,
#184898,#184899,#184900,#184901,#184902,#184903,#184904,#184905,#184906,
#184907,#184908,#184909,#184910,#184911,#184912,#184913,#184914,#184915,
#184916,#184917,#184918,#184919,#184920,#184921,#184922,#184923,#184924,
#184925,#184926,#184927,#184928,#184929,#184930,#184931,#184932,#184933,
#184934,#184935,#184936,#184937,#184938,#184939,#184940,#184941,#184942,
#184943,#184944,#184945,#184946,#184947,#184948,#184949,#184950,#184951,
#184952,#184953,#184954,#184955,#184956,#184957,#184958,#184959,#184960,
#184961,#184962,#184963,#184964,#184965,#184966,#184967,#184968,#184969),
 .UNSPECIFIED.,.F.,.F.)
B_SPLINE_CURVE_WITH_KNOTS((6,1,1,1,1,1,1,1,1,1,1,1,1,1,1,1,1,1,1,1,1,1,
1,1,1,1,1,1,1,1,1,1,1,1,1,1,1,1,1,1,1,1,1,1,1,1,1,1,1,1,1,1,1,1,1,1,1,1,
1,1,1,1,1,1,1,1,1,1,1,1,1,1,1,1,1,1,1,1,1,1,1,1,1,1,1,1,1,1,1,1,1,1,1,1,
1,1,1,1,1,1,1,1,1,1,1,1,1,1,1,1,1,1,1,1,1,1,1,1,1,1,1,1,1,1,1,1,1,1,1,1,
1,1,1,1,1,1,1,1,1,1,1,1,1,1,1,1,1,1,1,1,1,1,1,1,1,1,1,1,1,1,1,1,1,1,1,1,
1,1,1,1,1,1,1,1,1,1,1,1,1,1,1,1,1,1,1,1,1,1,1,1,1,1,1,1,1,1,1,1,1,1,6),
(0.,0.005,0.01,0.015,0.02,0.025,0.03,0.035,0.04,0.045,0.05,0.055,0.06,0.065,
0.07,0.075,0.08,0.085,0.09,0.095,0.1,0.105,0.11,0.115,0.12,0.125,0.13,0.135,
0.14,0.145,0.15,0.155,0.16,0.165,0.17,0.175,0.18,0.185,0.19,0.195,0.2,0.205,
0.21,0.215,0.22,0.225,0.23,0.235,0.24,0.245,0.25,0.255,0.26,0.265,0.27,
0.275,0.28,0.285,0.29,0.295,0.3,0.305,0.31,0.315,0.32,0.325,0.33,0.335,
0.34,0.345,0.35,0.355,0.36,0.365,0.37,0.375,0.38,0.385,0.39,0.395,0.4,0.405,
0.41,0.415,0.42,0.425,0.43,0.435,0.44,0.445,0.45,0.455,0.46,0.465,0.47,
0.475,0.48,0.485,0.49,0.495,0.5,0.505,0.51,0.515,0.52,0.525,0.53,0.535,
0.54,0.545,0.55,0.555,0.56,0.565,0.57,0.575,0.58,0.585,0.59,0.595,0.6,0.605,
0.61,0.615,0.62,0.625,0.63,0.635,0.64,0.645,0.65,0.655,0.66,0.665,0.67,
0.675,0.68,0.685,0.690000000000001,0.695000000000001,0.700000000000001,
0.705000000000001,0.710000000000001,0.715000000000001,0.720000000000001,
0.725000000000001,0.730000000000001,0.735000000000001,0.740000000000001,
0.745000000000001,0.750000000000001,0.755000000000001,0.760000000000001,
0.765000000000001,0.770000000000001,0.775000000000001,0.780000000000001,
0.785000000000001,0.790000000000001,0.795000000000001,0.800000000000001,
0.805000000000001,0.810000000000001,0.815000000000001,0.820000000000001,
0.825000000000001,0.830000000000001,0.835000000000001,0.840000000000001,
0.845000000000001,0.850000000000001,0.855000000000001,0.860000000000001,
0.865000000000001,0.870000000000001,0.875000000000001,0.880000000000001,
0.885000000000001,0.890000000000001,0.895000000000001,0.900000000000001,
0.905000000000001,0.910000000000001,0.915000000000001,0.920000000000001,
0.925000000000001,0.930000000000001,0.935000000000001,0.940000000000001,
0.945000000000001,0.950000000000001,0.955000000000001,0.960000000000001,
0.965000000000001,0.970000000000001,0.975000000000001,0.980000000000001,
0.985000000000001,0.990000000000001,0.995000000000001,1.),.UNSPECIFIED.)
CURVE()
GEOMETRIC_REPRESENTATION_ITEM()
RATIONAL_B_SPLINE_CURVE((1.,1.,1.,1.,1.,1.,1.,1.,1.,1.,1.,1.,1.,1.,1.,1.,
1.,1.,1.,1.,1.,1.,1.,1.,1.,1.,1.,1.,1.,1.,1.,1.,1.,1.,1.,1.,1.,1.,1.,1.,
1.,1.,1.,1.,1.,1.,1.,1.,1.,1.,1.,1.,1.,1.,1.,1.,1.,1.,1.,1.,1.,1.,1.,1.,
1.,1.,1.,1.,1.,1.,1.,1.,1.,1.,1.,1.,1.,1.,1.,1.,1.,1.,1.,1.,1.,1.,1.,1.,
1.,1.,1.,1.,1.,1.,1.,1.,1.,1.,1.,1.,1.,1.,1.,1.,1.,1.,1.,1.,1.,1.,1.,1.,
1.,1.,1.,1.,1.,1.,1.,1.,1.,1.,1.,1.,1.,1.,1.,1.,1.,1.,1.,1.,1.,1.,1.,1.,
1.,1.,1.,1.,1.,1.,1.,1.,1.,1.,1.,1.,1.,1.,1.,1.,1.,1.,1.,1.,1.,1.,1.,1.,
1.,1.,1.,1.,1.,1.,1.,1.,1.,1.,1.,1.,1.,1.,1.,1.,1.,1.,1.,1.,1.,1.,1.,1.,
1.,1.,1.,1.,1.,1.,1.,1.,1.,1.,1.,1.,1.,1.,1.,1.,1.,1.,1.,1.,1.))
REPRESENTATION_ITEM('')
);
#738=(
BOUNDED_CURVE()
B_SPLINE_CURVE(5,(#184973,#184974,#184975,#184976,#184977,#184978,#184979,
#184980,#184981,#184982,#184983,#184984,#184985,#184986,#184987,#184988,
#184989,#184990,#184991,#184992,#184993,#184994,#184995,#184996,#184997,
#184998,#184999,#185000,#185001,#185002,#185003,#185004,#185005,#185006,
#185007,#185008,#185009,#185010,#185011,#185012,#185013,#185014,#185015,
#185016,#185017,#185018,#185019,#185020,#185021,#185022,#185023,#185024,
#185025,#185026,#185027,#185028,#185029,#185030,#185031,#185032,#185033,
#185034,#185035,#185036,#185037,#185038,#185039,#185040,#185041,#185042,
#185043,#185044,#185045,#185046,#185047,#185048,#185049,#185050,#185051,
#185052,#185053,#185054,#185055,#185056,#185057,#185058,#185059,#185060,
#185061,#185062,#185063,#185064,#185065,#185066,#185067,#185068,#185069,
#185070,#185071,#185072,#185073,#185074,#185075,#185076,#185077,#185078,
#185079,#185080,#185081,#185082,#185083,#185084,#185085,#185086,#185087,
#185088,#185089,#185090,#185091,#185092,#185093,#185094,#185095,#185096,
#185097,#185098,#185099,#185100,#185101,#185102,#185103,#185104,#185105,
#185106,#185107,#185108,#185109,#185110,#185111,#185112,#185113,#185114,
#185115,#185116,#185117,#185118,#185119,#185120,#185121,#185122,#185123,
#185124,#185125,#185126,#185127,#185128,#185129,#185130,#185131,#185132,
#185133,#185134,#185135,#185136,#185137,#185138,#185139,#185140,#185141,
#185142,#185143,#185144,#185145,#185146,#185147,#185148,#185149,#185150,
#185151,#185152,#185153,#185154,#185155,#185156,#185157,#185158,#185159,
#185160,#185161,#185162,#185163,#185164,#185165,#185166,#185167,#185168,
#185169,#185170,#185171,#185172,#185173,#185174,#185175,#185176,#185177),
 .UNSPECIFIED.,.F.,.F.)
B_SPLINE_CURVE_WITH_KNOTS((6,1,1,1,1,1,1,1,1,1,1,1,1,1,1,1,1,1,1,1,1,1,
1,1,1,1,1,1,1,1,1,1,1,1,1,1,1,1,1,1,1,1,1,1,1,1,1,1,1,1,1,1,1,1,1,1,1,1,
1,1,1,1,1,1,1,1,1,1,1,1,1,1,1,1,1,1,1,1,1,1,1,1,1,1,1,1,1,1,1,1,1,1,1,1,
1,1,1,1,1,1,1,1,1,1,1,1,1,1,1,1,1,1,1,1,1,1,1,1,1,1,1,1,1,1,1,1,1,1,1,1,
1,1,1,1,1,1,1,1,1,1,1,1,1,1,1,1,1,1,1,1,1,1,1,1,1,1,1,1,1,1,1,1,1,1,1,1,
1,1,1,1,1,1,1,1,1,1,1,1,1,1,1,1,1,1,1,1,1,1,1,1,1,1,1,1,1,1,1,1,1,1,6),
(-1.,-0.995000000000001,-0.990000000000001,-0.985000000000001,-0.980000000000001,
-0.975000000000001,-0.970000000000001,-0.965000000000001,-0.960000000000001,
-0.955000000000001,-0.950000000000001,-0.945000000000001,-0.940000000000001,
-0.935000000000001,-0.930000000000001,-0.925000000000001,-0.920000000000001,
-0.915000000000001,-0.910000000000001,-0.905000000000001,-0.900000000000001,
-0.895000000000001,-0.890000000000001,-0.885000000000001,-0.880000000000001,
-0.875000000000001,-0.870000000000001,-0.865000000000001,-0.860000000000001,
-0.855000000000001,-0.850000000000001,-0.845000000000001,-0.840000000000001,
-0.835000000000001,-0.830000000000001,-0.825000000000001,-0.820000000000001,
-0.815000000000001,-0.810000000000001,-0.805000000000001,-0.800000000000001,
-0.795000000000001,-0.790000000000001,-0.785000000000001,-0.780000000000001,
-0.775000000000001,-0.770000000000001,-0.765000000000001,-0.760000000000001,
-0.755000000000001,-0.750000000000001,-0.745000000000001,-0.740000000000001,
-0.735000000000001,-0.730000000000001,-0.725000000000001,-0.720000000000001,
-0.715000000000001,-0.710000000000001,-0.705000000000001,-0.700000000000001,
-0.695000000000001,-0.690000000000001,-0.685,-0.68,-0.675,-0.67,-0.665,
-0.66,-0.655,-0.65,-0.645,-0.64,-0.635,-0.63,-0.625,-0.62,-0.615,-0.61,
-0.605,-0.6,-0.595,-0.59,-0.585,-0.58,-0.575,-0.57,-0.565,-0.56,-0.555,
-0.55,-0.545,-0.54,-0.535,-0.53,-0.525,-0.52,-0.515,-0.51,-0.505,-0.5,-0.495,
-0.49,-0.485,-0.48,-0.475,-0.47,-0.465,-0.46,-0.455,-0.45,-0.445,-0.44,
-0.435,-0.43,-0.425,-0.42,-0.415,-0.41,-0.405,-0.4,-0.395,-0.39,-0.385,
-0.38,-0.375,-0.37,-0.365,-0.36,-0.355,-0.35,-0.345,-0.34,-0.335,-0.33,
-0.325,-0.32,-0.315,-0.31,-0.305,-0.3,-0.295,-0.29,-0.285,-0.28,-0.275,
-0.27,-0.265,-0.26,-0.255,-0.25,-0.245,-0.24,-0.235,-0.23,-0.225,-0.22,
-0.215,-0.21,-0.205,-0.2,-0.195,-0.19,-0.185,-0.18,-0.175,-0.17,-0.165,
-0.16,-0.155,-0.15,-0.145,-0.14,-0.135,-0.13,-0.125,-0.12,-0.115,-0.11,
-0.105,-0.1,-0.095,-0.09,-0.085,-0.08,-0.075,-0.07,-0.065,-0.06,-0.055,
-0.05,-0.045,-0.04,-0.035,-0.03,-0.025,-0.02,-0.015,-0.01,-0.005,0.),
 .UNSPECIFIED.)
CURVE()
GEOMETRIC_REPRESENTATION_ITEM()
RATIONAL_B_SPLINE_CURVE((1.,1.,1.,1.,1.,1.,1.,1.,1.,1.,1.,1.,1.,1.,1.,1.,
1.,1.,1.,1.,1.,1.,1.,1.,1.,1.,1.,1.,1.,1.,1.,1.,1.,1.,1.,1.,1.,1.,1.,1.,
1.,1.,1.,1.,1.,1.,1.,1.,1.,1.,1.,1.,1.,1.,1.,1.,1.,1.,1.,1.,1.,1.,1.,1.,
1.,1.,1.,1.,1.,1.,1.,1.,1.,1.,1.,1.,1.,1.,1.,1.,1.,1.,1.,1.,1.,1.,1.,1.,
1.,1.,1.,1.,1.,1.,1.,1.,1.,1.,1.,1.,1.,1.,1.,1.,1.,1.,1.,1.,1.,1.,1.,1.,
1.,1.,1.,1.,1.,1.,1.,1.,1.,1.,1.,1.,1.,1.,1.,1.,1.,1.,1.,1.,1.,1.,1.,1.,
1.,1.,1.,1.,1.,1.,1.,1.,1.,1.,1.,1.,1.,1.,1.,1.,1.,1.,1.,1.,1.,1.,1.,1.,
1.,1.,1.,1.,1.,1.,1.,1.,1.,1.,1.,1.,1.,1.,1.,1.,1.,1.,1.,1.,1.,1.,1.,1.,
1.,1.,1.,1.,1.,1.,1.,1.,1.,1.,1.,1.,1.,1.,1.,1.,1.,1.,1.,1.,1.))
REPRESENTATION_ITEM('')
);
#739=(
BOUNDED_CURVE()
B_SPLINE_CURVE(5,(#186016,#186017,#186018,#186019,#186020,#186021,#186022,
#186023,#186024,#186025,#186026,#186027,#186028,#186029,#186030,#186031,
#186032,#186033,#186034,#186035,#186036,#186037,#186038,#186039,#186040,
#186041,#186042,#186043,#186044,#186045,#186046,#186047,#186048,#186049,
#186050,#186051,#186052,#186053,#186054,#186055,#186056,#186057,#186058,
#186059,#186060,#186061,#186062,#186063,#186064,#186065,#186066,#186067,
#186068,#186069,#186070,#186071,#186072,#186073,#186074,#186075,#186076,
#186077,#186078,#186079,#186080,#186081,#186082,#186083,#186084,#186085,
#186086,#186087,#186088,#186089,#186090,#186091,#186092,#186093,#186094,
#186095,#186096,#186097,#186098,#186099,#186100,#186101,#186102,#186103,
#186104,#186105,#186106,#186107,#186108,#186109,#186110,#186111,#186112,
#186113,#186114,#186115,#186116,#186117,#186118,#186119,#186120,#186121,
#186122,#186123,#186124,#186125,#186126,#186127,#186128,#186129,#186130,
#186131,#186132,#186133,#186134,#186135,#186136,#186137,#186138,#186139,
#186140,#186141,#186142,#186143,#186144,#186145,#186146,#186147,#186148,
#186149,#186150,#186151,#186152,#186153,#186154,#186155,#186156,#186157,
#186158,#186159,#186160,#186161,#186162,#186163,#186164,#186165,#186166,
#186167,#186168,#186169,#186170,#186171,#186172,#186173,#186174,#186175,
#186176,#186177,#186178,#186179,#186180,#186181,#186182,#186183,#186184,
#186185,#186186,#186187,#186188,#186189,#186190,#186191,#186192,#186193,
#186194,#186195,#186196,#186197,#186198,#186199,#186200,#186201,#186202,
#186203,#186204,#186205,#186206,#186207,#186208,#186209,#186210,#186211,
#186212,#186213,#186214,#186215,#186216,#186217,#186218,#186219,#186220),
 .UNSPECIFIED.,.F.,.F.)
B_SPLINE_CURVE_WITH_KNOTS((6,1,1,1,1,1,1,1,1,1,1,1,1,1,1,1,1,1,1,1,1,1,
1,1,1,1,1,1,1,1,1,1,1,1,1,1,1,1,1,1,1,1,1,1,1,1,1,1,1,1,1,1,1,1,1,1,1,1,
1,1,1,1,1,1,1,1,1,1,1,1,1,1,1,1,1,1,1,1,1,1,1,1,1,1,1,1,1,1,1,1,1,1,1,1,
1,1,1,1,1,1,1,1,1,1,1,1,1,1,1,1,1,1,1,1,1,1,1,1,1,1,1,1,1,1,1,1,1,1,1,1,
1,1,1,1,1,1,1,1,1,1,1,1,1,1,1,1,1,1,1,1,1,1,1,1,1,1,1,1,1,1,1,1,1,1,1,1,
1,1,1,1,1,1,1,1,1,1,1,1,1,1,1,1,1,1,1,1,1,1,1,1,1,1,1,1,1,1,1,1,1,1,6),
(-1.,-0.995000000000001,-0.990000000000001,-0.985000000000001,-0.980000000000001,
-0.975000000000001,-0.970000000000001,-0.965000000000001,-0.960000000000001,
-0.955000000000001,-0.950000000000001,-0.945000000000001,-0.940000000000001,
-0.935000000000001,-0.930000000000001,-0.925000000000001,-0.920000000000001,
-0.915000000000001,-0.910000000000001,-0.905000000000001,-0.900000000000001,
-0.895000000000001,-0.890000000000001,-0.885000000000001,-0.880000000000001,
-0.875000000000001,-0.870000000000001,-0.865000000000001,-0.860000000000001,
-0.855000000000001,-0.850000000000001,-0.845000000000001,-0.840000000000001,
-0.835000000000001,-0.830000000000001,-0.825000000000001,-0.820000000000001,
-0.815000000000001,-0.810000000000001,-0.805000000000001,-0.800000000000001,
-0.795000000000001,-0.790000000000001,-0.785000000000001,-0.780000000000001,
-0.775000000000001,-0.770000000000001,-0.765000000000001,-0.760000000000001,
-0.755000000000001,-0.750000000000001,-0.745000000000001,-0.740000000000001,
-0.735000000000001,-0.730000000000001,-0.725000000000001,-0.720000000000001,
-0.715000000000001,-0.710000000000001,-0.705000000000001,-0.700000000000001,
-0.695000000000001,-0.690000000000001,-0.685,-0.68,-0.675,-0.67,-0.665,
-0.66,-0.655,-0.65,-0.645,-0.64,-0.635,-0.63,-0.625,-0.62,-0.615,-0.61,
-0.605,-0.6,-0.595,-0.59,-0.585,-0.58,-0.575,-0.57,-0.565,-0.56,-0.555,
-0.55,-0.545,-0.54,-0.535,-0.53,-0.525,-0.52,-0.515,-0.51,-0.505,-0.5,-0.495,
-0.49,-0.485,-0.48,-0.475,-0.47,-0.465,-0.46,-0.455,-0.45,-0.445,-0.44,
-0.435,-0.43,-0.425,-0.42,-0.415,-0.41,-0.405,-0.4,-0.395,-0.39,-0.385,
-0.38,-0.375,-0.37,-0.365,-0.36,-0.355,-0.35,-0.345,-0.34,-0.335,-0.33,
-0.325,-0.32,-0.315,-0.31,-0.305,-0.3,-0.295,-0.29,-0.285,-0.28,-0.275,
-0.27,-0.265,-0.26,-0.255,-0.25,-0.245,-0.24,-0.235,-0.23,-0.225,-0.22,
-0.215,-0.21,-0.205,-0.2,-0.195,-0.19,-0.185,-0.18,-0.175,-0.17,-0.165,
-0.16,-0.155,-0.15,-0.145,-0.14,-0.135,-0.13,-0.125,-0.12,-0.115,-0.11,
-0.105,-0.1,-0.095,-0.09,-0.085,-0.08,-0.075,-0.07,-0.065,-0.06,-0.055,
-0.05,-0.045,-0.04,-0.035,-0.03,-0.025,-0.02,-0.015,-0.01,-0.005,0.),
 .UNSPECIFIED.)
CURVE()
GEOMETRIC_REPRESENTATION_ITEM()
RATIONAL_B_SPLINE_CURVE((1.,1.,1.,1.,1.,1.,1.,1.,1.,1.,1.,1.,1.,1.,1.,1.,
1.,1.,1.,1.,1.,1.,1.,1.,1.,1.,1.,1.,1.,1.,1.,1.,1.,1.,1.,1.,1.,1.,1.,1.,
1.,1.,1.,1.,1.,1.,1.,1.,1.,1.,1.,1.,1.,1.,1.,1.,1.,1.,1.,1.,1.,1.,1.,1.,
1.,1.,1.,1.,1.,1.,1.,1.,1.,1.,1.,1.,1.,1.,1.,1.,1.,1.,1.,1.,1.,1.,1.,1.,
1.,1.,1.,1.,1.,1.,1.,1.,1.,1.,1.,1.,1.,1.,1.,1.,1.,1.,1.,1.,1.,1.,1.,1.,
1.,1.,1.,1.,1.,1.,1.,1.,1.,1.,1.,1.,1.,1.,1.,1.,1.,1.,1.,1.,1.,1.,1.,1.,
1.,1.,1.,1.,1.,1.,1.,1.,1.,1.,1.,1.,1.,1.,1.,1.,1.,1.,1.,1.,1.,1.,1.,1.,
1.,1.,1.,1.,1.,1.,1.,1.,1.,1.,1.,1.,1.,1.,1.,1.,1.,1.,1.,1.,1.,1.,1.,1.,
1.,1.,1.,1.,1.,1.,1.,1.,1.,1.,1.,1.,1.,1.,1.,1.,1.,1.,1.,1.,1.))
REPRESENTATION_ITEM('')
);
#740=(
BOUNDED_CURVE()
B_SPLINE_CURVE(5,(#186633,#186634,#186635,#186636,#186637,#186638,#186639,
#186640,#186641,#186642,#186643,#186644,#186645,#186646,#186647,#186648,
#186649,#186650,#186651,#186652,#186653,#186654,#186655,#186656,#186657,
#186658,#186659,#186660,#186661,#186662,#186663,#186664,#186665,#186666,
#186667,#186668,#186669,#186670,#186671,#186672,#186673,#186674,#186675,
#186676,#186677,#186678,#186679,#186680,#186681,#186682,#186683,#186684,
#186685,#186686,#186687,#186688,#186689,#186690,#186691,#186692,#186693,
#186694,#186695,#186696,#186697,#186698,#186699,#186700,#186701,#186702,
#186703,#186704,#186705,#186706,#186707,#186708,#186709,#186710,#186711,
#186712,#186713,#186714,#186715,#186716,#186717,#186718,#186719,#186720,
#186721,#186722,#186723,#186724,#186725,#186726,#186727,#186728,#186729,
#186730,#186731,#186732,#186733,#186734,#186735,#186736,#186737,#186738,
#186739,#186740,#186741,#186742,#186743,#186744,#186745,#186746,#186747,
#186748,#186749,#186750,#186751,#186752,#186753,#186754,#186755,#186756,
#186757,#186758,#186759,#186760,#186761,#186762,#186763,#186764,#186765,
#186766,#186767,#186768,#186769,#186770,#186771,#186772,#186773,#186774,
#186775,#186776,#186777,#186778,#186779,#186780,#186781,#186782,#186783,
#186784,#186785,#186786,#186787,#186788,#186789,#186790,#186791,#186792,
#186793,#186794,#186795,#186796,#186797,#186798,#186799,#186800,#186801,
#186802,#186803,#186804,#186805,#186806,#186807,#186808,#186809,#186810,
#186811,#186812,#186813,#186814,#186815,#186816,#186817,#186818,#186819,
#186820,#186821,#186822,#186823,#186824,#186825,#186826,#186827,#186828,
#186829,#186830,#186831,#186832,#186833,#186834,#186835,#186836,#186837),
 .UNSPECIFIED.,.F.,.F.)
B_SPLINE_CURVE_WITH_KNOTS((6,1,1,1,1,1,1,1,1,1,1,1,1,1,1,1,1,1,1,1,1,1,
1,1,1,1,1,1,1,1,1,1,1,1,1,1,1,1,1,1,1,1,1,1,1,1,1,1,1,1,1,1,1,1,1,1,1,1,
1,1,1,1,1,1,1,1,1,1,1,1,1,1,1,1,1,1,1,1,1,1,1,1,1,1,1,1,1,1,1,1,1,1,1,1,
1,1,1,1,1,1,1,1,1,1,1,1,1,1,1,1,1,1,1,1,1,1,1,1,1,1,1,1,1,1,1,1,1,1,1,1,
1,1,1,1,1,1,1,1,1,1,1,1,1,1,1,1,1,1,1,1,1,1,1,1,1,1,1,1,1,1,1,1,1,1,1,1,
1,1,1,1,1,1,1,1,1,1,1,1,1,1,1,1,1,1,1,1,1,1,1,1,1,1,1,1,1,1,1,1,1,1,6),
(0.,0.005,0.01,0.015,0.02,0.025,0.03,0.035,0.04,0.045,0.05,0.055,0.06,0.065,
0.07,0.075,0.08,0.085,0.09,0.095,0.1,0.105,0.11,0.115,0.12,0.125,0.13,0.135,
0.14,0.145,0.15,0.155,0.16,0.165,0.17,0.175,0.18,0.185,0.19,0.195,0.2,0.205,
0.21,0.215,0.22,0.225,0.23,0.235,0.24,0.245,0.25,0.255,0.26,0.265,0.27,
0.275,0.28,0.285,0.29,0.295,0.3,0.305,0.31,0.315,0.32,0.325,0.33,0.335,
0.34,0.345,0.35,0.355,0.36,0.365,0.37,0.375,0.38,0.385,0.39,0.395,0.4,0.405,
0.41,0.415,0.42,0.425,0.43,0.435,0.44,0.445,0.45,0.455,0.46,0.465,0.47,
0.475,0.48,0.485,0.49,0.495,0.5,0.505,0.51,0.515,0.52,0.525,0.53,0.535,
0.54,0.545,0.55,0.555,0.56,0.565,0.57,0.575,0.58,0.585,0.59,0.595,0.6,0.605,
0.61,0.615,0.62,0.625,0.63,0.635,0.64,0.645,0.65,0.655,0.66,0.665,0.67,
0.675,0.68,0.685,0.690000000000001,0.695000000000001,0.700000000000001,
0.705000000000001,0.710000000000001,0.715000000000001,0.720000000000001,
0.725000000000001,0.730000000000001,0.735000000000001,0.740000000000001,
0.745000000000001,0.750000000000001,0.755000000000001,0.760000000000001,
0.765000000000001,0.770000000000001,0.775000000000001,0.780000000000001,
0.785000000000001,0.790000000000001,0.795000000000001,0.800000000000001,
0.805000000000001,0.810000000000001,0.815000000000001,0.820000000000001,
0.825000000000001,0.830000000000001,0.835000000000001,0.840000000000001,
0.845000000000001,0.850000000000001,0.855000000000001,0.860000000000001,
0.865000000000001,0.870000000000001,0.875000000000001,0.880000000000001,
0.885000000000001,0.890000000000001,0.895000000000001,0.900000000000001,
0.905000000000001,0.910000000000001,0.915000000000001,0.920000000000001,
0.925000000000001,0.930000000000001,0.935000000000001,0.940000000000001,
0.945000000000001,0.950000000000001,0.955000000000001,0.960000000000001,
0.965000000000001,0.970000000000001,0.975000000000001,0.980000000000001,
0.985000000000001,0.990000000000001,0.995000000000001,1.),.UNSPECIFIED.)
CURVE()
GEOMETRIC_REPRESENTATION_ITEM()
RATIONAL_B_SPLINE_CURVE((1.,1.,1.,1.,1.,1.,1.,1.,1.,1.,1.,1.,1.,1.,1.,1.,
1.,1.,1.,1.,1.,1.,1.,1.,1.,1.,1.,1.,1.,1.,1.,1.,1.,1.,1.,1.,1.,1.,1.,1.,
1.,1.,1.,1.,1.,1.,1.,1.,1.,1.,1.,1.,1.,1.,1.,1.,1.,1.,1.,1.,1.,1.,1.,1.,
1.,1.,1.,1.,1.,1.,1.,1.,1.,1.,1.,1.,1.,1.,1.,1.,1.,1.,1.,1.,1.,1.,1.,1.,
1.,1.,1.,1.,1.,1.,1.,1.,1.,1.,1.,1.,1.,1.,1.,1.,1.,1.,1.,1.,1.,1.,1.,1.,
1.,1.,1.,1.,1.,1.,1.,1.,1.,1.,1.,1.,1.,1.,1.,1.,1.,1.,1.,1.,1.,1.,1.,1.,
1.,1.,1.,1.,1.,1.,1.,1.,1.,1.,1.,1.,1.,1.,1.,1.,1.,1.,1.,1.,1.,1.,1.,1.,
1.,1.,1.,1.,1.,1.,1.,1.,1.,1.,1.,1.,1.,1.,1.,1.,1.,1.,1.,1.,1.,1.,1.,1.,
1.,1.,1.,1.,1.,1.,1.,1.,1.,1.,1.,1.,1.,1.,1.,1.,1.,1.,1.,1.,1.))
REPRESENTATION_ITEM('')
);
#741=(
BOUNDED_CURVE()
B_SPLINE_CURVE(5,(#187254,#187255,#187256,#187257,#187258,#187259,#187260,
#187261,#187262,#187263,#187264,#187265,#187266,#187267,#187268,#187269,
#187270,#187271,#187272,#187273,#187274,#187275,#187276,#187277,#187278,
#187279,#187280,#187281,#187282,#187283,#187284,#187285,#187286,#187287,
#187288,#187289,#187290,#187291,#187292,#187293,#187294,#187295,#187296,
#187297,#187298,#187299,#187300,#187301,#187302,#187303,#187304,#187305,
#187306,#187307,#187308,#187309,#187310,#187311,#187312,#187313,#187314,
#187315,#187316,#187317,#187318,#187319,#187320,#187321,#187322,#187323,
#187324,#187325,#187326,#187327,#187328,#187329,#187330,#187331,#187332,
#187333,#187334,#187335,#187336,#187337,#187338,#187339,#187340,#187341,
#187342,#187343,#187344,#187345,#187346,#187347,#187348,#187349,#187350,
#187351,#187352,#187353,#187354,#187355,#187356,#187357,#187358,#187359,
#187360,#187361,#187362,#187363,#187364,#187365,#187366,#187367,#187368,
#187369,#187370,#187371,#187372,#187373,#187374,#187375,#187376,#187377,
#187378,#187379,#187380,#187381,#187382,#187383,#187384,#187385,#187386,
#187387,#187388,#187389,#187390,#187391,#187392,#187393,#187394,#187395,
#187396,#187397,#187398,#187399,#187400,#187401,#187402,#187403,#187404,
#187405,#187406,#187407,#187408,#187409,#187410,#187411,#187412,#187413,
#187414,#187415,#187416,#187417,#187418,#187419,#187420,#187421,#187422,
#187423,#187424,#187425,#187426,#187427,#187428,#187429,#187430,#187431,
#187432,#187433,#187434,#187435,#187436,#187437,#187438,#187439,#187440,
#187441,#187442,#187443,#187444,#187445,#187446,#187447,#187448,#187449,
#187450,#187451,#187452,#187453,#187454,#187455,#187456,#187457,#187458),
 .UNSPECIFIED.,.F.,.F.)
B_SPLINE_CURVE_WITH_KNOTS((6,1,1,1,1,1,1,1,1,1,1,1,1,1,1,1,1,1,1,1,1,1,
1,1,1,1,1,1,1,1,1,1,1,1,1,1,1,1,1,1,1,1,1,1,1,1,1,1,1,1,1,1,1,1,1,1,1,1,
1,1,1,1,1,1,1,1,1,1,1,1,1,1,1,1,1,1,1,1,1,1,1,1,1,1,1,1,1,1,1,1,1,1,1,1,
1,1,1,1,1,1,1,1,1,1,1,1,1,1,1,1,1,1,1,1,1,1,1,1,1,1,1,1,1,1,1,1,1,1,1,1,
1,1,1,1,1,1,1,1,1,1,1,1,1,1,1,1,1,1,1,1,1,1,1,1,1,1,1,1,1,1,1,1,1,1,1,1,
1,1,1,1,1,1,1,1,1,1,1,1,1,1,1,1,1,1,1,1,1,1,1,1,1,1,1,1,1,1,1,1,1,1,6),
(-1.,-0.995000000000001,-0.990000000000001,-0.985000000000001,-0.980000000000001,
-0.975000000000001,-0.970000000000001,-0.965000000000001,-0.960000000000001,
-0.955000000000001,-0.950000000000001,-0.945000000000001,-0.940000000000001,
-0.935000000000001,-0.930000000000001,-0.925000000000001,-0.920000000000001,
-0.915000000000001,-0.910000000000001,-0.905000000000001,-0.900000000000001,
-0.895000000000001,-0.890000000000001,-0.885000000000001,-0.880000000000001,
-0.875000000000001,-0.870000000000001,-0.865000000000001,-0.860000000000001,
-0.855000000000001,-0.850000000000001,-0.845000000000001,-0.840000000000001,
-0.835000000000001,-0.830000000000001,-0.825000000000001,-0.820000000000001,
-0.815000000000001,-0.810000000000001,-0.805000000000001,-0.800000000000001,
-0.795000000000001,-0.790000000000001,-0.785000000000001,-0.780000000000001,
-0.775000000000001,-0.770000000000001,-0.765000000000001,-0.760000000000001,
-0.755000000000001,-0.750000000000001,-0.745000000000001,-0.740000000000001,
-0.735000000000001,-0.730000000000001,-0.725000000000001,-0.720000000000001,
-0.715000000000001,-0.710000000000001,-0.705000000000001,-0.700000000000001,
-0.695000000000001,-0.690000000000001,-0.685,-0.68,-0.675,-0.67,-0.665,
-0.66,-0.655,-0.65,-0.645,-0.64,-0.635,-0.63,-0.625,-0.62,-0.615,-0.61,
-0.605,-0.6,-0.595,-0.59,-0.585,-0.58,-0.575,-0.57,-0.565,-0.56,-0.555,
-0.55,-0.545,-0.54,-0.535,-0.53,-0.525,-0.52,-0.515,-0.51,-0.505,-0.5,-0.495,
-0.49,-0.485,-0.48,-0.475,-0.47,-0.465,-0.46,-0.455,-0.45,-0.445,-0.44,
-0.435,-0.43,-0.425,-0.42,-0.415,-0.41,-0.405,-0.4,-0.395,-0.39,-0.385,
-0.38,-0.375,-0.37,-0.365,-0.36,-0.355,-0.35,-0.345,-0.34,-0.335,-0.33,
-0.325,-0.32,-0.315,-0.31,-0.305,-0.3,-0.295,-0.29,-0.285,-0.28,-0.275,
-0.27,-0.265,-0.26,-0.255,-0.25,-0.245,-0.24,-0.235,-0.23,-0.225,-0.22,
-0.215,-0.21,-0.205,-0.2,-0.195,-0.19,-0.185,-0.18,-0.175,-0.17,-0.165,
-0.16,-0.155,-0.15,-0.145,-0.14,-0.135,-0.13,-0.125,-0.12,-0.115,-0.11,
-0.105,-0.1,-0.095,-0.09,-0.085,-0.08,-0.075,-0.07,-0.065,-0.06,-0.055,
-0.05,-0.045,-0.04,-0.035,-0.03,-0.025,-0.02,-0.015,-0.01,-0.005,0.),
 .UNSPECIFIED.)
CURVE()
GEOMETRIC_REPRESENTATION_ITEM()
RATIONAL_B_SPLINE_CURVE((1.,1.,1.,1.,1.,1.,1.,1.,1.,1.,1.,1.,1.,1.,1.,1.,
1.,1.,1.,1.,1.,1.,1.,1.,1.,1.,1.,1.,1.,1.,1.,1.,1.,1.,1.,1.,1.,1.,1.,1.,
1.,1.,1.,1.,1.,1.,1.,1.,1.,1.,1.,1.,1.,1.,1.,1.,1.,1.,1.,1.,1.,1.,1.,1.,
1.,1.,1.,1.,1.,1.,1.,1.,1.,1.,1.,1.,1.,1.,1.,1.,1.,1.,1.,1.,1.,1.,1.,1.,
1.,1.,1.,1.,1.,1.,1.,1.,1.,1.,1.,1.,1.,1.,1.,1.,1.,1.,1.,1.,1.,1.,1.,1.,
1.,1.,1.,1.,1.,1.,1.,1.,1.,1.,1.,1.,1.,1.,1.,1.,1.,1.,1.,1.,1.,1.,1.,1.,
1.,1.,1.,1.,1.,1.,1.,1.,1.,1.,1.,1.,1.,1.,1.,1.,1.,1.,1.,1.,1.,1.,1.,1.,
1.,1.,1.,1.,1.,1.,1.,1.,1.,1.,1.,1.,1.,1.,1.,1.,1.,1.,1.,1.,1.,1.,1.,1.,
1.,1.,1.,1.,1.,1.,1.,1.,1.,1.,1.,1.,1.,1.,1.,1.,1.,1.,1.,1.,1.))
REPRESENTATION_ITEM('')
);
#742=(
BOUNDED_CURVE()
B_SPLINE_CURVE(5,(#187871,#187872,#187873,#187874,#187875,#187876,#187877,
#187878,#187879,#187880,#187881,#187882,#187883,#187884,#187885,#187886,
#187887,#187888,#187889,#187890,#187891,#187892,#187893,#187894,#187895,
#187896,#187897,#187898,#187899,#187900,#187901,#187902,#187903,#187904,
#187905,#187906,#187907,#187908,#187909,#187910,#187911,#187912,#187913,
#187914,#187915,#187916,#187917,#187918,#187919,#187920,#187921,#187922,
#187923,#187924,#187925,#187926,#187927,#187928,#187929,#187930,#187931,
#187932,#187933,#187934,#187935,#187936,#187937,#187938,#187939,#187940,
#187941,#187942,#187943,#187944,#187945,#187946,#187947,#187948,#187949,
#187950,#187951,#187952,#187953,#187954,#187955,#187956,#187957,#187958,
#187959,#187960,#187961,#187962,#187963,#187964,#187965,#187966,#187967,
#187968,#187969,#187970,#187971,#187972,#187973,#187974,#187975,#187976,
#187977,#187978,#187979,#187980,#187981,#187982,#187983,#187984,#187985,
#187986,#187987,#187988,#187989,#187990,#187991,#187992,#187993,#187994,
#187995,#187996,#187997,#187998,#187999,#188000,#188001,#188002,#188003,
#188004,#188005,#188006,#188007,#188008,#188009,#188010,#188011,#188012,
#188013,#188014,#188015,#188016,#188017,#188018,#188019,#188020,#188021,
#188022,#188023,#188024,#188025,#188026,#188027,#188028,#188029,#188030,
#188031,#188032,#188033,#188034,#188035,#188036,#188037,#188038,#188039,
#188040,#188041,#188042,#188043,#188044,#188045,#188046,#188047,#188048,
#188049,#188050,#188051,#188052,#188053,#188054,#188055,#188056,#188057,
#188058,#188059,#188060,#188061,#188062,#188063,#188064,#188065,#188066,
#188067,#188068,#188069,#188070,#188071,#188072,#188073,#188074,#188075),
 .UNSPECIFIED.,.F.,.F.)
B_SPLINE_CURVE_WITH_KNOTS((6,1,1,1,1,1,1,1,1,1,1,1,1,1,1,1,1,1,1,1,1,1,
1,1,1,1,1,1,1,1,1,1,1,1,1,1,1,1,1,1,1,1,1,1,1,1,1,1,1,1,1,1,1,1,1,1,1,1,
1,1,1,1,1,1,1,1,1,1,1,1,1,1,1,1,1,1,1,1,1,1,1,1,1,1,1,1,1,1,1,1,1,1,1,1,
1,1,1,1,1,1,1,1,1,1,1,1,1,1,1,1,1,1,1,1,1,1,1,1,1,1,1,1,1,1,1,1,1,1,1,1,
1,1,1,1,1,1,1,1,1,1,1,1,1,1,1,1,1,1,1,1,1,1,1,1,1,1,1,1,1,1,1,1,1,1,1,1,
1,1,1,1,1,1,1,1,1,1,1,1,1,1,1,1,1,1,1,1,1,1,1,1,1,1,1,1,1,1,1,1,1,1,6),
(0.,0.005,0.01,0.015,0.02,0.025,0.03,0.035,0.04,0.045,0.05,0.055,0.06,0.065,
0.07,0.075,0.08,0.085,0.09,0.095,0.1,0.105,0.11,0.115,0.12,0.125,0.13,0.135,
0.14,0.145,0.15,0.155,0.16,0.165,0.17,0.175,0.18,0.185,0.19,0.195,0.2,0.205,
0.21,0.215,0.22,0.225,0.23,0.235,0.24,0.245,0.25,0.255,0.26,0.265,0.27,
0.275,0.28,0.285,0.29,0.295,0.3,0.305,0.31,0.315,0.32,0.325,0.33,0.335,
0.34,0.345,0.35,0.355,0.36,0.365,0.37,0.375,0.38,0.385,0.39,0.395,0.4,0.405,
0.41,0.415,0.42,0.425,0.43,0.435,0.44,0.445,0.45,0.455,0.46,0.465,0.47,
0.475,0.48,0.485,0.49,0.495,0.5,0.505,0.51,0.515,0.52,0.525,0.53,0.535,
0.54,0.545,0.55,0.555,0.56,0.565,0.57,0.575,0.58,0.585,0.59,0.595,0.6,0.605,
0.61,0.615,0.62,0.625,0.63,0.635,0.64,0.645,0.65,0.655,0.66,0.665,0.67,
0.675,0.68,0.685,0.690000000000001,0.695000000000001,0.700000000000001,
0.705000000000001,0.710000000000001,0.715000000000001,0.720000000000001,
0.725000000000001,0.730000000000001,0.735000000000001,0.740000000000001,
0.745000000000001,0.750000000000001,0.755000000000001,0.760000000000001,
0.765000000000001,0.770000000000001,0.775000000000001,0.780000000000001,
0.785000000000001,0.790000000000001,0.795000000000001,0.800000000000001,
0.805000000000001,0.810000000000001,0.815000000000001,0.820000000000001,
0.825000000000001,0.830000000000001,0.835000000000001,0.840000000000001,
0.845000000000001,0.850000000000001,0.855000000000001,0.860000000000001,
0.865000000000001,0.870000000000001,0.875000000000001,0.880000000000001,
0.885000000000001,0.890000000000001,0.895000000000001,0.900000000000001,
0.905000000000001,0.910000000000001,0.915000000000001,0.920000000000001,
0.925000000000001,0.930000000000001,0.935000000000001,0.940000000000001,
0.945000000000001,0.950000000000001,0.955000000000001,0.960000000000001,
0.965000000000001,0.970000000000001,0.975000000000001,0.980000000000001,
0.985000000000001,0.990000000000001,0.995000000000001,1.),.UNSPECIFIED.)
CURVE()
GEOMETRIC_REPRESENTATION_ITEM()
RATIONAL_B_SPLINE_CURVE((1.,1.,1.,1.,1.,1.,1.,1.,1.,1.,1.,1.,1.,1.,1.,1.,
1.,1.,1.,1.,1.,1.,1.,1.,1.,1.,1.,1.,1.,1.,1.,1.,1.,1.,1.,1.,1.,1.,1.,1.,
1.,1.,1.,1.,1.,1.,1.,1.,1.,1.,1.,1.,1.,1.,1.,1.,1.,1.,1.,1.,1.,1.,1.,1.,
1.,1.,1.,1.,1.,1.,1.,1.,1.,1.,1.,1.,1.,1.,1.,1.,1.,1.,1.,1.,1.,1.,1.,1.,
1.,1.,1.,1.,1.,1.,1.,1.,1.,1.,1.,1.,1.,1.,1.,1.,1.,1.,1.,1.,1.,1.,1.,1.,
1.,1.,1.,1.,1.,1.,1.,1.,1.,1.,1.,1.,1.,1.,1.,1.,1.,1.,1.,1.,1.,1.,1.,1.,
1.,1.,1.,1.,1.,1.,1.,1.,1.,1.,1.,1.,1.,1.,1.,1.,1.,1.,1.,1.,1.,1.,1.,1.,
1.,1.,1.,1.,1.,1.,1.,1.,1.,1.,1.,1.,1.,1.,1.,1.,1.,1.,1.,1.,1.,1.,1.,1.,
1.,1.,1.,1.,1.,1.,1.,1.,1.,1.,1.,1.,1.,1.,1.,1.,1.,1.,1.,1.,1.))
REPRESENTATION_ITEM('')
);
#743=(
BOUNDED_CURVE()
B_SPLINE_CURVE(5,(#188492,#188493,#188494,#188495,#188496,#188497,#188498,
#188499,#188500,#188501,#188502,#188503,#188504,#188505,#188506,#188507,
#188508,#188509,#188510,#188511,#188512,#188513,#188514,#188515,#188516,
#188517,#188518,#188519,#188520,#188521,#188522,#188523,#188524,#188525,
#188526,#188527,#188528,#188529,#188530,#188531,#188532,#188533,#188534,
#188535,#188536,#188537,#188538,#188539,#188540,#188541,#188542,#188543,
#188544,#188545,#188546,#188547,#188548,#188549,#188550,#188551,#188552,
#188553,#188554,#188555,#188556,#188557,#188558,#188559,#188560,#188561,
#188562,#188563,#188564,#188565,#188566,#188567,#188568,#188569,#188570,
#188571,#188572,#188573,#188574,#188575,#188576,#188577,#188578,#188579,
#188580,#188581,#188582,#188583,#188584,#188585,#188586,#188587,#188588,
#188589,#188590,#188591,#188592,#188593,#188594,#188595,#188596,#188597,
#188598,#188599,#188600,#188601,#188602,#188603,#188604,#188605,#188606,
#188607,#188608,#188609,#188610,#188611,#188612,#188613,#188614,#188615,
#188616,#188617,#188618,#188619,#188620,#188621,#188622,#188623,#188624,
#188625,#188626,#188627,#188628,#188629,#188630,#188631,#188632,#188633,
#188634,#188635,#188636,#188637,#188638,#188639,#188640,#188641,#188642,
#188643,#188644,#188645,#188646,#188647,#188648,#188649,#188650,#188651,
#188652,#188653,#188654,#188655,#188656,#188657,#188658,#188659,#188660,
#188661,#188662,#188663,#188664,#188665,#188666,#188667,#188668,#188669,
#188670,#188671,#188672,#188673,#188674,#188675,#188676,#188677,#188678,
#188679,#188680,#188681,#188682,#188683,#188684,#188685,#188686,#188687,
#188688,#188689,#188690,#188691,#188692,#188693,#188694,#188695,#188696),
 .UNSPECIFIED.,.F.,.F.)
B_SPLINE_CURVE_WITH_KNOTS((6,1,1,1,1,1,1,1,1,1,1,1,1,1,1,1,1,1,1,1,1,1,
1,1,1,1,1,1,1,1,1,1,1,1,1,1,1,1,1,1,1,1,1,1,1,1,1,1,1,1,1,1,1,1,1,1,1,1,
1,1,1,1,1,1,1,1,1,1,1,1,1,1,1,1,1,1,1,1,1,1,1,1,1,1,1,1,1,1,1,1,1,1,1,1,
1,1,1,1,1,1,1,1,1,1,1,1,1,1,1,1,1,1,1,1,1,1,1,1,1,1,1,1,1,1,1,1,1,1,1,1,
1,1,1,1,1,1,1,1,1,1,1,1,1,1,1,1,1,1,1,1,1,1,1,1,1,1,1,1,1,1,1,1,1,1,1,1,
1,1,1,1,1,1,1,1,1,1,1,1,1,1,1,1,1,1,1,1,1,1,1,1,1,1,1,1,1,1,1,1,1,1,6),
(-1.,-0.995000000000001,-0.990000000000001,-0.985000000000001,-0.980000000000001,
-0.975000000000001,-0.970000000000001,-0.965000000000001,-0.960000000000001,
-0.955000000000001,-0.950000000000001,-0.945000000000001,-0.940000000000001,
-0.935000000000001,-0.930000000000001,-0.925000000000001,-0.920000000000001,
-0.915000000000001,-0.910000000000001,-0.905000000000001,-0.900000000000001,
-0.895000000000001,-0.890000000000001,-0.885000000000001,-0.880000000000001,
-0.875000000000001,-0.870000000000001,-0.865000000000001,-0.860000000000001,
-0.855000000000001,-0.850000000000001,-0.845000000000001,-0.840000000000001,
-0.835000000000001,-0.830000000000001,-0.825000000000001,-0.820000000000001,
-0.815000000000001,-0.810000000000001,-0.805000000000001,-0.800000000000001,
-0.795000000000001,-0.790000000000001,-0.785000000000001,-0.780000000000001,
-0.775000000000001,-0.770000000000001,-0.765000000000001,-0.760000000000001,
-0.755000000000001,-0.750000000000001,-0.745000000000001,-0.740000000000001,
-0.735000000000001,-0.730000000000001,-0.725000000000001,-0.720000000000001,
-0.715000000000001,-0.710000000000001,-0.705000000000001,-0.700000000000001,
-0.695000000000001,-0.690000000000001,-0.685,-0.68,-0.675,-0.67,-0.665,
-0.66,-0.655,-0.65,-0.645,-0.64,-0.635,-0.63,-0.625,-0.62,-0.615,-0.61,
-0.605,-0.6,-0.595,-0.59,-0.585,-0.58,-0.575,-0.57,-0.565,-0.56,-0.555,
-0.55,-0.545,-0.54,-0.535,-0.53,-0.525,-0.52,-0.515,-0.51,-0.505,-0.5,-0.495,
-0.49,-0.485,-0.48,-0.475,-0.47,-0.465,-0.46,-0.455,-0.45,-0.445,-0.44,
-0.435,-0.43,-0.425,-0.42,-0.415,-0.41,-0.405,-0.4,-0.395,-0.39,-0.385,
-0.38,-0.375,-0.37,-0.365,-0.36,-0.355,-0.35,-0.345,-0.34,-0.335,-0.33,
-0.325,-0.32,-0.315,-0.31,-0.305,-0.3,-0.295,-0.29,-0.285,-0.28,-0.275,
-0.27,-0.265,-0.26,-0.255,-0.25,-0.245,-0.24,-0.235,-0.23,-0.225,-0.22,
-0.215,-0.21,-0.205,-0.2,-0.195,-0.19,-0.185,-0.18,-0.175,-0.17,-0.165,
-0.16,-0.155,-0.15,-0.145,-0.14,-0.135,-0.13,-0.125,-0.12,-0.115,-0.11,
-0.105,-0.1,-0.095,-0.09,-0.085,-0.08,-0.075,-0.07,-0.065,-0.06,-0.055,
-0.05,-0.045,-0.04,-0.035,-0.03,-0.025,-0.02,-0.015,-0.01,-0.005,0.),
 .UNSPECIFIED.)
CURVE()
GEOMETRIC_REPRESENTATION_ITEM()
RATIONAL_B_SPLINE_CURVE((1.,1.,1.,1.,1.,1.,1.,1.,1.,1.,1.,1.,1.,1.,1.,1.,
1.,1.,1.,1.,1.,1.,1.,1.,1.,1.,1.,1.,1.,1.,1.,1.,1.,1.,1.,1.,1.,1.,1.,1.,
1.,1.,1.,1.,1.,1.,1.,1.,1.,1.,1.,1.,1.,1.,1.,1.,1.,1.,1.,1.,1.,1.,1.,1.,
1.,1.,1.,1.,1.,1.,1.,1.,1.,1.,1.,1.,1.,1.,1.,1.,1.,1.,1.,1.,1.,1.,1.,1.,
1.,1.,1.,1.,1.,1.,1.,1.,1.,1.,1.,1.,1.,1.,1.,1.,1.,1.,1.,1.,1.,1.,1.,1.,
1.,1.,1.,1.,1.,1.,1.,1.,1.,1.,1.,1.,1.,1.,1.,1.,1.,1.,1.,1.,1.,1.,1.,1.,
1.,1.,1.,1.,1.,1.,1.,1.,1.,1.,1.,1.,1.,1.,1.,1.,1.,1.,1.,1.,1.,1.,1.,1.,
1.,1.,1.,1.,1.,1.,1.,1.,1.,1.,1.,1.,1.,1.,1.,1.,1.,1.,1.,1.,1.,1.,1.,1.,
1.,1.,1.,1.,1.,1.,1.,1.,1.,1.,1.,1.,1.,1.,1.,1.,1.,1.,1.,1.,1.))
REPRESENTATION_ITEM('')
);
#744=(
BOUNDED_CURVE()
B_SPLINE_CURVE(5,(#189109,#189110,#189111,#189112,#189113,#189114,#189115,
#189116,#189117,#189118,#189119,#189120,#189121,#189122,#189123,#189124,
#189125,#189126,#189127,#189128,#189129,#189130,#189131,#189132,#189133,
#189134,#189135,#189136,#189137,#189138,#189139,#189140,#189141,#189142,
#189143,#189144,#189145,#189146,#189147,#189148,#189149,#189150,#189151,
#189152,#189153,#189154,#189155,#189156,#189157,#189158,#189159,#189160,
#189161,#189162,#189163,#189164,#189165,#189166,#189167,#189168,#189169,
#189170,#189171,#189172,#189173,#189174,#189175,#189176,#189177,#189178,
#189179,#189180,#189181,#189182,#189183,#189184,#189185,#189186,#189187,
#189188,#189189,#189190,#189191,#189192,#189193,#189194,#189195,#189196,
#189197,#189198,#189199,#189200,#189201,#189202,#189203,#189204,#189205,
#189206,#189207,#189208,#189209,#189210,#189211,#189212,#189213,#189214,
#189215,#189216,#189217,#189218,#189219,#189220,#189221,#189222,#189223,
#189224,#189225,#189226,#189227,#189228,#189229,#189230,#189231,#189232,
#189233,#189234,#189235,#189236,#189237,#189238,#189239,#189240,#189241,
#189242,#189243,#189244,#189245,#189246,#189247,#189248,#189249,#189250,
#189251,#189252,#189253,#189254,#189255,#189256,#189257,#189258,#189259,
#189260,#189261,#189262,#189263,#189264,#189265,#189266,#189267,#189268,
#189269,#189270,#189271,#189272,#189273,#189274,#189275,#189276,#189277,
#189278,#189279,#189280,#189281,#189282,#189283,#189284,#189285,#189286,
#189287,#189288,#189289,#189290,#189291,#189292,#189293,#189294,#189295,
#189296,#189297,#189298,#189299,#189300,#189301,#189302,#189303,#189304,
#189305,#189306,#189307,#189308,#189309,#189310,#189311,#189312,#189313),
 .UNSPECIFIED.,.F.,.F.)
B_SPLINE_CURVE_WITH_KNOTS((6,1,1,1,1,1,1,1,1,1,1,1,1,1,1,1,1,1,1,1,1,1,
1,1,1,1,1,1,1,1,1,1,1,1,1,1,1,1,1,1,1,1,1,1,1,1,1,1,1,1,1,1,1,1,1,1,1,1,
1,1,1,1,1,1,1,1,1,1,1,1,1,1,1,1,1,1,1,1,1,1,1,1,1,1,1,1,1,1,1,1,1,1,1,1,
1,1,1,1,1,1,1,1,1,1,1,1,1,1,1,1,1,1,1,1,1,1,1,1,1,1,1,1,1,1,1,1,1,1,1,1,
1,1,1,1,1,1,1,1,1,1,1,1,1,1,1,1,1,1,1,1,1,1,1,1,1,1,1,1,1,1,1,1,1,1,1,1,
1,1,1,1,1,1,1,1,1,1,1,1,1,1,1,1,1,1,1,1,1,1,1,1,1,1,1,1,1,1,1,1,1,1,6),
(0.,0.005,0.01,0.015,0.02,0.025,0.03,0.035,0.04,0.045,0.05,0.055,0.06,0.065,
0.07,0.075,0.08,0.085,0.09,0.095,0.1,0.105,0.11,0.115,0.12,0.125,0.13,0.135,
0.14,0.145,0.15,0.155,0.16,0.165,0.17,0.175,0.18,0.185,0.19,0.195,0.2,0.205,
0.21,0.215,0.22,0.225,0.23,0.235,0.24,0.245,0.25,0.255,0.26,0.265,0.27,
0.275,0.28,0.285,0.29,0.295,0.3,0.305,0.31,0.315,0.32,0.325,0.33,0.335,
0.34,0.345,0.35,0.355,0.36,0.365,0.37,0.375,0.38,0.385,0.39,0.395,0.4,0.405,
0.41,0.415,0.42,0.425,0.43,0.435,0.44,0.445,0.45,0.455,0.46,0.465,0.47,
0.475,0.48,0.485,0.49,0.495,0.5,0.505,0.51,0.515,0.52,0.525,0.53,0.535,
0.54,0.545,0.55,0.555,0.56,0.565,0.57,0.575,0.58,0.585,0.59,0.595,0.6,0.605,
0.61,0.615,0.62,0.625,0.63,0.635,0.64,0.645,0.65,0.655,0.66,0.665,0.67,
0.675,0.68,0.685,0.690000000000001,0.695000000000001,0.700000000000001,
0.705000000000001,0.710000000000001,0.715000000000001,0.720000000000001,
0.725000000000001,0.730000000000001,0.735000000000001,0.740000000000001,
0.745000000000001,0.750000000000001,0.755000000000001,0.760000000000001,
0.765000000000001,0.770000000000001,0.775000000000001,0.780000000000001,
0.785000000000001,0.790000000000001,0.795000000000001,0.800000000000001,
0.805000000000001,0.810000000000001,0.815000000000001,0.820000000000001,
0.825000000000001,0.830000000000001,0.835000000000001,0.840000000000001,
0.845000000000001,0.850000000000001,0.855000000000001,0.860000000000001,
0.865000000000001,0.870000000000001,0.875000000000001,0.880000000000001,
0.885000000000001,0.890000000000001,0.895000000000001,0.900000000000001,
0.905000000000001,0.910000000000001,0.915000000000001,0.920000000000001,
0.925000000000001,0.930000000000001,0.935000000000001,0.940000000000001,
0.945000000000001,0.950000000000001,0.955000000000001,0.960000000000001,
0.965000000000001,0.970000000000001,0.975000000000001,0.980000000000001,
0.985000000000001,0.990000000000001,0.995000000000001,1.),.UNSPECIFIED.)
CURVE()
GEOMETRIC_REPRESENTATION_ITEM()
RATIONAL_B_SPLINE_CURVE((1.,1.,1.,1.,1.,1.,1.,1.,1.,1.,1.,1.,1.,1.,1.,1.,
1.,1.,1.,1.,1.,1.,1.,1.,1.,1.,1.,1.,1.,1.,1.,1.,1.,1.,1.,1.,1.,1.,1.,1.,
1.,1.,1.,1.,1.,1.,1.,1.,1.,1.,1.,1.,1.,1.,1.,1.,1.,1.,1.,1.,1.,1.,1.,1.,
1.,1.,1.,1.,1.,1.,1.,1.,1.,1.,1.,1.,1.,1.,1.,1.,1.,1.,1.,1.,1.,1.,1.,1.,
1.,1.,1.,1.,1.,1.,1.,1.,1.,1.,1.,1.,1.,1.,1.,1.,1.,1.,1.,1.,1.,1.,1.,1.,
1.,1.,1.,1.,1.,1.,1.,1.,1.,1.,1.,1.,1.,1.,1.,1.,1.,1.,1.,1.,1.,1.,1.,1.,
1.,1.,1.,1.,1.,1.,1.,1.,1.,1.,1.,1.,1.,1.,1.,1.,1.,1.,1.,1.,1.,1.,1.,1.,
1.,1.,1.,1.,1.,1.,1.,1.,1.,1.,1.,1.,1.,1.,1.,1.,1.,1.,1.,1.,1.,1.,1.,1.,
1.,1.,1.,1.,1.,1.,1.,1.,1.,1.,1.,1.,1.,1.,1.,1.,1.,1.,1.,1.,1.))
REPRESENTATION_ITEM('')
);
#745=(
BOUNDED_CURVE()
B_SPLINE_CURVE(5,(#189730,#189731,#189732,#189733,#189734,#189735,#189736,
#189737,#189738,#189739,#189740,#189741,#189742,#189743,#189744,#189745,
#189746,#189747,#189748,#189749,#189750,#189751,#189752,#189753,#189754,
#189755,#189756,#189757,#189758,#189759,#189760,#189761,#189762,#189763,
#189764,#189765,#189766,#189767,#189768,#189769,#189770,#189771,#189772,
#189773,#189774,#189775,#189776,#189777,#189778,#189779,#189780,#189781,
#189782,#189783,#189784,#189785,#189786,#189787,#189788,#189789,#189790,
#189791,#189792,#189793,#189794,#189795,#189796,#189797,#189798,#189799,
#189800,#189801,#189802,#189803,#189804,#189805,#189806,#189807,#189808,
#189809,#189810,#189811,#189812,#189813,#189814,#189815,#189816,#189817,
#189818,#189819,#189820,#189821,#189822,#189823,#189824,#189825,#189826,
#189827,#189828,#189829,#189830,#189831,#189832,#189833,#189834,#189835,
#189836,#189837,#189838,#189839,#189840,#189841,#189842,#189843,#189844,
#189845,#189846,#189847,#189848,#189849,#189850,#189851,#189852,#189853,
#189854,#189855,#189856,#189857,#189858,#189859,#189860,#189861,#189862,
#189863,#189864,#189865,#189866,#189867,#189868,#189869,#189870,#189871,
#189872,#189873,#189874,#189875,#189876,#189877,#189878,#189879,#189880,
#189881,#189882,#189883,#189884,#189885,#189886,#189887,#189888,#189889,
#189890,#189891,#189892,#189893,#189894,#189895,#189896,#189897,#189898,
#189899,#189900,#189901,#189902,#189903,#189904,#189905,#189906,#189907,
#189908,#189909,#189910,#189911,#189912,#189913,#189914,#189915,#189916,
#189917,#189918,#189919,#189920,#189921,#189922,#189923,#189924,#189925,
#189926,#189927,#189928,#189929,#189930,#189931,#189932,#189933,#189934),
 .UNSPECIFIED.,.F.,.F.)
B_SPLINE_CURVE_WITH_KNOTS((6,1,1,1,1,1,1,1,1,1,1,1,1,1,1,1,1,1,1,1,1,1,
1,1,1,1,1,1,1,1,1,1,1,1,1,1,1,1,1,1,1,1,1,1,1,1,1,1,1,1,1,1,1,1,1,1,1,1,
1,1,1,1,1,1,1,1,1,1,1,1,1,1,1,1,1,1,1,1,1,1,1,1,1,1,1,1,1,1,1,1,1,1,1,1,
1,1,1,1,1,1,1,1,1,1,1,1,1,1,1,1,1,1,1,1,1,1,1,1,1,1,1,1,1,1,1,1,1,1,1,1,
1,1,1,1,1,1,1,1,1,1,1,1,1,1,1,1,1,1,1,1,1,1,1,1,1,1,1,1,1,1,1,1,1,1,1,1,
1,1,1,1,1,1,1,1,1,1,1,1,1,1,1,1,1,1,1,1,1,1,1,1,1,1,1,1,1,1,1,1,1,1,6),
(-1.,-0.995000000000001,-0.990000000000001,-0.985000000000001,-0.980000000000001,
-0.975000000000001,-0.970000000000001,-0.965000000000001,-0.960000000000001,
-0.955000000000001,-0.950000000000001,-0.945000000000001,-0.940000000000001,
-0.935000000000001,-0.930000000000001,-0.925000000000001,-0.920000000000001,
-0.915000000000001,-0.910000000000001,-0.905000000000001,-0.900000000000001,
-0.895000000000001,-0.890000000000001,-0.885000000000001,-0.880000000000001,
-0.875000000000001,-0.870000000000001,-0.865000000000001,-0.860000000000001,
-0.855000000000001,-0.850000000000001,-0.845000000000001,-0.840000000000001,
-0.835000000000001,-0.830000000000001,-0.825000000000001,-0.820000000000001,
-0.815000000000001,-0.810000000000001,-0.805000000000001,-0.800000000000001,
-0.795000000000001,-0.790000000000001,-0.785000000000001,-0.780000000000001,
-0.775000000000001,-0.770000000000001,-0.765000000000001,-0.760000000000001,
-0.755000000000001,-0.750000000000001,-0.745000000000001,-0.740000000000001,
-0.735000000000001,-0.730000000000001,-0.725000000000001,-0.720000000000001,
-0.715000000000001,-0.710000000000001,-0.705000000000001,-0.700000000000001,
-0.695000000000001,-0.690000000000001,-0.685,-0.68,-0.675,-0.67,-0.665,
-0.66,-0.655,-0.65,-0.645,-0.64,-0.635,-0.63,-0.625,-0.62,-0.615,-0.61,
-0.605,-0.6,-0.595,-0.59,-0.585,-0.58,-0.575,-0.57,-0.565,-0.56,-0.555,
-0.55,-0.545,-0.54,-0.535,-0.53,-0.525,-0.52,-0.515,-0.51,-0.505,-0.5,-0.495,
-0.49,-0.485,-0.48,-0.475,-0.47,-0.465,-0.46,-0.455,-0.45,-0.445,-0.44,
-0.435,-0.43,-0.425,-0.42,-0.415,-0.41,-0.405,-0.4,-0.395,-0.39,-0.385,
-0.38,-0.375,-0.37,-0.365,-0.36,-0.355,-0.35,-0.345,-0.34,-0.335,-0.33,
-0.325,-0.32,-0.315,-0.31,-0.305,-0.3,-0.295,-0.29,-0.285,-0.28,-0.275,
-0.27,-0.265,-0.26,-0.255,-0.25,-0.245,-0.24,-0.235,-0.23,-0.225,-0.22,
-0.215,-0.21,-0.205,-0.2,-0.195,-0.19,-0.185,-0.18,-0.175,-0.17,-0.165,
-0.16,-0.155,-0.15,-0.145,-0.14,-0.135,-0.13,-0.125,-0.12,-0.115,-0.11,
-0.105,-0.1,-0.095,-0.09,-0.085,-0.08,-0.075,-0.07,-0.065,-0.06,-0.055,
-0.05,-0.045,-0.04,-0.035,-0.03,-0.025,-0.02,-0.015,-0.01,-0.005,0.),
 .UNSPECIFIED.)
CURVE()
GEOMETRIC_REPRESENTATION_ITEM()
RATIONAL_B_SPLINE_CURVE((1.,1.,1.,1.,1.,1.,1.,1.,1.,1.,1.,1.,1.,1.,1.,1.,
1.,1.,1.,1.,1.,1.,1.,1.,1.,1.,1.,1.,1.,1.,1.,1.,1.,1.,1.,1.,1.,1.,1.,1.,
1.,1.,1.,1.,1.,1.,1.,1.,1.,1.,1.,1.,1.,1.,1.,1.,1.,1.,1.,1.,1.,1.,1.,1.,
1.,1.,1.,1.,1.,1.,1.,1.,1.,1.,1.,1.,1.,1.,1.,1.,1.,1.,1.,1.,1.,1.,1.,1.,
1.,1.,1.,1.,1.,1.,1.,1.,1.,1.,1.,1.,1.,1.,1.,1.,1.,1.,1.,1.,1.,1.,1.,1.,
1.,1.,1.,1.,1.,1.,1.,1.,1.,1.,1.,1.,1.,1.,1.,1.,1.,1.,1.,1.,1.,1.,1.,1.,
1.,1.,1.,1.,1.,1.,1.,1.,1.,1.,1.,1.,1.,1.,1.,1.,1.,1.,1.,1.,1.,1.,1.,1.,
1.,1.,1.,1.,1.,1.,1.,1.,1.,1.,1.,1.,1.,1.,1.,1.,1.,1.,1.,1.,1.,1.,1.,1.,
1.,1.,1.,1.,1.,1.,1.,1.,1.,1.,1.,1.,1.,1.,1.,1.,1.,1.,1.,1.,1.))
REPRESENTATION_ITEM('')
);
#746=(
BOUNDED_CURVE()
B_SPLINE_CURVE(5,(#190347,#190348,#190349,#190350,#190351,#190352,#190353,
#190354,#190355,#190356,#190357,#190358,#190359,#190360,#190361,#190362,
#190363,#190364,#190365,#190366,#190367,#190368,#190369,#190370,#190371,
#190372,#190373,#190374,#190375,#190376,#190377,#190378,#190379,#190380,
#190381,#190382,#190383,#190384,#190385,#190386,#190387,#190388,#190389,
#190390,#190391,#190392,#190393,#190394,#190395,#190396,#190397,#190398,
#190399,#190400,#190401,#190402,#190403,#190404,#190405,#190406,#190407,
#190408,#190409,#190410,#190411,#190412,#190413,#190414,#190415,#190416,
#190417,#190418,#190419,#190420,#190421,#190422,#190423,#190424,#190425,
#190426,#190427,#190428,#190429,#190430,#190431,#190432,#190433,#190434,
#190435,#190436,#190437,#190438,#190439,#190440,#190441,#190442,#190443,
#190444,#190445,#190446,#190447,#190448,#190449,#190450,#190451,#190452,
#190453,#190454,#190455,#190456,#190457,#190458,#190459,#190460,#190461,
#190462,#190463,#190464,#190465,#190466,#190467,#190468,#190469,#190470,
#190471,#190472,#190473,#190474,#190475,#190476,#190477,#190478,#190479,
#190480,#190481,#190482,#190483,#190484,#190485,#190486,#190487,#190488,
#190489,#190490,#190491,#190492,#190493,#190494,#190495,#190496,#190497,
#190498,#190499,#190500,#190501,#190502,#190503,#190504,#190505,#190506,
#190507,#190508,#190509,#190510,#190511,#190512,#190513,#190514,#190515,
#190516,#190517,#190518,#190519,#190520,#190521,#190522,#190523,#190524,
#190525,#190526,#190527,#190528,#190529,#190530,#190531,#190532,#190533,
#190534,#190535,#190536,#190537,#190538,#190539,#190540,#190541,#190542,
#190543,#190544,#190545,#190546,#190547,#190548,#190549,#190550,#190551),
 .UNSPECIFIED.,.F.,.F.)
B_SPLINE_CURVE_WITH_KNOTS((6,1,1,1,1,1,1,1,1,1,1,1,1,1,1,1,1,1,1,1,1,1,
1,1,1,1,1,1,1,1,1,1,1,1,1,1,1,1,1,1,1,1,1,1,1,1,1,1,1,1,1,1,1,1,1,1,1,1,
1,1,1,1,1,1,1,1,1,1,1,1,1,1,1,1,1,1,1,1,1,1,1,1,1,1,1,1,1,1,1,1,1,1,1,1,
1,1,1,1,1,1,1,1,1,1,1,1,1,1,1,1,1,1,1,1,1,1,1,1,1,1,1,1,1,1,1,1,1,1,1,1,
1,1,1,1,1,1,1,1,1,1,1,1,1,1,1,1,1,1,1,1,1,1,1,1,1,1,1,1,1,1,1,1,1,1,1,1,
1,1,1,1,1,1,1,1,1,1,1,1,1,1,1,1,1,1,1,1,1,1,1,1,1,1,1,1,1,1,1,1,1,1,6),
(0.,0.005,0.01,0.015,0.02,0.025,0.03,0.035,0.04,0.045,0.05,0.055,0.06,0.065,
0.07,0.075,0.08,0.085,0.09,0.095,0.1,0.105,0.11,0.115,0.12,0.125,0.13,0.135,
0.14,0.145,0.15,0.155,0.16,0.165,0.17,0.175,0.18,0.185,0.19,0.195,0.2,0.205,
0.21,0.215,0.22,0.225,0.23,0.235,0.24,0.245,0.25,0.255,0.26,0.265,0.27,
0.275,0.28,0.285,0.29,0.295,0.3,0.305,0.31,0.315,0.32,0.325,0.33,0.335,
0.34,0.345,0.35,0.355,0.36,0.365,0.37,0.375,0.38,0.385,0.39,0.395,0.4,0.405,
0.41,0.415,0.42,0.425,0.43,0.435,0.44,0.445,0.45,0.455,0.46,0.465,0.47,
0.475,0.48,0.485,0.49,0.495,0.5,0.505,0.51,0.515,0.52,0.525,0.53,0.535,
0.54,0.545,0.55,0.555,0.56,0.565,0.57,0.575,0.58,0.585,0.59,0.595,0.6,0.605,
0.61,0.615,0.62,0.625,0.63,0.635,0.64,0.645,0.65,0.655,0.66,0.665,0.67,
0.675,0.68,0.685,0.690000000000001,0.695000000000001,0.700000000000001,
0.705000000000001,0.710000000000001,0.715000000000001,0.720000000000001,
0.725000000000001,0.730000000000001,0.735000000000001,0.740000000000001,
0.745000000000001,0.750000000000001,0.755000000000001,0.760000000000001,
0.765000000000001,0.770000000000001,0.775000000000001,0.780000000000001,
0.785000000000001,0.790000000000001,0.795000000000001,0.800000000000001,
0.805000000000001,0.810000000000001,0.815000000000001,0.820000000000001,
0.825000000000001,0.830000000000001,0.835000000000001,0.840000000000001,
0.845000000000001,0.850000000000001,0.855000000000001,0.860000000000001,
0.865000000000001,0.870000000000001,0.875000000000001,0.880000000000001,
0.885000000000001,0.890000000000001,0.895000000000001,0.900000000000001,
0.905000000000001,0.910000000000001,0.915000000000001,0.920000000000001,
0.925000000000001,0.930000000000001,0.935000000000001,0.940000000000001,
0.945000000000001,0.950000000000001,0.955000000000001,0.960000000000001,
0.965000000000001,0.970000000000001,0.975000000000001,0.980000000000001,
0.985000000000001,0.990000000000001,0.995000000000001,1.),.UNSPECIFIED.)
CURVE()
GEOMETRIC_REPRESENTATION_ITEM()
RATIONAL_B_SPLINE_CURVE((1.,1.,1.,1.,1.,1.,1.,1.,1.,1.,1.,1.,1.,1.,1.,1.,
1.,1.,1.,1.,1.,1.,1.,1.,1.,1.,1.,1.,1.,1.,1.,1.,1.,1.,1.,1.,1.,1.,1.,1.,
1.,1.,1.,1.,1.,1.,1.,1.,1.,1.,1.,1.,1.,1.,1.,1.,1.,1.,1.,1.,1.,1.,1.,1.,
1.,1.,1.,1.,1.,1.,1.,1.,1.,1.,1.,1.,1.,1.,1.,1.,1.,1.,1.,1.,1.,1.,1.,1.,
1.,1.,1.,1.,1.,1.,1.,1.,1.,1.,1.,1.,1.,1.,1.,1.,1.,1.,1.,1.,1.,1.,1.,1.,
1.,1.,1.,1.,1.,1.,1.,1.,1.,1.,1.,1.,1.,1.,1.,1.,1.,1.,1.,1.,1.,1.,1.,1.,
1.,1.,1.,1.,1.,1.,1.,1.,1.,1.,1.,1.,1.,1.,1.,1.,1.,1.,1.,1.,1.,1.,1.,1.,
1.,1.,1.,1.,1.,1.,1.,1.,1.,1.,1.,1.,1.,1.,1.,1.,1.,1.,1.,1.,1.,1.,1.,1.,
1.,1.,1.,1.,1.,1.,1.,1.,1.,1.,1.,1.,1.,1.,1.,1.,1.,1.,1.,1.,1.))
REPRESENTATION_ITEM('')
);
#747=(
BOUNDED_CURVE()
B_SPLINE_CURVE(5,(#190968,#190969,#190970,#190971,#190972,#190973,#190974,
#190975,#190976,#190977,#190978,#190979,#190980,#190981,#190982,#190983,
#190984,#190985,#190986,#190987,#190988,#190989,#190990,#190991,#190992,
#190993,#190994,#190995,#190996,#190997,#190998,#190999,#191000,#191001,
#191002,#191003,#191004,#191005,#191006,#191007,#191008,#191009,#191010,
#191011,#191012,#191013,#191014,#191015,#191016,#191017,#191018,#191019,
#191020,#191021,#191022,#191023,#191024,#191025,#191026,#191027,#191028,
#191029,#191030,#191031,#191032,#191033,#191034,#191035,#191036,#191037,
#191038,#191039,#191040,#191041,#191042,#191043,#191044,#191045,#191046,
#191047,#191048,#191049,#191050,#191051,#191052,#191053,#191054,#191055,
#191056,#191057,#191058,#191059,#191060,#191061,#191062,#191063,#191064,
#191065,#191066,#191067,#191068,#191069,#191070,#191071,#191072,#191073,
#191074,#191075,#191076,#191077,#191078,#191079,#191080,#191081,#191082,
#191083,#191084,#191085,#191086,#191087,#191088,#191089,#191090,#191091,
#191092,#191093,#191094,#191095,#191096,#191097,#191098,#191099,#191100,
#191101,#191102,#191103,#191104,#191105,#191106,#191107,#191108,#191109,
#191110,#191111,#191112,#191113,#191114,#191115,#191116,#191117,#191118,
#191119,#191120,#191121,#191122,#191123,#191124,#191125,#191126,#191127,
#191128,#191129,#191130,#191131,#191132,#191133,#191134,#191135,#191136,
#191137,#191138,#191139,#191140,#191141,#191142,#191143,#191144,#191145,
#191146,#191147,#191148,#191149,#191150,#191151,#191152,#191153,#191154,
#191155,#191156,#191157,#191158,#191159,#191160,#191161,#191162,#191163,
#191164,#191165,#191166,#191167,#191168,#191169,#191170,#191171,#191172),
 .UNSPECIFIED.,.F.,.F.)
B_SPLINE_CURVE_WITH_KNOTS((6,1,1,1,1,1,1,1,1,1,1,1,1,1,1,1,1,1,1,1,1,1,
1,1,1,1,1,1,1,1,1,1,1,1,1,1,1,1,1,1,1,1,1,1,1,1,1,1,1,1,1,1,1,1,1,1,1,1,
1,1,1,1,1,1,1,1,1,1,1,1,1,1,1,1,1,1,1,1,1,1,1,1,1,1,1,1,1,1,1,1,1,1,1,1,
1,1,1,1,1,1,1,1,1,1,1,1,1,1,1,1,1,1,1,1,1,1,1,1,1,1,1,1,1,1,1,1,1,1,1,1,
1,1,1,1,1,1,1,1,1,1,1,1,1,1,1,1,1,1,1,1,1,1,1,1,1,1,1,1,1,1,1,1,1,1,1,1,
1,1,1,1,1,1,1,1,1,1,1,1,1,1,1,1,1,1,1,1,1,1,1,1,1,1,1,1,1,1,1,1,1,1,6),
(-1.,-0.995000000000001,-0.990000000000001,-0.985000000000001,-0.980000000000001,
-0.975000000000001,-0.970000000000001,-0.965000000000001,-0.960000000000001,
-0.955000000000001,-0.950000000000001,-0.945000000000001,-0.940000000000001,
-0.935000000000001,-0.930000000000001,-0.925000000000001,-0.920000000000001,
-0.915000000000001,-0.910000000000001,-0.905000000000001,-0.900000000000001,
-0.895000000000001,-0.890000000000001,-0.885000000000001,-0.880000000000001,
-0.875000000000001,-0.870000000000001,-0.865000000000001,-0.860000000000001,
-0.855000000000001,-0.850000000000001,-0.845000000000001,-0.840000000000001,
-0.835000000000001,-0.830000000000001,-0.825000000000001,-0.820000000000001,
-0.815000000000001,-0.810000000000001,-0.805000000000001,-0.800000000000001,
-0.795000000000001,-0.790000000000001,-0.785000000000001,-0.780000000000001,
-0.775000000000001,-0.770000000000001,-0.765000000000001,-0.760000000000001,
-0.755000000000001,-0.750000000000001,-0.745000000000001,-0.740000000000001,
-0.735000000000001,-0.730000000000001,-0.725000000000001,-0.720000000000001,
-0.715000000000001,-0.710000000000001,-0.705000000000001,-0.700000000000001,
-0.695000000000001,-0.690000000000001,-0.685,-0.68,-0.675,-0.67,-0.665,
-0.66,-0.655,-0.65,-0.645,-0.64,-0.635,-0.63,-0.625,-0.62,-0.615,-0.61,
-0.605,-0.6,-0.595,-0.59,-0.585,-0.58,-0.575,-0.57,-0.565,-0.56,-0.555,
-0.55,-0.545,-0.54,-0.535,-0.53,-0.525,-0.52,-0.515,-0.51,-0.505,-0.5,-0.495,
-0.49,-0.485,-0.48,-0.475,-0.47,-0.465,-0.46,-0.455,-0.45,-0.445,-0.44,
-0.435,-0.43,-0.425,-0.42,-0.415,-0.41,-0.405,-0.4,-0.395,-0.39,-0.385,
-0.38,-0.375,-0.37,-0.365,-0.36,-0.355,-0.35,-0.345,-0.34,-0.335,-0.33,
-0.325,-0.32,-0.315,-0.31,-0.305,-0.3,-0.295,-0.29,-0.285,-0.28,-0.275,
-0.27,-0.265,-0.26,-0.255,-0.25,-0.245,-0.24,-0.235,-0.23,-0.225,-0.22,
-0.215,-0.21,-0.205,-0.2,-0.195,-0.19,-0.185,-0.18,-0.175,-0.17,-0.165,
-0.16,-0.155,-0.15,-0.145,-0.14,-0.135,-0.13,-0.125,-0.12,-0.115,-0.11,
-0.105,-0.1,-0.095,-0.09,-0.085,-0.08,-0.075,-0.07,-0.065,-0.06,-0.055,
-0.05,-0.045,-0.04,-0.035,-0.03,-0.025,-0.02,-0.015,-0.01,-0.005,0.),
 .UNSPECIFIED.)
CURVE()
GEOMETRIC_REPRESENTATION_ITEM()
RATIONAL_B_SPLINE_CURVE((1.,1.,1.,1.,1.,1.,1.,1.,1.,1.,1.,1.,1.,1.,1.,1.,
1.,1.,1.,1.,1.,1.,1.,1.,1.,1.,1.,1.,1.,1.,1.,1.,1.,1.,1.,1.,1.,1.,1.,1.,
1.,1.,1.,1.,1.,1.,1.,1.,1.,1.,1.,1.,1.,1.,1.,1.,1.,1.,1.,1.,1.,1.,1.,1.,
1.,1.,1.,1.,1.,1.,1.,1.,1.,1.,1.,1.,1.,1.,1.,1.,1.,1.,1.,1.,1.,1.,1.,1.,
1.,1.,1.,1.,1.,1.,1.,1.,1.,1.,1.,1.,1.,1.,1.,1.,1.,1.,1.,1.,1.,1.,1.,1.,
1.,1.,1.,1.,1.,1.,1.,1.,1.,1.,1.,1.,1.,1.,1.,1.,1.,1.,1.,1.,1.,1.,1.,1.,
1.,1.,1.,1.,1.,1.,1.,1.,1.,1.,1.,1.,1.,1.,1.,1.,1.,1.,1.,1.,1.,1.,1.,1.,
1.,1.,1.,1.,1.,1.,1.,1.,1.,1.,1.,1.,1.,1.,1.,1.,1.,1.,1.,1.,1.,1.,1.,1.,
1.,1.,1.,1.,1.,1.,1.,1.,1.,1.,1.,1.,1.,1.,1.,1.,1.,1.,1.,1.,1.))
REPRESENTATION_ITEM('')
);
#748=(
BOUNDED_CURVE()
B_SPLINE_CURVE(5,(#191585,#191586,#191587,#191588,#191589,#191590,#191591,
#191592,#191593,#191594,#191595,#191596,#191597,#191598,#191599,#191600,
#191601,#191602,#191603,#191604,#191605,#191606,#191607,#191608,#191609,
#191610,#191611,#191612,#191613,#191614,#191615,#191616,#191617,#191618,
#191619,#191620,#191621,#191622,#191623,#191624,#191625,#191626,#191627,
#191628,#191629,#191630,#191631,#191632,#191633,#191634,#191635,#191636,
#191637,#191638,#191639,#191640,#191641,#191642,#191643,#191644,#191645,
#191646,#191647,#191648,#191649,#191650,#191651,#191652,#191653,#191654,
#191655,#191656,#191657,#191658,#191659,#191660,#191661,#191662,#191663,
#191664,#191665,#191666,#191667,#191668,#191669,#191670,#191671,#191672,
#191673,#191674,#191675,#191676,#191677,#191678,#191679,#191680,#191681,
#191682,#191683,#191684,#191685,#191686,#191687,#191688,#191689,#191690,
#191691,#191692,#191693,#191694,#191695,#191696,#191697,#191698,#191699,
#191700,#191701,#191702,#191703,#191704,#191705,#191706,#191707,#191708,
#191709,#191710,#191711,#191712,#191713,#191714,#191715,#191716,#191717,
#191718,#191719,#191720,#191721,#191722,#191723,#191724,#191725,#191726,
#191727,#191728,#191729,#191730,#191731,#191732,#191733,#191734,#191735,
#191736,#191737,#191738,#191739,#191740,#191741,#191742,#191743,#191744,
#191745,#191746,#191747,#191748,#191749,#191750,#191751,#191752,#191753,
#191754,#191755,#191756,#191757,#191758,#191759,#191760,#191761,#191762,
#191763,#191764,#191765,#191766,#191767,#191768,#191769,#191770,#191771,
#191772,#191773,#191774,#191775,#191776,#191777,#191778,#191779,#191780,
#191781,#191782,#191783,#191784,#191785,#191786,#191787,#191788,#191789),
 .UNSPECIFIED.,.F.,.F.)
B_SPLINE_CURVE_WITH_KNOTS((6,1,1,1,1,1,1,1,1,1,1,1,1,1,1,1,1,1,1,1,1,1,
1,1,1,1,1,1,1,1,1,1,1,1,1,1,1,1,1,1,1,1,1,1,1,1,1,1,1,1,1,1,1,1,1,1,1,1,
1,1,1,1,1,1,1,1,1,1,1,1,1,1,1,1,1,1,1,1,1,1,1,1,1,1,1,1,1,1,1,1,1,1,1,1,
1,1,1,1,1,1,1,1,1,1,1,1,1,1,1,1,1,1,1,1,1,1,1,1,1,1,1,1,1,1,1,1,1,1,1,1,
1,1,1,1,1,1,1,1,1,1,1,1,1,1,1,1,1,1,1,1,1,1,1,1,1,1,1,1,1,1,1,1,1,1,1,1,
1,1,1,1,1,1,1,1,1,1,1,1,1,1,1,1,1,1,1,1,1,1,1,1,1,1,1,1,1,1,1,1,1,1,6),
(0.,0.005,0.01,0.015,0.02,0.025,0.03,0.035,0.04,0.045,0.05,0.055,0.06,0.065,
0.07,0.075,0.08,0.085,0.09,0.095,0.1,0.105,0.11,0.115,0.12,0.125,0.13,0.135,
0.14,0.145,0.15,0.155,0.16,0.165,0.17,0.175,0.18,0.185,0.19,0.195,0.2,0.205,
0.21,0.215,0.22,0.225,0.23,0.235,0.24,0.245,0.25,0.255,0.26,0.265,0.27,
0.275,0.28,0.285,0.29,0.295,0.3,0.305,0.31,0.315,0.32,0.325,0.33,0.335,
0.34,0.345,0.35,0.355,0.36,0.365,0.37,0.375,0.38,0.385,0.39,0.395,0.4,0.405,
0.41,0.415,0.42,0.425,0.43,0.435,0.44,0.445,0.45,0.455,0.46,0.465,0.47,
0.475,0.48,0.485,0.49,0.495,0.5,0.505,0.51,0.515,0.52,0.525,0.53,0.535,
0.54,0.545,0.55,0.555,0.56,0.565,0.57,0.575,0.58,0.585,0.59,0.595,0.6,0.605,
0.61,0.615,0.62,0.625,0.63,0.635,0.64,0.645,0.65,0.655,0.66,0.665,0.67,
0.675,0.68,0.685,0.690000000000001,0.695000000000001,0.700000000000001,
0.705000000000001,0.710000000000001,0.715000000000001,0.720000000000001,
0.725000000000001,0.730000000000001,0.735000000000001,0.740000000000001,
0.745000000000001,0.750000000000001,0.755000000000001,0.760000000000001,
0.765000000000001,0.770000000000001,0.775000000000001,0.780000000000001,
0.785000000000001,0.790000000000001,0.795000000000001,0.800000000000001,
0.805000000000001,0.810000000000001,0.815000000000001,0.820000000000001,
0.825000000000001,0.830000000000001,0.835000000000001,0.840000000000001,
0.845000000000001,0.850000000000001,0.855000000000001,0.860000000000001,
0.865000000000001,0.870000000000001,0.875000000000001,0.880000000000001,
0.885000000000001,0.890000000000001,0.895000000000001,0.900000000000001,
0.905000000000001,0.910000000000001,0.915000000000001,0.920000000000001,
0.925000000000001,0.930000000000001,0.935000000000001,0.940000000000001,
0.945000000000001,0.950000000000001,0.955000000000001,0.960000000000001,
0.965000000000001,0.970000000000001,0.975000000000001,0.980000000000001,
0.985000000000001,0.990000000000001,0.995000000000001,1.),.UNSPECIFIED.)
CURVE()
GEOMETRIC_REPRESENTATION_ITEM()
RATIONAL_B_SPLINE_CURVE((1.,1.,1.,1.,1.,1.,1.,1.,1.,1.,1.,1.,1.,1.,1.,1.,
1.,1.,1.,1.,1.,1.,1.,1.,1.,1.,1.,1.,1.,1.,1.,1.,1.,1.,1.,1.,1.,1.,1.,1.,
1.,1.,1.,1.,1.,1.,1.,1.,1.,1.,1.,1.,1.,1.,1.,1.,1.,1.,1.,1.,1.,1.,1.,1.,
1.,1.,1.,1.,1.,1.,1.,1.,1.,1.,1.,1.,1.,1.,1.,1.,1.,1.,1.,1.,1.,1.,1.,1.,
1.,1.,1.,1.,1.,1.,1.,1.,1.,1.,1.,1.,1.,1.,1.,1.,1.,1.,1.,1.,1.,1.,1.,1.,
1.,1.,1.,1.,1.,1.,1.,1.,1.,1.,1.,1.,1.,1.,1.,1.,1.,1.,1.,1.,1.,1.,1.,1.,
1.,1.,1.,1.,1.,1.,1.,1.,1.,1.,1.,1.,1.,1.,1.,1.,1.,1.,1.,1.,1.,1.,1.,1.,
1.,1.,1.,1.,1.,1.,1.,1.,1.,1.,1.,1.,1.,1.,1.,1.,1.,1.,1.,1.,1.,1.,1.,1.,
1.,1.,1.,1.,1.,1.,1.,1.,1.,1.,1.,1.,1.,1.,1.,1.,1.,1.,1.,1.,1.))
REPRESENTATION_ITEM('')
);
#749=(
BOUNDED_CURVE()
B_SPLINE_CURVE(5,(#192206,#192207,#192208,#192209,#192210,#192211,#192212,
#192213,#192214,#192215,#192216,#192217,#192218,#192219,#192220,#192221,
#192222,#192223,#192224,#192225,#192226,#192227,#192228,#192229,#192230,
#192231,#192232,#192233,#192234,#192235,#192236,#192237,#192238,#192239,
#192240,#192241,#192242,#192243,#192244,#192245,#192246,#192247,#192248,
#192249,#192250,#192251,#192252,#192253,#192254,#192255,#192256,#192257,
#192258,#192259,#192260,#192261,#192262,#192263,#192264,#192265,#192266,
#192267,#192268,#192269,#192270,#192271,#192272,#192273,#192274,#192275,
#192276,#192277,#192278,#192279,#192280,#192281,#192282,#192283,#192284,
#192285,#192286,#192287,#192288,#192289,#192290,#192291,#192292,#192293,
#192294,#192295,#192296,#192297,#192298,#192299,#192300,#192301,#192302,
#192303,#192304,#192305,#192306,#192307,#192308,#192309,#192310,#192311,
#192312,#192313,#192314,#192315,#192316,#192317,#192318,#192319,#192320,
#192321,#192322,#192323,#192324,#192325,#192326,#192327,#192328,#192329,
#192330,#192331,#192332,#192333,#192334,#192335,#192336,#192337,#192338,
#192339,#192340,#192341,#192342,#192343,#192344,#192345,#192346,#192347,
#192348,#192349,#192350,#192351,#192352,#192353,#192354,#192355,#192356,
#192357,#192358,#192359,#192360,#192361,#192362,#192363,#192364,#192365,
#192366,#192367,#192368,#192369,#192370,#192371,#192372,#192373,#192374,
#192375,#192376,#192377,#192378,#192379,#192380,#192381,#192382,#192383,
#192384,#192385,#192386,#192387,#192388,#192389,#192390,#192391,#192392,
#192393,#192394,#192395,#192396,#192397,#192398,#192399,#192400,#192401,
#192402,#192403,#192404,#192405,#192406,#192407,#192408,#192409,#192410),
 .UNSPECIFIED.,.F.,.F.)
B_SPLINE_CURVE_WITH_KNOTS((6,1,1,1,1,1,1,1,1,1,1,1,1,1,1,1,1,1,1,1,1,1,
1,1,1,1,1,1,1,1,1,1,1,1,1,1,1,1,1,1,1,1,1,1,1,1,1,1,1,1,1,1,1,1,1,1,1,1,
1,1,1,1,1,1,1,1,1,1,1,1,1,1,1,1,1,1,1,1,1,1,1,1,1,1,1,1,1,1,1,1,1,1,1,1,
1,1,1,1,1,1,1,1,1,1,1,1,1,1,1,1,1,1,1,1,1,1,1,1,1,1,1,1,1,1,1,1,1,1,1,1,
1,1,1,1,1,1,1,1,1,1,1,1,1,1,1,1,1,1,1,1,1,1,1,1,1,1,1,1,1,1,1,1,1,1,1,1,
1,1,1,1,1,1,1,1,1,1,1,1,1,1,1,1,1,1,1,1,1,1,1,1,1,1,1,1,1,1,1,1,1,1,6),
(-1.,-0.995000000000001,-0.990000000000001,-0.985000000000001,-0.980000000000001,
-0.975000000000001,-0.970000000000001,-0.965000000000001,-0.960000000000001,
-0.955000000000001,-0.950000000000001,-0.945000000000001,-0.940000000000001,
-0.935000000000001,-0.930000000000001,-0.925000000000001,-0.920000000000001,
-0.915000000000001,-0.910000000000001,-0.905000000000001,-0.900000000000001,
-0.895000000000001,-0.890000000000001,-0.885000000000001,-0.880000000000001,
-0.875000000000001,-0.870000000000001,-0.865000000000001,-0.860000000000001,
-0.855000000000001,-0.850000000000001,-0.845000000000001,-0.840000000000001,
-0.835000000000001,-0.830000000000001,-0.825000000000001,-0.820000000000001,
-0.815000000000001,-0.810000000000001,-0.805000000000001,-0.800000000000001,
-0.795000000000001,-0.790000000000001,-0.785000000000001,-0.780000000000001,
-0.775000000000001,-0.770000000000001,-0.765000000000001,-0.760000000000001,
-0.755000000000001,-0.750000000000001,-0.745000000000001,-0.740000000000001,
-0.735000000000001,-0.730000000000001,-0.725000000000001,-0.720000000000001,
-0.715000000000001,-0.710000000000001,-0.705000000000001,-0.700000000000001,
-0.695000000000001,-0.690000000000001,-0.685,-0.68,-0.675,-0.67,-0.665,
-0.66,-0.655,-0.65,-0.645,-0.64,-0.635,-0.63,-0.625,-0.62,-0.615,-0.61,
-0.605,-0.6,-0.595,-0.59,-0.585,-0.58,-0.575,-0.57,-0.565,-0.56,-0.555,
-0.55,-0.545,-0.54,-0.535,-0.53,-0.525,-0.52,-0.515,-0.51,-0.505,-0.5,-0.495,
-0.49,-0.485,-0.48,-0.475,-0.47,-0.465,-0.46,-0.455,-0.45,-0.445,-0.44,
-0.435,-0.43,-0.425,-0.42,-0.415,-0.41,-0.405,-0.4,-0.395,-0.39,-0.385,
-0.38,-0.375,-0.37,-0.365,-0.36,-0.355,-0.35,-0.345,-0.34,-0.335,-0.33,
-0.325,-0.32,-0.315,-0.31,-0.305,-0.3,-0.295,-0.29,-0.285,-0.28,-0.275,
-0.27,-0.265,-0.26,-0.255,-0.25,-0.245,-0.24,-0.235,-0.23,-0.225,-0.22,
-0.215,-0.21,-0.205,-0.2,-0.195,-0.19,-0.185,-0.18,-0.175,-0.17,-0.165,
-0.16,-0.155,-0.15,-0.145,-0.14,-0.135,-0.13,-0.125,-0.12,-0.115,-0.11,
-0.105,-0.1,-0.095,-0.09,-0.085,-0.08,-0.075,-0.07,-0.065,-0.06,-0.055,
-0.05,-0.045,-0.04,-0.035,-0.03,-0.025,-0.02,-0.015,-0.01,-0.005,0.),
 .UNSPECIFIED.)
CURVE()
GEOMETRIC_REPRESENTATION_ITEM()
RATIONAL_B_SPLINE_CURVE((1.,1.,1.,1.,1.,1.,1.,1.,1.,1.,1.,1.,1.,1.,1.,1.,
1.,1.,1.,1.,1.,1.,1.,1.,1.,1.,1.,1.,1.,1.,1.,1.,1.,1.,1.,1.,1.,1.,1.,1.,
1.,1.,1.,1.,1.,1.,1.,1.,1.,1.,1.,1.,1.,1.,1.,1.,1.,1.,1.,1.,1.,1.,1.,1.,
1.,1.,1.,1.,1.,1.,1.,1.,1.,1.,1.,1.,1.,1.,1.,1.,1.,1.,1.,1.,1.,1.,1.,1.,
1.,1.,1.,1.,1.,1.,1.,1.,1.,1.,1.,1.,1.,1.,1.,1.,1.,1.,1.,1.,1.,1.,1.,1.,
1.,1.,1.,1.,1.,1.,1.,1.,1.,1.,1.,1.,1.,1.,1.,1.,1.,1.,1.,1.,1.,1.,1.,1.,
1.,1.,1.,1.,1.,1.,1.,1.,1.,1.,1.,1.,1.,1.,1.,1.,1.,1.,1.,1.,1.,1.,1.,1.,
1.,1.,1.,1.,1.,1.,1.,1.,1.,1.,1.,1.,1.,1.,1.,1.,1.,1.,1.,1.,1.,1.,1.,1.,
1.,1.,1.,1.,1.,1.,1.,1.,1.,1.,1.,1.,1.,1.,1.,1.,1.,1.,1.,1.,1.))
REPRESENTATION_ITEM('')
);
#750=(
BOUNDED_CURVE()
B_SPLINE_CURVE(5,(#192823,#192824,#192825,#192826,#192827,#192828,#192829,
#192830,#192831,#192832,#192833,#192834,#192835,#192836,#192837,#192838,
#192839,#192840,#192841,#192842,#192843,#192844,#192845,#192846,#192847,
#192848,#192849,#192850,#192851,#192852,#192853,#192854,#192855,#192856,
#192857,#192858,#192859,#192860,#192861,#192862,#192863,#192864,#192865,
#192866,#192867,#192868,#192869,#192870,#192871,#192872,#192873,#192874,
#192875,#192876,#192877,#192878,#192879,#192880,#192881,#192882,#192883,
#192884,#192885,#192886,#192887,#192888,#192889,#192890,#192891,#192892,
#192893,#192894,#192895,#192896,#192897,#192898,#192899,#192900,#192901,
#192902,#192903,#192904,#192905,#192906,#192907,#192908,#192909,#192910,
#192911,#192912,#192913,#192914,#192915,#192916,#192917,#192918,#192919,
#192920,#192921,#192922,#192923,#192924,#192925,#192926,#192927,#192928,
#192929,#192930,#192931,#192932,#192933,#192934,#192935,#192936,#192937,
#192938,#192939,#192940,#192941,#192942,#192943,#192944,#192945,#192946,
#192947,#192948,#192949,#192950,#192951,#192952,#192953,#192954,#192955,
#192956,#192957,#192958,#192959,#192960,#192961,#192962,#192963,#192964,
#192965,#192966,#192967,#192968,#192969,#192970,#192971,#192972,#192973,
#192974,#192975,#192976,#192977,#192978,#192979,#192980,#192981,#192982,
#192983,#192984,#192985,#192986,#192987,#192988,#192989,#192990,#192991,
#192992,#192993,#192994,#192995,#192996,#192997,#192998,#192999,#193000,
#193001,#193002,#193003,#193004,#193005,#193006,#193007,#193008,#193009,
#193010,#193011,#193012,#193013,#193014,#193015,#193016,#193017,#193018,
#193019,#193020,#193021,#193022,#193023,#193024,#193025,#193026,#193027),
 .UNSPECIFIED.,.F.,.F.)
B_SPLINE_CURVE_WITH_KNOTS((6,1,1,1,1,1,1,1,1,1,1,1,1,1,1,1,1,1,1,1,1,1,
1,1,1,1,1,1,1,1,1,1,1,1,1,1,1,1,1,1,1,1,1,1,1,1,1,1,1,1,1,1,1,1,1,1,1,1,
1,1,1,1,1,1,1,1,1,1,1,1,1,1,1,1,1,1,1,1,1,1,1,1,1,1,1,1,1,1,1,1,1,1,1,1,
1,1,1,1,1,1,1,1,1,1,1,1,1,1,1,1,1,1,1,1,1,1,1,1,1,1,1,1,1,1,1,1,1,1,1,1,
1,1,1,1,1,1,1,1,1,1,1,1,1,1,1,1,1,1,1,1,1,1,1,1,1,1,1,1,1,1,1,1,1,1,1,1,
1,1,1,1,1,1,1,1,1,1,1,1,1,1,1,1,1,1,1,1,1,1,1,1,1,1,1,1,1,1,1,1,1,1,6),
(0.,0.005,0.01,0.015,0.02,0.025,0.03,0.035,0.04,0.045,0.05,0.055,0.06,0.065,
0.07,0.075,0.08,0.085,0.09,0.095,0.1,0.105,0.11,0.115,0.12,0.125,0.13,0.135,
0.14,0.145,0.15,0.155,0.16,0.165,0.17,0.175,0.18,0.185,0.19,0.195,0.2,0.205,
0.21,0.215,0.22,0.225,0.23,0.235,0.24,0.245,0.25,0.255,0.26,0.265,0.27,
0.275,0.28,0.285,0.29,0.295,0.3,0.305,0.31,0.315,0.32,0.325,0.33,0.335,
0.34,0.345,0.35,0.355,0.36,0.365,0.37,0.375,0.38,0.385,0.39,0.395,0.4,0.405,
0.41,0.415,0.42,0.425,0.43,0.435,0.44,0.445,0.45,0.455,0.46,0.465,0.47,
0.475,0.48,0.485,0.49,0.495,0.5,0.505,0.51,0.515,0.52,0.525,0.53,0.535,
0.54,0.545,0.55,0.555,0.56,0.565,0.57,0.575,0.58,0.585,0.59,0.595,0.6,0.605,
0.61,0.615,0.62,0.625,0.63,0.635,0.64,0.645,0.65,0.655,0.66,0.665,0.67,
0.675,0.68,0.685,0.690000000000001,0.695000000000001,0.700000000000001,
0.705000000000001,0.710000000000001,0.715000000000001,0.720000000000001,
0.725000000000001,0.730000000000001,0.735000000000001,0.740000000000001,
0.745000000000001,0.750000000000001,0.755000000000001,0.760000000000001,
0.765000000000001,0.770000000000001,0.775000000000001,0.780000000000001,
0.785000000000001,0.790000000000001,0.795000000000001,0.800000000000001,
0.805000000000001,0.810000000000001,0.815000000000001,0.820000000000001,
0.825000000000001,0.830000000000001,0.835000000000001,0.840000000000001,
0.845000000000001,0.850000000000001,0.855000000000001,0.860000000000001,
0.865000000000001,0.870000000000001,0.875000000000001,0.880000000000001,
0.885000000000001,0.890000000000001,0.895000000000001,0.900000000000001,
0.905000000000001,0.910000000000001,0.915000000000001,0.920000000000001,
0.925000000000001,0.930000000000001,0.935000000000001,0.940000000000001,
0.945000000000001,0.950000000000001,0.955000000000001,0.960000000000001,
0.965000000000001,0.970000000000001,0.975000000000001,0.980000000000001,
0.985000000000001,0.990000000000001,0.995000000000001,1.),.UNSPECIFIED.)
CURVE()
GEOMETRIC_REPRESENTATION_ITEM()
RATIONAL_B_SPLINE_CURVE((1.,1.,1.,1.,1.,1.,1.,1.,1.,1.,1.,1.,1.,1.,1.,1.,
1.,1.,1.,1.,1.,1.,1.,1.,1.,1.,1.,1.,1.,1.,1.,1.,1.,1.,1.,1.,1.,1.,1.,1.,
1.,1.,1.,1.,1.,1.,1.,1.,1.,1.,1.,1.,1.,1.,1.,1.,1.,1.,1.,1.,1.,1.,1.,1.,
1.,1.,1.,1.,1.,1.,1.,1.,1.,1.,1.,1.,1.,1.,1.,1.,1.,1.,1.,1.,1.,1.,1.,1.,
1.,1.,1.,1.,1.,1.,1.,1.,1.,1.,1.,1.,1.,1.,1.,1.,1.,1.,1.,1.,1.,1.,1.,1.,
1.,1.,1.,1.,1.,1.,1.,1.,1.,1.,1.,1.,1.,1.,1.,1.,1.,1.,1.,1.,1.,1.,1.,1.,
1.,1.,1.,1.,1.,1.,1.,1.,1.,1.,1.,1.,1.,1.,1.,1.,1.,1.,1.,1.,1.,1.,1.,1.,
1.,1.,1.,1.,1.,1.,1.,1.,1.,1.,1.,1.,1.,1.,1.,1.,1.,1.,1.,1.,1.,1.,1.,1.,
1.,1.,1.,1.,1.,1.,1.,1.,1.,1.,1.,1.,1.,1.,1.,1.,1.,1.,1.,1.,1.))
REPRESENTATION_ITEM('')
);
#751=(
BOUNDED_CURVE()
B_SPLINE_CURVE(5,(#193444,#193445,#193446,#193447,#193448,#193449,#193450,
#193451,#193452,#193453,#193454,#193455,#193456,#193457,#193458,#193459,
#193460,#193461,#193462,#193463,#193464,#193465,#193466,#193467,#193468,
#193469,#193470,#193471,#193472,#193473,#193474,#193475,#193476,#193477,
#193478,#193479,#193480,#193481,#193482,#193483,#193484,#193485,#193486,
#193487,#193488,#193489,#193490,#193491,#193492,#193493,#193494,#193495,
#193496,#193497,#193498,#193499,#193500,#193501,#193502,#193503,#193504,
#193505,#193506,#193507,#193508,#193509,#193510,#193511,#193512,#193513,
#193514,#193515,#193516,#193517,#193518,#193519,#193520,#193521,#193522,
#193523,#193524,#193525,#193526,#193527,#193528,#193529,#193530,#193531,
#193532,#193533,#193534,#193535,#193536,#193537,#193538,#193539,#193540,
#193541,#193542,#193543,#193544,#193545,#193546,#193547,#193548,#193549,
#193550,#193551,#193552,#193553,#193554,#193555,#193556,#193557,#193558,
#193559,#193560,#193561,#193562,#193563,#193564,#193565,#193566,#193567,
#193568,#193569,#193570,#193571,#193572,#193573,#193574,#193575,#193576,
#193577,#193578,#193579,#193580,#193581,#193582,#193583,#193584,#193585,
#193586,#193587,#193588,#193589,#193590,#193591,#193592,#193593,#193594,
#193595,#193596,#193597,#193598,#193599,#193600,#193601,#193602,#193603,
#193604,#193605,#193606,#193607,#193608,#193609,#193610,#193611,#193612,
#193613,#193614,#193615,#193616,#193617,#193618,#193619,#193620,#193621,
#193622,#193623,#193624,#193625,#193626,#193627,#193628,#193629,#193630,
#193631,#193632,#193633,#193634,#193635,#193636,#193637,#193638,#193639,
#193640,#193641,#193642,#193643,#193644,#193645,#193646,#193647,#193648),
 .UNSPECIFIED.,.F.,.F.)
B_SPLINE_CURVE_WITH_KNOTS((6,1,1,1,1,1,1,1,1,1,1,1,1,1,1,1,1,1,1,1,1,1,
1,1,1,1,1,1,1,1,1,1,1,1,1,1,1,1,1,1,1,1,1,1,1,1,1,1,1,1,1,1,1,1,1,1,1,1,
1,1,1,1,1,1,1,1,1,1,1,1,1,1,1,1,1,1,1,1,1,1,1,1,1,1,1,1,1,1,1,1,1,1,1,1,
1,1,1,1,1,1,1,1,1,1,1,1,1,1,1,1,1,1,1,1,1,1,1,1,1,1,1,1,1,1,1,1,1,1,1,1,
1,1,1,1,1,1,1,1,1,1,1,1,1,1,1,1,1,1,1,1,1,1,1,1,1,1,1,1,1,1,1,1,1,1,1,1,
1,1,1,1,1,1,1,1,1,1,1,1,1,1,1,1,1,1,1,1,1,1,1,1,1,1,1,1,1,1,1,1,1,1,6),
(-1.,-0.995000000000001,-0.990000000000001,-0.985000000000001,-0.980000000000001,
-0.975000000000001,-0.970000000000001,-0.965000000000001,-0.960000000000001,
-0.955000000000001,-0.950000000000001,-0.945000000000001,-0.940000000000001,
-0.935000000000001,-0.930000000000001,-0.925000000000001,-0.920000000000001,
-0.915000000000001,-0.910000000000001,-0.905000000000001,-0.900000000000001,
-0.895000000000001,-0.890000000000001,-0.885000000000001,-0.880000000000001,
-0.875000000000001,-0.870000000000001,-0.865000000000001,-0.860000000000001,
-0.855000000000001,-0.850000000000001,-0.845000000000001,-0.840000000000001,
-0.835000000000001,-0.830000000000001,-0.825000000000001,-0.820000000000001,
-0.815000000000001,-0.810000000000001,-0.805000000000001,-0.800000000000001,
-0.795000000000001,-0.790000000000001,-0.785000000000001,-0.780000000000001,
-0.775000000000001,-0.770000000000001,-0.765000000000001,-0.760000000000001,
-0.755000000000001,-0.750000000000001,-0.745000000000001,-0.740000000000001,
-0.735000000000001,-0.730000000000001,-0.725000000000001,-0.720000000000001,
-0.715000000000001,-0.710000000000001,-0.705000000000001,-0.700000000000001,
-0.695000000000001,-0.690000000000001,-0.685,-0.68,-0.675,-0.67,-0.665,
-0.66,-0.655,-0.65,-0.645,-0.64,-0.635,-0.63,-0.625,-0.62,-0.615,-0.61,
-0.605,-0.6,-0.595,-0.59,-0.585,-0.58,-0.575,-0.57,-0.565,-0.56,-0.555,
-0.55,-0.545,-0.54,-0.535,-0.53,-0.525,-0.52,-0.515,-0.51,-0.505,-0.5,-0.495,
-0.49,-0.485,-0.48,-0.475,-0.47,-0.465,-0.46,-0.455,-0.45,-0.445,-0.44,
-0.435,-0.43,-0.425,-0.42,-0.415,-0.41,-0.405,-0.4,-0.395,-0.39,-0.385,
-0.38,-0.375,-0.37,-0.365,-0.36,-0.355,-0.35,-0.345,-0.34,-0.335,-0.33,
-0.325,-0.32,-0.315,-0.31,-0.305,-0.3,-0.295,-0.29,-0.285,-0.28,-0.275,
-0.27,-0.265,-0.26,-0.255,-0.25,-0.245,-0.24,-0.235,-0.23,-0.225,-0.22,
-0.215,-0.21,-0.205,-0.2,-0.195,-0.19,-0.185,-0.18,-0.175,-0.17,-0.165,
-0.16,-0.155,-0.15,-0.145,-0.14,-0.135,-0.13,-0.125,-0.12,-0.115,-0.11,
-0.105,-0.1,-0.095,-0.09,-0.085,-0.08,-0.075,-0.07,-0.065,-0.06,-0.055,
-0.05,-0.045,-0.04,-0.035,-0.03,-0.025,-0.02,-0.015,-0.01,-0.005,0.),
 .UNSPECIFIED.)
CURVE()
GEOMETRIC_REPRESENTATION_ITEM()
RATIONAL_B_SPLINE_CURVE((1.,1.,1.,1.,1.,1.,1.,1.,1.,1.,1.,1.,1.,1.,1.,1.,
1.,1.,1.,1.,1.,1.,1.,1.,1.,1.,1.,1.,1.,1.,1.,1.,1.,1.,1.,1.,1.,1.,1.,1.,
1.,1.,1.,1.,1.,1.,1.,1.,1.,1.,1.,1.,1.,1.,1.,1.,1.,1.,1.,1.,1.,1.,1.,1.,
1.,1.,1.,1.,1.,1.,1.,1.,1.,1.,1.,1.,1.,1.,1.,1.,1.,1.,1.,1.,1.,1.,1.,1.,
1.,1.,1.,1.,1.,1.,1.,1.,1.,1.,1.,1.,1.,1.,1.,1.,1.,1.,1.,1.,1.,1.,1.,1.,
1.,1.,1.,1.,1.,1.,1.,1.,1.,1.,1.,1.,1.,1.,1.,1.,1.,1.,1.,1.,1.,1.,1.,1.,
1.,1.,1.,1.,1.,1.,1.,1.,1.,1.,1.,1.,1.,1.,1.,1.,1.,1.,1.,1.,1.,1.,1.,1.,
1.,1.,1.,1.,1.,1.,1.,1.,1.,1.,1.,1.,1.,1.,1.,1.,1.,1.,1.,1.,1.,1.,1.,1.,
1.,1.,1.,1.,1.,1.,1.,1.,1.,1.,1.,1.,1.,1.,1.,1.,1.,1.,1.,1.,1.))
REPRESENTATION_ITEM('')
);
#752=(
BOUNDED_CURVE()
B_SPLINE_CURVE(5,(#194061,#194062,#194063,#194064,#194065,#194066,#194067,
#194068,#194069,#194070,#194071,#194072,#194073,#194074,#194075,#194076,
#194077,#194078,#194079,#194080,#194081,#194082,#194083,#194084,#194085,
#194086,#194087,#194088,#194089,#194090,#194091,#194092,#194093,#194094,
#194095,#194096,#194097,#194098,#194099,#194100,#194101,#194102,#194103,
#194104,#194105,#194106,#194107,#194108,#194109,#194110,#194111,#194112,
#194113,#194114,#194115,#194116,#194117,#194118,#194119,#194120,#194121,
#194122,#194123,#194124,#194125,#194126,#194127,#194128,#194129,#194130,
#194131,#194132,#194133,#194134,#194135,#194136,#194137,#194138,#194139,
#194140,#194141,#194142,#194143,#194144,#194145,#194146,#194147,#194148,
#194149,#194150,#194151,#194152,#194153,#194154,#194155,#194156,#194157,
#194158,#194159,#194160,#194161,#194162,#194163,#194164,#194165,#194166,
#194167,#194168,#194169,#194170,#194171,#194172,#194173,#194174,#194175,
#194176,#194177,#194178,#194179,#194180,#194181,#194182,#194183,#194184,
#194185,#194186,#194187,#194188,#194189,#194190,#194191,#194192,#194193,
#194194,#194195,#194196,#194197,#194198,#194199,#194200,#194201,#194202,
#194203,#194204,#194205,#194206,#194207,#194208,#194209,#194210,#194211,
#194212,#194213,#194214,#194215,#194216,#194217,#194218,#194219,#194220,
#194221,#194222,#194223,#194224,#194225,#194226,#194227,#194228,#194229,
#194230,#194231,#194232,#194233,#194234,#194235,#194236,#194237,#194238,
#194239,#194240,#194241,#194242,#194243,#194244,#194245,#194246,#194247,
#194248,#194249,#194250,#194251,#194252,#194253,#194254,#194255,#194256,
#194257,#194258,#194259,#194260,#194261,#194262,#194263,#194264,#194265),
 .UNSPECIFIED.,.F.,.F.)
B_SPLINE_CURVE_WITH_KNOTS((6,1,1,1,1,1,1,1,1,1,1,1,1,1,1,1,1,1,1,1,1,1,
1,1,1,1,1,1,1,1,1,1,1,1,1,1,1,1,1,1,1,1,1,1,1,1,1,1,1,1,1,1,1,1,1,1,1,1,
1,1,1,1,1,1,1,1,1,1,1,1,1,1,1,1,1,1,1,1,1,1,1,1,1,1,1,1,1,1,1,1,1,1,1,1,
1,1,1,1,1,1,1,1,1,1,1,1,1,1,1,1,1,1,1,1,1,1,1,1,1,1,1,1,1,1,1,1,1,1,1,1,
1,1,1,1,1,1,1,1,1,1,1,1,1,1,1,1,1,1,1,1,1,1,1,1,1,1,1,1,1,1,1,1,1,1,1,1,
1,1,1,1,1,1,1,1,1,1,1,1,1,1,1,1,1,1,1,1,1,1,1,1,1,1,1,1,1,1,1,1,1,1,6),
(0.,0.005,0.01,0.015,0.02,0.025,0.03,0.035,0.04,0.045,0.05,0.055,0.06,0.065,
0.07,0.075,0.08,0.085,0.09,0.095,0.1,0.105,0.11,0.115,0.12,0.125,0.13,0.135,
0.14,0.145,0.15,0.155,0.16,0.165,0.17,0.175,0.18,0.185,0.19,0.195,0.2,0.205,
0.21,0.215,0.22,0.225,0.23,0.235,0.24,0.245,0.25,0.255,0.26,0.265,0.27,
0.275,0.28,0.285,0.29,0.295,0.3,0.305,0.31,0.315,0.32,0.325,0.33,0.335,
0.34,0.345,0.35,0.355,0.36,0.365,0.37,0.375,0.38,0.385,0.39,0.395,0.4,0.405,
0.41,0.415,0.42,0.425,0.43,0.435,0.44,0.445,0.45,0.455,0.46,0.465,0.47,
0.475,0.48,0.485,0.49,0.495,0.5,0.505,0.51,0.515,0.52,0.525,0.53,0.535,
0.54,0.545,0.55,0.555,0.56,0.565,0.57,0.575,0.58,0.585,0.59,0.595,0.6,0.605,
0.61,0.615,0.62,0.625,0.63,0.635,0.64,0.645,0.65,0.655,0.66,0.665,0.67,
0.675,0.68,0.685,0.690000000000001,0.695000000000001,0.700000000000001,
0.705000000000001,0.710000000000001,0.715000000000001,0.720000000000001,
0.725000000000001,0.730000000000001,0.735000000000001,0.740000000000001,
0.745000000000001,0.750000000000001,0.755000000000001,0.760000000000001,
0.765000000000001,0.770000000000001,0.775000000000001,0.780000000000001,
0.785000000000001,0.790000000000001,0.795000000000001,0.800000000000001,
0.805000000000001,0.810000000000001,0.815000000000001,0.820000000000001,
0.825000000000001,0.830000000000001,0.835000000000001,0.840000000000001,
0.845000000000001,0.850000000000001,0.855000000000001,0.860000000000001,
0.865000000000001,0.870000000000001,0.875000000000001,0.880000000000001,
0.885000000000001,0.890000000000001,0.895000000000001,0.900000000000001,
0.905000000000001,0.910000000000001,0.915000000000001,0.920000000000001,
0.925000000000001,0.930000000000001,0.935000000000001,0.940000000000001,
0.945000000000001,0.950000000000001,0.955000000000001,0.960000000000001,
0.965000000000001,0.970000000000001,0.975000000000001,0.980000000000001,
0.985000000000001,0.990000000000001,0.995000000000001,1.),.UNSPECIFIED.)
CURVE()
GEOMETRIC_REPRESENTATION_ITEM()
RATIONAL_B_SPLINE_CURVE((1.,1.,1.,1.,1.,1.,1.,1.,1.,1.,1.,1.,1.,1.,1.,1.,
1.,1.,1.,1.,1.,1.,1.,1.,1.,1.,1.,1.,1.,1.,1.,1.,1.,1.,1.,1.,1.,1.,1.,1.,
1.,1.,1.,1.,1.,1.,1.,1.,1.,1.,1.,1.,1.,1.,1.,1.,1.,1.,1.,1.,1.,1.,1.,1.,
1.,1.,1.,1.,1.,1.,1.,1.,1.,1.,1.,1.,1.,1.,1.,1.,1.,1.,1.,1.,1.,1.,1.,1.,
1.,1.,1.,1.,1.,1.,1.,1.,1.,1.,1.,1.,1.,1.,1.,1.,1.,1.,1.,1.,1.,1.,1.,1.,
1.,1.,1.,1.,1.,1.,1.,1.,1.,1.,1.,1.,1.,1.,1.,1.,1.,1.,1.,1.,1.,1.,1.,1.,
1.,1.,1.,1.,1.,1.,1.,1.,1.,1.,1.,1.,1.,1.,1.,1.,1.,1.,1.,1.,1.,1.,1.,1.,
1.,1.,1.,1.,1.,1.,1.,1.,1.,1.,1.,1.,1.,1.,1.,1.,1.,1.,1.,1.,1.,1.,1.,1.,
1.,1.,1.,1.,1.,1.,1.,1.,1.,1.,1.,1.,1.,1.,1.,1.,1.,1.,1.,1.,1.))
REPRESENTATION_ITEM('')
);
#753=(
BOUNDED_CURVE()
B_SPLINE_CURVE(5,(#194682,#194683,#194684,#194685,#194686,#194687,#194688,
#194689,#194690,#194691,#194692,#194693,#194694,#194695,#194696,#194697,
#194698,#194699,#194700,#194701,#194702,#194703,#194704,#194705,#194706,
#194707,#194708,#194709,#194710,#194711,#194712,#194713,#194714,#194715,
#194716,#194717,#194718,#194719,#194720,#194721,#194722,#194723,#194724,
#194725,#194726,#194727,#194728,#194729,#194730,#194731,#194732,#194733,
#194734,#194735,#194736,#194737,#194738,#194739,#194740,#194741,#194742,
#194743,#194744,#194745,#194746,#194747,#194748,#194749,#194750,#194751,
#194752,#194753,#194754,#194755,#194756,#194757,#194758,#194759,#194760,
#194761,#194762,#194763,#194764,#194765,#194766,#194767,#194768,#194769,
#194770,#194771,#194772,#194773,#194774,#194775,#194776,#194777,#194778,
#194779,#194780,#194781,#194782,#194783,#194784,#194785,#194786,#194787,
#194788,#194789,#194790,#194791,#194792,#194793,#194794,#194795,#194796,
#194797,#194798,#194799,#194800,#194801,#194802,#194803,#194804,#194805,
#194806,#194807,#194808,#194809,#194810,#194811,#194812,#194813,#194814,
#194815,#194816,#194817,#194818,#194819,#194820,#194821,#194822,#194823,
#194824,#194825,#194826,#194827,#194828,#194829,#194830,#194831,#194832,
#194833,#194834,#194835,#194836,#194837,#194838,#194839,#194840,#194841,
#194842,#194843,#194844,#194845,#194846,#194847,#194848,#194849,#194850,
#194851,#194852,#194853,#194854,#194855,#194856,#194857,#194858,#194859,
#194860,#194861,#194862,#194863,#194864,#194865,#194866,#194867,#194868,
#194869,#194870,#194871,#194872,#194873,#194874,#194875,#194876,#194877,
#194878,#194879,#194880,#194881,#194882,#194883,#194884,#194885,#194886),
 .UNSPECIFIED.,.F.,.F.)
B_SPLINE_CURVE_WITH_KNOTS((6,1,1,1,1,1,1,1,1,1,1,1,1,1,1,1,1,1,1,1,1,1,
1,1,1,1,1,1,1,1,1,1,1,1,1,1,1,1,1,1,1,1,1,1,1,1,1,1,1,1,1,1,1,1,1,1,1,1,
1,1,1,1,1,1,1,1,1,1,1,1,1,1,1,1,1,1,1,1,1,1,1,1,1,1,1,1,1,1,1,1,1,1,1,1,
1,1,1,1,1,1,1,1,1,1,1,1,1,1,1,1,1,1,1,1,1,1,1,1,1,1,1,1,1,1,1,1,1,1,1,1,
1,1,1,1,1,1,1,1,1,1,1,1,1,1,1,1,1,1,1,1,1,1,1,1,1,1,1,1,1,1,1,1,1,1,1,1,
1,1,1,1,1,1,1,1,1,1,1,1,1,1,1,1,1,1,1,1,1,1,1,1,1,1,1,1,1,1,1,1,1,1,6),
(-1.,-0.995000000000001,-0.990000000000001,-0.985000000000001,-0.980000000000001,
-0.975000000000001,-0.970000000000001,-0.965000000000001,-0.960000000000001,
-0.955000000000001,-0.950000000000001,-0.945000000000001,-0.940000000000001,
-0.935000000000001,-0.930000000000001,-0.925000000000001,-0.920000000000001,
-0.915000000000001,-0.910000000000001,-0.905000000000001,-0.900000000000001,
-0.895000000000001,-0.890000000000001,-0.885000000000001,-0.880000000000001,
-0.875000000000001,-0.870000000000001,-0.865000000000001,-0.860000000000001,
-0.855000000000001,-0.850000000000001,-0.845000000000001,-0.840000000000001,
-0.835000000000001,-0.830000000000001,-0.825000000000001,-0.820000000000001,
-0.815000000000001,-0.810000000000001,-0.805000000000001,-0.800000000000001,
-0.795000000000001,-0.790000000000001,-0.785000000000001,-0.780000000000001,
-0.775000000000001,-0.770000000000001,-0.765000000000001,-0.760000000000001,
-0.755000000000001,-0.750000000000001,-0.745000000000001,-0.740000000000001,
-0.735000000000001,-0.730000000000001,-0.725000000000001,-0.720000000000001,
-0.715000000000001,-0.710000000000001,-0.705000000000001,-0.700000000000001,
-0.695000000000001,-0.690000000000001,-0.685,-0.68,-0.675,-0.67,-0.665,
-0.66,-0.655,-0.65,-0.645,-0.64,-0.635,-0.63,-0.625,-0.62,-0.615,-0.61,
-0.605,-0.6,-0.595,-0.59,-0.585,-0.58,-0.575,-0.57,-0.565,-0.56,-0.555,
-0.55,-0.545,-0.54,-0.535,-0.53,-0.525,-0.52,-0.515,-0.51,-0.505,-0.5,-0.495,
-0.49,-0.485,-0.48,-0.475,-0.47,-0.465,-0.46,-0.455,-0.45,-0.445,-0.44,
-0.435,-0.43,-0.425,-0.42,-0.415,-0.41,-0.405,-0.4,-0.395,-0.39,-0.385,
-0.38,-0.375,-0.37,-0.365,-0.36,-0.355,-0.35,-0.345,-0.34,-0.335,-0.33,
-0.325,-0.32,-0.315,-0.31,-0.305,-0.3,-0.295,-0.29,-0.285,-0.28,-0.275,
-0.27,-0.265,-0.26,-0.255,-0.25,-0.245,-0.24,-0.235,-0.23,-0.225,-0.22,
-0.215,-0.21,-0.205,-0.2,-0.195,-0.19,-0.185,-0.18,-0.175,-0.17,-0.165,
-0.16,-0.155,-0.15,-0.145,-0.14,-0.135,-0.13,-0.125,-0.12,-0.115,-0.11,
-0.105,-0.1,-0.095,-0.09,-0.085,-0.08,-0.075,-0.07,-0.065,-0.06,-0.055,
-0.05,-0.045,-0.04,-0.035,-0.03,-0.025,-0.02,-0.015,-0.01,-0.005,0.),
 .UNSPECIFIED.)
CURVE()
GEOMETRIC_REPRESENTATION_ITEM()
RATIONAL_B_SPLINE_CURVE((1.,1.,1.,1.,1.,1.,1.,1.,1.,1.,1.,1.,1.,1.,1.,1.,
1.,1.,1.,1.,1.,1.,1.,1.,1.,1.,1.,1.,1.,1.,1.,1.,1.,1.,1.,1.,1.,1.,1.,1.,
1.,1.,1.,1.,1.,1.,1.,1.,1.,1.,1.,1.,1.,1.,1.,1.,1.,1.,1.,1.,1.,1.,1.,1.,
1.,1.,1.,1.,1.,1.,1.,1.,1.,1.,1.,1.,1.,1.,1.,1.,1.,1.,1.,1.,1.,1.,1.,1.,
1.,1.,1.,1.,1.,1.,1.,1.,1.,1.,1.,1.,1.,1.,1.,1.,1.,1.,1.,1.,1.,1.,1.,1.,
1.,1.,1.,1.,1.,1.,1.,1.,1.,1.,1.,1.,1.,1.,1.,1.,1.,1.,1.,1.,1.,1.,1.,1.,
1.,1.,1.,1.,1.,1.,1.,1.,1.,1.,1.,1.,1.,1.,1.,1.,1.,1.,1.,1.,1.,1.,1.,1.,
1.,1.,1.,1.,1.,1.,1.,1.,1.,1.,1.,1.,1.,1.,1.,1.,1.,1.,1.,1.,1.,1.,1.,1.,
1.,1.,1.,1.,1.,1.,1.,1.,1.,1.,1.,1.,1.,1.,1.,1.,1.,1.,1.,1.,1.))
REPRESENTATION_ITEM('')
);
#754=(
BOUNDED_CURVE()
B_SPLINE_CURVE(5,(#195299,#195300,#195301,#195302,#195303,#195304,#195305,
#195306,#195307,#195308,#195309,#195310,#195311,#195312,#195313,#195314,
#195315,#195316,#195317,#195318,#195319,#195320,#195321,#195322,#195323,
#195324,#195325,#195326,#195327,#195328,#195329,#195330,#195331,#195332,
#195333,#195334,#195335,#195336,#195337,#195338,#195339,#195340,#195341,
#195342,#195343,#195344,#195345,#195346,#195347,#195348,#195349,#195350,
#195351,#195352,#195353,#195354,#195355,#195356,#195357,#195358,#195359,
#195360,#195361,#195362,#195363,#195364,#195365,#195366,#195367,#195368,
#195369,#195370,#195371,#195372,#195373,#195374,#195375,#195376,#195377,
#195378,#195379,#195380,#195381,#195382,#195383,#195384,#195385,#195386,
#195387,#195388,#195389,#195390,#195391,#195392,#195393,#195394,#195395,
#195396,#195397,#195398,#195399,#195400,#195401,#195402,#195403,#195404,
#195405,#195406,#195407,#195408,#195409,#195410,#195411,#195412,#195413,
#195414,#195415,#195416,#195417,#195418,#195419,#195420,#195421,#195422,
#195423,#195424,#195425,#195426,#195427,#195428,#195429,#195430,#195431,
#195432,#195433,#195434,#195435,#195436,#195437,#195438,#195439,#195440,
#195441,#195442,#195443,#195444,#195445,#195446,#195447,#195448,#195449,
#195450,#195451,#195452,#195453,#195454,#195455,#195456,#195457,#195458,
#195459,#195460,#195461,#195462,#195463,#195464,#195465,#195466,#195467,
#195468,#195469,#195470,#195471,#195472,#195473,#195474,#195475,#195476,
#195477,#195478,#195479,#195480,#195481,#195482,#195483,#195484,#195485,
#195486,#195487,#195488,#195489,#195490,#195491,#195492,#195493,#195494,
#195495,#195496,#195497,#195498,#195499,#195500,#195501,#195502,#195503),
 .UNSPECIFIED.,.F.,.F.)
B_SPLINE_CURVE_WITH_KNOTS((6,1,1,1,1,1,1,1,1,1,1,1,1,1,1,1,1,1,1,1,1,1,
1,1,1,1,1,1,1,1,1,1,1,1,1,1,1,1,1,1,1,1,1,1,1,1,1,1,1,1,1,1,1,1,1,1,1,1,
1,1,1,1,1,1,1,1,1,1,1,1,1,1,1,1,1,1,1,1,1,1,1,1,1,1,1,1,1,1,1,1,1,1,1,1,
1,1,1,1,1,1,1,1,1,1,1,1,1,1,1,1,1,1,1,1,1,1,1,1,1,1,1,1,1,1,1,1,1,1,1,1,
1,1,1,1,1,1,1,1,1,1,1,1,1,1,1,1,1,1,1,1,1,1,1,1,1,1,1,1,1,1,1,1,1,1,1,1,
1,1,1,1,1,1,1,1,1,1,1,1,1,1,1,1,1,1,1,1,1,1,1,1,1,1,1,1,1,1,1,1,1,1,6),
(0.,0.005,0.01,0.015,0.02,0.025,0.03,0.035,0.04,0.045,0.05,0.055,0.06,0.065,
0.07,0.075,0.08,0.085,0.09,0.095,0.1,0.105,0.11,0.115,0.12,0.125,0.13,0.135,
0.14,0.145,0.15,0.155,0.16,0.165,0.17,0.175,0.18,0.185,0.19,0.195,0.2,0.205,
0.21,0.215,0.22,0.225,0.23,0.235,0.24,0.245,0.25,0.255,0.26,0.265,0.27,
0.275,0.28,0.285,0.29,0.295,0.3,0.305,0.31,0.315,0.32,0.325,0.33,0.335,
0.34,0.345,0.35,0.355,0.36,0.365,0.37,0.375,0.38,0.385,0.39,0.395,0.4,0.405,
0.41,0.415,0.42,0.425,0.43,0.435,0.44,0.445,0.45,0.455,0.46,0.465,0.47,
0.475,0.48,0.485,0.49,0.495,0.5,0.505,0.51,0.515,0.52,0.525,0.53,0.535,
0.54,0.545,0.55,0.555,0.56,0.565,0.57,0.575,0.58,0.585,0.59,0.595,0.6,0.605,
0.61,0.615,0.62,0.625,0.63,0.635,0.64,0.645,0.65,0.655,0.66,0.665,0.67,
0.675,0.68,0.685,0.690000000000001,0.695000000000001,0.700000000000001,
0.705000000000001,0.710000000000001,0.715000000000001,0.720000000000001,
0.725000000000001,0.730000000000001,0.735000000000001,0.740000000000001,
0.745000000000001,0.750000000000001,0.755000000000001,0.760000000000001,
0.765000000000001,0.770000000000001,0.775000000000001,0.780000000000001,
0.785000000000001,0.790000000000001,0.795000000000001,0.800000000000001,
0.805000000000001,0.810000000000001,0.815000000000001,0.820000000000001,
0.825000000000001,0.830000000000001,0.835000000000001,0.840000000000001,
0.845000000000001,0.850000000000001,0.855000000000001,0.860000000000001,
0.865000000000001,0.870000000000001,0.875000000000001,0.880000000000001,
0.885000000000001,0.890000000000001,0.895000000000001,0.900000000000001,
0.905000000000001,0.910000000000001,0.915000000000001,0.920000000000001,
0.925000000000001,0.930000000000001,0.935000000000001,0.940000000000001,
0.945000000000001,0.950000000000001,0.955000000000001,0.960000000000001,
0.965000000000001,0.970000000000001,0.975000000000001,0.980000000000001,
0.985000000000001,0.990000000000001,0.995000000000001,1.),.UNSPECIFIED.)
CURVE()
GEOMETRIC_REPRESENTATION_ITEM()
RATIONAL_B_SPLINE_CURVE((1.,1.,1.,1.,1.,1.,1.,1.,1.,1.,1.,1.,1.,1.,1.,1.,
1.,1.,1.,1.,1.,1.,1.,1.,1.,1.,1.,1.,1.,1.,1.,1.,1.,1.,1.,1.,1.,1.,1.,1.,
1.,1.,1.,1.,1.,1.,1.,1.,1.,1.,1.,1.,1.,1.,1.,1.,1.,1.,1.,1.,1.,1.,1.,1.,
1.,1.,1.,1.,1.,1.,1.,1.,1.,1.,1.,1.,1.,1.,1.,1.,1.,1.,1.,1.,1.,1.,1.,1.,
1.,1.,1.,1.,1.,1.,1.,1.,1.,1.,1.,1.,1.,1.,1.,1.,1.,1.,1.,1.,1.,1.,1.,1.,
1.,1.,1.,1.,1.,1.,1.,1.,1.,1.,1.,1.,1.,1.,1.,1.,1.,1.,1.,1.,1.,1.,1.,1.,
1.,1.,1.,1.,1.,1.,1.,1.,1.,1.,1.,1.,1.,1.,1.,1.,1.,1.,1.,1.,1.,1.,1.,1.,
1.,1.,1.,1.,1.,1.,1.,1.,1.,1.,1.,1.,1.,1.,1.,1.,1.,1.,1.,1.,1.,1.,1.,1.,
1.,1.,1.,1.,1.,1.,1.,1.,1.,1.,1.,1.,1.,1.,1.,1.,1.,1.,1.,1.,1.))
REPRESENTATION_ITEM('')
);
#755=(
BOUNDED_CURVE()
B_SPLINE_CURVE(5,(#195920,#195921,#195922,#195923,#195924,#195925,#195926,
#195927,#195928,#195929,#195930,#195931,#195932,#195933,#195934,#195935,
#195936,#195937,#195938,#195939,#195940,#195941,#195942,#195943,#195944,
#195945,#195946,#195947,#195948,#195949,#195950,#195951,#195952,#195953,
#195954,#195955,#195956,#195957,#195958,#195959,#195960,#195961,#195962,
#195963,#195964,#195965,#195966,#195967,#195968,#195969,#195970,#195971,
#195972,#195973,#195974,#195975,#195976,#195977,#195978,#195979,#195980,
#195981,#195982,#195983,#195984,#195985,#195986,#195987,#195988,#195989,
#195990,#195991,#195992,#195993,#195994,#195995,#195996,#195997,#195998,
#195999,#196000,#196001,#196002,#196003,#196004,#196005,#196006,#196007,
#196008,#196009,#196010,#196011,#196012,#196013,#196014,#196015,#196016,
#196017,#196018,#196019,#196020,#196021,#196022,#196023,#196024,#196025,
#196026,#196027,#196028,#196029,#196030,#196031,#196032,#196033,#196034,
#196035,#196036,#196037,#196038,#196039,#196040,#196041,#196042,#196043,
#196044,#196045,#196046,#196047,#196048,#196049,#196050,#196051,#196052,
#196053,#196054,#196055,#196056,#196057,#196058,#196059,#196060,#196061,
#196062,#196063,#196064,#196065,#196066,#196067,#196068,#196069,#196070,
#196071,#196072,#196073,#196074,#196075,#196076,#196077,#196078,#196079,
#196080,#196081,#196082,#196083,#196084,#196085,#196086,#196087,#196088,
#196089,#196090,#196091,#196092,#196093,#196094,#196095,#196096,#196097,
#196098,#196099,#196100,#196101,#196102,#196103,#196104,#196105,#196106,
#196107,#196108,#196109,#196110,#196111,#196112,#196113,#196114,#196115,
#196116,#196117,#196118,#196119,#196120,#196121,#196122,#196123,#196124),
 .UNSPECIFIED.,.F.,.F.)
B_SPLINE_CURVE_WITH_KNOTS((6,1,1,1,1,1,1,1,1,1,1,1,1,1,1,1,1,1,1,1,1,1,
1,1,1,1,1,1,1,1,1,1,1,1,1,1,1,1,1,1,1,1,1,1,1,1,1,1,1,1,1,1,1,1,1,1,1,1,
1,1,1,1,1,1,1,1,1,1,1,1,1,1,1,1,1,1,1,1,1,1,1,1,1,1,1,1,1,1,1,1,1,1,1,1,
1,1,1,1,1,1,1,1,1,1,1,1,1,1,1,1,1,1,1,1,1,1,1,1,1,1,1,1,1,1,1,1,1,1,1,1,
1,1,1,1,1,1,1,1,1,1,1,1,1,1,1,1,1,1,1,1,1,1,1,1,1,1,1,1,1,1,1,1,1,1,1,1,
1,1,1,1,1,1,1,1,1,1,1,1,1,1,1,1,1,1,1,1,1,1,1,1,1,1,1,1,1,1,1,1,1,1,6),
(-1.,-0.995000000000001,-0.990000000000001,-0.985000000000001,-0.980000000000001,
-0.975000000000001,-0.970000000000001,-0.965000000000001,-0.960000000000001,
-0.955000000000001,-0.950000000000001,-0.945000000000001,-0.940000000000001,
-0.935000000000001,-0.930000000000001,-0.925000000000001,-0.920000000000001,
-0.915000000000001,-0.910000000000001,-0.905000000000001,-0.900000000000001,
-0.895000000000001,-0.890000000000001,-0.885000000000001,-0.880000000000001,
-0.875000000000001,-0.870000000000001,-0.865000000000001,-0.860000000000001,
-0.855000000000001,-0.850000000000001,-0.845000000000001,-0.840000000000001,
-0.835000000000001,-0.830000000000001,-0.825000000000001,-0.820000000000001,
-0.815000000000001,-0.810000000000001,-0.805000000000001,-0.800000000000001,
-0.795000000000001,-0.790000000000001,-0.785000000000001,-0.780000000000001,
-0.775000000000001,-0.770000000000001,-0.765000000000001,-0.760000000000001,
-0.755000000000001,-0.750000000000001,-0.745000000000001,-0.740000000000001,
-0.735000000000001,-0.730000000000001,-0.725000000000001,-0.720000000000001,
-0.715000000000001,-0.710000000000001,-0.705000000000001,-0.700000000000001,
-0.695000000000001,-0.690000000000001,-0.685,-0.68,-0.675,-0.67,-0.665,
-0.66,-0.655,-0.65,-0.645,-0.64,-0.635,-0.63,-0.625,-0.62,-0.615,-0.61,
-0.605,-0.6,-0.595,-0.59,-0.585,-0.58,-0.575,-0.57,-0.565,-0.56,-0.555,
-0.55,-0.545,-0.54,-0.535,-0.53,-0.525,-0.52,-0.515,-0.51,-0.505,-0.5,-0.495,
-0.49,-0.485,-0.48,-0.475,-0.47,-0.465,-0.46,-0.455,-0.45,-0.445,-0.44,
-0.435,-0.43,-0.425,-0.42,-0.415,-0.41,-0.405,-0.4,-0.395,-0.39,-0.385,
-0.38,-0.375,-0.37,-0.365,-0.36,-0.355,-0.35,-0.345,-0.34,-0.335,-0.33,
-0.325,-0.32,-0.315,-0.31,-0.305,-0.3,-0.295,-0.29,-0.285,-0.28,-0.275,
-0.27,-0.265,-0.26,-0.255,-0.25,-0.245,-0.24,-0.235,-0.23,-0.225,-0.22,
-0.215,-0.21,-0.205,-0.2,-0.195,-0.19,-0.185,-0.18,-0.175,-0.17,-0.165,
-0.16,-0.155,-0.15,-0.145,-0.14,-0.135,-0.13,-0.125,-0.12,-0.115,-0.11,
-0.105,-0.1,-0.095,-0.09,-0.085,-0.08,-0.075,-0.07,-0.065,-0.06,-0.055,
-0.05,-0.045,-0.04,-0.035,-0.03,-0.025,-0.02,-0.015,-0.01,-0.005,0.),
 .UNSPECIFIED.)
CURVE()
GEOMETRIC_REPRESENTATION_ITEM()
RATIONAL_B_SPLINE_CURVE((1.,1.,1.,1.,1.,1.,1.,1.,1.,1.,1.,1.,1.,1.,1.,1.,
1.,1.,1.,1.,1.,1.,1.,1.,1.,1.,1.,1.,1.,1.,1.,1.,1.,1.,1.,1.,1.,1.,1.,1.,
1.,1.,1.,1.,1.,1.,1.,1.,1.,1.,1.,1.,1.,1.,1.,1.,1.,1.,1.,1.,1.,1.,1.,1.,
1.,1.,1.,1.,1.,1.,1.,1.,1.,1.,1.,1.,1.,1.,1.,1.,1.,1.,1.,1.,1.,1.,1.,1.,
1.,1.,1.,1.,1.,1.,1.,1.,1.,1.,1.,1.,1.,1.,1.,1.,1.,1.,1.,1.,1.,1.,1.,1.,
1.,1.,1.,1.,1.,1.,1.,1.,1.,1.,1.,1.,1.,1.,1.,1.,1.,1.,1.,1.,1.,1.,1.,1.,
1.,1.,1.,1.,1.,1.,1.,1.,1.,1.,1.,1.,1.,1.,1.,1.,1.,1.,1.,1.,1.,1.,1.,1.,
1.,1.,1.,1.,1.,1.,1.,1.,1.,1.,1.,1.,1.,1.,1.,1.,1.,1.,1.,1.,1.,1.,1.,1.,
1.,1.,1.,1.,1.,1.,1.,1.,1.,1.,1.,1.,1.,1.,1.,1.,1.,1.,1.,1.,1.))
REPRESENTATION_ITEM('')
);
#756=(
BOUNDED_CURVE()
B_SPLINE_CURVE(5,(#196537,#196538,#196539,#196540,#196541,#196542,#196543,
#196544,#196545,#196546,#196547,#196548,#196549,#196550,#196551,#196552,
#196553,#196554,#196555,#196556,#196557,#196558,#196559,#196560,#196561,
#196562,#196563,#196564,#196565,#196566,#196567,#196568,#196569,#196570,
#196571,#196572,#196573,#196574,#196575,#196576,#196577,#196578,#196579,
#196580,#196581,#196582,#196583,#196584,#196585,#196586,#196587,#196588,
#196589,#196590,#196591,#196592,#196593,#196594,#196595,#196596,#196597,
#196598,#196599,#196600,#196601,#196602,#196603,#196604,#196605,#196606,
#196607,#196608,#196609,#196610,#196611,#196612,#196613,#196614,#196615,
#196616,#196617,#196618,#196619,#196620,#196621,#196622,#196623,#196624,
#196625,#196626,#196627,#196628,#196629,#196630,#196631,#196632,#196633,
#196634,#196635,#196636,#196637,#196638,#196639,#196640,#196641,#196642,
#196643,#196644,#196645,#196646,#196647,#196648,#196649,#196650,#196651,
#196652,#196653,#196654,#196655,#196656,#196657,#196658,#196659,#196660,
#196661,#196662,#196663,#196664,#196665,#196666,#196667,#196668,#196669,
#196670,#196671,#196672,#196673,#196674,#196675,#196676,#196677,#196678,
#196679,#196680,#196681,#196682,#196683,#196684,#196685,#196686,#196687,
#196688,#196689,#196690,#196691,#196692,#196693,#196694,#196695,#196696,
#196697,#196698,#196699,#196700,#196701,#196702,#196703,#196704,#196705,
#196706,#196707,#196708,#196709,#196710,#196711,#196712,#196713,#196714,
#196715,#196716,#196717,#196718,#196719,#196720,#196721,#196722,#196723,
#196724,#196725,#196726,#196727,#196728,#196729,#196730,#196731,#196732,
#196733,#196734,#196735,#196736,#196737,#196738,#196739,#196740,#196741),
 .UNSPECIFIED.,.F.,.F.)
B_SPLINE_CURVE_WITH_KNOTS((6,1,1,1,1,1,1,1,1,1,1,1,1,1,1,1,1,1,1,1,1,1,
1,1,1,1,1,1,1,1,1,1,1,1,1,1,1,1,1,1,1,1,1,1,1,1,1,1,1,1,1,1,1,1,1,1,1,1,
1,1,1,1,1,1,1,1,1,1,1,1,1,1,1,1,1,1,1,1,1,1,1,1,1,1,1,1,1,1,1,1,1,1,1,1,
1,1,1,1,1,1,1,1,1,1,1,1,1,1,1,1,1,1,1,1,1,1,1,1,1,1,1,1,1,1,1,1,1,1,1,1,
1,1,1,1,1,1,1,1,1,1,1,1,1,1,1,1,1,1,1,1,1,1,1,1,1,1,1,1,1,1,1,1,1,1,1,1,
1,1,1,1,1,1,1,1,1,1,1,1,1,1,1,1,1,1,1,1,1,1,1,1,1,1,1,1,1,1,1,1,1,1,6),
(0.,0.005,0.01,0.015,0.02,0.025,0.03,0.035,0.04,0.045,0.05,0.055,0.06,0.065,
0.07,0.075,0.08,0.085,0.09,0.095,0.1,0.105,0.11,0.115,0.12,0.125,0.13,0.135,
0.14,0.145,0.15,0.155,0.16,0.165,0.17,0.175,0.18,0.185,0.19,0.195,0.2,0.205,
0.21,0.215,0.22,0.225,0.23,0.235,0.24,0.245,0.25,0.255,0.26,0.265,0.27,
0.275,0.28,0.285,0.29,0.295,0.3,0.305,0.31,0.315,0.32,0.325,0.33,0.335,
0.34,0.345,0.35,0.355,0.36,0.365,0.37,0.375,0.38,0.385,0.39,0.395,0.4,0.405,
0.41,0.415,0.42,0.425,0.43,0.435,0.44,0.445,0.45,0.455,0.46,0.465,0.47,
0.475,0.48,0.485,0.49,0.495,0.5,0.505,0.51,0.515,0.52,0.525,0.53,0.535,
0.54,0.545,0.55,0.555,0.56,0.565,0.57,0.575,0.58,0.585,0.59,0.595,0.6,0.605,
0.61,0.615,0.62,0.625,0.63,0.635,0.64,0.645,0.65,0.655,0.66,0.665,0.67,
0.675,0.68,0.685,0.690000000000001,0.695000000000001,0.700000000000001,
0.705000000000001,0.710000000000001,0.715000000000001,0.720000000000001,
0.725000000000001,0.730000000000001,0.735000000000001,0.740000000000001,
0.745000000000001,0.750000000000001,0.755000000000001,0.760000000000001,
0.765000000000001,0.770000000000001,0.775000000000001,0.780000000000001,
0.785000000000001,0.790000000000001,0.795000000000001,0.800000000000001,
0.805000000000001,0.810000000000001,0.815000000000001,0.820000000000001,
0.825000000000001,0.830000000000001,0.835000000000001,0.840000000000001,
0.845000000000001,0.850000000000001,0.855000000000001,0.860000000000001,
0.865000000000001,0.870000000000001,0.875000000000001,0.880000000000001,
0.885000000000001,0.890000000000001,0.895000000000001,0.900000000000001,
0.905000000000001,0.910000000000001,0.915000000000001,0.920000000000001,
0.925000000000001,0.930000000000001,0.935000000000001,0.940000000000001,
0.945000000000001,0.950000000000001,0.955000000000001,0.960000000000001,
0.965000000000001,0.970000000000001,0.975000000000001,0.980000000000001,
0.985000000000001,0.990000000000001,0.995000000000001,1.),.UNSPECIFIED.)
CURVE()
GEOMETRIC_REPRESENTATION_ITEM()
RATIONAL_B_SPLINE_CURVE((1.,1.,1.,1.,1.,1.,1.,1.,1.,1.,1.,1.,1.,1.,1.,1.,
1.,1.,1.,1.,1.,1.,1.,1.,1.,1.,1.,1.,1.,1.,1.,1.,1.,1.,1.,1.,1.,1.,1.,1.,
1.,1.,1.,1.,1.,1.,1.,1.,1.,1.,1.,1.,1.,1.,1.,1.,1.,1.,1.,1.,1.,1.,1.,1.,
1.,1.,1.,1.,1.,1.,1.,1.,1.,1.,1.,1.,1.,1.,1.,1.,1.,1.,1.,1.,1.,1.,1.,1.,
1.,1.,1.,1.,1.,1.,1.,1.,1.,1.,1.,1.,1.,1.,1.,1.,1.,1.,1.,1.,1.,1.,1.,1.,
1.,1.,1.,1.,1.,1.,1.,1.,1.,1.,1.,1.,1.,1.,1.,1.,1.,1.,1.,1.,1.,1.,1.,1.,
1.,1.,1.,1.,1.,1.,1.,1.,1.,1.,1.,1.,1.,1.,1.,1.,1.,1.,1.,1.,1.,1.,1.,1.,
1.,1.,1.,1.,1.,1.,1.,1.,1.,1.,1.,1.,1.,1.,1.,1.,1.,1.,1.,1.,1.,1.,1.,1.,
1.,1.,1.,1.,1.,1.,1.,1.,1.,1.,1.,1.,1.,1.,1.,1.,1.,1.,1.,1.,1.))
REPRESENTATION_ITEM('')
);
#757=(
BOUNDED_CURVE()
B_SPLINE_CURVE(5,(#197158,#197159,#197160,#197161,#197162,#197163,#197164,
#197165,#197166,#197167,#197168,#197169,#197170,#197171,#197172,#197173,
#197174,#197175,#197176,#197177,#197178,#197179,#197180,#197181,#197182,
#197183,#197184,#197185,#197186,#197187,#197188,#197189,#197190,#197191,
#197192,#197193,#197194,#197195,#197196,#197197,#197198,#197199,#197200,
#197201,#197202,#197203,#197204,#197205,#197206,#197207,#197208,#197209,
#197210,#197211,#197212,#197213,#197214,#197215,#197216,#197217,#197218,
#197219,#197220,#197221,#197222,#197223,#197224,#197225,#197226,#197227,
#197228,#197229,#197230,#197231,#197232,#197233,#197234,#197235,#197236,
#197237,#197238,#197239,#197240,#197241,#197242,#197243,#197244,#197245,
#197246,#197247,#197248,#197249,#197250,#197251,#197252,#197253,#197254,
#197255,#197256,#197257,#197258,#197259,#197260,#197261,#197262,#197263,
#197264,#197265,#197266,#197267,#197268,#197269,#197270,#197271,#197272,
#197273,#197274,#197275,#197276,#197277,#197278,#197279,#197280,#197281,
#197282,#197283,#197284,#197285,#197286,#197287,#197288,#197289,#197290,
#197291,#197292,#197293,#197294,#197295,#197296,#197297,#197298,#197299,
#197300,#197301,#197302,#197303,#197304,#197305,#197306,#197307,#197308,
#197309,#197310,#197311,#197312,#197313,#197314,#197315,#197316,#197317,
#197318,#197319,#197320,#197321,#197322,#197323,#197324,#197325,#197326,
#197327,#197328,#197329,#197330,#197331,#197332,#197333,#197334,#197335,
#197336,#197337,#197338,#197339,#197340,#197341,#197342,#197343,#197344,
#197345,#197346,#197347,#197348,#197349,#197350,#197351,#197352,#197353,
#197354,#197355,#197356,#197357,#197358,#197359,#197360,#197361,#197362),
 .UNSPECIFIED.,.F.,.F.)
B_SPLINE_CURVE_WITH_KNOTS((6,1,1,1,1,1,1,1,1,1,1,1,1,1,1,1,1,1,1,1,1,1,
1,1,1,1,1,1,1,1,1,1,1,1,1,1,1,1,1,1,1,1,1,1,1,1,1,1,1,1,1,1,1,1,1,1,1,1,
1,1,1,1,1,1,1,1,1,1,1,1,1,1,1,1,1,1,1,1,1,1,1,1,1,1,1,1,1,1,1,1,1,1,1,1,
1,1,1,1,1,1,1,1,1,1,1,1,1,1,1,1,1,1,1,1,1,1,1,1,1,1,1,1,1,1,1,1,1,1,1,1,
1,1,1,1,1,1,1,1,1,1,1,1,1,1,1,1,1,1,1,1,1,1,1,1,1,1,1,1,1,1,1,1,1,1,1,1,
1,1,1,1,1,1,1,1,1,1,1,1,1,1,1,1,1,1,1,1,1,1,1,1,1,1,1,1,1,1,1,1,1,1,6),
(-1.,-0.995000000000001,-0.990000000000001,-0.985000000000001,-0.980000000000001,
-0.975000000000001,-0.970000000000001,-0.965000000000001,-0.960000000000001,
-0.955000000000001,-0.950000000000001,-0.945000000000001,-0.940000000000001,
-0.935000000000001,-0.930000000000001,-0.925000000000001,-0.920000000000001,
-0.915000000000001,-0.910000000000001,-0.905000000000001,-0.900000000000001,
-0.895000000000001,-0.890000000000001,-0.885000000000001,-0.880000000000001,
-0.875000000000001,-0.870000000000001,-0.865000000000001,-0.860000000000001,
-0.855000000000001,-0.850000000000001,-0.845000000000001,-0.840000000000001,
-0.835000000000001,-0.830000000000001,-0.825000000000001,-0.820000000000001,
-0.815000000000001,-0.810000000000001,-0.805000000000001,-0.800000000000001,
-0.795000000000001,-0.790000000000001,-0.785000000000001,-0.780000000000001,
-0.775000000000001,-0.770000000000001,-0.765000000000001,-0.760000000000001,
-0.755000000000001,-0.750000000000001,-0.745000000000001,-0.740000000000001,
-0.735000000000001,-0.730000000000001,-0.725000000000001,-0.720000000000001,
-0.715000000000001,-0.710000000000001,-0.705000000000001,-0.700000000000001,
-0.695000000000001,-0.690000000000001,-0.685,-0.68,-0.675,-0.67,-0.665,
-0.66,-0.655,-0.65,-0.645,-0.64,-0.635,-0.63,-0.625,-0.62,-0.615,-0.61,
-0.605,-0.6,-0.595,-0.59,-0.585,-0.58,-0.575,-0.57,-0.565,-0.56,-0.555,
-0.55,-0.545,-0.54,-0.535,-0.53,-0.525,-0.52,-0.515,-0.51,-0.505,-0.5,-0.495,
-0.49,-0.485,-0.48,-0.475,-0.47,-0.465,-0.46,-0.455,-0.45,-0.445,-0.44,
-0.435,-0.43,-0.425,-0.42,-0.415,-0.41,-0.405,-0.4,-0.395,-0.39,-0.385,
-0.38,-0.375,-0.37,-0.365,-0.36,-0.355,-0.35,-0.345,-0.34,-0.335,-0.33,
-0.325,-0.32,-0.315,-0.31,-0.305,-0.3,-0.295,-0.29,-0.285,-0.28,-0.275,
-0.27,-0.265,-0.26,-0.255,-0.25,-0.245,-0.24,-0.235,-0.23,-0.225,-0.22,
-0.215,-0.21,-0.205,-0.2,-0.195,-0.19,-0.185,-0.18,-0.175,-0.17,-0.165,
-0.16,-0.155,-0.15,-0.145,-0.14,-0.135,-0.13,-0.125,-0.12,-0.115,-0.11,
-0.105,-0.1,-0.095,-0.09,-0.085,-0.08,-0.075,-0.07,-0.065,-0.06,-0.055,
-0.05,-0.045,-0.04,-0.035,-0.03,-0.025,-0.02,-0.015,-0.01,-0.005,0.),
 .UNSPECIFIED.)
CURVE()
GEOMETRIC_REPRESENTATION_ITEM()
RATIONAL_B_SPLINE_CURVE((1.,1.,1.,1.,1.,1.,1.,1.,1.,1.,1.,1.,1.,1.,1.,1.,
1.,1.,1.,1.,1.,1.,1.,1.,1.,1.,1.,1.,1.,1.,1.,1.,1.,1.,1.,1.,1.,1.,1.,1.,
1.,1.,1.,1.,1.,1.,1.,1.,1.,1.,1.,1.,1.,1.,1.,1.,1.,1.,1.,1.,1.,1.,1.,1.,
1.,1.,1.,1.,1.,1.,1.,1.,1.,1.,1.,1.,1.,1.,1.,1.,1.,1.,1.,1.,1.,1.,1.,1.,
1.,1.,1.,1.,1.,1.,1.,1.,1.,1.,1.,1.,1.,1.,1.,1.,1.,1.,1.,1.,1.,1.,1.,1.,
1.,1.,1.,1.,1.,1.,1.,1.,1.,1.,1.,1.,1.,1.,1.,1.,1.,1.,1.,1.,1.,1.,1.,1.,
1.,1.,1.,1.,1.,1.,1.,1.,1.,1.,1.,1.,1.,1.,1.,1.,1.,1.,1.,1.,1.,1.,1.,1.,
1.,1.,1.,1.,1.,1.,1.,1.,1.,1.,1.,1.,1.,1.,1.,1.,1.,1.,1.,1.,1.,1.,1.,1.,
1.,1.,1.,1.,1.,1.,1.,1.,1.,1.,1.,1.,1.,1.,1.,1.,1.,1.,1.,1.,1.))
REPRESENTATION_ITEM('')
);
#758=(
BOUNDED_CURVE()
B_SPLINE_CURVE(5,(#197775,#197776,#197777,#197778,#197779,#197780,#197781,
#197782,#197783,#197784,#197785,#197786,#197787,#197788,#197789,#197790,
#197791,#197792,#197793,#197794,#197795,#197796,#197797,#197798,#197799,
#197800,#197801,#197802,#197803,#197804,#197805,#197806,#197807,#197808,
#197809,#197810,#197811,#197812,#197813,#197814,#197815,#197816,#197817,
#197818,#197819,#197820,#197821,#197822,#197823,#197824,#197825,#197826,
#197827,#197828,#197829,#197830,#197831,#197832,#197833,#197834,#197835,
#197836,#197837,#197838,#197839,#197840,#197841,#197842,#197843,#197844,
#197845,#197846,#197847,#197848,#197849,#197850,#197851,#197852,#197853,
#197854,#197855,#197856,#197857,#197858,#197859,#197860,#197861,#197862,
#197863,#197864,#197865,#197866,#197867,#197868,#197869,#197870,#197871,
#197872,#197873,#197874,#197875,#197876,#197877,#197878,#197879,#197880,
#197881,#197882,#197883,#197884,#197885,#197886,#197887,#197888,#197889,
#197890,#197891,#197892,#197893,#197894,#197895,#197896,#197897,#197898,
#197899,#197900,#197901,#197902,#197903,#197904,#197905,#197906,#197907,
#197908,#197909,#197910,#197911,#197912,#197913,#197914,#197915,#197916,
#197917,#197918,#197919,#197920,#197921,#197922,#197923,#197924,#197925,
#197926,#197927,#197928,#197929,#197930,#197931,#197932,#197933,#197934,
#197935,#197936,#197937,#197938,#197939,#197940,#197941,#197942,#197943,
#197944,#197945,#197946,#197947,#197948,#197949,#197950,#197951,#197952,
#197953,#197954,#197955,#197956,#197957,#197958,#197959,#197960,#197961,
#197962,#197963,#197964,#197965,#197966,#197967,#197968,#197969,#197970,
#197971,#197972,#197973,#197974,#197975,#197976,#197977,#197978,#197979),
 .UNSPECIFIED.,.F.,.F.)
B_SPLINE_CURVE_WITH_KNOTS((6,1,1,1,1,1,1,1,1,1,1,1,1,1,1,1,1,1,1,1,1,1,
1,1,1,1,1,1,1,1,1,1,1,1,1,1,1,1,1,1,1,1,1,1,1,1,1,1,1,1,1,1,1,1,1,1,1,1,
1,1,1,1,1,1,1,1,1,1,1,1,1,1,1,1,1,1,1,1,1,1,1,1,1,1,1,1,1,1,1,1,1,1,1,1,
1,1,1,1,1,1,1,1,1,1,1,1,1,1,1,1,1,1,1,1,1,1,1,1,1,1,1,1,1,1,1,1,1,1,1,1,
1,1,1,1,1,1,1,1,1,1,1,1,1,1,1,1,1,1,1,1,1,1,1,1,1,1,1,1,1,1,1,1,1,1,1,1,
1,1,1,1,1,1,1,1,1,1,1,1,1,1,1,1,1,1,1,1,1,1,1,1,1,1,1,1,1,1,1,1,1,1,6),
(0.,0.005,0.01,0.015,0.02,0.025,0.03,0.035,0.04,0.045,0.05,0.055,0.06,0.065,
0.07,0.075,0.08,0.085,0.09,0.095,0.1,0.105,0.11,0.115,0.12,0.125,0.13,0.135,
0.14,0.145,0.15,0.155,0.16,0.165,0.17,0.175,0.18,0.185,0.19,0.195,0.2,0.205,
0.21,0.215,0.22,0.225,0.23,0.235,0.24,0.245,0.25,0.255,0.26,0.265,0.27,
0.275,0.28,0.285,0.29,0.295,0.3,0.305,0.31,0.315,0.32,0.325,0.33,0.335,
0.34,0.345,0.35,0.355,0.36,0.365,0.37,0.375,0.38,0.385,0.39,0.395,0.4,0.405,
0.41,0.415,0.42,0.425,0.43,0.435,0.44,0.445,0.45,0.455,0.46,0.465,0.47,
0.475,0.48,0.485,0.49,0.495,0.5,0.505,0.51,0.515,0.52,0.525,0.53,0.535,
0.54,0.545,0.55,0.555,0.56,0.565,0.57,0.575,0.58,0.585,0.59,0.595,0.6,0.605,
0.61,0.615,0.62,0.625,0.63,0.635,0.64,0.645,0.65,0.655,0.66,0.665,0.67,
0.675,0.68,0.685,0.690000000000001,0.695000000000001,0.700000000000001,
0.705000000000001,0.710000000000001,0.715000000000001,0.720000000000001,
0.725000000000001,0.730000000000001,0.735000000000001,0.740000000000001,
0.745000000000001,0.750000000000001,0.755000000000001,0.760000000000001,
0.765000000000001,0.770000000000001,0.775000000000001,0.780000000000001,
0.785000000000001,0.790000000000001,0.795000000000001,0.800000000000001,
0.805000000000001,0.810000000000001,0.815000000000001,0.820000000000001,
0.825000000000001,0.830000000000001,0.835000000000001,0.840000000000001,
0.845000000000001,0.850000000000001,0.855000000000001,0.860000000000001,
0.865000000000001,0.870000000000001,0.875000000000001,0.880000000000001,
0.885000000000001,0.890000000000001,0.895000000000001,0.900000000000001,
0.905000000000001,0.910000000000001,0.915000000000001,0.920000000000001,
0.925000000000001,0.930000000000001,0.935000000000001,0.940000000000001,
0.945000000000001,0.950000000000001,0.955000000000001,0.960000000000001,
0.965000000000001,0.970000000000001,0.975000000000001,0.980000000000001,
0.985000000000001,0.990000000000001,0.995000000000001,1.),.UNSPECIFIED.)
CURVE()
GEOMETRIC_REPRESENTATION_ITEM()
RATIONAL_B_SPLINE_CURVE((1.,1.,1.,1.,1.,1.,1.,1.,1.,1.,1.,1.,1.,1.,1.,1.,
1.,1.,1.,1.,1.,1.,1.,1.,1.,1.,1.,1.,1.,1.,1.,1.,1.,1.,1.,1.,1.,1.,1.,1.,
1.,1.,1.,1.,1.,1.,1.,1.,1.,1.,1.,1.,1.,1.,1.,1.,1.,1.,1.,1.,1.,1.,1.,1.,
1.,1.,1.,1.,1.,1.,1.,1.,1.,1.,1.,1.,1.,1.,1.,1.,1.,1.,1.,1.,1.,1.,1.,1.,
1.,1.,1.,1.,1.,1.,1.,1.,1.,1.,1.,1.,1.,1.,1.,1.,1.,1.,1.,1.,1.,1.,1.,1.,
1.,1.,1.,1.,1.,1.,1.,1.,1.,1.,1.,1.,1.,1.,1.,1.,1.,1.,1.,1.,1.,1.,1.,1.,
1.,1.,1.,1.,1.,1.,1.,1.,1.,1.,1.,1.,1.,1.,1.,1.,1.,1.,1.,1.,1.,1.,1.,1.,
1.,1.,1.,1.,1.,1.,1.,1.,1.,1.,1.,1.,1.,1.,1.,1.,1.,1.,1.,1.,1.,1.,1.,1.,
1.,1.,1.,1.,1.,1.,1.,1.,1.,1.,1.,1.,1.,1.,1.,1.,1.,1.,1.,1.,1.))
REPRESENTATION_ITEM('')
);
#759=(
BOUNDED_CURVE()
B_SPLINE_CURVE(5,(#198396,#198397,#198398,#198399,#198400,#198401,#198402,
#198403,#198404,#198405,#198406,#198407,#198408,#198409,#198410,#198411,
#198412,#198413,#198414,#198415,#198416,#198417,#198418,#198419,#198420,
#198421,#198422,#198423,#198424,#198425,#198426,#198427,#198428,#198429,
#198430,#198431,#198432,#198433,#198434,#198435,#198436,#198437,#198438,
#198439,#198440,#198441,#198442,#198443,#198444,#198445,#198446,#198447,
#198448,#198449,#198450,#198451,#198452,#198453,#198454,#198455,#198456,
#198457,#198458,#198459,#198460,#198461,#198462,#198463,#198464,#198465,
#198466,#198467,#198468,#198469,#198470,#198471,#198472,#198473,#198474,
#198475,#198476,#198477,#198478,#198479,#198480,#198481,#198482,#198483,
#198484,#198485,#198486,#198487,#198488,#198489,#198490,#198491,#198492,
#198493,#198494,#198495,#198496,#198497,#198498,#198499,#198500,#198501,
#198502,#198503,#198504,#198505,#198506,#198507,#198508,#198509,#198510,
#198511,#198512,#198513,#198514,#198515,#198516,#198517,#198518,#198519,
#198520,#198521,#198522,#198523,#198524,#198525,#198526,#198527,#198528,
#198529,#198530,#198531,#198532,#198533,#198534,#198535,#198536,#198537,
#198538,#198539,#198540,#198541,#198542,#198543,#198544,#198545,#198546,
#198547,#198548,#198549,#198550,#198551,#198552,#198553,#198554,#198555,
#198556,#198557,#198558,#198559,#198560,#198561,#198562,#198563,#198564,
#198565,#198566,#198567,#198568,#198569,#198570,#198571,#198572,#198573,
#198574,#198575,#198576,#198577,#198578,#198579,#198580,#198581,#198582,
#198583,#198584,#198585,#198586,#198587,#198588,#198589,#198590,#198591,
#198592,#198593,#198594,#198595,#198596,#198597,#198598,#198599,#198600),
 .UNSPECIFIED.,.F.,.F.)
B_SPLINE_CURVE_WITH_KNOTS((6,1,1,1,1,1,1,1,1,1,1,1,1,1,1,1,1,1,1,1,1,1,
1,1,1,1,1,1,1,1,1,1,1,1,1,1,1,1,1,1,1,1,1,1,1,1,1,1,1,1,1,1,1,1,1,1,1,1,
1,1,1,1,1,1,1,1,1,1,1,1,1,1,1,1,1,1,1,1,1,1,1,1,1,1,1,1,1,1,1,1,1,1,1,1,
1,1,1,1,1,1,1,1,1,1,1,1,1,1,1,1,1,1,1,1,1,1,1,1,1,1,1,1,1,1,1,1,1,1,1,1,
1,1,1,1,1,1,1,1,1,1,1,1,1,1,1,1,1,1,1,1,1,1,1,1,1,1,1,1,1,1,1,1,1,1,1,1,
1,1,1,1,1,1,1,1,1,1,1,1,1,1,1,1,1,1,1,1,1,1,1,1,1,1,1,1,1,1,1,1,1,1,6),
(-1.,-0.995000000000001,-0.990000000000001,-0.985000000000001,-0.980000000000001,
-0.975000000000001,-0.970000000000001,-0.965000000000001,-0.960000000000001,
-0.955000000000001,-0.950000000000001,-0.945000000000001,-0.940000000000001,
-0.935000000000001,-0.930000000000001,-0.925000000000001,-0.920000000000001,
-0.915000000000001,-0.910000000000001,-0.905000000000001,-0.900000000000001,
-0.895000000000001,-0.890000000000001,-0.885000000000001,-0.880000000000001,
-0.875000000000001,-0.870000000000001,-0.865000000000001,-0.860000000000001,
-0.855000000000001,-0.850000000000001,-0.845000000000001,-0.840000000000001,
-0.835000000000001,-0.830000000000001,-0.825000000000001,-0.820000000000001,
-0.815000000000001,-0.810000000000001,-0.805000000000001,-0.800000000000001,
-0.795000000000001,-0.790000000000001,-0.785000000000001,-0.780000000000001,
-0.775000000000001,-0.770000000000001,-0.765000000000001,-0.760000000000001,
-0.755000000000001,-0.750000000000001,-0.745000000000001,-0.740000000000001,
-0.735000000000001,-0.730000000000001,-0.725000000000001,-0.720000000000001,
-0.715000000000001,-0.710000000000001,-0.705000000000001,-0.700000000000001,
-0.695000000000001,-0.690000000000001,-0.685,-0.68,-0.675,-0.67,-0.665,
-0.66,-0.655,-0.65,-0.645,-0.64,-0.635,-0.63,-0.625,-0.62,-0.615,-0.61,
-0.605,-0.6,-0.595,-0.59,-0.585,-0.58,-0.575,-0.57,-0.565,-0.56,-0.555,
-0.55,-0.545,-0.54,-0.535,-0.53,-0.525,-0.52,-0.515,-0.51,-0.505,-0.5,-0.495,
-0.49,-0.485,-0.48,-0.475,-0.47,-0.465,-0.46,-0.455,-0.45,-0.445,-0.44,
-0.435,-0.43,-0.425,-0.42,-0.415,-0.41,-0.405,-0.4,-0.395,-0.39,-0.385,
-0.38,-0.375,-0.37,-0.365,-0.36,-0.355,-0.35,-0.345,-0.34,-0.335,-0.33,
-0.325,-0.32,-0.315,-0.31,-0.305,-0.3,-0.295,-0.29,-0.285,-0.28,-0.275,
-0.27,-0.265,-0.26,-0.255,-0.25,-0.245,-0.24,-0.235,-0.23,-0.225,-0.22,
-0.215,-0.21,-0.205,-0.2,-0.195,-0.19,-0.185,-0.18,-0.175,-0.17,-0.165,
-0.16,-0.155,-0.15,-0.145,-0.14,-0.135,-0.13,-0.125,-0.12,-0.115,-0.11,
-0.105,-0.1,-0.095,-0.09,-0.085,-0.08,-0.075,-0.07,-0.065,-0.06,-0.055,
-0.05,-0.045,-0.04,-0.035,-0.03,-0.025,-0.02,-0.015,-0.01,-0.005,0.),
 .UNSPECIFIED.)
CURVE()
GEOMETRIC_REPRESENTATION_ITEM()
RATIONAL_B_SPLINE_CURVE((1.,1.,1.,1.,1.,1.,1.,1.,1.,1.,1.,1.,1.,1.,1.,1.,
1.,1.,1.,1.,1.,1.,1.,1.,1.,1.,1.,1.,1.,1.,1.,1.,1.,1.,1.,1.,1.,1.,1.,1.,
1.,1.,1.,1.,1.,1.,1.,1.,1.,1.,1.,1.,1.,1.,1.,1.,1.,1.,1.,1.,1.,1.,1.,1.,
1.,1.,1.,1.,1.,1.,1.,1.,1.,1.,1.,1.,1.,1.,1.,1.,1.,1.,1.,1.,1.,1.,1.,1.,
1.,1.,1.,1.,1.,1.,1.,1.,1.,1.,1.,1.,1.,1.,1.,1.,1.,1.,1.,1.,1.,1.,1.,1.,
1.,1.,1.,1.,1.,1.,1.,1.,1.,1.,1.,1.,1.,1.,1.,1.,1.,1.,1.,1.,1.,1.,1.,1.,
1.,1.,1.,1.,1.,1.,1.,1.,1.,1.,1.,1.,1.,1.,1.,1.,1.,1.,1.,1.,1.,1.,1.,1.,
1.,1.,1.,1.,1.,1.,1.,1.,1.,1.,1.,1.,1.,1.,1.,1.,1.,1.,1.,1.,1.,1.,1.,1.,
1.,1.,1.,1.,1.,1.,1.,1.,1.,1.,1.,1.,1.,1.,1.,1.,1.,1.,1.,1.,1.))
REPRESENTATION_ITEM('')
);
#760=(
BOUNDED_CURVE()
B_SPLINE_CURVE(5,(#199013,#199014,#199015,#199016,#199017,#199018,#199019,
#199020,#199021,#199022,#199023,#199024,#199025,#199026,#199027,#199028,
#199029,#199030,#199031,#199032,#199033,#199034,#199035,#199036,#199037,
#199038,#199039,#199040,#199041,#199042,#199043,#199044,#199045,#199046,
#199047,#199048,#199049,#199050,#199051,#199052,#199053,#199054,#199055,
#199056,#199057,#199058,#199059,#199060,#199061,#199062,#199063,#199064,
#199065,#199066,#199067,#199068,#199069,#199070,#199071,#199072,#199073,
#199074,#199075,#199076,#199077,#199078,#199079,#199080,#199081,#199082,
#199083,#199084,#199085,#199086,#199087,#199088,#199089,#199090,#199091,
#199092,#199093,#199094,#199095,#199096,#199097,#199098,#199099,#199100,
#199101,#199102,#199103,#199104,#199105,#199106,#199107,#199108,#199109,
#199110,#199111,#199112,#199113,#199114,#199115,#199116,#199117,#199118,
#199119,#199120,#199121,#199122,#199123,#199124,#199125,#199126,#199127,
#199128,#199129,#199130,#199131,#199132,#199133,#199134,#199135,#199136,
#199137,#199138,#199139,#199140,#199141,#199142,#199143,#199144,#199145,
#199146,#199147,#199148,#199149,#199150,#199151,#199152,#199153,#199154,
#199155,#199156,#199157,#199158,#199159,#199160,#199161,#199162,#199163,
#199164,#199165,#199166,#199167,#199168,#199169,#199170,#199171,#199172,
#199173,#199174,#199175,#199176,#199177,#199178,#199179,#199180,#199181,
#199182,#199183,#199184,#199185,#199186,#199187,#199188,#199189,#199190,
#199191,#199192,#199193,#199194,#199195,#199196,#199197,#199198,#199199,
#199200,#199201,#199202,#199203,#199204,#199205,#199206,#199207,#199208,
#199209,#199210,#199211,#199212,#199213,#199214,#199215,#199216,#199217),
 .UNSPECIFIED.,.F.,.F.)
B_SPLINE_CURVE_WITH_KNOTS((6,1,1,1,1,1,1,1,1,1,1,1,1,1,1,1,1,1,1,1,1,1,
1,1,1,1,1,1,1,1,1,1,1,1,1,1,1,1,1,1,1,1,1,1,1,1,1,1,1,1,1,1,1,1,1,1,1,1,
1,1,1,1,1,1,1,1,1,1,1,1,1,1,1,1,1,1,1,1,1,1,1,1,1,1,1,1,1,1,1,1,1,1,1,1,
1,1,1,1,1,1,1,1,1,1,1,1,1,1,1,1,1,1,1,1,1,1,1,1,1,1,1,1,1,1,1,1,1,1,1,1,
1,1,1,1,1,1,1,1,1,1,1,1,1,1,1,1,1,1,1,1,1,1,1,1,1,1,1,1,1,1,1,1,1,1,1,1,
1,1,1,1,1,1,1,1,1,1,1,1,1,1,1,1,1,1,1,1,1,1,1,1,1,1,1,1,1,1,1,1,1,1,6),
(0.,0.005,0.01,0.015,0.02,0.025,0.03,0.035,0.04,0.045,0.05,0.055,0.06,0.065,
0.07,0.075,0.08,0.085,0.09,0.095,0.1,0.105,0.11,0.115,0.12,0.125,0.13,0.135,
0.14,0.145,0.15,0.155,0.16,0.165,0.17,0.175,0.18,0.185,0.19,0.195,0.2,0.205,
0.21,0.215,0.22,0.225,0.23,0.235,0.24,0.245,0.25,0.255,0.26,0.265,0.27,
0.275,0.28,0.285,0.29,0.295,0.3,0.305,0.31,0.315,0.32,0.325,0.33,0.335,
0.34,0.345,0.35,0.355,0.36,0.365,0.37,0.375,0.38,0.385,0.39,0.395,0.4,0.405,
0.41,0.415,0.42,0.425,0.43,0.435,0.44,0.445,0.45,0.455,0.46,0.465,0.47,
0.475,0.48,0.485,0.49,0.495,0.5,0.505,0.51,0.515,0.52,0.525,0.53,0.535,
0.54,0.545,0.55,0.555,0.56,0.565,0.57,0.575,0.58,0.585,0.59,0.595,0.6,0.605,
0.61,0.615,0.62,0.625,0.63,0.635,0.64,0.645,0.65,0.655,0.66,0.665,0.67,
0.675,0.68,0.685,0.690000000000001,0.695000000000001,0.700000000000001,
0.705000000000001,0.710000000000001,0.715000000000001,0.720000000000001,
0.725000000000001,0.730000000000001,0.735000000000001,0.740000000000001,
0.745000000000001,0.750000000000001,0.755000000000001,0.760000000000001,
0.765000000000001,0.770000000000001,0.775000000000001,0.780000000000001,
0.785000000000001,0.790000000000001,0.795000000000001,0.800000000000001,
0.805000000000001,0.810000000000001,0.815000000000001,0.820000000000001,
0.825000000000001,0.830000000000001,0.835000000000001,0.840000000000001,
0.845000000000001,0.850000000000001,0.855000000000001,0.860000000000001,
0.865000000000001,0.870000000000001,0.875000000000001,0.880000000000001,
0.885000000000001,0.890000000000001,0.895000000000001,0.900000000000001,
0.905000000000001,0.910000000000001,0.915000000000001,0.920000000000001,
0.925000000000001,0.930000000000001,0.935000000000001,0.940000000000001,
0.945000000000001,0.950000000000001,0.955000000000001,0.960000000000001,
0.965000000000001,0.970000000000001,0.975000000000001,0.980000000000001,
0.985000000000001,0.990000000000001,0.995000000000001,1.),.UNSPECIFIED.)
CURVE()
GEOMETRIC_REPRESENTATION_ITEM()
RATIONAL_B_SPLINE_CURVE((1.,1.,1.,1.,1.,1.,1.,1.,1.,1.,1.,1.,1.,1.,1.,1.,
1.,1.,1.,1.,1.,1.,1.,1.,1.,1.,1.,1.,1.,1.,1.,1.,1.,1.,1.,1.,1.,1.,1.,1.,
1.,1.,1.,1.,1.,1.,1.,1.,1.,1.,1.,1.,1.,1.,1.,1.,1.,1.,1.,1.,1.,1.,1.,1.,
1.,1.,1.,1.,1.,1.,1.,1.,1.,1.,1.,1.,1.,1.,1.,1.,1.,1.,1.,1.,1.,1.,1.,1.,
1.,1.,1.,1.,1.,1.,1.,1.,1.,1.,1.,1.,1.,1.,1.,1.,1.,1.,1.,1.,1.,1.,1.,1.,
1.,1.,1.,1.,1.,1.,1.,1.,1.,1.,1.,1.,1.,1.,1.,1.,1.,1.,1.,1.,1.,1.,1.,1.,
1.,1.,1.,1.,1.,1.,1.,1.,1.,1.,1.,1.,1.,1.,1.,1.,1.,1.,1.,1.,1.,1.,1.,1.,
1.,1.,1.,1.,1.,1.,1.,1.,1.,1.,1.,1.,1.,1.,1.,1.,1.,1.,1.,1.,1.,1.,1.,1.,
1.,1.,1.,1.,1.,1.,1.,1.,1.,1.,1.,1.,1.,1.,1.,1.,1.,1.,1.,1.,1.))
REPRESENTATION_ITEM('')
);
#761=(
BOUNDED_CURVE()
B_SPLINE_CURVE(5,(#199634,#199635,#199636,#199637,#199638,#199639,#199640,
#199641,#199642,#199643,#199644,#199645,#199646,#199647,#199648,#199649,
#199650,#199651,#199652,#199653,#199654,#199655,#199656,#199657,#199658,
#199659,#199660,#199661,#199662,#199663,#199664,#199665,#199666,#199667,
#199668,#199669,#199670,#199671,#199672,#199673,#199674,#199675,#199676,
#199677,#199678,#199679,#199680,#199681,#199682,#199683,#199684,#199685,
#199686,#199687,#199688,#199689,#199690,#199691,#199692,#199693,#199694,
#199695,#199696,#199697,#199698,#199699,#199700,#199701,#199702,#199703,
#199704,#199705,#199706,#199707,#199708,#199709,#199710,#199711,#199712,
#199713,#199714,#199715,#199716,#199717,#199718,#199719,#199720,#199721,
#199722,#199723,#199724,#199725,#199726,#199727,#199728,#199729,#199730,
#199731,#199732,#199733,#199734,#199735,#199736,#199737,#199738,#199739,
#199740,#199741,#199742,#199743,#199744,#199745,#199746,#199747,#199748,
#199749,#199750,#199751,#199752,#199753,#199754,#199755,#199756,#199757,
#199758,#199759,#199760,#199761,#199762,#199763,#199764,#199765,#199766,
#199767,#199768,#199769,#199770,#199771,#199772,#199773,#199774,#199775,
#199776,#199777,#199778,#199779,#199780,#199781,#199782,#199783,#199784,
#199785,#199786,#199787,#199788,#199789,#199790,#199791,#199792,#199793,
#199794,#199795,#199796,#199797,#199798,#199799,#199800,#199801,#199802,
#199803,#199804,#199805,#199806,#199807,#199808,#199809,#199810,#199811,
#199812,#199813,#199814,#199815,#199816,#199817,#199818,#199819,#199820,
#199821,#199822,#199823,#199824,#199825,#199826,#199827,#199828,#199829,
#199830,#199831,#199832,#199833,#199834,#199835,#199836,#199837,#199838),
 .UNSPECIFIED.,.F.,.F.)
B_SPLINE_CURVE_WITH_KNOTS((6,1,1,1,1,1,1,1,1,1,1,1,1,1,1,1,1,1,1,1,1,1,
1,1,1,1,1,1,1,1,1,1,1,1,1,1,1,1,1,1,1,1,1,1,1,1,1,1,1,1,1,1,1,1,1,1,1,1,
1,1,1,1,1,1,1,1,1,1,1,1,1,1,1,1,1,1,1,1,1,1,1,1,1,1,1,1,1,1,1,1,1,1,1,1,
1,1,1,1,1,1,1,1,1,1,1,1,1,1,1,1,1,1,1,1,1,1,1,1,1,1,1,1,1,1,1,1,1,1,1,1,
1,1,1,1,1,1,1,1,1,1,1,1,1,1,1,1,1,1,1,1,1,1,1,1,1,1,1,1,1,1,1,1,1,1,1,1,
1,1,1,1,1,1,1,1,1,1,1,1,1,1,1,1,1,1,1,1,1,1,1,1,1,1,1,1,1,1,1,1,1,1,6),
(-1.,-0.995000000000001,-0.990000000000001,-0.985000000000001,-0.980000000000001,
-0.975000000000001,-0.970000000000001,-0.965000000000001,-0.960000000000001,
-0.955000000000001,-0.950000000000001,-0.945000000000001,-0.940000000000001,
-0.935000000000001,-0.930000000000001,-0.925000000000001,-0.920000000000001,
-0.915000000000001,-0.910000000000001,-0.905000000000001,-0.900000000000001,
-0.895000000000001,-0.890000000000001,-0.885000000000001,-0.880000000000001,
-0.875000000000001,-0.870000000000001,-0.865000000000001,-0.860000000000001,
-0.855000000000001,-0.850000000000001,-0.845000000000001,-0.840000000000001,
-0.835000000000001,-0.830000000000001,-0.825000000000001,-0.820000000000001,
-0.815000000000001,-0.810000000000001,-0.805000000000001,-0.800000000000001,
-0.795000000000001,-0.790000000000001,-0.785000000000001,-0.780000000000001,
-0.775000000000001,-0.770000000000001,-0.765000000000001,-0.760000000000001,
-0.755000000000001,-0.750000000000001,-0.745000000000001,-0.740000000000001,
-0.735000000000001,-0.730000000000001,-0.725000000000001,-0.720000000000001,
-0.715000000000001,-0.710000000000001,-0.705000000000001,-0.700000000000001,
-0.695000000000001,-0.690000000000001,-0.685,-0.68,-0.675,-0.67,-0.665,
-0.66,-0.655,-0.65,-0.645,-0.64,-0.635,-0.63,-0.625,-0.62,-0.615,-0.61,
-0.605,-0.6,-0.595,-0.59,-0.585,-0.58,-0.575,-0.57,-0.565,-0.56,-0.555,
-0.55,-0.545,-0.54,-0.535,-0.53,-0.525,-0.52,-0.515,-0.51,-0.505,-0.5,-0.495,
-0.49,-0.485,-0.48,-0.475,-0.47,-0.465,-0.46,-0.455,-0.45,-0.445,-0.44,
-0.435,-0.43,-0.425,-0.42,-0.415,-0.41,-0.405,-0.4,-0.395,-0.39,-0.385,
-0.38,-0.375,-0.37,-0.365,-0.36,-0.355,-0.35,-0.345,-0.34,-0.335,-0.33,
-0.325,-0.32,-0.315,-0.31,-0.305,-0.3,-0.295,-0.29,-0.285,-0.28,-0.275,
-0.27,-0.265,-0.26,-0.255,-0.25,-0.245,-0.24,-0.235,-0.23,-0.225,-0.22,
-0.215,-0.21,-0.205,-0.2,-0.195,-0.19,-0.185,-0.18,-0.175,-0.17,-0.165,
-0.16,-0.155,-0.15,-0.145,-0.14,-0.135,-0.13,-0.125,-0.12,-0.115,-0.11,
-0.105,-0.1,-0.095,-0.09,-0.085,-0.08,-0.075,-0.07,-0.065,-0.06,-0.055,
-0.05,-0.045,-0.04,-0.035,-0.03,-0.025,-0.02,-0.015,-0.01,-0.005,0.),
 .UNSPECIFIED.)
CURVE()
GEOMETRIC_REPRESENTATION_ITEM()
RATIONAL_B_SPLINE_CURVE((1.,1.,1.,1.,1.,1.,1.,1.,1.,1.,1.,1.,1.,1.,1.,1.,
1.,1.,1.,1.,1.,1.,1.,1.,1.,1.,1.,1.,1.,1.,1.,1.,1.,1.,1.,1.,1.,1.,1.,1.,
1.,1.,1.,1.,1.,1.,1.,1.,1.,1.,1.,1.,1.,1.,1.,1.,1.,1.,1.,1.,1.,1.,1.,1.,
1.,1.,1.,1.,1.,1.,1.,1.,1.,1.,1.,1.,1.,1.,1.,1.,1.,1.,1.,1.,1.,1.,1.,1.,
1.,1.,1.,1.,1.,1.,1.,1.,1.,1.,1.,1.,1.,1.,1.,1.,1.,1.,1.,1.,1.,1.,1.,1.,
1.,1.,1.,1.,1.,1.,1.,1.,1.,1.,1.,1.,1.,1.,1.,1.,1.,1.,1.,1.,1.,1.,1.,1.,
1.,1.,1.,1.,1.,1.,1.,1.,1.,1.,1.,1.,1.,1.,1.,1.,1.,1.,1.,1.,1.,1.,1.,1.,
1.,1.,1.,1.,1.,1.,1.,1.,1.,1.,1.,1.,1.,1.,1.,1.,1.,1.,1.,1.,1.,1.,1.,1.,
1.,1.,1.,1.,1.,1.,1.,1.,1.,1.,1.,1.,1.,1.,1.,1.,1.,1.,1.,1.,1.))
REPRESENTATION_ITEM('')
);
#762=(
BOUNDED_CURVE()
B_SPLINE_CURVE(5,(#200251,#200252,#200253,#200254,#200255,#200256,#200257,
#200258,#200259,#200260,#200261,#200262,#200263,#200264,#200265,#200266,
#200267,#200268,#200269,#200270,#200271,#200272,#200273,#200274,#200275,
#200276,#200277,#200278,#200279,#200280,#200281,#200282,#200283,#200284,
#200285,#200286,#200287,#200288,#200289,#200290,#200291,#200292,#200293,
#200294,#200295,#200296,#200297,#200298,#200299,#200300,#200301,#200302,
#200303,#200304,#200305,#200306,#200307,#200308,#200309,#200310,#200311,
#200312,#200313,#200314,#200315,#200316,#200317,#200318,#200319,#200320,
#200321,#200322,#200323,#200324,#200325,#200326,#200327,#200328,#200329,
#200330,#200331,#200332,#200333,#200334,#200335,#200336,#200337,#200338,
#200339,#200340,#200341,#200342,#200343,#200344,#200345,#200346,#200347,
#200348,#200349,#200350,#200351,#200352,#200353,#200354,#200355,#200356,
#200357,#200358,#200359,#200360,#200361,#200362,#200363,#200364,#200365,
#200366,#200367,#200368,#200369,#200370,#200371,#200372,#200373,#200374,
#200375,#200376,#200377,#200378,#200379,#200380,#200381,#200382,#200383,
#200384,#200385,#200386,#200387,#200388,#200389,#200390,#200391,#200392,
#200393,#200394,#200395,#200396,#200397,#200398,#200399,#200400,#200401,
#200402,#200403,#200404,#200405,#200406,#200407,#200408,#200409,#200410,
#200411,#200412,#200413,#200414,#200415,#200416,#200417,#200418,#200419,
#200420,#200421,#200422,#200423,#200424,#200425,#200426,#200427,#200428,
#200429,#200430,#200431,#200432,#200433,#200434,#200435,#200436,#200437,
#200438,#200439,#200440,#200441,#200442,#200443,#200444,#200445,#200446,
#200447,#200448,#200449,#200450,#200451,#200452,#200453,#200454,#200455),
 .UNSPECIFIED.,.F.,.F.)
B_SPLINE_CURVE_WITH_KNOTS((6,1,1,1,1,1,1,1,1,1,1,1,1,1,1,1,1,1,1,1,1,1,
1,1,1,1,1,1,1,1,1,1,1,1,1,1,1,1,1,1,1,1,1,1,1,1,1,1,1,1,1,1,1,1,1,1,1,1,
1,1,1,1,1,1,1,1,1,1,1,1,1,1,1,1,1,1,1,1,1,1,1,1,1,1,1,1,1,1,1,1,1,1,1,1,
1,1,1,1,1,1,1,1,1,1,1,1,1,1,1,1,1,1,1,1,1,1,1,1,1,1,1,1,1,1,1,1,1,1,1,1,
1,1,1,1,1,1,1,1,1,1,1,1,1,1,1,1,1,1,1,1,1,1,1,1,1,1,1,1,1,1,1,1,1,1,1,1,
1,1,1,1,1,1,1,1,1,1,1,1,1,1,1,1,1,1,1,1,1,1,1,1,1,1,1,1,1,1,1,1,1,1,6),
(0.,0.005,0.01,0.015,0.02,0.025,0.03,0.035,0.04,0.045,0.05,0.055,0.06,0.065,
0.07,0.075,0.08,0.085,0.09,0.095,0.1,0.105,0.11,0.115,0.12,0.125,0.13,0.135,
0.14,0.145,0.15,0.155,0.16,0.165,0.17,0.175,0.18,0.185,0.19,0.195,0.2,0.205,
0.21,0.215,0.22,0.225,0.23,0.235,0.24,0.245,0.25,0.255,0.26,0.265,0.27,
0.275,0.28,0.285,0.29,0.295,0.3,0.305,0.31,0.315,0.32,0.325,0.33,0.335,
0.34,0.345,0.35,0.355,0.36,0.365,0.37,0.375,0.38,0.385,0.39,0.395,0.4,0.405,
0.41,0.415,0.42,0.425,0.43,0.435,0.44,0.445,0.45,0.455,0.46,0.465,0.47,
0.475,0.48,0.485,0.49,0.495,0.5,0.505,0.51,0.515,0.52,0.525,0.53,0.535,
0.54,0.545,0.55,0.555,0.56,0.565,0.57,0.575,0.58,0.585,0.59,0.595,0.6,0.605,
0.61,0.615,0.62,0.625,0.63,0.635,0.64,0.645,0.65,0.655,0.66,0.665,0.67,
0.675,0.68,0.685,0.690000000000001,0.695000000000001,0.700000000000001,
0.705000000000001,0.710000000000001,0.715000000000001,0.720000000000001,
0.725000000000001,0.730000000000001,0.735000000000001,0.740000000000001,
0.745000000000001,0.750000000000001,0.755000000000001,0.760000000000001,
0.765000000000001,0.770000000000001,0.775000000000001,0.780000000000001,
0.785000000000001,0.790000000000001,0.795000000000001,0.800000000000001,
0.805000000000001,0.810000000000001,0.815000000000001,0.820000000000001,
0.825000000000001,0.830000000000001,0.835000000000001,0.840000000000001,
0.845000000000001,0.850000000000001,0.855000000000001,0.860000000000001,
0.865000000000001,0.870000000000001,0.875000000000001,0.880000000000001,
0.885000000000001,0.890000000000001,0.895000000000001,0.900000000000001,
0.905000000000001,0.910000000000001,0.915000000000001,0.920000000000001,
0.925000000000001,0.930000000000001,0.935000000000001,0.940000000000001,
0.945000000000001,0.950000000000001,0.955000000000001,0.960000000000001,
0.965000000000001,0.970000000000001,0.975000000000001,0.980000000000001,
0.985000000000001,0.990000000000001,0.995000000000001,1.),.UNSPECIFIED.)
CURVE()
GEOMETRIC_REPRESENTATION_ITEM()
RATIONAL_B_SPLINE_CURVE((1.,1.,1.,1.,1.,1.,1.,1.,1.,1.,1.,1.,1.,1.,1.,1.,
1.,1.,1.,1.,1.,1.,1.,1.,1.,1.,1.,1.,1.,1.,1.,1.,1.,1.,1.,1.,1.,1.,1.,1.,
1.,1.,1.,1.,1.,1.,1.,1.,1.,1.,1.,1.,1.,1.,1.,1.,1.,1.,1.,1.,1.,1.,1.,1.,
1.,1.,1.,1.,1.,1.,1.,1.,1.,1.,1.,1.,1.,1.,1.,1.,1.,1.,1.,1.,1.,1.,1.,1.,
1.,1.,1.,1.,1.,1.,1.,1.,1.,1.,1.,1.,1.,1.,1.,1.,1.,1.,1.,1.,1.,1.,1.,1.,
1.,1.,1.,1.,1.,1.,1.,1.,1.,1.,1.,1.,1.,1.,1.,1.,1.,1.,1.,1.,1.,1.,1.,1.,
1.,1.,1.,1.,1.,1.,1.,1.,1.,1.,1.,1.,1.,1.,1.,1.,1.,1.,1.,1.,1.,1.,1.,1.,
1.,1.,1.,1.,1.,1.,1.,1.,1.,1.,1.,1.,1.,1.,1.,1.,1.,1.,1.,1.,1.,1.,1.,1.,
1.,1.,1.,1.,1.,1.,1.,1.,1.,1.,1.,1.,1.,1.,1.,1.,1.,1.,1.,1.,1.))
REPRESENTATION_ITEM('')
);
#763=(
BOUNDED_CURVE()
B_SPLINE_CURVE(5,(#200872,#200873,#200874,#200875,#200876,#200877,#200878,
#200879,#200880,#200881,#200882,#200883,#200884,#200885,#200886,#200887,
#200888,#200889,#200890,#200891,#200892,#200893,#200894,#200895,#200896,
#200897,#200898,#200899,#200900,#200901,#200902,#200903,#200904,#200905,
#200906,#200907,#200908,#200909,#200910,#200911,#200912,#200913,#200914,
#200915,#200916,#200917,#200918,#200919,#200920,#200921,#200922,#200923,
#200924,#200925,#200926,#200927,#200928,#200929,#200930,#200931,#200932,
#200933,#200934,#200935,#200936,#200937,#200938,#200939,#200940,#200941,
#200942,#200943,#200944,#200945,#200946,#200947,#200948,#200949,#200950,
#200951,#200952,#200953,#200954,#200955,#200956,#200957,#200958,#200959,
#200960,#200961,#200962,#200963,#200964,#200965,#200966,#200967,#200968,
#200969,#200970,#200971,#200972,#200973,#200974,#200975,#200976,#200977,
#200978,#200979,#200980,#200981,#200982,#200983,#200984,#200985,#200986,
#200987,#200988,#200989,#200990,#200991,#200992,#200993,#200994,#200995,
#200996,#200997,#200998,#200999,#201000,#201001,#201002,#201003,#201004,
#201005,#201006,#201007,#201008,#201009,#201010,#201011,#201012,#201013,
#201014,#201015,#201016,#201017,#201018,#201019,#201020,#201021,#201022,
#201023,#201024,#201025,#201026,#201027,#201028,#201029,#201030,#201031,
#201032,#201033,#201034,#201035,#201036,#201037,#201038,#201039,#201040,
#201041,#201042,#201043,#201044,#201045,#201046,#201047,#201048,#201049,
#201050,#201051,#201052,#201053,#201054,#201055,#201056,#201057,#201058,
#201059,#201060,#201061,#201062,#201063,#201064,#201065,#201066,#201067,
#201068,#201069,#201070,#201071,#201072,#201073,#201074,#201075,#201076),
 .UNSPECIFIED.,.F.,.F.)
B_SPLINE_CURVE_WITH_KNOTS((6,1,1,1,1,1,1,1,1,1,1,1,1,1,1,1,1,1,1,1,1,1,
1,1,1,1,1,1,1,1,1,1,1,1,1,1,1,1,1,1,1,1,1,1,1,1,1,1,1,1,1,1,1,1,1,1,1,1,
1,1,1,1,1,1,1,1,1,1,1,1,1,1,1,1,1,1,1,1,1,1,1,1,1,1,1,1,1,1,1,1,1,1,1,1,
1,1,1,1,1,1,1,1,1,1,1,1,1,1,1,1,1,1,1,1,1,1,1,1,1,1,1,1,1,1,1,1,1,1,1,1,
1,1,1,1,1,1,1,1,1,1,1,1,1,1,1,1,1,1,1,1,1,1,1,1,1,1,1,1,1,1,1,1,1,1,1,1,
1,1,1,1,1,1,1,1,1,1,1,1,1,1,1,1,1,1,1,1,1,1,1,1,1,1,1,1,1,1,1,1,1,1,6),
(-1.,-0.995000000000001,-0.990000000000001,-0.985000000000001,-0.980000000000001,
-0.975000000000001,-0.970000000000001,-0.965000000000001,-0.960000000000001,
-0.955000000000001,-0.950000000000001,-0.945000000000001,-0.940000000000001,
-0.935000000000001,-0.930000000000001,-0.925000000000001,-0.920000000000001,
-0.915000000000001,-0.910000000000001,-0.905000000000001,-0.900000000000001,
-0.895000000000001,-0.890000000000001,-0.885000000000001,-0.880000000000001,
-0.875000000000001,-0.870000000000001,-0.865000000000001,-0.860000000000001,
-0.855000000000001,-0.850000000000001,-0.845000000000001,-0.840000000000001,
-0.835000000000001,-0.830000000000001,-0.825000000000001,-0.820000000000001,
-0.815000000000001,-0.810000000000001,-0.805000000000001,-0.800000000000001,
-0.795000000000001,-0.790000000000001,-0.785000000000001,-0.780000000000001,
-0.775000000000001,-0.770000000000001,-0.765000000000001,-0.760000000000001,
-0.755000000000001,-0.750000000000001,-0.745000000000001,-0.740000000000001,
-0.735000000000001,-0.730000000000001,-0.725000000000001,-0.720000000000001,
-0.715000000000001,-0.710000000000001,-0.705000000000001,-0.700000000000001,
-0.695000000000001,-0.690000000000001,-0.685,-0.68,-0.675,-0.67,-0.665,
-0.66,-0.655,-0.65,-0.645,-0.64,-0.635,-0.63,-0.625,-0.62,-0.615,-0.61,
-0.605,-0.6,-0.595,-0.59,-0.585,-0.58,-0.575,-0.57,-0.565,-0.56,-0.555,
-0.55,-0.545,-0.54,-0.535,-0.53,-0.525,-0.52,-0.515,-0.51,-0.505,-0.5,-0.495,
-0.49,-0.485,-0.48,-0.475,-0.47,-0.465,-0.46,-0.455,-0.45,-0.445,-0.44,
-0.435,-0.43,-0.425,-0.42,-0.415,-0.41,-0.405,-0.4,-0.395,-0.39,-0.385,
-0.38,-0.375,-0.37,-0.365,-0.36,-0.355,-0.35,-0.345,-0.34,-0.335,-0.33,
-0.325,-0.32,-0.315,-0.31,-0.305,-0.3,-0.295,-0.29,-0.285,-0.28,-0.275,
-0.27,-0.265,-0.26,-0.255,-0.25,-0.245,-0.24,-0.235,-0.23,-0.225,-0.22,
-0.215,-0.21,-0.205,-0.2,-0.195,-0.19,-0.185,-0.18,-0.175,-0.17,-0.165,
-0.16,-0.155,-0.15,-0.145,-0.14,-0.135,-0.13,-0.125,-0.12,-0.115,-0.11,
-0.105,-0.1,-0.095,-0.09,-0.085,-0.08,-0.075,-0.07,-0.065,-0.06,-0.055,
-0.05,-0.045,-0.04,-0.035,-0.03,-0.025,-0.02,-0.015,-0.01,-0.005,0.),
 .UNSPECIFIED.)
CURVE()
GEOMETRIC_REPRESENTATION_ITEM()
RATIONAL_B_SPLINE_CURVE((1.,1.,1.,1.,1.,1.,1.,1.,1.,1.,1.,1.,1.,1.,1.,1.,
1.,1.,1.,1.,1.,1.,1.,1.,1.,1.,1.,1.,1.,1.,1.,1.,1.,1.,1.,1.,1.,1.,1.,1.,
1.,1.,1.,1.,1.,1.,1.,1.,1.,1.,1.,1.,1.,1.,1.,1.,1.,1.,1.,1.,1.,1.,1.,1.,
1.,1.,1.,1.,1.,1.,1.,1.,1.,1.,1.,1.,1.,1.,1.,1.,1.,1.,1.,1.,1.,1.,1.,1.,
1.,1.,1.,1.,1.,1.,1.,1.,1.,1.,1.,1.,1.,1.,1.,1.,1.,1.,1.,1.,1.,1.,1.,1.,
1.,1.,1.,1.,1.,1.,1.,1.,1.,1.,1.,1.,1.,1.,1.,1.,1.,1.,1.,1.,1.,1.,1.,1.,
1.,1.,1.,1.,1.,1.,1.,1.,1.,1.,1.,1.,1.,1.,1.,1.,1.,1.,1.,1.,1.,1.,1.,1.,
1.,1.,1.,1.,1.,1.,1.,1.,1.,1.,1.,1.,1.,1.,1.,1.,1.,1.,1.,1.,1.,1.,1.,1.,
1.,1.,1.,1.,1.,1.,1.,1.,1.,1.,1.,1.,1.,1.,1.,1.,1.,1.,1.,1.,1.))
REPRESENTATION_ITEM('')
);
#764=(
BOUNDED_CURVE()
B_SPLINE_CURVE(5,(#201489,#201490,#201491,#201492,#201493,#201494,#201495,
#201496,#201497,#201498,#201499,#201500,#201501,#201502,#201503,#201504,
#201505,#201506,#201507,#201508,#201509,#201510,#201511,#201512,#201513,
#201514,#201515,#201516,#201517,#201518,#201519,#201520,#201521,#201522,
#201523,#201524,#201525,#201526,#201527,#201528,#201529,#201530,#201531,
#201532,#201533,#201534,#201535,#201536,#201537,#201538,#201539,#201540,
#201541,#201542,#201543,#201544,#201545,#201546,#201547,#201548,#201549,
#201550,#201551,#201552,#201553,#201554,#201555,#201556,#201557,#201558,
#201559,#201560,#201561,#201562,#201563,#201564,#201565,#201566,#201567,
#201568,#201569,#201570,#201571,#201572,#201573,#201574,#201575,#201576,
#201577,#201578,#201579,#201580,#201581,#201582,#201583,#201584,#201585,
#201586,#201587,#201588,#201589,#201590,#201591,#201592,#201593,#201594,
#201595,#201596,#201597,#201598,#201599,#201600,#201601,#201602,#201603,
#201604,#201605,#201606,#201607,#201608,#201609,#201610,#201611,#201612,
#201613,#201614,#201615,#201616,#201617,#201618,#201619,#201620,#201621,
#201622,#201623,#201624,#201625,#201626,#201627,#201628,#201629,#201630,
#201631,#201632,#201633,#201634,#201635,#201636,#201637,#201638,#201639,
#201640,#201641,#201642,#201643,#201644,#201645,#201646,#201647,#201648,
#201649,#201650,#201651,#201652,#201653,#201654,#201655,#201656,#201657,
#201658,#201659,#201660,#201661,#201662,#201663,#201664,#201665,#201666,
#201667,#201668,#201669,#201670,#201671,#201672,#201673,#201674,#201675,
#201676,#201677,#201678,#201679,#201680,#201681,#201682,#201683,#201684,
#201685,#201686,#201687,#201688,#201689,#201690,#201691,#201692,#201693),
 .UNSPECIFIED.,.F.,.F.)
B_SPLINE_CURVE_WITH_KNOTS((6,1,1,1,1,1,1,1,1,1,1,1,1,1,1,1,1,1,1,1,1,1,
1,1,1,1,1,1,1,1,1,1,1,1,1,1,1,1,1,1,1,1,1,1,1,1,1,1,1,1,1,1,1,1,1,1,1,1,
1,1,1,1,1,1,1,1,1,1,1,1,1,1,1,1,1,1,1,1,1,1,1,1,1,1,1,1,1,1,1,1,1,1,1,1,
1,1,1,1,1,1,1,1,1,1,1,1,1,1,1,1,1,1,1,1,1,1,1,1,1,1,1,1,1,1,1,1,1,1,1,1,
1,1,1,1,1,1,1,1,1,1,1,1,1,1,1,1,1,1,1,1,1,1,1,1,1,1,1,1,1,1,1,1,1,1,1,1,
1,1,1,1,1,1,1,1,1,1,1,1,1,1,1,1,1,1,1,1,1,1,1,1,1,1,1,1,1,1,1,1,1,1,6),
(0.,0.005,0.01,0.015,0.02,0.025,0.03,0.035,0.04,0.045,0.05,0.055,0.06,0.065,
0.07,0.075,0.08,0.085,0.09,0.095,0.1,0.105,0.11,0.115,0.12,0.125,0.13,0.135,
0.14,0.145,0.15,0.155,0.16,0.165,0.17,0.175,0.18,0.185,0.19,0.195,0.2,0.205,
0.21,0.215,0.22,0.225,0.23,0.235,0.24,0.245,0.25,0.255,0.26,0.265,0.27,
0.275,0.28,0.285,0.29,0.295,0.3,0.305,0.31,0.315,0.32,0.325,0.33,0.335,
0.34,0.345,0.35,0.355,0.36,0.365,0.37,0.375,0.38,0.385,0.39,0.395,0.4,0.405,
0.41,0.415,0.42,0.425,0.43,0.435,0.44,0.445,0.45,0.455,0.46,0.465,0.47,
0.475,0.48,0.485,0.49,0.495,0.5,0.505,0.51,0.515,0.52,0.525,0.53,0.535,
0.54,0.545,0.55,0.555,0.56,0.565,0.57,0.575,0.58,0.585,0.59,0.595,0.6,0.605,
0.61,0.615,0.62,0.625,0.63,0.635,0.64,0.645,0.65,0.655,0.66,0.665,0.67,
0.675,0.68,0.685,0.690000000000001,0.695000000000001,0.700000000000001,
0.705000000000001,0.710000000000001,0.715000000000001,0.720000000000001,
0.725000000000001,0.730000000000001,0.735000000000001,0.740000000000001,
0.745000000000001,0.750000000000001,0.755000000000001,0.760000000000001,
0.765000000000001,0.770000000000001,0.775000000000001,0.780000000000001,
0.785000000000001,0.790000000000001,0.795000000000001,0.800000000000001,
0.805000000000001,0.810000000000001,0.815000000000001,0.820000000000001,
0.825000000000001,0.830000000000001,0.835000000000001,0.840000000000001,
0.845000000000001,0.850000000000001,0.855000000000001,0.860000000000001,
0.865000000000001,0.870000000000001,0.875000000000001,0.880000000000001,
0.885000000000001,0.890000000000001,0.895000000000001,0.900000000000001,
0.905000000000001,0.910000000000001,0.915000000000001,0.920000000000001,
0.925000000000001,0.930000000000001,0.935000000000001,0.940000000000001,
0.945000000000001,0.950000000000001,0.955000000000001,0.960000000000001,
0.965000000000001,0.970000000000001,0.975000000000001,0.980000000000001,
0.985000000000001,0.990000000000001,0.995000000000001,1.),.UNSPECIFIED.)
CURVE()
GEOMETRIC_REPRESENTATION_ITEM()
RATIONAL_B_SPLINE_CURVE((1.,1.,1.,1.,1.,1.,1.,1.,1.,1.,1.,1.,1.,1.,1.,1.,
1.,1.,1.,1.,1.,1.,1.,1.,1.,1.,1.,1.,1.,1.,1.,1.,1.,1.,1.,1.,1.,1.,1.,1.,
1.,1.,1.,1.,1.,1.,1.,1.,1.,1.,1.,1.,1.,1.,1.,1.,1.,1.,1.,1.,1.,1.,1.,1.,
1.,1.,1.,1.,1.,1.,1.,1.,1.,1.,1.,1.,1.,1.,1.,1.,1.,1.,1.,1.,1.,1.,1.,1.,
1.,1.,1.,1.,1.,1.,1.,1.,1.,1.,1.,1.,1.,1.,1.,1.,1.,1.,1.,1.,1.,1.,1.,1.,
1.,1.,1.,1.,1.,1.,1.,1.,1.,1.,1.,1.,1.,1.,1.,1.,1.,1.,1.,1.,1.,1.,1.,1.,
1.,1.,1.,1.,1.,1.,1.,1.,1.,1.,1.,1.,1.,1.,1.,1.,1.,1.,1.,1.,1.,1.,1.,1.,
1.,1.,1.,1.,1.,1.,1.,1.,1.,1.,1.,1.,1.,1.,1.,1.,1.,1.,1.,1.,1.,1.,1.,1.,
1.,1.,1.,1.,1.,1.,1.,1.,1.,1.,1.,1.,1.,1.,1.,1.,1.,1.,1.,1.,1.))
REPRESENTATION_ITEM('')
);
#765=(
BOUNDED_CURVE()
B_SPLINE_CURVE(5,(#202110,#202111,#202112,#202113,#202114,#202115,#202116,
#202117,#202118,#202119,#202120,#202121,#202122,#202123,#202124,#202125,
#202126,#202127,#202128,#202129,#202130,#202131,#202132,#202133,#202134,
#202135,#202136,#202137,#202138,#202139,#202140,#202141,#202142,#202143,
#202144,#202145,#202146,#202147,#202148,#202149,#202150,#202151,#202152,
#202153,#202154,#202155,#202156,#202157,#202158,#202159,#202160,#202161,
#202162,#202163,#202164,#202165,#202166,#202167,#202168,#202169,#202170,
#202171,#202172,#202173,#202174,#202175,#202176,#202177,#202178,#202179,
#202180,#202181,#202182,#202183,#202184,#202185,#202186,#202187,#202188,
#202189,#202190,#202191,#202192,#202193,#202194,#202195,#202196,#202197,
#202198,#202199,#202200,#202201,#202202,#202203,#202204,#202205,#202206,
#202207,#202208,#202209,#202210,#202211,#202212,#202213,#202214,#202215,
#202216,#202217,#202218,#202219,#202220,#202221,#202222,#202223,#202224,
#202225,#202226,#202227,#202228,#202229,#202230,#202231,#202232,#202233,
#202234,#202235,#202236,#202237,#202238,#202239,#202240,#202241,#202242,
#202243,#202244,#202245,#202246,#202247,#202248,#202249,#202250,#202251,
#202252,#202253,#202254,#202255,#202256,#202257,#202258,#202259,#202260,
#202261,#202262,#202263,#202264,#202265,#202266,#202267,#202268,#202269,
#202270,#202271,#202272,#202273,#202274,#202275,#202276,#202277,#202278,
#202279,#202280,#202281,#202282,#202283,#202284,#202285,#202286,#202287,
#202288,#202289,#202290,#202291,#202292,#202293,#202294,#202295,#202296,
#202297,#202298,#202299,#202300,#202301,#202302,#202303,#202304,#202305,
#202306,#202307,#202308,#202309,#202310,#202311,#202312,#202313,#202314),
 .UNSPECIFIED.,.F.,.F.)
B_SPLINE_CURVE_WITH_KNOTS((6,1,1,1,1,1,1,1,1,1,1,1,1,1,1,1,1,1,1,1,1,1,
1,1,1,1,1,1,1,1,1,1,1,1,1,1,1,1,1,1,1,1,1,1,1,1,1,1,1,1,1,1,1,1,1,1,1,1,
1,1,1,1,1,1,1,1,1,1,1,1,1,1,1,1,1,1,1,1,1,1,1,1,1,1,1,1,1,1,1,1,1,1,1,1,
1,1,1,1,1,1,1,1,1,1,1,1,1,1,1,1,1,1,1,1,1,1,1,1,1,1,1,1,1,1,1,1,1,1,1,1,
1,1,1,1,1,1,1,1,1,1,1,1,1,1,1,1,1,1,1,1,1,1,1,1,1,1,1,1,1,1,1,1,1,1,1,1,
1,1,1,1,1,1,1,1,1,1,1,1,1,1,1,1,1,1,1,1,1,1,1,1,1,1,1,1,1,1,1,1,1,1,6),
(-1.,-0.995000000000001,-0.990000000000001,-0.985000000000001,-0.980000000000001,
-0.975000000000001,-0.970000000000001,-0.965000000000001,-0.960000000000001,
-0.955000000000001,-0.950000000000001,-0.945000000000001,-0.940000000000001,
-0.935000000000001,-0.930000000000001,-0.925000000000001,-0.920000000000001,
-0.915000000000001,-0.910000000000001,-0.905000000000001,-0.900000000000001,
-0.895000000000001,-0.890000000000001,-0.885000000000001,-0.880000000000001,
-0.875000000000001,-0.870000000000001,-0.865000000000001,-0.860000000000001,
-0.855000000000001,-0.850000000000001,-0.845000000000001,-0.840000000000001,
-0.835000000000001,-0.830000000000001,-0.825000000000001,-0.820000000000001,
-0.815000000000001,-0.810000000000001,-0.805000000000001,-0.800000000000001,
-0.795000000000001,-0.790000000000001,-0.785000000000001,-0.780000000000001,
-0.775000000000001,-0.770000000000001,-0.765000000000001,-0.760000000000001,
-0.755000000000001,-0.750000000000001,-0.745000000000001,-0.740000000000001,
-0.735000000000001,-0.730000000000001,-0.725000000000001,-0.720000000000001,
-0.715000000000001,-0.710000000000001,-0.705000000000001,-0.700000000000001,
-0.695000000000001,-0.690000000000001,-0.685,-0.68,-0.675,-0.67,-0.665,
-0.66,-0.655,-0.65,-0.645,-0.64,-0.635,-0.63,-0.625,-0.62,-0.615,-0.61,
-0.605,-0.6,-0.595,-0.59,-0.585,-0.58,-0.575,-0.57,-0.565,-0.56,-0.555,
-0.55,-0.545,-0.54,-0.535,-0.53,-0.525,-0.52,-0.515,-0.51,-0.505,-0.5,-0.495,
-0.49,-0.485,-0.48,-0.475,-0.47,-0.465,-0.46,-0.455,-0.45,-0.445,-0.44,
-0.435,-0.43,-0.425,-0.42,-0.415,-0.41,-0.405,-0.4,-0.395,-0.39,-0.385,
-0.38,-0.375,-0.37,-0.365,-0.36,-0.355,-0.35,-0.345,-0.34,-0.335,-0.33,
-0.325,-0.32,-0.315,-0.31,-0.305,-0.3,-0.295,-0.29,-0.285,-0.28,-0.275,
-0.27,-0.265,-0.26,-0.255,-0.25,-0.245,-0.24,-0.235,-0.23,-0.225,-0.22,
-0.215,-0.21,-0.205,-0.2,-0.195,-0.19,-0.185,-0.18,-0.175,-0.17,-0.165,
-0.16,-0.155,-0.15,-0.145,-0.14,-0.135,-0.13,-0.125,-0.12,-0.115,-0.11,
-0.105,-0.1,-0.095,-0.09,-0.085,-0.08,-0.075,-0.07,-0.065,-0.06,-0.055,
-0.05,-0.045,-0.04,-0.035,-0.03,-0.025,-0.02,-0.015,-0.01,-0.005,0.),
 .UNSPECIFIED.)
CURVE()
GEOMETRIC_REPRESENTATION_ITEM()
RATIONAL_B_SPLINE_CURVE((1.,1.,1.,1.,1.,1.,1.,1.,1.,1.,1.,1.,1.,1.,1.,1.,
1.,1.,1.,1.,1.,1.,1.,1.,1.,1.,1.,1.,1.,1.,1.,1.,1.,1.,1.,1.,1.,1.,1.,1.,
1.,1.,1.,1.,1.,1.,1.,1.,1.,1.,1.,1.,1.,1.,1.,1.,1.,1.,1.,1.,1.,1.,1.,1.,
1.,1.,1.,1.,1.,1.,1.,1.,1.,1.,1.,1.,1.,1.,1.,1.,1.,1.,1.,1.,1.,1.,1.,1.,
1.,1.,1.,1.,1.,1.,1.,1.,1.,1.,1.,1.,1.,1.,1.,1.,1.,1.,1.,1.,1.,1.,1.,1.,
1.,1.,1.,1.,1.,1.,1.,1.,1.,1.,1.,1.,1.,1.,1.,1.,1.,1.,1.,1.,1.,1.,1.,1.,
1.,1.,1.,1.,1.,1.,1.,1.,1.,1.,1.,1.,1.,1.,1.,1.,1.,1.,1.,1.,1.,1.,1.,1.,
1.,1.,1.,1.,1.,1.,1.,1.,1.,1.,1.,1.,1.,1.,1.,1.,1.,1.,1.,1.,1.,1.,1.,1.,
1.,1.,1.,1.,1.,1.,1.,1.,1.,1.,1.,1.,1.,1.,1.,1.,1.,1.,1.,1.,1.))
REPRESENTATION_ITEM('')
);
#766=(
BOUNDED_CURVE()
B_SPLINE_CURVE(5,(#202727,#202728,#202729,#202730,#202731,#202732,#202733,
#202734,#202735,#202736,#202737,#202738,#202739,#202740,#202741,#202742,
#202743,#202744,#202745,#202746,#202747,#202748,#202749,#202750,#202751,
#202752,#202753,#202754,#202755,#202756,#202757,#202758,#202759,#202760,
#202761,#202762,#202763,#202764,#202765,#202766,#202767,#202768,#202769,
#202770,#202771,#202772,#202773,#202774,#202775,#202776,#202777,#202778,
#202779,#202780,#202781,#202782,#202783,#202784,#202785,#202786,#202787,
#202788,#202789,#202790,#202791,#202792,#202793,#202794,#202795,#202796,
#202797,#202798,#202799,#202800,#202801,#202802,#202803,#202804,#202805,
#202806,#202807,#202808,#202809,#202810,#202811,#202812,#202813,#202814,
#202815,#202816,#202817,#202818,#202819,#202820,#202821,#202822,#202823,
#202824,#202825,#202826,#202827,#202828,#202829,#202830,#202831,#202832,
#202833,#202834,#202835,#202836,#202837,#202838,#202839,#202840,#202841,
#202842,#202843,#202844,#202845,#202846,#202847,#202848,#202849,#202850,
#202851,#202852,#202853,#202854,#202855,#202856,#202857,#202858,#202859,
#202860,#202861,#202862,#202863,#202864,#202865,#202866,#202867,#202868,
#202869,#202870,#202871,#202872,#202873,#202874,#202875,#202876,#202877,
#202878,#202879,#202880,#202881,#202882,#202883,#202884,#202885,#202886,
#202887,#202888,#202889,#202890,#202891,#202892,#202893,#202894,#202895,
#202896,#202897,#202898,#202899,#202900,#202901,#202902,#202903,#202904,
#202905,#202906,#202907,#202908,#202909,#202910,#202911,#202912,#202913,
#202914,#202915,#202916,#202917,#202918,#202919,#202920,#202921,#202922,
#202923,#202924,#202925,#202926,#202927,#202928,#202929,#202930,#202931),
 .UNSPECIFIED.,.F.,.F.)
B_SPLINE_CURVE_WITH_KNOTS((6,1,1,1,1,1,1,1,1,1,1,1,1,1,1,1,1,1,1,1,1,1,
1,1,1,1,1,1,1,1,1,1,1,1,1,1,1,1,1,1,1,1,1,1,1,1,1,1,1,1,1,1,1,1,1,1,1,1,
1,1,1,1,1,1,1,1,1,1,1,1,1,1,1,1,1,1,1,1,1,1,1,1,1,1,1,1,1,1,1,1,1,1,1,1,
1,1,1,1,1,1,1,1,1,1,1,1,1,1,1,1,1,1,1,1,1,1,1,1,1,1,1,1,1,1,1,1,1,1,1,1,
1,1,1,1,1,1,1,1,1,1,1,1,1,1,1,1,1,1,1,1,1,1,1,1,1,1,1,1,1,1,1,1,1,1,1,1,
1,1,1,1,1,1,1,1,1,1,1,1,1,1,1,1,1,1,1,1,1,1,1,1,1,1,1,1,1,1,1,1,1,1,6),
(0.,0.005,0.01,0.015,0.02,0.025,0.03,0.035,0.04,0.045,0.05,0.055,0.06,0.065,
0.07,0.075,0.08,0.085,0.09,0.095,0.1,0.105,0.11,0.115,0.12,0.125,0.13,0.135,
0.14,0.145,0.15,0.155,0.16,0.165,0.17,0.175,0.18,0.185,0.19,0.195,0.2,0.205,
0.21,0.215,0.22,0.225,0.23,0.235,0.24,0.245,0.25,0.255,0.26,0.265,0.27,
0.275,0.28,0.285,0.29,0.295,0.3,0.305,0.31,0.315,0.32,0.325,0.33,0.335,
0.34,0.345,0.35,0.355,0.36,0.365,0.37,0.375,0.38,0.385,0.39,0.395,0.4,0.405,
0.41,0.415,0.42,0.425,0.43,0.435,0.44,0.445,0.45,0.455,0.46,0.465,0.47,
0.475,0.48,0.485,0.49,0.495,0.5,0.505,0.51,0.515,0.52,0.525,0.53,0.535,
0.54,0.545,0.55,0.555,0.56,0.565,0.57,0.575,0.58,0.585,0.59,0.595,0.6,0.605,
0.61,0.615,0.62,0.625,0.63,0.635,0.64,0.645,0.65,0.655,0.66,0.665,0.67,
0.675,0.68,0.685,0.690000000000001,0.695000000000001,0.700000000000001,
0.705000000000001,0.710000000000001,0.715000000000001,0.720000000000001,
0.725000000000001,0.730000000000001,0.735000000000001,0.740000000000001,
0.745000000000001,0.750000000000001,0.755000000000001,0.760000000000001,
0.765000000000001,0.770000000000001,0.775000000000001,0.780000000000001,
0.785000000000001,0.790000000000001,0.795000000000001,0.800000000000001,
0.805000000000001,0.810000000000001,0.815000000000001,0.820000000000001,
0.825000000000001,0.830000000000001,0.835000000000001,0.840000000000001,
0.845000000000001,0.850000000000001,0.855000000000001,0.860000000000001,
0.865000000000001,0.870000000000001,0.875000000000001,0.880000000000001,
0.885000000000001,0.890000000000001,0.895000000000001,0.900000000000001,
0.905000000000001,0.910000000000001,0.915000000000001,0.920000000000001,
0.925000000000001,0.930000000000001,0.935000000000001,0.940000000000001,
0.945000000000001,0.950000000000001,0.955000000000001,0.960000000000001,
0.965000000000001,0.970000000000001,0.975000000000001,0.980000000000001,
0.985000000000001,0.990000000000001,0.995000000000001,1.),.UNSPECIFIED.)
CURVE()
GEOMETRIC_REPRESENTATION_ITEM()
RATIONAL_B_SPLINE_CURVE((1.,1.,1.,1.,1.,1.,1.,1.,1.,1.,1.,1.,1.,1.,1.,1.,
1.,1.,1.,1.,1.,1.,1.,1.,1.,1.,1.,1.,1.,1.,1.,1.,1.,1.,1.,1.,1.,1.,1.,1.,
1.,1.,1.,1.,1.,1.,1.,1.,1.,1.,1.,1.,1.,1.,1.,1.,1.,1.,1.,1.,1.,1.,1.,1.,
1.,1.,1.,1.,1.,1.,1.,1.,1.,1.,1.,1.,1.,1.,1.,1.,1.,1.,1.,1.,1.,1.,1.,1.,
1.,1.,1.,1.,1.,1.,1.,1.,1.,1.,1.,1.,1.,1.,1.,1.,1.,1.,1.,1.,1.,1.,1.,1.,
1.,1.,1.,1.,1.,1.,1.,1.,1.,1.,1.,1.,1.,1.,1.,1.,1.,1.,1.,1.,1.,1.,1.,1.,
1.,1.,1.,1.,1.,1.,1.,1.,1.,1.,1.,1.,1.,1.,1.,1.,1.,1.,1.,1.,1.,1.,1.,1.,
1.,1.,1.,1.,1.,1.,1.,1.,1.,1.,1.,1.,1.,1.,1.,1.,1.,1.,1.,1.,1.,1.,1.,1.,
1.,1.,1.,1.,1.,1.,1.,1.,1.,1.,1.,1.,1.,1.,1.,1.,1.,1.,1.,1.,1.))
REPRESENTATION_ITEM('')
);
#767=(
BOUNDED_CURVE()
B_SPLINE_CURVE(5,(#203348,#203349,#203350,#203351,#203352,#203353,#203354,
#203355,#203356,#203357,#203358,#203359,#203360,#203361,#203362,#203363,
#203364,#203365,#203366,#203367,#203368,#203369,#203370,#203371,#203372,
#203373,#203374,#203375,#203376,#203377,#203378,#203379,#203380,#203381,
#203382,#203383,#203384,#203385,#203386,#203387,#203388,#203389,#203390,
#203391,#203392,#203393,#203394,#203395,#203396,#203397,#203398,#203399,
#203400,#203401,#203402,#203403,#203404,#203405,#203406,#203407,#203408,
#203409,#203410,#203411,#203412,#203413,#203414,#203415,#203416,#203417,
#203418,#203419,#203420,#203421,#203422,#203423,#203424,#203425,#203426,
#203427,#203428,#203429,#203430,#203431,#203432,#203433,#203434,#203435,
#203436,#203437,#203438,#203439,#203440,#203441,#203442,#203443,#203444,
#203445,#203446,#203447,#203448,#203449,#203450,#203451,#203452,#203453,
#203454,#203455,#203456,#203457,#203458,#203459,#203460,#203461,#203462,
#203463,#203464,#203465,#203466,#203467,#203468,#203469,#203470,#203471,
#203472,#203473,#203474,#203475,#203476,#203477,#203478,#203479,#203480,
#203481,#203482,#203483,#203484,#203485,#203486,#203487,#203488,#203489,
#203490,#203491,#203492,#203493,#203494,#203495,#203496,#203497,#203498,
#203499,#203500,#203501,#203502,#203503,#203504,#203505,#203506,#203507,
#203508,#203509,#203510,#203511,#203512,#203513,#203514,#203515,#203516,
#203517,#203518,#203519,#203520,#203521,#203522,#203523,#203524,#203525,
#203526,#203527,#203528,#203529,#203530,#203531,#203532,#203533,#203534,
#203535,#203536,#203537,#203538,#203539,#203540,#203541,#203542,#203543,
#203544,#203545,#203546,#203547,#203548,#203549,#203550,#203551,#203552),
 .UNSPECIFIED.,.F.,.F.)
B_SPLINE_CURVE_WITH_KNOTS((6,1,1,1,1,1,1,1,1,1,1,1,1,1,1,1,1,1,1,1,1,1,
1,1,1,1,1,1,1,1,1,1,1,1,1,1,1,1,1,1,1,1,1,1,1,1,1,1,1,1,1,1,1,1,1,1,1,1,
1,1,1,1,1,1,1,1,1,1,1,1,1,1,1,1,1,1,1,1,1,1,1,1,1,1,1,1,1,1,1,1,1,1,1,1,
1,1,1,1,1,1,1,1,1,1,1,1,1,1,1,1,1,1,1,1,1,1,1,1,1,1,1,1,1,1,1,1,1,1,1,1,
1,1,1,1,1,1,1,1,1,1,1,1,1,1,1,1,1,1,1,1,1,1,1,1,1,1,1,1,1,1,1,1,1,1,1,1,
1,1,1,1,1,1,1,1,1,1,1,1,1,1,1,1,1,1,1,1,1,1,1,1,1,1,1,1,1,1,1,1,1,1,6),
(-1.,-0.995000000000001,-0.990000000000001,-0.985000000000001,-0.980000000000001,
-0.975000000000001,-0.970000000000001,-0.965000000000001,-0.960000000000001,
-0.955000000000001,-0.950000000000001,-0.945000000000001,-0.940000000000001,
-0.935000000000001,-0.930000000000001,-0.925000000000001,-0.920000000000001,
-0.915000000000001,-0.910000000000001,-0.905000000000001,-0.900000000000001,
-0.895000000000001,-0.890000000000001,-0.885000000000001,-0.880000000000001,
-0.875000000000001,-0.870000000000001,-0.865000000000001,-0.860000000000001,
-0.855000000000001,-0.850000000000001,-0.845000000000001,-0.840000000000001,
-0.835000000000001,-0.830000000000001,-0.825000000000001,-0.820000000000001,
-0.815000000000001,-0.810000000000001,-0.805000000000001,-0.800000000000001,
-0.795000000000001,-0.790000000000001,-0.785000000000001,-0.780000000000001,
-0.775000000000001,-0.770000000000001,-0.765000000000001,-0.760000000000001,
-0.755000000000001,-0.750000000000001,-0.745000000000001,-0.740000000000001,
-0.735000000000001,-0.730000000000001,-0.725000000000001,-0.720000000000001,
-0.715000000000001,-0.710000000000001,-0.705000000000001,-0.700000000000001,
-0.695000000000001,-0.690000000000001,-0.685,-0.68,-0.675,-0.67,-0.665,
-0.66,-0.655,-0.65,-0.645,-0.64,-0.635,-0.63,-0.625,-0.62,-0.615,-0.61,
-0.605,-0.6,-0.595,-0.59,-0.585,-0.58,-0.575,-0.57,-0.565,-0.56,-0.555,
-0.55,-0.545,-0.54,-0.535,-0.53,-0.525,-0.52,-0.515,-0.51,-0.505,-0.5,-0.495,
-0.49,-0.485,-0.48,-0.475,-0.47,-0.465,-0.46,-0.455,-0.45,-0.445,-0.44,
-0.435,-0.43,-0.425,-0.42,-0.415,-0.41,-0.405,-0.4,-0.395,-0.39,-0.385,
-0.38,-0.375,-0.37,-0.365,-0.36,-0.355,-0.35,-0.345,-0.34,-0.335,-0.33,
-0.325,-0.32,-0.315,-0.31,-0.305,-0.3,-0.295,-0.29,-0.285,-0.28,-0.275,
-0.27,-0.265,-0.26,-0.255,-0.25,-0.245,-0.24,-0.235,-0.23,-0.225,-0.22,
-0.215,-0.21,-0.205,-0.2,-0.195,-0.19,-0.185,-0.18,-0.175,-0.17,-0.165,
-0.16,-0.155,-0.15,-0.145,-0.14,-0.135,-0.13,-0.125,-0.12,-0.115,-0.11,
-0.105,-0.1,-0.095,-0.09,-0.085,-0.08,-0.075,-0.07,-0.065,-0.06,-0.055,
-0.05,-0.045,-0.04,-0.035,-0.03,-0.025,-0.02,-0.015,-0.01,-0.005,0.),
 .UNSPECIFIED.)
CURVE()
GEOMETRIC_REPRESENTATION_ITEM()
RATIONAL_B_SPLINE_CURVE((1.,1.,1.,1.,1.,1.,1.,1.,1.,1.,1.,1.,1.,1.,1.,1.,
1.,1.,1.,1.,1.,1.,1.,1.,1.,1.,1.,1.,1.,1.,1.,1.,1.,1.,1.,1.,1.,1.,1.,1.,
1.,1.,1.,1.,1.,1.,1.,1.,1.,1.,1.,1.,1.,1.,1.,1.,1.,1.,1.,1.,1.,1.,1.,1.,
1.,1.,1.,1.,1.,1.,1.,1.,1.,1.,1.,1.,1.,1.,1.,1.,1.,1.,1.,1.,1.,1.,1.,1.,
1.,1.,1.,1.,1.,1.,1.,1.,1.,1.,1.,1.,1.,1.,1.,1.,1.,1.,1.,1.,1.,1.,1.,1.,
1.,1.,1.,1.,1.,1.,1.,1.,1.,1.,1.,1.,1.,1.,1.,1.,1.,1.,1.,1.,1.,1.,1.,1.,
1.,1.,1.,1.,1.,1.,1.,1.,1.,1.,1.,1.,1.,1.,1.,1.,1.,1.,1.,1.,1.,1.,1.,1.,
1.,1.,1.,1.,1.,1.,1.,1.,1.,1.,1.,1.,1.,1.,1.,1.,1.,1.,1.,1.,1.,1.,1.,1.,
1.,1.,1.,1.,1.,1.,1.,1.,1.,1.,1.,1.,1.,1.,1.,1.,1.,1.,1.,1.,1.))
REPRESENTATION_ITEM('')
);
#768=(
BOUNDED_CURVE()
B_SPLINE_CURVE(5,(#203965,#203966,#203967,#203968,#203969,#203970,#203971,
#203972,#203973,#203974,#203975,#203976,#203977,#203978,#203979,#203980,
#203981,#203982,#203983,#203984,#203985,#203986,#203987,#203988,#203989,
#203990,#203991,#203992,#203993,#203994,#203995,#203996,#203997,#203998,
#203999,#204000,#204001,#204002,#204003,#204004,#204005,#204006,#204007,
#204008,#204009,#204010,#204011,#204012,#204013,#204014,#204015,#204016,
#204017,#204018,#204019,#204020,#204021,#204022,#204023,#204024,#204025,
#204026,#204027,#204028,#204029,#204030,#204031,#204032,#204033,#204034,
#204035,#204036,#204037,#204038,#204039,#204040,#204041,#204042,#204043,
#204044,#204045,#204046,#204047,#204048,#204049,#204050,#204051,#204052,
#204053,#204054,#204055,#204056,#204057,#204058,#204059,#204060,#204061,
#204062,#204063,#204064,#204065,#204066,#204067,#204068,#204069,#204070,
#204071,#204072,#204073,#204074,#204075,#204076,#204077,#204078,#204079,
#204080,#204081,#204082,#204083,#204084,#204085,#204086,#204087,#204088,
#204089,#204090,#204091,#204092,#204093,#204094,#204095,#204096,#204097,
#204098,#204099,#204100,#204101,#204102,#204103,#204104,#204105,#204106,
#204107,#204108,#204109,#204110,#204111,#204112,#204113,#204114,#204115,
#204116,#204117,#204118,#204119,#204120,#204121,#204122,#204123,#204124,
#204125,#204126,#204127,#204128,#204129,#204130,#204131,#204132,#204133,
#204134,#204135,#204136,#204137,#204138,#204139,#204140,#204141,#204142,
#204143,#204144,#204145,#204146,#204147,#204148,#204149,#204150,#204151,
#204152,#204153,#204154,#204155,#204156,#204157,#204158,#204159,#204160,
#204161,#204162,#204163,#204164,#204165,#204166,#204167,#204168,#204169),
 .UNSPECIFIED.,.F.,.F.)
B_SPLINE_CURVE_WITH_KNOTS((6,1,1,1,1,1,1,1,1,1,1,1,1,1,1,1,1,1,1,1,1,1,
1,1,1,1,1,1,1,1,1,1,1,1,1,1,1,1,1,1,1,1,1,1,1,1,1,1,1,1,1,1,1,1,1,1,1,1,
1,1,1,1,1,1,1,1,1,1,1,1,1,1,1,1,1,1,1,1,1,1,1,1,1,1,1,1,1,1,1,1,1,1,1,1,
1,1,1,1,1,1,1,1,1,1,1,1,1,1,1,1,1,1,1,1,1,1,1,1,1,1,1,1,1,1,1,1,1,1,1,1,
1,1,1,1,1,1,1,1,1,1,1,1,1,1,1,1,1,1,1,1,1,1,1,1,1,1,1,1,1,1,1,1,1,1,1,1,
1,1,1,1,1,1,1,1,1,1,1,1,1,1,1,1,1,1,1,1,1,1,1,1,1,1,1,1,1,1,1,1,1,1,6),
(0.,0.005,0.01,0.015,0.02,0.025,0.03,0.035,0.04,0.045,0.05,0.055,0.06,0.065,
0.07,0.075,0.08,0.085,0.09,0.095,0.1,0.105,0.11,0.115,0.12,0.125,0.13,0.135,
0.14,0.145,0.15,0.155,0.16,0.165,0.17,0.175,0.18,0.185,0.19,0.195,0.2,0.205,
0.21,0.215,0.22,0.225,0.23,0.235,0.24,0.245,0.25,0.255,0.26,0.265,0.27,
0.275,0.28,0.285,0.29,0.295,0.3,0.305,0.31,0.315,0.32,0.325,0.33,0.335,
0.34,0.345,0.35,0.355,0.36,0.365,0.37,0.375,0.38,0.385,0.39,0.395,0.4,0.405,
0.41,0.415,0.42,0.425,0.43,0.435,0.44,0.445,0.45,0.455,0.46,0.465,0.47,
0.475,0.48,0.485,0.49,0.495,0.5,0.505,0.51,0.515,0.52,0.525,0.53,0.535,
0.54,0.545,0.55,0.555,0.56,0.565,0.57,0.575,0.58,0.585,0.59,0.595,0.6,0.605,
0.61,0.615,0.62,0.625,0.63,0.635,0.64,0.645,0.65,0.655,0.66,0.665,0.67,
0.675,0.68,0.685,0.690000000000001,0.695000000000001,0.700000000000001,
0.705000000000001,0.710000000000001,0.715000000000001,0.720000000000001,
0.725000000000001,0.730000000000001,0.735000000000001,0.740000000000001,
0.745000000000001,0.750000000000001,0.755000000000001,0.760000000000001,
0.765000000000001,0.770000000000001,0.775000000000001,0.780000000000001,
0.785000000000001,0.790000000000001,0.795000000000001,0.800000000000001,
0.805000000000001,0.810000000000001,0.815000000000001,0.820000000000001,
0.825000000000001,0.830000000000001,0.835000000000001,0.840000000000001,
0.845000000000001,0.850000000000001,0.855000000000001,0.860000000000001,
0.865000000000001,0.870000000000001,0.875000000000001,0.880000000000001,
0.885000000000001,0.890000000000001,0.895000000000001,0.900000000000001,
0.905000000000001,0.910000000000001,0.915000000000001,0.920000000000001,
0.925000000000001,0.930000000000001,0.935000000000001,0.940000000000001,
0.945000000000001,0.950000000000001,0.955000000000001,0.960000000000001,
0.965000000000001,0.970000000000001,0.975000000000001,0.980000000000001,
0.985000000000001,0.990000000000001,0.995000000000001,1.),.UNSPECIFIED.)
CURVE()
GEOMETRIC_REPRESENTATION_ITEM()
RATIONAL_B_SPLINE_CURVE((1.,1.,1.,1.,1.,1.,1.,1.,1.,1.,1.,1.,1.,1.,1.,1.,
1.,1.,1.,1.,1.,1.,1.,1.,1.,1.,1.,1.,1.,1.,1.,1.,1.,1.,1.,1.,1.,1.,1.,1.,
1.,1.,1.,1.,1.,1.,1.,1.,1.,1.,1.,1.,1.,1.,1.,1.,1.,1.,1.,1.,1.,1.,1.,1.,
1.,1.,1.,1.,1.,1.,1.,1.,1.,1.,1.,1.,1.,1.,1.,1.,1.,1.,1.,1.,1.,1.,1.,1.,
1.,1.,1.,1.,1.,1.,1.,1.,1.,1.,1.,1.,1.,1.,1.,1.,1.,1.,1.,1.,1.,1.,1.,1.,
1.,1.,1.,1.,1.,1.,1.,1.,1.,1.,1.,1.,1.,1.,1.,1.,1.,1.,1.,1.,1.,1.,1.,1.,
1.,1.,1.,1.,1.,1.,1.,1.,1.,1.,1.,1.,1.,1.,1.,1.,1.,1.,1.,1.,1.,1.,1.,1.,
1.,1.,1.,1.,1.,1.,1.,1.,1.,1.,1.,1.,1.,1.,1.,1.,1.,1.,1.,1.,1.,1.,1.,1.,
1.,1.,1.,1.,1.,1.,1.,1.,1.,1.,1.,1.,1.,1.,1.,1.,1.,1.,1.,1.,1.))
REPRESENTATION_ITEM('')
);
#769=(
BOUNDED_CURVE()
B_SPLINE_CURVE(5,(#204586,#204587,#204588,#204589,#204590,#204591,#204592,
#204593,#204594,#204595,#204596,#204597,#204598,#204599,#204600,#204601,
#204602,#204603,#204604,#204605,#204606,#204607,#204608,#204609,#204610,
#204611,#204612,#204613,#204614,#204615,#204616,#204617,#204618,#204619,
#204620,#204621,#204622,#204623,#204624,#204625,#204626,#204627,#204628,
#204629,#204630,#204631,#204632,#204633,#204634,#204635,#204636,#204637,
#204638,#204639,#204640,#204641,#204642,#204643,#204644,#204645,#204646,
#204647,#204648,#204649,#204650,#204651,#204652,#204653,#204654,#204655,
#204656,#204657,#204658,#204659,#204660,#204661,#204662,#204663,#204664,
#204665,#204666,#204667,#204668,#204669,#204670,#204671,#204672,#204673,
#204674,#204675,#204676,#204677,#204678,#204679,#204680,#204681,#204682,
#204683,#204684,#204685,#204686,#204687,#204688,#204689,#204690,#204691,
#204692,#204693,#204694,#204695,#204696,#204697,#204698,#204699,#204700,
#204701,#204702,#204703,#204704,#204705,#204706,#204707,#204708,#204709,
#204710,#204711,#204712,#204713,#204714,#204715,#204716,#204717,#204718,
#204719,#204720,#204721,#204722,#204723,#204724,#204725,#204726,#204727,
#204728,#204729,#204730,#204731,#204732,#204733,#204734,#204735,#204736,
#204737,#204738,#204739,#204740,#204741,#204742,#204743,#204744,#204745,
#204746,#204747,#204748,#204749,#204750,#204751,#204752,#204753,#204754,
#204755,#204756,#204757,#204758,#204759,#204760,#204761,#204762,#204763,
#204764,#204765,#204766,#204767,#204768,#204769,#204770,#204771,#204772,
#204773,#204774,#204775,#204776,#204777,#204778,#204779,#204780,#204781,
#204782,#204783,#204784,#204785,#204786,#204787,#204788,#204789,#204790),
 .UNSPECIFIED.,.F.,.F.)
B_SPLINE_CURVE_WITH_KNOTS((6,1,1,1,1,1,1,1,1,1,1,1,1,1,1,1,1,1,1,1,1,1,
1,1,1,1,1,1,1,1,1,1,1,1,1,1,1,1,1,1,1,1,1,1,1,1,1,1,1,1,1,1,1,1,1,1,1,1,
1,1,1,1,1,1,1,1,1,1,1,1,1,1,1,1,1,1,1,1,1,1,1,1,1,1,1,1,1,1,1,1,1,1,1,1,
1,1,1,1,1,1,1,1,1,1,1,1,1,1,1,1,1,1,1,1,1,1,1,1,1,1,1,1,1,1,1,1,1,1,1,1,
1,1,1,1,1,1,1,1,1,1,1,1,1,1,1,1,1,1,1,1,1,1,1,1,1,1,1,1,1,1,1,1,1,1,1,1,
1,1,1,1,1,1,1,1,1,1,1,1,1,1,1,1,1,1,1,1,1,1,1,1,1,1,1,1,1,1,1,1,1,1,6),
(-1.,-0.995000000000001,-0.990000000000001,-0.985000000000001,-0.980000000000001,
-0.975000000000001,-0.970000000000001,-0.965000000000001,-0.960000000000001,
-0.955000000000001,-0.950000000000001,-0.945000000000001,-0.940000000000001,
-0.935000000000001,-0.930000000000001,-0.925000000000001,-0.920000000000001,
-0.915000000000001,-0.910000000000001,-0.905000000000001,-0.900000000000001,
-0.895000000000001,-0.890000000000001,-0.885000000000001,-0.880000000000001,
-0.875000000000001,-0.870000000000001,-0.865000000000001,-0.860000000000001,
-0.855000000000001,-0.850000000000001,-0.845000000000001,-0.840000000000001,
-0.835000000000001,-0.830000000000001,-0.825000000000001,-0.820000000000001,
-0.815000000000001,-0.810000000000001,-0.805000000000001,-0.800000000000001,
-0.795000000000001,-0.790000000000001,-0.785000000000001,-0.780000000000001,
-0.775000000000001,-0.770000000000001,-0.765000000000001,-0.760000000000001,
-0.755000000000001,-0.750000000000001,-0.745000000000001,-0.740000000000001,
-0.735000000000001,-0.730000000000001,-0.725000000000001,-0.720000000000001,
-0.715000000000001,-0.710000000000001,-0.705000000000001,-0.700000000000001,
-0.695000000000001,-0.690000000000001,-0.685,-0.68,-0.675,-0.67,-0.665,
-0.66,-0.655,-0.65,-0.645,-0.64,-0.635,-0.63,-0.625,-0.62,-0.615,-0.61,
-0.605,-0.6,-0.595,-0.59,-0.585,-0.58,-0.575,-0.57,-0.565,-0.56,-0.555,
-0.55,-0.545,-0.54,-0.535,-0.53,-0.525,-0.52,-0.515,-0.51,-0.505,-0.5,-0.495,
-0.49,-0.485,-0.48,-0.475,-0.47,-0.465,-0.46,-0.455,-0.45,-0.445,-0.44,
-0.435,-0.43,-0.425,-0.42,-0.415,-0.41,-0.405,-0.4,-0.395,-0.39,-0.385,
-0.38,-0.375,-0.37,-0.365,-0.36,-0.355,-0.35,-0.345,-0.34,-0.335,-0.33,
-0.325,-0.32,-0.315,-0.31,-0.305,-0.3,-0.295,-0.29,-0.285,-0.28,-0.275,
-0.27,-0.265,-0.26,-0.255,-0.25,-0.245,-0.24,-0.235,-0.23,-0.225,-0.22,
-0.215,-0.21,-0.205,-0.2,-0.195,-0.19,-0.185,-0.18,-0.175,-0.17,-0.165,
-0.16,-0.155,-0.15,-0.145,-0.14,-0.135,-0.13,-0.125,-0.12,-0.115,-0.11,
-0.105,-0.1,-0.095,-0.09,-0.085,-0.08,-0.075,-0.07,-0.065,-0.06,-0.055,
-0.05,-0.045,-0.04,-0.035,-0.03,-0.025,-0.02,-0.015,-0.01,-0.005,0.),
 .UNSPECIFIED.)
CURVE()
GEOMETRIC_REPRESENTATION_ITEM()
RATIONAL_B_SPLINE_CURVE((1.,1.,1.,1.,1.,1.,1.,1.,1.,1.,1.,1.,1.,1.,1.,1.,
1.,1.,1.,1.,1.,1.,1.,1.,1.,1.,1.,1.,1.,1.,1.,1.,1.,1.,1.,1.,1.,1.,1.,1.,
1.,1.,1.,1.,1.,1.,1.,1.,1.,1.,1.,1.,1.,1.,1.,1.,1.,1.,1.,1.,1.,1.,1.,1.,
1.,1.,1.,1.,1.,1.,1.,1.,1.,1.,1.,1.,1.,1.,1.,1.,1.,1.,1.,1.,1.,1.,1.,1.,
1.,1.,1.,1.,1.,1.,1.,1.,1.,1.,1.,1.,1.,1.,1.,1.,1.,1.,1.,1.,1.,1.,1.,1.,
1.,1.,1.,1.,1.,1.,1.,1.,1.,1.,1.,1.,1.,1.,1.,1.,1.,1.,1.,1.,1.,1.,1.,1.,
1.,1.,1.,1.,1.,1.,1.,1.,1.,1.,1.,1.,1.,1.,1.,1.,1.,1.,1.,1.,1.,1.,1.,1.,
1.,1.,1.,1.,1.,1.,1.,1.,1.,1.,1.,1.,1.,1.,1.,1.,1.,1.,1.,1.,1.,1.,1.,1.,
1.,1.,1.,1.,1.,1.,1.,1.,1.,1.,1.,1.,1.,1.,1.,1.,1.,1.,1.,1.,1.))
REPRESENTATION_ITEM('')
);
#770=(
BOUNDED_CURVE()
B_SPLINE_CURVE(5,(#205203,#205204,#205205,#205206,#205207,#205208,#205209,
#205210,#205211,#205212,#205213,#205214,#205215,#205216,#205217,#205218,
#205219,#205220,#205221,#205222,#205223,#205224,#205225,#205226,#205227,
#205228,#205229,#205230,#205231,#205232,#205233,#205234,#205235,#205236,
#205237,#205238,#205239,#205240,#205241,#205242,#205243,#205244,#205245,
#205246,#205247,#205248,#205249,#205250,#205251,#205252,#205253,#205254,
#205255,#205256,#205257,#205258,#205259,#205260,#205261,#205262,#205263,
#205264,#205265,#205266,#205267,#205268,#205269,#205270,#205271,#205272,
#205273,#205274,#205275,#205276,#205277,#205278,#205279,#205280,#205281,
#205282,#205283,#205284,#205285,#205286,#205287,#205288,#205289,#205290,
#205291,#205292,#205293,#205294,#205295,#205296,#205297,#205298,#205299,
#205300,#205301,#205302,#205303,#205304,#205305,#205306,#205307,#205308,
#205309,#205310,#205311,#205312,#205313,#205314,#205315,#205316,#205317,
#205318,#205319,#205320,#205321,#205322,#205323,#205324,#205325,#205326,
#205327,#205328,#205329,#205330,#205331,#205332,#205333,#205334,#205335,
#205336,#205337,#205338,#205339,#205340,#205341,#205342,#205343,#205344,
#205345,#205346,#205347,#205348,#205349,#205350,#205351,#205352,#205353,
#205354,#205355,#205356,#205357,#205358,#205359,#205360,#205361,#205362,
#205363,#205364,#205365,#205366,#205367,#205368,#205369,#205370,#205371,
#205372,#205373,#205374,#205375,#205376,#205377,#205378,#205379,#205380,
#205381,#205382,#205383,#205384,#205385,#205386,#205387,#205388,#205389,
#205390,#205391,#205392,#205393,#205394,#205395,#205396,#205397,#205398,
#205399,#205400,#205401,#205402,#205403,#205404,#205405,#205406,#205407),
 .UNSPECIFIED.,.F.,.F.)
B_SPLINE_CURVE_WITH_KNOTS((6,1,1,1,1,1,1,1,1,1,1,1,1,1,1,1,1,1,1,1,1,1,
1,1,1,1,1,1,1,1,1,1,1,1,1,1,1,1,1,1,1,1,1,1,1,1,1,1,1,1,1,1,1,1,1,1,1,1,
1,1,1,1,1,1,1,1,1,1,1,1,1,1,1,1,1,1,1,1,1,1,1,1,1,1,1,1,1,1,1,1,1,1,1,1,
1,1,1,1,1,1,1,1,1,1,1,1,1,1,1,1,1,1,1,1,1,1,1,1,1,1,1,1,1,1,1,1,1,1,1,1,
1,1,1,1,1,1,1,1,1,1,1,1,1,1,1,1,1,1,1,1,1,1,1,1,1,1,1,1,1,1,1,1,1,1,1,1,
1,1,1,1,1,1,1,1,1,1,1,1,1,1,1,1,1,1,1,1,1,1,1,1,1,1,1,1,1,1,1,1,1,1,6),
(0.,0.005,0.01,0.015,0.02,0.025,0.03,0.035,0.04,0.045,0.05,0.055,0.06,0.065,
0.07,0.075,0.08,0.085,0.09,0.095,0.1,0.105,0.11,0.115,0.12,0.125,0.13,0.135,
0.14,0.145,0.15,0.155,0.16,0.165,0.17,0.175,0.18,0.185,0.19,0.195,0.2,0.205,
0.21,0.215,0.22,0.225,0.23,0.235,0.24,0.245,0.25,0.255,0.26,0.265,0.27,
0.275,0.28,0.285,0.29,0.295,0.3,0.305,0.31,0.315,0.32,0.325,0.33,0.335,
0.34,0.345,0.35,0.355,0.36,0.365,0.37,0.375,0.38,0.385,0.39,0.395,0.4,0.405,
0.41,0.415,0.42,0.425,0.43,0.435,0.44,0.445,0.45,0.455,0.46,0.465,0.47,
0.475,0.48,0.485,0.49,0.495,0.5,0.505,0.51,0.515,0.52,0.525,0.53,0.535,
0.54,0.545,0.55,0.555,0.56,0.565,0.57,0.575,0.58,0.585,0.59,0.595,0.6,0.605,
0.61,0.615,0.62,0.625,0.63,0.635,0.64,0.645,0.65,0.655,0.66,0.665,0.67,
0.675,0.68,0.685,0.690000000000001,0.695000000000001,0.700000000000001,
0.705000000000001,0.710000000000001,0.715000000000001,0.720000000000001,
0.725000000000001,0.730000000000001,0.735000000000001,0.740000000000001,
0.745000000000001,0.750000000000001,0.755000000000001,0.760000000000001,
0.765000000000001,0.770000000000001,0.775000000000001,0.780000000000001,
0.785000000000001,0.790000000000001,0.795000000000001,0.800000000000001,
0.805000000000001,0.810000000000001,0.815000000000001,0.820000000000001,
0.825000000000001,0.830000000000001,0.835000000000001,0.840000000000001,
0.845000000000001,0.850000000000001,0.855000000000001,0.860000000000001,
0.865000000000001,0.870000000000001,0.875000000000001,0.880000000000001,
0.885000000000001,0.890000000000001,0.895000000000001,0.900000000000001,
0.905000000000001,0.910000000000001,0.915000000000001,0.920000000000001,
0.925000000000001,0.930000000000001,0.935000000000001,0.940000000000001,
0.945000000000001,0.950000000000001,0.955000000000001,0.960000000000001,
0.965000000000001,0.970000000000001,0.975000000000001,0.980000000000001,
0.985000000000001,0.990000000000001,0.995000000000001,1.),.UNSPECIFIED.)
CURVE()
GEOMETRIC_REPRESENTATION_ITEM()
RATIONAL_B_SPLINE_CURVE((1.,1.,1.,1.,1.,1.,1.,1.,1.,1.,1.,1.,1.,1.,1.,1.,
1.,1.,1.,1.,1.,1.,1.,1.,1.,1.,1.,1.,1.,1.,1.,1.,1.,1.,1.,1.,1.,1.,1.,1.,
1.,1.,1.,1.,1.,1.,1.,1.,1.,1.,1.,1.,1.,1.,1.,1.,1.,1.,1.,1.,1.,1.,1.,1.,
1.,1.,1.,1.,1.,1.,1.,1.,1.,1.,1.,1.,1.,1.,1.,1.,1.,1.,1.,1.,1.,1.,1.,1.,
1.,1.,1.,1.,1.,1.,1.,1.,1.,1.,1.,1.,1.,1.,1.,1.,1.,1.,1.,1.,1.,1.,1.,1.,
1.,1.,1.,1.,1.,1.,1.,1.,1.,1.,1.,1.,1.,1.,1.,1.,1.,1.,1.,1.,1.,1.,1.,1.,
1.,1.,1.,1.,1.,1.,1.,1.,1.,1.,1.,1.,1.,1.,1.,1.,1.,1.,1.,1.,1.,1.,1.,1.,
1.,1.,1.,1.,1.,1.,1.,1.,1.,1.,1.,1.,1.,1.,1.,1.,1.,1.,1.,1.,1.,1.,1.,1.,
1.,1.,1.,1.,1.,1.,1.,1.,1.,1.,1.,1.,1.,1.,1.,1.,1.,1.,1.,1.,1.))
REPRESENTATION_ITEM('')
);
#771=(
BOUNDED_CURVE()
B_SPLINE_CURVE(5,(#205824,#205825,#205826,#205827,#205828,#205829,#205830,
#205831,#205832,#205833,#205834,#205835,#205836,#205837,#205838,#205839,
#205840,#205841,#205842,#205843,#205844,#205845,#205846,#205847,#205848,
#205849,#205850,#205851,#205852,#205853,#205854,#205855,#205856,#205857,
#205858,#205859,#205860,#205861,#205862,#205863,#205864,#205865,#205866,
#205867,#205868,#205869,#205870,#205871,#205872,#205873,#205874,#205875,
#205876,#205877,#205878,#205879,#205880,#205881,#205882,#205883,#205884,
#205885,#205886,#205887,#205888,#205889,#205890,#205891,#205892,#205893,
#205894,#205895,#205896,#205897,#205898,#205899,#205900,#205901,#205902,
#205903,#205904,#205905,#205906,#205907,#205908,#205909,#205910,#205911,
#205912,#205913,#205914,#205915,#205916,#205917,#205918,#205919,#205920,
#205921,#205922,#205923,#205924,#205925,#205926,#205927,#205928,#205929,
#205930,#205931,#205932,#205933,#205934,#205935,#205936,#205937,#205938,
#205939,#205940,#205941,#205942,#205943,#205944,#205945,#205946,#205947,
#205948,#205949,#205950,#205951,#205952,#205953,#205954,#205955,#205956,
#205957,#205958,#205959,#205960,#205961,#205962,#205963,#205964,#205965,
#205966,#205967,#205968,#205969,#205970,#205971,#205972,#205973,#205974,
#205975,#205976,#205977,#205978,#205979,#205980,#205981,#205982,#205983,
#205984,#205985,#205986,#205987,#205988,#205989,#205990,#205991,#205992,
#205993,#205994,#205995,#205996,#205997,#205998,#205999,#206000,#206001,
#206002,#206003,#206004,#206005,#206006,#206007,#206008,#206009,#206010,
#206011,#206012,#206013,#206014,#206015,#206016,#206017,#206018,#206019,
#206020,#206021,#206022,#206023,#206024,#206025,#206026,#206027,#206028),
 .UNSPECIFIED.,.F.,.F.)
B_SPLINE_CURVE_WITH_KNOTS((6,1,1,1,1,1,1,1,1,1,1,1,1,1,1,1,1,1,1,1,1,1,
1,1,1,1,1,1,1,1,1,1,1,1,1,1,1,1,1,1,1,1,1,1,1,1,1,1,1,1,1,1,1,1,1,1,1,1,
1,1,1,1,1,1,1,1,1,1,1,1,1,1,1,1,1,1,1,1,1,1,1,1,1,1,1,1,1,1,1,1,1,1,1,1,
1,1,1,1,1,1,1,1,1,1,1,1,1,1,1,1,1,1,1,1,1,1,1,1,1,1,1,1,1,1,1,1,1,1,1,1,
1,1,1,1,1,1,1,1,1,1,1,1,1,1,1,1,1,1,1,1,1,1,1,1,1,1,1,1,1,1,1,1,1,1,1,1,
1,1,1,1,1,1,1,1,1,1,1,1,1,1,1,1,1,1,1,1,1,1,1,1,1,1,1,1,1,1,1,1,1,1,6),
(-1.,-0.995000000000001,-0.990000000000001,-0.985000000000001,-0.980000000000001,
-0.975000000000001,-0.970000000000001,-0.965000000000001,-0.960000000000001,
-0.955000000000001,-0.950000000000001,-0.945000000000001,-0.940000000000001,
-0.935000000000001,-0.930000000000001,-0.925000000000001,-0.920000000000001,
-0.915000000000001,-0.910000000000001,-0.905000000000001,-0.900000000000001,
-0.895000000000001,-0.890000000000001,-0.885000000000001,-0.880000000000001,
-0.875000000000001,-0.870000000000001,-0.865000000000001,-0.860000000000001,
-0.855000000000001,-0.850000000000001,-0.845000000000001,-0.840000000000001,
-0.835000000000001,-0.830000000000001,-0.825000000000001,-0.820000000000001,
-0.815000000000001,-0.810000000000001,-0.805000000000001,-0.800000000000001,
-0.795000000000001,-0.790000000000001,-0.785000000000001,-0.780000000000001,
-0.775000000000001,-0.770000000000001,-0.765000000000001,-0.760000000000001,
-0.755000000000001,-0.750000000000001,-0.745000000000001,-0.740000000000001,
-0.735000000000001,-0.730000000000001,-0.725000000000001,-0.720000000000001,
-0.715000000000001,-0.710000000000001,-0.705000000000001,-0.700000000000001,
-0.695000000000001,-0.690000000000001,-0.685,-0.68,-0.675,-0.67,-0.665,
-0.66,-0.655,-0.65,-0.645,-0.64,-0.635,-0.63,-0.625,-0.62,-0.615,-0.61,
-0.605,-0.6,-0.595,-0.59,-0.585,-0.58,-0.575,-0.57,-0.565,-0.56,-0.555,
-0.55,-0.545,-0.54,-0.535,-0.53,-0.525,-0.52,-0.515,-0.51,-0.505,-0.5,-0.495,
-0.49,-0.485,-0.48,-0.475,-0.47,-0.465,-0.46,-0.455,-0.45,-0.445,-0.44,
-0.435,-0.43,-0.425,-0.42,-0.415,-0.41,-0.405,-0.4,-0.395,-0.39,-0.385,
-0.38,-0.375,-0.37,-0.365,-0.36,-0.355,-0.35,-0.345,-0.34,-0.335,-0.33,
-0.325,-0.32,-0.315,-0.31,-0.305,-0.3,-0.295,-0.29,-0.285,-0.28,-0.275,
-0.27,-0.265,-0.26,-0.255,-0.25,-0.245,-0.24,-0.235,-0.23,-0.225,-0.22,
-0.215,-0.21,-0.205,-0.2,-0.195,-0.19,-0.185,-0.18,-0.175,-0.17,-0.165,
-0.16,-0.155,-0.15,-0.145,-0.14,-0.135,-0.13,-0.125,-0.12,-0.115,-0.11,
-0.105,-0.1,-0.095,-0.09,-0.085,-0.08,-0.075,-0.07,-0.065,-0.06,-0.055,
-0.05,-0.045,-0.04,-0.035,-0.03,-0.025,-0.02,-0.015,-0.01,-0.005,0.),
 .UNSPECIFIED.)
CURVE()
GEOMETRIC_REPRESENTATION_ITEM()
RATIONAL_B_SPLINE_CURVE((1.,1.,1.,1.,1.,1.,1.,1.,1.,1.,1.,1.,1.,1.,1.,1.,
1.,1.,1.,1.,1.,1.,1.,1.,1.,1.,1.,1.,1.,1.,1.,1.,1.,1.,1.,1.,1.,1.,1.,1.,
1.,1.,1.,1.,1.,1.,1.,1.,1.,1.,1.,1.,1.,1.,1.,1.,1.,1.,1.,1.,1.,1.,1.,1.,
1.,1.,1.,1.,1.,1.,1.,1.,1.,1.,1.,1.,1.,1.,1.,1.,1.,1.,1.,1.,1.,1.,1.,1.,
1.,1.,1.,1.,1.,1.,1.,1.,1.,1.,1.,1.,1.,1.,1.,1.,1.,1.,1.,1.,1.,1.,1.,1.,
1.,1.,1.,1.,1.,1.,1.,1.,1.,1.,1.,1.,1.,1.,1.,1.,1.,1.,1.,1.,1.,1.,1.,1.,
1.,1.,1.,1.,1.,1.,1.,1.,1.,1.,1.,1.,1.,1.,1.,1.,1.,1.,1.,1.,1.,1.,1.,1.,
1.,1.,1.,1.,1.,1.,1.,1.,1.,1.,1.,1.,1.,1.,1.,1.,1.,1.,1.,1.,1.,1.,1.,1.,
1.,1.,1.,1.,1.,1.,1.,1.,1.,1.,1.,1.,1.,1.,1.,1.,1.,1.,1.,1.,1.))
REPRESENTATION_ITEM('')
);
#772=(
BOUNDED_CURVE()
B_SPLINE_CURVE(5,(#206441,#206442,#206443,#206444,#206445,#206446,#206447,
#206448,#206449,#206450,#206451,#206452,#206453,#206454,#206455,#206456,
#206457,#206458,#206459,#206460,#206461,#206462,#206463,#206464,#206465,
#206466,#206467,#206468,#206469,#206470,#206471,#206472,#206473,#206474,
#206475,#206476,#206477,#206478,#206479,#206480,#206481,#206482,#206483,
#206484,#206485,#206486,#206487,#206488,#206489,#206490,#206491,#206492,
#206493,#206494,#206495,#206496,#206497,#206498,#206499,#206500,#206501,
#206502,#206503,#206504,#206505,#206506,#206507,#206508,#206509,#206510,
#206511,#206512,#206513,#206514,#206515,#206516,#206517,#206518,#206519,
#206520,#206521,#206522,#206523,#206524,#206525,#206526,#206527,#206528,
#206529,#206530,#206531,#206532,#206533,#206534,#206535,#206536,#206537,
#206538,#206539,#206540,#206541,#206542,#206543,#206544,#206545,#206546,
#206547,#206548,#206549,#206550,#206551,#206552,#206553,#206554,#206555,
#206556,#206557,#206558,#206559,#206560,#206561,#206562,#206563,#206564,
#206565,#206566,#206567,#206568,#206569,#206570,#206571,#206572,#206573,
#206574,#206575,#206576,#206577,#206578,#206579,#206580,#206581,#206582,
#206583,#206584,#206585,#206586,#206587,#206588,#206589,#206590,#206591,
#206592,#206593,#206594,#206595,#206596,#206597,#206598,#206599,#206600,
#206601,#206602,#206603,#206604,#206605,#206606,#206607,#206608,#206609,
#206610,#206611,#206612,#206613,#206614,#206615,#206616,#206617,#206618,
#206619,#206620,#206621,#206622,#206623,#206624,#206625,#206626,#206627,
#206628,#206629,#206630,#206631,#206632,#206633,#206634,#206635,#206636,
#206637,#206638,#206639,#206640,#206641,#206642,#206643,#206644,#206645),
 .UNSPECIFIED.,.F.,.F.)
B_SPLINE_CURVE_WITH_KNOTS((6,1,1,1,1,1,1,1,1,1,1,1,1,1,1,1,1,1,1,1,1,1,
1,1,1,1,1,1,1,1,1,1,1,1,1,1,1,1,1,1,1,1,1,1,1,1,1,1,1,1,1,1,1,1,1,1,1,1,
1,1,1,1,1,1,1,1,1,1,1,1,1,1,1,1,1,1,1,1,1,1,1,1,1,1,1,1,1,1,1,1,1,1,1,1,
1,1,1,1,1,1,1,1,1,1,1,1,1,1,1,1,1,1,1,1,1,1,1,1,1,1,1,1,1,1,1,1,1,1,1,1,
1,1,1,1,1,1,1,1,1,1,1,1,1,1,1,1,1,1,1,1,1,1,1,1,1,1,1,1,1,1,1,1,1,1,1,1,
1,1,1,1,1,1,1,1,1,1,1,1,1,1,1,1,1,1,1,1,1,1,1,1,1,1,1,1,1,1,1,1,1,1,6),
(0.,0.005,0.01,0.015,0.02,0.025,0.03,0.035,0.04,0.045,0.05,0.055,0.06,0.065,
0.07,0.075,0.08,0.085,0.09,0.095,0.1,0.105,0.11,0.115,0.12,0.125,0.13,0.135,
0.14,0.145,0.15,0.155,0.16,0.165,0.17,0.175,0.18,0.185,0.19,0.195,0.2,0.205,
0.21,0.215,0.22,0.225,0.23,0.235,0.24,0.245,0.25,0.255,0.26,0.265,0.27,
0.275,0.28,0.285,0.29,0.295,0.3,0.305,0.31,0.315,0.32,0.325,0.33,0.335,
0.34,0.345,0.35,0.355,0.36,0.365,0.37,0.375,0.38,0.385,0.39,0.395,0.4,0.405,
0.41,0.415,0.42,0.425,0.43,0.435,0.44,0.445,0.45,0.455,0.46,0.465,0.47,
0.475,0.48,0.485,0.49,0.495,0.5,0.505,0.51,0.515,0.52,0.525,0.53,0.535,
0.54,0.545,0.55,0.555,0.56,0.565,0.57,0.575,0.58,0.585,0.59,0.595,0.6,0.605,
0.61,0.615,0.62,0.625,0.63,0.635,0.64,0.645,0.65,0.655,0.66,0.665,0.67,
0.675,0.68,0.685,0.690000000000001,0.695000000000001,0.700000000000001,
0.705000000000001,0.710000000000001,0.715000000000001,0.720000000000001,
0.725000000000001,0.730000000000001,0.735000000000001,0.740000000000001,
0.745000000000001,0.750000000000001,0.755000000000001,0.760000000000001,
0.765000000000001,0.770000000000001,0.775000000000001,0.780000000000001,
0.785000000000001,0.790000000000001,0.795000000000001,0.800000000000001,
0.805000000000001,0.810000000000001,0.815000000000001,0.820000000000001,
0.825000000000001,0.830000000000001,0.835000000000001,0.840000000000001,
0.845000000000001,0.850000000000001,0.855000000000001,0.860000000000001,
0.865000000000001,0.870000000000001,0.875000000000001,0.880000000000001,
0.885000000000001,0.890000000000001,0.895000000000001,0.900000000000001,
0.905000000000001,0.910000000000001,0.915000000000001,0.920000000000001,
0.925000000000001,0.930000000000001,0.935000000000001,0.940000000000001,
0.945000000000001,0.950000000000001,0.955000000000001,0.960000000000001,
0.965000000000001,0.970000000000001,0.975000000000001,0.980000000000001,
0.985000000000001,0.990000000000001,0.995000000000001,1.),.UNSPECIFIED.)
CURVE()
GEOMETRIC_REPRESENTATION_ITEM()
RATIONAL_B_SPLINE_CURVE((1.,1.,1.,1.,1.,1.,1.,1.,1.,1.,1.,1.,1.,1.,1.,1.,
1.,1.,1.,1.,1.,1.,1.,1.,1.,1.,1.,1.,1.,1.,1.,1.,1.,1.,1.,1.,1.,1.,1.,1.,
1.,1.,1.,1.,1.,1.,1.,1.,1.,1.,1.,1.,1.,1.,1.,1.,1.,1.,1.,1.,1.,1.,1.,1.,
1.,1.,1.,1.,1.,1.,1.,1.,1.,1.,1.,1.,1.,1.,1.,1.,1.,1.,1.,1.,1.,1.,1.,1.,
1.,1.,1.,1.,1.,1.,1.,1.,1.,1.,1.,1.,1.,1.,1.,1.,1.,1.,1.,1.,1.,1.,1.,1.,
1.,1.,1.,1.,1.,1.,1.,1.,1.,1.,1.,1.,1.,1.,1.,1.,1.,1.,1.,1.,1.,1.,1.,1.,
1.,1.,1.,1.,1.,1.,1.,1.,1.,1.,1.,1.,1.,1.,1.,1.,1.,1.,1.,1.,1.,1.,1.,1.,
1.,1.,1.,1.,1.,1.,1.,1.,1.,1.,1.,1.,1.,1.,1.,1.,1.,1.,1.,1.,1.,1.,1.,1.,
1.,1.,1.,1.,1.,1.,1.,1.,1.,1.,1.,1.,1.,1.,1.,1.,1.,1.,1.,1.,1.))
REPRESENTATION_ITEM('')
);
#773=(
BOUNDED_CURVE()
B_SPLINE_CURVE(5,(#207062,#207063,#207064,#207065,#207066,#207067,#207068,
#207069,#207070,#207071,#207072,#207073,#207074,#207075,#207076,#207077,
#207078,#207079,#207080,#207081,#207082,#207083,#207084,#207085,#207086,
#207087,#207088,#207089,#207090,#207091,#207092,#207093,#207094,#207095,
#207096,#207097,#207098,#207099,#207100,#207101,#207102,#207103,#207104,
#207105,#207106,#207107,#207108,#207109,#207110,#207111,#207112,#207113,
#207114,#207115,#207116,#207117,#207118,#207119,#207120,#207121,#207122,
#207123,#207124,#207125,#207126,#207127,#207128,#207129,#207130,#207131,
#207132,#207133,#207134,#207135,#207136,#207137,#207138,#207139,#207140,
#207141,#207142,#207143,#207144,#207145,#207146,#207147,#207148,#207149,
#207150,#207151,#207152,#207153,#207154,#207155,#207156,#207157,#207158,
#207159,#207160,#207161,#207162,#207163,#207164,#207165,#207166,#207167,
#207168,#207169,#207170,#207171,#207172,#207173,#207174,#207175,#207176,
#207177,#207178,#207179,#207180,#207181,#207182,#207183,#207184,#207185,
#207186,#207187,#207188,#207189,#207190,#207191,#207192,#207193,#207194,
#207195,#207196,#207197,#207198,#207199,#207200,#207201,#207202,#207203,
#207204,#207205,#207206,#207207,#207208,#207209,#207210,#207211,#207212,
#207213,#207214,#207215,#207216,#207217,#207218,#207219,#207220,#207221,
#207222,#207223,#207224,#207225,#207226,#207227,#207228,#207229,#207230,
#207231,#207232,#207233,#207234,#207235,#207236,#207237,#207238,#207239,
#207240,#207241,#207242,#207243,#207244,#207245,#207246,#207247,#207248,
#207249,#207250,#207251,#207252,#207253,#207254,#207255,#207256,#207257,
#207258,#207259,#207260,#207261,#207262,#207263,#207264,#207265,#207266),
 .UNSPECIFIED.,.F.,.F.)
B_SPLINE_CURVE_WITH_KNOTS((6,1,1,1,1,1,1,1,1,1,1,1,1,1,1,1,1,1,1,1,1,1,
1,1,1,1,1,1,1,1,1,1,1,1,1,1,1,1,1,1,1,1,1,1,1,1,1,1,1,1,1,1,1,1,1,1,1,1,
1,1,1,1,1,1,1,1,1,1,1,1,1,1,1,1,1,1,1,1,1,1,1,1,1,1,1,1,1,1,1,1,1,1,1,1,
1,1,1,1,1,1,1,1,1,1,1,1,1,1,1,1,1,1,1,1,1,1,1,1,1,1,1,1,1,1,1,1,1,1,1,1,
1,1,1,1,1,1,1,1,1,1,1,1,1,1,1,1,1,1,1,1,1,1,1,1,1,1,1,1,1,1,1,1,1,1,1,1,
1,1,1,1,1,1,1,1,1,1,1,1,1,1,1,1,1,1,1,1,1,1,1,1,1,1,1,1,1,1,1,1,1,1,6),
(-1.,-0.995000000000001,-0.990000000000001,-0.985000000000001,-0.980000000000001,
-0.975000000000001,-0.970000000000001,-0.965000000000001,-0.960000000000001,
-0.955000000000001,-0.950000000000001,-0.945000000000001,-0.940000000000001,
-0.935000000000001,-0.930000000000001,-0.925000000000001,-0.920000000000001,
-0.915000000000001,-0.910000000000001,-0.905000000000001,-0.900000000000001,
-0.895000000000001,-0.890000000000001,-0.885000000000001,-0.880000000000001,
-0.875000000000001,-0.870000000000001,-0.865000000000001,-0.860000000000001,
-0.855000000000001,-0.850000000000001,-0.845000000000001,-0.840000000000001,
-0.835000000000001,-0.830000000000001,-0.825000000000001,-0.820000000000001,
-0.815000000000001,-0.810000000000001,-0.805000000000001,-0.800000000000001,
-0.795000000000001,-0.790000000000001,-0.785000000000001,-0.780000000000001,
-0.775000000000001,-0.770000000000001,-0.765000000000001,-0.760000000000001,
-0.755000000000001,-0.750000000000001,-0.745000000000001,-0.740000000000001,
-0.735000000000001,-0.730000000000001,-0.725000000000001,-0.720000000000001,
-0.715000000000001,-0.710000000000001,-0.705000000000001,-0.700000000000001,
-0.695000000000001,-0.690000000000001,-0.685,-0.68,-0.675,-0.67,-0.665,
-0.66,-0.655,-0.65,-0.645,-0.64,-0.635,-0.63,-0.625,-0.62,-0.615,-0.61,
-0.605,-0.6,-0.595,-0.59,-0.585,-0.58,-0.575,-0.57,-0.565,-0.56,-0.555,
-0.55,-0.545,-0.54,-0.535,-0.53,-0.525,-0.52,-0.515,-0.51,-0.505,-0.5,-0.495,
-0.49,-0.485,-0.48,-0.475,-0.47,-0.465,-0.46,-0.455,-0.45,-0.445,-0.44,
-0.435,-0.43,-0.425,-0.42,-0.415,-0.41,-0.405,-0.4,-0.395,-0.39,-0.385,
-0.38,-0.375,-0.37,-0.365,-0.36,-0.355,-0.35,-0.345,-0.34,-0.335,-0.33,
-0.325,-0.32,-0.315,-0.31,-0.305,-0.3,-0.295,-0.29,-0.285,-0.28,-0.275,
-0.27,-0.265,-0.26,-0.255,-0.25,-0.245,-0.24,-0.235,-0.23,-0.225,-0.22,
-0.215,-0.21,-0.205,-0.2,-0.195,-0.19,-0.185,-0.18,-0.175,-0.17,-0.165,
-0.16,-0.155,-0.15,-0.145,-0.14,-0.135,-0.13,-0.125,-0.12,-0.115,-0.11,
-0.105,-0.1,-0.095,-0.09,-0.085,-0.08,-0.075,-0.07,-0.065,-0.06,-0.055,
-0.05,-0.045,-0.04,-0.035,-0.03,-0.025,-0.02,-0.015,-0.01,-0.005,0.),
 .UNSPECIFIED.)
CURVE()
GEOMETRIC_REPRESENTATION_ITEM()
RATIONAL_B_SPLINE_CURVE((1.,1.,1.,1.,1.,1.,1.,1.,1.,1.,1.,1.,1.,1.,1.,1.,
1.,1.,1.,1.,1.,1.,1.,1.,1.,1.,1.,1.,1.,1.,1.,1.,1.,1.,1.,1.,1.,1.,1.,1.,
1.,1.,1.,1.,1.,1.,1.,1.,1.,1.,1.,1.,1.,1.,1.,1.,1.,1.,1.,1.,1.,1.,1.,1.,
1.,1.,1.,1.,1.,1.,1.,1.,1.,1.,1.,1.,1.,1.,1.,1.,1.,1.,1.,1.,1.,1.,1.,1.,
1.,1.,1.,1.,1.,1.,1.,1.,1.,1.,1.,1.,1.,1.,1.,1.,1.,1.,1.,1.,1.,1.,1.,1.,
1.,1.,1.,1.,1.,1.,1.,1.,1.,1.,1.,1.,1.,1.,1.,1.,1.,1.,1.,1.,1.,1.,1.,1.,
1.,1.,1.,1.,1.,1.,1.,1.,1.,1.,1.,1.,1.,1.,1.,1.,1.,1.,1.,1.,1.,1.,1.,1.,
1.,1.,1.,1.,1.,1.,1.,1.,1.,1.,1.,1.,1.,1.,1.,1.,1.,1.,1.,1.,1.,1.,1.,1.,
1.,1.,1.,1.,1.,1.,1.,1.,1.,1.,1.,1.,1.,1.,1.,1.,1.,1.,1.,1.,1.))
REPRESENTATION_ITEM('')
);
#774=(
BOUNDED_CURVE()
B_SPLINE_CURVE(5,(#207679,#207680,#207681,#207682,#207683,#207684,#207685,
#207686,#207687,#207688,#207689,#207690,#207691,#207692,#207693,#207694,
#207695,#207696,#207697,#207698,#207699,#207700,#207701,#207702,#207703,
#207704,#207705,#207706,#207707,#207708,#207709,#207710,#207711,#207712,
#207713,#207714,#207715,#207716,#207717,#207718,#207719,#207720,#207721,
#207722,#207723,#207724,#207725,#207726,#207727,#207728,#207729,#207730,
#207731,#207732,#207733,#207734,#207735,#207736,#207737,#207738,#207739,
#207740,#207741,#207742,#207743,#207744,#207745,#207746,#207747,#207748,
#207749,#207750,#207751,#207752,#207753,#207754,#207755,#207756,#207757,
#207758,#207759,#207760,#207761,#207762,#207763,#207764,#207765,#207766,
#207767,#207768,#207769,#207770,#207771,#207772,#207773,#207774,#207775,
#207776,#207777,#207778,#207779,#207780,#207781,#207782,#207783,#207784,
#207785,#207786,#207787,#207788,#207789,#207790,#207791,#207792,#207793,
#207794,#207795,#207796,#207797,#207798,#207799,#207800,#207801,#207802,
#207803,#207804,#207805,#207806,#207807,#207808,#207809,#207810,#207811,
#207812,#207813,#207814,#207815,#207816,#207817,#207818,#207819,#207820,
#207821,#207822,#207823,#207824,#207825,#207826,#207827,#207828,#207829,
#207830,#207831,#207832,#207833,#207834,#207835,#207836,#207837,#207838,
#207839,#207840,#207841,#207842,#207843,#207844,#207845,#207846,#207847,
#207848,#207849,#207850,#207851,#207852,#207853,#207854,#207855,#207856,
#207857,#207858,#207859,#207860,#207861,#207862,#207863,#207864,#207865,
#207866,#207867,#207868,#207869,#207870,#207871,#207872,#207873,#207874,
#207875,#207876,#207877,#207878,#207879,#207880,#207881,#207882,#207883),
 .UNSPECIFIED.,.F.,.F.)
B_SPLINE_CURVE_WITH_KNOTS((6,1,1,1,1,1,1,1,1,1,1,1,1,1,1,1,1,1,1,1,1,1,
1,1,1,1,1,1,1,1,1,1,1,1,1,1,1,1,1,1,1,1,1,1,1,1,1,1,1,1,1,1,1,1,1,1,1,1,
1,1,1,1,1,1,1,1,1,1,1,1,1,1,1,1,1,1,1,1,1,1,1,1,1,1,1,1,1,1,1,1,1,1,1,1,
1,1,1,1,1,1,1,1,1,1,1,1,1,1,1,1,1,1,1,1,1,1,1,1,1,1,1,1,1,1,1,1,1,1,1,1,
1,1,1,1,1,1,1,1,1,1,1,1,1,1,1,1,1,1,1,1,1,1,1,1,1,1,1,1,1,1,1,1,1,1,1,1,
1,1,1,1,1,1,1,1,1,1,1,1,1,1,1,1,1,1,1,1,1,1,1,1,1,1,1,1,1,1,1,1,1,1,6),
(0.,0.005,0.01,0.015,0.02,0.025,0.03,0.035,0.04,0.045,0.05,0.055,0.06,0.065,
0.07,0.075,0.08,0.085,0.09,0.095,0.1,0.105,0.11,0.115,0.12,0.125,0.13,0.135,
0.14,0.145,0.15,0.155,0.16,0.165,0.17,0.175,0.18,0.185,0.19,0.195,0.2,0.205,
0.21,0.215,0.22,0.225,0.23,0.235,0.24,0.245,0.25,0.255,0.26,0.265,0.27,
0.275,0.28,0.285,0.29,0.295,0.3,0.305,0.31,0.315,0.32,0.325,0.33,0.335,
0.34,0.345,0.35,0.355,0.36,0.365,0.37,0.375,0.38,0.385,0.39,0.395,0.4,0.405,
0.41,0.415,0.42,0.425,0.43,0.435,0.44,0.445,0.45,0.455,0.46,0.465,0.47,
0.475,0.48,0.485,0.49,0.495,0.5,0.505,0.51,0.515,0.52,0.525,0.53,0.535,
0.54,0.545,0.55,0.555,0.56,0.565,0.57,0.575,0.58,0.585,0.59,0.595,0.6,0.605,
0.61,0.615,0.62,0.625,0.63,0.635,0.64,0.645,0.65,0.655,0.66,0.665,0.67,
0.675,0.68,0.685,0.690000000000001,0.695000000000001,0.700000000000001,
0.705000000000001,0.710000000000001,0.715000000000001,0.720000000000001,
0.725000000000001,0.730000000000001,0.735000000000001,0.740000000000001,
0.745000000000001,0.750000000000001,0.755000000000001,0.760000000000001,
0.765000000000001,0.770000000000001,0.775000000000001,0.780000000000001,
0.785000000000001,0.790000000000001,0.795000000000001,0.800000000000001,
0.805000000000001,0.810000000000001,0.815000000000001,0.820000000000001,
0.825000000000001,0.830000000000001,0.835000000000001,0.840000000000001,
0.845000000000001,0.850000000000001,0.855000000000001,0.860000000000001,
0.865000000000001,0.870000000000001,0.875000000000001,0.880000000000001,
0.885000000000001,0.890000000000001,0.895000000000001,0.900000000000001,
0.905000000000001,0.910000000000001,0.915000000000001,0.920000000000001,
0.925000000000001,0.930000000000001,0.935000000000001,0.940000000000001,
0.945000000000001,0.950000000000001,0.955000000000001,0.960000000000001,
0.965000000000001,0.970000000000001,0.975000000000001,0.980000000000001,
0.985000000000001,0.990000000000001,0.995000000000001,1.),.UNSPECIFIED.)
CURVE()
GEOMETRIC_REPRESENTATION_ITEM()
RATIONAL_B_SPLINE_CURVE((1.,1.,1.,1.,1.,1.,1.,1.,1.,1.,1.,1.,1.,1.,1.,1.,
1.,1.,1.,1.,1.,1.,1.,1.,1.,1.,1.,1.,1.,1.,1.,1.,1.,1.,1.,1.,1.,1.,1.,1.,
1.,1.,1.,1.,1.,1.,1.,1.,1.,1.,1.,1.,1.,1.,1.,1.,1.,1.,1.,1.,1.,1.,1.,1.,
1.,1.,1.,1.,1.,1.,1.,1.,1.,1.,1.,1.,1.,1.,1.,1.,1.,1.,1.,1.,1.,1.,1.,1.,
1.,1.,1.,1.,1.,1.,1.,1.,1.,1.,1.,1.,1.,1.,1.,1.,1.,1.,1.,1.,1.,1.,1.,1.,
1.,1.,1.,1.,1.,1.,1.,1.,1.,1.,1.,1.,1.,1.,1.,1.,1.,1.,1.,1.,1.,1.,1.,1.,
1.,1.,1.,1.,1.,1.,1.,1.,1.,1.,1.,1.,1.,1.,1.,1.,1.,1.,1.,1.,1.,1.,1.,1.,
1.,1.,1.,1.,1.,1.,1.,1.,1.,1.,1.,1.,1.,1.,1.,1.,1.,1.,1.,1.,1.,1.,1.,1.,
1.,1.,1.,1.,1.,1.,1.,1.,1.,1.,1.,1.,1.,1.,1.,1.,1.,1.,1.,1.,1.))
REPRESENTATION_ITEM('')
);
#775=(
BOUNDED_CURVE()
B_SPLINE_CURVE(5,(#208300,#208301,#208302,#208303,#208304,#208305,#208306,
#208307,#208308,#208309,#208310,#208311,#208312,#208313,#208314,#208315,
#208316,#208317,#208318,#208319,#208320,#208321,#208322,#208323,#208324,
#208325,#208326,#208327,#208328,#208329,#208330,#208331,#208332,#208333,
#208334,#208335,#208336,#208337,#208338,#208339,#208340,#208341,#208342,
#208343,#208344,#208345,#208346,#208347,#208348,#208349,#208350,#208351,
#208352,#208353,#208354,#208355,#208356,#208357,#208358,#208359,#208360,
#208361,#208362,#208363,#208364,#208365,#208366,#208367,#208368,#208369,
#208370,#208371,#208372,#208373,#208374,#208375,#208376,#208377,#208378,
#208379,#208380,#208381,#208382,#208383,#208384,#208385,#208386,#208387,
#208388,#208389,#208390,#208391,#208392,#208393,#208394,#208395,#208396,
#208397,#208398,#208399,#208400,#208401,#208402,#208403,#208404,#208405,
#208406,#208407,#208408,#208409,#208410,#208411,#208412,#208413,#208414,
#208415,#208416,#208417,#208418,#208419,#208420,#208421,#208422,#208423,
#208424,#208425,#208426,#208427,#208428,#208429,#208430,#208431,#208432,
#208433,#208434,#208435,#208436,#208437,#208438,#208439,#208440,#208441,
#208442,#208443,#208444,#208445,#208446,#208447,#208448,#208449,#208450,
#208451,#208452,#208453,#208454,#208455,#208456,#208457,#208458,#208459,
#208460,#208461,#208462,#208463,#208464,#208465,#208466,#208467,#208468,
#208469,#208470,#208471,#208472,#208473,#208474,#208475,#208476,#208477,
#208478,#208479,#208480,#208481,#208482,#208483,#208484,#208485,#208486,
#208487,#208488,#208489,#208490,#208491,#208492,#208493,#208494,#208495,
#208496,#208497,#208498,#208499,#208500,#208501,#208502,#208503,#208504),
 .UNSPECIFIED.,.F.,.F.)
B_SPLINE_CURVE_WITH_KNOTS((6,1,1,1,1,1,1,1,1,1,1,1,1,1,1,1,1,1,1,1,1,1,
1,1,1,1,1,1,1,1,1,1,1,1,1,1,1,1,1,1,1,1,1,1,1,1,1,1,1,1,1,1,1,1,1,1,1,1,
1,1,1,1,1,1,1,1,1,1,1,1,1,1,1,1,1,1,1,1,1,1,1,1,1,1,1,1,1,1,1,1,1,1,1,1,
1,1,1,1,1,1,1,1,1,1,1,1,1,1,1,1,1,1,1,1,1,1,1,1,1,1,1,1,1,1,1,1,1,1,1,1,
1,1,1,1,1,1,1,1,1,1,1,1,1,1,1,1,1,1,1,1,1,1,1,1,1,1,1,1,1,1,1,1,1,1,1,1,
1,1,1,1,1,1,1,1,1,1,1,1,1,1,1,1,1,1,1,1,1,1,1,1,1,1,1,1,1,1,1,1,1,1,6),
(-1.,-0.995000000000001,-0.990000000000001,-0.985000000000001,-0.980000000000001,
-0.975000000000001,-0.970000000000001,-0.965000000000001,-0.960000000000001,
-0.955000000000001,-0.950000000000001,-0.945000000000001,-0.940000000000001,
-0.935000000000001,-0.930000000000001,-0.925000000000001,-0.920000000000001,
-0.915000000000001,-0.910000000000001,-0.905000000000001,-0.900000000000001,
-0.895000000000001,-0.890000000000001,-0.885000000000001,-0.880000000000001,
-0.875000000000001,-0.870000000000001,-0.865000000000001,-0.860000000000001,
-0.855000000000001,-0.850000000000001,-0.845000000000001,-0.840000000000001,
-0.835000000000001,-0.830000000000001,-0.825000000000001,-0.820000000000001,
-0.815000000000001,-0.810000000000001,-0.805000000000001,-0.800000000000001,
-0.795000000000001,-0.790000000000001,-0.785000000000001,-0.780000000000001,
-0.775000000000001,-0.770000000000001,-0.765000000000001,-0.760000000000001,
-0.755000000000001,-0.750000000000001,-0.745000000000001,-0.740000000000001,
-0.735000000000001,-0.730000000000001,-0.725000000000001,-0.720000000000001,
-0.715000000000001,-0.710000000000001,-0.705000000000001,-0.700000000000001,
-0.695000000000001,-0.690000000000001,-0.685,-0.68,-0.675,-0.67,-0.665,
-0.66,-0.655,-0.65,-0.645,-0.64,-0.635,-0.63,-0.625,-0.62,-0.615,-0.61,
-0.605,-0.6,-0.595,-0.59,-0.585,-0.58,-0.575,-0.57,-0.565,-0.56,-0.555,
-0.55,-0.545,-0.54,-0.535,-0.53,-0.525,-0.52,-0.515,-0.51,-0.505,-0.5,-0.495,
-0.49,-0.485,-0.48,-0.475,-0.47,-0.465,-0.46,-0.455,-0.45,-0.445,-0.44,
-0.435,-0.43,-0.425,-0.42,-0.415,-0.41,-0.405,-0.4,-0.395,-0.39,-0.385,
-0.38,-0.375,-0.37,-0.365,-0.36,-0.355,-0.35,-0.345,-0.34,-0.335,-0.33,
-0.325,-0.32,-0.315,-0.31,-0.305,-0.3,-0.295,-0.29,-0.285,-0.28,-0.275,
-0.27,-0.265,-0.26,-0.255,-0.25,-0.245,-0.24,-0.235,-0.23,-0.225,-0.22,
-0.215,-0.21,-0.205,-0.2,-0.195,-0.19,-0.185,-0.18,-0.175,-0.17,-0.165,
-0.16,-0.155,-0.15,-0.145,-0.14,-0.135,-0.13,-0.125,-0.12,-0.115,-0.11,
-0.105,-0.1,-0.095,-0.09,-0.085,-0.08,-0.075,-0.07,-0.065,-0.06,-0.055,
-0.05,-0.045,-0.04,-0.035,-0.03,-0.025,-0.02,-0.015,-0.01,-0.005,0.),
 .UNSPECIFIED.)
CURVE()
GEOMETRIC_REPRESENTATION_ITEM()
RATIONAL_B_SPLINE_CURVE((1.,1.,1.,1.,1.,1.,1.,1.,1.,1.,1.,1.,1.,1.,1.,1.,
1.,1.,1.,1.,1.,1.,1.,1.,1.,1.,1.,1.,1.,1.,1.,1.,1.,1.,1.,1.,1.,1.,1.,1.,
1.,1.,1.,1.,1.,1.,1.,1.,1.,1.,1.,1.,1.,1.,1.,1.,1.,1.,1.,1.,1.,1.,1.,1.,
1.,1.,1.,1.,1.,1.,1.,1.,1.,1.,1.,1.,1.,1.,1.,1.,1.,1.,1.,1.,1.,1.,1.,1.,
1.,1.,1.,1.,1.,1.,1.,1.,1.,1.,1.,1.,1.,1.,1.,1.,1.,1.,1.,1.,1.,1.,1.,1.,
1.,1.,1.,1.,1.,1.,1.,1.,1.,1.,1.,1.,1.,1.,1.,1.,1.,1.,1.,1.,1.,1.,1.,1.,
1.,1.,1.,1.,1.,1.,1.,1.,1.,1.,1.,1.,1.,1.,1.,1.,1.,1.,1.,1.,1.,1.,1.,1.,
1.,1.,1.,1.,1.,1.,1.,1.,1.,1.,1.,1.,1.,1.,1.,1.,1.,1.,1.,1.,1.,1.,1.,1.,
1.,1.,1.,1.,1.,1.,1.,1.,1.,1.,1.,1.,1.,1.,1.,1.,1.,1.,1.,1.,1.))
REPRESENTATION_ITEM('')
);
#776=(
BOUNDED_CURVE()
B_SPLINE_CURVE(5,(#208917,#208918,#208919,#208920,#208921,#208922,#208923,
#208924,#208925,#208926,#208927,#208928,#208929,#208930,#208931,#208932,
#208933,#208934,#208935,#208936,#208937,#208938,#208939,#208940,#208941,
#208942,#208943,#208944,#208945,#208946,#208947,#208948,#208949,#208950,
#208951,#208952,#208953,#208954,#208955,#208956,#208957,#208958,#208959,
#208960,#208961,#208962,#208963,#208964,#208965,#208966,#208967,#208968,
#208969,#208970,#208971,#208972,#208973,#208974,#208975,#208976,#208977,
#208978,#208979,#208980,#208981,#208982,#208983,#208984,#208985,#208986,
#208987,#208988,#208989,#208990,#208991,#208992,#208993,#208994,#208995,
#208996,#208997,#208998,#208999,#209000,#209001,#209002,#209003,#209004,
#209005,#209006,#209007,#209008,#209009,#209010,#209011,#209012,#209013,
#209014,#209015,#209016,#209017,#209018,#209019,#209020,#209021,#209022,
#209023,#209024,#209025,#209026,#209027,#209028,#209029,#209030,#209031,
#209032,#209033,#209034,#209035,#209036,#209037,#209038,#209039,#209040,
#209041,#209042,#209043,#209044,#209045,#209046,#209047,#209048,#209049,
#209050,#209051,#209052,#209053,#209054,#209055,#209056,#209057,#209058,
#209059,#209060,#209061,#209062,#209063,#209064,#209065,#209066,#209067,
#209068,#209069,#209070,#209071,#209072,#209073,#209074,#209075,#209076,
#209077,#209078,#209079,#209080,#209081,#209082,#209083,#209084,#209085,
#209086,#209087,#209088,#209089,#209090,#209091,#209092,#209093,#209094,
#209095,#209096,#209097,#209098,#209099,#209100,#209101,#209102,#209103,
#209104,#209105,#209106,#209107,#209108,#209109,#209110,#209111,#209112,
#209113,#209114,#209115,#209116,#209117,#209118,#209119,#209120,#209121),
 .UNSPECIFIED.,.F.,.F.)
B_SPLINE_CURVE_WITH_KNOTS((6,1,1,1,1,1,1,1,1,1,1,1,1,1,1,1,1,1,1,1,1,1,
1,1,1,1,1,1,1,1,1,1,1,1,1,1,1,1,1,1,1,1,1,1,1,1,1,1,1,1,1,1,1,1,1,1,1,1,
1,1,1,1,1,1,1,1,1,1,1,1,1,1,1,1,1,1,1,1,1,1,1,1,1,1,1,1,1,1,1,1,1,1,1,1,
1,1,1,1,1,1,1,1,1,1,1,1,1,1,1,1,1,1,1,1,1,1,1,1,1,1,1,1,1,1,1,1,1,1,1,1,
1,1,1,1,1,1,1,1,1,1,1,1,1,1,1,1,1,1,1,1,1,1,1,1,1,1,1,1,1,1,1,1,1,1,1,1,
1,1,1,1,1,1,1,1,1,1,1,1,1,1,1,1,1,1,1,1,1,1,1,1,1,1,1,1,1,1,1,1,1,1,6),
(0.,0.005,0.01,0.015,0.02,0.025,0.03,0.035,0.04,0.045,0.05,0.055,0.06,0.065,
0.07,0.075,0.08,0.085,0.09,0.095,0.1,0.105,0.11,0.115,0.12,0.125,0.13,0.135,
0.14,0.145,0.15,0.155,0.16,0.165,0.17,0.175,0.18,0.185,0.19,0.195,0.2,0.205,
0.21,0.215,0.22,0.225,0.23,0.235,0.24,0.245,0.25,0.255,0.26,0.265,0.27,
0.275,0.28,0.285,0.29,0.295,0.3,0.305,0.31,0.315,0.32,0.325,0.33,0.335,
0.34,0.345,0.35,0.355,0.36,0.365,0.37,0.375,0.38,0.385,0.39,0.395,0.4,0.405,
0.41,0.415,0.42,0.425,0.43,0.435,0.44,0.445,0.45,0.455,0.46,0.465,0.47,
0.475,0.48,0.485,0.49,0.495,0.5,0.505,0.51,0.515,0.52,0.525,0.53,0.535,
0.54,0.545,0.55,0.555,0.56,0.565,0.57,0.575,0.58,0.585,0.59,0.595,0.6,0.605,
0.61,0.615,0.62,0.625,0.63,0.635,0.64,0.645,0.65,0.655,0.66,0.665,0.67,
0.675,0.68,0.685,0.690000000000001,0.695000000000001,0.700000000000001,
0.705000000000001,0.710000000000001,0.715000000000001,0.720000000000001,
0.725000000000001,0.730000000000001,0.735000000000001,0.740000000000001,
0.745000000000001,0.750000000000001,0.755000000000001,0.760000000000001,
0.765000000000001,0.770000000000001,0.775000000000001,0.780000000000001,
0.785000000000001,0.790000000000001,0.795000000000001,0.800000000000001,
0.805000000000001,0.810000000000001,0.815000000000001,0.820000000000001,
0.825000000000001,0.830000000000001,0.835000000000001,0.840000000000001,
0.845000000000001,0.850000000000001,0.855000000000001,0.860000000000001,
0.865000000000001,0.870000000000001,0.875000000000001,0.880000000000001,
0.885000000000001,0.890000000000001,0.895000000000001,0.900000000000001,
0.905000000000001,0.910000000000001,0.915000000000001,0.920000000000001,
0.925000000000001,0.930000000000001,0.935000000000001,0.940000000000001,
0.945000000000001,0.950000000000001,0.955000000000001,0.960000000000001,
0.965000000000001,0.970000000000001,0.975000000000001,0.980000000000001,
0.985000000000001,0.990000000000001,0.995000000000001,1.),.UNSPECIFIED.)
CURVE()
GEOMETRIC_REPRESENTATION_ITEM()
RATIONAL_B_SPLINE_CURVE((1.,1.,1.,1.,1.,1.,1.,1.,1.,1.,1.,1.,1.,1.,1.,1.,
1.,1.,1.,1.,1.,1.,1.,1.,1.,1.,1.,1.,1.,1.,1.,1.,1.,1.,1.,1.,1.,1.,1.,1.,
1.,1.,1.,1.,1.,1.,1.,1.,1.,1.,1.,1.,1.,1.,1.,1.,1.,1.,1.,1.,1.,1.,1.,1.,
1.,1.,1.,1.,1.,1.,1.,1.,1.,1.,1.,1.,1.,1.,1.,1.,1.,1.,1.,1.,1.,1.,1.,1.,
1.,1.,1.,1.,1.,1.,1.,1.,1.,1.,1.,1.,1.,1.,1.,1.,1.,1.,1.,1.,1.,1.,1.,1.,
1.,1.,1.,1.,1.,1.,1.,1.,1.,1.,1.,1.,1.,1.,1.,1.,1.,1.,1.,1.,1.,1.,1.,1.,
1.,1.,1.,1.,1.,1.,1.,1.,1.,1.,1.,1.,1.,1.,1.,1.,1.,1.,1.,1.,1.,1.,1.,1.,
1.,1.,1.,1.,1.,1.,1.,1.,1.,1.,1.,1.,1.,1.,1.,1.,1.,1.,1.,1.,1.,1.,1.,1.,
1.,1.,1.,1.,1.,1.,1.,1.,1.,1.,1.,1.,1.,1.,1.,1.,1.,1.,1.,1.,1.))
REPRESENTATION_ITEM('')
);
#777=(
BOUNDED_CURVE()
B_SPLINE_CURVE(5,(#209538,#209539,#209540,#209541,#209542,#209543,#209544,
#209545,#209546,#209547,#209548,#209549,#209550,#209551,#209552,#209553,
#209554,#209555,#209556,#209557,#209558,#209559,#209560,#209561,#209562,
#209563,#209564,#209565,#209566,#209567,#209568,#209569,#209570,#209571,
#209572,#209573,#209574,#209575,#209576,#209577,#209578,#209579,#209580,
#209581,#209582,#209583,#209584,#209585,#209586,#209587,#209588,#209589,
#209590,#209591,#209592,#209593,#209594,#209595,#209596,#209597,#209598,
#209599,#209600,#209601,#209602,#209603,#209604,#209605,#209606,#209607,
#209608,#209609,#209610,#209611,#209612,#209613,#209614,#209615,#209616,
#209617,#209618,#209619,#209620,#209621,#209622,#209623,#209624,#209625,
#209626,#209627,#209628,#209629,#209630,#209631,#209632,#209633,#209634,
#209635,#209636,#209637,#209638,#209639,#209640,#209641,#209642,#209643,
#209644,#209645,#209646,#209647,#209648,#209649,#209650,#209651,#209652,
#209653,#209654,#209655,#209656,#209657,#209658,#209659,#209660,#209661,
#209662,#209663,#209664,#209665,#209666,#209667,#209668,#209669,#209670,
#209671,#209672,#209673,#209674,#209675,#209676,#209677,#209678,#209679,
#209680,#209681,#209682,#209683,#209684,#209685,#209686,#209687,#209688,
#209689,#209690,#209691,#209692,#209693,#209694,#209695,#209696,#209697,
#209698,#209699,#209700,#209701,#209702,#209703,#209704,#209705,#209706,
#209707,#209708,#209709,#209710,#209711,#209712,#209713,#209714,#209715,
#209716,#209717,#209718,#209719,#209720,#209721,#209722,#209723,#209724,
#209725,#209726,#209727,#209728,#209729,#209730,#209731,#209732,#209733,
#209734,#209735,#209736,#209737,#209738,#209739,#209740,#209741,#209742),
 .UNSPECIFIED.,.F.,.F.)
B_SPLINE_CURVE_WITH_KNOTS((6,1,1,1,1,1,1,1,1,1,1,1,1,1,1,1,1,1,1,1,1,1,
1,1,1,1,1,1,1,1,1,1,1,1,1,1,1,1,1,1,1,1,1,1,1,1,1,1,1,1,1,1,1,1,1,1,1,1,
1,1,1,1,1,1,1,1,1,1,1,1,1,1,1,1,1,1,1,1,1,1,1,1,1,1,1,1,1,1,1,1,1,1,1,1,
1,1,1,1,1,1,1,1,1,1,1,1,1,1,1,1,1,1,1,1,1,1,1,1,1,1,1,1,1,1,1,1,1,1,1,1,
1,1,1,1,1,1,1,1,1,1,1,1,1,1,1,1,1,1,1,1,1,1,1,1,1,1,1,1,1,1,1,1,1,1,1,1,
1,1,1,1,1,1,1,1,1,1,1,1,1,1,1,1,1,1,1,1,1,1,1,1,1,1,1,1,1,1,1,1,1,1,6),
(-1.,-0.995000000000001,-0.990000000000001,-0.985000000000001,-0.980000000000001,
-0.975000000000001,-0.970000000000001,-0.965000000000001,-0.960000000000001,
-0.955000000000001,-0.950000000000001,-0.945000000000001,-0.940000000000001,
-0.935000000000001,-0.930000000000001,-0.925000000000001,-0.920000000000001,
-0.915000000000001,-0.910000000000001,-0.905000000000001,-0.900000000000001,
-0.895000000000001,-0.890000000000001,-0.885000000000001,-0.880000000000001,
-0.875000000000001,-0.870000000000001,-0.865000000000001,-0.860000000000001,
-0.855000000000001,-0.850000000000001,-0.845000000000001,-0.840000000000001,
-0.835000000000001,-0.830000000000001,-0.825000000000001,-0.820000000000001,
-0.815000000000001,-0.810000000000001,-0.805000000000001,-0.800000000000001,
-0.795000000000001,-0.790000000000001,-0.785000000000001,-0.780000000000001,
-0.775000000000001,-0.770000000000001,-0.765000000000001,-0.760000000000001,
-0.755000000000001,-0.750000000000001,-0.745000000000001,-0.740000000000001,
-0.735000000000001,-0.730000000000001,-0.725000000000001,-0.720000000000001,
-0.715000000000001,-0.710000000000001,-0.705000000000001,-0.700000000000001,
-0.695000000000001,-0.690000000000001,-0.685,-0.68,-0.675,-0.67,-0.665,
-0.66,-0.655,-0.65,-0.645,-0.64,-0.635,-0.63,-0.625,-0.62,-0.615,-0.61,
-0.605,-0.6,-0.595,-0.59,-0.585,-0.58,-0.575,-0.57,-0.565,-0.56,-0.555,
-0.55,-0.545,-0.54,-0.535,-0.53,-0.525,-0.52,-0.515,-0.51,-0.505,-0.5,-0.495,
-0.49,-0.485,-0.48,-0.475,-0.47,-0.465,-0.46,-0.455,-0.45,-0.445,-0.44,
-0.435,-0.43,-0.425,-0.42,-0.415,-0.41,-0.405,-0.4,-0.395,-0.39,-0.385,
-0.38,-0.375,-0.37,-0.365,-0.36,-0.355,-0.35,-0.345,-0.34,-0.335,-0.33,
-0.325,-0.32,-0.315,-0.31,-0.305,-0.3,-0.295,-0.29,-0.285,-0.28,-0.275,
-0.27,-0.265,-0.26,-0.255,-0.25,-0.245,-0.24,-0.235,-0.23,-0.225,-0.22,
-0.215,-0.21,-0.205,-0.2,-0.195,-0.19,-0.185,-0.18,-0.175,-0.17,-0.165,
-0.16,-0.155,-0.15,-0.145,-0.14,-0.135,-0.13,-0.125,-0.12,-0.115,-0.11,
-0.105,-0.1,-0.095,-0.09,-0.085,-0.08,-0.075,-0.07,-0.065,-0.06,-0.055,
-0.05,-0.045,-0.04,-0.035,-0.03,-0.025,-0.02,-0.015,-0.01,-0.005,0.),
 .UNSPECIFIED.)
CURVE()
GEOMETRIC_REPRESENTATION_ITEM()
RATIONAL_B_SPLINE_CURVE((1.,1.,1.,1.,1.,1.,1.,1.,1.,1.,1.,1.,1.,1.,1.,1.,
1.,1.,1.,1.,1.,1.,1.,1.,1.,1.,1.,1.,1.,1.,1.,1.,1.,1.,1.,1.,1.,1.,1.,1.,
1.,1.,1.,1.,1.,1.,1.,1.,1.,1.,1.,1.,1.,1.,1.,1.,1.,1.,1.,1.,1.,1.,1.,1.,
1.,1.,1.,1.,1.,1.,1.,1.,1.,1.,1.,1.,1.,1.,1.,1.,1.,1.,1.,1.,1.,1.,1.,1.,
1.,1.,1.,1.,1.,1.,1.,1.,1.,1.,1.,1.,1.,1.,1.,1.,1.,1.,1.,1.,1.,1.,1.,1.,
1.,1.,1.,1.,1.,1.,1.,1.,1.,1.,1.,1.,1.,1.,1.,1.,1.,1.,1.,1.,1.,1.,1.,1.,
1.,1.,1.,1.,1.,1.,1.,1.,1.,1.,1.,1.,1.,1.,1.,1.,1.,1.,1.,1.,1.,1.,1.,1.,
1.,1.,1.,1.,1.,1.,1.,1.,1.,1.,1.,1.,1.,1.,1.,1.,1.,1.,1.,1.,1.,1.,1.,1.,
1.,1.,1.,1.,1.,1.,1.,1.,1.,1.,1.,1.,1.,1.,1.,1.,1.,1.,1.,1.,1.))
REPRESENTATION_ITEM('')
);
#778=(
BOUNDED_CURVE()
B_SPLINE_CURVE(5,(#210155,#210156,#210157,#210158,#210159,#210160,#210161,
#210162,#210163,#210164,#210165,#210166,#210167,#210168,#210169,#210170,
#210171,#210172,#210173,#210174,#210175,#210176,#210177,#210178,#210179,
#210180,#210181,#210182,#210183,#210184,#210185,#210186,#210187,#210188,
#210189,#210190,#210191,#210192,#210193,#210194,#210195,#210196,#210197,
#210198,#210199,#210200,#210201,#210202,#210203,#210204,#210205,#210206,
#210207,#210208,#210209,#210210,#210211,#210212,#210213,#210214,#210215,
#210216,#210217,#210218,#210219,#210220,#210221,#210222,#210223,#210224,
#210225,#210226,#210227,#210228,#210229,#210230,#210231,#210232,#210233,
#210234,#210235,#210236,#210237,#210238,#210239,#210240,#210241,#210242,
#210243,#210244,#210245,#210246,#210247,#210248,#210249,#210250,#210251,
#210252,#210253,#210254,#210255,#210256,#210257,#210258,#210259,#210260,
#210261,#210262,#210263,#210264,#210265,#210266,#210267,#210268,#210269,
#210270,#210271,#210272,#210273,#210274,#210275,#210276,#210277,#210278,
#210279,#210280,#210281,#210282,#210283,#210284,#210285,#210286,#210287,
#210288,#210289,#210290,#210291,#210292,#210293,#210294,#210295,#210296,
#210297,#210298,#210299,#210300,#210301,#210302,#210303,#210304,#210305,
#210306,#210307,#210308,#210309,#210310,#210311,#210312,#210313,#210314,
#210315,#210316,#210317,#210318,#210319,#210320,#210321,#210322,#210323,
#210324,#210325,#210326,#210327,#210328,#210329,#210330,#210331,#210332,
#210333,#210334,#210335,#210336,#210337,#210338,#210339,#210340,#210341,
#210342,#210343,#210344,#210345,#210346,#210347,#210348,#210349,#210350,
#210351,#210352,#210353,#210354,#210355,#210356,#210357,#210358,#210359),
 .UNSPECIFIED.,.F.,.F.)
B_SPLINE_CURVE_WITH_KNOTS((6,1,1,1,1,1,1,1,1,1,1,1,1,1,1,1,1,1,1,1,1,1,
1,1,1,1,1,1,1,1,1,1,1,1,1,1,1,1,1,1,1,1,1,1,1,1,1,1,1,1,1,1,1,1,1,1,1,1,
1,1,1,1,1,1,1,1,1,1,1,1,1,1,1,1,1,1,1,1,1,1,1,1,1,1,1,1,1,1,1,1,1,1,1,1,
1,1,1,1,1,1,1,1,1,1,1,1,1,1,1,1,1,1,1,1,1,1,1,1,1,1,1,1,1,1,1,1,1,1,1,1,
1,1,1,1,1,1,1,1,1,1,1,1,1,1,1,1,1,1,1,1,1,1,1,1,1,1,1,1,1,1,1,1,1,1,1,1,
1,1,1,1,1,1,1,1,1,1,1,1,1,1,1,1,1,1,1,1,1,1,1,1,1,1,1,1,1,1,1,1,1,1,6),
(0.,0.005,0.01,0.015,0.02,0.025,0.03,0.035,0.04,0.045,0.05,0.055,0.06,0.065,
0.07,0.075,0.08,0.085,0.09,0.095,0.1,0.105,0.11,0.115,0.12,0.125,0.13,0.135,
0.14,0.145,0.15,0.155,0.16,0.165,0.17,0.175,0.18,0.185,0.19,0.195,0.2,0.205,
0.21,0.215,0.22,0.225,0.23,0.235,0.24,0.245,0.25,0.255,0.26,0.265,0.27,
0.275,0.28,0.285,0.29,0.295,0.3,0.305,0.31,0.315,0.32,0.325,0.33,0.335,
0.34,0.345,0.35,0.355,0.36,0.365,0.37,0.375,0.38,0.385,0.39,0.395,0.4,0.405,
0.41,0.415,0.42,0.425,0.43,0.435,0.44,0.445,0.45,0.455,0.46,0.465,0.47,
0.475,0.48,0.485,0.49,0.495,0.5,0.505,0.51,0.515,0.52,0.525,0.53,0.535,
0.54,0.545,0.55,0.555,0.56,0.565,0.57,0.575,0.58,0.585,0.59,0.595,0.6,0.605,
0.61,0.615,0.62,0.625,0.63,0.635,0.64,0.645,0.65,0.655,0.66,0.665,0.67,
0.675,0.68,0.685,0.690000000000001,0.695000000000001,0.700000000000001,
0.705000000000001,0.710000000000001,0.715000000000001,0.720000000000001,
0.725000000000001,0.730000000000001,0.735000000000001,0.740000000000001,
0.745000000000001,0.750000000000001,0.755000000000001,0.760000000000001,
0.765000000000001,0.770000000000001,0.775000000000001,0.780000000000001,
0.785000000000001,0.790000000000001,0.795000000000001,0.800000000000001,
0.805000000000001,0.810000000000001,0.815000000000001,0.820000000000001,
0.825000000000001,0.830000000000001,0.835000000000001,0.840000000000001,
0.845000000000001,0.850000000000001,0.855000000000001,0.860000000000001,
0.865000000000001,0.870000000000001,0.875000000000001,0.880000000000001,
0.885000000000001,0.890000000000001,0.895000000000001,0.900000000000001,
0.905000000000001,0.910000000000001,0.915000000000001,0.920000000000001,
0.925000000000001,0.930000000000001,0.935000000000001,0.940000000000001,
0.945000000000001,0.950000000000001,0.955000000000001,0.960000000000001,
0.965000000000001,0.970000000000001,0.975000000000001,0.980000000000001,
0.985000000000001,0.990000000000001,0.995000000000001,1.),.UNSPECIFIED.)
CURVE()
GEOMETRIC_REPRESENTATION_ITEM()
RATIONAL_B_SPLINE_CURVE((1.,1.,1.,1.,1.,1.,1.,1.,1.,1.,1.,1.,1.,1.,1.,1.,
1.,1.,1.,1.,1.,1.,1.,1.,1.,1.,1.,1.,1.,1.,1.,1.,1.,1.,1.,1.,1.,1.,1.,1.,
1.,1.,1.,1.,1.,1.,1.,1.,1.,1.,1.,1.,1.,1.,1.,1.,1.,1.,1.,1.,1.,1.,1.,1.,
1.,1.,1.,1.,1.,1.,1.,1.,1.,1.,1.,1.,1.,1.,1.,1.,1.,1.,1.,1.,1.,1.,1.,1.,
1.,1.,1.,1.,1.,1.,1.,1.,1.,1.,1.,1.,1.,1.,1.,1.,1.,1.,1.,1.,1.,1.,1.,1.,
1.,1.,1.,1.,1.,1.,1.,1.,1.,1.,1.,1.,1.,1.,1.,1.,1.,1.,1.,1.,1.,1.,1.,1.,
1.,1.,1.,1.,1.,1.,1.,1.,1.,1.,1.,1.,1.,1.,1.,1.,1.,1.,1.,1.,1.,1.,1.,1.,
1.,1.,1.,1.,1.,1.,1.,1.,1.,1.,1.,1.,1.,1.,1.,1.,1.,1.,1.,1.,1.,1.,1.,1.,
1.,1.,1.,1.,1.,1.,1.,1.,1.,1.,1.,1.,1.,1.,1.,1.,1.,1.,1.,1.,1.))
REPRESENTATION_ITEM('')
);
#779=(
BOUNDED_CURVE()
B_SPLINE_CURVE(5,(#210776,#210777,#210778,#210779,#210780,#210781,#210782,
#210783,#210784,#210785,#210786,#210787,#210788,#210789,#210790,#210791,
#210792,#210793,#210794,#210795,#210796,#210797,#210798,#210799,#210800,
#210801,#210802,#210803,#210804,#210805,#210806,#210807,#210808,#210809,
#210810,#210811,#210812,#210813,#210814,#210815,#210816,#210817,#210818,
#210819,#210820,#210821,#210822,#210823,#210824,#210825,#210826,#210827,
#210828,#210829,#210830,#210831,#210832,#210833,#210834,#210835,#210836,
#210837,#210838,#210839,#210840,#210841,#210842,#210843,#210844,#210845,
#210846,#210847,#210848,#210849,#210850,#210851,#210852,#210853,#210854,
#210855,#210856,#210857,#210858,#210859,#210860,#210861,#210862,#210863,
#210864,#210865,#210866,#210867,#210868,#210869,#210870,#210871,#210872,
#210873,#210874,#210875,#210876,#210877,#210878,#210879,#210880,#210881,
#210882,#210883,#210884,#210885,#210886,#210887,#210888,#210889,#210890,
#210891,#210892,#210893,#210894,#210895,#210896,#210897,#210898,#210899,
#210900,#210901,#210902,#210903,#210904,#210905,#210906,#210907,#210908,
#210909,#210910,#210911,#210912,#210913,#210914,#210915,#210916,#210917,
#210918,#210919,#210920,#210921,#210922,#210923,#210924,#210925,#210926,
#210927,#210928,#210929,#210930,#210931,#210932,#210933,#210934,#210935,
#210936,#210937,#210938,#210939,#210940,#210941,#210942,#210943,#210944,
#210945,#210946,#210947,#210948,#210949,#210950,#210951,#210952,#210953,
#210954,#210955,#210956,#210957,#210958,#210959,#210960,#210961,#210962,
#210963,#210964,#210965,#210966,#210967,#210968,#210969,#210970,#210971,
#210972,#210973,#210974,#210975,#210976,#210977,#210978,#210979,#210980),
 .UNSPECIFIED.,.F.,.F.)
B_SPLINE_CURVE_WITH_KNOTS((6,1,1,1,1,1,1,1,1,1,1,1,1,1,1,1,1,1,1,1,1,1,
1,1,1,1,1,1,1,1,1,1,1,1,1,1,1,1,1,1,1,1,1,1,1,1,1,1,1,1,1,1,1,1,1,1,1,1,
1,1,1,1,1,1,1,1,1,1,1,1,1,1,1,1,1,1,1,1,1,1,1,1,1,1,1,1,1,1,1,1,1,1,1,1,
1,1,1,1,1,1,1,1,1,1,1,1,1,1,1,1,1,1,1,1,1,1,1,1,1,1,1,1,1,1,1,1,1,1,1,1,
1,1,1,1,1,1,1,1,1,1,1,1,1,1,1,1,1,1,1,1,1,1,1,1,1,1,1,1,1,1,1,1,1,1,1,1,
1,1,1,1,1,1,1,1,1,1,1,1,1,1,1,1,1,1,1,1,1,1,1,1,1,1,1,1,1,1,1,1,1,1,6),
(-1.,-0.995000000000001,-0.990000000000001,-0.985000000000001,-0.980000000000001,
-0.975000000000001,-0.970000000000001,-0.965000000000001,-0.960000000000001,
-0.955000000000001,-0.950000000000001,-0.945000000000001,-0.940000000000001,
-0.935000000000001,-0.930000000000001,-0.925000000000001,-0.920000000000001,
-0.915000000000001,-0.910000000000001,-0.905000000000001,-0.900000000000001,
-0.895000000000001,-0.890000000000001,-0.885000000000001,-0.880000000000001,
-0.875000000000001,-0.870000000000001,-0.865000000000001,-0.860000000000001,
-0.855000000000001,-0.850000000000001,-0.845000000000001,-0.840000000000001,
-0.835000000000001,-0.830000000000001,-0.825000000000001,-0.820000000000001,
-0.815000000000001,-0.810000000000001,-0.805000000000001,-0.800000000000001,
-0.795000000000001,-0.790000000000001,-0.785000000000001,-0.780000000000001,
-0.775000000000001,-0.770000000000001,-0.765000000000001,-0.760000000000001,
-0.755000000000001,-0.750000000000001,-0.745000000000001,-0.740000000000001,
-0.735000000000001,-0.730000000000001,-0.725000000000001,-0.720000000000001,
-0.715000000000001,-0.710000000000001,-0.705000000000001,-0.700000000000001,
-0.695000000000001,-0.690000000000001,-0.685,-0.68,-0.675,-0.67,-0.665,
-0.66,-0.655,-0.65,-0.645,-0.64,-0.635,-0.63,-0.625,-0.62,-0.615,-0.61,
-0.605,-0.6,-0.595,-0.59,-0.585,-0.58,-0.575,-0.57,-0.565,-0.56,-0.555,
-0.55,-0.545,-0.54,-0.535,-0.53,-0.525,-0.52,-0.515,-0.51,-0.505,-0.5,-0.495,
-0.49,-0.485,-0.48,-0.475,-0.47,-0.465,-0.46,-0.455,-0.45,-0.445,-0.44,
-0.435,-0.43,-0.425,-0.42,-0.415,-0.41,-0.405,-0.4,-0.395,-0.39,-0.385,
-0.38,-0.375,-0.37,-0.365,-0.36,-0.355,-0.35,-0.345,-0.34,-0.335,-0.33,
-0.325,-0.32,-0.315,-0.31,-0.305,-0.3,-0.295,-0.29,-0.285,-0.28,-0.275,
-0.27,-0.265,-0.26,-0.255,-0.25,-0.245,-0.24,-0.235,-0.23,-0.225,-0.22,
-0.215,-0.21,-0.205,-0.2,-0.195,-0.19,-0.185,-0.18,-0.175,-0.17,-0.165,
-0.16,-0.155,-0.15,-0.145,-0.14,-0.135,-0.13,-0.125,-0.12,-0.115,-0.11,
-0.105,-0.1,-0.095,-0.09,-0.085,-0.08,-0.075,-0.07,-0.065,-0.06,-0.055,
-0.05,-0.045,-0.04,-0.035,-0.03,-0.025,-0.02,-0.015,-0.01,-0.005,0.),
 .UNSPECIFIED.)
CURVE()
GEOMETRIC_REPRESENTATION_ITEM()
RATIONAL_B_SPLINE_CURVE((1.,1.,1.,1.,1.,1.,1.,1.,1.,1.,1.,1.,1.,1.,1.,1.,
1.,1.,1.,1.,1.,1.,1.,1.,1.,1.,1.,1.,1.,1.,1.,1.,1.,1.,1.,1.,1.,1.,1.,1.,
1.,1.,1.,1.,1.,1.,1.,1.,1.,1.,1.,1.,1.,1.,1.,1.,1.,1.,1.,1.,1.,1.,1.,1.,
1.,1.,1.,1.,1.,1.,1.,1.,1.,1.,1.,1.,1.,1.,1.,1.,1.,1.,1.,1.,1.,1.,1.,1.,
1.,1.,1.,1.,1.,1.,1.,1.,1.,1.,1.,1.,1.,1.,1.,1.,1.,1.,1.,1.,1.,1.,1.,1.,
1.,1.,1.,1.,1.,1.,1.,1.,1.,1.,1.,1.,1.,1.,1.,1.,1.,1.,1.,1.,1.,1.,1.,1.,
1.,1.,1.,1.,1.,1.,1.,1.,1.,1.,1.,1.,1.,1.,1.,1.,1.,1.,1.,1.,1.,1.,1.,1.,
1.,1.,1.,1.,1.,1.,1.,1.,1.,1.,1.,1.,1.,1.,1.,1.,1.,1.,1.,1.,1.,1.,1.,1.,
1.,1.,1.,1.,1.,1.,1.,1.,1.,1.,1.,1.,1.,1.,1.,1.,1.,1.,1.,1.,1.))
REPRESENTATION_ITEM('')
);
#780=(
BOUNDED_CURVE()
B_SPLINE_CURVE(5,(#211393,#211394,#211395,#211396,#211397,#211398,#211399,
#211400,#211401,#211402,#211403,#211404,#211405,#211406,#211407,#211408,
#211409,#211410,#211411,#211412,#211413,#211414,#211415,#211416,#211417,
#211418,#211419,#211420,#211421,#211422,#211423,#211424,#211425,#211426,
#211427,#211428,#211429,#211430,#211431,#211432,#211433,#211434,#211435,
#211436,#211437,#211438,#211439,#211440,#211441,#211442,#211443,#211444,
#211445,#211446,#211447,#211448,#211449,#211450,#211451,#211452,#211453,
#211454,#211455,#211456,#211457,#211458,#211459,#211460,#211461,#211462,
#211463,#211464,#211465,#211466,#211467,#211468,#211469,#211470,#211471,
#211472,#211473,#211474,#211475,#211476,#211477,#211478,#211479,#211480,
#211481,#211482,#211483,#211484,#211485,#211486,#211487,#211488,#211489,
#211490,#211491,#211492,#211493,#211494,#211495,#211496,#211497,#211498,
#211499,#211500,#211501,#211502,#211503,#211504,#211505,#211506,#211507,
#211508,#211509,#211510,#211511,#211512,#211513,#211514,#211515,#211516,
#211517,#211518,#211519,#211520,#211521,#211522,#211523,#211524,#211525,
#211526,#211527,#211528,#211529,#211530,#211531,#211532,#211533,#211534,
#211535,#211536,#211537,#211538,#211539,#211540,#211541,#211542,#211543,
#211544,#211545,#211546,#211547,#211548,#211549,#211550,#211551,#211552,
#211553,#211554,#211555,#211556,#211557,#211558,#211559,#211560,#211561,
#211562,#211563,#211564,#211565,#211566,#211567,#211568,#211569,#211570,
#211571,#211572,#211573,#211574,#211575,#211576,#211577,#211578,#211579,
#211580,#211581,#211582,#211583,#211584,#211585,#211586,#211587,#211588,
#211589,#211590,#211591,#211592,#211593,#211594,#211595,#211596,#211597),
 .UNSPECIFIED.,.F.,.F.)
B_SPLINE_CURVE_WITH_KNOTS((6,1,1,1,1,1,1,1,1,1,1,1,1,1,1,1,1,1,1,1,1,1,
1,1,1,1,1,1,1,1,1,1,1,1,1,1,1,1,1,1,1,1,1,1,1,1,1,1,1,1,1,1,1,1,1,1,1,1,
1,1,1,1,1,1,1,1,1,1,1,1,1,1,1,1,1,1,1,1,1,1,1,1,1,1,1,1,1,1,1,1,1,1,1,1,
1,1,1,1,1,1,1,1,1,1,1,1,1,1,1,1,1,1,1,1,1,1,1,1,1,1,1,1,1,1,1,1,1,1,1,1,
1,1,1,1,1,1,1,1,1,1,1,1,1,1,1,1,1,1,1,1,1,1,1,1,1,1,1,1,1,1,1,1,1,1,1,1,
1,1,1,1,1,1,1,1,1,1,1,1,1,1,1,1,1,1,1,1,1,1,1,1,1,1,1,1,1,1,1,1,1,1,6),
(0.,0.005,0.01,0.015,0.02,0.025,0.03,0.035,0.04,0.045,0.05,0.055,0.06,0.065,
0.07,0.075,0.08,0.085,0.09,0.095,0.1,0.105,0.11,0.115,0.12,0.125,0.13,0.135,
0.14,0.145,0.15,0.155,0.16,0.165,0.17,0.175,0.18,0.185,0.19,0.195,0.2,0.205,
0.21,0.215,0.22,0.225,0.23,0.235,0.24,0.245,0.25,0.255,0.26,0.265,0.27,
0.275,0.28,0.285,0.29,0.295,0.3,0.305,0.31,0.315,0.32,0.325,0.33,0.335,
0.34,0.345,0.35,0.355,0.36,0.365,0.37,0.375,0.38,0.385,0.39,0.395,0.4,0.405,
0.41,0.415,0.42,0.425,0.43,0.435,0.44,0.445,0.45,0.455,0.46,0.465,0.47,
0.475,0.48,0.485,0.49,0.495,0.5,0.505,0.51,0.515,0.52,0.525,0.53,0.535,
0.54,0.545,0.55,0.555,0.56,0.565,0.57,0.575,0.58,0.585,0.59,0.595,0.6,0.605,
0.61,0.615,0.62,0.625,0.63,0.635,0.64,0.645,0.65,0.655,0.66,0.665,0.67,
0.675,0.68,0.685,0.690000000000001,0.695000000000001,0.700000000000001,
0.705000000000001,0.710000000000001,0.715000000000001,0.720000000000001,
0.725000000000001,0.730000000000001,0.735000000000001,0.740000000000001,
0.745000000000001,0.750000000000001,0.755000000000001,0.760000000000001,
0.765000000000001,0.770000000000001,0.775000000000001,0.780000000000001,
0.785000000000001,0.790000000000001,0.795000000000001,0.800000000000001,
0.805000000000001,0.810000000000001,0.815000000000001,0.820000000000001,
0.825000000000001,0.830000000000001,0.835000000000001,0.840000000000001,
0.845000000000001,0.850000000000001,0.855000000000001,0.860000000000001,
0.865000000000001,0.870000000000001,0.875000000000001,0.880000000000001,
0.885000000000001,0.890000000000001,0.895000000000001,0.900000000000001,
0.905000000000001,0.910000000000001,0.915000000000001,0.920000000000001,
0.925000000000001,0.930000000000001,0.935000000000001,0.940000000000001,
0.945000000000001,0.950000000000001,0.955000000000001,0.960000000000001,
0.965000000000001,0.970000000000001,0.975000000000001,0.980000000000001,
0.985000000000001,0.990000000000001,0.995000000000001,1.),.UNSPECIFIED.)
CURVE()
GEOMETRIC_REPRESENTATION_ITEM()
RATIONAL_B_SPLINE_CURVE((1.,1.,1.,1.,1.,1.,1.,1.,1.,1.,1.,1.,1.,1.,1.,1.,
1.,1.,1.,1.,1.,1.,1.,1.,1.,1.,1.,1.,1.,1.,1.,1.,1.,1.,1.,1.,1.,1.,1.,1.,
1.,1.,1.,1.,1.,1.,1.,1.,1.,1.,1.,1.,1.,1.,1.,1.,1.,1.,1.,1.,1.,1.,1.,1.,
1.,1.,1.,1.,1.,1.,1.,1.,1.,1.,1.,1.,1.,1.,1.,1.,1.,1.,1.,1.,1.,1.,1.,1.,
1.,1.,1.,1.,1.,1.,1.,1.,1.,1.,1.,1.,1.,1.,1.,1.,1.,1.,1.,1.,1.,1.,1.,1.,
1.,1.,1.,1.,1.,1.,1.,1.,1.,1.,1.,1.,1.,1.,1.,1.,1.,1.,1.,1.,1.,1.,1.,1.,
1.,1.,1.,1.,1.,1.,1.,1.,1.,1.,1.,1.,1.,1.,1.,1.,1.,1.,1.,1.,1.,1.,1.,1.,
1.,1.,1.,1.,1.,1.,1.,1.,1.,1.,1.,1.,1.,1.,1.,1.,1.,1.,1.,1.,1.,1.,1.,1.,
1.,1.,1.,1.,1.,1.,1.,1.,1.,1.,1.,1.,1.,1.,1.,1.,1.,1.,1.,1.,1.))
REPRESENTATION_ITEM('')
);
#781=(
BOUNDED_CURVE()
B_SPLINE_CURVE(5,(#212014,#212015,#212016,#212017,#212018,#212019,#212020,
#212021,#212022,#212023,#212024,#212025,#212026,#212027,#212028,#212029,
#212030,#212031,#212032,#212033,#212034,#212035,#212036,#212037,#212038,
#212039,#212040,#212041,#212042,#212043,#212044,#212045,#212046,#212047,
#212048,#212049,#212050,#212051,#212052,#212053,#212054,#212055,#212056,
#212057,#212058,#212059,#212060,#212061,#212062,#212063,#212064,#212065,
#212066,#212067,#212068,#212069,#212070,#212071,#212072,#212073,#212074,
#212075,#212076,#212077,#212078,#212079,#212080,#212081,#212082,#212083,
#212084,#212085,#212086,#212087,#212088,#212089,#212090,#212091,#212092,
#212093,#212094,#212095,#212096,#212097,#212098,#212099,#212100,#212101,
#212102,#212103,#212104,#212105,#212106,#212107,#212108,#212109,#212110,
#212111,#212112,#212113,#212114,#212115,#212116,#212117,#212118,#212119,
#212120,#212121,#212122,#212123,#212124,#212125,#212126,#212127,#212128,
#212129,#212130,#212131,#212132,#212133,#212134,#212135,#212136,#212137,
#212138,#212139,#212140,#212141,#212142,#212143,#212144,#212145,#212146,
#212147,#212148,#212149,#212150,#212151,#212152,#212153,#212154,#212155,
#212156,#212157,#212158,#212159,#212160,#212161,#212162,#212163,#212164,
#212165,#212166,#212167,#212168,#212169,#212170,#212171,#212172,#212173,
#212174,#212175,#212176,#212177,#212178,#212179,#212180,#212181,#212182,
#212183,#212184,#212185,#212186,#212187,#212188,#212189,#212190,#212191,
#212192,#212193,#212194,#212195,#212196,#212197,#212198,#212199,#212200,
#212201,#212202,#212203,#212204,#212205,#212206,#212207,#212208,#212209,
#212210,#212211,#212212,#212213,#212214,#212215,#212216,#212217,#212218),
 .UNSPECIFIED.,.F.,.F.)
B_SPLINE_CURVE_WITH_KNOTS((6,1,1,1,1,1,1,1,1,1,1,1,1,1,1,1,1,1,1,1,1,1,
1,1,1,1,1,1,1,1,1,1,1,1,1,1,1,1,1,1,1,1,1,1,1,1,1,1,1,1,1,1,1,1,1,1,1,1,
1,1,1,1,1,1,1,1,1,1,1,1,1,1,1,1,1,1,1,1,1,1,1,1,1,1,1,1,1,1,1,1,1,1,1,1,
1,1,1,1,1,1,1,1,1,1,1,1,1,1,1,1,1,1,1,1,1,1,1,1,1,1,1,1,1,1,1,1,1,1,1,1,
1,1,1,1,1,1,1,1,1,1,1,1,1,1,1,1,1,1,1,1,1,1,1,1,1,1,1,1,1,1,1,1,1,1,1,1,
1,1,1,1,1,1,1,1,1,1,1,1,1,1,1,1,1,1,1,1,1,1,1,1,1,1,1,1,1,1,1,1,1,1,6),
(-1.,-0.995000000000001,-0.990000000000001,-0.985000000000001,-0.980000000000001,
-0.975000000000001,-0.970000000000001,-0.965000000000001,-0.960000000000001,
-0.955000000000001,-0.950000000000001,-0.945000000000001,-0.940000000000001,
-0.935000000000001,-0.930000000000001,-0.925000000000001,-0.920000000000001,
-0.915000000000001,-0.910000000000001,-0.905000000000001,-0.900000000000001,
-0.895000000000001,-0.890000000000001,-0.885000000000001,-0.880000000000001,
-0.875000000000001,-0.870000000000001,-0.865000000000001,-0.860000000000001,
-0.855000000000001,-0.850000000000001,-0.845000000000001,-0.840000000000001,
-0.835000000000001,-0.830000000000001,-0.825000000000001,-0.820000000000001,
-0.815000000000001,-0.810000000000001,-0.805000000000001,-0.800000000000001,
-0.795000000000001,-0.790000000000001,-0.785000000000001,-0.780000000000001,
-0.775000000000001,-0.770000000000001,-0.765000000000001,-0.760000000000001,
-0.755000000000001,-0.750000000000001,-0.745000000000001,-0.740000000000001,
-0.735000000000001,-0.730000000000001,-0.725000000000001,-0.720000000000001,
-0.715000000000001,-0.710000000000001,-0.705000000000001,-0.700000000000001,
-0.695000000000001,-0.690000000000001,-0.685,-0.68,-0.675,-0.67,-0.665,
-0.66,-0.655,-0.65,-0.645,-0.64,-0.635,-0.63,-0.625,-0.62,-0.615,-0.61,
-0.605,-0.6,-0.595,-0.59,-0.585,-0.58,-0.575,-0.57,-0.565,-0.56,-0.555,
-0.55,-0.545,-0.54,-0.535,-0.53,-0.525,-0.52,-0.515,-0.51,-0.505,-0.5,-0.495,
-0.49,-0.485,-0.48,-0.475,-0.47,-0.465,-0.46,-0.455,-0.45,-0.445,-0.44,
-0.435,-0.43,-0.425,-0.42,-0.415,-0.41,-0.405,-0.4,-0.395,-0.39,-0.385,
-0.38,-0.375,-0.37,-0.365,-0.36,-0.355,-0.35,-0.345,-0.34,-0.335,-0.33,
-0.325,-0.32,-0.315,-0.31,-0.305,-0.3,-0.295,-0.29,-0.285,-0.28,-0.275,
-0.27,-0.265,-0.26,-0.255,-0.25,-0.245,-0.24,-0.235,-0.23,-0.225,-0.22,
-0.215,-0.21,-0.205,-0.2,-0.195,-0.19,-0.185,-0.18,-0.175,-0.17,-0.165,
-0.16,-0.155,-0.15,-0.145,-0.14,-0.135,-0.13,-0.125,-0.12,-0.115,-0.11,
-0.105,-0.1,-0.095,-0.09,-0.085,-0.08,-0.075,-0.07,-0.065,-0.06,-0.055,
-0.05,-0.045,-0.04,-0.035,-0.03,-0.025,-0.02,-0.015,-0.01,-0.005,0.),
 .UNSPECIFIED.)
CURVE()
GEOMETRIC_REPRESENTATION_ITEM()
RATIONAL_B_SPLINE_CURVE((1.,1.,1.,1.,1.,1.,1.,1.,1.,1.,1.,1.,1.,1.,1.,1.,
1.,1.,1.,1.,1.,1.,1.,1.,1.,1.,1.,1.,1.,1.,1.,1.,1.,1.,1.,1.,1.,1.,1.,1.,
1.,1.,1.,1.,1.,1.,1.,1.,1.,1.,1.,1.,1.,1.,1.,1.,1.,1.,1.,1.,1.,1.,1.,1.,
1.,1.,1.,1.,1.,1.,1.,1.,1.,1.,1.,1.,1.,1.,1.,1.,1.,1.,1.,1.,1.,1.,1.,1.,
1.,1.,1.,1.,1.,1.,1.,1.,1.,1.,1.,1.,1.,1.,1.,1.,1.,1.,1.,1.,1.,1.,1.,1.,
1.,1.,1.,1.,1.,1.,1.,1.,1.,1.,1.,1.,1.,1.,1.,1.,1.,1.,1.,1.,1.,1.,1.,1.,
1.,1.,1.,1.,1.,1.,1.,1.,1.,1.,1.,1.,1.,1.,1.,1.,1.,1.,1.,1.,1.,1.,1.,1.,
1.,1.,1.,1.,1.,1.,1.,1.,1.,1.,1.,1.,1.,1.,1.,1.,1.,1.,1.,1.,1.,1.,1.,1.,
1.,1.,1.,1.,1.,1.,1.,1.,1.,1.,1.,1.,1.,1.,1.,1.,1.,1.,1.,1.,1.))
REPRESENTATION_ITEM('')
);
#782=(
BOUNDED_CURVE()
B_SPLINE_CURVE(5,(#212631,#212632,#212633,#212634,#212635,#212636,#212637,
#212638,#212639,#212640,#212641,#212642,#212643,#212644,#212645,#212646,
#212647,#212648,#212649,#212650,#212651,#212652,#212653,#212654,#212655,
#212656,#212657,#212658,#212659,#212660,#212661,#212662,#212663,#212664,
#212665,#212666,#212667,#212668,#212669,#212670,#212671,#212672,#212673,
#212674,#212675,#212676,#212677,#212678,#212679,#212680,#212681,#212682,
#212683,#212684,#212685,#212686,#212687,#212688,#212689,#212690,#212691,
#212692,#212693,#212694,#212695,#212696,#212697,#212698,#212699,#212700,
#212701,#212702,#212703,#212704,#212705,#212706,#212707,#212708,#212709,
#212710,#212711,#212712,#212713,#212714,#212715,#212716,#212717,#212718,
#212719,#212720,#212721,#212722,#212723,#212724,#212725,#212726,#212727,
#212728,#212729,#212730,#212731,#212732,#212733,#212734,#212735,#212736,
#212737,#212738,#212739,#212740,#212741,#212742,#212743,#212744,#212745,
#212746,#212747,#212748,#212749,#212750,#212751,#212752,#212753,#212754,
#212755,#212756,#212757,#212758,#212759,#212760,#212761,#212762,#212763,
#212764,#212765,#212766,#212767,#212768,#212769,#212770,#212771,#212772,
#212773,#212774,#212775,#212776,#212777,#212778,#212779,#212780,#212781,
#212782,#212783,#212784,#212785,#212786,#212787,#212788,#212789,#212790,
#212791,#212792,#212793,#212794,#212795,#212796,#212797,#212798,#212799,
#212800,#212801,#212802,#212803,#212804,#212805,#212806,#212807,#212808,
#212809,#212810,#212811,#212812,#212813,#212814,#212815,#212816,#212817,
#212818,#212819,#212820,#212821,#212822,#212823,#212824,#212825,#212826,
#212827,#212828,#212829,#212830,#212831,#212832,#212833,#212834,#212835),
 .UNSPECIFIED.,.F.,.F.)
B_SPLINE_CURVE_WITH_KNOTS((6,1,1,1,1,1,1,1,1,1,1,1,1,1,1,1,1,1,1,1,1,1,
1,1,1,1,1,1,1,1,1,1,1,1,1,1,1,1,1,1,1,1,1,1,1,1,1,1,1,1,1,1,1,1,1,1,1,1,
1,1,1,1,1,1,1,1,1,1,1,1,1,1,1,1,1,1,1,1,1,1,1,1,1,1,1,1,1,1,1,1,1,1,1,1,
1,1,1,1,1,1,1,1,1,1,1,1,1,1,1,1,1,1,1,1,1,1,1,1,1,1,1,1,1,1,1,1,1,1,1,1,
1,1,1,1,1,1,1,1,1,1,1,1,1,1,1,1,1,1,1,1,1,1,1,1,1,1,1,1,1,1,1,1,1,1,1,1,
1,1,1,1,1,1,1,1,1,1,1,1,1,1,1,1,1,1,1,1,1,1,1,1,1,1,1,1,1,1,1,1,1,1,6),
(0.,0.005,0.01,0.015,0.02,0.025,0.03,0.035,0.04,0.045,0.05,0.055,0.06,0.065,
0.07,0.075,0.08,0.085,0.09,0.095,0.1,0.105,0.11,0.115,0.12,0.125,0.13,0.135,
0.14,0.145,0.15,0.155,0.16,0.165,0.17,0.175,0.18,0.185,0.19,0.195,0.2,0.205,
0.21,0.215,0.22,0.225,0.23,0.235,0.24,0.245,0.25,0.255,0.26,0.265,0.27,
0.275,0.28,0.285,0.29,0.295,0.3,0.305,0.31,0.315,0.32,0.325,0.33,0.335,
0.34,0.345,0.35,0.355,0.36,0.365,0.37,0.375,0.38,0.385,0.39,0.395,0.4,0.405,
0.41,0.415,0.42,0.425,0.43,0.435,0.44,0.445,0.45,0.455,0.46,0.465,0.47,
0.475,0.48,0.485,0.49,0.495,0.5,0.505,0.51,0.515,0.52,0.525,0.53,0.535,
0.54,0.545,0.55,0.555,0.56,0.565,0.57,0.575,0.58,0.585,0.59,0.595,0.6,0.605,
0.61,0.615,0.62,0.625,0.63,0.635,0.64,0.645,0.65,0.655,0.66,0.665,0.67,
0.675,0.68,0.685,0.690000000000001,0.695000000000001,0.700000000000001,
0.705000000000001,0.710000000000001,0.715000000000001,0.720000000000001,
0.725000000000001,0.730000000000001,0.735000000000001,0.740000000000001,
0.745000000000001,0.750000000000001,0.755000000000001,0.760000000000001,
0.765000000000001,0.770000000000001,0.775000000000001,0.780000000000001,
0.785000000000001,0.790000000000001,0.795000000000001,0.800000000000001,
0.805000000000001,0.810000000000001,0.815000000000001,0.820000000000001,
0.825000000000001,0.830000000000001,0.835000000000001,0.840000000000001,
0.845000000000001,0.850000000000001,0.855000000000001,0.860000000000001,
0.865000000000001,0.870000000000001,0.875000000000001,0.880000000000001,
0.885000000000001,0.890000000000001,0.895000000000001,0.900000000000001,
0.905000000000001,0.910000000000001,0.915000000000001,0.920000000000001,
0.925000000000001,0.930000000000001,0.935000000000001,0.940000000000001,
0.945000000000001,0.950000000000001,0.955000000000001,0.960000000000001,
0.965000000000001,0.970000000000001,0.975000000000001,0.980000000000001,
0.985000000000001,0.990000000000001,0.995000000000001,1.),.UNSPECIFIED.)
CURVE()
GEOMETRIC_REPRESENTATION_ITEM()
RATIONAL_B_SPLINE_CURVE((1.,1.,1.,1.,1.,1.,1.,1.,1.,1.,1.,1.,1.,1.,1.,1.,
1.,1.,1.,1.,1.,1.,1.,1.,1.,1.,1.,1.,1.,1.,1.,1.,1.,1.,1.,1.,1.,1.,1.,1.,
1.,1.,1.,1.,1.,1.,1.,1.,1.,1.,1.,1.,1.,1.,1.,1.,1.,1.,1.,1.,1.,1.,1.,1.,
1.,1.,1.,1.,1.,1.,1.,1.,1.,1.,1.,1.,1.,1.,1.,1.,1.,1.,1.,1.,1.,1.,1.,1.,
1.,1.,1.,1.,1.,1.,1.,1.,1.,1.,1.,1.,1.,1.,1.,1.,1.,1.,1.,1.,1.,1.,1.,1.,
1.,1.,1.,1.,1.,1.,1.,1.,1.,1.,1.,1.,1.,1.,1.,1.,1.,1.,1.,1.,1.,1.,1.,1.,
1.,1.,1.,1.,1.,1.,1.,1.,1.,1.,1.,1.,1.,1.,1.,1.,1.,1.,1.,1.,1.,1.,1.,1.,
1.,1.,1.,1.,1.,1.,1.,1.,1.,1.,1.,1.,1.,1.,1.,1.,1.,1.,1.,1.,1.,1.,1.,1.,
1.,1.,1.,1.,1.,1.,1.,1.,1.,1.,1.,1.,1.,1.,1.,1.,1.,1.,1.,1.,1.))
REPRESENTATION_ITEM('')
);
#783=(
BOUNDED_CURVE()
B_SPLINE_CURVE(5,(#213252,#213253,#213254,#213255,#213256,#213257,#213258,
#213259,#213260,#213261,#213262,#213263,#213264,#213265,#213266,#213267,
#213268,#213269,#213270,#213271,#213272,#213273,#213274,#213275,#213276,
#213277,#213278,#213279,#213280,#213281,#213282,#213283,#213284,#213285,
#213286,#213287,#213288,#213289,#213290,#213291,#213292,#213293,#213294,
#213295,#213296,#213297,#213298,#213299,#213300,#213301,#213302,#213303,
#213304,#213305,#213306,#213307,#213308,#213309,#213310,#213311,#213312,
#213313,#213314,#213315,#213316,#213317,#213318,#213319,#213320,#213321,
#213322,#213323,#213324,#213325,#213326,#213327,#213328,#213329,#213330,
#213331,#213332,#213333,#213334,#213335,#213336,#213337,#213338,#213339,
#213340,#213341,#213342,#213343,#213344,#213345,#213346,#213347,#213348,
#213349,#213350,#213351,#213352,#213353,#213354,#213355,#213356,#213357,
#213358,#213359,#213360,#213361,#213362,#213363,#213364,#213365,#213366,
#213367,#213368,#213369,#213370,#213371,#213372,#213373,#213374,#213375,
#213376,#213377,#213378,#213379,#213380,#213381,#213382,#213383,#213384,
#213385,#213386,#213387,#213388,#213389,#213390,#213391,#213392,#213393,
#213394,#213395,#213396,#213397,#213398,#213399,#213400,#213401,#213402,
#213403,#213404,#213405,#213406,#213407,#213408,#213409,#213410,#213411,
#213412,#213413,#213414,#213415,#213416,#213417,#213418,#213419,#213420,
#213421,#213422,#213423,#213424,#213425,#213426,#213427,#213428,#213429,
#213430,#213431,#213432,#213433,#213434,#213435,#213436,#213437,#213438,
#213439,#213440,#213441,#213442,#213443,#213444,#213445,#213446,#213447,
#213448,#213449,#213450,#213451,#213452,#213453,#213454,#213455,#213456),
 .UNSPECIFIED.,.F.,.F.)
B_SPLINE_CURVE_WITH_KNOTS((6,1,1,1,1,1,1,1,1,1,1,1,1,1,1,1,1,1,1,1,1,1,
1,1,1,1,1,1,1,1,1,1,1,1,1,1,1,1,1,1,1,1,1,1,1,1,1,1,1,1,1,1,1,1,1,1,1,1,
1,1,1,1,1,1,1,1,1,1,1,1,1,1,1,1,1,1,1,1,1,1,1,1,1,1,1,1,1,1,1,1,1,1,1,1,
1,1,1,1,1,1,1,1,1,1,1,1,1,1,1,1,1,1,1,1,1,1,1,1,1,1,1,1,1,1,1,1,1,1,1,1,
1,1,1,1,1,1,1,1,1,1,1,1,1,1,1,1,1,1,1,1,1,1,1,1,1,1,1,1,1,1,1,1,1,1,1,1,
1,1,1,1,1,1,1,1,1,1,1,1,1,1,1,1,1,1,1,1,1,1,1,1,1,1,1,1,1,1,1,1,1,1,6),
(-1.,-0.995000000000001,-0.990000000000001,-0.985000000000001,-0.980000000000001,
-0.975000000000001,-0.970000000000001,-0.965000000000001,-0.960000000000001,
-0.955000000000001,-0.950000000000001,-0.945000000000001,-0.940000000000001,
-0.935000000000001,-0.930000000000001,-0.925000000000001,-0.920000000000001,
-0.915000000000001,-0.910000000000001,-0.905000000000001,-0.900000000000001,
-0.895000000000001,-0.890000000000001,-0.885000000000001,-0.880000000000001,
-0.875000000000001,-0.870000000000001,-0.865000000000001,-0.860000000000001,
-0.855000000000001,-0.850000000000001,-0.845000000000001,-0.840000000000001,
-0.835000000000001,-0.830000000000001,-0.825000000000001,-0.820000000000001,
-0.815000000000001,-0.810000000000001,-0.805000000000001,-0.800000000000001,
-0.795000000000001,-0.790000000000001,-0.785000000000001,-0.780000000000001,
-0.775000000000001,-0.770000000000001,-0.765000000000001,-0.760000000000001,
-0.755000000000001,-0.750000000000001,-0.745000000000001,-0.740000000000001,
-0.735000000000001,-0.730000000000001,-0.725000000000001,-0.720000000000001,
-0.715000000000001,-0.710000000000001,-0.705000000000001,-0.700000000000001,
-0.695000000000001,-0.690000000000001,-0.685,-0.68,-0.675,-0.67,-0.665,
-0.66,-0.655,-0.65,-0.645,-0.64,-0.635,-0.63,-0.625,-0.62,-0.615,-0.61,
-0.605,-0.6,-0.595,-0.59,-0.585,-0.58,-0.575,-0.57,-0.565,-0.56,-0.555,
-0.55,-0.545,-0.54,-0.535,-0.53,-0.525,-0.52,-0.515,-0.51,-0.505,-0.5,-0.495,
-0.49,-0.485,-0.48,-0.475,-0.47,-0.465,-0.46,-0.455,-0.45,-0.445,-0.44,
-0.435,-0.43,-0.425,-0.42,-0.415,-0.41,-0.405,-0.4,-0.395,-0.39,-0.385,
-0.38,-0.375,-0.37,-0.365,-0.36,-0.355,-0.35,-0.345,-0.34,-0.335,-0.33,
-0.325,-0.32,-0.315,-0.31,-0.305,-0.3,-0.295,-0.29,-0.285,-0.28,-0.275,
-0.27,-0.265,-0.26,-0.255,-0.25,-0.245,-0.24,-0.235,-0.23,-0.225,-0.22,
-0.215,-0.21,-0.205,-0.2,-0.195,-0.19,-0.185,-0.18,-0.175,-0.17,-0.165,
-0.16,-0.155,-0.15,-0.145,-0.14,-0.135,-0.13,-0.125,-0.12,-0.115,-0.11,
-0.105,-0.1,-0.095,-0.09,-0.085,-0.08,-0.075,-0.07,-0.065,-0.06,-0.055,
-0.05,-0.045,-0.04,-0.035,-0.03,-0.025,-0.02,-0.015,-0.01,-0.005,0.),
 .UNSPECIFIED.)
CURVE()
GEOMETRIC_REPRESENTATION_ITEM()
RATIONAL_B_SPLINE_CURVE((1.,1.,1.,1.,1.,1.,1.,1.,1.,1.,1.,1.,1.,1.,1.,1.,
1.,1.,1.,1.,1.,1.,1.,1.,1.,1.,1.,1.,1.,1.,1.,1.,1.,1.,1.,1.,1.,1.,1.,1.,
1.,1.,1.,1.,1.,1.,1.,1.,1.,1.,1.,1.,1.,1.,1.,1.,1.,1.,1.,1.,1.,1.,1.,1.,
1.,1.,1.,1.,1.,1.,1.,1.,1.,1.,1.,1.,1.,1.,1.,1.,1.,1.,1.,1.,1.,1.,1.,1.,
1.,1.,1.,1.,1.,1.,1.,1.,1.,1.,1.,1.,1.,1.,1.,1.,1.,1.,1.,1.,1.,1.,1.,1.,
1.,1.,1.,1.,1.,1.,1.,1.,1.,1.,1.,1.,1.,1.,1.,1.,1.,1.,1.,1.,1.,1.,1.,1.,
1.,1.,1.,1.,1.,1.,1.,1.,1.,1.,1.,1.,1.,1.,1.,1.,1.,1.,1.,1.,1.,1.,1.,1.,
1.,1.,1.,1.,1.,1.,1.,1.,1.,1.,1.,1.,1.,1.,1.,1.,1.,1.,1.,1.,1.,1.,1.,1.,
1.,1.,1.,1.,1.,1.,1.,1.,1.,1.,1.,1.,1.,1.,1.,1.,1.,1.,1.,1.,1.))
REPRESENTATION_ITEM('')
);
#784=(
BOUNDED_CURVE()
B_SPLINE_CURVE(5,(#213869,#213870,#213871,#213872,#213873,#213874,#213875,
#213876,#213877,#213878,#213879,#213880,#213881,#213882,#213883,#213884,
#213885,#213886,#213887,#213888,#213889,#213890,#213891,#213892,#213893,
#213894,#213895,#213896,#213897,#213898,#213899,#213900,#213901,#213902,
#213903,#213904,#213905,#213906,#213907,#213908,#213909,#213910,#213911,
#213912,#213913,#213914,#213915,#213916,#213917,#213918,#213919,#213920,
#213921,#213922,#213923,#213924,#213925,#213926,#213927,#213928,#213929,
#213930,#213931,#213932,#213933,#213934,#213935,#213936,#213937,#213938,
#213939,#213940,#213941,#213942,#213943,#213944,#213945,#213946,#213947,
#213948,#213949,#213950,#213951,#213952,#213953,#213954,#213955,#213956,
#213957,#213958,#213959,#213960,#213961,#213962,#213963,#213964,#213965,
#213966,#213967,#213968,#213969,#213970,#213971,#213972,#213973,#213974,
#213975,#213976,#213977,#213978,#213979,#213980,#213981,#213982,#213983,
#213984,#213985,#213986,#213987,#213988,#213989,#213990,#213991,#213992,
#213993,#213994,#213995,#213996,#213997,#213998,#213999,#214000,#214001,
#214002,#214003,#214004,#214005,#214006,#214007,#214008,#214009,#214010,
#214011,#214012,#214013,#214014,#214015,#214016,#214017,#214018,#214019,
#214020,#214021,#214022,#214023,#214024,#214025,#214026,#214027,#214028,
#214029,#214030,#214031,#214032,#214033,#214034,#214035,#214036,#214037,
#214038,#214039,#214040,#214041,#214042,#214043,#214044,#214045,#214046,
#214047,#214048,#214049,#214050,#214051,#214052,#214053,#214054,#214055,
#214056,#214057,#214058,#214059,#214060,#214061,#214062,#214063,#214064,
#214065,#214066,#214067,#214068,#214069,#214070,#214071,#214072,#214073),
 .UNSPECIFIED.,.F.,.F.)
B_SPLINE_CURVE_WITH_KNOTS((6,1,1,1,1,1,1,1,1,1,1,1,1,1,1,1,1,1,1,1,1,1,
1,1,1,1,1,1,1,1,1,1,1,1,1,1,1,1,1,1,1,1,1,1,1,1,1,1,1,1,1,1,1,1,1,1,1,1,
1,1,1,1,1,1,1,1,1,1,1,1,1,1,1,1,1,1,1,1,1,1,1,1,1,1,1,1,1,1,1,1,1,1,1,1,
1,1,1,1,1,1,1,1,1,1,1,1,1,1,1,1,1,1,1,1,1,1,1,1,1,1,1,1,1,1,1,1,1,1,1,1,
1,1,1,1,1,1,1,1,1,1,1,1,1,1,1,1,1,1,1,1,1,1,1,1,1,1,1,1,1,1,1,1,1,1,1,1,
1,1,1,1,1,1,1,1,1,1,1,1,1,1,1,1,1,1,1,1,1,1,1,1,1,1,1,1,1,1,1,1,1,1,6),
(0.,0.005,0.01,0.015,0.02,0.025,0.03,0.035,0.04,0.045,0.05,0.055,0.06,0.065,
0.07,0.075,0.08,0.085,0.09,0.095,0.1,0.105,0.11,0.115,0.12,0.125,0.13,0.135,
0.14,0.145,0.15,0.155,0.16,0.165,0.17,0.175,0.18,0.185,0.19,0.195,0.2,0.205,
0.21,0.215,0.22,0.225,0.23,0.235,0.24,0.245,0.25,0.255,0.26,0.265,0.27,
0.275,0.28,0.285,0.29,0.295,0.3,0.305,0.31,0.315,0.32,0.325,0.33,0.335,
0.34,0.345,0.35,0.355,0.36,0.365,0.37,0.375,0.38,0.385,0.39,0.395,0.4,0.405,
0.41,0.415,0.42,0.425,0.43,0.435,0.44,0.445,0.45,0.455,0.46,0.465,0.47,
0.475,0.48,0.485,0.49,0.495,0.5,0.505,0.51,0.515,0.52,0.525,0.53,0.535,
0.54,0.545,0.55,0.555,0.56,0.565,0.57,0.575,0.58,0.585,0.59,0.595,0.6,0.605,
0.61,0.615,0.62,0.625,0.63,0.635,0.64,0.645,0.65,0.655,0.66,0.665,0.67,
0.675,0.68,0.685,0.690000000000001,0.695000000000001,0.700000000000001,
0.705000000000001,0.710000000000001,0.715000000000001,0.720000000000001,
0.725000000000001,0.730000000000001,0.735000000000001,0.740000000000001,
0.745000000000001,0.750000000000001,0.755000000000001,0.760000000000001,
0.765000000000001,0.770000000000001,0.775000000000001,0.780000000000001,
0.785000000000001,0.790000000000001,0.795000000000001,0.800000000000001,
0.805000000000001,0.810000000000001,0.815000000000001,0.820000000000001,
0.825000000000001,0.830000000000001,0.835000000000001,0.840000000000001,
0.845000000000001,0.850000000000001,0.855000000000001,0.860000000000001,
0.865000000000001,0.870000000000001,0.875000000000001,0.880000000000001,
0.885000000000001,0.890000000000001,0.895000000000001,0.900000000000001,
0.905000000000001,0.910000000000001,0.915000000000001,0.920000000000001,
0.925000000000001,0.930000000000001,0.935000000000001,0.940000000000001,
0.945000000000001,0.950000000000001,0.955000000000001,0.960000000000001,
0.965000000000001,0.970000000000001,0.975000000000001,0.980000000000001,
0.985000000000001,0.990000000000001,0.995000000000001,1.),.UNSPECIFIED.)
CURVE()
GEOMETRIC_REPRESENTATION_ITEM()
RATIONAL_B_SPLINE_CURVE((1.,1.,1.,1.,1.,1.,1.,1.,1.,1.,1.,1.,1.,1.,1.,1.,
1.,1.,1.,1.,1.,1.,1.,1.,1.,1.,1.,1.,1.,1.,1.,1.,1.,1.,1.,1.,1.,1.,1.,1.,
1.,1.,1.,1.,1.,1.,1.,1.,1.,1.,1.,1.,1.,1.,1.,1.,1.,1.,1.,1.,1.,1.,1.,1.,
1.,1.,1.,1.,1.,1.,1.,1.,1.,1.,1.,1.,1.,1.,1.,1.,1.,1.,1.,1.,1.,1.,1.,1.,
1.,1.,1.,1.,1.,1.,1.,1.,1.,1.,1.,1.,1.,1.,1.,1.,1.,1.,1.,1.,1.,1.,1.,1.,
1.,1.,1.,1.,1.,1.,1.,1.,1.,1.,1.,1.,1.,1.,1.,1.,1.,1.,1.,1.,1.,1.,1.,1.,
1.,1.,1.,1.,1.,1.,1.,1.,1.,1.,1.,1.,1.,1.,1.,1.,1.,1.,1.,1.,1.,1.,1.,1.,
1.,1.,1.,1.,1.,1.,1.,1.,1.,1.,1.,1.,1.,1.,1.,1.,1.,1.,1.,1.,1.,1.,1.,1.,
1.,1.,1.,1.,1.,1.,1.,1.,1.,1.,1.,1.,1.,1.,1.,1.,1.,1.,1.,1.,1.))
REPRESENTATION_ITEM('')
);
#785=(
BOUNDED_CURVE()
B_SPLINE_CURVE(5,(#214101,#214102,#214103,#214104,#214105,#214106,#214107,
#214108,#214109,#214110,#214111,#214112,#214113,#214114,#214115,#214116,
#214117,#214118,#214119,#214120,#214121,#214122,#214123,#214124,#214125,
#214126,#214127,#214128,#214129,#214130,#214131,#214132,#214133,#214134,
#214135,#214136,#214137,#214138,#214139,#214140,#214141,#214142,#214143,
#214144,#214145,#214146,#214147,#214148,#214149,#214150,#214151,#214152,
#214153,#214154,#214155,#214156,#214157,#214158,#214159,#214160,#214161,
#214162,#214163,#214164,#214165,#214166,#214167,#214168,#214169,#214170,
#214171,#214172,#214173,#214174,#214175,#214176,#214177,#214178,#214179,
#214180,#214181,#214182,#214183,#214184,#214185,#214186,#214187,#214188,
#214189,#214190,#214191,#214192,#214193,#214194,#214195,#214196,#214197,
#214198,#214199,#214200,#214201,#214202,#214203,#214204,#214205,#214206,
#214207,#214208,#214209,#214210,#214211,#214212,#214213,#214214,#214215,
#214216,#214217,#214218,#214219,#214220,#214221,#214222,#214223,#214224,
#214225,#214226,#214227,#214228,#214229,#214230,#214231,#214232,#214233,
#214234,#214235,#214236,#214237,#214238,#214239,#214240,#214241,#214242,
#214243,#214244,#214245,#214246,#214247,#214248,#214249,#214250,#214251,
#214252,#214253,#214254,#214255,#214256,#214257,#214258,#214259,#214260,
#214261,#214262,#214263,#214264,#214265,#214266,#214267,#214268,#214269,
#214270,#214271,#214272,#214273,#214274,#214275,#214276,#214277,#214278,
#214279,#214280,#214281,#214282,#214283,#214284,#214285,#214286,#214287,
#214288,#214289,#214290,#214291,#214292,#214293,#214294,#214295,#214296,
#214297,#214298,#214299,#214300,#214301,#214302,#214303,#214304,#214305),
 .UNSPECIFIED.,.F.,.F.)
B_SPLINE_CURVE_WITH_KNOTS((6,1,1,1,1,1,1,1,1,1,1,1,1,1,1,1,1,1,1,1,1,1,
1,1,1,1,1,1,1,1,1,1,1,1,1,1,1,1,1,1,1,1,1,1,1,1,1,1,1,1,1,1,1,1,1,1,1,1,
1,1,1,1,1,1,1,1,1,1,1,1,1,1,1,1,1,1,1,1,1,1,1,1,1,1,1,1,1,1,1,1,1,1,1,1,
1,1,1,1,1,1,1,1,1,1,1,1,1,1,1,1,1,1,1,1,1,1,1,1,1,1,1,1,1,1,1,1,1,1,1,1,
1,1,1,1,1,1,1,1,1,1,1,1,1,1,1,1,1,1,1,1,1,1,1,1,1,1,1,1,1,1,1,1,1,1,1,1,
1,1,1,1,1,1,1,1,1,1,1,1,1,1,1,1,1,1,1,1,1,1,1,1,1,1,1,1,1,1,1,1,1,1,6),
(-1.,-0.995000000000001,-0.990000000000001,-0.985000000000001,-0.980000000000001,
-0.975000000000001,-0.970000000000001,-0.965000000000001,-0.960000000000001,
-0.955000000000001,-0.950000000000001,-0.945000000000001,-0.940000000000001,
-0.935000000000001,-0.930000000000001,-0.925000000000001,-0.920000000000001,
-0.915000000000001,-0.910000000000001,-0.905000000000001,-0.900000000000001,
-0.895000000000001,-0.890000000000001,-0.885000000000001,-0.880000000000001,
-0.875000000000001,-0.870000000000001,-0.865000000000001,-0.860000000000001,
-0.855000000000001,-0.850000000000001,-0.845000000000001,-0.840000000000001,
-0.835000000000001,-0.830000000000001,-0.825000000000001,-0.820000000000001,
-0.815000000000001,-0.810000000000001,-0.805000000000001,-0.800000000000001,
-0.795000000000001,-0.790000000000001,-0.785000000000001,-0.780000000000001,
-0.775000000000001,-0.770000000000001,-0.765000000000001,-0.760000000000001,
-0.755000000000001,-0.750000000000001,-0.745000000000001,-0.740000000000001,
-0.735000000000001,-0.730000000000001,-0.725000000000001,-0.720000000000001,
-0.715000000000001,-0.710000000000001,-0.705000000000001,-0.700000000000001,
-0.695000000000001,-0.690000000000001,-0.685,-0.68,-0.675,-0.67,-0.665,
-0.66,-0.655,-0.65,-0.645,-0.64,-0.635,-0.63,-0.625,-0.62,-0.615,-0.61,
-0.605,-0.6,-0.595,-0.59,-0.585,-0.58,-0.575,-0.57,-0.565,-0.56,-0.555,
-0.55,-0.545,-0.54,-0.535,-0.53,-0.525,-0.52,-0.515,-0.51,-0.505,-0.5,-0.495,
-0.49,-0.485,-0.48,-0.475,-0.47,-0.465,-0.46,-0.455,-0.45,-0.445,-0.44,
-0.435,-0.43,-0.425,-0.42,-0.415,-0.41,-0.405,-0.4,-0.395,-0.39,-0.385,
-0.38,-0.375,-0.37,-0.365,-0.36,-0.355,-0.35,-0.345,-0.34,-0.335,-0.33,
-0.325,-0.32,-0.315,-0.31,-0.305,-0.3,-0.295,-0.29,-0.285,-0.28,-0.275,
-0.27,-0.265,-0.26,-0.255,-0.25,-0.245,-0.24,-0.235,-0.23,-0.225,-0.22,
-0.215,-0.21,-0.205,-0.2,-0.195,-0.19,-0.185,-0.18,-0.175,-0.17,-0.165,
-0.16,-0.155,-0.15,-0.145,-0.14,-0.135,-0.13,-0.125,-0.12,-0.115,-0.11,
-0.105,-0.1,-0.095,-0.09,-0.085,-0.08,-0.075,-0.07,-0.065,-0.06,-0.055,
-0.05,-0.045,-0.04,-0.035,-0.03,-0.025,-0.02,-0.015,-0.01,-0.005,0.),
 .UNSPECIFIED.)
CURVE()
GEOMETRIC_REPRESENTATION_ITEM()
RATIONAL_B_SPLINE_CURVE((1.,1.,1.,1.,1.,1.,1.,1.,1.,1.,1.,1.,1.,1.,1.,1.,
1.,1.,1.,1.,1.,1.,1.,1.,1.,1.,1.,1.,1.,1.,1.,1.,1.,1.,1.,1.,1.,1.,1.,1.,
1.,1.,1.,1.,1.,1.,1.,1.,1.,1.,1.,1.,1.,1.,1.,1.,1.,1.,1.,1.,1.,1.,1.,1.,
1.,1.,1.,1.,1.,1.,1.,1.,1.,1.,1.,1.,1.,1.,1.,1.,1.,1.,1.,1.,1.,1.,1.,1.,
1.,1.,1.,1.,1.,1.,1.,1.,1.,1.,1.,1.,1.,1.,1.,1.,1.,1.,1.,1.,1.,1.,1.,1.,
1.,1.,1.,1.,1.,1.,1.,1.,1.,1.,1.,1.,1.,1.,1.,1.,1.,1.,1.,1.,1.,1.,1.,1.,
1.,1.,1.,1.,1.,1.,1.,1.,1.,1.,1.,1.,1.,1.,1.,1.,1.,1.,1.,1.,1.,1.,1.,1.,
1.,1.,1.,1.,1.,1.,1.,1.,1.,1.,1.,1.,1.,1.,1.,1.,1.,1.,1.,1.,1.,1.,1.,1.,
1.,1.,1.,1.,1.,1.,1.,1.,1.,1.,1.,1.,1.,1.,1.,1.,1.,1.,1.,1.,1.))
REPRESENTATION_ITEM('')
);
#786=(
BOUNDED_CURVE()
B_SPLINE_CURVE(5,(#214317,#214318,#214319,#214320,#214321,#214322,#214323,
#214324,#214325,#214326,#214327,#214328,#214329,#214330,#214331,#214332,
#214333,#214334,#214335,#214336,#214337,#214338,#214339,#214340,#214341,
#214342,#214343,#214344,#214345,#214346,#214347,#214348,#214349,#214350,
#214351,#214352,#214353,#214354,#214355,#214356,#214357,#214358,#214359,
#214360,#214361,#214362,#214363,#214364,#214365,#214366,#214367,#214368,
#214369,#214370,#214371,#214372,#214373,#214374,#214375,#214376,#214377,
#214378,#214379,#214380,#214381,#214382,#214383,#214384,#214385,#214386,
#214387,#214388,#214389,#214390,#214391,#214392,#214393,#214394,#214395,
#214396,#214397,#214398,#214399,#214400,#214401,#214402,#214403,#214404,
#214405,#214406,#214407,#214408,#214409,#214410,#214411,#214412,#214413,
#214414,#214415,#214416,#214417,#214418,#214419,#214420,#214421,#214422,
#214423,#214424,#214425,#214426,#214427,#214428,#214429,#214430,#214431,
#214432,#214433,#214434,#214435,#214436,#214437,#214438,#214439,#214440,
#214441,#214442,#214443,#214444,#214445,#214446,#214447,#214448,#214449,
#214450,#214451,#214452,#214453,#214454,#214455,#214456,#214457,#214458,
#214459,#214460,#214461,#214462,#214463,#214464,#214465,#214466,#214467,
#214468,#214469,#214470,#214471,#214472,#214473,#214474,#214475,#214476,
#214477,#214478,#214479,#214480,#214481,#214482,#214483,#214484,#214485,
#214486,#214487,#214488,#214489,#214490,#214491,#214492,#214493,#214494,
#214495,#214496,#214497,#214498,#214499,#214500,#214501,#214502,#214503,
#214504,#214505,#214506,#214507,#214508,#214509,#214510,#214511,#214512,
#214513,#214514,#214515,#214516,#214517,#214518,#214519,#214520,#214521),
 .UNSPECIFIED.,.F.,.F.)
B_SPLINE_CURVE_WITH_KNOTS((6,1,1,1,1,1,1,1,1,1,1,1,1,1,1,1,1,1,1,1,1,1,
1,1,1,1,1,1,1,1,1,1,1,1,1,1,1,1,1,1,1,1,1,1,1,1,1,1,1,1,1,1,1,1,1,1,1,1,
1,1,1,1,1,1,1,1,1,1,1,1,1,1,1,1,1,1,1,1,1,1,1,1,1,1,1,1,1,1,1,1,1,1,1,1,
1,1,1,1,1,1,1,1,1,1,1,1,1,1,1,1,1,1,1,1,1,1,1,1,1,1,1,1,1,1,1,1,1,1,1,1,
1,1,1,1,1,1,1,1,1,1,1,1,1,1,1,1,1,1,1,1,1,1,1,1,1,1,1,1,1,1,1,1,1,1,1,1,
1,1,1,1,1,1,1,1,1,1,1,1,1,1,1,1,1,1,1,1,1,1,1,1,1,1,1,1,1,1,1,1,1,1,6),
(0.,0.005,0.01,0.015,0.02,0.025,0.03,0.035,0.04,0.045,0.05,0.055,0.06,0.065,
0.07,0.075,0.08,0.085,0.09,0.095,0.1,0.105,0.11,0.115,0.12,0.125,0.13,0.135,
0.14,0.145,0.15,0.155,0.16,0.165,0.17,0.175,0.18,0.185,0.19,0.195,0.2,0.205,
0.21,0.215,0.22,0.225,0.23,0.235,0.24,0.245,0.25,0.255,0.26,0.265,0.27,
0.275,0.28,0.285,0.29,0.295,0.3,0.305,0.31,0.315,0.32,0.325,0.33,0.335,
0.34,0.345,0.35,0.355,0.36,0.365,0.37,0.375,0.38,0.385,0.39,0.395,0.4,0.405,
0.41,0.415,0.42,0.425,0.43,0.435,0.44,0.445,0.45,0.455,0.46,0.465,0.47,
0.475,0.48,0.485,0.49,0.495,0.5,0.505,0.51,0.515,0.52,0.525,0.53,0.535,
0.54,0.545,0.55,0.555,0.56,0.565,0.57,0.575,0.58,0.585,0.59,0.595,0.6,0.605,
0.61,0.615,0.62,0.625,0.63,0.635,0.64,0.645,0.65,0.655,0.66,0.665,0.67,
0.675,0.68,0.685,0.690000000000001,0.695000000000001,0.700000000000001,
0.705000000000001,0.710000000000001,0.715000000000001,0.720000000000001,
0.725000000000001,0.730000000000001,0.735000000000001,0.740000000000001,
0.745000000000001,0.750000000000001,0.755000000000001,0.760000000000001,
0.765000000000001,0.770000000000001,0.775000000000001,0.780000000000001,
0.785000000000001,0.790000000000001,0.795000000000001,0.800000000000001,
0.805000000000001,0.810000000000001,0.815000000000001,0.820000000000001,
0.825000000000001,0.830000000000001,0.835000000000001,0.840000000000001,
0.845000000000001,0.850000000000001,0.855000000000001,0.860000000000001,
0.865000000000001,0.870000000000001,0.875000000000001,0.880000000000001,
0.885000000000001,0.890000000000001,0.895000000000001,0.900000000000001,
0.905000000000001,0.910000000000001,0.915000000000001,0.920000000000001,
0.925000000000001,0.930000000000001,0.935000000000001,0.940000000000001,
0.945000000000001,0.950000000000001,0.955000000000001,0.960000000000001,
0.965000000000001,0.970000000000001,0.975000000000001,0.980000000000001,
0.985000000000001,0.990000000000001,0.995000000000001,1.),.UNSPECIFIED.)
CURVE()
GEOMETRIC_REPRESENTATION_ITEM()
RATIONAL_B_SPLINE_CURVE((1.,1.,1.,1.,1.,1.,1.,1.,1.,1.,1.,1.,1.,1.,1.,1.,
1.,1.,1.,1.,1.,1.,1.,1.,1.,1.,1.,1.,1.,1.,1.,1.,1.,1.,1.,1.,1.,1.,1.,1.,
1.,1.,1.,1.,1.,1.,1.,1.,1.,1.,1.,1.,1.,1.,1.,1.,1.,1.,1.,1.,1.,1.,1.,1.,
1.,1.,1.,1.,1.,1.,1.,1.,1.,1.,1.,1.,1.,1.,1.,1.,1.,1.,1.,1.,1.,1.,1.,1.,
1.,1.,1.,1.,1.,1.,1.,1.,1.,1.,1.,1.,1.,1.,1.,1.,1.,1.,1.,1.,1.,1.,1.,1.,
1.,1.,1.,1.,1.,1.,1.,1.,1.,1.,1.,1.,1.,1.,1.,1.,1.,1.,1.,1.,1.,1.,1.,1.,
1.,1.,1.,1.,1.,1.,1.,1.,1.,1.,1.,1.,1.,1.,1.,1.,1.,1.,1.,1.,1.,1.,1.,1.,
1.,1.,1.,1.,1.,1.,1.,1.,1.,1.,1.,1.,1.,1.,1.,1.,1.,1.,1.,1.,1.,1.,1.,1.,
1.,1.,1.,1.,1.,1.,1.,1.,1.,1.,1.,1.,1.,1.,1.,1.,1.,1.,1.,1.,1.))
REPRESENTATION_ITEM('')
);
#787=(
BOUNDED_CURVE()
B_SPLINE_CURVE(5,(#216419,#216420,#216421,#216422,#216423,#216424,#216425,
#216426,#216427,#216428,#216429,#216430,#216431,#216432,#216433,#216434,
#216435,#216436,#216437,#216438,#216439,#216440,#216441,#216442,#216443,
#216444,#216445,#216446,#216447,#216448,#216449,#216450,#216451,#216452,
#216453,#216454,#216455,#216456,#216457,#216458,#216459,#216460,#216461,
#216462,#216463,#216464,#216465,#216466,#216467,#216468,#216469,#216470,
#216471,#216472,#216473,#216474,#216475,#216476,#216477,#216478,#216479,
#216480,#216481,#216482,#216483,#216484,#216485,#216486,#216487,#216488,
#216489,#216490,#216491,#216492,#216493,#216494,#216495,#216496,#216497,
#216498,#216499,#216500,#216501,#216502,#216503,#216504,#216505,#216506,
#216507,#216508,#216509,#216510,#216511,#216512,#216513,#216514,#216515,
#216516,#216517,#216518,#216519,#216520,#216521,#216522,#216523,#216524,
#216525,#216526,#216527,#216528,#216529,#216530,#216531,#216532,#216533,
#216534,#216535,#216536,#216537,#216538,#216539,#216540,#216541,#216542,
#216543,#216544,#216545,#216546,#216547,#216548,#216549,#216550,#216551,
#216552,#216553,#216554,#216555,#216556,#216557,#216558,#216559,#216560,
#216561,#216562,#216563,#216564,#216565,#216566,#216567,#216568,#216569,
#216570,#216571,#216572,#216573,#216574,#216575,#216576,#216577,#216578,
#216579,#216580,#216581,#216582,#216583,#216584,#216585,#216586,#216587,
#216588,#216589,#216590,#216591,#216592,#216593,#216594,#216595,#216596,
#216597,#216598,#216599,#216600,#216601,#216602,#216603,#216604,#216605,
#216606,#216607,#216608,#216609,#216610,#216611,#216612,#216613,#216614,
#216615,#216616,#216617,#216618,#216619,#216620,#216621,#216622,#216623),
 .UNSPECIFIED.,.F.,.F.)
B_SPLINE_CURVE_WITH_KNOTS((6,1,1,1,1,1,1,1,1,1,1,1,1,1,1,1,1,1,1,1,1,1,
1,1,1,1,1,1,1,1,1,1,1,1,1,1,1,1,1,1,1,1,1,1,1,1,1,1,1,1,1,1,1,1,1,1,1,1,
1,1,1,1,1,1,1,1,1,1,1,1,1,1,1,1,1,1,1,1,1,1,1,1,1,1,1,1,1,1,1,1,1,1,1,1,
1,1,1,1,1,1,1,1,1,1,1,1,1,1,1,1,1,1,1,1,1,1,1,1,1,1,1,1,1,1,1,1,1,1,1,1,
1,1,1,1,1,1,1,1,1,1,1,1,1,1,1,1,1,1,1,1,1,1,1,1,1,1,1,1,1,1,1,1,1,1,1,1,
1,1,1,1,1,1,1,1,1,1,1,1,1,1,1,1,1,1,1,1,1,1,1,1,1,1,1,1,1,1,1,1,1,1,6),
(-1.,-0.995000000000001,-0.990000000000001,-0.985000000000001,-0.980000000000001,
-0.975000000000001,-0.970000000000001,-0.965000000000001,-0.960000000000001,
-0.955000000000001,-0.950000000000001,-0.945000000000001,-0.940000000000001,
-0.935000000000001,-0.930000000000001,-0.925000000000001,-0.920000000000001,
-0.915000000000001,-0.910000000000001,-0.905000000000001,-0.900000000000001,
-0.895000000000001,-0.890000000000001,-0.885000000000001,-0.880000000000001,
-0.875000000000001,-0.870000000000001,-0.865000000000001,-0.860000000000001,
-0.855000000000001,-0.850000000000001,-0.845000000000001,-0.840000000000001,
-0.835000000000001,-0.830000000000001,-0.825000000000001,-0.820000000000001,
-0.815000000000001,-0.810000000000001,-0.805000000000001,-0.800000000000001,
-0.795000000000001,-0.790000000000001,-0.785000000000001,-0.780000000000001,
-0.775000000000001,-0.770000000000001,-0.765000000000001,-0.760000000000001,
-0.755000000000001,-0.750000000000001,-0.745000000000001,-0.740000000000001,
-0.735000000000001,-0.730000000000001,-0.725000000000001,-0.720000000000001,
-0.715000000000001,-0.710000000000001,-0.705000000000001,-0.700000000000001,
-0.695000000000001,-0.690000000000001,-0.685,-0.68,-0.675,-0.67,-0.665,
-0.66,-0.655,-0.65,-0.645,-0.64,-0.635,-0.63,-0.625,-0.62,-0.615,-0.61,
-0.605,-0.6,-0.595,-0.59,-0.585,-0.58,-0.575,-0.57,-0.565,-0.56,-0.555,
-0.55,-0.545,-0.54,-0.535,-0.53,-0.525,-0.52,-0.515,-0.51,-0.505,-0.5,-0.495,
-0.49,-0.485,-0.48,-0.475,-0.47,-0.465,-0.46,-0.455,-0.45,-0.445,-0.44,
-0.435,-0.43,-0.425,-0.42,-0.415,-0.41,-0.405,-0.4,-0.395,-0.39,-0.385,
-0.38,-0.375,-0.37,-0.365,-0.36,-0.355,-0.35,-0.345,-0.34,-0.335,-0.33,
-0.325,-0.32,-0.315,-0.31,-0.305,-0.3,-0.295,-0.29,-0.285,-0.28,-0.275,
-0.27,-0.265,-0.26,-0.255,-0.25,-0.245,-0.24,-0.235,-0.23,-0.225,-0.22,
-0.215,-0.21,-0.205,-0.2,-0.195,-0.19,-0.185,-0.18,-0.175,-0.17,-0.165,
-0.16,-0.155,-0.15,-0.145,-0.14,-0.135,-0.13,-0.125,-0.12,-0.115,-0.11,
-0.105,-0.1,-0.095,-0.09,-0.085,-0.08,-0.075,-0.07,-0.065,-0.06,-0.055,
-0.05,-0.045,-0.04,-0.035,-0.03,-0.025,-0.02,-0.015,-0.01,-0.005,0.),
 .UNSPECIFIED.)
CURVE()
GEOMETRIC_REPRESENTATION_ITEM()
RATIONAL_B_SPLINE_CURVE((1.,1.,1.,1.,1.,1.,1.,1.,1.,1.,1.,1.,1.,1.,1.,1.,
1.,1.,1.,1.,1.,1.,1.,1.,1.,1.,1.,1.,1.,1.,1.,1.,1.,1.,1.,1.,1.,1.,1.,1.,
1.,1.,1.,1.,1.,1.,1.,1.,1.,1.,1.,1.,1.,1.,1.,1.,1.,1.,1.,1.,1.,1.,1.,1.,
1.,1.,1.,1.,1.,1.,1.,1.,1.,1.,1.,1.,1.,1.,1.,1.,1.,1.,1.,1.,1.,1.,1.,1.,
1.,1.,1.,1.,1.,1.,1.,1.,1.,1.,1.,1.,1.,1.,1.,1.,1.,1.,1.,1.,1.,1.,1.,1.,
1.,1.,1.,1.,1.,1.,1.,1.,1.,1.,1.,1.,1.,1.,1.,1.,1.,1.,1.,1.,1.,1.,1.,1.,
1.,1.,1.,1.,1.,1.,1.,1.,1.,1.,1.,1.,1.,1.,1.,1.,1.,1.,1.,1.,1.,1.,1.,1.,
1.,1.,1.,1.,1.,1.,1.,1.,1.,1.,1.,1.,1.,1.,1.,1.,1.,1.,1.,1.,1.,1.,1.,1.,
1.,1.,1.,1.,1.,1.,1.,1.,1.,1.,1.,1.,1.,1.,1.,1.,1.,1.,1.,1.,1.))
REPRESENTATION_ITEM('')
);
#788=(
BOUNDED_CURVE()
B_SPLINE_CURVE(5,(#216626,#216627,#216628,#216629,#216630,#216631,#216632,
#216633,#216634,#216635,#216636,#216637,#216638,#216639,#216640,#216641,
#216642,#216643,#216644,#216645,#216646,#216647,#216648,#216649,#216650,
#216651,#216652,#216653,#216654,#216655,#216656,#216657,#216658,#216659,
#216660,#216661,#216662,#216663,#216664,#216665,#216666,#216667,#216668,
#216669,#216670,#216671,#216672,#216673,#216674,#216675,#216676,#216677,
#216678,#216679,#216680,#216681,#216682,#216683,#216684,#216685,#216686,
#216687,#216688,#216689,#216690,#216691,#216692,#216693,#216694,#216695,
#216696,#216697,#216698,#216699,#216700,#216701,#216702,#216703,#216704,
#216705,#216706,#216707,#216708,#216709,#216710,#216711,#216712,#216713,
#216714,#216715,#216716,#216717,#216718,#216719,#216720,#216721,#216722,
#216723,#216724,#216725,#216726,#216727,#216728,#216729,#216730,#216731,
#216732,#216733,#216734,#216735,#216736,#216737,#216738,#216739,#216740,
#216741,#216742,#216743,#216744,#216745,#216746,#216747,#216748,#216749,
#216750,#216751,#216752,#216753,#216754,#216755,#216756,#216757,#216758,
#216759,#216760,#216761,#216762,#216763,#216764,#216765,#216766,#216767,
#216768,#216769,#216770,#216771,#216772,#216773,#216774,#216775,#216776,
#216777,#216778,#216779,#216780,#216781,#216782,#216783,#216784,#216785,
#216786,#216787,#216788,#216789,#216790,#216791,#216792,#216793,#216794,
#216795,#216796,#216797,#216798,#216799,#216800,#216801,#216802,#216803,
#216804,#216805,#216806,#216807,#216808,#216809,#216810,#216811,#216812,
#216813,#216814,#216815,#216816,#216817,#216818,#216819,#216820,#216821,
#216822,#216823,#216824,#216825,#216826,#216827,#216828,#216829,#216830),
 .UNSPECIFIED.,.F.,.F.)
B_SPLINE_CURVE_WITH_KNOTS((6,1,1,1,1,1,1,1,1,1,1,1,1,1,1,1,1,1,1,1,1,1,
1,1,1,1,1,1,1,1,1,1,1,1,1,1,1,1,1,1,1,1,1,1,1,1,1,1,1,1,1,1,1,1,1,1,1,1,
1,1,1,1,1,1,1,1,1,1,1,1,1,1,1,1,1,1,1,1,1,1,1,1,1,1,1,1,1,1,1,1,1,1,1,1,
1,1,1,1,1,1,1,1,1,1,1,1,1,1,1,1,1,1,1,1,1,1,1,1,1,1,1,1,1,1,1,1,1,1,1,1,
1,1,1,1,1,1,1,1,1,1,1,1,1,1,1,1,1,1,1,1,1,1,1,1,1,1,1,1,1,1,1,1,1,1,1,1,
1,1,1,1,1,1,1,1,1,1,1,1,1,1,1,1,1,1,1,1,1,1,1,1,1,1,1,1,1,1,1,1,1,1,6),
(0.,0.005,0.01,0.015,0.02,0.025,0.03,0.035,0.04,0.045,0.05,0.055,0.06,0.065,
0.07,0.075,0.08,0.085,0.09,0.095,0.1,0.105,0.11,0.115,0.12,0.125,0.13,0.135,
0.14,0.145,0.15,0.155,0.16,0.165,0.17,0.175,0.18,0.185,0.19,0.195,0.2,0.205,
0.21,0.215,0.22,0.225,0.23,0.235,0.24,0.245,0.25,0.255,0.26,0.265,0.27,
0.275,0.28,0.285,0.29,0.295,0.3,0.305,0.31,0.315,0.32,0.325,0.33,0.335,
0.34,0.345,0.35,0.355,0.36,0.365,0.37,0.375,0.38,0.385,0.39,0.395,0.4,0.405,
0.41,0.415,0.42,0.425,0.43,0.435,0.44,0.445,0.45,0.455,0.46,0.465,0.47,
0.475,0.48,0.485,0.49,0.495,0.5,0.505,0.51,0.515,0.52,0.525,0.53,0.535,
0.54,0.545,0.55,0.555,0.56,0.565,0.57,0.575,0.58,0.585,0.59,0.595,0.6,0.605,
0.61,0.615,0.62,0.625,0.63,0.635,0.64,0.645,0.65,0.655,0.66,0.665,0.67,
0.675,0.68,0.685,0.690000000000001,0.695000000000001,0.700000000000001,
0.705000000000001,0.710000000000001,0.715000000000001,0.720000000000001,
0.725000000000001,0.730000000000001,0.735000000000001,0.740000000000001,
0.745000000000001,0.750000000000001,0.755000000000001,0.760000000000001,
0.765000000000001,0.770000000000001,0.775000000000001,0.780000000000001,
0.785000000000001,0.790000000000001,0.795000000000001,0.800000000000001,
0.805000000000001,0.810000000000001,0.815000000000001,0.820000000000001,
0.825000000000001,0.830000000000001,0.835000000000001,0.840000000000001,
0.845000000000001,0.850000000000001,0.855000000000001,0.860000000000001,
0.865000000000001,0.870000000000001,0.875000000000001,0.880000000000001,
0.885000000000001,0.890000000000001,0.895000000000001,0.900000000000001,
0.905000000000001,0.910000000000001,0.915000000000001,0.920000000000001,
0.925000000000001,0.930000000000001,0.935000000000001,0.940000000000001,
0.945000000000001,0.950000000000001,0.955000000000001,0.960000000000001,
0.965000000000001,0.970000000000001,0.975000000000001,0.980000000000001,
0.985000000000001,0.990000000000001,0.995000000000001,1.),.UNSPECIFIED.)
CURVE()
GEOMETRIC_REPRESENTATION_ITEM()
RATIONAL_B_SPLINE_CURVE((1.,1.,1.,1.,1.,1.,1.,1.,1.,1.,1.,1.,1.,1.,1.,1.,
1.,1.,1.,1.,1.,1.,1.,1.,1.,1.,1.,1.,1.,1.,1.,1.,1.,1.,1.,1.,1.,1.,1.,1.,
1.,1.,1.,1.,1.,1.,1.,1.,1.,1.,1.,1.,1.,1.,1.,1.,1.,1.,1.,1.,1.,1.,1.,1.,
1.,1.,1.,1.,1.,1.,1.,1.,1.,1.,1.,1.,1.,1.,1.,1.,1.,1.,1.,1.,1.,1.,1.,1.,
1.,1.,1.,1.,1.,1.,1.,1.,1.,1.,1.,1.,1.,1.,1.,1.,1.,1.,1.,1.,1.,1.,1.,1.,
1.,1.,1.,1.,1.,1.,1.,1.,1.,1.,1.,1.,1.,1.,1.,1.,1.,1.,1.,1.,1.,1.,1.,1.,
1.,1.,1.,1.,1.,1.,1.,1.,1.,1.,1.,1.,1.,1.,1.,1.,1.,1.,1.,1.,1.,1.,1.,1.,
1.,1.,1.,1.,1.,1.,1.,1.,1.,1.,1.,1.,1.,1.,1.,1.,1.,1.,1.,1.,1.,1.,1.,1.,
1.,1.,1.,1.,1.,1.,1.,1.,1.,1.,1.,1.,1.,1.,1.,1.,1.,1.,1.,1.,1.))
REPRESENTATION_ITEM('')
);
#789=(
BOUNDED_CURVE()
B_SPLINE_CURVE(5,(#217242,#217243,#217244,#217245,#217246,#217247,#217248,
#217249,#217250,#217251,#217252,#217253,#217254,#217255,#217256,#217257,
#217258,#217259,#217260,#217261,#217262,#217263,#217264,#217265,#217266,
#217267,#217268,#217269,#217270,#217271,#217272,#217273,#217274,#217275,
#217276,#217277,#217278,#217279,#217280,#217281,#217282,#217283,#217284,
#217285,#217286,#217287,#217288,#217289,#217290,#217291,#217292,#217293,
#217294,#217295,#217296,#217297,#217298,#217299,#217300,#217301,#217302,
#217303,#217304,#217305,#217306,#217307,#217308,#217309,#217310,#217311,
#217312,#217313,#217314,#217315,#217316,#217317,#217318,#217319,#217320,
#217321,#217322,#217323,#217324,#217325,#217326,#217327,#217328,#217329,
#217330,#217331,#217332,#217333,#217334,#217335,#217336,#217337,#217338,
#217339,#217340,#217341,#217342,#217343,#217344,#217345,#217346,#217347,
#217348,#217349,#217350,#217351,#217352,#217353,#217354,#217355,#217356,
#217357,#217358,#217359,#217360,#217361,#217362,#217363,#217364,#217365,
#217366,#217367,#217368,#217369,#217370,#217371,#217372,#217373,#217374,
#217375,#217376,#217377,#217378,#217379,#217380,#217381,#217382,#217383,
#217384,#217385,#217386,#217387,#217388,#217389,#217390,#217391,#217392,
#217393,#217394,#217395,#217396,#217397,#217398,#217399,#217400,#217401,
#217402,#217403,#217404,#217405,#217406,#217407,#217408,#217409,#217410,
#217411,#217412,#217413,#217414,#217415,#217416,#217417,#217418,#217419,
#217420,#217421,#217422,#217423,#217424,#217425,#217426,#217427,#217428,
#217429,#217430,#217431,#217432,#217433,#217434,#217435,#217436,#217437,
#217438,#217439,#217440,#217441,#217442,#217443,#217444,#217445,#217446),
 .UNSPECIFIED.,.F.,.F.)
B_SPLINE_CURVE_WITH_KNOTS((6,1,1,1,1,1,1,1,1,1,1,1,1,1,1,1,1,1,1,1,1,1,
1,1,1,1,1,1,1,1,1,1,1,1,1,1,1,1,1,1,1,1,1,1,1,1,1,1,1,1,1,1,1,1,1,1,1,1,
1,1,1,1,1,1,1,1,1,1,1,1,1,1,1,1,1,1,1,1,1,1,1,1,1,1,1,1,1,1,1,1,1,1,1,1,
1,1,1,1,1,1,1,1,1,1,1,1,1,1,1,1,1,1,1,1,1,1,1,1,1,1,1,1,1,1,1,1,1,1,1,1,
1,1,1,1,1,1,1,1,1,1,1,1,1,1,1,1,1,1,1,1,1,1,1,1,1,1,1,1,1,1,1,1,1,1,1,1,
1,1,1,1,1,1,1,1,1,1,1,1,1,1,1,1,1,1,1,1,1,1,1,1,1,1,1,1,1,1,1,1,1,1,6),
(0.,0.005,0.01,0.015,0.02,0.025,0.03,0.035,0.04,0.045,0.05,0.055,0.06,0.065,
0.07,0.075,0.08,0.085,0.09,0.095,0.1,0.105,0.11,0.115,0.12,0.125,0.13,0.135,
0.14,0.145,0.15,0.155,0.16,0.165,0.17,0.175,0.18,0.185,0.19,0.195,0.2,0.205,
0.21,0.215,0.22,0.225,0.23,0.235,0.24,0.245,0.25,0.255,0.26,0.265,0.27,
0.275,0.28,0.285,0.29,0.295,0.3,0.305,0.31,0.315,0.32,0.325,0.33,0.335,
0.34,0.345,0.35,0.355,0.36,0.365,0.37,0.375,0.38,0.385,0.39,0.395,0.4,0.405,
0.41,0.415,0.42,0.425,0.43,0.435,0.44,0.445,0.45,0.455,0.46,0.465,0.47,
0.475,0.48,0.485,0.49,0.495,0.5,0.505,0.51,0.515,0.52,0.525,0.53,0.535,
0.54,0.545,0.55,0.555,0.56,0.565,0.57,0.575,0.58,0.585,0.59,0.595,0.6,0.605,
0.61,0.615,0.62,0.625,0.63,0.635,0.64,0.645,0.65,0.655,0.66,0.665,0.67,
0.675,0.68,0.685,0.690000000000001,0.695000000000001,0.700000000000001,
0.705000000000001,0.710000000000001,0.715000000000001,0.720000000000001,
0.725000000000001,0.730000000000001,0.735000000000001,0.740000000000001,
0.745000000000001,0.750000000000001,0.755000000000001,0.760000000000001,
0.765000000000001,0.770000000000001,0.775000000000001,0.780000000000001,
0.785000000000001,0.790000000000001,0.795000000000001,0.800000000000001,
0.805000000000001,0.810000000000001,0.815000000000001,0.820000000000001,
0.825000000000001,0.830000000000001,0.835000000000001,0.840000000000001,
0.845000000000001,0.850000000000001,0.855000000000001,0.860000000000001,
0.865000000000001,0.870000000000001,0.875000000000001,0.880000000000001,
0.885000000000001,0.890000000000001,0.895000000000001,0.900000000000001,
0.905000000000001,0.910000000000001,0.915000000000001,0.920000000000001,
0.925000000000001,0.930000000000001,0.935000000000001,0.940000000000001,
0.945000000000001,0.950000000000001,0.955000000000001,0.960000000000001,
0.965000000000001,0.970000000000001,0.975000000000001,0.980000000000001,
0.985000000000001,0.990000000000001,0.995000000000001,1.),.UNSPECIFIED.)
CURVE()
GEOMETRIC_REPRESENTATION_ITEM()
RATIONAL_B_SPLINE_CURVE((1.,1.,1.,1.,1.,1.,1.,1.,1.,1.,1.,1.,1.,1.,1.,1.,
1.,1.,1.,1.,1.,1.,1.,1.,1.,1.,1.,1.,1.,1.,1.,1.,1.,1.,1.,1.,1.,1.,1.,1.,
1.,1.,1.,1.,1.,1.,1.,1.,1.,1.,1.,1.,1.,1.,1.,1.,1.,1.,1.,1.,1.,1.,1.,1.,
1.,1.,1.,1.,1.,1.,1.,1.,1.,1.,1.,1.,1.,1.,1.,1.,1.,1.,1.,1.,1.,1.,1.,1.,
1.,1.,1.,1.,1.,1.,1.,1.,1.,1.,1.,1.,1.,1.,1.,1.,1.,1.,1.,1.,1.,1.,1.,1.,
1.,1.,1.,1.,1.,1.,1.,1.,1.,1.,1.,1.,1.,1.,1.,1.,1.,1.,1.,1.,1.,1.,1.,1.,
1.,1.,1.,1.,1.,1.,1.,1.,1.,1.,1.,1.,1.,1.,1.,1.,1.,1.,1.,1.,1.,1.,1.,1.,
1.,1.,1.,1.,1.,1.,1.,1.,1.,1.,1.,1.,1.,1.,1.,1.,1.,1.,1.,1.,1.,1.,1.,1.,
1.,1.,1.,1.,1.,1.,1.,1.,1.,1.,1.,1.,1.,1.,1.,1.,1.,1.,1.,1.,1.))
REPRESENTATION_ITEM('')
);
#790=(
BOUNDED_CURVE()
B_SPLINE_CURVE(5,(#217448,#217449,#217450,#217451,#217452,#217453,#217454,
#217455,#217456,#217457,#217458,#217459,#217460,#217461,#217462,#217463,
#217464,#217465,#217466,#217467,#217468,#217469,#217470,#217471,#217472,
#217473,#217474,#217475,#217476,#217477,#217478,#217479,#217480,#217481,
#217482,#217483,#217484,#217485,#217486,#217487,#217488,#217489,#217490,
#217491,#217492,#217493,#217494,#217495,#217496,#217497,#217498,#217499,
#217500,#217501,#217502,#217503,#217504,#217505,#217506,#217507,#217508,
#217509,#217510,#217511,#217512,#217513,#217514,#217515,#217516,#217517,
#217518,#217519,#217520,#217521,#217522,#217523,#217524,#217525,#217526,
#217527,#217528,#217529,#217530,#217531,#217532,#217533,#217534,#217535,
#217536,#217537,#217538,#217539,#217540,#217541,#217542,#217543,#217544,
#217545,#217546,#217547,#217548,#217549,#217550,#217551,#217552,#217553,
#217554,#217555,#217556,#217557,#217558,#217559,#217560,#217561,#217562,
#217563,#217564,#217565,#217566,#217567,#217568,#217569,#217570,#217571,
#217572,#217573,#217574,#217575,#217576,#217577,#217578,#217579,#217580,
#217581,#217582,#217583,#217584,#217585,#217586,#217587,#217588,#217589,
#217590,#217591,#217592,#217593,#217594,#217595,#217596,#217597,#217598,
#217599,#217600,#217601,#217602,#217603,#217604,#217605,#217606,#217607,
#217608,#217609,#217610,#217611,#217612,#217613,#217614,#217615,#217616,
#217617,#217618,#217619,#217620,#217621,#217622,#217623,#217624,#217625,
#217626,#217627,#217628,#217629,#217630,#217631,#217632,#217633,#217634,
#217635,#217636,#217637,#217638,#217639,#217640,#217641,#217642,#217643,
#217644,#217645,#217646,#217647,#217648,#217649,#217650,#217651,#217652),
 .UNSPECIFIED.,.F.,.F.)
B_SPLINE_CURVE_WITH_KNOTS((6,1,1,1,1,1,1,1,1,1,1,1,1,1,1,1,1,1,1,1,1,1,
1,1,1,1,1,1,1,1,1,1,1,1,1,1,1,1,1,1,1,1,1,1,1,1,1,1,1,1,1,1,1,1,1,1,1,1,
1,1,1,1,1,1,1,1,1,1,1,1,1,1,1,1,1,1,1,1,1,1,1,1,1,1,1,1,1,1,1,1,1,1,1,1,
1,1,1,1,1,1,1,1,1,1,1,1,1,1,1,1,1,1,1,1,1,1,1,1,1,1,1,1,1,1,1,1,1,1,1,1,
1,1,1,1,1,1,1,1,1,1,1,1,1,1,1,1,1,1,1,1,1,1,1,1,1,1,1,1,1,1,1,1,1,1,1,1,
1,1,1,1,1,1,1,1,1,1,1,1,1,1,1,1,1,1,1,1,1,1,1,1,1,1,1,1,1,1,1,1,1,1,6),
(-1.,-0.995000000000001,-0.990000000000001,-0.985000000000001,-0.980000000000001,
-0.975000000000001,-0.970000000000001,-0.965000000000001,-0.960000000000001,
-0.955000000000001,-0.950000000000001,-0.945000000000001,-0.940000000000001,
-0.935000000000001,-0.930000000000001,-0.925000000000001,-0.920000000000001,
-0.915000000000001,-0.910000000000001,-0.905000000000001,-0.900000000000001,
-0.895000000000001,-0.890000000000001,-0.885000000000001,-0.880000000000001,
-0.875000000000001,-0.870000000000001,-0.865000000000001,-0.860000000000001,
-0.855000000000001,-0.850000000000001,-0.845000000000001,-0.840000000000001,
-0.835000000000001,-0.830000000000001,-0.825000000000001,-0.820000000000001,
-0.815000000000001,-0.810000000000001,-0.805000000000001,-0.800000000000001,
-0.795000000000001,-0.790000000000001,-0.785000000000001,-0.780000000000001,
-0.775000000000001,-0.770000000000001,-0.765000000000001,-0.760000000000001,
-0.755000000000001,-0.750000000000001,-0.745000000000001,-0.740000000000001,
-0.735000000000001,-0.730000000000001,-0.725000000000001,-0.720000000000001,
-0.715000000000001,-0.710000000000001,-0.705000000000001,-0.700000000000001,
-0.695000000000001,-0.690000000000001,-0.685,-0.68,-0.675,-0.67,-0.665,
-0.66,-0.655,-0.65,-0.645,-0.64,-0.635,-0.63,-0.625,-0.62,-0.615,-0.61,
-0.605,-0.6,-0.595,-0.59,-0.585,-0.58,-0.575,-0.57,-0.565,-0.56,-0.555,
-0.55,-0.545,-0.54,-0.535,-0.53,-0.525,-0.52,-0.515,-0.51,-0.505,-0.5,-0.495,
-0.49,-0.485,-0.48,-0.475,-0.47,-0.465,-0.46,-0.455,-0.45,-0.445,-0.44,
-0.435,-0.43,-0.425,-0.42,-0.415,-0.41,-0.405,-0.4,-0.395,-0.39,-0.385,
-0.38,-0.375,-0.37,-0.365,-0.36,-0.355,-0.35,-0.345,-0.34,-0.335,-0.33,
-0.325,-0.32,-0.315,-0.31,-0.305,-0.3,-0.295,-0.29,-0.285,-0.28,-0.275,
-0.27,-0.265,-0.26,-0.255,-0.25,-0.245,-0.24,-0.235,-0.23,-0.225,-0.22,
-0.215,-0.21,-0.205,-0.2,-0.195,-0.19,-0.185,-0.18,-0.175,-0.17,-0.165,
-0.16,-0.155,-0.15,-0.145,-0.14,-0.135,-0.13,-0.125,-0.12,-0.115,-0.11,
-0.105,-0.1,-0.095,-0.09,-0.085,-0.08,-0.075,-0.07,-0.065,-0.06,-0.055,
-0.05,-0.045,-0.04,-0.035,-0.03,-0.025,-0.02,-0.015,-0.01,-0.005,0.),
 .UNSPECIFIED.)
CURVE()
GEOMETRIC_REPRESENTATION_ITEM()
RATIONAL_B_SPLINE_CURVE((1.,1.,1.,1.,1.,1.,1.,1.,1.,1.,1.,1.,1.,1.,1.,1.,
1.,1.,1.,1.,1.,1.,1.,1.,1.,1.,1.,1.,1.,1.,1.,1.,1.,1.,1.,1.,1.,1.,1.,1.,
1.,1.,1.,1.,1.,1.,1.,1.,1.,1.,1.,1.,1.,1.,1.,1.,1.,1.,1.,1.,1.,1.,1.,1.,
1.,1.,1.,1.,1.,1.,1.,1.,1.,1.,1.,1.,1.,1.,1.,1.,1.,1.,1.,1.,1.,1.,1.,1.,
1.,1.,1.,1.,1.,1.,1.,1.,1.,1.,1.,1.,1.,1.,1.,1.,1.,1.,1.,1.,1.,1.,1.,1.,
1.,1.,1.,1.,1.,1.,1.,1.,1.,1.,1.,1.,1.,1.,1.,1.,1.,1.,1.,1.,1.,1.,1.,1.,
1.,1.,1.,1.,1.,1.,1.,1.,1.,1.,1.,1.,1.,1.,1.,1.,1.,1.,1.,1.,1.,1.,1.,1.,
1.,1.,1.,1.,1.,1.,1.,1.,1.,1.,1.,1.,1.,1.,1.,1.,1.,1.,1.,1.,1.,1.,1.,1.,
1.,1.,1.,1.,1.,1.,1.,1.,1.,1.,1.,1.,1.,1.,1.,1.,1.,1.,1.,1.,1.))
REPRESENTATION_ITEM('')
);
#791=(
BOUNDED_CURVE()
B_SPLINE_CURVE(5,(#218071,#218072,#218073,#218074,#218075,#218076,#218077,
#218078,#218079,#218080,#218081,#218082,#218083,#218084,#218085,#218086,
#218087,#218088,#218089,#218090,#218091,#218092,#218093,#218094,#218095,
#218096,#218097,#218098,#218099,#218100,#218101,#218102,#218103,#218104,
#218105,#218106,#218107,#218108,#218109,#218110,#218111,#218112,#218113,
#218114,#218115,#218116,#218117,#218118,#218119,#218120,#218121,#218122,
#218123,#218124,#218125,#218126,#218127,#218128,#218129,#218130,#218131,
#218132,#218133,#218134,#218135,#218136,#218137,#218138,#218139,#218140,
#218141,#218142,#218143,#218144,#218145,#218146,#218147,#218148,#218149,
#218150,#218151,#218152,#218153,#218154,#218155,#218156,#218157,#218158,
#218159,#218160,#218161,#218162,#218163,#218164,#218165,#218166,#218167,
#218168,#218169,#218170,#218171,#218172,#218173,#218174,#218175,#218176,
#218177,#218178,#218179,#218180,#218181,#218182,#218183,#218184,#218185,
#218186,#218187,#218188,#218189,#218190,#218191,#218192,#218193,#218194,
#218195,#218196,#218197,#218198,#218199,#218200,#218201,#218202,#218203,
#218204,#218205,#218206,#218207,#218208,#218209,#218210,#218211,#218212,
#218213,#218214,#218215,#218216,#218217,#218218,#218219,#218220,#218221,
#218222,#218223,#218224,#218225,#218226,#218227,#218228,#218229,#218230,
#218231,#218232,#218233,#218234,#218235,#218236,#218237,#218238,#218239,
#218240,#218241,#218242,#218243,#218244,#218245,#218246,#218247,#218248,
#218249,#218250,#218251,#218252,#218253,#218254,#218255,#218256,#218257,
#218258,#218259,#218260,#218261,#218262,#218263,#218264,#218265,#218266,
#218267,#218268,#218269,#218270,#218271,#218272,#218273,#218274,#218275),
 .UNSPECIFIED.,.F.,.F.)
B_SPLINE_CURVE_WITH_KNOTS((6,1,1,1,1,1,1,1,1,1,1,1,1,1,1,1,1,1,1,1,1,1,
1,1,1,1,1,1,1,1,1,1,1,1,1,1,1,1,1,1,1,1,1,1,1,1,1,1,1,1,1,1,1,1,1,1,1,1,
1,1,1,1,1,1,1,1,1,1,1,1,1,1,1,1,1,1,1,1,1,1,1,1,1,1,1,1,1,1,1,1,1,1,1,1,
1,1,1,1,1,1,1,1,1,1,1,1,1,1,1,1,1,1,1,1,1,1,1,1,1,1,1,1,1,1,1,1,1,1,1,1,
1,1,1,1,1,1,1,1,1,1,1,1,1,1,1,1,1,1,1,1,1,1,1,1,1,1,1,1,1,1,1,1,1,1,1,1,
1,1,1,1,1,1,1,1,1,1,1,1,1,1,1,1,1,1,1,1,1,1,1,1,1,1,1,1,1,1,1,1,1,1,6),
(-1.,-0.995000000000001,-0.990000000000001,-0.985000000000001,-0.980000000000001,
-0.975000000000001,-0.970000000000001,-0.965000000000001,-0.960000000000001,
-0.955000000000001,-0.950000000000001,-0.945000000000001,-0.940000000000001,
-0.935000000000001,-0.930000000000001,-0.925000000000001,-0.920000000000001,
-0.915000000000001,-0.910000000000001,-0.905000000000001,-0.900000000000001,
-0.895000000000001,-0.890000000000001,-0.885000000000001,-0.880000000000001,
-0.875000000000001,-0.870000000000001,-0.865000000000001,-0.860000000000001,
-0.855000000000001,-0.850000000000001,-0.845000000000001,-0.840000000000001,
-0.835000000000001,-0.830000000000001,-0.825000000000001,-0.820000000000001,
-0.815000000000001,-0.810000000000001,-0.805000000000001,-0.800000000000001,
-0.795000000000001,-0.790000000000001,-0.785000000000001,-0.780000000000001,
-0.775000000000001,-0.770000000000001,-0.765000000000001,-0.760000000000001,
-0.755000000000001,-0.750000000000001,-0.745000000000001,-0.740000000000001,
-0.735000000000001,-0.730000000000001,-0.725000000000001,-0.720000000000001,
-0.715000000000001,-0.710000000000001,-0.705000000000001,-0.700000000000001,
-0.695000000000001,-0.690000000000001,-0.685,-0.68,-0.675,-0.67,-0.665,
-0.66,-0.655,-0.65,-0.645,-0.64,-0.635,-0.63,-0.625,-0.62,-0.615,-0.61,
-0.605,-0.6,-0.595,-0.59,-0.585,-0.58,-0.575,-0.57,-0.565,-0.56,-0.555,
-0.55,-0.545,-0.54,-0.535,-0.53,-0.525,-0.52,-0.515,-0.51,-0.505,-0.5,-0.495,
-0.49,-0.485,-0.48,-0.475,-0.47,-0.465,-0.46,-0.455,-0.45,-0.445,-0.44,
-0.435,-0.43,-0.425,-0.42,-0.415,-0.41,-0.405,-0.4,-0.395,-0.39,-0.385,
-0.38,-0.375,-0.37,-0.365,-0.36,-0.355,-0.35,-0.345,-0.34,-0.335,-0.33,
-0.325,-0.32,-0.315,-0.31,-0.305,-0.3,-0.295,-0.29,-0.285,-0.28,-0.275,
-0.27,-0.265,-0.26,-0.255,-0.25,-0.245,-0.24,-0.235,-0.23,-0.225,-0.22,
-0.215,-0.21,-0.205,-0.2,-0.195,-0.19,-0.185,-0.18,-0.175,-0.17,-0.165,
-0.16,-0.155,-0.15,-0.145,-0.14,-0.135,-0.13,-0.125,-0.12,-0.115,-0.11,
-0.105,-0.1,-0.095,-0.09,-0.085,-0.08,-0.075,-0.07,-0.065,-0.06,-0.055,
-0.05,-0.045,-0.04,-0.035,-0.03,-0.025,-0.02,-0.015,-0.01,-0.005,0.),
 .UNSPECIFIED.)
CURVE()
GEOMETRIC_REPRESENTATION_ITEM()
RATIONAL_B_SPLINE_CURVE((1.,1.,1.,1.,1.,1.,1.,1.,1.,1.,1.,1.,1.,1.,1.,1.,
1.,1.,1.,1.,1.,1.,1.,1.,1.,1.,1.,1.,1.,1.,1.,1.,1.,1.,1.,1.,1.,1.,1.,1.,
1.,1.,1.,1.,1.,1.,1.,1.,1.,1.,1.,1.,1.,1.,1.,1.,1.,1.,1.,1.,1.,1.,1.,1.,
1.,1.,1.,1.,1.,1.,1.,1.,1.,1.,1.,1.,1.,1.,1.,1.,1.,1.,1.,1.,1.,1.,1.,1.,
1.,1.,1.,1.,1.,1.,1.,1.,1.,1.,1.,1.,1.,1.,1.,1.,1.,1.,1.,1.,1.,1.,1.,1.,
1.,1.,1.,1.,1.,1.,1.,1.,1.,1.,1.,1.,1.,1.,1.,1.,1.,1.,1.,1.,1.,1.,1.,1.,
1.,1.,1.,1.,1.,1.,1.,1.,1.,1.,1.,1.,1.,1.,1.,1.,1.,1.,1.,1.,1.,1.,1.,1.,
1.,1.,1.,1.,1.,1.,1.,1.,1.,1.,1.,1.,1.,1.,1.,1.,1.,1.,1.,1.,1.,1.,1.,1.,
1.,1.,1.,1.,1.,1.,1.,1.,1.,1.,1.,1.,1.,1.,1.,1.,1.,1.,1.,1.,1.))
REPRESENTATION_ITEM('')
);
#792=(
BOUNDED_CURVE()
B_SPLINE_CURVE(5,(#218278,#218279,#218280,#218281,#218282,#218283,#218284,
#218285,#218286,#218287,#218288,#218289,#218290,#218291,#218292,#218293,
#218294,#218295,#218296,#218297,#218298,#218299,#218300,#218301,#218302,
#218303,#218304,#218305,#218306,#218307,#218308,#218309,#218310,#218311,
#218312,#218313,#218314,#218315,#218316,#218317,#218318,#218319,#218320,
#218321,#218322,#218323,#218324,#218325,#218326,#218327,#218328,#218329,
#218330,#218331,#218332,#218333,#218334,#218335,#218336,#218337,#218338,
#218339,#218340,#218341,#218342,#218343,#218344,#218345,#218346,#218347,
#218348,#218349,#218350,#218351,#218352,#218353,#218354,#218355,#218356,
#218357,#218358,#218359,#218360,#218361,#218362,#218363,#218364,#218365,
#218366,#218367,#218368,#218369,#218370,#218371,#218372,#218373,#218374,
#218375,#218376,#218377,#218378,#218379,#218380,#218381,#218382,#218383,
#218384,#218385,#218386,#218387,#218388,#218389,#218390,#218391,#218392,
#218393,#218394,#218395,#218396,#218397,#218398,#218399,#218400,#218401,
#218402,#218403,#218404,#218405,#218406,#218407,#218408,#218409,#218410,
#218411,#218412,#218413,#218414,#218415,#218416,#218417,#218418,#218419,
#218420,#218421,#218422,#218423,#218424,#218425,#218426,#218427,#218428,
#218429,#218430,#218431,#218432,#218433,#218434,#218435,#218436,#218437,
#218438,#218439,#218440,#218441,#218442,#218443,#218444,#218445,#218446,
#218447,#218448,#218449,#218450,#218451,#218452,#218453,#218454,#218455,
#218456,#218457,#218458,#218459,#218460,#218461,#218462,#218463,#218464,
#218465,#218466,#218467,#218468,#218469,#218470,#218471,#218472,#218473,
#218474,#218475,#218476,#218477,#218478,#218479,#218480,#218481,#218482),
 .UNSPECIFIED.,.F.,.F.)
B_SPLINE_CURVE_WITH_KNOTS((6,1,1,1,1,1,1,1,1,1,1,1,1,1,1,1,1,1,1,1,1,1,
1,1,1,1,1,1,1,1,1,1,1,1,1,1,1,1,1,1,1,1,1,1,1,1,1,1,1,1,1,1,1,1,1,1,1,1,
1,1,1,1,1,1,1,1,1,1,1,1,1,1,1,1,1,1,1,1,1,1,1,1,1,1,1,1,1,1,1,1,1,1,1,1,
1,1,1,1,1,1,1,1,1,1,1,1,1,1,1,1,1,1,1,1,1,1,1,1,1,1,1,1,1,1,1,1,1,1,1,1,
1,1,1,1,1,1,1,1,1,1,1,1,1,1,1,1,1,1,1,1,1,1,1,1,1,1,1,1,1,1,1,1,1,1,1,1,
1,1,1,1,1,1,1,1,1,1,1,1,1,1,1,1,1,1,1,1,1,1,1,1,1,1,1,1,1,1,1,1,1,1,6),
(0.,0.005,0.01,0.015,0.02,0.025,0.03,0.035,0.04,0.045,0.05,0.055,0.06,0.065,
0.07,0.075,0.08,0.085,0.09,0.095,0.1,0.105,0.11,0.115,0.12,0.125,0.13,0.135,
0.14,0.145,0.15,0.155,0.16,0.165,0.17,0.175,0.18,0.185,0.19,0.195,0.2,0.205,
0.21,0.215,0.22,0.225,0.23,0.235,0.24,0.245,0.25,0.255,0.26,0.265,0.27,
0.275,0.28,0.285,0.29,0.295,0.3,0.305,0.31,0.315,0.32,0.325,0.33,0.335,
0.34,0.345,0.35,0.355,0.36,0.365,0.37,0.375,0.38,0.385,0.39,0.395,0.4,0.405,
0.41,0.415,0.42,0.425,0.43,0.435,0.44,0.445,0.45,0.455,0.46,0.465,0.47,
0.475,0.48,0.485,0.49,0.495,0.5,0.505,0.51,0.515,0.52,0.525,0.53,0.535,
0.54,0.545,0.55,0.555,0.56,0.565,0.57,0.575,0.58,0.585,0.59,0.595,0.6,0.605,
0.61,0.615,0.62,0.625,0.63,0.635,0.64,0.645,0.65,0.655,0.66,0.665,0.67,
0.675,0.68,0.685,0.690000000000001,0.695000000000001,0.700000000000001,
0.705000000000001,0.710000000000001,0.715000000000001,0.720000000000001,
0.725000000000001,0.730000000000001,0.735000000000001,0.740000000000001,
0.745000000000001,0.750000000000001,0.755000000000001,0.760000000000001,
0.765000000000001,0.770000000000001,0.775000000000001,0.780000000000001,
0.785000000000001,0.790000000000001,0.795000000000001,0.800000000000001,
0.805000000000001,0.810000000000001,0.815000000000001,0.820000000000001,
0.825000000000001,0.830000000000001,0.835000000000001,0.840000000000001,
0.845000000000001,0.850000000000001,0.855000000000001,0.860000000000001,
0.865000000000001,0.870000000000001,0.875000000000001,0.880000000000001,
0.885000000000001,0.890000000000001,0.895000000000001,0.900000000000001,
0.905000000000001,0.910000000000001,0.915000000000001,0.920000000000001,
0.925000000000001,0.930000000000001,0.935000000000001,0.940000000000001,
0.945000000000001,0.950000000000001,0.955000000000001,0.960000000000001,
0.965000000000001,0.970000000000001,0.975000000000001,0.980000000000001,
0.985000000000001,0.990000000000001,0.995000000000001,1.),.UNSPECIFIED.)
CURVE()
GEOMETRIC_REPRESENTATION_ITEM()
RATIONAL_B_SPLINE_CURVE((1.,1.,1.,1.,1.,1.,1.,1.,1.,1.,1.,1.,1.,1.,1.,1.,
1.,1.,1.,1.,1.,1.,1.,1.,1.,1.,1.,1.,1.,1.,1.,1.,1.,1.,1.,1.,1.,1.,1.,1.,
1.,1.,1.,1.,1.,1.,1.,1.,1.,1.,1.,1.,1.,1.,1.,1.,1.,1.,1.,1.,1.,1.,1.,1.,
1.,1.,1.,1.,1.,1.,1.,1.,1.,1.,1.,1.,1.,1.,1.,1.,1.,1.,1.,1.,1.,1.,1.,1.,
1.,1.,1.,1.,1.,1.,1.,1.,1.,1.,1.,1.,1.,1.,1.,1.,1.,1.,1.,1.,1.,1.,1.,1.,
1.,1.,1.,1.,1.,1.,1.,1.,1.,1.,1.,1.,1.,1.,1.,1.,1.,1.,1.,1.,1.,1.,1.,1.,
1.,1.,1.,1.,1.,1.,1.,1.,1.,1.,1.,1.,1.,1.,1.,1.,1.,1.,1.,1.,1.,1.,1.,1.,
1.,1.,1.,1.,1.,1.,1.,1.,1.,1.,1.,1.,1.,1.,1.,1.,1.,1.,1.,1.,1.,1.,1.,1.,
1.,1.,1.,1.,1.,1.,1.,1.,1.,1.,1.,1.,1.,1.,1.,1.,1.,1.,1.,1.,1.))
REPRESENTATION_ITEM('')
);
#793=(
BOUNDED_CURVE()
B_SPLINE_CURVE(5,(#218894,#218895,#218896,#218897,#218898,#218899,#218900,
#218901,#218902,#218903,#218904,#218905,#218906,#218907,#218908,#218909,
#218910,#218911,#218912,#218913,#218914,#218915,#218916,#218917,#218918,
#218919,#218920,#218921,#218922,#218923,#218924,#218925,#218926,#218927,
#218928,#218929,#218930,#218931,#218932,#218933,#218934,#218935,#218936,
#218937,#218938,#218939,#218940,#218941,#218942,#218943,#218944,#218945,
#218946,#218947,#218948,#218949,#218950,#218951,#218952,#218953,#218954,
#218955,#218956,#218957,#218958,#218959,#218960,#218961,#218962,#218963,
#218964,#218965,#218966,#218967,#218968,#218969,#218970,#218971,#218972,
#218973,#218974,#218975,#218976,#218977,#218978,#218979,#218980,#218981,
#218982,#218983,#218984,#218985,#218986,#218987,#218988,#218989,#218990,
#218991,#218992,#218993,#218994,#218995,#218996,#218997,#218998,#218999,
#219000,#219001,#219002,#219003,#219004,#219005,#219006,#219007,#219008,
#219009,#219010,#219011,#219012,#219013,#219014,#219015,#219016,#219017,
#219018,#219019,#219020,#219021,#219022,#219023,#219024,#219025,#219026,
#219027,#219028,#219029,#219030,#219031,#219032,#219033,#219034,#219035,
#219036,#219037,#219038,#219039,#219040,#219041,#219042,#219043,#219044,
#219045,#219046,#219047,#219048,#219049,#219050,#219051,#219052,#219053,
#219054,#219055,#219056,#219057,#219058,#219059,#219060,#219061,#219062,
#219063,#219064,#219065,#219066,#219067,#219068,#219069,#219070,#219071,
#219072,#219073,#219074,#219075,#219076,#219077,#219078,#219079,#219080,
#219081,#219082,#219083,#219084,#219085,#219086,#219087,#219088,#219089,
#219090,#219091,#219092,#219093,#219094,#219095,#219096,#219097,#219098),
 .UNSPECIFIED.,.F.,.F.)
B_SPLINE_CURVE_WITH_KNOTS((6,1,1,1,1,1,1,1,1,1,1,1,1,1,1,1,1,1,1,1,1,1,
1,1,1,1,1,1,1,1,1,1,1,1,1,1,1,1,1,1,1,1,1,1,1,1,1,1,1,1,1,1,1,1,1,1,1,1,
1,1,1,1,1,1,1,1,1,1,1,1,1,1,1,1,1,1,1,1,1,1,1,1,1,1,1,1,1,1,1,1,1,1,1,1,
1,1,1,1,1,1,1,1,1,1,1,1,1,1,1,1,1,1,1,1,1,1,1,1,1,1,1,1,1,1,1,1,1,1,1,1,
1,1,1,1,1,1,1,1,1,1,1,1,1,1,1,1,1,1,1,1,1,1,1,1,1,1,1,1,1,1,1,1,1,1,1,1,
1,1,1,1,1,1,1,1,1,1,1,1,1,1,1,1,1,1,1,1,1,1,1,1,1,1,1,1,1,1,1,1,1,1,6),
(0.,0.005,0.01,0.015,0.02,0.025,0.03,0.035,0.04,0.045,0.05,0.055,0.06,0.065,
0.07,0.075,0.08,0.085,0.09,0.095,0.1,0.105,0.11,0.115,0.12,0.125,0.13,0.135,
0.14,0.145,0.15,0.155,0.16,0.165,0.17,0.175,0.18,0.185,0.19,0.195,0.2,0.205,
0.21,0.215,0.22,0.225,0.23,0.235,0.24,0.245,0.25,0.255,0.26,0.265,0.27,
0.275,0.28,0.285,0.29,0.295,0.3,0.305,0.31,0.315,0.32,0.325,0.33,0.335,
0.34,0.345,0.35,0.355,0.36,0.365,0.37,0.375,0.38,0.385,0.39,0.395,0.4,0.405,
0.41,0.415,0.42,0.425,0.43,0.435,0.44,0.445,0.45,0.455,0.46,0.465,0.47,
0.475,0.48,0.485,0.49,0.495,0.5,0.505,0.51,0.515,0.52,0.525,0.53,0.535,
0.54,0.545,0.55,0.555,0.56,0.565,0.57,0.575,0.58,0.585,0.59,0.595,0.6,0.605,
0.61,0.615,0.62,0.625,0.63,0.635,0.64,0.645,0.65,0.655,0.66,0.665,0.67,
0.675,0.68,0.685,0.690000000000001,0.695000000000001,0.700000000000001,
0.705000000000001,0.710000000000001,0.715000000000001,0.720000000000001,
0.725000000000001,0.730000000000001,0.735000000000001,0.740000000000001,
0.745000000000001,0.750000000000001,0.755000000000001,0.760000000000001,
0.765000000000001,0.770000000000001,0.775000000000001,0.780000000000001,
0.785000000000001,0.790000000000001,0.795000000000001,0.800000000000001,
0.805000000000001,0.810000000000001,0.815000000000001,0.820000000000001,
0.825000000000001,0.830000000000001,0.835000000000001,0.840000000000001,
0.845000000000001,0.850000000000001,0.855000000000001,0.860000000000001,
0.865000000000001,0.870000000000001,0.875000000000001,0.880000000000001,
0.885000000000001,0.890000000000001,0.895000000000001,0.900000000000001,
0.905000000000001,0.910000000000001,0.915000000000001,0.920000000000001,
0.925000000000001,0.930000000000001,0.935000000000001,0.940000000000001,
0.945000000000001,0.950000000000001,0.955000000000001,0.960000000000001,
0.965000000000001,0.970000000000001,0.975000000000001,0.980000000000001,
0.985000000000001,0.990000000000001,0.995000000000001,1.),.UNSPECIFIED.)
CURVE()
GEOMETRIC_REPRESENTATION_ITEM()
RATIONAL_B_SPLINE_CURVE((1.,1.,1.,1.,1.,1.,1.,1.,1.,1.,1.,1.,1.,1.,1.,1.,
1.,1.,1.,1.,1.,1.,1.,1.,1.,1.,1.,1.,1.,1.,1.,1.,1.,1.,1.,1.,1.,1.,1.,1.,
1.,1.,1.,1.,1.,1.,1.,1.,1.,1.,1.,1.,1.,1.,1.,1.,1.,1.,1.,1.,1.,1.,1.,1.,
1.,1.,1.,1.,1.,1.,1.,1.,1.,1.,1.,1.,1.,1.,1.,1.,1.,1.,1.,1.,1.,1.,1.,1.,
1.,1.,1.,1.,1.,1.,1.,1.,1.,1.,1.,1.,1.,1.,1.,1.,1.,1.,1.,1.,1.,1.,1.,1.,
1.,1.,1.,1.,1.,1.,1.,1.,1.,1.,1.,1.,1.,1.,1.,1.,1.,1.,1.,1.,1.,1.,1.,1.,
1.,1.,1.,1.,1.,1.,1.,1.,1.,1.,1.,1.,1.,1.,1.,1.,1.,1.,1.,1.,1.,1.,1.,1.,
1.,1.,1.,1.,1.,1.,1.,1.,1.,1.,1.,1.,1.,1.,1.,1.,1.,1.,1.,1.,1.,1.,1.,1.,
1.,1.,1.,1.,1.,1.,1.,1.,1.,1.,1.,1.,1.,1.,1.,1.,1.,1.,1.,1.,1.))
REPRESENTATION_ITEM('')
);
#794=(
BOUNDED_CURVE()
B_SPLINE_CURVE(5,(#219100,#219101,#219102,#219103,#219104,#219105,#219106,
#219107,#219108,#219109,#219110,#219111,#219112,#219113,#219114,#219115,
#219116,#219117,#219118,#219119,#219120,#219121,#219122,#219123,#219124,
#219125,#219126,#219127,#219128,#219129,#219130,#219131,#219132,#219133,
#219134,#219135,#219136,#219137,#219138,#219139,#219140,#219141,#219142,
#219143,#219144,#219145,#219146,#219147,#219148,#219149,#219150,#219151,
#219152,#219153,#219154,#219155,#219156,#219157,#219158,#219159,#219160,
#219161,#219162,#219163,#219164,#219165,#219166,#219167,#219168,#219169,
#219170,#219171,#219172,#219173,#219174,#219175,#219176,#219177,#219178,
#219179,#219180,#219181,#219182,#219183,#219184,#219185,#219186,#219187,
#219188,#219189,#219190,#219191,#219192,#219193,#219194,#219195,#219196,
#219197,#219198,#219199,#219200,#219201,#219202,#219203,#219204,#219205,
#219206,#219207,#219208,#219209,#219210,#219211,#219212,#219213,#219214,
#219215,#219216,#219217,#219218,#219219,#219220,#219221,#219222,#219223,
#219224,#219225,#219226,#219227,#219228,#219229,#219230,#219231,#219232,
#219233,#219234,#219235,#219236,#219237,#219238,#219239,#219240,#219241,
#219242,#219243,#219244,#219245,#219246,#219247,#219248,#219249,#219250,
#219251,#219252,#219253,#219254,#219255,#219256,#219257,#219258,#219259,
#219260,#219261,#219262,#219263,#219264,#219265,#219266,#219267,#219268,
#219269,#219270,#219271,#219272,#219273,#219274,#219275,#219276,#219277,
#219278,#219279,#219280,#219281,#219282,#219283,#219284,#219285,#219286,
#219287,#219288,#219289,#219290,#219291,#219292,#219293,#219294,#219295,
#219296,#219297,#219298,#219299,#219300,#219301,#219302,#219303,#219304),
 .UNSPECIFIED.,.F.,.F.)
B_SPLINE_CURVE_WITH_KNOTS((6,1,1,1,1,1,1,1,1,1,1,1,1,1,1,1,1,1,1,1,1,1,
1,1,1,1,1,1,1,1,1,1,1,1,1,1,1,1,1,1,1,1,1,1,1,1,1,1,1,1,1,1,1,1,1,1,1,1,
1,1,1,1,1,1,1,1,1,1,1,1,1,1,1,1,1,1,1,1,1,1,1,1,1,1,1,1,1,1,1,1,1,1,1,1,
1,1,1,1,1,1,1,1,1,1,1,1,1,1,1,1,1,1,1,1,1,1,1,1,1,1,1,1,1,1,1,1,1,1,1,1,
1,1,1,1,1,1,1,1,1,1,1,1,1,1,1,1,1,1,1,1,1,1,1,1,1,1,1,1,1,1,1,1,1,1,1,1,
1,1,1,1,1,1,1,1,1,1,1,1,1,1,1,1,1,1,1,1,1,1,1,1,1,1,1,1,1,1,1,1,1,1,6),
(-1.,-0.995000000000001,-0.990000000000001,-0.985000000000001,-0.980000000000001,
-0.975000000000001,-0.970000000000001,-0.965000000000001,-0.960000000000001,
-0.955000000000001,-0.950000000000001,-0.945000000000001,-0.940000000000001,
-0.935000000000001,-0.930000000000001,-0.925000000000001,-0.920000000000001,
-0.915000000000001,-0.910000000000001,-0.905000000000001,-0.900000000000001,
-0.895000000000001,-0.890000000000001,-0.885000000000001,-0.880000000000001,
-0.875000000000001,-0.870000000000001,-0.865000000000001,-0.860000000000001,
-0.855000000000001,-0.850000000000001,-0.845000000000001,-0.840000000000001,
-0.835000000000001,-0.830000000000001,-0.825000000000001,-0.820000000000001,
-0.815000000000001,-0.810000000000001,-0.805000000000001,-0.800000000000001,
-0.795000000000001,-0.790000000000001,-0.785000000000001,-0.780000000000001,
-0.775000000000001,-0.770000000000001,-0.765000000000001,-0.760000000000001,
-0.755000000000001,-0.750000000000001,-0.745000000000001,-0.740000000000001,
-0.735000000000001,-0.730000000000001,-0.725000000000001,-0.720000000000001,
-0.715000000000001,-0.710000000000001,-0.705000000000001,-0.700000000000001,
-0.695000000000001,-0.690000000000001,-0.685,-0.68,-0.675,-0.67,-0.665,
-0.66,-0.655,-0.65,-0.645,-0.64,-0.635,-0.63,-0.625,-0.62,-0.615,-0.61,
-0.605,-0.6,-0.595,-0.59,-0.585,-0.58,-0.575,-0.57,-0.565,-0.56,-0.555,
-0.55,-0.545,-0.54,-0.535,-0.53,-0.525,-0.52,-0.515,-0.51,-0.505,-0.5,-0.495,
-0.49,-0.485,-0.48,-0.475,-0.47,-0.465,-0.46,-0.455,-0.45,-0.445,-0.44,
-0.435,-0.43,-0.425,-0.42,-0.415,-0.41,-0.405,-0.4,-0.395,-0.39,-0.385,
-0.38,-0.375,-0.37,-0.365,-0.36,-0.355,-0.35,-0.345,-0.34,-0.335,-0.33,
-0.325,-0.32,-0.315,-0.31,-0.305,-0.3,-0.295,-0.29,-0.285,-0.28,-0.275,
-0.27,-0.265,-0.26,-0.255,-0.25,-0.245,-0.24,-0.235,-0.23,-0.225,-0.22,
-0.215,-0.21,-0.205,-0.2,-0.195,-0.19,-0.185,-0.18,-0.175,-0.17,-0.165,
-0.16,-0.155,-0.15,-0.145,-0.14,-0.135,-0.13,-0.125,-0.12,-0.115,-0.11,
-0.105,-0.1,-0.095,-0.09,-0.085,-0.08,-0.075,-0.07,-0.065,-0.06,-0.055,
-0.05,-0.045,-0.04,-0.035,-0.03,-0.025,-0.02,-0.015,-0.01,-0.005,0.),
 .UNSPECIFIED.)
CURVE()
GEOMETRIC_REPRESENTATION_ITEM()
RATIONAL_B_SPLINE_CURVE((1.,1.,1.,1.,1.,1.,1.,1.,1.,1.,1.,1.,1.,1.,1.,1.,
1.,1.,1.,1.,1.,1.,1.,1.,1.,1.,1.,1.,1.,1.,1.,1.,1.,1.,1.,1.,1.,1.,1.,1.,
1.,1.,1.,1.,1.,1.,1.,1.,1.,1.,1.,1.,1.,1.,1.,1.,1.,1.,1.,1.,1.,1.,1.,1.,
1.,1.,1.,1.,1.,1.,1.,1.,1.,1.,1.,1.,1.,1.,1.,1.,1.,1.,1.,1.,1.,1.,1.,1.,
1.,1.,1.,1.,1.,1.,1.,1.,1.,1.,1.,1.,1.,1.,1.,1.,1.,1.,1.,1.,1.,1.,1.,1.,
1.,1.,1.,1.,1.,1.,1.,1.,1.,1.,1.,1.,1.,1.,1.,1.,1.,1.,1.,1.,1.,1.,1.,1.,
1.,1.,1.,1.,1.,1.,1.,1.,1.,1.,1.,1.,1.,1.,1.,1.,1.,1.,1.,1.,1.,1.,1.,1.,
1.,1.,1.,1.,1.,1.,1.,1.,1.,1.,1.,1.,1.,1.,1.,1.,1.,1.,1.,1.,1.,1.,1.,1.,
1.,1.,1.,1.,1.,1.,1.,1.,1.,1.,1.,1.,1.,1.,1.,1.,1.,1.,1.,1.,1.))
REPRESENTATION_ITEM('')
);
#795=(
BOUNDED_CURVE()
B_SPLINE_CURVE(5,(#219723,#219724,#219725,#219726,#219727,#219728,#219729,
#219730,#219731,#219732,#219733,#219734,#219735,#219736,#219737,#219738,
#219739,#219740,#219741,#219742,#219743,#219744,#219745,#219746,#219747,
#219748,#219749,#219750,#219751,#219752,#219753,#219754,#219755,#219756,
#219757,#219758,#219759,#219760,#219761,#219762,#219763,#219764,#219765,
#219766,#219767,#219768,#219769,#219770,#219771,#219772,#219773,#219774,
#219775,#219776,#219777,#219778,#219779,#219780,#219781,#219782,#219783,
#219784,#219785,#219786,#219787,#219788,#219789,#219790,#219791,#219792,
#219793,#219794,#219795,#219796,#219797,#219798,#219799,#219800,#219801,
#219802,#219803,#219804,#219805,#219806,#219807,#219808,#219809,#219810,
#219811,#219812,#219813,#219814,#219815,#219816,#219817,#219818,#219819,
#219820,#219821,#219822,#219823,#219824,#219825,#219826,#219827,#219828,
#219829,#219830,#219831,#219832,#219833,#219834,#219835,#219836,#219837,
#219838,#219839,#219840,#219841,#219842,#219843,#219844,#219845,#219846,
#219847,#219848,#219849,#219850,#219851,#219852,#219853,#219854,#219855,
#219856,#219857,#219858,#219859,#219860,#219861,#219862,#219863,#219864,
#219865,#219866,#219867,#219868,#219869,#219870,#219871,#219872,#219873,
#219874,#219875,#219876,#219877,#219878,#219879,#219880,#219881,#219882,
#219883,#219884,#219885,#219886,#219887,#219888,#219889,#219890,#219891,
#219892,#219893,#219894,#219895,#219896,#219897,#219898,#219899,#219900,
#219901,#219902,#219903,#219904,#219905,#219906,#219907,#219908,#219909,
#219910,#219911,#219912,#219913,#219914,#219915,#219916,#219917,#219918,
#219919,#219920,#219921,#219922,#219923,#219924,#219925,#219926,#219927),
 .UNSPECIFIED.,.F.,.F.)
B_SPLINE_CURVE_WITH_KNOTS((6,1,1,1,1,1,1,1,1,1,1,1,1,1,1,1,1,1,1,1,1,1,
1,1,1,1,1,1,1,1,1,1,1,1,1,1,1,1,1,1,1,1,1,1,1,1,1,1,1,1,1,1,1,1,1,1,1,1,
1,1,1,1,1,1,1,1,1,1,1,1,1,1,1,1,1,1,1,1,1,1,1,1,1,1,1,1,1,1,1,1,1,1,1,1,
1,1,1,1,1,1,1,1,1,1,1,1,1,1,1,1,1,1,1,1,1,1,1,1,1,1,1,1,1,1,1,1,1,1,1,1,
1,1,1,1,1,1,1,1,1,1,1,1,1,1,1,1,1,1,1,1,1,1,1,1,1,1,1,1,1,1,1,1,1,1,1,1,
1,1,1,1,1,1,1,1,1,1,1,1,1,1,1,1,1,1,1,1,1,1,1,1,1,1,1,1,1,1,1,1,1,1,6),
(-1.,-0.995000000000001,-0.990000000000001,-0.985000000000001,-0.980000000000001,
-0.975000000000001,-0.970000000000001,-0.965000000000001,-0.960000000000001,
-0.955000000000001,-0.950000000000001,-0.945000000000001,-0.940000000000001,
-0.935000000000001,-0.930000000000001,-0.925000000000001,-0.920000000000001,
-0.915000000000001,-0.910000000000001,-0.905000000000001,-0.900000000000001,
-0.895000000000001,-0.890000000000001,-0.885000000000001,-0.880000000000001,
-0.875000000000001,-0.870000000000001,-0.865000000000001,-0.860000000000001,
-0.855000000000001,-0.850000000000001,-0.845000000000001,-0.840000000000001,
-0.835000000000001,-0.830000000000001,-0.825000000000001,-0.820000000000001,
-0.815000000000001,-0.810000000000001,-0.805000000000001,-0.800000000000001,
-0.795000000000001,-0.790000000000001,-0.785000000000001,-0.780000000000001,
-0.775000000000001,-0.770000000000001,-0.765000000000001,-0.760000000000001,
-0.755000000000001,-0.750000000000001,-0.745000000000001,-0.740000000000001,
-0.735000000000001,-0.730000000000001,-0.725000000000001,-0.720000000000001,
-0.715000000000001,-0.710000000000001,-0.705000000000001,-0.700000000000001,
-0.695000000000001,-0.690000000000001,-0.685,-0.68,-0.675,-0.67,-0.665,
-0.66,-0.655,-0.65,-0.645,-0.64,-0.635,-0.63,-0.625,-0.62,-0.615,-0.61,
-0.605,-0.6,-0.595,-0.59,-0.585,-0.58,-0.575,-0.57,-0.565,-0.56,-0.555,
-0.55,-0.545,-0.54,-0.535,-0.53,-0.525,-0.52,-0.515,-0.51,-0.505,-0.5,-0.495,
-0.49,-0.485,-0.48,-0.475,-0.47,-0.465,-0.46,-0.455,-0.45,-0.445,-0.44,
-0.435,-0.43,-0.425,-0.42,-0.415,-0.41,-0.405,-0.4,-0.395,-0.39,-0.385,
-0.38,-0.375,-0.37,-0.365,-0.36,-0.355,-0.35,-0.345,-0.34,-0.335,-0.33,
-0.325,-0.32,-0.315,-0.31,-0.305,-0.3,-0.295,-0.29,-0.285,-0.28,-0.275,
-0.27,-0.265,-0.26,-0.255,-0.25,-0.245,-0.24,-0.235,-0.23,-0.225,-0.22,
-0.215,-0.21,-0.205,-0.2,-0.195,-0.19,-0.185,-0.18,-0.175,-0.17,-0.165,
-0.16,-0.155,-0.15,-0.145,-0.14,-0.135,-0.13,-0.125,-0.12,-0.115,-0.11,
-0.105,-0.1,-0.095,-0.09,-0.085,-0.08,-0.075,-0.07,-0.065,-0.06,-0.055,
-0.05,-0.045,-0.04,-0.035,-0.03,-0.025,-0.02,-0.015,-0.01,-0.005,0.),
 .UNSPECIFIED.)
CURVE()
GEOMETRIC_REPRESENTATION_ITEM()
RATIONAL_B_SPLINE_CURVE((1.,1.,1.,1.,1.,1.,1.,1.,1.,1.,1.,1.,1.,1.,1.,1.,
1.,1.,1.,1.,1.,1.,1.,1.,1.,1.,1.,1.,1.,1.,1.,1.,1.,1.,1.,1.,1.,1.,1.,1.,
1.,1.,1.,1.,1.,1.,1.,1.,1.,1.,1.,1.,1.,1.,1.,1.,1.,1.,1.,1.,1.,1.,1.,1.,
1.,1.,1.,1.,1.,1.,1.,1.,1.,1.,1.,1.,1.,1.,1.,1.,1.,1.,1.,1.,1.,1.,1.,1.,
1.,1.,1.,1.,1.,1.,1.,1.,1.,1.,1.,1.,1.,1.,1.,1.,1.,1.,1.,1.,1.,1.,1.,1.,
1.,1.,1.,1.,1.,1.,1.,1.,1.,1.,1.,1.,1.,1.,1.,1.,1.,1.,1.,1.,1.,1.,1.,1.,
1.,1.,1.,1.,1.,1.,1.,1.,1.,1.,1.,1.,1.,1.,1.,1.,1.,1.,1.,1.,1.,1.,1.,1.,
1.,1.,1.,1.,1.,1.,1.,1.,1.,1.,1.,1.,1.,1.,1.,1.,1.,1.,1.,1.,1.,1.,1.,1.,
1.,1.,1.,1.,1.,1.,1.,1.,1.,1.,1.,1.,1.,1.,1.,1.,1.,1.,1.,1.,1.))
REPRESENTATION_ITEM('')
);
#796=(
BOUNDED_CURVE()
B_SPLINE_CURVE(5,(#219930,#219931,#219932,#219933,#219934,#219935,#219936,
#219937,#219938,#219939,#219940,#219941,#219942,#219943,#219944,#219945,
#219946,#219947,#219948,#219949,#219950,#219951,#219952,#219953,#219954,
#219955,#219956,#219957,#219958,#219959,#219960,#219961,#219962,#219963,
#219964,#219965,#219966,#219967,#219968,#219969,#219970,#219971,#219972,
#219973,#219974,#219975,#219976,#219977,#219978,#219979,#219980,#219981,
#219982,#219983,#219984,#219985,#219986,#219987,#219988,#219989,#219990,
#219991,#219992,#219993,#219994,#219995,#219996,#219997,#219998,#219999,
#220000,#220001,#220002,#220003,#220004,#220005,#220006,#220007,#220008,
#220009,#220010,#220011,#220012,#220013,#220014,#220015,#220016,#220017,
#220018,#220019,#220020,#220021,#220022,#220023,#220024,#220025,#220026,
#220027,#220028,#220029,#220030,#220031,#220032,#220033,#220034,#220035,
#220036,#220037,#220038,#220039,#220040,#220041,#220042,#220043,#220044,
#220045,#220046,#220047,#220048,#220049,#220050,#220051,#220052,#220053,
#220054,#220055,#220056,#220057,#220058,#220059,#220060,#220061,#220062,
#220063,#220064,#220065,#220066,#220067,#220068,#220069,#220070,#220071,
#220072,#220073,#220074,#220075,#220076,#220077,#220078,#220079,#220080,
#220081,#220082,#220083,#220084,#220085,#220086,#220087,#220088,#220089,
#220090,#220091,#220092,#220093,#220094,#220095,#220096,#220097,#220098,
#220099,#220100,#220101,#220102,#220103,#220104,#220105,#220106,#220107,
#220108,#220109,#220110,#220111,#220112,#220113,#220114,#220115,#220116,
#220117,#220118,#220119,#220120,#220121,#220122,#220123,#220124,#220125,
#220126,#220127,#220128,#220129,#220130,#220131,#220132,#220133,#220134),
 .UNSPECIFIED.,.F.,.F.)
B_SPLINE_CURVE_WITH_KNOTS((6,1,1,1,1,1,1,1,1,1,1,1,1,1,1,1,1,1,1,1,1,1,
1,1,1,1,1,1,1,1,1,1,1,1,1,1,1,1,1,1,1,1,1,1,1,1,1,1,1,1,1,1,1,1,1,1,1,1,
1,1,1,1,1,1,1,1,1,1,1,1,1,1,1,1,1,1,1,1,1,1,1,1,1,1,1,1,1,1,1,1,1,1,1,1,
1,1,1,1,1,1,1,1,1,1,1,1,1,1,1,1,1,1,1,1,1,1,1,1,1,1,1,1,1,1,1,1,1,1,1,1,
1,1,1,1,1,1,1,1,1,1,1,1,1,1,1,1,1,1,1,1,1,1,1,1,1,1,1,1,1,1,1,1,1,1,1,1,
1,1,1,1,1,1,1,1,1,1,1,1,1,1,1,1,1,1,1,1,1,1,1,1,1,1,1,1,1,1,1,1,1,1,6),
(0.,0.005,0.01,0.015,0.02,0.025,0.03,0.035,0.04,0.045,0.05,0.055,0.06,0.065,
0.07,0.075,0.08,0.085,0.09,0.095,0.1,0.105,0.11,0.115,0.12,0.125,0.13,0.135,
0.14,0.145,0.15,0.155,0.16,0.165,0.17,0.175,0.18,0.185,0.19,0.195,0.2,0.205,
0.21,0.215,0.22,0.225,0.23,0.235,0.24,0.245,0.25,0.255,0.26,0.265,0.27,
0.275,0.28,0.285,0.29,0.295,0.3,0.305,0.31,0.315,0.32,0.325,0.33,0.335,
0.34,0.345,0.35,0.355,0.36,0.365,0.37,0.375,0.38,0.385,0.39,0.395,0.4,0.405,
0.41,0.415,0.42,0.425,0.43,0.435,0.44,0.445,0.45,0.455,0.46,0.465,0.47,
0.475,0.48,0.485,0.49,0.495,0.5,0.505,0.51,0.515,0.52,0.525,0.53,0.535,
0.54,0.545,0.55,0.555,0.56,0.565,0.57,0.575,0.58,0.585,0.59,0.595,0.6,0.605,
0.61,0.615,0.62,0.625,0.63,0.635,0.64,0.645,0.65,0.655,0.66,0.665,0.67,
0.675,0.68,0.685,0.690000000000001,0.695000000000001,0.700000000000001,
0.705000000000001,0.710000000000001,0.715000000000001,0.720000000000001,
0.725000000000001,0.730000000000001,0.735000000000001,0.740000000000001,
0.745000000000001,0.750000000000001,0.755000000000001,0.760000000000001,
0.765000000000001,0.770000000000001,0.775000000000001,0.780000000000001,
0.785000000000001,0.790000000000001,0.795000000000001,0.800000000000001,
0.805000000000001,0.810000000000001,0.815000000000001,0.820000000000001,
0.825000000000001,0.830000000000001,0.835000000000001,0.840000000000001,
0.845000000000001,0.850000000000001,0.855000000000001,0.860000000000001,
0.865000000000001,0.870000000000001,0.875000000000001,0.880000000000001,
0.885000000000001,0.890000000000001,0.895000000000001,0.900000000000001,
0.905000000000001,0.910000000000001,0.915000000000001,0.920000000000001,
0.925000000000001,0.930000000000001,0.935000000000001,0.940000000000001,
0.945000000000001,0.950000000000001,0.955000000000001,0.960000000000001,
0.965000000000001,0.970000000000001,0.975000000000001,0.980000000000001,
0.985000000000001,0.990000000000001,0.995000000000001,1.),.UNSPECIFIED.)
CURVE()
GEOMETRIC_REPRESENTATION_ITEM()
RATIONAL_B_SPLINE_CURVE((1.,1.,1.,1.,1.,1.,1.,1.,1.,1.,1.,1.,1.,1.,1.,1.,
1.,1.,1.,1.,1.,1.,1.,1.,1.,1.,1.,1.,1.,1.,1.,1.,1.,1.,1.,1.,1.,1.,1.,1.,
1.,1.,1.,1.,1.,1.,1.,1.,1.,1.,1.,1.,1.,1.,1.,1.,1.,1.,1.,1.,1.,1.,1.,1.,
1.,1.,1.,1.,1.,1.,1.,1.,1.,1.,1.,1.,1.,1.,1.,1.,1.,1.,1.,1.,1.,1.,1.,1.,
1.,1.,1.,1.,1.,1.,1.,1.,1.,1.,1.,1.,1.,1.,1.,1.,1.,1.,1.,1.,1.,1.,1.,1.,
1.,1.,1.,1.,1.,1.,1.,1.,1.,1.,1.,1.,1.,1.,1.,1.,1.,1.,1.,1.,1.,1.,1.,1.,
1.,1.,1.,1.,1.,1.,1.,1.,1.,1.,1.,1.,1.,1.,1.,1.,1.,1.,1.,1.,1.,1.,1.,1.,
1.,1.,1.,1.,1.,1.,1.,1.,1.,1.,1.,1.,1.,1.,1.,1.,1.,1.,1.,1.,1.,1.,1.,1.,
1.,1.,1.,1.,1.,1.,1.,1.,1.,1.,1.,1.,1.,1.,1.,1.,1.,1.,1.,1.,1.))
REPRESENTATION_ITEM('')
);
#797=(
BOUNDED_CURVE()
B_SPLINE_CURVE(5,(#220546,#220547,#220548,#220549,#220550,#220551,#220552,
#220553,#220554,#220555,#220556,#220557,#220558,#220559,#220560,#220561,
#220562,#220563,#220564,#220565,#220566,#220567,#220568,#220569,#220570,
#220571,#220572,#220573,#220574,#220575,#220576,#220577,#220578,#220579,
#220580,#220581,#220582,#220583,#220584,#220585,#220586,#220587,#220588,
#220589,#220590,#220591,#220592,#220593,#220594,#220595,#220596,#220597,
#220598,#220599,#220600,#220601,#220602,#220603,#220604,#220605,#220606,
#220607,#220608,#220609,#220610,#220611,#220612,#220613,#220614,#220615,
#220616,#220617,#220618,#220619,#220620,#220621,#220622,#220623,#220624,
#220625,#220626,#220627,#220628,#220629,#220630,#220631,#220632,#220633,
#220634,#220635,#220636,#220637,#220638,#220639,#220640,#220641,#220642,
#220643,#220644,#220645,#220646,#220647,#220648,#220649,#220650,#220651,
#220652,#220653,#220654,#220655,#220656,#220657,#220658,#220659,#220660,
#220661,#220662,#220663,#220664,#220665,#220666,#220667,#220668,#220669,
#220670,#220671,#220672,#220673,#220674,#220675,#220676,#220677,#220678,
#220679,#220680,#220681,#220682,#220683,#220684,#220685,#220686,#220687,
#220688,#220689,#220690,#220691,#220692,#220693,#220694,#220695,#220696,
#220697,#220698,#220699,#220700,#220701,#220702,#220703,#220704,#220705,
#220706,#220707,#220708,#220709,#220710,#220711,#220712,#220713,#220714,
#220715,#220716,#220717,#220718,#220719,#220720,#220721,#220722,#220723,
#220724,#220725,#220726,#220727,#220728,#220729,#220730,#220731,#220732,
#220733,#220734,#220735,#220736,#220737,#220738,#220739,#220740,#220741,
#220742,#220743,#220744,#220745,#220746,#220747,#220748,#220749,#220750),
 .UNSPECIFIED.,.F.,.F.)
B_SPLINE_CURVE_WITH_KNOTS((6,1,1,1,1,1,1,1,1,1,1,1,1,1,1,1,1,1,1,1,1,1,
1,1,1,1,1,1,1,1,1,1,1,1,1,1,1,1,1,1,1,1,1,1,1,1,1,1,1,1,1,1,1,1,1,1,1,1,
1,1,1,1,1,1,1,1,1,1,1,1,1,1,1,1,1,1,1,1,1,1,1,1,1,1,1,1,1,1,1,1,1,1,1,1,
1,1,1,1,1,1,1,1,1,1,1,1,1,1,1,1,1,1,1,1,1,1,1,1,1,1,1,1,1,1,1,1,1,1,1,1,
1,1,1,1,1,1,1,1,1,1,1,1,1,1,1,1,1,1,1,1,1,1,1,1,1,1,1,1,1,1,1,1,1,1,1,1,
1,1,1,1,1,1,1,1,1,1,1,1,1,1,1,1,1,1,1,1,1,1,1,1,1,1,1,1,1,1,1,1,1,1,6),
(0.,0.005,0.01,0.015,0.02,0.025,0.03,0.035,0.04,0.045,0.05,0.055,0.06,0.065,
0.07,0.075,0.08,0.085,0.09,0.095,0.1,0.105,0.11,0.115,0.12,0.125,0.13,0.135,
0.14,0.145,0.15,0.155,0.16,0.165,0.17,0.175,0.18,0.185,0.19,0.195,0.2,0.205,
0.21,0.215,0.22,0.225,0.23,0.235,0.24,0.245,0.25,0.255,0.26,0.265,0.27,
0.275,0.28,0.285,0.29,0.295,0.3,0.305,0.31,0.315,0.32,0.325,0.33,0.335,
0.34,0.345,0.35,0.355,0.36,0.365,0.37,0.375,0.38,0.385,0.39,0.395,0.4,0.405,
0.41,0.415,0.42,0.425,0.43,0.435,0.44,0.445,0.45,0.455,0.46,0.465,0.47,
0.475,0.48,0.485,0.49,0.495,0.5,0.505,0.51,0.515,0.52,0.525,0.53,0.535,
0.54,0.545,0.55,0.555,0.56,0.565,0.57,0.575,0.58,0.585,0.59,0.595,0.6,0.605,
0.61,0.615,0.62,0.625,0.63,0.635,0.64,0.645,0.65,0.655,0.66,0.665,0.67,
0.675,0.68,0.685,0.690000000000001,0.695000000000001,0.700000000000001,
0.705000000000001,0.710000000000001,0.715000000000001,0.720000000000001,
0.725000000000001,0.730000000000001,0.735000000000001,0.740000000000001,
0.745000000000001,0.750000000000001,0.755000000000001,0.760000000000001,
0.765000000000001,0.770000000000001,0.775000000000001,0.780000000000001,
0.785000000000001,0.790000000000001,0.795000000000001,0.800000000000001,
0.805000000000001,0.810000000000001,0.815000000000001,0.820000000000001,
0.825000000000001,0.830000000000001,0.835000000000001,0.840000000000001,
0.845000000000001,0.850000000000001,0.855000000000001,0.860000000000001,
0.865000000000001,0.870000000000001,0.875000000000001,0.880000000000001,
0.885000000000001,0.890000000000001,0.895000000000001,0.900000000000001,
0.905000000000001,0.910000000000001,0.915000000000001,0.920000000000001,
0.925000000000001,0.930000000000001,0.935000000000001,0.940000000000001,
0.945000000000001,0.950000000000001,0.955000000000001,0.960000000000001,
0.965000000000001,0.970000000000001,0.975000000000001,0.980000000000001,
0.985000000000001,0.990000000000001,0.995000000000001,1.),.UNSPECIFIED.)
CURVE()
GEOMETRIC_REPRESENTATION_ITEM()
RATIONAL_B_SPLINE_CURVE((1.,1.,1.,1.,1.,1.,1.,1.,1.,1.,1.,1.,1.,1.,1.,1.,
1.,1.,1.,1.,1.,1.,1.,1.,1.,1.,1.,1.,1.,1.,1.,1.,1.,1.,1.,1.,1.,1.,1.,1.,
1.,1.,1.,1.,1.,1.,1.,1.,1.,1.,1.,1.,1.,1.,1.,1.,1.,1.,1.,1.,1.,1.,1.,1.,
1.,1.,1.,1.,1.,1.,1.,1.,1.,1.,1.,1.,1.,1.,1.,1.,1.,1.,1.,1.,1.,1.,1.,1.,
1.,1.,1.,1.,1.,1.,1.,1.,1.,1.,1.,1.,1.,1.,1.,1.,1.,1.,1.,1.,1.,1.,1.,1.,
1.,1.,1.,1.,1.,1.,1.,1.,1.,1.,1.,1.,1.,1.,1.,1.,1.,1.,1.,1.,1.,1.,1.,1.,
1.,1.,1.,1.,1.,1.,1.,1.,1.,1.,1.,1.,1.,1.,1.,1.,1.,1.,1.,1.,1.,1.,1.,1.,
1.,1.,1.,1.,1.,1.,1.,1.,1.,1.,1.,1.,1.,1.,1.,1.,1.,1.,1.,1.,1.,1.,1.,1.,
1.,1.,1.,1.,1.,1.,1.,1.,1.,1.,1.,1.,1.,1.,1.,1.,1.,1.,1.,1.,1.))
REPRESENTATION_ITEM('')
);
#798=(
BOUNDED_CURVE()
B_SPLINE_CURVE(5,(#220752,#220753,#220754,#220755,#220756,#220757,#220758,
#220759,#220760,#220761,#220762,#220763,#220764,#220765,#220766,#220767,
#220768,#220769,#220770,#220771,#220772,#220773,#220774,#220775,#220776,
#220777,#220778,#220779,#220780,#220781,#220782,#220783,#220784,#220785,
#220786,#220787,#220788,#220789,#220790,#220791,#220792,#220793,#220794,
#220795,#220796,#220797,#220798,#220799,#220800,#220801,#220802,#220803,
#220804,#220805,#220806,#220807,#220808,#220809,#220810,#220811,#220812,
#220813,#220814,#220815,#220816,#220817,#220818,#220819,#220820,#220821,
#220822,#220823,#220824,#220825,#220826,#220827,#220828,#220829,#220830,
#220831,#220832,#220833,#220834,#220835,#220836,#220837,#220838,#220839,
#220840,#220841,#220842,#220843,#220844,#220845,#220846,#220847,#220848,
#220849,#220850,#220851,#220852,#220853,#220854,#220855,#220856,#220857,
#220858,#220859,#220860,#220861,#220862,#220863,#220864,#220865,#220866,
#220867,#220868,#220869,#220870,#220871,#220872,#220873,#220874,#220875,
#220876,#220877,#220878,#220879,#220880,#220881,#220882,#220883,#220884,
#220885,#220886,#220887,#220888,#220889,#220890,#220891,#220892,#220893,
#220894,#220895,#220896,#220897,#220898,#220899,#220900,#220901,#220902,
#220903,#220904,#220905,#220906,#220907,#220908,#220909,#220910,#220911,
#220912,#220913,#220914,#220915,#220916,#220917,#220918,#220919,#220920,
#220921,#220922,#220923,#220924,#220925,#220926,#220927,#220928,#220929,
#220930,#220931,#220932,#220933,#220934,#220935,#220936,#220937,#220938,
#220939,#220940,#220941,#220942,#220943,#220944,#220945,#220946,#220947,
#220948,#220949,#220950,#220951,#220952,#220953,#220954,#220955,#220956),
 .UNSPECIFIED.,.F.,.F.)
B_SPLINE_CURVE_WITH_KNOTS((6,1,1,1,1,1,1,1,1,1,1,1,1,1,1,1,1,1,1,1,1,1,
1,1,1,1,1,1,1,1,1,1,1,1,1,1,1,1,1,1,1,1,1,1,1,1,1,1,1,1,1,1,1,1,1,1,1,1,
1,1,1,1,1,1,1,1,1,1,1,1,1,1,1,1,1,1,1,1,1,1,1,1,1,1,1,1,1,1,1,1,1,1,1,1,
1,1,1,1,1,1,1,1,1,1,1,1,1,1,1,1,1,1,1,1,1,1,1,1,1,1,1,1,1,1,1,1,1,1,1,1,
1,1,1,1,1,1,1,1,1,1,1,1,1,1,1,1,1,1,1,1,1,1,1,1,1,1,1,1,1,1,1,1,1,1,1,1,
1,1,1,1,1,1,1,1,1,1,1,1,1,1,1,1,1,1,1,1,1,1,1,1,1,1,1,1,1,1,1,1,1,1,6),
(-1.,-0.995000000000001,-0.990000000000001,-0.985000000000001,-0.980000000000001,
-0.975000000000001,-0.970000000000001,-0.965000000000001,-0.960000000000001,
-0.955000000000001,-0.950000000000001,-0.945000000000001,-0.940000000000001,
-0.935000000000001,-0.930000000000001,-0.925000000000001,-0.920000000000001,
-0.915000000000001,-0.910000000000001,-0.905000000000001,-0.900000000000001,
-0.895000000000001,-0.890000000000001,-0.885000000000001,-0.880000000000001,
-0.875000000000001,-0.870000000000001,-0.865000000000001,-0.860000000000001,
-0.855000000000001,-0.850000000000001,-0.845000000000001,-0.840000000000001,
-0.835000000000001,-0.830000000000001,-0.825000000000001,-0.820000000000001,
-0.815000000000001,-0.810000000000001,-0.805000000000001,-0.800000000000001,
-0.795000000000001,-0.790000000000001,-0.785000000000001,-0.780000000000001,
-0.775000000000001,-0.770000000000001,-0.765000000000001,-0.760000000000001,
-0.755000000000001,-0.750000000000001,-0.745000000000001,-0.740000000000001,
-0.735000000000001,-0.730000000000001,-0.725000000000001,-0.720000000000001,
-0.715000000000001,-0.710000000000001,-0.705000000000001,-0.700000000000001,
-0.695000000000001,-0.690000000000001,-0.685,-0.68,-0.675,-0.67,-0.665,
-0.66,-0.655,-0.65,-0.645,-0.64,-0.635,-0.63,-0.625,-0.62,-0.615,-0.61,
-0.605,-0.6,-0.595,-0.59,-0.585,-0.58,-0.575,-0.57,-0.565,-0.56,-0.555,
-0.55,-0.545,-0.54,-0.535,-0.53,-0.525,-0.52,-0.515,-0.51,-0.505,-0.5,-0.495,
-0.49,-0.485,-0.48,-0.475,-0.47,-0.465,-0.46,-0.455,-0.45,-0.445,-0.44,
-0.435,-0.43,-0.425,-0.42,-0.415,-0.41,-0.405,-0.4,-0.395,-0.39,-0.385,
-0.38,-0.375,-0.37,-0.365,-0.36,-0.355,-0.35,-0.345,-0.34,-0.335,-0.33,
-0.325,-0.32,-0.315,-0.31,-0.305,-0.3,-0.295,-0.29,-0.285,-0.28,-0.275,
-0.27,-0.265,-0.26,-0.255,-0.25,-0.245,-0.24,-0.235,-0.23,-0.225,-0.22,
-0.215,-0.21,-0.205,-0.2,-0.195,-0.19,-0.185,-0.18,-0.175,-0.17,-0.165,
-0.16,-0.155,-0.15,-0.145,-0.14,-0.135,-0.13,-0.125,-0.12,-0.115,-0.11,
-0.105,-0.1,-0.095,-0.09,-0.085,-0.08,-0.075,-0.07,-0.065,-0.06,-0.055,
-0.05,-0.045,-0.04,-0.035,-0.03,-0.025,-0.02,-0.015,-0.01,-0.005,0.),
 .UNSPECIFIED.)
CURVE()
GEOMETRIC_REPRESENTATION_ITEM()
RATIONAL_B_SPLINE_CURVE((1.,1.,1.,1.,1.,1.,1.,1.,1.,1.,1.,1.,1.,1.,1.,1.,
1.,1.,1.,1.,1.,1.,1.,1.,1.,1.,1.,1.,1.,1.,1.,1.,1.,1.,1.,1.,1.,1.,1.,1.,
1.,1.,1.,1.,1.,1.,1.,1.,1.,1.,1.,1.,1.,1.,1.,1.,1.,1.,1.,1.,1.,1.,1.,1.,
1.,1.,1.,1.,1.,1.,1.,1.,1.,1.,1.,1.,1.,1.,1.,1.,1.,1.,1.,1.,1.,1.,1.,1.,
1.,1.,1.,1.,1.,1.,1.,1.,1.,1.,1.,1.,1.,1.,1.,1.,1.,1.,1.,1.,1.,1.,1.,1.,
1.,1.,1.,1.,1.,1.,1.,1.,1.,1.,1.,1.,1.,1.,1.,1.,1.,1.,1.,1.,1.,1.,1.,1.,
1.,1.,1.,1.,1.,1.,1.,1.,1.,1.,1.,1.,1.,1.,1.,1.,1.,1.,1.,1.,1.,1.,1.,1.,
1.,1.,1.,1.,1.,1.,1.,1.,1.,1.,1.,1.,1.,1.,1.,1.,1.,1.,1.,1.,1.,1.,1.,1.,
1.,1.,1.,1.,1.,1.,1.,1.,1.,1.,1.,1.,1.,1.,1.,1.,1.,1.,1.,1.,1.))
REPRESENTATION_ITEM('')
);
#799=(
BOUNDED_CURVE()
B_SPLINE_CURVE(5,(#221375,#221376,#221377,#221378,#221379,#221380,#221381,
#221382,#221383,#221384,#221385,#221386,#221387,#221388,#221389,#221390,
#221391,#221392,#221393,#221394,#221395,#221396,#221397,#221398,#221399,
#221400,#221401,#221402,#221403,#221404,#221405,#221406,#221407,#221408,
#221409,#221410,#221411,#221412,#221413,#221414,#221415,#221416,#221417,
#221418,#221419,#221420,#221421,#221422,#221423,#221424,#221425,#221426,
#221427,#221428,#221429,#221430,#221431,#221432,#221433,#221434,#221435,
#221436,#221437,#221438,#221439,#221440,#221441,#221442,#221443,#221444,
#221445,#221446,#221447,#221448,#221449,#221450,#221451,#221452,#221453,
#221454,#221455,#221456,#221457,#221458,#221459,#221460,#221461,#221462,
#221463,#221464,#221465,#221466,#221467,#221468,#221469,#221470,#221471,
#221472,#221473,#221474,#221475,#221476,#221477,#221478,#221479,#221480,
#221481,#221482,#221483,#221484,#221485,#221486,#221487,#221488,#221489,
#221490,#221491,#221492,#221493,#221494,#221495,#221496,#221497,#221498,
#221499,#221500,#221501,#221502,#221503,#221504,#221505,#221506,#221507,
#221508,#221509,#221510,#221511,#221512,#221513,#221514,#221515,#221516,
#221517,#221518,#221519,#221520,#221521,#221522,#221523,#221524,#221525,
#221526,#221527,#221528,#221529,#221530,#221531,#221532,#221533,#221534,
#221535,#221536,#221537,#221538,#221539,#221540,#221541,#221542,#221543,
#221544,#221545,#221546,#221547,#221548,#221549,#221550,#221551,#221552,
#221553,#221554,#221555,#221556,#221557,#221558,#221559,#221560,#221561,
#221562,#221563,#221564,#221565,#221566,#221567,#221568,#221569,#221570,
#221571,#221572,#221573,#221574,#221575,#221576,#221577,#221578,#221579),
 .UNSPECIFIED.,.F.,.F.)
B_SPLINE_CURVE_WITH_KNOTS((6,1,1,1,1,1,1,1,1,1,1,1,1,1,1,1,1,1,1,1,1,1,
1,1,1,1,1,1,1,1,1,1,1,1,1,1,1,1,1,1,1,1,1,1,1,1,1,1,1,1,1,1,1,1,1,1,1,1,
1,1,1,1,1,1,1,1,1,1,1,1,1,1,1,1,1,1,1,1,1,1,1,1,1,1,1,1,1,1,1,1,1,1,1,1,
1,1,1,1,1,1,1,1,1,1,1,1,1,1,1,1,1,1,1,1,1,1,1,1,1,1,1,1,1,1,1,1,1,1,1,1,
1,1,1,1,1,1,1,1,1,1,1,1,1,1,1,1,1,1,1,1,1,1,1,1,1,1,1,1,1,1,1,1,1,1,1,1,
1,1,1,1,1,1,1,1,1,1,1,1,1,1,1,1,1,1,1,1,1,1,1,1,1,1,1,1,1,1,1,1,1,1,6),
(-1.,-0.995000000000001,-0.990000000000001,-0.985000000000001,-0.980000000000001,
-0.975000000000001,-0.970000000000001,-0.965000000000001,-0.960000000000001,
-0.955000000000001,-0.950000000000001,-0.945000000000001,-0.940000000000001,
-0.935000000000001,-0.930000000000001,-0.925000000000001,-0.920000000000001,
-0.915000000000001,-0.910000000000001,-0.905000000000001,-0.900000000000001,
-0.895000000000001,-0.890000000000001,-0.885000000000001,-0.880000000000001,
-0.875000000000001,-0.870000000000001,-0.865000000000001,-0.860000000000001,
-0.855000000000001,-0.850000000000001,-0.845000000000001,-0.840000000000001,
-0.835000000000001,-0.830000000000001,-0.825000000000001,-0.820000000000001,
-0.815000000000001,-0.810000000000001,-0.805000000000001,-0.800000000000001,
-0.795000000000001,-0.790000000000001,-0.785000000000001,-0.780000000000001,
-0.775000000000001,-0.770000000000001,-0.765000000000001,-0.760000000000001,
-0.755000000000001,-0.750000000000001,-0.745000000000001,-0.740000000000001,
-0.735000000000001,-0.730000000000001,-0.725000000000001,-0.720000000000001,
-0.715000000000001,-0.710000000000001,-0.705000000000001,-0.700000000000001,
-0.695000000000001,-0.690000000000001,-0.685,-0.68,-0.675,-0.67,-0.665,
-0.66,-0.655,-0.65,-0.645,-0.64,-0.635,-0.63,-0.625,-0.62,-0.615,-0.61,
-0.605,-0.6,-0.595,-0.59,-0.585,-0.58,-0.575,-0.57,-0.565,-0.56,-0.555,
-0.55,-0.545,-0.54,-0.535,-0.53,-0.525,-0.52,-0.515,-0.51,-0.505,-0.5,-0.495,
-0.49,-0.485,-0.48,-0.475,-0.47,-0.465,-0.46,-0.455,-0.45,-0.445,-0.44,
-0.435,-0.43,-0.425,-0.42,-0.415,-0.41,-0.405,-0.4,-0.395,-0.39,-0.385,
-0.38,-0.375,-0.37,-0.365,-0.36,-0.355,-0.35,-0.345,-0.34,-0.335,-0.33,
-0.325,-0.32,-0.315,-0.31,-0.305,-0.3,-0.295,-0.29,-0.285,-0.28,-0.275,
-0.27,-0.265,-0.26,-0.255,-0.25,-0.245,-0.24,-0.235,-0.23,-0.225,-0.22,
-0.215,-0.21,-0.205,-0.2,-0.195,-0.19,-0.185,-0.18,-0.175,-0.17,-0.165,
-0.16,-0.155,-0.15,-0.145,-0.14,-0.135,-0.13,-0.125,-0.12,-0.115,-0.11,
-0.105,-0.1,-0.095,-0.09,-0.085,-0.08,-0.075,-0.07,-0.065,-0.06,-0.055,
-0.05,-0.045,-0.04,-0.035,-0.03,-0.025,-0.02,-0.015,-0.01,-0.005,0.),
 .UNSPECIFIED.)
CURVE()
GEOMETRIC_REPRESENTATION_ITEM()
RATIONAL_B_SPLINE_CURVE((1.,1.,1.,1.,1.,1.,1.,1.,1.,1.,1.,1.,1.,1.,1.,1.,
1.,1.,1.,1.,1.,1.,1.,1.,1.,1.,1.,1.,1.,1.,1.,1.,1.,1.,1.,1.,1.,1.,1.,1.,
1.,1.,1.,1.,1.,1.,1.,1.,1.,1.,1.,1.,1.,1.,1.,1.,1.,1.,1.,1.,1.,1.,1.,1.,
1.,1.,1.,1.,1.,1.,1.,1.,1.,1.,1.,1.,1.,1.,1.,1.,1.,1.,1.,1.,1.,1.,1.,1.,
1.,1.,1.,1.,1.,1.,1.,1.,1.,1.,1.,1.,1.,1.,1.,1.,1.,1.,1.,1.,1.,1.,1.,1.,
1.,1.,1.,1.,1.,1.,1.,1.,1.,1.,1.,1.,1.,1.,1.,1.,1.,1.,1.,1.,1.,1.,1.,1.,
1.,1.,1.,1.,1.,1.,1.,1.,1.,1.,1.,1.,1.,1.,1.,1.,1.,1.,1.,1.,1.,1.,1.,1.,
1.,1.,1.,1.,1.,1.,1.,1.,1.,1.,1.,1.,1.,1.,1.,1.,1.,1.,1.,1.,1.,1.,1.,1.,
1.,1.,1.,1.,1.,1.,1.,1.,1.,1.,1.,1.,1.,1.,1.,1.,1.,1.,1.,1.,1.))
REPRESENTATION_ITEM('')
);
#800=(
BOUNDED_CURVE()
B_SPLINE_CURVE(5,(#221582,#221583,#221584,#221585,#221586,#221587,#221588,
#221589,#221590,#221591,#221592,#221593,#221594,#221595,#221596,#221597,
#221598,#221599,#221600,#221601,#221602,#221603,#221604,#221605,#221606,
#221607,#221608,#221609,#221610,#221611,#221612,#221613,#221614,#221615,
#221616,#221617,#221618,#221619,#221620,#221621,#221622,#221623,#221624,
#221625,#221626,#221627,#221628,#221629,#221630,#221631,#221632,#221633,
#221634,#221635,#221636,#221637,#221638,#221639,#221640,#221641,#221642,
#221643,#221644,#221645,#221646,#221647,#221648,#221649,#221650,#221651,
#221652,#221653,#221654,#221655,#221656,#221657,#221658,#221659,#221660,
#221661,#221662,#221663,#221664,#221665,#221666,#221667,#221668,#221669,
#221670,#221671,#221672,#221673,#221674,#221675,#221676,#221677,#221678,
#221679,#221680,#221681,#221682,#221683,#221684,#221685,#221686,#221687,
#221688,#221689,#221690,#221691,#221692,#221693,#221694,#221695,#221696,
#221697,#221698,#221699,#221700,#221701,#221702,#221703,#221704,#221705,
#221706,#221707,#221708,#221709,#221710,#221711,#221712,#221713,#221714,
#221715,#221716,#221717,#221718,#221719,#221720,#221721,#221722,#221723,
#221724,#221725,#221726,#221727,#221728,#221729,#221730,#221731,#221732,
#221733,#221734,#221735,#221736,#221737,#221738,#221739,#221740,#221741,
#221742,#221743,#221744,#221745,#221746,#221747,#221748,#221749,#221750,
#221751,#221752,#221753,#221754,#221755,#221756,#221757,#221758,#221759,
#221760,#221761,#221762,#221763,#221764,#221765,#221766,#221767,#221768,
#221769,#221770,#221771,#221772,#221773,#221774,#221775,#221776,#221777,
#221778,#221779,#221780,#221781,#221782,#221783,#221784,#221785,#221786),
 .UNSPECIFIED.,.F.,.F.)
B_SPLINE_CURVE_WITH_KNOTS((6,1,1,1,1,1,1,1,1,1,1,1,1,1,1,1,1,1,1,1,1,1,
1,1,1,1,1,1,1,1,1,1,1,1,1,1,1,1,1,1,1,1,1,1,1,1,1,1,1,1,1,1,1,1,1,1,1,1,
1,1,1,1,1,1,1,1,1,1,1,1,1,1,1,1,1,1,1,1,1,1,1,1,1,1,1,1,1,1,1,1,1,1,1,1,
1,1,1,1,1,1,1,1,1,1,1,1,1,1,1,1,1,1,1,1,1,1,1,1,1,1,1,1,1,1,1,1,1,1,1,1,
1,1,1,1,1,1,1,1,1,1,1,1,1,1,1,1,1,1,1,1,1,1,1,1,1,1,1,1,1,1,1,1,1,1,1,1,
1,1,1,1,1,1,1,1,1,1,1,1,1,1,1,1,1,1,1,1,1,1,1,1,1,1,1,1,1,1,1,1,1,1,6),
(0.,0.005,0.01,0.015,0.02,0.025,0.03,0.035,0.04,0.045,0.05,0.055,0.06,0.065,
0.07,0.075,0.08,0.085,0.09,0.095,0.1,0.105,0.11,0.115,0.12,0.125,0.13,0.135,
0.14,0.145,0.15,0.155,0.16,0.165,0.17,0.175,0.18,0.185,0.19,0.195,0.2,0.205,
0.21,0.215,0.22,0.225,0.23,0.235,0.24,0.245,0.25,0.255,0.26,0.265,0.27,
0.275,0.28,0.285,0.29,0.295,0.3,0.305,0.31,0.315,0.32,0.325,0.33,0.335,
0.34,0.345,0.35,0.355,0.36,0.365,0.37,0.375,0.38,0.385,0.39,0.395,0.4,0.405,
0.41,0.415,0.42,0.425,0.43,0.435,0.44,0.445,0.45,0.455,0.46,0.465,0.47,
0.475,0.48,0.485,0.49,0.495,0.5,0.505,0.51,0.515,0.52,0.525,0.53,0.535,
0.54,0.545,0.55,0.555,0.56,0.565,0.57,0.575,0.58,0.585,0.59,0.595,0.6,0.605,
0.61,0.615,0.62,0.625,0.63,0.635,0.64,0.645,0.65,0.655,0.66,0.665,0.67,
0.675,0.68,0.685,0.690000000000001,0.695000000000001,0.700000000000001,
0.705000000000001,0.710000000000001,0.715000000000001,0.720000000000001,
0.725000000000001,0.730000000000001,0.735000000000001,0.740000000000001,
0.745000000000001,0.750000000000001,0.755000000000001,0.760000000000001,
0.765000000000001,0.770000000000001,0.775000000000001,0.780000000000001,
0.785000000000001,0.790000000000001,0.795000000000001,0.800000000000001,
0.805000000000001,0.810000000000001,0.815000000000001,0.820000000000001,
0.825000000000001,0.830000000000001,0.835000000000001,0.840000000000001,
0.845000000000001,0.850000000000001,0.855000000000001,0.860000000000001,
0.865000000000001,0.870000000000001,0.875000000000001,0.880000000000001,
0.885000000000001,0.890000000000001,0.895000000000001,0.900000000000001,
0.905000000000001,0.910000000000001,0.915000000000001,0.920000000000001,
0.925000000000001,0.930000000000001,0.935000000000001,0.940000000000001,
0.945000000000001,0.950000000000001,0.955000000000001,0.960000000000001,
0.965000000000001,0.970000000000001,0.975000000000001,0.980000000000001,
0.985000000000001,0.990000000000001,0.995000000000001,1.),.UNSPECIFIED.)
CURVE()
GEOMETRIC_REPRESENTATION_ITEM()
RATIONAL_B_SPLINE_CURVE((1.,1.,1.,1.,1.,1.,1.,1.,1.,1.,1.,1.,1.,1.,1.,1.,
1.,1.,1.,1.,1.,1.,1.,1.,1.,1.,1.,1.,1.,1.,1.,1.,1.,1.,1.,1.,1.,1.,1.,1.,
1.,1.,1.,1.,1.,1.,1.,1.,1.,1.,1.,1.,1.,1.,1.,1.,1.,1.,1.,1.,1.,1.,1.,1.,
1.,1.,1.,1.,1.,1.,1.,1.,1.,1.,1.,1.,1.,1.,1.,1.,1.,1.,1.,1.,1.,1.,1.,1.,
1.,1.,1.,1.,1.,1.,1.,1.,1.,1.,1.,1.,1.,1.,1.,1.,1.,1.,1.,1.,1.,1.,1.,1.,
1.,1.,1.,1.,1.,1.,1.,1.,1.,1.,1.,1.,1.,1.,1.,1.,1.,1.,1.,1.,1.,1.,1.,1.,
1.,1.,1.,1.,1.,1.,1.,1.,1.,1.,1.,1.,1.,1.,1.,1.,1.,1.,1.,1.,1.,1.,1.,1.,
1.,1.,1.,1.,1.,1.,1.,1.,1.,1.,1.,1.,1.,1.,1.,1.,1.,1.,1.,1.,1.,1.,1.,1.,
1.,1.,1.,1.,1.,1.,1.,1.,1.,1.,1.,1.,1.,1.,1.,1.,1.,1.,1.,1.,1.))
REPRESENTATION_ITEM('')
);
#801=(
BOUNDED_CURVE()
B_SPLINE_CURVE(5,(#222198,#222199,#222200,#222201,#222202,#222203,#222204,
#222205,#222206,#222207,#222208,#222209,#222210,#222211,#222212,#222213,
#222214,#222215,#222216,#222217,#222218,#222219,#222220,#222221,#222222,
#222223,#222224,#222225,#222226,#222227,#222228,#222229,#222230,#222231,
#222232,#222233,#222234,#222235,#222236,#222237,#222238,#222239,#222240,
#222241,#222242,#222243,#222244,#222245,#222246,#222247,#222248,#222249,
#222250,#222251,#222252,#222253,#222254,#222255,#222256,#222257,#222258,
#222259,#222260,#222261,#222262,#222263,#222264,#222265,#222266,#222267,
#222268,#222269,#222270,#222271,#222272,#222273,#222274,#222275,#222276,
#222277,#222278,#222279,#222280,#222281,#222282,#222283,#222284,#222285,
#222286,#222287,#222288,#222289,#222290,#222291,#222292,#222293,#222294,
#222295,#222296,#222297,#222298,#222299,#222300,#222301,#222302,#222303,
#222304,#222305,#222306,#222307,#222308,#222309,#222310,#222311,#222312,
#222313,#222314,#222315,#222316,#222317,#222318,#222319,#222320,#222321,
#222322,#222323,#222324,#222325,#222326,#222327,#222328,#222329,#222330,
#222331,#222332,#222333,#222334,#222335,#222336,#222337,#222338,#222339,
#222340,#222341,#222342,#222343,#222344,#222345,#222346,#222347,#222348,
#222349,#222350,#222351,#222352,#222353,#222354,#222355,#222356,#222357,
#222358,#222359,#222360,#222361,#222362,#222363,#222364,#222365,#222366,
#222367,#222368,#222369,#222370,#222371,#222372,#222373,#222374,#222375,
#222376,#222377,#222378,#222379,#222380,#222381,#222382,#222383,#222384,
#222385,#222386,#222387,#222388,#222389,#222390,#222391,#222392,#222393,
#222394,#222395,#222396,#222397,#222398,#222399,#222400,#222401,#222402),
 .UNSPECIFIED.,.F.,.F.)
B_SPLINE_CURVE_WITH_KNOTS((6,1,1,1,1,1,1,1,1,1,1,1,1,1,1,1,1,1,1,1,1,1,
1,1,1,1,1,1,1,1,1,1,1,1,1,1,1,1,1,1,1,1,1,1,1,1,1,1,1,1,1,1,1,1,1,1,1,1,
1,1,1,1,1,1,1,1,1,1,1,1,1,1,1,1,1,1,1,1,1,1,1,1,1,1,1,1,1,1,1,1,1,1,1,1,
1,1,1,1,1,1,1,1,1,1,1,1,1,1,1,1,1,1,1,1,1,1,1,1,1,1,1,1,1,1,1,1,1,1,1,1,
1,1,1,1,1,1,1,1,1,1,1,1,1,1,1,1,1,1,1,1,1,1,1,1,1,1,1,1,1,1,1,1,1,1,1,1,
1,1,1,1,1,1,1,1,1,1,1,1,1,1,1,1,1,1,1,1,1,1,1,1,1,1,1,1,1,1,1,1,1,1,6),
(0.,0.005,0.01,0.015,0.02,0.025,0.03,0.035,0.04,0.045,0.05,0.055,0.06,0.065,
0.07,0.075,0.08,0.085,0.09,0.095,0.1,0.105,0.11,0.115,0.12,0.125,0.13,0.135,
0.14,0.145,0.15,0.155,0.16,0.165,0.17,0.175,0.18,0.185,0.19,0.195,0.2,0.205,
0.21,0.215,0.22,0.225,0.23,0.235,0.24,0.245,0.25,0.255,0.26,0.265,0.27,
0.275,0.28,0.285,0.29,0.295,0.3,0.305,0.31,0.315,0.32,0.325,0.33,0.335,
0.34,0.345,0.35,0.355,0.36,0.365,0.37,0.375,0.38,0.385,0.39,0.395,0.4,0.405,
0.41,0.415,0.42,0.425,0.43,0.435,0.44,0.445,0.45,0.455,0.46,0.465,0.47,
0.475,0.48,0.485,0.49,0.495,0.5,0.505,0.51,0.515,0.52,0.525,0.53,0.535,
0.54,0.545,0.55,0.555,0.56,0.565,0.57,0.575,0.58,0.585,0.59,0.595,0.6,0.605,
0.61,0.615,0.62,0.625,0.63,0.635,0.64,0.645,0.65,0.655,0.66,0.665,0.67,
0.675,0.68,0.685,0.690000000000001,0.695000000000001,0.700000000000001,
0.705000000000001,0.710000000000001,0.715000000000001,0.720000000000001,
0.725000000000001,0.730000000000001,0.735000000000001,0.740000000000001,
0.745000000000001,0.750000000000001,0.755000000000001,0.760000000000001,
0.765000000000001,0.770000000000001,0.775000000000001,0.780000000000001,
0.785000000000001,0.790000000000001,0.795000000000001,0.800000000000001,
0.805000000000001,0.810000000000001,0.815000000000001,0.820000000000001,
0.825000000000001,0.830000000000001,0.835000000000001,0.840000000000001,
0.845000000000001,0.850000000000001,0.855000000000001,0.860000000000001,
0.865000000000001,0.870000000000001,0.875000000000001,0.880000000000001,
0.885000000000001,0.890000000000001,0.895000000000001,0.900000000000001,
0.905000000000001,0.910000000000001,0.915000000000001,0.920000000000001,
0.925000000000001,0.930000000000001,0.935000000000001,0.940000000000001,
0.945000000000001,0.950000000000001,0.955000000000001,0.960000000000001,
0.965000000000001,0.970000000000001,0.975000000000001,0.980000000000001,
0.985000000000001,0.990000000000001,0.995000000000001,1.),.UNSPECIFIED.)
CURVE()
GEOMETRIC_REPRESENTATION_ITEM()
RATIONAL_B_SPLINE_CURVE((1.,1.,1.,1.,1.,1.,1.,1.,1.,1.,1.,1.,1.,1.,1.,1.,
1.,1.,1.,1.,1.,1.,1.,1.,1.,1.,1.,1.,1.,1.,1.,1.,1.,1.,1.,1.,1.,1.,1.,1.,
1.,1.,1.,1.,1.,1.,1.,1.,1.,1.,1.,1.,1.,1.,1.,1.,1.,1.,1.,1.,1.,1.,1.,1.,
1.,1.,1.,1.,1.,1.,1.,1.,1.,1.,1.,1.,1.,1.,1.,1.,1.,1.,1.,1.,1.,1.,1.,1.,
1.,1.,1.,1.,1.,1.,1.,1.,1.,1.,1.,1.,1.,1.,1.,1.,1.,1.,1.,1.,1.,1.,1.,1.,
1.,1.,1.,1.,1.,1.,1.,1.,1.,1.,1.,1.,1.,1.,1.,1.,1.,1.,1.,1.,1.,1.,1.,1.,
1.,1.,1.,1.,1.,1.,1.,1.,1.,1.,1.,1.,1.,1.,1.,1.,1.,1.,1.,1.,1.,1.,1.,1.,
1.,1.,1.,1.,1.,1.,1.,1.,1.,1.,1.,1.,1.,1.,1.,1.,1.,1.,1.,1.,1.,1.,1.,1.,
1.,1.,1.,1.,1.,1.,1.,1.,1.,1.,1.,1.,1.,1.,1.,1.,1.,1.,1.,1.,1.))
REPRESENTATION_ITEM('')
);
#802=(
BOUNDED_CURVE()
B_SPLINE_CURVE(5,(#222404,#222405,#222406,#222407,#222408,#222409,#222410,
#222411,#222412,#222413,#222414,#222415,#222416,#222417,#222418,#222419,
#222420,#222421,#222422,#222423,#222424,#222425,#222426,#222427,#222428,
#222429,#222430,#222431,#222432,#222433,#222434,#222435,#222436,#222437,
#222438,#222439,#222440,#222441,#222442,#222443,#222444,#222445,#222446,
#222447,#222448,#222449,#222450,#222451,#222452,#222453,#222454,#222455,
#222456,#222457,#222458,#222459,#222460,#222461,#222462,#222463,#222464,
#222465,#222466,#222467,#222468,#222469,#222470,#222471,#222472,#222473,
#222474,#222475,#222476,#222477,#222478,#222479,#222480,#222481,#222482,
#222483,#222484,#222485,#222486,#222487,#222488,#222489,#222490,#222491,
#222492,#222493,#222494,#222495,#222496,#222497,#222498,#222499,#222500,
#222501,#222502,#222503,#222504,#222505,#222506,#222507,#222508,#222509,
#222510,#222511,#222512,#222513,#222514,#222515,#222516,#222517,#222518,
#222519,#222520,#222521,#222522,#222523,#222524,#222525,#222526,#222527,
#222528,#222529,#222530,#222531,#222532,#222533,#222534,#222535,#222536,
#222537,#222538,#222539,#222540,#222541,#222542,#222543,#222544,#222545,
#222546,#222547,#222548,#222549,#222550,#222551,#222552,#222553,#222554,
#222555,#222556,#222557,#222558,#222559,#222560,#222561,#222562,#222563,
#222564,#222565,#222566,#222567,#222568,#222569,#222570,#222571,#222572,
#222573,#222574,#222575,#222576,#222577,#222578,#222579,#222580,#222581,
#222582,#222583,#222584,#222585,#222586,#222587,#222588,#222589,#222590,
#222591,#222592,#222593,#222594,#222595,#222596,#222597,#222598,#222599,
#222600,#222601,#222602,#222603,#222604,#222605,#222606,#222607,#222608),
 .UNSPECIFIED.,.F.,.F.)
B_SPLINE_CURVE_WITH_KNOTS((6,1,1,1,1,1,1,1,1,1,1,1,1,1,1,1,1,1,1,1,1,1,
1,1,1,1,1,1,1,1,1,1,1,1,1,1,1,1,1,1,1,1,1,1,1,1,1,1,1,1,1,1,1,1,1,1,1,1,
1,1,1,1,1,1,1,1,1,1,1,1,1,1,1,1,1,1,1,1,1,1,1,1,1,1,1,1,1,1,1,1,1,1,1,1,
1,1,1,1,1,1,1,1,1,1,1,1,1,1,1,1,1,1,1,1,1,1,1,1,1,1,1,1,1,1,1,1,1,1,1,1,
1,1,1,1,1,1,1,1,1,1,1,1,1,1,1,1,1,1,1,1,1,1,1,1,1,1,1,1,1,1,1,1,1,1,1,1,
1,1,1,1,1,1,1,1,1,1,1,1,1,1,1,1,1,1,1,1,1,1,1,1,1,1,1,1,1,1,1,1,1,1,6),
(-1.,-0.995000000000001,-0.990000000000001,-0.985000000000001,-0.980000000000001,
-0.975000000000001,-0.970000000000001,-0.965000000000001,-0.960000000000001,
-0.955000000000001,-0.950000000000001,-0.945000000000001,-0.940000000000001,
-0.935000000000001,-0.930000000000001,-0.925000000000001,-0.920000000000001,
-0.915000000000001,-0.910000000000001,-0.905000000000001,-0.900000000000001,
-0.895000000000001,-0.890000000000001,-0.885000000000001,-0.880000000000001,
-0.875000000000001,-0.870000000000001,-0.865000000000001,-0.860000000000001,
-0.855000000000001,-0.850000000000001,-0.845000000000001,-0.840000000000001,
-0.835000000000001,-0.830000000000001,-0.825000000000001,-0.820000000000001,
-0.815000000000001,-0.810000000000001,-0.805000000000001,-0.800000000000001,
-0.795000000000001,-0.790000000000001,-0.785000000000001,-0.780000000000001,
-0.775000000000001,-0.770000000000001,-0.765000000000001,-0.760000000000001,
-0.755000000000001,-0.750000000000001,-0.745000000000001,-0.740000000000001,
-0.735000000000001,-0.730000000000001,-0.725000000000001,-0.720000000000001,
-0.715000000000001,-0.710000000000001,-0.705000000000001,-0.700000000000001,
-0.695000000000001,-0.690000000000001,-0.685,-0.68,-0.675,-0.67,-0.665,
-0.66,-0.655,-0.65,-0.645,-0.64,-0.635,-0.63,-0.625,-0.62,-0.615,-0.61,
-0.605,-0.6,-0.595,-0.59,-0.585,-0.58,-0.575,-0.57,-0.565,-0.56,-0.555,
-0.55,-0.545,-0.54,-0.535,-0.53,-0.525,-0.52,-0.515,-0.51,-0.505,-0.5,-0.495,
-0.49,-0.485,-0.48,-0.475,-0.47,-0.465,-0.46,-0.455,-0.45,-0.445,-0.44,
-0.435,-0.43,-0.425,-0.42,-0.415,-0.41,-0.405,-0.4,-0.395,-0.39,-0.385,
-0.38,-0.375,-0.37,-0.365,-0.36,-0.355,-0.35,-0.345,-0.34,-0.335,-0.33,
-0.325,-0.32,-0.315,-0.31,-0.305,-0.3,-0.295,-0.29,-0.285,-0.28,-0.275,
-0.27,-0.265,-0.26,-0.255,-0.25,-0.245,-0.24,-0.235,-0.23,-0.225,-0.22,
-0.215,-0.21,-0.205,-0.2,-0.195,-0.19,-0.185,-0.18,-0.175,-0.17,-0.165,
-0.16,-0.155,-0.15,-0.145,-0.14,-0.135,-0.13,-0.125,-0.12,-0.115,-0.11,
-0.105,-0.1,-0.095,-0.09,-0.085,-0.08,-0.075,-0.07,-0.065,-0.06,-0.055,
-0.05,-0.045,-0.04,-0.035,-0.03,-0.025,-0.02,-0.015,-0.01,-0.005,0.),
 .UNSPECIFIED.)
CURVE()
GEOMETRIC_REPRESENTATION_ITEM()
RATIONAL_B_SPLINE_CURVE((1.,1.,1.,1.,1.,1.,1.,1.,1.,1.,1.,1.,1.,1.,1.,1.,
1.,1.,1.,1.,1.,1.,1.,1.,1.,1.,1.,1.,1.,1.,1.,1.,1.,1.,1.,1.,1.,1.,1.,1.,
1.,1.,1.,1.,1.,1.,1.,1.,1.,1.,1.,1.,1.,1.,1.,1.,1.,1.,1.,1.,1.,1.,1.,1.,
1.,1.,1.,1.,1.,1.,1.,1.,1.,1.,1.,1.,1.,1.,1.,1.,1.,1.,1.,1.,1.,1.,1.,1.,
1.,1.,1.,1.,1.,1.,1.,1.,1.,1.,1.,1.,1.,1.,1.,1.,1.,1.,1.,1.,1.,1.,1.,1.,
1.,1.,1.,1.,1.,1.,1.,1.,1.,1.,1.,1.,1.,1.,1.,1.,1.,1.,1.,1.,1.,1.,1.,1.,
1.,1.,1.,1.,1.,1.,1.,1.,1.,1.,1.,1.,1.,1.,1.,1.,1.,1.,1.,1.,1.,1.,1.,1.,
1.,1.,1.,1.,1.,1.,1.,1.,1.,1.,1.,1.,1.,1.,1.,1.,1.,1.,1.,1.,1.,1.,1.,1.,
1.,1.,1.,1.,1.,1.,1.,1.,1.,1.,1.,1.,1.,1.,1.,1.,1.,1.,1.,1.,1.))
REPRESENTATION_ITEM('')
);
#803=(
BOUNDED_CURVE()
B_SPLINE_CURVE(5,(#223027,#223028,#223029,#223030,#223031,#223032,#223033,
#223034,#223035,#223036,#223037,#223038,#223039,#223040,#223041,#223042,
#223043,#223044,#223045,#223046,#223047,#223048,#223049,#223050,#223051,
#223052,#223053,#223054,#223055,#223056,#223057,#223058,#223059,#223060,
#223061,#223062,#223063,#223064,#223065,#223066,#223067,#223068,#223069,
#223070,#223071,#223072,#223073,#223074,#223075,#223076,#223077,#223078,
#223079,#223080,#223081,#223082,#223083,#223084,#223085,#223086,#223087,
#223088,#223089,#223090,#223091,#223092,#223093,#223094,#223095,#223096,
#223097,#223098,#223099,#223100,#223101,#223102,#223103,#223104,#223105,
#223106,#223107,#223108,#223109,#223110,#223111,#223112,#223113,#223114,
#223115,#223116,#223117,#223118,#223119,#223120,#223121,#223122,#223123,
#223124,#223125,#223126,#223127,#223128,#223129,#223130,#223131,#223132,
#223133,#223134,#223135,#223136,#223137,#223138,#223139,#223140,#223141,
#223142,#223143,#223144,#223145,#223146,#223147,#223148,#223149,#223150,
#223151,#223152,#223153,#223154,#223155,#223156,#223157,#223158,#223159,
#223160,#223161,#223162,#223163,#223164,#223165,#223166,#223167,#223168,
#223169,#223170,#223171,#223172,#223173,#223174,#223175,#223176,#223177,
#223178,#223179,#223180,#223181,#223182,#223183,#223184,#223185,#223186,
#223187,#223188,#223189,#223190,#223191,#223192,#223193,#223194,#223195,
#223196,#223197,#223198,#223199,#223200,#223201,#223202,#223203,#223204,
#223205,#223206,#223207,#223208,#223209,#223210,#223211,#223212,#223213,
#223214,#223215,#223216,#223217,#223218,#223219,#223220,#223221,#223222,
#223223,#223224,#223225,#223226,#223227,#223228,#223229,#223230,#223231),
 .UNSPECIFIED.,.F.,.F.)
B_SPLINE_CURVE_WITH_KNOTS((6,1,1,1,1,1,1,1,1,1,1,1,1,1,1,1,1,1,1,1,1,1,
1,1,1,1,1,1,1,1,1,1,1,1,1,1,1,1,1,1,1,1,1,1,1,1,1,1,1,1,1,1,1,1,1,1,1,1,
1,1,1,1,1,1,1,1,1,1,1,1,1,1,1,1,1,1,1,1,1,1,1,1,1,1,1,1,1,1,1,1,1,1,1,1,
1,1,1,1,1,1,1,1,1,1,1,1,1,1,1,1,1,1,1,1,1,1,1,1,1,1,1,1,1,1,1,1,1,1,1,1,
1,1,1,1,1,1,1,1,1,1,1,1,1,1,1,1,1,1,1,1,1,1,1,1,1,1,1,1,1,1,1,1,1,1,1,1,
1,1,1,1,1,1,1,1,1,1,1,1,1,1,1,1,1,1,1,1,1,1,1,1,1,1,1,1,1,1,1,1,1,1,6),
(-1.,-0.995000000000001,-0.990000000000001,-0.985000000000001,-0.980000000000001,
-0.975000000000001,-0.970000000000001,-0.965000000000001,-0.960000000000001,
-0.955000000000001,-0.950000000000001,-0.945000000000001,-0.940000000000001,
-0.935000000000001,-0.930000000000001,-0.925000000000001,-0.920000000000001,
-0.915000000000001,-0.910000000000001,-0.905000000000001,-0.900000000000001,
-0.895000000000001,-0.890000000000001,-0.885000000000001,-0.880000000000001,
-0.875000000000001,-0.870000000000001,-0.865000000000001,-0.860000000000001,
-0.855000000000001,-0.850000000000001,-0.845000000000001,-0.840000000000001,
-0.835000000000001,-0.830000000000001,-0.825000000000001,-0.820000000000001,
-0.815000000000001,-0.810000000000001,-0.805000000000001,-0.800000000000001,
-0.795000000000001,-0.790000000000001,-0.785000000000001,-0.780000000000001,
-0.775000000000001,-0.770000000000001,-0.765000000000001,-0.760000000000001,
-0.755000000000001,-0.750000000000001,-0.745000000000001,-0.740000000000001,
-0.735000000000001,-0.730000000000001,-0.725000000000001,-0.720000000000001,
-0.715000000000001,-0.710000000000001,-0.705000000000001,-0.700000000000001,
-0.695000000000001,-0.690000000000001,-0.685,-0.68,-0.675,-0.67,-0.665,
-0.66,-0.655,-0.65,-0.645,-0.64,-0.635,-0.63,-0.625,-0.62,-0.615,-0.61,
-0.605,-0.6,-0.595,-0.59,-0.585,-0.58,-0.575,-0.57,-0.565,-0.56,-0.555,
-0.55,-0.545,-0.54,-0.535,-0.53,-0.525,-0.52,-0.515,-0.51,-0.505,-0.5,-0.495,
-0.49,-0.485,-0.48,-0.475,-0.47,-0.465,-0.46,-0.455,-0.45,-0.445,-0.44,
-0.435,-0.43,-0.425,-0.42,-0.415,-0.41,-0.405,-0.4,-0.395,-0.39,-0.385,
-0.38,-0.375,-0.37,-0.365,-0.36,-0.355,-0.35,-0.345,-0.34,-0.335,-0.33,
-0.325,-0.32,-0.315,-0.31,-0.305,-0.3,-0.295,-0.29,-0.285,-0.28,-0.275,
-0.27,-0.265,-0.26,-0.255,-0.25,-0.245,-0.24,-0.235,-0.23,-0.225,-0.22,
-0.215,-0.21,-0.205,-0.2,-0.195,-0.19,-0.185,-0.18,-0.175,-0.17,-0.165,
-0.16,-0.155,-0.15,-0.145,-0.14,-0.135,-0.13,-0.125,-0.12,-0.115,-0.11,
-0.105,-0.1,-0.095,-0.09,-0.085,-0.08,-0.075,-0.07,-0.065,-0.06,-0.055,
-0.05,-0.045,-0.04,-0.035,-0.03,-0.025,-0.02,-0.015,-0.01,-0.005,0.),
 .UNSPECIFIED.)
CURVE()
GEOMETRIC_REPRESENTATION_ITEM()
RATIONAL_B_SPLINE_CURVE((1.,1.,1.,1.,1.,1.,1.,1.,1.,1.,1.,1.,1.,1.,1.,1.,
1.,1.,1.,1.,1.,1.,1.,1.,1.,1.,1.,1.,1.,1.,1.,1.,1.,1.,1.,1.,1.,1.,1.,1.,
1.,1.,1.,1.,1.,1.,1.,1.,1.,1.,1.,1.,1.,1.,1.,1.,1.,1.,1.,1.,1.,1.,1.,1.,
1.,1.,1.,1.,1.,1.,1.,1.,1.,1.,1.,1.,1.,1.,1.,1.,1.,1.,1.,1.,1.,1.,1.,1.,
1.,1.,1.,1.,1.,1.,1.,1.,1.,1.,1.,1.,1.,1.,1.,1.,1.,1.,1.,1.,1.,1.,1.,1.,
1.,1.,1.,1.,1.,1.,1.,1.,1.,1.,1.,1.,1.,1.,1.,1.,1.,1.,1.,1.,1.,1.,1.,1.,
1.,1.,1.,1.,1.,1.,1.,1.,1.,1.,1.,1.,1.,1.,1.,1.,1.,1.,1.,1.,1.,1.,1.,1.,
1.,1.,1.,1.,1.,1.,1.,1.,1.,1.,1.,1.,1.,1.,1.,1.,1.,1.,1.,1.,1.,1.,1.,1.,
1.,1.,1.,1.,1.,1.,1.,1.,1.,1.,1.,1.,1.,1.,1.,1.,1.,1.,1.,1.,1.))
REPRESENTATION_ITEM('')
);
#804=(
BOUNDED_CURVE()
B_SPLINE_CURVE(5,(#223234,#223235,#223236,#223237,#223238,#223239,#223240,
#223241,#223242,#223243,#223244,#223245,#223246,#223247,#223248,#223249,
#223250,#223251,#223252,#223253,#223254,#223255,#223256,#223257,#223258,
#223259,#223260,#223261,#223262,#223263,#223264,#223265,#223266,#223267,
#223268,#223269,#223270,#223271,#223272,#223273,#223274,#223275,#223276,
#223277,#223278,#223279,#223280,#223281,#223282,#223283,#223284,#223285,
#223286,#223287,#223288,#223289,#223290,#223291,#223292,#223293,#223294,
#223295,#223296,#223297,#223298,#223299,#223300,#223301,#223302,#223303,
#223304,#223305,#223306,#223307,#223308,#223309,#223310,#223311,#223312,
#223313,#223314,#223315,#223316,#223317,#223318,#223319,#223320,#223321,
#223322,#223323,#223324,#223325,#223326,#223327,#223328,#223329,#223330,
#223331,#223332,#223333,#223334,#223335,#223336,#223337,#223338,#223339,
#223340,#223341,#223342,#223343,#223344,#223345,#223346,#223347,#223348,
#223349,#223350,#223351,#223352,#223353,#223354,#223355,#223356,#223357,
#223358,#223359,#223360,#223361,#223362,#223363,#223364,#223365,#223366,
#223367,#223368,#223369,#223370,#223371,#223372,#223373,#223374,#223375,
#223376,#223377,#223378,#223379,#223380,#223381,#223382,#223383,#223384,
#223385,#223386,#223387,#223388,#223389,#223390,#223391,#223392,#223393,
#223394,#223395,#223396,#223397,#223398,#223399,#223400,#223401,#223402,
#223403,#223404,#223405,#223406,#223407,#223408,#223409,#223410,#223411,
#223412,#223413,#223414,#223415,#223416,#223417,#223418,#223419,#223420,
#223421,#223422,#223423,#223424,#223425,#223426,#223427,#223428,#223429,
#223430,#223431,#223432,#223433,#223434,#223435,#223436,#223437,#223438),
 .UNSPECIFIED.,.F.,.F.)
B_SPLINE_CURVE_WITH_KNOTS((6,1,1,1,1,1,1,1,1,1,1,1,1,1,1,1,1,1,1,1,1,1,
1,1,1,1,1,1,1,1,1,1,1,1,1,1,1,1,1,1,1,1,1,1,1,1,1,1,1,1,1,1,1,1,1,1,1,1,
1,1,1,1,1,1,1,1,1,1,1,1,1,1,1,1,1,1,1,1,1,1,1,1,1,1,1,1,1,1,1,1,1,1,1,1,
1,1,1,1,1,1,1,1,1,1,1,1,1,1,1,1,1,1,1,1,1,1,1,1,1,1,1,1,1,1,1,1,1,1,1,1,
1,1,1,1,1,1,1,1,1,1,1,1,1,1,1,1,1,1,1,1,1,1,1,1,1,1,1,1,1,1,1,1,1,1,1,1,
1,1,1,1,1,1,1,1,1,1,1,1,1,1,1,1,1,1,1,1,1,1,1,1,1,1,1,1,1,1,1,1,1,1,6),
(0.,0.005,0.01,0.015,0.02,0.025,0.03,0.035,0.04,0.045,0.05,0.055,0.06,0.065,
0.07,0.075,0.08,0.085,0.09,0.095,0.1,0.105,0.11,0.115,0.12,0.125,0.13,0.135,
0.14,0.145,0.15,0.155,0.16,0.165,0.17,0.175,0.18,0.185,0.19,0.195,0.2,0.205,
0.21,0.215,0.22,0.225,0.23,0.235,0.24,0.245,0.25,0.255,0.26,0.265,0.27,
0.275,0.28,0.285,0.29,0.295,0.3,0.305,0.31,0.315,0.32,0.325,0.33,0.335,
0.34,0.345,0.35,0.355,0.36,0.365,0.37,0.375,0.38,0.385,0.39,0.395,0.4,0.405,
0.41,0.415,0.42,0.425,0.43,0.435,0.44,0.445,0.45,0.455,0.46,0.465,0.47,
0.475,0.48,0.485,0.49,0.495,0.5,0.505,0.51,0.515,0.52,0.525,0.53,0.535,
0.54,0.545,0.55,0.555,0.56,0.565,0.57,0.575,0.58,0.585,0.59,0.595,0.6,0.605,
0.61,0.615,0.62,0.625,0.63,0.635,0.64,0.645,0.65,0.655,0.66,0.665,0.67,
0.675,0.68,0.685,0.690000000000001,0.695000000000001,0.700000000000001,
0.705000000000001,0.710000000000001,0.715000000000001,0.720000000000001,
0.725000000000001,0.730000000000001,0.735000000000001,0.740000000000001,
0.745000000000001,0.750000000000001,0.755000000000001,0.760000000000001,
0.765000000000001,0.770000000000001,0.775000000000001,0.780000000000001,
0.785000000000001,0.790000000000001,0.795000000000001,0.800000000000001,
0.805000000000001,0.810000000000001,0.815000000000001,0.820000000000001,
0.825000000000001,0.830000000000001,0.835000000000001,0.840000000000001,
0.845000000000001,0.850000000000001,0.855000000000001,0.860000000000001,
0.865000000000001,0.870000000000001,0.875000000000001,0.880000000000001,
0.885000000000001,0.890000000000001,0.895000000000001,0.900000000000001,
0.905000000000001,0.910000000000001,0.915000000000001,0.920000000000001,
0.925000000000001,0.930000000000001,0.935000000000001,0.940000000000001,
0.945000000000001,0.950000000000001,0.955000000000001,0.960000000000001,
0.965000000000001,0.970000000000001,0.975000000000001,0.980000000000001,
0.985000000000001,0.990000000000001,0.995000000000001,1.),.UNSPECIFIED.)
CURVE()
GEOMETRIC_REPRESENTATION_ITEM()
RATIONAL_B_SPLINE_CURVE((1.,1.,1.,1.,1.,1.,1.,1.,1.,1.,1.,1.,1.,1.,1.,1.,
1.,1.,1.,1.,1.,1.,1.,1.,1.,1.,1.,1.,1.,1.,1.,1.,1.,1.,1.,1.,1.,1.,1.,1.,
1.,1.,1.,1.,1.,1.,1.,1.,1.,1.,1.,1.,1.,1.,1.,1.,1.,1.,1.,1.,1.,1.,1.,1.,
1.,1.,1.,1.,1.,1.,1.,1.,1.,1.,1.,1.,1.,1.,1.,1.,1.,1.,1.,1.,1.,1.,1.,1.,
1.,1.,1.,1.,1.,1.,1.,1.,1.,1.,1.,1.,1.,1.,1.,1.,1.,1.,1.,1.,1.,1.,1.,1.,
1.,1.,1.,1.,1.,1.,1.,1.,1.,1.,1.,1.,1.,1.,1.,1.,1.,1.,1.,1.,1.,1.,1.,1.,
1.,1.,1.,1.,1.,1.,1.,1.,1.,1.,1.,1.,1.,1.,1.,1.,1.,1.,1.,1.,1.,1.,1.,1.,
1.,1.,1.,1.,1.,1.,1.,1.,1.,1.,1.,1.,1.,1.,1.,1.,1.,1.,1.,1.,1.,1.,1.,1.,
1.,1.,1.,1.,1.,1.,1.,1.,1.,1.,1.,1.,1.,1.,1.,1.,1.,1.,1.,1.,1.))
REPRESENTATION_ITEM('')
);
#805=(
BOUNDED_CURVE()
B_SPLINE_CURVE(5,(#223850,#223851,#223852,#223853,#223854,#223855,#223856,
#223857,#223858,#223859,#223860,#223861,#223862,#223863,#223864,#223865,
#223866,#223867,#223868,#223869,#223870,#223871,#223872,#223873,#223874,
#223875,#223876,#223877,#223878,#223879,#223880,#223881,#223882,#223883,
#223884,#223885,#223886,#223887,#223888,#223889,#223890,#223891,#223892,
#223893,#223894,#223895,#223896,#223897,#223898,#223899,#223900,#223901,
#223902,#223903,#223904,#223905,#223906,#223907,#223908,#223909,#223910,
#223911,#223912,#223913,#223914,#223915,#223916,#223917,#223918,#223919,
#223920,#223921,#223922,#223923,#223924,#223925,#223926,#223927,#223928,
#223929,#223930,#223931,#223932,#223933,#223934,#223935,#223936,#223937,
#223938,#223939,#223940,#223941,#223942,#223943,#223944,#223945,#223946,
#223947,#223948,#223949,#223950,#223951,#223952,#223953,#223954,#223955,
#223956,#223957,#223958,#223959,#223960,#223961,#223962,#223963,#223964,
#223965,#223966,#223967,#223968,#223969,#223970,#223971,#223972,#223973,
#223974,#223975,#223976,#223977,#223978,#223979,#223980,#223981,#223982,
#223983,#223984,#223985,#223986,#223987,#223988,#223989,#223990,#223991,
#223992,#223993,#223994,#223995,#223996,#223997,#223998,#223999,#224000,
#224001,#224002,#224003,#224004,#224005,#224006,#224007,#224008,#224009,
#224010,#224011,#224012,#224013,#224014,#224015,#224016,#224017,#224018,
#224019,#224020,#224021,#224022,#224023,#224024,#224025,#224026,#224027,
#224028,#224029,#224030,#224031,#224032,#224033,#224034,#224035,#224036,
#224037,#224038,#224039,#224040,#224041,#224042,#224043,#224044,#224045,
#224046,#224047,#224048,#224049,#224050,#224051,#224052,#224053,#224054),
 .UNSPECIFIED.,.F.,.F.)
B_SPLINE_CURVE_WITH_KNOTS((6,1,1,1,1,1,1,1,1,1,1,1,1,1,1,1,1,1,1,1,1,1,
1,1,1,1,1,1,1,1,1,1,1,1,1,1,1,1,1,1,1,1,1,1,1,1,1,1,1,1,1,1,1,1,1,1,1,1,
1,1,1,1,1,1,1,1,1,1,1,1,1,1,1,1,1,1,1,1,1,1,1,1,1,1,1,1,1,1,1,1,1,1,1,1,
1,1,1,1,1,1,1,1,1,1,1,1,1,1,1,1,1,1,1,1,1,1,1,1,1,1,1,1,1,1,1,1,1,1,1,1,
1,1,1,1,1,1,1,1,1,1,1,1,1,1,1,1,1,1,1,1,1,1,1,1,1,1,1,1,1,1,1,1,1,1,1,1,
1,1,1,1,1,1,1,1,1,1,1,1,1,1,1,1,1,1,1,1,1,1,1,1,1,1,1,1,1,1,1,1,1,1,6),
(0.,0.005,0.01,0.015,0.02,0.025,0.03,0.035,0.04,0.045,0.05,0.055,0.06,0.065,
0.07,0.075,0.08,0.085,0.09,0.095,0.1,0.105,0.11,0.115,0.12,0.125,0.13,0.135,
0.14,0.145,0.15,0.155,0.16,0.165,0.17,0.175,0.18,0.185,0.19,0.195,0.2,0.205,
0.21,0.215,0.22,0.225,0.23,0.235,0.24,0.245,0.25,0.255,0.26,0.265,0.27,
0.275,0.28,0.285,0.29,0.295,0.3,0.305,0.31,0.315,0.32,0.325,0.33,0.335,
0.34,0.345,0.35,0.355,0.36,0.365,0.37,0.375,0.38,0.385,0.39,0.395,0.4,0.405,
0.41,0.415,0.42,0.425,0.43,0.435,0.44,0.445,0.45,0.455,0.46,0.465,0.47,
0.475,0.48,0.485,0.49,0.495,0.5,0.505,0.51,0.515,0.52,0.525,0.53,0.535,
0.54,0.545,0.55,0.555,0.56,0.565,0.57,0.575,0.58,0.585,0.59,0.595,0.6,0.605,
0.61,0.615,0.62,0.625,0.63,0.635,0.64,0.645,0.65,0.655,0.66,0.665,0.67,
0.675,0.68,0.685,0.690000000000001,0.695000000000001,0.700000000000001,
0.705000000000001,0.710000000000001,0.715000000000001,0.720000000000001,
0.725000000000001,0.730000000000001,0.735000000000001,0.740000000000001,
0.745000000000001,0.750000000000001,0.755000000000001,0.760000000000001,
0.765000000000001,0.770000000000001,0.775000000000001,0.780000000000001,
0.785000000000001,0.790000000000001,0.795000000000001,0.800000000000001,
0.805000000000001,0.810000000000001,0.815000000000001,0.820000000000001,
0.825000000000001,0.830000000000001,0.835000000000001,0.840000000000001,
0.845000000000001,0.850000000000001,0.855000000000001,0.860000000000001,
0.865000000000001,0.870000000000001,0.875000000000001,0.880000000000001,
0.885000000000001,0.890000000000001,0.895000000000001,0.900000000000001,
0.905000000000001,0.910000000000001,0.915000000000001,0.920000000000001,
0.925000000000001,0.930000000000001,0.935000000000001,0.940000000000001,
0.945000000000001,0.950000000000001,0.955000000000001,0.960000000000001,
0.965000000000001,0.970000000000001,0.975000000000001,0.980000000000001,
0.985000000000001,0.990000000000001,0.995000000000001,1.),.UNSPECIFIED.)
CURVE()
GEOMETRIC_REPRESENTATION_ITEM()
RATIONAL_B_SPLINE_CURVE((1.,1.,1.,1.,1.,1.,1.,1.,1.,1.,1.,1.,1.,1.,1.,1.,
1.,1.,1.,1.,1.,1.,1.,1.,1.,1.,1.,1.,1.,1.,1.,1.,1.,1.,1.,1.,1.,1.,1.,1.,
1.,1.,1.,1.,1.,1.,1.,1.,1.,1.,1.,1.,1.,1.,1.,1.,1.,1.,1.,1.,1.,1.,1.,1.,
1.,1.,1.,1.,1.,1.,1.,1.,1.,1.,1.,1.,1.,1.,1.,1.,1.,1.,1.,1.,1.,1.,1.,1.,
1.,1.,1.,1.,1.,1.,1.,1.,1.,1.,1.,1.,1.,1.,1.,1.,1.,1.,1.,1.,1.,1.,1.,1.,
1.,1.,1.,1.,1.,1.,1.,1.,1.,1.,1.,1.,1.,1.,1.,1.,1.,1.,1.,1.,1.,1.,1.,1.,
1.,1.,1.,1.,1.,1.,1.,1.,1.,1.,1.,1.,1.,1.,1.,1.,1.,1.,1.,1.,1.,1.,1.,1.,
1.,1.,1.,1.,1.,1.,1.,1.,1.,1.,1.,1.,1.,1.,1.,1.,1.,1.,1.,1.,1.,1.,1.,1.,
1.,1.,1.,1.,1.,1.,1.,1.,1.,1.,1.,1.,1.,1.,1.,1.,1.,1.,1.,1.,1.))
REPRESENTATION_ITEM('')
);
#806=(
BOUNDED_CURVE()
B_SPLINE_CURVE(5,(#224056,#224057,#224058,#224059,#224060,#224061,#224062,
#224063,#224064,#224065,#224066,#224067,#224068,#224069,#224070,#224071,
#224072,#224073,#224074,#224075,#224076,#224077,#224078,#224079,#224080,
#224081,#224082,#224083,#224084,#224085,#224086,#224087,#224088,#224089,
#224090,#224091,#224092,#224093,#224094,#224095,#224096,#224097,#224098,
#224099,#224100,#224101,#224102,#224103,#224104,#224105,#224106,#224107,
#224108,#224109,#224110,#224111,#224112,#224113,#224114,#224115,#224116,
#224117,#224118,#224119,#224120,#224121,#224122,#224123,#224124,#224125,
#224126,#224127,#224128,#224129,#224130,#224131,#224132,#224133,#224134,
#224135,#224136,#224137,#224138,#224139,#224140,#224141,#224142,#224143,
#224144,#224145,#224146,#224147,#224148,#224149,#224150,#224151,#224152,
#224153,#224154,#224155,#224156,#224157,#224158,#224159,#224160,#224161,
#224162,#224163,#224164,#224165,#224166,#224167,#224168,#224169,#224170,
#224171,#224172,#224173,#224174,#224175,#224176,#224177,#224178,#224179,
#224180,#224181,#224182,#224183,#224184,#224185,#224186,#224187,#224188,
#224189,#224190,#224191,#224192,#224193,#224194,#224195,#224196,#224197,
#224198,#224199,#224200,#224201,#224202,#224203,#224204,#224205,#224206,
#224207,#224208,#224209,#224210,#224211,#224212,#224213,#224214,#224215,
#224216,#224217,#224218,#224219,#224220,#224221,#224222,#224223,#224224,
#224225,#224226,#224227,#224228,#224229,#224230,#224231,#224232,#224233,
#224234,#224235,#224236,#224237,#224238,#224239,#224240,#224241,#224242,
#224243,#224244,#224245,#224246,#224247,#224248,#224249,#224250,#224251,
#224252,#224253,#224254,#224255,#224256,#224257,#224258,#224259,#224260),
 .UNSPECIFIED.,.F.,.F.)
B_SPLINE_CURVE_WITH_KNOTS((6,1,1,1,1,1,1,1,1,1,1,1,1,1,1,1,1,1,1,1,1,1,
1,1,1,1,1,1,1,1,1,1,1,1,1,1,1,1,1,1,1,1,1,1,1,1,1,1,1,1,1,1,1,1,1,1,1,1,
1,1,1,1,1,1,1,1,1,1,1,1,1,1,1,1,1,1,1,1,1,1,1,1,1,1,1,1,1,1,1,1,1,1,1,1,
1,1,1,1,1,1,1,1,1,1,1,1,1,1,1,1,1,1,1,1,1,1,1,1,1,1,1,1,1,1,1,1,1,1,1,1,
1,1,1,1,1,1,1,1,1,1,1,1,1,1,1,1,1,1,1,1,1,1,1,1,1,1,1,1,1,1,1,1,1,1,1,1,
1,1,1,1,1,1,1,1,1,1,1,1,1,1,1,1,1,1,1,1,1,1,1,1,1,1,1,1,1,1,1,1,1,1,6),
(-1.,-0.995000000000001,-0.990000000000001,-0.985000000000001,-0.980000000000001,
-0.975000000000001,-0.970000000000001,-0.965000000000001,-0.960000000000001,
-0.955000000000001,-0.950000000000001,-0.945000000000001,-0.940000000000001,
-0.935000000000001,-0.930000000000001,-0.925000000000001,-0.920000000000001,
-0.915000000000001,-0.910000000000001,-0.905000000000001,-0.900000000000001,
-0.895000000000001,-0.890000000000001,-0.885000000000001,-0.880000000000001,
-0.875000000000001,-0.870000000000001,-0.865000000000001,-0.860000000000001,
-0.855000000000001,-0.850000000000001,-0.845000000000001,-0.840000000000001,
-0.835000000000001,-0.830000000000001,-0.825000000000001,-0.820000000000001,
-0.815000000000001,-0.810000000000001,-0.805000000000001,-0.800000000000001,
-0.795000000000001,-0.790000000000001,-0.785000000000001,-0.780000000000001,
-0.775000000000001,-0.770000000000001,-0.765000000000001,-0.760000000000001,
-0.755000000000001,-0.750000000000001,-0.745000000000001,-0.740000000000001,
-0.735000000000001,-0.730000000000001,-0.725000000000001,-0.720000000000001,
-0.715000000000001,-0.710000000000001,-0.705000000000001,-0.700000000000001,
-0.695000000000001,-0.690000000000001,-0.685,-0.68,-0.675,-0.67,-0.665,
-0.66,-0.655,-0.65,-0.645,-0.64,-0.635,-0.63,-0.625,-0.62,-0.615,-0.61,
-0.605,-0.6,-0.595,-0.59,-0.585,-0.58,-0.575,-0.57,-0.565,-0.56,-0.555,
-0.55,-0.545,-0.54,-0.535,-0.53,-0.525,-0.52,-0.515,-0.51,-0.505,-0.5,-0.495,
-0.49,-0.485,-0.48,-0.475,-0.47,-0.465,-0.46,-0.455,-0.45,-0.445,-0.44,
-0.435,-0.43,-0.425,-0.42,-0.415,-0.41,-0.405,-0.4,-0.395,-0.39,-0.385,
-0.38,-0.375,-0.37,-0.365,-0.36,-0.355,-0.35,-0.345,-0.34,-0.335,-0.33,
-0.325,-0.32,-0.315,-0.31,-0.305,-0.3,-0.295,-0.29,-0.285,-0.28,-0.275,
-0.27,-0.265,-0.26,-0.255,-0.25,-0.245,-0.24,-0.235,-0.23,-0.225,-0.22,
-0.215,-0.21,-0.205,-0.2,-0.195,-0.19,-0.185,-0.18,-0.175,-0.17,-0.165,
-0.16,-0.155,-0.15,-0.145,-0.14,-0.135,-0.13,-0.125,-0.12,-0.115,-0.11,
-0.105,-0.1,-0.095,-0.09,-0.085,-0.08,-0.075,-0.07,-0.065,-0.06,-0.055,
-0.05,-0.045,-0.04,-0.035,-0.03,-0.025,-0.02,-0.015,-0.01,-0.005,0.),
 .UNSPECIFIED.)
CURVE()
GEOMETRIC_REPRESENTATION_ITEM()
RATIONAL_B_SPLINE_CURVE((1.,1.,1.,1.,1.,1.,1.,1.,1.,1.,1.,1.,1.,1.,1.,1.,
1.,1.,1.,1.,1.,1.,1.,1.,1.,1.,1.,1.,1.,1.,1.,1.,1.,1.,1.,1.,1.,1.,1.,1.,
1.,1.,1.,1.,1.,1.,1.,1.,1.,1.,1.,1.,1.,1.,1.,1.,1.,1.,1.,1.,1.,1.,1.,1.,
1.,1.,1.,1.,1.,1.,1.,1.,1.,1.,1.,1.,1.,1.,1.,1.,1.,1.,1.,1.,1.,1.,1.,1.,
1.,1.,1.,1.,1.,1.,1.,1.,1.,1.,1.,1.,1.,1.,1.,1.,1.,1.,1.,1.,1.,1.,1.,1.,
1.,1.,1.,1.,1.,1.,1.,1.,1.,1.,1.,1.,1.,1.,1.,1.,1.,1.,1.,1.,1.,1.,1.,1.,
1.,1.,1.,1.,1.,1.,1.,1.,1.,1.,1.,1.,1.,1.,1.,1.,1.,1.,1.,1.,1.,1.,1.,1.,
1.,1.,1.,1.,1.,1.,1.,1.,1.,1.,1.,1.,1.,1.,1.,1.,1.,1.,1.,1.,1.,1.,1.,1.,
1.,1.,1.,1.,1.,1.,1.,1.,1.,1.,1.,1.,1.,1.,1.,1.,1.,1.,1.,1.,1.))
REPRESENTATION_ITEM('')
);
#807=(
BOUNDED_CURVE()
B_SPLINE_CURVE(5,(#224679,#224680,#224681,#224682,#224683,#224684,#224685,
#224686,#224687,#224688,#224689,#224690,#224691,#224692,#224693,#224694,
#224695,#224696,#224697,#224698,#224699,#224700,#224701,#224702,#224703,
#224704,#224705,#224706,#224707,#224708,#224709,#224710,#224711,#224712,
#224713,#224714,#224715,#224716,#224717,#224718,#224719,#224720,#224721,
#224722,#224723,#224724,#224725,#224726,#224727,#224728,#224729,#224730,
#224731,#224732,#224733,#224734,#224735,#224736,#224737,#224738,#224739,
#224740,#224741,#224742,#224743,#224744,#224745,#224746,#224747,#224748,
#224749,#224750,#224751,#224752,#224753,#224754,#224755,#224756,#224757,
#224758,#224759,#224760,#224761,#224762,#224763,#224764,#224765,#224766,
#224767,#224768,#224769,#224770,#224771,#224772,#224773,#224774,#224775,
#224776,#224777,#224778,#224779,#224780,#224781,#224782,#224783,#224784,
#224785,#224786,#224787,#224788,#224789,#224790,#224791,#224792,#224793,
#224794,#224795,#224796,#224797,#224798,#224799,#224800,#224801,#224802,
#224803,#224804,#224805,#224806,#224807,#224808,#224809,#224810,#224811,
#224812,#224813,#224814,#224815,#224816,#224817,#224818,#224819,#224820,
#224821,#224822,#224823,#224824,#224825,#224826,#224827,#224828,#224829,
#224830,#224831,#224832,#224833,#224834,#224835,#224836,#224837,#224838,
#224839,#224840,#224841,#224842,#224843,#224844,#224845,#224846,#224847,
#224848,#224849,#224850,#224851,#224852,#224853,#224854,#224855,#224856,
#224857,#224858,#224859,#224860,#224861,#224862,#224863,#224864,#224865,
#224866,#224867,#224868,#224869,#224870,#224871,#224872,#224873,#224874,
#224875,#224876,#224877,#224878,#224879,#224880,#224881,#224882,#224883),
 .UNSPECIFIED.,.F.,.F.)
B_SPLINE_CURVE_WITH_KNOTS((6,1,1,1,1,1,1,1,1,1,1,1,1,1,1,1,1,1,1,1,1,1,
1,1,1,1,1,1,1,1,1,1,1,1,1,1,1,1,1,1,1,1,1,1,1,1,1,1,1,1,1,1,1,1,1,1,1,1,
1,1,1,1,1,1,1,1,1,1,1,1,1,1,1,1,1,1,1,1,1,1,1,1,1,1,1,1,1,1,1,1,1,1,1,1,
1,1,1,1,1,1,1,1,1,1,1,1,1,1,1,1,1,1,1,1,1,1,1,1,1,1,1,1,1,1,1,1,1,1,1,1,
1,1,1,1,1,1,1,1,1,1,1,1,1,1,1,1,1,1,1,1,1,1,1,1,1,1,1,1,1,1,1,1,1,1,1,1,
1,1,1,1,1,1,1,1,1,1,1,1,1,1,1,1,1,1,1,1,1,1,1,1,1,1,1,1,1,1,1,1,1,1,6),
(-1.,-0.995000000000001,-0.990000000000001,-0.985000000000001,-0.980000000000001,
-0.975000000000001,-0.970000000000001,-0.965000000000001,-0.960000000000001,
-0.955000000000001,-0.950000000000001,-0.945000000000001,-0.940000000000001,
-0.935000000000001,-0.930000000000001,-0.925000000000001,-0.920000000000001,
-0.915000000000001,-0.910000000000001,-0.905000000000001,-0.900000000000001,
-0.895000000000001,-0.890000000000001,-0.885000000000001,-0.880000000000001,
-0.875000000000001,-0.870000000000001,-0.865000000000001,-0.860000000000001,
-0.855000000000001,-0.850000000000001,-0.845000000000001,-0.840000000000001,
-0.835000000000001,-0.830000000000001,-0.825000000000001,-0.820000000000001,
-0.815000000000001,-0.810000000000001,-0.805000000000001,-0.800000000000001,
-0.795000000000001,-0.790000000000001,-0.785000000000001,-0.780000000000001,
-0.775000000000001,-0.770000000000001,-0.765000000000001,-0.760000000000001,
-0.755000000000001,-0.750000000000001,-0.745000000000001,-0.740000000000001,
-0.735000000000001,-0.730000000000001,-0.725000000000001,-0.720000000000001,
-0.715000000000001,-0.710000000000001,-0.705000000000001,-0.700000000000001,
-0.695000000000001,-0.690000000000001,-0.685,-0.68,-0.675,-0.67,-0.665,
-0.66,-0.655,-0.65,-0.645,-0.64,-0.635,-0.63,-0.625,-0.62,-0.615,-0.61,
-0.605,-0.6,-0.595,-0.59,-0.585,-0.58,-0.575,-0.57,-0.565,-0.56,-0.555,
-0.55,-0.545,-0.54,-0.535,-0.53,-0.525,-0.52,-0.515,-0.51,-0.505,-0.5,-0.495,
-0.49,-0.485,-0.48,-0.475,-0.47,-0.465,-0.46,-0.455,-0.45,-0.445,-0.44,
-0.435,-0.43,-0.425,-0.42,-0.415,-0.41,-0.405,-0.4,-0.395,-0.39,-0.385,
-0.38,-0.375,-0.37,-0.365,-0.36,-0.355,-0.35,-0.345,-0.34,-0.335,-0.33,
-0.325,-0.32,-0.315,-0.31,-0.305,-0.3,-0.295,-0.29,-0.285,-0.28,-0.275,
-0.27,-0.265,-0.26,-0.255,-0.25,-0.245,-0.24,-0.235,-0.23,-0.225,-0.22,
-0.215,-0.21,-0.205,-0.2,-0.195,-0.19,-0.185,-0.18,-0.175,-0.17,-0.165,
-0.16,-0.155,-0.15,-0.145,-0.14,-0.135,-0.13,-0.125,-0.12,-0.115,-0.11,
-0.105,-0.1,-0.095,-0.09,-0.085,-0.08,-0.075,-0.07,-0.065,-0.06,-0.055,
-0.05,-0.045,-0.04,-0.035,-0.03,-0.025,-0.02,-0.015,-0.01,-0.005,0.),
 .UNSPECIFIED.)
CURVE()
GEOMETRIC_REPRESENTATION_ITEM()
RATIONAL_B_SPLINE_CURVE((1.,1.,1.,1.,1.,1.,1.,1.,1.,1.,1.,1.,1.,1.,1.,1.,
1.,1.,1.,1.,1.,1.,1.,1.,1.,1.,1.,1.,1.,1.,1.,1.,1.,1.,1.,1.,1.,1.,1.,1.,
1.,1.,1.,1.,1.,1.,1.,1.,1.,1.,1.,1.,1.,1.,1.,1.,1.,1.,1.,1.,1.,1.,1.,1.,
1.,1.,1.,1.,1.,1.,1.,1.,1.,1.,1.,1.,1.,1.,1.,1.,1.,1.,1.,1.,1.,1.,1.,1.,
1.,1.,1.,1.,1.,1.,1.,1.,1.,1.,1.,1.,1.,1.,1.,1.,1.,1.,1.,1.,1.,1.,1.,1.,
1.,1.,1.,1.,1.,1.,1.,1.,1.,1.,1.,1.,1.,1.,1.,1.,1.,1.,1.,1.,1.,1.,1.,1.,
1.,1.,1.,1.,1.,1.,1.,1.,1.,1.,1.,1.,1.,1.,1.,1.,1.,1.,1.,1.,1.,1.,1.,1.,
1.,1.,1.,1.,1.,1.,1.,1.,1.,1.,1.,1.,1.,1.,1.,1.,1.,1.,1.,1.,1.,1.,1.,1.,
1.,1.,1.,1.,1.,1.,1.,1.,1.,1.,1.,1.,1.,1.,1.,1.,1.,1.,1.,1.,1.))
REPRESENTATION_ITEM('')
);
#808=(
BOUNDED_CURVE()
B_SPLINE_CURVE(5,(#224886,#224887,#224888,#224889,#224890,#224891,#224892,
#224893,#224894,#224895,#224896,#224897,#224898,#224899,#224900,#224901,
#224902,#224903,#224904,#224905,#224906,#224907,#224908,#224909,#224910,
#224911,#224912,#224913,#224914,#224915,#224916,#224917,#224918,#224919,
#224920,#224921,#224922,#224923,#224924,#224925,#224926,#224927,#224928,
#224929,#224930,#224931,#224932,#224933,#224934,#224935,#224936,#224937,
#224938,#224939,#224940,#224941,#224942,#224943,#224944,#224945,#224946,
#224947,#224948,#224949,#224950,#224951,#224952,#224953,#224954,#224955,
#224956,#224957,#224958,#224959,#224960,#224961,#224962,#224963,#224964,
#224965,#224966,#224967,#224968,#224969,#224970,#224971,#224972,#224973,
#224974,#224975,#224976,#224977,#224978,#224979,#224980,#224981,#224982,
#224983,#224984,#224985,#224986,#224987,#224988,#224989,#224990,#224991,
#224992,#224993,#224994,#224995,#224996,#224997,#224998,#224999,#225000,
#225001,#225002,#225003,#225004,#225005,#225006,#225007,#225008,#225009,
#225010,#225011,#225012,#225013,#225014,#225015,#225016,#225017,#225018,
#225019,#225020,#225021,#225022,#225023,#225024,#225025,#225026,#225027,
#225028,#225029,#225030,#225031,#225032,#225033,#225034,#225035,#225036,
#225037,#225038,#225039,#225040,#225041,#225042,#225043,#225044,#225045,
#225046,#225047,#225048,#225049,#225050,#225051,#225052,#225053,#225054,
#225055,#225056,#225057,#225058,#225059,#225060,#225061,#225062,#225063,
#225064,#225065,#225066,#225067,#225068,#225069,#225070,#225071,#225072,
#225073,#225074,#225075,#225076,#225077,#225078,#225079,#225080,#225081,
#225082,#225083,#225084,#225085,#225086,#225087,#225088,#225089,#225090),
 .UNSPECIFIED.,.F.,.F.)
B_SPLINE_CURVE_WITH_KNOTS((6,1,1,1,1,1,1,1,1,1,1,1,1,1,1,1,1,1,1,1,1,1,
1,1,1,1,1,1,1,1,1,1,1,1,1,1,1,1,1,1,1,1,1,1,1,1,1,1,1,1,1,1,1,1,1,1,1,1,
1,1,1,1,1,1,1,1,1,1,1,1,1,1,1,1,1,1,1,1,1,1,1,1,1,1,1,1,1,1,1,1,1,1,1,1,
1,1,1,1,1,1,1,1,1,1,1,1,1,1,1,1,1,1,1,1,1,1,1,1,1,1,1,1,1,1,1,1,1,1,1,1,
1,1,1,1,1,1,1,1,1,1,1,1,1,1,1,1,1,1,1,1,1,1,1,1,1,1,1,1,1,1,1,1,1,1,1,1,
1,1,1,1,1,1,1,1,1,1,1,1,1,1,1,1,1,1,1,1,1,1,1,1,1,1,1,1,1,1,1,1,1,1,6),
(0.,0.005,0.01,0.015,0.02,0.025,0.03,0.035,0.04,0.045,0.05,0.055,0.06,0.065,
0.07,0.075,0.08,0.085,0.09,0.095,0.1,0.105,0.11,0.115,0.12,0.125,0.13,0.135,
0.14,0.145,0.15,0.155,0.16,0.165,0.17,0.175,0.18,0.185,0.19,0.195,0.2,0.205,
0.21,0.215,0.22,0.225,0.23,0.235,0.24,0.245,0.25,0.255,0.26,0.265,0.27,
0.275,0.28,0.285,0.29,0.295,0.3,0.305,0.31,0.315,0.32,0.325,0.33,0.335,
0.34,0.345,0.35,0.355,0.36,0.365,0.37,0.375,0.38,0.385,0.39,0.395,0.4,0.405,
0.41,0.415,0.42,0.425,0.43,0.435,0.44,0.445,0.45,0.455,0.46,0.465,0.47,
0.475,0.48,0.485,0.49,0.495,0.5,0.505,0.51,0.515,0.52,0.525,0.53,0.535,
0.54,0.545,0.55,0.555,0.56,0.565,0.57,0.575,0.58,0.585,0.59,0.595,0.6,0.605,
0.61,0.615,0.62,0.625,0.63,0.635,0.64,0.645,0.65,0.655,0.66,0.665,0.67,
0.675,0.68,0.685,0.690000000000001,0.695000000000001,0.700000000000001,
0.705000000000001,0.710000000000001,0.715000000000001,0.720000000000001,
0.725000000000001,0.730000000000001,0.735000000000001,0.740000000000001,
0.745000000000001,0.750000000000001,0.755000000000001,0.760000000000001,
0.765000000000001,0.770000000000001,0.775000000000001,0.780000000000001,
0.785000000000001,0.790000000000001,0.795000000000001,0.800000000000001,
0.805000000000001,0.810000000000001,0.815000000000001,0.820000000000001,
0.825000000000001,0.830000000000001,0.835000000000001,0.840000000000001,
0.845000000000001,0.850000000000001,0.855000000000001,0.860000000000001,
0.865000000000001,0.870000000000001,0.875000000000001,0.880000000000001,
0.885000000000001,0.890000000000001,0.895000000000001,0.900000000000001,
0.905000000000001,0.910000000000001,0.915000000000001,0.920000000000001,
0.925000000000001,0.930000000000001,0.935000000000001,0.940000000000001,
0.945000000000001,0.950000000000001,0.955000000000001,0.960000000000001,
0.965000000000001,0.970000000000001,0.975000000000001,0.980000000000001,
0.985000000000001,0.990000000000001,0.995000000000001,1.),.UNSPECIFIED.)
CURVE()
GEOMETRIC_REPRESENTATION_ITEM()
RATIONAL_B_SPLINE_CURVE((1.,1.,1.,1.,1.,1.,1.,1.,1.,1.,1.,1.,1.,1.,1.,1.,
1.,1.,1.,1.,1.,1.,1.,1.,1.,1.,1.,1.,1.,1.,1.,1.,1.,1.,1.,1.,1.,1.,1.,1.,
1.,1.,1.,1.,1.,1.,1.,1.,1.,1.,1.,1.,1.,1.,1.,1.,1.,1.,1.,1.,1.,1.,1.,1.,
1.,1.,1.,1.,1.,1.,1.,1.,1.,1.,1.,1.,1.,1.,1.,1.,1.,1.,1.,1.,1.,1.,1.,1.,
1.,1.,1.,1.,1.,1.,1.,1.,1.,1.,1.,1.,1.,1.,1.,1.,1.,1.,1.,1.,1.,1.,1.,1.,
1.,1.,1.,1.,1.,1.,1.,1.,1.,1.,1.,1.,1.,1.,1.,1.,1.,1.,1.,1.,1.,1.,1.,1.,
1.,1.,1.,1.,1.,1.,1.,1.,1.,1.,1.,1.,1.,1.,1.,1.,1.,1.,1.,1.,1.,1.,1.,1.,
1.,1.,1.,1.,1.,1.,1.,1.,1.,1.,1.,1.,1.,1.,1.,1.,1.,1.,1.,1.,1.,1.,1.,1.,
1.,1.,1.,1.,1.,1.,1.,1.,1.,1.,1.,1.,1.,1.,1.,1.,1.,1.,1.,1.,1.))
REPRESENTATION_ITEM('')
);
#809=(
BOUNDED_CURVE()
B_SPLINE_CURVE(5,(#225502,#225503,#225504,#225505,#225506,#225507,#225508,
#225509,#225510,#225511,#225512,#225513,#225514,#225515,#225516,#225517,
#225518,#225519,#225520,#225521,#225522,#225523,#225524,#225525,#225526,
#225527,#225528,#225529,#225530,#225531,#225532,#225533,#225534,#225535,
#225536,#225537,#225538,#225539,#225540,#225541,#225542,#225543,#225544,
#225545,#225546,#225547,#225548,#225549,#225550,#225551,#225552,#225553,
#225554,#225555,#225556,#225557,#225558,#225559,#225560,#225561,#225562,
#225563,#225564,#225565,#225566,#225567,#225568,#225569,#225570,#225571,
#225572,#225573,#225574,#225575,#225576,#225577,#225578,#225579,#225580,
#225581,#225582,#225583,#225584,#225585,#225586,#225587,#225588,#225589,
#225590,#225591,#225592,#225593,#225594,#225595,#225596,#225597,#225598,
#225599,#225600,#225601,#225602,#225603,#225604,#225605,#225606,#225607,
#225608,#225609,#225610,#225611,#225612,#225613,#225614,#225615,#225616,
#225617,#225618,#225619,#225620,#225621,#225622,#225623,#225624,#225625,
#225626,#225627,#225628,#225629,#225630,#225631,#225632,#225633,#225634,
#225635,#225636,#225637,#225638,#225639,#225640,#225641,#225642,#225643,
#225644,#225645,#225646,#225647,#225648,#225649,#225650,#225651,#225652,
#225653,#225654,#225655,#225656,#225657,#225658,#225659,#225660,#225661,
#225662,#225663,#225664,#225665,#225666,#225667,#225668,#225669,#225670,
#225671,#225672,#225673,#225674,#225675,#225676,#225677,#225678,#225679,
#225680,#225681,#225682,#225683,#225684,#225685,#225686,#225687,#225688,
#225689,#225690,#225691,#225692,#225693,#225694,#225695,#225696,#225697,
#225698,#225699,#225700,#225701,#225702,#225703,#225704,#225705,#225706),
 .UNSPECIFIED.,.F.,.F.)
B_SPLINE_CURVE_WITH_KNOTS((6,1,1,1,1,1,1,1,1,1,1,1,1,1,1,1,1,1,1,1,1,1,
1,1,1,1,1,1,1,1,1,1,1,1,1,1,1,1,1,1,1,1,1,1,1,1,1,1,1,1,1,1,1,1,1,1,1,1,
1,1,1,1,1,1,1,1,1,1,1,1,1,1,1,1,1,1,1,1,1,1,1,1,1,1,1,1,1,1,1,1,1,1,1,1,
1,1,1,1,1,1,1,1,1,1,1,1,1,1,1,1,1,1,1,1,1,1,1,1,1,1,1,1,1,1,1,1,1,1,1,1,
1,1,1,1,1,1,1,1,1,1,1,1,1,1,1,1,1,1,1,1,1,1,1,1,1,1,1,1,1,1,1,1,1,1,1,1,
1,1,1,1,1,1,1,1,1,1,1,1,1,1,1,1,1,1,1,1,1,1,1,1,1,1,1,1,1,1,1,1,1,1,6),
(0.,0.005,0.01,0.015,0.02,0.025,0.03,0.035,0.04,0.045,0.05,0.055,0.06,0.065,
0.07,0.075,0.08,0.085,0.09,0.095,0.1,0.105,0.11,0.115,0.12,0.125,0.13,0.135,
0.14,0.145,0.15,0.155,0.16,0.165,0.17,0.175,0.18,0.185,0.19,0.195,0.2,0.205,
0.21,0.215,0.22,0.225,0.23,0.235,0.24,0.245,0.25,0.255,0.26,0.265,0.27,
0.275,0.28,0.285,0.29,0.295,0.3,0.305,0.31,0.315,0.32,0.325,0.33,0.335,
0.34,0.345,0.35,0.355,0.36,0.365,0.37,0.375,0.38,0.385,0.39,0.395,0.4,0.405,
0.41,0.415,0.42,0.425,0.43,0.435,0.44,0.445,0.45,0.455,0.46,0.465,0.47,
0.475,0.48,0.485,0.49,0.495,0.5,0.505,0.51,0.515,0.52,0.525,0.53,0.535,
0.54,0.545,0.55,0.555,0.56,0.565,0.57,0.575,0.58,0.585,0.59,0.595,0.6,0.605,
0.61,0.615,0.62,0.625,0.63,0.635,0.64,0.645,0.65,0.655,0.66,0.665,0.67,
0.675,0.68,0.685,0.690000000000001,0.695000000000001,0.700000000000001,
0.705000000000001,0.710000000000001,0.715000000000001,0.720000000000001,
0.725000000000001,0.730000000000001,0.735000000000001,0.740000000000001,
0.745000000000001,0.750000000000001,0.755000000000001,0.760000000000001,
0.765000000000001,0.770000000000001,0.775000000000001,0.780000000000001,
0.785000000000001,0.790000000000001,0.795000000000001,0.800000000000001,
0.805000000000001,0.810000000000001,0.815000000000001,0.820000000000001,
0.825000000000001,0.830000000000001,0.835000000000001,0.840000000000001,
0.845000000000001,0.850000000000001,0.855000000000001,0.860000000000001,
0.865000000000001,0.870000000000001,0.875000000000001,0.880000000000001,
0.885000000000001,0.890000000000001,0.895000000000001,0.900000000000001,
0.905000000000001,0.910000000000001,0.915000000000001,0.920000000000001,
0.925000000000001,0.930000000000001,0.935000000000001,0.940000000000001,
0.945000000000001,0.950000000000001,0.955000000000001,0.960000000000001,
0.965000000000001,0.970000000000001,0.975000000000001,0.980000000000001,
0.985000000000001,0.990000000000001,0.995000000000001,1.),.UNSPECIFIED.)
CURVE()
GEOMETRIC_REPRESENTATION_ITEM()
RATIONAL_B_SPLINE_CURVE((1.,1.,1.,1.,1.,1.,1.,1.,1.,1.,1.,1.,1.,1.,1.,1.,
1.,1.,1.,1.,1.,1.,1.,1.,1.,1.,1.,1.,1.,1.,1.,1.,1.,1.,1.,1.,1.,1.,1.,1.,
1.,1.,1.,1.,1.,1.,1.,1.,1.,1.,1.,1.,1.,1.,1.,1.,1.,1.,1.,1.,1.,1.,1.,1.,
1.,1.,1.,1.,1.,1.,1.,1.,1.,1.,1.,1.,1.,1.,1.,1.,1.,1.,1.,1.,1.,1.,1.,1.,
1.,1.,1.,1.,1.,1.,1.,1.,1.,1.,1.,1.,1.,1.,1.,1.,1.,1.,1.,1.,1.,1.,1.,1.,
1.,1.,1.,1.,1.,1.,1.,1.,1.,1.,1.,1.,1.,1.,1.,1.,1.,1.,1.,1.,1.,1.,1.,1.,
1.,1.,1.,1.,1.,1.,1.,1.,1.,1.,1.,1.,1.,1.,1.,1.,1.,1.,1.,1.,1.,1.,1.,1.,
1.,1.,1.,1.,1.,1.,1.,1.,1.,1.,1.,1.,1.,1.,1.,1.,1.,1.,1.,1.,1.,1.,1.,1.,
1.,1.,1.,1.,1.,1.,1.,1.,1.,1.,1.,1.,1.,1.,1.,1.,1.,1.,1.,1.,1.))
REPRESENTATION_ITEM('')
);
#810=(
BOUNDED_CURVE()
B_SPLINE_CURVE(5,(#225708,#225709,#225710,#225711,#225712,#225713,#225714,
#225715,#225716,#225717,#225718,#225719,#225720,#225721,#225722,#225723,
#225724,#225725,#225726,#225727,#225728,#225729,#225730,#225731,#225732,
#225733,#225734,#225735,#225736,#225737,#225738,#225739,#225740,#225741,
#225742,#225743,#225744,#225745,#225746,#225747,#225748,#225749,#225750,
#225751,#225752,#225753,#225754,#225755,#225756,#225757,#225758,#225759,
#225760,#225761,#225762,#225763,#225764,#225765,#225766,#225767,#225768,
#225769,#225770,#225771,#225772,#225773,#225774,#225775,#225776,#225777,
#225778,#225779,#225780,#225781,#225782,#225783,#225784,#225785,#225786,
#225787,#225788,#225789,#225790,#225791,#225792,#225793,#225794,#225795,
#225796,#225797,#225798,#225799,#225800,#225801,#225802,#225803,#225804,
#225805,#225806,#225807,#225808,#225809,#225810,#225811,#225812,#225813,
#225814,#225815,#225816,#225817,#225818,#225819,#225820,#225821,#225822,
#225823,#225824,#225825,#225826,#225827,#225828,#225829,#225830,#225831,
#225832,#225833,#225834,#225835,#225836,#225837,#225838,#225839,#225840,
#225841,#225842,#225843,#225844,#225845,#225846,#225847,#225848,#225849,
#225850,#225851,#225852,#225853,#225854,#225855,#225856,#225857,#225858,
#225859,#225860,#225861,#225862,#225863,#225864,#225865,#225866,#225867,
#225868,#225869,#225870,#225871,#225872,#225873,#225874,#225875,#225876,
#225877,#225878,#225879,#225880,#225881,#225882,#225883,#225884,#225885,
#225886,#225887,#225888,#225889,#225890,#225891,#225892,#225893,#225894,
#225895,#225896,#225897,#225898,#225899,#225900,#225901,#225902,#225903,
#225904,#225905,#225906,#225907,#225908,#225909,#225910,#225911,#225912),
 .UNSPECIFIED.,.F.,.F.)
B_SPLINE_CURVE_WITH_KNOTS((6,1,1,1,1,1,1,1,1,1,1,1,1,1,1,1,1,1,1,1,1,1,
1,1,1,1,1,1,1,1,1,1,1,1,1,1,1,1,1,1,1,1,1,1,1,1,1,1,1,1,1,1,1,1,1,1,1,1,
1,1,1,1,1,1,1,1,1,1,1,1,1,1,1,1,1,1,1,1,1,1,1,1,1,1,1,1,1,1,1,1,1,1,1,1,
1,1,1,1,1,1,1,1,1,1,1,1,1,1,1,1,1,1,1,1,1,1,1,1,1,1,1,1,1,1,1,1,1,1,1,1,
1,1,1,1,1,1,1,1,1,1,1,1,1,1,1,1,1,1,1,1,1,1,1,1,1,1,1,1,1,1,1,1,1,1,1,1,
1,1,1,1,1,1,1,1,1,1,1,1,1,1,1,1,1,1,1,1,1,1,1,1,1,1,1,1,1,1,1,1,1,1,6),
(-1.,-0.995000000000001,-0.990000000000001,-0.985000000000001,-0.980000000000001,
-0.975000000000001,-0.970000000000001,-0.965000000000001,-0.960000000000001,
-0.955000000000001,-0.950000000000001,-0.945000000000001,-0.940000000000001,
-0.935000000000001,-0.930000000000001,-0.925000000000001,-0.920000000000001,
-0.915000000000001,-0.910000000000001,-0.905000000000001,-0.900000000000001,
-0.895000000000001,-0.890000000000001,-0.885000000000001,-0.880000000000001,
-0.875000000000001,-0.870000000000001,-0.865000000000001,-0.860000000000001,
-0.855000000000001,-0.850000000000001,-0.845000000000001,-0.840000000000001,
-0.835000000000001,-0.830000000000001,-0.825000000000001,-0.820000000000001,
-0.815000000000001,-0.810000000000001,-0.805000000000001,-0.800000000000001,
-0.795000000000001,-0.790000000000001,-0.785000000000001,-0.780000000000001,
-0.775000000000001,-0.770000000000001,-0.765000000000001,-0.760000000000001,
-0.755000000000001,-0.750000000000001,-0.745000000000001,-0.740000000000001,
-0.735000000000001,-0.730000000000001,-0.725000000000001,-0.720000000000001,
-0.715000000000001,-0.710000000000001,-0.705000000000001,-0.700000000000001,
-0.695000000000001,-0.690000000000001,-0.685,-0.68,-0.675,-0.67,-0.665,
-0.66,-0.655,-0.65,-0.645,-0.64,-0.635,-0.63,-0.625,-0.62,-0.615,-0.61,
-0.605,-0.6,-0.595,-0.59,-0.585,-0.58,-0.575,-0.57,-0.565,-0.56,-0.555,
-0.55,-0.545,-0.54,-0.535,-0.53,-0.525,-0.52,-0.515,-0.51,-0.505,-0.5,-0.495,
-0.49,-0.485,-0.48,-0.475,-0.47,-0.465,-0.46,-0.455,-0.45,-0.445,-0.44,
-0.435,-0.43,-0.425,-0.42,-0.415,-0.41,-0.405,-0.4,-0.395,-0.39,-0.385,
-0.38,-0.375,-0.37,-0.365,-0.36,-0.355,-0.35,-0.345,-0.34,-0.335,-0.33,
-0.325,-0.32,-0.315,-0.31,-0.305,-0.3,-0.295,-0.29,-0.285,-0.28,-0.275,
-0.27,-0.265,-0.26,-0.255,-0.25,-0.245,-0.24,-0.235,-0.23,-0.225,-0.22,
-0.215,-0.21,-0.205,-0.2,-0.195,-0.19,-0.185,-0.18,-0.175,-0.17,-0.165,
-0.16,-0.155,-0.15,-0.145,-0.14,-0.135,-0.13,-0.125,-0.12,-0.115,-0.11,
-0.105,-0.1,-0.095,-0.09,-0.085,-0.08,-0.075,-0.07,-0.065,-0.06,-0.055,
-0.05,-0.045,-0.04,-0.035,-0.03,-0.025,-0.02,-0.015,-0.01,-0.005,0.),
 .UNSPECIFIED.)
CURVE()
GEOMETRIC_REPRESENTATION_ITEM()
RATIONAL_B_SPLINE_CURVE((1.,1.,1.,1.,1.,1.,1.,1.,1.,1.,1.,1.,1.,1.,1.,1.,
1.,1.,1.,1.,1.,1.,1.,1.,1.,1.,1.,1.,1.,1.,1.,1.,1.,1.,1.,1.,1.,1.,1.,1.,
1.,1.,1.,1.,1.,1.,1.,1.,1.,1.,1.,1.,1.,1.,1.,1.,1.,1.,1.,1.,1.,1.,1.,1.,
1.,1.,1.,1.,1.,1.,1.,1.,1.,1.,1.,1.,1.,1.,1.,1.,1.,1.,1.,1.,1.,1.,1.,1.,
1.,1.,1.,1.,1.,1.,1.,1.,1.,1.,1.,1.,1.,1.,1.,1.,1.,1.,1.,1.,1.,1.,1.,1.,
1.,1.,1.,1.,1.,1.,1.,1.,1.,1.,1.,1.,1.,1.,1.,1.,1.,1.,1.,1.,1.,1.,1.,1.,
1.,1.,1.,1.,1.,1.,1.,1.,1.,1.,1.,1.,1.,1.,1.,1.,1.,1.,1.,1.,1.,1.,1.,1.,
1.,1.,1.,1.,1.,1.,1.,1.,1.,1.,1.,1.,1.,1.,1.,1.,1.,1.,1.,1.,1.,1.,1.,1.,
1.,1.,1.,1.,1.,1.,1.,1.,1.,1.,1.,1.,1.,1.,1.,1.,1.,1.,1.,1.,1.))
REPRESENTATION_ITEM('')
);
#811=(
BOUNDED_CURVE()
B_SPLINE_CURVE(5,(#226331,#226332,#226333,#226334,#226335,#226336,#226337,
#226338,#226339,#226340,#226341,#226342,#226343,#226344,#226345,#226346,
#226347,#226348,#226349,#226350,#226351,#226352,#226353,#226354,#226355,
#226356,#226357,#226358,#226359,#226360,#226361,#226362,#226363,#226364,
#226365,#226366,#226367,#226368,#226369,#226370,#226371,#226372,#226373,
#226374,#226375,#226376,#226377,#226378,#226379,#226380,#226381,#226382,
#226383,#226384,#226385,#226386,#226387,#226388,#226389,#226390,#226391,
#226392,#226393,#226394,#226395,#226396,#226397,#226398,#226399,#226400,
#226401,#226402,#226403,#226404,#226405,#226406,#226407,#226408,#226409,
#226410,#226411,#226412,#226413,#226414,#226415,#226416,#226417,#226418,
#226419,#226420,#226421,#226422,#226423,#226424,#226425,#226426,#226427,
#226428,#226429,#226430,#226431,#226432,#226433,#226434,#226435,#226436,
#226437,#226438,#226439,#226440,#226441,#226442,#226443,#226444,#226445,
#226446,#226447,#226448,#226449,#226450,#226451,#226452,#226453,#226454,
#226455,#226456,#226457,#226458,#226459,#226460,#226461,#226462,#226463,
#226464,#226465,#226466,#226467,#226468,#226469,#226470,#226471,#226472,
#226473,#226474,#226475,#226476,#226477,#226478,#226479,#226480,#226481,
#226482,#226483,#226484,#226485,#226486,#226487,#226488,#226489,#226490,
#226491,#226492,#226493,#226494,#226495,#226496,#226497,#226498,#226499,
#226500,#226501,#226502,#226503,#226504,#226505,#226506,#226507,#226508,
#226509,#226510,#226511,#226512,#226513,#226514,#226515,#226516,#226517,
#226518,#226519,#226520,#226521,#226522,#226523,#226524,#226525,#226526,
#226527,#226528,#226529,#226530,#226531,#226532,#226533,#226534,#226535),
 .UNSPECIFIED.,.F.,.F.)
B_SPLINE_CURVE_WITH_KNOTS((6,1,1,1,1,1,1,1,1,1,1,1,1,1,1,1,1,1,1,1,1,1,
1,1,1,1,1,1,1,1,1,1,1,1,1,1,1,1,1,1,1,1,1,1,1,1,1,1,1,1,1,1,1,1,1,1,1,1,
1,1,1,1,1,1,1,1,1,1,1,1,1,1,1,1,1,1,1,1,1,1,1,1,1,1,1,1,1,1,1,1,1,1,1,1,
1,1,1,1,1,1,1,1,1,1,1,1,1,1,1,1,1,1,1,1,1,1,1,1,1,1,1,1,1,1,1,1,1,1,1,1,
1,1,1,1,1,1,1,1,1,1,1,1,1,1,1,1,1,1,1,1,1,1,1,1,1,1,1,1,1,1,1,1,1,1,1,1,
1,1,1,1,1,1,1,1,1,1,1,1,1,1,1,1,1,1,1,1,1,1,1,1,1,1,1,1,1,1,1,1,1,1,6),
(-1.,-0.995000000000001,-0.990000000000001,-0.985000000000001,-0.980000000000001,
-0.975000000000001,-0.970000000000001,-0.965000000000001,-0.960000000000001,
-0.955000000000001,-0.950000000000001,-0.945000000000001,-0.940000000000001,
-0.935000000000001,-0.930000000000001,-0.925000000000001,-0.920000000000001,
-0.915000000000001,-0.910000000000001,-0.905000000000001,-0.900000000000001,
-0.895000000000001,-0.890000000000001,-0.885000000000001,-0.880000000000001,
-0.875000000000001,-0.870000000000001,-0.865000000000001,-0.860000000000001,
-0.855000000000001,-0.850000000000001,-0.845000000000001,-0.840000000000001,
-0.835000000000001,-0.830000000000001,-0.825000000000001,-0.820000000000001,
-0.815000000000001,-0.810000000000001,-0.805000000000001,-0.800000000000001,
-0.795000000000001,-0.790000000000001,-0.785000000000001,-0.780000000000001,
-0.775000000000001,-0.770000000000001,-0.765000000000001,-0.760000000000001,
-0.755000000000001,-0.750000000000001,-0.745000000000001,-0.740000000000001,
-0.735000000000001,-0.730000000000001,-0.725000000000001,-0.720000000000001,
-0.715000000000001,-0.710000000000001,-0.705000000000001,-0.700000000000001,
-0.695000000000001,-0.690000000000001,-0.685,-0.68,-0.675,-0.67,-0.665,
-0.66,-0.655,-0.65,-0.645,-0.64,-0.635,-0.63,-0.625,-0.62,-0.615,-0.61,
-0.605,-0.6,-0.595,-0.59,-0.585,-0.58,-0.575,-0.57,-0.565,-0.56,-0.555,
-0.55,-0.545,-0.54,-0.535,-0.53,-0.525,-0.52,-0.515,-0.51,-0.505,-0.5,-0.495,
-0.49,-0.485,-0.48,-0.475,-0.47,-0.465,-0.46,-0.455,-0.45,-0.445,-0.44,
-0.435,-0.43,-0.425,-0.42,-0.415,-0.41,-0.405,-0.4,-0.395,-0.39,-0.385,
-0.38,-0.375,-0.37,-0.365,-0.36,-0.355,-0.35,-0.345,-0.34,-0.335,-0.33,
-0.325,-0.32,-0.315,-0.31,-0.305,-0.3,-0.295,-0.29,-0.285,-0.28,-0.275,
-0.27,-0.265,-0.26,-0.255,-0.25,-0.245,-0.24,-0.235,-0.23,-0.225,-0.22,
-0.215,-0.21,-0.205,-0.2,-0.195,-0.19,-0.185,-0.18,-0.175,-0.17,-0.165,
-0.16,-0.155,-0.15,-0.145,-0.14,-0.135,-0.13,-0.125,-0.12,-0.115,-0.11,
-0.105,-0.1,-0.095,-0.09,-0.085,-0.08,-0.075,-0.07,-0.065,-0.06,-0.055,
-0.05,-0.045,-0.04,-0.035,-0.03,-0.025,-0.02,-0.015,-0.01,-0.005,0.),
 .UNSPECIFIED.)
CURVE()
GEOMETRIC_REPRESENTATION_ITEM()
RATIONAL_B_SPLINE_CURVE((1.,1.,1.,1.,1.,1.,1.,1.,1.,1.,1.,1.,1.,1.,1.,1.,
1.,1.,1.,1.,1.,1.,1.,1.,1.,1.,1.,1.,1.,1.,1.,1.,1.,1.,1.,1.,1.,1.,1.,1.,
1.,1.,1.,1.,1.,1.,1.,1.,1.,1.,1.,1.,1.,1.,1.,1.,1.,1.,1.,1.,1.,1.,1.,1.,
1.,1.,1.,1.,1.,1.,1.,1.,1.,1.,1.,1.,1.,1.,1.,1.,1.,1.,1.,1.,1.,1.,1.,1.,
1.,1.,1.,1.,1.,1.,1.,1.,1.,1.,1.,1.,1.,1.,1.,1.,1.,1.,1.,1.,1.,1.,1.,1.,
1.,1.,1.,1.,1.,1.,1.,1.,1.,1.,1.,1.,1.,1.,1.,1.,1.,1.,1.,1.,1.,1.,1.,1.,
1.,1.,1.,1.,1.,1.,1.,1.,1.,1.,1.,1.,1.,1.,1.,1.,1.,1.,1.,1.,1.,1.,1.,1.,
1.,1.,1.,1.,1.,1.,1.,1.,1.,1.,1.,1.,1.,1.,1.,1.,1.,1.,1.,1.,1.,1.,1.,1.,
1.,1.,1.,1.,1.,1.,1.,1.,1.,1.,1.,1.,1.,1.,1.,1.,1.,1.,1.,1.,1.))
REPRESENTATION_ITEM('')
);
#812=(
BOUNDED_CURVE()
B_SPLINE_CURVE(5,(#226538,#226539,#226540,#226541,#226542,#226543,#226544,
#226545,#226546,#226547,#226548,#226549,#226550,#226551,#226552,#226553,
#226554,#226555,#226556,#226557,#226558,#226559,#226560,#226561,#226562,
#226563,#226564,#226565,#226566,#226567,#226568,#226569,#226570,#226571,
#226572,#226573,#226574,#226575,#226576,#226577,#226578,#226579,#226580,
#226581,#226582,#226583,#226584,#226585,#226586,#226587,#226588,#226589,
#226590,#226591,#226592,#226593,#226594,#226595,#226596,#226597,#226598,
#226599,#226600,#226601,#226602,#226603,#226604,#226605,#226606,#226607,
#226608,#226609,#226610,#226611,#226612,#226613,#226614,#226615,#226616,
#226617,#226618,#226619,#226620,#226621,#226622,#226623,#226624,#226625,
#226626,#226627,#226628,#226629,#226630,#226631,#226632,#226633,#226634,
#226635,#226636,#226637,#226638,#226639,#226640,#226641,#226642,#226643,
#226644,#226645,#226646,#226647,#226648,#226649,#226650,#226651,#226652,
#226653,#226654,#226655,#226656,#226657,#226658,#226659,#226660,#226661,
#226662,#226663,#226664,#226665,#226666,#226667,#226668,#226669,#226670,
#226671,#226672,#226673,#226674,#226675,#226676,#226677,#226678,#226679,
#226680,#226681,#226682,#226683,#226684,#226685,#226686,#226687,#226688,
#226689,#226690,#226691,#226692,#226693,#226694,#226695,#226696,#226697,
#226698,#226699,#226700,#226701,#226702,#226703,#226704,#226705,#226706,
#226707,#226708,#226709,#226710,#226711,#226712,#226713,#226714,#226715,
#226716,#226717,#226718,#226719,#226720,#226721,#226722,#226723,#226724,
#226725,#226726,#226727,#226728,#226729,#226730,#226731,#226732,#226733,
#226734,#226735,#226736,#226737,#226738,#226739,#226740,#226741,#226742),
 .UNSPECIFIED.,.F.,.F.)
B_SPLINE_CURVE_WITH_KNOTS((6,1,1,1,1,1,1,1,1,1,1,1,1,1,1,1,1,1,1,1,1,1,
1,1,1,1,1,1,1,1,1,1,1,1,1,1,1,1,1,1,1,1,1,1,1,1,1,1,1,1,1,1,1,1,1,1,1,1,
1,1,1,1,1,1,1,1,1,1,1,1,1,1,1,1,1,1,1,1,1,1,1,1,1,1,1,1,1,1,1,1,1,1,1,1,
1,1,1,1,1,1,1,1,1,1,1,1,1,1,1,1,1,1,1,1,1,1,1,1,1,1,1,1,1,1,1,1,1,1,1,1,
1,1,1,1,1,1,1,1,1,1,1,1,1,1,1,1,1,1,1,1,1,1,1,1,1,1,1,1,1,1,1,1,1,1,1,1,
1,1,1,1,1,1,1,1,1,1,1,1,1,1,1,1,1,1,1,1,1,1,1,1,1,1,1,1,1,1,1,1,1,1,6),
(0.,0.005,0.01,0.015,0.02,0.025,0.03,0.035,0.04,0.045,0.05,0.055,0.06,0.065,
0.07,0.075,0.08,0.085,0.09,0.095,0.1,0.105,0.11,0.115,0.12,0.125,0.13,0.135,
0.14,0.145,0.15,0.155,0.16,0.165,0.17,0.175,0.18,0.185,0.19,0.195,0.2,0.205,
0.21,0.215,0.22,0.225,0.23,0.235,0.24,0.245,0.25,0.255,0.26,0.265,0.27,
0.275,0.28,0.285,0.29,0.295,0.3,0.305,0.31,0.315,0.32,0.325,0.33,0.335,
0.34,0.345,0.35,0.355,0.36,0.365,0.37,0.375,0.38,0.385,0.39,0.395,0.4,0.405,
0.41,0.415,0.42,0.425,0.43,0.435,0.44,0.445,0.45,0.455,0.46,0.465,0.47,
0.475,0.48,0.485,0.49,0.495,0.5,0.505,0.51,0.515,0.52,0.525,0.53,0.535,
0.54,0.545,0.55,0.555,0.56,0.565,0.57,0.575,0.58,0.585,0.59,0.595,0.6,0.605,
0.61,0.615,0.62,0.625,0.63,0.635,0.64,0.645,0.65,0.655,0.66,0.665,0.67,
0.675,0.68,0.685,0.690000000000001,0.695000000000001,0.700000000000001,
0.705000000000001,0.710000000000001,0.715000000000001,0.720000000000001,
0.725000000000001,0.730000000000001,0.735000000000001,0.740000000000001,
0.745000000000001,0.750000000000001,0.755000000000001,0.760000000000001,
0.765000000000001,0.770000000000001,0.775000000000001,0.780000000000001,
0.785000000000001,0.790000000000001,0.795000000000001,0.800000000000001,
0.805000000000001,0.810000000000001,0.815000000000001,0.820000000000001,
0.825000000000001,0.830000000000001,0.835000000000001,0.840000000000001,
0.845000000000001,0.850000000000001,0.855000000000001,0.860000000000001,
0.865000000000001,0.870000000000001,0.875000000000001,0.880000000000001,
0.885000000000001,0.890000000000001,0.895000000000001,0.900000000000001,
0.905000000000001,0.910000000000001,0.915000000000001,0.920000000000001,
0.925000000000001,0.930000000000001,0.935000000000001,0.940000000000001,
0.945000000000001,0.950000000000001,0.955000000000001,0.960000000000001,
0.965000000000001,0.970000000000001,0.975000000000001,0.980000000000001,
0.985000000000001,0.990000000000001,0.995000000000001,1.),.UNSPECIFIED.)
CURVE()
GEOMETRIC_REPRESENTATION_ITEM()
RATIONAL_B_SPLINE_CURVE((1.,1.,1.,1.,1.,1.,1.,1.,1.,1.,1.,1.,1.,1.,1.,1.,
1.,1.,1.,1.,1.,1.,1.,1.,1.,1.,1.,1.,1.,1.,1.,1.,1.,1.,1.,1.,1.,1.,1.,1.,
1.,1.,1.,1.,1.,1.,1.,1.,1.,1.,1.,1.,1.,1.,1.,1.,1.,1.,1.,1.,1.,1.,1.,1.,
1.,1.,1.,1.,1.,1.,1.,1.,1.,1.,1.,1.,1.,1.,1.,1.,1.,1.,1.,1.,1.,1.,1.,1.,
1.,1.,1.,1.,1.,1.,1.,1.,1.,1.,1.,1.,1.,1.,1.,1.,1.,1.,1.,1.,1.,1.,1.,1.,
1.,1.,1.,1.,1.,1.,1.,1.,1.,1.,1.,1.,1.,1.,1.,1.,1.,1.,1.,1.,1.,1.,1.,1.,
1.,1.,1.,1.,1.,1.,1.,1.,1.,1.,1.,1.,1.,1.,1.,1.,1.,1.,1.,1.,1.,1.,1.,1.,
1.,1.,1.,1.,1.,1.,1.,1.,1.,1.,1.,1.,1.,1.,1.,1.,1.,1.,1.,1.,1.,1.,1.,1.,
1.,1.,1.,1.,1.,1.,1.,1.,1.,1.,1.,1.,1.,1.,1.,1.,1.,1.,1.,1.,1.))
REPRESENTATION_ITEM('')
);
#813=(
BOUNDED_CURVE()
B_SPLINE_CURVE(5,(#227154,#227155,#227156,#227157,#227158,#227159,#227160,
#227161,#227162,#227163,#227164,#227165,#227166,#227167,#227168,#227169,
#227170,#227171,#227172,#227173,#227174,#227175,#227176,#227177,#227178,
#227179,#227180,#227181,#227182,#227183,#227184,#227185,#227186,#227187,
#227188,#227189,#227190,#227191,#227192,#227193,#227194,#227195,#227196,
#227197,#227198,#227199,#227200,#227201,#227202,#227203,#227204,#227205,
#227206,#227207,#227208,#227209,#227210,#227211,#227212,#227213,#227214,
#227215,#227216,#227217,#227218,#227219,#227220,#227221,#227222,#227223,
#227224,#227225,#227226,#227227,#227228,#227229,#227230,#227231,#227232,
#227233,#227234,#227235,#227236,#227237,#227238,#227239,#227240,#227241,
#227242,#227243,#227244,#227245,#227246,#227247,#227248,#227249,#227250,
#227251,#227252,#227253,#227254,#227255,#227256,#227257,#227258,#227259,
#227260,#227261,#227262,#227263,#227264,#227265,#227266,#227267,#227268,
#227269,#227270,#227271,#227272,#227273,#227274,#227275,#227276,#227277,
#227278,#227279,#227280,#227281,#227282,#227283,#227284,#227285,#227286,
#227287,#227288,#227289,#227290,#227291,#227292,#227293,#227294,#227295,
#227296,#227297,#227298,#227299,#227300,#227301,#227302,#227303,#227304,
#227305,#227306,#227307,#227308,#227309,#227310,#227311,#227312,#227313,
#227314,#227315,#227316,#227317,#227318,#227319,#227320,#227321,#227322,
#227323,#227324,#227325,#227326,#227327,#227328,#227329,#227330,#227331,
#227332,#227333,#227334,#227335,#227336,#227337,#227338,#227339,#227340,
#227341,#227342,#227343,#227344,#227345,#227346,#227347,#227348,#227349,
#227350,#227351,#227352,#227353,#227354,#227355,#227356,#227357,#227358),
 .UNSPECIFIED.,.F.,.F.)
B_SPLINE_CURVE_WITH_KNOTS((6,1,1,1,1,1,1,1,1,1,1,1,1,1,1,1,1,1,1,1,1,1,
1,1,1,1,1,1,1,1,1,1,1,1,1,1,1,1,1,1,1,1,1,1,1,1,1,1,1,1,1,1,1,1,1,1,1,1,
1,1,1,1,1,1,1,1,1,1,1,1,1,1,1,1,1,1,1,1,1,1,1,1,1,1,1,1,1,1,1,1,1,1,1,1,
1,1,1,1,1,1,1,1,1,1,1,1,1,1,1,1,1,1,1,1,1,1,1,1,1,1,1,1,1,1,1,1,1,1,1,1,
1,1,1,1,1,1,1,1,1,1,1,1,1,1,1,1,1,1,1,1,1,1,1,1,1,1,1,1,1,1,1,1,1,1,1,1,
1,1,1,1,1,1,1,1,1,1,1,1,1,1,1,1,1,1,1,1,1,1,1,1,1,1,1,1,1,1,1,1,1,1,6),
(0.,0.005,0.01,0.015,0.02,0.025,0.03,0.035,0.04,0.045,0.05,0.055,0.06,0.065,
0.07,0.075,0.08,0.085,0.09,0.095,0.1,0.105,0.11,0.115,0.12,0.125,0.13,0.135,
0.14,0.145,0.15,0.155,0.16,0.165,0.17,0.175,0.18,0.185,0.19,0.195,0.2,0.205,
0.21,0.215,0.22,0.225,0.23,0.235,0.24,0.245,0.25,0.255,0.26,0.265,0.27,
0.275,0.28,0.285,0.29,0.295,0.3,0.305,0.31,0.315,0.32,0.325,0.33,0.335,
0.34,0.345,0.35,0.355,0.36,0.365,0.37,0.375,0.38,0.385,0.39,0.395,0.4,0.405,
0.41,0.415,0.42,0.425,0.43,0.435,0.44,0.445,0.45,0.455,0.46,0.465,0.47,
0.475,0.48,0.485,0.49,0.495,0.5,0.505,0.51,0.515,0.52,0.525,0.53,0.535,
0.54,0.545,0.55,0.555,0.56,0.565,0.57,0.575,0.58,0.585,0.59,0.595,0.6,0.605,
0.61,0.615,0.62,0.625,0.63,0.635,0.64,0.645,0.65,0.655,0.66,0.665,0.67,
0.675,0.68,0.685,0.690000000000001,0.695000000000001,0.700000000000001,
0.705000000000001,0.710000000000001,0.715000000000001,0.720000000000001,
0.725000000000001,0.730000000000001,0.735000000000001,0.740000000000001,
0.745000000000001,0.750000000000001,0.755000000000001,0.760000000000001,
0.765000000000001,0.770000000000001,0.775000000000001,0.780000000000001,
0.785000000000001,0.790000000000001,0.795000000000001,0.800000000000001,
0.805000000000001,0.810000000000001,0.815000000000001,0.820000000000001,
0.825000000000001,0.830000000000001,0.835000000000001,0.840000000000001,
0.845000000000001,0.850000000000001,0.855000000000001,0.860000000000001,
0.865000000000001,0.870000000000001,0.875000000000001,0.880000000000001,
0.885000000000001,0.890000000000001,0.895000000000001,0.900000000000001,
0.905000000000001,0.910000000000001,0.915000000000001,0.920000000000001,
0.925000000000001,0.930000000000001,0.935000000000001,0.940000000000001,
0.945000000000001,0.950000000000001,0.955000000000001,0.960000000000001,
0.965000000000001,0.970000000000001,0.975000000000001,0.980000000000001,
0.985000000000001,0.990000000000001,0.995000000000001,1.),.UNSPECIFIED.)
CURVE()
GEOMETRIC_REPRESENTATION_ITEM()
RATIONAL_B_SPLINE_CURVE((1.,1.,1.,1.,1.,1.,1.,1.,1.,1.,1.,1.,1.,1.,1.,1.,
1.,1.,1.,1.,1.,1.,1.,1.,1.,1.,1.,1.,1.,1.,1.,1.,1.,1.,1.,1.,1.,1.,1.,1.,
1.,1.,1.,1.,1.,1.,1.,1.,1.,1.,1.,1.,1.,1.,1.,1.,1.,1.,1.,1.,1.,1.,1.,1.,
1.,1.,1.,1.,1.,1.,1.,1.,1.,1.,1.,1.,1.,1.,1.,1.,1.,1.,1.,1.,1.,1.,1.,1.,
1.,1.,1.,1.,1.,1.,1.,1.,1.,1.,1.,1.,1.,1.,1.,1.,1.,1.,1.,1.,1.,1.,1.,1.,
1.,1.,1.,1.,1.,1.,1.,1.,1.,1.,1.,1.,1.,1.,1.,1.,1.,1.,1.,1.,1.,1.,1.,1.,
1.,1.,1.,1.,1.,1.,1.,1.,1.,1.,1.,1.,1.,1.,1.,1.,1.,1.,1.,1.,1.,1.,1.,1.,
1.,1.,1.,1.,1.,1.,1.,1.,1.,1.,1.,1.,1.,1.,1.,1.,1.,1.,1.,1.,1.,1.,1.,1.,
1.,1.,1.,1.,1.,1.,1.,1.,1.,1.,1.,1.,1.,1.,1.,1.,1.,1.,1.,1.,1.))
REPRESENTATION_ITEM('')
);
#814=(
BOUNDED_CURVE()
B_SPLINE_CURVE(5,(#227360,#227361,#227362,#227363,#227364,#227365,#227366,
#227367,#227368,#227369,#227370,#227371,#227372,#227373,#227374,#227375,
#227376,#227377,#227378,#227379,#227380,#227381,#227382,#227383,#227384,
#227385,#227386,#227387,#227388,#227389,#227390,#227391,#227392,#227393,
#227394,#227395,#227396,#227397,#227398,#227399,#227400,#227401,#227402,
#227403,#227404,#227405,#227406,#227407,#227408,#227409,#227410,#227411,
#227412,#227413,#227414,#227415,#227416,#227417,#227418,#227419,#227420,
#227421,#227422,#227423,#227424,#227425,#227426,#227427,#227428,#227429,
#227430,#227431,#227432,#227433,#227434,#227435,#227436,#227437,#227438,
#227439,#227440,#227441,#227442,#227443,#227444,#227445,#227446,#227447,
#227448,#227449,#227450,#227451,#227452,#227453,#227454,#227455,#227456,
#227457,#227458,#227459,#227460,#227461,#227462,#227463,#227464,#227465,
#227466,#227467,#227468,#227469,#227470,#227471,#227472,#227473,#227474,
#227475,#227476,#227477,#227478,#227479,#227480,#227481,#227482,#227483,
#227484,#227485,#227486,#227487,#227488,#227489,#227490,#227491,#227492,
#227493,#227494,#227495,#227496,#227497,#227498,#227499,#227500,#227501,
#227502,#227503,#227504,#227505,#227506,#227507,#227508,#227509,#227510,
#227511,#227512,#227513,#227514,#227515,#227516,#227517,#227518,#227519,
#227520,#227521,#227522,#227523,#227524,#227525,#227526,#227527,#227528,
#227529,#227530,#227531,#227532,#227533,#227534,#227535,#227536,#227537,
#227538,#227539,#227540,#227541,#227542,#227543,#227544,#227545,#227546,
#227547,#227548,#227549,#227550,#227551,#227552,#227553,#227554,#227555,
#227556,#227557,#227558,#227559,#227560,#227561,#227562,#227563,#227564),
 .UNSPECIFIED.,.F.,.F.)
B_SPLINE_CURVE_WITH_KNOTS((6,1,1,1,1,1,1,1,1,1,1,1,1,1,1,1,1,1,1,1,1,1,
1,1,1,1,1,1,1,1,1,1,1,1,1,1,1,1,1,1,1,1,1,1,1,1,1,1,1,1,1,1,1,1,1,1,1,1,
1,1,1,1,1,1,1,1,1,1,1,1,1,1,1,1,1,1,1,1,1,1,1,1,1,1,1,1,1,1,1,1,1,1,1,1,
1,1,1,1,1,1,1,1,1,1,1,1,1,1,1,1,1,1,1,1,1,1,1,1,1,1,1,1,1,1,1,1,1,1,1,1,
1,1,1,1,1,1,1,1,1,1,1,1,1,1,1,1,1,1,1,1,1,1,1,1,1,1,1,1,1,1,1,1,1,1,1,1,
1,1,1,1,1,1,1,1,1,1,1,1,1,1,1,1,1,1,1,1,1,1,1,1,1,1,1,1,1,1,1,1,1,1,6),
(-1.,-0.995000000000001,-0.990000000000001,-0.985000000000001,-0.980000000000001,
-0.975000000000001,-0.970000000000001,-0.965000000000001,-0.960000000000001,
-0.955000000000001,-0.950000000000001,-0.945000000000001,-0.940000000000001,
-0.935000000000001,-0.930000000000001,-0.925000000000001,-0.920000000000001,
-0.915000000000001,-0.910000000000001,-0.905000000000001,-0.900000000000001,
-0.895000000000001,-0.890000000000001,-0.885000000000001,-0.880000000000001,
-0.875000000000001,-0.870000000000001,-0.865000000000001,-0.860000000000001,
-0.855000000000001,-0.850000000000001,-0.845000000000001,-0.840000000000001,
-0.835000000000001,-0.830000000000001,-0.825000000000001,-0.820000000000001,
-0.815000000000001,-0.810000000000001,-0.805000000000001,-0.800000000000001,
-0.795000000000001,-0.790000000000001,-0.785000000000001,-0.780000000000001,
-0.775000000000001,-0.770000000000001,-0.765000000000001,-0.760000000000001,
-0.755000000000001,-0.750000000000001,-0.745000000000001,-0.740000000000001,
-0.735000000000001,-0.730000000000001,-0.725000000000001,-0.720000000000001,
-0.715000000000001,-0.710000000000001,-0.705000000000001,-0.700000000000001,
-0.695000000000001,-0.690000000000001,-0.685,-0.68,-0.675,-0.67,-0.665,
-0.66,-0.655,-0.65,-0.645,-0.64,-0.635,-0.63,-0.625,-0.62,-0.615,-0.61,
-0.605,-0.6,-0.595,-0.59,-0.585,-0.58,-0.575,-0.57,-0.565,-0.56,-0.555,
-0.55,-0.545,-0.54,-0.535,-0.53,-0.525,-0.52,-0.515,-0.51,-0.505,-0.5,-0.495,
-0.49,-0.485,-0.48,-0.475,-0.47,-0.465,-0.46,-0.455,-0.45,-0.445,-0.44,
-0.435,-0.43,-0.425,-0.42,-0.415,-0.41,-0.405,-0.4,-0.395,-0.39,-0.385,
-0.38,-0.375,-0.37,-0.365,-0.36,-0.355,-0.35,-0.345,-0.34,-0.335,-0.33,
-0.325,-0.32,-0.315,-0.31,-0.305,-0.3,-0.295,-0.29,-0.285,-0.28,-0.275,
-0.27,-0.265,-0.26,-0.255,-0.25,-0.245,-0.24,-0.235,-0.23,-0.225,-0.22,
-0.215,-0.21,-0.205,-0.2,-0.195,-0.19,-0.185,-0.18,-0.175,-0.17,-0.165,
-0.16,-0.155,-0.15,-0.145,-0.14,-0.135,-0.13,-0.125,-0.12,-0.115,-0.11,
-0.105,-0.1,-0.095,-0.09,-0.085,-0.08,-0.075,-0.07,-0.065,-0.06,-0.055,
-0.05,-0.045,-0.04,-0.035,-0.03,-0.025,-0.02,-0.015,-0.01,-0.005,0.),
 .UNSPECIFIED.)
CURVE()
GEOMETRIC_REPRESENTATION_ITEM()
RATIONAL_B_SPLINE_CURVE((1.,1.,1.,1.,1.,1.,1.,1.,1.,1.,1.,1.,1.,1.,1.,1.,
1.,1.,1.,1.,1.,1.,1.,1.,1.,1.,1.,1.,1.,1.,1.,1.,1.,1.,1.,1.,1.,1.,1.,1.,
1.,1.,1.,1.,1.,1.,1.,1.,1.,1.,1.,1.,1.,1.,1.,1.,1.,1.,1.,1.,1.,1.,1.,1.,
1.,1.,1.,1.,1.,1.,1.,1.,1.,1.,1.,1.,1.,1.,1.,1.,1.,1.,1.,1.,1.,1.,1.,1.,
1.,1.,1.,1.,1.,1.,1.,1.,1.,1.,1.,1.,1.,1.,1.,1.,1.,1.,1.,1.,1.,1.,1.,1.,
1.,1.,1.,1.,1.,1.,1.,1.,1.,1.,1.,1.,1.,1.,1.,1.,1.,1.,1.,1.,1.,1.,1.,1.,
1.,1.,1.,1.,1.,1.,1.,1.,1.,1.,1.,1.,1.,1.,1.,1.,1.,1.,1.,1.,1.,1.,1.,1.,
1.,1.,1.,1.,1.,1.,1.,1.,1.,1.,1.,1.,1.,1.,1.,1.,1.,1.,1.,1.,1.,1.,1.,1.,
1.,1.,1.,1.,1.,1.,1.,1.,1.,1.,1.,1.,1.,1.,1.,1.,1.,1.,1.,1.,1.))
REPRESENTATION_ITEM('')
);
#815=(
BOUNDED_CURVE()
B_SPLINE_CURVE(5,(#227983,#227984,#227985,#227986,#227987,#227988,#227989,
#227990,#227991,#227992,#227993,#227994,#227995,#227996,#227997,#227998,
#227999,#228000,#228001,#228002,#228003,#228004,#228005,#228006,#228007,
#228008,#228009,#228010,#228011,#228012,#228013,#228014,#228015,#228016,
#228017,#228018,#228019,#228020,#228021,#228022,#228023,#228024,#228025,
#228026,#228027,#228028,#228029,#228030,#228031,#228032,#228033,#228034,
#228035,#228036,#228037,#228038,#228039,#228040,#228041,#228042,#228043,
#228044,#228045,#228046,#228047,#228048,#228049,#228050,#228051,#228052,
#228053,#228054,#228055,#228056,#228057,#228058,#228059,#228060,#228061,
#228062,#228063,#228064,#228065,#228066,#228067,#228068,#228069,#228070,
#228071,#228072,#228073,#228074,#228075,#228076,#228077,#228078,#228079,
#228080,#228081,#228082,#228083,#228084,#228085,#228086,#228087,#228088,
#228089,#228090,#228091,#228092,#228093,#228094,#228095,#228096,#228097,
#228098,#228099,#228100,#228101,#228102,#228103,#228104,#228105,#228106,
#228107,#228108,#228109,#228110,#228111,#228112,#228113,#228114,#228115,
#228116,#228117,#228118,#228119,#228120,#228121,#228122,#228123,#228124,
#228125,#228126,#228127,#228128,#228129,#228130,#228131,#228132,#228133,
#228134,#228135,#228136,#228137,#228138,#228139,#228140,#228141,#228142,
#228143,#228144,#228145,#228146,#228147,#228148,#228149,#228150,#228151,
#228152,#228153,#228154,#228155,#228156,#228157,#228158,#228159,#228160,
#228161,#228162,#228163,#228164,#228165,#228166,#228167,#228168,#228169,
#228170,#228171,#228172,#228173,#228174,#228175,#228176,#228177,#228178,
#228179,#228180,#228181,#228182,#228183,#228184,#228185,#228186,#228187),
 .UNSPECIFIED.,.F.,.F.)
B_SPLINE_CURVE_WITH_KNOTS((6,1,1,1,1,1,1,1,1,1,1,1,1,1,1,1,1,1,1,1,1,1,
1,1,1,1,1,1,1,1,1,1,1,1,1,1,1,1,1,1,1,1,1,1,1,1,1,1,1,1,1,1,1,1,1,1,1,1,
1,1,1,1,1,1,1,1,1,1,1,1,1,1,1,1,1,1,1,1,1,1,1,1,1,1,1,1,1,1,1,1,1,1,1,1,
1,1,1,1,1,1,1,1,1,1,1,1,1,1,1,1,1,1,1,1,1,1,1,1,1,1,1,1,1,1,1,1,1,1,1,1,
1,1,1,1,1,1,1,1,1,1,1,1,1,1,1,1,1,1,1,1,1,1,1,1,1,1,1,1,1,1,1,1,1,1,1,1,
1,1,1,1,1,1,1,1,1,1,1,1,1,1,1,1,1,1,1,1,1,1,1,1,1,1,1,1,1,1,1,1,1,1,6),
(-1.,-0.995000000000001,-0.990000000000001,-0.985000000000001,-0.980000000000001,
-0.975000000000001,-0.970000000000001,-0.965000000000001,-0.960000000000001,
-0.955000000000001,-0.950000000000001,-0.945000000000001,-0.940000000000001,
-0.935000000000001,-0.930000000000001,-0.925000000000001,-0.920000000000001,
-0.915000000000001,-0.910000000000001,-0.905000000000001,-0.900000000000001,
-0.895000000000001,-0.890000000000001,-0.885000000000001,-0.880000000000001,
-0.875000000000001,-0.870000000000001,-0.865000000000001,-0.860000000000001,
-0.855000000000001,-0.850000000000001,-0.845000000000001,-0.840000000000001,
-0.835000000000001,-0.830000000000001,-0.825000000000001,-0.820000000000001,
-0.815000000000001,-0.810000000000001,-0.805000000000001,-0.800000000000001,
-0.795000000000001,-0.790000000000001,-0.785000000000001,-0.780000000000001,
-0.775000000000001,-0.770000000000001,-0.765000000000001,-0.760000000000001,
-0.755000000000001,-0.750000000000001,-0.745000000000001,-0.740000000000001,
-0.735000000000001,-0.730000000000001,-0.725000000000001,-0.720000000000001,
-0.715000000000001,-0.710000000000001,-0.705000000000001,-0.700000000000001,
-0.695000000000001,-0.690000000000001,-0.685,-0.68,-0.675,-0.67,-0.665,
-0.66,-0.655,-0.65,-0.645,-0.64,-0.635,-0.63,-0.625,-0.62,-0.615,-0.61,
-0.605,-0.6,-0.595,-0.59,-0.585,-0.58,-0.575,-0.57,-0.565,-0.56,-0.555,
-0.55,-0.545,-0.54,-0.535,-0.53,-0.525,-0.52,-0.515,-0.51,-0.505,-0.5,-0.495,
-0.49,-0.485,-0.48,-0.475,-0.47,-0.465,-0.46,-0.455,-0.45,-0.445,-0.44,
-0.435,-0.43,-0.425,-0.42,-0.415,-0.41,-0.405,-0.4,-0.395,-0.39,-0.385,
-0.38,-0.375,-0.37,-0.365,-0.36,-0.355,-0.35,-0.345,-0.34,-0.335,-0.33,
-0.325,-0.32,-0.315,-0.31,-0.305,-0.3,-0.295,-0.29,-0.285,-0.28,-0.275,
-0.27,-0.265,-0.26,-0.255,-0.25,-0.245,-0.24,-0.235,-0.23,-0.225,-0.22,
-0.215,-0.21,-0.205,-0.2,-0.195,-0.19,-0.185,-0.18,-0.175,-0.17,-0.165,
-0.16,-0.155,-0.15,-0.145,-0.14,-0.135,-0.13,-0.125,-0.12,-0.115,-0.11,
-0.105,-0.1,-0.095,-0.09,-0.085,-0.08,-0.075,-0.07,-0.065,-0.06,-0.055,
-0.05,-0.045,-0.04,-0.035,-0.03,-0.025,-0.02,-0.015,-0.01,-0.005,0.),
 .UNSPECIFIED.)
CURVE()
GEOMETRIC_REPRESENTATION_ITEM()
RATIONAL_B_SPLINE_CURVE((1.,1.,1.,1.,1.,1.,1.,1.,1.,1.,1.,1.,1.,1.,1.,1.,
1.,1.,1.,1.,1.,1.,1.,1.,1.,1.,1.,1.,1.,1.,1.,1.,1.,1.,1.,1.,1.,1.,1.,1.,
1.,1.,1.,1.,1.,1.,1.,1.,1.,1.,1.,1.,1.,1.,1.,1.,1.,1.,1.,1.,1.,1.,1.,1.,
1.,1.,1.,1.,1.,1.,1.,1.,1.,1.,1.,1.,1.,1.,1.,1.,1.,1.,1.,1.,1.,1.,1.,1.,
1.,1.,1.,1.,1.,1.,1.,1.,1.,1.,1.,1.,1.,1.,1.,1.,1.,1.,1.,1.,1.,1.,1.,1.,
1.,1.,1.,1.,1.,1.,1.,1.,1.,1.,1.,1.,1.,1.,1.,1.,1.,1.,1.,1.,1.,1.,1.,1.,
1.,1.,1.,1.,1.,1.,1.,1.,1.,1.,1.,1.,1.,1.,1.,1.,1.,1.,1.,1.,1.,1.,1.,1.,
1.,1.,1.,1.,1.,1.,1.,1.,1.,1.,1.,1.,1.,1.,1.,1.,1.,1.,1.,1.,1.,1.,1.,1.,
1.,1.,1.,1.,1.,1.,1.,1.,1.,1.,1.,1.,1.,1.,1.,1.,1.,1.,1.,1.,1.))
REPRESENTATION_ITEM('')
);
#816=(
BOUNDED_CURVE()
B_SPLINE_CURVE(5,(#228190,#228191,#228192,#228193,#228194,#228195,#228196,
#228197,#228198,#228199,#228200,#228201,#228202,#228203,#228204,#228205,
#228206,#228207,#228208,#228209,#228210,#228211,#228212,#228213,#228214,
#228215,#228216,#228217,#228218,#228219,#228220,#228221,#228222,#228223,
#228224,#228225,#228226,#228227,#228228,#228229,#228230,#228231,#228232,
#228233,#228234,#228235,#228236,#228237,#228238,#228239,#228240,#228241,
#228242,#228243,#228244,#228245,#228246,#228247,#228248,#228249,#228250,
#228251,#228252,#228253,#228254,#228255,#228256,#228257,#228258,#228259,
#228260,#228261,#228262,#228263,#228264,#228265,#228266,#228267,#228268,
#228269,#228270,#228271,#228272,#228273,#228274,#228275,#228276,#228277,
#228278,#228279,#228280,#228281,#228282,#228283,#228284,#228285,#228286,
#228287,#228288,#228289,#228290,#228291,#228292,#228293,#228294,#228295,
#228296,#228297,#228298,#228299,#228300,#228301,#228302,#228303,#228304,
#228305,#228306,#228307,#228308,#228309,#228310,#228311,#228312,#228313,
#228314,#228315,#228316,#228317,#228318,#228319,#228320,#228321,#228322,
#228323,#228324,#228325,#228326,#228327,#228328,#228329,#228330,#228331,
#228332,#228333,#228334,#228335,#228336,#228337,#228338,#228339,#228340,
#228341,#228342,#228343,#228344,#228345,#228346,#228347,#228348,#228349,
#228350,#228351,#228352,#228353,#228354,#228355,#228356,#228357,#228358,
#228359,#228360,#228361,#228362,#228363,#228364,#228365,#228366,#228367,
#228368,#228369,#228370,#228371,#228372,#228373,#228374,#228375,#228376,
#228377,#228378,#228379,#228380,#228381,#228382,#228383,#228384,#228385,
#228386,#228387,#228388,#228389,#228390,#228391,#228392,#228393,#228394),
 .UNSPECIFIED.,.F.,.F.)
B_SPLINE_CURVE_WITH_KNOTS((6,1,1,1,1,1,1,1,1,1,1,1,1,1,1,1,1,1,1,1,1,1,
1,1,1,1,1,1,1,1,1,1,1,1,1,1,1,1,1,1,1,1,1,1,1,1,1,1,1,1,1,1,1,1,1,1,1,1,
1,1,1,1,1,1,1,1,1,1,1,1,1,1,1,1,1,1,1,1,1,1,1,1,1,1,1,1,1,1,1,1,1,1,1,1,
1,1,1,1,1,1,1,1,1,1,1,1,1,1,1,1,1,1,1,1,1,1,1,1,1,1,1,1,1,1,1,1,1,1,1,1,
1,1,1,1,1,1,1,1,1,1,1,1,1,1,1,1,1,1,1,1,1,1,1,1,1,1,1,1,1,1,1,1,1,1,1,1,
1,1,1,1,1,1,1,1,1,1,1,1,1,1,1,1,1,1,1,1,1,1,1,1,1,1,1,1,1,1,1,1,1,1,6),
(0.,0.005,0.01,0.015,0.02,0.025,0.03,0.035,0.04,0.045,0.05,0.055,0.06,0.065,
0.07,0.075,0.08,0.085,0.09,0.095,0.1,0.105,0.11,0.115,0.12,0.125,0.13,0.135,
0.14,0.145,0.15,0.155,0.16,0.165,0.17,0.175,0.18,0.185,0.19,0.195,0.2,0.205,
0.21,0.215,0.22,0.225,0.23,0.235,0.24,0.245,0.25,0.255,0.26,0.265,0.27,
0.275,0.28,0.285,0.29,0.295,0.3,0.305,0.31,0.315,0.32,0.325,0.33,0.335,
0.34,0.345,0.35,0.355,0.36,0.365,0.37,0.375,0.38,0.385,0.39,0.395,0.4,0.405,
0.41,0.415,0.42,0.425,0.43,0.435,0.44,0.445,0.45,0.455,0.46,0.465,0.47,
0.475,0.48,0.485,0.49,0.495,0.5,0.505,0.51,0.515,0.52,0.525,0.53,0.535,
0.54,0.545,0.55,0.555,0.56,0.565,0.57,0.575,0.58,0.585,0.59,0.595,0.6,0.605,
0.61,0.615,0.62,0.625,0.63,0.635,0.64,0.645,0.65,0.655,0.66,0.665,0.67,
0.675,0.68,0.685,0.690000000000001,0.695000000000001,0.700000000000001,
0.705000000000001,0.710000000000001,0.715000000000001,0.720000000000001,
0.725000000000001,0.730000000000001,0.735000000000001,0.740000000000001,
0.745000000000001,0.750000000000001,0.755000000000001,0.760000000000001,
0.765000000000001,0.770000000000001,0.775000000000001,0.780000000000001,
0.785000000000001,0.790000000000001,0.795000000000001,0.800000000000001,
0.805000000000001,0.810000000000001,0.815000000000001,0.820000000000001,
0.825000000000001,0.830000000000001,0.835000000000001,0.840000000000001,
0.845000000000001,0.850000000000001,0.855000000000001,0.860000000000001,
0.865000000000001,0.870000000000001,0.875000000000001,0.880000000000001,
0.885000000000001,0.890000000000001,0.895000000000001,0.900000000000001,
0.905000000000001,0.910000000000001,0.915000000000001,0.920000000000001,
0.925000000000001,0.930000000000001,0.935000000000001,0.940000000000001,
0.945000000000001,0.950000000000001,0.955000000000001,0.960000000000001,
0.965000000000001,0.970000000000001,0.975000000000001,0.980000000000001,
0.985000000000001,0.990000000000001,0.995000000000001,1.),.UNSPECIFIED.)
CURVE()
GEOMETRIC_REPRESENTATION_ITEM()
RATIONAL_B_SPLINE_CURVE((1.,1.,1.,1.,1.,1.,1.,1.,1.,1.,1.,1.,1.,1.,1.,1.,
1.,1.,1.,1.,1.,1.,1.,1.,1.,1.,1.,1.,1.,1.,1.,1.,1.,1.,1.,1.,1.,1.,1.,1.,
1.,1.,1.,1.,1.,1.,1.,1.,1.,1.,1.,1.,1.,1.,1.,1.,1.,1.,1.,1.,1.,1.,1.,1.,
1.,1.,1.,1.,1.,1.,1.,1.,1.,1.,1.,1.,1.,1.,1.,1.,1.,1.,1.,1.,1.,1.,1.,1.,
1.,1.,1.,1.,1.,1.,1.,1.,1.,1.,1.,1.,1.,1.,1.,1.,1.,1.,1.,1.,1.,1.,1.,1.,
1.,1.,1.,1.,1.,1.,1.,1.,1.,1.,1.,1.,1.,1.,1.,1.,1.,1.,1.,1.,1.,1.,1.,1.,
1.,1.,1.,1.,1.,1.,1.,1.,1.,1.,1.,1.,1.,1.,1.,1.,1.,1.,1.,1.,1.,1.,1.,1.,
1.,1.,1.,1.,1.,1.,1.,1.,1.,1.,1.,1.,1.,1.,1.,1.,1.,1.,1.,1.,1.,1.,1.,1.,
1.,1.,1.,1.,1.,1.,1.,1.,1.,1.,1.,1.,1.,1.,1.,1.,1.,1.,1.,1.,1.))
REPRESENTATION_ITEM('')
);
#817=(
BOUNDED_CURVE()
B_SPLINE_CURVE(5,(#228806,#228807,#228808,#228809,#228810,#228811,#228812,
#228813,#228814,#228815,#228816,#228817,#228818,#228819,#228820,#228821,
#228822,#228823,#228824,#228825,#228826,#228827,#228828,#228829,#228830,
#228831,#228832,#228833,#228834,#228835,#228836,#228837,#228838,#228839,
#228840,#228841,#228842,#228843,#228844,#228845,#228846,#228847,#228848,
#228849,#228850,#228851,#228852,#228853,#228854,#228855,#228856,#228857,
#228858,#228859,#228860,#228861,#228862,#228863,#228864,#228865,#228866,
#228867,#228868,#228869,#228870,#228871,#228872,#228873,#228874,#228875,
#228876,#228877,#228878,#228879,#228880,#228881,#228882,#228883,#228884,
#228885,#228886,#228887,#228888,#228889,#228890,#228891,#228892,#228893,
#228894,#228895,#228896,#228897,#228898,#228899,#228900,#228901,#228902,
#228903,#228904,#228905,#228906,#228907,#228908,#228909,#228910,#228911,
#228912,#228913,#228914,#228915,#228916,#228917,#228918,#228919,#228920,
#228921,#228922,#228923,#228924,#228925,#228926,#228927,#228928,#228929,
#228930,#228931,#228932,#228933,#228934,#228935,#228936,#228937,#228938,
#228939,#228940,#228941,#228942,#228943,#228944,#228945,#228946,#228947,
#228948,#228949,#228950,#228951,#228952,#228953,#228954,#228955,#228956,
#228957,#228958,#228959,#228960,#228961,#228962,#228963,#228964,#228965,
#228966,#228967,#228968,#228969,#228970,#228971,#228972,#228973,#228974,
#228975,#228976,#228977,#228978,#228979,#228980,#228981,#228982,#228983,
#228984,#228985,#228986,#228987,#228988,#228989,#228990,#228991,#228992,
#228993,#228994,#228995,#228996,#228997,#228998,#228999,#229000,#229001,
#229002,#229003,#229004,#229005,#229006,#229007,#229008,#229009,#229010),
 .UNSPECIFIED.,.F.,.F.)
B_SPLINE_CURVE_WITH_KNOTS((6,1,1,1,1,1,1,1,1,1,1,1,1,1,1,1,1,1,1,1,1,1,
1,1,1,1,1,1,1,1,1,1,1,1,1,1,1,1,1,1,1,1,1,1,1,1,1,1,1,1,1,1,1,1,1,1,1,1,
1,1,1,1,1,1,1,1,1,1,1,1,1,1,1,1,1,1,1,1,1,1,1,1,1,1,1,1,1,1,1,1,1,1,1,1,
1,1,1,1,1,1,1,1,1,1,1,1,1,1,1,1,1,1,1,1,1,1,1,1,1,1,1,1,1,1,1,1,1,1,1,1,
1,1,1,1,1,1,1,1,1,1,1,1,1,1,1,1,1,1,1,1,1,1,1,1,1,1,1,1,1,1,1,1,1,1,1,1,
1,1,1,1,1,1,1,1,1,1,1,1,1,1,1,1,1,1,1,1,1,1,1,1,1,1,1,1,1,1,1,1,1,1,6),
(0.,0.005,0.01,0.015,0.02,0.025,0.03,0.035,0.04,0.045,0.05,0.055,0.06,0.065,
0.07,0.075,0.08,0.085,0.09,0.095,0.1,0.105,0.11,0.115,0.12,0.125,0.13,0.135,
0.14,0.145,0.15,0.155,0.16,0.165,0.17,0.175,0.18,0.185,0.19,0.195,0.2,0.205,
0.21,0.215,0.22,0.225,0.23,0.235,0.24,0.245,0.25,0.255,0.26,0.265,0.27,
0.275,0.28,0.285,0.29,0.295,0.3,0.305,0.31,0.315,0.32,0.325,0.33,0.335,
0.34,0.345,0.35,0.355,0.36,0.365,0.37,0.375,0.38,0.385,0.39,0.395,0.4,0.405,
0.41,0.415,0.42,0.425,0.43,0.435,0.44,0.445,0.45,0.455,0.46,0.465,0.47,
0.475,0.48,0.485,0.49,0.495,0.5,0.505,0.51,0.515,0.52,0.525,0.53,0.535,
0.54,0.545,0.55,0.555,0.56,0.565,0.57,0.575,0.58,0.585,0.59,0.595,0.6,0.605,
0.61,0.615,0.62,0.625,0.63,0.635,0.64,0.645,0.65,0.655,0.66,0.665,0.67,
0.675,0.68,0.685,0.690000000000001,0.695000000000001,0.700000000000001,
0.705000000000001,0.710000000000001,0.715000000000001,0.720000000000001,
0.725000000000001,0.730000000000001,0.735000000000001,0.740000000000001,
0.745000000000001,0.750000000000001,0.755000000000001,0.760000000000001,
0.765000000000001,0.770000000000001,0.775000000000001,0.780000000000001,
0.785000000000001,0.790000000000001,0.795000000000001,0.800000000000001,
0.805000000000001,0.810000000000001,0.815000000000001,0.820000000000001,
0.825000000000001,0.830000000000001,0.835000000000001,0.840000000000001,
0.845000000000001,0.850000000000001,0.855000000000001,0.860000000000001,
0.865000000000001,0.870000000000001,0.875000000000001,0.880000000000001,
0.885000000000001,0.890000000000001,0.895000000000001,0.900000000000001,
0.905000000000001,0.910000000000001,0.915000000000001,0.920000000000001,
0.925000000000001,0.930000000000001,0.935000000000001,0.940000000000001,
0.945000000000001,0.950000000000001,0.955000000000001,0.960000000000001,
0.965000000000001,0.970000000000001,0.975000000000001,0.980000000000001,
0.985000000000001,0.990000000000001,0.995000000000001,1.),.UNSPECIFIED.)
CURVE()
GEOMETRIC_REPRESENTATION_ITEM()
RATIONAL_B_SPLINE_CURVE((1.,1.,1.,1.,1.,1.,1.,1.,1.,1.,1.,1.,1.,1.,1.,1.,
1.,1.,1.,1.,1.,1.,1.,1.,1.,1.,1.,1.,1.,1.,1.,1.,1.,1.,1.,1.,1.,1.,1.,1.,
1.,1.,1.,1.,1.,1.,1.,1.,1.,1.,1.,1.,1.,1.,1.,1.,1.,1.,1.,1.,1.,1.,1.,1.,
1.,1.,1.,1.,1.,1.,1.,1.,1.,1.,1.,1.,1.,1.,1.,1.,1.,1.,1.,1.,1.,1.,1.,1.,
1.,1.,1.,1.,1.,1.,1.,1.,1.,1.,1.,1.,1.,1.,1.,1.,1.,1.,1.,1.,1.,1.,1.,1.,
1.,1.,1.,1.,1.,1.,1.,1.,1.,1.,1.,1.,1.,1.,1.,1.,1.,1.,1.,1.,1.,1.,1.,1.,
1.,1.,1.,1.,1.,1.,1.,1.,1.,1.,1.,1.,1.,1.,1.,1.,1.,1.,1.,1.,1.,1.,1.,1.,
1.,1.,1.,1.,1.,1.,1.,1.,1.,1.,1.,1.,1.,1.,1.,1.,1.,1.,1.,1.,1.,1.,1.,1.,
1.,1.,1.,1.,1.,1.,1.,1.,1.,1.,1.,1.,1.,1.,1.,1.,1.,1.,1.,1.,1.))
REPRESENTATION_ITEM('')
);
#818=(
BOUNDED_CURVE()
B_SPLINE_CURVE(5,(#229012,#229013,#229014,#229015,#229016,#229017,#229018,
#229019,#229020,#229021,#229022,#229023,#229024,#229025,#229026,#229027,
#229028,#229029,#229030,#229031,#229032,#229033,#229034,#229035,#229036,
#229037,#229038,#229039,#229040,#229041,#229042,#229043,#229044,#229045,
#229046,#229047,#229048,#229049,#229050,#229051,#229052,#229053,#229054,
#229055,#229056,#229057,#229058,#229059,#229060,#229061,#229062,#229063,
#229064,#229065,#229066,#229067,#229068,#229069,#229070,#229071,#229072,
#229073,#229074,#229075,#229076,#229077,#229078,#229079,#229080,#229081,
#229082,#229083,#229084,#229085,#229086,#229087,#229088,#229089,#229090,
#229091,#229092,#229093,#229094,#229095,#229096,#229097,#229098,#229099,
#229100,#229101,#229102,#229103,#229104,#229105,#229106,#229107,#229108,
#229109,#229110,#229111,#229112,#229113,#229114,#229115,#229116,#229117,
#229118,#229119,#229120,#229121,#229122,#229123,#229124,#229125,#229126,
#229127,#229128,#229129,#229130,#229131,#229132,#229133,#229134,#229135,
#229136,#229137,#229138,#229139,#229140,#229141,#229142,#229143,#229144,
#229145,#229146,#229147,#229148,#229149,#229150,#229151,#229152,#229153,
#229154,#229155,#229156,#229157,#229158,#229159,#229160,#229161,#229162,
#229163,#229164,#229165,#229166,#229167,#229168,#229169,#229170,#229171,
#229172,#229173,#229174,#229175,#229176,#229177,#229178,#229179,#229180,
#229181,#229182,#229183,#229184,#229185,#229186,#229187,#229188,#229189,
#229190,#229191,#229192,#229193,#229194,#229195,#229196,#229197,#229198,
#229199,#229200,#229201,#229202,#229203,#229204,#229205,#229206,#229207,
#229208,#229209,#229210,#229211,#229212,#229213,#229214,#229215,#229216),
 .UNSPECIFIED.,.F.,.F.)
B_SPLINE_CURVE_WITH_KNOTS((6,1,1,1,1,1,1,1,1,1,1,1,1,1,1,1,1,1,1,1,1,1,
1,1,1,1,1,1,1,1,1,1,1,1,1,1,1,1,1,1,1,1,1,1,1,1,1,1,1,1,1,1,1,1,1,1,1,1,
1,1,1,1,1,1,1,1,1,1,1,1,1,1,1,1,1,1,1,1,1,1,1,1,1,1,1,1,1,1,1,1,1,1,1,1,
1,1,1,1,1,1,1,1,1,1,1,1,1,1,1,1,1,1,1,1,1,1,1,1,1,1,1,1,1,1,1,1,1,1,1,1,
1,1,1,1,1,1,1,1,1,1,1,1,1,1,1,1,1,1,1,1,1,1,1,1,1,1,1,1,1,1,1,1,1,1,1,1,
1,1,1,1,1,1,1,1,1,1,1,1,1,1,1,1,1,1,1,1,1,1,1,1,1,1,1,1,1,1,1,1,1,1,6),
(-1.,-0.995000000000001,-0.990000000000001,-0.985000000000001,-0.980000000000001,
-0.975000000000001,-0.970000000000001,-0.965000000000001,-0.960000000000001,
-0.955000000000001,-0.950000000000001,-0.945000000000001,-0.940000000000001,
-0.935000000000001,-0.930000000000001,-0.925000000000001,-0.920000000000001,
-0.915000000000001,-0.910000000000001,-0.905000000000001,-0.900000000000001,
-0.895000000000001,-0.890000000000001,-0.885000000000001,-0.880000000000001,
-0.875000000000001,-0.870000000000001,-0.865000000000001,-0.860000000000001,
-0.855000000000001,-0.850000000000001,-0.845000000000001,-0.840000000000001,
-0.835000000000001,-0.830000000000001,-0.825000000000001,-0.820000000000001,
-0.815000000000001,-0.810000000000001,-0.805000000000001,-0.800000000000001,
-0.795000000000001,-0.790000000000001,-0.785000000000001,-0.780000000000001,
-0.775000000000001,-0.770000000000001,-0.765000000000001,-0.760000000000001,
-0.755000000000001,-0.750000000000001,-0.745000000000001,-0.740000000000001,
-0.735000000000001,-0.730000000000001,-0.725000000000001,-0.720000000000001,
-0.715000000000001,-0.710000000000001,-0.705000000000001,-0.700000000000001,
-0.695000000000001,-0.690000000000001,-0.685,-0.68,-0.675,-0.67,-0.665,
-0.66,-0.655,-0.65,-0.645,-0.64,-0.635,-0.63,-0.625,-0.62,-0.615,-0.61,
-0.605,-0.6,-0.595,-0.59,-0.585,-0.58,-0.575,-0.57,-0.565,-0.56,-0.555,
-0.55,-0.545,-0.54,-0.535,-0.53,-0.525,-0.52,-0.515,-0.51,-0.505,-0.5,-0.495,
-0.49,-0.485,-0.48,-0.475,-0.47,-0.465,-0.46,-0.455,-0.45,-0.445,-0.44,
-0.435,-0.43,-0.425,-0.42,-0.415,-0.41,-0.405,-0.4,-0.395,-0.39,-0.385,
-0.38,-0.375,-0.37,-0.365,-0.36,-0.355,-0.35,-0.345,-0.34,-0.335,-0.33,
-0.325,-0.32,-0.315,-0.31,-0.305,-0.3,-0.295,-0.29,-0.285,-0.28,-0.275,
-0.27,-0.265,-0.26,-0.255,-0.25,-0.245,-0.24,-0.235,-0.23,-0.225,-0.22,
-0.215,-0.21,-0.205,-0.2,-0.195,-0.19,-0.185,-0.18,-0.175,-0.17,-0.165,
-0.16,-0.155,-0.15,-0.145,-0.14,-0.135,-0.13,-0.125,-0.12,-0.115,-0.11,
-0.105,-0.1,-0.095,-0.09,-0.085,-0.08,-0.075,-0.07,-0.065,-0.06,-0.055,
-0.05,-0.045,-0.04,-0.035,-0.03,-0.025,-0.02,-0.015,-0.01,-0.005,0.),
 .UNSPECIFIED.)
CURVE()
GEOMETRIC_REPRESENTATION_ITEM()
RATIONAL_B_SPLINE_CURVE((1.,1.,1.,1.,1.,1.,1.,1.,1.,1.,1.,1.,1.,1.,1.,1.,
1.,1.,1.,1.,1.,1.,1.,1.,1.,1.,1.,1.,1.,1.,1.,1.,1.,1.,1.,1.,1.,1.,1.,1.,
1.,1.,1.,1.,1.,1.,1.,1.,1.,1.,1.,1.,1.,1.,1.,1.,1.,1.,1.,1.,1.,1.,1.,1.,
1.,1.,1.,1.,1.,1.,1.,1.,1.,1.,1.,1.,1.,1.,1.,1.,1.,1.,1.,1.,1.,1.,1.,1.,
1.,1.,1.,1.,1.,1.,1.,1.,1.,1.,1.,1.,1.,1.,1.,1.,1.,1.,1.,1.,1.,1.,1.,1.,
1.,1.,1.,1.,1.,1.,1.,1.,1.,1.,1.,1.,1.,1.,1.,1.,1.,1.,1.,1.,1.,1.,1.,1.,
1.,1.,1.,1.,1.,1.,1.,1.,1.,1.,1.,1.,1.,1.,1.,1.,1.,1.,1.,1.,1.,1.,1.,1.,
1.,1.,1.,1.,1.,1.,1.,1.,1.,1.,1.,1.,1.,1.,1.,1.,1.,1.,1.,1.,1.,1.,1.,1.,
1.,1.,1.,1.,1.,1.,1.,1.,1.,1.,1.,1.,1.,1.,1.,1.,1.,1.,1.,1.,1.))
REPRESENTATION_ITEM('')
);
#819=(
BOUNDED_CURVE()
B_SPLINE_CURVE(5,(#229635,#229636,#229637,#229638,#229639,#229640,#229641,
#229642,#229643,#229644,#229645,#229646,#229647,#229648,#229649,#229650,
#229651,#229652,#229653,#229654,#229655,#229656,#229657,#229658,#229659,
#229660,#229661,#229662,#229663,#229664,#229665,#229666,#229667,#229668,
#229669,#229670,#229671,#229672,#229673,#229674,#229675,#229676,#229677,
#229678,#229679,#229680,#229681,#229682,#229683,#229684,#229685,#229686,
#229687,#229688,#229689,#229690,#229691,#229692,#229693,#229694,#229695,
#229696,#229697,#229698,#229699,#229700,#229701,#229702,#229703,#229704,
#229705,#229706,#229707,#229708,#229709,#229710,#229711,#229712,#229713,
#229714,#229715,#229716,#229717,#229718,#229719,#229720,#229721,#229722,
#229723,#229724,#229725,#229726,#229727,#229728,#229729,#229730,#229731,
#229732,#229733,#229734,#229735,#229736,#229737,#229738,#229739,#229740,
#229741,#229742,#229743,#229744,#229745,#229746,#229747,#229748,#229749,
#229750,#229751,#229752,#229753,#229754,#229755,#229756,#229757,#229758,
#229759,#229760,#229761,#229762,#229763,#229764,#229765,#229766,#229767,
#229768,#229769,#229770,#229771,#229772,#229773,#229774,#229775,#229776,
#229777,#229778,#229779,#229780,#229781,#229782,#229783,#229784,#229785,
#229786,#229787,#229788,#229789,#229790,#229791,#229792,#229793,#229794,
#229795,#229796,#229797,#229798,#229799,#229800,#229801,#229802,#229803,
#229804,#229805,#229806,#229807,#229808,#229809,#229810,#229811,#229812,
#229813,#229814,#229815,#229816,#229817,#229818,#229819,#229820,#229821,
#229822,#229823,#229824,#229825,#229826,#229827,#229828,#229829,#229830,
#229831,#229832,#229833,#229834,#229835,#229836,#229837,#229838,#229839),
 .UNSPECIFIED.,.F.,.F.)
B_SPLINE_CURVE_WITH_KNOTS((6,1,1,1,1,1,1,1,1,1,1,1,1,1,1,1,1,1,1,1,1,1,
1,1,1,1,1,1,1,1,1,1,1,1,1,1,1,1,1,1,1,1,1,1,1,1,1,1,1,1,1,1,1,1,1,1,1,1,
1,1,1,1,1,1,1,1,1,1,1,1,1,1,1,1,1,1,1,1,1,1,1,1,1,1,1,1,1,1,1,1,1,1,1,1,
1,1,1,1,1,1,1,1,1,1,1,1,1,1,1,1,1,1,1,1,1,1,1,1,1,1,1,1,1,1,1,1,1,1,1,1,
1,1,1,1,1,1,1,1,1,1,1,1,1,1,1,1,1,1,1,1,1,1,1,1,1,1,1,1,1,1,1,1,1,1,1,1,
1,1,1,1,1,1,1,1,1,1,1,1,1,1,1,1,1,1,1,1,1,1,1,1,1,1,1,1,1,1,1,1,1,1,6),
(-1.,-0.995000000000001,-0.990000000000001,-0.985000000000001,-0.980000000000001,
-0.975000000000001,-0.970000000000001,-0.965000000000001,-0.960000000000001,
-0.955000000000001,-0.950000000000001,-0.945000000000001,-0.940000000000001,
-0.935000000000001,-0.930000000000001,-0.925000000000001,-0.920000000000001,
-0.915000000000001,-0.910000000000001,-0.905000000000001,-0.900000000000001,
-0.895000000000001,-0.890000000000001,-0.885000000000001,-0.880000000000001,
-0.875000000000001,-0.870000000000001,-0.865000000000001,-0.860000000000001,
-0.855000000000001,-0.850000000000001,-0.845000000000001,-0.840000000000001,
-0.835000000000001,-0.830000000000001,-0.825000000000001,-0.820000000000001,
-0.815000000000001,-0.810000000000001,-0.805000000000001,-0.800000000000001,
-0.795000000000001,-0.790000000000001,-0.785000000000001,-0.780000000000001,
-0.775000000000001,-0.770000000000001,-0.765000000000001,-0.760000000000001,
-0.755000000000001,-0.750000000000001,-0.745000000000001,-0.740000000000001,
-0.735000000000001,-0.730000000000001,-0.725000000000001,-0.720000000000001,
-0.715000000000001,-0.710000000000001,-0.705000000000001,-0.700000000000001,
-0.695000000000001,-0.690000000000001,-0.685,-0.68,-0.675,-0.67,-0.665,
-0.66,-0.655,-0.65,-0.645,-0.64,-0.635,-0.63,-0.625,-0.62,-0.615,-0.61,
-0.605,-0.6,-0.595,-0.59,-0.585,-0.58,-0.575,-0.57,-0.565,-0.56,-0.555,
-0.55,-0.545,-0.54,-0.535,-0.53,-0.525,-0.52,-0.515,-0.51,-0.505,-0.5,-0.495,
-0.49,-0.485,-0.48,-0.475,-0.47,-0.465,-0.46,-0.455,-0.45,-0.445,-0.44,
-0.435,-0.43,-0.425,-0.42,-0.415,-0.41,-0.405,-0.4,-0.395,-0.39,-0.385,
-0.38,-0.375,-0.37,-0.365,-0.36,-0.355,-0.35,-0.345,-0.34,-0.335,-0.33,
-0.325,-0.32,-0.315,-0.31,-0.305,-0.3,-0.295,-0.29,-0.285,-0.28,-0.275,
-0.27,-0.265,-0.26,-0.255,-0.25,-0.245,-0.24,-0.235,-0.23,-0.225,-0.22,
-0.215,-0.21,-0.205,-0.2,-0.195,-0.19,-0.185,-0.18,-0.175,-0.17,-0.165,
-0.16,-0.155,-0.15,-0.145,-0.14,-0.135,-0.13,-0.125,-0.12,-0.115,-0.11,
-0.105,-0.1,-0.095,-0.09,-0.085,-0.08,-0.075,-0.07,-0.065,-0.06,-0.055,
-0.05,-0.045,-0.04,-0.035,-0.03,-0.025,-0.02,-0.015,-0.01,-0.005,0.),
 .UNSPECIFIED.)
CURVE()
GEOMETRIC_REPRESENTATION_ITEM()
RATIONAL_B_SPLINE_CURVE((1.,1.,1.,1.,1.,1.,1.,1.,1.,1.,1.,1.,1.,1.,1.,1.,
1.,1.,1.,1.,1.,1.,1.,1.,1.,1.,1.,1.,1.,1.,1.,1.,1.,1.,1.,1.,1.,1.,1.,1.,
1.,1.,1.,1.,1.,1.,1.,1.,1.,1.,1.,1.,1.,1.,1.,1.,1.,1.,1.,1.,1.,1.,1.,1.,
1.,1.,1.,1.,1.,1.,1.,1.,1.,1.,1.,1.,1.,1.,1.,1.,1.,1.,1.,1.,1.,1.,1.,1.,
1.,1.,1.,1.,1.,1.,1.,1.,1.,1.,1.,1.,1.,1.,1.,1.,1.,1.,1.,1.,1.,1.,1.,1.,
1.,1.,1.,1.,1.,1.,1.,1.,1.,1.,1.,1.,1.,1.,1.,1.,1.,1.,1.,1.,1.,1.,1.,1.,
1.,1.,1.,1.,1.,1.,1.,1.,1.,1.,1.,1.,1.,1.,1.,1.,1.,1.,1.,1.,1.,1.,1.,1.,
1.,1.,1.,1.,1.,1.,1.,1.,1.,1.,1.,1.,1.,1.,1.,1.,1.,1.,1.,1.,1.,1.,1.,1.,
1.,1.,1.,1.,1.,1.,1.,1.,1.,1.,1.,1.,1.,1.,1.,1.,1.,1.,1.,1.,1.))
REPRESENTATION_ITEM('')
);
#820=(
BOUNDED_CURVE()
B_SPLINE_CURVE(5,(#229842,#229843,#229844,#229845,#229846,#229847,#229848,
#229849,#229850,#229851,#229852,#229853,#229854,#229855,#229856,#229857,
#229858,#229859,#229860,#229861,#229862,#229863,#229864,#229865,#229866,
#229867,#229868,#229869,#229870,#229871,#229872,#229873,#229874,#229875,
#229876,#229877,#229878,#229879,#229880,#229881,#229882,#229883,#229884,
#229885,#229886,#229887,#229888,#229889,#229890,#229891,#229892,#229893,
#229894,#229895,#229896,#229897,#229898,#229899,#229900,#229901,#229902,
#229903,#229904,#229905,#229906,#229907,#229908,#229909,#229910,#229911,
#229912,#229913,#229914,#229915,#229916,#229917,#229918,#229919,#229920,
#229921,#229922,#229923,#229924,#229925,#229926,#229927,#229928,#229929,
#229930,#229931,#229932,#229933,#229934,#229935,#229936,#229937,#229938,
#229939,#229940,#229941,#229942,#229943,#229944,#229945,#229946,#229947,
#229948,#229949,#229950,#229951,#229952,#229953,#229954,#229955,#229956,
#229957,#229958,#229959,#229960,#229961,#229962,#229963,#229964,#229965,
#229966,#229967,#229968,#229969,#229970,#229971,#229972,#229973,#229974,
#229975,#229976,#229977,#229978,#229979,#229980,#229981,#229982,#229983,
#229984,#229985,#229986,#229987,#229988,#229989,#229990,#229991,#229992,
#229993,#229994,#229995,#229996,#229997,#229998,#229999,#230000,#230001,
#230002,#230003,#230004,#230005,#230006,#230007,#230008,#230009,#230010,
#230011,#230012,#230013,#230014,#230015,#230016,#230017,#230018,#230019,
#230020,#230021,#230022,#230023,#230024,#230025,#230026,#230027,#230028,
#230029,#230030,#230031,#230032,#230033,#230034,#230035,#230036,#230037,
#230038,#230039,#230040,#230041,#230042,#230043,#230044,#230045,#230046),
 .UNSPECIFIED.,.F.,.F.)
B_SPLINE_CURVE_WITH_KNOTS((6,1,1,1,1,1,1,1,1,1,1,1,1,1,1,1,1,1,1,1,1,1,
1,1,1,1,1,1,1,1,1,1,1,1,1,1,1,1,1,1,1,1,1,1,1,1,1,1,1,1,1,1,1,1,1,1,1,1,
1,1,1,1,1,1,1,1,1,1,1,1,1,1,1,1,1,1,1,1,1,1,1,1,1,1,1,1,1,1,1,1,1,1,1,1,
1,1,1,1,1,1,1,1,1,1,1,1,1,1,1,1,1,1,1,1,1,1,1,1,1,1,1,1,1,1,1,1,1,1,1,1,
1,1,1,1,1,1,1,1,1,1,1,1,1,1,1,1,1,1,1,1,1,1,1,1,1,1,1,1,1,1,1,1,1,1,1,1,
1,1,1,1,1,1,1,1,1,1,1,1,1,1,1,1,1,1,1,1,1,1,1,1,1,1,1,1,1,1,1,1,1,1,6),
(0.,0.005,0.01,0.015,0.02,0.025,0.03,0.035,0.04,0.045,0.05,0.055,0.06,0.065,
0.07,0.075,0.08,0.085,0.09,0.095,0.1,0.105,0.11,0.115,0.12,0.125,0.13,0.135,
0.14,0.145,0.15,0.155,0.16,0.165,0.17,0.175,0.18,0.185,0.19,0.195,0.2,0.205,
0.21,0.215,0.22,0.225,0.23,0.235,0.24,0.245,0.25,0.255,0.26,0.265,0.27,
0.275,0.28,0.285,0.29,0.295,0.3,0.305,0.31,0.315,0.32,0.325,0.33,0.335,
0.34,0.345,0.35,0.355,0.36,0.365,0.37,0.375,0.38,0.385,0.39,0.395,0.4,0.405,
0.41,0.415,0.42,0.425,0.43,0.435,0.44,0.445,0.45,0.455,0.46,0.465,0.47,
0.475,0.48,0.485,0.49,0.495,0.5,0.505,0.51,0.515,0.52,0.525,0.53,0.535,
0.54,0.545,0.55,0.555,0.56,0.565,0.57,0.575,0.58,0.585,0.59,0.595,0.6,0.605,
0.61,0.615,0.62,0.625,0.63,0.635,0.64,0.645,0.65,0.655,0.66,0.665,0.67,
0.675,0.68,0.685,0.690000000000001,0.695000000000001,0.700000000000001,
0.705000000000001,0.710000000000001,0.715000000000001,0.720000000000001,
0.725000000000001,0.730000000000001,0.735000000000001,0.740000000000001,
0.745000000000001,0.750000000000001,0.755000000000001,0.760000000000001,
0.765000000000001,0.770000000000001,0.775000000000001,0.780000000000001,
0.785000000000001,0.790000000000001,0.795000000000001,0.800000000000001,
0.805000000000001,0.810000000000001,0.815000000000001,0.820000000000001,
0.825000000000001,0.830000000000001,0.835000000000001,0.840000000000001,
0.845000000000001,0.850000000000001,0.855000000000001,0.860000000000001,
0.865000000000001,0.870000000000001,0.875000000000001,0.880000000000001,
0.885000000000001,0.890000000000001,0.895000000000001,0.900000000000001,
0.905000000000001,0.910000000000001,0.915000000000001,0.920000000000001,
0.925000000000001,0.930000000000001,0.935000000000001,0.940000000000001,
0.945000000000001,0.950000000000001,0.955000000000001,0.960000000000001,
0.965000000000001,0.970000000000001,0.975000000000001,0.980000000000001,
0.985000000000001,0.990000000000001,0.995000000000001,1.),.UNSPECIFIED.)
CURVE()
GEOMETRIC_REPRESENTATION_ITEM()
RATIONAL_B_SPLINE_CURVE((1.,1.,1.,1.,1.,1.,1.,1.,1.,1.,1.,1.,1.,1.,1.,1.,
1.,1.,1.,1.,1.,1.,1.,1.,1.,1.,1.,1.,1.,1.,1.,1.,1.,1.,1.,1.,1.,1.,1.,1.,
1.,1.,1.,1.,1.,1.,1.,1.,1.,1.,1.,1.,1.,1.,1.,1.,1.,1.,1.,1.,1.,1.,1.,1.,
1.,1.,1.,1.,1.,1.,1.,1.,1.,1.,1.,1.,1.,1.,1.,1.,1.,1.,1.,1.,1.,1.,1.,1.,
1.,1.,1.,1.,1.,1.,1.,1.,1.,1.,1.,1.,1.,1.,1.,1.,1.,1.,1.,1.,1.,1.,1.,1.,
1.,1.,1.,1.,1.,1.,1.,1.,1.,1.,1.,1.,1.,1.,1.,1.,1.,1.,1.,1.,1.,1.,1.,1.,
1.,1.,1.,1.,1.,1.,1.,1.,1.,1.,1.,1.,1.,1.,1.,1.,1.,1.,1.,1.,1.,1.,1.,1.,
1.,1.,1.,1.,1.,1.,1.,1.,1.,1.,1.,1.,1.,1.,1.,1.,1.,1.,1.,1.,1.,1.,1.,1.,
1.,1.,1.,1.,1.,1.,1.,1.,1.,1.,1.,1.,1.,1.,1.,1.,1.,1.,1.,1.,1.))
REPRESENTATION_ITEM('')
);
#821=(
BOUNDED_CURVE()
B_SPLINE_CURVE(5,(#230458,#230459,#230460,#230461,#230462,#230463,#230464,
#230465,#230466,#230467,#230468,#230469,#230470,#230471,#230472,#230473,
#230474,#230475,#230476,#230477,#230478,#230479,#230480,#230481,#230482,
#230483,#230484,#230485,#230486,#230487,#230488,#230489,#230490,#230491,
#230492,#230493,#230494,#230495,#230496,#230497,#230498,#230499,#230500,
#230501,#230502,#230503,#230504,#230505,#230506,#230507,#230508,#230509,
#230510,#230511,#230512,#230513,#230514,#230515,#230516,#230517,#230518,
#230519,#230520,#230521,#230522,#230523,#230524,#230525,#230526,#230527,
#230528,#230529,#230530,#230531,#230532,#230533,#230534,#230535,#230536,
#230537,#230538,#230539,#230540,#230541,#230542,#230543,#230544,#230545,
#230546,#230547,#230548,#230549,#230550,#230551,#230552,#230553,#230554,
#230555,#230556,#230557,#230558,#230559,#230560,#230561,#230562,#230563,
#230564,#230565,#230566,#230567,#230568,#230569,#230570,#230571,#230572,
#230573,#230574,#230575,#230576,#230577,#230578,#230579,#230580,#230581,
#230582,#230583,#230584,#230585,#230586,#230587,#230588,#230589,#230590,
#230591,#230592,#230593,#230594,#230595,#230596,#230597,#230598,#230599,
#230600,#230601,#230602,#230603,#230604,#230605,#230606,#230607,#230608,
#230609,#230610,#230611,#230612,#230613,#230614,#230615,#230616,#230617,
#230618,#230619,#230620,#230621,#230622,#230623,#230624,#230625,#230626,
#230627,#230628,#230629,#230630,#230631,#230632,#230633,#230634,#230635,
#230636,#230637,#230638,#230639,#230640,#230641,#230642,#230643,#230644,
#230645,#230646,#230647,#230648,#230649,#230650,#230651,#230652,#230653,
#230654,#230655,#230656,#230657,#230658,#230659,#230660,#230661,#230662),
 .UNSPECIFIED.,.F.,.F.)
B_SPLINE_CURVE_WITH_KNOTS((6,1,1,1,1,1,1,1,1,1,1,1,1,1,1,1,1,1,1,1,1,1,
1,1,1,1,1,1,1,1,1,1,1,1,1,1,1,1,1,1,1,1,1,1,1,1,1,1,1,1,1,1,1,1,1,1,1,1,
1,1,1,1,1,1,1,1,1,1,1,1,1,1,1,1,1,1,1,1,1,1,1,1,1,1,1,1,1,1,1,1,1,1,1,1,
1,1,1,1,1,1,1,1,1,1,1,1,1,1,1,1,1,1,1,1,1,1,1,1,1,1,1,1,1,1,1,1,1,1,1,1,
1,1,1,1,1,1,1,1,1,1,1,1,1,1,1,1,1,1,1,1,1,1,1,1,1,1,1,1,1,1,1,1,1,1,1,1,
1,1,1,1,1,1,1,1,1,1,1,1,1,1,1,1,1,1,1,1,1,1,1,1,1,1,1,1,1,1,1,1,1,1,6),
(0.,0.005,0.01,0.015,0.02,0.025,0.03,0.035,0.04,0.045,0.05,0.055,0.06,0.065,
0.07,0.075,0.08,0.085,0.09,0.095,0.1,0.105,0.11,0.115,0.12,0.125,0.13,0.135,
0.14,0.145,0.15,0.155,0.16,0.165,0.17,0.175,0.18,0.185,0.19,0.195,0.2,0.205,
0.21,0.215,0.22,0.225,0.23,0.235,0.24,0.245,0.25,0.255,0.26,0.265,0.27,
0.275,0.28,0.285,0.29,0.295,0.3,0.305,0.31,0.315,0.32,0.325,0.33,0.335,
0.34,0.345,0.35,0.355,0.36,0.365,0.37,0.375,0.38,0.385,0.39,0.395,0.4,0.405,
0.41,0.415,0.42,0.425,0.43,0.435,0.44,0.445,0.45,0.455,0.46,0.465,0.47,
0.475,0.48,0.485,0.49,0.495,0.5,0.505,0.51,0.515,0.52,0.525,0.53,0.535,
0.54,0.545,0.55,0.555,0.56,0.565,0.57,0.575,0.58,0.585,0.59,0.595,0.6,0.605,
0.61,0.615,0.62,0.625,0.63,0.635,0.64,0.645,0.65,0.655,0.66,0.665,0.67,
0.675,0.68,0.685,0.690000000000001,0.695000000000001,0.700000000000001,
0.705000000000001,0.710000000000001,0.715000000000001,0.720000000000001,
0.725000000000001,0.730000000000001,0.735000000000001,0.740000000000001,
0.745000000000001,0.750000000000001,0.755000000000001,0.760000000000001,
0.765000000000001,0.770000000000001,0.775000000000001,0.780000000000001,
0.785000000000001,0.790000000000001,0.795000000000001,0.800000000000001,
0.805000000000001,0.810000000000001,0.815000000000001,0.820000000000001,
0.825000000000001,0.830000000000001,0.835000000000001,0.840000000000001,
0.845000000000001,0.850000000000001,0.855000000000001,0.860000000000001,
0.865000000000001,0.870000000000001,0.875000000000001,0.880000000000001,
0.885000000000001,0.890000000000001,0.895000000000001,0.900000000000001,
0.905000000000001,0.910000000000001,0.915000000000001,0.920000000000001,
0.925000000000001,0.930000000000001,0.935000000000001,0.940000000000001,
0.945000000000001,0.950000000000001,0.955000000000001,0.960000000000001,
0.965000000000001,0.970000000000001,0.975000000000001,0.980000000000001,
0.985000000000001,0.990000000000001,0.995000000000001,1.),.UNSPECIFIED.)
CURVE()
GEOMETRIC_REPRESENTATION_ITEM()
RATIONAL_B_SPLINE_CURVE((1.,1.,1.,1.,1.,1.,1.,1.,1.,1.,1.,1.,1.,1.,1.,1.,
1.,1.,1.,1.,1.,1.,1.,1.,1.,1.,1.,1.,1.,1.,1.,1.,1.,1.,1.,1.,1.,1.,1.,1.,
1.,1.,1.,1.,1.,1.,1.,1.,1.,1.,1.,1.,1.,1.,1.,1.,1.,1.,1.,1.,1.,1.,1.,1.,
1.,1.,1.,1.,1.,1.,1.,1.,1.,1.,1.,1.,1.,1.,1.,1.,1.,1.,1.,1.,1.,1.,1.,1.,
1.,1.,1.,1.,1.,1.,1.,1.,1.,1.,1.,1.,1.,1.,1.,1.,1.,1.,1.,1.,1.,1.,1.,1.,
1.,1.,1.,1.,1.,1.,1.,1.,1.,1.,1.,1.,1.,1.,1.,1.,1.,1.,1.,1.,1.,1.,1.,1.,
1.,1.,1.,1.,1.,1.,1.,1.,1.,1.,1.,1.,1.,1.,1.,1.,1.,1.,1.,1.,1.,1.,1.,1.,
1.,1.,1.,1.,1.,1.,1.,1.,1.,1.,1.,1.,1.,1.,1.,1.,1.,1.,1.,1.,1.,1.,1.,1.,
1.,1.,1.,1.,1.,1.,1.,1.,1.,1.,1.,1.,1.,1.,1.,1.,1.,1.,1.,1.,1.))
REPRESENTATION_ITEM('')
);
#822=(
BOUNDED_CURVE()
B_SPLINE_CURVE(5,(#230664,#230665,#230666,#230667,#230668,#230669,#230670,
#230671,#230672,#230673,#230674,#230675,#230676,#230677,#230678,#230679,
#230680,#230681,#230682,#230683,#230684,#230685,#230686,#230687,#230688,
#230689,#230690,#230691,#230692,#230693,#230694,#230695,#230696,#230697,
#230698,#230699,#230700,#230701,#230702,#230703,#230704,#230705,#230706,
#230707,#230708,#230709,#230710,#230711,#230712,#230713,#230714,#230715,
#230716,#230717,#230718,#230719,#230720,#230721,#230722,#230723,#230724,
#230725,#230726,#230727,#230728,#230729,#230730,#230731,#230732,#230733,
#230734,#230735,#230736,#230737,#230738,#230739,#230740,#230741,#230742,
#230743,#230744,#230745,#230746,#230747,#230748,#230749,#230750,#230751,
#230752,#230753,#230754,#230755,#230756,#230757,#230758,#230759,#230760,
#230761,#230762,#230763,#230764,#230765,#230766,#230767,#230768,#230769,
#230770,#230771,#230772,#230773,#230774,#230775,#230776,#230777,#230778,
#230779,#230780,#230781,#230782,#230783,#230784,#230785,#230786,#230787,
#230788,#230789,#230790,#230791,#230792,#230793,#230794,#230795,#230796,
#230797,#230798,#230799,#230800,#230801,#230802,#230803,#230804,#230805,
#230806,#230807,#230808,#230809,#230810,#230811,#230812,#230813,#230814,
#230815,#230816,#230817,#230818,#230819,#230820,#230821,#230822,#230823,
#230824,#230825,#230826,#230827,#230828,#230829,#230830,#230831,#230832,
#230833,#230834,#230835,#230836,#230837,#230838,#230839,#230840,#230841,
#230842,#230843,#230844,#230845,#230846,#230847,#230848,#230849,#230850,
#230851,#230852,#230853,#230854,#230855,#230856,#230857,#230858,#230859,
#230860,#230861,#230862,#230863,#230864,#230865,#230866,#230867,#230868),
 .UNSPECIFIED.,.F.,.F.)
B_SPLINE_CURVE_WITH_KNOTS((6,1,1,1,1,1,1,1,1,1,1,1,1,1,1,1,1,1,1,1,1,1,
1,1,1,1,1,1,1,1,1,1,1,1,1,1,1,1,1,1,1,1,1,1,1,1,1,1,1,1,1,1,1,1,1,1,1,1,
1,1,1,1,1,1,1,1,1,1,1,1,1,1,1,1,1,1,1,1,1,1,1,1,1,1,1,1,1,1,1,1,1,1,1,1,
1,1,1,1,1,1,1,1,1,1,1,1,1,1,1,1,1,1,1,1,1,1,1,1,1,1,1,1,1,1,1,1,1,1,1,1,
1,1,1,1,1,1,1,1,1,1,1,1,1,1,1,1,1,1,1,1,1,1,1,1,1,1,1,1,1,1,1,1,1,1,1,1,
1,1,1,1,1,1,1,1,1,1,1,1,1,1,1,1,1,1,1,1,1,1,1,1,1,1,1,1,1,1,1,1,1,1,6),
(-1.,-0.995000000000001,-0.990000000000001,-0.985000000000001,-0.980000000000001,
-0.975000000000001,-0.970000000000001,-0.965000000000001,-0.960000000000001,
-0.955000000000001,-0.950000000000001,-0.945000000000001,-0.940000000000001,
-0.935000000000001,-0.930000000000001,-0.925000000000001,-0.920000000000001,
-0.915000000000001,-0.910000000000001,-0.905000000000001,-0.900000000000001,
-0.895000000000001,-0.890000000000001,-0.885000000000001,-0.880000000000001,
-0.875000000000001,-0.870000000000001,-0.865000000000001,-0.860000000000001,
-0.855000000000001,-0.850000000000001,-0.845000000000001,-0.840000000000001,
-0.835000000000001,-0.830000000000001,-0.825000000000001,-0.820000000000001,
-0.815000000000001,-0.810000000000001,-0.805000000000001,-0.800000000000001,
-0.795000000000001,-0.790000000000001,-0.785000000000001,-0.780000000000001,
-0.775000000000001,-0.770000000000001,-0.765000000000001,-0.760000000000001,
-0.755000000000001,-0.750000000000001,-0.745000000000001,-0.740000000000001,
-0.735000000000001,-0.730000000000001,-0.725000000000001,-0.720000000000001,
-0.715000000000001,-0.710000000000001,-0.705000000000001,-0.700000000000001,
-0.695000000000001,-0.690000000000001,-0.685,-0.68,-0.675,-0.67,-0.665,
-0.66,-0.655,-0.65,-0.645,-0.64,-0.635,-0.63,-0.625,-0.62,-0.615,-0.61,
-0.605,-0.6,-0.595,-0.59,-0.585,-0.58,-0.575,-0.57,-0.565,-0.56,-0.555,
-0.55,-0.545,-0.54,-0.535,-0.53,-0.525,-0.52,-0.515,-0.51,-0.505,-0.5,-0.495,
-0.49,-0.485,-0.48,-0.475,-0.47,-0.465,-0.46,-0.455,-0.45,-0.445,-0.44,
-0.435,-0.43,-0.425,-0.42,-0.415,-0.41,-0.405,-0.4,-0.395,-0.39,-0.385,
-0.38,-0.375,-0.37,-0.365,-0.36,-0.355,-0.35,-0.345,-0.34,-0.335,-0.33,
-0.325,-0.32,-0.315,-0.31,-0.305,-0.3,-0.295,-0.29,-0.285,-0.28,-0.275,
-0.27,-0.265,-0.26,-0.255,-0.25,-0.245,-0.24,-0.235,-0.23,-0.225,-0.22,
-0.215,-0.21,-0.205,-0.2,-0.195,-0.19,-0.185,-0.18,-0.175,-0.17,-0.165,
-0.16,-0.155,-0.15,-0.145,-0.14,-0.135,-0.13,-0.125,-0.12,-0.115,-0.11,
-0.105,-0.1,-0.095,-0.09,-0.085,-0.08,-0.075,-0.07,-0.065,-0.06,-0.055,
-0.05,-0.045,-0.04,-0.035,-0.03,-0.025,-0.02,-0.015,-0.01,-0.005,0.),
 .UNSPECIFIED.)
CURVE()
GEOMETRIC_REPRESENTATION_ITEM()
RATIONAL_B_SPLINE_CURVE((1.,1.,1.,1.,1.,1.,1.,1.,1.,1.,1.,1.,1.,1.,1.,1.,
1.,1.,1.,1.,1.,1.,1.,1.,1.,1.,1.,1.,1.,1.,1.,1.,1.,1.,1.,1.,1.,1.,1.,1.,
1.,1.,1.,1.,1.,1.,1.,1.,1.,1.,1.,1.,1.,1.,1.,1.,1.,1.,1.,1.,1.,1.,1.,1.,
1.,1.,1.,1.,1.,1.,1.,1.,1.,1.,1.,1.,1.,1.,1.,1.,1.,1.,1.,1.,1.,1.,1.,1.,
1.,1.,1.,1.,1.,1.,1.,1.,1.,1.,1.,1.,1.,1.,1.,1.,1.,1.,1.,1.,1.,1.,1.,1.,
1.,1.,1.,1.,1.,1.,1.,1.,1.,1.,1.,1.,1.,1.,1.,1.,1.,1.,1.,1.,1.,1.,1.,1.,
1.,1.,1.,1.,1.,1.,1.,1.,1.,1.,1.,1.,1.,1.,1.,1.,1.,1.,1.,1.,1.,1.,1.,1.,
1.,1.,1.,1.,1.,1.,1.,1.,1.,1.,1.,1.,1.,1.,1.,1.,1.,1.,1.,1.,1.,1.,1.,1.,
1.,1.,1.,1.,1.,1.,1.,1.,1.,1.,1.,1.,1.,1.,1.,1.,1.,1.,1.,1.,1.))
REPRESENTATION_ITEM('')
);
#823=(
BOUNDED_CURVE()
B_SPLINE_CURVE(5,(#231287,#231288,#231289,#231290,#231291,#231292,#231293,
#231294,#231295,#231296,#231297,#231298,#231299,#231300,#231301,#231302,
#231303,#231304,#231305,#231306,#231307,#231308,#231309,#231310,#231311,
#231312,#231313,#231314,#231315,#231316,#231317,#231318,#231319,#231320,
#231321,#231322,#231323,#231324,#231325,#231326,#231327,#231328,#231329,
#231330,#231331,#231332,#231333,#231334,#231335,#231336,#231337,#231338,
#231339,#231340,#231341,#231342,#231343,#231344,#231345,#231346,#231347,
#231348,#231349,#231350,#231351,#231352,#231353,#231354,#231355,#231356,
#231357,#231358,#231359,#231360,#231361,#231362,#231363,#231364,#231365,
#231366,#231367,#231368,#231369,#231370,#231371,#231372,#231373,#231374,
#231375,#231376,#231377,#231378,#231379,#231380,#231381,#231382,#231383,
#231384,#231385,#231386,#231387,#231388,#231389,#231390,#231391,#231392,
#231393,#231394,#231395,#231396,#231397,#231398,#231399,#231400,#231401,
#231402,#231403,#231404,#231405,#231406,#231407,#231408,#231409,#231410,
#231411,#231412,#231413,#231414,#231415,#231416,#231417,#231418,#231419,
#231420,#231421,#231422,#231423,#231424,#231425,#231426,#231427,#231428,
#231429,#231430,#231431,#231432,#231433,#231434,#231435,#231436,#231437,
#231438,#231439,#231440,#231441,#231442,#231443,#231444,#231445,#231446,
#231447,#231448,#231449,#231450,#231451,#231452,#231453,#231454,#231455,
#231456,#231457,#231458,#231459,#231460,#231461,#231462,#231463,#231464,
#231465,#231466,#231467,#231468,#231469,#231470,#231471,#231472,#231473,
#231474,#231475,#231476,#231477,#231478,#231479,#231480,#231481,#231482,
#231483,#231484,#231485,#231486,#231487,#231488,#231489,#231490,#231491),
 .UNSPECIFIED.,.F.,.F.)
B_SPLINE_CURVE_WITH_KNOTS((6,1,1,1,1,1,1,1,1,1,1,1,1,1,1,1,1,1,1,1,1,1,
1,1,1,1,1,1,1,1,1,1,1,1,1,1,1,1,1,1,1,1,1,1,1,1,1,1,1,1,1,1,1,1,1,1,1,1,
1,1,1,1,1,1,1,1,1,1,1,1,1,1,1,1,1,1,1,1,1,1,1,1,1,1,1,1,1,1,1,1,1,1,1,1,
1,1,1,1,1,1,1,1,1,1,1,1,1,1,1,1,1,1,1,1,1,1,1,1,1,1,1,1,1,1,1,1,1,1,1,1,
1,1,1,1,1,1,1,1,1,1,1,1,1,1,1,1,1,1,1,1,1,1,1,1,1,1,1,1,1,1,1,1,1,1,1,1,
1,1,1,1,1,1,1,1,1,1,1,1,1,1,1,1,1,1,1,1,1,1,1,1,1,1,1,1,1,1,1,1,1,1,6),
(-1.,-0.995000000000001,-0.990000000000001,-0.985000000000001,-0.980000000000001,
-0.975000000000001,-0.970000000000001,-0.965000000000001,-0.960000000000001,
-0.955000000000001,-0.950000000000001,-0.945000000000001,-0.940000000000001,
-0.935000000000001,-0.930000000000001,-0.925000000000001,-0.920000000000001,
-0.915000000000001,-0.910000000000001,-0.905000000000001,-0.900000000000001,
-0.895000000000001,-0.890000000000001,-0.885000000000001,-0.880000000000001,
-0.875000000000001,-0.870000000000001,-0.865000000000001,-0.860000000000001,
-0.855000000000001,-0.850000000000001,-0.845000000000001,-0.840000000000001,
-0.835000000000001,-0.830000000000001,-0.825000000000001,-0.820000000000001,
-0.815000000000001,-0.810000000000001,-0.805000000000001,-0.800000000000001,
-0.795000000000001,-0.790000000000001,-0.785000000000001,-0.780000000000001,
-0.775000000000001,-0.770000000000001,-0.765000000000001,-0.760000000000001,
-0.755000000000001,-0.750000000000001,-0.745000000000001,-0.740000000000001,
-0.735000000000001,-0.730000000000001,-0.725000000000001,-0.720000000000001,
-0.715000000000001,-0.710000000000001,-0.705000000000001,-0.700000000000001,
-0.695000000000001,-0.690000000000001,-0.685,-0.68,-0.675,-0.67,-0.665,
-0.66,-0.655,-0.65,-0.645,-0.64,-0.635,-0.63,-0.625,-0.62,-0.615,-0.61,
-0.605,-0.6,-0.595,-0.59,-0.585,-0.58,-0.575,-0.57,-0.565,-0.56,-0.555,
-0.55,-0.545,-0.54,-0.535,-0.53,-0.525,-0.52,-0.515,-0.51,-0.505,-0.5,-0.495,
-0.49,-0.485,-0.48,-0.475,-0.47,-0.465,-0.46,-0.455,-0.45,-0.445,-0.44,
-0.435,-0.43,-0.425,-0.42,-0.415,-0.41,-0.405,-0.4,-0.395,-0.39,-0.385,
-0.38,-0.375,-0.37,-0.365,-0.36,-0.355,-0.35,-0.345,-0.34,-0.335,-0.33,
-0.325,-0.32,-0.315,-0.31,-0.305,-0.3,-0.295,-0.29,-0.285,-0.28,-0.275,
-0.27,-0.265,-0.26,-0.255,-0.25,-0.245,-0.24,-0.235,-0.23,-0.225,-0.22,
-0.215,-0.21,-0.205,-0.2,-0.195,-0.19,-0.185,-0.18,-0.175,-0.17,-0.165,
-0.16,-0.155,-0.15,-0.145,-0.14,-0.135,-0.13,-0.125,-0.12,-0.115,-0.11,
-0.105,-0.1,-0.095,-0.09,-0.085,-0.08,-0.075,-0.07,-0.065,-0.06,-0.055,
-0.05,-0.045,-0.04,-0.035,-0.03,-0.025,-0.02,-0.015,-0.01,-0.005,0.),
 .UNSPECIFIED.)
CURVE()
GEOMETRIC_REPRESENTATION_ITEM()
RATIONAL_B_SPLINE_CURVE((1.,1.,1.,1.,1.,1.,1.,1.,1.,1.,1.,1.,1.,1.,1.,1.,
1.,1.,1.,1.,1.,1.,1.,1.,1.,1.,1.,1.,1.,1.,1.,1.,1.,1.,1.,1.,1.,1.,1.,1.,
1.,1.,1.,1.,1.,1.,1.,1.,1.,1.,1.,1.,1.,1.,1.,1.,1.,1.,1.,1.,1.,1.,1.,1.,
1.,1.,1.,1.,1.,1.,1.,1.,1.,1.,1.,1.,1.,1.,1.,1.,1.,1.,1.,1.,1.,1.,1.,1.,
1.,1.,1.,1.,1.,1.,1.,1.,1.,1.,1.,1.,1.,1.,1.,1.,1.,1.,1.,1.,1.,1.,1.,1.,
1.,1.,1.,1.,1.,1.,1.,1.,1.,1.,1.,1.,1.,1.,1.,1.,1.,1.,1.,1.,1.,1.,1.,1.,
1.,1.,1.,1.,1.,1.,1.,1.,1.,1.,1.,1.,1.,1.,1.,1.,1.,1.,1.,1.,1.,1.,1.,1.,
1.,1.,1.,1.,1.,1.,1.,1.,1.,1.,1.,1.,1.,1.,1.,1.,1.,1.,1.,1.,1.,1.,1.,1.,
1.,1.,1.,1.,1.,1.,1.,1.,1.,1.,1.,1.,1.,1.,1.,1.,1.,1.,1.,1.,1.))
REPRESENTATION_ITEM('')
);
#824=(
BOUNDED_CURVE()
B_SPLINE_CURVE(5,(#231494,#231495,#231496,#231497,#231498,#231499,#231500,
#231501,#231502,#231503,#231504,#231505,#231506,#231507,#231508,#231509,
#231510,#231511,#231512,#231513,#231514,#231515,#231516,#231517,#231518,
#231519,#231520,#231521,#231522,#231523,#231524,#231525,#231526,#231527,
#231528,#231529,#231530,#231531,#231532,#231533,#231534,#231535,#231536,
#231537,#231538,#231539,#231540,#231541,#231542,#231543,#231544,#231545,
#231546,#231547,#231548,#231549,#231550,#231551,#231552,#231553,#231554,
#231555,#231556,#231557,#231558,#231559,#231560,#231561,#231562,#231563,
#231564,#231565,#231566,#231567,#231568,#231569,#231570,#231571,#231572,
#231573,#231574,#231575,#231576,#231577,#231578,#231579,#231580,#231581,
#231582,#231583,#231584,#231585,#231586,#231587,#231588,#231589,#231590,
#231591,#231592,#231593,#231594,#231595,#231596,#231597,#231598,#231599,
#231600,#231601,#231602,#231603,#231604,#231605,#231606,#231607,#231608,
#231609,#231610,#231611,#231612,#231613,#231614,#231615,#231616,#231617,
#231618,#231619,#231620,#231621,#231622,#231623,#231624,#231625,#231626,
#231627,#231628,#231629,#231630,#231631,#231632,#231633,#231634,#231635,
#231636,#231637,#231638,#231639,#231640,#231641,#231642,#231643,#231644,
#231645,#231646,#231647,#231648,#231649,#231650,#231651,#231652,#231653,
#231654,#231655,#231656,#231657,#231658,#231659,#231660,#231661,#231662,
#231663,#231664,#231665,#231666,#231667,#231668,#231669,#231670,#231671,
#231672,#231673,#231674,#231675,#231676,#231677,#231678,#231679,#231680,
#231681,#231682,#231683,#231684,#231685,#231686,#231687,#231688,#231689,
#231690,#231691,#231692,#231693,#231694,#231695,#231696,#231697,#231698),
 .UNSPECIFIED.,.F.,.F.)
B_SPLINE_CURVE_WITH_KNOTS((6,1,1,1,1,1,1,1,1,1,1,1,1,1,1,1,1,1,1,1,1,1,
1,1,1,1,1,1,1,1,1,1,1,1,1,1,1,1,1,1,1,1,1,1,1,1,1,1,1,1,1,1,1,1,1,1,1,1,
1,1,1,1,1,1,1,1,1,1,1,1,1,1,1,1,1,1,1,1,1,1,1,1,1,1,1,1,1,1,1,1,1,1,1,1,
1,1,1,1,1,1,1,1,1,1,1,1,1,1,1,1,1,1,1,1,1,1,1,1,1,1,1,1,1,1,1,1,1,1,1,1,
1,1,1,1,1,1,1,1,1,1,1,1,1,1,1,1,1,1,1,1,1,1,1,1,1,1,1,1,1,1,1,1,1,1,1,1,
1,1,1,1,1,1,1,1,1,1,1,1,1,1,1,1,1,1,1,1,1,1,1,1,1,1,1,1,1,1,1,1,1,1,6),
(0.,0.005,0.01,0.015,0.02,0.025,0.03,0.035,0.04,0.045,0.05,0.055,0.06,0.065,
0.07,0.075,0.08,0.085,0.09,0.095,0.1,0.105,0.11,0.115,0.12,0.125,0.13,0.135,
0.14,0.145,0.15,0.155,0.16,0.165,0.17,0.175,0.18,0.185,0.19,0.195,0.2,0.205,
0.21,0.215,0.22,0.225,0.23,0.235,0.24,0.245,0.25,0.255,0.26,0.265,0.27,
0.275,0.28,0.285,0.29,0.295,0.3,0.305,0.31,0.315,0.32,0.325,0.33,0.335,
0.34,0.345,0.35,0.355,0.36,0.365,0.37,0.375,0.38,0.385,0.39,0.395,0.4,0.405,
0.41,0.415,0.42,0.425,0.43,0.435,0.44,0.445,0.45,0.455,0.46,0.465,0.47,
0.475,0.48,0.485,0.49,0.495,0.5,0.505,0.51,0.515,0.52,0.525,0.53,0.535,
0.54,0.545,0.55,0.555,0.56,0.565,0.57,0.575,0.58,0.585,0.59,0.595,0.6,0.605,
0.61,0.615,0.62,0.625,0.63,0.635,0.64,0.645,0.65,0.655,0.66,0.665,0.67,
0.675,0.68,0.685,0.690000000000001,0.695000000000001,0.700000000000001,
0.705000000000001,0.710000000000001,0.715000000000001,0.720000000000001,
0.725000000000001,0.730000000000001,0.735000000000001,0.740000000000001,
0.745000000000001,0.750000000000001,0.755000000000001,0.760000000000001,
0.765000000000001,0.770000000000001,0.775000000000001,0.780000000000001,
0.785000000000001,0.790000000000001,0.795000000000001,0.800000000000001,
0.805000000000001,0.810000000000001,0.815000000000001,0.820000000000001,
0.825000000000001,0.830000000000001,0.835000000000001,0.840000000000001,
0.845000000000001,0.850000000000001,0.855000000000001,0.860000000000001,
0.865000000000001,0.870000000000001,0.875000000000001,0.880000000000001,
0.885000000000001,0.890000000000001,0.895000000000001,0.900000000000001,
0.905000000000001,0.910000000000001,0.915000000000001,0.920000000000001,
0.925000000000001,0.930000000000001,0.935000000000001,0.940000000000001,
0.945000000000001,0.950000000000001,0.955000000000001,0.960000000000001,
0.965000000000001,0.970000000000001,0.975000000000001,0.980000000000001,
0.985000000000001,0.990000000000001,0.995000000000001,1.),.UNSPECIFIED.)
CURVE()
GEOMETRIC_REPRESENTATION_ITEM()
RATIONAL_B_SPLINE_CURVE((1.,1.,1.,1.,1.,1.,1.,1.,1.,1.,1.,1.,1.,1.,1.,1.,
1.,1.,1.,1.,1.,1.,1.,1.,1.,1.,1.,1.,1.,1.,1.,1.,1.,1.,1.,1.,1.,1.,1.,1.,
1.,1.,1.,1.,1.,1.,1.,1.,1.,1.,1.,1.,1.,1.,1.,1.,1.,1.,1.,1.,1.,1.,1.,1.,
1.,1.,1.,1.,1.,1.,1.,1.,1.,1.,1.,1.,1.,1.,1.,1.,1.,1.,1.,1.,1.,1.,1.,1.,
1.,1.,1.,1.,1.,1.,1.,1.,1.,1.,1.,1.,1.,1.,1.,1.,1.,1.,1.,1.,1.,1.,1.,1.,
1.,1.,1.,1.,1.,1.,1.,1.,1.,1.,1.,1.,1.,1.,1.,1.,1.,1.,1.,1.,1.,1.,1.,1.,
1.,1.,1.,1.,1.,1.,1.,1.,1.,1.,1.,1.,1.,1.,1.,1.,1.,1.,1.,1.,1.,1.,1.,1.,
1.,1.,1.,1.,1.,1.,1.,1.,1.,1.,1.,1.,1.,1.,1.,1.,1.,1.,1.,1.,1.,1.,1.,1.,
1.,1.,1.,1.,1.,1.,1.,1.,1.,1.,1.,1.,1.,1.,1.,1.,1.,1.,1.,1.,1.))
REPRESENTATION_ITEM('')
);
#825=(
BOUNDED_CURVE()
B_SPLINE_CURVE(5,(#232110,#232111,#232112,#232113,#232114,#232115,#232116,
#232117,#232118,#232119,#232120,#232121,#232122,#232123,#232124,#232125,
#232126,#232127,#232128,#232129,#232130,#232131,#232132,#232133,#232134,
#232135,#232136,#232137,#232138,#232139,#232140,#232141,#232142,#232143,
#232144,#232145,#232146,#232147,#232148,#232149,#232150,#232151,#232152,
#232153,#232154,#232155,#232156,#232157,#232158,#232159,#232160,#232161,
#232162,#232163,#232164,#232165,#232166,#232167,#232168,#232169,#232170,
#232171,#232172,#232173,#232174,#232175,#232176,#232177,#232178,#232179,
#232180,#232181,#232182,#232183,#232184,#232185,#232186,#232187,#232188,
#232189,#232190,#232191,#232192,#232193,#232194,#232195,#232196,#232197,
#232198,#232199,#232200,#232201,#232202,#232203,#232204,#232205,#232206,
#232207,#232208,#232209,#232210,#232211,#232212,#232213,#232214,#232215,
#232216,#232217,#232218,#232219,#232220,#232221,#232222,#232223,#232224,
#232225,#232226,#232227,#232228,#232229,#232230,#232231,#232232,#232233,
#232234,#232235,#232236,#232237,#232238,#232239,#232240,#232241,#232242,
#232243,#232244,#232245,#232246,#232247,#232248,#232249,#232250,#232251,
#232252,#232253,#232254,#232255,#232256,#232257,#232258,#232259,#232260,
#232261,#232262,#232263,#232264,#232265,#232266,#232267,#232268,#232269,
#232270,#232271,#232272,#232273,#232274,#232275,#232276,#232277,#232278,
#232279,#232280,#232281,#232282,#232283,#232284,#232285,#232286,#232287,
#232288,#232289,#232290,#232291,#232292,#232293,#232294,#232295,#232296,
#232297,#232298,#232299,#232300,#232301,#232302,#232303,#232304,#232305,
#232306,#232307,#232308,#232309,#232310,#232311,#232312,#232313,#232314),
 .UNSPECIFIED.,.F.,.F.)
B_SPLINE_CURVE_WITH_KNOTS((6,1,1,1,1,1,1,1,1,1,1,1,1,1,1,1,1,1,1,1,1,1,
1,1,1,1,1,1,1,1,1,1,1,1,1,1,1,1,1,1,1,1,1,1,1,1,1,1,1,1,1,1,1,1,1,1,1,1,
1,1,1,1,1,1,1,1,1,1,1,1,1,1,1,1,1,1,1,1,1,1,1,1,1,1,1,1,1,1,1,1,1,1,1,1,
1,1,1,1,1,1,1,1,1,1,1,1,1,1,1,1,1,1,1,1,1,1,1,1,1,1,1,1,1,1,1,1,1,1,1,1,
1,1,1,1,1,1,1,1,1,1,1,1,1,1,1,1,1,1,1,1,1,1,1,1,1,1,1,1,1,1,1,1,1,1,1,1,
1,1,1,1,1,1,1,1,1,1,1,1,1,1,1,1,1,1,1,1,1,1,1,1,1,1,1,1,1,1,1,1,1,1,6),
(0.,0.005,0.01,0.015,0.02,0.025,0.03,0.035,0.04,0.045,0.05,0.055,0.06,0.065,
0.07,0.075,0.08,0.085,0.09,0.095,0.1,0.105,0.11,0.115,0.12,0.125,0.13,0.135,
0.14,0.145,0.15,0.155,0.16,0.165,0.17,0.175,0.18,0.185,0.19,0.195,0.2,0.205,
0.21,0.215,0.22,0.225,0.23,0.235,0.24,0.245,0.25,0.255,0.26,0.265,0.27,
0.275,0.28,0.285,0.29,0.295,0.3,0.305,0.31,0.315,0.32,0.325,0.33,0.335,
0.34,0.345,0.35,0.355,0.36,0.365,0.37,0.375,0.38,0.385,0.39,0.395,0.4,0.405,
0.41,0.415,0.42,0.425,0.43,0.435,0.44,0.445,0.45,0.455,0.46,0.465,0.47,
0.475,0.48,0.485,0.49,0.495,0.5,0.505,0.51,0.515,0.52,0.525,0.53,0.535,
0.54,0.545,0.55,0.555,0.56,0.565,0.57,0.575,0.58,0.585,0.59,0.595,0.6,0.605,
0.61,0.615,0.62,0.625,0.63,0.635,0.64,0.645,0.65,0.655,0.66,0.665,0.67,
0.675,0.68,0.685,0.690000000000001,0.695000000000001,0.700000000000001,
0.705000000000001,0.710000000000001,0.715000000000001,0.720000000000001,
0.725000000000001,0.730000000000001,0.735000000000001,0.740000000000001,
0.745000000000001,0.750000000000001,0.755000000000001,0.760000000000001,
0.765000000000001,0.770000000000001,0.775000000000001,0.780000000000001,
0.785000000000001,0.790000000000001,0.795000000000001,0.800000000000001,
0.805000000000001,0.810000000000001,0.815000000000001,0.820000000000001,
0.825000000000001,0.830000000000001,0.835000000000001,0.840000000000001,
0.845000000000001,0.850000000000001,0.855000000000001,0.860000000000001,
0.865000000000001,0.870000000000001,0.875000000000001,0.880000000000001,
0.885000000000001,0.890000000000001,0.895000000000001,0.900000000000001,
0.905000000000001,0.910000000000001,0.915000000000001,0.920000000000001,
0.925000000000001,0.930000000000001,0.935000000000001,0.940000000000001,
0.945000000000001,0.950000000000001,0.955000000000001,0.960000000000001,
0.965000000000001,0.970000000000001,0.975000000000001,0.980000000000001,
0.985000000000001,0.990000000000001,0.995000000000001,1.),.UNSPECIFIED.)
CURVE()
GEOMETRIC_REPRESENTATION_ITEM()
RATIONAL_B_SPLINE_CURVE((1.,1.,1.,1.,1.,1.,1.,1.,1.,1.,1.,1.,1.,1.,1.,1.,
1.,1.,1.,1.,1.,1.,1.,1.,1.,1.,1.,1.,1.,1.,1.,1.,1.,1.,1.,1.,1.,1.,1.,1.,
1.,1.,1.,1.,1.,1.,1.,1.,1.,1.,1.,1.,1.,1.,1.,1.,1.,1.,1.,1.,1.,1.,1.,1.,
1.,1.,1.,1.,1.,1.,1.,1.,1.,1.,1.,1.,1.,1.,1.,1.,1.,1.,1.,1.,1.,1.,1.,1.,
1.,1.,1.,1.,1.,1.,1.,1.,1.,1.,1.,1.,1.,1.,1.,1.,1.,1.,1.,1.,1.,1.,1.,1.,
1.,1.,1.,1.,1.,1.,1.,1.,1.,1.,1.,1.,1.,1.,1.,1.,1.,1.,1.,1.,1.,1.,1.,1.,
1.,1.,1.,1.,1.,1.,1.,1.,1.,1.,1.,1.,1.,1.,1.,1.,1.,1.,1.,1.,1.,1.,1.,1.,
1.,1.,1.,1.,1.,1.,1.,1.,1.,1.,1.,1.,1.,1.,1.,1.,1.,1.,1.,1.,1.,1.,1.,1.,
1.,1.,1.,1.,1.,1.,1.,1.,1.,1.,1.,1.,1.,1.,1.,1.,1.,1.,1.,1.,1.))
REPRESENTATION_ITEM('')
);
#826=(
BOUNDED_CURVE()
B_SPLINE_CURVE(5,(#232316,#232317,#232318,#232319,#232320,#232321,#232322,
#232323,#232324,#232325,#232326,#232327,#232328,#232329,#232330,#232331,
#232332,#232333,#232334,#232335,#232336,#232337,#232338,#232339,#232340,
#232341,#232342,#232343,#232344,#232345,#232346,#232347,#232348,#232349,
#232350,#232351,#232352,#232353,#232354,#232355,#232356,#232357,#232358,
#232359,#232360,#232361,#232362,#232363,#232364,#232365,#232366,#232367,
#232368,#232369,#232370,#232371,#232372,#232373,#232374,#232375,#232376,
#232377,#232378,#232379,#232380,#232381,#232382,#232383,#232384,#232385,
#232386,#232387,#232388,#232389,#232390,#232391,#232392,#232393,#232394,
#232395,#232396,#232397,#232398,#232399,#232400,#232401,#232402,#232403,
#232404,#232405,#232406,#232407,#232408,#232409,#232410,#232411,#232412,
#232413,#232414,#232415,#232416,#232417,#232418,#232419,#232420,#232421,
#232422,#232423,#232424,#232425,#232426,#232427,#232428,#232429,#232430,
#232431,#232432,#232433,#232434,#232435,#232436,#232437,#232438,#232439,
#232440,#232441,#232442,#232443,#232444,#232445,#232446,#232447,#232448,
#232449,#232450,#232451,#232452,#232453,#232454,#232455,#232456,#232457,
#232458,#232459,#232460,#232461,#232462,#232463,#232464,#232465,#232466,
#232467,#232468,#232469,#232470,#232471,#232472,#232473,#232474,#232475,
#232476,#232477,#232478,#232479,#232480,#232481,#232482,#232483,#232484,
#232485,#232486,#232487,#232488,#232489,#232490,#232491,#232492,#232493,
#232494,#232495,#232496,#232497,#232498,#232499,#232500,#232501,#232502,
#232503,#232504,#232505,#232506,#232507,#232508,#232509,#232510,#232511,
#232512,#232513,#232514,#232515,#232516,#232517,#232518,#232519,#232520),
 .UNSPECIFIED.,.F.,.F.)
B_SPLINE_CURVE_WITH_KNOTS((6,1,1,1,1,1,1,1,1,1,1,1,1,1,1,1,1,1,1,1,1,1,
1,1,1,1,1,1,1,1,1,1,1,1,1,1,1,1,1,1,1,1,1,1,1,1,1,1,1,1,1,1,1,1,1,1,1,1,
1,1,1,1,1,1,1,1,1,1,1,1,1,1,1,1,1,1,1,1,1,1,1,1,1,1,1,1,1,1,1,1,1,1,1,1,
1,1,1,1,1,1,1,1,1,1,1,1,1,1,1,1,1,1,1,1,1,1,1,1,1,1,1,1,1,1,1,1,1,1,1,1,
1,1,1,1,1,1,1,1,1,1,1,1,1,1,1,1,1,1,1,1,1,1,1,1,1,1,1,1,1,1,1,1,1,1,1,1,
1,1,1,1,1,1,1,1,1,1,1,1,1,1,1,1,1,1,1,1,1,1,1,1,1,1,1,1,1,1,1,1,1,1,6),
(-1.,-0.995000000000001,-0.990000000000001,-0.985000000000001,-0.980000000000001,
-0.975000000000001,-0.970000000000001,-0.965000000000001,-0.960000000000001,
-0.955000000000001,-0.950000000000001,-0.945000000000001,-0.940000000000001,
-0.935000000000001,-0.930000000000001,-0.925000000000001,-0.920000000000001,
-0.915000000000001,-0.910000000000001,-0.905000000000001,-0.900000000000001,
-0.895000000000001,-0.890000000000001,-0.885000000000001,-0.880000000000001,
-0.875000000000001,-0.870000000000001,-0.865000000000001,-0.860000000000001,
-0.855000000000001,-0.850000000000001,-0.845000000000001,-0.840000000000001,
-0.835000000000001,-0.830000000000001,-0.825000000000001,-0.820000000000001,
-0.815000000000001,-0.810000000000001,-0.805000000000001,-0.800000000000001,
-0.795000000000001,-0.790000000000001,-0.785000000000001,-0.780000000000001,
-0.775000000000001,-0.770000000000001,-0.765000000000001,-0.760000000000001,
-0.755000000000001,-0.750000000000001,-0.745000000000001,-0.740000000000001,
-0.735000000000001,-0.730000000000001,-0.725000000000001,-0.720000000000001,
-0.715000000000001,-0.710000000000001,-0.705000000000001,-0.700000000000001,
-0.695000000000001,-0.690000000000001,-0.685,-0.68,-0.675,-0.67,-0.665,
-0.66,-0.655,-0.65,-0.645,-0.64,-0.635,-0.63,-0.625,-0.62,-0.615,-0.61,
-0.605,-0.6,-0.595,-0.59,-0.585,-0.58,-0.575,-0.57,-0.565,-0.56,-0.555,
-0.55,-0.545,-0.54,-0.535,-0.53,-0.525,-0.52,-0.515,-0.51,-0.505,-0.5,-0.495,
-0.49,-0.485,-0.48,-0.475,-0.47,-0.465,-0.46,-0.455,-0.45,-0.445,-0.44,
-0.435,-0.43,-0.425,-0.42,-0.415,-0.41,-0.405,-0.4,-0.395,-0.39,-0.385,
-0.38,-0.375,-0.37,-0.365,-0.36,-0.355,-0.35,-0.345,-0.34,-0.335,-0.33,
-0.325,-0.32,-0.315,-0.31,-0.305,-0.3,-0.295,-0.29,-0.285,-0.28,-0.275,
-0.27,-0.265,-0.26,-0.255,-0.25,-0.245,-0.24,-0.235,-0.23,-0.225,-0.22,
-0.215,-0.21,-0.205,-0.2,-0.195,-0.19,-0.185,-0.18,-0.175,-0.17,-0.165,
-0.16,-0.155,-0.15,-0.145,-0.14,-0.135,-0.13,-0.125,-0.12,-0.115,-0.11,
-0.105,-0.1,-0.095,-0.09,-0.085,-0.08,-0.075,-0.07,-0.065,-0.06,-0.055,
-0.05,-0.045,-0.04,-0.035,-0.03,-0.025,-0.02,-0.015,-0.01,-0.005,0.),
 .UNSPECIFIED.)
CURVE()
GEOMETRIC_REPRESENTATION_ITEM()
RATIONAL_B_SPLINE_CURVE((1.,1.,1.,1.,1.,1.,1.,1.,1.,1.,1.,1.,1.,1.,1.,1.,
1.,1.,1.,1.,1.,1.,1.,1.,1.,1.,1.,1.,1.,1.,1.,1.,1.,1.,1.,1.,1.,1.,1.,1.,
1.,1.,1.,1.,1.,1.,1.,1.,1.,1.,1.,1.,1.,1.,1.,1.,1.,1.,1.,1.,1.,1.,1.,1.,
1.,1.,1.,1.,1.,1.,1.,1.,1.,1.,1.,1.,1.,1.,1.,1.,1.,1.,1.,1.,1.,1.,1.,1.,
1.,1.,1.,1.,1.,1.,1.,1.,1.,1.,1.,1.,1.,1.,1.,1.,1.,1.,1.,1.,1.,1.,1.,1.,
1.,1.,1.,1.,1.,1.,1.,1.,1.,1.,1.,1.,1.,1.,1.,1.,1.,1.,1.,1.,1.,1.,1.,1.,
1.,1.,1.,1.,1.,1.,1.,1.,1.,1.,1.,1.,1.,1.,1.,1.,1.,1.,1.,1.,1.,1.,1.,1.,
1.,1.,1.,1.,1.,1.,1.,1.,1.,1.,1.,1.,1.,1.,1.,1.,1.,1.,1.,1.,1.,1.,1.,1.,
1.,1.,1.,1.,1.,1.,1.,1.,1.,1.,1.,1.,1.,1.,1.,1.,1.,1.,1.,1.,1.))
REPRESENTATION_ITEM('')
);
#827=(
BOUNDED_CURVE()
B_SPLINE_CURVE(5,(#232939,#232940,#232941,#232942,#232943,#232944,#232945,
#232946,#232947,#232948,#232949,#232950,#232951,#232952,#232953,#232954,
#232955,#232956,#232957,#232958,#232959,#232960,#232961,#232962,#232963,
#232964,#232965,#232966,#232967,#232968,#232969,#232970,#232971,#232972,
#232973,#232974,#232975,#232976,#232977,#232978,#232979,#232980,#232981,
#232982,#232983,#232984,#232985,#232986,#232987,#232988,#232989,#232990,
#232991,#232992,#232993,#232994,#232995,#232996,#232997,#232998,#232999,
#233000,#233001,#233002,#233003,#233004,#233005,#233006,#233007,#233008,
#233009,#233010,#233011,#233012,#233013,#233014,#233015,#233016,#233017,
#233018,#233019,#233020,#233021,#233022,#233023,#233024,#233025,#233026,
#233027,#233028,#233029,#233030,#233031,#233032,#233033,#233034,#233035,
#233036,#233037,#233038,#233039,#233040,#233041,#233042,#233043,#233044,
#233045,#233046,#233047,#233048,#233049,#233050,#233051,#233052,#233053,
#233054,#233055,#233056,#233057,#233058,#233059,#233060,#233061,#233062,
#233063,#233064,#233065,#233066,#233067,#233068,#233069,#233070,#233071,
#233072,#233073,#233074,#233075,#233076,#233077,#233078,#233079,#233080,
#233081,#233082,#233083,#233084,#233085,#233086,#233087,#233088,#233089,
#233090,#233091,#233092,#233093,#233094,#233095,#233096,#233097,#233098,
#233099,#233100,#233101,#233102,#233103,#233104,#233105,#233106,#233107,
#233108,#233109,#233110,#233111,#233112,#233113,#233114,#233115,#233116,
#233117,#233118,#233119,#233120,#233121,#233122,#233123,#233124,#233125,
#233126,#233127,#233128,#233129,#233130,#233131,#233132,#233133,#233134,
#233135,#233136,#233137,#233138,#233139,#233140,#233141,#233142,#233143),
 .UNSPECIFIED.,.F.,.F.)
B_SPLINE_CURVE_WITH_KNOTS((6,1,1,1,1,1,1,1,1,1,1,1,1,1,1,1,1,1,1,1,1,1,
1,1,1,1,1,1,1,1,1,1,1,1,1,1,1,1,1,1,1,1,1,1,1,1,1,1,1,1,1,1,1,1,1,1,1,1,
1,1,1,1,1,1,1,1,1,1,1,1,1,1,1,1,1,1,1,1,1,1,1,1,1,1,1,1,1,1,1,1,1,1,1,1,
1,1,1,1,1,1,1,1,1,1,1,1,1,1,1,1,1,1,1,1,1,1,1,1,1,1,1,1,1,1,1,1,1,1,1,1,
1,1,1,1,1,1,1,1,1,1,1,1,1,1,1,1,1,1,1,1,1,1,1,1,1,1,1,1,1,1,1,1,1,1,1,1,
1,1,1,1,1,1,1,1,1,1,1,1,1,1,1,1,1,1,1,1,1,1,1,1,1,1,1,1,1,1,1,1,1,1,6),
(-1.,-0.995000000000001,-0.990000000000001,-0.985000000000001,-0.980000000000001,
-0.975000000000001,-0.970000000000001,-0.965000000000001,-0.960000000000001,
-0.955000000000001,-0.950000000000001,-0.945000000000001,-0.940000000000001,
-0.935000000000001,-0.930000000000001,-0.925000000000001,-0.920000000000001,
-0.915000000000001,-0.910000000000001,-0.905000000000001,-0.900000000000001,
-0.895000000000001,-0.890000000000001,-0.885000000000001,-0.880000000000001,
-0.875000000000001,-0.870000000000001,-0.865000000000001,-0.860000000000001,
-0.855000000000001,-0.850000000000001,-0.845000000000001,-0.840000000000001,
-0.835000000000001,-0.830000000000001,-0.825000000000001,-0.820000000000001,
-0.815000000000001,-0.810000000000001,-0.805000000000001,-0.800000000000001,
-0.795000000000001,-0.790000000000001,-0.785000000000001,-0.780000000000001,
-0.775000000000001,-0.770000000000001,-0.765000000000001,-0.760000000000001,
-0.755000000000001,-0.750000000000001,-0.745000000000001,-0.740000000000001,
-0.735000000000001,-0.730000000000001,-0.725000000000001,-0.720000000000001,
-0.715000000000001,-0.710000000000001,-0.705000000000001,-0.700000000000001,
-0.695000000000001,-0.690000000000001,-0.685,-0.68,-0.675,-0.67,-0.665,
-0.66,-0.655,-0.65,-0.645,-0.64,-0.635,-0.63,-0.625,-0.62,-0.615,-0.61,
-0.605,-0.6,-0.595,-0.59,-0.585,-0.58,-0.575,-0.57,-0.565,-0.56,-0.555,
-0.55,-0.545,-0.54,-0.535,-0.53,-0.525,-0.52,-0.515,-0.51,-0.505,-0.5,-0.495,
-0.49,-0.485,-0.48,-0.475,-0.47,-0.465,-0.46,-0.455,-0.45,-0.445,-0.44,
-0.435,-0.43,-0.425,-0.42,-0.415,-0.41,-0.405,-0.4,-0.395,-0.39,-0.385,
-0.38,-0.375,-0.37,-0.365,-0.36,-0.355,-0.35,-0.345,-0.34,-0.335,-0.33,
-0.325,-0.32,-0.315,-0.31,-0.305,-0.3,-0.295,-0.29,-0.285,-0.28,-0.275,
-0.27,-0.265,-0.26,-0.255,-0.25,-0.245,-0.24,-0.235,-0.23,-0.225,-0.22,
-0.215,-0.21,-0.205,-0.2,-0.195,-0.19,-0.185,-0.18,-0.175,-0.17,-0.165,
-0.16,-0.155,-0.15,-0.145,-0.14,-0.135,-0.13,-0.125,-0.12,-0.115,-0.11,
-0.105,-0.1,-0.095,-0.09,-0.085,-0.08,-0.075,-0.07,-0.065,-0.06,-0.055,
-0.05,-0.045,-0.04,-0.035,-0.03,-0.025,-0.02,-0.015,-0.01,-0.005,0.),
 .UNSPECIFIED.)
CURVE()
GEOMETRIC_REPRESENTATION_ITEM()
RATIONAL_B_SPLINE_CURVE((1.,1.,1.,1.,1.,1.,1.,1.,1.,1.,1.,1.,1.,1.,1.,1.,
1.,1.,1.,1.,1.,1.,1.,1.,1.,1.,1.,1.,1.,1.,1.,1.,1.,1.,1.,1.,1.,1.,1.,1.,
1.,1.,1.,1.,1.,1.,1.,1.,1.,1.,1.,1.,1.,1.,1.,1.,1.,1.,1.,1.,1.,1.,1.,1.,
1.,1.,1.,1.,1.,1.,1.,1.,1.,1.,1.,1.,1.,1.,1.,1.,1.,1.,1.,1.,1.,1.,1.,1.,
1.,1.,1.,1.,1.,1.,1.,1.,1.,1.,1.,1.,1.,1.,1.,1.,1.,1.,1.,1.,1.,1.,1.,1.,
1.,1.,1.,1.,1.,1.,1.,1.,1.,1.,1.,1.,1.,1.,1.,1.,1.,1.,1.,1.,1.,1.,1.,1.,
1.,1.,1.,1.,1.,1.,1.,1.,1.,1.,1.,1.,1.,1.,1.,1.,1.,1.,1.,1.,1.,1.,1.,1.,
1.,1.,1.,1.,1.,1.,1.,1.,1.,1.,1.,1.,1.,1.,1.,1.,1.,1.,1.,1.,1.,1.,1.,1.,
1.,1.,1.,1.,1.,1.,1.,1.,1.,1.,1.,1.,1.,1.,1.,1.,1.,1.,1.,1.,1.))
REPRESENTATION_ITEM('')
);
#828=(
BOUNDED_CURVE()
B_SPLINE_CURVE(5,(#233146,#233147,#233148,#233149,#233150,#233151,#233152,
#233153,#233154,#233155,#233156,#233157,#233158,#233159,#233160,#233161,
#233162,#233163,#233164,#233165,#233166,#233167,#233168,#233169,#233170,
#233171,#233172,#233173,#233174,#233175,#233176,#233177,#233178,#233179,
#233180,#233181,#233182,#233183,#233184,#233185,#233186,#233187,#233188,
#233189,#233190,#233191,#233192,#233193,#233194,#233195,#233196,#233197,
#233198,#233199,#233200,#233201,#233202,#233203,#233204,#233205,#233206,
#233207,#233208,#233209,#233210,#233211,#233212,#233213,#233214,#233215,
#233216,#233217,#233218,#233219,#233220,#233221,#233222,#233223,#233224,
#233225,#233226,#233227,#233228,#233229,#233230,#233231,#233232,#233233,
#233234,#233235,#233236,#233237,#233238,#233239,#233240,#233241,#233242,
#233243,#233244,#233245,#233246,#233247,#233248,#233249,#233250,#233251,
#233252,#233253,#233254,#233255,#233256,#233257,#233258,#233259,#233260,
#233261,#233262,#233263,#233264,#233265,#233266,#233267,#233268,#233269,
#233270,#233271,#233272,#233273,#233274,#233275,#233276,#233277,#233278,
#233279,#233280,#233281,#233282,#233283,#233284,#233285,#233286,#233287,
#233288,#233289,#233290,#233291,#233292,#233293,#233294,#233295,#233296,
#233297,#233298,#233299,#233300,#233301,#233302,#233303,#233304,#233305,
#233306,#233307,#233308,#233309,#233310,#233311,#233312,#233313,#233314,
#233315,#233316,#233317,#233318,#233319,#233320,#233321,#233322,#233323,
#233324,#233325,#233326,#233327,#233328,#233329,#233330,#233331,#233332,
#233333,#233334,#233335,#233336,#233337,#233338,#233339,#233340,#233341,
#233342,#233343,#233344,#233345,#233346,#233347,#233348,#233349,#233350),
 .UNSPECIFIED.,.F.,.F.)
B_SPLINE_CURVE_WITH_KNOTS((6,1,1,1,1,1,1,1,1,1,1,1,1,1,1,1,1,1,1,1,1,1,
1,1,1,1,1,1,1,1,1,1,1,1,1,1,1,1,1,1,1,1,1,1,1,1,1,1,1,1,1,1,1,1,1,1,1,1,
1,1,1,1,1,1,1,1,1,1,1,1,1,1,1,1,1,1,1,1,1,1,1,1,1,1,1,1,1,1,1,1,1,1,1,1,
1,1,1,1,1,1,1,1,1,1,1,1,1,1,1,1,1,1,1,1,1,1,1,1,1,1,1,1,1,1,1,1,1,1,1,1,
1,1,1,1,1,1,1,1,1,1,1,1,1,1,1,1,1,1,1,1,1,1,1,1,1,1,1,1,1,1,1,1,1,1,1,1,
1,1,1,1,1,1,1,1,1,1,1,1,1,1,1,1,1,1,1,1,1,1,1,1,1,1,1,1,1,1,1,1,1,1,6),
(0.,0.005,0.01,0.015,0.02,0.025,0.03,0.035,0.04,0.045,0.05,0.055,0.06,0.065,
0.07,0.075,0.08,0.085,0.09,0.095,0.1,0.105,0.11,0.115,0.12,0.125,0.13,0.135,
0.14,0.145,0.15,0.155,0.16,0.165,0.17,0.175,0.18,0.185,0.19,0.195,0.2,0.205,
0.21,0.215,0.22,0.225,0.23,0.235,0.24,0.245,0.25,0.255,0.26,0.265,0.27,
0.275,0.28,0.285,0.29,0.295,0.3,0.305,0.31,0.315,0.32,0.325,0.33,0.335,
0.34,0.345,0.35,0.355,0.36,0.365,0.37,0.375,0.38,0.385,0.39,0.395,0.4,0.405,
0.41,0.415,0.42,0.425,0.43,0.435,0.44,0.445,0.45,0.455,0.46,0.465,0.47,
0.475,0.48,0.485,0.49,0.495,0.5,0.505,0.51,0.515,0.52,0.525,0.53,0.535,
0.54,0.545,0.55,0.555,0.56,0.565,0.57,0.575,0.58,0.585,0.59,0.595,0.6,0.605,
0.61,0.615,0.62,0.625,0.63,0.635,0.64,0.645,0.65,0.655,0.66,0.665,0.67,
0.675,0.68,0.685,0.690000000000001,0.695000000000001,0.700000000000001,
0.705000000000001,0.710000000000001,0.715000000000001,0.720000000000001,
0.725000000000001,0.730000000000001,0.735000000000001,0.740000000000001,
0.745000000000001,0.750000000000001,0.755000000000001,0.760000000000001,
0.765000000000001,0.770000000000001,0.775000000000001,0.780000000000001,
0.785000000000001,0.790000000000001,0.795000000000001,0.800000000000001,
0.805000000000001,0.810000000000001,0.815000000000001,0.820000000000001,
0.825000000000001,0.830000000000001,0.835000000000001,0.840000000000001,
0.845000000000001,0.850000000000001,0.855000000000001,0.860000000000001,
0.865000000000001,0.870000000000001,0.875000000000001,0.880000000000001,
0.885000000000001,0.890000000000001,0.895000000000001,0.900000000000001,
0.905000000000001,0.910000000000001,0.915000000000001,0.920000000000001,
0.925000000000001,0.930000000000001,0.935000000000001,0.940000000000001,
0.945000000000001,0.950000000000001,0.955000000000001,0.960000000000001,
0.965000000000001,0.970000000000001,0.975000000000001,0.980000000000001,
0.985000000000001,0.990000000000001,0.995000000000001,1.),.UNSPECIFIED.)
CURVE()
GEOMETRIC_REPRESENTATION_ITEM()
RATIONAL_B_SPLINE_CURVE((1.,1.,1.,1.,1.,1.,1.,1.,1.,1.,1.,1.,1.,1.,1.,1.,
1.,1.,1.,1.,1.,1.,1.,1.,1.,1.,1.,1.,1.,1.,1.,1.,1.,1.,1.,1.,1.,1.,1.,1.,
1.,1.,1.,1.,1.,1.,1.,1.,1.,1.,1.,1.,1.,1.,1.,1.,1.,1.,1.,1.,1.,1.,1.,1.,
1.,1.,1.,1.,1.,1.,1.,1.,1.,1.,1.,1.,1.,1.,1.,1.,1.,1.,1.,1.,1.,1.,1.,1.,
1.,1.,1.,1.,1.,1.,1.,1.,1.,1.,1.,1.,1.,1.,1.,1.,1.,1.,1.,1.,1.,1.,1.,1.,
1.,1.,1.,1.,1.,1.,1.,1.,1.,1.,1.,1.,1.,1.,1.,1.,1.,1.,1.,1.,1.,1.,1.,1.,
1.,1.,1.,1.,1.,1.,1.,1.,1.,1.,1.,1.,1.,1.,1.,1.,1.,1.,1.,1.,1.,1.,1.,1.,
1.,1.,1.,1.,1.,1.,1.,1.,1.,1.,1.,1.,1.,1.,1.,1.,1.,1.,1.,1.,1.,1.,1.,1.,
1.,1.,1.,1.,1.,1.,1.,1.,1.,1.,1.,1.,1.,1.,1.,1.,1.,1.,1.,1.,1.))
REPRESENTATION_ITEM('')
);
#829=(
BOUNDED_CURVE()
B_SPLINE_CURVE(5,(#233762,#233763,#233764,#233765,#233766,#233767,#233768,
#233769,#233770,#233771,#233772,#233773,#233774,#233775,#233776,#233777,
#233778,#233779,#233780,#233781,#233782,#233783,#233784,#233785,#233786,
#233787,#233788,#233789,#233790,#233791,#233792,#233793,#233794,#233795,
#233796,#233797,#233798,#233799,#233800,#233801,#233802,#233803,#233804,
#233805,#233806,#233807,#233808,#233809,#233810,#233811,#233812,#233813,
#233814,#233815,#233816,#233817,#233818,#233819,#233820,#233821,#233822,
#233823,#233824,#233825,#233826,#233827,#233828,#233829,#233830,#233831,
#233832,#233833,#233834,#233835,#233836,#233837,#233838,#233839,#233840,
#233841,#233842,#233843,#233844,#233845,#233846,#233847,#233848,#233849,
#233850,#233851,#233852,#233853,#233854,#233855,#233856,#233857,#233858,
#233859,#233860,#233861,#233862,#233863,#233864,#233865,#233866,#233867,
#233868,#233869,#233870,#233871,#233872,#233873,#233874,#233875,#233876,
#233877,#233878,#233879,#233880,#233881,#233882,#233883,#233884,#233885,
#233886,#233887,#233888,#233889,#233890,#233891,#233892,#233893,#233894,
#233895,#233896,#233897,#233898,#233899,#233900,#233901,#233902,#233903,
#233904,#233905,#233906,#233907,#233908,#233909,#233910,#233911,#233912,
#233913,#233914,#233915,#233916,#233917,#233918,#233919,#233920,#233921,
#233922,#233923,#233924,#233925,#233926,#233927,#233928,#233929,#233930,
#233931,#233932,#233933,#233934,#233935,#233936,#233937,#233938,#233939,
#233940,#233941,#233942,#233943,#233944,#233945,#233946,#233947,#233948,
#233949,#233950,#233951,#233952,#233953,#233954,#233955,#233956,#233957,
#233958,#233959,#233960,#233961,#233962,#233963,#233964,#233965,#233966),
 .UNSPECIFIED.,.F.,.F.)
B_SPLINE_CURVE_WITH_KNOTS((6,1,1,1,1,1,1,1,1,1,1,1,1,1,1,1,1,1,1,1,1,1,
1,1,1,1,1,1,1,1,1,1,1,1,1,1,1,1,1,1,1,1,1,1,1,1,1,1,1,1,1,1,1,1,1,1,1,1,
1,1,1,1,1,1,1,1,1,1,1,1,1,1,1,1,1,1,1,1,1,1,1,1,1,1,1,1,1,1,1,1,1,1,1,1,
1,1,1,1,1,1,1,1,1,1,1,1,1,1,1,1,1,1,1,1,1,1,1,1,1,1,1,1,1,1,1,1,1,1,1,1,
1,1,1,1,1,1,1,1,1,1,1,1,1,1,1,1,1,1,1,1,1,1,1,1,1,1,1,1,1,1,1,1,1,1,1,1,
1,1,1,1,1,1,1,1,1,1,1,1,1,1,1,1,1,1,1,1,1,1,1,1,1,1,1,1,1,1,1,1,1,1,6),
(0.,0.005,0.01,0.015,0.02,0.025,0.03,0.035,0.04,0.045,0.05,0.055,0.06,0.065,
0.07,0.075,0.08,0.085,0.09,0.095,0.1,0.105,0.11,0.115,0.12,0.125,0.13,0.135,
0.14,0.145,0.15,0.155,0.16,0.165,0.17,0.175,0.18,0.185,0.19,0.195,0.2,0.205,
0.21,0.215,0.22,0.225,0.23,0.235,0.24,0.245,0.25,0.255,0.26,0.265,0.27,
0.275,0.28,0.285,0.29,0.295,0.3,0.305,0.31,0.315,0.32,0.325,0.33,0.335,
0.34,0.345,0.35,0.355,0.36,0.365,0.37,0.375,0.38,0.385,0.39,0.395,0.4,0.405,
0.41,0.415,0.42,0.425,0.43,0.435,0.44,0.445,0.45,0.455,0.46,0.465,0.47,
0.475,0.48,0.485,0.49,0.495,0.5,0.505,0.51,0.515,0.52,0.525,0.53,0.535,
0.54,0.545,0.55,0.555,0.56,0.565,0.57,0.575,0.58,0.585,0.59,0.595,0.6,0.605,
0.61,0.615,0.62,0.625,0.63,0.635,0.64,0.645,0.65,0.655,0.66,0.665,0.67,
0.675,0.68,0.685,0.690000000000001,0.695000000000001,0.700000000000001,
0.705000000000001,0.710000000000001,0.715000000000001,0.720000000000001,
0.725000000000001,0.730000000000001,0.735000000000001,0.740000000000001,
0.745000000000001,0.750000000000001,0.755000000000001,0.760000000000001,
0.765000000000001,0.770000000000001,0.775000000000001,0.780000000000001,
0.785000000000001,0.790000000000001,0.795000000000001,0.800000000000001,
0.805000000000001,0.810000000000001,0.815000000000001,0.820000000000001,
0.825000000000001,0.830000000000001,0.835000000000001,0.840000000000001,
0.845000000000001,0.850000000000001,0.855000000000001,0.860000000000001,
0.865000000000001,0.870000000000001,0.875000000000001,0.880000000000001,
0.885000000000001,0.890000000000001,0.895000000000001,0.900000000000001,
0.905000000000001,0.910000000000001,0.915000000000001,0.920000000000001,
0.925000000000001,0.930000000000001,0.935000000000001,0.940000000000001,
0.945000000000001,0.950000000000001,0.955000000000001,0.960000000000001,
0.965000000000001,0.970000000000001,0.975000000000001,0.980000000000001,
0.985000000000001,0.990000000000001,0.995000000000001,1.),.UNSPECIFIED.)
CURVE()
GEOMETRIC_REPRESENTATION_ITEM()
RATIONAL_B_SPLINE_CURVE((1.,1.,1.,1.,1.,1.,1.,1.,1.,1.,1.,1.,1.,1.,1.,1.,
1.,1.,1.,1.,1.,1.,1.,1.,1.,1.,1.,1.,1.,1.,1.,1.,1.,1.,1.,1.,1.,1.,1.,1.,
1.,1.,1.,1.,1.,1.,1.,1.,1.,1.,1.,1.,1.,1.,1.,1.,1.,1.,1.,1.,1.,1.,1.,1.,
1.,1.,1.,1.,1.,1.,1.,1.,1.,1.,1.,1.,1.,1.,1.,1.,1.,1.,1.,1.,1.,1.,1.,1.,
1.,1.,1.,1.,1.,1.,1.,1.,1.,1.,1.,1.,1.,1.,1.,1.,1.,1.,1.,1.,1.,1.,1.,1.,
1.,1.,1.,1.,1.,1.,1.,1.,1.,1.,1.,1.,1.,1.,1.,1.,1.,1.,1.,1.,1.,1.,1.,1.,
1.,1.,1.,1.,1.,1.,1.,1.,1.,1.,1.,1.,1.,1.,1.,1.,1.,1.,1.,1.,1.,1.,1.,1.,
1.,1.,1.,1.,1.,1.,1.,1.,1.,1.,1.,1.,1.,1.,1.,1.,1.,1.,1.,1.,1.,1.,1.,1.,
1.,1.,1.,1.,1.,1.,1.,1.,1.,1.,1.,1.,1.,1.,1.,1.,1.,1.,1.,1.,1.))
REPRESENTATION_ITEM('')
);
#830=(
BOUNDED_CURVE()
B_SPLINE_CURVE(5,(#233968,#233969,#233970,#233971,#233972,#233973,#233974,
#233975,#233976,#233977,#233978,#233979,#233980,#233981,#233982,#233983,
#233984,#233985,#233986,#233987,#233988,#233989,#233990,#233991,#233992,
#233993,#233994,#233995,#233996,#233997,#233998,#233999,#234000,#234001,
#234002,#234003,#234004,#234005,#234006,#234007,#234008,#234009,#234010,
#234011,#234012,#234013,#234014,#234015,#234016,#234017,#234018,#234019,
#234020,#234021,#234022,#234023,#234024,#234025,#234026,#234027,#234028,
#234029,#234030,#234031,#234032,#234033,#234034,#234035,#234036,#234037,
#234038,#234039,#234040,#234041,#234042,#234043,#234044,#234045,#234046,
#234047,#234048,#234049,#234050,#234051,#234052,#234053,#234054,#234055,
#234056,#234057,#234058,#234059,#234060,#234061,#234062,#234063,#234064,
#234065,#234066,#234067,#234068,#234069,#234070,#234071,#234072,#234073,
#234074,#234075,#234076,#234077,#234078,#234079,#234080,#234081,#234082,
#234083,#234084,#234085,#234086,#234087,#234088,#234089,#234090,#234091,
#234092,#234093,#234094,#234095,#234096,#234097,#234098,#234099,#234100,
#234101,#234102,#234103,#234104,#234105,#234106,#234107,#234108,#234109,
#234110,#234111,#234112,#234113,#234114,#234115,#234116,#234117,#234118,
#234119,#234120,#234121,#234122,#234123,#234124,#234125,#234126,#234127,
#234128,#234129,#234130,#234131,#234132,#234133,#234134,#234135,#234136,
#234137,#234138,#234139,#234140,#234141,#234142,#234143,#234144,#234145,
#234146,#234147,#234148,#234149,#234150,#234151,#234152,#234153,#234154,
#234155,#234156,#234157,#234158,#234159,#234160,#234161,#234162,#234163,
#234164,#234165,#234166,#234167,#234168,#234169,#234170,#234171,#234172),
 .UNSPECIFIED.,.F.,.F.)
B_SPLINE_CURVE_WITH_KNOTS((6,1,1,1,1,1,1,1,1,1,1,1,1,1,1,1,1,1,1,1,1,1,
1,1,1,1,1,1,1,1,1,1,1,1,1,1,1,1,1,1,1,1,1,1,1,1,1,1,1,1,1,1,1,1,1,1,1,1,
1,1,1,1,1,1,1,1,1,1,1,1,1,1,1,1,1,1,1,1,1,1,1,1,1,1,1,1,1,1,1,1,1,1,1,1,
1,1,1,1,1,1,1,1,1,1,1,1,1,1,1,1,1,1,1,1,1,1,1,1,1,1,1,1,1,1,1,1,1,1,1,1,
1,1,1,1,1,1,1,1,1,1,1,1,1,1,1,1,1,1,1,1,1,1,1,1,1,1,1,1,1,1,1,1,1,1,1,1,
1,1,1,1,1,1,1,1,1,1,1,1,1,1,1,1,1,1,1,1,1,1,1,1,1,1,1,1,1,1,1,1,1,1,6),
(-1.,-0.995000000000001,-0.990000000000001,-0.985000000000001,-0.980000000000001,
-0.975000000000001,-0.970000000000001,-0.965000000000001,-0.960000000000001,
-0.955000000000001,-0.950000000000001,-0.945000000000001,-0.940000000000001,
-0.935000000000001,-0.930000000000001,-0.925000000000001,-0.920000000000001,
-0.915000000000001,-0.910000000000001,-0.905000000000001,-0.900000000000001,
-0.895000000000001,-0.890000000000001,-0.885000000000001,-0.880000000000001,
-0.875000000000001,-0.870000000000001,-0.865000000000001,-0.860000000000001,
-0.855000000000001,-0.850000000000001,-0.845000000000001,-0.840000000000001,
-0.835000000000001,-0.830000000000001,-0.825000000000001,-0.820000000000001,
-0.815000000000001,-0.810000000000001,-0.805000000000001,-0.800000000000001,
-0.795000000000001,-0.790000000000001,-0.785000000000001,-0.780000000000001,
-0.775000000000001,-0.770000000000001,-0.765000000000001,-0.760000000000001,
-0.755000000000001,-0.750000000000001,-0.745000000000001,-0.740000000000001,
-0.735000000000001,-0.730000000000001,-0.725000000000001,-0.720000000000001,
-0.715000000000001,-0.710000000000001,-0.705000000000001,-0.700000000000001,
-0.695000000000001,-0.690000000000001,-0.685,-0.68,-0.675,-0.67,-0.665,
-0.66,-0.655,-0.65,-0.645,-0.64,-0.635,-0.63,-0.625,-0.62,-0.615,-0.61,
-0.605,-0.6,-0.595,-0.59,-0.585,-0.58,-0.575,-0.57,-0.565,-0.56,-0.555,
-0.55,-0.545,-0.54,-0.535,-0.53,-0.525,-0.52,-0.515,-0.51,-0.505,-0.5,-0.495,
-0.49,-0.485,-0.48,-0.475,-0.47,-0.465,-0.46,-0.455,-0.45,-0.445,-0.44,
-0.435,-0.43,-0.425,-0.42,-0.415,-0.41,-0.405,-0.4,-0.395,-0.39,-0.385,
-0.38,-0.375,-0.37,-0.365,-0.36,-0.355,-0.35,-0.345,-0.34,-0.335,-0.33,
-0.325,-0.32,-0.315,-0.31,-0.305,-0.3,-0.295,-0.29,-0.285,-0.28,-0.275,
-0.27,-0.265,-0.26,-0.255,-0.25,-0.245,-0.24,-0.235,-0.23,-0.225,-0.22,
-0.215,-0.21,-0.205,-0.2,-0.195,-0.19,-0.185,-0.18,-0.175,-0.17,-0.165,
-0.16,-0.155,-0.15,-0.145,-0.14,-0.135,-0.13,-0.125,-0.12,-0.115,-0.11,
-0.105,-0.1,-0.095,-0.09,-0.085,-0.08,-0.075,-0.07,-0.065,-0.06,-0.055,
-0.05,-0.045,-0.04,-0.035,-0.03,-0.025,-0.02,-0.015,-0.01,-0.005,0.),
 .UNSPECIFIED.)
CURVE()
GEOMETRIC_REPRESENTATION_ITEM()
RATIONAL_B_SPLINE_CURVE((1.,1.,1.,1.,1.,1.,1.,1.,1.,1.,1.,1.,1.,1.,1.,1.,
1.,1.,1.,1.,1.,1.,1.,1.,1.,1.,1.,1.,1.,1.,1.,1.,1.,1.,1.,1.,1.,1.,1.,1.,
1.,1.,1.,1.,1.,1.,1.,1.,1.,1.,1.,1.,1.,1.,1.,1.,1.,1.,1.,1.,1.,1.,1.,1.,
1.,1.,1.,1.,1.,1.,1.,1.,1.,1.,1.,1.,1.,1.,1.,1.,1.,1.,1.,1.,1.,1.,1.,1.,
1.,1.,1.,1.,1.,1.,1.,1.,1.,1.,1.,1.,1.,1.,1.,1.,1.,1.,1.,1.,1.,1.,1.,1.,
1.,1.,1.,1.,1.,1.,1.,1.,1.,1.,1.,1.,1.,1.,1.,1.,1.,1.,1.,1.,1.,1.,1.,1.,
1.,1.,1.,1.,1.,1.,1.,1.,1.,1.,1.,1.,1.,1.,1.,1.,1.,1.,1.,1.,1.,1.,1.,1.,
1.,1.,1.,1.,1.,1.,1.,1.,1.,1.,1.,1.,1.,1.,1.,1.,1.,1.,1.,1.,1.,1.,1.,1.,
1.,1.,1.,1.,1.,1.,1.,1.,1.,1.,1.,1.,1.,1.,1.,1.,1.,1.,1.,1.,1.))
REPRESENTATION_ITEM('')
);
#831=(
BOUNDED_CURVE()
B_SPLINE_CURVE(5,(#234591,#234592,#234593,#234594,#234595,#234596,#234597,
#234598,#234599,#234600,#234601,#234602,#234603,#234604,#234605,#234606,
#234607,#234608,#234609,#234610,#234611,#234612,#234613,#234614,#234615,
#234616,#234617,#234618,#234619,#234620,#234621,#234622,#234623,#234624,
#234625,#234626,#234627,#234628,#234629,#234630,#234631,#234632,#234633,
#234634,#234635,#234636,#234637,#234638,#234639,#234640,#234641,#234642,
#234643,#234644,#234645,#234646,#234647,#234648,#234649,#234650,#234651,
#234652,#234653,#234654,#234655,#234656,#234657,#234658,#234659,#234660,
#234661,#234662,#234663,#234664,#234665,#234666,#234667,#234668,#234669,
#234670,#234671,#234672,#234673,#234674,#234675,#234676,#234677,#234678,
#234679,#234680,#234681,#234682,#234683,#234684,#234685,#234686,#234687,
#234688,#234689,#234690,#234691,#234692,#234693,#234694,#234695,#234696,
#234697,#234698,#234699,#234700,#234701,#234702,#234703,#234704,#234705,
#234706,#234707,#234708,#234709,#234710,#234711,#234712,#234713,#234714,
#234715,#234716,#234717,#234718,#234719,#234720,#234721,#234722,#234723,
#234724,#234725,#234726,#234727,#234728,#234729,#234730,#234731,#234732,
#234733,#234734,#234735,#234736,#234737,#234738,#234739,#234740,#234741,
#234742,#234743,#234744,#234745,#234746,#234747,#234748,#234749,#234750,
#234751,#234752,#234753,#234754,#234755,#234756,#234757,#234758,#234759,
#234760,#234761,#234762,#234763,#234764,#234765,#234766,#234767,#234768,
#234769,#234770,#234771,#234772,#234773,#234774,#234775,#234776,#234777,
#234778,#234779,#234780,#234781,#234782,#234783,#234784,#234785,#234786,
#234787,#234788,#234789,#234790,#234791,#234792,#234793,#234794,#234795),
 .UNSPECIFIED.,.F.,.F.)
B_SPLINE_CURVE_WITH_KNOTS((6,1,1,1,1,1,1,1,1,1,1,1,1,1,1,1,1,1,1,1,1,1,
1,1,1,1,1,1,1,1,1,1,1,1,1,1,1,1,1,1,1,1,1,1,1,1,1,1,1,1,1,1,1,1,1,1,1,1,
1,1,1,1,1,1,1,1,1,1,1,1,1,1,1,1,1,1,1,1,1,1,1,1,1,1,1,1,1,1,1,1,1,1,1,1,
1,1,1,1,1,1,1,1,1,1,1,1,1,1,1,1,1,1,1,1,1,1,1,1,1,1,1,1,1,1,1,1,1,1,1,1,
1,1,1,1,1,1,1,1,1,1,1,1,1,1,1,1,1,1,1,1,1,1,1,1,1,1,1,1,1,1,1,1,1,1,1,1,
1,1,1,1,1,1,1,1,1,1,1,1,1,1,1,1,1,1,1,1,1,1,1,1,1,1,1,1,1,1,1,1,1,1,6),
(-1.,-0.995000000000001,-0.990000000000001,-0.985000000000001,-0.980000000000001,
-0.975000000000001,-0.970000000000001,-0.965000000000001,-0.960000000000001,
-0.955000000000001,-0.950000000000001,-0.945000000000001,-0.940000000000001,
-0.935000000000001,-0.930000000000001,-0.925000000000001,-0.920000000000001,
-0.915000000000001,-0.910000000000001,-0.905000000000001,-0.900000000000001,
-0.895000000000001,-0.890000000000001,-0.885000000000001,-0.880000000000001,
-0.875000000000001,-0.870000000000001,-0.865000000000001,-0.860000000000001,
-0.855000000000001,-0.850000000000001,-0.845000000000001,-0.840000000000001,
-0.835000000000001,-0.830000000000001,-0.825000000000001,-0.820000000000001,
-0.815000000000001,-0.810000000000001,-0.805000000000001,-0.800000000000001,
-0.795000000000001,-0.790000000000001,-0.785000000000001,-0.780000000000001,
-0.775000000000001,-0.770000000000001,-0.765000000000001,-0.760000000000001,
-0.755000000000001,-0.750000000000001,-0.745000000000001,-0.740000000000001,
-0.735000000000001,-0.730000000000001,-0.725000000000001,-0.720000000000001,
-0.715000000000001,-0.710000000000001,-0.705000000000001,-0.700000000000001,
-0.695000000000001,-0.690000000000001,-0.685,-0.68,-0.675,-0.67,-0.665,
-0.66,-0.655,-0.65,-0.645,-0.64,-0.635,-0.63,-0.625,-0.62,-0.615,-0.61,
-0.605,-0.6,-0.595,-0.59,-0.585,-0.58,-0.575,-0.57,-0.565,-0.56,-0.555,
-0.55,-0.545,-0.54,-0.535,-0.53,-0.525,-0.52,-0.515,-0.51,-0.505,-0.5,-0.495,
-0.49,-0.485,-0.48,-0.475,-0.47,-0.465,-0.46,-0.455,-0.45,-0.445,-0.44,
-0.435,-0.43,-0.425,-0.42,-0.415,-0.41,-0.405,-0.4,-0.395,-0.39,-0.385,
-0.38,-0.375,-0.37,-0.365,-0.36,-0.355,-0.35,-0.345,-0.34,-0.335,-0.33,
-0.325,-0.32,-0.315,-0.31,-0.305,-0.3,-0.295,-0.29,-0.285,-0.28,-0.275,
-0.27,-0.265,-0.26,-0.255,-0.25,-0.245,-0.24,-0.235,-0.23,-0.225,-0.22,
-0.215,-0.21,-0.205,-0.2,-0.195,-0.19,-0.185,-0.18,-0.175,-0.17,-0.165,
-0.16,-0.155,-0.15,-0.145,-0.14,-0.135,-0.13,-0.125,-0.12,-0.115,-0.11,
-0.105,-0.1,-0.095,-0.09,-0.085,-0.08,-0.075,-0.07,-0.065,-0.06,-0.055,
-0.05,-0.045,-0.04,-0.035,-0.03,-0.025,-0.02,-0.015,-0.01,-0.005,0.),
 .UNSPECIFIED.)
CURVE()
GEOMETRIC_REPRESENTATION_ITEM()
RATIONAL_B_SPLINE_CURVE((1.,1.,1.,1.,1.,1.,1.,1.,1.,1.,1.,1.,1.,1.,1.,1.,
1.,1.,1.,1.,1.,1.,1.,1.,1.,1.,1.,1.,1.,1.,1.,1.,1.,1.,1.,1.,1.,1.,1.,1.,
1.,1.,1.,1.,1.,1.,1.,1.,1.,1.,1.,1.,1.,1.,1.,1.,1.,1.,1.,1.,1.,1.,1.,1.,
1.,1.,1.,1.,1.,1.,1.,1.,1.,1.,1.,1.,1.,1.,1.,1.,1.,1.,1.,1.,1.,1.,1.,1.,
1.,1.,1.,1.,1.,1.,1.,1.,1.,1.,1.,1.,1.,1.,1.,1.,1.,1.,1.,1.,1.,1.,1.,1.,
1.,1.,1.,1.,1.,1.,1.,1.,1.,1.,1.,1.,1.,1.,1.,1.,1.,1.,1.,1.,1.,1.,1.,1.,
1.,1.,1.,1.,1.,1.,1.,1.,1.,1.,1.,1.,1.,1.,1.,1.,1.,1.,1.,1.,1.,1.,1.,1.,
1.,1.,1.,1.,1.,1.,1.,1.,1.,1.,1.,1.,1.,1.,1.,1.,1.,1.,1.,1.,1.,1.,1.,1.,
1.,1.,1.,1.,1.,1.,1.,1.,1.,1.,1.,1.,1.,1.,1.,1.,1.,1.,1.,1.,1.))
REPRESENTATION_ITEM('')
);
#832=(
BOUNDED_CURVE()
B_SPLINE_CURVE(5,(#234798,#234799,#234800,#234801,#234802,#234803,#234804,
#234805,#234806,#234807,#234808,#234809,#234810,#234811,#234812,#234813,
#234814,#234815,#234816,#234817,#234818,#234819,#234820,#234821,#234822,
#234823,#234824,#234825,#234826,#234827,#234828,#234829,#234830,#234831,
#234832,#234833,#234834,#234835,#234836,#234837,#234838,#234839,#234840,
#234841,#234842,#234843,#234844,#234845,#234846,#234847,#234848,#234849,
#234850,#234851,#234852,#234853,#234854,#234855,#234856,#234857,#234858,
#234859,#234860,#234861,#234862,#234863,#234864,#234865,#234866,#234867,
#234868,#234869,#234870,#234871,#234872,#234873,#234874,#234875,#234876,
#234877,#234878,#234879,#234880,#234881,#234882,#234883,#234884,#234885,
#234886,#234887,#234888,#234889,#234890,#234891,#234892,#234893,#234894,
#234895,#234896,#234897,#234898,#234899,#234900,#234901,#234902,#234903,
#234904,#234905,#234906,#234907,#234908,#234909,#234910,#234911,#234912,
#234913,#234914,#234915,#234916,#234917,#234918,#234919,#234920,#234921,
#234922,#234923,#234924,#234925,#234926,#234927,#234928,#234929,#234930,
#234931,#234932,#234933,#234934,#234935,#234936,#234937,#234938,#234939,
#234940,#234941,#234942,#234943,#234944,#234945,#234946,#234947,#234948,
#234949,#234950,#234951,#234952,#234953,#234954,#234955,#234956,#234957,
#234958,#234959,#234960,#234961,#234962,#234963,#234964,#234965,#234966,
#234967,#234968,#234969,#234970,#234971,#234972,#234973,#234974,#234975,
#234976,#234977,#234978,#234979,#234980,#234981,#234982,#234983,#234984,
#234985,#234986,#234987,#234988,#234989,#234990,#234991,#234992,#234993,
#234994,#234995,#234996,#234997,#234998,#234999,#235000,#235001,#235002),
 .UNSPECIFIED.,.F.,.F.)
B_SPLINE_CURVE_WITH_KNOTS((6,1,1,1,1,1,1,1,1,1,1,1,1,1,1,1,1,1,1,1,1,1,
1,1,1,1,1,1,1,1,1,1,1,1,1,1,1,1,1,1,1,1,1,1,1,1,1,1,1,1,1,1,1,1,1,1,1,1,
1,1,1,1,1,1,1,1,1,1,1,1,1,1,1,1,1,1,1,1,1,1,1,1,1,1,1,1,1,1,1,1,1,1,1,1,
1,1,1,1,1,1,1,1,1,1,1,1,1,1,1,1,1,1,1,1,1,1,1,1,1,1,1,1,1,1,1,1,1,1,1,1,
1,1,1,1,1,1,1,1,1,1,1,1,1,1,1,1,1,1,1,1,1,1,1,1,1,1,1,1,1,1,1,1,1,1,1,1,
1,1,1,1,1,1,1,1,1,1,1,1,1,1,1,1,1,1,1,1,1,1,1,1,1,1,1,1,1,1,1,1,1,1,6),
(0.,0.005,0.01,0.015,0.02,0.025,0.03,0.035,0.04,0.045,0.05,0.055,0.06,0.065,
0.07,0.075,0.08,0.085,0.09,0.095,0.1,0.105,0.11,0.115,0.12,0.125,0.13,0.135,
0.14,0.145,0.15,0.155,0.16,0.165,0.17,0.175,0.18,0.185,0.19,0.195,0.2,0.205,
0.21,0.215,0.22,0.225,0.23,0.235,0.24,0.245,0.25,0.255,0.26,0.265,0.27,
0.275,0.28,0.285,0.29,0.295,0.3,0.305,0.31,0.315,0.32,0.325,0.33,0.335,
0.34,0.345,0.35,0.355,0.36,0.365,0.37,0.375,0.38,0.385,0.39,0.395,0.4,0.405,
0.41,0.415,0.42,0.425,0.43,0.435,0.44,0.445,0.45,0.455,0.46,0.465,0.47,
0.475,0.48,0.485,0.49,0.495,0.5,0.505,0.51,0.515,0.52,0.525,0.53,0.535,
0.54,0.545,0.55,0.555,0.56,0.565,0.57,0.575,0.58,0.585,0.59,0.595,0.6,0.605,
0.61,0.615,0.62,0.625,0.63,0.635,0.64,0.645,0.65,0.655,0.66,0.665,0.67,
0.675,0.68,0.685,0.690000000000001,0.695000000000001,0.700000000000001,
0.705000000000001,0.710000000000001,0.715000000000001,0.720000000000001,
0.725000000000001,0.730000000000001,0.735000000000001,0.740000000000001,
0.745000000000001,0.750000000000001,0.755000000000001,0.760000000000001,
0.765000000000001,0.770000000000001,0.775000000000001,0.780000000000001,
0.785000000000001,0.790000000000001,0.795000000000001,0.800000000000001,
0.805000000000001,0.810000000000001,0.815000000000001,0.820000000000001,
0.825000000000001,0.830000000000001,0.835000000000001,0.840000000000001,
0.845000000000001,0.850000000000001,0.855000000000001,0.860000000000001,
0.865000000000001,0.870000000000001,0.875000000000001,0.880000000000001,
0.885000000000001,0.890000000000001,0.895000000000001,0.900000000000001,
0.905000000000001,0.910000000000001,0.915000000000001,0.920000000000001,
0.925000000000001,0.930000000000001,0.935000000000001,0.940000000000001,
0.945000000000001,0.950000000000001,0.955000000000001,0.960000000000001,
0.965000000000001,0.970000000000001,0.975000000000001,0.980000000000001,
0.985000000000001,0.990000000000001,0.995000000000001,1.),.UNSPECIFIED.)
CURVE()
GEOMETRIC_REPRESENTATION_ITEM()
RATIONAL_B_SPLINE_CURVE((1.,1.,1.,1.,1.,1.,1.,1.,1.,1.,1.,1.,1.,1.,1.,1.,
1.,1.,1.,1.,1.,1.,1.,1.,1.,1.,1.,1.,1.,1.,1.,1.,1.,1.,1.,1.,1.,1.,1.,1.,
1.,1.,1.,1.,1.,1.,1.,1.,1.,1.,1.,1.,1.,1.,1.,1.,1.,1.,1.,1.,1.,1.,1.,1.,
1.,1.,1.,1.,1.,1.,1.,1.,1.,1.,1.,1.,1.,1.,1.,1.,1.,1.,1.,1.,1.,1.,1.,1.,
1.,1.,1.,1.,1.,1.,1.,1.,1.,1.,1.,1.,1.,1.,1.,1.,1.,1.,1.,1.,1.,1.,1.,1.,
1.,1.,1.,1.,1.,1.,1.,1.,1.,1.,1.,1.,1.,1.,1.,1.,1.,1.,1.,1.,1.,1.,1.,1.,
1.,1.,1.,1.,1.,1.,1.,1.,1.,1.,1.,1.,1.,1.,1.,1.,1.,1.,1.,1.,1.,1.,1.,1.,
1.,1.,1.,1.,1.,1.,1.,1.,1.,1.,1.,1.,1.,1.,1.,1.,1.,1.,1.,1.,1.,1.,1.,1.,
1.,1.,1.,1.,1.,1.,1.,1.,1.,1.,1.,1.,1.,1.,1.,1.,1.,1.,1.,1.,1.))
REPRESENTATION_ITEM('')
);
#833=(
BOUNDED_CURVE()
B_SPLINE_CURVE(5,(#235414,#235415,#235416,#235417,#235418,#235419,#235420,
#235421,#235422,#235423,#235424,#235425,#235426,#235427,#235428,#235429,
#235430,#235431,#235432,#235433,#235434,#235435,#235436,#235437,#235438,
#235439,#235440,#235441,#235442,#235443,#235444,#235445,#235446,#235447,
#235448,#235449,#235450,#235451,#235452,#235453,#235454,#235455,#235456,
#235457,#235458,#235459,#235460,#235461,#235462,#235463,#235464,#235465,
#235466,#235467,#235468,#235469,#235470,#235471,#235472,#235473,#235474,
#235475,#235476,#235477,#235478,#235479,#235480,#235481,#235482,#235483,
#235484,#235485,#235486,#235487,#235488,#235489,#235490,#235491,#235492,
#235493,#235494,#235495,#235496,#235497,#235498,#235499,#235500,#235501,
#235502,#235503,#235504,#235505,#235506,#235507,#235508,#235509,#235510,
#235511,#235512,#235513,#235514,#235515,#235516,#235517,#235518,#235519,
#235520,#235521,#235522,#235523,#235524,#235525,#235526,#235527,#235528,
#235529,#235530,#235531,#235532,#235533,#235534,#235535,#235536,#235537,
#235538,#235539,#235540,#235541,#235542,#235543,#235544,#235545,#235546,
#235547,#235548,#235549,#235550,#235551,#235552,#235553,#235554,#235555,
#235556,#235557,#235558,#235559,#235560,#235561,#235562,#235563,#235564,
#235565,#235566,#235567,#235568,#235569,#235570,#235571,#235572,#235573,
#235574,#235575,#235576,#235577,#235578,#235579,#235580,#235581,#235582,
#235583,#235584,#235585,#235586,#235587,#235588,#235589,#235590,#235591,
#235592,#235593,#235594,#235595,#235596,#235597,#235598,#235599,#235600,
#235601,#235602,#235603,#235604,#235605,#235606,#235607,#235608,#235609,
#235610,#235611,#235612,#235613,#235614,#235615,#235616,#235617,#235618),
 .UNSPECIFIED.,.F.,.F.)
B_SPLINE_CURVE_WITH_KNOTS((6,1,1,1,1,1,1,1,1,1,1,1,1,1,1,1,1,1,1,1,1,1,
1,1,1,1,1,1,1,1,1,1,1,1,1,1,1,1,1,1,1,1,1,1,1,1,1,1,1,1,1,1,1,1,1,1,1,1,
1,1,1,1,1,1,1,1,1,1,1,1,1,1,1,1,1,1,1,1,1,1,1,1,1,1,1,1,1,1,1,1,1,1,1,1,
1,1,1,1,1,1,1,1,1,1,1,1,1,1,1,1,1,1,1,1,1,1,1,1,1,1,1,1,1,1,1,1,1,1,1,1,
1,1,1,1,1,1,1,1,1,1,1,1,1,1,1,1,1,1,1,1,1,1,1,1,1,1,1,1,1,1,1,1,1,1,1,1,
1,1,1,1,1,1,1,1,1,1,1,1,1,1,1,1,1,1,1,1,1,1,1,1,1,1,1,1,1,1,1,1,1,1,6),
(0.,0.005,0.01,0.015,0.02,0.025,0.03,0.035,0.04,0.045,0.05,0.055,0.06,0.065,
0.07,0.075,0.08,0.085,0.09,0.095,0.1,0.105,0.11,0.115,0.12,0.125,0.13,0.135,
0.14,0.145,0.15,0.155,0.16,0.165,0.17,0.175,0.18,0.185,0.19,0.195,0.2,0.205,
0.21,0.215,0.22,0.225,0.23,0.235,0.24,0.245,0.25,0.255,0.26,0.265,0.27,
0.275,0.28,0.285,0.29,0.295,0.3,0.305,0.31,0.315,0.32,0.325,0.33,0.335,
0.34,0.345,0.35,0.355,0.36,0.365,0.37,0.375,0.38,0.385,0.39,0.395,0.4,0.405,
0.41,0.415,0.42,0.425,0.43,0.435,0.44,0.445,0.45,0.455,0.46,0.465,0.47,
0.475,0.48,0.485,0.49,0.495,0.5,0.505,0.51,0.515,0.52,0.525,0.53,0.535,
0.54,0.545,0.55,0.555,0.56,0.565,0.57,0.575,0.58,0.585,0.59,0.595,0.6,0.605,
0.61,0.615,0.62,0.625,0.63,0.635,0.64,0.645,0.65,0.655,0.66,0.665,0.67,
0.675,0.68,0.685,0.690000000000001,0.695000000000001,0.700000000000001,
0.705000000000001,0.710000000000001,0.715000000000001,0.720000000000001,
0.725000000000001,0.730000000000001,0.735000000000001,0.740000000000001,
0.745000000000001,0.750000000000001,0.755000000000001,0.760000000000001,
0.765000000000001,0.770000000000001,0.775000000000001,0.780000000000001,
0.785000000000001,0.790000000000001,0.795000000000001,0.800000000000001,
0.805000000000001,0.810000000000001,0.815000000000001,0.820000000000001,
0.825000000000001,0.830000000000001,0.835000000000001,0.840000000000001,
0.845000000000001,0.850000000000001,0.855000000000001,0.860000000000001,
0.865000000000001,0.870000000000001,0.875000000000001,0.880000000000001,
0.885000000000001,0.890000000000001,0.895000000000001,0.900000000000001,
0.905000000000001,0.910000000000001,0.915000000000001,0.920000000000001,
0.925000000000001,0.930000000000001,0.935000000000001,0.940000000000001,
0.945000000000001,0.950000000000001,0.955000000000001,0.960000000000001,
0.965000000000001,0.970000000000001,0.975000000000001,0.980000000000001,
0.985000000000001,0.990000000000001,0.995000000000001,1.),.UNSPECIFIED.)
CURVE()
GEOMETRIC_REPRESENTATION_ITEM()
RATIONAL_B_SPLINE_CURVE((1.,1.,1.,1.,1.,1.,1.,1.,1.,1.,1.,1.,1.,1.,1.,1.,
1.,1.,1.,1.,1.,1.,1.,1.,1.,1.,1.,1.,1.,1.,1.,1.,1.,1.,1.,1.,1.,1.,1.,1.,
1.,1.,1.,1.,1.,1.,1.,1.,1.,1.,1.,1.,1.,1.,1.,1.,1.,1.,1.,1.,1.,1.,1.,1.,
1.,1.,1.,1.,1.,1.,1.,1.,1.,1.,1.,1.,1.,1.,1.,1.,1.,1.,1.,1.,1.,1.,1.,1.,
1.,1.,1.,1.,1.,1.,1.,1.,1.,1.,1.,1.,1.,1.,1.,1.,1.,1.,1.,1.,1.,1.,1.,1.,
1.,1.,1.,1.,1.,1.,1.,1.,1.,1.,1.,1.,1.,1.,1.,1.,1.,1.,1.,1.,1.,1.,1.,1.,
1.,1.,1.,1.,1.,1.,1.,1.,1.,1.,1.,1.,1.,1.,1.,1.,1.,1.,1.,1.,1.,1.,1.,1.,
1.,1.,1.,1.,1.,1.,1.,1.,1.,1.,1.,1.,1.,1.,1.,1.,1.,1.,1.,1.,1.,1.,1.,1.,
1.,1.,1.,1.,1.,1.,1.,1.,1.,1.,1.,1.,1.,1.,1.,1.,1.,1.,1.,1.,1.))
REPRESENTATION_ITEM('')
);
#834=(
BOUNDED_CURVE()
B_SPLINE_CURVE(5,(#235620,#235621,#235622,#235623,#235624,#235625,#235626,
#235627,#235628,#235629,#235630,#235631,#235632,#235633,#235634,#235635,
#235636,#235637,#235638,#235639,#235640,#235641,#235642,#235643,#235644,
#235645,#235646,#235647,#235648,#235649,#235650,#235651,#235652,#235653,
#235654,#235655,#235656,#235657,#235658,#235659,#235660,#235661,#235662,
#235663,#235664,#235665,#235666,#235667,#235668,#235669,#235670,#235671,
#235672,#235673,#235674,#235675,#235676,#235677,#235678,#235679,#235680,
#235681,#235682,#235683,#235684,#235685,#235686,#235687,#235688,#235689,
#235690,#235691,#235692,#235693,#235694,#235695,#235696,#235697,#235698,
#235699,#235700,#235701,#235702,#235703,#235704,#235705,#235706,#235707,
#235708,#235709,#235710,#235711,#235712,#235713,#235714,#235715,#235716,
#235717,#235718,#235719,#235720,#235721,#235722,#235723,#235724,#235725,
#235726,#235727,#235728,#235729,#235730,#235731,#235732,#235733,#235734,
#235735,#235736,#235737,#235738,#235739,#235740,#235741,#235742,#235743,
#235744,#235745,#235746,#235747,#235748,#235749,#235750,#235751,#235752,
#235753,#235754,#235755,#235756,#235757,#235758,#235759,#235760,#235761,
#235762,#235763,#235764,#235765,#235766,#235767,#235768,#235769,#235770,
#235771,#235772,#235773,#235774,#235775,#235776,#235777,#235778,#235779,
#235780,#235781,#235782,#235783,#235784,#235785,#235786,#235787,#235788,
#235789,#235790,#235791,#235792,#235793,#235794,#235795,#235796,#235797,
#235798,#235799,#235800,#235801,#235802,#235803,#235804,#235805,#235806,
#235807,#235808,#235809,#235810,#235811,#235812,#235813,#235814,#235815,
#235816,#235817,#235818,#235819,#235820,#235821,#235822,#235823,#235824),
 .UNSPECIFIED.,.F.,.F.)
B_SPLINE_CURVE_WITH_KNOTS((6,1,1,1,1,1,1,1,1,1,1,1,1,1,1,1,1,1,1,1,1,1,
1,1,1,1,1,1,1,1,1,1,1,1,1,1,1,1,1,1,1,1,1,1,1,1,1,1,1,1,1,1,1,1,1,1,1,1,
1,1,1,1,1,1,1,1,1,1,1,1,1,1,1,1,1,1,1,1,1,1,1,1,1,1,1,1,1,1,1,1,1,1,1,1,
1,1,1,1,1,1,1,1,1,1,1,1,1,1,1,1,1,1,1,1,1,1,1,1,1,1,1,1,1,1,1,1,1,1,1,1,
1,1,1,1,1,1,1,1,1,1,1,1,1,1,1,1,1,1,1,1,1,1,1,1,1,1,1,1,1,1,1,1,1,1,1,1,
1,1,1,1,1,1,1,1,1,1,1,1,1,1,1,1,1,1,1,1,1,1,1,1,1,1,1,1,1,1,1,1,1,1,6),
(-1.,-0.995000000000001,-0.990000000000001,-0.985000000000001,-0.980000000000001,
-0.975000000000001,-0.970000000000001,-0.965000000000001,-0.960000000000001,
-0.955000000000001,-0.950000000000001,-0.945000000000001,-0.940000000000001,
-0.935000000000001,-0.930000000000001,-0.925000000000001,-0.920000000000001,
-0.915000000000001,-0.910000000000001,-0.905000000000001,-0.900000000000001,
-0.895000000000001,-0.890000000000001,-0.885000000000001,-0.880000000000001,
-0.875000000000001,-0.870000000000001,-0.865000000000001,-0.860000000000001,
-0.855000000000001,-0.850000000000001,-0.845000000000001,-0.840000000000001,
-0.835000000000001,-0.830000000000001,-0.825000000000001,-0.820000000000001,
-0.815000000000001,-0.810000000000001,-0.805000000000001,-0.800000000000001,
-0.795000000000001,-0.790000000000001,-0.785000000000001,-0.780000000000001,
-0.775000000000001,-0.770000000000001,-0.765000000000001,-0.760000000000001,
-0.755000000000001,-0.750000000000001,-0.745000000000001,-0.740000000000001,
-0.735000000000001,-0.730000000000001,-0.725000000000001,-0.720000000000001,
-0.715000000000001,-0.710000000000001,-0.705000000000001,-0.700000000000001,
-0.695000000000001,-0.690000000000001,-0.685,-0.68,-0.675,-0.67,-0.665,
-0.66,-0.655,-0.65,-0.645,-0.64,-0.635,-0.63,-0.625,-0.62,-0.615,-0.61,
-0.605,-0.6,-0.595,-0.59,-0.585,-0.58,-0.575,-0.57,-0.565,-0.56,-0.555,
-0.55,-0.545,-0.54,-0.535,-0.53,-0.525,-0.52,-0.515,-0.51,-0.505,-0.5,-0.495,
-0.49,-0.485,-0.48,-0.475,-0.47,-0.465,-0.46,-0.455,-0.45,-0.445,-0.44,
-0.435,-0.43,-0.425,-0.42,-0.415,-0.41,-0.405,-0.4,-0.395,-0.39,-0.385,
-0.38,-0.375,-0.37,-0.365,-0.36,-0.355,-0.35,-0.345,-0.34,-0.335,-0.33,
-0.325,-0.32,-0.315,-0.31,-0.305,-0.3,-0.295,-0.29,-0.285,-0.28,-0.275,
-0.27,-0.265,-0.26,-0.255,-0.25,-0.245,-0.24,-0.235,-0.23,-0.225,-0.22,
-0.215,-0.21,-0.205,-0.2,-0.195,-0.19,-0.185,-0.18,-0.175,-0.17,-0.165,
-0.16,-0.155,-0.15,-0.145,-0.14,-0.135,-0.13,-0.125,-0.12,-0.115,-0.11,
-0.105,-0.1,-0.095,-0.09,-0.085,-0.08,-0.075,-0.07,-0.065,-0.06,-0.055,
-0.05,-0.045,-0.04,-0.035,-0.03,-0.025,-0.02,-0.015,-0.01,-0.005,0.),
 .UNSPECIFIED.)
CURVE()
GEOMETRIC_REPRESENTATION_ITEM()
RATIONAL_B_SPLINE_CURVE((1.,1.,1.,1.,1.,1.,1.,1.,1.,1.,1.,1.,1.,1.,1.,1.,
1.,1.,1.,1.,1.,1.,1.,1.,1.,1.,1.,1.,1.,1.,1.,1.,1.,1.,1.,1.,1.,1.,1.,1.,
1.,1.,1.,1.,1.,1.,1.,1.,1.,1.,1.,1.,1.,1.,1.,1.,1.,1.,1.,1.,1.,1.,1.,1.,
1.,1.,1.,1.,1.,1.,1.,1.,1.,1.,1.,1.,1.,1.,1.,1.,1.,1.,1.,1.,1.,1.,1.,1.,
1.,1.,1.,1.,1.,1.,1.,1.,1.,1.,1.,1.,1.,1.,1.,1.,1.,1.,1.,1.,1.,1.,1.,1.,
1.,1.,1.,1.,1.,1.,1.,1.,1.,1.,1.,1.,1.,1.,1.,1.,1.,1.,1.,1.,1.,1.,1.,1.,
1.,1.,1.,1.,1.,1.,1.,1.,1.,1.,1.,1.,1.,1.,1.,1.,1.,1.,1.,1.,1.,1.,1.,1.,
1.,1.,1.,1.,1.,1.,1.,1.,1.,1.,1.,1.,1.,1.,1.,1.,1.,1.,1.,1.,1.,1.,1.,1.,
1.,1.,1.,1.,1.,1.,1.,1.,1.,1.,1.,1.,1.,1.,1.,1.,1.,1.,1.,1.,1.))
REPRESENTATION_ITEM('')
);
#835=(
BOUNDED_CURVE()
B_SPLINE_CURVE(5,(#236243,#236244,#236245,#236246,#236247,#236248,#236249,
#236250,#236251,#236252,#236253,#236254,#236255,#236256,#236257,#236258,
#236259,#236260,#236261,#236262,#236263,#236264,#236265,#236266,#236267,
#236268,#236269,#236270,#236271,#236272,#236273,#236274,#236275,#236276,
#236277,#236278,#236279,#236280,#236281,#236282,#236283,#236284,#236285,
#236286,#236287,#236288,#236289,#236290,#236291,#236292,#236293,#236294,
#236295,#236296,#236297,#236298,#236299,#236300,#236301,#236302,#236303,
#236304,#236305,#236306,#236307,#236308,#236309,#236310,#236311,#236312,
#236313,#236314,#236315,#236316,#236317,#236318,#236319,#236320,#236321,
#236322,#236323,#236324,#236325,#236326,#236327,#236328,#236329,#236330,
#236331,#236332,#236333,#236334,#236335,#236336,#236337,#236338,#236339,
#236340,#236341,#236342,#236343,#236344,#236345,#236346,#236347,#236348,
#236349,#236350,#236351,#236352,#236353,#236354,#236355,#236356,#236357,
#236358,#236359,#236360,#236361,#236362,#236363,#236364,#236365,#236366,
#236367,#236368,#236369,#236370,#236371,#236372,#236373,#236374,#236375,
#236376,#236377,#236378,#236379,#236380,#236381,#236382,#236383,#236384,
#236385,#236386,#236387,#236388,#236389,#236390,#236391,#236392,#236393,
#236394,#236395,#236396,#236397,#236398,#236399,#236400,#236401,#236402,
#236403,#236404,#236405,#236406,#236407,#236408,#236409,#236410,#236411,
#236412,#236413,#236414,#236415,#236416,#236417,#236418,#236419,#236420,
#236421,#236422,#236423,#236424,#236425,#236426,#236427,#236428,#236429,
#236430,#236431,#236432,#236433,#236434,#236435,#236436,#236437,#236438,
#236439,#236440,#236441,#236442,#236443,#236444,#236445,#236446,#236447),
 .UNSPECIFIED.,.F.,.F.)
B_SPLINE_CURVE_WITH_KNOTS((6,1,1,1,1,1,1,1,1,1,1,1,1,1,1,1,1,1,1,1,1,1,
1,1,1,1,1,1,1,1,1,1,1,1,1,1,1,1,1,1,1,1,1,1,1,1,1,1,1,1,1,1,1,1,1,1,1,1,
1,1,1,1,1,1,1,1,1,1,1,1,1,1,1,1,1,1,1,1,1,1,1,1,1,1,1,1,1,1,1,1,1,1,1,1,
1,1,1,1,1,1,1,1,1,1,1,1,1,1,1,1,1,1,1,1,1,1,1,1,1,1,1,1,1,1,1,1,1,1,1,1,
1,1,1,1,1,1,1,1,1,1,1,1,1,1,1,1,1,1,1,1,1,1,1,1,1,1,1,1,1,1,1,1,1,1,1,1,
1,1,1,1,1,1,1,1,1,1,1,1,1,1,1,1,1,1,1,1,1,1,1,1,1,1,1,1,1,1,1,1,1,1,6),
(-1.,-0.995000000000001,-0.990000000000001,-0.985000000000001,-0.980000000000001,
-0.975000000000001,-0.970000000000001,-0.965000000000001,-0.960000000000001,
-0.955000000000001,-0.950000000000001,-0.945000000000001,-0.940000000000001,
-0.935000000000001,-0.930000000000001,-0.925000000000001,-0.920000000000001,
-0.915000000000001,-0.910000000000001,-0.905000000000001,-0.900000000000001,
-0.895000000000001,-0.890000000000001,-0.885000000000001,-0.880000000000001,
-0.875000000000001,-0.870000000000001,-0.865000000000001,-0.860000000000001,
-0.855000000000001,-0.850000000000001,-0.845000000000001,-0.840000000000001,
-0.835000000000001,-0.830000000000001,-0.825000000000001,-0.820000000000001,
-0.815000000000001,-0.810000000000001,-0.805000000000001,-0.800000000000001,
-0.795000000000001,-0.790000000000001,-0.785000000000001,-0.780000000000001,
-0.775000000000001,-0.770000000000001,-0.765000000000001,-0.760000000000001,
-0.755000000000001,-0.750000000000001,-0.745000000000001,-0.740000000000001,
-0.735000000000001,-0.730000000000001,-0.725000000000001,-0.720000000000001,
-0.715000000000001,-0.710000000000001,-0.705000000000001,-0.700000000000001,
-0.695000000000001,-0.690000000000001,-0.685,-0.68,-0.675,-0.67,-0.665,
-0.66,-0.655,-0.65,-0.645,-0.64,-0.635,-0.63,-0.625,-0.62,-0.615,-0.61,
-0.605,-0.6,-0.595,-0.59,-0.585,-0.58,-0.575,-0.57,-0.565,-0.56,-0.555,
-0.55,-0.545,-0.54,-0.535,-0.53,-0.525,-0.52,-0.515,-0.51,-0.505,-0.5,-0.495,
-0.49,-0.485,-0.48,-0.475,-0.47,-0.465,-0.46,-0.455,-0.45,-0.445,-0.44,
-0.435,-0.43,-0.425,-0.42,-0.415,-0.41,-0.405,-0.4,-0.395,-0.39,-0.385,
-0.38,-0.375,-0.37,-0.365,-0.36,-0.355,-0.35,-0.345,-0.34,-0.335,-0.33,
-0.325,-0.32,-0.315,-0.31,-0.305,-0.3,-0.295,-0.29,-0.285,-0.28,-0.275,
-0.27,-0.265,-0.26,-0.255,-0.25,-0.245,-0.24,-0.235,-0.23,-0.225,-0.22,
-0.215,-0.21,-0.205,-0.2,-0.195,-0.19,-0.185,-0.18,-0.175,-0.17,-0.165,
-0.16,-0.155,-0.15,-0.145,-0.14,-0.135,-0.13,-0.125,-0.12,-0.115,-0.11,
-0.105,-0.1,-0.095,-0.09,-0.085,-0.08,-0.075,-0.07,-0.065,-0.06,-0.055,
-0.05,-0.045,-0.04,-0.035,-0.03,-0.025,-0.02,-0.015,-0.01,-0.005,0.),
 .UNSPECIFIED.)
CURVE()
GEOMETRIC_REPRESENTATION_ITEM()
RATIONAL_B_SPLINE_CURVE((1.,1.,1.,1.,1.,1.,1.,1.,1.,1.,1.,1.,1.,1.,1.,1.,
1.,1.,1.,1.,1.,1.,1.,1.,1.,1.,1.,1.,1.,1.,1.,1.,1.,1.,1.,1.,1.,1.,1.,1.,
1.,1.,1.,1.,1.,1.,1.,1.,1.,1.,1.,1.,1.,1.,1.,1.,1.,1.,1.,1.,1.,1.,1.,1.,
1.,1.,1.,1.,1.,1.,1.,1.,1.,1.,1.,1.,1.,1.,1.,1.,1.,1.,1.,1.,1.,1.,1.,1.,
1.,1.,1.,1.,1.,1.,1.,1.,1.,1.,1.,1.,1.,1.,1.,1.,1.,1.,1.,1.,1.,1.,1.,1.,
1.,1.,1.,1.,1.,1.,1.,1.,1.,1.,1.,1.,1.,1.,1.,1.,1.,1.,1.,1.,1.,1.,1.,1.,
1.,1.,1.,1.,1.,1.,1.,1.,1.,1.,1.,1.,1.,1.,1.,1.,1.,1.,1.,1.,1.,1.,1.,1.,
1.,1.,1.,1.,1.,1.,1.,1.,1.,1.,1.,1.,1.,1.,1.,1.,1.,1.,1.,1.,1.,1.,1.,1.,
1.,1.,1.,1.,1.,1.,1.,1.,1.,1.,1.,1.,1.,1.,1.,1.,1.,1.,1.,1.,1.))
REPRESENTATION_ITEM('')
);
#836=(
BOUNDED_CURVE()
B_SPLINE_CURVE(5,(#236450,#236451,#236452,#236453,#236454,#236455,#236456,
#236457,#236458,#236459,#236460,#236461,#236462,#236463,#236464,#236465,
#236466,#236467,#236468,#236469,#236470,#236471,#236472,#236473,#236474,
#236475,#236476,#236477,#236478,#236479,#236480,#236481,#236482,#236483,
#236484,#236485,#236486,#236487,#236488,#236489,#236490,#236491,#236492,
#236493,#236494,#236495,#236496,#236497,#236498,#236499,#236500,#236501,
#236502,#236503,#236504,#236505,#236506,#236507,#236508,#236509,#236510,
#236511,#236512,#236513,#236514,#236515,#236516,#236517,#236518,#236519,
#236520,#236521,#236522,#236523,#236524,#236525,#236526,#236527,#236528,
#236529,#236530,#236531,#236532,#236533,#236534,#236535,#236536,#236537,
#236538,#236539,#236540,#236541,#236542,#236543,#236544,#236545,#236546,
#236547,#236548,#236549,#236550,#236551,#236552,#236553,#236554,#236555,
#236556,#236557,#236558,#236559,#236560,#236561,#236562,#236563,#236564,
#236565,#236566,#236567,#236568,#236569,#236570,#236571,#236572,#236573,
#236574,#236575,#236576,#236577,#236578,#236579,#236580,#236581,#236582,
#236583,#236584,#236585,#236586,#236587,#236588,#236589,#236590,#236591,
#236592,#236593,#236594,#236595,#236596,#236597,#236598,#236599,#236600,
#236601,#236602,#236603,#236604,#236605,#236606,#236607,#236608,#236609,
#236610,#236611,#236612,#236613,#236614,#236615,#236616,#236617,#236618,
#236619,#236620,#236621,#236622,#236623,#236624,#236625,#236626,#236627,
#236628,#236629,#236630,#236631,#236632,#236633,#236634,#236635,#236636,
#236637,#236638,#236639,#236640,#236641,#236642,#236643,#236644,#236645,
#236646,#236647,#236648,#236649,#236650,#236651,#236652,#236653,#236654),
 .UNSPECIFIED.,.F.,.F.)
B_SPLINE_CURVE_WITH_KNOTS((6,1,1,1,1,1,1,1,1,1,1,1,1,1,1,1,1,1,1,1,1,1,
1,1,1,1,1,1,1,1,1,1,1,1,1,1,1,1,1,1,1,1,1,1,1,1,1,1,1,1,1,1,1,1,1,1,1,1,
1,1,1,1,1,1,1,1,1,1,1,1,1,1,1,1,1,1,1,1,1,1,1,1,1,1,1,1,1,1,1,1,1,1,1,1,
1,1,1,1,1,1,1,1,1,1,1,1,1,1,1,1,1,1,1,1,1,1,1,1,1,1,1,1,1,1,1,1,1,1,1,1,
1,1,1,1,1,1,1,1,1,1,1,1,1,1,1,1,1,1,1,1,1,1,1,1,1,1,1,1,1,1,1,1,1,1,1,1,
1,1,1,1,1,1,1,1,1,1,1,1,1,1,1,1,1,1,1,1,1,1,1,1,1,1,1,1,1,1,1,1,1,1,6),
(0.,0.005,0.01,0.015,0.02,0.025,0.03,0.035,0.04,0.045,0.05,0.055,0.06,0.065,
0.07,0.075,0.08,0.085,0.09,0.095,0.1,0.105,0.11,0.115,0.12,0.125,0.13,0.135,
0.14,0.145,0.15,0.155,0.16,0.165,0.17,0.175,0.18,0.185,0.19,0.195,0.2,0.205,
0.21,0.215,0.22,0.225,0.23,0.235,0.24,0.245,0.25,0.255,0.26,0.265,0.27,
0.275,0.28,0.285,0.29,0.295,0.3,0.305,0.31,0.315,0.32,0.325,0.33,0.335,
0.34,0.345,0.35,0.355,0.36,0.365,0.37,0.375,0.38,0.385,0.39,0.395,0.4,0.405,
0.41,0.415,0.42,0.425,0.43,0.435,0.44,0.445,0.45,0.455,0.46,0.465,0.47,
0.475,0.48,0.485,0.49,0.495,0.5,0.505,0.51,0.515,0.52,0.525,0.53,0.535,
0.54,0.545,0.55,0.555,0.56,0.565,0.57,0.575,0.58,0.585,0.59,0.595,0.6,0.605,
0.61,0.615,0.62,0.625,0.63,0.635,0.64,0.645,0.65,0.655,0.66,0.665,0.67,
0.675,0.68,0.685,0.690000000000001,0.695000000000001,0.700000000000001,
0.705000000000001,0.710000000000001,0.715000000000001,0.720000000000001,
0.725000000000001,0.730000000000001,0.735000000000001,0.740000000000001,
0.745000000000001,0.750000000000001,0.755000000000001,0.760000000000001,
0.765000000000001,0.770000000000001,0.775000000000001,0.780000000000001,
0.785000000000001,0.790000000000001,0.795000000000001,0.800000000000001,
0.805000000000001,0.810000000000001,0.815000000000001,0.820000000000001,
0.825000000000001,0.830000000000001,0.835000000000001,0.840000000000001,
0.845000000000001,0.850000000000001,0.855000000000001,0.860000000000001,
0.865000000000001,0.870000000000001,0.875000000000001,0.880000000000001,
0.885000000000001,0.890000000000001,0.895000000000001,0.900000000000001,
0.905000000000001,0.910000000000001,0.915000000000001,0.920000000000001,
0.925000000000001,0.930000000000001,0.935000000000001,0.940000000000001,
0.945000000000001,0.950000000000001,0.955000000000001,0.960000000000001,
0.965000000000001,0.970000000000001,0.975000000000001,0.980000000000001,
0.985000000000001,0.990000000000001,0.995000000000001,1.),.UNSPECIFIED.)
CURVE()
GEOMETRIC_REPRESENTATION_ITEM()
RATIONAL_B_SPLINE_CURVE((1.,1.,1.,1.,1.,1.,1.,1.,1.,1.,1.,1.,1.,1.,1.,1.,
1.,1.,1.,1.,1.,1.,1.,1.,1.,1.,1.,1.,1.,1.,1.,1.,1.,1.,1.,1.,1.,1.,1.,1.,
1.,1.,1.,1.,1.,1.,1.,1.,1.,1.,1.,1.,1.,1.,1.,1.,1.,1.,1.,1.,1.,1.,1.,1.,
1.,1.,1.,1.,1.,1.,1.,1.,1.,1.,1.,1.,1.,1.,1.,1.,1.,1.,1.,1.,1.,1.,1.,1.,
1.,1.,1.,1.,1.,1.,1.,1.,1.,1.,1.,1.,1.,1.,1.,1.,1.,1.,1.,1.,1.,1.,1.,1.,
1.,1.,1.,1.,1.,1.,1.,1.,1.,1.,1.,1.,1.,1.,1.,1.,1.,1.,1.,1.,1.,1.,1.,1.,
1.,1.,1.,1.,1.,1.,1.,1.,1.,1.,1.,1.,1.,1.,1.,1.,1.,1.,1.,1.,1.,1.,1.,1.,
1.,1.,1.,1.,1.,1.,1.,1.,1.,1.,1.,1.,1.,1.,1.,1.,1.,1.,1.,1.,1.,1.,1.,1.,
1.,1.,1.,1.,1.,1.,1.,1.,1.,1.,1.,1.,1.,1.,1.,1.,1.,1.,1.,1.,1.))
REPRESENTATION_ITEM('')
);
#837=(
BOUNDED_CURVE()
B_SPLINE_CURVE(5,(#237066,#237067,#237068,#237069,#237070,#237071,#237072,
#237073,#237074,#237075,#237076,#237077,#237078,#237079,#237080,#237081,
#237082,#237083,#237084,#237085,#237086,#237087,#237088,#237089,#237090,
#237091,#237092,#237093,#237094,#237095,#237096,#237097,#237098,#237099,
#237100,#237101,#237102,#237103,#237104,#237105,#237106,#237107,#237108,
#237109,#237110,#237111,#237112,#237113,#237114,#237115,#237116,#237117,
#237118,#237119,#237120,#237121,#237122,#237123,#237124,#237125,#237126,
#237127,#237128,#237129,#237130,#237131,#237132,#237133,#237134,#237135,
#237136,#237137,#237138,#237139,#237140,#237141,#237142,#237143,#237144,
#237145,#237146,#237147,#237148,#237149,#237150,#237151,#237152,#237153,
#237154,#237155,#237156,#237157,#237158,#237159,#237160,#237161,#237162,
#237163,#237164,#237165,#237166,#237167,#237168,#237169,#237170,#237171,
#237172,#237173,#237174,#237175,#237176,#237177,#237178,#237179,#237180,
#237181,#237182,#237183,#237184,#237185,#237186,#237187,#237188,#237189,
#237190,#237191,#237192,#237193,#237194,#237195,#237196,#237197,#237198,
#237199,#237200,#237201,#237202,#237203,#237204,#237205,#237206,#237207,
#237208,#237209,#237210,#237211,#237212,#237213,#237214,#237215,#237216,
#237217,#237218,#237219,#237220,#237221,#237222,#237223,#237224,#237225,
#237226,#237227,#237228,#237229,#237230,#237231,#237232,#237233,#237234,
#237235,#237236,#237237,#237238,#237239,#237240,#237241,#237242,#237243,
#237244,#237245,#237246,#237247,#237248,#237249,#237250,#237251,#237252,
#237253,#237254,#237255,#237256,#237257,#237258,#237259,#237260,#237261,
#237262,#237263,#237264,#237265,#237266,#237267,#237268,#237269,#237270),
 .UNSPECIFIED.,.F.,.F.)
B_SPLINE_CURVE_WITH_KNOTS((6,1,1,1,1,1,1,1,1,1,1,1,1,1,1,1,1,1,1,1,1,1,
1,1,1,1,1,1,1,1,1,1,1,1,1,1,1,1,1,1,1,1,1,1,1,1,1,1,1,1,1,1,1,1,1,1,1,1,
1,1,1,1,1,1,1,1,1,1,1,1,1,1,1,1,1,1,1,1,1,1,1,1,1,1,1,1,1,1,1,1,1,1,1,1,
1,1,1,1,1,1,1,1,1,1,1,1,1,1,1,1,1,1,1,1,1,1,1,1,1,1,1,1,1,1,1,1,1,1,1,1,
1,1,1,1,1,1,1,1,1,1,1,1,1,1,1,1,1,1,1,1,1,1,1,1,1,1,1,1,1,1,1,1,1,1,1,1,
1,1,1,1,1,1,1,1,1,1,1,1,1,1,1,1,1,1,1,1,1,1,1,1,1,1,1,1,1,1,1,1,1,1,6),
(0.,0.005,0.01,0.015,0.02,0.025,0.03,0.035,0.04,0.045,0.05,0.055,0.06,0.065,
0.07,0.075,0.08,0.085,0.09,0.095,0.1,0.105,0.11,0.115,0.12,0.125,0.13,0.135,
0.14,0.145,0.15,0.155,0.16,0.165,0.17,0.175,0.18,0.185,0.19,0.195,0.2,0.205,
0.21,0.215,0.22,0.225,0.23,0.235,0.24,0.245,0.25,0.255,0.26,0.265,0.27,
0.275,0.28,0.285,0.29,0.295,0.3,0.305,0.31,0.315,0.32,0.325,0.33,0.335,
0.34,0.345,0.35,0.355,0.36,0.365,0.37,0.375,0.38,0.385,0.39,0.395,0.4,0.405,
0.41,0.415,0.42,0.425,0.43,0.435,0.44,0.445,0.45,0.455,0.46,0.465,0.47,
0.475,0.48,0.485,0.49,0.495,0.5,0.505,0.51,0.515,0.52,0.525,0.53,0.535,
0.54,0.545,0.55,0.555,0.56,0.565,0.57,0.575,0.58,0.585,0.59,0.595,0.6,0.605,
0.61,0.615,0.62,0.625,0.63,0.635,0.64,0.645,0.65,0.655,0.66,0.665,0.67,
0.675,0.68,0.685,0.690000000000001,0.695000000000001,0.700000000000001,
0.705000000000001,0.710000000000001,0.715000000000001,0.720000000000001,
0.725000000000001,0.730000000000001,0.735000000000001,0.740000000000001,
0.745000000000001,0.750000000000001,0.755000000000001,0.760000000000001,
0.765000000000001,0.770000000000001,0.775000000000001,0.780000000000001,
0.785000000000001,0.790000000000001,0.795000000000001,0.800000000000001,
0.805000000000001,0.810000000000001,0.815000000000001,0.820000000000001,
0.825000000000001,0.830000000000001,0.835000000000001,0.840000000000001,
0.845000000000001,0.850000000000001,0.855000000000001,0.860000000000001,
0.865000000000001,0.870000000000001,0.875000000000001,0.880000000000001,
0.885000000000001,0.890000000000001,0.895000000000001,0.900000000000001,
0.905000000000001,0.910000000000001,0.915000000000001,0.920000000000001,
0.925000000000001,0.930000000000001,0.935000000000001,0.940000000000001,
0.945000000000001,0.950000000000001,0.955000000000001,0.960000000000001,
0.965000000000001,0.970000000000001,0.975000000000001,0.980000000000001,
0.985000000000001,0.990000000000001,0.995000000000001,1.),.UNSPECIFIED.)
CURVE()
GEOMETRIC_REPRESENTATION_ITEM()
RATIONAL_B_SPLINE_CURVE((1.,1.,1.,1.,1.,1.,1.,1.,1.,1.,1.,1.,1.,1.,1.,1.,
1.,1.,1.,1.,1.,1.,1.,1.,1.,1.,1.,1.,1.,1.,1.,1.,1.,1.,1.,1.,1.,1.,1.,1.,
1.,1.,1.,1.,1.,1.,1.,1.,1.,1.,1.,1.,1.,1.,1.,1.,1.,1.,1.,1.,1.,1.,1.,1.,
1.,1.,1.,1.,1.,1.,1.,1.,1.,1.,1.,1.,1.,1.,1.,1.,1.,1.,1.,1.,1.,1.,1.,1.,
1.,1.,1.,1.,1.,1.,1.,1.,1.,1.,1.,1.,1.,1.,1.,1.,1.,1.,1.,1.,1.,1.,1.,1.,
1.,1.,1.,1.,1.,1.,1.,1.,1.,1.,1.,1.,1.,1.,1.,1.,1.,1.,1.,1.,1.,1.,1.,1.,
1.,1.,1.,1.,1.,1.,1.,1.,1.,1.,1.,1.,1.,1.,1.,1.,1.,1.,1.,1.,1.,1.,1.,1.,
1.,1.,1.,1.,1.,1.,1.,1.,1.,1.,1.,1.,1.,1.,1.,1.,1.,1.,1.,1.,1.,1.,1.,1.,
1.,1.,1.,1.,1.,1.,1.,1.,1.,1.,1.,1.,1.,1.,1.,1.,1.,1.,1.,1.,1.))
REPRESENTATION_ITEM('')
);
#838=(
BOUNDED_CURVE()
B_SPLINE_CURVE(5,(#237272,#237273,#237274,#237275,#237276,#237277,#237278,
#237279,#237280,#237281,#237282,#237283,#237284,#237285,#237286,#237287,
#237288,#237289,#237290,#237291,#237292,#237293,#237294,#237295,#237296,
#237297,#237298,#237299,#237300,#237301,#237302,#237303,#237304,#237305,
#237306,#237307,#237308,#237309,#237310,#237311,#237312,#237313,#237314,
#237315,#237316,#237317,#237318,#237319,#237320,#237321,#237322,#237323,
#237324,#237325,#237326,#237327,#237328,#237329,#237330,#237331,#237332,
#237333,#237334,#237335,#237336,#237337,#237338,#237339,#237340,#237341,
#237342,#237343,#237344,#237345,#237346,#237347,#237348,#237349,#237350,
#237351,#237352,#237353,#237354,#237355,#237356,#237357,#237358,#237359,
#237360,#237361,#237362,#237363,#237364,#237365,#237366,#237367,#237368,
#237369,#237370,#237371,#237372,#237373,#237374,#237375,#237376,#237377,
#237378,#237379,#237380,#237381,#237382,#237383,#237384,#237385,#237386,
#237387,#237388,#237389,#237390,#237391,#237392,#237393,#237394,#237395,
#237396,#237397,#237398,#237399,#237400,#237401,#237402,#237403,#237404,
#237405,#237406,#237407,#237408,#237409,#237410,#237411,#237412,#237413,
#237414,#237415,#237416,#237417,#237418,#237419,#237420,#237421,#237422,
#237423,#237424,#237425,#237426,#237427,#237428,#237429,#237430,#237431,
#237432,#237433,#237434,#237435,#237436,#237437,#237438,#237439,#237440,
#237441,#237442,#237443,#237444,#237445,#237446,#237447,#237448,#237449,
#237450,#237451,#237452,#237453,#237454,#237455,#237456,#237457,#237458,
#237459,#237460,#237461,#237462,#237463,#237464,#237465,#237466,#237467,
#237468,#237469,#237470,#237471,#237472,#237473,#237474,#237475,#237476),
 .UNSPECIFIED.,.F.,.F.)
B_SPLINE_CURVE_WITH_KNOTS((6,1,1,1,1,1,1,1,1,1,1,1,1,1,1,1,1,1,1,1,1,1,
1,1,1,1,1,1,1,1,1,1,1,1,1,1,1,1,1,1,1,1,1,1,1,1,1,1,1,1,1,1,1,1,1,1,1,1,
1,1,1,1,1,1,1,1,1,1,1,1,1,1,1,1,1,1,1,1,1,1,1,1,1,1,1,1,1,1,1,1,1,1,1,1,
1,1,1,1,1,1,1,1,1,1,1,1,1,1,1,1,1,1,1,1,1,1,1,1,1,1,1,1,1,1,1,1,1,1,1,1,
1,1,1,1,1,1,1,1,1,1,1,1,1,1,1,1,1,1,1,1,1,1,1,1,1,1,1,1,1,1,1,1,1,1,1,1,
1,1,1,1,1,1,1,1,1,1,1,1,1,1,1,1,1,1,1,1,1,1,1,1,1,1,1,1,1,1,1,1,1,1,6),
(-1.,-0.995000000000001,-0.990000000000001,-0.985000000000001,-0.980000000000001,
-0.975000000000001,-0.970000000000001,-0.965000000000001,-0.960000000000001,
-0.955000000000001,-0.950000000000001,-0.945000000000001,-0.940000000000001,
-0.935000000000001,-0.930000000000001,-0.925000000000001,-0.920000000000001,
-0.915000000000001,-0.910000000000001,-0.905000000000001,-0.900000000000001,
-0.895000000000001,-0.890000000000001,-0.885000000000001,-0.880000000000001,
-0.875000000000001,-0.870000000000001,-0.865000000000001,-0.860000000000001,
-0.855000000000001,-0.850000000000001,-0.845000000000001,-0.840000000000001,
-0.835000000000001,-0.830000000000001,-0.825000000000001,-0.820000000000001,
-0.815000000000001,-0.810000000000001,-0.805000000000001,-0.800000000000001,
-0.795000000000001,-0.790000000000001,-0.785000000000001,-0.780000000000001,
-0.775000000000001,-0.770000000000001,-0.765000000000001,-0.760000000000001,
-0.755000000000001,-0.750000000000001,-0.745000000000001,-0.740000000000001,
-0.735000000000001,-0.730000000000001,-0.725000000000001,-0.720000000000001,
-0.715000000000001,-0.710000000000001,-0.705000000000001,-0.700000000000001,
-0.695000000000001,-0.690000000000001,-0.685,-0.68,-0.675,-0.67,-0.665,
-0.66,-0.655,-0.65,-0.645,-0.64,-0.635,-0.63,-0.625,-0.62,-0.615,-0.61,
-0.605,-0.6,-0.595,-0.59,-0.585,-0.58,-0.575,-0.57,-0.565,-0.56,-0.555,
-0.55,-0.545,-0.54,-0.535,-0.53,-0.525,-0.52,-0.515,-0.51,-0.505,-0.5,-0.495,
-0.49,-0.485,-0.48,-0.475,-0.47,-0.465,-0.46,-0.455,-0.45,-0.445,-0.44,
-0.435,-0.43,-0.425,-0.42,-0.415,-0.41,-0.405,-0.4,-0.395,-0.39,-0.385,
-0.38,-0.375,-0.37,-0.365,-0.36,-0.355,-0.35,-0.345,-0.34,-0.335,-0.33,
-0.325,-0.32,-0.315,-0.31,-0.305,-0.3,-0.295,-0.29,-0.285,-0.28,-0.275,
-0.27,-0.265,-0.26,-0.255,-0.25,-0.245,-0.24,-0.235,-0.23,-0.225,-0.22,
-0.215,-0.21,-0.205,-0.2,-0.195,-0.19,-0.185,-0.18,-0.175,-0.17,-0.165,
-0.16,-0.155,-0.15,-0.145,-0.14,-0.135,-0.13,-0.125,-0.12,-0.115,-0.11,
-0.105,-0.1,-0.095,-0.09,-0.085,-0.08,-0.075,-0.07,-0.065,-0.06,-0.055,
-0.05,-0.045,-0.04,-0.035,-0.03,-0.025,-0.02,-0.015,-0.01,-0.005,0.),
 .UNSPECIFIED.)
CURVE()
GEOMETRIC_REPRESENTATION_ITEM()
RATIONAL_B_SPLINE_CURVE((1.,1.,1.,1.,1.,1.,1.,1.,1.,1.,1.,1.,1.,1.,1.,1.,
1.,1.,1.,1.,1.,1.,1.,1.,1.,1.,1.,1.,1.,1.,1.,1.,1.,1.,1.,1.,1.,1.,1.,1.,
1.,1.,1.,1.,1.,1.,1.,1.,1.,1.,1.,1.,1.,1.,1.,1.,1.,1.,1.,1.,1.,1.,1.,1.,
1.,1.,1.,1.,1.,1.,1.,1.,1.,1.,1.,1.,1.,1.,1.,1.,1.,1.,1.,1.,1.,1.,1.,1.,
1.,1.,1.,1.,1.,1.,1.,1.,1.,1.,1.,1.,1.,1.,1.,1.,1.,1.,1.,1.,1.,1.,1.,1.,
1.,1.,1.,1.,1.,1.,1.,1.,1.,1.,1.,1.,1.,1.,1.,1.,1.,1.,1.,1.,1.,1.,1.,1.,
1.,1.,1.,1.,1.,1.,1.,1.,1.,1.,1.,1.,1.,1.,1.,1.,1.,1.,1.,1.,1.,1.,1.,1.,
1.,1.,1.,1.,1.,1.,1.,1.,1.,1.,1.,1.,1.,1.,1.,1.,1.,1.,1.,1.,1.,1.,1.,1.,
1.,1.,1.,1.,1.,1.,1.,1.,1.,1.,1.,1.,1.,1.,1.,1.,1.,1.,1.,1.,1.))
REPRESENTATION_ITEM('')
);
#839=(
BOUNDED_CURVE()
B_SPLINE_CURVE(5,(#237895,#237896,#237897,#237898,#237899,#237900,#237901,
#237902,#237903,#237904,#237905,#237906,#237907,#237908,#237909,#237910,
#237911,#237912,#237913,#237914,#237915,#237916,#237917,#237918,#237919,
#237920,#237921,#237922,#237923,#237924,#237925,#237926,#237927,#237928,
#237929,#237930,#237931,#237932,#237933,#237934,#237935,#237936,#237937,
#237938,#237939,#237940,#237941,#237942,#237943,#237944,#237945,#237946,
#237947,#237948,#237949,#237950,#237951,#237952,#237953,#237954,#237955,
#237956,#237957,#237958,#237959,#237960,#237961,#237962,#237963,#237964,
#237965,#237966,#237967,#237968,#237969,#237970,#237971,#237972,#237973,
#237974,#237975,#237976,#237977,#237978,#237979,#237980,#237981,#237982,
#237983,#237984,#237985,#237986,#237987,#237988,#237989,#237990,#237991,
#237992,#237993,#237994,#237995,#237996,#237997,#237998,#237999,#238000,
#238001,#238002,#238003,#238004,#238005,#238006,#238007,#238008,#238009,
#238010,#238011,#238012,#238013,#238014,#238015,#238016,#238017,#238018,
#238019,#238020,#238021,#238022,#238023,#238024,#238025,#238026,#238027,
#238028,#238029,#238030,#238031,#238032,#238033,#238034,#238035,#238036,
#238037,#238038,#238039,#238040,#238041,#238042,#238043,#238044,#238045,
#238046,#238047,#238048,#238049,#238050,#238051,#238052,#238053,#238054,
#238055,#238056,#238057,#238058,#238059,#238060,#238061,#238062,#238063,
#238064,#238065,#238066,#238067,#238068,#238069,#238070,#238071,#238072,
#238073,#238074,#238075,#238076,#238077,#238078,#238079,#238080,#238081,
#238082,#238083,#238084,#238085,#238086,#238087,#238088,#238089,#238090,
#238091,#238092,#238093,#238094,#238095,#238096,#238097,#238098,#238099),
 .UNSPECIFIED.,.F.,.F.)
B_SPLINE_CURVE_WITH_KNOTS((6,1,1,1,1,1,1,1,1,1,1,1,1,1,1,1,1,1,1,1,1,1,
1,1,1,1,1,1,1,1,1,1,1,1,1,1,1,1,1,1,1,1,1,1,1,1,1,1,1,1,1,1,1,1,1,1,1,1,
1,1,1,1,1,1,1,1,1,1,1,1,1,1,1,1,1,1,1,1,1,1,1,1,1,1,1,1,1,1,1,1,1,1,1,1,
1,1,1,1,1,1,1,1,1,1,1,1,1,1,1,1,1,1,1,1,1,1,1,1,1,1,1,1,1,1,1,1,1,1,1,1,
1,1,1,1,1,1,1,1,1,1,1,1,1,1,1,1,1,1,1,1,1,1,1,1,1,1,1,1,1,1,1,1,1,1,1,1,
1,1,1,1,1,1,1,1,1,1,1,1,1,1,1,1,1,1,1,1,1,1,1,1,1,1,1,1,1,1,1,1,1,1,6),
(-1.,-0.995000000000001,-0.990000000000001,-0.985000000000001,-0.980000000000001,
-0.975000000000001,-0.970000000000001,-0.965000000000001,-0.960000000000001,
-0.955000000000001,-0.950000000000001,-0.945000000000001,-0.940000000000001,
-0.935000000000001,-0.930000000000001,-0.925000000000001,-0.920000000000001,
-0.915000000000001,-0.910000000000001,-0.905000000000001,-0.900000000000001,
-0.895000000000001,-0.890000000000001,-0.885000000000001,-0.880000000000001,
-0.875000000000001,-0.870000000000001,-0.865000000000001,-0.860000000000001,
-0.855000000000001,-0.850000000000001,-0.845000000000001,-0.840000000000001,
-0.835000000000001,-0.830000000000001,-0.825000000000001,-0.820000000000001,
-0.815000000000001,-0.810000000000001,-0.805000000000001,-0.800000000000001,
-0.795000000000001,-0.790000000000001,-0.785000000000001,-0.780000000000001,
-0.775000000000001,-0.770000000000001,-0.765000000000001,-0.760000000000001,
-0.755000000000001,-0.750000000000001,-0.745000000000001,-0.740000000000001,
-0.735000000000001,-0.730000000000001,-0.725000000000001,-0.720000000000001,
-0.715000000000001,-0.710000000000001,-0.705000000000001,-0.700000000000001,
-0.695000000000001,-0.690000000000001,-0.685,-0.68,-0.675,-0.67,-0.665,
-0.66,-0.655,-0.65,-0.645,-0.64,-0.635,-0.63,-0.625,-0.62,-0.615,-0.61,
-0.605,-0.6,-0.595,-0.59,-0.585,-0.58,-0.575,-0.57,-0.565,-0.56,-0.555,
-0.55,-0.545,-0.54,-0.535,-0.53,-0.525,-0.52,-0.515,-0.51,-0.505,-0.5,-0.495,
-0.49,-0.485,-0.48,-0.475,-0.47,-0.465,-0.46,-0.455,-0.45,-0.445,-0.44,
-0.435,-0.43,-0.425,-0.42,-0.415,-0.41,-0.405,-0.4,-0.395,-0.39,-0.385,
-0.38,-0.375,-0.37,-0.365,-0.36,-0.355,-0.35,-0.345,-0.34,-0.335,-0.33,
-0.325,-0.32,-0.315,-0.31,-0.305,-0.3,-0.295,-0.29,-0.285,-0.28,-0.275,
-0.27,-0.265,-0.26,-0.255,-0.25,-0.245,-0.24,-0.235,-0.23,-0.225,-0.22,
-0.215,-0.21,-0.205,-0.2,-0.195,-0.19,-0.185,-0.18,-0.175,-0.17,-0.165,
-0.16,-0.155,-0.15,-0.145,-0.14,-0.135,-0.13,-0.125,-0.12,-0.115,-0.11,
-0.105,-0.1,-0.095,-0.09,-0.085,-0.08,-0.075,-0.07,-0.065,-0.06,-0.055,
-0.05,-0.045,-0.04,-0.035,-0.03,-0.025,-0.02,-0.015,-0.01,-0.005,0.),
 .UNSPECIFIED.)
CURVE()
GEOMETRIC_REPRESENTATION_ITEM()
RATIONAL_B_SPLINE_CURVE((1.,1.,1.,1.,1.,1.,1.,1.,1.,1.,1.,1.,1.,1.,1.,1.,
1.,1.,1.,1.,1.,1.,1.,1.,1.,1.,1.,1.,1.,1.,1.,1.,1.,1.,1.,1.,1.,1.,1.,1.,
1.,1.,1.,1.,1.,1.,1.,1.,1.,1.,1.,1.,1.,1.,1.,1.,1.,1.,1.,1.,1.,1.,1.,1.,
1.,1.,1.,1.,1.,1.,1.,1.,1.,1.,1.,1.,1.,1.,1.,1.,1.,1.,1.,1.,1.,1.,1.,1.,
1.,1.,1.,1.,1.,1.,1.,1.,1.,1.,1.,1.,1.,1.,1.,1.,1.,1.,1.,1.,1.,1.,1.,1.,
1.,1.,1.,1.,1.,1.,1.,1.,1.,1.,1.,1.,1.,1.,1.,1.,1.,1.,1.,1.,1.,1.,1.,1.,
1.,1.,1.,1.,1.,1.,1.,1.,1.,1.,1.,1.,1.,1.,1.,1.,1.,1.,1.,1.,1.,1.,1.,1.,
1.,1.,1.,1.,1.,1.,1.,1.,1.,1.,1.,1.,1.,1.,1.,1.,1.,1.,1.,1.,1.,1.,1.,1.,
1.,1.,1.,1.,1.,1.,1.,1.,1.,1.,1.,1.,1.,1.,1.,1.,1.,1.,1.,1.,1.))
REPRESENTATION_ITEM('')
);
#840=(
BOUNDED_CURVE()
B_SPLINE_CURVE(5,(#238102,#238103,#238104,#238105,#238106,#238107,#238108,
#238109,#238110,#238111,#238112,#238113,#238114,#238115,#238116,#238117,
#238118,#238119,#238120,#238121,#238122,#238123,#238124,#238125,#238126,
#238127,#238128,#238129,#238130,#238131,#238132,#238133,#238134,#238135,
#238136,#238137,#238138,#238139,#238140,#238141,#238142,#238143,#238144,
#238145,#238146,#238147,#238148,#238149,#238150,#238151,#238152,#238153,
#238154,#238155,#238156,#238157,#238158,#238159,#238160,#238161,#238162,
#238163,#238164,#238165,#238166,#238167,#238168,#238169,#238170,#238171,
#238172,#238173,#238174,#238175,#238176,#238177,#238178,#238179,#238180,
#238181,#238182,#238183,#238184,#238185,#238186,#238187,#238188,#238189,
#238190,#238191,#238192,#238193,#238194,#238195,#238196,#238197,#238198,
#238199,#238200,#238201,#238202,#238203,#238204,#238205,#238206,#238207,
#238208,#238209,#238210,#238211,#238212,#238213,#238214,#238215,#238216,
#238217,#238218,#238219,#238220,#238221,#238222,#238223,#238224,#238225,
#238226,#238227,#238228,#238229,#238230,#238231,#238232,#238233,#238234,
#238235,#238236,#238237,#238238,#238239,#238240,#238241,#238242,#238243,
#238244,#238245,#238246,#238247,#238248,#238249,#238250,#238251,#238252,
#238253,#238254,#238255,#238256,#238257,#238258,#238259,#238260,#238261,
#238262,#238263,#238264,#238265,#238266,#238267,#238268,#238269,#238270,
#238271,#238272,#238273,#238274,#238275,#238276,#238277,#238278,#238279,
#238280,#238281,#238282,#238283,#238284,#238285,#238286,#238287,#238288,
#238289,#238290,#238291,#238292,#238293,#238294,#238295,#238296,#238297,
#238298,#238299,#238300,#238301,#238302,#238303,#238304,#238305,#238306),
 .UNSPECIFIED.,.F.,.F.)
B_SPLINE_CURVE_WITH_KNOTS((6,1,1,1,1,1,1,1,1,1,1,1,1,1,1,1,1,1,1,1,1,1,
1,1,1,1,1,1,1,1,1,1,1,1,1,1,1,1,1,1,1,1,1,1,1,1,1,1,1,1,1,1,1,1,1,1,1,1,
1,1,1,1,1,1,1,1,1,1,1,1,1,1,1,1,1,1,1,1,1,1,1,1,1,1,1,1,1,1,1,1,1,1,1,1,
1,1,1,1,1,1,1,1,1,1,1,1,1,1,1,1,1,1,1,1,1,1,1,1,1,1,1,1,1,1,1,1,1,1,1,1,
1,1,1,1,1,1,1,1,1,1,1,1,1,1,1,1,1,1,1,1,1,1,1,1,1,1,1,1,1,1,1,1,1,1,1,1,
1,1,1,1,1,1,1,1,1,1,1,1,1,1,1,1,1,1,1,1,1,1,1,1,1,1,1,1,1,1,1,1,1,1,6),
(0.,0.005,0.01,0.015,0.02,0.025,0.03,0.035,0.04,0.045,0.05,0.055,0.06,0.065,
0.07,0.075,0.08,0.085,0.09,0.095,0.1,0.105,0.11,0.115,0.12,0.125,0.13,0.135,
0.14,0.145,0.15,0.155,0.16,0.165,0.17,0.175,0.18,0.185,0.19,0.195,0.2,0.205,
0.21,0.215,0.22,0.225,0.23,0.235,0.24,0.245,0.25,0.255,0.26,0.265,0.27,
0.275,0.28,0.285,0.29,0.295,0.3,0.305,0.31,0.315,0.32,0.325,0.33,0.335,
0.34,0.345,0.35,0.355,0.36,0.365,0.37,0.375,0.38,0.385,0.39,0.395,0.4,0.405,
0.41,0.415,0.42,0.425,0.43,0.435,0.44,0.445,0.45,0.455,0.46,0.465,0.47,
0.475,0.48,0.485,0.49,0.495,0.5,0.505,0.51,0.515,0.52,0.525,0.53,0.535,
0.54,0.545,0.55,0.555,0.56,0.565,0.57,0.575,0.58,0.585,0.59,0.595,0.6,0.605,
0.61,0.615,0.62,0.625,0.63,0.635,0.64,0.645,0.65,0.655,0.66,0.665,0.67,
0.675,0.68,0.685,0.690000000000001,0.695000000000001,0.700000000000001,
0.705000000000001,0.710000000000001,0.715000000000001,0.720000000000001,
0.725000000000001,0.730000000000001,0.735000000000001,0.740000000000001,
0.745000000000001,0.750000000000001,0.755000000000001,0.760000000000001,
0.765000000000001,0.770000000000001,0.775000000000001,0.780000000000001,
0.785000000000001,0.790000000000001,0.795000000000001,0.800000000000001,
0.805000000000001,0.810000000000001,0.815000000000001,0.820000000000001,
0.825000000000001,0.830000000000001,0.835000000000001,0.840000000000001,
0.845000000000001,0.850000000000001,0.855000000000001,0.860000000000001,
0.865000000000001,0.870000000000001,0.875000000000001,0.880000000000001,
0.885000000000001,0.890000000000001,0.895000000000001,0.900000000000001,
0.905000000000001,0.910000000000001,0.915000000000001,0.920000000000001,
0.925000000000001,0.930000000000001,0.935000000000001,0.940000000000001,
0.945000000000001,0.950000000000001,0.955000000000001,0.960000000000001,
0.965000000000001,0.970000000000001,0.975000000000001,0.980000000000001,
0.985000000000001,0.990000000000001,0.995000000000001,1.),.UNSPECIFIED.)
CURVE()
GEOMETRIC_REPRESENTATION_ITEM()
RATIONAL_B_SPLINE_CURVE((1.,1.,1.,1.,1.,1.,1.,1.,1.,1.,1.,1.,1.,1.,1.,1.,
1.,1.,1.,1.,1.,1.,1.,1.,1.,1.,1.,1.,1.,1.,1.,1.,1.,1.,1.,1.,1.,1.,1.,1.,
1.,1.,1.,1.,1.,1.,1.,1.,1.,1.,1.,1.,1.,1.,1.,1.,1.,1.,1.,1.,1.,1.,1.,1.,
1.,1.,1.,1.,1.,1.,1.,1.,1.,1.,1.,1.,1.,1.,1.,1.,1.,1.,1.,1.,1.,1.,1.,1.,
1.,1.,1.,1.,1.,1.,1.,1.,1.,1.,1.,1.,1.,1.,1.,1.,1.,1.,1.,1.,1.,1.,1.,1.,
1.,1.,1.,1.,1.,1.,1.,1.,1.,1.,1.,1.,1.,1.,1.,1.,1.,1.,1.,1.,1.,1.,1.,1.,
1.,1.,1.,1.,1.,1.,1.,1.,1.,1.,1.,1.,1.,1.,1.,1.,1.,1.,1.,1.,1.,1.,1.,1.,
1.,1.,1.,1.,1.,1.,1.,1.,1.,1.,1.,1.,1.,1.,1.,1.,1.,1.,1.,1.,1.,1.,1.,1.,
1.,1.,1.,1.,1.,1.,1.,1.,1.,1.,1.,1.,1.,1.,1.,1.,1.,1.,1.,1.,1.))
REPRESENTATION_ITEM('')
);
#841=(
BOUNDED_CURVE()
B_SPLINE_CURVE(5,(#238718,#238719,#238720,#238721,#238722,#238723,#238724,
#238725,#238726,#238727,#238728,#238729,#238730,#238731,#238732,#238733,
#238734,#238735,#238736,#238737,#238738,#238739,#238740,#238741,#238742,
#238743,#238744,#238745,#238746,#238747,#238748,#238749,#238750,#238751,
#238752,#238753,#238754,#238755,#238756,#238757,#238758,#238759,#238760,
#238761,#238762,#238763,#238764,#238765,#238766,#238767,#238768,#238769,
#238770,#238771,#238772,#238773,#238774,#238775,#238776,#238777,#238778,
#238779,#238780,#238781,#238782,#238783,#238784,#238785,#238786,#238787,
#238788,#238789,#238790,#238791,#238792,#238793,#238794,#238795,#238796,
#238797,#238798,#238799,#238800,#238801,#238802,#238803,#238804,#238805,
#238806,#238807,#238808,#238809,#238810,#238811,#238812,#238813,#238814,
#238815,#238816,#238817,#238818,#238819,#238820,#238821,#238822,#238823,
#238824,#238825,#238826,#238827,#238828,#238829,#238830,#238831,#238832,
#238833,#238834,#238835,#238836,#238837,#238838,#238839,#238840,#238841,
#238842,#238843,#238844,#238845,#238846,#238847,#238848,#238849,#238850,
#238851,#238852,#238853,#238854,#238855,#238856,#238857,#238858,#238859,
#238860,#238861,#238862,#238863,#238864,#238865,#238866,#238867,#238868,
#238869,#238870,#238871,#238872,#238873,#238874,#238875,#238876,#238877,
#238878,#238879,#238880,#238881,#238882,#238883,#238884,#238885,#238886,
#238887,#238888,#238889,#238890,#238891,#238892,#238893,#238894,#238895,
#238896,#238897,#238898,#238899,#238900,#238901,#238902,#238903,#238904,
#238905,#238906,#238907,#238908,#238909,#238910,#238911,#238912,#238913,
#238914,#238915,#238916,#238917,#238918,#238919,#238920,#238921,#238922),
 .UNSPECIFIED.,.F.,.F.)
B_SPLINE_CURVE_WITH_KNOTS((6,1,1,1,1,1,1,1,1,1,1,1,1,1,1,1,1,1,1,1,1,1,
1,1,1,1,1,1,1,1,1,1,1,1,1,1,1,1,1,1,1,1,1,1,1,1,1,1,1,1,1,1,1,1,1,1,1,1,
1,1,1,1,1,1,1,1,1,1,1,1,1,1,1,1,1,1,1,1,1,1,1,1,1,1,1,1,1,1,1,1,1,1,1,1,
1,1,1,1,1,1,1,1,1,1,1,1,1,1,1,1,1,1,1,1,1,1,1,1,1,1,1,1,1,1,1,1,1,1,1,1,
1,1,1,1,1,1,1,1,1,1,1,1,1,1,1,1,1,1,1,1,1,1,1,1,1,1,1,1,1,1,1,1,1,1,1,1,
1,1,1,1,1,1,1,1,1,1,1,1,1,1,1,1,1,1,1,1,1,1,1,1,1,1,1,1,1,1,1,1,1,1,6),
(0.,0.005,0.01,0.015,0.02,0.025,0.03,0.035,0.04,0.045,0.05,0.055,0.06,0.065,
0.07,0.075,0.08,0.085,0.09,0.095,0.1,0.105,0.11,0.115,0.12,0.125,0.13,0.135,
0.14,0.145,0.15,0.155,0.16,0.165,0.17,0.175,0.18,0.185,0.19,0.195,0.2,0.205,
0.21,0.215,0.22,0.225,0.23,0.235,0.24,0.245,0.25,0.255,0.26,0.265,0.27,
0.275,0.28,0.285,0.29,0.295,0.3,0.305,0.31,0.315,0.32,0.325,0.33,0.335,
0.34,0.345,0.35,0.355,0.36,0.365,0.37,0.375,0.38,0.385,0.39,0.395,0.4,0.405,
0.41,0.415,0.42,0.425,0.43,0.435,0.44,0.445,0.45,0.455,0.46,0.465,0.47,
0.475,0.48,0.485,0.49,0.495,0.5,0.505,0.51,0.515,0.52,0.525,0.53,0.535,
0.54,0.545,0.55,0.555,0.56,0.565,0.57,0.575,0.58,0.585,0.59,0.595,0.6,0.605,
0.61,0.615,0.62,0.625,0.63,0.635,0.64,0.645,0.65,0.655,0.66,0.665,0.67,
0.675,0.68,0.685,0.690000000000001,0.695000000000001,0.700000000000001,
0.705000000000001,0.710000000000001,0.715000000000001,0.720000000000001,
0.725000000000001,0.730000000000001,0.735000000000001,0.740000000000001,
0.745000000000001,0.750000000000001,0.755000000000001,0.760000000000001,
0.765000000000001,0.770000000000001,0.775000000000001,0.780000000000001,
0.785000000000001,0.790000000000001,0.795000000000001,0.800000000000001,
0.805000000000001,0.810000000000001,0.815000000000001,0.820000000000001,
0.825000000000001,0.830000000000001,0.835000000000001,0.840000000000001,
0.845000000000001,0.850000000000001,0.855000000000001,0.860000000000001,
0.865000000000001,0.870000000000001,0.875000000000001,0.880000000000001,
0.885000000000001,0.890000000000001,0.895000000000001,0.900000000000001,
0.905000000000001,0.910000000000001,0.915000000000001,0.920000000000001,
0.925000000000001,0.930000000000001,0.935000000000001,0.940000000000001,
0.945000000000001,0.950000000000001,0.955000000000001,0.960000000000001,
0.965000000000001,0.970000000000001,0.975000000000001,0.980000000000001,
0.985000000000001,0.990000000000001,0.995000000000001,1.),.UNSPECIFIED.)
CURVE()
GEOMETRIC_REPRESENTATION_ITEM()
RATIONAL_B_SPLINE_CURVE((1.,1.,1.,1.,1.,1.,1.,1.,1.,1.,1.,1.,1.,1.,1.,1.,
1.,1.,1.,1.,1.,1.,1.,1.,1.,1.,1.,1.,1.,1.,1.,1.,1.,1.,1.,1.,1.,1.,1.,1.,
1.,1.,1.,1.,1.,1.,1.,1.,1.,1.,1.,1.,1.,1.,1.,1.,1.,1.,1.,1.,1.,1.,1.,1.,
1.,1.,1.,1.,1.,1.,1.,1.,1.,1.,1.,1.,1.,1.,1.,1.,1.,1.,1.,1.,1.,1.,1.,1.,
1.,1.,1.,1.,1.,1.,1.,1.,1.,1.,1.,1.,1.,1.,1.,1.,1.,1.,1.,1.,1.,1.,1.,1.,
1.,1.,1.,1.,1.,1.,1.,1.,1.,1.,1.,1.,1.,1.,1.,1.,1.,1.,1.,1.,1.,1.,1.,1.,
1.,1.,1.,1.,1.,1.,1.,1.,1.,1.,1.,1.,1.,1.,1.,1.,1.,1.,1.,1.,1.,1.,1.,1.,
1.,1.,1.,1.,1.,1.,1.,1.,1.,1.,1.,1.,1.,1.,1.,1.,1.,1.,1.,1.,1.,1.,1.,1.,
1.,1.,1.,1.,1.,1.,1.,1.,1.,1.,1.,1.,1.,1.,1.,1.,1.,1.,1.,1.,1.))
REPRESENTATION_ITEM('')
);
#842=(
BOUNDED_CURVE()
B_SPLINE_CURVE(5,(#238924,#238925,#238926,#238927,#238928,#238929,#238930,
#238931,#238932,#238933,#238934,#238935,#238936,#238937,#238938,#238939,
#238940,#238941,#238942,#238943,#238944,#238945,#238946,#238947,#238948,
#238949,#238950,#238951,#238952,#238953,#238954,#238955,#238956,#238957,
#238958,#238959,#238960,#238961,#238962,#238963,#238964,#238965,#238966,
#238967,#238968,#238969,#238970,#238971,#238972,#238973,#238974,#238975,
#238976,#238977,#238978,#238979,#238980,#238981,#238982,#238983,#238984,
#238985,#238986,#238987,#238988,#238989,#238990,#238991,#238992,#238993,
#238994,#238995,#238996,#238997,#238998,#238999,#239000,#239001,#239002,
#239003,#239004,#239005,#239006,#239007,#239008,#239009,#239010,#239011,
#239012,#239013,#239014,#239015,#239016,#239017,#239018,#239019,#239020,
#239021,#239022,#239023,#239024,#239025,#239026,#239027,#239028,#239029,
#239030,#239031,#239032,#239033,#239034,#239035,#239036,#239037,#239038,
#239039,#239040,#239041,#239042,#239043,#239044,#239045,#239046,#239047,
#239048,#239049,#239050,#239051,#239052,#239053,#239054,#239055,#239056,
#239057,#239058,#239059,#239060,#239061,#239062,#239063,#239064,#239065,
#239066,#239067,#239068,#239069,#239070,#239071,#239072,#239073,#239074,
#239075,#239076,#239077,#239078,#239079,#239080,#239081,#239082,#239083,
#239084,#239085,#239086,#239087,#239088,#239089,#239090,#239091,#239092,
#239093,#239094,#239095,#239096,#239097,#239098,#239099,#239100,#239101,
#239102,#239103,#239104,#239105,#239106,#239107,#239108,#239109,#239110,
#239111,#239112,#239113,#239114,#239115,#239116,#239117,#239118,#239119,
#239120,#239121,#239122,#239123,#239124,#239125,#239126,#239127,#239128),
 .UNSPECIFIED.,.F.,.F.)
B_SPLINE_CURVE_WITH_KNOTS((6,1,1,1,1,1,1,1,1,1,1,1,1,1,1,1,1,1,1,1,1,1,
1,1,1,1,1,1,1,1,1,1,1,1,1,1,1,1,1,1,1,1,1,1,1,1,1,1,1,1,1,1,1,1,1,1,1,1,
1,1,1,1,1,1,1,1,1,1,1,1,1,1,1,1,1,1,1,1,1,1,1,1,1,1,1,1,1,1,1,1,1,1,1,1,
1,1,1,1,1,1,1,1,1,1,1,1,1,1,1,1,1,1,1,1,1,1,1,1,1,1,1,1,1,1,1,1,1,1,1,1,
1,1,1,1,1,1,1,1,1,1,1,1,1,1,1,1,1,1,1,1,1,1,1,1,1,1,1,1,1,1,1,1,1,1,1,1,
1,1,1,1,1,1,1,1,1,1,1,1,1,1,1,1,1,1,1,1,1,1,1,1,1,1,1,1,1,1,1,1,1,1,6),
(-1.,-0.995000000000001,-0.990000000000001,-0.985000000000001,-0.980000000000001,
-0.975000000000001,-0.970000000000001,-0.965000000000001,-0.960000000000001,
-0.955000000000001,-0.950000000000001,-0.945000000000001,-0.940000000000001,
-0.935000000000001,-0.930000000000001,-0.925000000000001,-0.920000000000001,
-0.915000000000001,-0.910000000000001,-0.905000000000001,-0.900000000000001,
-0.895000000000001,-0.890000000000001,-0.885000000000001,-0.880000000000001,
-0.875000000000001,-0.870000000000001,-0.865000000000001,-0.860000000000001,
-0.855000000000001,-0.850000000000001,-0.845000000000001,-0.840000000000001,
-0.835000000000001,-0.830000000000001,-0.825000000000001,-0.820000000000001,
-0.815000000000001,-0.810000000000001,-0.805000000000001,-0.800000000000001,
-0.795000000000001,-0.790000000000001,-0.785000000000001,-0.780000000000001,
-0.775000000000001,-0.770000000000001,-0.765000000000001,-0.760000000000001,
-0.755000000000001,-0.750000000000001,-0.745000000000001,-0.740000000000001,
-0.735000000000001,-0.730000000000001,-0.725000000000001,-0.720000000000001,
-0.715000000000001,-0.710000000000001,-0.705000000000001,-0.700000000000001,
-0.695000000000001,-0.690000000000001,-0.685,-0.68,-0.675,-0.67,-0.665,
-0.66,-0.655,-0.65,-0.645,-0.64,-0.635,-0.63,-0.625,-0.62,-0.615,-0.61,
-0.605,-0.6,-0.595,-0.59,-0.585,-0.58,-0.575,-0.57,-0.565,-0.56,-0.555,
-0.55,-0.545,-0.54,-0.535,-0.53,-0.525,-0.52,-0.515,-0.51,-0.505,-0.5,-0.495,
-0.49,-0.485,-0.48,-0.475,-0.47,-0.465,-0.46,-0.455,-0.45,-0.445,-0.44,
-0.435,-0.43,-0.425,-0.42,-0.415,-0.41,-0.405,-0.4,-0.395,-0.39,-0.385,
-0.38,-0.375,-0.37,-0.365,-0.36,-0.355,-0.35,-0.345,-0.34,-0.335,-0.33,
-0.325,-0.32,-0.315,-0.31,-0.305,-0.3,-0.295,-0.29,-0.285,-0.28,-0.275,
-0.27,-0.265,-0.26,-0.255,-0.25,-0.245,-0.24,-0.235,-0.23,-0.225,-0.22,
-0.215,-0.21,-0.205,-0.2,-0.195,-0.19,-0.185,-0.18,-0.175,-0.17,-0.165,
-0.16,-0.155,-0.15,-0.145,-0.14,-0.135,-0.13,-0.125,-0.12,-0.115,-0.11,
-0.105,-0.1,-0.095,-0.09,-0.085,-0.08,-0.075,-0.07,-0.065,-0.06,-0.055,
-0.05,-0.045,-0.04,-0.035,-0.03,-0.025,-0.02,-0.015,-0.01,-0.005,0.),
 .UNSPECIFIED.)
CURVE()
GEOMETRIC_REPRESENTATION_ITEM()
RATIONAL_B_SPLINE_CURVE((1.,1.,1.,1.,1.,1.,1.,1.,1.,1.,1.,1.,1.,1.,1.,1.,
1.,1.,1.,1.,1.,1.,1.,1.,1.,1.,1.,1.,1.,1.,1.,1.,1.,1.,1.,1.,1.,1.,1.,1.,
1.,1.,1.,1.,1.,1.,1.,1.,1.,1.,1.,1.,1.,1.,1.,1.,1.,1.,1.,1.,1.,1.,1.,1.,
1.,1.,1.,1.,1.,1.,1.,1.,1.,1.,1.,1.,1.,1.,1.,1.,1.,1.,1.,1.,1.,1.,1.,1.,
1.,1.,1.,1.,1.,1.,1.,1.,1.,1.,1.,1.,1.,1.,1.,1.,1.,1.,1.,1.,1.,1.,1.,1.,
1.,1.,1.,1.,1.,1.,1.,1.,1.,1.,1.,1.,1.,1.,1.,1.,1.,1.,1.,1.,1.,1.,1.,1.,
1.,1.,1.,1.,1.,1.,1.,1.,1.,1.,1.,1.,1.,1.,1.,1.,1.,1.,1.,1.,1.,1.,1.,1.,
1.,1.,1.,1.,1.,1.,1.,1.,1.,1.,1.,1.,1.,1.,1.,1.,1.,1.,1.,1.,1.,1.,1.,1.,
1.,1.,1.,1.,1.,1.,1.,1.,1.,1.,1.,1.,1.,1.,1.,1.,1.,1.,1.,1.,1.))
REPRESENTATION_ITEM('')
);
#843=(
BOUNDED_CURVE()
B_SPLINE_CURVE(5,(#239547,#239548,#239549,#239550,#239551,#239552,#239553,
#239554,#239555,#239556,#239557,#239558,#239559,#239560,#239561,#239562,
#239563,#239564,#239565,#239566,#239567,#239568,#239569,#239570,#239571,
#239572,#239573,#239574,#239575,#239576,#239577,#239578,#239579,#239580,
#239581,#239582,#239583,#239584,#239585,#239586,#239587,#239588,#239589,
#239590,#239591,#239592,#239593,#239594,#239595,#239596,#239597,#239598,
#239599,#239600,#239601,#239602,#239603,#239604,#239605,#239606,#239607,
#239608,#239609,#239610,#239611,#239612,#239613,#239614,#239615,#239616,
#239617,#239618,#239619,#239620,#239621,#239622,#239623,#239624,#239625,
#239626,#239627,#239628,#239629,#239630,#239631,#239632,#239633,#239634,
#239635,#239636,#239637,#239638,#239639,#239640,#239641,#239642,#239643,
#239644,#239645,#239646,#239647,#239648,#239649,#239650,#239651,#239652,
#239653,#239654,#239655,#239656,#239657,#239658,#239659,#239660,#239661,
#239662,#239663,#239664,#239665,#239666,#239667,#239668,#239669,#239670,
#239671,#239672,#239673,#239674,#239675,#239676,#239677,#239678,#239679,
#239680,#239681,#239682,#239683,#239684,#239685,#239686,#239687,#239688,
#239689,#239690,#239691,#239692,#239693,#239694,#239695,#239696,#239697,
#239698,#239699,#239700,#239701,#239702,#239703,#239704,#239705,#239706,
#239707,#239708,#239709,#239710,#239711,#239712,#239713,#239714,#239715,
#239716,#239717,#239718,#239719,#239720,#239721,#239722,#239723,#239724,
#239725,#239726,#239727,#239728,#239729,#239730,#239731,#239732,#239733,
#239734,#239735,#239736,#239737,#239738,#239739,#239740,#239741,#239742,
#239743,#239744,#239745,#239746,#239747,#239748,#239749,#239750,#239751),
 .UNSPECIFIED.,.F.,.F.)
B_SPLINE_CURVE_WITH_KNOTS((6,1,1,1,1,1,1,1,1,1,1,1,1,1,1,1,1,1,1,1,1,1,
1,1,1,1,1,1,1,1,1,1,1,1,1,1,1,1,1,1,1,1,1,1,1,1,1,1,1,1,1,1,1,1,1,1,1,1,
1,1,1,1,1,1,1,1,1,1,1,1,1,1,1,1,1,1,1,1,1,1,1,1,1,1,1,1,1,1,1,1,1,1,1,1,
1,1,1,1,1,1,1,1,1,1,1,1,1,1,1,1,1,1,1,1,1,1,1,1,1,1,1,1,1,1,1,1,1,1,1,1,
1,1,1,1,1,1,1,1,1,1,1,1,1,1,1,1,1,1,1,1,1,1,1,1,1,1,1,1,1,1,1,1,1,1,1,1,
1,1,1,1,1,1,1,1,1,1,1,1,1,1,1,1,1,1,1,1,1,1,1,1,1,1,1,1,1,1,1,1,1,1,6),
(-1.,-0.995000000000001,-0.990000000000001,-0.985000000000001,-0.980000000000001,
-0.975000000000001,-0.970000000000001,-0.965000000000001,-0.960000000000001,
-0.955000000000001,-0.950000000000001,-0.945000000000001,-0.940000000000001,
-0.935000000000001,-0.930000000000001,-0.925000000000001,-0.920000000000001,
-0.915000000000001,-0.910000000000001,-0.905000000000001,-0.900000000000001,
-0.895000000000001,-0.890000000000001,-0.885000000000001,-0.880000000000001,
-0.875000000000001,-0.870000000000001,-0.865000000000001,-0.860000000000001,
-0.855000000000001,-0.850000000000001,-0.845000000000001,-0.840000000000001,
-0.835000000000001,-0.830000000000001,-0.825000000000001,-0.820000000000001,
-0.815000000000001,-0.810000000000001,-0.805000000000001,-0.800000000000001,
-0.795000000000001,-0.790000000000001,-0.785000000000001,-0.780000000000001,
-0.775000000000001,-0.770000000000001,-0.765000000000001,-0.760000000000001,
-0.755000000000001,-0.750000000000001,-0.745000000000001,-0.740000000000001,
-0.735000000000001,-0.730000000000001,-0.725000000000001,-0.720000000000001,
-0.715000000000001,-0.710000000000001,-0.705000000000001,-0.700000000000001,
-0.695000000000001,-0.690000000000001,-0.685,-0.68,-0.675,-0.67,-0.665,
-0.66,-0.655,-0.65,-0.645,-0.64,-0.635,-0.63,-0.625,-0.62,-0.615,-0.61,
-0.605,-0.6,-0.595,-0.59,-0.585,-0.58,-0.575,-0.57,-0.565,-0.56,-0.555,
-0.55,-0.545,-0.54,-0.535,-0.53,-0.525,-0.52,-0.515,-0.51,-0.505,-0.5,-0.495,
-0.49,-0.485,-0.48,-0.475,-0.47,-0.465,-0.46,-0.455,-0.45,-0.445,-0.44,
-0.435,-0.43,-0.425,-0.42,-0.415,-0.41,-0.405,-0.4,-0.395,-0.39,-0.385,
-0.38,-0.375,-0.37,-0.365,-0.36,-0.355,-0.35,-0.345,-0.34,-0.335,-0.33,
-0.325,-0.32,-0.315,-0.31,-0.305,-0.3,-0.295,-0.29,-0.285,-0.28,-0.275,
-0.27,-0.265,-0.26,-0.255,-0.25,-0.245,-0.24,-0.235,-0.23,-0.225,-0.22,
-0.215,-0.21,-0.205,-0.2,-0.195,-0.19,-0.185,-0.18,-0.175,-0.17,-0.165,
-0.16,-0.155,-0.15,-0.145,-0.14,-0.135,-0.13,-0.125,-0.12,-0.115,-0.11,
-0.105,-0.1,-0.095,-0.09,-0.085,-0.08,-0.075,-0.07,-0.065,-0.06,-0.055,
-0.05,-0.045,-0.04,-0.035,-0.03,-0.025,-0.02,-0.015,-0.01,-0.005,0.),
 .UNSPECIFIED.)
CURVE()
GEOMETRIC_REPRESENTATION_ITEM()
RATIONAL_B_SPLINE_CURVE((1.,1.,1.,1.,1.,1.,1.,1.,1.,1.,1.,1.,1.,1.,1.,1.,
1.,1.,1.,1.,1.,1.,1.,1.,1.,1.,1.,1.,1.,1.,1.,1.,1.,1.,1.,1.,1.,1.,1.,1.,
1.,1.,1.,1.,1.,1.,1.,1.,1.,1.,1.,1.,1.,1.,1.,1.,1.,1.,1.,1.,1.,1.,1.,1.,
1.,1.,1.,1.,1.,1.,1.,1.,1.,1.,1.,1.,1.,1.,1.,1.,1.,1.,1.,1.,1.,1.,1.,1.,
1.,1.,1.,1.,1.,1.,1.,1.,1.,1.,1.,1.,1.,1.,1.,1.,1.,1.,1.,1.,1.,1.,1.,1.,
1.,1.,1.,1.,1.,1.,1.,1.,1.,1.,1.,1.,1.,1.,1.,1.,1.,1.,1.,1.,1.,1.,1.,1.,
1.,1.,1.,1.,1.,1.,1.,1.,1.,1.,1.,1.,1.,1.,1.,1.,1.,1.,1.,1.,1.,1.,1.,1.,
1.,1.,1.,1.,1.,1.,1.,1.,1.,1.,1.,1.,1.,1.,1.,1.,1.,1.,1.,1.,1.,1.,1.,1.,
1.,1.,1.,1.,1.,1.,1.,1.,1.,1.,1.,1.,1.,1.,1.,1.,1.,1.,1.,1.,1.))
REPRESENTATION_ITEM('')
);
#844=(
BOUNDED_CURVE()
B_SPLINE_CURVE(5,(#239754,#239755,#239756,#239757,#239758,#239759,#239760,
#239761,#239762,#239763,#239764,#239765,#239766,#239767,#239768,#239769,
#239770,#239771,#239772,#239773,#239774,#239775,#239776,#239777,#239778,
#239779,#239780,#239781,#239782,#239783,#239784,#239785,#239786,#239787,
#239788,#239789,#239790,#239791,#239792,#239793,#239794,#239795,#239796,
#239797,#239798,#239799,#239800,#239801,#239802,#239803,#239804,#239805,
#239806,#239807,#239808,#239809,#239810,#239811,#239812,#239813,#239814,
#239815,#239816,#239817,#239818,#239819,#239820,#239821,#239822,#239823,
#239824,#239825,#239826,#239827,#239828,#239829,#239830,#239831,#239832,
#239833,#239834,#239835,#239836,#239837,#239838,#239839,#239840,#239841,
#239842,#239843,#239844,#239845,#239846,#239847,#239848,#239849,#239850,
#239851,#239852,#239853,#239854,#239855,#239856,#239857,#239858,#239859,
#239860,#239861,#239862,#239863,#239864,#239865,#239866,#239867,#239868,
#239869,#239870,#239871,#239872,#239873,#239874,#239875,#239876,#239877,
#239878,#239879,#239880,#239881,#239882,#239883,#239884,#239885,#239886,
#239887,#239888,#239889,#239890,#239891,#239892,#239893,#239894,#239895,
#239896,#239897,#239898,#239899,#239900,#239901,#239902,#239903,#239904,
#239905,#239906,#239907,#239908,#239909,#239910,#239911,#239912,#239913,
#239914,#239915,#239916,#239917,#239918,#239919,#239920,#239921,#239922,
#239923,#239924,#239925,#239926,#239927,#239928,#239929,#239930,#239931,
#239932,#239933,#239934,#239935,#239936,#239937,#239938,#239939,#239940,
#239941,#239942,#239943,#239944,#239945,#239946,#239947,#239948,#239949,
#239950,#239951,#239952,#239953,#239954,#239955,#239956,#239957,#239958),
 .UNSPECIFIED.,.F.,.F.)
B_SPLINE_CURVE_WITH_KNOTS((6,1,1,1,1,1,1,1,1,1,1,1,1,1,1,1,1,1,1,1,1,1,
1,1,1,1,1,1,1,1,1,1,1,1,1,1,1,1,1,1,1,1,1,1,1,1,1,1,1,1,1,1,1,1,1,1,1,1,
1,1,1,1,1,1,1,1,1,1,1,1,1,1,1,1,1,1,1,1,1,1,1,1,1,1,1,1,1,1,1,1,1,1,1,1,
1,1,1,1,1,1,1,1,1,1,1,1,1,1,1,1,1,1,1,1,1,1,1,1,1,1,1,1,1,1,1,1,1,1,1,1,
1,1,1,1,1,1,1,1,1,1,1,1,1,1,1,1,1,1,1,1,1,1,1,1,1,1,1,1,1,1,1,1,1,1,1,1,
1,1,1,1,1,1,1,1,1,1,1,1,1,1,1,1,1,1,1,1,1,1,1,1,1,1,1,1,1,1,1,1,1,1,6),
(0.,0.005,0.01,0.015,0.02,0.025,0.03,0.035,0.04,0.045,0.05,0.055,0.06,0.065,
0.07,0.075,0.08,0.085,0.09,0.095,0.1,0.105,0.11,0.115,0.12,0.125,0.13,0.135,
0.14,0.145,0.15,0.155,0.16,0.165,0.17,0.175,0.18,0.185,0.19,0.195,0.2,0.205,
0.21,0.215,0.22,0.225,0.23,0.235,0.24,0.245,0.25,0.255,0.26,0.265,0.27,
0.275,0.28,0.285,0.29,0.295,0.3,0.305,0.31,0.315,0.32,0.325,0.33,0.335,
0.34,0.345,0.35,0.355,0.36,0.365,0.37,0.375,0.38,0.385,0.39,0.395,0.4,0.405,
0.41,0.415,0.42,0.425,0.43,0.435,0.44,0.445,0.45,0.455,0.46,0.465,0.47,
0.475,0.48,0.485,0.49,0.495,0.5,0.505,0.51,0.515,0.52,0.525,0.53,0.535,
0.54,0.545,0.55,0.555,0.56,0.565,0.57,0.575,0.58,0.585,0.59,0.595,0.6,0.605,
0.61,0.615,0.62,0.625,0.63,0.635,0.64,0.645,0.65,0.655,0.66,0.665,0.67,
0.675,0.68,0.685,0.690000000000001,0.695000000000001,0.700000000000001,
0.705000000000001,0.710000000000001,0.715000000000001,0.720000000000001,
0.725000000000001,0.730000000000001,0.735000000000001,0.740000000000001,
0.745000000000001,0.750000000000001,0.755000000000001,0.760000000000001,
0.765000000000001,0.770000000000001,0.775000000000001,0.780000000000001,
0.785000000000001,0.790000000000001,0.795000000000001,0.800000000000001,
0.805000000000001,0.810000000000001,0.815000000000001,0.820000000000001,
0.825000000000001,0.830000000000001,0.835000000000001,0.840000000000001,
0.845000000000001,0.850000000000001,0.855000000000001,0.860000000000001,
0.865000000000001,0.870000000000001,0.875000000000001,0.880000000000001,
0.885000000000001,0.890000000000001,0.895000000000001,0.900000000000001,
0.905000000000001,0.910000000000001,0.915000000000001,0.920000000000001,
0.925000000000001,0.930000000000001,0.935000000000001,0.940000000000001,
0.945000000000001,0.950000000000001,0.955000000000001,0.960000000000001,
0.965000000000001,0.970000000000001,0.975000000000001,0.980000000000001,
0.985000000000001,0.990000000000001,0.995000000000001,1.),.UNSPECIFIED.)
CURVE()
GEOMETRIC_REPRESENTATION_ITEM()
RATIONAL_B_SPLINE_CURVE((1.,1.,1.,1.,1.,1.,1.,1.,1.,1.,1.,1.,1.,1.,1.,1.,
1.,1.,1.,1.,1.,1.,1.,1.,1.,1.,1.,1.,1.,1.,1.,1.,1.,1.,1.,1.,1.,1.,1.,1.,
1.,1.,1.,1.,1.,1.,1.,1.,1.,1.,1.,1.,1.,1.,1.,1.,1.,1.,1.,1.,1.,1.,1.,1.,
1.,1.,1.,1.,1.,1.,1.,1.,1.,1.,1.,1.,1.,1.,1.,1.,1.,1.,1.,1.,1.,1.,1.,1.,
1.,1.,1.,1.,1.,1.,1.,1.,1.,1.,1.,1.,1.,1.,1.,1.,1.,1.,1.,1.,1.,1.,1.,1.,
1.,1.,1.,1.,1.,1.,1.,1.,1.,1.,1.,1.,1.,1.,1.,1.,1.,1.,1.,1.,1.,1.,1.,1.,
1.,1.,1.,1.,1.,1.,1.,1.,1.,1.,1.,1.,1.,1.,1.,1.,1.,1.,1.,1.,1.,1.,1.,1.,
1.,1.,1.,1.,1.,1.,1.,1.,1.,1.,1.,1.,1.,1.,1.,1.,1.,1.,1.,1.,1.,1.,1.,1.,
1.,1.,1.,1.,1.,1.,1.,1.,1.,1.,1.,1.,1.,1.,1.,1.,1.,1.,1.,1.,1.))
REPRESENTATION_ITEM('')
);
#845=(
BOUNDED_CURVE()
B_SPLINE_CURVE(5,(#240370,#240371,#240372,#240373,#240374,#240375,#240376,
#240377,#240378,#240379,#240380,#240381,#240382,#240383,#240384,#240385,
#240386,#240387,#240388,#240389,#240390,#240391,#240392,#240393,#240394,
#240395,#240396,#240397,#240398,#240399,#240400,#240401,#240402,#240403,
#240404,#240405,#240406,#240407,#240408,#240409,#240410,#240411,#240412,
#240413,#240414,#240415,#240416,#240417,#240418,#240419,#240420,#240421,
#240422,#240423,#240424,#240425,#240426,#240427,#240428,#240429,#240430,
#240431,#240432,#240433,#240434,#240435,#240436,#240437,#240438,#240439,
#240440,#240441,#240442,#240443,#240444,#240445,#240446,#240447,#240448,
#240449,#240450,#240451,#240452,#240453,#240454,#240455,#240456,#240457,
#240458,#240459,#240460,#240461,#240462,#240463,#240464,#240465,#240466,
#240467,#240468,#240469,#240470,#240471,#240472,#240473,#240474,#240475,
#240476,#240477,#240478,#240479,#240480,#240481,#240482,#240483,#240484,
#240485,#240486,#240487,#240488,#240489,#240490,#240491,#240492,#240493,
#240494,#240495,#240496,#240497,#240498,#240499,#240500,#240501,#240502,
#240503,#240504,#240505,#240506,#240507,#240508,#240509,#240510,#240511,
#240512,#240513,#240514,#240515,#240516,#240517,#240518,#240519,#240520,
#240521,#240522,#240523,#240524,#240525,#240526,#240527,#240528,#240529,
#240530,#240531,#240532,#240533,#240534,#240535,#240536,#240537,#240538,
#240539,#240540,#240541,#240542,#240543,#240544,#240545,#240546,#240547,
#240548,#240549,#240550,#240551,#240552,#240553,#240554,#240555,#240556,
#240557,#240558,#240559,#240560,#240561,#240562,#240563,#240564,#240565,
#240566,#240567,#240568,#240569,#240570,#240571,#240572,#240573,#240574),
 .UNSPECIFIED.,.F.,.F.)
B_SPLINE_CURVE_WITH_KNOTS((6,1,1,1,1,1,1,1,1,1,1,1,1,1,1,1,1,1,1,1,1,1,
1,1,1,1,1,1,1,1,1,1,1,1,1,1,1,1,1,1,1,1,1,1,1,1,1,1,1,1,1,1,1,1,1,1,1,1,
1,1,1,1,1,1,1,1,1,1,1,1,1,1,1,1,1,1,1,1,1,1,1,1,1,1,1,1,1,1,1,1,1,1,1,1,
1,1,1,1,1,1,1,1,1,1,1,1,1,1,1,1,1,1,1,1,1,1,1,1,1,1,1,1,1,1,1,1,1,1,1,1,
1,1,1,1,1,1,1,1,1,1,1,1,1,1,1,1,1,1,1,1,1,1,1,1,1,1,1,1,1,1,1,1,1,1,1,1,
1,1,1,1,1,1,1,1,1,1,1,1,1,1,1,1,1,1,1,1,1,1,1,1,1,1,1,1,1,1,1,1,1,1,6),
(0.,0.005,0.01,0.015,0.02,0.025,0.03,0.035,0.04,0.045,0.05,0.055,0.06,0.065,
0.07,0.075,0.08,0.085,0.09,0.095,0.1,0.105,0.11,0.115,0.12,0.125,0.13,0.135,
0.14,0.145,0.15,0.155,0.16,0.165,0.17,0.175,0.18,0.185,0.19,0.195,0.2,0.205,
0.21,0.215,0.22,0.225,0.23,0.235,0.24,0.245,0.25,0.255,0.26,0.265,0.27,
0.275,0.28,0.285,0.29,0.295,0.3,0.305,0.31,0.315,0.32,0.325,0.33,0.335,
0.34,0.345,0.35,0.355,0.36,0.365,0.37,0.375,0.38,0.385,0.39,0.395,0.4,0.405,
0.41,0.415,0.42,0.425,0.43,0.435,0.44,0.445,0.45,0.455,0.46,0.465,0.47,
0.475,0.48,0.485,0.49,0.495,0.5,0.505,0.51,0.515,0.52,0.525,0.53,0.535,
0.54,0.545,0.55,0.555,0.56,0.565,0.57,0.575,0.58,0.585,0.59,0.595,0.6,0.605,
0.61,0.615,0.62,0.625,0.63,0.635,0.64,0.645,0.65,0.655,0.66,0.665,0.67,
0.675,0.68,0.685,0.690000000000001,0.695000000000001,0.700000000000001,
0.705000000000001,0.710000000000001,0.715000000000001,0.720000000000001,
0.725000000000001,0.730000000000001,0.735000000000001,0.740000000000001,
0.745000000000001,0.750000000000001,0.755000000000001,0.760000000000001,
0.765000000000001,0.770000000000001,0.775000000000001,0.780000000000001,
0.785000000000001,0.790000000000001,0.795000000000001,0.800000000000001,
0.805000000000001,0.810000000000001,0.815000000000001,0.820000000000001,
0.825000000000001,0.830000000000001,0.835000000000001,0.840000000000001,
0.845000000000001,0.850000000000001,0.855000000000001,0.860000000000001,
0.865000000000001,0.870000000000001,0.875000000000001,0.880000000000001,
0.885000000000001,0.890000000000001,0.895000000000001,0.900000000000001,
0.905000000000001,0.910000000000001,0.915000000000001,0.920000000000001,
0.925000000000001,0.930000000000001,0.935000000000001,0.940000000000001,
0.945000000000001,0.950000000000001,0.955000000000001,0.960000000000001,
0.965000000000001,0.970000000000001,0.975000000000001,0.980000000000001,
0.985000000000001,0.990000000000001,0.995000000000001,1.),.UNSPECIFIED.)
CURVE()
GEOMETRIC_REPRESENTATION_ITEM()
RATIONAL_B_SPLINE_CURVE((1.,1.,1.,1.,1.,1.,1.,1.,1.,1.,1.,1.,1.,1.,1.,1.,
1.,1.,1.,1.,1.,1.,1.,1.,1.,1.,1.,1.,1.,1.,1.,1.,1.,1.,1.,1.,1.,1.,1.,1.,
1.,1.,1.,1.,1.,1.,1.,1.,1.,1.,1.,1.,1.,1.,1.,1.,1.,1.,1.,1.,1.,1.,1.,1.,
1.,1.,1.,1.,1.,1.,1.,1.,1.,1.,1.,1.,1.,1.,1.,1.,1.,1.,1.,1.,1.,1.,1.,1.,
1.,1.,1.,1.,1.,1.,1.,1.,1.,1.,1.,1.,1.,1.,1.,1.,1.,1.,1.,1.,1.,1.,1.,1.,
1.,1.,1.,1.,1.,1.,1.,1.,1.,1.,1.,1.,1.,1.,1.,1.,1.,1.,1.,1.,1.,1.,1.,1.,
1.,1.,1.,1.,1.,1.,1.,1.,1.,1.,1.,1.,1.,1.,1.,1.,1.,1.,1.,1.,1.,1.,1.,1.,
1.,1.,1.,1.,1.,1.,1.,1.,1.,1.,1.,1.,1.,1.,1.,1.,1.,1.,1.,1.,1.,1.,1.,1.,
1.,1.,1.,1.,1.,1.,1.,1.,1.,1.,1.,1.,1.,1.,1.,1.,1.,1.,1.,1.,1.))
REPRESENTATION_ITEM('')
);
#846=(
BOUNDED_CURVE()
B_SPLINE_CURVE(5,(#240576,#240577,#240578,#240579,#240580,#240581,#240582,
#240583,#240584,#240585,#240586,#240587,#240588,#240589,#240590,#240591,
#240592,#240593,#240594,#240595,#240596,#240597,#240598,#240599,#240600,
#240601,#240602,#240603,#240604,#240605,#240606,#240607,#240608,#240609,
#240610,#240611,#240612,#240613,#240614,#240615,#240616,#240617,#240618,
#240619,#240620,#240621,#240622,#240623,#240624,#240625,#240626,#240627,
#240628,#240629,#240630,#240631,#240632,#240633,#240634,#240635,#240636,
#240637,#240638,#240639,#240640,#240641,#240642,#240643,#240644,#240645,
#240646,#240647,#240648,#240649,#240650,#240651,#240652,#240653,#240654,
#240655,#240656,#240657,#240658,#240659,#240660,#240661,#240662,#240663,
#240664,#240665,#240666,#240667,#240668,#240669,#240670,#240671,#240672,
#240673,#240674,#240675,#240676,#240677,#240678,#240679,#240680,#240681,
#240682,#240683,#240684,#240685,#240686,#240687,#240688,#240689,#240690,
#240691,#240692,#240693,#240694,#240695,#240696,#240697,#240698,#240699,
#240700,#240701,#240702,#240703,#240704,#240705,#240706,#240707,#240708,
#240709,#240710,#240711,#240712,#240713,#240714,#240715,#240716,#240717,
#240718,#240719,#240720,#240721,#240722,#240723,#240724,#240725,#240726,
#240727,#240728,#240729,#240730,#240731,#240732,#240733,#240734,#240735,
#240736,#240737,#240738,#240739,#240740,#240741,#240742,#240743,#240744,
#240745,#240746,#240747,#240748,#240749,#240750,#240751,#240752,#240753,
#240754,#240755,#240756,#240757,#240758,#240759,#240760,#240761,#240762,
#240763,#240764,#240765,#240766,#240767,#240768,#240769,#240770,#240771,
#240772,#240773,#240774,#240775,#240776,#240777,#240778,#240779,#240780),
 .UNSPECIFIED.,.F.,.F.)
B_SPLINE_CURVE_WITH_KNOTS((6,1,1,1,1,1,1,1,1,1,1,1,1,1,1,1,1,1,1,1,1,1,
1,1,1,1,1,1,1,1,1,1,1,1,1,1,1,1,1,1,1,1,1,1,1,1,1,1,1,1,1,1,1,1,1,1,1,1,
1,1,1,1,1,1,1,1,1,1,1,1,1,1,1,1,1,1,1,1,1,1,1,1,1,1,1,1,1,1,1,1,1,1,1,1,
1,1,1,1,1,1,1,1,1,1,1,1,1,1,1,1,1,1,1,1,1,1,1,1,1,1,1,1,1,1,1,1,1,1,1,1,
1,1,1,1,1,1,1,1,1,1,1,1,1,1,1,1,1,1,1,1,1,1,1,1,1,1,1,1,1,1,1,1,1,1,1,1,
1,1,1,1,1,1,1,1,1,1,1,1,1,1,1,1,1,1,1,1,1,1,1,1,1,1,1,1,1,1,1,1,1,1,6),
(-1.,-0.995000000000001,-0.990000000000001,-0.985000000000001,-0.980000000000001,
-0.975000000000001,-0.970000000000001,-0.965000000000001,-0.960000000000001,
-0.955000000000001,-0.950000000000001,-0.945000000000001,-0.940000000000001,
-0.935000000000001,-0.930000000000001,-0.925000000000001,-0.920000000000001,
-0.915000000000001,-0.910000000000001,-0.905000000000001,-0.900000000000001,
-0.895000000000001,-0.890000000000001,-0.885000000000001,-0.880000000000001,
-0.875000000000001,-0.870000000000001,-0.865000000000001,-0.860000000000001,
-0.855000000000001,-0.850000000000001,-0.845000000000001,-0.840000000000001,
-0.835000000000001,-0.830000000000001,-0.825000000000001,-0.820000000000001,
-0.815000000000001,-0.810000000000001,-0.805000000000001,-0.800000000000001,
-0.795000000000001,-0.790000000000001,-0.785000000000001,-0.780000000000001,
-0.775000000000001,-0.770000000000001,-0.765000000000001,-0.760000000000001,
-0.755000000000001,-0.750000000000001,-0.745000000000001,-0.740000000000001,
-0.735000000000001,-0.730000000000001,-0.725000000000001,-0.720000000000001,
-0.715000000000001,-0.710000000000001,-0.705000000000001,-0.700000000000001,
-0.695000000000001,-0.690000000000001,-0.685,-0.68,-0.675,-0.67,-0.665,
-0.66,-0.655,-0.65,-0.645,-0.64,-0.635,-0.63,-0.625,-0.62,-0.615,-0.61,
-0.605,-0.6,-0.595,-0.59,-0.585,-0.58,-0.575,-0.57,-0.565,-0.56,-0.555,
-0.55,-0.545,-0.54,-0.535,-0.53,-0.525,-0.52,-0.515,-0.51,-0.505,-0.5,-0.495,
-0.49,-0.485,-0.48,-0.475,-0.47,-0.465,-0.46,-0.455,-0.45,-0.445,-0.44,
-0.435,-0.43,-0.425,-0.42,-0.415,-0.41,-0.405,-0.4,-0.395,-0.39,-0.385,
-0.38,-0.375,-0.37,-0.365,-0.36,-0.355,-0.35,-0.345,-0.34,-0.335,-0.33,
-0.325,-0.32,-0.315,-0.31,-0.305,-0.3,-0.295,-0.29,-0.285,-0.28,-0.275,
-0.27,-0.265,-0.26,-0.255,-0.25,-0.245,-0.24,-0.235,-0.23,-0.225,-0.22,
-0.215,-0.21,-0.205,-0.2,-0.195,-0.19,-0.185,-0.18,-0.175,-0.17,-0.165,
-0.16,-0.155,-0.15,-0.145,-0.14,-0.135,-0.13,-0.125,-0.12,-0.115,-0.11,
-0.105,-0.1,-0.095,-0.09,-0.085,-0.08,-0.075,-0.07,-0.065,-0.06,-0.055,
-0.05,-0.045,-0.04,-0.035,-0.03,-0.025,-0.02,-0.015,-0.01,-0.005,0.),
 .UNSPECIFIED.)
CURVE()
GEOMETRIC_REPRESENTATION_ITEM()
RATIONAL_B_SPLINE_CURVE((1.,1.,1.,1.,1.,1.,1.,1.,1.,1.,1.,1.,1.,1.,1.,1.,
1.,1.,1.,1.,1.,1.,1.,1.,1.,1.,1.,1.,1.,1.,1.,1.,1.,1.,1.,1.,1.,1.,1.,1.,
1.,1.,1.,1.,1.,1.,1.,1.,1.,1.,1.,1.,1.,1.,1.,1.,1.,1.,1.,1.,1.,1.,1.,1.,
1.,1.,1.,1.,1.,1.,1.,1.,1.,1.,1.,1.,1.,1.,1.,1.,1.,1.,1.,1.,1.,1.,1.,1.,
1.,1.,1.,1.,1.,1.,1.,1.,1.,1.,1.,1.,1.,1.,1.,1.,1.,1.,1.,1.,1.,1.,1.,1.,
1.,1.,1.,1.,1.,1.,1.,1.,1.,1.,1.,1.,1.,1.,1.,1.,1.,1.,1.,1.,1.,1.,1.,1.,
1.,1.,1.,1.,1.,1.,1.,1.,1.,1.,1.,1.,1.,1.,1.,1.,1.,1.,1.,1.,1.,1.,1.,1.,
1.,1.,1.,1.,1.,1.,1.,1.,1.,1.,1.,1.,1.,1.,1.,1.,1.,1.,1.,1.,1.,1.,1.,1.,
1.,1.,1.,1.,1.,1.,1.,1.,1.,1.,1.,1.,1.,1.,1.,1.,1.,1.,1.,1.,1.))
REPRESENTATION_ITEM('')
);
#847=(
BOUNDED_CURVE()
B_SPLINE_CURVE(5,(#241199,#241200,#241201,#241202,#241203,#241204,#241205,
#241206,#241207,#241208,#241209,#241210,#241211,#241212,#241213,#241214,
#241215,#241216,#241217,#241218,#241219,#241220,#241221,#241222,#241223,
#241224,#241225,#241226,#241227,#241228,#241229,#241230,#241231,#241232,
#241233,#241234,#241235,#241236,#241237,#241238,#241239,#241240,#241241,
#241242,#241243,#241244,#241245,#241246,#241247,#241248,#241249,#241250,
#241251,#241252,#241253,#241254,#241255,#241256,#241257,#241258,#241259,
#241260,#241261,#241262,#241263,#241264,#241265,#241266,#241267,#241268,
#241269,#241270,#241271,#241272,#241273,#241274,#241275,#241276,#241277,
#241278,#241279,#241280,#241281,#241282,#241283,#241284,#241285,#241286,
#241287,#241288,#241289,#241290,#241291,#241292,#241293,#241294,#241295,
#241296,#241297,#241298,#241299,#241300,#241301,#241302,#241303,#241304,
#241305,#241306,#241307,#241308,#241309,#241310,#241311,#241312,#241313,
#241314,#241315,#241316,#241317,#241318,#241319,#241320,#241321,#241322,
#241323,#241324,#241325,#241326,#241327,#241328,#241329,#241330,#241331,
#241332,#241333,#241334,#241335,#241336,#241337,#241338,#241339,#241340,
#241341,#241342,#241343,#241344,#241345,#241346,#241347,#241348,#241349,
#241350,#241351,#241352,#241353,#241354,#241355,#241356,#241357,#241358,
#241359,#241360,#241361,#241362,#241363,#241364,#241365,#241366,#241367,
#241368,#241369,#241370,#241371,#241372,#241373,#241374,#241375,#241376,
#241377,#241378,#241379,#241380,#241381,#241382,#241383,#241384,#241385,
#241386,#241387,#241388,#241389,#241390,#241391,#241392,#241393,#241394,
#241395,#241396,#241397,#241398,#241399,#241400,#241401,#241402,#241403),
 .UNSPECIFIED.,.F.,.F.)
B_SPLINE_CURVE_WITH_KNOTS((6,1,1,1,1,1,1,1,1,1,1,1,1,1,1,1,1,1,1,1,1,1,
1,1,1,1,1,1,1,1,1,1,1,1,1,1,1,1,1,1,1,1,1,1,1,1,1,1,1,1,1,1,1,1,1,1,1,1,
1,1,1,1,1,1,1,1,1,1,1,1,1,1,1,1,1,1,1,1,1,1,1,1,1,1,1,1,1,1,1,1,1,1,1,1,
1,1,1,1,1,1,1,1,1,1,1,1,1,1,1,1,1,1,1,1,1,1,1,1,1,1,1,1,1,1,1,1,1,1,1,1,
1,1,1,1,1,1,1,1,1,1,1,1,1,1,1,1,1,1,1,1,1,1,1,1,1,1,1,1,1,1,1,1,1,1,1,1,
1,1,1,1,1,1,1,1,1,1,1,1,1,1,1,1,1,1,1,1,1,1,1,1,1,1,1,1,1,1,1,1,1,1,6),
(-1.,-0.995000000000001,-0.990000000000001,-0.985000000000001,-0.980000000000001,
-0.975000000000001,-0.970000000000001,-0.965000000000001,-0.960000000000001,
-0.955000000000001,-0.950000000000001,-0.945000000000001,-0.940000000000001,
-0.935000000000001,-0.930000000000001,-0.925000000000001,-0.920000000000001,
-0.915000000000001,-0.910000000000001,-0.905000000000001,-0.900000000000001,
-0.895000000000001,-0.890000000000001,-0.885000000000001,-0.880000000000001,
-0.875000000000001,-0.870000000000001,-0.865000000000001,-0.860000000000001,
-0.855000000000001,-0.850000000000001,-0.845000000000001,-0.840000000000001,
-0.835000000000001,-0.830000000000001,-0.825000000000001,-0.820000000000001,
-0.815000000000001,-0.810000000000001,-0.805000000000001,-0.800000000000001,
-0.795000000000001,-0.790000000000001,-0.785000000000001,-0.780000000000001,
-0.775000000000001,-0.770000000000001,-0.765000000000001,-0.760000000000001,
-0.755000000000001,-0.750000000000001,-0.745000000000001,-0.740000000000001,
-0.735000000000001,-0.730000000000001,-0.725000000000001,-0.720000000000001,
-0.715000000000001,-0.710000000000001,-0.705000000000001,-0.700000000000001,
-0.695000000000001,-0.690000000000001,-0.685,-0.68,-0.675,-0.67,-0.665,
-0.66,-0.655,-0.65,-0.645,-0.64,-0.635,-0.63,-0.625,-0.62,-0.615,-0.61,
-0.605,-0.6,-0.595,-0.59,-0.585,-0.58,-0.575,-0.57,-0.565,-0.56,-0.555,
-0.55,-0.545,-0.54,-0.535,-0.53,-0.525,-0.52,-0.515,-0.51,-0.505,-0.5,-0.495,
-0.49,-0.485,-0.48,-0.475,-0.47,-0.465,-0.46,-0.455,-0.45,-0.445,-0.44,
-0.435,-0.43,-0.425,-0.42,-0.415,-0.41,-0.405,-0.4,-0.395,-0.39,-0.385,
-0.38,-0.375,-0.37,-0.365,-0.36,-0.355,-0.35,-0.345,-0.34,-0.335,-0.33,
-0.325,-0.32,-0.315,-0.31,-0.305,-0.3,-0.295,-0.29,-0.285,-0.28,-0.275,
-0.27,-0.265,-0.26,-0.255,-0.25,-0.245,-0.24,-0.235,-0.23,-0.225,-0.22,
-0.215,-0.21,-0.205,-0.2,-0.195,-0.19,-0.185,-0.18,-0.175,-0.17,-0.165,
-0.16,-0.155,-0.15,-0.145,-0.14,-0.135,-0.13,-0.125,-0.12,-0.115,-0.11,
-0.105,-0.1,-0.095,-0.09,-0.085,-0.08,-0.075,-0.07,-0.065,-0.06,-0.055,
-0.05,-0.045,-0.04,-0.035,-0.03,-0.025,-0.02,-0.015,-0.01,-0.005,0.),
 .UNSPECIFIED.)
CURVE()
GEOMETRIC_REPRESENTATION_ITEM()
RATIONAL_B_SPLINE_CURVE((1.,1.,1.,1.,1.,1.,1.,1.,1.,1.,1.,1.,1.,1.,1.,1.,
1.,1.,1.,1.,1.,1.,1.,1.,1.,1.,1.,1.,1.,1.,1.,1.,1.,1.,1.,1.,1.,1.,1.,1.,
1.,1.,1.,1.,1.,1.,1.,1.,1.,1.,1.,1.,1.,1.,1.,1.,1.,1.,1.,1.,1.,1.,1.,1.,
1.,1.,1.,1.,1.,1.,1.,1.,1.,1.,1.,1.,1.,1.,1.,1.,1.,1.,1.,1.,1.,1.,1.,1.,
1.,1.,1.,1.,1.,1.,1.,1.,1.,1.,1.,1.,1.,1.,1.,1.,1.,1.,1.,1.,1.,1.,1.,1.,
1.,1.,1.,1.,1.,1.,1.,1.,1.,1.,1.,1.,1.,1.,1.,1.,1.,1.,1.,1.,1.,1.,1.,1.,
1.,1.,1.,1.,1.,1.,1.,1.,1.,1.,1.,1.,1.,1.,1.,1.,1.,1.,1.,1.,1.,1.,1.,1.,
1.,1.,1.,1.,1.,1.,1.,1.,1.,1.,1.,1.,1.,1.,1.,1.,1.,1.,1.,1.,1.,1.,1.,1.,
1.,1.,1.,1.,1.,1.,1.,1.,1.,1.,1.,1.,1.,1.,1.,1.,1.,1.,1.,1.,1.))
REPRESENTATION_ITEM('')
);
#848=(
BOUNDED_CURVE()
B_SPLINE_CURVE(5,(#241406,#241407,#241408,#241409,#241410,#241411,#241412,
#241413,#241414,#241415,#241416,#241417,#241418,#241419,#241420,#241421,
#241422,#241423,#241424,#241425,#241426,#241427,#241428,#241429,#241430,
#241431,#241432,#241433,#241434,#241435,#241436,#241437,#241438,#241439,
#241440,#241441,#241442,#241443,#241444,#241445,#241446,#241447,#241448,
#241449,#241450,#241451,#241452,#241453,#241454,#241455,#241456,#241457,
#241458,#241459,#241460,#241461,#241462,#241463,#241464,#241465,#241466,
#241467,#241468,#241469,#241470,#241471,#241472,#241473,#241474,#241475,
#241476,#241477,#241478,#241479,#241480,#241481,#241482,#241483,#241484,
#241485,#241486,#241487,#241488,#241489,#241490,#241491,#241492,#241493,
#241494,#241495,#241496,#241497,#241498,#241499,#241500,#241501,#241502,
#241503,#241504,#241505,#241506,#241507,#241508,#241509,#241510,#241511,
#241512,#241513,#241514,#241515,#241516,#241517,#241518,#241519,#241520,
#241521,#241522,#241523,#241524,#241525,#241526,#241527,#241528,#241529,
#241530,#241531,#241532,#241533,#241534,#241535,#241536,#241537,#241538,
#241539,#241540,#241541,#241542,#241543,#241544,#241545,#241546,#241547,
#241548,#241549,#241550,#241551,#241552,#241553,#241554,#241555,#241556,
#241557,#241558,#241559,#241560,#241561,#241562,#241563,#241564,#241565,
#241566,#241567,#241568,#241569,#241570,#241571,#241572,#241573,#241574,
#241575,#241576,#241577,#241578,#241579,#241580,#241581,#241582,#241583,
#241584,#241585,#241586,#241587,#241588,#241589,#241590,#241591,#241592,
#241593,#241594,#241595,#241596,#241597,#241598,#241599,#241600,#241601,
#241602,#241603,#241604,#241605,#241606,#241607,#241608,#241609,#241610),
 .UNSPECIFIED.,.F.,.F.)
B_SPLINE_CURVE_WITH_KNOTS((6,1,1,1,1,1,1,1,1,1,1,1,1,1,1,1,1,1,1,1,1,1,
1,1,1,1,1,1,1,1,1,1,1,1,1,1,1,1,1,1,1,1,1,1,1,1,1,1,1,1,1,1,1,1,1,1,1,1,
1,1,1,1,1,1,1,1,1,1,1,1,1,1,1,1,1,1,1,1,1,1,1,1,1,1,1,1,1,1,1,1,1,1,1,1,
1,1,1,1,1,1,1,1,1,1,1,1,1,1,1,1,1,1,1,1,1,1,1,1,1,1,1,1,1,1,1,1,1,1,1,1,
1,1,1,1,1,1,1,1,1,1,1,1,1,1,1,1,1,1,1,1,1,1,1,1,1,1,1,1,1,1,1,1,1,1,1,1,
1,1,1,1,1,1,1,1,1,1,1,1,1,1,1,1,1,1,1,1,1,1,1,1,1,1,1,1,1,1,1,1,1,1,6),
(0.,0.005,0.01,0.015,0.02,0.025,0.03,0.035,0.04,0.045,0.05,0.055,0.06,0.065,
0.07,0.075,0.08,0.085,0.09,0.095,0.1,0.105,0.11,0.115,0.12,0.125,0.13,0.135,
0.14,0.145,0.15,0.155,0.16,0.165,0.17,0.175,0.18,0.185,0.19,0.195,0.2,0.205,
0.21,0.215,0.22,0.225,0.23,0.235,0.24,0.245,0.25,0.255,0.26,0.265,0.27,
0.275,0.28,0.285,0.29,0.295,0.3,0.305,0.31,0.315,0.32,0.325,0.33,0.335,
0.34,0.345,0.35,0.355,0.36,0.365,0.37,0.375,0.38,0.385,0.39,0.395,0.4,0.405,
0.41,0.415,0.42,0.425,0.43,0.435,0.44,0.445,0.45,0.455,0.46,0.465,0.47,
0.475,0.48,0.485,0.49,0.495,0.5,0.505,0.51,0.515,0.52,0.525,0.53,0.535,
0.54,0.545,0.55,0.555,0.56,0.565,0.57,0.575,0.58,0.585,0.59,0.595,0.6,0.605,
0.61,0.615,0.62,0.625,0.63,0.635,0.64,0.645,0.65,0.655,0.66,0.665,0.67,
0.675,0.68,0.685,0.690000000000001,0.695000000000001,0.700000000000001,
0.705000000000001,0.710000000000001,0.715000000000001,0.720000000000001,
0.725000000000001,0.730000000000001,0.735000000000001,0.740000000000001,
0.745000000000001,0.750000000000001,0.755000000000001,0.760000000000001,
0.765000000000001,0.770000000000001,0.775000000000001,0.780000000000001,
0.785000000000001,0.790000000000001,0.795000000000001,0.800000000000001,
0.805000000000001,0.810000000000001,0.815000000000001,0.820000000000001,
0.825000000000001,0.830000000000001,0.835000000000001,0.840000000000001,
0.845000000000001,0.850000000000001,0.855000000000001,0.860000000000001,
0.865000000000001,0.870000000000001,0.875000000000001,0.880000000000001,
0.885000000000001,0.890000000000001,0.895000000000001,0.900000000000001,
0.905000000000001,0.910000000000001,0.915000000000001,0.920000000000001,
0.925000000000001,0.930000000000001,0.935000000000001,0.940000000000001,
0.945000000000001,0.950000000000001,0.955000000000001,0.960000000000001,
0.965000000000001,0.970000000000001,0.975000000000001,0.980000000000001,
0.985000000000001,0.990000000000001,0.995000000000001,1.),.UNSPECIFIED.)
CURVE()
GEOMETRIC_REPRESENTATION_ITEM()
RATIONAL_B_SPLINE_CURVE((1.,1.,1.,1.,1.,1.,1.,1.,1.,1.,1.,1.,1.,1.,1.,1.,
1.,1.,1.,1.,1.,1.,1.,1.,1.,1.,1.,1.,1.,1.,1.,1.,1.,1.,1.,1.,1.,1.,1.,1.,
1.,1.,1.,1.,1.,1.,1.,1.,1.,1.,1.,1.,1.,1.,1.,1.,1.,1.,1.,1.,1.,1.,1.,1.,
1.,1.,1.,1.,1.,1.,1.,1.,1.,1.,1.,1.,1.,1.,1.,1.,1.,1.,1.,1.,1.,1.,1.,1.,
1.,1.,1.,1.,1.,1.,1.,1.,1.,1.,1.,1.,1.,1.,1.,1.,1.,1.,1.,1.,1.,1.,1.,1.,
1.,1.,1.,1.,1.,1.,1.,1.,1.,1.,1.,1.,1.,1.,1.,1.,1.,1.,1.,1.,1.,1.,1.,1.,
1.,1.,1.,1.,1.,1.,1.,1.,1.,1.,1.,1.,1.,1.,1.,1.,1.,1.,1.,1.,1.,1.,1.,1.,
1.,1.,1.,1.,1.,1.,1.,1.,1.,1.,1.,1.,1.,1.,1.,1.,1.,1.,1.,1.,1.,1.,1.,1.,
1.,1.,1.,1.,1.,1.,1.,1.,1.,1.,1.,1.,1.,1.,1.,1.,1.,1.,1.,1.,1.))
REPRESENTATION_ITEM('')
);
#849=(
BOUNDED_CURVE()
B_SPLINE_CURVE(5,(#242022,#242023,#242024,#242025,#242026,#242027,#242028,
#242029,#242030,#242031,#242032,#242033,#242034,#242035,#242036,#242037,
#242038,#242039,#242040,#242041,#242042,#242043,#242044,#242045,#242046,
#242047,#242048,#242049,#242050,#242051,#242052,#242053,#242054,#242055,
#242056,#242057,#242058,#242059,#242060,#242061,#242062,#242063,#242064,
#242065,#242066,#242067,#242068,#242069,#242070,#242071,#242072,#242073,
#242074,#242075,#242076,#242077,#242078,#242079,#242080,#242081,#242082,
#242083,#242084,#242085,#242086,#242087,#242088,#242089,#242090,#242091,
#242092,#242093,#242094,#242095,#242096,#242097,#242098,#242099,#242100,
#242101,#242102,#242103,#242104,#242105,#242106,#242107,#242108,#242109,
#242110,#242111,#242112,#242113,#242114,#242115,#242116,#242117,#242118,
#242119,#242120,#242121,#242122,#242123,#242124,#242125,#242126,#242127,
#242128,#242129,#242130,#242131,#242132,#242133,#242134,#242135,#242136,
#242137,#242138,#242139,#242140,#242141,#242142,#242143,#242144,#242145,
#242146,#242147,#242148,#242149,#242150,#242151,#242152,#242153,#242154,
#242155,#242156,#242157,#242158,#242159,#242160,#242161,#242162,#242163,
#242164,#242165,#242166,#242167,#242168,#242169,#242170,#242171,#242172,
#242173,#242174,#242175,#242176,#242177,#242178,#242179,#242180,#242181,
#242182,#242183,#242184,#242185,#242186,#242187,#242188,#242189,#242190,
#242191,#242192,#242193,#242194,#242195,#242196,#242197,#242198,#242199,
#242200,#242201,#242202,#242203,#242204,#242205,#242206,#242207,#242208,
#242209,#242210,#242211,#242212,#242213,#242214,#242215,#242216,#242217,
#242218,#242219,#242220,#242221,#242222,#242223,#242224,#242225,#242226),
 .UNSPECIFIED.,.F.,.F.)
B_SPLINE_CURVE_WITH_KNOTS((6,1,1,1,1,1,1,1,1,1,1,1,1,1,1,1,1,1,1,1,1,1,
1,1,1,1,1,1,1,1,1,1,1,1,1,1,1,1,1,1,1,1,1,1,1,1,1,1,1,1,1,1,1,1,1,1,1,1,
1,1,1,1,1,1,1,1,1,1,1,1,1,1,1,1,1,1,1,1,1,1,1,1,1,1,1,1,1,1,1,1,1,1,1,1,
1,1,1,1,1,1,1,1,1,1,1,1,1,1,1,1,1,1,1,1,1,1,1,1,1,1,1,1,1,1,1,1,1,1,1,1,
1,1,1,1,1,1,1,1,1,1,1,1,1,1,1,1,1,1,1,1,1,1,1,1,1,1,1,1,1,1,1,1,1,1,1,1,
1,1,1,1,1,1,1,1,1,1,1,1,1,1,1,1,1,1,1,1,1,1,1,1,1,1,1,1,1,1,1,1,1,1,6),
(0.,0.005,0.01,0.015,0.02,0.025,0.03,0.035,0.04,0.045,0.05,0.055,0.06,0.065,
0.07,0.075,0.08,0.085,0.09,0.095,0.1,0.105,0.11,0.115,0.12,0.125,0.13,0.135,
0.14,0.145,0.15,0.155,0.16,0.165,0.17,0.175,0.18,0.185,0.19,0.195,0.2,0.205,
0.21,0.215,0.22,0.225,0.23,0.235,0.24,0.245,0.25,0.255,0.26,0.265,0.27,
0.275,0.28,0.285,0.29,0.295,0.3,0.305,0.31,0.315,0.32,0.325,0.33,0.335,
0.34,0.345,0.35,0.355,0.36,0.365,0.37,0.375,0.38,0.385,0.39,0.395,0.4,0.405,
0.41,0.415,0.42,0.425,0.43,0.435,0.44,0.445,0.45,0.455,0.46,0.465,0.47,
0.475,0.48,0.485,0.49,0.495,0.5,0.505,0.51,0.515,0.52,0.525,0.53,0.535,
0.54,0.545,0.55,0.555,0.56,0.565,0.57,0.575,0.58,0.585,0.59,0.595,0.6,0.605,
0.61,0.615,0.62,0.625,0.63,0.635,0.64,0.645,0.65,0.655,0.66,0.665,0.67,
0.675,0.68,0.685,0.690000000000001,0.695000000000001,0.700000000000001,
0.705000000000001,0.710000000000001,0.715000000000001,0.720000000000001,
0.725000000000001,0.730000000000001,0.735000000000001,0.740000000000001,
0.745000000000001,0.750000000000001,0.755000000000001,0.760000000000001,
0.765000000000001,0.770000000000001,0.775000000000001,0.780000000000001,
0.785000000000001,0.790000000000001,0.795000000000001,0.800000000000001,
0.805000000000001,0.810000000000001,0.815000000000001,0.820000000000001,
0.825000000000001,0.830000000000001,0.835000000000001,0.840000000000001,
0.845000000000001,0.850000000000001,0.855000000000001,0.860000000000001,
0.865000000000001,0.870000000000001,0.875000000000001,0.880000000000001,
0.885000000000001,0.890000000000001,0.895000000000001,0.900000000000001,
0.905000000000001,0.910000000000001,0.915000000000001,0.920000000000001,
0.925000000000001,0.930000000000001,0.935000000000001,0.940000000000001,
0.945000000000001,0.950000000000001,0.955000000000001,0.960000000000001,
0.965000000000001,0.970000000000001,0.975000000000001,0.980000000000001,
0.985000000000001,0.990000000000001,0.995000000000001,1.),.UNSPECIFIED.)
CURVE()
GEOMETRIC_REPRESENTATION_ITEM()
RATIONAL_B_SPLINE_CURVE((1.,1.,1.,1.,1.,1.,1.,1.,1.,1.,1.,1.,1.,1.,1.,1.,
1.,1.,1.,1.,1.,1.,1.,1.,1.,1.,1.,1.,1.,1.,1.,1.,1.,1.,1.,1.,1.,1.,1.,1.,
1.,1.,1.,1.,1.,1.,1.,1.,1.,1.,1.,1.,1.,1.,1.,1.,1.,1.,1.,1.,1.,1.,1.,1.,
1.,1.,1.,1.,1.,1.,1.,1.,1.,1.,1.,1.,1.,1.,1.,1.,1.,1.,1.,1.,1.,1.,1.,1.,
1.,1.,1.,1.,1.,1.,1.,1.,1.,1.,1.,1.,1.,1.,1.,1.,1.,1.,1.,1.,1.,1.,1.,1.,
1.,1.,1.,1.,1.,1.,1.,1.,1.,1.,1.,1.,1.,1.,1.,1.,1.,1.,1.,1.,1.,1.,1.,1.,
1.,1.,1.,1.,1.,1.,1.,1.,1.,1.,1.,1.,1.,1.,1.,1.,1.,1.,1.,1.,1.,1.,1.,1.,
1.,1.,1.,1.,1.,1.,1.,1.,1.,1.,1.,1.,1.,1.,1.,1.,1.,1.,1.,1.,1.,1.,1.,1.,
1.,1.,1.,1.,1.,1.,1.,1.,1.,1.,1.,1.,1.,1.,1.,1.,1.,1.,1.,1.,1.))
REPRESENTATION_ITEM('')
);
#850=(
BOUNDED_CURVE()
B_SPLINE_CURVE(5,(#242228,#242229,#242230,#242231,#242232,#242233,#242234,
#242235,#242236,#242237,#242238,#242239,#242240,#242241,#242242,#242243,
#242244,#242245,#242246,#242247,#242248,#242249,#242250,#242251,#242252,
#242253,#242254,#242255,#242256,#242257,#242258,#242259,#242260,#242261,
#242262,#242263,#242264,#242265,#242266,#242267,#242268,#242269,#242270,
#242271,#242272,#242273,#242274,#242275,#242276,#242277,#242278,#242279,
#242280,#242281,#242282,#242283,#242284,#242285,#242286,#242287,#242288,
#242289,#242290,#242291,#242292,#242293,#242294,#242295,#242296,#242297,
#242298,#242299,#242300,#242301,#242302,#242303,#242304,#242305,#242306,
#242307,#242308,#242309,#242310,#242311,#242312,#242313,#242314,#242315,
#242316,#242317,#242318,#242319,#242320,#242321,#242322,#242323,#242324,
#242325,#242326,#242327,#242328,#242329,#242330,#242331,#242332,#242333,
#242334,#242335,#242336,#242337,#242338,#242339,#242340,#242341,#242342,
#242343,#242344,#242345,#242346,#242347,#242348,#242349,#242350,#242351,
#242352,#242353,#242354,#242355,#242356,#242357,#242358,#242359,#242360,
#242361,#242362,#242363,#242364,#242365,#242366,#242367,#242368,#242369,
#242370,#242371,#242372,#242373,#242374,#242375,#242376,#242377,#242378,
#242379,#242380,#242381,#242382,#242383,#242384,#242385,#242386,#242387,
#242388,#242389,#242390,#242391,#242392,#242393,#242394,#242395,#242396,
#242397,#242398,#242399,#242400,#242401,#242402,#242403,#242404,#242405,
#242406,#242407,#242408,#242409,#242410,#242411,#242412,#242413,#242414,
#242415,#242416,#242417,#242418,#242419,#242420,#242421,#242422,#242423,
#242424,#242425,#242426,#242427,#242428,#242429,#242430,#242431,#242432),
 .UNSPECIFIED.,.F.,.F.)
B_SPLINE_CURVE_WITH_KNOTS((6,1,1,1,1,1,1,1,1,1,1,1,1,1,1,1,1,1,1,1,1,1,
1,1,1,1,1,1,1,1,1,1,1,1,1,1,1,1,1,1,1,1,1,1,1,1,1,1,1,1,1,1,1,1,1,1,1,1,
1,1,1,1,1,1,1,1,1,1,1,1,1,1,1,1,1,1,1,1,1,1,1,1,1,1,1,1,1,1,1,1,1,1,1,1,
1,1,1,1,1,1,1,1,1,1,1,1,1,1,1,1,1,1,1,1,1,1,1,1,1,1,1,1,1,1,1,1,1,1,1,1,
1,1,1,1,1,1,1,1,1,1,1,1,1,1,1,1,1,1,1,1,1,1,1,1,1,1,1,1,1,1,1,1,1,1,1,1,
1,1,1,1,1,1,1,1,1,1,1,1,1,1,1,1,1,1,1,1,1,1,1,1,1,1,1,1,1,1,1,1,1,1,6),
(-1.,-0.995000000000001,-0.990000000000001,-0.985000000000001,-0.980000000000001,
-0.975000000000001,-0.970000000000001,-0.965000000000001,-0.960000000000001,
-0.955000000000001,-0.950000000000001,-0.945000000000001,-0.940000000000001,
-0.935000000000001,-0.930000000000001,-0.925000000000001,-0.920000000000001,
-0.915000000000001,-0.910000000000001,-0.905000000000001,-0.900000000000001,
-0.895000000000001,-0.890000000000001,-0.885000000000001,-0.880000000000001,
-0.875000000000001,-0.870000000000001,-0.865000000000001,-0.860000000000001,
-0.855000000000001,-0.850000000000001,-0.845000000000001,-0.840000000000001,
-0.835000000000001,-0.830000000000001,-0.825000000000001,-0.820000000000001,
-0.815000000000001,-0.810000000000001,-0.805000000000001,-0.800000000000001,
-0.795000000000001,-0.790000000000001,-0.785000000000001,-0.780000000000001,
-0.775000000000001,-0.770000000000001,-0.765000000000001,-0.760000000000001,
-0.755000000000001,-0.750000000000001,-0.745000000000001,-0.740000000000001,
-0.735000000000001,-0.730000000000001,-0.725000000000001,-0.720000000000001,
-0.715000000000001,-0.710000000000001,-0.705000000000001,-0.700000000000001,
-0.695000000000001,-0.690000000000001,-0.685,-0.68,-0.675,-0.67,-0.665,
-0.66,-0.655,-0.65,-0.645,-0.64,-0.635,-0.63,-0.625,-0.62,-0.615,-0.61,
-0.605,-0.6,-0.595,-0.59,-0.585,-0.58,-0.575,-0.57,-0.565,-0.56,-0.555,
-0.55,-0.545,-0.54,-0.535,-0.53,-0.525,-0.52,-0.515,-0.51,-0.505,-0.5,-0.495,
-0.49,-0.485,-0.48,-0.475,-0.47,-0.465,-0.46,-0.455,-0.45,-0.445,-0.44,
-0.435,-0.43,-0.425,-0.42,-0.415,-0.41,-0.405,-0.4,-0.395,-0.39,-0.385,
-0.38,-0.375,-0.37,-0.365,-0.36,-0.355,-0.35,-0.345,-0.34,-0.335,-0.33,
-0.325,-0.32,-0.315,-0.31,-0.305,-0.3,-0.295,-0.29,-0.285,-0.28,-0.275,
-0.27,-0.265,-0.26,-0.255,-0.25,-0.245,-0.24,-0.235,-0.23,-0.225,-0.22,
-0.215,-0.21,-0.205,-0.2,-0.195,-0.19,-0.185,-0.18,-0.175,-0.17,-0.165,
-0.16,-0.155,-0.15,-0.145,-0.14,-0.135,-0.13,-0.125,-0.12,-0.115,-0.11,
-0.105,-0.1,-0.095,-0.09,-0.085,-0.08,-0.075,-0.07,-0.065,-0.06,-0.055,
-0.05,-0.045,-0.04,-0.035,-0.03,-0.025,-0.02,-0.015,-0.01,-0.005,0.),
 .UNSPECIFIED.)
CURVE()
GEOMETRIC_REPRESENTATION_ITEM()
RATIONAL_B_SPLINE_CURVE((1.,1.,1.,1.,1.,1.,1.,1.,1.,1.,1.,1.,1.,1.,1.,1.,
1.,1.,1.,1.,1.,1.,1.,1.,1.,1.,1.,1.,1.,1.,1.,1.,1.,1.,1.,1.,1.,1.,1.,1.,
1.,1.,1.,1.,1.,1.,1.,1.,1.,1.,1.,1.,1.,1.,1.,1.,1.,1.,1.,1.,1.,1.,1.,1.,
1.,1.,1.,1.,1.,1.,1.,1.,1.,1.,1.,1.,1.,1.,1.,1.,1.,1.,1.,1.,1.,1.,1.,1.,
1.,1.,1.,1.,1.,1.,1.,1.,1.,1.,1.,1.,1.,1.,1.,1.,1.,1.,1.,1.,1.,1.,1.,1.,
1.,1.,1.,1.,1.,1.,1.,1.,1.,1.,1.,1.,1.,1.,1.,1.,1.,1.,1.,1.,1.,1.,1.,1.,
1.,1.,1.,1.,1.,1.,1.,1.,1.,1.,1.,1.,1.,1.,1.,1.,1.,1.,1.,1.,1.,1.,1.,1.,
1.,1.,1.,1.,1.,1.,1.,1.,1.,1.,1.,1.,1.,1.,1.,1.,1.,1.,1.,1.,1.,1.,1.,1.,
1.,1.,1.,1.,1.,1.,1.,1.,1.,1.,1.,1.,1.,1.,1.,1.,1.,1.,1.,1.,1.))
REPRESENTATION_ITEM('')
);
#851=(
BOUNDED_CURVE()
B_SPLINE_CURVE(5,(#242851,#242852,#242853,#242854,#242855,#242856,#242857,
#242858,#242859,#242860,#242861,#242862,#242863,#242864,#242865,#242866,
#242867,#242868,#242869,#242870,#242871,#242872,#242873,#242874,#242875,
#242876,#242877,#242878,#242879,#242880,#242881,#242882,#242883,#242884,
#242885,#242886,#242887,#242888,#242889,#242890,#242891,#242892,#242893,
#242894,#242895,#242896,#242897,#242898,#242899,#242900,#242901,#242902,
#242903,#242904,#242905,#242906,#242907,#242908,#242909,#242910,#242911,
#242912,#242913,#242914,#242915,#242916,#242917,#242918,#242919,#242920,
#242921,#242922,#242923,#242924,#242925,#242926,#242927,#242928,#242929,
#242930,#242931,#242932,#242933,#242934,#242935,#242936,#242937,#242938,
#242939,#242940,#242941,#242942,#242943,#242944,#242945,#242946,#242947,
#242948,#242949,#242950,#242951,#242952,#242953,#242954,#242955,#242956,
#242957,#242958,#242959,#242960,#242961,#242962,#242963,#242964,#242965,
#242966,#242967,#242968,#242969,#242970,#242971,#242972,#242973,#242974,
#242975,#242976,#242977,#242978,#242979,#242980,#242981,#242982,#242983,
#242984,#242985,#242986,#242987,#242988,#242989,#242990,#242991,#242992,
#242993,#242994,#242995,#242996,#242997,#242998,#242999,#243000,#243001,
#243002,#243003,#243004,#243005,#243006,#243007,#243008,#243009,#243010,
#243011,#243012,#243013,#243014,#243015,#243016,#243017,#243018,#243019,
#243020,#243021,#243022,#243023,#243024,#243025,#243026,#243027,#243028,
#243029,#243030,#243031,#243032,#243033,#243034,#243035,#243036,#243037,
#243038,#243039,#243040,#243041,#243042,#243043,#243044,#243045,#243046,
#243047,#243048,#243049,#243050,#243051,#243052,#243053,#243054,#243055),
 .UNSPECIFIED.,.F.,.F.)
B_SPLINE_CURVE_WITH_KNOTS((6,1,1,1,1,1,1,1,1,1,1,1,1,1,1,1,1,1,1,1,1,1,
1,1,1,1,1,1,1,1,1,1,1,1,1,1,1,1,1,1,1,1,1,1,1,1,1,1,1,1,1,1,1,1,1,1,1,1,
1,1,1,1,1,1,1,1,1,1,1,1,1,1,1,1,1,1,1,1,1,1,1,1,1,1,1,1,1,1,1,1,1,1,1,1,
1,1,1,1,1,1,1,1,1,1,1,1,1,1,1,1,1,1,1,1,1,1,1,1,1,1,1,1,1,1,1,1,1,1,1,1,
1,1,1,1,1,1,1,1,1,1,1,1,1,1,1,1,1,1,1,1,1,1,1,1,1,1,1,1,1,1,1,1,1,1,1,1,
1,1,1,1,1,1,1,1,1,1,1,1,1,1,1,1,1,1,1,1,1,1,1,1,1,1,1,1,1,1,1,1,1,1,6),
(-1.,-0.995000000000001,-0.990000000000001,-0.985000000000001,-0.980000000000001,
-0.975000000000001,-0.970000000000001,-0.965000000000001,-0.960000000000001,
-0.955000000000001,-0.950000000000001,-0.945000000000001,-0.940000000000001,
-0.935000000000001,-0.930000000000001,-0.925000000000001,-0.920000000000001,
-0.915000000000001,-0.910000000000001,-0.905000000000001,-0.900000000000001,
-0.895000000000001,-0.890000000000001,-0.885000000000001,-0.880000000000001,
-0.875000000000001,-0.870000000000001,-0.865000000000001,-0.860000000000001,
-0.855000000000001,-0.850000000000001,-0.845000000000001,-0.840000000000001,
-0.835000000000001,-0.830000000000001,-0.825000000000001,-0.820000000000001,
-0.815000000000001,-0.810000000000001,-0.805000000000001,-0.800000000000001,
-0.795000000000001,-0.790000000000001,-0.785000000000001,-0.780000000000001,
-0.775000000000001,-0.770000000000001,-0.765000000000001,-0.760000000000001,
-0.755000000000001,-0.750000000000001,-0.745000000000001,-0.740000000000001,
-0.735000000000001,-0.730000000000001,-0.725000000000001,-0.720000000000001,
-0.715000000000001,-0.710000000000001,-0.705000000000001,-0.700000000000001,
-0.695000000000001,-0.690000000000001,-0.685,-0.68,-0.675,-0.67,-0.665,
-0.66,-0.655,-0.65,-0.645,-0.64,-0.635,-0.63,-0.625,-0.62,-0.615,-0.61,
-0.605,-0.6,-0.595,-0.59,-0.585,-0.58,-0.575,-0.57,-0.565,-0.56,-0.555,
-0.55,-0.545,-0.54,-0.535,-0.53,-0.525,-0.52,-0.515,-0.51,-0.505,-0.5,-0.495,
-0.49,-0.485,-0.48,-0.475,-0.47,-0.465,-0.46,-0.455,-0.45,-0.445,-0.44,
-0.435,-0.43,-0.425,-0.42,-0.415,-0.41,-0.405,-0.4,-0.395,-0.39,-0.385,
-0.38,-0.375,-0.37,-0.365,-0.36,-0.355,-0.35,-0.345,-0.34,-0.335,-0.33,
-0.325,-0.32,-0.315,-0.31,-0.305,-0.3,-0.295,-0.29,-0.285,-0.28,-0.275,
-0.27,-0.265,-0.26,-0.255,-0.25,-0.245,-0.24,-0.235,-0.23,-0.225,-0.22,
-0.215,-0.21,-0.205,-0.2,-0.195,-0.19,-0.185,-0.18,-0.175,-0.17,-0.165,
-0.16,-0.155,-0.15,-0.145,-0.14,-0.135,-0.13,-0.125,-0.12,-0.115,-0.11,
-0.105,-0.1,-0.095,-0.09,-0.085,-0.08,-0.075,-0.07,-0.065,-0.06,-0.055,
-0.05,-0.045,-0.04,-0.035,-0.03,-0.025,-0.02,-0.015,-0.01,-0.005,0.),
 .UNSPECIFIED.)
CURVE()
GEOMETRIC_REPRESENTATION_ITEM()
RATIONAL_B_SPLINE_CURVE((1.,1.,1.,1.,1.,1.,1.,1.,1.,1.,1.,1.,1.,1.,1.,1.,
1.,1.,1.,1.,1.,1.,1.,1.,1.,1.,1.,1.,1.,1.,1.,1.,1.,1.,1.,1.,1.,1.,1.,1.,
1.,1.,1.,1.,1.,1.,1.,1.,1.,1.,1.,1.,1.,1.,1.,1.,1.,1.,1.,1.,1.,1.,1.,1.,
1.,1.,1.,1.,1.,1.,1.,1.,1.,1.,1.,1.,1.,1.,1.,1.,1.,1.,1.,1.,1.,1.,1.,1.,
1.,1.,1.,1.,1.,1.,1.,1.,1.,1.,1.,1.,1.,1.,1.,1.,1.,1.,1.,1.,1.,1.,1.,1.,
1.,1.,1.,1.,1.,1.,1.,1.,1.,1.,1.,1.,1.,1.,1.,1.,1.,1.,1.,1.,1.,1.,1.,1.,
1.,1.,1.,1.,1.,1.,1.,1.,1.,1.,1.,1.,1.,1.,1.,1.,1.,1.,1.,1.,1.,1.,1.,1.,
1.,1.,1.,1.,1.,1.,1.,1.,1.,1.,1.,1.,1.,1.,1.,1.,1.,1.,1.,1.,1.,1.,1.,1.,
1.,1.,1.,1.,1.,1.,1.,1.,1.,1.,1.,1.,1.,1.,1.,1.,1.,1.,1.,1.,1.))
REPRESENTATION_ITEM('')
);
#852=(
BOUNDED_CURVE()
B_SPLINE_CURVE(5,(#243058,#243059,#243060,#243061,#243062,#243063,#243064,
#243065,#243066,#243067,#243068,#243069,#243070,#243071,#243072,#243073,
#243074,#243075,#243076,#243077,#243078,#243079,#243080,#243081,#243082,
#243083,#243084,#243085,#243086,#243087,#243088,#243089,#243090,#243091,
#243092,#243093,#243094,#243095,#243096,#243097,#243098,#243099,#243100,
#243101,#243102,#243103,#243104,#243105,#243106,#243107,#243108,#243109,
#243110,#243111,#243112,#243113,#243114,#243115,#243116,#243117,#243118,
#243119,#243120,#243121,#243122,#243123,#243124,#243125,#243126,#243127,
#243128,#243129,#243130,#243131,#243132,#243133,#243134,#243135,#243136,
#243137,#243138,#243139,#243140,#243141,#243142,#243143,#243144,#243145,
#243146,#243147,#243148,#243149,#243150,#243151,#243152,#243153,#243154,
#243155,#243156,#243157,#243158,#243159,#243160,#243161,#243162,#243163,
#243164,#243165,#243166,#243167,#243168,#243169,#243170,#243171,#243172,
#243173,#243174,#243175,#243176,#243177,#243178,#243179,#243180,#243181,
#243182,#243183,#243184,#243185,#243186,#243187,#243188,#243189,#243190,
#243191,#243192,#243193,#243194,#243195,#243196,#243197,#243198,#243199,
#243200,#243201,#243202,#243203,#243204,#243205,#243206,#243207,#243208,
#243209,#243210,#243211,#243212,#243213,#243214,#243215,#243216,#243217,
#243218,#243219,#243220,#243221,#243222,#243223,#243224,#243225,#243226,
#243227,#243228,#243229,#243230,#243231,#243232,#243233,#243234,#243235,
#243236,#243237,#243238,#243239,#243240,#243241,#243242,#243243,#243244,
#243245,#243246,#243247,#243248,#243249,#243250,#243251,#243252,#243253,
#243254,#243255,#243256,#243257,#243258,#243259,#243260,#243261,#243262),
 .UNSPECIFIED.,.F.,.F.)
B_SPLINE_CURVE_WITH_KNOTS((6,1,1,1,1,1,1,1,1,1,1,1,1,1,1,1,1,1,1,1,1,1,
1,1,1,1,1,1,1,1,1,1,1,1,1,1,1,1,1,1,1,1,1,1,1,1,1,1,1,1,1,1,1,1,1,1,1,1,
1,1,1,1,1,1,1,1,1,1,1,1,1,1,1,1,1,1,1,1,1,1,1,1,1,1,1,1,1,1,1,1,1,1,1,1,
1,1,1,1,1,1,1,1,1,1,1,1,1,1,1,1,1,1,1,1,1,1,1,1,1,1,1,1,1,1,1,1,1,1,1,1,
1,1,1,1,1,1,1,1,1,1,1,1,1,1,1,1,1,1,1,1,1,1,1,1,1,1,1,1,1,1,1,1,1,1,1,1,
1,1,1,1,1,1,1,1,1,1,1,1,1,1,1,1,1,1,1,1,1,1,1,1,1,1,1,1,1,1,1,1,1,1,6),
(0.,0.005,0.01,0.015,0.02,0.025,0.03,0.035,0.04,0.045,0.05,0.055,0.06,0.065,
0.07,0.075,0.08,0.085,0.09,0.095,0.1,0.105,0.11,0.115,0.12,0.125,0.13,0.135,
0.14,0.145,0.15,0.155,0.16,0.165,0.17,0.175,0.18,0.185,0.19,0.195,0.2,0.205,
0.21,0.215,0.22,0.225,0.23,0.235,0.24,0.245,0.25,0.255,0.26,0.265,0.27,
0.275,0.28,0.285,0.29,0.295,0.3,0.305,0.31,0.315,0.32,0.325,0.33,0.335,
0.34,0.345,0.35,0.355,0.36,0.365,0.37,0.375,0.38,0.385,0.39,0.395,0.4,0.405,
0.41,0.415,0.42,0.425,0.43,0.435,0.44,0.445,0.45,0.455,0.46,0.465,0.47,
0.475,0.48,0.485,0.49,0.495,0.5,0.505,0.51,0.515,0.52,0.525,0.53,0.535,
0.54,0.545,0.55,0.555,0.56,0.565,0.57,0.575,0.58,0.585,0.59,0.595,0.6,0.605,
0.61,0.615,0.62,0.625,0.63,0.635,0.64,0.645,0.65,0.655,0.66,0.665,0.67,
0.675,0.68,0.685,0.690000000000001,0.695000000000001,0.700000000000001,
0.705000000000001,0.710000000000001,0.715000000000001,0.720000000000001,
0.725000000000001,0.730000000000001,0.735000000000001,0.740000000000001,
0.745000000000001,0.750000000000001,0.755000000000001,0.760000000000001,
0.765000000000001,0.770000000000001,0.775000000000001,0.780000000000001,
0.785000000000001,0.790000000000001,0.795000000000001,0.800000000000001,
0.805000000000001,0.810000000000001,0.815000000000001,0.820000000000001,
0.825000000000001,0.830000000000001,0.835000000000001,0.840000000000001,
0.845000000000001,0.850000000000001,0.855000000000001,0.860000000000001,
0.865000000000001,0.870000000000001,0.875000000000001,0.880000000000001,
0.885000000000001,0.890000000000001,0.895000000000001,0.900000000000001,
0.905000000000001,0.910000000000001,0.915000000000001,0.920000000000001,
0.925000000000001,0.930000000000001,0.935000000000001,0.940000000000001,
0.945000000000001,0.950000000000001,0.955000000000001,0.960000000000001,
0.965000000000001,0.970000000000001,0.975000000000001,0.980000000000001,
0.985000000000001,0.990000000000001,0.995000000000001,1.),.UNSPECIFIED.)
CURVE()
GEOMETRIC_REPRESENTATION_ITEM()
RATIONAL_B_SPLINE_CURVE((1.,1.,1.,1.,1.,1.,1.,1.,1.,1.,1.,1.,1.,1.,1.,1.,
1.,1.,1.,1.,1.,1.,1.,1.,1.,1.,1.,1.,1.,1.,1.,1.,1.,1.,1.,1.,1.,1.,1.,1.,
1.,1.,1.,1.,1.,1.,1.,1.,1.,1.,1.,1.,1.,1.,1.,1.,1.,1.,1.,1.,1.,1.,1.,1.,
1.,1.,1.,1.,1.,1.,1.,1.,1.,1.,1.,1.,1.,1.,1.,1.,1.,1.,1.,1.,1.,1.,1.,1.,
1.,1.,1.,1.,1.,1.,1.,1.,1.,1.,1.,1.,1.,1.,1.,1.,1.,1.,1.,1.,1.,1.,1.,1.,
1.,1.,1.,1.,1.,1.,1.,1.,1.,1.,1.,1.,1.,1.,1.,1.,1.,1.,1.,1.,1.,1.,1.,1.,
1.,1.,1.,1.,1.,1.,1.,1.,1.,1.,1.,1.,1.,1.,1.,1.,1.,1.,1.,1.,1.,1.,1.,1.,
1.,1.,1.,1.,1.,1.,1.,1.,1.,1.,1.,1.,1.,1.,1.,1.,1.,1.,1.,1.,1.,1.,1.,1.,
1.,1.,1.,1.,1.,1.,1.,1.,1.,1.,1.,1.,1.,1.,1.,1.,1.,1.,1.,1.,1.))
REPRESENTATION_ITEM('')
);
#853=(
BOUNDED_CURVE()
B_SPLINE_CURVE(5,(#243674,#243675,#243676,#243677,#243678,#243679,#243680,
#243681,#243682,#243683,#243684,#243685,#243686,#243687,#243688,#243689,
#243690,#243691,#243692,#243693,#243694,#243695,#243696,#243697,#243698,
#243699,#243700,#243701,#243702,#243703,#243704,#243705,#243706,#243707,
#243708,#243709,#243710,#243711,#243712,#243713,#243714,#243715,#243716,
#243717,#243718,#243719,#243720,#243721,#243722,#243723,#243724,#243725,
#243726,#243727,#243728,#243729,#243730,#243731,#243732,#243733,#243734,
#243735,#243736,#243737,#243738,#243739,#243740,#243741,#243742,#243743,
#243744,#243745,#243746,#243747,#243748,#243749,#243750,#243751,#243752,
#243753,#243754,#243755,#243756,#243757,#243758,#243759,#243760,#243761,
#243762,#243763,#243764,#243765,#243766,#243767,#243768,#243769,#243770,
#243771,#243772,#243773,#243774,#243775,#243776,#243777,#243778,#243779,
#243780,#243781,#243782,#243783,#243784,#243785,#243786,#243787,#243788,
#243789,#243790,#243791,#243792,#243793,#243794,#243795,#243796,#243797,
#243798,#243799,#243800,#243801,#243802,#243803,#243804,#243805,#243806,
#243807,#243808,#243809,#243810,#243811,#243812,#243813,#243814,#243815,
#243816,#243817,#243818,#243819,#243820,#243821,#243822,#243823,#243824,
#243825,#243826,#243827,#243828,#243829,#243830,#243831,#243832,#243833,
#243834,#243835,#243836,#243837,#243838,#243839,#243840,#243841,#243842,
#243843,#243844,#243845,#243846,#243847,#243848,#243849,#243850,#243851,
#243852,#243853,#243854,#243855,#243856,#243857,#243858,#243859,#243860,
#243861,#243862,#243863,#243864,#243865,#243866,#243867,#243868,#243869,
#243870,#243871,#243872,#243873,#243874,#243875,#243876,#243877,#243878),
 .UNSPECIFIED.,.F.,.F.)
B_SPLINE_CURVE_WITH_KNOTS((6,1,1,1,1,1,1,1,1,1,1,1,1,1,1,1,1,1,1,1,1,1,
1,1,1,1,1,1,1,1,1,1,1,1,1,1,1,1,1,1,1,1,1,1,1,1,1,1,1,1,1,1,1,1,1,1,1,1,
1,1,1,1,1,1,1,1,1,1,1,1,1,1,1,1,1,1,1,1,1,1,1,1,1,1,1,1,1,1,1,1,1,1,1,1,
1,1,1,1,1,1,1,1,1,1,1,1,1,1,1,1,1,1,1,1,1,1,1,1,1,1,1,1,1,1,1,1,1,1,1,1,
1,1,1,1,1,1,1,1,1,1,1,1,1,1,1,1,1,1,1,1,1,1,1,1,1,1,1,1,1,1,1,1,1,1,1,1,
1,1,1,1,1,1,1,1,1,1,1,1,1,1,1,1,1,1,1,1,1,1,1,1,1,1,1,1,1,1,1,1,1,1,6),
(0.,0.005,0.01,0.015,0.02,0.025,0.03,0.035,0.04,0.045,0.05,0.055,0.06,0.065,
0.07,0.075,0.08,0.085,0.09,0.095,0.1,0.105,0.11,0.115,0.12,0.125,0.13,0.135,
0.14,0.145,0.15,0.155,0.16,0.165,0.17,0.175,0.18,0.185,0.19,0.195,0.2,0.205,
0.21,0.215,0.22,0.225,0.23,0.235,0.24,0.245,0.25,0.255,0.26,0.265,0.27,
0.275,0.28,0.285,0.29,0.295,0.3,0.305,0.31,0.315,0.32,0.325,0.33,0.335,
0.34,0.345,0.35,0.355,0.36,0.365,0.37,0.375,0.38,0.385,0.39,0.395,0.4,0.405,
0.41,0.415,0.42,0.425,0.43,0.435,0.44,0.445,0.45,0.455,0.46,0.465,0.47,
0.475,0.48,0.485,0.49,0.495,0.5,0.505,0.51,0.515,0.52,0.525,0.53,0.535,
0.54,0.545,0.55,0.555,0.56,0.565,0.57,0.575,0.58,0.585,0.59,0.595,0.6,0.605,
0.61,0.615,0.62,0.625,0.63,0.635,0.64,0.645,0.65,0.655,0.66,0.665,0.67,
0.675,0.68,0.685,0.690000000000001,0.695000000000001,0.700000000000001,
0.705000000000001,0.710000000000001,0.715000000000001,0.720000000000001,
0.725000000000001,0.730000000000001,0.735000000000001,0.740000000000001,
0.745000000000001,0.750000000000001,0.755000000000001,0.760000000000001,
0.765000000000001,0.770000000000001,0.775000000000001,0.780000000000001,
0.785000000000001,0.790000000000001,0.795000000000001,0.800000000000001,
0.805000000000001,0.810000000000001,0.815000000000001,0.820000000000001,
0.825000000000001,0.830000000000001,0.835000000000001,0.840000000000001,
0.845000000000001,0.850000000000001,0.855000000000001,0.860000000000001,
0.865000000000001,0.870000000000001,0.875000000000001,0.880000000000001,
0.885000000000001,0.890000000000001,0.895000000000001,0.900000000000001,
0.905000000000001,0.910000000000001,0.915000000000001,0.920000000000001,
0.925000000000001,0.930000000000001,0.935000000000001,0.940000000000001,
0.945000000000001,0.950000000000001,0.955000000000001,0.960000000000001,
0.965000000000001,0.970000000000001,0.975000000000001,0.980000000000001,
0.985000000000001,0.990000000000001,0.995000000000001,1.),.UNSPECIFIED.)
CURVE()
GEOMETRIC_REPRESENTATION_ITEM()
RATIONAL_B_SPLINE_CURVE((1.,1.,1.,1.,1.,1.,1.,1.,1.,1.,1.,1.,1.,1.,1.,1.,
1.,1.,1.,1.,1.,1.,1.,1.,1.,1.,1.,1.,1.,1.,1.,1.,1.,1.,1.,1.,1.,1.,1.,1.,
1.,1.,1.,1.,1.,1.,1.,1.,1.,1.,1.,1.,1.,1.,1.,1.,1.,1.,1.,1.,1.,1.,1.,1.,
1.,1.,1.,1.,1.,1.,1.,1.,1.,1.,1.,1.,1.,1.,1.,1.,1.,1.,1.,1.,1.,1.,1.,1.,
1.,1.,1.,1.,1.,1.,1.,1.,1.,1.,1.,1.,1.,1.,1.,1.,1.,1.,1.,1.,1.,1.,1.,1.,
1.,1.,1.,1.,1.,1.,1.,1.,1.,1.,1.,1.,1.,1.,1.,1.,1.,1.,1.,1.,1.,1.,1.,1.,
1.,1.,1.,1.,1.,1.,1.,1.,1.,1.,1.,1.,1.,1.,1.,1.,1.,1.,1.,1.,1.,1.,1.,1.,
1.,1.,1.,1.,1.,1.,1.,1.,1.,1.,1.,1.,1.,1.,1.,1.,1.,1.,1.,1.,1.,1.,1.,1.,
1.,1.,1.,1.,1.,1.,1.,1.,1.,1.,1.,1.,1.,1.,1.,1.,1.,1.,1.,1.,1.))
REPRESENTATION_ITEM('')
);
#854=(
BOUNDED_CURVE()
B_SPLINE_CURVE(5,(#243880,#243881,#243882,#243883,#243884,#243885,#243886,
#243887,#243888,#243889,#243890,#243891,#243892,#243893,#243894,#243895,
#243896,#243897,#243898,#243899,#243900,#243901,#243902,#243903,#243904,
#243905,#243906,#243907,#243908,#243909,#243910,#243911,#243912,#243913,
#243914,#243915,#243916,#243917,#243918,#243919,#243920,#243921,#243922,
#243923,#243924,#243925,#243926,#243927,#243928,#243929,#243930,#243931,
#243932,#243933,#243934,#243935,#243936,#243937,#243938,#243939,#243940,
#243941,#243942,#243943,#243944,#243945,#243946,#243947,#243948,#243949,
#243950,#243951,#243952,#243953,#243954,#243955,#243956,#243957,#243958,
#243959,#243960,#243961,#243962,#243963,#243964,#243965,#243966,#243967,
#243968,#243969,#243970,#243971,#243972,#243973,#243974,#243975,#243976,
#243977,#243978,#243979,#243980,#243981,#243982,#243983,#243984,#243985,
#243986,#243987,#243988,#243989,#243990,#243991,#243992,#243993,#243994,
#243995,#243996,#243997,#243998,#243999,#244000,#244001,#244002,#244003,
#244004,#244005,#244006,#244007,#244008,#244009,#244010,#244011,#244012,
#244013,#244014,#244015,#244016,#244017,#244018,#244019,#244020,#244021,
#244022,#244023,#244024,#244025,#244026,#244027,#244028,#244029,#244030,
#244031,#244032,#244033,#244034,#244035,#244036,#244037,#244038,#244039,
#244040,#244041,#244042,#244043,#244044,#244045,#244046,#244047,#244048,
#244049,#244050,#244051,#244052,#244053,#244054,#244055,#244056,#244057,
#244058,#244059,#244060,#244061,#244062,#244063,#244064,#244065,#244066,
#244067,#244068,#244069,#244070,#244071,#244072,#244073,#244074,#244075,
#244076,#244077,#244078,#244079,#244080,#244081,#244082,#244083,#244084),
 .UNSPECIFIED.,.F.,.F.)
B_SPLINE_CURVE_WITH_KNOTS((6,1,1,1,1,1,1,1,1,1,1,1,1,1,1,1,1,1,1,1,1,1,
1,1,1,1,1,1,1,1,1,1,1,1,1,1,1,1,1,1,1,1,1,1,1,1,1,1,1,1,1,1,1,1,1,1,1,1,
1,1,1,1,1,1,1,1,1,1,1,1,1,1,1,1,1,1,1,1,1,1,1,1,1,1,1,1,1,1,1,1,1,1,1,1,
1,1,1,1,1,1,1,1,1,1,1,1,1,1,1,1,1,1,1,1,1,1,1,1,1,1,1,1,1,1,1,1,1,1,1,1,
1,1,1,1,1,1,1,1,1,1,1,1,1,1,1,1,1,1,1,1,1,1,1,1,1,1,1,1,1,1,1,1,1,1,1,1,
1,1,1,1,1,1,1,1,1,1,1,1,1,1,1,1,1,1,1,1,1,1,1,1,1,1,1,1,1,1,1,1,1,1,6),
(-1.,-0.995000000000001,-0.990000000000001,-0.985000000000001,-0.980000000000001,
-0.975000000000001,-0.970000000000001,-0.965000000000001,-0.960000000000001,
-0.955000000000001,-0.950000000000001,-0.945000000000001,-0.940000000000001,
-0.935000000000001,-0.930000000000001,-0.925000000000001,-0.920000000000001,
-0.915000000000001,-0.910000000000001,-0.905000000000001,-0.900000000000001,
-0.895000000000001,-0.890000000000001,-0.885000000000001,-0.880000000000001,
-0.875000000000001,-0.870000000000001,-0.865000000000001,-0.860000000000001,
-0.855000000000001,-0.850000000000001,-0.845000000000001,-0.840000000000001,
-0.835000000000001,-0.830000000000001,-0.825000000000001,-0.820000000000001,
-0.815000000000001,-0.810000000000001,-0.805000000000001,-0.800000000000001,
-0.795000000000001,-0.790000000000001,-0.785000000000001,-0.780000000000001,
-0.775000000000001,-0.770000000000001,-0.765000000000001,-0.760000000000001,
-0.755000000000001,-0.750000000000001,-0.745000000000001,-0.740000000000001,
-0.735000000000001,-0.730000000000001,-0.725000000000001,-0.720000000000001,
-0.715000000000001,-0.710000000000001,-0.705000000000001,-0.700000000000001,
-0.695000000000001,-0.690000000000001,-0.685,-0.68,-0.675,-0.67,-0.665,
-0.66,-0.655,-0.65,-0.645,-0.64,-0.635,-0.63,-0.625,-0.62,-0.615,-0.61,
-0.605,-0.6,-0.595,-0.59,-0.585,-0.58,-0.575,-0.57,-0.565,-0.56,-0.555,
-0.55,-0.545,-0.54,-0.535,-0.53,-0.525,-0.52,-0.515,-0.51,-0.505,-0.5,-0.495,
-0.49,-0.485,-0.48,-0.475,-0.47,-0.465,-0.46,-0.455,-0.45,-0.445,-0.44,
-0.435,-0.43,-0.425,-0.42,-0.415,-0.41,-0.405,-0.4,-0.395,-0.39,-0.385,
-0.38,-0.375,-0.37,-0.365,-0.36,-0.355,-0.35,-0.345,-0.34,-0.335,-0.33,
-0.325,-0.32,-0.315,-0.31,-0.305,-0.3,-0.295,-0.29,-0.285,-0.28,-0.275,
-0.27,-0.265,-0.26,-0.255,-0.25,-0.245,-0.24,-0.235,-0.23,-0.225,-0.22,
-0.215,-0.21,-0.205,-0.2,-0.195,-0.19,-0.185,-0.18,-0.175,-0.17,-0.165,
-0.16,-0.155,-0.15,-0.145,-0.14,-0.135,-0.13,-0.125,-0.12,-0.115,-0.11,
-0.105,-0.1,-0.095,-0.09,-0.085,-0.08,-0.075,-0.07,-0.065,-0.06,-0.055,
-0.05,-0.045,-0.04,-0.035,-0.03,-0.025,-0.02,-0.015,-0.01,-0.005,0.),
 .UNSPECIFIED.)
CURVE()
GEOMETRIC_REPRESENTATION_ITEM()
RATIONAL_B_SPLINE_CURVE((1.,1.,1.,1.,1.,1.,1.,1.,1.,1.,1.,1.,1.,1.,1.,1.,
1.,1.,1.,1.,1.,1.,1.,1.,1.,1.,1.,1.,1.,1.,1.,1.,1.,1.,1.,1.,1.,1.,1.,1.,
1.,1.,1.,1.,1.,1.,1.,1.,1.,1.,1.,1.,1.,1.,1.,1.,1.,1.,1.,1.,1.,1.,1.,1.,
1.,1.,1.,1.,1.,1.,1.,1.,1.,1.,1.,1.,1.,1.,1.,1.,1.,1.,1.,1.,1.,1.,1.,1.,
1.,1.,1.,1.,1.,1.,1.,1.,1.,1.,1.,1.,1.,1.,1.,1.,1.,1.,1.,1.,1.,1.,1.,1.,
1.,1.,1.,1.,1.,1.,1.,1.,1.,1.,1.,1.,1.,1.,1.,1.,1.,1.,1.,1.,1.,1.,1.,1.,
1.,1.,1.,1.,1.,1.,1.,1.,1.,1.,1.,1.,1.,1.,1.,1.,1.,1.,1.,1.,1.,1.,1.,1.,
1.,1.,1.,1.,1.,1.,1.,1.,1.,1.,1.,1.,1.,1.,1.,1.,1.,1.,1.,1.,1.,1.,1.,1.,
1.,1.,1.,1.,1.,1.,1.,1.,1.,1.,1.,1.,1.,1.,1.,1.,1.,1.,1.,1.,1.))
REPRESENTATION_ITEM('')
);
#855=(
BOUNDED_CURVE()
B_SPLINE_CURVE(5,(#244503,#244504,#244505,#244506,#244507,#244508,#244509,
#244510,#244511,#244512,#244513,#244514,#244515,#244516,#244517,#244518,
#244519,#244520,#244521,#244522,#244523,#244524,#244525,#244526,#244527,
#244528,#244529,#244530,#244531,#244532,#244533,#244534,#244535,#244536,
#244537,#244538,#244539,#244540,#244541,#244542,#244543,#244544,#244545,
#244546,#244547,#244548,#244549,#244550,#244551,#244552,#244553,#244554,
#244555,#244556,#244557,#244558,#244559,#244560,#244561,#244562,#244563,
#244564,#244565,#244566,#244567,#244568,#244569,#244570,#244571,#244572,
#244573,#244574,#244575,#244576,#244577,#244578,#244579,#244580,#244581,
#244582,#244583,#244584,#244585,#244586,#244587,#244588,#244589,#244590,
#244591,#244592,#244593,#244594,#244595,#244596,#244597,#244598,#244599,
#244600,#244601,#244602,#244603,#244604,#244605,#244606,#244607,#244608,
#244609,#244610,#244611,#244612,#244613,#244614,#244615,#244616,#244617,
#244618,#244619,#244620,#244621,#244622,#244623,#244624,#244625,#244626,
#244627,#244628,#244629,#244630,#244631,#244632,#244633,#244634,#244635,
#244636,#244637,#244638,#244639,#244640,#244641,#244642,#244643,#244644,
#244645,#244646,#244647,#244648,#244649,#244650,#244651,#244652,#244653,
#244654,#244655,#244656,#244657,#244658,#244659,#244660,#244661,#244662,
#244663,#244664,#244665,#244666,#244667,#244668,#244669,#244670,#244671,
#244672,#244673,#244674,#244675,#244676,#244677,#244678,#244679,#244680,
#244681,#244682,#244683,#244684,#244685,#244686,#244687,#244688,#244689,
#244690,#244691,#244692,#244693,#244694,#244695,#244696,#244697,#244698,
#244699,#244700,#244701,#244702,#244703,#244704,#244705,#244706,#244707),
 .UNSPECIFIED.,.F.,.F.)
B_SPLINE_CURVE_WITH_KNOTS((6,1,1,1,1,1,1,1,1,1,1,1,1,1,1,1,1,1,1,1,1,1,
1,1,1,1,1,1,1,1,1,1,1,1,1,1,1,1,1,1,1,1,1,1,1,1,1,1,1,1,1,1,1,1,1,1,1,1,
1,1,1,1,1,1,1,1,1,1,1,1,1,1,1,1,1,1,1,1,1,1,1,1,1,1,1,1,1,1,1,1,1,1,1,1,
1,1,1,1,1,1,1,1,1,1,1,1,1,1,1,1,1,1,1,1,1,1,1,1,1,1,1,1,1,1,1,1,1,1,1,1,
1,1,1,1,1,1,1,1,1,1,1,1,1,1,1,1,1,1,1,1,1,1,1,1,1,1,1,1,1,1,1,1,1,1,1,1,
1,1,1,1,1,1,1,1,1,1,1,1,1,1,1,1,1,1,1,1,1,1,1,1,1,1,1,1,1,1,1,1,1,1,6),
(-1.,-0.995000000000001,-0.990000000000001,-0.985000000000001,-0.980000000000001,
-0.975000000000001,-0.970000000000001,-0.965000000000001,-0.960000000000001,
-0.955000000000001,-0.950000000000001,-0.945000000000001,-0.940000000000001,
-0.935000000000001,-0.930000000000001,-0.925000000000001,-0.920000000000001,
-0.915000000000001,-0.910000000000001,-0.905000000000001,-0.900000000000001,
-0.895000000000001,-0.890000000000001,-0.885000000000001,-0.880000000000001,
-0.875000000000001,-0.870000000000001,-0.865000000000001,-0.860000000000001,
-0.855000000000001,-0.850000000000001,-0.845000000000001,-0.840000000000001,
-0.835000000000001,-0.830000000000001,-0.825000000000001,-0.820000000000001,
-0.815000000000001,-0.810000000000001,-0.805000000000001,-0.800000000000001,
-0.795000000000001,-0.790000000000001,-0.785000000000001,-0.780000000000001,
-0.775000000000001,-0.770000000000001,-0.765000000000001,-0.760000000000001,
-0.755000000000001,-0.750000000000001,-0.745000000000001,-0.740000000000001,
-0.735000000000001,-0.730000000000001,-0.725000000000001,-0.720000000000001,
-0.715000000000001,-0.710000000000001,-0.705000000000001,-0.700000000000001,
-0.695000000000001,-0.690000000000001,-0.685,-0.68,-0.675,-0.67,-0.665,
-0.66,-0.655,-0.65,-0.645,-0.64,-0.635,-0.63,-0.625,-0.62,-0.615,-0.61,
-0.605,-0.6,-0.595,-0.59,-0.585,-0.58,-0.575,-0.57,-0.565,-0.56,-0.555,
-0.55,-0.545,-0.54,-0.535,-0.53,-0.525,-0.52,-0.515,-0.51,-0.505,-0.5,-0.495,
-0.49,-0.485,-0.48,-0.475,-0.47,-0.465,-0.46,-0.455,-0.45,-0.445,-0.44,
-0.435,-0.43,-0.425,-0.42,-0.415,-0.41,-0.405,-0.4,-0.395,-0.39,-0.385,
-0.38,-0.375,-0.37,-0.365,-0.36,-0.355,-0.35,-0.345,-0.34,-0.335,-0.33,
-0.325,-0.32,-0.315,-0.31,-0.305,-0.3,-0.295,-0.29,-0.285,-0.28,-0.275,
-0.27,-0.265,-0.26,-0.255,-0.25,-0.245,-0.24,-0.235,-0.23,-0.225,-0.22,
-0.215,-0.21,-0.205,-0.2,-0.195,-0.19,-0.185,-0.18,-0.175,-0.17,-0.165,
-0.16,-0.155,-0.15,-0.145,-0.14,-0.135,-0.13,-0.125,-0.12,-0.115,-0.11,
-0.105,-0.1,-0.095,-0.09,-0.085,-0.08,-0.075,-0.07,-0.065,-0.06,-0.055,
-0.05,-0.045,-0.04,-0.035,-0.03,-0.025,-0.02,-0.015,-0.01,-0.005,0.),
 .UNSPECIFIED.)
CURVE()
GEOMETRIC_REPRESENTATION_ITEM()
RATIONAL_B_SPLINE_CURVE((1.,1.,1.,1.,1.,1.,1.,1.,1.,1.,1.,1.,1.,1.,1.,1.,
1.,1.,1.,1.,1.,1.,1.,1.,1.,1.,1.,1.,1.,1.,1.,1.,1.,1.,1.,1.,1.,1.,1.,1.,
1.,1.,1.,1.,1.,1.,1.,1.,1.,1.,1.,1.,1.,1.,1.,1.,1.,1.,1.,1.,1.,1.,1.,1.,
1.,1.,1.,1.,1.,1.,1.,1.,1.,1.,1.,1.,1.,1.,1.,1.,1.,1.,1.,1.,1.,1.,1.,1.,
1.,1.,1.,1.,1.,1.,1.,1.,1.,1.,1.,1.,1.,1.,1.,1.,1.,1.,1.,1.,1.,1.,1.,1.,
1.,1.,1.,1.,1.,1.,1.,1.,1.,1.,1.,1.,1.,1.,1.,1.,1.,1.,1.,1.,1.,1.,1.,1.,
1.,1.,1.,1.,1.,1.,1.,1.,1.,1.,1.,1.,1.,1.,1.,1.,1.,1.,1.,1.,1.,1.,1.,1.,
1.,1.,1.,1.,1.,1.,1.,1.,1.,1.,1.,1.,1.,1.,1.,1.,1.,1.,1.,1.,1.,1.,1.,1.,
1.,1.,1.,1.,1.,1.,1.,1.,1.,1.,1.,1.,1.,1.,1.,1.,1.,1.,1.,1.,1.))
REPRESENTATION_ITEM('')
);
#856=(
BOUNDED_CURVE()
B_SPLINE_CURVE(5,(#244710,#244711,#244712,#244713,#244714,#244715,#244716,
#244717,#244718,#244719,#244720,#244721,#244722,#244723,#244724,#244725,
#244726,#244727,#244728,#244729,#244730,#244731,#244732,#244733,#244734,
#244735,#244736,#244737,#244738,#244739,#244740,#244741,#244742,#244743,
#244744,#244745,#244746,#244747,#244748,#244749,#244750,#244751,#244752,
#244753,#244754,#244755,#244756,#244757,#244758,#244759,#244760,#244761,
#244762,#244763,#244764,#244765,#244766,#244767,#244768,#244769,#244770,
#244771,#244772,#244773,#244774,#244775,#244776,#244777,#244778,#244779,
#244780,#244781,#244782,#244783,#244784,#244785,#244786,#244787,#244788,
#244789,#244790,#244791,#244792,#244793,#244794,#244795,#244796,#244797,
#244798,#244799,#244800,#244801,#244802,#244803,#244804,#244805,#244806,
#244807,#244808,#244809,#244810,#244811,#244812,#244813,#244814,#244815,
#244816,#244817,#244818,#244819,#244820,#244821,#244822,#244823,#244824,
#244825,#244826,#244827,#244828,#244829,#244830,#244831,#244832,#244833,
#244834,#244835,#244836,#244837,#244838,#244839,#244840,#244841,#244842,
#244843,#244844,#244845,#244846,#244847,#244848,#244849,#244850,#244851,
#244852,#244853,#244854,#244855,#244856,#244857,#244858,#244859,#244860,
#244861,#244862,#244863,#244864,#244865,#244866,#244867,#244868,#244869,
#244870,#244871,#244872,#244873,#244874,#244875,#244876,#244877,#244878,
#244879,#244880,#244881,#244882,#244883,#244884,#244885,#244886,#244887,
#244888,#244889,#244890,#244891,#244892,#244893,#244894,#244895,#244896,
#244897,#244898,#244899,#244900,#244901,#244902,#244903,#244904,#244905,
#244906,#244907,#244908,#244909,#244910,#244911,#244912,#244913,#244914),
 .UNSPECIFIED.,.F.,.F.)
B_SPLINE_CURVE_WITH_KNOTS((6,1,1,1,1,1,1,1,1,1,1,1,1,1,1,1,1,1,1,1,1,1,
1,1,1,1,1,1,1,1,1,1,1,1,1,1,1,1,1,1,1,1,1,1,1,1,1,1,1,1,1,1,1,1,1,1,1,1,
1,1,1,1,1,1,1,1,1,1,1,1,1,1,1,1,1,1,1,1,1,1,1,1,1,1,1,1,1,1,1,1,1,1,1,1,
1,1,1,1,1,1,1,1,1,1,1,1,1,1,1,1,1,1,1,1,1,1,1,1,1,1,1,1,1,1,1,1,1,1,1,1,
1,1,1,1,1,1,1,1,1,1,1,1,1,1,1,1,1,1,1,1,1,1,1,1,1,1,1,1,1,1,1,1,1,1,1,1,
1,1,1,1,1,1,1,1,1,1,1,1,1,1,1,1,1,1,1,1,1,1,1,1,1,1,1,1,1,1,1,1,1,1,6),
(0.,0.005,0.01,0.015,0.02,0.025,0.03,0.035,0.04,0.045,0.05,0.055,0.06,0.065,
0.07,0.075,0.08,0.085,0.09,0.095,0.1,0.105,0.11,0.115,0.12,0.125,0.13,0.135,
0.14,0.145,0.15,0.155,0.16,0.165,0.17,0.175,0.18,0.185,0.19,0.195,0.2,0.205,
0.21,0.215,0.22,0.225,0.23,0.235,0.24,0.245,0.25,0.255,0.26,0.265,0.27,
0.275,0.28,0.285,0.29,0.295,0.3,0.305,0.31,0.315,0.32,0.325,0.33,0.335,
0.34,0.345,0.35,0.355,0.36,0.365,0.37,0.375,0.38,0.385,0.39,0.395,0.4,0.405,
0.41,0.415,0.42,0.425,0.43,0.435,0.44,0.445,0.45,0.455,0.46,0.465,0.47,
0.475,0.48,0.485,0.49,0.495,0.5,0.505,0.51,0.515,0.52,0.525,0.53,0.535,
0.54,0.545,0.55,0.555,0.56,0.565,0.57,0.575,0.58,0.585,0.59,0.595,0.6,0.605,
0.61,0.615,0.62,0.625,0.63,0.635,0.64,0.645,0.65,0.655,0.66,0.665,0.67,
0.675,0.68,0.685,0.690000000000001,0.695000000000001,0.700000000000001,
0.705000000000001,0.710000000000001,0.715000000000001,0.720000000000001,
0.725000000000001,0.730000000000001,0.735000000000001,0.740000000000001,
0.745000000000001,0.750000000000001,0.755000000000001,0.760000000000001,
0.765000000000001,0.770000000000001,0.775000000000001,0.780000000000001,
0.785000000000001,0.790000000000001,0.795000000000001,0.800000000000001,
0.805000000000001,0.810000000000001,0.815000000000001,0.820000000000001,
0.825000000000001,0.830000000000001,0.835000000000001,0.840000000000001,
0.845000000000001,0.850000000000001,0.855000000000001,0.860000000000001,
0.865000000000001,0.870000000000001,0.875000000000001,0.880000000000001,
0.885000000000001,0.890000000000001,0.895000000000001,0.900000000000001,
0.905000000000001,0.910000000000001,0.915000000000001,0.920000000000001,
0.925000000000001,0.930000000000001,0.935000000000001,0.940000000000001,
0.945000000000001,0.950000000000001,0.955000000000001,0.960000000000001,
0.965000000000001,0.970000000000001,0.975000000000001,0.980000000000001,
0.985000000000001,0.990000000000001,0.995000000000001,1.),.UNSPECIFIED.)
CURVE()
GEOMETRIC_REPRESENTATION_ITEM()
RATIONAL_B_SPLINE_CURVE((1.,1.,1.,1.,1.,1.,1.,1.,1.,1.,1.,1.,1.,1.,1.,1.,
1.,1.,1.,1.,1.,1.,1.,1.,1.,1.,1.,1.,1.,1.,1.,1.,1.,1.,1.,1.,1.,1.,1.,1.,
1.,1.,1.,1.,1.,1.,1.,1.,1.,1.,1.,1.,1.,1.,1.,1.,1.,1.,1.,1.,1.,1.,1.,1.,
1.,1.,1.,1.,1.,1.,1.,1.,1.,1.,1.,1.,1.,1.,1.,1.,1.,1.,1.,1.,1.,1.,1.,1.,
1.,1.,1.,1.,1.,1.,1.,1.,1.,1.,1.,1.,1.,1.,1.,1.,1.,1.,1.,1.,1.,1.,1.,1.,
1.,1.,1.,1.,1.,1.,1.,1.,1.,1.,1.,1.,1.,1.,1.,1.,1.,1.,1.,1.,1.,1.,1.,1.,
1.,1.,1.,1.,1.,1.,1.,1.,1.,1.,1.,1.,1.,1.,1.,1.,1.,1.,1.,1.,1.,1.,1.,1.,
1.,1.,1.,1.,1.,1.,1.,1.,1.,1.,1.,1.,1.,1.,1.,1.,1.,1.,1.,1.,1.,1.,1.,1.,
1.,1.,1.,1.,1.,1.,1.,1.,1.,1.,1.,1.,1.,1.,1.,1.,1.,1.,1.,1.,1.))
REPRESENTATION_ITEM('')
);
#857=(
BOUNDED_CURVE()
B_SPLINE_CURVE(5,(#245326,#245327,#245328,#245329,#245330,#245331,#245332,
#245333,#245334,#245335,#245336,#245337,#245338,#245339,#245340,#245341,
#245342,#245343,#245344,#245345,#245346,#245347,#245348,#245349,#245350,
#245351,#245352,#245353,#245354,#245355,#245356,#245357,#245358,#245359,
#245360,#245361,#245362,#245363,#245364,#245365,#245366,#245367,#245368,
#245369,#245370,#245371,#245372,#245373,#245374,#245375,#245376,#245377,
#245378,#245379,#245380,#245381,#245382,#245383,#245384,#245385,#245386,
#245387,#245388,#245389,#245390,#245391,#245392,#245393,#245394,#245395,
#245396,#245397,#245398,#245399,#245400,#245401,#245402,#245403,#245404,
#245405,#245406,#245407,#245408,#245409,#245410,#245411,#245412,#245413,
#245414,#245415,#245416,#245417,#245418,#245419,#245420,#245421,#245422,
#245423,#245424,#245425,#245426,#245427,#245428,#245429,#245430,#245431,
#245432,#245433,#245434,#245435,#245436,#245437,#245438,#245439,#245440,
#245441,#245442,#245443,#245444,#245445,#245446,#245447,#245448,#245449,
#245450,#245451,#245452,#245453,#245454,#245455,#245456,#245457,#245458,
#245459,#245460,#245461,#245462,#245463,#245464,#245465,#245466,#245467,
#245468,#245469,#245470,#245471,#245472,#245473,#245474,#245475,#245476,
#245477,#245478,#245479,#245480,#245481,#245482,#245483,#245484,#245485,
#245486,#245487,#245488,#245489,#245490,#245491,#245492,#245493,#245494,
#245495,#245496,#245497,#245498,#245499,#245500,#245501,#245502,#245503,
#245504,#245505,#245506,#245507,#245508,#245509,#245510,#245511,#245512,
#245513,#245514,#245515,#245516,#245517,#245518,#245519,#245520,#245521,
#245522,#245523,#245524,#245525,#245526,#245527,#245528,#245529,#245530),
 .UNSPECIFIED.,.F.,.F.)
B_SPLINE_CURVE_WITH_KNOTS((6,1,1,1,1,1,1,1,1,1,1,1,1,1,1,1,1,1,1,1,1,1,
1,1,1,1,1,1,1,1,1,1,1,1,1,1,1,1,1,1,1,1,1,1,1,1,1,1,1,1,1,1,1,1,1,1,1,1,
1,1,1,1,1,1,1,1,1,1,1,1,1,1,1,1,1,1,1,1,1,1,1,1,1,1,1,1,1,1,1,1,1,1,1,1,
1,1,1,1,1,1,1,1,1,1,1,1,1,1,1,1,1,1,1,1,1,1,1,1,1,1,1,1,1,1,1,1,1,1,1,1,
1,1,1,1,1,1,1,1,1,1,1,1,1,1,1,1,1,1,1,1,1,1,1,1,1,1,1,1,1,1,1,1,1,1,1,1,
1,1,1,1,1,1,1,1,1,1,1,1,1,1,1,1,1,1,1,1,1,1,1,1,1,1,1,1,1,1,1,1,1,1,6),
(0.,0.005,0.01,0.015,0.02,0.025,0.03,0.035,0.04,0.045,0.05,0.055,0.06,0.065,
0.07,0.075,0.08,0.085,0.09,0.095,0.1,0.105,0.11,0.115,0.12,0.125,0.13,0.135,
0.14,0.145,0.15,0.155,0.16,0.165,0.17,0.175,0.18,0.185,0.19,0.195,0.2,0.205,
0.21,0.215,0.22,0.225,0.23,0.235,0.24,0.245,0.25,0.255,0.26,0.265,0.27,
0.275,0.28,0.285,0.29,0.295,0.3,0.305,0.31,0.315,0.32,0.325,0.33,0.335,
0.34,0.345,0.35,0.355,0.36,0.365,0.37,0.375,0.38,0.385,0.39,0.395,0.4,0.405,
0.41,0.415,0.42,0.425,0.43,0.435,0.44,0.445,0.45,0.455,0.46,0.465,0.47,
0.475,0.48,0.485,0.49,0.495,0.5,0.505,0.51,0.515,0.52,0.525,0.53,0.535,
0.54,0.545,0.55,0.555,0.56,0.565,0.57,0.575,0.58,0.585,0.59,0.595,0.6,0.605,
0.61,0.615,0.62,0.625,0.63,0.635,0.64,0.645,0.65,0.655,0.66,0.665,0.67,
0.675,0.68,0.685,0.690000000000001,0.695000000000001,0.700000000000001,
0.705000000000001,0.710000000000001,0.715000000000001,0.720000000000001,
0.725000000000001,0.730000000000001,0.735000000000001,0.740000000000001,
0.745000000000001,0.750000000000001,0.755000000000001,0.760000000000001,
0.765000000000001,0.770000000000001,0.775000000000001,0.780000000000001,
0.785000000000001,0.790000000000001,0.795000000000001,0.800000000000001,
0.805000000000001,0.810000000000001,0.815000000000001,0.820000000000001,
0.825000000000001,0.830000000000001,0.835000000000001,0.840000000000001,
0.845000000000001,0.850000000000001,0.855000000000001,0.860000000000001,
0.865000000000001,0.870000000000001,0.875000000000001,0.880000000000001,
0.885000000000001,0.890000000000001,0.895000000000001,0.900000000000001,
0.905000000000001,0.910000000000001,0.915000000000001,0.920000000000001,
0.925000000000001,0.930000000000001,0.935000000000001,0.940000000000001,
0.945000000000001,0.950000000000001,0.955000000000001,0.960000000000001,
0.965000000000001,0.970000000000001,0.975000000000001,0.980000000000001,
0.985000000000001,0.990000000000001,0.995000000000001,1.),.UNSPECIFIED.)
CURVE()
GEOMETRIC_REPRESENTATION_ITEM()
RATIONAL_B_SPLINE_CURVE((1.,1.,1.,1.,1.,1.,1.,1.,1.,1.,1.,1.,1.,1.,1.,1.,
1.,1.,1.,1.,1.,1.,1.,1.,1.,1.,1.,1.,1.,1.,1.,1.,1.,1.,1.,1.,1.,1.,1.,1.,
1.,1.,1.,1.,1.,1.,1.,1.,1.,1.,1.,1.,1.,1.,1.,1.,1.,1.,1.,1.,1.,1.,1.,1.,
1.,1.,1.,1.,1.,1.,1.,1.,1.,1.,1.,1.,1.,1.,1.,1.,1.,1.,1.,1.,1.,1.,1.,1.,
1.,1.,1.,1.,1.,1.,1.,1.,1.,1.,1.,1.,1.,1.,1.,1.,1.,1.,1.,1.,1.,1.,1.,1.,
1.,1.,1.,1.,1.,1.,1.,1.,1.,1.,1.,1.,1.,1.,1.,1.,1.,1.,1.,1.,1.,1.,1.,1.,
1.,1.,1.,1.,1.,1.,1.,1.,1.,1.,1.,1.,1.,1.,1.,1.,1.,1.,1.,1.,1.,1.,1.,1.,
1.,1.,1.,1.,1.,1.,1.,1.,1.,1.,1.,1.,1.,1.,1.,1.,1.,1.,1.,1.,1.,1.,1.,1.,
1.,1.,1.,1.,1.,1.,1.,1.,1.,1.,1.,1.,1.,1.,1.,1.,1.,1.,1.,1.,1.))
REPRESENTATION_ITEM('')
);
#858=(
BOUNDED_CURVE()
B_SPLINE_CURVE(5,(#245532,#245533,#245534,#245535,#245536,#245537,#245538,
#245539,#245540,#245541,#245542,#245543,#245544,#245545,#245546,#245547,
#245548,#245549,#245550,#245551,#245552,#245553,#245554,#245555,#245556,
#245557,#245558,#245559,#245560,#245561,#245562,#245563,#245564,#245565,
#245566,#245567,#245568,#245569,#245570,#245571,#245572,#245573,#245574,
#245575,#245576,#245577,#245578,#245579,#245580,#245581,#245582,#245583,
#245584,#245585,#245586,#245587,#245588,#245589,#245590,#245591,#245592,
#245593,#245594,#245595,#245596,#245597,#245598,#245599,#245600,#245601,
#245602,#245603,#245604,#245605,#245606,#245607,#245608,#245609,#245610,
#245611,#245612,#245613,#245614,#245615,#245616,#245617,#245618,#245619,
#245620,#245621,#245622,#245623,#245624,#245625,#245626,#245627,#245628,
#245629,#245630,#245631,#245632,#245633,#245634,#245635,#245636,#245637,
#245638,#245639,#245640,#245641,#245642,#245643,#245644,#245645,#245646,
#245647,#245648,#245649,#245650,#245651,#245652,#245653,#245654,#245655,
#245656,#245657,#245658,#245659,#245660,#245661,#245662,#245663,#245664,
#245665,#245666,#245667,#245668,#245669,#245670,#245671,#245672,#245673,
#245674,#245675,#245676,#245677,#245678,#245679,#245680,#245681,#245682,
#245683,#245684,#245685,#245686,#245687,#245688,#245689,#245690,#245691,
#245692,#245693,#245694,#245695,#245696,#245697,#245698,#245699,#245700,
#245701,#245702,#245703,#245704,#245705,#245706,#245707,#245708,#245709,
#245710,#245711,#245712,#245713,#245714,#245715,#245716,#245717,#245718,
#245719,#245720,#245721,#245722,#245723,#245724,#245725,#245726,#245727,
#245728,#245729,#245730,#245731,#245732,#245733,#245734,#245735,#245736),
 .UNSPECIFIED.,.F.,.F.)
B_SPLINE_CURVE_WITH_KNOTS((6,1,1,1,1,1,1,1,1,1,1,1,1,1,1,1,1,1,1,1,1,1,
1,1,1,1,1,1,1,1,1,1,1,1,1,1,1,1,1,1,1,1,1,1,1,1,1,1,1,1,1,1,1,1,1,1,1,1,
1,1,1,1,1,1,1,1,1,1,1,1,1,1,1,1,1,1,1,1,1,1,1,1,1,1,1,1,1,1,1,1,1,1,1,1,
1,1,1,1,1,1,1,1,1,1,1,1,1,1,1,1,1,1,1,1,1,1,1,1,1,1,1,1,1,1,1,1,1,1,1,1,
1,1,1,1,1,1,1,1,1,1,1,1,1,1,1,1,1,1,1,1,1,1,1,1,1,1,1,1,1,1,1,1,1,1,1,1,
1,1,1,1,1,1,1,1,1,1,1,1,1,1,1,1,1,1,1,1,1,1,1,1,1,1,1,1,1,1,1,1,1,1,6),
(-1.,-0.995000000000001,-0.990000000000001,-0.985000000000001,-0.980000000000001,
-0.975000000000001,-0.970000000000001,-0.965000000000001,-0.960000000000001,
-0.955000000000001,-0.950000000000001,-0.945000000000001,-0.940000000000001,
-0.935000000000001,-0.930000000000001,-0.925000000000001,-0.920000000000001,
-0.915000000000001,-0.910000000000001,-0.905000000000001,-0.900000000000001,
-0.895000000000001,-0.890000000000001,-0.885000000000001,-0.880000000000001,
-0.875000000000001,-0.870000000000001,-0.865000000000001,-0.860000000000001,
-0.855000000000001,-0.850000000000001,-0.845000000000001,-0.840000000000001,
-0.835000000000001,-0.830000000000001,-0.825000000000001,-0.820000000000001,
-0.815000000000001,-0.810000000000001,-0.805000000000001,-0.800000000000001,
-0.795000000000001,-0.790000000000001,-0.785000000000001,-0.780000000000001,
-0.775000000000001,-0.770000000000001,-0.765000000000001,-0.760000000000001,
-0.755000000000001,-0.750000000000001,-0.745000000000001,-0.740000000000001,
-0.735000000000001,-0.730000000000001,-0.725000000000001,-0.720000000000001,
-0.715000000000001,-0.710000000000001,-0.705000000000001,-0.700000000000001,
-0.695000000000001,-0.690000000000001,-0.685,-0.68,-0.675,-0.67,-0.665,
-0.66,-0.655,-0.65,-0.645,-0.64,-0.635,-0.63,-0.625,-0.62,-0.615,-0.61,
-0.605,-0.6,-0.595,-0.59,-0.585,-0.58,-0.575,-0.57,-0.565,-0.56,-0.555,
-0.55,-0.545,-0.54,-0.535,-0.53,-0.525,-0.52,-0.515,-0.51,-0.505,-0.5,-0.495,
-0.49,-0.485,-0.48,-0.475,-0.47,-0.465,-0.46,-0.455,-0.45,-0.445,-0.44,
-0.435,-0.43,-0.425,-0.42,-0.415,-0.41,-0.405,-0.4,-0.395,-0.39,-0.385,
-0.38,-0.375,-0.37,-0.365,-0.36,-0.355,-0.35,-0.345,-0.34,-0.335,-0.33,
-0.325,-0.32,-0.315,-0.31,-0.305,-0.3,-0.295,-0.29,-0.285,-0.28,-0.275,
-0.27,-0.265,-0.26,-0.255,-0.25,-0.245,-0.24,-0.235,-0.23,-0.225,-0.22,
-0.215,-0.21,-0.205,-0.2,-0.195,-0.19,-0.185,-0.18,-0.175,-0.17,-0.165,
-0.16,-0.155,-0.15,-0.145,-0.14,-0.135,-0.13,-0.125,-0.12,-0.115,-0.11,
-0.105,-0.1,-0.095,-0.09,-0.085,-0.08,-0.075,-0.07,-0.065,-0.06,-0.055,
-0.05,-0.045,-0.04,-0.035,-0.03,-0.025,-0.02,-0.015,-0.01,-0.005,0.),
 .UNSPECIFIED.)
CURVE()
GEOMETRIC_REPRESENTATION_ITEM()
RATIONAL_B_SPLINE_CURVE((1.,1.,1.,1.,1.,1.,1.,1.,1.,1.,1.,1.,1.,1.,1.,1.,
1.,1.,1.,1.,1.,1.,1.,1.,1.,1.,1.,1.,1.,1.,1.,1.,1.,1.,1.,1.,1.,1.,1.,1.,
1.,1.,1.,1.,1.,1.,1.,1.,1.,1.,1.,1.,1.,1.,1.,1.,1.,1.,1.,1.,1.,1.,1.,1.,
1.,1.,1.,1.,1.,1.,1.,1.,1.,1.,1.,1.,1.,1.,1.,1.,1.,1.,1.,1.,1.,1.,1.,1.,
1.,1.,1.,1.,1.,1.,1.,1.,1.,1.,1.,1.,1.,1.,1.,1.,1.,1.,1.,1.,1.,1.,1.,1.,
1.,1.,1.,1.,1.,1.,1.,1.,1.,1.,1.,1.,1.,1.,1.,1.,1.,1.,1.,1.,1.,1.,1.,1.,
1.,1.,1.,1.,1.,1.,1.,1.,1.,1.,1.,1.,1.,1.,1.,1.,1.,1.,1.,1.,1.,1.,1.,1.,
1.,1.,1.,1.,1.,1.,1.,1.,1.,1.,1.,1.,1.,1.,1.,1.,1.,1.,1.,1.,1.,1.,1.,1.,
1.,1.,1.,1.,1.,1.,1.,1.,1.,1.,1.,1.,1.,1.,1.,1.,1.,1.,1.,1.,1.))
REPRESENTATION_ITEM('')
);
#859=(
BOUNDED_CURVE()
B_SPLINE_CURVE(5,(#246155,#246156,#246157,#246158,#246159,#246160,#246161,
#246162,#246163,#246164,#246165,#246166,#246167,#246168,#246169,#246170,
#246171,#246172,#246173,#246174,#246175,#246176,#246177,#246178,#246179,
#246180,#246181,#246182,#246183,#246184,#246185,#246186,#246187,#246188,
#246189,#246190,#246191,#246192,#246193,#246194,#246195,#246196,#246197,
#246198,#246199,#246200,#246201,#246202,#246203,#246204,#246205,#246206,
#246207,#246208,#246209,#246210,#246211,#246212,#246213,#246214,#246215,
#246216,#246217,#246218,#246219,#246220,#246221,#246222,#246223,#246224,
#246225,#246226,#246227,#246228,#246229,#246230,#246231,#246232,#246233,
#246234,#246235,#246236,#246237,#246238,#246239,#246240,#246241,#246242,
#246243,#246244,#246245,#246246,#246247,#246248,#246249,#246250,#246251,
#246252,#246253,#246254,#246255,#246256,#246257,#246258,#246259,#246260,
#246261,#246262,#246263,#246264,#246265,#246266,#246267,#246268,#246269,
#246270,#246271,#246272,#246273,#246274,#246275,#246276,#246277,#246278,
#246279,#246280,#246281,#246282,#246283,#246284,#246285,#246286,#246287,
#246288,#246289,#246290,#246291,#246292,#246293,#246294,#246295,#246296,
#246297,#246298,#246299,#246300,#246301,#246302,#246303,#246304,#246305,
#246306,#246307,#246308,#246309,#246310,#246311,#246312,#246313,#246314,
#246315,#246316,#246317,#246318,#246319,#246320,#246321,#246322,#246323,
#246324,#246325,#246326,#246327,#246328,#246329,#246330,#246331,#246332,
#246333,#246334,#246335,#246336,#246337,#246338,#246339,#246340,#246341,
#246342,#246343,#246344,#246345,#246346,#246347,#246348,#246349,#246350,
#246351,#246352,#246353,#246354,#246355,#246356,#246357,#246358,#246359),
 .UNSPECIFIED.,.F.,.F.)
B_SPLINE_CURVE_WITH_KNOTS((6,1,1,1,1,1,1,1,1,1,1,1,1,1,1,1,1,1,1,1,1,1,
1,1,1,1,1,1,1,1,1,1,1,1,1,1,1,1,1,1,1,1,1,1,1,1,1,1,1,1,1,1,1,1,1,1,1,1,
1,1,1,1,1,1,1,1,1,1,1,1,1,1,1,1,1,1,1,1,1,1,1,1,1,1,1,1,1,1,1,1,1,1,1,1,
1,1,1,1,1,1,1,1,1,1,1,1,1,1,1,1,1,1,1,1,1,1,1,1,1,1,1,1,1,1,1,1,1,1,1,1,
1,1,1,1,1,1,1,1,1,1,1,1,1,1,1,1,1,1,1,1,1,1,1,1,1,1,1,1,1,1,1,1,1,1,1,1,
1,1,1,1,1,1,1,1,1,1,1,1,1,1,1,1,1,1,1,1,1,1,1,1,1,1,1,1,1,1,1,1,1,1,6),
(-1.,-0.995000000000001,-0.990000000000001,-0.985000000000001,-0.980000000000001,
-0.975000000000001,-0.970000000000001,-0.965000000000001,-0.960000000000001,
-0.955000000000001,-0.950000000000001,-0.945000000000001,-0.940000000000001,
-0.935000000000001,-0.930000000000001,-0.925000000000001,-0.920000000000001,
-0.915000000000001,-0.910000000000001,-0.905000000000001,-0.900000000000001,
-0.895000000000001,-0.890000000000001,-0.885000000000001,-0.880000000000001,
-0.875000000000001,-0.870000000000001,-0.865000000000001,-0.860000000000001,
-0.855000000000001,-0.850000000000001,-0.845000000000001,-0.840000000000001,
-0.835000000000001,-0.830000000000001,-0.825000000000001,-0.820000000000001,
-0.815000000000001,-0.810000000000001,-0.805000000000001,-0.800000000000001,
-0.795000000000001,-0.790000000000001,-0.785000000000001,-0.780000000000001,
-0.775000000000001,-0.770000000000001,-0.765000000000001,-0.760000000000001,
-0.755000000000001,-0.750000000000001,-0.745000000000001,-0.740000000000001,
-0.735000000000001,-0.730000000000001,-0.725000000000001,-0.720000000000001,
-0.715000000000001,-0.710000000000001,-0.705000000000001,-0.700000000000001,
-0.695000000000001,-0.690000000000001,-0.685,-0.68,-0.675,-0.67,-0.665,
-0.66,-0.655,-0.65,-0.645,-0.64,-0.635,-0.63,-0.625,-0.62,-0.615,-0.61,
-0.605,-0.6,-0.595,-0.59,-0.585,-0.58,-0.575,-0.57,-0.565,-0.56,-0.555,
-0.55,-0.545,-0.54,-0.535,-0.53,-0.525,-0.52,-0.515,-0.51,-0.505,-0.5,-0.495,
-0.49,-0.485,-0.48,-0.475,-0.47,-0.465,-0.46,-0.455,-0.45,-0.445,-0.44,
-0.435,-0.43,-0.425,-0.42,-0.415,-0.41,-0.405,-0.4,-0.395,-0.39,-0.385,
-0.38,-0.375,-0.37,-0.365,-0.36,-0.355,-0.35,-0.345,-0.34,-0.335,-0.33,
-0.325,-0.32,-0.315,-0.31,-0.305,-0.3,-0.295,-0.29,-0.285,-0.28,-0.275,
-0.27,-0.265,-0.26,-0.255,-0.25,-0.245,-0.24,-0.235,-0.23,-0.225,-0.22,
-0.215,-0.21,-0.205,-0.2,-0.195,-0.19,-0.185,-0.18,-0.175,-0.17,-0.165,
-0.16,-0.155,-0.15,-0.145,-0.14,-0.135,-0.13,-0.125,-0.12,-0.115,-0.11,
-0.105,-0.1,-0.095,-0.09,-0.085,-0.08,-0.075,-0.07,-0.065,-0.06,-0.055,
-0.05,-0.045,-0.04,-0.035,-0.03,-0.025,-0.02,-0.015,-0.01,-0.005,0.),
 .UNSPECIFIED.)
CURVE()
GEOMETRIC_REPRESENTATION_ITEM()
RATIONAL_B_SPLINE_CURVE((1.,1.,1.,1.,1.,1.,1.,1.,1.,1.,1.,1.,1.,1.,1.,1.,
1.,1.,1.,1.,1.,1.,1.,1.,1.,1.,1.,1.,1.,1.,1.,1.,1.,1.,1.,1.,1.,1.,1.,1.,
1.,1.,1.,1.,1.,1.,1.,1.,1.,1.,1.,1.,1.,1.,1.,1.,1.,1.,1.,1.,1.,1.,1.,1.,
1.,1.,1.,1.,1.,1.,1.,1.,1.,1.,1.,1.,1.,1.,1.,1.,1.,1.,1.,1.,1.,1.,1.,1.,
1.,1.,1.,1.,1.,1.,1.,1.,1.,1.,1.,1.,1.,1.,1.,1.,1.,1.,1.,1.,1.,1.,1.,1.,
1.,1.,1.,1.,1.,1.,1.,1.,1.,1.,1.,1.,1.,1.,1.,1.,1.,1.,1.,1.,1.,1.,1.,1.,
1.,1.,1.,1.,1.,1.,1.,1.,1.,1.,1.,1.,1.,1.,1.,1.,1.,1.,1.,1.,1.,1.,1.,1.,
1.,1.,1.,1.,1.,1.,1.,1.,1.,1.,1.,1.,1.,1.,1.,1.,1.,1.,1.,1.,1.,1.,1.,1.,
1.,1.,1.,1.,1.,1.,1.,1.,1.,1.,1.,1.,1.,1.,1.,1.,1.,1.,1.,1.,1.))
REPRESENTATION_ITEM('')
);
#860=(
BOUNDED_CURVE()
B_SPLINE_CURVE(5,(#246362,#246363,#246364,#246365,#246366,#246367,#246368,
#246369,#246370,#246371,#246372,#246373,#246374,#246375,#246376,#246377,
#246378,#246379,#246380,#246381,#246382,#246383,#246384,#246385,#246386,
#246387,#246388,#246389,#246390,#246391,#246392,#246393,#246394,#246395,
#246396,#246397,#246398,#246399,#246400,#246401,#246402,#246403,#246404,
#246405,#246406,#246407,#246408,#246409,#246410,#246411,#246412,#246413,
#246414,#246415,#246416,#246417,#246418,#246419,#246420,#246421,#246422,
#246423,#246424,#246425,#246426,#246427,#246428,#246429,#246430,#246431,
#246432,#246433,#246434,#246435,#246436,#246437,#246438,#246439,#246440,
#246441,#246442,#246443,#246444,#246445,#246446,#246447,#246448,#246449,
#246450,#246451,#246452,#246453,#246454,#246455,#246456,#246457,#246458,
#246459,#246460,#246461,#246462,#246463,#246464,#246465,#246466,#246467,
#246468,#246469,#246470,#246471,#246472,#246473,#246474,#246475,#246476,
#246477,#246478,#246479,#246480,#246481,#246482,#246483,#246484,#246485,
#246486,#246487,#246488,#246489,#246490,#246491,#246492,#246493,#246494,
#246495,#246496,#246497,#246498,#246499,#246500,#246501,#246502,#246503,
#246504,#246505,#246506,#246507,#246508,#246509,#246510,#246511,#246512,
#246513,#246514,#246515,#246516,#246517,#246518,#246519,#246520,#246521,
#246522,#246523,#246524,#246525,#246526,#246527,#246528,#246529,#246530,
#246531,#246532,#246533,#246534,#246535,#246536,#246537,#246538,#246539,
#246540,#246541,#246542,#246543,#246544,#246545,#246546,#246547,#246548,
#246549,#246550,#246551,#246552,#246553,#246554,#246555,#246556,#246557,
#246558,#246559,#246560,#246561,#246562,#246563,#246564,#246565,#246566),
 .UNSPECIFIED.,.F.,.F.)
B_SPLINE_CURVE_WITH_KNOTS((6,1,1,1,1,1,1,1,1,1,1,1,1,1,1,1,1,1,1,1,1,1,
1,1,1,1,1,1,1,1,1,1,1,1,1,1,1,1,1,1,1,1,1,1,1,1,1,1,1,1,1,1,1,1,1,1,1,1,
1,1,1,1,1,1,1,1,1,1,1,1,1,1,1,1,1,1,1,1,1,1,1,1,1,1,1,1,1,1,1,1,1,1,1,1,
1,1,1,1,1,1,1,1,1,1,1,1,1,1,1,1,1,1,1,1,1,1,1,1,1,1,1,1,1,1,1,1,1,1,1,1,
1,1,1,1,1,1,1,1,1,1,1,1,1,1,1,1,1,1,1,1,1,1,1,1,1,1,1,1,1,1,1,1,1,1,1,1,
1,1,1,1,1,1,1,1,1,1,1,1,1,1,1,1,1,1,1,1,1,1,1,1,1,1,1,1,1,1,1,1,1,1,6),
(0.,0.005,0.01,0.015,0.02,0.025,0.03,0.035,0.04,0.045,0.05,0.055,0.06,0.065,
0.07,0.075,0.08,0.085,0.09,0.095,0.1,0.105,0.11,0.115,0.12,0.125,0.13,0.135,
0.14,0.145,0.15,0.155,0.16,0.165,0.17,0.175,0.18,0.185,0.19,0.195,0.2,0.205,
0.21,0.215,0.22,0.225,0.23,0.235,0.24,0.245,0.25,0.255,0.26,0.265,0.27,
0.275,0.28,0.285,0.29,0.295,0.3,0.305,0.31,0.315,0.32,0.325,0.33,0.335,
0.34,0.345,0.35,0.355,0.36,0.365,0.37,0.375,0.38,0.385,0.39,0.395,0.4,0.405,
0.41,0.415,0.42,0.425,0.43,0.435,0.44,0.445,0.45,0.455,0.46,0.465,0.47,
0.475,0.48,0.485,0.49,0.495,0.5,0.505,0.51,0.515,0.52,0.525,0.53,0.535,
0.54,0.545,0.55,0.555,0.56,0.565,0.57,0.575,0.58,0.585,0.59,0.595,0.6,0.605,
0.61,0.615,0.62,0.625,0.63,0.635,0.64,0.645,0.65,0.655,0.66,0.665,0.67,
0.675,0.68,0.685,0.690000000000001,0.695000000000001,0.700000000000001,
0.705000000000001,0.710000000000001,0.715000000000001,0.720000000000001,
0.725000000000001,0.730000000000001,0.735000000000001,0.740000000000001,
0.745000000000001,0.750000000000001,0.755000000000001,0.760000000000001,
0.765000000000001,0.770000000000001,0.775000000000001,0.780000000000001,
0.785000000000001,0.790000000000001,0.795000000000001,0.800000000000001,
0.805000000000001,0.810000000000001,0.815000000000001,0.820000000000001,
0.825000000000001,0.830000000000001,0.835000000000001,0.840000000000001,
0.845000000000001,0.850000000000001,0.855000000000001,0.860000000000001,
0.865000000000001,0.870000000000001,0.875000000000001,0.880000000000001,
0.885000000000001,0.890000000000001,0.895000000000001,0.900000000000001,
0.905000000000001,0.910000000000001,0.915000000000001,0.920000000000001,
0.925000000000001,0.930000000000001,0.935000000000001,0.940000000000001,
0.945000000000001,0.950000000000001,0.955000000000001,0.960000000000001,
0.965000000000001,0.970000000000001,0.975000000000001,0.980000000000001,
0.985000000000001,0.990000000000001,0.995000000000001,1.),.UNSPECIFIED.)
CURVE()
GEOMETRIC_REPRESENTATION_ITEM()
RATIONAL_B_SPLINE_CURVE((1.,1.,1.,1.,1.,1.,1.,1.,1.,1.,1.,1.,1.,1.,1.,1.,
1.,1.,1.,1.,1.,1.,1.,1.,1.,1.,1.,1.,1.,1.,1.,1.,1.,1.,1.,1.,1.,1.,1.,1.,
1.,1.,1.,1.,1.,1.,1.,1.,1.,1.,1.,1.,1.,1.,1.,1.,1.,1.,1.,1.,1.,1.,1.,1.,
1.,1.,1.,1.,1.,1.,1.,1.,1.,1.,1.,1.,1.,1.,1.,1.,1.,1.,1.,1.,1.,1.,1.,1.,
1.,1.,1.,1.,1.,1.,1.,1.,1.,1.,1.,1.,1.,1.,1.,1.,1.,1.,1.,1.,1.,1.,1.,1.,
1.,1.,1.,1.,1.,1.,1.,1.,1.,1.,1.,1.,1.,1.,1.,1.,1.,1.,1.,1.,1.,1.,1.,1.,
1.,1.,1.,1.,1.,1.,1.,1.,1.,1.,1.,1.,1.,1.,1.,1.,1.,1.,1.,1.,1.,1.,1.,1.,
1.,1.,1.,1.,1.,1.,1.,1.,1.,1.,1.,1.,1.,1.,1.,1.,1.,1.,1.,1.,1.,1.,1.,1.,
1.,1.,1.,1.,1.,1.,1.,1.,1.,1.,1.,1.,1.,1.,1.,1.,1.,1.,1.,1.,1.))
REPRESENTATION_ITEM('')
);
#861=(
BOUNDED_CURVE()
B_SPLINE_CURVE(5,(#246978,#246979,#246980,#246981,#246982,#246983,#246984,
#246985,#246986,#246987,#246988,#246989,#246990,#246991,#246992,#246993,
#246994,#246995,#246996,#246997,#246998,#246999,#247000,#247001,#247002,
#247003,#247004,#247005,#247006,#247007,#247008,#247009,#247010,#247011,
#247012,#247013,#247014,#247015,#247016,#247017,#247018,#247019,#247020,
#247021,#247022,#247023,#247024,#247025,#247026,#247027,#247028,#247029,
#247030,#247031,#247032,#247033,#247034,#247035,#247036,#247037,#247038,
#247039,#247040,#247041,#247042,#247043,#247044,#247045,#247046,#247047,
#247048,#247049,#247050,#247051,#247052,#247053,#247054,#247055,#247056,
#247057,#247058,#247059,#247060,#247061,#247062,#247063,#247064,#247065,
#247066,#247067,#247068,#247069,#247070,#247071,#247072,#247073,#247074,
#247075,#247076,#247077,#247078,#247079,#247080,#247081,#247082,#247083,
#247084,#247085,#247086,#247087,#247088,#247089,#247090,#247091,#247092,
#247093,#247094,#247095,#247096,#247097,#247098,#247099,#247100,#247101,
#247102,#247103,#247104,#247105,#247106,#247107,#247108,#247109,#247110,
#247111,#247112,#247113,#247114,#247115,#247116,#247117,#247118,#247119,
#247120,#247121,#247122,#247123,#247124,#247125,#247126,#247127,#247128,
#247129,#247130,#247131,#247132,#247133,#247134,#247135,#247136,#247137,
#247138,#247139,#247140,#247141,#247142,#247143,#247144,#247145,#247146,
#247147,#247148,#247149,#247150,#247151,#247152,#247153,#247154,#247155,
#247156,#247157,#247158,#247159,#247160,#247161,#247162,#247163,#247164,
#247165,#247166,#247167,#247168,#247169,#247170,#247171,#247172,#247173,
#247174,#247175,#247176,#247177,#247178,#247179,#247180,#247181,#247182),
 .UNSPECIFIED.,.F.,.F.)
B_SPLINE_CURVE_WITH_KNOTS((6,1,1,1,1,1,1,1,1,1,1,1,1,1,1,1,1,1,1,1,1,1,
1,1,1,1,1,1,1,1,1,1,1,1,1,1,1,1,1,1,1,1,1,1,1,1,1,1,1,1,1,1,1,1,1,1,1,1,
1,1,1,1,1,1,1,1,1,1,1,1,1,1,1,1,1,1,1,1,1,1,1,1,1,1,1,1,1,1,1,1,1,1,1,1,
1,1,1,1,1,1,1,1,1,1,1,1,1,1,1,1,1,1,1,1,1,1,1,1,1,1,1,1,1,1,1,1,1,1,1,1,
1,1,1,1,1,1,1,1,1,1,1,1,1,1,1,1,1,1,1,1,1,1,1,1,1,1,1,1,1,1,1,1,1,1,1,1,
1,1,1,1,1,1,1,1,1,1,1,1,1,1,1,1,1,1,1,1,1,1,1,1,1,1,1,1,1,1,1,1,1,1,6),
(0.,0.005,0.01,0.015,0.02,0.025,0.03,0.035,0.04,0.045,0.05,0.055,0.06,0.065,
0.07,0.075,0.08,0.085,0.09,0.095,0.1,0.105,0.11,0.115,0.12,0.125,0.13,0.135,
0.14,0.145,0.15,0.155,0.16,0.165,0.17,0.175,0.18,0.185,0.19,0.195,0.2,0.205,
0.21,0.215,0.22,0.225,0.23,0.235,0.24,0.245,0.25,0.255,0.26,0.265,0.27,
0.275,0.28,0.285,0.29,0.295,0.3,0.305,0.31,0.315,0.32,0.325,0.33,0.335,
0.34,0.345,0.35,0.355,0.36,0.365,0.37,0.375,0.38,0.385,0.39,0.395,0.4,0.405,
0.41,0.415,0.42,0.425,0.43,0.435,0.44,0.445,0.45,0.455,0.46,0.465,0.47,
0.475,0.48,0.485,0.49,0.495,0.5,0.505,0.51,0.515,0.52,0.525,0.53,0.535,
0.54,0.545,0.55,0.555,0.56,0.565,0.57,0.575,0.58,0.585,0.59,0.595,0.6,0.605,
0.61,0.615,0.62,0.625,0.63,0.635,0.64,0.645,0.65,0.655,0.66,0.665,0.67,
0.675,0.68,0.685,0.690000000000001,0.695000000000001,0.700000000000001,
0.705000000000001,0.710000000000001,0.715000000000001,0.720000000000001,
0.725000000000001,0.730000000000001,0.735000000000001,0.740000000000001,
0.745000000000001,0.750000000000001,0.755000000000001,0.760000000000001,
0.765000000000001,0.770000000000001,0.775000000000001,0.780000000000001,
0.785000000000001,0.790000000000001,0.795000000000001,0.800000000000001,
0.805000000000001,0.810000000000001,0.815000000000001,0.820000000000001,
0.825000000000001,0.830000000000001,0.835000000000001,0.840000000000001,
0.845000000000001,0.850000000000001,0.855000000000001,0.860000000000001,
0.865000000000001,0.870000000000001,0.875000000000001,0.880000000000001,
0.885000000000001,0.890000000000001,0.895000000000001,0.900000000000001,
0.905000000000001,0.910000000000001,0.915000000000001,0.920000000000001,
0.925000000000001,0.930000000000001,0.935000000000001,0.940000000000001,
0.945000000000001,0.950000000000001,0.955000000000001,0.960000000000001,
0.965000000000001,0.970000000000001,0.975000000000001,0.980000000000001,
0.985000000000001,0.990000000000001,0.995000000000001,1.),.UNSPECIFIED.)
CURVE()
GEOMETRIC_REPRESENTATION_ITEM()
RATIONAL_B_SPLINE_CURVE((1.,1.,1.,1.,1.,1.,1.,1.,1.,1.,1.,1.,1.,1.,1.,1.,
1.,1.,1.,1.,1.,1.,1.,1.,1.,1.,1.,1.,1.,1.,1.,1.,1.,1.,1.,1.,1.,1.,1.,1.,
1.,1.,1.,1.,1.,1.,1.,1.,1.,1.,1.,1.,1.,1.,1.,1.,1.,1.,1.,1.,1.,1.,1.,1.,
1.,1.,1.,1.,1.,1.,1.,1.,1.,1.,1.,1.,1.,1.,1.,1.,1.,1.,1.,1.,1.,1.,1.,1.,
1.,1.,1.,1.,1.,1.,1.,1.,1.,1.,1.,1.,1.,1.,1.,1.,1.,1.,1.,1.,1.,1.,1.,1.,
1.,1.,1.,1.,1.,1.,1.,1.,1.,1.,1.,1.,1.,1.,1.,1.,1.,1.,1.,1.,1.,1.,1.,1.,
1.,1.,1.,1.,1.,1.,1.,1.,1.,1.,1.,1.,1.,1.,1.,1.,1.,1.,1.,1.,1.,1.,1.,1.,
1.,1.,1.,1.,1.,1.,1.,1.,1.,1.,1.,1.,1.,1.,1.,1.,1.,1.,1.,1.,1.,1.,1.,1.,
1.,1.,1.,1.,1.,1.,1.,1.,1.,1.,1.,1.,1.,1.,1.,1.,1.,1.,1.,1.,1.))
REPRESENTATION_ITEM('')
);
#862=(
BOUNDED_CURVE()
B_SPLINE_CURVE(5,(#247184,#247185,#247186,#247187,#247188,#247189,#247190,
#247191,#247192,#247193,#247194,#247195,#247196,#247197,#247198,#247199,
#247200,#247201,#247202,#247203,#247204,#247205,#247206,#247207,#247208,
#247209,#247210,#247211,#247212,#247213,#247214,#247215,#247216,#247217,
#247218,#247219,#247220,#247221,#247222,#247223,#247224,#247225,#247226,
#247227,#247228,#247229,#247230,#247231,#247232,#247233,#247234,#247235,
#247236,#247237,#247238,#247239,#247240,#247241,#247242,#247243,#247244,
#247245,#247246,#247247,#247248,#247249,#247250,#247251,#247252,#247253,
#247254,#247255,#247256,#247257,#247258,#247259,#247260,#247261,#247262,
#247263,#247264,#247265,#247266,#247267,#247268,#247269,#247270,#247271,
#247272,#247273,#247274,#247275,#247276,#247277,#247278,#247279,#247280,
#247281,#247282,#247283,#247284,#247285,#247286,#247287,#247288,#247289,
#247290,#247291,#247292,#247293,#247294,#247295,#247296,#247297,#247298,
#247299,#247300,#247301,#247302,#247303,#247304,#247305,#247306,#247307,
#247308,#247309,#247310,#247311,#247312,#247313,#247314,#247315,#247316,
#247317,#247318,#247319,#247320,#247321,#247322,#247323,#247324,#247325,
#247326,#247327,#247328,#247329,#247330,#247331,#247332,#247333,#247334,
#247335,#247336,#247337,#247338,#247339,#247340,#247341,#247342,#247343,
#247344,#247345,#247346,#247347,#247348,#247349,#247350,#247351,#247352,
#247353,#247354,#247355,#247356,#247357,#247358,#247359,#247360,#247361,
#247362,#247363,#247364,#247365,#247366,#247367,#247368,#247369,#247370,
#247371,#247372,#247373,#247374,#247375,#247376,#247377,#247378,#247379,
#247380,#247381,#247382,#247383,#247384,#247385,#247386,#247387,#247388),
 .UNSPECIFIED.,.F.,.F.)
B_SPLINE_CURVE_WITH_KNOTS((6,1,1,1,1,1,1,1,1,1,1,1,1,1,1,1,1,1,1,1,1,1,
1,1,1,1,1,1,1,1,1,1,1,1,1,1,1,1,1,1,1,1,1,1,1,1,1,1,1,1,1,1,1,1,1,1,1,1,
1,1,1,1,1,1,1,1,1,1,1,1,1,1,1,1,1,1,1,1,1,1,1,1,1,1,1,1,1,1,1,1,1,1,1,1,
1,1,1,1,1,1,1,1,1,1,1,1,1,1,1,1,1,1,1,1,1,1,1,1,1,1,1,1,1,1,1,1,1,1,1,1,
1,1,1,1,1,1,1,1,1,1,1,1,1,1,1,1,1,1,1,1,1,1,1,1,1,1,1,1,1,1,1,1,1,1,1,1,
1,1,1,1,1,1,1,1,1,1,1,1,1,1,1,1,1,1,1,1,1,1,1,1,1,1,1,1,1,1,1,1,1,1,6),
(-1.,-0.995000000000001,-0.990000000000001,-0.985000000000001,-0.980000000000001,
-0.975000000000001,-0.970000000000001,-0.965000000000001,-0.960000000000001,
-0.955000000000001,-0.950000000000001,-0.945000000000001,-0.940000000000001,
-0.935000000000001,-0.930000000000001,-0.925000000000001,-0.920000000000001,
-0.915000000000001,-0.910000000000001,-0.905000000000001,-0.900000000000001,
-0.895000000000001,-0.890000000000001,-0.885000000000001,-0.880000000000001,
-0.875000000000001,-0.870000000000001,-0.865000000000001,-0.860000000000001,
-0.855000000000001,-0.850000000000001,-0.845000000000001,-0.840000000000001,
-0.835000000000001,-0.830000000000001,-0.825000000000001,-0.820000000000001,
-0.815000000000001,-0.810000000000001,-0.805000000000001,-0.800000000000001,
-0.795000000000001,-0.790000000000001,-0.785000000000001,-0.780000000000001,
-0.775000000000001,-0.770000000000001,-0.765000000000001,-0.760000000000001,
-0.755000000000001,-0.750000000000001,-0.745000000000001,-0.740000000000001,
-0.735000000000001,-0.730000000000001,-0.725000000000001,-0.720000000000001,
-0.715000000000001,-0.710000000000001,-0.705000000000001,-0.700000000000001,
-0.695000000000001,-0.690000000000001,-0.685,-0.68,-0.675,-0.67,-0.665,
-0.66,-0.655,-0.65,-0.645,-0.64,-0.635,-0.63,-0.625,-0.62,-0.615,-0.61,
-0.605,-0.6,-0.595,-0.59,-0.585,-0.58,-0.575,-0.57,-0.565,-0.56,-0.555,
-0.55,-0.545,-0.54,-0.535,-0.53,-0.525,-0.52,-0.515,-0.51,-0.505,-0.5,-0.495,
-0.49,-0.485,-0.48,-0.475,-0.47,-0.465,-0.46,-0.455,-0.45,-0.445,-0.44,
-0.435,-0.43,-0.425,-0.42,-0.415,-0.41,-0.405,-0.4,-0.395,-0.39,-0.385,
-0.38,-0.375,-0.37,-0.365,-0.36,-0.355,-0.35,-0.345,-0.34,-0.335,-0.33,
-0.325,-0.32,-0.315,-0.31,-0.305,-0.3,-0.295,-0.29,-0.285,-0.28,-0.275,
-0.27,-0.265,-0.26,-0.255,-0.25,-0.245,-0.24,-0.235,-0.23,-0.225,-0.22,
-0.215,-0.21,-0.205,-0.2,-0.195,-0.19,-0.185,-0.18,-0.175,-0.17,-0.165,
-0.16,-0.155,-0.15,-0.145,-0.14,-0.135,-0.13,-0.125,-0.12,-0.115,-0.11,
-0.105,-0.1,-0.095,-0.09,-0.085,-0.08,-0.075,-0.07,-0.065,-0.06,-0.055,
-0.05,-0.045,-0.04,-0.035,-0.03,-0.025,-0.02,-0.015,-0.01,-0.005,0.),
 .UNSPECIFIED.)
CURVE()
GEOMETRIC_REPRESENTATION_ITEM()
RATIONAL_B_SPLINE_CURVE((1.,1.,1.,1.,1.,1.,1.,1.,1.,1.,1.,1.,1.,1.,1.,1.,
1.,1.,1.,1.,1.,1.,1.,1.,1.,1.,1.,1.,1.,1.,1.,1.,1.,1.,1.,1.,1.,1.,1.,1.,
1.,1.,1.,1.,1.,1.,1.,1.,1.,1.,1.,1.,1.,1.,1.,1.,1.,1.,1.,1.,1.,1.,1.,1.,
1.,1.,1.,1.,1.,1.,1.,1.,1.,1.,1.,1.,1.,1.,1.,1.,1.,1.,1.,1.,1.,1.,1.,1.,
1.,1.,1.,1.,1.,1.,1.,1.,1.,1.,1.,1.,1.,1.,1.,1.,1.,1.,1.,1.,1.,1.,1.,1.,
1.,1.,1.,1.,1.,1.,1.,1.,1.,1.,1.,1.,1.,1.,1.,1.,1.,1.,1.,1.,1.,1.,1.,1.,
1.,1.,1.,1.,1.,1.,1.,1.,1.,1.,1.,1.,1.,1.,1.,1.,1.,1.,1.,1.,1.,1.,1.,1.,
1.,1.,1.,1.,1.,1.,1.,1.,1.,1.,1.,1.,1.,1.,1.,1.,1.,1.,1.,1.,1.,1.,1.,1.,
1.,1.,1.,1.,1.,1.,1.,1.,1.,1.,1.,1.,1.,1.,1.,1.,1.,1.,1.,1.,1.))
REPRESENTATION_ITEM('')
);
#863=(
BOUNDED_CURVE()
B_SPLINE_CURVE(5,(#247807,#247808,#247809,#247810,#247811,#247812,#247813,
#247814,#247815,#247816,#247817,#247818,#247819,#247820,#247821,#247822,
#247823,#247824,#247825,#247826,#247827,#247828,#247829,#247830,#247831,
#247832,#247833,#247834,#247835,#247836,#247837,#247838,#247839,#247840,
#247841,#247842,#247843,#247844,#247845,#247846,#247847,#247848,#247849,
#247850,#247851,#247852,#247853,#247854,#247855,#247856,#247857,#247858,
#247859,#247860,#247861,#247862,#247863,#247864,#247865,#247866,#247867,
#247868,#247869,#247870,#247871,#247872,#247873,#247874,#247875,#247876,
#247877,#247878,#247879,#247880,#247881,#247882,#247883,#247884,#247885,
#247886,#247887,#247888,#247889,#247890,#247891,#247892,#247893,#247894,
#247895,#247896,#247897,#247898,#247899,#247900,#247901,#247902,#247903,
#247904,#247905,#247906,#247907,#247908,#247909,#247910,#247911,#247912,
#247913,#247914,#247915,#247916,#247917,#247918,#247919,#247920,#247921,
#247922,#247923,#247924,#247925,#247926,#247927,#247928,#247929,#247930,
#247931,#247932,#247933,#247934,#247935,#247936,#247937,#247938,#247939,
#247940,#247941,#247942,#247943,#247944,#247945,#247946,#247947,#247948,
#247949,#247950,#247951,#247952,#247953,#247954,#247955,#247956,#247957,
#247958,#247959,#247960,#247961,#247962,#247963,#247964,#247965,#247966,
#247967,#247968,#247969,#247970,#247971,#247972,#247973,#247974,#247975,
#247976,#247977,#247978,#247979,#247980,#247981,#247982,#247983,#247984,
#247985,#247986,#247987,#247988,#247989,#247990,#247991,#247992,#247993,
#247994,#247995,#247996,#247997,#247998,#247999,#248000,#248001,#248002,
#248003,#248004,#248005,#248006,#248007,#248008,#248009,#248010,#248011),
 .UNSPECIFIED.,.F.,.F.)
B_SPLINE_CURVE_WITH_KNOTS((6,1,1,1,1,1,1,1,1,1,1,1,1,1,1,1,1,1,1,1,1,1,
1,1,1,1,1,1,1,1,1,1,1,1,1,1,1,1,1,1,1,1,1,1,1,1,1,1,1,1,1,1,1,1,1,1,1,1,
1,1,1,1,1,1,1,1,1,1,1,1,1,1,1,1,1,1,1,1,1,1,1,1,1,1,1,1,1,1,1,1,1,1,1,1,
1,1,1,1,1,1,1,1,1,1,1,1,1,1,1,1,1,1,1,1,1,1,1,1,1,1,1,1,1,1,1,1,1,1,1,1,
1,1,1,1,1,1,1,1,1,1,1,1,1,1,1,1,1,1,1,1,1,1,1,1,1,1,1,1,1,1,1,1,1,1,1,1,
1,1,1,1,1,1,1,1,1,1,1,1,1,1,1,1,1,1,1,1,1,1,1,1,1,1,1,1,1,1,1,1,1,1,6),
(-1.,-0.995000000000001,-0.990000000000001,-0.985000000000001,-0.980000000000001,
-0.975000000000001,-0.970000000000001,-0.965000000000001,-0.960000000000001,
-0.955000000000001,-0.950000000000001,-0.945000000000001,-0.940000000000001,
-0.935000000000001,-0.930000000000001,-0.925000000000001,-0.920000000000001,
-0.915000000000001,-0.910000000000001,-0.905000000000001,-0.900000000000001,
-0.895000000000001,-0.890000000000001,-0.885000000000001,-0.880000000000001,
-0.875000000000001,-0.870000000000001,-0.865000000000001,-0.860000000000001,
-0.855000000000001,-0.850000000000001,-0.845000000000001,-0.840000000000001,
-0.835000000000001,-0.830000000000001,-0.825000000000001,-0.820000000000001,
-0.815000000000001,-0.810000000000001,-0.805000000000001,-0.800000000000001,
-0.795000000000001,-0.790000000000001,-0.785000000000001,-0.780000000000001,
-0.775000000000001,-0.770000000000001,-0.765000000000001,-0.760000000000001,
-0.755000000000001,-0.750000000000001,-0.745000000000001,-0.740000000000001,
-0.735000000000001,-0.730000000000001,-0.725000000000001,-0.720000000000001,
-0.715000000000001,-0.710000000000001,-0.705000000000001,-0.700000000000001,
-0.695000000000001,-0.690000000000001,-0.685,-0.68,-0.675,-0.67,-0.665,
-0.66,-0.655,-0.65,-0.645,-0.64,-0.635,-0.63,-0.625,-0.62,-0.615,-0.61,
-0.605,-0.6,-0.595,-0.59,-0.585,-0.58,-0.575,-0.57,-0.565,-0.56,-0.555,
-0.55,-0.545,-0.54,-0.535,-0.53,-0.525,-0.52,-0.515,-0.51,-0.505,-0.5,-0.495,
-0.49,-0.485,-0.48,-0.475,-0.47,-0.465,-0.46,-0.455,-0.45,-0.445,-0.44,
-0.435,-0.43,-0.425,-0.42,-0.415,-0.41,-0.405,-0.4,-0.395,-0.39,-0.385,
-0.38,-0.375,-0.37,-0.365,-0.36,-0.355,-0.35,-0.345,-0.34,-0.335,-0.33,
-0.325,-0.32,-0.315,-0.31,-0.305,-0.3,-0.295,-0.29,-0.285,-0.28,-0.275,
-0.27,-0.265,-0.26,-0.255,-0.25,-0.245,-0.24,-0.235,-0.23,-0.225,-0.22,
-0.215,-0.21,-0.205,-0.2,-0.195,-0.19,-0.185,-0.18,-0.175,-0.17,-0.165,
-0.16,-0.155,-0.15,-0.145,-0.14,-0.135,-0.13,-0.125,-0.12,-0.115,-0.11,
-0.105,-0.1,-0.095,-0.09,-0.085,-0.08,-0.075,-0.07,-0.065,-0.06,-0.055,
-0.05,-0.045,-0.04,-0.035,-0.03,-0.025,-0.02,-0.015,-0.01,-0.005,0.),
 .UNSPECIFIED.)
CURVE()
GEOMETRIC_REPRESENTATION_ITEM()
RATIONAL_B_SPLINE_CURVE((1.,1.,1.,1.,1.,1.,1.,1.,1.,1.,1.,1.,1.,1.,1.,1.,
1.,1.,1.,1.,1.,1.,1.,1.,1.,1.,1.,1.,1.,1.,1.,1.,1.,1.,1.,1.,1.,1.,1.,1.,
1.,1.,1.,1.,1.,1.,1.,1.,1.,1.,1.,1.,1.,1.,1.,1.,1.,1.,1.,1.,1.,1.,1.,1.,
1.,1.,1.,1.,1.,1.,1.,1.,1.,1.,1.,1.,1.,1.,1.,1.,1.,1.,1.,1.,1.,1.,1.,1.,
1.,1.,1.,1.,1.,1.,1.,1.,1.,1.,1.,1.,1.,1.,1.,1.,1.,1.,1.,1.,1.,1.,1.,1.,
1.,1.,1.,1.,1.,1.,1.,1.,1.,1.,1.,1.,1.,1.,1.,1.,1.,1.,1.,1.,1.,1.,1.,1.,
1.,1.,1.,1.,1.,1.,1.,1.,1.,1.,1.,1.,1.,1.,1.,1.,1.,1.,1.,1.,1.,1.,1.,1.,
1.,1.,1.,1.,1.,1.,1.,1.,1.,1.,1.,1.,1.,1.,1.,1.,1.,1.,1.,1.,1.,1.,1.,1.,
1.,1.,1.,1.,1.,1.,1.,1.,1.,1.,1.,1.,1.,1.,1.,1.,1.,1.,1.,1.,1.))
REPRESENTATION_ITEM('')
);
#864=(
BOUNDED_CURVE()
B_SPLINE_CURVE(5,(#248014,#248015,#248016,#248017,#248018,#248019,#248020,
#248021,#248022,#248023,#248024,#248025,#248026,#248027,#248028,#248029,
#248030,#248031,#248032,#248033,#248034,#248035,#248036,#248037,#248038,
#248039,#248040,#248041,#248042,#248043,#248044,#248045,#248046,#248047,
#248048,#248049,#248050,#248051,#248052,#248053,#248054,#248055,#248056,
#248057,#248058,#248059,#248060,#248061,#248062,#248063,#248064,#248065,
#248066,#248067,#248068,#248069,#248070,#248071,#248072,#248073,#248074,
#248075,#248076,#248077,#248078,#248079,#248080,#248081,#248082,#248083,
#248084,#248085,#248086,#248087,#248088,#248089,#248090,#248091,#248092,
#248093,#248094,#248095,#248096,#248097,#248098,#248099,#248100,#248101,
#248102,#248103,#248104,#248105,#248106,#248107,#248108,#248109,#248110,
#248111,#248112,#248113,#248114,#248115,#248116,#248117,#248118,#248119,
#248120,#248121,#248122,#248123,#248124,#248125,#248126,#248127,#248128,
#248129,#248130,#248131,#248132,#248133,#248134,#248135,#248136,#248137,
#248138,#248139,#248140,#248141,#248142,#248143,#248144,#248145,#248146,
#248147,#248148,#248149,#248150,#248151,#248152,#248153,#248154,#248155,
#248156,#248157,#248158,#248159,#248160,#248161,#248162,#248163,#248164,
#248165,#248166,#248167,#248168,#248169,#248170,#248171,#248172,#248173,
#248174,#248175,#248176,#248177,#248178,#248179,#248180,#248181,#248182,
#248183,#248184,#248185,#248186,#248187,#248188,#248189,#248190,#248191,
#248192,#248193,#248194,#248195,#248196,#248197,#248198,#248199,#248200,
#248201,#248202,#248203,#248204,#248205,#248206,#248207,#248208,#248209,
#248210,#248211,#248212,#248213,#248214,#248215,#248216,#248217,#248218),
 .UNSPECIFIED.,.F.,.F.)
B_SPLINE_CURVE_WITH_KNOTS((6,1,1,1,1,1,1,1,1,1,1,1,1,1,1,1,1,1,1,1,1,1,
1,1,1,1,1,1,1,1,1,1,1,1,1,1,1,1,1,1,1,1,1,1,1,1,1,1,1,1,1,1,1,1,1,1,1,1,
1,1,1,1,1,1,1,1,1,1,1,1,1,1,1,1,1,1,1,1,1,1,1,1,1,1,1,1,1,1,1,1,1,1,1,1,
1,1,1,1,1,1,1,1,1,1,1,1,1,1,1,1,1,1,1,1,1,1,1,1,1,1,1,1,1,1,1,1,1,1,1,1,
1,1,1,1,1,1,1,1,1,1,1,1,1,1,1,1,1,1,1,1,1,1,1,1,1,1,1,1,1,1,1,1,1,1,1,1,
1,1,1,1,1,1,1,1,1,1,1,1,1,1,1,1,1,1,1,1,1,1,1,1,1,1,1,1,1,1,1,1,1,1,6),
(0.,0.005,0.01,0.015,0.02,0.025,0.03,0.035,0.04,0.045,0.05,0.055,0.06,0.065,
0.07,0.075,0.08,0.085,0.09,0.095,0.1,0.105,0.11,0.115,0.12,0.125,0.13,0.135,
0.14,0.145,0.15,0.155,0.16,0.165,0.17,0.175,0.18,0.185,0.19,0.195,0.2,0.205,
0.21,0.215,0.22,0.225,0.23,0.235,0.24,0.245,0.25,0.255,0.26,0.265,0.27,
0.275,0.28,0.285,0.29,0.295,0.3,0.305,0.31,0.315,0.32,0.325,0.33,0.335,
0.34,0.345,0.35,0.355,0.36,0.365,0.37,0.375,0.38,0.385,0.39,0.395,0.4,0.405,
0.41,0.415,0.42,0.425,0.43,0.435,0.44,0.445,0.45,0.455,0.46,0.465,0.47,
0.475,0.48,0.485,0.49,0.495,0.5,0.505,0.51,0.515,0.52,0.525,0.53,0.535,
0.54,0.545,0.55,0.555,0.56,0.565,0.57,0.575,0.58,0.585,0.59,0.595,0.6,0.605,
0.61,0.615,0.62,0.625,0.63,0.635,0.64,0.645,0.65,0.655,0.66,0.665,0.67,
0.675,0.68,0.685,0.690000000000001,0.695000000000001,0.700000000000001,
0.705000000000001,0.710000000000001,0.715000000000001,0.720000000000001,
0.725000000000001,0.730000000000001,0.735000000000001,0.740000000000001,
0.745000000000001,0.750000000000001,0.755000000000001,0.760000000000001,
0.765000000000001,0.770000000000001,0.775000000000001,0.780000000000001,
0.785000000000001,0.790000000000001,0.795000000000001,0.800000000000001,
0.805000000000001,0.810000000000001,0.815000000000001,0.820000000000001,
0.825000000000001,0.830000000000001,0.835000000000001,0.840000000000001,
0.845000000000001,0.850000000000001,0.855000000000001,0.860000000000001,
0.865000000000001,0.870000000000001,0.875000000000001,0.880000000000001,
0.885000000000001,0.890000000000001,0.895000000000001,0.900000000000001,
0.905000000000001,0.910000000000001,0.915000000000001,0.920000000000001,
0.925000000000001,0.930000000000001,0.935000000000001,0.940000000000001,
0.945000000000001,0.950000000000001,0.955000000000001,0.960000000000001,
0.965000000000001,0.970000000000001,0.975000000000001,0.980000000000001,
0.985000000000001,0.990000000000001,0.995000000000001,1.),.UNSPECIFIED.)
CURVE()
GEOMETRIC_REPRESENTATION_ITEM()
RATIONAL_B_SPLINE_CURVE((1.,1.,1.,1.,1.,1.,1.,1.,1.,1.,1.,1.,1.,1.,1.,1.,
1.,1.,1.,1.,1.,1.,1.,1.,1.,1.,1.,1.,1.,1.,1.,1.,1.,1.,1.,1.,1.,1.,1.,1.,
1.,1.,1.,1.,1.,1.,1.,1.,1.,1.,1.,1.,1.,1.,1.,1.,1.,1.,1.,1.,1.,1.,1.,1.,
1.,1.,1.,1.,1.,1.,1.,1.,1.,1.,1.,1.,1.,1.,1.,1.,1.,1.,1.,1.,1.,1.,1.,1.,
1.,1.,1.,1.,1.,1.,1.,1.,1.,1.,1.,1.,1.,1.,1.,1.,1.,1.,1.,1.,1.,1.,1.,1.,
1.,1.,1.,1.,1.,1.,1.,1.,1.,1.,1.,1.,1.,1.,1.,1.,1.,1.,1.,1.,1.,1.,1.,1.,
1.,1.,1.,1.,1.,1.,1.,1.,1.,1.,1.,1.,1.,1.,1.,1.,1.,1.,1.,1.,1.,1.,1.,1.,
1.,1.,1.,1.,1.,1.,1.,1.,1.,1.,1.,1.,1.,1.,1.,1.,1.,1.,1.,1.,1.,1.,1.,1.,
1.,1.,1.,1.,1.,1.,1.,1.,1.,1.,1.,1.,1.,1.,1.,1.,1.,1.,1.,1.,1.))
REPRESENTATION_ITEM('')
);
#865=(
BOUNDED_CURVE()
B_SPLINE_CURVE(5,(#248630,#248631,#248632,#248633,#248634,#248635,#248636,
#248637,#248638,#248639,#248640,#248641,#248642,#248643,#248644,#248645,
#248646,#248647,#248648,#248649,#248650,#248651,#248652,#248653,#248654,
#248655,#248656,#248657,#248658,#248659,#248660,#248661,#248662,#248663,
#248664,#248665,#248666,#248667,#248668,#248669,#248670,#248671,#248672,
#248673,#248674,#248675,#248676,#248677,#248678,#248679,#248680,#248681,
#248682,#248683,#248684,#248685,#248686,#248687,#248688,#248689,#248690,
#248691,#248692,#248693,#248694,#248695,#248696,#248697,#248698,#248699,
#248700,#248701,#248702,#248703,#248704,#248705,#248706,#248707,#248708,
#248709,#248710,#248711,#248712,#248713,#248714,#248715,#248716,#248717,
#248718,#248719,#248720,#248721,#248722,#248723,#248724,#248725,#248726,
#248727,#248728,#248729,#248730,#248731,#248732,#248733,#248734,#248735,
#248736,#248737,#248738,#248739,#248740,#248741,#248742,#248743,#248744,
#248745,#248746,#248747,#248748,#248749,#248750,#248751,#248752,#248753,
#248754,#248755,#248756,#248757,#248758,#248759,#248760,#248761,#248762,
#248763,#248764,#248765,#248766,#248767,#248768,#248769,#248770,#248771,
#248772,#248773,#248774,#248775,#248776,#248777,#248778,#248779,#248780,
#248781,#248782,#248783,#248784,#248785,#248786,#248787,#248788,#248789,
#248790,#248791,#248792,#248793,#248794,#248795,#248796,#248797,#248798,
#248799,#248800,#248801,#248802,#248803,#248804,#248805,#248806,#248807,
#248808,#248809,#248810,#248811,#248812,#248813,#248814,#248815,#248816,
#248817,#248818,#248819,#248820,#248821,#248822,#248823,#248824,#248825,
#248826,#248827,#248828,#248829,#248830,#248831,#248832,#248833,#248834),
 .UNSPECIFIED.,.F.,.F.)
B_SPLINE_CURVE_WITH_KNOTS((6,1,1,1,1,1,1,1,1,1,1,1,1,1,1,1,1,1,1,1,1,1,
1,1,1,1,1,1,1,1,1,1,1,1,1,1,1,1,1,1,1,1,1,1,1,1,1,1,1,1,1,1,1,1,1,1,1,1,
1,1,1,1,1,1,1,1,1,1,1,1,1,1,1,1,1,1,1,1,1,1,1,1,1,1,1,1,1,1,1,1,1,1,1,1,
1,1,1,1,1,1,1,1,1,1,1,1,1,1,1,1,1,1,1,1,1,1,1,1,1,1,1,1,1,1,1,1,1,1,1,1,
1,1,1,1,1,1,1,1,1,1,1,1,1,1,1,1,1,1,1,1,1,1,1,1,1,1,1,1,1,1,1,1,1,1,1,1,
1,1,1,1,1,1,1,1,1,1,1,1,1,1,1,1,1,1,1,1,1,1,1,1,1,1,1,1,1,1,1,1,1,1,6),
(0.,0.005,0.01,0.015,0.02,0.025,0.03,0.035,0.04,0.045,0.05,0.055,0.06,0.065,
0.07,0.075,0.08,0.085,0.09,0.095,0.1,0.105,0.11,0.115,0.12,0.125,0.13,0.135,
0.14,0.145,0.15,0.155,0.16,0.165,0.17,0.175,0.18,0.185,0.19,0.195,0.2,0.205,
0.21,0.215,0.22,0.225,0.23,0.235,0.24,0.245,0.25,0.255,0.26,0.265,0.27,
0.275,0.28,0.285,0.29,0.295,0.3,0.305,0.31,0.315,0.32,0.325,0.33,0.335,
0.34,0.345,0.35,0.355,0.36,0.365,0.37,0.375,0.38,0.385,0.39,0.395,0.4,0.405,
0.41,0.415,0.42,0.425,0.43,0.435,0.44,0.445,0.45,0.455,0.46,0.465,0.47,
0.475,0.48,0.485,0.49,0.495,0.5,0.505,0.51,0.515,0.52,0.525,0.53,0.535,
0.54,0.545,0.55,0.555,0.56,0.565,0.57,0.575,0.58,0.585,0.59,0.595,0.6,0.605,
0.61,0.615,0.62,0.625,0.63,0.635,0.64,0.645,0.65,0.655,0.66,0.665,0.67,
0.675,0.68,0.685,0.690000000000001,0.695000000000001,0.700000000000001,
0.705000000000001,0.710000000000001,0.715000000000001,0.720000000000001,
0.725000000000001,0.730000000000001,0.735000000000001,0.740000000000001,
0.745000000000001,0.750000000000001,0.755000000000001,0.760000000000001,
0.765000000000001,0.770000000000001,0.775000000000001,0.780000000000001,
0.785000000000001,0.790000000000001,0.795000000000001,0.800000000000001,
0.805000000000001,0.810000000000001,0.815000000000001,0.820000000000001,
0.825000000000001,0.830000000000001,0.835000000000001,0.840000000000001,
0.845000000000001,0.850000000000001,0.855000000000001,0.860000000000001,
0.865000000000001,0.870000000000001,0.875000000000001,0.880000000000001,
0.885000000000001,0.890000000000001,0.895000000000001,0.900000000000001,
0.905000000000001,0.910000000000001,0.915000000000001,0.920000000000001,
0.925000000000001,0.930000000000001,0.935000000000001,0.940000000000001,
0.945000000000001,0.950000000000001,0.955000000000001,0.960000000000001,
0.965000000000001,0.970000000000001,0.975000000000001,0.980000000000001,
0.985000000000001,0.990000000000001,0.995000000000001,1.),.UNSPECIFIED.)
CURVE()
GEOMETRIC_REPRESENTATION_ITEM()
RATIONAL_B_SPLINE_CURVE((1.,1.,1.,1.,1.,1.,1.,1.,1.,1.,1.,1.,1.,1.,1.,1.,
1.,1.,1.,1.,1.,1.,1.,1.,1.,1.,1.,1.,1.,1.,1.,1.,1.,1.,1.,1.,1.,1.,1.,1.,
1.,1.,1.,1.,1.,1.,1.,1.,1.,1.,1.,1.,1.,1.,1.,1.,1.,1.,1.,1.,1.,1.,1.,1.,
1.,1.,1.,1.,1.,1.,1.,1.,1.,1.,1.,1.,1.,1.,1.,1.,1.,1.,1.,1.,1.,1.,1.,1.,
1.,1.,1.,1.,1.,1.,1.,1.,1.,1.,1.,1.,1.,1.,1.,1.,1.,1.,1.,1.,1.,1.,1.,1.,
1.,1.,1.,1.,1.,1.,1.,1.,1.,1.,1.,1.,1.,1.,1.,1.,1.,1.,1.,1.,1.,1.,1.,1.,
1.,1.,1.,1.,1.,1.,1.,1.,1.,1.,1.,1.,1.,1.,1.,1.,1.,1.,1.,1.,1.,1.,1.,1.,
1.,1.,1.,1.,1.,1.,1.,1.,1.,1.,1.,1.,1.,1.,1.,1.,1.,1.,1.,1.,1.,1.,1.,1.,
1.,1.,1.,1.,1.,1.,1.,1.,1.,1.,1.,1.,1.,1.,1.,1.,1.,1.,1.,1.,1.))
REPRESENTATION_ITEM('')
);
#866=(
BOUNDED_CURVE()
B_SPLINE_CURVE(5,(#248836,#248837,#248838,#248839,#248840,#248841,#248842,
#248843,#248844,#248845,#248846,#248847,#248848,#248849,#248850,#248851,
#248852,#248853,#248854,#248855,#248856,#248857,#248858,#248859,#248860,
#248861,#248862,#248863,#248864,#248865,#248866,#248867,#248868,#248869,
#248870,#248871,#248872,#248873,#248874,#248875,#248876,#248877,#248878,
#248879,#248880,#248881,#248882,#248883,#248884,#248885,#248886,#248887,
#248888,#248889,#248890,#248891,#248892,#248893,#248894,#248895,#248896,
#248897,#248898,#248899,#248900,#248901,#248902,#248903,#248904,#248905,
#248906,#248907,#248908,#248909,#248910,#248911,#248912,#248913,#248914,
#248915,#248916,#248917,#248918,#248919,#248920,#248921,#248922,#248923,
#248924,#248925,#248926,#248927,#248928,#248929,#248930,#248931,#248932,
#248933,#248934,#248935,#248936,#248937,#248938,#248939,#248940,#248941,
#248942,#248943,#248944,#248945,#248946,#248947,#248948,#248949,#248950,
#248951,#248952,#248953,#248954,#248955,#248956,#248957,#248958,#248959,
#248960,#248961,#248962,#248963,#248964,#248965,#248966,#248967,#248968,
#248969,#248970,#248971,#248972,#248973,#248974,#248975,#248976,#248977,
#248978,#248979,#248980,#248981,#248982,#248983,#248984,#248985,#248986,
#248987,#248988,#248989,#248990,#248991,#248992,#248993,#248994,#248995,
#248996,#248997,#248998,#248999,#249000,#249001,#249002,#249003,#249004,
#249005,#249006,#249007,#249008,#249009,#249010,#249011,#249012,#249013,
#249014,#249015,#249016,#249017,#249018,#249019,#249020,#249021,#249022,
#249023,#249024,#249025,#249026,#249027,#249028,#249029,#249030,#249031,
#249032,#249033,#249034,#249035,#249036,#249037,#249038,#249039,#249040),
 .UNSPECIFIED.,.F.,.F.)
B_SPLINE_CURVE_WITH_KNOTS((6,1,1,1,1,1,1,1,1,1,1,1,1,1,1,1,1,1,1,1,1,1,
1,1,1,1,1,1,1,1,1,1,1,1,1,1,1,1,1,1,1,1,1,1,1,1,1,1,1,1,1,1,1,1,1,1,1,1,
1,1,1,1,1,1,1,1,1,1,1,1,1,1,1,1,1,1,1,1,1,1,1,1,1,1,1,1,1,1,1,1,1,1,1,1,
1,1,1,1,1,1,1,1,1,1,1,1,1,1,1,1,1,1,1,1,1,1,1,1,1,1,1,1,1,1,1,1,1,1,1,1,
1,1,1,1,1,1,1,1,1,1,1,1,1,1,1,1,1,1,1,1,1,1,1,1,1,1,1,1,1,1,1,1,1,1,1,1,
1,1,1,1,1,1,1,1,1,1,1,1,1,1,1,1,1,1,1,1,1,1,1,1,1,1,1,1,1,1,1,1,1,1,6),
(-1.,-0.995000000000001,-0.990000000000001,-0.985000000000001,-0.980000000000001,
-0.975000000000001,-0.970000000000001,-0.965000000000001,-0.960000000000001,
-0.955000000000001,-0.950000000000001,-0.945000000000001,-0.940000000000001,
-0.935000000000001,-0.930000000000001,-0.925000000000001,-0.920000000000001,
-0.915000000000001,-0.910000000000001,-0.905000000000001,-0.900000000000001,
-0.895000000000001,-0.890000000000001,-0.885000000000001,-0.880000000000001,
-0.875000000000001,-0.870000000000001,-0.865000000000001,-0.860000000000001,
-0.855000000000001,-0.850000000000001,-0.845000000000001,-0.840000000000001,
-0.835000000000001,-0.830000000000001,-0.825000000000001,-0.820000000000001,
-0.815000000000001,-0.810000000000001,-0.805000000000001,-0.800000000000001,
-0.795000000000001,-0.790000000000001,-0.785000000000001,-0.780000000000001,
-0.775000000000001,-0.770000000000001,-0.765000000000001,-0.760000000000001,
-0.755000000000001,-0.750000000000001,-0.745000000000001,-0.740000000000001,
-0.735000000000001,-0.730000000000001,-0.725000000000001,-0.720000000000001,
-0.715000000000001,-0.710000000000001,-0.705000000000001,-0.700000000000001,
-0.695000000000001,-0.690000000000001,-0.685,-0.68,-0.675,-0.67,-0.665,
-0.66,-0.655,-0.65,-0.645,-0.64,-0.635,-0.63,-0.625,-0.62,-0.615,-0.61,
-0.605,-0.6,-0.595,-0.59,-0.585,-0.58,-0.575,-0.57,-0.565,-0.56,-0.555,
-0.55,-0.545,-0.54,-0.535,-0.53,-0.525,-0.52,-0.515,-0.51,-0.505,-0.5,-0.495,
-0.49,-0.485,-0.48,-0.475,-0.47,-0.465,-0.46,-0.455,-0.45,-0.445,-0.44,
-0.435,-0.43,-0.425,-0.42,-0.415,-0.41,-0.405,-0.4,-0.395,-0.39,-0.385,
-0.38,-0.375,-0.37,-0.365,-0.36,-0.355,-0.35,-0.345,-0.34,-0.335,-0.33,
-0.325,-0.32,-0.315,-0.31,-0.305,-0.3,-0.295,-0.29,-0.285,-0.28,-0.275,
-0.27,-0.265,-0.26,-0.255,-0.25,-0.245,-0.24,-0.235,-0.23,-0.225,-0.22,
-0.215,-0.21,-0.205,-0.2,-0.195,-0.19,-0.185,-0.18,-0.175,-0.17,-0.165,
-0.16,-0.155,-0.15,-0.145,-0.14,-0.135,-0.13,-0.125,-0.12,-0.115,-0.11,
-0.105,-0.1,-0.095,-0.09,-0.085,-0.08,-0.075,-0.07,-0.065,-0.06,-0.055,
-0.05,-0.045,-0.04,-0.035,-0.03,-0.025,-0.02,-0.015,-0.01,-0.005,0.),
 .UNSPECIFIED.)
CURVE()
GEOMETRIC_REPRESENTATION_ITEM()
RATIONAL_B_SPLINE_CURVE((1.,1.,1.,1.,1.,1.,1.,1.,1.,1.,1.,1.,1.,1.,1.,1.,
1.,1.,1.,1.,1.,1.,1.,1.,1.,1.,1.,1.,1.,1.,1.,1.,1.,1.,1.,1.,1.,1.,1.,1.,
1.,1.,1.,1.,1.,1.,1.,1.,1.,1.,1.,1.,1.,1.,1.,1.,1.,1.,1.,1.,1.,1.,1.,1.,
1.,1.,1.,1.,1.,1.,1.,1.,1.,1.,1.,1.,1.,1.,1.,1.,1.,1.,1.,1.,1.,1.,1.,1.,
1.,1.,1.,1.,1.,1.,1.,1.,1.,1.,1.,1.,1.,1.,1.,1.,1.,1.,1.,1.,1.,1.,1.,1.,
1.,1.,1.,1.,1.,1.,1.,1.,1.,1.,1.,1.,1.,1.,1.,1.,1.,1.,1.,1.,1.,1.,1.,1.,
1.,1.,1.,1.,1.,1.,1.,1.,1.,1.,1.,1.,1.,1.,1.,1.,1.,1.,1.,1.,1.,1.,1.,1.,
1.,1.,1.,1.,1.,1.,1.,1.,1.,1.,1.,1.,1.,1.,1.,1.,1.,1.,1.,1.,1.,1.,1.,1.,
1.,1.,1.,1.,1.,1.,1.,1.,1.,1.,1.,1.,1.,1.,1.,1.,1.,1.,1.,1.,1.))
REPRESENTATION_ITEM('')
);
#867=(
BOUNDED_CURVE()
B_SPLINE_CURVE(5,(#249459,#249460,#249461,#249462,#249463,#249464,#249465,
#249466,#249467,#249468,#249469,#249470,#249471,#249472,#249473,#249474,
#249475,#249476,#249477,#249478,#249479,#249480,#249481,#249482,#249483,
#249484,#249485,#249486,#249487,#249488,#249489,#249490,#249491,#249492,
#249493,#249494,#249495,#249496,#249497,#249498,#249499,#249500,#249501,
#249502,#249503,#249504,#249505,#249506,#249507,#249508,#249509,#249510,
#249511,#249512,#249513,#249514,#249515,#249516,#249517,#249518,#249519,
#249520,#249521,#249522,#249523,#249524,#249525,#249526,#249527,#249528,
#249529,#249530,#249531,#249532,#249533,#249534,#249535,#249536,#249537,
#249538,#249539,#249540,#249541,#249542,#249543,#249544,#249545,#249546,
#249547,#249548,#249549,#249550,#249551,#249552,#249553,#249554,#249555,
#249556,#249557,#249558,#249559,#249560,#249561,#249562,#249563,#249564,
#249565,#249566,#249567,#249568,#249569,#249570,#249571,#249572,#249573,
#249574,#249575,#249576,#249577,#249578,#249579,#249580,#249581,#249582,
#249583,#249584,#249585,#249586,#249587,#249588,#249589,#249590,#249591,
#249592,#249593,#249594,#249595,#249596,#249597,#249598,#249599,#249600,
#249601,#249602,#249603,#249604,#249605,#249606,#249607,#249608,#249609,
#249610,#249611,#249612,#249613,#249614,#249615,#249616,#249617,#249618,
#249619,#249620,#249621,#249622,#249623,#249624,#249625,#249626,#249627,
#249628,#249629,#249630,#249631,#249632,#249633,#249634,#249635,#249636,
#249637,#249638,#249639,#249640,#249641,#249642,#249643,#249644,#249645,
#249646,#249647,#249648,#249649,#249650,#249651,#249652,#249653,#249654,
#249655,#249656,#249657,#249658,#249659,#249660,#249661,#249662,#249663),
 .UNSPECIFIED.,.F.,.F.)
B_SPLINE_CURVE_WITH_KNOTS((6,1,1,1,1,1,1,1,1,1,1,1,1,1,1,1,1,1,1,1,1,1,
1,1,1,1,1,1,1,1,1,1,1,1,1,1,1,1,1,1,1,1,1,1,1,1,1,1,1,1,1,1,1,1,1,1,1,1,
1,1,1,1,1,1,1,1,1,1,1,1,1,1,1,1,1,1,1,1,1,1,1,1,1,1,1,1,1,1,1,1,1,1,1,1,
1,1,1,1,1,1,1,1,1,1,1,1,1,1,1,1,1,1,1,1,1,1,1,1,1,1,1,1,1,1,1,1,1,1,1,1,
1,1,1,1,1,1,1,1,1,1,1,1,1,1,1,1,1,1,1,1,1,1,1,1,1,1,1,1,1,1,1,1,1,1,1,1,
1,1,1,1,1,1,1,1,1,1,1,1,1,1,1,1,1,1,1,1,1,1,1,1,1,1,1,1,1,1,1,1,1,1,6),
(-1.,-0.995000000000001,-0.990000000000001,-0.985000000000001,-0.980000000000001,
-0.975000000000001,-0.970000000000001,-0.965000000000001,-0.960000000000001,
-0.955000000000001,-0.950000000000001,-0.945000000000001,-0.940000000000001,
-0.935000000000001,-0.930000000000001,-0.925000000000001,-0.920000000000001,
-0.915000000000001,-0.910000000000001,-0.905000000000001,-0.900000000000001,
-0.895000000000001,-0.890000000000001,-0.885000000000001,-0.880000000000001,
-0.875000000000001,-0.870000000000001,-0.865000000000001,-0.860000000000001,
-0.855000000000001,-0.850000000000001,-0.845000000000001,-0.840000000000001,
-0.835000000000001,-0.830000000000001,-0.825000000000001,-0.820000000000001,
-0.815000000000001,-0.810000000000001,-0.805000000000001,-0.800000000000001,
-0.795000000000001,-0.790000000000001,-0.785000000000001,-0.780000000000001,
-0.775000000000001,-0.770000000000001,-0.765000000000001,-0.760000000000001,
-0.755000000000001,-0.750000000000001,-0.745000000000001,-0.740000000000001,
-0.735000000000001,-0.730000000000001,-0.725000000000001,-0.720000000000001,
-0.715000000000001,-0.710000000000001,-0.705000000000001,-0.700000000000001,
-0.695000000000001,-0.690000000000001,-0.685,-0.68,-0.675,-0.67,-0.665,
-0.66,-0.655,-0.65,-0.645,-0.64,-0.635,-0.63,-0.625,-0.62,-0.615,-0.61,
-0.605,-0.6,-0.595,-0.59,-0.585,-0.58,-0.575,-0.57,-0.565,-0.56,-0.555,
-0.55,-0.545,-0.54,-0.535,-0.53,-0.525,-0.52,-0.515,-0.51,-0.505,-0.5,-0.495,
-0.49,-0.485,-0.48,-0.475,-0.47,-0.465,-0.46,-0.455,-0.45,-0.445,-0.44,
-0.435,-0.43,-0.425,-0.42,-0.415,-0.41,-0.405,-0.4,-0.395,-0.39,-0.385,
-0.38,-0.375,-0.37,-0.365,-0.36,-0.355,-0.35,-0.345,-0.34,-0.335,-0.33,
-0.325,-0.32,-0.315,-0.31,-0.305,-0.3,-0.295,-0.29,-0.285,-0.28,-0.275,
-0.27,-0.265,-0.26,-0.255,-0.25,-0.245,-0.24,-0.235,-0.23,-0.225,-0.22,
-0.215,-0.21,-0.205,-0.2,-0.195,-0.19,-0.185,-0.18,-0.175,-0.17,-0.165,
-0.16,-0.155,-0.15,-0.145,-0.14,-0.135,-0.13,-0.125,-0.12,-0.115,-0.11,
-0.105,-0.1,-0.095,-0.09,-0.085,-0.08,-0.075,-0.07,-0.065,-0.06,-0.055,
-0.05,-0.045,-0.04,-0.035,-0.03,-0.025,-0.02,-0.015,-0.01,-0.005,0.),
 .UNSPECIFIED.)
CURVE()
GEOMETRIC_REPRESENTATION_ITEM()
RATIONAL_B_SPLINE_CURVE((1.,1.,1.,1.,1.,1.,1.,1.,1.,1.,1.,1.,1.,1.,1.,1.,
1.,1.,1.,1.,1.,1.,1.,1.,1.,1.,1.,1.,1.,1.,1.,1.,1.,1.,1.,1.,1.,1.,1.,1.,
1.,1.,1.,1.,1.,1.,1.,1.,1.,1.,1.,1.,1.,1.,1.,1.,1.,1.,1.,1.,1.,1.,1.,1.,
1.,1.,1.,1.,1.,1.,1.,1.,1.,1.,1.,1.,1.,1.,1.,1.,1.,1.,1.,1.,1.,1.,1.,1.,
1.,1.,1.,1.,1.,1.,1.,1.,1.,1.,1.,1.,1.,1.,1.,1.,1.,1.,1.,1.,1.,1.,1.,1.,
1.,1.,1.,1.,1.,1.,1.,1.,1.,1.,1.,1.,1.,1.,1.,1.,1.,1.,1.,1.,1.,1.,1.,1.,
1.,1.,1.,1.,1.,1.,1.,1.,1.,1.,1.,1.,1.,1.,1.,1.,1.,1.,1.,1.,1.,1.,1.,1.,
1.,1.,1.,1.,1.,1.,1.,1.,1.,1.,1.,1.,1.,1.,1.,1.,1.,1.,1.,1.,1.,1.,1.,1.,
1.,1.,1.,1.,1.,1.,1.,1.,1.,1.,1.,1.,1.,1.,1.,1.,1.,1.,1.,1.,1.))
REPRESENTATION_ITEM('')
);
#868=(
BOUNDED_CURVE()
B_SPLINE_CURVE(5,(#249666,#249667,#249668,#249669,#249670,#249671,#249672,
#249673,#249674,#249675,#249676,#249677,#249678,#249679,#249680,#249681,
#249682,#249683,#249684,#249685,#249686,#249687,#249688,#249689,#249690,
#249691,#249692,#249693,#249694,#249695,#249696,#249697,#249698,#249699,
#249700,#249701,#249702,#249703,#249704,#249705,#249706,#249707,#249708,
#249709,#249710,#249711,#249712,#249713,#249714,#249715,#249716,#249717,
#249718,#249719,#249720,#249721,#249722,#249723,#249724,#249725,#249726,
#249727,#249728,#249729,#249730,#249731,#249732,#249733,#249734,#249735,
#249736,#249737,#249738,#249739,#249740,#249741,#249742,#249743,#249744,
#249745,#249746,#249747,#249748,#249749,#249750,#249751,#249752,#249753,
#249754,#249755,#249756,#249757,#249758,#249759,#249760,#249761,#249762,
#249763,#249764,#249765,#249766,#249767,#249768,#249769,#249770,#249771,
#249772,#249773,#249774,#249775,#249776,#249777,#249778,#249779,#249780,
#249781,#249782,#249783,#249784,#249785,#249786,#249787,#249788,#249789,
#249790,#249791,#249792,#249793,#249794,#249795,#249796,#249797,#249798,
#249799,#249800,#249801,#249802,#249803,#249804,#249805,#249806,#249807,
#249808,#249809,#249810,#249811,#249812,#249813,#249814,#249815,#249816,
#249817,#249818,#249819,#249820,#249821,#249822,#249823,#249824,#249825,
#249826,#249827,#249828,#249829,#249830,#249831,#249832,#249833,#249834,
#249835,#249836,#249837,#249838,#249839,#249840,#249841,#249842,#249843,
#249844,#249845,#249846,#249847,#249848,#249849,#249850,#249851,#249852,
#249853,#249854,#249855,#249856,#249857,#249858,#249859,#249860,#249861,
#249862,#249863,#249864,#249865,#249866,#249867,#249868,#249869,#249870),
 .UNSPECIFIED.,.F.,.F.)
B_SPLINE_CURVE_WITH_KNOTS((6,1,1,1,1,1,1,1,1,1,1,1,1,1,1,1,1,1,1,1,1,1,
1,1,1,1,1,1,1,1,1,1,1,1,1,1,1,1,1,1,1,1,1,1,1,1,1,1,1,1,1,1,1,1,1,1,1,1,
1,1,1,1,1,1,1,1,1,1,1,1,1,1,1,1,1,1,1,1,1,1,1,1,1,1,1,1,1,1,1,1,1,1,1,1,
1,1,1,1,1,1,1,1,1,1,1,1,1,1,1,1,1,1,1,1,1,1,1,1,1,1,1,1,1,1,1,1,1,1,1,1,
1,1,1,1,1,1,1,1,1,1,1,1,1,1,1,1,1,1,1,1,1,1,1,1,1,1,1,1,1,1,1,1,1,1,1,1,
1,1,1,1,1,1,1,1,1,1,1,1,1,1,1,1,1,1,1,1,1,1,1,1,1,1,1,1,1,1,1,1,1,1,6),
(0.,0.005,0.01,0.015,0.02,0.025,0.03,0.035,0.04,0.045,0.05,0.055,0.06,0.065,
0.07,0.075,0.08,0.085,0.09,0.095,0.1,0.105,0.11,0.115,0.12,0.125,0.13,0.135,
0.14,0.145,0.15,0.155,0.16,0.165,0.17,0.175,0.18,0.185,0.19,0.195,0.2,0.205,
0.21,0.215,0.22,0.225,0.23,0.235,0.24,0.245,0.25,0.255,0.26,0.265,0.27,
0.275,0.28,0.285,0.29,0.295,0.3,0.305,0.31,0.315,0.32,0.325,0.33,0.335,
0.34,0.345,0.35,0.355,0.36,0.365,0.37,0.375,0.38,0.385,0.39,0.395,0.4,0.405,
0.41,0.415,0.42,0.425,0.43,0.435,0.44,0.445,0.45,0.455,0.46,0.465,0.47,
0.475,0.48,0.485,0.49,0.495,0.5,0.505,0.51,0.515,0.52,0.525,0.53,0.535,
0.54,0.545,0.55,0.555,0.56,0.565,0.57,0.575,0.58,0.585,0.59,0.595,0.6,0.605,
0.61,0.615,0.62,0.625,0.63,0.635,0.64,0.645,0.65,0.655,0.66,0.665,0.67,
0.675,0.68,0.685,0.690000000000001,0.695000000000001,0.700000000000001,
0.705000000000001,0.710000000000001,0.715000000000001,0.720000000000001,
0.725000000000001,0.730000000000001,0.735000000000001,0.740000000000001,
0.745000000000001,0.750000000000001,0.755000000000001,0.760000000000001,
0.765000000000001,0.770000000000001,0.775000000000001,0.780000000000001,
0.785000000000001,0.790000000000001,0.795000000000001,0.800000000000001,
0.805000000000001,0.810000000000001,0.815000000000001,0.820000000000001,
0.825000000000001,0.830000000000001,0.835000000000001,0.840000000000001,
0.845000000000001,0.850000000000001,0.855000000000001,0.860000000000001,
0.865000000000001,0.870000000000001,0.875000000000001,0.880000000000001,
0.885000000000001,0.890000000000001,0.895000000000001,0.900000000000001,
0.905000000000001,0.910000000000001,0.915000000000001,0.920000000000001,
0.925000000000001,0.930000000000001,0.935000000000001,0.940000000000001,
0.945000000000001,0.950000000000001,0.955000000000001,0.960000000000001,
0.965000000000001,0.970000000000001,0.975000000000001,0.980000000000001,
0.985000000000001,0.990000000000001,0.995000000000001,1.),.UNSPECIFIED.)
CURVE()
GEOMETRIC_REPRESENTATION_ITEM()
RATIONAL_B_SPLINE_CURVE((1.,1.,1.,1.,1.,1.,1.,1.,1.,1.,1.,1.,1.,1.,1.,1.,
1.,1.,1.,1.,1.,1.,1.,1.,1.,1.,1.,1.,1.,1.,1.,1.,1.,1.,1.,1.,1.,1.,1.,1.,
1.,1.,1.,1.,1.,1.,1.,1.,1.,1.,1.,1.,1.,1.,1.,1.,1.,1.,1.,1.,1.,1.,1.,1.,
1.,1.,1.,1.,1.,1.,1.,1.,1.,1.,1.,1.,1.,1.,1.,1.,1.,1.,1.,1.,1.,1.,1.,1.,
1.,1.,1.,1.,1.,1.,1.,1.,1.,1.,1.,1.,1.,1.,1.,1.,1.,1.,1.,1.,1.,1.,1.,1.,
1.,1.,1.,1.,1.,1.,1.,1.,1.,1.,1.,1.,1.,1.,1.,1.,1.,1.,1.,1.,1.,1.,1.,1.,
1.,1.,1.,1.,1.,1.,1.,1.,1.,1.,1.,1.,1.,1.,1.,1.,1.,1.,1.,1.,1.,1.,1.,1.,
1.,1.,1.,1.,1.,1.,1.,1.,1.,1.,1.,1.,1.,1.,1.,1.,1.,1.,1.,1.,1.,1.,1.,1.,
1.,1.,1.,1.,1.,1.,1.,1.,1.,1.,1.,1.,1.,1.,1.,1.,1.,1.,1.,1.,1.))
REPRESENTATION_ITEM('')
);
#869=(
BOUNDED_CURVE()
B_SPLINE_CURVE(5,(#250282,#250283,#250284,#250285,#250286,#250287,#250288,
#250289,#250290,#250291,#250292,#250293,#250294,#250295,#250296,#250297,
#250298,#250299,#250300,#250301,#250302,#250303,#250304,#250305,#250306,
#250307,#250308,#250309,#250310,#250311,#250312,#250313,#250314,#250315,
#250316,#250317,#250318,#250319,#250320,#250321,#250322,#250323,#250324,
#250325,#250326,#250327,#250328,#250329,#250330,#250331,#250332,#250333,
#250334,#250335,#250336,#250337,#250338,#250339,#250340,#250341,#250342,
#250343,#250344,#250345,#250346,#250347,#250348,#250349,#250350,#250351,
#250352,#250353,#250354,#250355,#250356,#250357,#250358,#250359,#250360,
#250361,#250362,#250363,#250364,#250365,#250366,#250367,#250368,#250369,
#250370,#250371,#250372,#250373,#250374,#250375,#250376,#250377,#250378,
#250379,#250380,#250381,#250382,#250383,#250384,#250385,#250386,#250387,
#250388,#250389,#250390,#250391,#250392,#250393,#250394,#250395,#250396,
#250397,#250398,#250399,#250400,#250401,#250402,#250403,#250404,#250405,
#250406,#250407,#250408,#250409,#250410,#250411,#250412,#250413,#250414,
#250415,#250416,#250417,#250418,#250419,#250420,#250421,#250422,#250423,
#250424,#250425,#250426,#250427,#250428,#250429,#250430,#250431,#250432,
#250433,#250434,#250435,#250436,#250437,#250438,#250439,#250440,#250441,
#250442,#250443,#250444,#250445,#250446,#250447,#250448,#250449,#250450,
#250451,#250452,#250453,#250454,#250455,#250456,#250457,#250458,#250459,
#250460,#250461,#250462,#250463,#250464,#250465,#250466,#250467,#250468,
#250469,#250470,#250471,#250472,#250473,#250474,#250475,#250476,#250477,
#250478,#250479,#250480,#250481,#250482,#250483,#250484,#250485,#250486),
 .UNSPECIFIED.,.F.,.F.)
B_SPLINE_CURVE_WITH_KNOTS((6,1,1,1,1,1,1,1,1,1,1,1,1,1,1,1,1,1,1,1,1,1,
1,1,1,1,1,1,1,1,1,1,1,1,1,1,1,1,1,1,1,1,1,1,1,1,1,1,1,1,1,1,1,1,1,1,1,1,
1,1,1,1,1,1,1,1,1,1,1,1,1,1,1,1,1,1,1,1,1,1,1,1,1,1,1,1,1,1,1,1,1,1,1,1,
1,1,1,1,1,1,1,1,1,1,1,1,1,1,1,1,1,1,1,1,1,1,1,1,1,1,1,1,1,1,1,1,1,1,1,1,
1,1,1,1,1,1,1,1,1,1,1,1,1,1,1,1,1,1,1,1,1,1,1,1,1,1,1,1,1,1,1,1,1,1,1,1,
1,1,1,1,1,1,1,1,1,1,1,1,1,1,1,1,1,1,1,1,1,1,1,1,1,1,1,1,1,1,1,1,1,1,6),
(0.,0.005,0.01,0.015,0.02,0.025,0.03,0.035,0.04,0.045,0.05,0.055,0.06,0.065,
0.07,0.075,0.08,0.085,0.09,0.095,0.1,0.105,0.11,0.115,0.12,0.125,0.13,0.135,
0.14,0.145,0.15,0.155,0.16,0.165,0.17,0.175,0.18,0.185,0.19,0.195,0.2,0.205,
0.21,0.215,0.22,0.225,0.23,0.235,0.24,0.245,0.25,0.255,0.26,0.265,0.27,
0.275,0.28,0.285,0.29,0.295,0.3,0.305,0.31,0.315,0.32,0.325,0.33,0.335,
0.34,0.345,0.35,0.355,0.36,0.365,0.37,0.375,0.38,0.385,0.39,0.395,0.4,0.405,
0.41,0.415,0.42,0.425,0.43,0.435,0.44,0.445,0.45,0.455,0.46,0.465,0.47,
0.475,0.48,0.485,0.49,0.495,0.5,0.505,0.51,0.515,0.52,0.525,0.53,0.535,
0.54,0.545,0.55,0.555,0.56,0.565,0.57,0.575,0.58,0.585,0.59,0.595,0.6,0.605,
0.61,0.615,0.62,0.625,0.63,0.635,0.64,0.645,0.65,0.655,0.66,0.665,0.67,
0.675,0.68,0.685,0.690000000000001,0.695000000000001,0.700000000000001,
0.705000000000001,0.710000000000001,0.715000000000001,0.720000000000001,
0.725000000000001,0.730000000000001,0.735000000000001,0.740000000000001,
0.745000000000001,0.750000000000001,0.755000000000001,0.760000000000001,
0.765000000000001,0.770000000000001,0.775000000000001,0.780000000000001,
0.785000000000001,0.790000000000001,0.795000000000001,0.800000000000001,
0.805000000000001,0.810000000000001,0.815000000000001,0.820000000000001,
0.825000000000001,0.830000000000001,0.835000000000001,0.840000000000001,
0.845000000000001,0.850000000000001,0.855000000000001,0.860000000000001,
0.865000000000001,0.870000000000001,0.875000000000001,0.880000000000001,
0.885000000000001,0.890000000000001,0.895000000000001,0.900000000000001,
0.905000000000001,0.910000000000001,0.915000000000001,0.920000000000001,
0.925000000000001,0.930000000000001,0.935000000000001,0.940000000000001,
0.945000000000001,0.950000000000001,0.955000000000001,0.960000000000001,
0.965000000000001,0.970000000000001,0.975000000000001,0.980000000000001,
0.985000000000001,0.990000000000001,0.995000000000001,1.),.UNSPECIFIED.)
CURVE()
GEOMETRIC_REPRESENTATION_ITEM()
RATIONAL_B_SPLINE_CURVE((1.,1.,1.,1.,1.,1.,1.,1.,1.,1.,1.,1.,1.,1.,1.,1.,
1.,1.,1.,1.,1.,1.,1.,1.,1.,1.,1.,1.,1.,1.,1.,1.,1.,1.,1.,1.,1.,1.,1.,1.,
1.,1.,1.,1.,1.,1.,1.,1.,1.,1.,1.,1.,1.,1.,1.,1.,1.,1.,1.,1.,1.,1.,1.,1.,
1.,1.,1.,1.,1.,1.,1.,1.,1.,1.,1.,1.,1.,1.,1.,1.,1.,1.,1.,1.,1.,1.,1.,1.,
1.,1.,1.,1.,1.,1.,1.,1.,1.,1.,1.,1.,1.,1.,1.,1.,1.,1.,1.,1.,1.,1.,1.,1.,
1.,1.,1.,1.,1.,1.,1.,1.,1.,1.,1.,1.,1.,1.,1.,1.,1.,1.,1.,1.,1.,1.,1.,1.,
1.,1.,1.,1.,1.,1.,1.,1.,1.,1.,1.,1.,1.,1.,1.,1.,1.,1.,1.,1.,1.,1.,1.,1.,
1.,1.,1.,1.,1.,1.,1.,1.,1.,1.,1.,1.,1.,1.,1.,1.,1.,1.,1.,1.,1.,1.,1.,1.,
1.,1.,1.,1.,1.,1.,1.,1.,1.,1.,1.,1.,1.,1.,1.,1.,1.,1.,1.,1.,1.))
REPRESENTATION_ITEM('')
);
#870=(
BOUNDED_CURVE()
B_SPLINE_CURVE(5,(#250488,#250489,#250490,#250491,#250492,#250493,#250494,
#250495,#250496,#250497,#250498,#250499,#250500,#250501,#250502,#250503,
#250504,#250505,#250506,#250507,#250508,#250509,#250510,#250511,#250512,
#250513,#250514,#250515,#250516,#250517,#250518,#250519,#250520,#250521,
#250522,#250523,#250524,#250525,#250526,#250527,#250528,#250529,#250530,
#250531,#250532,#250533,#250534,#250535,#250536,#250537,#250538,#250539,
#250540,#250541,#250542,#250543,#250544,#250545,#250546,#250547,#250548,
#250549,#250550,#250551,#250552,#250553,#250554,#250555,#250556,#250557,
#250558,#250559,#250560,#250561,#250562,#250563,#250564,#250565,#250566,
#250567,#250568,#250569,#250570,#250571,#250572,#250573,#250574,#250575,
#250576,#250577,#250578,#250579,#250580,#250581,#250582,#250583,#250584,
#250585,#250586,#250587,#250588,#250589,#250590,#250591,#250592,#250593,
#250594,#250595,#250596,#250597,#250598,#250599,#250600,#250601,#250602,
#250603,#250604,#250605,#250606,#250607,#250608,#250609,#250610,#250611,
#250612,#250613,#250614,#250615,#250616,#250617,#250618,#250619,#250620,
#250621,#250622,#250623,#250624,#250625,#250626,#250627,#250628,#250629,
#250630,#250631,#250632,#250633,#250634,#250635,#250636,#250637,#250638,
#250639,#250640,#250641,#250642,#250643,#250644,#250645,#250646,#250647,
#250648,#250649,#250650,#250651,#250652,#250653,#250654,#250655,#250656,
#250657,#250658,#250659,#250660,#250661,#250662,#250663,#250664,#250665,
#250666,#250667,#250668,#250669,#250670,#250671,#250672,#250673,#250674,
#250675,#250676,#250677,#250678,#250679,#250680,#250681,#250682,#250683,
#250684,#250685,#250686,#250687,#250688,#250689,#250690,#250691,#250692),
 .UNSPECIFIED.,.F.,.F.)
B_SPLINE_CURVE_WITH_KNOTS((6,1,1,1,1,1,1,1,1,1,1,1,1,1,1,1,1,1,1,1,1,1,
1,1,1,1,1,1,1,1,1,1,1,1,1,1,1,1,1,1,1,1,1,1,1,1,1,1,1,1,1,1,1,1,1,1,1,1,
1,1,1,1,1,1,1,1,1,1,1,1,1,1,1,1,1,1,1,1,1,1,1,1,1,1,1,1,1,1,1,1,1,1,1,1,
1,1,1,1,1,1,1,1,1,1,1,1,1,1,1,1,1,1,1,1,1,1,1,1,1,1,1,1,1,1,1,1,1,1,1,1,
1,1,1,1,1,1,1,1,1,1,1,1,1,1,1,1,1,1,1,1,1,1,1,1,1,1,1,1,1,1,1,1,1,1,1,1,
1,1,1,1,1,1,1,1,1,1,1,1,1,1,1,1,1,1,1,1,1,1,1,1,1,1,1,1,1,1,1,1,1,1,6),
(-1.,-0.995000000000001,-0.990000000000001,-0.985000000000001,-0.980000000000001,
-0.975000000000001,-0.970000000000001,-0.965000000000001,-0.960000000000001,
-0.955000000000001,-0.950000000000001,-0.945000000000001,-0.940000000000001,
-0.935000000000001,-0.930000000000001,-0.925000000000001,-0.920000000000001,
-0.915000000000001,-0.910000000000001,-0.905000000000001,-0.900000000000001,
-0.895000000000001,-0.890000000000001,-0.885000000000001,-0.880000000000001,
-0.875000000000001,-0.870000000000001,-0.865000000000001,-0.860000000000001,
-0.855000000000001,-0.850000000000001,-0.845000000000001,-0.840000000000001,
-0.835000000000001,-0.830000000000001,-0.825000000000001,-0.820000000000001,
-0.815000000000001,-0.810000000000001,-0.805000000000001,-0.800000000000001,
-0.795000000000001,-0.790000000000001,-0.785000000000001,-0.780000000000001,
-0.775000000000001,-0.770000000000001,-0.765000000000001,-0.760000000000001,
-0.755000000000001,-0.750000000000001,-0.745000000000001,-0.740000000000001,
-0.735000000000001,-0.730000000000001,-0.725000000000001,-0.720000000000001,
-0.715000000000001,-0.710000000000001,-0.705000000000001,-0.700000000000001,
-0.695000000000001,-0.690000000000001,-0.685,-0.68,-0.675,-0.67,-0.665,
-0.66,-0.655,-0.65,-0.645,-0.64,-0.635,-0.63,-0.625,-0.62,-0.615,-0.61,
-0.605,-0.6,-0.595,-0.59,-0.585,-0.58,-0.575,-0.57,-0.565,-0.56,-0.555,
-0.55,-0.545,-0.54,-0.535,-0.53,-0.525,-0.52,-0.515,-0.51,-0.505,-0.5,-0.495,
-0.49,-0.485,-0.48,-0.475,-0.47,-0.465,-0.46,-0.455,-0.45,-0.445,-0.44,
-0.435,-0.43,-0.425,-0.42,-0.415,-0.41,-0.405,-0.4,-0.395,-0.39,-0.385,
-0.38,-0.375,-0.37,-0.365,-0.36,-0.355,-0.35,-0.345,-0.34,-0.335,-0.33,
-0.325,-0.32,-0.315,-0.31,-0.305,-0.3,-0.295,-0.29,-0.285,-0.28,-0.275,
-0.27,-0.265,-0.26,-0.255,-0.25,-0.245,-0.24,-0.235,-0.23,-0.225,-0.22,
-0.215,-0.21,-0.205,-0.2,-0.195,-0.19,-0.185,-0.18,-0.175,-0.17,-0.165,
-0.16,-0.155,-0.15,-0.145,-0.14,-0.135,-0.13,-0.125,-0.12,-0.115,-0.11,
-0.105,-0.1,-0.095,-0.09,-0.085,-0.08,-0.075,-0.07,-0.065,-0.06,-0.055,
-0.05,-0.045,-0.04,-0.035,-0.03,-0.025,-0.02,-0.015,-0.01,-0.005,0.),
 .UNSPECIFIED.)
CURVE()
GEOMETRIC_REPRESENTATION_ITEM()
RATIONAL_B_SPLINE_CURVE((1.,1.,1.,1.,1.,1.,1.,1.,1.,1.,1.,1.,1.,1.,1.,1.,
1.,1.,1.,1.,1.,1.,1.,1.,1.,1.,1.,1.,1.,1.,1.,1.,1.,1.,1.,1.,1.,1.,1.,1.,
1.,1.,1.,1.,1.,1.,1.,1.,1.,1.,1.,1.,1.,1.,1.,1.,1.,1.,1.,1.,1.,1.,1.,1.,
1.,1.,1.,1.,1.,1.,1.,1.,1.,1.,1.,1.,1.,1.,1.,1.,1.,1.,1.,1.,1.,1.,1.,1.,
1.,1.,1.,1.,1.,1.,1.,1.,1.,1.,1.,1.,1.,1.,1.,1.,1.,1.,1.,1.,1.,1.,1.,1.,
1.,1.,1.,1.,1.,1.,1.,1.,1.,1.,1.,1.,1.,1.,1.,1.,1.,1.,1.,1.,1.,1.,1.,1.,
1.,1.,1.,1.,1.,1.,1.,1.,1.,1.,1.,1.,1.,1.,1.,1.,1.,1.,1.,1.,1.,1.,1.,1.,
1.,1.,1.,1.,1.,1.,1.,1.,1.,1.,1.,1.,1.,1.,1.,1.,1.,1.,1.,1.,1.,1.,1.,1.,
1.,1.,1.,1.,1.,1.,1.,1.,1.,1.,1.,1.,1.,1.,1.,1.,1.,1.,1.,1.,1.))
REPRESENTATION_ITEM('')
);
#871=(
BOUNDED_CURVE()
B_SPLINE_CURVE(5,(#251111,#251112,#251113,#251114,#251115,#251116,#251117,
#251118,#251119,#251120,#251121,#251122,#251123,#251124,#251125,#251126,
#251127,#251128,#251129,#251130,#251131,#251132,#251133,#251134,#251135,
#251136,#251137,#251138,#251139,#251140,#251141,#251142,#251143,#251144,
#251145,#251146,#251147,#251148,#251149,#251150,#251151,#251152,#251153,
#251154,#251155,#251156,#251157,#251158,#251159,#251160,#251161,#251162,
#251163,#251164,#251165,#251166,#251167,#251168,#251169,#251170,#251171,
#251172,#251173,#251174,#251175,#251176,#251177,#251178,#251179,#251180,
#251181,#251182,#251183,#251184,#251185,#251186,#251187,#251188,#251189,
#251190,#251191,#251192,#251193,#251194,#251195,#251196,#251197,#251198,
#251199,#251200,#251201,#251202,#251203,#251204,#251205,#251206,#251207,
#251208,#251209,#251210,#251211,#251212,#251213,#251214,#251215,#251216,
#251217,#251218,#251219,#251220,#251221,#251222,#251223,#251224,#251225,
#251226,#251227,#251228,#251229,#251230,#251231,#251232,#251233,#251234,
#251235,#251236,#251237,#251238,#251239,#251240,#251241,#251242,#251243,
#251244,#251245,#251246,#251247,#251248,#251249,#251250,#251251,#251252,
#251253,#251254,#251255,#251256,#251257,#251258,#251259,#251260,#251261,
#251262,#251263,#251264,#251265,#251266,#251267,#251268,#251269,#251270,
#251271,#251272,#251273,#251274,#251275,#251276,#251277,#251278,#251279,
#251280,#251281,#251282,#251283,#251284,#251285,#251286,#251287,#251288,
#251289,#251290,#251291,#251292,#251293,#251294,#251295,#251296,#251297,
#251298,#251299,#251300,#251301,#251302,#251303,#251304,#251305,#251306,
#251307,#251308,#251309,#251310,#251311,#251312,#251313,#251314,#251315),
 .UNSPECIFIED.,.F.,.F.)
B_SPLINE_CURVE_WITH_KNOTS((6,1,1,1,1,1,1,1,1,1,1,1,1,1,1,1,1,1,1,1,1,1,
1,1,1,1,1,1,1,1,1,1,1,1,1,1,1,1,1,1,1,1,1,1,1,1,1,1,1,1,1,1,1,1,1,1,1,1,
1,1,1,1,1,1,1,1,1,1,1,1,1,1,1,1,1,1,1,1,1,1,1,1,1,1,1,1,1,1,1,1,1,1,1,1,
1,1,1,1,1,1,1,1,1,1,1,1,1,1,1,1,1,1,1,1,1,1,1,1,1,1,1,1,1,1,1,1,1,1,1,1,
1,1,1,1,1,1,1,1,1,1,1,1,1,1,1,1,1,1,1,1,1,1,1,1,1,1,1,1,1,1,1,1,1,1,1,1,
1,1,1,1,1,1,1,1,1,1,1,1,1,1,1,1,1,1,1,1,1,1,1,1,1,1,1,1,1,1,1,1,1,1,6),
(-1.,-0.995000000000001,-0.990000000000001,-0.985000000000001,-0.980000000000001,
-0.975000000000001,-0.970000000000001,-0.965000000000001,-0.960000000000001,
-0.955000000000001,-0.950000000000001,-0.945000000000001,-0.940000000000001,
-0.935000000000001,-0.930000000000001,-0.925000000000001,-0.920000000000001,
-0.915000000000001,-0.910000000000001,-0.905000000000001,-0.900000000000001,
-0.895000000000001,-0.890000000000001,-0.885000000000001,-0.880000000000001,
-0.875000000000001,-0.870000000000001,-0.865000000000001,-0.860000000000001,
-0.855000000000001,-0.850000000000001,-0.845000000000001,-0.840000000000001,
-0.835000000000001,-0.830000000000001,-0.825000000000001,-0.820000000000001,
-0.815000000000001,-0.810000000000001,-0.805000000000001,-0.800000000000001,
-0.795000000000001,-0.790000000000001,-0.785000000000001,-0.780000000000001,
-0.775000000000001,-0.770000000000001,-0.765000000000001,-0.760000000000001,
-0.755000000000001,-0.750000000000001,-0.745000000000001,-0.740000000000001,
-0.735000000000001,-0.730000000000001,-0.725000000000001,-0.720000000000001,
-0.715000000000001,-0.710000000000001,-0.705000000000001,-0.700000000000001,
-0.695000000000001,-0.690000000000001,-0.685,-0.68,-0.675,-0.67,-0.665,
-0.66,-0.655,-0.65,-0.645,-0.64,-0.635,-0.63,-0.625,-0.62,-0.615,-0.61,
-0.605,-0.6,-0.595,-0.59,-0.585,-0.58,-0.575,-0.57,-0.565,-0.56,-0.555,
-0.55,-0.545,-0.54,-0.535,-0.53,-0.525,-0.52,-0.515,-0.51,-0.505,-0.5,-0.495,
-0.49,-0.485,-0.48,-0.475,-0.47,-0.465,-0.46,-0.455,-0.45,-0.445,-0.44,
-0.435,-0.43,-0.425,-0.42,-0.415,-0.41,-0.405,-0.4,-0.395,-0.39,-0.385,
-0.38,-0.375,-0.37,-0.365,-0.36,-0.355,-0.35,-0.345,-0.34,-0.335,-0.33,
-0.325,-0.32,-0.315,-0.31,-0.305,-0.3,-0.295,-0.29,-0.285,-0.28,-0.275,
-0.27,-0.265,-0.26,-0.255,-0.25,-0.245,-0.24,-0.235,-0.23,-0.225,-0.22,
-0.215,-0.21,-0.205,-0.2,-0.195,-0.19,-0.185,-0.18,-0.175,-0.17,-0.165,
-0.16,-0.155,-0.15,-0.145,-0.14,-0.135,-0.13,-0.125,-0.12,-0.115,-0.11,
-0.105,-0.1,-0.095,-0.09,-0.085,-0.08,-0.075,-0.07,-0.065,-0.06,-0.055,
-0.05,-0.045,-0.04,-0.035,-0.03,-0.025,-0.02,-0.015,-0.01,-0.005,0.),
 .UNSPECIFIED.)
CURVE()
GEOMETRIC_REPRESENTATION_ITEM()
RATIONAL_B_SPLINE_CURVE((1.,1.,1.,1.,1.,1.,1.,1.,1.,1.,1.,1.,1.,1.,1.,1.,
1.,1.,1.,1.,1.,1.,1.,1.,1.,1.,1.,1.,1.,1.,1.,1.,1.,1.,1.,1.,1.,1.,1.,1.,
1.,1.,1.,1.,1.,1.,1.,1.,1.,1.,1.,1.,1.,1.,1.,1.,1.,1.,1.,1.,1.,1.,1.,1.,
1.,1.,1.,1.,1.,1.,1.,1.,1.,1.,1.,1.,1.,1.,1.,1.,1.,1.,1.,1.,1.,1.,1.,1.,
1.,1.,1.,1.,1.,1.,1.,1.,1.,1.,1.,1.,1.,1.,1.,1.,1.,1.,1.,1.,1.,1.,1.,1.,
1.,1.,1.,1.,1.,1.,1.,1.,1.,1.,1.,1.,1.,1.,1.,1.,1.,1.,1.,1.,1.,1.,1.,1.,
1.,1.,1.,1.,1.,1.,1.,1.,1.,1.,1.,1.,1.,1.,1.,1.,1.,1.,1.,1.,1.,1.,1.,1.,
1.,1.,1.,1.,1.,1.,1.,1.,1.,1.,1.,1.,1.,1.,1.,1.,1.,1.,1.,1.,1.,1.,1.,1.,
1.,1.,1.,1.,1.,1.,1.,1.,1.,1.,1.,1.,1.,1.,1.,1.,1.,1.,1.,1.,1.))
REPRESENTATION_ITEM('')
);
#872=(
BOUNDED_CURVE()
B_SPLINE_CURVE(5,(#251318,#251319,#251320,#251321,#251322,#251323,#251324,
#251325,#251326,#251327,#251328,#251329,#251330,#251331,#251332,#251333,
#251334,#251335,#251336,#251337,#251338,#251339,#251340,#251341,#251342,
#251343,#251344,#251345,#251346,#251347,#251348,#251349,#251350,#251351,
#251352,#251353,#251354,#251355,#251356,#251357,#251358,#251359,#251360,
#251361,#251362,#251363,#251364,#251365,#251366,#251367,#251368,#251369,
#251370,#251371,#251372,#251373,#251374,#251375,#251376,#251377,#251378,
#251379,#251380,#251381,#251382,#251383,#251384,#251385,#251386,#251387,
#251388,#251389,#251390,#251391,#251392,#251393,#251394,#251395,#251396,
#251397,#251398,#251399,#251400,#251401,#251402,#251403,#251404,#251405,
#251406,#251407,#251408,#251409,#251410,#251411,#251412,#251413,#251414,
#251415,#251416,#251417,#251418,#251419,#251420,#251421,#251422,#251423,
#251424,#251425,#251426,#251427,#251428,#251429,#251430,#251431,#251432,
#251433,#251434,#251435,#251436,#251437,#251438,#251439,#251440,#251441,
#251442,#251443,#251444,#251445,#251446,#251447,#251448,#251449,#251450,
#251451,#251452,#251453,#251454,#251455,#251456,#251457,#251458,#251459,
#251460,#251461,#251462,#251463,#251464,#251465,#251466,#251467,#251468,
#251469,#251470,#251471,#251472,#251473,#251474,#251475,#251476,#251477,
#251478,#251479,#251480,#251481,#251482,#251483,#251484,#251485,#251486,
#251487,#251488,#251489,#251490,#251491,#251492,#251493,#251494,#251495,
#251496,#251497,#251498,#251499,#251500,#251501,#251502,#251503,#251504,
#251505,#251506,#251507,#251508,#251509,#251510,#251511,#251512,#251513,
#251514,#251515,#251516,#251517,#251518,#251519,#251520,#251521,#251522),
 .UNSPECIFIED.,.F.,.F.)
B_SPLINE_CURVE_WITH_KNOTS((6,1,1,1,1,1,1,1,1,1,1,1,1,1,1,1,1,1,1,1,1,1,
1,1,1,1,1,1,1,1,1,1,1,1,1,1,1,1,1,1,1,1,1,1,1,1,1,1,1,1,1,1,1,1,1,1,1,1,
1,1,1,1,1,1,1,1,1,1,1,1,1,1,1,1,1,1,1,1,1,1,1,1,1,1,1,1,1,1,1,1,1,1,1,1,
1,1,1,1,1,1,1,1,1,1,1,1,1,1,1,1,1,1,1,1,1,1,1,1,1,1,1,1,1,1,1,1,1,1,1,1,
1,1,1,1,1,1,1,1,1,1,1,1,1,1,1,1,1,1,1,1,1,1,1,1,1,1,1,1,1,1,1,1,1,1,1,1,
1,1,1,1,1,1,1,1,1,1,1,1,1,1,1,1,1,1,1,1,1,1,1,1,1,1,1,1,1,1,1,1,1,1,6),
(0.,0.005,0.01,0.015,0.02,0.025,0.03,0.035,0.04,0.045,0.05,0.055,0.06,0.065,
0.07,0.075,0.08,0.085,0.09,0.095,0.1,0.105,0.11,0.115,0.12,0.125,0.13,0.135,
0.14,0.145,0.15,0.155,0.16,0.165,0.17,0.175,0.18,0.185,0.19,0.195,0.2,0.205,
0.21,0.215,0.22,0.225,0.23,0.235,0.24,0.245,0.25,0.255,0.26,0.265,0.27,
0.275,0.28,0.285,0.29,0.295,0.3,0.305,0.31,0.315,0.32,0.325,0.33,0.335,
0.34,0.345,0.35,0.355,0.36,0.365,0.37,0.375,0.38,0.385,0.39,0.395,0.4,0.405,
0.41,0.415,0.42,0.425,0.43,0.435,0.44,0.445,0.45,0.455,0.46,0.465,0.47,
0.475,0.48,0.485,0.49,0.495,0.5,0.505,0.51,0.515,0.52,0.525,0.53,0.535,
0.54,0.545,0.55,0.555,0.56,0.565,0.57,0.575,0.58,0.585,0.59,0.595,0.6,0.605,
0.61,0.615,0.62,0.625,0.63,0.635,0.64,0.645,0.65,0.655,0.66,0.665,0.67,
0.675,0.68,0.685,0.690000000000001,0.695000000000001,0.700000000000001,
0.705000000000001,0.710000000000001,0.715000000000001,0.720000000000001,
0.725000000000001,0.730000000000001,0.735000000000001,0.740000000000001,
0.745000000000001,0.750000000000001,0.755000000000001,0.760000000000001,
0.765000000000001,0.770000000000001,0.775000000000001,0.780000000000001,
0.785000000000001,0.790000000000001,0.795000000000001,0.800000000000001,
0.805000000000001,0.810000000000001,0.815000000000001,0.820000000000001,
0.825000000000001,0.830000000000001,0.835000000000001,0.840000000000001,
0.845000000000001,0.850000000000001,0.855000000000001,0.860000000000001,
0.865000000000001,0.870000000000001,0.875000000000001,0.880000000000001,
0.885000000000001,0.890000000000001,0.895000000000001,0.900000000000001,
0.905000000000001,0.910000000000001,0.915000000000001,0.920000000000001,
0.925000000000001,0.930000000000001,0.935000000000001,0.940000000000001,
0.945000000000001,0.950000000000001,0.955000000000001,0.960000000000001,
0.965000000000001,0.970000000000001,0.975000000000001,0.980000000000001,
0.985000000000001,0.990000000000001,0.995000000000001,1.),.UNSPECIFIED.)
CURVE()
GEOMETRIC_REPRESENTATION_ITEM()
RATIONAL_B_SPLINE_CURVE((1.,1.,1.,1.,1.,1.,1.,1.,1.,1.,1.,1.,1.,1.,1.,1.,
1.,1.,1.,1.,1.,1.,1.,1.,1.,1.,1.,1.,1.,1.,1.,1.,1.,1.,1.,1.,1.,1.,1.,1.,
1.,1.,1.,1.,1.,1.,1.,1.,1.,1.,1.,1.,1.,1.,1.,1.,1.,1.,1.,1.,1.,1.,1.,1.,
1.,1.,1.,1.,1.,1.,1.,1.,1.,1.,1.,1.,1.,1.,1.,1.,1.,1.,1.,1.,1.,1.,1.,1.,
1.,1.,1.,1.,1.,1.,1.,1.,1.,1.,1.,1.,1.,1.,1.,1.,1.,1.,1.,1.,1.,1.,1.,1.,
1.,1.,1.,1.,1.,1.,1.,1.,1.,1.,1.,1.,1.,1.,1.,1.,1.,1.,1.,1.,1.,1.,1.,1.,
1.,1.,1.,1.,1.,1.,1.,1.,1.,1.,1.,1.,1.,1.,1.,1.,1.,1.,1.,1.,1.,1.,1.,1.,
1.,1.,1.,1.,1.,1.,1.,1.,1.,1.,1.,1.,1.,1.,1.,1.,1.,1.,1.,1.,1.,1.,1.,1.,
1.,1.,1.,1.,1.,1.,1.,1.,1.,1.,1.,1.,1.,1.,1.,1.,1.,1.,1.,1.,1.))
REPRESENTATION_ITEM('')
);
#873=(
BOUNDED_CURVE()
B_SPLINE_CURVE(5,(#251934,#251935,#251936,#251937,#251938,#251939,#251940,
#251941,#251942,#251943,#251944,#251945,#251946,#251947,#251948,#251949,
#251950,#251951,#251952,#251953,#251954,#251955,#251956,#251957,#251958,
#251959,#251960,#251961,#251962,#251963,#251964,#251965,#251966,#251967,
#251968,#251969,#251970,#251971,#251972,#251973,#251974,#251975,#251976,
#251977,#251978,#251979,#251980,#251981,#251982,#251983,#251984,#251985,
#251986,#251987,#251988,#251989,#251990,#251991,#251992,#251993,#251994,
#251995,#251996,#251997,#251998,#251999,#252000,#252001,#252002,#252003,
#252004,#252005,#252006,#252007,#252008,#252009,#252010,#252011,#252012,
#252013,#252014,#252015,#252016,#252017,#252018,#252019,#252020,#252021,
#252022,#252023,#252024,#252025,#252026,#252027,#252028,#252029,#252030,
#252031,#252032,#252033,#252034,#252035,#252036,#252037,#252038,#252039,
#252040,#252041,#252042,#252043,#252044,#252045,#252046,#252047,#252048,
#252049,#252050,#252051,#252052,#252053,#252054,#252055,#252056,#252057,
#252058,#252059,#252060,#252061,#252062,#252063,#252064,#252065,#252066,
#252067,#252068,#252069,#252070,#252071,#252072,#252073,#252074,#252075,
#252076,#252077,#252078,#252079,#252080,#252081,#252082,#252083,#252084,
#252085,#252086,#252087,#252088,#252089,#252090,#252091,#252092,#252093,
#252094,#252095,#252096,#252097,#252098,#252099,#252100,#252101,#252102,
#252103,#252104,#252105,#252106,#252107,#252108,#252109,#252110,#252111,
#252112,#252113,#252114,#252115,#252116,#252117,#252118,#252119,#252120,
#252121,#252122,#252123,#252124,#252125,#252126,#252127,#252128,#252129,
#252130,#252131,#252132,#252133,#252134,#252135,#252136,#252137,#252138),
 .UNSPECIFIED.,.F.,.F.)
B_SPLINE_CURVE_WITH_KNOTS((6,1,1,1,1,1,1,1,1,1,1,1,1,1,1,1,1,1,1,1,1,1,
1,1,1,1,1,1,1,1,1,1,1,1,1,1,1,1,1,1,1,1,1,1,1,1,1,1,1,1,1,1,1,1,1,1,1,1,
1,1,1,1,1,1,1,1,1,1,1,1,1,1,1,1,1,1,1,1,1,1,1,1,1,1,1,1,1,1,1,1,1,1,1,1,
1,1,1,1,1,1,1,1,1,1,1,1,1,1,1,1,1,1,1,1,1,1,1,1,1,1,1,1,1,1,1,1,1,1,1,1,
1,1,1,1,1,1,1,1,1,1,1,1,1,1,1,1,1,1,1,1,1,1,1,1,1,1,1,1,1,1,1,1,1,1,1,1,
1,1,1,1,1,1,1,1,1,1,1,1,1,1,1,1,1,1,1,1,1,1,1,1,1,1,1,1,1,1,1,1,1,1,6),
(0.,0.005,0.01,0.015,0.02,0.025,0.03,0.035,0.04,0.045,0.05,0.055,0.06,0.065,
0.07,0.075,0.08,0.085,0.09,0.095,0.1,0.105,0.11,0.115,0.12,0.125,0.13,0.135,
0.14,0.145,0.15,0.155,0.16,0.165,0.17,0.175,0.18,0.185,0.19,0.195,0.2,0.205,
0.21,0.215,0.22,0.225,0.23,0.235,0.24,0.245,0.25,0.255,0.26,0.265,0.27,
0.275,0.28,0.285,0.29,0.295,0.3,0.305,0.31,0.315,0.32,0.325,0.33,0.335,
0.34,0.345,0.35,0.355,0.36,0.365,0.37,0.375,0.38,0.385,0.39,0.395,0.4,0.405,
0.41,0.415,0.42,0.425,0.43,0.435,0.44,0.445,0.45,0.455,0.46,0.465,0.47,
0.475,0.48,0.485,0.49,0.495,0.5,0.505,0.51,0.515,0.52,0.525,0.53,0.535,
0.54,0.545,0.55,0.555,0.56,0.565,0.57,0.575,0.58,0.585,0.59,0.595,0.6,0.605,
0.61,0.615,0.62,0.625,0.63,0.635,0.64,0.645,0.65,0.655,0.66,0.665,0.67,
0.675,0.68,0.685,0.690000000000001,0.695000000000001,0.700000000000001,
0.705000000000001,0.710000000000001,0.715000000000001,0.720000000000001,
0.725000000000001,0.730000000000001,0.735000000000001,0.740000000000001,
0.745000000000001,0.750000000000001,0.755000000000001,0.760000000000001,
0.765000000000001,0.770000000000001,0.775000000000001,0.780000000000001,
0.785000000000001,0.790000000000001,0.795000000000001,0.800000000000001,
0.805000000000001,0.810000000000001,0.815000000000001,0.820000000000001,
0.825000000000001,0.830000000000001,0.835000000000001,0.840000000000001,
0.845000000000001,0.850000000000001,0.855000000000001,0.860000000000001,
0.865000000000001,0.870000000000001,0.875000000000001,0.880000000000001,
0.885000000000001,0.890000000000001,0.895000000000001,0.900000000000001,
0.905000000000001,0.910000000000001,0.915000000000001,0.920000000000001,
0.925000000000001,0.930000000000001,0.935000000000001,0.940000000000001,
0.945000000000001,0.950000000000001,0.955000000000001,0.960000000000001,
0.965000000000001,0.970000000000001,0.975000000000001,0.980000000000001,
0.985000000000001,0.990000000000001,0.995000000000001,1.),.UNSPECIFIED.)
CURVE()
GEOMETRIC_REPRESENTATION_ITEM()
RATIONAL_B_SPLINE_CURVE((1.,1.,1.,1.,1.,1.,1.,1.,1.,1.,1.,1.,1.,1.,1.,1.,
1.,1.,1.,1.,1.,1.,1.,1.,1.,1.,1.,1.,1.,1.,1.,1.,1.,1.,1.,1.,1.,1.,1.,1.,
1.,1.,1.,1.,1.,1.,1.,1.,1.,1.,1.,1.,1.,1.,1.,1.,1.,1.,1.,1.,1.,1.,1.,1.,
1.,1.,1.,1.,1.,1.,1.,1.,1.,1.,1.,1.,1.,1.,1.,1.,1.,1.,1.,1.,1.,1.,1.,1.,
1.,1.,1.,1.,1.,1.,1.,1.,1.,1.,1.,1.,1.,1.,1.,1.,1.,1.,1.,1.,1.,1.,1.,1.,
1.,1.,1.,1.,1.,1.,1.,1.,1.,1.,1.,1.,1.,1.,1.,1.,1.,1.,1.,1.,1.,1.,1.,1.,
1.,1.,1.,1.,1.,1.,1.,1.,1.,1.,1.,1.,1.,1.,1.,1.,1.,1.,1.,1.,1.,1.,1.,1.,
1.,1.,1.,1.,1.,1.,1.,1.,1.,1.,1.,1.,1.,1.,1.,1.,1.,1.,1.,1.,1.,1.,1.,1.,
1.,1.,1.,1.,1.,1.,1.,1.,1.,1.,1.,1.,1.,1.,1.,1.,1.,1.,1.,1.,1.))
REPRESENTATION_ITEM('')
);
#874=(
BOUNDED_CURVE()
B_SPLINE_CURVE(5,(#252140,#252141,#252142,#252143,#252144,#252145,#252146,
#252147,#252148,#252149,#252150,#252151,#252152,#252153,#252154,#252155,
#252156,#252157,#252158,#252159,#252160,#252161,#252162,#252163,#252164,
#252165,#252166,#252167,#252168,#252169,#252170,#252171,#252172,#252173,
#252174,#252175,#252176,#252177,#252178,#252179,#252180,#252181,#252182,
#252183,#252184,#252185,#252186,#252187,#252188,#252189,#252190,#252191,
#252192,#252193,#252194,#252195,#252196,#252197,#252198,#252199,#252200,
#252201,#252202,#252203,#252204,#252205,#252206,#252207,#252208,#252209,
#252210,#252211,#252212,#252213,#252214,#252215,#252216,#252217,#252218,
#252219,#252220,#252221,#252222,#252223,#252224,#252225,#252226,#252227,
#252228,#252229,#252230,#252231,#252232,#252233,#252234,#252235,#252236,
#252237,#252238,#252239,#252240,#252241,#252242,#252243,#252244,#252245,
#252246,#252247,#252248,#252249,#252250,#252251,#252252,#252253,#252254,
#252255,#252256,#252257,#252258,#252259,#252260,#252261,#252262,#252263,
#252264,#252265,#252266,#252267,#252268,#252269,#252270,#252271,#252272,
#252273,#252274,#252275,#252276,#252277,#252278,#252279,#252280,#252281,
#252282,#252283,#252284,#252285,#252286,#252287,#252288,#252289,#252290,
#252291,#252292,#252293,#252294,#252295,#252296,#252297,#252298,#252299,
#252300,#252301,#252302,#252303,#252304,#252305,#252306,#252307,#252308,
#252309,#252310,#252311,#252312,#252313,#252314,#252315,#252316,#252317,
#252318,#252319,#252320,#252321,#252322,#252323,#252324,#252325,#252326,
#252327,#252328,#252329,#252330,#252331,#252332,#252333,#252334,#252335,
#252336,#252337,#252338,#252339,#252340,#252341,#252342,#252343,#252344),
 .UNSPECIFIED.,.F.,.F.)
B_SPLINE_CURVE_WITH_KNOTS((6,1,1,1,1,1,1,1,1,1,1,1,1,1,1,1,1,1,1,1,1,1,
1,1,1,1,1,1,1,1,1,1,1,1,1,1,1,1,1,1,1,1,1,1,1,1,1,1,1,1,1,1,1,1,1,1,1,1,
1,1,1,1,1,1,1,1,1,1,1,1,1,1,1,1,1,1,1,1,1,1,1,1,1,1,1,1,1,1,1,1,1,1,1,1,
1,1,1,1,1,1,1,1,1,1,1,1,1,1,1,1,1,1,1,1,1,1,1,1,1,1,1,1,1,1,1,1,1,1,1,1,
1,1,1,1,1,1,1,1,1,1,1,1,1,1,1,1,1,1,1,1,1,1,1,1,1,1,1,1,1,1,1,1,1,1,1,1,
1,1,1,1,1,1,1,1,1,1,1,1,1,1,1,1,1,1,1,1,1,1,1,1,1,1,1,1,1,1,1,1,1,1,6),
(-1.,-0.995000000000001,-0.990000000000001,-0.985000000000001,-0.980000000000001,
-0.975000000000001,-0.970000000000001,-0.965000000000001,-0.960000000000001,
-0.955000000000001,-0.950000000000001,-0.945000000000001,-0.940000000000001,
-0.935000000000001,-0.930000000000001,-0.925000000000001,-0.920000000000001,
-0.915000000000001,-0.910000000000001,-0.905000000000001,-0.900000000000001,
-0.895000000000001,-0.890000000000001,-0.885000000000001,-0.880000000000001,
-0.875000000000001,-0.870000000000001,-0.865000000000001,-0.860000000000001,
-0.855000000000001,-0.850000000000001,-0.845000000000001,-0.840000000000001,
-0.835000000000001,-0.830000000000001,-0.825000000000001,-0.820000000000001,
-0.815000000000001,-0.810000000000001,-0.805000000000001,-0.800000000000001,
-0.795000000000001,-0.790000000000001,-0.785000000000001,-0.780000000000001,
-0.775000000000001,-0.770000000000001,-0.765000000000001,-0.760000000000001,
-0.755000000000001,-0.750000000000001,-0.745000000000001,-0.740000000000001,
-0.735000000000001,-0.730000000000001,-0.725000000000001,-0.720000000000001,
-0.715000000000001,-0.710000000000001,-0.705000000000001,-0.700000000000001,
-0.695000000000001,-0.690000000000001,-0.685,-0.68,-0.675,-0.67,-0.665,
-0.66,-0.655,-0.65,-0.645,-0.64,-0.635,-0.63,-0.625,-0.62,-0.615,-0.61,
-0.605,-0.6,-0.595,-0.59,-0.585,-0.58,-0.575,-0.57,-0.565,-0.56,-0.555,
-0.55,-0.545,-0.54,-0.535,-0.53,-0.525,-0.52,-0.515,-0.51,-0.505,-0.5,-0.495,
-0.49,-0.485,-0.48,-0.475,-0.47,-0.465,-0.46,-0.455,-0.45,-0.445,-0.44,
-0.435,-0.43,-0.425,-0.42,-0.415,-0.41,-0.405,-0.4,-0.395,-0.39,-0.385,
-0.38,-0.375,-0.37,-0.365,-0.36,-0.355,-0.35,-0.345,-0.34,-0.335,-0.33,
-0.325,-0.32,-0.315,-0.31,-0.305,-0.3,-0.295,-0.29,-0.285,-0.28,-0.275,
-0.27,-0.265,-0.26,-0.255,-0.25,-0.245,-0.24,-0.235,-0.23,-0.225,-0.22,
-0.215,-0.21,-0.205,-0.2,-0.195,-0.19,-0.185,-0.18,-0.175,-0.17,-0.165,
-0.16,-0.155,-0.15,-0.145,-0.14,-0.135,-0.13,-0.125,-0.12,-0.115,-0.11,
-0.105,-0.1,-0.095,-0.09,-0.085,-0.08,-0.075,-0.07,-0.065,-0.06,-0.055,
-0.05,-0.045,-0.04,-0.035,-0.03,-0.025,-0.02,-0.015,-0.01,-0.005,0.),
 .UNSPECIFIED.)
CURVE()
GEOMETRIC_REPRESENTATION_ITEM()
RATIONAL_B_SPLINE_CURVE((1.,1.,1.,1.,1.,1.,1.,1.,1.,1.,1.,1.,1.,1.,1.,1.,
1.,1.,1.,1.,1.,1.,1.,1.,1.,1.,1.,1.,1.,1.,1.,1.,1.,1.,1.,1.,1.,1.,1.,1.,
1.,1.,1.,1.,1.,1.,1.,1.,1.,1.,1.,1.,1.,1.,1.,1.,1.,1.,1.,1.,1.,1.,1.,1.,
1.,1.,1.,1.,1.,1.,1.,1.,1.,1.,1.,1.,1.,1.,1.,1.,1.,1.,1.,1.,1.,1.,1.,1.,
1.,1.,1.,1.,1.,1.,1.,1.,1.,1.,1.,1.,1.,1.,1.,1.,1.,1.,1.,1.,1.,1.,1.,1.,
1.,1.,1.,1.,1.,1.,1.,1.,1.,1.,1.,1.,1.,1.,1.,1.,1.,1.,1.,1.,1.,1.,1.,1.,
1.,1.,1.,1.,1.,1.,1.,1.,1.,1.,1.,1.,1.,1.,1.,1.,1.,1.,1.,1.,1.,1.,1.,1.,
1.,1.,1.,1.,1.,1.,1.,1.,1.,1.,1.,1.,1.,1.,1.,1.,1.,1.,1.,1.,1.,1.,1.,1.,
1.,1.,1.,1.,1.,1.,1.,1.,1.,1.,1.,1.,1.,1.,1.,1.,1.,1.,1.,1.,1.))
REPRESENTATION_ITEM('')
);
#875=(
BOUNDED_CURVE()
B_SPLINE_CURVE(5,(#252763,#252764,#252765,#252766,#252767,#252768,#252769,
#252770,#252771,#252772,#252773,#252774,#252775,#252776,#252777,#252778,
#252779,#252780,#252781,#252782,#252783,#252784,#252785,#252786,#252787,
#252788,#252789,#252790,#252791,#252792,#252793,#252794,#252795,#252796,
#252797,#252798,#252799,#252800,#252801,#252802,#252803,#252804,#252805,
#252806,#252807,#252808,#252809,#252810,#252811,#252812,#252813,#252814,
#252815,#252816,#252817,#252818,#252819,#252820,#252821,#252822,#252823,
#252824,#252825,#252826,#252827,#252828,#252829,#252830,#252831,#252832,
#252833,#252834,#252835,#252836,#252837,#252838,#252839,#252840,#252841,
#252842,#252843,#252844,#252845,#252846,#252847,#252848,#252849,#252850,
#252851,#252852,#252853,#252854,#252855,#252856,#252857,#252858,#252859,
#252860,#252861,#252862,#252863,#252864,#252865,#252866,#252867,#252868,
#252869,#252870,#252871,#252872,#252873,#252874,#252875,#252876,#252877,
#252878,#252879,#252880,#252881,#252882,#252883,#252884,#252885,#252886,
#252887,#252888,#252889,#252890,#252891,#252892,#252893,#252894,#252895,
#252896,#252897,#252898,#252899,#252900,#252901,#252902,#252903,#252904,
#252905,#252906,#252907,#252908,#252909,#252910,#252911,#252912,#252913,
#252914,#252915,#252916,#252917,#252918,#252919,#252920,#252921,#252922,
#252923,#252924,#252925,#252926,#252927,#252928,#252929,#252930,#252931,
#252932,#252933,#252934,#252935,#252936,#252937,#252938,#252939,#252940,
#252941,#252942,#252943,#252944,#252945,#252946,#252947,#252948,#252949,
#252950,#252951,#252952,#252953,#252954,#252955,#252956,#252957,#252958,
#252959,#252960,#252961,#252962,#252963,#252964,#252965,#252966,#252967),
 .UNSPECIFIED.,.F.,.F.)
B_SPLINE_CURVE_WITH_KNOTS((6,1,1,1,1,1,1,1,1,1,1,1,1,1,1,1,1,1,1,1,1,1,
1,1,1,1,1,1,1,1,1,1,1,1,1,1,1,1,1,1,1,1,1,1,1,1,1,1,1,1,1,1,1,1,1,1,1,1,
1,1,1,1,1,1,1,1,1,1,1,1,1,1,1,1,1,1,1,1,1,1,1,1,1,1,1,1,1,1,1,1,1,1,1,1,
1,1,1,1,1,1,1,1,1,1,1,1,1,1,1,1,1,1,1,1,1,1,1,1,1,1,1,1,1,1,1,1,1,1,1,1,
1,1,1,1,1,1,1,1,1,1,1,1,1,1,1,1,1,1,1,1,1,1,1,1,1,1,1,1,1,1,1,1,1,1,1,1,
1,1,1,1,1,1,1,1,1,1,1,1,1,1,1,1,1,1,1,1,1,1,1,1,1,1,1,1,1,1,1,1,1,1,6),
(-1.,-0.995000000000001,-0.990000000000001,-0.985000000000001,-0.980000000000001,
-0.975000000000001,-0.970000000000001,-0.965000000000001,-0.960000000000001,
-0.955000000000001,-0.950000000000001,-0.945000000000001,-0.940000000000001,
-0.935000000000001,-0.930000000000001,-0.925000000000001,-0.920000000000001,
-0.915000000000001,-0.910000000000001,-0.905000000000001,-0.900000000000001,
-0.895000000000001,-0.890000000000001,-0.885000000000001,-0.880000000000001,
-0.875000000000001,-0.870000000000001,-0.865000000000001,-0.860000000000001,
-0.855000000000001,-0.850000000000001,-0.845000000000001,-0.840000000000001,
-0.835000000000001,-0.830000000000001,-0.825000000000001,-0.820000000000001,
-0.815000000000001,-0.810000000000001,-0.805000000000001,-0.800000000000001,
-0.795000000000001,-0.790000000000001,-0.785000000000001,-0.780000000000001,
-0.775000000000001,-0.770000000000001,-0.765000000000001,-0.760000000000001,
-0.755000000000001,-0.750000000000001,-0.745000000000001,-0.740000000000001,
-0.735000000000001,-0.730000000000001,-0.725000000000001,-0.720000000000001,
-0.715000000000001,-0.710000000000001,-0.705000000000001,-0.700000000000001,
-0.695000000000001,-0.690000000000001,-0.685,-0.68,-0.675,-0.67,-0.665,
-0.66,-0.655,-0.65,-0.645,-0.64,-0.635,-0.63,-0.625,-0.62,-0.615,-0.61,
-0.605,-0.6,-0.595,-0.59,-0.585,-0.58,-0.575,-0.57,-0.565,-0.56,-0.555,
-0.55,-0.545,-0.54,-0.535,-0.53,-0.525,-0.52,-0.515,-0.51,-0.505,-0.5,-0.495,
-0.49,-0.485,-0.48,-0.475,-0.47,-0.465,-0.46,-0.455,-0.45,-0.445,-0.44,
-0.435,-0.43,-0.425,-0.42,-0.415,-0.41,-0.405,-0.4,-0.395,-0.39,-0.385,
-0.38,-0.375,-0.37,-0.365,-0.36,-0.355,-0.35,-0.345,-0.34,-0.335,-0.33,
-0.325,-0.32,-0.315,-0.31,-0.305,-0.3,-0.295,-0.29,-0.285,-0.28,-0.275,
-0.27,-0.265,-0.26,-0.255,-0.25,-0.245,-0.24,-0.235,-0.23,-0.225,-0.22,
-0.215,-0.21,-0.205,-0.2,-0.195,-0.19,-0.185,-0.18,-0.175,-0.17,-0.165,
-0.16,-0.155,-0.15,-0.145,-0.14,-0.135,-0.13,-0.125,-0.12,-0.115,-0.11,
-0.105,-0.1,-0.095,-0.09,-0.085,-0.08,-0.075,-0.07,-0.065,-0.06,-0.055,
-0.05,-0.045,-0.04,-0.035,-0.03,-0.025,-0.02,-0.015,-0.01,-0.005,0.),
 .UNSPECIFIED.)
CURVE()
GEOMETRIC_REPRESENTATION_ITEM()
RATIONAL_B_SPLINE_CURVE((1.,1.,1.,1.,1.,1.,1.,1.,1.,1.,1.,1.,1.,1.,1.,1.,
1.,1.,1.,1.,1.,1.,1.,1.,1.,1.,1.,1.,1.,1.,1.,1.,1.,1.,1.,1.,1.,1.,1.,1.,
1.,1.,1.,1.,1.,1.,1.,1.,1.,1.,1.,1.,1.,1.,1.,1.,1.,1.,1.,1.,1.,1.,1.,1.,
1.,1.,1.,1.,1.,1.,1.,1.,1.,1.,1.,1.,1.,1.,1.,1.,1.,1.,1.,1.,1.,1.,1.,1.,
1.,1.,1.,1.,1.,1.,1.,1.,1.,1.,1.,1.,1.,1.,1.,1.,1.,1.,1.,1.,1.,1.,1.,1.,
1.,1.,1.,1.,1.,1.,1.,1.,1.,1.,1.,1.,1.,1.,1.,1.,1.,1.,1.,1.,1.,1.,1.,1.,
1.,1.,1.,1.,1.,1.,1.,1.,1.,1.,1.,1.,1.,1.,1.,1.,1.,1.,1.,1.,1.,1.,1.,1.,
1.,1.,1.,1.,1.,1.,1.,1.,1.,1.,1.,1.,1.,1.,1.,1.,1.,1.,1.,1.,1.,1.,1.,1.,
1.,1.,1.,1.,1.,1.,1.,1.,1.,1.,1.,1.,1.,1.,1.,1.,1.,1.,1.,1.,1.))
REPRESENTATION_ITEM('')
);
#876=(
BOUNDED_CURVE()
B_SPLINE_CURVE(5,(#252970,#252971,#252972,#252973,#252974,#252975,#252976,
#252977,#252978,#252979,#252980,#252981,#252982,#252983,#252984,#252985,
#252986,#252987,#252988,#252989,#252990,#252991,#252992,#252993,#252994,
#252995,#252996,#252997,#252998,#252999,#253000,#253001,#253002,#253003,
#253004,#253005,#253006,#253007,#253008,#253009,#253010,#253011,#253012,
#253013,#253014,#253015,#253016,#253017,#253018,#253019,#253020,#253021,
#253022,#253023,#253024,#253025,#253026,#253027,#253028,#253029,#253030,
#253031,#253032,#253033,#253034,#253035,#253036,#253037,#253038,#253039,
#253040,#253041,#253042,#253043,#253044,#253045,#253046,#253047,#253048,
#253049,#253050,#253051,#253052,#253053,#253054,#253055,#253056,#253057,
#253058,#253059,#253060,#253061,#253062,#253063,#253064,#253065,#253066,
#253067,#253068,#253069,#253070,#253071,#253072,#253073,#253074,#253075,
#253076,#253077,#253078,#253079,#253080,#253081,#253082,#253083,#253084,
#253085,#253086,#253087,#253088,#253089,#253090,#253091,#253092,#253093,
#253094,#253095,#253096,#253097,#253098,#253099,#253100,#253101,#253102,
#253103,#253104,#253105,#253106,#253107,#253108,#253109,#253110,#253111,
#253112,#253113,#253114,#253115,#253116,#253117,#253118,#253119,#253120,
#253121,#253122,#253123,#253124,#253125,#253126,#253127,#253128,#253129,
#253130,#253131,#253132,#253133,#253134,#253135,#253136,#253137,#253138,
#253139,#253140,#253141,#253142,#253143,#253144,#253145,#253146,#253147,
#253148,#253149,#253150,#253151,#253152,#253153,#253154,#253155,#253156,
#253157,#253158,#253159,#253160,#253161,#253162,#253163,#253164,#253165,
#253166,#253167,#253168,#253169,#253170,#253171,#253172,#253173,#253174),
 .UNSPECIFIED.,.F.,.F.)
B_SPLINE_CURVE_WITH_KNOTS((6,1,1,1,1,1,1,1,1,1,1,1,1,1,1,1,1,1,1,1,1,1,
1,1,1,1,1,1,1,1,1,1,1,1,1,1,1,1,1,1,1,1,1,1,1,1,1,1,1,1,1,1,1,1,1,1,1,1,
1,1,1,1,1,1,1,1,1,1,1,1,1,1,1,1,1,1,1,1,1,1,1,1,1,1,1,1,1,1,1,1,1,1,1,1,
1,1,1,1,1,1,1,1,1,1,1,1,1,1,1,1,1,1,1,1,1,1,1,1,1,1,1,1,1,1,1,1,1,1,1,1,
1,1,1,1,1,1,1,1,1,1,1,1,1,1,1,1,1,1,1,1,1,1,1,1,1,1,1,1,1,1,1,1,1,1,1,1,
1,1,1,1,1,1,1,1,1,1,1,1,1,1,1,1,1,1,1,1,1,1,1,1,1,1,1,1,1,1,1,1,1,1,6),
(0.,0.005,0.01,0.015,0.02,0.025,0.03,0.035,0.04,0.045,0.05,0.055,0.06,0.065,
0.07,0.075,0.08,0.085,0.09,0.095,0.1,0.105,0.11,0.115,0.12,0.125,0.13,0.135,
0.14,0.145,0.15,0.155,0.16,0.165,0.17,0.175,0.18,0.185,0.19,0.195,0.2,0.205,
0.21,0.215,0.22,0.225,0.23,0.235,0.24,0.245,0.25,0.255,0.26,0.265,0.27,
0.275,0.28,0.285,0.29,0.295,0.3,0.305,0.31,0.315,0.32,0.325,0.33,0.335,
0.34,0.345,0.35,0.355,0.36,0.365,0.37,0.375,0.38,0.385,0.39,0.395,0.4,0.405,
0.41,0.415,0.42,0.425,0.43,0.435,0.44,0.445,0.45,0.455,0.46,0.465,0.47,
0.475,0.48,0.485,0.49,0.495,0.5,0.505,0.51,0.515,0.52,0.525,0.53,0.535,
0.54,0.545,0.55,0.555,0.56,0.565,0.57,0.575,0.58,0.585,0.59,0.595,0.6,0.605,
0.61,0.615,0.62,0.625,0.63,0.635,0.64,0.645,0.65,0.655,0.66,0.665,0.67,
0.675,0.68,0.685,0.690000000000001,0.695000000000001,0.700000000000001,
0.705000000000001,0.710000000000001,0.715000000000001,0.720000000000001,
0.725000000000001,0.730000000000001,0.735000000000001,0.740000000000001,
0.745000000000001,0.750000000000001,0.755000000000001,0.760000000000001,
0.765000000000001,0.770000000000001,0.775000000000001,0.780000000000001,
0.785000000000001,0.790000000000001,0.795000000000001,0.800000000000001,
0.805000000000001,0.810000000000001,0.815000000000001,0.820000000000001,
0.825000000000001,0.830000000000001,0.835000000000001,0.840000000000001,
0.845000000000001,0.850000000000001,0.855000000000001,0.860000000000001,
0.865000000000001,0.870000000000001,0.875000000000001,0.880000000000001,
0.885000000000001,0.890000000000001,0.895000000000001,0.900000000000001,
0.905000000000001,0.910000000000001,0.915000000000001,0.920000000000001,
0.925000000000001,0.930000000000001,0.935000000000001,0.940000000000001,
0.945000000000001,0.950000000000001,0.955000000000001,0.960000000000001,
0.965000000000001,0.970000000000001,0.975000000000001,0.980000000000001,
0.985000000000001,0.990000000000001,0.995000000000001,1.),.UNSPECIFIED.)
CURVE()
GEOMETRIC_REPRESENTATION_ITEM()
RATIONAL_B_SPLINE_CURVE((1.,1.,1.,1.,1.,1.,1.,1.,1.,1.,1.,1.,1.,1.,1.,1.,
1.,1.,1.,1.,1.,1.,1.,1.,1.,1.,1.,1.,1.,1.,1.,1.,1.,1.,1.,1.,1.,1.,1.,1.,
1.,1.,1.,1.,1.,1.,1.,1.,1.,1.,1.,1.,1.,1.,1.,1.,1.,1.,1.,1.,1.,1.,1.,1.,
1.,1.,1.,1.,1.,1.,1.,1.,1.,1.,1.,1.,1.,1.,1.,1.,1.,1.,1.,1.,1.,1.,1.,1.,
1.,1.,1.,1.,1.,1.,1.,1.,1.,1.,1.,1.,1.,1.,1.,1.,1.,1.,1.,1.,1.,1.,1.,1.,
1.,1.,1.,1.,1.,1.,1.,1.,1.,1.,1.,1.,1.,1.,1.,1.,1.,1.,1.,1.,1.,1.,1.,1.,
1.,1.,1.,1.,1.,1.,1.,1.,1.,1.,1.,1.,1.,1.,1.,1.,1.,1.,1.,1.,1.,1.,1.,1.,
1.,1.,1.,1.,1.,1.,1.,1.,1.,1.,1.,1.,1.,1.,1.,1.,1.,1.,1.,1.,1.,1.,1.,1.,
1.,1.,1.,1.,1.,1.,1.,1.,1.,1.,1.,1.,1.,1.,1.,1.,1.,1.,1.,1.,1.))
REPRESENTATION_ITEM('')
);
#877=(
BOUNDED_CURVE()
B_SPLINE_CURVE(5,(#253586,#253587,#253588,#253589,#253590,#253591,#253592,
#253593,#253594,#253595,#253596,#253597,#253598,#253599,#253600,#253601,
#253602,#253603,#253604,#253605,#253606,#253607,#253608,#253609,#253610,
#253611,#253612,#253613,#253614,#253615,#253616,#253617,#253618,#253619,
#253620,#253621,#253622,#253623,#253624,#253625,#253626,#253627,#253628,
#253629,#253630,#253631,#253632,#253633,#253634,#253635,#253636,#253637,
#253638,#253639,#253640,#253641,#253642,#253643,#253644,#253645,#253646,
#253647,#253648,#253649,#253650,#253651,#253652,#253653,#253654,#253655,
#253656,#253657,#253658,#253659,#253660,#253661,#253662,#253663,#253664,
#253665,#253666,#253667,#253668,#253669,#253670,#253671,#253672,#253673,
#253674,#253675,#253676,#253677,#253678,#253679,#253680,#253681,#253682,
#253683,#253684,#253685,#253686,#253687,#253688,#253689,#253690,#253691,
#253692,#253693,#253694,#253695,#253696,#253697,#253698,#253699,#253700,
#253701,#253702,#253703,#253704,#253705,#253706,#253707,#253708,#253709,
#253710,#253711,#253712,#253713,#253714,#253715,#253716,#253717,#253718,
#253719,#253720,#253721,#253722,#253723,#253724,#253725,#253726,#253727,
#253728,#253729,#253730,#253731,#253732,#253733,#253734,#253735,#253736,
#253737,#253738,#253739,#253740,#253741,#253742,#253743,#253744,#253745,
#253746,#253747,#253748,#253749,#253750,#253751,#253752,#253753,#253754,
#253755,#253756,#253757,#253758,#253759,#253760,#253761,#253762,#253763,
#253764,#253765,#253766,#253767,#253768,#253769,#253770,#253771,#253772,
#253773,#253774,#253775,#253776,#253777,#253778,#253779,#253780,#253781,
#253782,#253783,#253784,#253785,#253786,#253787,#253788,#253789,#253790),
 .UNSPECIFIED.,.F.,.F.)
B_SPLINE_CURVE_WITH_KNOTS((6,1,1,1,1,1,1,1,1,1,1,1,1,1,1,1,1,1,1,1,1,1,
1,1,1,1,1,1,1,1,1,1,1,1,1,1,1,1,1,1,1,1,1,1,1,1,1,1,1,1,1,1,1,1,1,1,1,1,
1,1,1,1,1,1,1,1,1,1,1,1,1,1,1,1,1,1,1,1,1,1,1,1,1,1,1,1,1,1,1,1,1,1,1,1,
1,1,1,1,1,1,1,1,1,1,1,1,1,1,1,1,1,1,1,1,1,1,1,1,1,1,1,1,1,1,1,1,1,1,1,1,
1,1,1,1,1,1,1,1,1,1,1,1,1,1,1,1,1,1,1,1,1,1,1,1,1,1,1,1,1,1,1,1,1,1,1,1,
1,1,1,1,1,1,1,1,1,1,1,1,1,1,1,1,1,1,1,1,1,1,1,1,1,1,1,1,1,1,1,1,1,1,6),
(0.,0.005,0.01,0.015,0.02,0.025,0.03,0.035,0.04,0.045,0.05,0.055,0.06,0.065,
0.07,0.075,0.08,0.085,0.09,0.095,0.1,0.105,0.11,0.115,0.12,0.125,0.13,0.135,
0.14,0.145,0.15,0.155,0.16,0.165,0.17,0.175,0.18,0.185,0.19,0.195,0.2,0.205,
0.21,0.215,0.22,0.225,0.23,0.235,0.24,0.245,0.25,0.255,0.26,0.265,0.27,
0.275,0.28,0.285,0.29,0.295,0.3,0.305,0.31,0.315,0.32,0.325,0.33,0.335,
0.34,0.345,0.35,0.355,0.36,0.365,0.37,0.375,0.38,0.385,0.39,0.395,0.4,0.405,
0.41,0.415,0.42,0.425,0.43,0.435,0.44,0.445,0.45,0.455,0.46,0.465,0.47,
0.475,0.48,0.485,0.49,0.495,0.5,0.505,0.51,0.515,0.52,0.525,0.53,0.535,
0.54,0.545,0.55,0.555,0.56,0.565,0.57,0.575,0.58,0.585,0.59,0.595,0.6,0.605,
0.61,0.615,0.62,0.625,0.63,0.635,0.64,0.645,0.65,0.655,0.66,0.665,0.67,
0.675,0.68,0.685,0.690000000000001,0.695000000000001,0.700000000000001,
0.705000000000001,0.710000000000001,0.715000000000001,0.720000000000001,
0.725000000000001,0.730000000000001,0.735000000000001,0.740000000000001,
0.745000000000001,0.750000000000001,0.755000000000001,0.760000000000001,
0.765000000000001,0.770000000000001,0.775000000000001,0.780000000000001,
0.785000000000001,0.790000000000001,0.795000000000001,0.800000000000001,
0.805000000000001,0.810000000000001,0.815000000000001,0.820000000000001,
0.825000000000001,0.830000000000001,0.835000000000001,0.840000000000001,
0.845000000000001,0.850000000000001,0.855000000000001,0.860000000000001,
0.865000000000001,0.870000000000001,0.875000000000001,0.880000000000001,
0.885000000000001,0.890000000000001,0.895000000000001,0.900000000000001,
0.905000000000001,0.910000000000001,0.915000000000001,0.920000000000001,
0.925000000000001,0.930000000000001,0.935000000000001,0.940000000000001,
0.945000000000001,0.950000000000001,0.955000000000001,0.960000000000001,
0.965000000000001,0.970000000000001,0.975000000000001,0.980000000000001,
0.985000000000001,0.990000000000001,0.995000000000001,1.),.UNSPECIFIED.)
CURVE()
GEOMETRIC_REPRESENTATION_ITEM()
RATIONAL_B_SPLINE_CURVE((1.,1.,1.,1.,1.,1.,1.,1.,1.,1.,1.,1.,1.,1.,1.,1.,
1.,1.,1.,1.,1.,1.,1.,1.,1.,1.,1.,1.,1.,1.,1.,1.,1.,1.,1.,1.,1.,1.,1.,1.,
1.,1.,1.,1.,1.,1.,1.,1.,1.,1.,1.,1.,1.,1.,1.,1.,1.,1.,1.,1.,1.,1.,1.,1.,
1.,1.,1.,1.,1.,1.,1.,1.,1.,1.,1.,1.,1.,1.,1.,1.,1.,1.,1.,1.,1.,1.,1.,1.,
1.,1.,1.,1.,1.,1.,1.,1.,1.,1.,1.,1.,1.,1.,1.,1.,1.,1.,1.,1.,1.,1.,1.,1.,
1.,1.,1.,1.,1.,1.,1.,1.,1.,1.,1.,1.,1.,1.,1.,1.,1.,1.,1.,1.,1.,1.,1.,1.,
1.,1.,1.,1.,1.,1.,1.,1.,1.,1.,1.,1.,1.,1.,1.,1.,1.,1.,1.,1.,1.,1.,1.,1.,
1.,1.,1.,1.,1.,1.,1.,1.,1.,1.,1.,1.,1.,1.,1.,1.,1.,1.,1.,1.,1.,1.,1.,1.,
1.,1.,1.,1.,1.,1.,1.,1.,1.,1.,1.,1.,1.,1.,1.,1.,1.,1.,1.,1.,1.))
REPRESENTATION_ITEM('')
);
#878=(
BOUNDED_CURVE()
B_SPLINE_CURVE(5,(#253792,#253793,#253794,#253795,#253796,#253797,#253798,
#253799,#253800,#253801,#253802,#253803,#253804,#253805,#253806,#253807,
#253808,#253809,#253810,#253811,#253812,#253813,#253814,#253815,#253816,
#253817,#253818,#253819,#253820,#253821,#253822,#253823,#253824,#253825,
#253826,#253827,#253828,#253829,#253830,#253831,#253832,#253833,#253834,
#253835,#253836,#253837,#253838,#253839,#253840,#253841,#253842,#253843,
#253844,#253845,#253846,#253847,#253848,#253849,#253850,#253851,#253852,
#253853,#253854,#253855,#253856,#253857,#253858,#253859,#253860,#253861,
#253862,#253863,#253864,#253865,#253866,#253867,#253868,#253869,#253870,
#253871,#253872,#253873,#253874,#253875,#253876,#253877,#253878,#253879,
#253880,#253881,#253882,#253883,#253884,#253885,#253886,#253887,#253888,
#253889,#253890,#253891,#253892,#253893,#253894,#253895,#253896,#253897,
#253898,#253899,#253900,#253901,#253902,#253903,#253904,#253905,#253906,
#253907,#253908,#253909,#253910,#253911,#253912,#253913,#253914,#253915,
#253916,#253917,#253918,#253919,#253920,#253921,#253922,#253923,#253924,
#253925,#253926,#253927,#253928,#253929,#253930,#253931,#253932,#253933,
#253934,#253935,#253936,#253937,#253938,#253939,#253940,#253941,#253942,
#253943,#253944,#253945,#253946,#253947,#253948,#253949,#253950,#253951,
#253952,#253953,#253954,#253955,#253956,#253957,#253958,#253959,#253960,
#253961,#253962,#253963,#253964,#253965,#253966,#253967,#253968,#253969,
#253970,#253971,#253972,#253973,#253974,#253975,#253976,#253977,#253978,
#253979,#253980,#253981,#253982,#253983,#253984,#253985,#253986,#253987,
#253988,#253989,#253990,#253991,#253992,#253993,#253994,#253995,#253996),
 .UNSPECIFIED.,.F.,.F.)
B_SPLINE_CURVE_WITH_KNOTS((6,1,1,1,1,1,1,1,1,1,1,1,1,1,1,1,1,1,1,1,1,1,
1,1,1,1,1,1,1,1,1,1,1,1,1,1,1,1,1,1,1,1,1,1,1,1,1,1,1,1,1,1,1,1,1,1,1,1,
1,1,1,1,1,1,1,1,1,1,1,1,1,1,1,1,1,1,1,1,1,1,1,1,1,1,1,1,1,1,1,1,1,1,1,1,
1,1,1,1,1,1,1,1,1,1,1,1,1,1,1,1,1,1,1,1,1,1,1,1,1,1,1,1,1,1,1,1,1,1,1,1,
1,1,1,1,1,1,1,1,1,1,1,1,1,1,1,1,1,1,1,1,1,1,1,1,1,1,1,1,1,1,1,1,1,1,1,1,
1,1,1,1,1,1,1,1,1,1,1,1,1,1,1,1,1,1,1,1,1,1,1,1,1,1,1,1,1,1,1,1,1,1,6),
(-1.,-0.995000000000001,-0.990000000000001,-0.985000000000001,-0.980000000000001,
-0.975000000000001,-0.970000000000001,-0.965000000000001,-0.960000000000001,
-0.955000000000001,-0.950000000000001,-0.945000000000001,-0.940000000000001,
-0.935000000000001,-0.930000000000001,-0.925000000000001,-0.920000000000001,
-0.915000000000001,-0.910000000000001,-0.905000000000001,-0.900000000000001,
-0.895000000000001,-0.890000000000001,-0.885000000000001,-0.880000000000001,
-0.875000000000001,-0.870000000000001,-0.865000000000001,-0.860000000000001,
-0.855000000000001,-0.850000000000001,-0.845000000000001,-0.840000000000001,
-0.835000000000001,-0.830000000000001,-0.825000000000001,-0.820000000000001,
-0.815000000000001,-0.810000000000001,-0.805000000000001,-0.800000000000001,
-0.795000000000001,-0.790000000000001,-0.785000000000001,-0.780000000000001,
-0.775000000000001,-0.770000000000001,-0.765000000000001,-0.760000000000001,
-0.755000000000001,-0.750000000000001,-0.745000000000001,-0.740000000000001,
-0.735000000000001,-0.730000000000001,-0.725000000000001,-0.720000000000001,
-0.715000000000001,-0.710000000000001,-0.705000000000001,-0.700000000000001,
-0.695000000000001,-0.690000000000001,-0.685,-0.68,-0.675,-0.67,-0.665,
-0.66,-0.655,-0.65,-0.645,-0.64,-0.635,-0.63,-0.625,-0.62,-0.615,-0.61,
-0.605,-0.6,-0.595,-0.59,-0.585,-0.58,-0.575,-0.57,-0.565,-0.56,-0.555,
-0.55,-0.545,-0.54,-0.535,-0.53,-0.525,-0.52,-0.515,-0.51,-0.505,-0.5,-0.495,
-0.49,-0.485,-0.48,-0.475,-0.47,-0.465,-0.46,-0.455,-0.45,-0.445,-0.44,
-0.435,-0.43,-0.425,-0.42,-0.415,-0.41,-0.405,-0.4,-0.395,-0.39,-0.385,
-0.38,-0.375,-0.37,-0.365,-0.36,-0.355,-0.35,-0.345,-0.34,-0.335,-0.33,
-0.325,-0.32,-0.315,-0.31,-0.305,-0.3,-0.295,-0.29,-0.285,-0.28,-0.275,
-0.27,-0.265,-0.26,-0.255,-0.25,-0.245,-0.24,-0.235,-0.23,-0.225,-0.22,
-0.215,-0.21,-0.205,-0.2,-0.195,-0.19,-0.185,-0.18,-0.175,-0.17,-0.165,
-0.16,-0.155,-0.15,-0.145,-0.14,-0.135,-0.13,-0.125,-0.12,-0.115,-0.11,
-0.105,-0.1,-0.095,-0.09,-0.085,-0.08,-0.075,-0.07,-0.065,-0.06,-0.055,
-0.05,-0.045,-0.04,-0.035,-0.03,-0.025,-0.02,-0.015,-0.01,-0.005,0.),
 .UNSPECIFIED.)
CURVE()
GEOMETRIC_REPRESENTATION_ITEM()
RATIONAL_B_SPLINE_CURVE((1.,1.,1.,1.,1.,1.,1.,1.,1.,1.,1.,1.,1.,1.,1.,1.,
1.,1.,1.,1.,1.,1.,1.,1.,1.,1.,1.,1.,1.,1.,1.,1.,1.,1.,1.,1.,1.,1.,1.,1.,
1.,1.,1.,1.,1.,1.,1.,1.,1.,1.,1.,1.,1.,1.,1.,1.,1.,1.,1.,1.,1.,1.,1.,1.,
1.,1.,1.,1.,1.,1.,1.,1.,1.,1.,1.,1.,1.,1.,1.,1.,1.,1.,1.,1.,1.,1.,1.,1.,
1.,1.,1.,1.,1.,1.,1.,1.,1.,1.,1.,1.,1.,1.,1.,1.,1.,1.,1.,1.,1.,1.,1.,1.,
1.,1.,1.,1.,1.,1.,1.,1.,1.,1.,1.,1.,1.,1.,1.,1.,1.,1.,1.,1.,1.,1.,1.,1.,
1.,1.,1.,1.,1.,1.,1.,1.,1.,1.,1.,1.,1.,1.,1.,1.,1.,1.,1.,1.,1.,1.,1.,1.,
1.,1.,1.,1.,1.,1.,1.,1.,1.,1.,1.,1.,1.,1.,1.,1.,1.,1.,1.,1.,1.,1.,1.,1.,
1.,1.,1.,1.,1.,1.,1.,1.,1.,1.,1.,1.,1.,1.,1.,1.,1.,1.,1.,1.,1.))
REPRESENTATION_ITEM('')
);
#879=(
BOUNDED_CURVE()
B_SPLINE_CURVE(5,(#254024,#254025,#254026,#254027,#254028,#254029,#254030,
#254031,#254032,#254033,#254034,#254035,#254036,#254037,#254038,#254039,
#254040,#254041,#254042,#254043,#254044,#254045,#254046,#254047,#254048,
#254049,#254050,#254051,#254052,#254053,#254054,#254055,#254056,#254057,
#254058,#254059,#254060,#254061,#254062,#254063,#254064,#254065,#254066,
#254067,#254068,#254069,#254070,#254071,#254072,#254073,#254074,#254075,
#254076,#254077,#254078,#254079,#254080,#254081,#254082,#254083,#254084,
#254085,#254086,#254087,#254088,#254089,#254090,#254091,#254092,#254093,
#254094,#254095,#254096,#254097,#254098,#254099,#254100,#254101,#254102,
#254103,#254104,#254105,#254106,#254107,#254108,#254109,#254110,#254111,
#254112,#254113,#254114,#254115,#254116,#254117,#254118,#254119,#254120,
#254121,#254122,#254123,#254124,#254125,#254126,#254127,#254128,#254129,
#254130,#254131,#254132,#254133,#254134,#254135,#254136,#254137,#254138,
#254139,#254140,#254141,#254142,#254143,#254144,#254145,#254146,#254147,
#254148,#254149,#254150,#254151,#254152,#254153,#254154,#254155,#254156,
#254157,#254158,#254159,#254160,#254161,#254162,#254163,#254164,#254165,
#254166,#254167,#254168,#254169,#254170,#254171,#254172,#254173,#254174,
#254175,#254176,#254177,#254178,#254179,#254180,#254181,#254182,#254183,
#254184,#254185,#254186,#254187,#254188,#254189,#254190,#254191,#254192,
#254193,#254194,#254195,#254196,#254197,#254198,#254199,#254200,#254201,
#254202,#254203,#254204,#254205,#254206,#254207,#254208,#254209,#254210,
#254211,#254212,#254213,#254214,#254215,#254216,#254217,#254218,#254219,
#254220,#254221,#254222,#254223,#254224,#254225,#254226,#254227,#254228),
 .UNSPECIFIED.,.F.,.F.)
B_SPLINE_CURVE_WITH_KNOTS((6,1,1,1,1,1,1,1,1,1,1,1,1,1,1,1,1,1,1,1,1,1,
1,1,1,1,1,1,1,1,1,1,1,1,1,1,1,1,1,1,1,1,1,1,1,1,1,1,1,1,1,1,1,1,1,1,1,1,
1,1,1,1,1,1,1,1,1,1,1,1,1,1,1,1,1,1,1,1,1,1,1,1,1,1,1,1,1,1,1,1,1,1,1,1,
1,1,1,1,1,1,1,1,1,1,1,1,1,1,1,1,1,1,1,1,1,1,1,1,1,1,1,1,1,1,1,1,1,1,1,1,
1,1,1,1,1,1,1,1,1,1,1,1,1,1,1,1,1,1,1,1,1,1,1,1,1,1,1,1,1,1,1,1,1,1,1,1,
1,1,1,1,1,1,1,1,1,1,1,1,1,1,1,1,1,1,1,1,1,1,1,1,1,1,1,1,1,1,1,1,1,1,6),
(-1.,-0.995000000000001,-0.990000000000001,-0.985000000000001,-0.980000000000001,
-0.975000000000001,-0.970000000000001,-0.965000000000001,-0.960000000000001,
-0.955000000000001,-0.950000000000001,-0.945000000000001,-0.940000000000001,
-0.935000000000001,-0.930000000000001,-0.925000000000001,-0.920000000000001,
-0.915000000000001,-0.910000000000001,-0.905000000000001,-0.900000000000001,
-0.895000000000001,-0.890000000000001,-0.885000000000001,-0.880000000000001,
-0.875000000000001,-0.870000000000001,-0.865000000000001,-0.860000000000001,
-0.855000000000001,-0.850000000000001,-0.845000000000001,-0.840000000000001,
-0.835000000000001,-0.830000000000001,-0.825000000000001,-0.820000000000001,
-0.815000000000001,-0.810000000000001,-0.805000000000001,-0.800000000000001,
-0.795000000000001,-0.790000000000001,-0.785000000000001,-0.780000000000001,
-0.775000000000001,-0.770000000000001,-0.765000000000001,-0.760000000000001,
-0.755000000000001,-0.750000000000001,-0.745000000000001,-0.740000000000001,
-0.735000000000001,-0.730000000000001,-0.725000000000001,-0.720000000000001,
-0.715000000000001,-0.710000000000001,-0.705000000000001,-0.700000000000001,
-0.695000000000001,-0.690000000000001,-0.685,-0.68,-0.675,-0.67,-0.665,
-0.66,-0.655,-0.65,-0.645,-0.64,-0.635,-0.63,-0.625,-0.62,-0.615,-0.61,
-0.605,-0.6,-0.595,-0.59,-0.585,-0.58,-0.575,-0.57,-0.565,-0.56,-0.555,
-0.55,-0.545,-0.54,-0.535,-0.53,-0.525,-0.52,-0.515,-0.51,-0.505,-0.5,-0.495,
-0.49,-0.485,-0.48,-0.475,-0.47,-0.465,-0.46,-0.455,-0.45,-0.445,-0.44,
-0.435,-0.43,-0.425,-0.42,-0.415,-0.41,-0.405,-0.4,-0.395,-0.39,-0.385,
-0.38,-0.375,-0.37,-0.365,-0.36,-0.355,-0.35,-0.345,-0.34,-0.335,-0.33,
-0.325,-0.32,-0.315,-0.31,-0.305,-0.3,-0.295,-0.29,-0.285,-0.28,-0.275,
-0.27,-0.265,-0.26,-0.255,-0.25,-0.245,-0.24,-0.235,-0.23,-0.225,-0.22,
-0.215,-0.21,-0.205,-0.2,-0.195,-0.19,-0.185,-0.18,-0.175,-0.17,-0.165,
-0.16,-0.155,-0.15,-0.145,-0.14,-0.135,-0.13,-0.125,-0.12,-0.115,-0.11,
-0.105,-0.1,-0.095,-0.09,-0.085,-0.08,-0.075,-0.07,-0.065,-0.06,-0.055,
-0.05,-0.045,-0.04,-0.035,-0.03,-0.025,-0.02,-0.015,-0.01,-0.005,0.),
 .UNSPECIFIED.)
CURVE()
GEOMETRIC_REPRESENTATION_ITEM()
RATIONAL_B_SPLINE_CURVE((1.,1.,1.,1.,1.,1.,1.,1.,1.,1.,1.,1.,1.,1.,1.,1.,
1.,1.,1.,1.,1.,1.,1.,1.,1.,1.,1.,1.,1.,1.,1.,1.,1.,1.,1.,1.,1.,1.,1.,1.,
1.,1.,1.,1.,1.,1.,1.,1.,1.,1.,1.,1.,1.,1.,1.,1.,1.,1.,1.,1.,1.,1.,1.,1.,
1.,1.,1.,1.,1.,1.,1.,1.,1.,1.,1.,1.,1.,1.,1.,1.,1.,1.,1.,1.,1.,1.,1.,1.,
1.,1.,1.,1.,1.,1.,1.,1.,1.,1.,1.,1.,1.,1.,1.,1.,1.,1.,1.,1.,1.,1.,1.,1.,
1.,1.,1.,1.,1.,1.,1.,1.,1.,1.,1.,1.,1.,1.,1.,1.,1.,1.,1.,1.,1.,1.,1.,1.,
1.,1.,1.,1.,1.,1.,1.,1.,1.,1.,1.,1.,1.,1.,1.,1.,1.,1.,1.,1.,1.,1.,1.,1.,
1.,1.,1.,1.,1.,1.,1.,1.,1.,1.,1.,1.,1.,1.,1.,1.,1.,1.,1.,1.,1.,1.,1.,1.,
1.,1.,1.,1.,1.,1.,1.,1.,1.,1.,1.,1.,1.,1.,1.,1.,1.,1.,1.,1.,1.))
REPRESENTATION_ITEM('')
);
#880=(
BOUNDED_CURVE()
B_SPLINE_CURVE(5,(#254240,#254241,#254242,#254243,#254244,#254245,#254246,
#254247,#254248,#254249,#254250,#254251,#254252,#254253,#254254,#254255,
#254256,#254257,#254258,#254259,#254260,#254261,#254262,#254263,#254264,
#254265,#254266,#254267,#254268,#254269,#254270,#254271,#254272,#254273,
#254274,#254275,#254276,#254277,#254278,#254279,#254280,#254281,#254282,
#254283,#254284,#254285,#254286,#254287,#254288,#254289,#254290,#254291,
#254292,#254293,#254294,#254295,#254296,#254297,#254298,#254299,#254300,
#254301,#254302,#254303,#254304,#254305,#254306,#254307,#254308,#254309,
#254310,#254311,#254312,#254313,#254314,#254315,#254316,#254317,#254318,
#254319,#254320,#254321,#254322,#254323,#254324,#254325,#254326,#254327,
#254328,#254329,#254330,#254331,#254332,#254333,#254334,#254335,#254336,
#254337,#254338,#254339,#254340,#254341,#254342,#254343,#254344,#254345,
#254346,#254347,#254348,#254349,#254350,#254351,#254352,#254353,#254354,
#254355,#254356,#254357,#254358,#254359,#254360,#254361,#254362,#254363,
#254364,#254365,#254366,#254367,#254368,#254369,#254370,#254371,#254372,
#254373,#254374,#254375,#254376,#254377,#254378,#254379,#254380,#254381,
#254382,#254383,#254384,#254385,#254386,#254387,#254388,#254389,#254390,
#254391,#254392,#254393,#254394,#254395,#254396,#254397,#254398,#254399,
#254400,#254401,#254402,#254403,#254404,#254405,#254406,#254407,#254408,
#254409,#254410,#254411,#254412,#254413,#254414,#254415,#254416,#254417,
#254418,#254419,#254420,#254421,#254422,#254423,#254424,#254425,#254426,
#254427,#254428,#254429,#254430,#254431,#254432,#254433,#254434,#254435,
#254436,#254437,#254438,#254439,#254440,#254441,#254442,#254443,#254444),
 .UNSPECIFIED.,.F.,.F.)
B_SPLINE_CURVE_WITH_KNOTS((6,1,1,1,1,1,1,1,1,1,1,1,1,1,1,1,1,1,1,1,1,1,
1,1,1,1,1,1,1,1,1,1,1,1,1,1,1,1,1,1,1,1,1,1,1,1,1,1,1,1,1,1,1,1,1,1,1,1,
1,1,1,1,1,1,1,1,1,1,1,1,1,1,1,1,1,1,1,1,1,1,1,1,1,1,1,1,1,1,1,1,1,1,1,1,
1,1,1,1,1,1,1,1,1,1,1,1,1,1,1,1,1,1,1,1,1,1,1,1,1,1,1,1,1,1,1,1,1,1,1,1,
1,1,1,1,1,1,1,1,1,1,1,1,1,1,1,1,1,1,1,1,1,1,1,1,1,1,1,1,1,1,1,1,1,1,1,1,
1,1,1,1,1,1,1,1,1,1,1,1,1,1,1,1,1,1,1,1,1,1,1,1,1,1,1,1,1,1,1,1,1,1,6),
(0.,0.005,0.01,0.015,0.02,0.025,0.03,0.035,0.04,0.045,0.05,0.055,0.06,0.065,
0.07,0.075,0.08,0.085,0.09,0.095,0.1,0.105,0.11,0.115,0.12,0.125,0.13,0.135,
0.14,0.145,0.15,0.155,0.16,0.165,0.17,0.175,0.18,0.185,0.19,0.195,0.2,0.205,
0.21,0.215,0.22,0.225,0.23,0.235,0.24,0.245,0.25,0.255,0.26,0.265,0.27,
0.275,0.28,0.285,0.29,0.295,0.3,0.305,0.31,0.315,0.32,0.325,0.33,0.335,
0.34,0.345,0.35,0.355,0.36,0.365,0.37,0.375,0.38,0.385,0.39,0.395,0.4,0.405,
0.41,0.415,0.42,0.425,0.43,0.435,0.44,0.445,0.45,0.455,0.46,0.465,0.47,
0.475,0.48,0.485,0.49,0.495,0.5,0.505,0.51,0.515,0.52,0.525,0.53,0.535,
0.54,0.545,0.55,0.555,0.56,0.565,0.57,0.575,0.58,0.585,0.59,0.595,0.6,0.605,
0.61,0.615,0.62,0.625,0.63,0.635,0.64,0.645,0.65,0.655,0.66,0.665,0.67,
0.675,0.68,0.685,0.690000000000001,0.695000000000001,0.700000000000001,
0.705000000000001,0.710000000000001,0.715000000000001,0.720000000000001,
0.725000000000001,0.730000000000001,0.735000000000001,0.740000000000001,
0.745000000000001,0.750000000000001,0.755000000000001,0.760000000000001,
0.765000000000001,0.770000000000001,0.775000000000001,0.780000000000001,
0.785000000000001,0.790000000000001,0.795000000000001,0.800000000000001,
0.805000000000001,0.810000000000001,0.815000000000001,0.820000000000001,
0.825000000000001,0.830000000000001,0.835000000000001,0.840000000000001,
0.845000000000001,0.850000000000001,0.855000000000001,0.860000000000001,
0.865000000000001,0.870000000000001,0.875000000000001,0.880000000000001,
0.885000000000001,0.890000000000001,0.895000000000001,0.900000000000001,
0.905000000000001,0.910000000000001,0.915000000000001,0.920000000000001,
0.925000000000001,0.930000000000001,0.935000000000001,0.940000000000001,
0.945000000000001,0.950000000000001,0.955000000000001,0.960000000000001,
0.965000000000001,0.970000000000001,0.975000000000001,0.980000000000001,
0.985000000000001,0.990000000000001,0.995000000000001,1.),.UNSPECIFIED.)
CURVE()
GEOMETRIC_REPRESENTATION_ITEM()
RATIONAL_B_SPLINE_CURVE((1.,1.,1.,1.,1.,1.,1.,1.,1.,1.,1.,1.,1.,1.,1.,1.,
1.,1.,1.,1.,1.,1.,1.,1.,1.,1.,1.,1.,1.,1.,1.,1.,1.,1.,1.,1.,1.,1.,1.,1.,
1.,1.,1.,1.,1.,1.,1.,1.,1.,1.,1.,1.,1.,1.,1.,1.,1.,1.,1.,1.,1.,1.,1.,1.,
1.,1.,1.,1.,1.,1.,1.,1.,1.,1.,1.,1.,1.,1.,1.,1.,1.,1.,1.,1.,1.,1.,1.,1.,
1.,1.,1.,1.,1.,1.,1.,1.,1.,1.,1.,1.,1.,1.,1.,1.,1.,1.,1.,1.,1.,1.,1.,1.,
1.,1.,1.,1.,1.,1.,1.,1.,1.,1.,1.,1.,1.,1.,1.,1.,1.,1.,1.,1.,1.,1.,1.,1.,
1.,1.,1.,1.,1.,1.,1.,1.,1.,1.,1.,1.,1.,1.,1.,1.,1.,1.,1.,1.,1.,1.,1.,1.,
1.,1.,1.,1.,1.,1.,1.,1.,1.,1.,1.,1.,1.,1.,1.,1.,1.,1.,1.,1.,1.,1.,1.,1.,
1.,1.,1.,1.,1.,1.,1.,1.,1.,1.,1.,1.,1.,1.,1.,1.,1.,1.,1.,1.,1.))
REPRESENTATION_ITEM('')
);
#881=(
BOUNDED_CURVE()
B_SPLINE_CURVE(5,(#254452,#254453,#254454,#254455,#254456,#254457,#254458,
#254459,#254460,#254461,#254462,#254463,#254464,#254465,#254466,#254467,
#254468,#254469,#254470,#254471,#254472,#254473,#254474,#254475,#254476,
#254477,#254478,#254479,#254480,#254481,#254482,#254483,#254484,#254485,
#254486,#254487,#254488,#254489,#254490,#254491,#254492,#254493,#254494,
#254495,#254496,#254497,#254498,#254499,#254500,#254501,#254502,#254503,
#254504,#254505,#254506,#254507,#254508,#254509,#254510,#254511,#254512,
#254513,#254514,#254515,#254516,#254517,#254518,#254519,#254520,#254521,
#254522,#254523,#254524,#254525,#254526,#254527,#254528,#254529,#254530,
#254531,#254532,#254533,#254534,#254535,#254536,#254537,#254538,#254539,
#254540,#254541,#254542,#254543,#254544,#254545,#254546,#254547,#254548,
#254549,#254550,#254551,#254552,#254553,#254554,#254555,#254556,#254557,
#254558,#254559,#254560,#254561,#254562,#254563,#254564,#254565,#254566,
#254567,#254568,#254569,#254570,#254571,#254572,#254573,#254574,#254575,
#254576,#254577,#254578,#254579,#254580,#254581,#254582,#254583,#254584,
#254585,#254586,#254587,#254588,#254589,#254590,#254591,#254592,#254593,
#254594,#254595,#254596,#254597,#254598,#254599,#254600,#254601,#254602,
#254603,#254604,#254605,#254606,#254607,#254608,#254609,#254610,#254611,
#254612,#254613,#254614,#254615,#254616,#254617,#254618,#254619,#254620,
#254621,#254622,#254623,#254624,#254625,#254626,#254627,#254628,#254629,
#254630,#254631,#254632,#254633,#254634,#254635,#254636,#254637,#254638,
#254639,#254640,#254641,#254642,#254643,#254644,#254645,#254646,#254647,
#254648,#254649,#254650,#254651,#254652,#254653,#254654,#254655,#254656),
 .UNSPECIFIED.,.F.,.F.)
B_SPLINE_CURVE_WITH_KNOTS((6,1,1,1,1,1,1,1,1,1,1,1,1,1,1,1,1,1,1,1,1,1,
1,1,1,1,1,1,1,1,1,1,1,1,1,1,1,1,1,1,1,1,1,1,1,1,1,1,1,1,1,1,1,1,1,1,1,1,
1,1,1,1,1,1,1,1,1,1,1,1,1,1,1,1,1,1,1,1,1,1,1,1,1,1,1,1,1,1,1,1,1,1,1,1,
1,1,1,1,1,1,1,1,1,1,1,1,1,1,1,1,1,1,1,1,1,1,1,1,1,1,1,1,1,1,1,1,1,1,1,1,
1,1,1,1,1,1,1,1,1,1,1,1,1,1,1,1,1,1,1,1,1,1,1,1,1,1,1,1,1,1,1,1,1,1,1,1,
1,1,1,1,1,1,1,1,1,1,1,1,1,1,1,1,1,1,1,1,1,1,1,1,1,1,1,1,1,1,1,1,1,1,6),
(-1.,-0.995000000000001,-0.990000000000001,-0.985000000000001,-0.980000000000001,
-0.975000000000001,-0.970000000000001,-0.965000000000001,-0.960000000000001,
-0.955000000000001,-0.950000000000001,-0.945000000000001,-0.940000000000001,
-0.935000000000001,-0.930000000000001,-0.925000000000001,-0.920000000000001,
-0.915000000000001,-0.910000000000001,-0.905000000000001,-0.900000000000001,
-0.895000000000001,-0.890000000000001,-0.885000000000001,-0.880000000000001,
-0.875000000000001,-0.870000000000001,-0.865000000000001,-0.860000000000001,
-0.855000000000001,-0.850000000000001,-0.845000000000001,-0.840000000000001,
-0.835000000000001,-0.830000000000001,-0.825000000000001,-0.820000000000001,
-0.815000000000001,-0.810000000000001,-0.805000000000001,-0.800000000000001,
-0.795000000000001,-0.790000000000001,-0.785000000000001,-0.780000000000001,
-0.775000000000001,-0.770000000000001,-0.765000000000001,-0.760000000000001,
-0.755000000000001,-0.750000000000001,-0.745000000000001,-0.740000000000001,
-0.735000000000001,-0.730000000000001,-0.725000000000001,-0.720000000000001,
-0.715000000000001,-0.710000000000001,-0.705000000000001,-0.700000000000001,
-0.695000000000001,-0.690000000000001,-0.685,-0.68,-0.675,-0.67,-0.665,
-0.66,-0.655,-0.65,-0.645,-0.64,-0.635,-0.63,-0.625,-0.62,-0.615,-0.61,
-0.605,-0.6,-0.595,-0.59,-0.585,-0.58,-0.575,-0.57,-0.565,-0.56,-0.555,
-0.55,-0.545,-0.54,-0.535,-0.53,-0.525,-0.52,-0.515,-0.51,-0.505,-0.5,-0.495,
-0.49,-0.485,-0.48,-0.475,-0.47,-0.465,-0.46,-0.455,-0.45,-0.445,-0.44,
-0.435,-0.43,-0.425,-0.42,-0.415,-0.41,-0.405,-0.4,-0.395,-0.39,-0.385,
-0.38,-0.375,-0.37,-0.365,-0.36,-0.355,-0.35,-0.345,-0.34,-0.335,-0.33,
-0.325,-0.32,-0.315,-0.31,-0.305,-0.3,-0.295,-0.29,-0.285,-0.28,-0.275,
-0.27,-0.265,-0.26,-0.255,-0.25,-0.245,-0.24,-0.235,-0.23,-0.225,-0.22,
-0.215,-0.21,-0.205,-0.2,-0.195,-0.19,-0.185,-0.18,-0.175,-0.17,-0.165,
-0.16,-0.155,-0.15,-0.145,-0.14,-0.135,-0.13,-0.125,-0.12,-0.115,-0.11,
-0.105,-0.1,-0.095,-0.09,-0.085,-0.08,-0.075,-0.07,-0.065,-0.06,-0.055,
-0.05,-0.045,-0.04,-0.035,-0.03,-0.025,-0.02,-0.015,-0.01,-0.005,0.),
 .UNSPECIFIED.)
CURVE()
GEOMETRIC_REPRESENTATION_ITEM()
RATIONAL_B_SPLINE_CURVE((1.,1.,1.,1.,1.,1.,1.,1.,1.,1.,1.,1.,1.,1.,1.,1.,
1.,1.,1.,1.,1.,1.,1.,1.,1.,1.,1.,1.,1.,1.,1.,1.,1.,1.,1.,1.,1.,1.,1.,1.,
1.,1.,1.,1.,1.,1.,1.,1.,1.,1.,1.,1.,1.,1.,1.,1.,1.,1.,1.,1.,1.,1.,1.,1.,
1.,1.,1.,1.,1.,1.,1.,1.,1.,1.,1.,1.,1.,1.,1.,1.,1.,1.,1.,1.,1.,1.,1.,1.,
1.,1.,1.,1.,1.,1.,1.,1.,1.,1.,1.,1.,1.,1.,1.,1.,1.,1.,1.,1.,1.,1.,1.,1.,
1.,1.,1.,1.,1.,1.,1.,1.,1.,1.,1.,1.,1.,1.,1.,1.,1.,1.,1.,1.,1.,1.,1.,1.,
1.,1.,1.,1.,1.,1.,1.,1.,1.,1.,1.,1.,1.,1.,1.,1.,1.,1.,1.,1.,1.,1.,1.,1.,
1.,1.,1.,1.,1.,1.,1.,1.,1.,1.,1.,1.,1.,1.,1.,1.,1.,1.,1.,1.,1.,1.,1.,1.,
1.,1.,1.,1.,1.,1.,1.,1.,1.,1.,1.,1.,1.,1.,1.,1.,1.,1.,1.,1.,1.))
REPRESENTATION_ITEM('')
);
#882=(
BOUNDED_CURVE()
B_SPLINE_CURVE(5,(#254668,#254669,#254670,#254671,#254672,#254673,#254674,
#254675,#254676,#254677,#254678,#254679,#254680,#254681,#254682,#254683,
#254684,#254685,#254686,#254687,#254688,#254689,#254690,#254691,#254692,
#254693,#254694,#254695,#254696,#254697,#254698,#254699,#254700,#254701,
#254702,#254703,#254704,#254705,#254706,#254707,#254708,#254709,#254710,
#254711,#254712,#254713,#254714,#254715,#254716,#254717,#254718,#254719,
#254720,#254721,#254722,#254723,#254724,#254725,#254726,#254727,#254728,
#254729,#254730,#254731,#254732,#254733,#254734,#254735,#254736,#254737,
#254738,#254739,#254740,#254741,#254742,#254743,#254744,#254745,#254746,
#254747,#254748,#254749,#254750,#254751,#254752,#254753,#254754,#254755,
#254756,#254757,#254758,#254759,#254760,#254761,#254762,#254763,#254764,
#254765,#254766,#254767,#254768,#254769,#254770,#254771,#254772,#254773,
#254774,#254775,#254776,#254777,#254778,#254779,#254780,#254781,#254782,
#254783,#254784,#254785,#254786,#254787,#254788,#254789,#254790,#254791,
#254792,#254793,#254794,#254795,#254796,#254797,#254798,#254799,#254800,
#254801,#254802,#254803,#254804,#254805,#254806,#254807,#254808,#254809,
#254810,#254811,#254812,#254813,#254814,#254815,#254816,#254817,#254818,
#254819,#254820,#254821,#254822,#254823,#254824,#254825,#254826,#254827,
#254828,#254829,#254830,#254831,#254832,#254833,#254834,#254835,#254836,
#254837,#254838,#254839,#254840,#254841,#254842,#254843,#254844,#254845,
#254846,#254847,#254848,#254849,#254850,#254851,#254852,#254853,#254854,
#254855,#254856,#254857,#254858,#254859,#254860,#254861,#254862,#254863,
#254864,#254865,#254866,#254867,#254868,#254869,#254870,#254871,#254872),
 .UNSPECIFIED.,.F.,.F.)
B_SPLINE_CURVE_WITH_KNOTS((6,1,1,1,1,1,1,1,1,1,1,1,1,1,1,1,1,1,1,1,1,1,
1,1,1,1,1,1,1,1,1,1,1,1,1,1,1,1,1,1,1,1,1,1,1,1,1,1,1,1,1,1,1,1,1,1,1,1,
1,1,1,1,1,1,1,1,1,1,1,1,1,1,1,1,1,1,1,1,1,1,1,1,1,1,1,1,1,1,1,1,1,1,1,1,
1,1,1,1,1,1,1,1,1,1,1,1,1,1,1,1,1,1,1,1,1,1,1,1,1,1,1,1,1,1,1,1,1,1,1,1,
1,1,1,1,1,1,1,1,1,1,1,1,1,1,1,1,1,1,1,1,1,1,1,1,1,1,1,1,1,1,1,1,1,1,1,1,
1,1,1,1,1,1,1,1,1,1,1,1,1,1,1,1,1,1,1,1,1,1,1,1,1,1,1,1,1,1,1,1,1,1,6),
(0.,0.005,0.01,0.015,0.02,0.025,0.03,0.035,0.04,0.045,0.05,0.055,0.06,0.065,
0.07,0.075,0.08,0.085,0.09,0.095,0.1,0.105,0.11,0.115,0.12,0.125,0.13,0.135,
0.14,0.145,0.15,0.155,0.16,0.165,0.17,0.175,0.18,0.185,0.19,0.195,0.2,0.205,
0.21,0.215,0.22,0.225,0.23,0.235,0.24,0.245,0.25,0.255,0.26,0.265,0.27,
0.275,0.28,0.285,0.29,0.295,0.3,0.305,0.31,0.315,0.32,0.325,0.33,0.335,
0.34,0.345,0.35,0.355,0.36,0.365,0.37,0.375,0.38,0.385,0.39,0.395,0.4,0.405,
0.41,0.415,0.42,0.425,0.43,0.435,0.44,0.445,0.45,0.455,0.46,0.465,0.47,
0.475,0.48,0.485,0.49,0.495,0.5,0.505,0.51,0.515,0.52,0.525,0.53,0.535,
0.54,0.545,0.55,0.555,0.56,0.565,0.57,0.575,0.58,0.585,0.59,0.595,0.6,0.605,
0.61,0.615,0.62,0.625,0.63,0.635,0.64,0.645,0.65,0.655,0.66,0.665,0.67,
0.675,0.68,0.685,0.690000000000001,0.695000000000001,0.700000000000001,
0.705000000000001,0.710000000000001,0.715000000000001,0.720000000000001,
0.725000000000001,0.730000000000001,0.735000000000001,0.740000000000001,
0.745000000000001,0.750000000000001,0.755000000000001,0.760000000000001,
0.765000000000001,0.770000000000001,0.775000000000001,0.780000000000001,
0.785000000000001,0.790000000000001,0.795000000000001,0.800000000000001,
0.805000000000001,0.810000000000001,0.815000000000001,0.820000000000001,
0.825000000000001,0.830000000000001,0.835000000000001,0.840000000000001,
0.845000000000001,0.850000000000001,0.855000000000001,0.860000000000001,
0.865000000000001,0.870000000000001,0.875000000000001,0.880000000000001,
0.885000000000001,0.890000000000001,0.895000000000001,0.900000000000001,
0.905000000000001,0.910000000000001,0.915000000000001,0.920000000000001,
0.925000000000001,0.930000000000001,0.935000000000001,0.940000000000001,
0.945000000000001,0.950000000000001,0.955000000000001,0.960000000000001,
0.965000000000001,0.970000000000001,0.975000000000001,0.980000000000001,
0.985000000000001,0.990000000000001,0.995000000000001,1.),.UNSPECIFIED.)
CURVE()
GEOMETRIC_REPRESENTATION_ITEM()
RATIONAL_B_SPLINE_CURVE((1.,1.,1.,1.,1.,1.,1.,1.,1.,1.,1.,1.,1.,1.,1.,1.,
1.,1.,1.,1.,1.,1.,1.,1.,1.,1.,1.,1.,1.,1.,1.,1.,1.,1.,1.,1.,1.,1.,1.,1.,
1.,1.,1.,1.,1.,1.,1.,1.,1.,1.,1.,1.,1.,1.,1.,1.,1.,1.,1.,1.,1.,1.,1.,1.,
1.,1.,1.,1.,1.,1.,1.,1.,1.,1.,1.,1.,1.,1.,1.,1.,1.,1.,1.,1.,1.,1.,1.,1.,
1.,1.,1.,1.,1.,1.,1.,1.,1.,1.,1.,1.,1.,1.,1.,1.,1.,1.,1.,1.,1.,1.,1.,1.,
1.,1.,1.,1.,1.,1.,1.,1.,1.,1.,1.,1.,1.,1.,1.,1.,1.,1.,1.,1.,1.,1.,1.,1.,
1.,1.,1.,1.,1.,1.,1.,1.,1.,1.,1.,1.,1.,1.,1.,1.,1.,1.,1.,1.,1.,1.,1.,1.,
1.,1.,1.,1.,1.,1.,1.,1.,1.,1.,1.,1.,1.,1.,1.,1.,1.,1.,1.,1.,1.,1.,1.,1.,
1.,1.,1.,1.,1.,1.,1.,1.,1.,1.,1.,1.,1.,1.,1.,1.,1.,1.,1.,1.,1.))
REPRESENTATION_ITEM('')
);
#883=(
BOUNDED_SURFACE()
B_SPLINE_SURFACE(5,1,((#52622,#52623),(#52624,#52625),(#52626,#52627),(#52628,
#52629),(#52630,#52631),(#52632,#52633),(#52634,#52635),(#52636,#52637),
(#52638,#52639),(#52640,#52641),(#52642,#52643),(#52644,#52645),(#52646,
#52647),(#52648,#52649),(#52650,#52651),(#52652,#52653),(#52654,#52655),
(#52656,#52657),(#52658,#52659),(#52660,#52661),(#52662,#52663),(#52664,
#52665),(#52666,#52667),(#52668,#52669),(#52670,#52671),(#52672,#52673),
(#52674,#52675),(#52676,#52677),(#52678,#52679),(#52680,#52681),(#52682,
#52683),(#52684,#52685),(#52686,#52687),(#52688,#52689),(#52690,#52691),
(#52692,#52693),(#52694,#52695),(#52696,#52697),(#52698,#52699),(#52700,
#52701),(#52702,#52703),(#52704,#52705),(#52706,#52707),(#52708,#52709),
(#52710,#52711),(#52712,#52713),(#52714,#52715),(#52716,#52717),(#52718,
#52719),(#52720,#52721),(#52722,#52723),(#52724,#52725),(#52726,#52727),
(#52728,#52729),(#52730,#52731),(#52732,#52733),(#52734,#52735),(#52736,
#52737),(#52738,#52739),(#52740,#52741),(#52742,#52743),(#52744,#52745),
(#52746,#52747),(#52748,#52749),(#52750,#52751),(#52752,#52753),(#52754,
#52755),(#52756,#52757),(#52758,#52759),(#52760,#52761),(#52762,#52763),
(#52764,#52765),(#52766,#52767),(#52768,#52769),(#52770,#52771),(#52772,
#52773),(#52774,#52775),(#52776,#52777),(#52778,#52779),(#52780,#52781),
(#52782,#52783),(#52784,#52785),(#52786,#52787),(#52788,#52789),(#52790,
#52791),(#52792,#52793),(#52794,#52795),(#52796,#52797),(#52798,#52799),
(#52800,#52801),(#52802,#52803),(#52804,#52805),(#52806,#52807),(#52808,
#52809),(#52810,#52811),(#52812,#52813),(#52814,#52815),(#52816,#52817),
(#52818,#52819),(#52820,#52821),(#52822,#52823),(#52824,#52825),(#52826,
#52827),(#52828,#52829),(#52830,#52831),(#52832,#52833),(#52834,#52835),
(#52836,#52837),(#52838,#52839),(#52840,#52841),(#52842,#52843),(#52844,
#52845),(#52846,#52847),(#52848,#52849),(#52850,#52851),(#52852,#52853),
(#52854,#52855),(#52856,#52857),(#52858,#52859),(#52860,#52861),(#52862,
#52863),(#52864,#52865),(#52866,#52867),(#52868,#52869),(#52870,#52871),
(#52872,#52873),(#52874,#52875),(#52876,#52877),(#52878,#52879),(#52880,
#52881),(#52882,#52883),(#52884,#52885),(#52886,#52887),(#52888,#52889),
(#52890,#52891),(#52892,#52893),(#52894,#52895),(#52896,#52897),(#52898,
#52899),(#52900,#52901),(#52902,#52903),(#52904,#52905),(#52906,#52907),
(#52908,#52909),(#52910,#52911),(#52912,#52913),(#52914,#52915),(#52916,
#52917),(#52918,#52919),(#52920,#52921),(#52922,#52923),(#52924,#52925),
(#52926,#52927),(#52928,#52929),(#52930,#52931),(#52932,#52933),(#52934,
#52935),(#52936,#52937),(#52938,#52939),(#52940,#52941),(#52942,#52943),
(#52944,#52945),(#52946,#52947),(#52948,#52949),(#52950,#52951),(#52952,
#52953),(#52954,#52955),(#52956,#52957),(#52958,#52959),(#52960,#52961),
(#52962,#52963),(#52964,#52965),(#52966,#52967),(#52968,#52969),(#52970,
#52971),(#52972,#52973),(#52974,#52975),(#52976,#52977),(#52978,#52979),
(#52980,#52981),(#52982,#52983),(#52984,#52985),(#52986,#52987),(#52988,
#52989),(#52990,#52991),(#52992,#52993),(#52994,#52995),(#52996,#52997),
(#52998,#52999),(#53000,#53001),(#53002,#53003),(#53004,#53005),(#53006,
#53007),(#53008,#53009),(#53010,#53011),(#53012,#53013),(#53014,#53015),
(#53016,#53017),(#53018,#53019),(#53020,#53021),(#53022,#53023),(#53024,
#53025),(#53026,#53027),(#53028,#53029),(#53030,#53031)),.UNSPECIFIED.,
 .F.,.F.,.F.)
B_SPLINE_SURFACE_WITH_KNOTS((6,1,1,1,1,1,1,1,1,1,1,1,1,1,1,1,1,1,1,1,1,
1,1,1,1,1,1,1,1,1,1,1,1,1,1,1,1,1,1,1,1,1,1,1,1,1,1,1,1,1,1,1,1,1,1,1,1,
1,1,1,1,1,1,1,1,1,1,1,1,1,1,1,1,1,1,1,1,1,1,1,1,1,1,1,1,1,1,1,1,1,1,1,1,
1,1,1,1,1,1,1,1,1,1,1,1,1,1,1,1,1,1,1,1,1,1,1,1,1,1,1,1,1,1,1,1,1,1,1,1,
1,1,1,1,1,1,1,1,1,1,1,1,1,1,1,1,1,1,1,1,1,1,1,1,1,1,1,1,1,1,1,1,1,1,1,1,
1,1,1,1,1,1,1,1,1,1,1,1,1,1,1,1,1,1,1,1,1,1,1,1,1,1,1,1,1,1,1,1,1,1,1,6),
(2,2),(0.,0.005,0.01,0.015,0.02,0.025,0.03,0.035,0.04,0.045,0.05,0.055,
0.06,0.065,0.07,0.075,0.08,0.085,0.09,0.095,0.1,0.105,0.11,0.115,0.12,0.125,
0.13,0.135,0.14,0.145,0.15,0.155,0.16,0.165,0.17,0.175,0.18,0.185,0.19,
0.195,0.2,0.205,0.21,0.215,0.22,0.225,0.23,0.235,0.24,0.245,0.25,0.255,
0.26,0.265,0.27,0.275,0.28,0.285,0.29,0.295,0.3,0.305,0.31,0.315,0.32,0.325,
0.33,0.335,0.34,0.345,0.35,0.355,0.36,0.365,0.37,0.375,0.38,0.385,0.39,
0.395,0.4,0.405,0.41,0.415,0.42,0.425,0.43,0.435,0.44,0.445,0.45,0.455,
0.46,0.465,0.47,0.475,0.48,0.485,0.49,0.495,0.5,0.505,0.51,0.515,0.52,0.525,
0.53,0.535,0.54,0.545,0.55,0.555,0.56,0.565,0.57,0.575,0.58,0.585,0.59,
0.595,0.6,0.605,0.61,0.615,0.62,0.625,0.63,0.635,0.64,0.645,0.65,0.655,
0.66,0.665,0.67,0.675,0.68,0.685,0.690000000000001,0.695000000000001,0.700000000000001,
0.705000000000001,0.710000000000001,0.715000000000001,0.720000000000001,
0.725000000000001,0.730000000000001,0.735000000000001,0.740000000000001,
0.745000000000001,0.750000000000001,0.755000000000001,0.760000000000001,
0.765000000000001,0.770000000000001,0.775000000000001,0.780000000000001,
0.785000000000001,0.790000000000001,0.795000000000001,0.800000000000001,
0.805000000000001,0.810000000000001,0.815000000000001,0.820000000000001,
0.825000000000001,0.830000000000001,0.835000000000001,0.840000000000001,
0.845000000000001,0.850000000000001,0.855000000000001,0.860000000000001,
0.865000000000001,0.870000000000001,0.875000000000001,0.880000000000001,
0.885000000000001,0.890000000000001,0.895000000000001,0.900000000000001,
0.905000000000001,0.910000000000001,0.915000000000001,0.920000000000001,
0.925000000000001,0.930000000000001,0.935000000000001,0.940000000000001,
0.945000000000001,0.950000000000001,0.955000000000001,0.960000000000001,
0.965000000000001,0.970000000000001,0.975000000000001,0.980000000000001,
0.985000000000001,0.990000000000001,0.995000000000001,1.),(0.,1.2),
 .UNSPECIFIED.)
GEOMETRIC_REPRESENTATION_ITEM()
RATIONAL_B_SPLINE_SURFACE(((1.,1.),(1.,1.),(1.,1.),(1.,1.),(1.,1.),(1.,
1.),(1.,1.),(1.,1.),(1.,1.),(1.,1.),(1.,1.),(1.,1.),(1.,1.),(1.,1.),(1.,
1.),(1.,1.),(1.,1.),(1.,1.),(1.,1.),(1.,1.),(1.,1.),(1.,1.),(1.,1.),(1.,
1.),(1.,1.),(1.,1.),(1.,1.),(1.,1.),(1.,1.),(1.,1.),(1.,1.),(1.,1.),(1.,
1.),(1.,1.),(1.,1.),(1.,1.),(1.,1.),(1.,1.),(1.,1.),(1.,1.),(1.,1.),(1.,
1.),(1.,1.),(1.,1.),(1.,1.),(1.,1.),(1.,1.),(1.,1.),(1.,1.),(1.,1.),(1.,
1.),(1.,1.),(1.,1.),(1.,1.),(1.,1.),(1.,1.),(1.,1.),(1.,1.),(1.,1.),(1.,
1.),(1.,1.),(1.,1.),(1.,1.),(1.,1.),(1.,1.),(1.,1.),(1.,1.),(1.,1.),(1.,
1.),(1.,1.),(1.,1.),(1.,1.),(1.,1.),(1.,1.),(1.,1.),(1.,1.),(1.,1.),(1.,
1.),(1.,1.),(1.,1.),(1.,1.),(1.,1.),(1.,1.),(1.,1.),(1.,1.),(1.,1.),(1.,
1.),(1.,1.),(1.,1.),(1.,1.),(1.,1.),(1.,1.),(1.,1.),(1.,1.),(1.,1.),(1.,
1.),(1.,1.),(1.,1.),(1.,1.),(1.,1.),(1.,1.),(1.,1.),(1.,1.),(1.,1.),(1.,
1.),(1.,1.),(1.,1.),(1.,1.),(1.,1.),(1.,1.),(1.,1.),(1.,1.),(1.,1.),(1.,
1.),(1.,1.),(1.,1.),(1.,1.),(1.,1.),(1.,1.),(1.,1.),(1.,1.),(1.,1.),(1.,
1.),(1.,1.),(1.,1.),(1.,1.),(1.,1.),(1.,1.),(1.,1.),(1.,1.),(1.,1.),(1.,
1.),(1.,1.),(1.,1.),(1.,1.),(1.,1.),(1.,1.),(1.,1.),(1.,1.),(1.,1.),(1.,
1.),(1.,1.),(1.,1.),(1.,1.),(1.,1.),(1.,1.),(1.,1.),(1.,1.),(1.,1.),(1.,
1.),(1.,1.),(1.,1.),(1.,1.),(1.,1.),(1.,1.),(1.,1.),(1.,1.),(1.,1.),(1.,
1.),(1.,1.),(1.,1.),(1.,1.),(1.,1.),(1.,1.),(1.,1.),(1.,1.),(1.,1.),(1.,
1.),(1.,1.),(1.,1.),(1.,1.),(1.,1.),(1.,1.),(1.,1.),(1.,1.),(1.,1.),(1.,
1.),(1.,1.),(1.,1.),(1.,1.),(1.,1.),(1.,1.),(1.,1.),(1.,1.),(1.,1.),(1.,
1.),(1.,1.),(1.,1.),(1.,1.),(1.,1.),(1.,1.),(1.,1.),(1.,1.),(1.,1.),(1.,
1.),(1.,1.),(1.,1.),(1.,1.),(1.,1.),(1.,1.),(1.,1.),(1.,1.),(1.,1.),(1.,
1.),(1.,1.)))
REPRESENTATION_ITEM('')
SURFACE()
);
#884=(
BOUNDED_SURFACE()
B_SPLINE_SURFACE(5,1,((#53518,#53519),(#53520,#53521),(#53522,#53523),(#53524,
#53525),(#53526,#53527),(#53528,#53529),(#53530,#53531),(#53532,#53533),
(#53534,#53535),(#53536,#53537),(#53538,#53539),(#53540,#53541),(#53542,
#53543),(#53544,#53545),(#53546,#53547),(#53548,#53549),(#53550,#53551),
(#53552,#53553),(#53554,#53555),(#53556,#53557),(#53558,#53559),(#53560,
#53561),(#53562,#53563),(#53564,#53565),(#53566,#53567),(#53568,#53569),
(#53570,#53571),(#53572,#53573),(#53574,#53575),(#53576,#53577),(#53578,
#53579),(#53580,#53581),(#53582,#53583),(#53584,#53585),(#53586,#53587),
(#53588,#53589),(#53590,#53591),(#53592,#53593),(#53594,#53595),(#53596,
#53597),(#53598,#53599),(#53600,#53601),(#53602,#53603),(#53604,#53605),
(#53606,#53607),(#53608,#53609),(#53610,#53611),(#53612,#53613),(#53614,
#53615),(#53616,#53617),(#53618,#53619),(#53620,#53621),(#53622,#53623),
(#53624,#53625),(#53626,#53627),(#53628,#53629),(#53630,#53631),(#53632,
#53633),(#53634,#53635),(#53636,#53637),(#53638,#53639),(#53640,#53641),
(#53642,#53643),(#53644,#53645),(#53646,#53647),(#53648,#53649),(#53650,
#53651),(#53652,#53653),(#53654,#53655),(#53656,#53657),(#53658,#53659),
(#53660,#53661),(#53662,#53663),(#53664,#53665),(#53666,#53667),(#53668,
#53669),(#53670,#53671),(#53672,#53673),(#53674,#53675),(#53676,#53677),
(#53678,#53679),(#53680,#53681),(#53682,#53683),(#53684,#53685),(#53686,
#53687),(#53688,#53689),(#53690,#53691),(#53692,#53693),(#53694,#53695),
(#53696,#53697),(#53698,#53699),(#53700,#53701),(#53702,#53703),(#53704,
#53705),(#53706,#53707),(#53708,#53709),(#53710,#53711),(#53712,#53713),
(#53714,#53715),(#53716,#53717),(#53718,#53719),(#53720,#53721),(#53722,
#53723),(#53724,#53725),(#53726,#53727),(#53728,#53729),(#53730,#53731),
(#53732,#53733),(#53734,#53735),(#53736,#53737),(#53738,#53739),(#53740,
#53741),(#53742,#53743),(#53744,#53745),(#53746,#53747),(#53748,#53749),
(#53750,#53751),(#53752,#53753),(#53754,#53755),(#53756,#53757),(#53758,
#53759),(#53760,#53761),(#53762,#53763),(#53764,#53765),(#53766,#53767),
(#53768,#53769),(#53770,#53771),(#53772,#53773),(#53774,#53775),(#53776,
#53777),(#53778,#53779),(#53780,#53781),(#53782,#53783),(#53784,#53785),
(#53786,#53787),(#53788,#53789),(#53790,#53791),(#53792,#53793),(#53794,
#53795),(#53796,#53797),(#53798,#53799),(#53800,#53801),(#53802,#53803),
(#53804,#53805),(#53806,#53807),(#53808,#53809),(#53810,#53811),(#53812,
#53813),(#53814,#53815),(#53816,#53817),(#53818,#53819),(#53820,#53821),
(#53822,#53823),(#53824,#53825),(#53826,#53827),(#53828,#53829),(#53830,
#53831),(#53832,#53833),(#53834,#53835),(#53836,#53837),(#53838,#53839),
(#53840,#53841),(#53842,#53843),(#53844,#53845),(#53846,#53847),(#53848,
#53849),(#53850,#53851),(#53852,#53853),(#53854,#53855),(#53856,#53857),
(#53858,#53859),(#53860,#53861),(#53862,#53863),(#53864,#53865),(#53866,
#53867),(#53868,#53869),(#53870,#53871),(#53872,#53873),(#53874,#53875),
(#53876,#53877),(#53878,#53879),(#53880,#53881),(#53882,#53883),(#53884,
#53885),(#53886,#53887),(#53888,#53889),(#53890,#53891),(#53892,#53893),
(#53894,#53895),(#53896,#53897),(#53898,#53899),(#53900,#53901),(#53902,
#53903),(#53904,#53905),(#53906,#53907),(#53908,#53909),(#53910,#53911),
(#53912,#53913),(#53914,#53915),(#53916,#53917),(#53918,#53919),(#53920,
#53921),(#53922,#53923),(#53924,#53925),(#53926,#53927)),.UNSPECIFIED.,
 .F.,.F.,.F.)
B_SPLINE_SURFACE_WITH_KNOTS((6,1,1,1,1,1,1,1,1,1,1,1,1,1,1,1,1,1,1,1,1,
1,1,1,1,1,1,1,1,1,1,1,1,1,1,1,1,1,1,1,1,1,1,1,1,1,1,1,1,1,1,1,1,1,1,1,1,
1,1,1,1,1,1,1,1,1,1,1,1,1,1,1,1,1,1,1,1,1,1,1,1,1,1,1,1,1,1,1,1,1,1,1,1,
1,1,1,1,1,1,1,1,1,1,1,1,1,1,1,1,1,1,1,1,1,1,1,1,1,1,1,1,1,1,1,1,1,1,1,1,
1,1,1,1,1,1,1,1,1,1,1,1,1,1,1,1,1,1,1,1,1,1,1,1,1,1,1,1,1,1,1,1,1,1,1,1,
1,1,1,1,1,1,1,1,1,1,1,1,1,1,1,1,1,1,1,1,1,1,1,1,1,1,1,1,1,1,1,1,1,1,1,6),
(2,2),(0.,0.005,0.01,0.015,0.02,0.025,0.03,0.035,0.04,0.045,0.05,0.055,
0.06,0.065,0.07,0.075,0.08,0.085,0.09,0.095,0.1,0.105,0.11,0.115,0.12,0.125,
0.13,0.135,0.14,0.145,0.15,0.155,0.16,0.165,0.17,0.175,0.18,0.185,0.19,
0.195,0.2,0.205,0.21,0.215,0.22,0.225,0.23,0.235,0.24,0.245,0.25,0.255,
0.26,0.265,0.27,0.275,0.28,0.285,0.29,0.295,0.3,0.305,0.31,0.315,0.32,0.325,
0.33,0.335,0.34,0.345,0.35,0.355,0.36,0.365,0.37,0.375,0.38,0.385,0.39,
0.395,0.4,0.405,0.41,0.415,0.42,0.425,0.43,0.435,0.44,0.445,0.45,0.455,
0.46,0.465,0.47,0.475,0.48,0.485,0.49,0.495,0.5,0.505,0.51,0.515,0.52,0.525,
0.53,0.535,0.54,0.545,0.55,0.555,0.56,0.565,0.57,0.575,0.58,0.585,0.59,
0.595,0.6,0.605,0.61,0.615,0.62,0.625,0.63,0.635,0.64,0.645,0.65,0.655,
0.66,0.665,0.67,0.675,0.68,0.685,0.690000000000001,0.695000000000001,0.700000000000001,
0.705000000000001,0.710000000000001,0.715000000000001,0.720000000000001,
0.725000000000001,0.730000000000001,0.735000000000001,0.740000000000001,
0.745000000000001,0.750000000000001,0.755000000000001,0.760000000000001,
0.765000000000001,0.770000000000001,0.775000000000001,0.780000000000001,
0.785000000000001,0.790000000000001,0.795000000000001,0.800000000000001,
0.805000000000001,0.810000000000001,0.815000000000001,0.820000000000001,
0.825000000000001,0.830000000000001,0.835000000000001,0.840000000000001,
0.845000000000001,0.850000000000001,0.855000000000001,0.860000000000001,
0.865000000000001,0.870000000000001,0.875000000000001,0.880000000000001,
0.885000000000001,0.890000000000001,0.895000000000001,0.900000000000001,
0.905000000000001,0.910000000000001,0.915000000000001,0.920000000000001,
0.925000000000001,0.930000000000001,0.935000000000001,0.940000000000001,
0.945000000000001,0.950000000000001,0.955000000000001,0.960000000000001,
0.965000000000001,0.970000000000001,0.975000000000001,0.980000000000001,
0.985000000000001,0.990000000000001,0.995000000000001,1.),(0.,1.2),
 .UNSPECIFIED.)
GEOMETRIC_REPRESENTATION_ITEM()
RATIONAL_B_SPLINE_SURFACE(((1.,1.),(1.,1.),(1.,1.),(1.,1.),(1.,1.),(1.,
1.),(1.,1.),(1.,1.),(1.,1.),(1.,1.),(1.,1.),(1.,1.),(1.,1.),(1.,1.),(1.,
1.),(1.,1.),(1.,1.),(1.,1.),(1.,1.),(1.,1.),(1.,1.),(1.,1.),(1.,1.),(1.,
1.),(1.,1.),(1.,1.),(1.,1.),(1.,1.),(1.,1.),(1.,1.),(1.,1.),(1.,1.),(1.,
1.),(1.,1.),(1.,1.),(1.,1.),(1.,1.),(1.,1.),(1.,1.),(1.,1.),(1.,1.),(1.,
1.),(1.,1.),(1.,1.),(1.,1.),(1.,1.),(1.,1.),(1.,1.),(1.,1.),(1.,1.),(1.,
1.),(1.,1.),(1.,1.),(1.,1.),(1.,1.),(1.,1.),(1.,1.),(1.,1.),(1.,1.),(1.,
1.),(1.,1.),(1.,1.),(1.,1.),(1.,1.),(1.,1.),(1.,1.),(1.,1.),(1.,1.),(1.,
1.),(1.,1.),(1.,1.),(1.,1.),(1.,1.),(1.,1.),(1.,1.),(1.,1.),(1.,1.),(1.,
1.),(1.,1.),(1.,1.),(1.,1.),(1.,1.),(1.,1.),(1.,1.),(1.,1.),(1.,1.),(1.,
1.),(1.,1.),(1.,1.),(1.,1.),(1.,1.),(1.,1.),(1.,1.),(1.,1.),(1.,1.),(1.,
1.),(1.,1.),(1.,1.),(1.,1.),(1.,1.),(1.,1.),(1.,1.),(1.,1.),(1.,1.),(1.,
1.),(1.,1.),(1.,1.),(1.,1.),(1.,1.),(1.,1.),(1.,1.),(1.,1.),(1.,1.),(1.,
1.),(1.,1.),(1.,1.),(1.,1.),(1.,1.),(1.,1.),(1.,1.),(1.,1.),(1.,1.),(1.,
1.),(1.,1.),(1.,1.),(1.,1.),(1.,1.),(1.,1.),(1.,1.),(1.,1.),(1.,1.),(1.,
1.),(1.,1.),(1.,1.),(1.,1.),(1.,1.),(1.,1.),(1.,1.),(1.,1.),(1.,1.),(1.,
1.),(1.,1.),(1.,1.),(1.,1.),(1.,1.),(1.,1.),(1.,1.),(1.,1.),(1.,1.),(1.,
1.),(1.,1.),(1.,1.),(1.,1.),(1.,1.),(1.,1.),(1.,1.),(1.,1.),(1.,1.),(1.,
1.),(1.,1.),(1.,1.),(1.,1.),(1.,1.),(1.,1.),(1.,1.),(1.,1.),(1.,1.),(1.,
1.),(1.,1.),(1.,1.),(1.,1.),(1.,1.),(1.,1.),(1.,1.),(1.,1.),(1.,1.),(1.,
1.),(1.,1.),(1.,1.),(1.,1.),(1.,1.),(1.,1.),(1.,1.),(1.,1.),(1.,1.),(1.,
1.),(1.,1.),(1.,1.),(1.,1.),(1.,1.),(1.,1.),(1.,1.),(1.,1.),(1.,1.),(1.,
1.),(1.,1.),(1.,1.),(1.,1.),(1.,1.),(1.,1.),(1.,1.),(1.,1.),(1.,1.),(1.,
1.),(1.,1.)))
REPRESENTATION_ITEM('')
SURFACE()
);
#885=(
BOUNDED_SURFACE()
B_SPLINE_SURFACE(5,1,((#54414,#54415),(#54416,#54417),(#54418,#54419),(#54420,
#54421),(#54422,#54423),(#54424,#54425),(#54426,#54427),(#54428,#54429),
(#54430,#54431),(#54432,#54433),(#54434,#54435),(#54436,#54437),(#54438,
#54439),(#54440,#54441),(#54442,#54443),(#54444,#54445),(#54446,#54447),
(#54448,#54449),(#54450,#54451),(#54452,#54453),(#54454,#54455),(#54456,
#54457),(#54458,#54459),(#54460,#54461),(#54462,#54463),(#54464,#54465),
(#54466,#54467),(#54468,#54469),(#54470,#54471),(#54472,#54473),(#54474,
#54475),(#54476,#54477),(#54478,#54479),(#54480,#54481),(#54482,#54483),
(#54484,#54485),(#54486,#54487),(#54488,#54489),(#54490,#54491),(#54492,
#54493),(#54494,#54495),(#54496,#54497),(#54498,#54499),(#54500,#54501),
(#54502,#54503),(#54504,#54505),(#54506,#54507),(#54508,#54509),(#54510,
#54511),(#54512,#54513),(#54514,#54515),(#54516,#54517),(#54518,#54519),
(#54520,#54521),(#54522,#54523),(#54524,#54525),(#54526,#54527),(#54528,
#54529),(#54530,#54531),(#54532,#54533),(#54534,#54535),(#54536,#54537),
(#54538,#54539),(#54540,#54541),(#54542,#54543),(#54544,#54545),(#54546,
#54547),(#54548,#54549),(#54550,#54551),(#54552,#54553),(#54554,#54555),
(#54556,#54557),(#54558,#54559),(#54560,#54561),(#54562,#54563),(#54564,
#54565),(#54566,#54567),(#54568,#54569),(#54570,#54571),(#54572,#54573),
(#54574,#54575),(#54576,#54577),(#54578,#54579),(#54580,#54581),(#54582,
#54583),(#54584,#54585),(#54586,#54587),(#54588,#54589),(#54590,#54591),
(#54592,#54593),(#54594,#54595),(#54596,#54597),(#54598,#54599),(#54600,
#54601),(#54602,#54603),(#54604,#54605),(#54606,#54607),(#54608,#54609),
(#54610,#54611),(#54612,#54613),(#54614,#54615),(#54616,#54617),(#54618,
#54619),(#54620,#54621),(#54622,#54623),(#54624,#54625),(#54626,#54627),
(#54628,#54629),(#54630,#54631),(#54632,#54633),(#54634,#54635),(#54636,
#54637),(#54638,#54639),(#54640,#54641),(#54642,#54643),(#54644,#54645),
(#54646,#54647),(#54648,#54649),(#54650,#54651),(#54652,#54653),(#54654,
#54655),(#54656,#54657),(#54658,#54659),(#54660,#54661),(#54662,#54663),
(#54664,#54665),(#54666,#54667),(#54668,#54669),(#54670,#54671),(#54672,
#54673),(#54674,#54675),(#54676,#54677),(#54678,#54679),(#54680,#54681),
(#54682,#54683),(#54684,#54685),(#54686,#54687),(#54688,#54689),(#54690,
#54691),(#54692,#54693),(#54694,#54695),(#54696,#54697),(#54698,#54699),
(#54700,#54701),(#54702,#54703),(#54704,#54705),(#54706,#54707),(#54708,
#54709),(#54710,#54711),(#54712,#54713),(#54714,#54715),(#54716,#54717),
(#54718,#54719),(#54720,#54721),(#54722,#54723),(#54724,#54725),(#54726,
#54727),(#54728,#54729),(#54730,#54731),(#54732,#54733),(#54734,#54735),
(#54736,#54737),(#54738,#54739),(#54740,#54741),(#54742,#54743),(#54744,
#54745),(#54746,#54747),(#54748,#54749),(#54750,#54751),(#54752,#54753),
(#54754,#54755),(#54756,#54757),(#54758,#54759),(#54760,#54761),(#54762,
#54763),(#54764,#54765),(#54766,#54767),(#54768,#54769),(#54770,#54771),
(#54772,#54773),(#54774,#54775),(#54776,#54777),(#54778,#54779),(#54780,
#54781),(#54782,#54783),(#54784,#54785),(#54786,#54787),(#54788,#54789),
(#54790,#54791),(#54792,#54793),(#54794,#54795),(#54796,#54797),(#54798,
#54799),(#54800,#54801),(#54802,#54803),(#54804,#54805),(#54806,#54807),
(#54808,#54809),(#54810,#54811),(#54812,#54813),(#54814,#54815),(#54816,
#54817),(#54818,#54819),(#54820,#54821),(#54822,#54823)),.UNSPECIFIED.,
 .F.,.F.,.F.)
B_SPLINE_SURFACE_WITH_KNOTS((6,1,1,1,1,1,1,1,1,1,1,1,1,1,1,1,1,1,1,1,1,
1,1,1,1,1,1,1,1,1,1,1,1,1,1,1,1,1,1,1,1,1,1,1,1,1,1,1,1,1,1,1,1,1,1,1,1,
1,1,1,1,1,1,1,1,1,1,1,1,1,1,1,1,1,1,1,1,1,1,1,1,1,1,1,1,1,1,1,1,1,1,1,1,
1,1,1,1,1,1,1,1,1,1,1,1,1,1,1,1,1,1,1,1,1,1,1,1,1,1,1,1,1,1,1,1,1,1,1,1,
1,1,1,1,1,1,1,1,1,1,1,1,1,1,1,1,1,1,1,1,1,1,1,1,1,1,1,1,1,1,1,1,1,1,1,1,
1,1,1,1,1,1,1,1,1,1,1,1,1,1,1,1,1,1,1,1,1,1,1,1,1,1,1,1,1,1,1,1,1,1,1,6),
(2,2),(0.,0.005,0.01,0.015,0.02,0.025,0.03,0.035,0.04,0.045,0.05,0.055,
0.06,0.065,0.07,0.075,0.08,0.085,0.09,0.095,0.1,0.105,0.11,0.115,0.12,0.125,
0.13,0.135,0.14,0.145,0.15,0.155,0.16,0.165,0.17,0.175,0.18,0.185,0.19,
0.195,0.2,0.205,0.21,0.215,0.22,0.225,0.23,0.235,0.24,0.245,0.25,0.255,
0.26,0.265,0.27,0.275,0.28,0.285,0.29,0.295,0.3,0.305,0.31,0.315,0.32,0.325,
0.33,0.335,0.34,0.345,0.35,0.355,0.36,0.365,0.37,0.375,0.38,0.385,0.39,
0.395,0.4,0.405,0.41,0.415,0.42,0.425,0.43,0.435,0.44,0.445,0.45,0.455,
0.46,0.465,0.47,0.475,0.48,0.485,0.49,0.495,0.5,0.505,0.51,0.515,0.52,0.525,
0.53,0.535,0.54,0.545,0.55,0.555,0.56,0.565,0.57,0.575,0.58,0.585,0.59,
0.595,0.6,0.605,0.61,0.615,0.62,0.625,0.63,0.635,0.64,0.645,0.65,0.655,
0.66,0.665,0.67,0.675,0.68,0.685,0.690000000000001,0.695000000000001,0.700000000000001,
0.705000000000001,0.710000000000001,0.715000000000001,0.720000000000001,
0.725000000000001,0.730000000000001,0.735000000000001,0.740000000000001,
0.745000000000001,0.750000000000001,0.755000000000001,0.760000000000001,
0.765000000000001,0.770000000000001,0.775000000000001,0.780000000000001,
0.785000000000001,0.790000000000001,0.795000000000001,0.800000000000001,
0.805000000000001,0.810000000000001,0.815000000000001,0.820000000000001,
0.825000000000001,0.830000000000001,0.835000000000001,0.840000000000001,
0.845000000000001,0.850000000000001,0.855000000000001,0.860000000000001,
0.865000000000001,0.870000000000001,0.875000000000001,0.880000000000001,
0.885000000000001,0.890000000000001,0.895000000000001,0.900000000000001,
0.905000000000001,0.910000000000001,0.915000000000001,0.920000000000001,
0.925000000000001,0.930000000000001,0.935000000000001,0.940000000000001,
0.945000000000001,0.950000000000001,0.955000000000001,0.960000000000001,
0.965000000000001,0.970000000000001,0.975000000000001,0.980000000000001,
0.985000000000001,0.990000000000001,0.995000000000001,1.),(0.,1.2),
 .UNSPECIFIED.)
GEOMETRIC_REPRESENTATION_ITEM()
RATIONAL_B_SPLINE_SURFACE(((1.,1.),(1.,1.),(1.,1.),(1.,1.),(1.,1.),(1.,
1.),(1.,1.),(1.,1.),(1.,1.),(1.,1.),(1.,1.),(1.,1.),(1.,1.),(1.,1.),(1.,
1.),(1.,1.),(1.,1.),(1.,1.),(1.,1.),(1.,1.),(1.,1.),(1.,1.),(1.,1.),(1.,
1.),(1.,1.),(1.,1.),(1.,1.),(1.,1.),(1.,1.),(1.,1.),(1.,1.),(1.,1.),(1.,
1.),(1.,1.),(1.,1.),(1.,1.),(1.,1.),(1.,1.),(1.,1.),(1.,1.),(1.,1.),(1.,
1.),(1.,1.),(1.,1.),(1.,1.),(1.,1.),(1.,1.),(1.,1.),(1.,1.),(1.,1.),(1.,
1.),(1.,1.),(1.,1.),(1.,1.),(1.,1.),(1.,1.),(1.,1.),(1.,1.),(1.,1.),(1.,
1.),(1.,1.),(1.,1.),(1.,1.),(1.,1.),(1.,1.),(1.,1.),(1.,1.),(1.,1.),(1.,
1.),(1.,1.),(1.,1.),(1.,1.),(1.,1.),(1.,1.),(1.,1.),(1.,1.),(1.,1.),(1.,
1.),(1.,1.),(1.,1.),(1.,1.),(1.,1.),(1.,1.),(1.,1.),(1.,1.),(1.,1.),(1.,
1.),(1.,1.),(1.,1.),(1.,1.),(1.,1.),(1.,1.),(1.,1.),(1.,1.),(1.,1.),(1.,
1.),(1.,1.),(1.,1.),(1.,1.),(1.,1.),(1.,1.),(1.,1.),(1.,1.),(1.,1.),(1.,
1.),(1.,1.),(1.,1.),(1.,1.),(1.,1.),(1.,1.),(1.,1.),(1.,1.),(1.,1.),(1.,
1.),(1.,1.),(1.,1.),(1.,1.),(1.,1.),(1.,1.),(1.,1.),(1.,1.),(1.,1.),(1.,
1.),(1.,1.),(1.,1.),(1.,1.),(1.,1.),(1.,1.),(1.,1.),(1.,1.),(1.,1.),(1.,
1.),(1.,1.),(1.,1.),(1.,1.),(1.,1.),(1.,1.),(1.,1.),(1.,1.),(1.,1.),(1.,
1.),(1.,1.),(1.,1.),(1.,1.),(1.,1.),(1.,1.),(1.,1.),(1.,1.),(1.,1.),(1.,
1.),(1.,1.),(1.,1.),(1.,1.),(1.,1.),(1.,1.),(1.,1.),(1.,1.),(1.,1.),(1.,
1.),(1.,1.),(1.,1.),(1.,1.),(1.,1.),(1.,1.),(1.,1.),(1.,1.),(1.,1.),(1.,
1.),(1.,1.),(1.,1.),(1.,1.),(1.,1.),(1.,1.),(1.,1.),(1.,1.),(1.,1.),(1.,
1.),(1.,1.),(1.,1.),(1.,1.),(1.,1.),(1.,1.),(1.,1.),(1.,1.),(1.,1.),(1.,
1.),(1.,1.),(1.,1.),(1.,1.),(1.,1.),(1.,1.),(1.,1.),(1.,1.),(1.,1.),(1.,
1.),(1.,1.),(1.,1.),(1.,1.),(1.,1.),(1.,1.),(1.,1.),(1.,1.),(1.,1.),(1.,
1.),(1.,1.)))
REPRESENTATION_ITEM('')
SURFACE()
);
#886=(
BOUNDED_SURFACE()
B_SPLINE_SURFACE(5,1,((#55310,#55311),(#55312,#55313),(#55314,#55315),(#55316,
#55317),(#55318,#55319),(#55320,#55321),(#55322,#55323),(#55324,#55325),
(#55326,#55327),(#55328,#55329),(#55330,#55331),(#55332,#55333),(#55334,
#55335),(#55336,#55337),(#55338,#55339),(#55340,#55341),(#55342,#55343),
(#55344,#55345),(#55346,#55347),(#55348,#55349),(#55350,#55351),(#55352,
#55353),(#55354,#55355),(#55356,#55357),(#55358,#55359),(#55360,#55361),
(#55362,#55363),(#55364,#55365),(#55366,#55367),(#55368,#55369),(#55370,
#55371),(#55372,#55373),(#55374,#55375),(#55376,#55377),(#55378,#55379),
(#55380,#55381),(#55382,#55383),(#55384,#55385),(#55386,#55387),(#55388,
#55389),(#55390,#55391),(#55392,#55393),(#55394,#55395),(#55396,#55397),
(#55398,#55399),(#55400,#55401),(#55402,#55403),(#55404,#55405),(#55406,
#55407),(#55408,#55409),(#55410,#55411),(#55412,#55413),(#55414,#55415),
(#55416,#55417),(#55418,#55419),(#55420,#55421),(#55422,#55423),(#55424,
#55425),(#55426,#55427),(#55428,#55429),(#55430,#55431),(#55432,#55433),
(#55434,#55435),(#55436,#55437),(#55438,#55439),(#55440,#55441),(#55442,
#55443),(#55444,#55445),(#55446,#55447),(#55448,#55449),(#55450,#55451),
(#55452,#55453),(#55454,#55455),(#55456,#55457),(#55458,#55459),(#55460,
#55461),(#55462,#55463),(#55464,#55465),(#55466,#55467),(#55468,#55469),
(#55470,#55471),(#55472,#55473),(#55474,#55475),(#55476,#55477),(#55478,
#55479),(#55480,#55481),(#55482,#55483),(#55484,#55485),(#55486,#55487),
(#55488,#55489),(#55490,#55491),(#55492,#55493),(#55494,#55495),(#55496,
#55497),(#55498,#55499),(#55500,#55501),(#55502,#55503),(#55504,#55505),
(#55506,#55507),(#55508,#55509),(#55510,#55511),(#55512,#55513),(#55514,
#55515),(#55516,#55517),(#55518,#55519),(#55520,#55521),(#55522,#55523),
(#55524,#55525),(#55526,#55527),(#55528,#55529),(#55530,#55531),(#55532,
#55533),(#55534,#55535),(#55536,#55537),(#55538,#55539),(#55540,#55541),
(#55542,#55543),(#55544,#55545),(#55546,#55547),(#55548,#55549),(#55550,
#55551),(#55552,#55553),(#55554,#55555),(#55556,#55557),(#55558,#55559),
(#55560,#55561),(#55562,#55563),(#55564,#55565),(#55566,#55567),(#55568,
#55569),(#55570,#55571),(#55572,#55573),(#55574,#55575),(#55576,#55577),
(#55578,#55579),(#55580,#55581),(#55582,#55583),(#55584,#55585),(#55586,
#55587),(#55588,#55589),(#55590,#55591),(#55592,#55593),(#55594,#55595),
(#55596,#55597),(#55598,#55599),(#55600,#55601),(#55602,#55603),(#55604,
#55605),(#55606,#55607),(#55608,#55609),(#55610,#55611),(#55612,#55613),
(#55614,#55615),(#55616,#55617),(#55618,#55619),(#55620,#55621),(#55622,
#55623),(#55624,#55625),(#55626,#55627),(#55628,#55629),(#55630,#55631),
(#55632,#55633),(#55634,#55635),(#55636,#55637),(#55638,#55639),(#55640,
#55641),(#55642,#55643),(#55644,#55645),(#55646,#55647),(#55648,#55649),
(#55650,#55651),(#55652,#55653),(#55654,#55655),(#55656,#55657),(#55658,
#55659),(#55660,#55661),(#55662,#55663),(#55664,#55665),(#55666,#55667),
(#55668,#55669),(#55670,#55671),(#55672,#55673),(#55674,#55675),(#55676,
#55677),(#55678,#55679),(#55680,#55681),(#55682,#55683),(#55684,#55685),
(#55686,#55687),(#55688,#55689),(#55690,#55691),(#55692,#55693),(#55694,
#55695),(#55696,#55697),(#55698,#55699),(#55700,#55701),(#55702,#55703),
(#55704,#55705),(#55706,#55707),(#55708,#55709),(#55710,#55711),(#55712,
#55713),(#55714,#55715),(#55716,#55717),(#55718,#55719)),.UNSPECIFIED.,
 .F.,.F.,.F.)
B_SPLINE_SURFACE_WITH_KNOTS((6,1,1,1,1,1,1,1,1,1,1,1,1,1,1,1,1,1,1,1,1,
1,1,1,1,1,1,1,1,1,1,1,1,1,1,1,1,1,1,1,1,1,1,1,1,1,1,1,1,1,1,1,1,1,1,1,1,
1,1,1,1,1,1,1,1,1,1,1,1,1,1,1,1,1,1,1,1,1,1,1,1,1,1,1,1,1,1,1,1,1,1,1,1,
1,1,1,1,1,1,1,1,1,1,1,1,1,1,1,1,1,1,1,1,1,1,1,1,1,1,1,1,1,1,1,1,1,1,1,1,
1,1,1,1,1,1,1,1,1,1,1,1,1,1,1,1,1,1,1,1,1,1,1,1,1,1,1,1,1,1,1,1,1,1,1,1,
1,1,1,1,1,1,1,1,1,1,1,1,1,1,1,1,1,1,1,1,1,1,1,1,1,1,1,1,1,1,1,1,1,1,1,6),
(2,2),(0.,0.005,0.01,0.015,0.02,0.025,0.03,0.035,0.04,0.045,0.05,0.055,
0.06,0.065,0.07,0.075,0.08,0.085,0.09,0.095,0.1,0.105,0.11,0.115,0.12,0.125,
0.13,0.135,0.14,0.145,0.15,0.155,0.16,0.165,0.17,0.175,0.18,0.185,0.19,
0.195,0.2,0.205,0.21,0.215,0.22,0.225,0.23,0.235,0.24,0.245,0.25,0.255,
0.26,0.265,0.27,0.275,0.28,0.285,0.29,0.295,0.3,0.305,0.31,0.315,0.32,0.325,
0.33,0.335,0.34,0.345,0.35,0.355,0.36,0.365,0.37,0.375,0.38,0.385,0.39,
0.395,0.4,0.405,0.41,0.415,0.42,0.425,0.43,0.435,0.44,0.445,0.45,0.455,
0.46,0.465,0.47,0.475,0.48,0.485,0.49,0.495,0.5,0.505,0.51,0.515,0.52,0.525,
0.53,0.535,0.54,0.545,0.55,0.555,0.56,0.565,0.57,0.575,0.58,0.585,0.59,
0.595,0.6,0.605,0.61,0.615,0.62,0.625,0.63,0.635,0.64,0.645,0.65,0.655,
0.66,0.665,0.67,0.675,0.68,0.685,0.690000000000001,0.695000000000001,0.700000000000001,
0.705000000000001,0.710000000000001,0.715000000000001,0.720000000000001,
0.725000000000001,0.730000000000001,0.735000000000001,0.740000000000001,
0.745000000000001,0.750000000000001,0.755000000000001,0.760000000000001,
0.765000000000001,0.770000000000001,0.775000000000001,0.780000000000001,
0.785000000000001,0.790000000000001,0.795000000000001,0.800000000000001,
0.805000000000001,0.810000000000001,0.815000000000001,0.820000000000001,
0.825000000000001,0.830000000000001,0.835000000000001,0.840000000000001,
0.845000000000001,0.850000000000001,0.855000000000001,0.860000000000001,
0.865000000000001,0.870000000000001,0.875000000000001,0.880000000000001,
0.885000000000001,0.890000000000001,0.895000000000001,0.900000000000001,
0.905000000000001,0.910000000000001,0.915000000000001,0.920000000000001,
0.925000000000001,0.930000000000001,0.935000000000001,0.940000000000001,
0.945000000000001,0.950000000000001,0.955000000000001,0.960000000000001,
0.965000000000001,0.970000000000001,0.975000000000001,0.980000000000001,
0.985000000000001,0.990000000000001,0.995000000000001,1.),(0.,1.2),
 .UNSPECIFIED.)
GEOMETRIC_REPRESENTATION_ITEM()
RATIONAL_B_SPLINE_SURFACE(((1.,1.),(1.,1.),(1.,1.),(1.,1.),(1.,1.),(1.,
1.),(1.,1.),(1.,1.),(1.,1.),(1.,1.),(1.,1.),(1.,1.),(1.,1.),(1.,1.),(1.,
1.),(1.,1.),(1.,1.),(1.,1.),(1.,1.),(1.,1.),(1.,1.),(1.,1.),(1.,1.),(1.,
1.),(1.,1.),(1.,1.),(1.,1.),(1.,1.),(1.,1.),(1.,1.),(1.,1.),(1.,1.),(1.,
1.),(1.,1.),(1.,1.),(1.,1.),(1.,1.),(1.,1.),(1.,1.),(1.,1.),(1.,1.),(1.,
1.),(1.,1.),(1.,1.),(1.,1.),(1.,1.),(1.,1.),(1.,1.),(1.,1.),(1.,1.),(1.,
1.),(1.,1.),(1.,1.),(1.,1.),(1.,1.),(1.,1.),(1.,1.),(1.,1.),(1.,1.),(1.,
1.),(1.,1.),(1.,1.),(1.,1.),(1.,1.),(1.,1.),(1.,1.),(1.,1.),(1.,1.),(1.,
1.),(1.,1.),(1.,1.),(1.,1.),(1.,1.),(1.,1.),(1.,1.),(1.,1.),(1.,1.),(1.,
1.),(1.,1.),(1.,1.),(1.,1.),(1.,1.),(1.,1.),(1.,1.),(1.,1.),(1.,1.),(1.,
1.),(1.,1.),(1.,1.),(1.,1.),(1.,1.),(1.,1.),(1.,1.),(1.,1.),(1.,1.),(1.,
1.),(1.,1.),(1.,1.),(1.,1.),(1.,1.),(1.,1.),(1.,1.),(1.,1.),(1.,1.),(1.,
1.),(1.,1.),(1.,1.),(1.,1.),(1.,1.),(1.,1.),(1.,1.),(1.,1.),(1.,1.),(1.,
1.),(1.,1.),(1.,1.),(1.,1.),(1.,1.),(1.,1.),(1.,1.),(1.,1.),(1.,1.),(1.,
1.),(1.,1.),(1.,1.),(1.,1.),(1.,1.),(1.,1.),(1.,1.),(1.,1.),(1.,1.),(1.,
1.),(1.,1.),(1.,1.),(1.,1.),(1.,1.),(1.,1.),(1.,1.),(1.,1.),(1.,1.),(1.,
1.),(1.,1.),(1.,1.),(1.,1.),(1.,1.),(1.,1.),(1.,1.),(1.,1.),(1.,1.),(1.,
1.),(1.,1.),(1.,1.),(1.,1.),(1.,1.),(1.,1.),(1.,1.),(1.,1.),(1.,1.),(1.,
1.),(1.,1.),(1.,1.),(1.,1.),(1.,1.),(1.,1.),(1.,1.),(1.,1.),(1.,1.),(1.,
1.),(1.,1.),(1.,1.),(1.,1.),(1.,1.),(1.,1.),(1.,1.),(1.,1.),(1.,1.),(1.,
1.),(1.,1.),(1.,1.),(1.,1.),(1.,1.),(1.,1.),(1.,1.),(1.,1.),(1.,1.),(1.,
1.),(1.,1.),(1.,1.),(1.,1.),(1.,1.),(1.,1.),(1.,1.),(1.,1.),(1.,1.),(1.,
1.),(1.,1.),(1.,1.),(1.,1.),(1.,1.),(1.,1.),(1.,1.),(1.,1.),(1.,1.),(1.,
1.),(1.,1.)))
REPRESENTATION_ITEM('')
SURFACE()
);
#887=(
BOUNDED_SURFACE()
B_SPLINE_SURFACE(5,1,((#56206,#56207),(#56208,#56209),(#56210,#56211),(#56212,
#56213),(#56214,#56215),(#56216,#56217),(#56218,#56219),(#56220,#56221),
(#56222,#56223),(#56224,#56225),(#56226,#56227),(#56228,#56229),(#56230,
#56231),(#56232,#56233),(#56234,#56235),(#56236,#56237),(#56238,#56239),
(#56240,#56241),(#56242,#56243),(#56244,#56245),(#56246,#56247),(#56248,
#56249),(#56250,#56251),(#56252,#56253),(#56254,#56255),(#56256,#56257),
(#56258,#56259),(#56260,#56261),(#56262,#56263),(#56264,#56265),(#56266,
#56267),(#56268,#56269),(#56270,#56271),(#56272,#56273),(#56274,#56275),
(#56276,#56277),(#56278,#56279),(#56280,#56281),(#56282,#56283),(#56284,
#56285),(#56286,#56287),(#56288,#56289),(#56290,#56291),(#56292,#56293),
(#56294,#56295),(#56296,#56297),(#56298,#56299),(#56300,#56301),(#56302,
#56303),(#56304,#56305),(#56306,#56307),(#56308,#56309),(#56310,#56311),
(#56312,#56313),(#56314,#56315),(#56316,#56317),(#56318,#56319),(#56320,
#56321),(#56322,#56323),(#56324,#56325),(#56326,#56327),(#56328,#56329),
(#56330,#56331),(#56332,#56333),(#56334,#56335),(#56336,#56337),(#56338,
#56339),(#56340,#56341),(#56342,#56343),(#56344,#56345),(#56346,#56347),
(#56348,#56349),(#56350,#56351),(#56352,#56353),(#56354,#56355),(#56356,
#56357),(#56358,#56359),(#56360,#56361),(#56362,#56363),(#56364,#56365),
(#56366,#56367),(#56368,#56369),(#56370,#56371),(#56372,#56373),(#56374,
#56375),(#56376,#56377),(#56378,#56379),(#56380,#56381),(#56382,#56383),
(#56384,#56385),(#56386,#56387),(#56388,#56389),(#56390,#56391),(#56392,
#56393),(#56394,#56395),(#56396,#56397),(#56398,#56399),(#56400,#56401),
(#56402,#56403),(#56404,#56405),(#56406,#56407),(#56408,#56409),(#56410,
#56411),(#56412,#56413),(#56414,#56415),(#56416,#56417),(#56418,#56419),
(#56420,#56421),(#56422,#56423),(#56424,#56425),(#56426,#56427),(#56428,
#56429),(#56430,#56431),(#56432,#56433),(#56434,#56435),(#56436,#56437),
(#56438,#56439),(#56440,#56441),(#56442,#56443),(#56444,#56445),(#56446,
#56447),(#56448,#56449),(#56450,#56451),(#56452,#56453),(#56454,#56455),
(#56456,#56457),(#56458,#56459),(#56460,#56461),(#56462,#56463),(#56464,
#56465),(#56466,#56467),(#56468,#56469),(#56470,#56471),(#56472,#56473),
(#56474,#56475),(#56476,#56477),(#56478,#56479),(#56480,#56481),(#56482,
#56483),(#56484,#56485),(#56486,#56487),(#56488,#56489),(#56490,#56491),
(#56492,#56493),(#56494,#56495),(#56496,#56497),(#56498,#56499),(#56500,
#56501),(#56502,#56503),(#56504,#56505),(#56506,#56507),(#56508,#56509),
(#56510,#56511),(#56512,#56513),(#56514,#56515),(#56516,#56517),(#56518,
#56519),(#56520,#56521),(#56522,#56523),(#56524,#56525),(#56526,#56527),
(#56528,#56529),(#56530,#56531),(#56532,#56533),(#56534,#56535),(#56536,
#56537),(#56538,#56539),(#56540,#56541),(#56542,#56543),(#56544,#56545),
(#56546,#56547),(#56548,#56549),(#56550,#56551),(#56552,#56553),(#56554,
#56555),(#56556,#56557),(#56558,#56559),(#56560,#56561),(#56562,#56563),
(#56564,#56565),(#56566,#56567),(#56568,#56569),(#56570,#56571),(#56572,
#56573),(#56574,#56575),(#56576,#56577),(#56578,#56579),(#56580,#56581),
(#56582,#56583),(#56584,#56585),(#56586,#56587),(#56588,#56589),(#56590,
#56591),(#56592,#56593),(#56594,#56595),(#56596,#56597),(#56598,#56599),
(#56600,#56601),(#56602,#56603),(#56604,#56605),(#56606,#56607),(#56608,
#56609),(#56610,#56611),(#56612,#56613),(#56614,#56615)),.UNSPECIFIED.,
 .F.,.F.,.F.)
B_SPLINE_SURFACE_WITH_KNOTS((6,1,1,1,1,1,1,1,1,1,1,1,1,1,1,1,1,1,1,1,1,
1,1,1,1,1,1,1,1,1,1,1,1,1,1,1,1,1,1,1,1,1,1,1,1,1,1,1,1,1,1,1,1,1,1,1,1,
1,1,1,1,1,1,1,1,1,1,1,1,1,1,1,1,1,1,1,1,1,1,1,1,1,1,1,1,1,1,1,1,1,1,1,1,
1,1,1,1,1,1,1,1,1,1,1,1,1,1,1,1,1,1,1,1,1,1,1,1,1,1,1,1,1,1,1,1,1,1,1,1,
1,1,1,1,1,1,1,1,1,1,1,1,1,1,1,1,1,1,1,1,1,1,1,1,1,1,1,1,1,1,1,1,1,1,1,1,
1,1,1,1,1,1,1,1,1,1,1,1,1,1,1,1,1,1,1,1,1,1,1,1,1,1,1,1,1,1,1,1,1,1,1,6),
(2,2),(0.,0.005,0.01,0.015,0.02,0.025,0.03,0.035,0.04,0.045,0.05,0.055,
0.06,0.065,0.07,0.075,0.08,0.085,0.09,0.095,0.1,0.105,0.11,0.115,0.12,0.125,
0.13,0.135,0.14,0.145,0.15,0.155,0.16,0.165,0.17,0.175,0.18,0.185,0.19,
0.195,0.2,0.205,0.21,0.215,0.22,0.225,0.23,0.235,0.24,0.245,0.25,0.255,
0.26,0.265,0.27,0.275,0.28,0.285,0.29,0.295,0.3,0.305,0.31,0.315,0.32,0.325,
0.33,0.335,0.34,0.345,0.35,0.355,0.36,0.365,0.37,0.375,0.38,0.385,0.39,
0.395,0.4,0.405,0.41,0.415,0.42,0.425,0.43,0.435,0.44,0.445,0.45,0.455,
0.46,0.465,0.47,0.475,0.48,0.485,0.49,0.495,0.5,0.505,0.51,0.515,0.52,0.525,
0.53,0.535,0.54,0.545,0.55,0.555,0.56,0.565,0.57,0.575,0.58,0.585,0.59,
0.595,0.6,0.605,0.61,0.615,0.62,0.625,0.63,0.635,0.64,0.645,0.65,0.655,
0.66,0.665,0.67,0.675,0.68,0.685,0.690000000000001,0.695000000000001,0.700000000000001,
0.705000000000001,0.710000000000001,0.715000000000001,0.720000000000001,
0.725000000000001,0.730000000000001,0.735000000000001,0.740000000000001,
0.745000000000001,0.750000000000001,0.755000000000001,0.760000000000001,
0.765000000000001,0.770000000000001,0.775000000000001,0.780000000000001,
0.785000000000001,0.790000000000001,0.795000000000001,0.800000000000001,
0.805000000000001,0.810000000000001,0.815000000000001,0.820000000000001,
0.825000000000001,0.830000000000001,0.835000000000001,0.840000000000001,
0.845000000000001,0.850000000000001,0.855000000000001,0.860000000000001,
0.865000000000001,0.870000000000001,0.875000000000001,0.880000000000001,
0.885000000000001,0.890000000000001,0.895000000000001,0.900000000000001,
0.905000000000001,0.910000000000001,0.915000000000001,0.920000000000001,
0.925000000000001,0.930000000000001,0.935000000000001,0.940000000000001,
0.945000000000001,0.950000000000001,0.955000000000001,0.960000000000001,
0.965000000000001,0.970000000000001,0.975000000000001,0.980000000000001,
0.985000000000001,0.990000000000001,0.995000000000001,1.),(0.,1.2),
 .UNSPECIFIED.)
GEOMETRIC_REPRESENTATION_ITEM()
RATIONAL_B_SPLINE_SURFACE(((1.,1.),(1.,1.),(1.,1.),(1.,1.),(1.,1.),(1.,
1.),(1.,1.),(1.,1.),(1.,1.),(1.,1.),(1.,1.),(1.,1.),(1.,1.),(1.,1.),(1.,
1.),(1.,1.),(1.,1.),(1.,1.),(1.,1.),(1.,1.),(1.,1.),(1.,1.),(1.,1.),(1.,
1.),(1.,1.),(1.,1.),(1.,1.),(1.,1.),(1.,1.),(1.,1.),(1.,1.),(1.,1.),(1.,
1.),(1.,1.),(1.,1.),(1.,1.),(1.,1.),(1.,1.),(1.,1.),(1.,1.),(1.,1.),(1.,
1.),(1.,1.),(1.,1.),(1.,1.),(1.,1.),(1.,1.),(1.,1.),(1.,1.),(1.,1.),(1.,
1.),(1.,1.),(1.,1.),(1.,1.),(1.,1.),(1.,1.),(1.,1.),(1.,1.),(1.,1.),(1.,
1.),(1.,1.),(1.,1.),(1.,1.),(1.,1.),(1.,1.),(1.,1.),(1.,1.),(1.,1.),(1.,
1.),(1.,1.),(1.,1.),(1.,1.),(1.,1.),(1.,1.),(1.,1.),(1.,1.),(1.,1.),(1.,
1.),(1.,1.),(1.,1.),(1.,1.),(1.,1.),(1.,1.),(1.,1.),(1.,1.),(1.,1.),(1.,
1.),(1.,1.),(1.,1.),(1.,1.),(1.,1.),(1.,1.),(1.,1.),(1.,1.),(1.,1.),(1.,
1.),(1.,1.),(1.,1.),(1.,1.),(1.,1.),(1.,1.),(1.,1.),(1.,1.),(1.,1.),(1.,
1.),(1.,1.),(1.,1.),(1.,1.),(1.,1.),(1.,1.),(1.,1.),(1.,1.),(1.,1.),(1.,
1.),(1.,1.),(1.,1.),(1.,1.),(1.,1.),(1.,1.),(1.,1.),(1.,1.),(1.,1.),(1.,
1.),(1.,1.),(1.,1.),(1.,1.),(1.,1.),(1.,1.),(1.,1.),(1.,1.),(1.,1.),(1.,
1.),(1.,1.),(1.,1.),(1.,1.),(1.,1.),(1.,1.),(1.,1.),(1.,1.),(1.,1.),(1.,
1.),(1.,1.),(1.,1.),(1.,1.),(1.,1.),(1.,1.),(1.,1.),(1.,1.),(1.,1.),(1.,
1.),(1.,1.),(1.,1.),(1.,1.),(1.,1.),(1.,1.),(1.,1.),(1.,1.),(1.,1.),(1.,
1.),(1.,1.),(1.,1.),(1.,1.),(1.,1.),(1.,1.),(1.,1.),(1.,1.),(1.,1.),(1.,
1.),(1.,1.),(1.,1.),(1.,1.),(1.,1.),(1.,1.),(1.,1.),(1.,1.),(1.,1.),(1.,
1.),(1.,1.),(1.,1.),(1.,1.),(1.,1.),(1.,1.),(1.,1.),(1.,1.),(1.,1.),(1.,
1.),(1.,1.),(1.,1.),(1.,1.),(1.,1.),(1.,1.),(1.,1.),(1.,1.),(1.,1.),(1.,
1.),(1.,1.),(1.,1.),(1.,1.),(1.,1.),(1.,1.),(1.,1.),(1.,1.),(1.,1.),(1.,
1.),(1.,1.)))
REPRESENTATION_ITEM('')
SURFACE()
);
#888=(
BOUNDED_SURFACE()
B_SPLINE_SURFACE(5,1,((#57102,#57103),(#57104,#57105),(#57106,#57107),(#57108,
#57109),(#57110,#57111),(#57112,#57113),(#57114,#57115),(#57116,#57117),
(#57118,#57119),(#57120,#57121),(#57122,#57123),(#57124,#57125),(#57126,
#57127),(#57128,#57129),(#57130,#57131),(#57132,#57133),(#57134,#57135),
(#57136,#57137),(#57138,#57139),(#57140,#57141),(#57142,#57143),(#57144,
#57145),(#57146,#57147),(#57148,#57149),(#57150,#57151),(#57152,#57153),
(#57154,#57155),(#57156,#57157),(#57158,#57159),(#57160,#57161),(#57162,
#57163),(#57164,#57165),(#57166,#57167),(#57168,#57169),(#57170,#57171),
(#57172,#57173),(#57174,#57175),(#57176,#57177),(#57178,#57179),(#57180,
#57181),(#57182,#57183),(#57184,#57185),(#57186,#57187),(#57188,#57189),
(#57190,#57191),(#57192,#57193),(#57194,#57195),(#57196,#57197),(#57198,
#57199),(#57200,#57201),(#57202,#57203),(#57204,#57205),(#57206,#57207),
(#57208,#57209),(#57210,#57211),(#57212,#57213),(#57214,#57215),(#57216,
#57217),(#57218,#57219),(#57220,#57221),(#57222,#57223),(#57224,#57225),
(#57226,#57227),(#57228,#57229),(#57230,#57231),(#57232,#57233),(#57234,
#57235),(#57236,#57237),(#57238,#57239),(#57240,#57241),(#57242,#57243),
(#57244,#57245),(#57246,#57247),(#57248,#57249),(#57250,#57251),(#57252,
#57253),(#57254,#57255),(#57256,#57257),(#57258,#57259),(#57260,#57261),
(#57262,#57263),(#57264,#57265),(#57266,#57267),(#57268,#57269),(#57270,
#57271),(#57272,#57273),(#57274,#57275),(#57276,#57277),(#57278,#57279),
(#57280,#57281),(#57282,#57283),(#57284,#57285),(#57286,#57287),(#57288,
#57289),(#57290,#57291),(#57292,#57293),(#57294,#57295),(#57296,#57297),
(#57298,#57299),(#57300,#57301),(#57302,#57303),(#57304,#57305),(#57306,
#57307),(#57308,#57309),(#57310,#57311),(#57312,#57313),(#57314,#57315),
(#57316,#57317),(#57318,#57319),(#57320,#57321),(#57322,#57323),(#57324,
#57325),(#57326,#57327),(#57328,#57329),(#57330,#57331),(#57332,#57333),
(#57334,#57335),(#57336,#57337),(#57338,#57339),(#57340,#57341),(#57342,
#57343),(#57344,#57345),(#57346,#57347),(#57348,#57349),(#57350,#57351),
(#57352,#57353),(#57354,#57355),(#57356,#57357),(#57358,#57359),(#57360,
#57361),(#57362,#57363),(#57364,#57365),(#57366,#57367),(#57368,#57369),
(#57370,#57371),(#57372,#57373),(#57374,#57375),(#57376,#57377),(#57378,
#57379),(#57380,#57381),(#57382,#57383),(#57384,#57385),(#57386,#57387),
(#57388,#57389),(#57390,#57391),(#57392,#57393),(#57394,#57395),(#57396,
#57397),(#57398,#57399),(#57400,#57401),(#57402,#57403),(#57404,#57405),
(#57406,#57407),(#57408,#57409),(#57410,#57411),(#57412,#57413),(#57414,
#57415),(#57416,#57417),(#57418,#57419),(#57420,#57421),(#57422,#57423),
(#57424,#57425),(#57426,#57427),(#57428,#57429),(#57430,#57431),(#57432,
#57433),(#57434,#57435),(#57436,#57437),(#57438,#57439),(#57440,#57441),
(#57442,#57443),(#57444,#57445),(#57446,#57447),(#57448,#57449),(#57450,
#57451),(#57452,#57453),(#57454,#57455),(#57456,#57457),(#57458,#57459),
(#57460,#57461),(#57462,#57463),(#57464,#57465),(#57466,#57467),(#57468,
#57469),(#57470,#57471),(#57472,#57473),(#57474,#57475),(#57476,#57477),
(#57478,#57479),(#57480,#57481),(#57482,#57483),(#57484,#57485),(#57486,
#57487),(#57488,#57489),(#57490,#57491),(#57492,#57493),(#57494,#57495),
(#57496,#57497),(#57498,#57499),(#57500,#57501),(#57502,#57503),(#57504,
#57505),(#57506,#57507),(#57508,#57509),(#57510,#57511)),.UNSPECIFIED.,
 .F.,.F.,.F.)
B_SPLINE_SURFACE_WITH_KNOTS((6,1,1,1,1,1,1,1,1,1,1,1,1,1,1,1,1,1,1,1,1,
1,1,1,1,1,1,1,1,1,1,1,1,1,1,1,1,1,1,1,1,1,1,1,1,1,1,1,1,1,1,1,1,1,1,1,1,
1,1,1,1,1,1,1,1,1,1,1,1,1,1,1,1,1,1,1,1,1,1,1,1,1,1,1,1,1,1,1,1,1,1,1,1,
1,1,1,1,1,1,1,1,1,1,1,1,1,1,1,1,1,1,1,1,1,1,1,1,1,1,1,1,1,1,1,1,1,1,1,1,
1,1,1,1,1,1,1,1,1,1,1,1,1,1,1,1,1,1,1,1,1,1,1,1,1,1,1,1,1,1,1,1,1,1,1,1,
1,1,1,1,1,1,1,1,1,1,1,1,1,1,1,1,1,1,1,1,1,1,1,1,1,1,1,1,1,1,1,1,1,1,1,6),
(2,2),(0.,0.005,0.01,0.015,0.02,0.025,0.03,0.035,0.04,0.045,0.05,0.055,
0.06,0.065,0.07,0.075,0.08,0.085,0.09,0.095,0.1,0.105,0.11,0.115,0.12,0.125,
0.13,0.135,0.14,0.145,0.15,0.155,0.16,0.165,0.17,0.175,0.18,0.185,0.19,
0.195,0.2,0.205,0.21,0.215,0.22,0.225,0.23,0.235,0.24,0.245,0.25,0.255,
0.26,0.265,0.27,0.275,0.28,0.285,0.29,0.295,0.3,0.305,0.31,0.315,0.32,0.325,
0.33,0.335,0.34,0.345,0.35,0.355,0.36,0.365,0.37,0.375,0.38,0.385,0.39,
0.395,0.4,0.405,0.41,0.415,0.42,0.425,0.43,0.435,0.44,0.445,0.45,0.455,
0.46,0.465,0.47,0.475,0.48,0.485,0.49,0.495,0.5,0.505,0.51,0.515,0.52,0.525,
0.53,0.535,0.54,0.545,0.55,0.555,0.56,0.565,0.57,0.575,0.58,0.585,0.59,
0.595,0.6,0.605,0.61,0.615,0.62,0.625,0.63,0.635,0.64,0.645,0.65,0.655,
0.66,0.665,0.67,0.675,0.68,0.685,0.690000000000001,0.695000000000001,0.700000000000001,
0.705000000000001,0.710000000000001,0.715000000000001,0.720000000000001,
0.725000000000001,0.730000000000001,0.735000000000001,0.740000000000001,
0.745000000000001,0.750000000000001,0.755000000000001,0.760000000000001,
0.765000000000001,0.770000000000001,0.775000000000001,0.780000000000001,
0.785000000000001,0.790000000000001,0.795000000000001,0.800000000000001,
0.805000000000001,0.810000000000001,0.815000000000001,0.820000000000001,
0.825000000000001,0.830000000000001,0.835000000000001,0.840000000000001,
0.845000000000001,0.850000000000001,0.855000000000001,0.860000000000001,
0.865000000000001,0.870000000000001,0.875000000000001,0.880000000000001,
0.885000000000001,0.890000000000001,0.895000000000001,0.900000000000001,
0.905000000000001,0.910000000000001,0.915000000000001,0.920000000000001,
0.925000000000001,0.930000000000001,0.935000000000001,0.940000000000001,
0.945000000000001,0.950000000000001,0.955000000000001,0.960000000000001,
0.965000000000001,0.970000000000001,0.975000000000001,0.980000000000001,
0.985000000000001,0.990000000000001,0.995000000000001,1.),(0.,1.2),
 .UNSPECIFIED.)
GEOMETRIC_REPRESENTATION_ITEM()
RATIONAL_B_SPLINE_SURFACE(((1.,1.),(1.,1.),(1.,1.),(1.,1.),(1.,1.),(1.,
1.),(1.,1.),(1.,1.),(1.,1.),(1.,1.),(1.,1.),(1.,1.),(1.,1.),(1.,1.),(1.,
1.),(1.,1.),(1.,1.),(1.,1.),(1.,1.),(1.,1.),(1.,1.),(1.,1.),(1.,1.),(1.,
1.),(1.,1.),(1.,1.),(1.,1.),(1.,1.),(1.,1.),(1.,1.),(1.,1.),(1.,1.),(1.,
1.),(1.,1.),(1.,1.),(1.,1.),(1.,1.),(1.,1.),(1.,1.),(1.,1.),(1.,1.),(1.,
1.),(1.,1.),(1.,1.),(1.,1.),(1.,1.),(1.,1.),(1.,1.),(1.,1.),(1.,1.),(1.,
1.),(1.,1.),(1.,1.),(1.,1.),(1.,1.),(1.,1.),(1.,1.),(1.,1.),(1.,1.),(1.,
1.),(1.,1.),(1.,1.),(1.,1.),(1.,1.),(1.,1.),(1.,1.),(1.,1.),(1.,1.),(1.,
1.),(1.,1.),(1.,1.),(1.,1.),(1.,1.),(1.,1.),(1.,1.),(1.,1.),(1.,1.),(1.,
1.),(1.,1.),(1.,1.),(1.,1.),(1.,1.),(1.,1.),(1.,1.),(1.,1.),(1.,1.),(1.,
1.),(1.,1.),(1.,1.),(1.,1.),(1.,1.),(1.,1.),(1.,1.),(1.,1.),(1.,1.),(1.,
1.),(1.,1.),(1.,1.),(1.,1.),(1.,1.),(1.,1.),(1.,1.),(1.,1.),(1.,1.),(1.,
1.),(1.,1.),(1.,1.),(1.,1.),(1.,1.),(1.,1.),(1.,1.),(1.,1.),(1.,1.),(1.,
1.),(1.,1.),(1.,1.),(1.,1.),(1.,1.),(1.,1.),(1.,1.),(1.,1.),(1.,1.),(1.,
1.),(1.,1.),(1.,1.),(1.,1.),(1.,1.),(1.,1.),(1.,1.),(1.,1.),(1.,1.),(1.,
1.),(1.,1.),(1.,1.),(1.,1.),(1.,1.),(1.,1.),(1.,1.),(1.,1.),(1.,1.),(1.,
1.),(1.,1.),(1.,1.),(1.,1.),(1.,1.),(1.,1.),(1.,1.),(1.,1.),(1.,1.),(1.,
1.),(1.,1.),(1.,1.),(1.,1.),(1.,1.),(1.,1.),(1.,1.),(1.,1.),(1.,1.),(1.,
1.),(1.,1.),(1.,1.),(1.,1.),(1.,1.),(1.,1.),(1.,1.),(1.,1.),(1.,1.),(1.,
1.),(1.,1.),(1.,1.),(1.,1.),(1.,1.),(1.,1.),(1.,1.),(1.,1.),(1.,1.),(1.,
1.),(1.,1.),(1.,1.),(1.,1.),(1.,1.),(1.,1.),(1.,1.),(1.,1.),(1.,1.),(1.,
1.),(1.,1.),(1.,1.),(1.,1.),(1.,1.),(1.,1.),(1.,1.),(1.,1.),(1.,1.),(1.,
1.),(1.,1.),(1.,1.),(1.,1.),(1.,1.),(1.,1.),(1.,1.),(1.,1.),(1.,1.),(1.,
1.),(1.,1.)))
REPRESENTATION_ITEM('')
SURFACE()
);
#889=(
BOUNDED_SURFACE()
B_SPLINE_SURFACE(5,1,((#57998,#57999),(#58000,#58001),(#58002,#58003),(#58004,
#58005),(#58006,#58007),(#58008,#58009),(#58010,#58011),(#58012,#58013),
(#58014,#58015),(#58016,#58017),(#58018,#58019),(#58020,#58021),(#58022,
#58023),(#58024,#58025),(#58026,#58027),(#58028,#58029),(#58030,#58031),
(#58032,#58033),(#58034,#58035),(#58036,#58037),(#58038,#58039),(#58040,
#58041),(#58042,#58043),(#58044,#58045),(#58046,#58047),(#58048,#58049),
(#58050,#58051),(#58052,#58053),(#58054,#58055),(#58056,#58057),(#58058,
#58059),(#58060,#58061),(#58062,#58063),(#58064,#58065),(#58066,#58067),
(#58068,#58069),(#58070,#58071),(#58072,#58073),(#58074,#58075),(#58076,
#58077),(#58078,#58079),(#58080,#58081),(#58082,#58083),(#58084,#58085),
(#58086,#58087),(#58088,#58089),(#58090,#58091),(#58092,#58093),(#58094,
#58095),(#58096,#58097),(#58098,#58099),(#58100,#58101),(#58102,#58103),
(#58104,#58105),(#58106,#58107),(#58108,#58109),(#58110,#58111),(#58112,
#58113),(#58114,#58115),(#58116,#58117),(#58118,#58119),(#58120,#58121),
(#58122,#58123),(#58124,#58125),(#58126,#58127),(#58128,#58129),(#58130,
#58131),(#58132,#58133),(#58134,#58135),(#58136,#58137),(#58138,#58139),
(#58140,#58141),(#58142,#58143),(#58144,#58145),(#58146,#58147),(#58148,
#58149),(#58150,#58151),(#58152,#58153),(#58154,#58155),(#58156,#58157),
(#58158,#58159),(#58160,#58161),(#58162,#58163),(#58164,#58165),(#58166,
#58167),(#58168,#58169),(#58170,#58171),(#58172,#58173),(#58174,#58175),
(#58176,#58177),(#58178,#58179),(#58180,#58181),(#58182,#58183),(#58184,
#58185),(#58186,#58187),(#58188,#58189),(#58190,#58191),(#58192,#58193),
(#58194,#58195),(#58196,#58197),(#58198,#58199),(#58200,#58201),(#58202,
#58203),(#58204,#58205),(#58206,#58207),(#58208,#58209),(#58210,#58211),
(#58212,#58213),(#58214,#58215),(#58216,#58217),(#58218,#58219),(#58220,
#58221),(#58222,#58223),(#58224,#58225),(#58226,#58227),(#58228,#58229),
(#58230,#58231),(#58232,#58233),(#58234,#58235),(#58236,#58237),(#58238,
#58239),(#58240,#58241),(#58242,#58243),(#58244,#58245),(#58246,#58247),
(#58248,#58249),(#58250,#58251),(#58252,#58253),(#58254,#58255),(#58256,
#58257),(#58258,#58259),(#58260,#58261),(#58262,#58263),(#58264,#58265),
(#58266,#58267),(#58268,#58269),(#58270,#58271),(#58272,#58273),(#58274,
#58275),(#58276,#58277),(#58278,#58279),(#58280,#58281),(#58282,#58283),
(#58284,#58285),(#58286,#58287),(#58288,#58289),(#58290,#58291),(#58292,
#58293),(#58294,#58295),(#58296,#58297),(#58298,#58299),(#58300,#58301),
(#58302,#58303),(#58304,#58305),(#58306,#58307),(#58308,#58309),(#58310,
#58311),(#58312,#58313),(#58314,#58315),(#58316,#58317),(#58318,#58319),
(#58320,#58321),(#58322,#58323),(#58324,#58325),(#58326,#58327),(#58328,
#58329),(#58330,#58331),(#58332,#58333),(#58334,#58335),(#58336,#58337),
(#58338,#58339),(#58340,#58341),(#58342,#58343),(#58344,#58345),(#58346,
#58347),(#58348,#58349),(#58350,#58351),(#58352,#58353),(#58354,#58355),
(#58356,#58357),(#58358,#58359),(#58360,#58361),(#58362,#58363),(#58364,
#58365),(#58366,#58367),(#58368,#58369),(#58370,#58371),(#58372,#58373),
(#58374,#58375),(#58376,#58377),(#58378,#58379),(#58380,#58381),(#58382,
#58383),(#58384,#58385),(#58386,#58387),(#58388,#58389),(#58390,#58391),
(#58392,#58393),(#58394,#58395),(#58396,#58397),(#58398,#58399),(#58400,
#58401),(#58402,#58403),(#58404,#58405),(#58406,#58407)),.UNSPECIFIED.,
 .F.,.F.,.F.)
B_SPLINE_SURFACE_WITH_KNOTS((6,1,1,1,1,1,1,1,1,1,1,1,1,1,1,1,1,1,1,1,1,
1,1,1,1,1,1,1,1,1,1,1,1,1,1,1,1,1,1,1,1,1,1,1,1,1,1,1,1,1,1,1,1,1,1,1,1,
1,1,1,1,1,1,1,1,1,1,1,1,1,1,1,1,1,1,1,1,1,1,1,1,1,1,1,1,1,1,1,1,1,1,1,1,
1,1,1,1,1,1,1,1,1,1,1,1,1,1,1,1,1,1,1,1,1,1,1,1,1,1,1,1,1,1,1,1,1,1,1,1,
1,1,1,1,1,1,1,1,1,1,1,1,1,1,1,1,1,1,1,1,1,1,1,1,1,1,1,1,1,1,1,1,1,1,1,1,
1,1,1,1,1,1,1,1,1,1,1,1,1,1,1,1,1,1,1,1,1,1,1,1,1,1,1,1,1,1,1,1,1,1,1,6),
(2,2),(0.,0.005,0.01,0.015,0.02,0.025,0.03,0.035,0.04,0.045,0.05,0.055,
0.06,0.065,0.07,0.075,0.08,0.085,0.09,0.095,0.1,0.105,0.11,0.115,0.12,0.125,
0.13,0.135,0.14,0.145,0.15,0.155,0.16,0.165,0.17,0.175,0.18,0.185,0.19,
0.195,0.2,0.205,0.21,0.215,0.22,0.225,0.23,0.235,0.24,0.245,0.25,0.255,
0.26,0.265,0.27,0.275,0.28,0.285,0.29,0.295,0.3,0.305,0.31,0.315,0.32,0.325,
0.33,0.335,0.34,0.345,0.35,0.355,0.36,0.365,0.37,0.375,0.38,0.385,0.39,
0.395,0.4,0.405,0.41,0.415,0.42,0.425,0.43,0.435,0.44,0.445,0.45,0.455,
0.46,0.465,0.47,0.475,0.48,0.485,0.49,0.495,0.5,0.505,0.51,0.515,0.52,0.525,
0.53,0.535,0.54,0.545,0.55,0.555,0.56,0.565,0.57,0.575,0.58,0.585,0.59,
0.595,0.6,0.605,0.61,0.615,0.62,0.625,0.63,0.635,0.64,0.645,0.65,0.655,
0.66,0.665,0.67,0.675,0.68,0.685,0.690000000000001,0.695000000000001,0.700000000000001,
0.705000000000001,0.710000000000001,0.715000000000001,0.720000000000001,
0.725000000000001,0.730000000000001,0.735000000000001,0.740000000000001,
0.745000000000001,0.750000000000001,0.755000000000001,0.760000000000001,
0.765000000000001,0.770000000000001,0.775000000000001,0.780000000000001,
0.785000000000001,0.790000000000001,0.795000000000001,0.800000000000001,
0.805000000000001,0.810000000000001,0.815000000000001,0.820000000000001,
0.825000000000001,0.830000000000001,0.835000000000001,0.840000000000001,
0.845000000000001,0.850000000000001,0.855000000000001,0.860000000000001,
0.865000000000001,0.870000000000001,0.875000000000001,0.880000000000001,
0.885000000000001,0.890000000000001,0.895000000000001,0.900000000000001,
0.905000000000001,0.910000000000001,0.915000000000001,0.920000000000001,
0.925000000000001,0.930000000000001,0.935000000000001,0.940000000000001,
0.945000000000001,0.950000000000001,0.955000000000001,0.960000000000001,
0.965000000000001,0.970000000000001,0.975000000000001,0.980000000000001,
0.985000000000001,0.990000000000001,0.995000000000001,1.),(0.,1.2),
 .UNSPECIFIED.)
GEOMETRIC_REPRESENTATION_ITEM()
RATIONAL_B_SPLINE_SURFACE(((1.,1.),(1.,1.),(1.,1.),(1.,1.),(1.,1.),(1.,
1.),(1.,1.),(1.,1.),(1.,1.),(1.,1.),(1.,1.),(1.,1.),(1.,1.),(1.,1.),(1.,
1.),(1.,1.),(1.,1.),(1.,1.),(1.,1.),(1.,1.),(1.,1.),(1.,1.),(1.,1.),(1.,
1.),(1.,1.),(1.,1.),(1.,1.),(1.,1.),(1.,1.),(1.,1.),(1.,1.),(1.,1.),(1.,
1.),(1.,1.),(1.,1.),(1.,1.),(1.,1.),(1.,1.),(1.,1.),(1.,1.),(1.,1.),(1.,
1.),(1.,1.),(1.,1.),(1.,1.),(1.,1.),(1.,1.),(1.,1.),(1.,1.),(1.,1.),(1.,
1.),(1.,1.),(1.,1.),(1.,1.),(1.,1.),(1.,1.),(1.,1.),(1.,1.),(1.,1.),(1.,
1.),(1.,1.),(1.,1.),(1.,1.),(1.,1.),(1.,1.),(1.,1.),(1.,1.),(1.,1.),(1.,
1.),(1.,1.),(1.,1.),(1.,1.),(1.,1.),(1.,1.),(1.,1.),(1.,1.),(1.,1.),(1.,
1.),(1.,1.),(1.,1.),(1.,1.),(1.,1.),(1.,1.),(1.,1.),(1.,1.),(1.,1.),(1.,
1.),(1.,1.),(1.,1.),(1.,1.),(1.,1.),(1.,1.),(1.,1.),(1.,1.),(1.,1.),(1.,
1.),(1.,1.),(1.,1.),(1.,1.),(1.,1.),(1.,1.),(1.,1.),(1.,1.),(1.,1.),(1.,
1.),(1.,1.),(1.,1.),(1.,1.),(1.,1.),(1.,1.),(1.,1.),(1.,1.),(1.,1.),(1.,
1.),(1.,1.),(1.,1.),(1.,1.),(1.,1.),(1.,1.),(1.,1.),(1.,1.),(1.,1.),(1.,
1.),(1.,1.),(1.,1.),(1.,1.),(1.,1.),(1.,1.),(1.,1.),(1.,1.),(1.,1.),(1.,
1.),(1.,1.),(1.,1.),(1.,1.),(1.,1.),(1.,1.),(1.,1.),(1.,1.),(1.,1.),(1.,
1.),(1.,1.),(1.,1.),(1.,1.),(1.,1.),(1.,1.),(1.,1.),(1.,1.),(1.,1.),(1.,
1.),(1.,1.),(1.,1.),(1.,1.),(1.,1.),(1.,1.),(1.,1.),(1.,1.),(1.,1.),(1.,
1.),(1.,1.),(1.,1.),(1.,1.),(1.,1.),(1.,1.),(1.,1.),(1.,1.),(1.,1.),(1.,
1.),(1.,1.),(1.,1.),(1.,1.),(1.,1.),(1.,1.),(1.,1.),(1.,1.),(1.,1.),(1.,
1.),(1.,1.),(1.,1.),(1.,1.),(1.,1.),(1.,1.),(1.,1.),(1.,1.),(1.,1.),(1.,
1.),(1.,1.),(1.,1.),(1.,1.),(1.,1.),(1.,1.),(1.,1.),(1.,1.),(1.,1.),(1.,
1.),(1.,1.),(1.,1.),(1.,1.),(1.,1.),(1.,1.),(1.,1.),(1.,1.),(1.,1.),(1.,
1.),(1.,1.)))
REPRESENTATION_ITEM('')
SURFACE()
);
#890=(
BOUNDED_SURFACE()
B_SPLINE_SURFACE(5,1,((#58894,#58895),(#58896,#58897),(#58898,#58899),(#58900,
#58901),(#58902,#58903),(#58904,#58905),(#58906,#58907),(#58908,#58909),
(#58910,#58911),(#58912,#58913),(#58914,#58915),(#58916,#58917),(#58918,
#58919),(#58920,#58921),(#58922,#58923),(#58924,#58925),(#58926,#58927),
(#58928,#58929),(#58930,#58931),(#58932,#58933),(#58934,#58935),(#58936,
#58937),(#58938,#58939),(#58940,#58941),(#58942,#58943),(#58944,#58945),
(#58946,#58947),(#58948,#58949),(#58950,#58951),(#58952,#58953),(#58954,
#58955),(#58956,#58957),(#58958,#58959),(#58960,#58961),(#58962,#58963),
(#58964,#58965),(#58966,#58967),(#58968,#58969),(#58970,#58971),(#58972,
#58973),(#58974,#58975),(#58976,#58977),(#58978,#58979),(#58980,#58981),
(#58982,#58983),(#58984,#58985),(#58986,#58987),(#58988,#58989),(#58990,
#58991),(#58992,#58993),(#58994,#58995),(#58996,#58997),(#58998,#58999),
(#59000,#59001),(#59002,#59003),(#59004,#59005),(#59006,#59007),(#59008,
#59009),(#59010,#59011),(#59012,#59013),(#59014,#59015),(#59016,#59017),
(#59018,#59019),(#59020,#59021),(#59022,#59023),(#59024,#59025),(#59026,
#59027),(#59028,#59029),(#59030,#59031),(#59032,#59033),(#59034,#59035),
(#59036,#59037),(#59038,#59039),(#59040,#59041),(#59042,#59043),(#59044,
#59045),(#59046,#59047),(#59048,#59049),(#59050,#59051),(#59052,#59053),
(#59054,#59055),(#59056,#59057),(#59058,#59059),(#59060,#59061),(#59062,
#59063),(#59064,#59065),(#59066,#59067),(#59068,#59069),(#59070,#59071),
(#59072,#59073),(#59074,#59075),(#59076,#59077),(#59078,#59079),(#59080,
#59081),(#59082,#59083),(#59084,#59085),(#59086,#59087),(#59088,#59089),
(#59090,#59091),(#59092,#59093),(#59094,#59095),(#59096,#59097),(#59098,
#59099),(#59100,#59101),(#59102,#59103),(#59104,#59105),(#59106,#59107),
(#59108,#59109),(#59110,#59111),(#59112,#59113),(#59114,#59115),(#59116,
#59117),(#59118,#59119),(#59120,#59121),(#59122,#59123),(#59124,#59125),
(#59126,#59127),(#59128,#59129),(#59130,#59131),(#59132,#59133),(#59134,
#59135),(#59136,#59137),(#59138,#59139),(#59140,#59141),(#59142,#59143),
(#59144,#59145),(#59146,#59147),(#59148,#59149),(#59150,#59151),(#59152,
#59153),(#59154,#59155),(#59156,#59157),(#59158,#59159),(#59160,#59161),
(#59162,#59163),(#59164,#59165),(#59166,#59167),(#59168,#59169),(#59170,
#59171),(#59172,#59173),(#59174,#59175),(#59176,#59177),(#59178,#59179),
(#59180,#59181),(#59182,#59183),(#59184,#59185),(#59186,#59187),(#59188,
#59189),(#59190,#59191),(#59192,#59193),(#59194,#59195),(#59196,#59197),
(#59198,#59199),(#59200,#59201),(#59202,#59203),(#59204,#59205),(#59206,
#59207),(#59208,#59209),(#59210,#59211),(#59212,#59213),(#59214,#59215),
(#59216,#59217),(#59218,#59219),(#59220,#59221),(#59222,#59223),(#59224,
#59225),(#59226,#59227),(#59228,#59229),(#59230,#59231),(#59232,#59233),
(#59234,#59235),(#59236,#59237),(#59238,#59239),(#59240,#59241),(#59242,
#59243),(#59244,#59245),(#59246,#59247),(#59248,#59249),(#59250,#59251),
(#59252,#59253),(#59254,#59255),(#59256,#59257),(#59258,#59259),(#59260,
#59261),(#59262,#59263),(#59264,#59265),(#59266,#59267),(#59268,#59269),
(#59270,#59271),(#59272,#59273),(#59274,#59275),(#59276,#59277),(#59278,
#59279),(#59280,#59281),(#59282,#59283),(#59284,#59285),(#59286,#59287),
(#59288,#59289),(#59290,#59291),(#59292,#59293),(#59294,#59295),(#59296,
#59297),(#59298,#59299),(#59300,#59301),(#59302,#59303)),.UNSPECIFIED.,
 .F.,.F.,.F.)
B_SPLINE_SURFACE_WITH_KNOTS((6,1,1,1,1,1,1,1,1,1,1,1,1,1,1,1,1,1,1,1,1,
1,1,1,1,1,1,1,1,1,1,1,1,1,1,1,1,1,1,1,1,1,1,1,1,1,1,1,1,1,1,1,1,1,1,1,1,
1,1,1,1,1,1,1,1,1,1,1,1,1,1,1,1,1,1,1,1,1,1,1,1,1,1,1,1,1,1,1,1,1,1,1,1,
1,1,1,1,1,1,1,1,1,1,1,1,1,1,1,1,1,1,1,1,1,1,1,1,1,1,1,1,1,1,1,1,1,1,1,1,
1,1,1,1,1,1,1,1,1,1,1,1,1,1,1,1,1,1,1,1,1,1,1,1,1,1,1,1,1,1,1,1,1,1,1,1,
1,1,1,1,1,1,1,1,1,1,1,1,1,1,1,1,1,1,1,1,1,1,1,1,1,1,1,1,1,1,1,1,1,1,1,6),
(2,2),(0.,0.005,0.01,0.015,0.02,0.025,0.03,0.035,0.04,0.045,0.05,0.055,
0.06,0.065,0.07,0.075,0.08,0.085,0.09,0.095,0.1,0.105,0.11,0.115,0.12,0.125,
0.13,0.135,0.14,0.145,0.15,0.155,0.16,0.165,0.17,0.175,0.18,0.185,0.19,
0.195,0.2,0.205,0.21,0.215,0.22,0.225,0.23,0.235,0.24,0.245,0.25,0.255,
0.26,0.265,0.27,0.275,0.28,0.285,0.29,0.295,0.3,0.305,0.31,0.315,0.32,0.325,
0.33,0.335,0.34,0.345,0.35,0.355,0.36,0.365,0.37,0.375,0.38,0.385,0.39,
0.395,0.4,0.405,0.41,0.415,0.42,0.425,0.43,0.435,0.44,0.445,0.45,0.455,
0.46,0.465,0.47,0.475,0.48,0.485,0.49,0.495,0.5,0.505,0.51,0.515,0.52,0.525,
0.53,0.535,0.54,0.545,0.55,0.555,0.56,0.565,0.57,0.575,0.58,0.585,0.59,
0.595,0.6,0.605,0.61,0.615,0.62,0.625,0.63,0.635,0.64,0.645,0.65,0.655,
0.66,0.665,0.67,0.675,0.68,0.685,0.690000000000001,0.695000000000001,0.700000000000001,
0.705000000000001,0.710000000000001,0.715000000000001,0.720000000000001,
0.725000000000001,0.730000000000001,0.735000000000001,0.740000000000001,
0.745000000000001,0.750000000000001,0.755000000000001,0.760000000000001,
0.765000000000001,0.770000000000001,0.775000000000001,0.780000000000001,
0.785000000000001,0.790000000000001,0.795000000000001,0.800000000000001,
0.805000000000001,0.810000000000001,0.815000000000001,0.820000000000001,
0.825000000000001,0.830000000000001,0.835000000000001,0.840000000000001,
0.845000000000001,0.850000000000001,0.855000000000001,0.860000000000001,
0.865000000000001,0.870000000000001,0.875000000000001,0.880000000000001,
0.885000000000001,0.890000000000001,0.895000000000001,0.900000000000001,
0.905000000000001,0.910000000000001,0.915000000000001,0.920000000000001,
0.925000000000001,0.930000000000001,0.935000000000001,0.940000000000001,
0.945000000000001,0.950000000000001,0.955000000000001,0.960000000000001,
0.965000000000001,0.970000000000001,0.975000000000001,0.980000000000001,
0.985000000000001,0.990000000000001,0.995000000000001,1.),(0.,1.2),
 .UNSPECIFIED.)
GEOMETRIC_REPRESENTATION_ITEM()
RATIONAL_B_SPLINE_SURFACE(((1.,1.),(1.,1.),(1.,1.),(1.,1.),(1.,1.),(1.,
1.),(1.,1.),(1.,1.),(1.,1.),(1.,1.),(1.,1.),(1.,1.),(1.,1.),(1.,1.),(1.,
1.),(1.,1.),(1.,1.),(1.,1.),(1.,1.),(1.,1.),(1.,1.),(1.,1.),(1.,1.),(1.,
1.),(1.,1.),(1.,1.),(1.,1.),(1.,1.),(1.,1.),(1.,1.),(1.,1.),(1.,1.),(1.,
1.),(1.,1.),(1.,1.),(1.,1.),(1.,1.),(1.,1.),(1.,1.),(1.,1.),(1.,1.),(1.,
1.),(1.,1.),(1.,1.),(1.,1.),(1.,1.),(1.,1.),(1.,1.),(1.,1.),(1.,1.),(1.,
1.),(1.,1.),(1.,1.),(1.,1.),(1.,1.),(1.,1.),(1.,1.),(1.,1.),(1.,1.),(1.,
1.),(1.,1.),(1.,1.),(1.,1.),(1.,1.),(1.,1.),(1.,1.),(1.,1.),(1.,1.),(1.,
1.),(1.,1.),(1.,1.),(1.,1.),(1.,1.),(1.,1.),(1.,1.),(1.,1.),(1.,1.),(1.,
1.),(1.,1.),(1.,1.),(1.,1.),(1.,1.),(1.,1.),(1.,1.),(1.,1.),(1.,1.),(1.,
1.),(1.,1.),(1.,1.),(1.,1.),(1.,1.),(1.,1.),(1.,1.),(1.,1.),(1.,1.),(1.,
1.),(1.,1.),(1.,1.),(1.,1.),(1.,1.),(1.,1.),(1.,1.),(1.,1.),(1.,1.),(1.,
1.),(1.,1.),(1.,1.),(1.,1.),(1.,1.),(1.,1.),(1.,1.),(1.,1.),(1.,1.),(1.,
1.),(1.,1.),(1.,1.),(1.,1.),(1.,1.),(1.,1.),(1.,1.),(1.,1.),(1.,1.),(1.,
1.),(1.,1.),(1.,1.),(1.,1.),(1.,1.),(1.,1.),(1.,1.),(1.,1.),(1.,1.),(1.,
1.),(1.,1.),(1.,1.),(1.,1.),(1.,1.),(1.,1.),(1.,1.),(1.,1.),(1.,1.),(1.,
1.),(1.,1.),(1.,1.),(1.,1.),(1.,1.),(1.,1.),(1.,1.),(1.,1.),(1.,1.),(1.,
1.),(1.,1.),(1.,1.),(1.,1.),(1.,1.),(1.,1.),(1.,1.),(1.,1.),(1.,1.),(1.,
1.),(1.,1.),(1.,1.),(1.,1.),(1.,1.),(1.,1.),(1.,1.),(1.,1.),(1.,1.),(1.,
1.),(1.,1.),(1.,1.),(1.,1.),(1.,1.),(1.,1.),(1.,1.),(1.,1.),(1.,1.),(1.,
1.),(1.,1.),(1.,1.),(1.,1.),(1.,1.),(1.,1.),(1.,1.),(1.,1.),(1.,1.),(1.,
1.),(1.,1.),(1.,1.),(1.,1.),(1.,1.),(1.,1.),(1.,1.),(1.,1.),(1.,1.),(1.,
1.),(1.,1.),(1.,1.),(1.,1.),(1.,1.),(1.,1.),(1.,1.),(1.,1.),(1.,1.),(1.,
1.),(1.,1.)))
REPRESENTATION_ITEM('')
SURFACE()
);
#891=(
BOUNDED_SURFACE()
B_SPLINE_SURFACE(5,1,((#59790,#59791),(#59792,#59793),(#59794,#59795),(#59796,
#59797),(#59798,#59799),(#59800,#59801),(#59802,#59803),(#59804,#59805),
(#59806,#59807),(#59808,#59809),(#59810,#59811),(#59812,#59813),(#59814,
#59815),(#59816,#59817),(#59818,#59819),(#59820,#59821),(#59822,#59823),
(#59824,#59825),(#59826,#59827),(#59828,#59829),(#59830,#59831),(#59832,
#59833),(#59834,#59835),(#59836,#59837),(#59838,#59839),(#59840,#59841),
(#59842,#59843),(#59844,#59845),(#59846,#59847),(#59848,#59849),(#59850,
#59851),(#59852,#59853),(#59854,#59855),(#59856,#59857),(#59858,#59859),
(#59860,#59861),(#59862,#59863),(#59864,#59865),(#59866,#59867),(#59868,
#59869),(#59870,#59871),(#59872,#59873),(#59874,#59875),(#59876,#59877),
(#59878,#59879),(#59880,#59881),(#59882,#59883),(#59884,#59885),(#59886,
#59887),(#59888,#59889),(#59890,#59891),(#59892,#59893),(#59894,#59895),
(#59896,#59897),(#59898,#59899),(#59900,#59901),(#59902,#59903),(#59904,
#59905),(#59906,#59907),(#59908,#59909),(#59910,#59911),(#59912,#59913),
(#59914,#59915),(#59916,#59917),(#59918,#59919),(#59920,#59921),(#59922,
#59923),(#59924,#59925),(#59926,#59927),(#59928,#59929),(#59930,#59931),
(#59932,#59933),(#59934,#59935),(#59936,#59937),(#59938,#59939),(#59940,
#59941),(#59942,#59943),(#59944,#59945),(#59946,#59947),(#59948,#59949),
(#59950,#59951),(#59952,#59953),(#59954,#59955),(#59956,#59957),(#59958,
#59959),(#59960,#59961),(#59962,#59963),(#59964,#59965),(#59966,#59967),
(#59968,#59969),(#59970,#59971),(#59972,#59973),(#59974,#59975),(#59976,
#59977),(#59978,#59979),(#59980,#59981),(#59982,#59983),(#59984,#59985),
(#59986,#59987),(#59988,#59989),(#59990,#59991),(#59992,#59993),(#59994,
#59995),(#59996,#59997),(#59998,#59999),(#60000,#60001),(#60002,#60003),
(#60004,#60005),(#60006,#60007),(#60008,#60009),(#60010,#60011),(#60012,
#60013),(#60014,#60015),(#60016,#60017),(#60018,#60019),(#60020,#60021),
(#60022,#60023),(#60024,#60025),(#60026,#60027),(#60028,#60029),(#60030,
#60031),(#60032,#60033),(#60034,#60035),(#60036,#60037),(#60038,#60039),
(#60040,#60041),(#60042,#60043),(#60044,#60045),(#60046,#60047),(#60048,
#60049),(#60050,#60051),(#60052,#60053),(#60054,#60055),(#60056,#60057),
(#60058,#60059),(#60060,#60061),(#60062,#60063),(#60064,#60065),(#60066,
#60067),(#60068,#60069),(#60070,#60071),(#60072,#60073),(#60074,#60075),
(#60076,#60077),(#60078,#60079),(#60080,#60081),(#60082,#60083),(#60084,
#60085),(#60086,#60087),(#60088,#60089),(#60090,#60091),(#60092,#60093),
(#60094,#60095),(#60096,#60097),(#60098,#60099),(#60100,#60101),(#60102,
#60103),(#60104,#60105),(#60106,#60107),(#60108,#60109),(#60110,#60111),
(#60112,#60113),(#60114,#60115),(#60116,#60117),(#60118,#60119),(#60120,
#60121),(#60122,#60123),(#60124,#60125),(#60126,#60127),(#60128,#60129),
(#60130,#60131),(#60132,#60133),(#60134,#60135),(#60136,#60137),(#60138,
#60139),(#60140,#60141),(#60142,#60143),(#60144,#60145),(#60146,#60147),
(#60148,#60149),(#60150,#60151),(#60152,#60153),(#60154,#60155),(#60156,
#60157),(#60158,#60159),(#60160,#60161),(#60162,#60163),(#60164,#60165),
(#60166,#60167),(#60168,#60169),(#60170,#60171),(#60172,#60173),(#60174,
#60175),(#60176,#60177),(#60178,#60179),(#60180,#60181),(#60182,#60183),
(#60184,#60185),(#60186,#60187),(#60188,#60189),(#60190,#60191),(#60192,
#60193),(#60194,#60195),(#60196,#60197),(#60198,#60199)),.UNSPECIFIED.,
 .F.,.F.,.F.)
B_SPLINE_SURFACE_WITH_KNOTS((6,1,1,1,1,1,1,1,1,1,1,1,1,1,1,1,1,1,1,1,1,
1,1,1,1,1,1,1,1,1,1,1,1,1,1,1,1,1,1,1,1,1,1,1,1,1,1,1,1,1,1,1,1,1,1,1,1,
1,1,1,1,1,1,1,1,1,1,1,1,1,1,1,1,1,1,1,1,1,1,1,1,1,1,1,1,1,1,1,1,1,1,1,1,
1,1,1,1,1,1,1,1,1,1,1,1,1,1,1,1,1,1,1,1,1,1,1,1,1,1,1,1,1,1,1,1,1,1,1,1,
1,1,1,1,1,1,1,1,1,1,1,1,1,1,1,1,1,1,1,1,1,1,1,1,1,1,1,1,1,1,1,1,1,1,1,1,
1,1,1,1,1,1,1,1,1,1,1,1,1,1,1,1,1,1,1,1,1,1,1,1,1,1,1,1,1,1,1,1,1,1,1,6),
(2,2),(0.,0.005,0.01,0.015,0.02,0.025,0.03,0.035,0.04,0.045,0.05,0.055,
0.06,0.065,0.07,0.075,0.08,0.085,0.09,0.095,0.1,0.105,0.11,0.115,0.12,0.125,
0.13,0.135,0.14,0.145,0.15,0.155,0.16,0.165,0.17,0.175,0.18,0.185,0.19,
0.195,0.2,0.205,0.21,0.215,0.22,0.225,0.23,0.235,0.24,0.245,0.25,0.255,
0.26,0.265,0.27,0.275,0.28,0.285,0.29,0.295,0.3,0.305,0.31,0.315,0.32,0.325,
0.33,0.335,0.34,0.345,0.35,0.355,0.36,0.365,0.37,0.375,0.38,0.385,0.39,
0.395,0.4,0.405,0.41,0.415,0.42,0.425,0.43,0.435,0.44,0.445,0.45,0.455,
0.46,0.465,0.47,0.475,0.48,0.485,0.49,0.495,0.5,0.505,0.51,0.515,0.52,0.525,
0.53,0.535,0.54,0.545,0.55,0.555,0.56,0.565,0.57,0.575,0.58,0.585,0.59,
0.595,0.6,0.605,0.61,0.615,0.62,0.625,0.63,0.635,0.64,0.645,0.65,0.655,
0.66,0.665,0.67,0.675,0.68,0.685,0.690000000000001,0.695000000000001,0.700000000000001,
0.705000000000001,0.710000000000001,0.715000000000001,0.720000000000001,
0.725000000000001,0.730000000000001,0.735000000000001,0.740000000000001,
0.745000000000001,0.750000000000001,0.755000000000001,0.760000000000001,
0.765000000000001,0.770000000000001,0.775000000000001,0.780000000000001,
0.785000000000001,0.790000000000001,0.795000000000001,0.800000000000001,
0.805000000000001,0.810000000000001,0.815000000000001,0.820000000000001,
0.825000000000001,0.830000000000001,0.835000000000001,0.840000000000001,
0.845000000000001,0.850000000000001,0.855000000000001,0.860000000000001,
0.865000000000001,0.870000000000001,0.875000000000001,0.880000000000001,
0.885000000000001,0.890000000000001,0.895000000000001,0.900000000000001,
0.905000000000001,0.910000000000001,0.915000000000001,0.920000000000001,
0.925000000000001,0.930000000000001,0.935000000000001,0.940000000000001,
0.945000000000001,0.950000000000001,0.955000000000001,0.960000000000001,
0.965000000000001,0.970000000000001,0.975000000000001,0.980000000000001,
0.985000000000001,0.990000000000001,0.995000000000001,1.),(0.,1.2),
 .UNSPECIFIED.)
GEOMETRIC_REPRESENTATION_ITEM()
RATIONAL_B_SPLINE_SURFACE(((1.,1.),(1.,1.),(1.,1.),(1.,1.),(1.,1.),(1.,
1.),(1.,1.),(1.,1.),(1.,1.),(1.,1.),(1.,1.),(1.,1.),(1.,1.),(1.,1.),(1.,
1.),(1.,1.),(1.,1.),(1.,1.),(1.,1.),(1.,1.),(1.,1.),(1.,1.),(1.,1.),(1.,
1.),(1.,1.),(1.,1.),(1.,1.),(1.,1.),(1.,1.),(1.,1.),(1.,1.),(1.,1.),(1.,
1.),(1.,1.),(1.,1.),(1.,1.),(1.,1.),(1.,1.),(1.,1.),(1.,1.),(1.,1.),(1.,
1.),(1.,1.),(1.,1.),(1.,1.),(1.,1.),(1.,1.),(1.,1.),(1.,1.),(1.,1.),(1.,
1.),(1.,1.),(1.,1.),(1.,1.),(1.,1.),(1.,1.),(1.,1.),(1.,1.),(1.,1.),(1.,
1.),(1.,1.),(1.,1.),(1.,1.),(1.,1.),(1.,1.),(1.,1.),(1.,1.),(1.,1.),(1.,
1.),(1.,1.),(1.,1.),(1.,1.),(1.,1.),(1.,1.),(1.,1.),(1.,1.),(1.,1.),(1.,
1.),(1.,1.),(1.,1.),(1.,1.),(1.,1.),(1.,1.),(1.,1.),(1.,1.),(1.,1.),(1.,
1.),(1.,1.),(1.,1.),(1.,1.),(1.,1.),(1.,1.),(1.,1.),(1.,1.),(1.,1.),(1.,
1.),(1.,1.),(1.,1.),(1.,1.),(1.,1.),(1.,1.),(1.,1.),(1.,1.),(1.,1.),(1.,
1.),(1.,1.),(1.,1.),(1.,1.),(1.,1.),(1.,1.),(1.,1.),(1.,1.),(1.,1.),(1.,
1.),(1.,1.),(1.,1.),(1.,1.),(1.,1.),(1.,1.),(1.,1.),(1.,1.),(1.,1.),(1.,
1.),(1.,1.),(1.,1.),(1.,1.),(1.,1.),(1.,1.),(1.,1.),(1.,1.),(1.,1.),(1.,
1.),(1.,1.),(1.,1.),(1.,1.),(1.,1.),(1.,1.),(1.,1.),(1.,1.),(1.,1.),(1.,
1.),(1.,1.),(1.,1.),(1.,1.),(1.,1.),(1.,1.),(1.,1.),(1.,1.),(1.,1.),(1.,
1.),(1.,1.),(1.,1.),(1.,1.),(1.,1.),(1.,1.),(1.,1.),(1.,1.),(1.,1.),(1.,
1.),(1.,1.),(1.,1.),(1.,1.),(1.,1.),(1.,1.),(1.,1.),(1.,1.),(1.,1.),(1.,
1.),(1.,1.),(1.,1.),(1.,1.),(1.,1.),(1.,1.),(1.,1.),(1.,1.),(1.,1.),(1.,
1.),(1.,1.),(1.,1.),(1.,1.),(1.,1.),(1.,1.),(1.,1.),(1.,1.),(1.,1.),(1.,
1.),(1.,1.),(1.,1.),(1.,1.),(1.,1.),(1.,1.),(1.,1.),(1.,1.),(1.,1.),(1.,
1.),(1.,1.),(1.,1.),(1.,1.),(1.,1.),(1.,1.),(1.,1.),(1.,1.),(1.,1.),(1.,
1.),(1.,1.)))
REPRESENTATION_ITEM('')
SURFACE()
);
#892=(
BOUNDED_SURFACE()
B_SPLINE_SURFACE(5,1,((#60686,#60687),(#60688,#60689),(#60690,#60691),(#60692,
#60693),(#60694,#60695),(#60696,#60697),(#60698,#60699),(#60700,#60701),
(#60702,#60703),(#60704,#60705),(#60706,#60707),(#60708,#60709),(#60710,
#60711),(#60712,#60713),(#60714,#60715),(#60716,#60717),(#60718,#60719),
(#60720,#60721),(#60722,#60723),(#60724,#60725),(#60726,#60727),(#60728,
#60729),(#60730,#60731),(#60732,#60733),(#60734,#60735),(#60736,#60737),
(#60738,#60739),(#60740,#60741),(#60742,#60743),(#60744,#60745),(#60746,
#60747),(#60748,#60749),(#60750,#60751),(#60752,#60753),(#60754,#60755),
(#60756,#60757),(#60758,#60759),(#60760,#60761),(#60762,#60763),(#60764,
#60765),(#60766,#60767),(#60768,#60769),(#60770,#60771),(#60772,#60773),
(#60774,#60775),(#60776,#60777),(#60778,#60779),(#60780,#60781),(#60782,
#60783),(#60784,#60785),(#60786,#60787),(#60788,#60789),(#60790,#60791),
(#60792,#60793),(#60794,#60795),(#60796,#60797),(#60798,#60799),(#60800,
#60801),(#60802,#60803),(#60804,#60805),(#60806,#60807),(#60808,#60809),
(#60810,#60811),(#60812,#60813),(#60814,#60815),(#60816,#60817),(#60818,
#60819),(#60820,#60821),(#60822,#60823),(#60824,#60825),(#60826,#60827),
(#60828,#60829),(#60830,#60831),(#60832,#60833),(#60834,#60835),(#60836,
#60837),(#60838,#60839),(#60840,#60841),(#60842,#60843),(#60844,#60845),
(#60846,#60847),(#60848,#60849),(#60850,#60851),(#60852,#60853),(#60854,
#60855),(#60856,#60857),(#60858,#60859),(#60860,#60861),(#60862,#60863),
(#60864,#60865),(#60866,#60867),(#60868,#60869),(#60870,#60871),(#60872,
#60873),(#60874,#60875),(#60876,#60877),(#60878,#60879),(#60880,#60881),
(#60882,#60883),(#60884,#60885),(#60886,#60887),(#60888,#60889),(#60890,
#60891),(#60892,#60893),(#60894,#60895),(#60896,#60897),(#60898,#60899),
(#60900,#60901),(#60902,#60903),(#60904,#60905),(#60906,#60907),(#60908,
#60909),(#60910,#60911),(#60912,#60913),(#60914,#60915),(#60916,#60917),
(#60918,#60919),(#60920,#60921),(#60922,#60923),(#60924,#60925),(#60926,
#60927),(#60928,#60929),(#60930,#60931),(#60932,#60933),(#60934,#60935),
(#60936,#60937),(#60938,#60939),(#60940,#60941),(#60942,#60943),(#60944,
#60945),(#60946,#60947),(#60948,#60949),(#60950,#60951),(#60952,#60953),
(#60954,#60955),(#60956,#60957),(#60958,#60959),(#60960,#60961),(#60962,
#60963),(#60964,#60965),(#60966,#60967),(#60968,#60969),(#60970,#60971),
(#60972,#60973),(#60974,#60975),(#60976,#60977),(#60978,#60979),(#60980,
#60981),(#60982,#60983),(#60984,#60985),(#60986,#60987),(#60988,#60989),
(#60990,#60991),(#60992,#60993),(#60994,#60995),(#60996,#60997),(#60998,
#60999),(#61000,#61001),(#61002,#61003),(#61004,#61005),(#61006,#61007),
(#61008,#61009),(#61010,#61011),(#61012,#61013),(#61014,#61015),(#61016,
#61017),(#61018,#61019),(#61020,#61021),(#61022,#61023),(#61024,#61025),
(#61026,#61027),(#61028,#61029),(#61030,#61031),(#61032,#61033),(#61034,
#61035),(#61036,#61037),(#61038,#61039),(#61040,#61041),(#61042,#61043),
(#61044,#61045),(#61046,#61047),(#61048,#61049),(#61050,#61051),(#61052,
#61053),(#61054,#61055),(#61056,#61057),(#61058,#61059),(#61060,#61061),
(#61062,#61063),(#61064,#61065),(#61066,#61067),(#61068,#61069),(#61070,
#61071),(#61072,#61073),(#61074,#61075),(#61076,#61077),(#61078,#61079),
(#61080,#61081),(#61082,#61083),(#61084,#61085),(#61086,#61087),(#61088,
#61089),(#61090,#61091),(#61092,#61093),(#61094,#61095)),.UNSPECIFIED.,
 .F.,.F.,.F.)
B_SPLINE_SURFACE_WITH_KNOTS((6,1,1,1,1,1,1,1,1,1,1,1,1,1,1,1,1,1,1,1,1,
1,1,1,1,1,1,1,1,1,1,1,1,1,1,1,1,1,1,1,1,1,1,1,1,1,1,1,1,1,1,1,1,1,1,1,1,
1,1,1,1,1,1,1,1,1,1,1,1,1,1,1,1,1,1,1,1,1,1,1,1,1,1,1,1,1,1,1,1,1,1,1,1,
1,1,1,1,1,1,1,1,1,1,1,1,1,1,1,1,1,1,1,1,1,1,1,1,1,1,1,1,1,1,1,1,1,1,1,1,
1,1,1,1,1,1,1,1,1,1,1,1,1,1,1,1,1,1,1,1,1,1,1,1,1,1,1,1,1,1,1,1,1,1,1,1,
1,1,1,1,1,1,1,1,1,1,1,1,1,1,1,1,1,1,1,1,1,1,1,1,1,1,1,1,1,1,1,1,1,1,1,6),
(2,2),(0.,0.005,0.01,0.015,0.02,0.025,0.03,0.035,0.04,0.045,0.05,0.055,
0.06,0.065,0.07,0.075,0.08,0.085,0.09,0.095,0.1,0.105,0.11,0.115,0.12,0.125,
0.13,0.135,0.14,0.145,0.15,0.155,0.16,0.165,0.17,0.175,0.18,0.185,0.19,
0.195,0.2,0.205,0.21,0.215,0.22,0.225,0.23,0.235,0.24,0.245,0.25,0.255,
0.26,0.265,0.27,0.275,0.28,0.285,0.29,0.295,0.3,0.305,0.31,0.315,0.32,0.325,
0.33,0.335,0.34,0.345,0.35,0.355,0.36,0.365,0.37,0.375,0.38,0.385,0.39,
0.395,0.4,0.405,0.41,0.415,0.42,0.425,0.43,0.435,0.44,0.445,0.45,0.455,
0.46,0.465,0.47,0.475,0.48,0.485,0.49,0.495,0.5,0.505,0.51,0.515,0.52,0.525,
0.53,0.535,0.54,0.545,0.55,0.555,0.56,0.565,0.57,0.575,0.58,0.585,0.59,
0.595,0.6,0.605,0.61,0.615,0.62,0.625,0.63,0.635,0.64,0.645,0.65,0.655,
0.66,0.665,0.67,0.675,0.68,0.685,0.690000000000001,0.695000000000001,0.700000000000001,
0.705000000000001,0.710000000000001,0.715000000000001,0.720000000000001,
0.725000000000001,0.730000000000001,0.735000000000001,0.740000000000001,
0.745000000000001,0.750000000000001,0.755000000000001,0.760000000000001,
0.765000000000001,0.770000000000001,0.775000000000001,0.780000000000001,
0.785000000000001,0.790000000000001,0.795000000000001,0.800000000000001,
0.805000000000001,0.810000000000001,0.815000000000001,0.820000000000001,
0.825000000000001,0.830000000000001,0.835000000000001,0.840000000000001,
0.845000000000001,0.850000000000001,0.855000000000001,0.860000000000001,
0.865000000000001,0.870000000000001,0.875000000000001,0.880000000000001,
0.885000000000001,0.890000000000001,0.895000000000001,0.900000000000001,
0.905000000000001,0.910000000000001,0.915000000000001,0.920000000000001,
0.925000000000001,0.930000000000001,0.935000000000001,0.940000000000001,
0.945000000000001,0.950000000000001,0.955000000000001,0.960000000000001,
0.965000000000001,0.970000000000001,0.975000000000001,0.980000000000001,
0.985000000000001,0.990000000000001,0.995000000000001,1.),(0.,1.2),
 .UNSPECIFIED.)
GEOMETRIC_REPRESENTATION_ITEM()
RATIONAL_B_SPLINE_SURFACE(((1.,1.),(1.,1.),(1.,1.),(1.,1.),(1.,1.),(1.,
1.),(1.,1.),(1.,1.),(1.,1.),(1.,1.),(1.,1.),(1.,1.),(1.,1.),(1.,1.),(1.,
1.),(1.,1.),(1.,1.),(1.,1.),(1.,1.),(1.,1.),(1.,1.),(1.,1.),(1.,1.),(1.,
1.),(1.,1.),(1.,1.),(1.,1.),(1.,1.),(1.,1.),(1.,1.),(1.,1.),(1.,1.),(1.,
1.),(1.,1.),(1.,1.),(1.,1.),(1.,1.),(1.,1.),(1.,1.),(1.,1.),(1.,1.),(1.,
1.),(1.,1.),(1.,1.),(1.,1.),(1.,1.),(1.,1.),(1.,1.),(1.,1.),(1.,1.),(1.,
1.),(1.,1.),(1.,1.),(1.,1.),(1.,1.),(1.,1.),(1.,1.),(1.,1.),(1.,1.),(1.,
1.),(1.,1.),(1.,1.),(1.,1.),(1.,1.),(1.,1.),(1.,1.),(1.,1.),(1.,1.),(1.,
1.),(1.,1.),(1.,1.),(1.,1.),(1.,1.),(1.,1.),(1.,1.),(1.,1.),(1.,1.),(1.,
1.),(1.,1.),(1.,1.),(1.,1.),(1.,1.),(1.,1.),(1.,1.),(1.,1.),(1.,1.),(1.,
1.),(1.,1.),(1.,1.),(1.,1.),(1.,1.),(1.,1.),(1.,1.),(1.,1.),(1.,1.),(1.,
1.),(1.,1.),(1.,1.),(1.,1.),(1.,1.),(1.,1.),(1.,1.),(1.,1.),(1.,1.),(1.,
1.),(1.,1.),(1.,1.),(1.,1.),(1.,1.),(1.,1.),(1.,1.),(1.,1.),(1.,1.),(1.,
1.),(1.,1.),(1.,1.),(1.,1.),(1.,1.),(1.,1.),(1.,1.),(1.,1.),(1.,1.),(1.,
1.),(1.,1.),(1.,1.),(1.,1.),(1.,1.),(1.,1.),(1.,1.),(1.,1.),(1.,1.),(1.,
1.),(1.,1.),(1.,1.),(1.,1.),(1.,1.),(1.,1.),(1.,1.),(1.,1.),(1.,1.),(1.,
1.),(1.,1.),(1.,1.),(1.,1.),(1.,1.),(1.,1.),(1.,1.),(1.,1.),(1.,1.),(1.,
1.),(1.,1.),(1.,1.),(1.,1.),(1.,1.),(1.,1.),(1.,1.),(1.,1.),(1.,1.),(1.,
1.),(1.,1.),(1.,1.),(1.,1.),(1.,1.),(1.,1.),(1.,1.),(1.,1.),(1.,1.),(1.,
1.),(1.,1.),(1.,1.),(1.,1.),(1.,1.),(1.,1.),(1.,1.),(1.,1.),(1.,1.),(1.,
1.),(1.,1.),(1.,1.),(1.,1.),(1.,1.),(1.,1.),(1.,1.),(1.,1.),(1.,1.),(1.,
1.),(1.,1.),(1.,1.),(1.,1.),(1.,1.),(1.,1.),(1.,1.),(1.,1.),(1.,1.),(1.,
1.),(1.,1.),(1.,1.),(1.,1.),(1.,1.),(1.,1.),(1.,1.),(1.,1.),(1.,1.),(1.,
1.),(1.,1.)))
REPRESENTATION_ITEM('')
SURFACE()
);
#893=(
BOUNDED_SURFACE()
B_SPLINE_SURFACE(5,1,((#61582,#61583),(#61584,#61585),(#61586,#61587),(#61588,
#61589),(#61590,#61591),(#61592,#61593),(#61594,#61595),(#61596,#61597),
(#61598,#61599),(#61600,#61601),(#61602,#61603),(#61604,#61605),(#61606,
#61607),(#61608,#61609),(#61610,#61611),(#61612,#61613),(#61614,#61615),
(#61616,#61617),(#61618,#61619),(#61620,#61621),(#61622,#61623),(#61624,
#61625),(#61626,#61627),(#61628,#61629),(#61630,#61631),(#61632,#61633),
(#61634,#61635),(#61636,#61637),(#61638,#61639),(#61640,#61641),(#61642,
#61643),(#61644,#61645),(#61646,#61647),(#61648,#61649),(#61650,#61651),
(#61652,#61653),(#61654,#61655),(#61656,#61657),(#61658,#61659),(#61660,
#61661),(#61662,#61663),(#61664,#61665),(#61666,#61667),(#61668,#61669),
(#61670,#61671),(#61672,#61673),(#61674,#61675),(#61676,#61677),(#61678,
#61679),(#61680,#61681),(#61682,#61683),(#61684,#61685),(#61686,#61687),
(#61688,#61689),(#61690,#61691),(#61692,#61693),(#61694,#61695),(#61696,
#61697),(#61698,#61699),(#61700,#61701),(#61702,#61703),(#61704,#61705),
(#61706,#61707),(#61708,#61709),(#61710,#61711),(#61712,#61713),(#61714,
#61715),(#61716,#61717),(#61718,#61719),(#61720,#61721),(#61722,#61723),
(#61724,#61725),(#61726,#61727),(#61728,#61729),(#61730,#61731),(#61732,
#61733),(#61734,#61735),(#61736,#61737),(#61738,#61739),(#61740,#61741),
(#61742,#61743),(#61744,#61745),(#61746,#61747),(#61748,#61749),(#61750,
#61751),(#61752,#61753),(#61754,#61755),(#61756,#61757),(#61758,#61759),
(#61760,#61761),(#61762,#61763),(#61764,#61765),(#61766,#61767),(#61768,
#61769),(#61770,#61771),(#61772,#61773),(#61774,#61775),(#61776,#61777),
(#61778,#61779),(#61780,#61781),(#61782,#61783),(#61784,#61785),(#61786,
#61787),(#61788,#61789),(#61790,#61791),(#61792,#61793),(#61794,#61795),
(#61796,#61797),(#61798,#61799),(#61800,#61801),(#61802,#61803),(#61804,
#61805),(#61806,#61807),(#61808,#61809),(#61810,#61811),(#61812,#61813),
(#61814,#61815),(#61816,#61817),(#61818,#61819),(#61820,#61821),(#61822,
#61823),(#61824,#61825),(#61826,#61827),(#61828,#61829),(#61830,#61831),
(#61832,#61833),(#61834,#61835),(#61836,#61837),(#61838,#61839),(#61840,
#61841),(#61842,#61843),(#61844,#61845),(#61846,#61847),(#61848,#61849),
(#61850,#61851),(#61852,#61853),(#61854,#61855),(#61856,#61857),(#61858,
#61859),(#61860,#61861),(#61862,#61863),(#61864,#61865),(#61866,#61867),
(#61868,#61869),(#61870,#61871),(#61872,#61873),(#61874,#61875),(#61876,
#61877),(#61878,#61879),(#61880,#61881),(#61882,#61883),(#61884,#61885),
(#61886,#61887),(#61888,#61889),(#61890,#61891),(#61892,#61893),(#61894,
#61895),(#61896,#61897),(#61898,#61899),(#61900,#61901),(#61902,#61903),
(#61904,#61905),(#61906,#61907),(#61908,#61909),(#61910,#61911),(#61912,
#61913),(#61914,#61915),(#61916,#61917),(#61918,#61919),(#61920,#61921),
(#61922,#61923),(#61924,#61925),(#61926,#61927),(#61928,#61929),(#61930,
#61931),(#61932,#61933),(#61934,#61935),(#61936,#61937),(#61938,#61939),
(#61940,#61941),(#61942,#61943),(#61944,#61945),(#61946,#61947),(#61948,
#61949),(#61950,#61951),(#61952,#61953),(#61954,#61955),(#61956,#61957),
(#61958,#61959),(#61960,#61961),(#61962,#61963),(#61964,#61965),(#61966,
#61967),(#61968,#61969),(#61970,#61971),(#61972,#61973),(#61974,#61975),
(#61976,#61977),(#61978,#61979),(#61980,#61981),(#61982,#61983),(#61984,
#61985),(#61986,#61987),(#61988,#61989),(#61990,#61991)),.UNSPECIFIED.,
 .F.,.F.,.F.)
B_SPLINE_SURFACE_WITH_KNOTS((6,1,1,1,1,1,1,1,1,1,1,1,1,1,1,1,1,1,1,1,1,
1,1,1,1,1,1,1,1,1,1,1,1,1,1,1,1,1,1,1,1,1,1,1,1,1,1,1,1,1,1,1,1,1,1,1,1,
1,1,1,1,1,1,1,1,1,1,1,1,1,1,1,1,1,1,1,1,1,1,1,1,1,1,1,1,1,1,1,1,1,1,1,1,
1,1,1,1,1,1,1,1,1,1,1,1,1,1,1,1,1,1,1,1,1,1,1,1,1,1,1,1,1,1,1,1,1,1,1,1,
1,1,1,1,1,1,1,1,1,1,1,1,1,1,1,1,1,1,1,1,1,1,1,1,1,1,1,1,1,1,1,1,1,1,1,1,
1,1,1,1,1,1,1,1,1,1,1,1,1,1,1,1,1,1,1,1,1,1,1,1,1,1,1,1,1,1,1,1,1,1,1,6),
(2,2),(0.,0.005,0.01,0.015,0.02,0.025,0.03,0.035,0.04,0.045,0.05,0.055,
0.06,0.065,0.07,0.075,0.08,0.085,0.09,0.095,0.1,0.105,0.11,0.115,0.12,0.125,
0.13,0.135,0.14,0.145,0.15,0.155,0.16,0.165,0.17,0.175,0.18,0.185,0.19,
0.195,0.2,0.205,0.21,0.215,0.22,0.225,0.23,0.235,0.24,0.245,0.25,0.255,
0.26,0.265,0.27,0.275,0.28,0.285,0.29,0.295,0.3,0.305,0.31,0.315,0.32,0.325,
0.33,0.335,0.34,0.345,0.35,0.355,0.36,0.365,0.37,0.375,0.38,0.385,0.39,
0.395,0.4,0.405,0.41,0.415,0.42,0.425,0.43,0.435,0.44,0.445,0.45,0.455,
0.46,0.465,0.47,0.475,0.48,0.485,0.49,0.495,0.5,0.505,0.51,0.515,0.52,0.525,
0.53,0.535,0.54,0.545,0.55,0.555,0.56,0.565,0.57,0.575,0.58,0.585,0.59,
0.595,0.6,0.605,0.61,0.615,0.62,0.625,0.63,0.635,0.64,0.645,0.65,0.655,
0.66,0.665,0.67,0.675,0.68,0.685,0.690000000000001,0.695000000000001,0.700000000000001,
0.705000000000001,0.710000000000001,0.715000000000001,0.720000000000001,
0.725000000000001,0.730000000000001,0.735000000000001,0.740000000000001,
0.745000000000001,0.750000000000001,0.755000000000001,0.760000000000001,
0.765000000000001,0.770000000000001,0.775000000000001,0.780000000000001,
0.785000000000001,0.790000000000001,0.795000000000001,0.800000000000001,
0.805000000000001,0.810000000000001,0.815000000000001,0.820000000000001,
0.825000000000001,0.830000000000001,0.835000000000001,0.840000000000001,
0.845000000000001,0.850000000000001,0.855000000000001,0.860000000000001,
0.865000000000001,0.870000000000001,0.875000000000001,0.880000000000001,
0.885000000000001,0.890000000000001,0.895000000000001,0.900000000000001,
0.905000000000001,0.910000000000001,0.915000000000001,0.920000000000001,
0.925000000000001,0.930000000000001,0.935000000000001,0.940000000000001,
0.945000000000001,0.950000000000001,0.955000000000001,0.960000000000001,
0.965000000000001,0.970000000000001,0.975000000000001,0.980000000000001,
0.985000000000001,0.990000000000001,0.995000000000001,1.),(0.,1.2),
 .UNSPECIFIED.)
GEOMETRIC_REPRESENTATION_ITEM()
RATIONAL_B_SPLINE_SURFACE(((1.,1.),(1.,1.),(1.,1.),(1.,1.),(1.,1.),(1.,
1.),(1.,1.),(1.,1.),(1.,1.),(1.,1.),(1.,1.),(1.,1.),(1.,1.),(1.,1.),(1.,
1.),(1.,1.),(1.,1.),(1.,1.),(1.,1.),(1.,1.),(1.,1.),(1.,1.),(1.,1.),(1.,
1.),(1.,1.),(1.,1.),(1.,1.),(1.,1.),(1.,1.),(1.,1.),(1.,1.),(1.,1.),(1.,
1.),(1.,1.),(1.,1.),(1.,1.),(1.,1.),(1.,1.),(1.,1.),(1.,1.),(1.,1.),(1.,
1.),(1.,1.),(1.,1.),(1.,1.),(1.,1.),(1.,1.),(1.,1.),(1.,1.),(1.,1.),(1.,
1.),(1.,1.),(1.,1.),(1.,1.),(1.,1.),(1.,1.),(1.,1.),(1.,1.),(1.,1.),(1.,
1.),(1.,1.),(1.,1.),(1.,1.),(1.,1.),(1.,1.),(1.,1.),(1.,1.),(1.,1.),(1.,
1.),(1.,1.),(1.,1.),(1.,1.),(1.,1.),(1.,1.),(1.,1.),(1.,1.),(1.,1.),(1.,
1.),(1.,1.),(1.,1.),(1.,1.),(1.,1.),(1.,1.),(1.,1.),(1.,1.),(1.,1.),(1.,
1.),(1.,1.),(1.,1.),(1.,1.),(1.,1.),(1.,1.),(1.,1.),(1.,1.),(1.,1.),(1.,
1.),(1.,1.),(1.,1.),(1.,1.),(1.,1.),(1.,1.),(1.,1.),(1.,1.),(1.,1.),(1.,
1.),(1.,1.),(1.,1.),(1.,1.),(1.,1.),(1.,1.),(1.,1.),(1.,1.),(1.,1.),(1.,
1.),(1.,1.),(1.,1.),(1.,1.),(1.,1.),(1.,1.),(1.,1.),(1.,1.),(1.,1.),(1.,
1.),(1.,1.),(1.,1.),(1.,1.),(1.,1.),(1.,1.),(1.,1.),(1.,1.),(1.,1.),(1.,
1.),(1.,1.),(1.,1.),(1.,1.),(1.,1.),(1.,1.),(1.,1.),(1.,1.),(1.,1.),(1.,
1.),(1.,1.),(1.,1.),(1.,1.),(1.,1.),(1.,1.),(1.,1.),(1.,1.),(1.,1.),(1.,
1.),(1.,1.),(1.,1.),(1.,1.),(1.,1.),(1.,1.),(1.,1.),(1.,1.),(1.,1.),(1.,
1.),(1.,1.),(1.,1.),(1.,1.),(1.,1.),(1.,1.),(1.,1.),(1.,1.),(1.,1.),(1.,
1.),(1.,1.),(1.,1.),(1.,1.),(1.,1.),(1.,1.),(1.,1.),(1.,1.),(1.,1.),(1.,
1.),(1.,1.),(1.,1.),(1.,1.),(1.,1.),(1.,1.),(1.,1.),(1.,1.),(1.,1.),(1.,
1.),(1.,1.),(1.,1.),(1.,1.),(1.,1.),(1.,1.),(1.,1.),(1.,1.),(1.,1.),(1.,
1.),(1.,1.),(1.,1.),(1.,1.),(1.,1.),(1.,1.),(1.,1.),(1.,1.),(1.,1.),(1.,
1.),(1.,1.)))
REPRESENTATION_ITEM('')
SURFACE()
);
#894=(
BOUNDED_SURFACE()
B_SPLINE_SURFACE(5,1,((#62478,#62479),(#62480,#62481),(#62482,#62483),(#62484,
#62485),(#62486,#62487),(#62488,#62489),(#62490,#62491),(#62492,#62493),
(#62494,#62495),(#62496,#62497),(#62498,#62499),(#62500,#62501),(#62502,
#62503),(#62504,#62505),(#62506,#62507),(#62508,#62509),(#62510,#62511),
(#62512,#62513),(#62514,#62515),(#62516,#62517),(#62518,#62519),(#62520,
#62521),(#62522,#62523),(#62524,#62525),(#62526,#62527),(#62528,#62529),
(#62530,#62531),(#62532,#62533),(#62534,#62535),(#62536,#62537),(#62538,
#62539),(#62540,#62541),(#62542,#62543),(#62544,#62545),(#62546,#62547),
(#62548,#62549),(#62550,#62551),(#62552,#62553),(#62554,#62555),(#62556,
#62557),(#62558,#62559),(#62560,#62561),(#62562,#62563),(#62564,#62565),
(#62566,#62567),(#62568,#62569),(#62570,#62571),(#62572,#62573),(#62574,
#62575),(#62576,#62577),(#62578,#62579),(#62580,#62581),(#62582,#62583),
(#62584,#62585),(#62586,#62587),(#62588,#62589),(#62590,#62591),(#62592,
#62593),(#62594,#62595),(#62596,#62597),(#62598,#62599),(#62600,#62601),
(#62602,#62603),(#62604,#62605),(#62606,#62607),(#62608,#62609),(#62610,
#62611),(#62612,#62613),(#62614,#62615),(#62616,#62617),(#62618,#62619),
(#62620,#62621),(#62622,#62623),(#62624,#62625),(#62626,#62627),(#62628,
#62629),(#62630,#62631),(#62632,#62633),(#62634,#62635),(#62636,#62637),
(#62638,#62639),(#62640,#62641),(#62642,#62643),(#62644,#62645),(#62646,
#62647),(#62648,#62649),(#62650,#62651),(#62652,#62653),(#62654,#62655),
(#62656,#62657),(#62658,#62659),(#62660,#62661),(#62662,#62663),(#62664,
#62665),(#62666,#62667),(#62668,#62669),(#62670,#62671),(#62672,#62673),
(#62674,#62675),(#62676,#62677),(#62678,#62679),(#62680,#62681),(#62682,
#62683),(#62684,#62685),(#62686,#62687),(#62688,#62689),(#62690,#62691),
(#62692,#62693),(#62694,#62695),(#62696,#62697),(#62698,#62699),(#62700,
#62701),(#62702,#62703),(#62704,#62705),(#62706,#62707),(#62708,#62709),
(#62710,#62711),(#62712,#62713),(#62714,#62715),(#62716,#62717),(#62718,
#62719),(#62720,#62721),(#62722,#62723),(#62724,#62725),(#62726,#62727),
(#62728,#62729),(#62730,#62731),(#62732,#62733),(#62734,#62735),(#62736,
#62737),(#62738,#62739),(#62740,#62741),(#62742,#62743),(#62744,#62745),
(#62746,#62747),(#62748,#62749),(#62750,#62751),(#62752,#62753),(#62754,
#62755),(#62756,#62757),(#62758,#62759),(#62760,#62761),(#62762,#62763),
(#62764,#62765),(#62766,#62767),(#62768,#62769),(#62770,#62771),(#62772,
#62773),(#62774,#62775),(#62776,#62777),(#62778,#62779),(#62780,#62781),
(#62782,#62783),(#62784,#62785),(#62786,#62787),(#62788,#62789),(#62790,
#62791),(#62792,#62793),(#62794,#62795),(#62796,#62797),(#62798,#62799),
(#62800,#62801),(#62802,#62803),(#62804,#62805),(#62806,#62807),(#62808,
#62809),(#62810,#62811),(#62812,#62813),(#62814,#62815),(#62816,#62817),
(#62818,#62819),(#62820,#62821),(#62822,#62823),(#62824,#62825),(#62826,
#62827),(#62828,#62829),(#62830,#62831),(#62832,#62833),(#62834,#62835),
(#62836,#62837),(#62838,#62839),(#62840,#62841),(#62842,#62843),(#62844,
#62845),(#62846,#62847),(#62848,#62849),(#62850,#62851),(#62852,#62853),
(#62854,#62855),(#62856,#62857),(#62858,#62859),(#62860,#62861),(#62862,
#62863),(#62864,#62865),(#62866,#62867),(#62868,#62869),(#62870,#62871),
(#62872,#62873),(#62874,#62875),(#62876,#62877),(#62878,#62879),(#62880,
#62881),(#62882,#62883),(#62884,#62885),(#62886,#62887)),.UNSPECIFIED.,
 .F.,.F.,.F.)
B_SPLINE_SURFACE_WITH_KNOTS((6,1,1,1,1,1,1,1,1,1,1,1,1,1,1,1,1,1,1,1,1,
1,1,1,1,1,1,1,1,1,1,1,1,1,1,1,1,1,1,1,1,1,1,1,1,1,1,1,1,1,1,1,1,1,1,1,1,
1,1,1,1,1,1,1,1,1,1,1,1,1,1,1,1,1,1,1,1,1,1,1,1,1,1,1,1,1,1,1,1,1,1,1,1,
1,1,1,1,1,1,1,1,1,1,1,1,1,1,1,1,1,1,1,1,1,1,1,1,1,1,1,1,1,1,1,1,1,1,1,1,
1,1,1,1,1,1,1,1,1,1,1,1,1,1,1,1,1,1,1,1,1,1,1,1,1,1,1,1,1,1,1,1,1,1,1,1,
1,1,1,1,1,1,1,1,1,1,1,1,1,1,1,1,1,1,1,1,1,1,1,1,1,1,1,1,1,1,1,1,1,1,1,6),
(2,2),(0.,0.005,0.01,0.015,0.02,0.025,0.03,0.035,0.04,0.045,0.05,0.055,
0.06,0.065,0.07,0.075,0.08,0.085,0.09,0.095,0.1,0.105,0.11,0.115,0.12,0.125,
0.13,0.135,0.14,0.145,0.15,0.155,0.16,0.165,0.17,0.175,0.18,0.185,0.19,
0.195,0.2,0.205,0.21,0.215,0.22,0.225,0.23,0.235,0.24,0.245,0.25,0.255,
0.26,0.265,0.27,0.275,0.28,0.285,0.29,0.295,0.3,0.305,0.31,0.315,0.32,0.325,
0.33,0.335,0.34,0.345,0.35,0.355,0.36,0.365,0.37,0.375,0.38,0.385,0.39,
0.395,0.4,0.405,0.41,0.415,0.42,0.425,0.43,0.435,0.44,0.445,0.45,0.455,
0.46,0.465,0.47,0.475,0.48,0.485,0.49,0.495,0.5,0.505,0.51,0.515,0.52,0.525,
0.53,0.535,0.54,0.545,0.55,0.555,0.56,0.565,0.57,0.575,0.58,0.585,0.59,
0.595,0.6,0.605,0.61,0.615,0.62,0.625,0.63,0.635,0.64,0.645,0.65,0.655,
0.66,0.665,0.67,0.675,0.68,0.685,0.690000000000001,0.695000000000001,0.700000000000001,
0.705000000000001,0.710000000000001,0.715000000000001,0.720000000000001,
0.725000000000001,0.730000000000001,0.735000000000001,0.740000000000001,
0.745000000000001,0.750000000000001,0.755000000000001,0.760000000000001,
0.765000000000001,0.770000000000001,0.775000000000001,0.780000000000001,
0.785000000000001,0.790000000000001,0.795000000000001,0.800000000000001,
0.805000000000001,0.810000000000001,0.815000000000001,0.820000000000001,
0.825000000000001,0.830000000000001,0.835000000000001,0.840000000000001,
0.845000000000001,0.850000000000001,0.855000000000001,0.860000000000001,
0.865000000000001,0.870000000000001,0.875000000000001,0.880000000000001,
0.885000000000001,0.890000000000001,0.895000000000001,0.900000000000001,
0.905000000000001,0.910000000000001,0.915000000000001,0.920000000000001,
0.925000000000001,0.930000000000001,0.935000000000001,0.940000000000001,
0.945000000000001,0.950000000000001,0.955000000000001,0.960000000000001,
0.965000000000001,0.970000000000001,0.975000000000001,0.980000000000001,
0.985000000000001,0.990000000000001,0.995000000000001,1.),(0.,1.2),
 .UNSPECIFIED.)
GEOMETRIC_REPRESENTATION_ITEM()
RATIONAL_B_SPLINE_SURFACE(((1.,1.),(1.,1.),(1.,1.),(1.,1.),(1.,1.),(1.,
1.),(1.,1.),(1.,1.),(1.,1.),(1.,1.),(1.,1.),(1.,1.),(1.,1.),(1.,1.),(1.,
1.),(1.,1.),(1.,1.),(1.,1.),(1.,1.),(1.,1.),(1.,1.),(1.,1.),(1.,1.),(1.,
1.),(1.,1.),(1.,1.),(1.,1.),(1.,1.),(1.,1.),(1.,1.),(1.,1.),(1.,1.),(1.,
1.),(1.,1.),(1.,1.),(1.,1.),(1.,1.),(1.,1.),(1.,1.),(1.,1.),(1.,1.),(1.,
1.),(1.,1.),(1.,1.),(1.,1.),(1.,1.),(1.,1.),(1.,1.),(1.,1.),(1.,1.),(1.,
1.),(1.,1.),(1.,1.),(1.,1.),(1.,1.),(1.,1.),(1.,1.),(1.,1.),(1.,1.),(1.,
1.),(1.,1.),(1.,1.),(1.,1.),(1.,1.),(1.,1.),(1.,1.),(1.,1.),(1.,1.),(1.,
1.),(1.,1.),(1.,1.),(1.,1.),(1.,1.),(1.,1.),(1.,1.),(1.,1.),(1.,1.),(1.,
1.),(1.,1.),(1.,1.),(1.,1.),(1.,1.),(1.,1.),(1.,1.),(1.,1.),(1.,1.),(1.,
1.),(1.,1.),(1.,1.),(1.,1.),(1.,1.),(1.,1.),(1.,1.),(1.,1.),(1.,1.),(1.,
1.),(1.,1.),(1.,1.),(1.,1.),(1.,1.),(1.,1.),(1.,1.),(1.,1.),(1.,1.),(1.,
1.),(1.,1.),(1.,1.),(1.,1.),(1.,1.),(1.,1.),(1.,1.),(1.,1.),(1.,1.),(1.,
1.),(1.,1.),(1.,1.),(1.,1.),(1.,1.),(1.,1.),(1.,1.),(1.,1.),(1.,1.),(1.,
1.),(1.,1.),(1.,1.),(1.,1.),(1.,1.),(1.,1.),(1.,1.),(1.,1.),(1.,1.),(1.,
1.),(1.,1.),(1.,1.),(1.,1.),(1.,1.),(1.,1.),(1.,1.),(1.,1.),(1.,1.),(1.,
1.),(1.,1.),(1.,1.),(1.,1.),(1.,1.),(1.,1.),(1.,1.),(1.,1.),(1.,1.),(1.,
1.),(1.,1.),(1.,1.),(1.,1.),(1.,1.),(1.,1.),(1.,1.),(1.,1.),(1.,1.),(1.,
1.),(1.,1.),(1.,1.),(1.,1.),(1.,1.),(1.,1.),(1.,1.),(1.,1.),(1.,1.),(1.,
1.),(1.,1.),(1.,1.),(1.,1.),(1.,1.),(1.,1.),(1.,1.),(1.,1.),(1.,1.),(1.,
1.),(1.,1.),(1.,1.),(1.,1.),(1.,1.),(1.,1.),(1.,1.),(1.,1.),(1.,1.),(1.,
1.),(1.,1.),(1.,1.),(1.,1.),(1.,1.),(1.,1.),(1.,1.),(1.,1.),(1.,1.),(1.,
1.),(1.,1.),(1.,1.),(1.,1.),(1.,1.),(1.,1.),(1.,1.),(1.,1.),(1.,1.),(1.,
1.),(1.,1.)))
REPRESENTATION_ITEM('')
SURFACE()
);
#895=(
BOUNDED_SURFACE()
B_SPLINE_SURFACE(5,1,((#63374,#63375),(#63376,#63377),(#63378,#63379),(#63380,
#63381),(#63382,#63383),(#63384,#63385),(#63386,#63387),(#63388,#63389),
(#63390,#63391),(#63392,#63393),(#63394,#63395),(#63396,#63397),(#63398,
#63399),(#63400,#63401),(#63402,#63403),(#63404,#63405),(#63406,#63407),
(#63408,#63409),(#63410,#63411),(#63412,#63413),(#63414,#63415),(#63416,
#63417),(#63418,#63419),(#63420,#63421),(#63422,#63423),(#63424,#63425),
(#63426,#63427),(#63428,#63429),(#63430,#63431),(#63432,#63433),(#63434,
#63435),(#63436,#63437),(#63438,#63439),(#63440,#63441),(#63442,#63443),
(#63444,#63445),(#63446,#63447),(#63448,#63449),(#63450,#63451),(#63452,
#63453),(#63454,#63455),(#63456,#63457),(#63458,#63459),(#63460,#63461),
(#63462,#63463),(#63464,#63465),(#63466,#63467),(#63468,#63469),(#63470,
#63471),(#63472,#63473),(#63474,#63475),(#63476,#63477),(#63478,#63479),
(#63480,#63481),(#63482,#63483),(#63484,#63485),(#63486,#63487),(#63488,
#63489),(#63490,#63491),(#63492,#63493),(#63494,#63495),(#63496,#63497),
(#63498,#63499),(#63500,#63501),(#63502,#63503),(#63504,#63505),(#63506,
#63507),(#63508,#63509),(#63510,#63511),(#63512,#63513),(#63514,#63515),
(#63516,#63517),(#63518,#63519),(#63520,#63521),(#63522,#63523),(#63524,
#63525),(#63526,#63527),(#63528,#63529),(#63530,#63531),(#63532,#63533),
(#63534,#63535),(#63536,#63537),(#63538,#63539),(#63540,#63541),(#63542,
#63543),(#63544,#63545),(#63546,#63547),(#63548,#63549),(#63550,#63551),
(#63552,#63553),(#63554,#63555),(#63556,#63557),(#63558,#63559),(#63560,
#63561),(#63562,#63563),(#63564,#63565),(#63566,#63567),(#63568,#63569),
(#63570,#63571),(#63572,#63573),(#63574,#63575),(#63576,#63577),(#63578,
#63579),(#63580,#63581),(#63582,#63583),(#63584,#63585),(#63586,#63587),
(#63588,#63589),(#63590,#63591),(#63592,#63593),(#63594,#63595),(#63596,
#63597),(#63598,#63599),(#63600,#63601),(#63602,#63603),(#63604,#63605),
(#63606,#63607),(#63608,#63609),(#63610,#63611),(#63612,#63613),(#63614,
#63615),(#63616,#63617),(#63618,#63619),(#63620,#63621),(#63622,#63623),
(#63624,#63625),(#63626,#63627),(#63628,#63629),(#63630,#63631),(#63632,
#63633),(#63634,#63635),(#63636,#63637),(#63638,#63639),(#63640,#63641),
(#63642,#63643),(#63644,#63645),(#63646,#63647),(#63648,#63649),(#63650,
#63651),(#63652,#63653),(#63654,#63655),(#63656,#63657),(#63658,#63659),
(#63660,#63661),(#63662,#63663),(#63664,#63665),(#63666,#63667),(#63668,
#63669),(#63670,#63671),(#63672,#63673),(#63674,#63675),(#63676,#63677),
(#63678,#63679),(#63680,#63681),(#63682,#63683),(#63684,#63685),(#63686,
#63687),(#63688,#63689),(#63690,#63691),(#63692,#63693),(#63694,#63695),
(#63696,#63697),(#63698,#63699),(#63700,#63701),(#63702,#63703),(#63704,
#63705),(#63706,#63707),(#63708,#63709),(#63710,#63711),(#63712,#63713),
(#63714,#63715),(#63716,#63717),(#63718,#63719),(#63720,#63721),(#63722,
#63723),(#63724,#63725),(#63726,#63727),(#63728,#63729),(#63730,#63731),
(#63732,#63733),(#63734,#63735),(#63736,#63737),(#63738,#63739),(#63740,
#63741),(#63742,#63743),(#63744,#63745),(#63746,#63747),(#63748,#63749),
(#63750,#63751),(#63752,#63753),(#63754,#63755),(#63756,#63757),(#63758,
#63759),(#63760,#63761),(#63762,#63763),(#63764,#63765),(#63766,#63767),
(#63768,#63769),(#63770,#63771),(#63772,#63773),(#63774,#63775),(#63776,
#63777),(#63778,#63779),(#63780,#63781),(#63782,#63783)),.UNSPECIFIED.,
 .F.,.F.,.F.)
B_SPLINE_SURFACE_WITH_KNOTS((6,1,1,1,1,1,1,1,1,1,1,1,1,1,1,1,1,1,1,1,1,
1,1,1,1,1,1,1,1,1,1,1,1,1,1,1,1,1,1,1,1,1,1,1,1,1,1,1,1,1,1,1,1,1,1,1,1,
1,1,1,1,1,1,1,1,1,1,1,1,1,1,1,1,1,1,1,1,1,1,1,1,1,1,1,1,1,1,1,1,1,1,1,1,
1,1,1,1,1,1,1,1,1,1,1,1,1,1,1,1,1,1,1,1,1,1,1,1,1,1,1,1,1,1,1,1,1,1,1,1,
1,1,1,1,1,1,1,1,1,1,1,1,1,1,1,1,1,1,1,1,1,1,1,1,1,1,1,1,1,1,1,1,1,1,1,1,
1,1,1,1,1,1,1,1,1,1,1,1,1,1,1,1,1,1,1,1,1,1,1,1,1,1,1,1,1,1,1,1,1,1,1,6),
(2,2),(0.,0.005,0.01,0.015,0.02,0.025,0.03,0.035,0.04,0.045,0.05,0.055,
0.06,0.065,0.07,0.075,0.08,0.085,0.09,0.095,0.1,0.105,0.11,0.115,0.12,0.125,
0.13,0.135,0.14,0.145,0.15,0.155,0.16,0.165,0.17,0.175,0.18,0.185,0.19,
0.195,0.2,0.205,0.21,0.215,0.22,0.225,0.23,0.235,0.24,0.245,0.25,0.255,
0.26,0.265,0.27,0.275,0.28,0.285,0.29,0.295,0.3,0.305,0.31,0.315,0.32,0.325,
0.33,0.335,0.34,0.345,0.35,0.355,0.36,0.365,0.37,0.375,0.38,0.385,0.39,
0.395,0.4,0.405,0.41,0.415,0.42,0.425,0.43,0.435,0.44,0.445,0.45,0.455,
0.46,0.465,0.47,0.475,0.48,0.485,0.49,0.495,0.5,0.505,0.51,0.515,0.52,0.525,
0.53,0.535,0.54,0.545,0.55,0.555,0.56,0.565,0.57,0.575,0.58,0.585,0.59,
0.595,0.6,0.605,0.61,0.615,0.62,0.625,0.63,0.635,0.64,0.645,0.65,0.655,
0.66,0.665,0.67,0.675,0.68,0.685,0.690000000000001,0.695000000000001,0.700000000000001,
0.705000000000001,0.710000000000001,0.715000000000001,0.720000000000001,
0.725000000000001,0.730000000000001,0.735000000000001,0.740000000000001,
0.745000000000001,0.750000000000001,0.755000000000001,0.760000000000001,
0.765000000000001,0.770000000000001,0.775000000000001,0.780000000000001,
0.785000000000001,0.790000000000001,0.795000000000001,0.800000000000001,
0.805000000000001,0.810000000000001,0.815000000000001,0.820000000000001,
0.825000000000001,0.830000000000001,0.835000000000001,0.840000000000001,
0.845000000000001,0.850000000000001,0.855000000000001,0.860000000000001,
0.865000000000001,0.870000000000001,0.875000000000001,0.880000000000001,
0.885000000000001,0.890000000000001,0.895000000000001,0.900000000000001,
0.905000000000001,0.910000000000001,0.915000000000001,0.920000000000001,
0.925000000000001,0.930000000000001,0.935000000000001,0.940000000000001,
0.945000000000001,0.950000000000001,0.955000000000001,0.960000000000001,
0.965000000000001,0.970000000000001,0.975000000000001,0.980000000000001,
0.985000000000001,0.990000000000001,0.995000000000001,1.),(0.,1.2),
 .UNSPECIFIED.)
GEOMETRIC_REPRESENTATION_ITEM()
RATIONAL_B_SPLINE_SURFACE(((1.,1.),(1.,1.),(1.,1.),(1.,1.),(1.,1.),(1.,
1.),(1.,1.),(1.,1.),(1.,1.),(1.,1.),(1.,1.),(1.,1.),(1.,1.),(1.,1.),(1.,
1.),(1.,1.),(1.,1.),(1.,1.),(1.,1.),(1.,1.),(1.,1.),(1.,1.),(1.,1.),(1.,
1.),(1.,1.),(1.,1.),(1.,1.),(1.,1.),(1.,1.),(1.,1.),(1.,1.),(1.,1.),(1.,
1.),(1.,1.),(1.,1.),(1.,1.),(1.,1.),(1.,1.),(1.,1.),(1.,1.),(1.,1.),(1.,
1.),(1.,1.),(1.,1.),(1.,1.),(1.,1.),(1.,1.),(1.,1.),(1.,1.),(1.,1.),(1.,
1.),(1.,1.),(1.,1.),(1.,1.),(1.,1.),(1.,1.),(1.,1.),(1.,1.),(1.,1.),(1.,
1.),(1.,1.),(1.,1.),(1.,1.),(1.,1.),(1.,1.),(1.,1.),(1.,1.),(1.,1.),(1.,
1.),(1.,1.),(1.,1.),(1.,1.),(1.,1.),(1.,1.),(1.,1.),(1.,1.),(1.,1.),(1.,
1.),(1.,1.),(1.,1.),(1.,1.),(1.,1.),(1.,1.),(1.,1.),(1.,1.),(1.,1.),(1.,
1.),(1.,1.),(1.,1.),(1.,1.),(1.,1.),(1.,1.),(1.,1.),(1.,1.),(1.,1.),(1.,
1.),(1.,1.),(1.,1.),(1.,1.),(1.,1.),(1.,1.),(1.,1.),(1.,1.),(1.,1.),(1.,
1.),(1.,1.),(1.,1.),(1.,1.),(1.,1.),(1.,1.),(1.,1.),(1.,1.),(1.,1.),(1.,
1.),(1.,1.),(1.,1.),(1.,1.),(1.,1.),(1.,1.),(1.,1.),(1.,1.),(1.,1.),(1.,
1.),(1.,1.),(1.,1.),(1.,1.),(1.,1.),(1.,1.),(1.,1.),(1.,1.),(1.,1.),(1.,
1.),(1.,1.),(1.,1.),(1.,1.),(1.,1.),(1.,1.),(1.,1.),(1.,1.),(1.,1.),(1.,
1.),(1.,1.),(1.,1.),(1.,1.),(1.,1.),(1.,1.),(1.,1.),(1.,1.),(1.,1.),(1.,
1.),(1.,1.),(1.,1.),(1.,1.),(1.,1.),(1.,1.),(1.,1.),(1.,1.),(1.,1.),(1.,
1.),(1.,1.),(1.,1.),(1.,1.),(1.,1.),(1.,1.),(1.,1.),(1.,1.),(1.,1.),(1.,
1.),(1.,1.),(1.,1.),(1.,1.),(1.,1.),(1.,1.),(1.,1.),(1.,1.),(1.,1.),(1.,
1.),(1.,1.),(1.,1.),(1.,1.),(1.,1.),(1.,1.),(1.,1.),(1.,1.),(1.,1.),(1.,
1.),(1.,1.),(1.,1.),(1.,1.),(1.,1.),(1.,1.),(1.,1.),(1.,1.),(1.,1.),(1.,
1.),(1.,1.),(1.,1.),(1.,1.),(1.,1.),(1.,1.),(1.,1.),(1.,1.),(1.,1.),(1.,
1.),(1.,1.)))
REPRESENTATION_ITEM('')
SURFACE()
);
#896=(
BOUNDED_SURFACE()
B_SPLINE_SURFACE(5,1,((#64270,#64271),(#64272,#64273),(#64274,#64275),(#64276,
#64277),(#64278,#64279),(#64280,#64281),(#64282,#64283),(#64284,#64285),
(#64286,#64287),(#64288,#64289),(#64290,#64291),(#64292,#64293),(#64294,
#64295),(#64296,#64297),(#64298,#64299),(#64300,#64301),(#64302,#64303),
(#64304,#64305),(#64306,#64307),(#64308,#64309),(#64310,#64311),(#64312,
#64313),(#64314,#64315),(#64316,#64317),(#64318,#64319),(#64320,#64321),
(#64322,#64323),(#64324,#64325),(#64326,#64327),(#64328,#64329),(#64330,
#64331),(#64332,#64333),(#64334,#64335),(#64336,#64337),(#64338,#64339),
(#64340,#64341),(#64342,#64343),(#64344,#64345),(#64346,#64347),(#64348,
#64349),(#64350,#64351),(#64352,#64353),(#64354,#64355),(#64356,#64357),
(#64358,#64359),(#64360,#64361),(#64362,#64363),(#64364,#64365),(#64366,
#64367),(#64368,#64369),(#64370,#64371),(#64372,#64373),(#64374,#64375),
(#64376,#64377),(#64378,#64379),(#64380,#64381),(#64382,#64383),(#64384,
#64385),(#64386,#64387),(#64388,#64389),(#64390,#64391),(#64392,#64393),
(#64394,#64395),(#64396,#64397),(#64398,#64399),(#64400,#64401),(#64402,
#64403),(#64404,#64405),(#64406,#64407),(#64408,#64409),(#64410,#64411),
(#64412,#64413),(#64414,#64415),(#64416,#64417),(#64418,#64419),(#64420,
#64421),(#64422,#64423),(#64424,#64425),(#64426,#64427),(#64428,#64429),
(#64430,#64431),(#64432,#64433),(#64434,#64435),(#64436,#64437),(#64438,
#64439),(#64440,#64441),(#64442,#64443),(#64444,#64445),(#64446,#64447),
(#64448,#64449),(#64450,#64451),(#64452,#64453),(#64454,#64455),(#64456,
#64457),(#64458,#64459),(#64460,#64461),(#64462,#64463),(#64464,#64465),
(#64466,#64467),(#64468,#64469),(#64470,#64471),(#64472,#64473),(#64474,
#64475),(#64476,#64477),(#64478,#64479),(#64480,#64481),(#64482,#64483),
(#64484,#64485),(#64486,#64487),(#64488,#64489),(#64490,#64491),(#64492,
#64493),(#64494,#64495),(#64496,#64497),(#64498,#64499),(#64500,#64501),
(#64502,#64503),(#64504,#64505),(#64506,#64507),(#64508,#64509),(#64510,
#64511),(#64512,#64513),(#64514,#64515),(#64516,#64517),(#64518,#64519),
(#64520,#64521),(#64522,#64523),(#64524,#64525),(#64526,#64527),(#64528,
#64529),(#64530,#64531),(#64532,#64533),(#64534,#64535),(#64536,#64537),
(#64538,#64539),(#64540,#64541),(#64542,#64543),(#64544,#64545),(#64546,
#64547),(#64548,#64549),(#64550,#64551),(#64552,#64553),(#64554,#64555),
(#64556,#64557),(#64558,#64559),(#64560,#64561),(#64562,#64563),(#64564,
#64565),(#64566,#64567),(#64568,#64569),(#64570,#64571),(#64572,#64573),
(#64574,#64575),(#64576,#64577),(#64578,#64579),(#64580,#64581),(#64582,
#64583),(#64584,#64585),(#64586,#64587),(#64588,#64589),(#64590,#64591),
(#64592,#64593),(#64594,#64595),(#64596,#64597),(#64598,#64599),(#64600,
#64601),(#64602,#64603),(#64604,#64605),(#64606,#64607),(#64608,#64609),
(#64610,#64611),(#64612,#64613),(#64614,#64615),(#64616,#64617),(#64618,
#64619),(#64620,#64621),(#64622,#64623),(#64624,#64625),(#64626,#64627),
(#64628,#64629),(#64630,#64631),(#64632,#64633),(#64634,#64635),(#64636,
#64637),(#64638,#64639),(#64640,#64641),(#64642,#64643),(#64644,#64645),
(#64646,#64647),(#64648,#64649),(#64650,#64651),(#64652,#64653),(#64654,
#64655),(#64656,#64657),(#64658,#64659),(#64660,#64661),(#64662,#64663),
(#64664,#64665),(#64666,#64667),(#64668,#64669),(#64670,#64671),(#64672,
#64673),(#64674,#64675),(#64676,#64677),(#64678,#64679)),.UNSPECIFIED.,
 .F.,.F.,.F.)
B_SPLINE_SURFACE_WITH_KNOTS((6,1,1,1,1,1,1,1,1,1,1,1,1,1,1,1,1,1,1,1,1,
1,1,1,1,1,1,1,1,1,1,1,1,1,1,1,1,1,1,1,1,1,1,1,1,1,1,1,1,1,1,1,1,1,1,1,1,
1,1,1,1,1,1,1,1,1,1,1,1,1,1,1,1,1,1,1,1,1,1,1,1,1,1,1,1,1,1,1,1,1,1,1,1,
1,1,1,1,1,1,1,1,1,1,1,1,1,1,1,1,1,1,1,1,1,1,1,1,1,1,1,1,1,1,1,1,1,1,1,1,
1,1,1,1,1,1,1,1,1,1,1,1,1,1,1,1,1,1,1,1,1,1,1,1,1,1,1,1,1,1,1,1,1,1,1,1,
1,1,1,1,1,1,1,1,1,1,1,1,1,1,1,1,1,1,1,1,1,1,1,1,1,1,1,1,1,1,1,1,1,1,1,6),
(2,2),(0.,0.005,0.01,0.015,0.02,0.025,0.03,0.035,0.04,0.045,0.05,0.055,
0.06,0.065,0.07,0.075,0.08,0.085,0.09,0.095,0.1,0.105,0.11,0.115,0.12,0.125,
0.13,0.135,0.14,0.145,0.15,0.155,0.16,0.165,0.17,0.175,0.18,0.185,0.19,
0.195,0.2,0.205,0.21,0.215,0.22,0.225,0.23,0.235,0.24,0.245,0.25,0.255,
0.26,0.265,0.27,0.275,0.28,0.285,0.29,0.295,0.3,0.305,0.31,0.315,0.32,0.325,
0.33,0.335,0.34,0.345,0.35,0.355,0.36,0.365,0.37,0.375,0.38,0.385,0.39,
0.395,0.4,0.405,0.41,0.415,0.42,0.425,0.43,0.435,0.44,0.445,0.45,0.455,
0.46,0.465,0.47,0.475,0.48,0.485,0.49,0.495,0.5,0.505,0.51,0.515,0.52,0.525,
0.53,0.535,0.54,0.545,0.55,0.555,0.56,0.565,0.57,0.575,0.58,0.585,0.59,
0.595,0.6,0.605,0.61,0.615,0.62,0.625,0.63,0.635,0.64,0.645,0.65,0.655,
0.66,0.665,0.67,0.675,0.68,0.685,0.690000000000001,0.695000000000001,0.700000000000001,
0.705000000000001,0.710000000000001,0.715000000000001,0.720000000000001,
0.725000000000001,0.730000000000001,0.735000000000001,0.740000000000001,
0.745000000000001,0.750000000000001,0.755000000000001,0.760000000000001,
0.765000000000001,0.770000000000001,0.775000000000001,0.780000000000001,
0.785000000000001,0.790000000000001,0.795000000000001,0.800000000000001,
0.805000000000001,0.810000000000001,0.815000000000001,0.820000000000001,
0.825000000000001,0.830000000000001,0.835000000000001,0.840000000000001,
0.845000000000001,0.850000000000001,0.855000000000001,0.860000000000001,
0.865000000000001,0.870000000000001,0.875000000000001,0.880000000000001,
0.885000000000001,0.890000000000001,0.895000000000001,0.900000000000001,
0.905000000000001,0.910000000000001,0.915000000000001,0.920000000000001,
0.925000000000001,0.930000000000001,0.935000000000001,0.940000000000001,
0.945000000000001,0.950000000000001,0.955000000000001,0.960000000000001,
0.965000000000001,0.970000000000001,0.975000000000001,0.980000000000001,
0.985000000000001,0.990000000000001,0.995000000000001,1.),(0.,1.2),
 .UNSPECIFIED.)
GEOMETRIC_REPRESENTATION_ITEM()
RATIONAL_B_SPLINE_SURFACE(((1.,1.),(1.,1.),(1.,1.),(1.,1.),(1.,1.),(1.,
1.),(1.,1.),(1.,1.),(1.,1.),(1.,1.),(1.,1.),(1.,1.),(1.,1.),(1.,1.),(1.,
1.),(1.,1.),(1.,1.),(1.,1.),(1.,1.),(1.,1.),(1.,1.),(1.,1.),(1.,1.),(1.,
1.),(1.,1.),(1.,1.),(1.,1.),(1.,1.),(1.,1.),(1.,1.),(1.,1.),(1.,1.),(1.,
1.),(1.,1.),(1.,1.),(1.,1.),(1.,1.),(1.,1.),(1.,1.),(1.,1.),(1.,1.),(1.,
1.),(1.,1.),(1.,1.),(1.,1.),(1.,1.),(1.,1.),(1.,1.),(1.,1.),(1.,1.),(1.,
1.),(1.,1.),(1.,1.),(1.,1.),(1.,1.),(1.,1.),(1.,1.),(1.,1.),(1.,1.),(1.,
1.),(1.,1.),(1.,1.),(1.,1.),(1.,1.),(1.,1.),(1.,1.),(1.,1.),(1.,1.),(1.,
1.),(1.,1.),(1.,1.),(1.,1.),(1.,1.),(1.,1.),(1.,1.),(1.,1.),(1.,1.),(1.,
1.),(1.,1.),(1.,1.),(1.,1.),(1.,1.),(1.,1.),(1.,1.),(1.,1.),(1.,1.),(1.,
1.),(1.,1.),(1.,1.),(1.,1.),(1.,1.),(1.,1.),(1.,1.),(1.,1.),(1.,1.),(1.,
1.),(1.,1.),(1.,1.),(1.,1.),(1.,1.),(1.,1.),(1.,1.),(1.,1.),(1.,1.),(1.,
1.),(1.,1.),(1.,1.),(1.,1.),(1.,1.),(1.,1.),(1.,1.),(1.,1.),(1.,1.),(1.,
1.),(1.,1.),(1.,1.),(1.,1.),(1.,1.),(1.,1.),(1.,1.),(1.,1.),(1.,1.),(1.,
1.),(1.,1.),(1.,1.),(1.,1.),(1.,1.),(1.,1.),(1.,1.),(1.,1.),(1.,1.),(1.,
1.),(1.,1.),(1.,1.),(1.,1.),(1.,1.),(1.,1.),(1.,1.),(1.,1.),(1.,1.),(1.,
1.),(1.,1.),(1.,1.),(1.,1.),(1.,1.),(1.,1.),(1.,1.),(1.,1.),(1.,1.),(1.,
1.),(1.,1.),(1.,1.),(1.,1.),(1.,1.),(1.,1.),(1.,1.),(1.,1.),(1.,1.),(1.,
1.),(1.,1.),(1.,1.),(1.,1.),(1.,1.),(1.,1.),(1.,1.),(1.,1.),(1.,1.),(1.,
1.),(1.,1.),(1.,1.),(1.,1.),(1.,1.),(1.,1.),(1.,1.),(1.,1.),(1.,1.),(1.,
1.),(1.,1.),(1.,1.),(1.,1.),(1.,1.),(1.,1.),(1.,1.),(1.,1.),(1.,1.),(1.,
1.),(1.,1.),(1.,1.),(1.,1.),(1.,1.),(1.,1.),(1.,1.),(1.,1.),(1.,1.),(1.,
1.),(1.,1.),(1.,1.),(1.,1.),(1.,1.),(1.,1.),(1.,1.),(1.,1.),(1.,1.),(1.,
1.),(1.,1.)))
REPRESENTATION_ITEM('')
SURFACE()
);
#897=(
BOUNDED_SURFACE()
B_SPLINE_SURFACE(5,1,((#65166,#65167),(#65168,#65169),(#65170,#65171),(#65172,
#65173),(#65174,#65175),(#65176,#65177),(#65178,#65179),(#65180,#65181),
(#65182,#65183),(#65184,#65185),(#65186,#65187),(#65188,#65189),(#65190,
#65191),(#65192,#65193),(#65194,#65195),(#65196,#65197),(#65198,#65199),
(#65200,#65201),(#65202,#65203),(#65204,#65205),(#65206,#65207),(#65208,
#65209),(#65210,#65211),(#65212,#65213),(#65214,#65215),(#65216,#65217),
(#65218,#65219),(#65220,#65221),(#65222,#65223),(#65224,#65225),(#65226,
#65227),(#65228,#65229),(#65230,#65231),(#65232,#65233),(#65234,#65235),
(#65236,#65237),(#65238,#65239),(#65240,#65241),(#65242,#65243),(#65244,
#65245),(#65246,#65247),(#65248,#65249),(#65250,#65251),(#65252,#65253),
(#65254,#65255),(#65256,#65257),(#65258,#65259),(#65260,#65261),(#65262,
#65263),(#65264,#65265),(#65266,#65267),(#65268,#65269),(#65270,#65271),
(#65272,#65273),(#65274,#65275),(#65276,#65277),(#65278,#65279),(#65280,
#65281),(#65282,#65283),(#65284,#65285),(#65286,#65287),(#65288,#65289),
(#65290,#65291),(#65292,#65293),(#65294,#65295),(#65296,#65297),(#65298,
#65299),(#65300,#65301),(#65302,#65303),(#65304,#65305),(#65306,#65307),
(#65308,#65309),(#65310,#65311),(#65312,#65313),(#65314,#65315),(#65316,
#65317),(#65318,#65319),(#65320,#65321),(#65322,#65323),(#65324,#65325),
(#65326,#65327),(#65328,#65329),(#65330,#65331),(#65332,#65333),(#65334,
#65335),(#65336,#65337),(#65338,#65339),(#65340,#65341),(#65342,#65343),
(#65344,#65345),(#65346,#65347),(#65348,#65349),(#65350,#65351),(#65352,
#65353),(#65354,#65355),(#65356,#65357),(#65358,#65359),(#65360,#65361),
(#65362,#65363),(#65364,#65365),(#65366,#65367),(#65368,#65369),(#65370,
#65371),(#65372,#65373),(#65374,#65375),(#65376,#65377),(#65378,#65379),
(#65380,#65381),(#65382,#65383),(#65384,#65385),(#65386,#65387),(#65388,
#65389),(#65390,#65391),(#65392,#65393),(#65394,#65395),(#65396,#65397),
(#65398,#65399),(#65400,#65401),(#65402,#65403),(#65404,#65405),(#65406,
#65407),(#65408,#65409),(#65410,#65411),(#65412,#65413),(#65414,#65415),
(#65416,#65417),(#65418,#65419),(#65420,#65421),(#65422,#65423),(#65424,
#65425),(#65426,#65427),(#65428,#65429),(#65430,#65431),(#65432,#65433),
(#65434,#65435),(#65436,#65437),(#65438,#65439),(#65440,#65441),(#65442,
#65443),(#65444,#65445),(#65446,#65447),(#65448,#65449),(#65450,#65451),
(#65452,#65453),(#65454,#65455),(#65456,#65457),(#65458,#65459),(#65460,
#65461),(#65462,#65463),(#65464,#65465),(#65466,#65467),(#65468,#65469),
(#65470,#65471),(#65472,#65473),(#65474,#65475),(#65476,#65477),(#65478,
#65479),(#65480,#65481),(#65482,#65483),(#65484,#65485),(#65486,#65487),
(#65488,#65489),(#65490,#65491),(#65492,#65493),(#65494,#65495),(#65496,
#65497),(#65498,#65499),(#65500,#65501),(#65502,#65503),(#65504,#65505),
(#65506,#65507),(#65508,#65509),(#65510,#65511),(#65512,#65513),(#65514,
#65515),(#65516,#65517),(#65518,#65519),(#65520,#65521),(#65522,#65523),
(#65524,#65525),(#65526,#65527),(#65528,#65529),(#65530,#65531),(#65532,
#65533),(#65534,#65535),(#65536,#65537),(#65538,#65539),(#65540,#65541),
(#65542,#65543),(#65544,#65545),(#65546,#65547),(#65548,#65549),(#65550,
#65551),(#65552,#65553),(#65554,#65555),(#65556,#65557),(#65558,#65559),
(#65560,#65561),(#65562,#65563),(#65564,#65565),(#65566,#65567),(#65568,
#65569),(#65570,#65571),(#65572,#65573),(#65574,#65575)),.UNSPECIFIED.,
 .F.,.F.,.F.)
B_SPLINE_SURFACE_WITH_KNOTS((6,1,1,1,1,1,1,1,1,1,1,1,1,1,1,1,1,1,1,1,1,
1,1,1,1,1,1,1,1,1,1,1,1,1,1,1,1,1,1,1,1,1,1,1,1,1,1,1,1,1,1,1,1,1,1,1,1,
1,1,1,1,1,1,1,1,1,1,1,1,1,1,1,1,1,1,1,1,1,1,1,1,1,1,1,1,1,1,1,1,1,1,1,1,
1,1,1,1,1,1,1,1,1,1,1,1,1,1,1,1,1,1,1,1,1,1,1,1,1,1,1,1,1,1,1,1,1,1,1,1,
1,1,1,1,1,1,1,1,1,1,1,1,1,1,1,1,1,1,1,1,1,1,1,1,1,1,1,1,1,1,1,1,1,1,1,1,
1,1,1,1,1,1,1,1,1,1,1,1,1,1,1,1,1,1,1,1,1,1,1,1,1,1,1,1,1,1,1,1,1,1,1,6),
(2,2),(0.,0.005,0.01,0.015,0.02,0.025,0.03,0.035,0.04,0.045,0.05,0.055,
0.06,0.065,0.07,0.075,0.08,0.085,0.09,0.095,0.1,0.105,0.11,0.115,0.12,0.125,
0.13,0.135,0.14,0.145,0.15,0.155,0.16,0.165,0.17,0.175,0.18,0.185,0.19,
0.195,0.2,0.205,0.21,0.215,0.22,0.225,0.23,0.235,0.24,0.245,0.25,0.255,
0.26,0.265,0.27,0.275,0.28,0.285,0.29,0.295,0.3,0.305,0.31,0.315,0.32,0.325,
0.33,0.335,0.34,0.345,0.35,0.355,0.36,0.365,0.37,0.375,0.38,0.385,0.39,
0.395,0.4,0.405,0.41,0.415,0.42,0.425,0.43,0.435,0.44,0.445,0.45,0.455,
0.46,0.465,0.47,0.475,0.48,0.485,0.49,0.495,0.5,0.505,0.51,0.515,0.52,0.525,
0.53,0.535,0.54,0.545,0.55,0.555,0.56,0.565,0.57,0.575,0.58,0.585,0.59,
0.595,0.6,0.605,0.61,0.615,0.62,0.625,0.63,0.635,0.64,0.645,0.65,0.655,
0.66,0.665,0.67,0.675,0.68,0.685,0.690000000000001,0.695000000000001,0.700000000000001,
0.705000000000001,0.710000000000001,0.715000000000001,0.720000000000001,
0.725000000000001,0.730000000000001,0.735000000000001,0.740000000000001,
0.745000000000001,0.750000000000001,0.755000000000001,0.760000000000001,
0.765000000000001,0.770000000000001,0.775000000000001,0.780000000000001,
0.785000000000001,0.790000000000001,0.795000000000001,0.800000000000001,
0.805000000000001,0.810000000000001,0.815000000000001,0.820000000000001,
0.825000000000001,0.830000000000001,0.835000000000001,0.840000000000001,
0.845000000000001,0.850000000000001,0.855000000000001,0.860000000000001,
0.865000000000001,0.870000000000001,0.875000000000001,0.880000000000001,
0.885000000000001,0.890000000000001,0.895000000000001,0.900000000000001,
0.905000000000001,0.910000000000001,0.915000000000001,0.920000000000001,
0.925000000000001,0.930000000000001,0.935000000000001,0.940000000000001,
0.945000000000001,0.950000000000001,0.955000000000001,0.960000000000001,
0.965000000000001,0.970000000000001,0.975000000000001,0.980000000000001,
0.985000000000001,0.990000000000001,0.995000000000001,1.),(0.,1.2),
 .UNSPECIFIED.)
GEOMETRIC_REPRESENTATION_ITEM()
RATIONAL_B_SPLINE_SURFACE(((1.,1.),(1.,1.),(1.,1.),(1.,1.),(1.,1.),(1.,
1.),(1.,1.),(1.,1.),(1.,1.),(1.,1.),(1.,1.),(1.,1.),(1.,1.),(1.,1.),(1.,
1.),(1.,1.),(1.,1.),(1.,1.),(1.,1.),(1.,1.),(1.,1.),(1.,1.),(1.,1.),(1.,
1.),(1.,1.),(1.,1.),(1.,1.),(1.,1.),(1.,1.),(1.,1.),(1.,1.),(1.,1.),(1.,
1.),(1.,1.),(1.,1.),(1.,1.),(1.,1.),(1.,1.),(1.,1.),(1.,1.),(1.,1.),(1.,
1.),(1.,1.),(1.,1.),(1.,1.),(1.,1.),(1.,1.),(1.,1.),(1.,1.),(1.,1.),(1.,
1.),(1.,1.),(1.,1.),(1.,1.),(1.,1.),(1.,1.),(1.,1.),(1.,1.),(1.,1.),(1.,
1.),(1.,1.),(1.,1.),(1.,1.),(1.,1.),(1.,1.),(1.,1.),(1.,1.),(1.,1.),(1.,
1.),(1.,1.),(1.,1.),(1.,1.),(1.,1.),(1.,1.),(1.,1.),(1.,1.),(1.,1.),(1.,
1.),(1.,1.),(1.,1.),(1.,1.),(1.,1.),(1.,1.),(1.,1.),(1.,1.),(1.,1.),(1.,
1.),(1.,1.),(1.,1.),(1.,1.),(1.,1.),(1.,1.),(1.,1.),(1.,1.),(1.,1.),(1.,
1.),(1.,1.),(1.,1.),(1.,1.),(1.,1.),(1.,1.),(1.,1.),(1.,1.),(1.,1.),(1.,
1.),(1.,1.),(1.,1.),(1.,1.),(1.,1.),(1.,1.),(1.,1.),(1.,1.),(1.,1.),(1.,
1.),(1.,1.),(1.,1.),(1.,1.),(1.,1.),(1.,1.),(1.,1.),(1.,1.),(1.,1.),(1.,
1.),(1.,1.),(1.,1.),(1.,1.),(1.,1.),(1.,1.),(1.,1.),(1.,1.),(1.,1.),(1.,
1.),(1.,1.),(1.,1.),(1.,1.),(1.,1.),(1.,1.),(1.,1.),(1.,1.),(1.,1.),(1.,
1.),(1.,1.),(1.,1.),(1.,1.),(1.,1.),(1.,1.),(1.,1.),(1.,1.),(1.,1.),(1.,
1.),(1.,1.),(1.,1.),(1.,1.),(1.,1.),(1.,1.),(1.,1.),(1.,1.),(1.,1.),(1.,
1.),(1.,1.),(1.,1.),(1.,1.),(1.,1.),(1.,1.),(1.,1.),(1.,1.),(1.,1.),(1.,
1.),(1.,1.),(1.,1.),(1.,1.),(1.,1.),(1.,1.),(1.,1.),(1.,1.),(1.,1.),(1.,
1.),(1.,1.),(1.,1.),(1.,1.),(1.,1.),(1.,1.),(1.,1.),(1.,1.),(1.,1.),(1.,
1.),(1.,1.),(1.,1.),(1.,1.),(1.,1.),(1.,1.),(1.,1.),(1.,1.),(1.,1.),(1.,
1.),(1.,1.),(1.,1.),(1.,1.),(1.,1.),(1.,1.),(1.,1.),(1.,1.),(1.,1.),(1.,
1.),(1.,1.)))
REPRESENTATION_ITEM('')
SURFACE()
);
#898=(
BOUNDED_SURFACE()
B_SPLINE_SURFACE(5,1,((#66062,#66063),(#66064,#66065),(#66066,#66067),(#66068,
#66069),(#66070,#66071),(#66072,#66073),(#66074,#66075),(#66076,#66077),
(#66078,#66079),(#66080,#66081),(#66082,#66083),(#66084,#66085),(#66086,
#66087),(#66088,#66089),(#66090,#66091),(#66092,#66093),(#66094,#66095),
(#66096,#66097),(#66098,#66099),(#66100,#66101),(#66102,#66103),(#66104,
#66105),(#66106,#66107),(#66108,#66109),(#66110,#66111),(#66112,#66113),
(#66114,#66115),(#66116,#66117),(#66118,#66119),(#66120,#66121),(#66122,
#66123),(#66124,#66125),(#66126,#66127),(#66128,#66129),(#66130,#66131),
(#66132,#66133),(#66134,#66135),(#66136,#66137),(#66138,#66139),(#66140,
#66141),(#66142,#66143),(#66144,#66145),(#66146,#66147),(#66148,#66149),
(#66150,#66151),(#66152,#66153),(#66154,#66155),(#66156,#66157),(#66158,
#66159),(#66160,#66161),(#66162,#66163),(#66164,#66165),(#66166,#66167),
(#66168,#66169),(#66170,#66171),(#66172,#66173),(#66174,#66175),(#66176,
#66177),(#66178,#66179),(#66180,#66181),(#66182,#66183),(#66184,#66185),
(#66186,#66187),(#66188,#66189),(#66190,#66191),(#66192,#66193),(#66194,
#66195),(#66196,#66197),(#66198,#66199),(#66200,#66201),(#66202,#66203),
(#66204,#66205),(#66206,#66207),(#66208,#66209),(#66210,#66211),(#66212,
#66213),(#66214,#66215),(#66216,#66217),(#66218,#66219),(#66220,#66221),
(#66222,#66223),(#66224,#66225),(#66226,#66227),(#66228,#66229),(#66230,
#66231),(#66232,#66233),(#66234,#66235),(#66236,#66237),(#66238,#66239),
(#66240,#66241),(#66242,#66243),(#66244,#66245),(#66246,#66247),(#66248,
#66249),(#66250,#66251),(#66252,#66253),(#66254,#66255),(#66256,#66257),
(#66258,#66259),(#66260,#66261),(#66262,#66263),(#66264,#66265),(#66266,
#66267),(#66268,#66269),(#66270,#66271),(#66272,#66273),(#66274,#66275),
(#66276,#66277),(#66278,#66279),(#66280,#66281),(#66282,#66283),(#66284,
#66285),(#66286,#66287),(#66288,#66289),(#66290,#66291),(#66292,#66293),
(#66294,#66295),(#66296,#66297),(#66298,#66299),(#66300,#66301),(#66302,
#66303),(#66304,#66305),(#66306,#66307),(#66308,#66309),(#66310,#66311),
(#66312,#66313),(#66314,#66315),(#66316,#66317),(#66318,#66319),(#66320,
#66321),(#66322,#66323),(#66324,#66325),(#66326,#66327),(#66328,#66329),
(#66330,#66331),(#66332,#66333),(#66334,#66335),(#66336,#66337),(#66338,
#66339),(#66340,#66341),(#66342,#66343),(#66344,#66345),(#66346,#66347),
(#66348,#66349),(#66350,#66351),(#66352,#66353),(#66354,#66355),(#66356,
#66357),(#66358,#66359),(#66360,#66361),(#66362,#66363),(#66364,#66365),
(#66366,#66367),(#66368,#66369),(#66370,#66371),(#66372,#66373),(#66374,
#66375),(#66376,#66377),(#66378,#66379),(#66380,#66381),(#66382,#66383),
(#66384,#66385),(#66386,#66387),(#66388,#66389),(#66390,#66391),(#66392,
#66393),(#66394,#66395),(#66396,#66397),(#66398,#66399),(#66400,#66401),
(#66402,#66403),(#66404,#66405),(#66406,#66407),(#66408,#66409),(#66410,
#66411),(#66412,#66413),(#66414,#66415),(#66416,#66417),(#66418,#66419),
(#66420,#66421),(#66422,#66423),(#66424,#66425),(#66426,#66427),(#66428,
#66429),(#66430,#66431),(#66432,#66433),(#66434,#66435),(#66436,#66437),
(#66438,#66439),(#66440,#66441),(#66442,#66443),(#66444,#66445),(#66446,
#66447),(#66448,#66449),(#66450,#66451),(#66452,#66453),(#66454,#66455),
(#66456,#66457),(#66458,#66459),(#66460,#66461),(#66462,#66463),(#66464,
#66465),(#66466,#66467),(#66468,#66469),(#66470,#66471)),.UNSPECIFIED.,
 .F.,.F.,.F.)
B_SPLINE_SURFACE_WITH_KNOTS((6,1,1,1,1,1,1,1,1,1,1,1,1,1,1,1,1,1,1,1,1,
1,1,1,1,1,1,1,1,1,1,1,1,1,1,1,1,1,1,1,1,1,1,1,1,1,1,1,1,1,1,1,1,1,1,1,1,
1,1,1,1,1,1,1,1,1,1,1,1,1,1,1,1,1,1,1,1,1,1,1,1,1,1,1,1,1,1,1,1,1,1,1,1,
1,1,1,1,1,1,1,1,1,1,1,1,1,1,1,1,1,1,1,1,1,1,1,1,1,1,1,1,1,1,1,1,1,1,1,1,
1,1,1,1,1,1,1,1,1,1,1,1,1,1,1,1,1,1,1,1,1,1,1,1,1,1,1,1,1,1,1,1,1,1,1,1,
1,1,1,1,1,1,1,1,1,1,1,1,1,1,1,1,1,1,1,1,1,1,1,1,1,1,1,1,1,1,1,1,1,1,1,6),
(2,2),(0.,0.005,0.01,0.015,0.02,0.025,0.03,0.035,0.04,0.045,0.05,0.055,
0.06,0.065,0.07,0.075,0.08,0.085,0.09,0.095,0.1,0.105,0.11,0.115,0.12,0.125,
0.13,0.135,0.14,0.145,0.15,0.155,0.16,0.165,0.17,0.175,0.18,0.185,0.19,
0.195,0.2,0.205,0.21,0.215,0.22,0.225,0.23,0.235,0.24,0.245,0.25,0.255,
0.26,0.265,0.27,0.275,0.28,0.285,0.29,0.295,0.3,0.305,0.31,0.315,0.32,0.325,
0.33,0.335,0.34,0.345,0.35,0.355,0.36,0.365,0.37,0.375,0.38,0.385,0.39,
0.395,0.4,0.405,0.41,0.415,0.42,0.425,0.43,0.435,0.44,0.445,0.45,0.455,
0.46,0.465,0.47,0.475,0.48,0.485,0.49,0.495,0.5,0.505,0.51,0.515,0.52,0.525,
0.53,0.535,0.54,0.545,0.55,0.555,0.56,0.565,0.57,0.575,0.58,0.585,0.59,
0.595,0.6,0.605,0.61,0.615,0.62,0.625,0.63,0.635,0.64,0.645,0.65,0.655,
0.66,0.665,0.67,0.675,0.68,0.685,0.690000000000001,0.695000000000001,0.700000000000001,
0.705000000000001,0.710000000000001,0.715000000000001,0.720000000000001,
0.725000000000001,0.730000000000001,0.735000000000001,0.740000000000001,
0.745000000000001,0.750000000000001,0.755000000000001,0.760000000000001,
0.765000000000001,0.770000000000001,0.775000000000001,0.780000000000001,
0.785000000000001,0.790000000000001,0.795000000000001,0.800000000000001,
0.805000000000001,0.810000000000001,0.815000000000001,0.820000000000001,
0.825000000000001,0.830000000000001,0.835000000000001,0.840000000000001,
0.845000000000001,0.850000000000001,0.855000000000001,0.860000000000001,
0.865000000000001,0.870000000000001,0.875000000000001,0.880000000000001,
0.885000000000001,0.890000000000001,0.895000000000001,0.900000000000001,
0.905000000000001,0.910000000000001,0.915000000000001,0.920000000000001,
0.925000000000001,0.930000000000001,0.935000000000001,0.940000000000001,
0.945000000000001,0.950000000000001,0.955000000000001,0.960000000000001,
0.965000000000001,0.970000000000001,0.975000000000001,0.980000000000001,
0.985000000000001,0.990000000000001,0.995000000000001,1.),(0.,1.2),
 .UNSPECIFIED.)
GEOMETRIC_REPRESENTATION_ITEM()
RATIONAL_B_SPLINE_SURFACE(((1.,1.),(1.,1.),(1.,1.),(1.,1.),(1.,1.),(1.,
1.),(1.,1.),(1.,1.),(1.,1.),(1.,1.),(1.,1.),(1.,1.),(1.,1.),(1.,1.),(1.,
1.),(1.,1.),(1.,1.),(1.,1.),(1.,1.),(1.,1.),(1.,1.),(1.,1.),(1.,1.),(1.,
1.),(1.,1.),(1.,1.),(1.,1.),(1.,1.),(1.,1.),(1.,1.),(1.,1.),(1.,1.),(1.,
1.),(1.,1.),(1.,1.),(1.,1.),(1.,1.),(1.,1.),(1.,1.),(1.,1.),(1.,1.),(1.,
1.),(1.,1.),(1.,1.),(1.,1.),(1.,1.),(1.,1.),(1.,1.),(1.,1.),(1.,1.),(1.,
1.),(1.,1.),(1.,1.),(1.,1.),(1.,1.),(1.,1.),(1.,1.),(1.,1.),(1.,1.),(1.,
1.),(1.,1.),(1.,1.),(1.,1.),(1.,1.),(1.,1.),(1.,1.),(1.,1.),(1.,1.),(1.,
1.),(1.,1.),(1.,1.),(1.,1.),(1.,1.),(1.,1.),(1.,1.),(1.,1.),(1.,1.),(1.,
1.),(1.,1.),(1.,1.),(1.,1.),(1.,1.),(1.,1.),(1.,1.),(1.,1.),(1.,1.),(1.,
1.),(1.,1.),(1.,1.),(1.,1.),(1.,1.),(1.,1.),(1.,1.),(1.,1.),(1.,1.),(1.,
1.),(1.,1.),(1.,1.),(1.,1.),(1.,1.),(1.,1.),(1.,1.),(1.,1.),(1.,1.),(1.,
1.),(1.,1.),(1.,1.),(1.,1.),(1.,1.),(1.,1.),(1.,1.),(1.,1.),(1.,1.),(1.,
1.),(1.,1.),(1.,1.),(1.,1.),(1.,1.),(1.,1.),(1.,1.),(1.,1.),(1.,1.),(1.,
1.),(1.,1.),(1.,1.),(1.,1.),(1.,1.),(1.,1.),(1.,1.),(1.,1.),(1.,1.),(1.,
1.),(1.,1.),(1.,1.),(1.,1.),(1.,1.),(1.,1.),(1.,1.),(1.,1.),(1.,1.),(1.,
1.),(1.,1.),(1.,1.),(1.,1.),(1.,1.),(1.,1.),(1.,1.),(1.,1.),(1.,1.),(1.,
1.),(1.,1.),(1.,1.),(1.,1.),(1.,1.),(1.,1.),(1.,1.),(1.,1.),(1.,1.),(1.,
1.),(1.,1.),(1.,1.),(1.,1.),(1.,1.),(1.,1.),(1.,1.),(1.,1.),(1.,1.),(1.,
1.),(1.,1.),(1.,1.),(1.,1.),(1.,1.),(1.,1.),(1.,1.),(1.,1.),(1.,1.),(1.,
1.),(1.,1.),(1.,1.),(1.,1.),(1.,1.),(1.,1.),(1.,1.),(1.,1.),(1.,1.),(1.,
1.),(1.,1.),(1.,1.),(1.,1.),(1.,1.),(1.,1.),(1.,1.),(1.,1.),(1.,1.),(1.,
1.),(1.,1.),(1.,1.),(1.,1.),(1.,1.),(1.,1.),(1.,1.),(1.,1.),(1.,1.),(1.,
1.),(1.,1.)))
REPRESENTATION_ITEM('')
SURFACE()
);
#899=(
BOUNDED_SURFACE()
B_SPLINE_SURFACE(5,1,((#66958,#66959),(#66960,#66961),(#66962,#66963),(#66964,
#66965),(#66966,#66967),(#66968,#66969),(#66970,#66971),(#66972,#66973),
(#66974,#66975),(#66976,#66977),(#66978,#66979),(#66980,#66981),(#66982,
#66983),(#66984,#66985),(#66986,#66987),(#66988,#66989),(#66990,#66991),
(#66992,#66993),(#66994,#66995),(#66996,#66997),(#66998,#66999),(#67000,
#67001),(#67002,#67003),(#67004,#67005),(#67006,#67007),(#67008,#67009),
(#67010,#67011),(#67012,#67013),(#67014,#67015),(#67016,#67017),(#67018,
#67019),(#67020,#67021),(#67022,#67023),(#67024,#67025),(#67026,#67027),
(#67028,#67029),(#67030,#67031),(#67032,#67033),(#67034,#67035),(#67036,
#67037),(#67038,#67039),(#67040,#67041),(#67042,#67043),(#67044,#67045),
(#67046,#67047),(#67048,#67049),(#67050,#67051),(#67052,#67053),(#67054,
#67055),(#67056,#67057),(#67058,#67059),(#67060,#67061),(#67062,#67063),
(#67064,#67065),(#67066,#67067),(#67068,#67069),(#67070,#67071),(#67072,
#67073),(#67074,#67075),(#67076,#67077),(#67078,#67079),(#67080,#67081),
(#67082,#67083),(#67084,#67085),(#67086,#67087),(#67088,#67089),(#67090,
#67091),(#67092,#67093),(#67094,#67095),(#67096,#67097),(#67098,#67099),
(#67100,#67101),(#67102,#67103),(#67104,#67105),(#67106,#67107),(#67108,
#67109),(#67110,#67111),(#67112,#67113),(#67114,#67115),(#67116,#67117),
(#67118,#67119),(#67120,#67121),(#67122,#67123),(#67124,#67125),(#67126,
#67127),(#67128,#67129),(#67130,#67131),(#67132,#67133),(#67134,#67135),
(#67136,#67137),(#67138,#67139),(#67140,#67141),(#67142,#67143),(#67144,
#67145),(#67146,#67147),(#67148,#67149),(#67150,#67151),(#67152,#67153),
(#67154,#67155),(#67156,#67157),(#67158,#67159),(#67160,#67161),(#67162,
#67163),(#67164,#67165),(#67166,#67167),(#67168,#67169),(#67170,#67171),
(#67172,#67173),(#67174,#67175),(#67176,#67177),(#67178,#67179),(#67180,
#67181),(#67182,#67183),(#67184,#67185),(#67186,#67187),(#67188,#67189),
(#67190,#67191),(#67192,#67193),(#67194,#67195),(#67196,#67197),(#67198,
#67199),(#67200,#67201),(#67202,#67203),(#67204,#67205),(#67206,#67207),
(#67208,#67209),(#67210,#67211),(#67212,#67213),(#67214,#67215),(#67216,
#67217),(#67218,#67219),(#67220,#67221),(#67222,#67223),(#67224,#67225),
(#67226,#67227),(#67228,#67229),(#67230,#67231),(#67232,#67233),(#67234,
#67235),(#67236,#67237),(#67238,#67239),(#67240,#67241),(#67242,#67243),
(#67244,#67245),(#67246,#67247),(#67248,#67249),(#67250,#67251),(#67252,
#67253),(#67254,#67255),(#67256,#67257),(#67258,#67259),(#67260,#67261),
(#67262,#67263),(#67264,#67265),(#67266,#67267),(#67268,#67269),(#67270,
#67271),(#67272,#67273),(#67274,#67275),(#67276,#67277),(#67278,#67279),
(#67280,#67281),(#67282,#67283),(#67284,#67285),(#67286,#67287),(#67288,
#67289),(#67290,#67291),(#67292,#67293),(#67294,#67295),(#67296,#67297),
(#67298,#67299),(#67300,#67301),(#67302,#67303),(#67304,#67305),(#67306,
#67307),(#67308,#67309),(#67310,#67311),(#67312,#67313),(#67314,#67315),
(#67316,#67317),(#67318,#67319),(#67320,#67321),(#67322,#67323),(#67324,
#67325),(#67326,#67327),(#67328,#67329),(#67330,#67331),(#67332,#67333),
(#67334,#67335),(#67336,#67337),(#67338,#67339),(#67340,#67341),(#67342,
#67343),(#67344,#67345),(#67346,#67347),(#67348,#67349),(#67350,#67351),
(#67352,#67353),(#67354,#67355),(#67356,#67357),(#67358,#67359),(#67360,
#67361),(#67362,#67363),(#67364,#67365),(#67366,#67367)),.UNSPECIFIED.,
 .F.,.F.,.F.)
B_SPLINE_SURFACE_WITH_KNOTS((6,1,1,1,1,1,1,1,1,1,1,1,1,1,1,1,1,1,1,1,1,
1,1,1,1,1,1,1,1,1,1,1,1,1,1,1,1,1,1,1,1,1,1,1,1,1,1,1,1,1,1,1,1,1,1,1,1,
1,1,1,1,1,1,1,1,1,1,1,1,1,1,1,1,1,1,1,1,1,1,1,1,1,1,1,1,1,1,1,1,1,1,1,1,
1,1,1,1,1,1,1,1,1,1,1,1,1,1,1,1,1,1,1,1,1,1,1,1,1,1,1,1,1,1,1,1,1,1,1,1,
1,1,1,1,1,1,1,1,1,1,1,1,1,1,1,1,1,1,1,1,1,1,1,1,1,1,1,1,1,1,1,1,1,1,1,1,
1,1,1,1,1,1,1,1,1,1,1,1,1,1,1,1,1,1,1,1,1,1,1,1,1,1,1,1,1,1,1,1,1,1,1,6),
(2,2),(0.,0.005,0.01,0.015,0.02,0.025,0.03,0.035,0.04,0.045,0.05,0.055,
0.06,0.065,0.07,0.075,0.08,0.085,0.09,0.095,0.1,0.105,0.11,0.115,0.12,0.125,
0.13,0.135,0.14,0.145,0.15,0.155,0.16,0.165,0.17,0.175,0.18,0.185,0.19,
0.195,0.2,0.205,0.21,0.215,0.22,0.225,0.23,0.235,0.24,0.245,0.25,0.255,
0.26,0.265,0.27,0.275,0.28,0.285,0.29,0.295,0.3,0.305,0.31,0.315,0.32,0.325,
0.33,0.335,0.34,0.345,0.35,0.355,0.36,0.365,0.37,0.375,0.38,0.385,0.39,
0.395,0.4,0.405,0.41,0.415,0.42,0.425,0.43,0.435,0.44,0.445,0.45,0.455,
0.46,0.465,0.47,0.475,0.48,0.485,0.49,0.495,0.5,0.505,0.51,0.515,0.52,0.525,
0.53,0.535,0.54,0.545,0.55,0.555,0.56,0.565,0.57,0.575,0.58,0.585,0.59,
0.595,0.6,0.605,0.61,0.615,0.62,0.625,0.63,0.635,0.64,0.645,0.65,0.655,
0.66,0.665,0.67,0.675,0.68,0.685,0.690000000000001,0.695000000000001,0.700000000000001,
0.705000000000001,0.710000000000001,0.715000000000001,0.720000000000001,
0.725000000000001,0.730000000000001,0.735000000000001,0.740000000000001,
0.745000000000001,0.750000000000001,0.755000000000001,0.760000000000001,
0.765000000000001,0.770000000000001,0.775000000000001,0.780000000000001,
0.785000000000001,0.790000000000001,0.795000000000001,0.800000000000001,
0.805000000000001,0.810000000000001,0.815000000000001,0.820000000000001,
0.825000000000001,0.830000000000001,0.835000000000001,0.840000000000001,
0.845000000000001,0.850000000000001,0.855000000000001,0.860000000000001,
0.865000000000001,0.870000000000001,0.875000000000001,0.880000000000001,
0.885000000000001,0.890000000000001,0.895000000000001,0.900000000000001,
0.905000000000001,0.910000000000001,0.915000000000001,0.920000000000001,
0.925000000000001,0.930000000000001,0.935000000000001,0.940000000000001,
0.945000000000001,0.950000000000001,0.955000000000001,0.960000000000001,
0.965000000000001,0.970000000000001,0.975000000000001,0.980000000000001,
0.985000000000001,0.990000000000001,0.995000000000001,1.),(0.,1.2),
 .UNSPECIFIED.)
GEOMETRIC_REPRESENTATION_ITEM()
RATIONAL_B_SPLINE_SURFACE(((1.,1.),(1.,1.),(1.,1.),(1.,1.),(1.,1.),(1.,
1.),(1.,1.),(1.,1.),(1.,1.),(1.,1.),(1.,1.),(1.,1.),(1.,1.),(1.,1.),(1.,
1.),(1.,1.),(1.,1.),(1.,1.),(1.,1.),(1.,1.),(1.,1.),(1.,1.),(1.,1.),(1.,
1.),(1.,1.),(1.,1.),(1.,1.),(1.,1.),(1.,1.),(1.,1.),(1.,1.),(1.,1.),(1.,
1.),(1.,1.),(1.,1.),(1.,1.),(1.,1.),(1.,1.),(1.,1.),(1.,1.),(1.,1.),(1.,
1.),(1.,1.),(1.,1.),(1.,1.),(1.,1.),(1.,1.),(1.,1.),(1.,1.),(1.,1.),(1.,
1.),(1.,1.),(1.,1.),(1.,1.),(1.,1.),(1.,1.),(1.,1.),(1.,1.),(1.,1.),(1.,
1.),(1.,1.),(1.,1.),(1.,1.),(1.,1.),(1.,1.),(1.,1.),(1.,1.),(1.,1.),(1.,
1.),(1.,1.),(1.,1.),(1.,1.),(1.,1.),(1.,1.),(1.,1.),(1.,1.),(1.,1.),(1.,
1.),(1.,1.),(1.,1.),(1.,1.),(1.,1.),(1.,1.),(1.,1.),(1.,1.),(1.,1.),(1.,
1.),(1.,1.),(1.,1.),(1.,1.),(1.,1.),(1.,1.),(1.,1.),(1.,1.),(1.,1.),(1.,
1.),(1.,1.),(1.,1.),(1.,1.),(1.,1.),(1.,1.),(1.,1.),(1.,1.),(1.,1.),(1.,
1.),(1.,1.),(1.,1.),(1.,1.),(1.,1.),(1.,1.),(1.,1.),(1.,1.),(1.,1.),(1.,
1.),(1.,1.),(1.,1.),(1.,1.),(1.,1.),(1.,1.),(1.,1.),(1.,1.),(1.,1.),(1.,
1.),(1.,1.),(1.,1.),(1.,1.),(1.,1.),(1.,1.),(1.,1.),(1.,1.),(1.,1.),(1.,
1.),(1.,1.),(1.,1.),(1.,1.),(1.,1.),(1.,1.),(1.,1.),(1.,1.),(1.,1.),(1.,
1.),(1.,1.),(1.,1.),(1.,1.),(1.,1.),(1.,1.),(1.,1.),(1.,1.),(1.,1.),(1.,
1.),(1.,1.),(1.,1.),(1.,1.),(1.,1.),(1.,1.),(1.,1.),(1.,1.),(1.,1.),(1.,
1.),(1.,1.),(1.,1.),(1.,1.),(1.,1.),(1.,1.),(1.,1.),(1.,1.),(1.,1.),(1.,
1.),(1.,1.),(1.,1.),(1.,1.),(1.,1.),(1.,1.),(1.,1.),(1.,1.),(1.,1.),(1.,
1.),(1.,1.),(1.,1.),(1.,1.),(1.,1.),(1.,1.),(1.,1.),(1.,1.),(1.,1.),(1.,
1.),(1.,1.),(1.,1.),(1.,1.),(1.,1.),(1.,1.),(1.,1.),(1.,1.),(1.,1.),(1.,
1.),(1.,1.),(1.,1.),(1.,1.),(1.,1.),(1.,1.),(1.,1.),(1.,1.),(1.,1.),(1.,
1.),(1.,1.)))
REPRESENTATION_ITEM('')
SURFACE()
);
#900=(
BOUNDED_SURFACE()
B_SPLINE_SURFACE(5,1,((#67854,#67855),(#67856,#67857),(#67858,#67859),(#67860,
#67861),(#67862,#67863),(#67864,#67865),(#67866,#67867),(#67868,#67869),
(#67870,#67871),(#67872,#67873),(#67874,#67875),(#67876,#67877),(#67878,
#67879),(#67880,#67881),(#67882,#67883),(#67884,#67885),(#67886,#67887),
(#67888,#67889),(#67890,#67891),(#67892,#67893),(#67894,#67895),(#67896,
#67897),(#67898,#67899),(#67900,#67901),(#67902,#67903),(#67904,#67905),
(#67906,#67907),(#67908,#67909),(#67910,#67911),(#67912,#67913),(#67914,
#67915),(#67916,#67917),(#67918,#67919),(#67920,#67921),(#67922,#67923),
(#67924,#67925),(#67926,#67927),(#67928,#67929),(#67930,#67931),(#67932,
#67933),(#67934,#67935),(#67936,#67937),(#67938,#67939),(#67940,#67941),
(#67942,#67943),(#67944,#67945),(#67946,#67947),(#67948,#67949),(#67950,
#67951),(#67952,#67953),(#67954,#67955),(#67956,#67957),(#67958,#67959),
(#67960,#67961),(#67962,#67963),(#67964,#67965),(#67966,#67967),(#67968,
#67969),(#67970,#67971),(#67972,#67973),(#67974,#67975),(#67976,#67977),
(#67978,#67979),(#67980,#67981),(#67982,#67983),(#67984,#67985),(#67986,
#67987),(#67988,#67989),(#67990,#67991),(#67992,#67993),(#67994,#67995),
(#67996,#67997),(#67998,#67999),(#68000,#68001),(#68002,#68003),(#68004,
#68005),(#68006,#68007),(#68008,#68009),(#68010,#68011),(#68012,#68013),
(#68014,#68015),(#68016,#68017),(#68018,#68019),(#68020,#68021),(#68022,
#68023),(#68024,#68025),(#68026,#68027),(#68028,#68029),(#68030,#68031),
(#68032,#68033),(#68034,#68035),(#68036,#68037),(#68038,#68039),(#68040,
#68041),(#68042,#68043),(#68044,#68045),(#68046,#68047),(#68048,#68049),
(#68050,#68051),(#68052,#68053),(#68054,#68055),(#68056,#68057),(#68058,
#68059),(#68060,#68061),(#68062,#68063),(#68064,#68065),(#68066,#68067),
(#68068,#68069),(#68070,#68071),(#68072,#68073),(#68074,#68075),(#68076,
#68077),(#68078,#68079),(#68080,#68081),(#68082,#68083),(#68084,#68085),
(#68086,#68087),(#68088,#68089),(#68090,#68091),(#68092,#68093),(#68094,
#68095),(#68096,#68097),(#68098,#68099),(#68100,#68101),(#68102,#68103),
(#68104,#68105),(#68106,#68107),(#68108,#68109),(#68110,#68111),(#68112,
#68113),(#68114,#68115),(#68116,#68117),(#68118,#68119),(#68120,#68121),
(#68122,#68123),(#68124,#68125),(#68126,#68127),(#68128,#68129),(#68130,
#68131),(#68132,#68133),(#68134,#68135),(#68136,#68137),(#68138,#68139),
(#68140,#68141),(#68142,#68143),(#68144,#68145),(#68146,#68147),(#68148,
#68149),(#68150,#68151),(#68152,#68153),(#68154,#68155),(#68156,#68157),
(#68158,#68159),(#68160,#68161),(#68162,#68163),(#68164,#68165),(#68166,
#68167),(#68168,#68169),(#68170,#68171),(#68172,#68173),(#68174,#68175),
(#68176,#68177),(#68178,#68179),(#68180,#68181),(#68182,#68183),(#68184,
#68185),(#68186,#68187),(#68188,#68189),(#68190,#68191),(#68192,#68193),
(#68194,#68195),(#68196,#68197),(#68198,#68199),(#68200,#68201),(#68202,
#68203),(#68204,#68205),(#68206,#68207),(#68208,#68209),(#68210,#68211),
(#68212,#68213),(#68214,#68215),(#68216,#68217),(#68218,#68219),(#68220,
#68221),(#68222,#68223),(#68224,#68225),(#68226,#68227),(#68228,#68229),
(#68230,#68231),(#68232,#68233),(#68234,#68235),(#68236,#68237),(#68238,
#68239),(#68240,#68241),(#68242,#68243),(#68244,#68245),(#68246,#68247),
(#68248,#68249),(#68250,#68251),(#68252,#68253),(#68254,#68255),(#68256,
#68257),(#68258,#68259),(#68260,#68261),(#68262,#68263)),.UNSPECIFIED.,
 .F.,.F.,.F.)
B_SPLINE_SURFACE_WITH_KNOTS((6,1,1,1,1,1,1,1,1,1,1,1,1,1,1,1,1,1,1,1,1,
1,1,1,1,1,1,1,1,1,1,1,1,1,1,1,1,1,1,1,1,1,1,1,1,1,1,1,1,1,1,1,1,1,1,1,1,
1,1,1,1,1,1,1,1,1,1,1,1,1,1,1,1,1,1,1,1,1,1,1,1,1,1,1,1,1,1,1,1,1,1,1,1,
1,1,1,1,1,1,1,1,1,1,1,1,1,1,1,1,1,1,1,1,1,1,1,1,1,1,1,1,1,1,1,1,1,1,1,1,
1,1,1,1,1,1,1,1,1,1,1,1,1,1,1,1,1,1,1,1,1,1,1,1,1,1,1,1,1,1,1,1,1,1,1,1,
1,1,1,1,1,1,1,1,1,1,1,1,1,1,1,1,1,1,1,1,1,1,1,1,1,1,1,1,1,1,1,1,1,1,1,6),
(2,2),(0.,0.005,0.01,0.015,0.02,0.025,0.03,0.035,0.04,0.045,0.05,0.055,
0.06,0.065,0.07,0.075,0.08,0.085,0.09,0.095,0.1,0.105,0.11,0.115,0.12,0.125,
0.13,0.135,0.14,0.145,0.15,0.155,0.16,0.165,0.17,0.175,0.18,0.185,0.19,
0.195,0.2,0.205,0.21,0.215,0.22,0.225,0.23,0.235,0.24,0.245,0.25,0.255,
0.26,0.265,0.27,0.275,0.28,0.285,0.29,0.295,0.3,0.305,0.31,0.315,0.32,0.325,
0.33,0.335,0.34,0.345,0.35,0.355,0.36,0.365,0.37,0.375,0.38,0.385,0.39,
0.395,0.4,0.405,0.41,0.415,0.42,0.425,0.43,0.435,0.44,0.445,0.45,0.455,
0.46,0.465,0.47,0.475,0.48,0.485,0.49,0.495,0.5,0.505,0.51,0.515,0.52,0.525,
0.53,0.535,0.54,0.545,0.55,0.555,0.56,0.565,0.57,0.575,0.58,0.585,0.59,
0.595,0.6,0.605,0.61,0.615,0.62,0.625,0.63,0.635,0.64,0.645,0.65,0.655,
0.66,0.665,0.67,0.675,0.68,0.685,0.690000000000001,0.695000000000001,0.700000000000001,
0.705000000000001,0.710000000000001,0.715000000000001,0.720000000000001,
0.725000000000001,0.730000000000001,0.735000000000001,0.740000000000001,
0.745000000000001,0.750000000000001,0.755000000000001,0.760000000000001,
0.765000000000001,0.770000000000001,0.775000000000001,0.780000000000001,
0.785000000000001,0.790000000000001,0.795000000000001,0.800000000000001,
0.805000000000001,0.810000000000001,0.815000000000001,0.820000000000001,
0.825000000000001,0.830000000000001,0.835000000000001,0.840000000000001,
0.845000000000001,0.850000000000001,0.855000000000001,0.860000000000001,
0.865000000000001,0.870000000000001,0.875000000000001,0.880000000000001,
0.885000000000001,0.890000000000001,0.895000000000001,0.900000000000001,
0.905000000000001,0.910000000000001,0.915000000000001,0.920000000000001,
0.925000000000001,0.930000000000001,0.935000000000001,0.940000000000001,
0.945000000000001,0.950000000000001,0.955000000000001,0.960000000000001,
0.965000000000001,0.970000000000001,0.975000000000001,0.980000000000001,
0.985000000000001,0.990000000000001,0.995000000000001,1.),(0.,1.2),
 .UNSPECIFIED.)
GEOMETRIC_REPRESENTATION_ITEM()
RATIONAL_B_SPLINE_SURFACE(((1.,1.),(1.,1.),(1.,1.),(1.,1.),(1.,1.),(1.,
1.),(1.,1.),(1.,1.),(1.,1.),(1.,1.),(1.,1.),(1.,1.),(1.,1.),(1.,1.),(1.,
1.),(1.,1.),(1.,1.),(1.,1.),(1.,1.),(1.,1.),(1.,1.),(1.,1.),(1.,1.),(1.,
1.),(1.,1.),(1.,1.),(1.,1.),(1.,1.),(1.,1.),(1.,1.),(1.,1.),(1.,1.),(1.,
1.),(1.,1.),(1.,1.),(1.,1.),(1.,1.),(1.,1.),(1.,1.),(1.,1.),(1.,1.),(1.,
1.),(1.,1.),(1.,1.),(1.,1.),(1.,1.),(1.,1.),(1.,1.),(1.,1.),(1.,1.),(1.,
1.),(1.,1.),(1.,1.),(1.,1.),(1.,1.),(1.,1.),(1.,1.),(1.,1.),(1.,1.),(1.,
1.),(1.,1.),(1.,1.),(1.,1.),(1.,1.),(1.,1.),(1.,1.),(1.,1.),(1.,1.),(1.,
1.),(1.,1.),(1.,1.),(1.,1.),(1.,1.),(1.,1.),(1.,1.),(1.,1.),(1.,1.),(1.,
1.),(1.,1.),(1.,1.),(1.,1.),(1.,1.),(1.,1.),(1.,1.),(1.,1.),(1.,1.),(1.,
1.),(1.,1.),(1.,1.),(1.,1.),(1.,1.),(1.,1.),(1.,1.),(1.,1.),(1.,1.),(1.,
1.),(1.,1.),(1.,1.),(1.,1.),(1.,1.),(1.,1.),(1.,1.),(1.,1.),(1.,1.),(1.,
1.),(1.,1.),(1.,1.),(1.,1.),(1.,1.),(1.,1.),(1.,1.),(1.,1.),(1.,1.),(1.,
1.),(1.,1.),(1.,1.),(1.,1.),(1.,1.),(1.,1.),(1.,1.),(1.,1.),(1.,1.),(1.,
1.),(1.,1.),(1.,1.),(1.,1.),(1.,1.),(1.,1.),(1.,1.),(1.,1.),(1.,1.),(1.,
1.),(1.,1.),(1.,1.),(1.,1.),(1.,1.),(1.,1.),(1.,1.),(1.,1.),(1.,1.),(1.,
1.),(1.,1.),(1.,1.),(1.,1.),(1.,1.),(1.,1.),(1.,1.),(1.,1.),(1.,1.),(1.,
1.),(1.,1.),(1.,1.),(1.,1.),(1.,1.),(1.,1.),(1.,1.),(1.,1.),(1.,1.),(1.,
1.),(1.,1.),(1.,1.),(1.,1.),(1.,1.),(1.,1.),(1.,1.),(1.,1.),(1.,1.),(1.,
1.),(1.,1.),(1.,1.),(1.,1.),(1.,1.),(1.,1.),(1.,1.),(1.,1.),(1.,1.),(1.,
1.),(1.,1.),(1.,1.),(1.,1.),(1.,1.),(1.,1.),(1.,1.),(1.,1.),(1.,1.),(1.,
1.),(1.,1.),(1.,1.),(1.,1.),(1.,1.),(1.,1.),(1.,1.),(1.,1.),(1.,1.),(1.,
1.),(1.,1.),(1.,1.),(1.,1.),(1.,1.),(1.,1.),(1.,1.),(1.,1.),(1.,1.),(1.,
1.),(1.,1.)))
REPRESENTATION_ITEM('')
SURFACE()
);
#901=(
BOUNDED_SURFACE()
B_SPLINE_SURFACE(5,1,((#68750,#68751),(#68752,#68753),(#68754,#68755),(#68756,
#68757),(#68758,#68759),(#68760,#68761),(#68762,#68763),(#68764,#68765),
(#68766,#68767),(#68768,#68769),(#68770,#68771),(#68772,#68773),(#68774,
#68775),(#68776,#68777),(#68778,#68779),(#68780,#68781),(#68782,#68783),
(#68784,#68785),(#68786,#68787),(#68788,#68789),(#68790,#68791),(#68792,
#68793),(#68794,#68795),(#68796,#68797),(#68798,#68799),(#68800,#68801),
(#68802,#68803),(#68804,#68805),(#68806,#68807),(#68808,#68809),(#68810,
#68811),(#68812,#68813),(#68814,#68815),(#68816,#68817),(#68818,#68819),
(#68820,#68821),(#68822,#68823),(#68824,#68825),(#68826,#68827),(#68828,
#68829),(#68830,#68831),(#68832,#68833),(#68834,#68835),(#68836,#68837),
(#68838,#68839),(#68840,#68841),(#68842,#68843),(#68844,#68845),(#68846,
#68847),(#68848,#68849),(#68850,#68851),(#68852,#68853),(#68854,#68855),
(#68856,#68857),(#68858,#68859),(#68860,#68861),(#68862,#68863),(#68864,
#68865),(#68866,#68867),(#68868,#68869),(#68870,#68871),(#68872,#68873),
(#68874,#68875),(#68876,#68877),(#68878,#68879),(#68880,#68881),(#68882,
#68883),(#68884,#68885),(#68886,#68887),(#68888,#68889),(#68890,#68891),
(#68892,#68893),(#68894,#68895),(#68896,#68897),(#68898,#68899),(#68900,
#68901),(#68902,#68903),(#68904,#68905),(#68906,#68907),(#68908,#68909),
(#68910,#68911),(#68912,#68913),(#68914,#68915),(#68916,#68917),(#68918,
#68919),(#68920,#68921),(#68922,#68923),(#68924,#68925),(#68926,#68927),
(#68928,#68929),(#68930,#68931),(#68932,#68933),(#68934,#68935),(#68936,
#68937),(#68938,#68939),(#68940,#68941),(#68942,#68943),(#68944,#68945),
(#68946,#68947),(#68948,#68949),(#68950,#68951),(#68952,#68953),(#68954,
#68955),(#68956,#68957),(#68958,#68959),(#68960,#68961),(#68962,#68963),
(#68964,#68965),(#68966,#68967),(#68968,#68969),(#68970,#68971),(#68972,
#68973),(#68974,#68975),(#68976,#68977),(#68978,#68979),(#68980,#68981),
(#68982,#68983),(#68984,#68985),(#68986,#68987),(#68988,#68989),(#68990,
#68991),(#68992,#68993),(#68994,#68995),(#68996,#68997),(#68998,#68999),
(#69000,#69001),(#69002,#69003),(#69004,#69005),(#69006,#69007),(#69008,
#69009),(#69010,#69011),(#69012,#69013),(#69014,#69015),(#69016,#69017),
(#69018,#69019),(#69020,#69021),(#69022,#69023),(#69024,#69025),(#69026,
#69027),(#69028,#69029),(#69030,#69031),(#69032,#69033),(#69034,#69035),
(#69036,#69037),(#69038,#69039),(#69040,#69041),(#69042,#69043),(#69044,
#69045),(#69046,#69047),(#69048,#69049),(#69050,#69051),(#69052,#69053),
(#69054,#69055),(#69056,#69057),(#69058,#69059),(#69060,#69061),(#69062,
#69063),(#69064,#69065),(#69066,#69067),(#69068,#69069),(#69070,#69071),
(#69072,#69073),(#69074,#69075),(#69076,#69077),(#69078,#69079),(#69080,
#69081),(#69082,#69083),(#69084,#69085),(#69086,#69087),(#69088,#69089),
(#69090,#69091),(#69092,#69093),(#69094,#69095),(#69096,#69097),(#69098,
#69099),(#69100,#69101),(#69102,#69103),(#69104,#69105),(#69106,#69107),
(#69108,#69109),(#69110,#69111),(#69112,#69113),(#69114,#69115),(#69116,
#69117),(#69118,#69119),(#69120,#69121),(#69122,#69123),(#69124,#69125),
(#69126,#69127),(#69128,#69129),(#69130,#69131),(#69132,#69133),(#69134,
#69135),(#69136,#69137),(#69138,#69139),(#69140,#69141),(#69142,#69143),
(#69144,#69145),(#69146,#69147),(#69148,#69149),(#69150,#69151),(#69152,
#69153),(#69154,#69155),(#69156,#69157),(#69158,#69159)),.UNSPECIFIED.,
 .F.,.F.,.F.)
B_SPLINE_SURFACE_WITH_KNOTS((6,1,1,1,1,1,1,1,1,1,1,1,1,1,1,1,1,1,1,1,1,
1,1,1,1,1,1,1,1,1,1,1,1,1,1,1,1,1,1,1,1,1,1,1,1,1,1,1,1,1,1,1,1,1,1,1,1,
1,1,1,1,1,1,1,1,1,1,1,1,1,1,1,1,1,1,1,1,1,1,1,1,1,1,1,1,1,1,1,1,1,1,1,1,
1,1,1,1,1,1,1,1,1,1,1,1,1,1,1,1,1,1,1,1,1,1,1,1,1,1,1,1,1,1,1,1,1,1,1,1,
1,1,1,1,1,1,1,1,1,1,1,1,1,1,1,1,1,1,1,1,1,1,1,1,1,1,1,1,1,1,1,1,1,1,1,1,
1,1,1,1,1,1,1,1,1,1,1,1,1,1,1,1,1,1,1,1,1,1,1,1,1,1,1,1,1,1,1,1,1,1,1,6),
(2,2),(0.,0.005,0.01,0.015,0.02,0.025,0.03,0.035,0.04,0.045,0.05,0.055,
0.06,0.065,0.07,0.075,0.08,0.085,0.09,0.095,0.1,0.105,0.11,0.115,0.12,0.125,
0.13,0.135,0.14,0.145,0.15,0.155,0.16,0.165,0.17,0.175,0.18,0.185,0.19,
0.195,0.2,0.205,0.21,0.215,0.22,0.225,0.23,0.235,0.24,0.245,0.25,0.255,
0.26,0.265,0.27,0.275,0.28,0.285,0.29,0.295,0.3,0.305,0.31,0.315,0.32,0.325,
0.33,0.335,0.34,0.345,0.35,0.355,0.36,0.365,0.37,0.375,0.38,0.385,0.39,
0.395,0.4,0.405,0.41,0.415,0.42,0.425,0.43,0.435,0.44,0.445,0.45,0.455,
0.46,0.465,0.47,0.475,0.48,0.485,0.49,0.495,0.5,0.505,0.51,0.515,0.52,0.525,
0.53,0.535,0.54,0.545,0.55,0.555,0.56,0.565,0.57,0.575,0.58,0.585,0.59,
0.595,0.6,0.605,0.61,0.615,0.62,0.625,0.63,0.635,0.64,0.645,0.65,0.655,
0.66,0.665,0.67,0.675,0.68,0.685,0.690000000000001,0.695000000000001,0.700000000000001,
0.705000000000001,0.710000000000001,0.715000000000001,0.720000000000001,
0.725000000000001,0.730000000000001,0.735000000000001,0.740000000000001,
0.745000000000001,0.750000000000001,0.755000000000001,0.760000000000001,
0.765000000000001,0.770000000000001,0.775000000000001,0.780000000000001,
0.785000000000001,0.790000000000001,0.795000000000001,0.800000000000001,
0.805000000000001,0.810000000000001,0.815000000000001,0.820000000000001,
0.825000000000001,0.830000000000001,0.835000000000001,0.840000000000001,
0.845000000000001,0.850000000000001,0.855000000000001,0.860000000000001,
0.865000000000001,0.870000000000001,0.875000000000001,0.880000000000001,
0.885000000000001,0.890000000000001,0.895000000000001,0.900000000000001,
0.905000000000001,0.910000000000001,0.915000000000001,0.920000000000001,
0.925000000000001,0.930000000000001,0.935000000000001,0.940000000000001,
0.945000000000001,0.950000000000001,0.955000000000001,0.960000000000001,
0.965000000000001,0.970000000000001,0.975000000000001,0.980000000000001,
0.985000000000001,0.990000000000001,0.995000000000001,1.),(0.,1.2),
 .UNSPECIFIED.)
GEOMETRIC_REPRESENTATION_ITEM()
RATIONAL_B_SPLINE_SURFACE(((1.,1.),(1.,1.),(1.,1.),(1.,1.),(1.,1.),(1.,
1.),(1.,1.),(1.,1.),(1.,1.),(1.,1.),(1.,1.),(1.,1.),(1.,1.),(1.,1.),(1.,
1.),(1.,1.),(1.,1.),(1.,1.),(1.,1.),(1.,1.),(1.,1.),(1.,1.),(1.,1.),(1.,
1.),(1.,1.),(1.,1.),(1.,1.),(1.,1.),(1.,1.),(1.,1.),(1.,1.),(1.,1.),(1.,
1.),(1.,1.),(1.,1.),(1.,1.),(1.,1.),(1.,1.),(1.,1.),(1.,1.),(1.,1.),(1.,
1.),(1.,1.),(1.,1.),(1.,1.),(1.,1.),(1.,1.),(1.,1.),(1.,1.),(1.,1.),(1.,
1.),(1.,1.),(1.,1.),(1.,1.),(1.,1.),(1.,1.),(1.,1.),(1.,1.),(1.,1.),(1.,
1.),(1.,1.),(1.,1.),(1.,1.),(1.,1.),(1.,1.),(1.,1.),(1.,1.),(1.,1.),(1.,
1.),(1.,1.),(1.,1.),(1.,1.),(1.,1.),(1.,1.),(1.,1.),(1.,1.),(1.,1.),(1.,
1.),(1.,1.),(1.,1.),(1.,1.),(1.,1.),(1.,1.),(1.,1.),(1.,1.),(1.,1.),(1.,
1.),(1.,1.),(1.,1.),(1.,1.),(1.,1.),(1.,1.),(1.,1.),(1.,1.),(1.,1.),(1.,
1.),(1.,1.),(1.,1.),(1.,1.),(1.,1.),(1.,1.),(1.,1.),(1.,1.),(1.,1.),(1.,
1.),(1.,1.),(1.,1.),(1.,1.),(1.,1.),(1.,1.),(1.,1.),(1.,1.),(1.,1.),(1.,
1.),(1.,1.),(1.,1.),(1.,1.),(1.,1.),(1.,1.),(1.,1.),(1.,1.),(1.,1.),(1.,
1.),(1.,1.),(1.,1.),(1.,1.),(1.,1.),(1.,1.),(1.,1.),(1.,1.),(1.,1.),(1.,
1.),(1.,1.),(1.,1.),(1.,1.),(1.,1.),(1.,1.),(1.,1.),(1.,1.),(1.,1.),(1.,
1.),(1.,1.),(1.,1.),(1.,1.),(1.,1.),(1.,1.),(1.,1.),(1.,1.),(1.,1.),(1.,
1.),(1.,1.),(1.,1.),(1.,1.),(1.,1.),(1.,1.),(1.,1.),(1.,1.),(1.,1.),(1.,
1.),(1.,1.),(1.,1.),(1.,1.),(1.,1.),(1.,1.),(1.,1.),(1.,1.),(1.,1.),(1.,
1.),(1.,1.),(1.,1.),(1.,1.),(1.,1.),(1.,1.),(1.,1.),(1.,1.),(1.,1.),(1.,
1.),(1.,1.),(1.,1.),(1.,1.),(1.,1.),(1.,1.),(1.,1.),(1.,1.),(1.,1.),(1.,
1.),(1.,1.),(1.,1.),(1.,1.),(1.,1.),(1.,1.),(1.,1.),(1.,1.),(1.,1.),(1.,
1.),(1.,1.),(1.,1.),(1.,1.),(1.,1.),(1.,1.),(1.,1.),(1.,1.),(1.,1.),(1.,
1.),(1.,1.)))
REPRESENTATION_ITEM('')
SURFACE()
);
#902=(
BOUNDED_SURFACE()
B_SPLINE_SURFACE(5,1,((#69646,#69647),(#69648,#69649),(#69650,#69651),(#69652,
#69653),(#69654,#69655),(#69656,#69657),(#69658,#69659),(#69660,#69661),
(#69662,#69663),(#69664,#69665),(#69666,#69667),(#69668,#69669),(#69670,
#69671),(#69672,#69673),(#69674,#69675),(#69676,#69677),(#69678,#69679),
(#69680,#69681),(#69682,#69683),(#69684,#69685),(#69686,#69687),(#69688,
#69689),(#69690,#69691),(#69692,#69693),(#69694,#69695),(#69696,#69697),
(#69698,#69699),(#69700,#69701),(#69702,#69703),(#69704,#69705),(#69706,
#69707),(#69708,#69709),(#69710,#69711),(#69712,#69713),(#69714,#69715),
(#69716,#69717),(#69718,#69719),(#69720,#69721),(#69722,#69723),(#69724,
#69725),(#69726,#69727),(#69728,#69729),(#69730,#69731),(#69732,#69733),
(#69734,#69735),(#69736,#69737),(#69738,#69739),(#69740,#69741),(#69742,
#69743),(#69744,#69745),(#69746,#69747),(#69748,#69749),(#69750,#69751),
(#69752,#69753),(#69754,#69755),(#69756,#69757),(#69758,#69759),(#69760,
#69761),(#69762,#69763),(#69764,#69765),(#69766,#69767),(#69768,#69769),
(#69770,#69771),(#69772,#69773),(#69774,#69775),(#69776,#69777),(#69778,
#69779),(#69780,#69781),(#69782,#69783),(#69784,#69785),(#69786,#69787),
(#69788,#69789),(#69790,#69791),(#69792,#69793),(#69794,#69795),(#69796,
#69797),(#69798,#69799),(#69800,#69801),(#69802,#69803),(#69804,#69805),
(#69806,#69807),(#69808,#69809),(#69810,#69811),(#69812,#69813),(#69814,
#69815),(#69816,#69817),(#69818,#69819),(#69820,#69821),(#69822,#69823),
(#69824,#69825),(#69826,#69827),(#69828,#69829),(#69830,#69831),(#69832,
#69833),(#69834,#69835),(#69836,#69837),(#69838,#69839),(#69840,#69841),
(#69842,#69843),(#69844,#69845),(#69846,#69847),(#69848,#69849),(#69850,
#69851),(#69852,#69853),(#69854,#69855),(#69856,#69857),(#69858,#69859),
(#69860,#69861),(#69862,#69863),(#69864,#69865),(#69866,#69867),(#69868,
#69869),(#69870,#69871),(#69872,#69873),(#69874,#69875),(#69876,#69877),
(#69878,#69879),(#69880,#69881),(#69882,#69883),(#69884,#69885),(#69886,
#69887),(#69888,#69889),(#69890,#69891),(#69892,#69893),(#69894,#69895),
(#69896,#69897),(#69898,#69899),(#69900,#69901),(#69902,#69903),(#69904,
#69905),(#69906,#69907),(#69908,#69909),(#69910,#69911),(#69912,#69913),
(#69914,#69915),(#69916,#69917),(#69918,#69919),(#69920,#69921),(#69922,
#69923),(#69924,#69925),(#69926,#69927),(#69928,#69929),(#69930,#69931),
(#69932,#69933),(#69934,#69935),(#69936,#69937),(#69938,#69939),(#69940,
#69941),(#69942,#69943),(#69944,#69945),(#69946,#69947),(#69948,#69949),
(#69950,#69951),(#69952,#69953),(#69954,#69955),(#69956,#69957),(#69958,
#69959),(#69960,#69961),(#69962,#69963),(#69964,#69965),(#69966,#69967),
(#69968,#69969),(#69970,#69971),(#69972,#69973),(#69974,#69975),(#69976,
#69977),(#69978,#69979),(#69980,#69981),(#69982,#69983),(#69984,#69985),
(#69986,#69987),(#69988,#69989),(#69990,#69991),(#69992,#69993),(#69994,
#69995),(#69996,#69997),(#69998,#69999),(#70000,#70001),(#70002,#70003),
(#70004,#70005),(#70006,#70007),(#70008,#70009),(#70010,#70011),(#70012,
#70013),(#70014,#70015),(#70016,#70017),(#70018,#70019),(#70020,#70021),
(#70022,#70023),(#70024,#70025),(#70026,#70027),(#70028,#70029),(#70030,
#70031),(#70032,#70033),(#70034,#70035),(#70036,#70037),(#70038,#70039),
(#70040,#70041),(#70042,#70043),(#70044,#70045),(#70046,#70047),(#70048,
#70049),(#70050,#70051),(#70052,#70053),(#70054,#70055)),.UNSPECIFIED.,
 .F.,.F.,.F.)
B_SPLINE_SURFACE_WITH_KNOTS((6,1,1,1,1,1,1,1,1,1,1,1,1,1,1,1,1,1,1,1,1,
1,1,1,1,1,1,1,1,1,1,1,1,1,1,1,1,1,1,1,1,1,1,1,1,1,1,1,1,1,1,1,1,1,1,1,1,
1,1,1,1,1,1,1,1,1,1,1,1,1,1,1,1,1,1,1,1,1,1,1,1,1,1,1,1,1,1,1,1,1,1,1,1,
1,1,1,1,1,1,1,1,1,1,1,1,1,1,1,1,1,1,1,1,1,1,1,1,1,1,1,1,1,1,1,1,1,1,1,1,
1,1,1,1,1,1,1,1,1,1,1,1,1,1,1,1,1,1,1,1,1,1,1,1,1,1,1,1,1,1,1,1,1,1,1,1,
1,1,1,1,1,1,1,1,1,1,1,1,1,1,1,1,1,1,1,1,1,1,1,1,1,1,1,1,1,1,1,1,1,1,1,6),
(2,2),(0.,0.005,0.01,0.015,0.02,0.025,0.03,0.035,0.04,0.045,0.05,0.055,
0.06,0.065,0.07,0.075,0.08,0.085,0.09,0.095,0.1,0.105,0.11,0.115,0.12,0.125,
0.13,0.135,0.14,0.145,0.15,0.155,0.16,0.165,0.17,0.175,0.18,0.185,0.19,
0.195,0.2,0.205,0.21,0.215,0.22,0.225,0.23,0.235,0.24,0.245,0.25,0.255,
0.26,0.265,0.27,0.275,0.28,0.285,0.29,0.295,0.3,0.305,0.31,0.315,0.32,0.325,
0.33,0.335,0.34,0.345,0.35,0.355,0.36,0.365,0.37,0.375,0.38,0.385,0.39,
0.395,0.4,0.405,0.41,0.415,0.42,0.425,0.43,0.435,0.44,0.445,0.45,0.455,
0.46,0.465,0.47,0.475,0.48,0.485,0.49,0.495,0.5,0.505,0.51,0.515,0.52,0.525,
0.53,0.535,0.54,0.545,0.55,0.555,0.56,0.565,0.57,0.575,0.58,0.585,0.59,
0.595,0.6,0.605,0.61,0.615,0.62,0.625,0.63,0.635,0.64,0.645,0.65,0.655,
0.66,0.665,0.67,0.675,0.68,0.685,0.690000000000001,0.695000000000001,0.700000000000001,
0.705000000000001,0.710000000000001,0.715000000000001,0.720000000000001,
0.725000000000001,0.730000000000001,0.735000000000001,0.740000000000001,
0.745000000000001,0.750000000000001,0.755000000000001,0.760000000000001,
0.765000000000001,0.770000000000001,0.775000000000001,0.780000000000001,
0.785000000000001,0.790000000000001,0.795000000000001,0.800000000000001,
0.805000000000001,0.810000000000001,0.815000000000001,0.820000000000001,
0.825000000000001,0.830000000000001,0.835000000000001,0.840000000000001,
0.845000000000001,0.850000000000001,0.855000000000001,0.860000000000001,
0.865000000000001,0.870000000000001,0.875000000000001,0.880000000000001,
0.885000000000001,0.890000000000001,0.895000000000001,0.900000000000001,
0.905000000000001,0.910000000000001,0.915000000000001,0.920000000000001,
0.925000000000001,0.930000000000001,0.935000000000001,0.940000000000001,
0.945000000000001,0.950000000000001,0.955000000000001,0.960000000000001,
0.965000000000001,0.970000000000001,0.975000000000001,0.980000000000001,
0.985000000000001,0.990000000000001,0.995000000000001,1.),(0.,1.2),
 .UNSPECIFIED.)
GEOMETRIC_REPRESENTATION_ITEM()
RATIONAL_B_SPLINE_SURFACE(((1.,1.),(1.,1.),(1.,1.),(1.,1.),(1.,1.),(1.,
1.),(1.,1.),(1.,1.),(1.,1.),(1.,1.),(1.,1.),(1.,1.),(1.,1.),(1.,1.),(1.,
1.),(1.,1.),(1.,1.),(1.,1.),(1.,1.),(1.,1.),(1.,1.),(1.,1.),(1.,1.),(1.,
1.),(1.,1.),(1.,1.),(1.,1.),(1.,1.),(1.,1.),(1.,1.),(1.,1.),(1.,1.),(1.,
1.),(1.,1.),(1.,1.),(1.,1.),(1.,1.),(1.,1.),(1.,1.),(1.,1.),(1.,1.),(1.,
1.),(1.,1.),(1.,1.),(1.,1.),(1.,1.),(1.,1.),(1.,1.),(1.,1.),(1.,1.),(1.,
1.),(1.,1.),(1.,1.),(1.,1.),(1.,1.),(1.,1.),(1.,1.),(1.,1.),(1.,1.),(1.,
1.),(1.,1.),(1.,1.),(1.,1.),(1.,1.),(1.,1.),(1.,1.),(1.,1.),(1.,1.),(1.,
1.),(1.,1.),(1.,1.),(1.,1.),(1.,1.),(1.,1.),(1.,1.),(1.,1.),(1.,1.),(1.,
1.),(1.,1.),(1.,1.),(1.,1.),(1.,1.),(1.,1.),(1.,1.),(1.,1.),(1.,1.),(1.,
1.),(1.,1.),(1.,1.),(1.,1.),(1.,1.),(1.,1.),(1.,1.),(1.,1.),(1.,1.),(1.,
1.),(1.,1.),(1.,1.),(1.,1.),(1.,1.),(1.,1.),(1.,1.),(1.,1.),(1.,1.),(1.,
1.),(1.,1.),(1.,1.),(1.,1.),(1.,1.),(1.,1.),(1.,1.),(1.,1.),(1.,1.),(1.,
1.),(1.,1.),(1.,1.),(1.,1.),(1.,1.),(1.,1.),(1.,1.),(1.,1.),(1.,1.),(1.,
1.),(1.,1.),(1.,1.),(1.,1.),(1.,1.),(1.,1.),(1.,1.),(1.,1.),(1.,1.),(1.,
1.),(1.,1.),(1.,1.),(1.,1.),(1.,1.),(1.,1.),(1.,1.),(1.,1.),(1.,1.),(1.,
1.),(1.,1.),(1.,1.),(1.,1.),(1.,1.),(1.,1.),(1.,1.),(1.,1.),(1.,1.),(1.,
1.),(1.,1.),(1.,1.),(1.,1.),(1.,1.),(1.,1.),(1.,1.),(1.,1.),(1.,1.),(1.,
1.),(1.,1.),(1.,1.),(1.,1.),(1.,1.),(1.,1.),(1.,1.),(1.,1.),(1.,1.),(1.,
1.),(1.,1.),(1.,1.),(1.,1.),(1.,1.),(1.,1.),(1.,1.),(1.,1.),(1.,1.),(1.,
1.),(1.,1.),(1.,1.),(1.,1.),(1.,1.),(1.,1.),(1.,1.),(1.,1.),(1.,1.),(1.,
1.),(1.,1.),(1.,1.),(1.,1.),(1.,1.),(1.,1.),(1.,1.),(1.,1.),(1.,1.),(1.,
1.),(1.,1.),(1.,1.),(1.,1.),(1.,1.),(1.,1.),(1.,1.),(1.,1.),(1.,1.),(1.,
1.),(1.,1.)))
REPRESENTATION_ITEM('')
SURFACE()
);
#903=(
BOUNDED_SURFACE()
B_SPLINE_SURFACE(5,1,((#70542,#70543),(#70544,#70545),(#70546,#70547),(#70548,
#70549),(#70550,#70551),(#70552,#70553),(#70554,#70555),(#70556,#70557),
(#70558,#70559),(#70560,#70561),(#70562,#70563),(#70564,#70565),(#70566,
#70567),(#70568,#70569),(#70570,#70571),(#70572,#70573),(#70574,#70575),
(#70576,#70577),(#70578,#70579),(#70580,#70581),(#70582,#70583),(#70584,
#70585),(#70586,#70587),(#70588,#70589),(#70590,#70591),(#70592,#70593),
(#70594,#70595),(#70596,#70597),(#70598,#70599),(#70600,#70601),(#70602,
#70603),(#70604,#70605),(#70606,#70607),(#70608,#70609),(#70610,#70611),
(#70612,#70613),(#70614,#70615),(#70616,#70617),(#70618,#70619),(#70620,
#70621),(#70622,#70623),(#70624,#70625),(#70626,#70627),(#70628,#70629),
(#70630,#70631),(#70632,#70633),(#70634,#70635),(#70636,#70637),(#70638,
#70639),(#70640,#70641),(#70642,#70643),(#70644,#70645),(#70646,#70647),
(#70648,#70649),(#70650,#70651),(#70652,#70653),(#70654,#70655),(#70656,
#70657),(#70658,#70659),(#70660,#70661),(#70662,#70663),(#70664,#70665),
(#70666,#70667),(#70668,#70669),(#70670,#70671),(#70672,#70673),(#70674,
#70675),(#70676,#70677),(#70678,#70679),(#70680,#70681),(#70682,#70683),
(#70684,#70685),(#70686,#70687),(#70688,#70689),(#70690,#70691),(#70692,
#70693),(#70694,#70695),(#70696,#70697),(#70698,#70699),(#70700,#70701),
(#70702,#70703),(#70704,#70705),(#70706,#70707),(#70708,#70709),(#70710,
#70711),(#70712,#70713),(#70714,#70715),(#70716,#70717),(#70718,#70719),
(#70720,#70721),(#70722,#70723),(#70724,#70725),(#70726,#70727),(#70728,
#70729),(#70730,#70731),(#70732,#70733),(#70734,#70735),(#70736,#70737),
(#70738,#70739),(#70740,#70741),(#70742,#70743),(#70744,#70745),(#70746,
#70747),(#70748,#70749),(#70750,#70751),(#70752,#70753),(#70754,#70755),
(#70756,#70757),(#70758,#70759),(#70760,#70761),(#70762,#70763),(#70764,
#70765),(#70766,#70767),(#70768,#70769),(#70770,#70771),(#70772,#70773),
(#70774,#70775),(#70776,#70777),(#70778,#70779),(#70780,#70781),(#70782,
#70783),(#70784,#70785),(#70786,#70787),(#70788,#70789),(#70790,#70791),
(#70792,#70793),(#70794,#70795),(#70796,#70797),(#70798,#70799),(#70800,
#70801),(#70802,#70803),(#70804,#70805),(#70806,#70807),(#70808,#70809),
(#70810,#70811),(#70812,#70813),(#70814,#70815),(#70816,#70817),(#70818,
#70819),(#70820,#70821),(#70822,#70823),(#70824,#70825),(#70826,#70827),
(#70828,#70829),(#70830,#70831),(#70832,#70833),(#70834,#70835),(#70836,
#70837),(#70838,#70839),(#70840,#70841),(#70842,#70843),(#70844,#70845),
(#70846,#70847),(#70848,#70849),(#70850,#70851),(#70852,#70853),(#70854,
#70855),(#70856,#70857),(#70858,#70859),(#70860,#70861),(#70862,#70863),
(#70864,#70865),(#70866,#70867),(#70868,#70869),(#70870,#70871),(#70872,
#70873),(#70874,#70875),(#70876,#70877),(#70878,#70879),(#70880,#70881),
(#70882,#70883),(#70884,#70885),(#70886,#70887),(#70888,#70889),(#70890,
#70891),(#70892,#70893),(#70894,#70895),(#70896,#70897),(#70898,#70899),
(#70900,#70901),(#70902,#70903),(#70904,#70905),(#70906,#70907),(#70908,
#70909),(#70910,#70911),(#70912,#70913),(#70914,#70915),(#70916,#70917),
(#70918,#70919),(#70920,#70921),(#70922,#70923),(#70924,#70925),(#70926,
#70927),(#70928,#70929),(#70930,#70931),(#70932,#70933),(#70934,#70935),
(#70936,#70937),(#70938,#70939),(#70940,#70941),(#70942,#70943),(#70944,
#70945),(#70946,#70947),(#70948,#70949),(#70950,#70951)),.UNSPECIFIED.,
 .F.,.F.,.F.)
B_SPLINE_SURFACE_WITH_KNOTS((6,1,1,1,1,1,1,1,1,1,1,1,1,1,1,1,1,1,1,1,1,
1,1,1,1,1,1,1,1,1,1,1,1,1,1,1,1,1,1,1,1,1,1,1,1,1,1,1,1,1,1,1,1,1,1,1,1,
1,1,1,1,1,1,1,1,1,1,1,1,1,1,1,1,1,1,1,1,1,1,1,1,1,1,1,1,1,1,1,1,1,1,1,1,
1,1,1,1,1,1,1,1,1,1,1,1,1,1,1,1,1,1,1,1,1,1,1,1,1,1,1,1,1,1,1,1,1,1,1,1,
1,1,1,1,1,1,1,1,1,1,1,1,1,1,1,1,1,1,1,1,1,1,1,1,1,1,1,1,1,1,1,1,1,1,1,1,
1,1,1,1,1,1,1,1,1,1,1,1,1,1,1,1,1,1,1,1,1,1,1,1,1,1,1,1,1,1,1,1,1,1,1,6),
(2,2),(0.,0.005,0.01,0.015,0.02,0.025,0.03,0.035,0.04,0.045,0.05,0.055,
0.06,0.065,0.07,0.075,0.08,0.085,0.09,0.095,0.1,0.105,0.11,0.115,0.12,0.125,
0.13,0.135,0.14,0.145,0.15,0.155,0.16,0.165,0.17,0.175,0.18,0.185,0.19,
0.195,0.2,0.205,0.21,0.215,0.22,0.225,0.23,0.235,0.24,0.245,0.25,0.255,
0.26,0.265,0.27,0.275,0.28,0.285,0.29,0.295,0.3,0.305,0.31,0.315,0.32,0.325,
0.33,0.335,0.34,0.345,0.35,0.355,0.36,0.365,0.37,0.375,0.38,0.385,0.39,
0.395,0.4,0.405,0.41,0.415,0.42,0.425,0.43,0.435,0.44,0.445,0.45,0.455,
0.46,0.465,0.47,0.475,0.48,0.485,0.49,0.495,0.5,0.505,0.51,0.515,0.52,0.525,
0.53,0.535,0.54,0.545,0.55,0.555,0.56,0.565,0.57,0.575,0.58,0.585,0.59,
0.595,0.6,0.605,0.61,0.615,0.62,0.625,0.63,0.635,0.64,0.645,0.65,0.655,
0.66,0.665,0.67,0.675,0.68,0.685,0.690000000000001,0.695000000000001,0.700000000000001,
0.705000000000001,0.710000000000001,0.715000000000001,0.720000000000001,
0.725000000000001,0.730000000000001,0.735000000000001,0.740000000000001,
0.745000000000001,0.750000000000001,0.755000000000001,0.760000000000001,
0.765000000000001,0.770000000000001,0.775000000000001,0.780000000000001,
0.785000000000001,0.790000000000001,0.795000000000001,0.800000000000001,
0.805000000000001,0.810000000000001,0.815000000000001,0.820000000000001,
0.825000000000001,0.830000000000001,0.835000000000001,0.840000000000001,
0.845000000000001,0.850000000000001,0.855000000000001,0.860000000000001,
0.865000000000001,0.870000000000001,0.875000000000001,0.880000000000001,
0.885000000000001,0.890000000000001,0.895000000000001,0.900000000000001,
0.905000000000001,0.910000000000001,0.915000000000001,0.920000000000001,
0.925000000000001,0.930000000000001,0.935000000000001,0.940000000000001,
0.945000000000001,0.950000000000001,0.955000000000001,0.960000000000001,
0.965000000000001,0.970000000000001,0.975000000000001,0.980000000000001,
0.985000000000001,0.990000000000001,0.995000000000001,1.),(0.,1.2),
 .UNSPECIFIED.)
GEOMETRIC_REPRESENTATION_ITEM()
RATIONAL_B_SPLINE_SURFACE(((1.,1.),(1.,1.),(1.,1.),(1.,1.),(1.,1.),(1.,
1.),(1.,1.),(1.,1.),(1.,1.),(1.,1.),(1.,1.),(1.,1.),(1.,1.),(1.,1.),(1.,
1.),(1.,1.),(1.,1.),(1.,1.),(1.,1.),(1.,1.),(1.,1.),(1.,1.),(1.,1.),(1.,
1.),(1.,1.),(1.,1.),(1.,1.),(1.,1.),(1.,1.),(1.,1.),(1.,1.),(1.,1.),(1.,
1.),(1.,1.),(1.,1.),(1.,1.),(1.,1.),(1.,1.),(1.,1.),(1.,1.),(1.,1.),(1.,
1.),(1.,1.),(1.,1.),(1.,1.),(1.,1.),(1.,1.),(1.,1.),(1.,1.),(1.,1.),(1.,
1.),(1.,1.),(1.,1.),(1.,1.),(1.,1.),(1.,1.),(1.,1.),(1.,1.),(1.,1.),(1.,
1.),(1.,1.),(1.,1.),(1.,1.),(1.,1.),(1.,1.),(1.,1.),(1.,1.),(1.,1.),(1.,
1.),(1.,1.),(1.,1.),(1.,1.),(1.,1.),(1.,1.),(1.,1.),(1.,1.),(1.,1.),(1.,
1.),(1.,1.),(1.,1.),(1.,1.),(1.,1.),(1.,1.),(1.,1.),(1.,1.),(1.,1.),(1.,
1.),(1.,1.),(1.,1.),(1.,1.),(1.,1.),(1.,1.),(1.,1.),(1.,1.),(1.,1.),(1.,
1.),(1.,1.),(1.,1.),(1.,1.),(1.,1.),(1.,1.),(1.,1.),(1.,1.),(1.,1.),(1.,
1.),(1.,1.),(1.,1.),(1.,1.),(1.,1.),(1.,1.),(1.,1.),(1.,1.),(1.,1.),(1.,
1.),(1.,1.),(1.,1.),(1.,1.),(1.,1.),(1.,1.),(1.,1.),(1.,1.),(1.,1.),(1.,
1.),(1.,1.),(1.,1.),(1.,1.),(1.,1.),(1.,1.),(1.,1.),(1.,1.),(1.,1.),(1.,
1.),(1.,1.),(1.,1.),(1.,1.),(1.,1.),(1.,1.),(1.,1.),(1.,1.),(1.,1.),(1.,
1.),(1.,1.),(1.,1.),(1.,1.),(1.,1.),(1.,1.),(1.,1.),(1.,1.),(1.,1.),(1.,
1.),(1.,1.),(1.,1.),(1.,1.),(1.,1.),(1.,1.),(1.,1.),(1.,1.),(1.,1.),(1.,
1.),(1.,1.),(1.,1.),(1.,1.),(1.,1.),(1.,1.),(1.,1.),(1.,1.),(1.,1.),(1.,
1.),(1.,1.),(1.,1.),(1.,1.),(1.,1.),(1.,1.),(1.,1.),(1.,1.),(1.,1.),(1.,
1.),(1.,1.),(1.,1.),(1.,1.),(1.,1.),(1.,1.),(1.,1.),(1.,1.),(1.,1.),(1.,
1.),(1.,1.),(1.,1.),(1.,1.),(1.,1.),(1.,1.),(1.,1.),(1.,1.),(1.,1.),(1.,
1.),(1.,1.),(1.,1.),(1.,1.),(1.,1.),(1.,1.),(1.,1.),(1.,1.),(1.,1.),(1.,
1.),(1.,1.)))
REPRESENTATION_ITEM('')
SURFACE()
);
#904=(
BOUNDED_SURFACE()
B_SPLINE_SURFACE(5,1,((#71438,#71439),(#71440,#71441),(#71442,#71443),(#71444,
#71445),(#71446,#71447),(#71448,#71449),(#71450,#71451),(#71452,#71453),
(#71454,#71455),(#71456,#71457),(#71458,#71459),(#71460,#71461),(#71462,
#71463),(#71464,#71465),(#71466,#71467),(#71468,#71469),(#71470,#71471),
(#71472,#71473),(#71474,#71475),(#71476,#71477),(#71478,#71479),(#71480,
#71481),(#71482,#71483),(#71484,#71485),(#71486,#71487),(#71488,#71489),
(#71490,#71491),(#71492,#71493),(#71494,#71495),(#71496,#71497),(#71498,
#71499),(#71500,#71501),(#71502,#71503),(#71504,#71505),(#71506,#71507),
(#71508,#71509),(#71510,#71511),(#71512,#71513),(#71514,#71515),(#71516,
#71517),(#71518,#71519),(#71520,#71521),(#71522,#71523),(#71524,#71525),
(#71526,#71527),(#71528,#71529),(#71530,#71531),(#71532,#71533),(#71534,
#71535),(#71536,#71537),(#71538,#71539),(#71540,#71541),(#71542,#71543),
(#71544,#71545),(#71546,#71547),(#71548,#71549),(#71550,#71551),(#71552,
#71553),(#71554,#71555),(#71556,#71557),(#71558,#71559),(#71560,#71561),
(#71562,#71563),(#71564,#71565),(#71566,#71567),(#71568,#71569),(#71570,
#71571),(#71572,#71573),(#71574,#71575),(#71576,#71577),(#71578,#71579),
(#71580,#71581),(#71582,#71583),(#71584,#71585),(#71586,#71587),(#71588,
#71589),(#71590,#71591),(#71592,#71593),(#71594,#71595),(#71596,#71597),
(#71598,#71599),(#71600,#71601),(#71602,#71603),(#71604,#71605),(#71606,
#71607),(#71608,#71609),(#71610,#71611),(#71612,#71613),(#71614,#71615),
(#71616,#71617),(#71618,#71619),(#71620,#71621),(#71622,#71623),(#71624,
#71625),(#71626,#71627),(#71628,#71629),(#71630,#71631),(#71632,#71633),
(#71634,#71635),(#71636,#71637),(#71638,#71639),(#71640,#71641),(#71642,
#71643),(#71644,#71645),(#71646,#71647),(#71648,#71649),(#71650,#71651),
(#71652,#71653),(#71654,#71655),(#71656,#71657),(#71658,#71659),(#71660,
#71661),(#71662,#71663),(#71664,#71665),(#71666,#71667),(#71668,#71669),
(#71670,#71671),(#71672,#71673),(#71674,#71675),(#71676,#71677),(#71678,
#71679),(#71680,#71681),(#71682,#71683),(#71684,#71685),(#71686,#71687),
(#71688,#71689),(#71690,#71691),(#71692,#71693),(#71694,#71695),(#71696,
#71697),(#71698,#71699),(#71700,#71701),(#71702,#71703),(#71704,#71705),
(#71706,#71707),(#71708,#71709),(#71710,#71711),(#71712,#71713),(#71714,
#71715),(#71716,#71717),(#71718,#71719),(#71720,#71721),(#71722,#71723),
(#71724,#71725),(#71726,#71727),(#71728,#71729),(#71730,#71731),(#71732,
#71733),(#71734,#71735),(#71736,#71737),(#71738,#71739),(#71740,#71741),
(#71742,#71743),(#71744,#71745),(#71746,#71747),(#71748,#71749),(#71750,
#71751),(#71752,#71753),(#71754,#71755),(#71756,#71757),(#71758,#71759),
(#71760,#71761),(#71762,#71763),(#71764,#71765),(#71766,#71767),(#71768,
#71769),(#71770,#71771),(#71772,#71773),(#71774,#71775),(#71776,#71777),
(#71778,#71779),(#71780,#71781),(#71782,#71783),(#71784,#71785),(#71786,
#71787),(#71788,#71789),(#71790,#71791),(#71792,#71793),(#71794,#71795),
(#71796,#71797),(#71798,#71799),(#71800,#71801),(#71802,#71803),(#71804,
#71805),(#71806,#71807),(#71808,#71809),(#71810,#71811),(#71812,#71813),
(#71814,#71815),(#71816,#71817),(#71818,#71819),(#71820,#71821),(#71822,
#71823),(#71824,#71825),(#71826,#71827),(#71828,#71829),(#71830,#71831),
(#71832,#71833),(#71834,#71835),(#71836,#71837),(#71838,#71839),(#71840,
#71841),(#71842,#71843),(#71844,#71845),(#71846,#71847)),.UNSPECIFIED.,
 .F.,.F.,.F.)
B_SPLINE_SURFACE_WITH_KNOTS((6,1,1,1,1,1,1,1,1,1,1,1,1,1,1,1,1,1,1,1,1,
1,1,1,1,1,1,1,1,1,1,1,1,1,1,1,1,1,1,1,1,1,1,1,1,1,1,1,1,1,1,1,1,1,1,1,1,
1,1,1,1,1,1,1,1,1,1,1,1,1,1,1,1,1,1,1,1,1,1,1,1,1,1,1,1,1,1,1,1,1,1,1,1,
1,1,1,1,1,1,1,1,1,1,1,1,1,1,1,1,1,1,1,1,1,1,1,1,1,1,1,1,1,1,1,1,1,1,1,1,
1,1,1,1,1,1,1,1,1,1,1,1,1,1,1,1,1,1,1,1,1,1,1,1,1,1,1,1,1,1,1,1,1,1,1,1,
1,1,1,1,1,1,1,1,1,1,1,1,1,1,1,1,1,1,1,1,1,1,1,1,1,1,1,1,1,1,1,1,1,1,1,6),
(2,2),(0.,0.005,0.01,0.015,0.02,0.025,0.03,0.035,0.04,0.045,0.05,0.055,
0.06,0.065,0.07,0.075,0.08,0.085,0.09,0.095,0.1,0.105,0.11,0.115,0.12,0.125,
0.13,0.135,0.14,0.145,0.15,0.155,0.16,0.165,0.17,0.175,0.18,0.185,0.19,
0.195,0.2,0.205,0.21,0.215,0.22,0.225,0.23,0.235,0.24,0.245,0.25,0.255,
0.26,0.265,0.27,0.275,0.28,0.285,0.29,0.295,0.3,0.305,0.31,0.315,0.32,0.325,
0.33,0.335,0.34,0.345,0.35,0.355,0.36,0.365,0.37,0.375,0.38,0.385,0.39,
0.395,0.4,0.405,0.41,0.415,0.42,0.425,0.43,0.435,0.44,0.445,0.45,0.455,
0.46,0.465,0.47,0.475,0.48,0.485,0.49,0.495,0.5,0.505,0.51,0.515,0.52,0.525,
0.53,0.535,0.54,0.545,0.55,0.555,0.56,0.565,0.57,0.575,0.58,0.585,0.59,
0.595,0.6,0.605,0.61,0.615,0.62,0.625,0.63,0.635,0.64,0.645,0.65,0.655,
0.66,0.665,0.67,0.675,0.68,0.685,0.690000000000001,0.695000000000001,0.700000000000001,
0.705000000000001,0.710000000000001,0.715000000000001,0.720000000000001,
0.725000000000001,0.730000000000001,0.735000000000001,0.740000000000001,
0.745000000000001,0.750000000000001,0.755000000000001,0.760000000000001,
0.765000000000001,0.770000000000001,0.775000000000001,0.780000000000001,
0.785000000000001,0.790000000000001,0.795000000000001,0.800000000000001,
0.805000000000001,0.810000000000001,0.815000000000001,0.820000000000001,
0.825000000000001,0.830000000000001,0.835000000000001,0.840000000000001,
0.845000000000001,0.850000000000001,0.855000000000001,0.860000000000001,
0.865000000000001,0.870000000000001,0.875000000000001,0.880000000000001,
0.885000000000001,0.890000000000001,0.895000000000001,0.900000000000001,
0.905000000000001,0.910000000000001,0.915000000000001,0.920000000000001,
0.925000000000001,0.930000000000001,0.935000000000001,0.940000000000001,
0.945000000000001,0.950000000000001,0.955000000000001,0.960000000000001,
0.965000000000001,0.970000000000001,0.975000000000001,0.980000000000001,
0.985000000000001,0.990000000000001,0.995000000000001,1.),(0.,1.2),
 .UNSPECIFIED.)
GEOMETRIC_REPRESENTATION_ITEM()
RATIONAL_B_SPLINE_SURFACE(((1.,1.),(1.,1.),(1.,1.),(1.,1.),(1.,1.),(1.,
1.),(1.,1.),(1.,1.),(1.,1.),(1.,1.),(1.,1.),(1.,1.),(1.,1.),(1.,1.),(1.,
1.),(1.,1.),(1.,1.),(1.,1.),(1.,1.),(1.,1.),(1.,1.),(1.,1.),(1.,1.),(1.,
1.),(1.,1.),(1.,1.),(1.,1.),(1.,1.),(1.,1.),(1.,1.),(1.,1.),(1.,1.),(1.,
1.),(1.,1.),(1.,1.),(1.,1.),(1.,1.),(1.,1.),(1.,1.),(1.,1.),(1.,1.),(1.,
1.),(1.,1.),(1.,1.),(1.,1.),(1.,1.),(1.,1.),(1.,1.),(1.,1.),(1.,1.),(1.,
1.),(1.,1.),(1.,1.),(1.,1.),(1.,1.),(1.,1.),(1.,1.),(1.,1.),(1.,1.),(1.,
1.),(1.,1.),(1.,1.),(1.,1.),(1.,1.),(1.,1.),(1.,1.),(1.,1.),(1.,1.),(1.,
1.),(1.,1.),(1.,1.),(1.,1.),(1.,1.),(1.,1.),(1.,1.),(1.,1.),(1.,1.),(1.,
1.),(1.,1.),(1.,1.),(1.,1.),(1.,1.),(1.,1.),(1.,1.),(1.,1.),(1.,1.),(1.,
1.),(1.,1.),(1.,1.),(1.,1.),(1.,1.),(1.,1.),(1.,1.),(1.,1.),(1.,1.),(1.,
1.),(1.,1.),(1.,1.),(1.,1.),(1.,1.),(1.,1.),(1.,1.),(1.,1.),(1.,1.),(1.,
1.),(1.,1.),(1.,1.),(1.,1.),(1.,1.),(1.,1.),(1.,1.),(1.,1.),(1.,1.),(1.,
1.),(1.,1.),(1.,1.),(1.,1.),(1.,1.),(1.,1.),(1.,1.),(1.,1.),(1.,1.),(1.,
1.),(1.,1.),(1.,1.),(1.,1.),(1.,1.),(1.,1.),(1.,1.),(1.,1.),(1.,1.),(1.,
1.),(1.,1.),(1.,1.),(1.,1.),(1.,1.),(1.,1.),(1.,1.),(1.,1.),(1.,1.),(1.,
1.),(1.,1.),(1.,1.),(1.,1.),(1.,1.),(1.,1.),(1.,1.),(1.,1.),(1.,1.),(1.,
1.),(1.,1.),(1.,1.),(1.,1.),(1.,1.),(1.,1.),(1.,1.),(1.,1.),(1.,1.),(1.,
1.),(1.,1.),(1.,1.),(1.,1.),(1.,1.),(1.,1.),(1.,1.),(1.,1.),(1.,1.),(1.,
1.),(1.,1.),(1.,1.),(1.,1.),(1.,1.),(1.,1.),(1.,1.),(1.,1.),(1.,1.),(1.,
1.),(1.,1.),(1.,1.),(1.,1.),(1.,1.),(1.,1.),(1.,1.),(1.,1.),(1.,1.),(1.,
1.),(1.,1.),(1.,1.),(1.,1.),(1.,1.),(1.,1.),(1.,1.),(1.,1.),(1.,1.),(1.,
1.),(1.,1.),(1.,1.),(1.,1.),(1.,1.),(1.,1.),(1.,1.),(1.,1.),(1.,1.),(1.,
1.),(1.,1.)))
REPRESENTATION_ITEM('')
SURFACE()
);
#905=(
BOUNDED_SURFACE()
B_SPLINE_SURFACE(5,1,((#72334,#72335),(#72336,#72337),(#72338,#72339),(#72340,
#72341),(#72342,#72343),(#72344,#72345),(#72346,#72347),(#72348,#72349),
(#72350,#72351),(#72352,#72353),(#72354,#72355),(#72356,#72357),(#72358,
#72359),(#72360,#72361),(#72362,#72363),(#72364,#72365),(#72366,#72367),
(#72368,#72369),(#72370,#72371),(#72372,#72373),(#72374,#72375),(#72376,
#72377),(#72378,#72379),(#72380,#72381),(#72382,#72383),(#72384,#72385),
(#72386,#72387),(#72388,#72389),(#72390,#72391),(#72392,#72393),(#72394,
#72395),(#72396,#72397),(#72398,#72399),(#72400,#72401),(#72402,#72403),
(#72404,#72405),(#72406,#72407),(#72408,#72409),(#72410,#72411),(#72412,
#72413),(#72414,#72415),(#72416,#72417),(#72418,#72419),(#72420,#72421),
(#72422,#72423),(#72424,#72425),(#72426,#72427),(#72428,#72429),(#72430,
#72431),(#72432,#72433),(#72434,#72435),(#72436,#72437),(#72438,#72439),
(#72440,#72441),(#72442,#72443),(#72444,#72445),(#72446,#72447),(#72448,
#72449),(#72450,#72451),(#72452,#72453),(#72454,#72455),(#72456,#72457),
(#72458,#72459),(#72460,#72461),(#72462,#72463),(#72464,#72465),(#72466,
#72467),(#72468,#72469),(#72470,#72471),(#72472,#72473),(#72474,#72475),
(#72476,#72477),(#72478,#72479),(#72480,#72481),(#72482,#72483),(#72484,
#72485),(#72486,#72487),(#72488,#72489),(#72490,#72491),(#72492,#72493),
(#72494,#72495),(#72496,#72497),(#72498,#72499),(#72500,#72501),(#72502,
#72503),(#72504,#72505),(#72506,#72507),(#72508,#72509),(#72510,#72511),
(#72512,#72513),(#72514,#72515),(#72516,#72517),(#72518,#72519),(#72520,
#72521),(#72522,#72523),(#72524,#72525),(#72526,#72527),(#72528,#72529),
(#72530,#72531),(#72532,#72533),(#72534,#72535),(#72536,#72537),(#72538,
#72539),(#72540,#72541),(#72542,#72543),(#72544,#72545),(#72546,#72547),
(#72548,#72549),(#72550,#72551),(#72552,#72553),(#72554,#72555),(#72556,
#72557),(#72558,#72559),(#72560,#72561),(#72562,#72563),(#72564,#72565),
(#72566,#72567),(#72568,#72569),(#72570,#72571),(#72572,#72573),(#72574,
#72575),(#72576,#72577),(#72578,#72579),(#72580,#72581),(#72582,#72583),
(#72584,#72585),(#72586,#72587),(#72588,#72589),(#72590,#72591),(#72592,
#72593),(#72594,#72595),(#72596,#72597),(#72598,#72599),(#72600,#72601),
(#72602,#72603),(#72604,#72605),(#72606,#72607),(#72608,#72609),(#72610,
#72611),(#72612,#72613),(#72614,#72615),(#72616,#72617),(#72618,#72619),
(#72620,#72621),(#72622,#72623),(#72624,#72625),(#72626,#72627),(#72628,
#72629),(#72630,#72631),(#72632,#72633),(#72634,#72635),(#72636,#72637),
(#72638,#72639),(#72640,#72641),(#72642,#72643),(#72644,#72645),(#72646,
#72647),(#72648,#72649),(#72650,#72651),(#72652,#72653),(#72654,#72655),
(#72656,#72657),(#72658,#72659),(#72660,#72661),(#72662,#72663),(#72664,
#72665),(#72666,#72667),(#72668,#72669),(#72670,#72671),(#72672,#72673),
(#72674,#72675),(#72676,#72677),(#72678,#72679),(#72680,#72681),(#72682,
#72683),(#72684,#72685),(#72686,#72687),(#72688,#72689),(#72690,#72691),
(#72692,#72693),(#72694,#72695),(#72696,#72697),(#72698,#72699),(#72700,
#72701),(#72702,#72703),(#72704,#72705),(#72706,#72707),(#72708,#72709),
(#72710,#72711),(#72712,#72713),(#72714,#72715),(#72716,#72717),(#72718,
#72719),(#72720,#72721),(#72722,#72723),(#72724,#72725),(#72726,#72727),
(#72728,#72729),(#72730,#72731),(#72732,#72733),(#72734,#72735),(#72736,
#72737),(#72738,#72739),(#72740,#72741),(#72742,#72743)),.UNSPECIFIED.,
 .F.,.F.,.F.)
B_SPLINE_SURFACE_WITH_KNOTS((6,1,1,1,1,1,1,1,1,1,1,1,1,1,1,1,1,1,1,1,1,
1,1,1,1,1,1,1,1,1,1,1,1,1,1,1,1,1,1,1,1,1,1,1,1,1,1,1,1,1,1,1,1,1,1,1,1,
1,1,1,1,1,1,1,1,1,1,1,1,1,1,1,1,1,1,1,1,1,1,1,1,1,1,1,1,1,1,1,1,1,1,1,1,
1,1,1,1,1,1,1,1,1,1,1,1,1,1,1,1,1,1,1,1,1,1,1,1,1,1,1,1,1,1,1,1,1,1,1,1,
1,1,1,1,1,1,1,1,1,1,1,1,1,1,1,1,1,1,1,1,1,1,1,1,1,1,1,1,1,1,1,1,1,1,1,1,
1,1,1,1,1,1,1,1,1,1,1,1,1,1,1,1,1,1,1,1,1,1,1,1,1,1,1,1,1,1,1,1,1,1,1,6),
(2,2),(0.,0.005,0.01,0.015,0.02,0.025,0.03,0.035,0.04,0.045,0.05,0.055,
0.06,0.065,0.07,0.075,0.08,0.085,0.09,0.095,0.1,0.105,0.11,0.115,0.12,0.125,
0.13,0.135,0.14,0.145,0.15,0.155,0.16,0.165,0.17,0.175,0.18,0.185,0.19,
0.195,0.2,0.205,0.21,0.215,0.22,0.225,0.23,0.235,0.24,0.245,0.25,0.255,
0.26,0.265,0.27,0.275,0.28,0.285,0.29,0.295,0.3,0.305,0.31,0.315,0.32,0.325,
0.33,0.335,0.34,0.345,0.35,0.355,0.36,0.365,0.37,0.375,0.38,0.385,0.39,
0.395,0.4,0.405,0.41,0.415,0.42,0.425,0.43,0.435,0.44,0.445,0.45,0.455,
0.46,0.465,0.47,0.475,0.48,0.485,0.49,0.495,0.5,0.505,0.51,0.515,0.52,0.525,
0.53,0.535,0.54,0.545,0.55,0.555,0.56,0.565,0.57,0.575,0.58,0.585,0.59,
0.595,0.6,0.605,0.61,0.615,0.62,0.625,0.63,0.635,0.64,0.645,0.65,0.655,
0.66,0.665,0.67,0.675,0.68,0.685,0.690000000000001,0.695000000000001,0.700000000000001,
0.705000000000001,0.710000000000001,0.715000000000001,0.720000000000001,
0.725000000000001,0.730000000000001,0.735000000000001,0.740000000000001,
0.745000000000001,0.750000000000001,0.755000000000001,0.760000000000001,
0.765000000000001,0.770000000000001,0.775000000000001,0.780000000000001,
0.785000000000001,0.790000000000001,0.795000000000001,0.800000000000001,
0.805000000000001,0.810000000000001,0.815000000000001,0.820000000000001,
0.825000000000001,0.830000000000001,0.835000000000001,0.840000000000001,
0.845000000000001,0.850000000000001,0.855000000000001,0.860000000000001,
0.865000000000001,0.870000000000001,0.875000000000001,0.880000000000001,
0.885000000000001,0.890000000000001,0.895000000000001,0.900000000000001,
0.905000000000001,0.910000000000001,0.915000000000001,0.920000000000001,
0.925000000000001,0.930000000000001,0.935000000000001,0.940000000000001,
0.945000000000001,0.950000000000001,0.955000000000001,0.960000000000001,
0.965000000000001,0.970000000000001,0.975000000000001,0.980000000000001,
0.985000000000001,0.990000000000001,0.995000000000001,1.),(0.,1.2),
 .UNSPECIFIED.)
GEOMETRIC_REPRESENTATION_ITEM()
RATIONAL_B_SPLINE_SURFACE(((1.,1.),(1.,1.),(1.,1.),(1.,1.),(1.,1.),(1.,
1.),(1.,1.),(1.,1.),(1.,1.),(1.,1.),(1.,1.),(1.,1.),(1.,1.),(1.,1.),(1.,
1.),(1.,1.),(1.,1.),(1.,1.),(1.,1.),(1.,1.),(1.,1.),(1.,1.),(1.,1.),(1.,
1.),(1.,1.),(1.,1.),(1.,1.),(1.,1.),(1.,1.),(1.,1.),(1.,1.),(1.,1.),(1.,
1.),(1.,1.),(1.,1.),(1.,1.),(1.,1.),(1.,1.),(1.,1.),(1.,1.),(1.,1.),(1.,
1.),(1.,1.),(1.,1.),(1.,1.),(1.,1.),(1.,1.),(1.,1.),(1.,1.),(1.,1.),(1.,
1.),(1.,1.),(1.,1.),(1.,1.),(1.,1.),(1.,1.),(1.,1.),(1.,1.),(1.,1.),(1.,
1.),(1.,1.),(1.,1.),(1.,1.),(1.,1.),(1.,1.),(1.,1.),(1.,1.),(1.,1.),(1.,
1.),(1.,1.),(1.,1.),(1.,1.),(1.,1.),(1.,1.),(1.,1.),(1.,1.),(1.,1.),(1.,
1.),(1.,1.),(1.,1.),(1.,1.),(1.,1.),(1.,1.),(1.,1.),(1.,1.),(1.,1.),(1.,
1.),(1.,1.),(1.,1.),(1.,1.),(1.,1.),(1.,1.),(1.,1.),(1.,1.),(1.,1.),(1.,
1.),(1.,1.),(1.,1.),(1.,1.),(1.,1.),(1.,1.),(1.,1.),(1.,1.),(1.,1.),(1.,
1.),(1.,1.),(1.,1.),(1.,1.),(1.,1.),(1.,1.),(1.,1.),(1.,1.),(1.,1.),(1.,
1.),(1.,1.),(1.,1.),(1.,1.),(1.,1.),(1.,1.),(1.,1.),(1.,1.),(1.,1.),(1.,
1.),(1.,1.),(1.,1.),(1.,1.),(1.,1.),(1.,1.),(1.,1.),(1.,1.),(1.,1.),(1.,
1.),(1.,1.),(1.,1.),(1.,1.),(1.,1.),(1.,1.),(1.,1.),(1.,1.),(1.,1.),(1.,
1.),(1.,1.),(1.,1.),(1.,1.),(1.,1.),(1.,1.),(1.,1.),(1.,1.),(1.,1.),(1.,
1.),(1.,1.),(1.,1.),(1.,1.),(1.,1.),(1.,1.),(1.,1.),(1.,1.),(1.,1.),(1.,
1.),(1.,1.),(1.,1.),(1.,1.),(1.,1.),(1.,1.),(1.,1.),(1.,1.),(1.,1.),(1.,
1.),(1.,1.),(1.,1.),(1.,1.),(1.,1.),(1.,1.),(1.,1.),(1.,1.),(1.,1.),(1.,
1.),(1.,1.),(1.,1.),(1.,1.),(1.,1.),(1.,1.),(1.,1.),(1.,1.),(1.,1.),(1.,
1.),(1.,1.),(1.,1.),(1.,1.),(1.,1.),(1.,1.),(1.,1.),(1.,1.),(1.,1.),(1.,
1.),(1.,1.),(1.,1.),(1.,1.),(1.,1.),(1.,1.),(1.,1.),(1.,1.),(1.,1.),(1.,
1.),(1.,1.)))
REPRESENTATION_ITEM('')
SURFACE()
);
#906=(
BOUNDED_SURFACE()
B_SPLINE_SURFACE(5,1,((#73230,#73231),(#73232,#73233),(#73234,#73235),(#73236,
#73237),(#73238,#73239),(#73240,#73241),(#73242,#73243),(#73244,#73245),
(#73246,#73247),(#73248,#73249),(#73250,#73251),(#73252,#73253),(#73254,
#73255),(#73256,#73257),(#73258,#73259),(#73260,#73261),(#73262,#73263),
(#73264,#73265),(#73266,#73267),(#73268,#73269),(#73270,#73271),(#73272,
#73273),(#73274,#73275),(#73276,#73277),(#73278,#73279),(#73280,#73281),
(#73282,#73283),(#73284,#73285),(#73286,#73287),(#73288,#73289),(#73290,
#73291),(#73292,#73293),(#73294,#73295),(#73296,#73297),(#73298,#73299),
(#73300,#73301),(#73302,#73303),(#73304,#73305),(#73306,#73307),(#73308,
#73309),(#73310,#73311),(#73312,#73313),(#73314,#73315),(#73316,#73317),
(#73318,#73319),(#73320,#73321),(#73322,#73323),(#73324,#73325),(#73326,
#73327),(#73328,#73329),(#73330,#73331),(#73332,#73333),(#73334,#73335),
(#73336,#73337),(#73338,#73339),(#73340,#73341),(#73342,#73343),(#73344,
#73345),(#73346,#73347),(#73348,#73349),(#73350,#73351),(#73352,#73353),
(#73354,#73355),(#73356,#73357),(#73358,#73359),(#73360,#73361),(#73362,
#73363),(#73364,#73365),(#73366,#73367),(#73368,#73369),(#73370,#73371),
(#73372,#73373),(#73374,#73375),(#73376,#73377),(#73378,#73379),(#73380,
#73381),(#73382,#73383),(#73384,#73385),(#73386,#73387),(#73388,#73389),
(#73390,#73391),(#73392,#73393),(#73394,#73395),(#73396,#73397),(#73398,
#73399),(#73400,#73401),(#73402,#73403),(#73404,#73405),(#73406,#73407),
(#73408,#73409),(#73410,#73411),(#73412,#73413),(#73414,#73415),(#73416,
#73417),(#73418,#73419),(#73420,#73421),(#73422,#73423),(#73424,#73425),
(#73426,#73427),(#73428,#73429),(#73430,#73431),(#73432,#73433),(#73434,
#73435),(#73436,#73437),(#73438,#73439),(#73440,#73441),(#73442,#73443),
(#73444,#73445),(#73446,#73447),(#73448,#73449),(#73450,#73451),(#73452,
#73453),(#73454,#73455),(#73456,#73457),(#73458,#73459),(#73460,#73461),
(#73462,#73463),(#73464,#73465),(#73466,#73467),(#73468,#73469),(#73470,
#73471),(#73472,#73473),(#73474,#73475),(#73476,#73477),(#73478,#73479),
(#73480,#73481),(#73482,#73483),(#73484,#73485),(#73486,#73487),(#73488,
#73489),(#73490,#73491),(#73492,#73493),(#73494,#73495),(#73496,#73497),
(#73498,#73499),(#73500,#73501),(#73502,#73503),(#73504,#73505),(#73506,
#73507),(#73508,#73509),(#73510,#73511),(#73512,#73513),(#73514,#73515),
(#73516,#73517),(#73518,#73519),(#73520,#73521),(#73522,#73523),(#73524,
#73525),(#73526,#73527),(#73528,#73529),(#73530,#73531),(#73532,#73533),
(#73534,#73535),(#73536,#73537),(#73538,#73539),(#73540,#73541),(#73542,
#73543),(#73544,#73545),(#73546,#73547),(#73548,#73549),(#73550,#73551),
(#73552,#73553),(#73554,#73555),(#73556,#73557),(#73558,#73559),(#73560,
#73561),(#73562,#73563),(#73564,#73565),(#73566,#73567),(#73568,#73569),
(#73570,#73571),(#73572,#73573),(#73574,#73575),(#73576,#73577),(#73578,
#73579),(#73580,#73581),(#73582,#73583),(#73584,#73585),(#73586,#73587),
(#73588,#73589),(#73590,#73591),(#73592,#73593),(#73594,#73595),(#73596,
#73597),(#73598,#73599),(#73600,#73601),(#73602,#73603),(#73604,#73605),
(#73606,#73607),(#73608,#73609),(#73610,#73611),(#73612,#73613),(#73614,
#73615),(#73616,#73617),(#73618,#73619),(#73620,#73621),(#73622,#73623),
(#73624,#73625),(#73626,#73627),(#73628,#73629),(#73630,#73631),(#73632,
#73633),(#73634,#73635),(#73636,#73637),(#73638,#73639)),.UNSPECIFIED.,
 .F.,.F.,.F.)
B_SPLINE_SURFACE_WITH_KNOTS((6,1,1,1,1,1,1,1,1,1,1,1,1,1,1,1,1,1,1,1,1,
1,1,1,1,1,1,1,1,1,1,1,1,1,1,1,1,1,1,1,1,1,1,1,1,1,1,1,1,1,1,1,1,1,1,1,1,
1,1,1,1,1,1,1,1,1,1,1,1,1,1,1,1,1,1,1,1,1,1,1,1,1,1,1,1,1,1,1,1,1,1,1,1,
1,1,1,1,1,1,1,1,1,1,1,1,1,1,1,1,1,1,1,1,1,1,1,1,1,1,1,1,1,1,1,1,1,1,1,1,
1,1,1,1,1,1,1,1,1,1,1,1,1,1,1,1,1,1,1,1,1,1,1,1,1,1,1,1,1,1,1,1,1,1,1,1,
1,1,1,1,1,1,1,1,1,1,1,1,1,1,1,1,1,1,1,1,1,1,1,1,1,1,1,1,1,1,1,1,1,1,1,6),
(2,2),(0.,0.005,0.01,0.015,0.02,0.025,0.03,0.035,0.04,0.045,0.05,0.055,
0.06,0.065,0.07,0.075,0.08,0.085,0.09,0.095,0.1,0.105,0.11,0.115,0.12,0.125,
0.13,0.135,0.14,0.145,0.15,0.155,0.16,0.165,0.17,0.175,0.18,0.185,0.19,
0.195,0.2,0.205,0.21,0.215,0.22,0.225,0.23,0.235,0.24,0.245,0.25,0.255,
0.26,0.265,0.27,0.275,0.28,0.285,0.29,0.295,0.3,0.305,0.31,0.315,0.32,0.325,
0.33,0.335,0.34,0.345,0.35,0.355,0.36,0.365,0.37,0.375,0.38,0.385,0.39,
0.395,0.4,0.405,0.41,0.415,0.42,0.425,0.43,0.435,0.44,0.445,0.45,0.455,
0.46,0.465,0.47,0.475,0.48,0.485,0.49,0.495,0.5,0.505,0.51,0.515,0.52,0.525,
0.53,0.535,0.54,0.545,0.55,0.555,0.56,0.565,0.57,0.575,0.58,0.585,0.59,
0.595,0.6,0.605,0.61,0.615,0.62,0.625,0.63,0.635,0.64,0.645,0.65,0.655,
0.66,0.665,0.67,0.675,0.68,0.685,0.690000000000001,0.695000000000001,0.700000000000001,
0.705000000000001,0.710000000000001,0.715000000000001,0.720000000000001,
0.725000000000001,0.730000000000001,0.735000000000001,0.740000000000001,
0.745000000000001,0.750000000000001,0.755000000000001,0.760000000000001,
0.765000000000001,0.770000000000001,0.775000000000001,0.780000000000001,
0.785000000000001,0.790000000000001,0.795000000000001,0.800000000000001,
0.805000000000001,0.810000000000001,0.815000000000001,0.820000000000001,
0.825000000000001,0.830000000000001,0.835000000000001,0.840000000000001,
0.845000000000001,0.850000000000001,0.855000000000001,0.860000000000001,
0.865000000000001,0.870000000000001,0.875000000000001,0.880000000000001,
0.885000000000001,0.890000000000001,0.895000000000001,0.900000000000001,
0.905000000000001,0.910000000000001,0.915000000000001,0.920000000000001,
0.925000000000001,0.930000000000001,0.935000000000001,0.940000000000001,
0.945000000000001,0.950000000000001,0.955000000000001,0.960000000000001,
0.965000000000001,0.970000000000001,0.975000000000001,0.980000000000001,
0.985000000000001,0.990000000000001,0.995000000000001,1.),(0.,1.2),
 .UNSPECIFIED.)
GEOMETRIC_REPRESENTATION_ITEM()
RATIONAL_B_SPLINE_SURFACE(((1.,1.),(1.,1.),(1.,1.),(1.,1.),(1.,1.),(1.,
1.),(1.,1.),(1.,1.),(1.,1.),(1.,1.),(1.,1.),(1.,1.),(1.,1.),(1.,1.),(1.,
1.),(1.,1.),(1.,1.),(1.,1.),(1.,1.),(1.,1.),(1.,1.),(1.,1.),(1.,1.),(1.,
1.),(1.,1.),(1.,1.),(1.,1.),(1.,1.),(1.,1.),(1.,1.),(1.,1.),(1.,1.),(1.,
1.),(1.,1.),(1.,1.),(1.,1.),(1.,1.),(1.,1.),(1.,1.),(1.,1.),(1.,1.),(1.,
1.),(1.,1.),(1.,1.),(1.,1.),(1.,1.),(1.,1.),(1.,1.),(1.,1.),(1.,1.),(1.,
1.),(1.,1.),(1.,1.),(1.,1.),(1.,1.),(1.,1.),(1.,1.),(1.,1.),(1.,1.),(1.,
1.),(1.,1.),(1.,1.),(1.,1.),(1.,1.),(1.,1.),(1.,1.),(1.,1.),(1.,1.),(1.,
1.),(1.,1.),(1.,1.),(1.,1.),(1.,1.),(1.,1.),(1.,1.),(1.,1.),(1.,1.),(1.,
1.),(1.,1.),(1.,1.),(1.,1.),(1.,1.),(1.,1.),(1.,1.),(1.,1.),(1.,1.),(1.,
1.),(1.,1.),(1.,1.),(1.,1.),(1.,1.),(1.,1.),(1.,1.),(1.,1.),(1.,1.),(1.,
1.),(1.,1.),(1.,1.),(1.,1.),(1.,1.),(1.,1.),(1.,1.),(1.,1.),(1.,1.),(1.,
1.),(1.,1.),(1.,1.),(1.,1.),(1.,1.),(1.,1.),(1.,1.),(1.,1.),(1.,1.),(1.,
1.),(1.,1.),(1.,1.),(1.,1.),(1.,1.),(1.,1.),(1.,1.),(1.,1.),(1.,1.),(1.,
1.),(1.,1.),(1.,1.),(1.,1.),(1.,1.),(1.,1.),(1.,1.),(1.,1.),(1.,1.),(1.,
1.),(1.,1.),(1.,1.),(1.,1.),(1.,1.),(1.,1.),(1.,1.),(1.,1.),(1.,1.),(1.,
1.),(1.,1.),(1.,1.),(1.,1.),(1.,1.),(1.,1.),(1.,1.),(1.,1.),(1.,1.),(1.,
1.),(1.,1.),(1.,1.),(1.,1.),(1.,1.),(1.,1.),(1.,1.),(1.,1.),(1.,1.),(1.,
1.),(1.,1.),(1.,1.),(1.,1.),(1.,1.),(1.,1.),(1.,1.),(1.,1.),(1.,1.),(1.,
1.),(1.,1.),(1.,1.),(1.,1.),(1.,1.),(1.,1.),(1.,1.),(1.,1.),(1.,1.),(1.,
1.),(1.,1.),(1.,1.),(1.,1.),(1.,1.),(1.,1.),(1.,1.),(1.,1.),(1.,1.),(1.,
1.),(1.,1.),(1.,1.),(1.,1.),(1.,1.),(1.,1.),(1.,1.),(1.,1.),(1.,1.),(1.,
1.),(1.,1.),(1.,1.),(1.,1.),(1.,1.),(1.,1.),(1.,1.),(1.,1.),(1.,1.),(1.,
1.),(1.,1.)))
REPRESENTATION_ITEM('')
SURFACE()
);
#907=(
BOUNDED_SURFACE()
B_SPLINE_SURFACE(5,1,((#74126,#74127),(#74128,#74129),(#74130,#74131),(#74132,
#74133),(#74134,#74135),(#74136,#74137),(#74138,#74139),(#74140,#74141),
(#74142,#74143),(#74144,#74145),(#74146,#74147),(#74148,#74149),(#74150,
#74151),(#74152,#74153),(#74154,#74155),(#74156,#74157),(#74158,#74159),
(#74160,#74161),(#74162,#74163),(#74164,#74165),(#74166,#74167),(#74168,
#74169),(#74170,#74171),(#74172,#74173),(#74174,#74175),(#74176,#74177),
(#74178,#74179),(#74180,#74181),(#74182,#74183),(#74184,#74185),(#74186,
#74187),(#74188,#74189),(#74190,#74191),(#74192,#74193),(#74194,#74195),
(#74196,#74197),(#74198,#74199),(#74200,#74201),(#74202,#74203),(#74204,
#74205),(#74206,#74207),(#74208,#74209),(#74210,#74211),(#74212,#74213),
(#74214,#74215),(#74216,#74217),(#74218,#74219),(#74220,#74221),(#74222,
#74223),(#74224,#74225),(#74226,#74227),(#74228,#74229),(#74230,#74231),
(#74232,#74233),(#74234,#74235),(#74236,#74237),(#74238,#74239),(#74240,
#74241),(#74242,#74243),(#74244,#74245),(#74246,#74247),(#74248,#74249),
(#74250,#74251),(#74252,#74253),(#74254,#74255),(#74256,#74257),(#74258,
#74259),(#74260,#74261),(#74262,#74263),(#74264,#74265),(#74266,#74267),
(#74268,#74269),(#74270,#74271),(#74272,#74273),(#74274,#74275),(#74276,
#74277),(#74278,#74279),(#74280,#74281),(#74282,#74283),(#74284,#74285),
(#74286,#74287),(#74288,#74289),(#74290,#74291),(#74292,#74293),(#74294,
#74295),(#74296,#74297),(#74298,#74299),(#74300,#74301),(#74302,#74303),
(#74304,#74305),(#74306,#74307),(#74308,#74309),(#74310,#74311),(#74312,
#74313),(#74314,#74315),(#74316,#74317),(#74318,#74319),(#74320,#74321),
(#74322,#74323),(#74324,#74325),(#74326,#74327),(#74328,#74329),(#74330,
#74331),(#74332,#74333),(#74334,#74335),(#74336,#74337),(#74338,#74339),
(#74340,#74341),(#74342,#74343),(#74344,#74345),(#74346,#74347),(#74348,
#74349),(#74350,#74351),(#74352,#74353),(#74354,#74355),(#74356,#74357),
(#74358,#74359),(#74360,#74361),(#74362,#74363),(#74364,#74365),(#74366,
#74367),(#74368,#74369),(#74370,#74371),(#74372,#74373),(#74374,#74375),
(#74376,#74377),(#74378,#74379),(#74380,#74381),(#74382,#74383),(#74384,
#74385),(#74386,#74387),(#74388,#74389),(#74390,#74391),(#74392,#74393),
(#74394,#74395),(#74396,#74397),(#74398,#74399),(#74400,#74401),(#74402,
#74403),(#74404,#74405),(#74406,#74407),(#74408,#74409),(#74410,#74411),
(#74412,#74413),(#74414,#74415),(#74416,#74417),(#74418,#74419),(#74420,
#74421),(#74422,#74423),(#74424,#74425),(#74426,#74427),(#74428,#74429),
(#74430,#74431),(#74432,#74433),(#74434,#74435),(#74436,#74437),(#74438,
#74439),(#74440,#74441),(#74442,#74443),(#74444,#74445),(#74446,#74447),
(#74448,#74449),(#74450,#74451),(#74452,#74453),(#74454,#74455),(#74456,
#74457),(#74458,#74459),(#74460,#74461),(#74462,#74463),(#74464,#74465),
(#74466,#74467),(#74468,#74469),(#74470,#74471),(#74472,#74473),(#74474,
#74475),(#74476,#74477),(#74478,#74479),(#74480,#74481),(#74482,#74483),
(#74484,#74485),(#74486,#74487),(#74488,#74489),(#74490,#74491),(#74492,
#74493),(#74494,#74495),(#74496,#74497),(#74498,#74499),(#74500,#74501),
(#74502,#74503),(#74504,#74505),(#74506,#74507),(#74508,#74509),(#74510,
#74511),(#74512,#74513),(#74514,#74515),(#74516,#74517),(#74518,#74519),
(#74520,#74521),(#74522,#74523),(#74524,#74525),(#74526,#74527),(#74528,
#74529),(#74530,#74531),(#74532,#74533),(#74534,#74535)),.UNSPECIFIED.,
 .F.,.F.,.F.)
B_SPLINE_SURFACE_WITH_KNOTS((6,1,1,1,1,1,1,1,1,1,1,1,1,1,1,1,1,1,1,1,1,
1,1,1,1,1,1,1,1,1,1,1,1,1,1,1,1,1,1,1,1,1,1,1,1,1,1,1,1,1,1,1,1,1,1,1,1,
1,1,1,1,1,1,1,1,1,1,1,1,1,1,1,1,1,1,1,1,1,1,1,1,1,1,1,1,1,1,1,1,1,1,1,1,
1,1,1,1,1,1,1,1,1,1,1,1,1,1,1,1,1,1,1,1,1,1,1,1,1,1,1,1,1,1,1,1,1,1,1,1,
1,1,1,1,1,1,1,1,1,1,1,1,1,1,1,1,1,1,1,1,1,1,1,1,1,1,1,1,1,1,1,1,1,1,1,1,
1,1,1,1,1,1,1,1,1,1,1,1,1,1,1,1,1,1,1,1,1,1,1,1,1,1,1,1,1,1,1,1,1,1,1,6),
(2,2),(0.,0.005,0.01,0.015,0.02,0.025,0.03,0.035,0.04,0.045,0.05,0.055,
0.06,0.065,0.07,0.075,0.08,0.085,0.09,0.095,0.1,0.105,0.11,0.115,0.12,0.125,
0.13,0.135,0.14,0.145,0.15,0.155,0.16,0.165,0.17,0.175,0.18,0.185,0.19,
0.195,0.2,0.205,0.21,0.215,0.22,0.225,0.23,0.235,0.24,0.245,0.25,0.255,
0.26,0.265,0.27,0.275,0.28,0.285,0.29,0.295,0.3,0.305,0.31,0.315,0.32,0.325,
0.33,0.335,0.34,0.345,0.35,0.355,0.36,0.365,0.37,0.375,0.38,0.385,0.39,
0.395,0.4,0.405,0.41,0.415,0.42,0.425,0.43,0.435,0.44,0.445,0.45,0.455,
0.46,0.465,0.47,0.475,0.48,0.485,0.49,0.495,0.5,0.505,0.51,0.515,0.52,0.525,
0.53,0.535,0.54,0.545,0.55,0.555,0.56,0.565,0.57,0.575,0.58,0.585,0.59,
0.595,0.6,0.605,0.61,0.615,0.62,0.625,0.63,0.635,0.64,0.645,0.65,0.655,
0.66,0.665,0.67,0.675,0.68,0.685,0.690000000000001,0.695000000000001,0.700000000000001,
0.705000000000001,0.710000000000001,0.715000000000001,0.720000000000001,
0.725000000000001,0.730000000000001,0.735000000000001,0.740000000000001,
0.745000000000001,0.750000000000001,0.755000000000001,0.760000000000001,
0.765000000000001,0.770000000000001,0.775000000000001,0.780000000000001,
0.785000000000001,0.790000000000001,0.795000000000001,0.800000000000001,
0.805000000000001,0.810000000000001,0.815000000000001,0.820000000000001,
0.825000000000001,0.830000000000001,0.835000000000001,0.840000000000001,
0.845000000000001,0.850000000000001,0.855000000000001,0.860000000000001,
0.865000000000001,0.870000000000001,0.875000000000001,0.880000000000001,
0.885000000000001,0.890000000000001,0.895000000000001,0.900000000000001,
0.905000000000001,0.910000000000001,0.915000000000001,0.920000000000001,
0.925000000000001,0.930000000000001,0.935000000000001,0.940000000000001,
0.945000000000001,0.950000000000001,0.955000000000001,0.960000000000001,
0.965000000000001,0.970000000000001,0.975000000000001,0.980000000000001,
0.985000000000001,0.990000000000001,0.995000000000001,1.),(0.,1.2),
 .UNSPECIFIED.)
GEOMETRIC_REPRESENTATION_ITEM()
RATIONAL_B_SPLINE_SURFACE(((1.,1.),(1.,1.),(1.,1.),(1.,1.),(1.,1.),(1.,
1.),(1.,1.),(1.,1.),(1.,1.),(1.,1.),(1.,1.),(1.,1.),(1.,1.),(1.,1.),(1.,
1.),(1.,1.),(1.,1.),(1.,1.),(1.,1.),(1.,1.),(1.,1.),(1.,1.),(1.,1.),(1.,
1.),(1.,1.),(1.,1.),(1.,1.),(1.,1.),(1.,1.),(1.,1.),(1.,1.),(1.,1.),(1.,
1.),(1.,1.),(1.,1.),(1.,1.),(1.,1.),(1.,1.),(1.,1.),(1.,1.),(1.,1.),(1.,
1.),(1.,1.),(1.,1.),(1.,1.),(1.,1.),(1.,1.),(1.,1.),(1.,1.),(1.,1.),(1.,
1.),(1.,1.),(1.,1.),(1.,1.),(1.,1.),(1.,1.),(1.,1.),(1.,1.),(1.,1.),(1.,
1.),(1.,1.),(1.,1.),(1.,1.),(1.,1.),(1.,1.),(1.,1.),(1.,1.),(1.,1.),(1.,
1.),(1.,1.),(1.,1.),(1.,1.),(1.,1.),(1.,1.),(1.,1.),(1.,1.),(1.,1.),(1.,
1.),(1.,1.),(1.,1.),(1.,1.),(1.,1.),(1.,1.),(1.,1.),(1.,1.),(1.,1.),(1.,
1.),(1.,1.),(1.,1.),(1.,1.),(1.,1.),(1.,1.),(1.,1.),(1.,1.),(1.,1.),(1.,
1.),(1.,1.),(1.,1.),(1.,1.),(1.,1.),(1.,1.),(1.,1.),(1.,1.),(1.,1.),(1.,
1.),(1.,1.),(1.,1.),(1.,1.),(1.,1.),(1.,1.),(1.,1.),(1.,1.),(1.,1.),(1.,
1.),(1.,1.),(1.,1.),(1.,1.),(1.,1.),(1.,1.),(1.,1.),(1.,1.),(1.,1.),(1.,
1.),(1.,1.),(1.,1.),(1.,1.),(1.,1.),(1.,1.),(1.,1.),(1.,1.),(1.,1.),(1.,
1.),(1.,1.),(1.,1.),(1.,1.),(1.,1.),(1.,1.),(1.,1.),(1.,1.),(1.,1.),(1.,
1.),(1.,1.),(1.,1.),(1.,1.),(1.,1.),(1.,1.),(1.,1.),(1.,1.),(1.,1.),(1.,
1.),(1.,1.),(1.,1.),(1.,1.),(1.,1.),(1.,1.),(1.,1.),(1.,1.),(1.,1.),(1.,
1.),(1.,1.),(1.,1.),(1.,1.),(1.,1.),(1.,1.),(1.,1.),(1.,1.),(1.,1.),(1.,
1.),(1.,1.),(1.,1.),(1.,1.),(1.,1.),(1.,1.),(1.,1.),(1.,1.),(1.,1.),(1.,
1.),(1.,1.),(1.,1.),(1.,1.),(1.,1.),(1.,1.),(1.,1.),(1.,1.),(1.,1.),(1.,
1.),(1.,1.),(1.,1.),(1.,1.),(1.,1.),(1.,1.),(1.,1.),(1.,1.),(1.,1.),(1.,
1.),(1.,1.),(1.,1.),(1.,1.),(1.,1.),(1.,1.),(1.,1.),(1.,1.),(1.,1.),(1.,
1.),(1.,1.)))
REPRESENTATION_ITEM('')
SURFACE()
);
#908=(
BOUNDED_SURFACE()
B_SPLINE_SURFACE(5,1,((#75022,#75023),(#75024,#75025),(#75026,#75027),(#75028,
#75029),(#75030,#75031),(#75032,#75033),(#75034,#75035),(#75036,#75037),
(#75038,#75039),(#75040,#75041),(#75042,#75043),(#75044,#75045),(#75046,
#75047),(#75048,#75049),(#75050,#75051),(#75052,#75053),(#75054,#75055),
(#75056,#75057),(#75058,#75059),(#75060,#75061),(#75062,#75063),(#75064,
#75065),(#75066,#75067),(#75068,#75069),(#75070,#75071),(#75072,#75073),
(#75074,#75075),(#75076,#75077),(#75078,#75079),(#75080,#75081),(#75082,
#75083),(#75084,#75085),(#75086,#75087),(#75088,#75089),(#75090,#75091),
(#75092,#75093),(#75094,#75095),(#75096,#75097),(#75098,#75099),(#75100,
#75101),(#75102,#75103),(#75104,#75105),(#75106,#75107),(#75108,#75109),
(#75110,#75111),(#75112,#75113),(#75114,#75115),(#75116,#75117),(#75118,
#75119),(#75120,#75121),(#75122,#75123),(#75124,#75125),(#75126,#75127),
(#75128,#75129),(#75130,#75131),(#75132,#75133),(#75134,#75135),(#75136,
#75137),(#75138,#75139),(#75140,#75141),(#75142,#75143),(#75144,#75145),
(#75146,#75147),(#75148,#75149),(#75150,#75151),(#75152,#75153),(#75154,
#75155),(#75156,#75157),(#75158,#75159),(#75160,#75161),(#75162,#75163),
(#75164,#75165),(#75166,#75167),(#75168,#75169),(#75170,#75171),(#75172,
#75173),(#75174,#75175),(#75176,#75177),(#75178,#75179),(#75180,#75181),
(#75182,#75183),(#75184,#75185),(#75186,#75187),(#75188,#75189),(#75190,
#75191),(#75192,#75193),(#75194,#75195),(#75196,#75197),(#75198,#75199),
(#75200,#75201),(#75202,#75203),(#75204,#75205),(#75206,#75207),(#75208,
#75209),(#75210,#75211),(#75212,#75213),(#75214,#75215),(#75216,#75217),
(#75218,#75219),(#75220,#75221),(#75222,#75223),(#75224,#75225),(#75226,
#75227),(#75228,#75229),(#75230,#75231),(#75232,#75233),(#75234,#75235),
(#75236,#75237),(#75238,#75239),(#75240,#75241),(#75242,#75243),(#75244,
#75245),(#75246,#75247),(#75248,#75249),(#75250,#75251),(#75252,#75253),
(#75254,#75255),(#75256,#75257),(#75258,#75259),(#75260,#75261),(#75262,
#75263),(#75264,#75265),(#75266,#75267),(#75268,#75269),(#75270,#75271),
(#75272,#75273),(#75274,#75275),(#75276,#75277),(#75278,#75279),(#75280,
#75281),(#75282,#75283),(#75284,#75285),(#75286,#75287),(#75288,#75289),
(#75290,#75291),(#75292,#75293),(#75294,#75295),(#75296,#75297),(#75298,
#75299),(#75300,#75301),(#75302,#75303),(#75304,#75305),(#75306,#75307),
(#75308,#75309),(#75310,#75311),(#75312,#75313),(#75314,#75315),(#75316,
#75317),(#75318,#75319),(#75320,#75321),(#75322,#75323),(#75324,#75325),
(#75326,#75327),(#75328,#75329),(#75330,#75331),(#75332,#75333),(#75334,
#75335),(#75336,#75337),(#75338,#75339),(#75340,#75341),(#75342,#75343),
(#75344,#75345),(#75346,#75347),(#75348,#75349),(#75350,#75351),(#75352,
#75353),(#75354,#75355),(#75356,#75357),(#75358,#75359),(#75360,#75361),
(#75362,#75363),(#75364,#75365),(#75366,#75367),(#75368,#75369),(#75370,
#75371),(#75372,#75373),(#75374,#75375),(#75376,#75377),(#75378,#75379),
(#75380,#75381),(#75382,#75383),(#75384,#75385),(#75386,#75387),(#75388,
#75389),(#75390,#75391),(#75392,#75393),(#75394,#75395),(#75396,#75397),
(#75398,#75399),(#75400,#75401),(#75402,#75403),(#75404,#75405),(#75406,
#75407),(#75408,#75409),(#75410,#75411),(#75412,#75413),(#75414,#75415),
(#75416,#75417),(#75418,#75419),(#75420,#75421),(#75422,#75423),(#75424,
#75425),(#75426,#75427),(#75428,#75429),(#75430,#75431)),.UNSPECIFIED.,
 .F.,.F.,.F.)
B_SPLINE_SURFACE_WITH_KNOTS((6,1,1,1,1,1,1,1,1,1,1,1,1,1,1,1,1,1,1,1,1,
1,1,1,1,1,1,1,1,1,1,1,1,1,1,1,1,1,1,1,1,1,1,1,1,1,1,1,1,1,1,1,1,1,1,1,1,
1,1,1,1,1,1,1,1,1,1,1,1,1,1,1,1,1,1,1,1,1,1,1,1,1,1,1,1,1,1,1,1,1,1,1,1,
1,1,1,1,1,1,1,1,1,1,1,1,1,1,1,1,1,1,1,1,1,1,1,1,1,1,1,1,1,1,1,1,1,1,1,1,
1,1,1,1,1,1,1,1,1,1,1,1,1,1,1,1,1,1,1,1,1,1,1,1,1,1,1,1,1,1,1,1,1,1,1,1,
1,1,1,1,1,1,1,1,1,1,1,1,1,1,1,1,1,1,1,1,1,1,1,1,1,1,1,1,1,1,1,1,1,1,1,6),
(2,2),(0.,0.005,0.01,0.015,0.02,0.025,0.03,0.035,0.04,0.045,0.05,0.055,
0.06,0.065,0.07,0.075,0.08,0.085,0.09,0.095,0.1,0.105,0.11,0.115,0.12,0.125,
0.13,0.135,0.14,0.145,0.15,0.155,0.16,0.165,0.17,0.175,0.18,0.185,0.19,
0.195,0.2,0.205,0.21,0.215,0.22,0.225,0.23,0.235,0.24,0.245,0.25,0.255,
0.26,0.265,0.27,0.275,0.28,0.285,0.29,0.295,0.3,0.305,0.31,0.315,0.32,0.325,
0.33,0.335,0.34,0.345,0.35,0.355,0.36,0.365,0.37,0.375,0.38,0.385,0.39,
0.395,0.4,0.405,0.41,0.415,0.42,0.425,0.43,0.435,0.44,0.445,0.45,0.455,
0.46,0.465,0.47,0.475,0.48,0.485,0.49,0.495,0.5,0.505,0.51,0.515,0.52,0.525,
0.53,0.535,0.54,0.545,0.55,0.555,0.56,0.565,0.57,0.575,0.58,0.585,0.59,
0.595,0.6,0.605,0.61,0.615,0.62,0.625,0.63,0.635,0.64,0.645,0.65,0.655,
0.66,0.665,0.67,0.675,0.68,0.685,0.690000000000001,0.695000000000001,0.700000000000001,
0.705000000000001,0.710000000000001,0.715000000000001,0.720000000000001,
0.725000000000001,0.730000000000001,0.735000000000001,0.740000000000001,
0.745000000000001,0.750000000000001,0.755000000000001,0.760000000000001,
0.765000000000001,0.770000000000001,0.775000000000001,0.780000000000001,
0.785000000000001,0.790000000000001,0.795000000000001,0.800000000000001,
0.805000000000001,0.810000000000001,0.815000000000001,0.820000000000001,
0.825000000000001,0.830000000000001,0.835000000000001,0.840000000000001,
0.845000000000001,0.850000000000001,0.855000000000001,0.860000000000001,
0.865000000000001,0.870000000000001,0.875000000000001,0.880000000000001,
0.885000000000001,0.890000000000001,0.895000000000001,0.900000000000001,
0.905000000000001,0.910000000000001,0.915000000000001,0.920000000000001,
0.925000000000001,0.930000000000001,0.935000000000001,0.940000000000001,
0.945000000000001,0.950000000000001,0.955000000000001,0.960000000000001,
0.965000000000001,0.970000000000001,0.975000000000001,0.980000000000001,
0.985000000000001,0.990000000000001,0.995000000000001,1.),(0.,1.2),
 .UNSPECIFIED.)
GEOMETRIC_REPRESENTATION_ITEM()
RATIONAL_B_SPLINE_SURFACE(((1.,1.),(1.,1.),(1.,1.),(1.,1.),(1.,1.),(1.,
1.),(1.,1.),(1.,1.),(1.,1.),(1.,1.),(1.,1.),(1.,1.),(1.,1.),(1.,1.),(1.,
1.),(1.,1.),(1.,1.),(1.,1.),(1.,1.),(1.,1.),(1.,1.),(1.,1.),(1.,1.),(1.,
1.),(1.,1.),(1.,1.),(1.,1.),(1.,1.),(1.,1.),(1.,1.),(1.,1.),(1.,1.),(1.,
1.),(1.,1.),(1.,1.),(1.,1.),(1.,1.),(1.,1.),(1.,1.),(1.,1.),(1.,1.),(1.,
1.),(1.,1.),(1.,1.),(1.,1.),(1.,1.),(1.,1.),(1.,1.),(1.,1.),(1.,1.),(1.,
1.),(1.,1.),(1.,1.),(1.,1.),(1.,1.),(1.,1.),(1.,1.),(1.,1.),(1.,1.),(1.,
1.),(1.,1.),(1.,1.),(1.,1.),(1.,1.),(1.,1.),(1.,1.),(1.,1.),(1.,1.),(1.,
1.),(1.,1.),(1.,1.),(1.,1.),(1.,1.),(1.,1.),(1.,1.),(1.,1.),(1.,1.),(1.,
1.),(1.,1.),(1.,1.),(1.,1.),(1.,1.),(1.,1.),(1.,1.),(1.,1.),(1.,1.),(1.,
1.),(1.,1.),(1.,1.),(1.,1.),(1.,1.),(1.,1.),(1.,1.),(1.,1.),(1.,1.),(1.,
1.),(1.,1.),(1.,1.),(1.,1.),(1.,1.),(1.,1.),(1.,1.),(1.,1.),(1.,1.),(1.,
1.),(1.,1.),(1.,1.),(1.,1.),(1.,1.),(1.,1.),(1.,1.),(1.,1.),(1.,1.),(1.,
1.),(1.,1.),(1.,1.),(1.,1.),(1.,1.),(1.,1.),(1.,1.),(1.,1.),(1.,1.),(1.,
1.),(1.,1.),(1.,1.),(1.,1.),(1.,1.),(1.,1.),(1.,1.),(1.,1.),(1.,1.),(1.,
1.),(1.,1.),(1.,1.),(1.,1.),(1.,1.),(1.,1.),(1.,1.),(1.,1.),(1.,1.),(1.,
1.),(1.,1.),(1.,1.),(1.,1.),(1.,1.),(1.,1.),(1.,1.),(1.,1.),(1.,1.),(1.,
1.),(1.,1.),(1.,1.),(1.,1.),(1.,1.),(1.,1.),(1.,1.),(1.,1.),(1.,1.),(1.,
1.),(1.,1.),(1.,1.),(1.,1.),(1.,1.),(1.,1.),(1.,1.),(1.,1.),(1.,1.),(1.,
1.),(1.,1.),(1.,1.),(1.,1.),(1.,1.),(1.,1.),(1.,1.),(1.,1.),(1.,1.),(1.,
1.),(1.,1.),(1.,1.),(1.,1.),(1.,1.),(1.,1.),(1.,1.),(1.,1.),(1.,1.),(1.,
1.),(1.,1.),(1.,1.),(1.,1.),(1.,1.),(1.,1.),(1.,1.),(1.,1.),(1.,1.),(1.,
1.),(1.,1.),(1.,1.),(1.,1.),(1.,1.),(1.,1.),(1.,1.),(1.,1.),(1.,1.),(1.,
1.),(1.,1.)))
REPRESENTATION_ITEM('')
SURFACE()
);
#909=(
BOUNDED_SURFACE()
B_SPLINE_SURFACE(5,1,((#75918,#75919),(#75920,#75921),(#75922,#75923),(#75924,
#75925),(#75926,#75927),(#75928,#75929),(#75930,#75931),(#75932,#75933),
(#75934,#75935),(#75936,#75937),(#75938,#75939),(#75940,#75941),(#75942,
#75943),(#75944,#75945),(#75946,#75947),(#75948,#75949),(#75950,#75951),
(#75952,#75953),(#75954,#75955),(#75956,#75957),(#75958,#75959),(#75960,
#75961),(#75962,#75963),(#75964,#75965),(#75966,#75967),(#75968,#75969),
(#75970,#75971),(#75972,#75973),(#75974,#75975),(#75976,#75977),(#75978,
#75979),(#75980,#75981),(#75982,#75983),(#75984,#75985),(#75986,#75987),
(#75988,#75989),(#75990,#75991),(#75992,#75993),(#75994,#75995),(#75996,
#75997),(#75998,#75999),(#76000,#76001),(#76002,#76003),(#76004,#76005),
(#76006,#76007),(#76008,#76009),(#76010,#76011),(#76012,#76013),(#76014,
#76015),(#76016,#76017),(#76018,#76019),(#76020,#76021),(#76022,#76023),
(#76024,#76025),(#76026,#76027),(#76028,#76029),(#76030,#76031),(#76032,
#76033),(#76034,#76035),(#76036,#76037),(#76038,#76039),(#76040,#76041),
(#76042,#76043),(#76044,#76045),(#76046,#76047),(#76048,#76049),(#76050,
#76051),(#76052,#76053),(#76054,#76055),(#76056,#76057),(#76058,#76059),
(#76060,#76061),(#76062,#76063),(#76064,#76065),(#76066,#76067),(#76068,
#76069),(#76070,#76071),(#76072,#76073),(#76074,#76075),(#76076,#76077),
(#76078,#76079),(#76080,#76081),(#76082,#76083),(#76084,#76085),(#76086,
#76087),(#76088,#76089),(#76090,#76091),(#76092,#76093),(#76094,#76095),
(#76096,#76097),(#76098,#76099),(#76100,#76101),(#76102,#76103),(#76104,
#76105),(#76106,#76107),(#76108,#76109),(#76110,#76111),(#76112,#76113),
(#76114,#76115),(#76116,#76117),(#76118,#76119),(#76120,#76121),(#76122,
#76123),(#76124,#76125),(#76126,#76127),(#76128,#76129),(#76130,#76131),
(#76132,#76133),(#76134,#76135),(#76136,#76137),(#76138,#76139),(#76140,
#76141),(#76142,#76143),(#76144,#76145),(#76146,#76147),(#76148,#76149),
(#76150,#76151),(#76152,#76153),(#76154,#76155),(#76156,#76157),(#76158,
#76159),(#76160,#76161),(#76162,#76163),(#76164,#76165),(#76166,#76167),
(#76168,#76169),(#76170,#76171),(#76172,#76173),(#76174,#76175),(#76176,
#76177),(#76178,#76179),(#76180,#76181),(#76182,#76183),(#76184,#76185),
(#76186,#76187),(#76188,#76189),(#76190,#76191),(#76192,#76193),(#76194,
#76195),(#76196,#76197),(#76198,#76199),(#76200,#76201),(#76202,#76203),
(#76204,#76205),(#76206,#76207),(#76208,#76209),(#76210,#76211),(#76212,
#76213),(#76214,#76215),(#76216,#76217),(#76218,#76219),(#76220,#76221),
(#76222,#76223),(#76224,#76225),(#76226,#76227),(#76228,#76229),(#76230,
#76231),(#76232,#76233),(#76234,#76235),(#76236,#76237),(#76238,#76239),
(#76240,#76241),(#76242,#76243),(#76244,#76245),(#76246,#76247),(#76248,
#76249),(#76250,#76251),(#76252,#76253),(#76254,#76255),(#76256,#76257),
(#76258,#76259),(#76260,#76261),(#76262,#76263),(#76264,#76265),(#76266,
#76267),(#76268,#76269),(#76270,#76271),(#76272,#76273),(#76274,#76275),
(#76276,#76277),(#76278,#76279),(#76280,#76281),(#76282,#76283),(#76284,
#76285),(#76286,#76287),(#76288,#76289),(#76290,#76291),(#76292,#76293),
(#76294,#76295),(#76296,#76297),(#76298,#76299),(#76300,#76301),(#76302,
#76303),(#76304,#76305),(#76306,#76307),(#76308,#76309),(#76310,#76311),
(#76312,#76313),(#76314,#76315),(#76316,#76317),(#76318,#76319),(#76320,
#76321),(#76322,#76323),(#76324,#76325),(#76326,#76327)),.UNSPECIFIED.,
 .F.,.F.,.F.)
B_SPLINE_SURFACE_WITH_KNOTS((6,1,1,1,1,1,1,1,1,1,1,1,1,1,1,1,1,1,1,1,1,
1,1,1,1,1,1,1,1,1,1,1,1,1,1,1,1,1,1,1,1,1,1,1,1,1,1,1,1,1,1,1,1,1,1,1,1,
1,1,1,1,1,1,1,1,1,1,1,1,1,1,1,1,1,1,1,1,1,1,1,1,1,1,1,1,1,1,1,1,1,1,1,1,
1,1,1,1,1,1,1,1,1,1,1,1,1,1,1,1,1,1,1,1,1,1,1,1,1,1,1,1,1,1,1,1,1,1,1,1,
1,1,1,1,1,1,1,1,1,1,1,1,1,1,1,1,1,1,1,1,1,1,1,1,1,1,1,1,1,1,1,1,1,1,1,1,
1,1,1,1,1,1,1,1,1,1,1,1,1,1,1,1,1,1,1,1,1,1,1,1,1,1,1,1,1,1,1,1,1,1,1,6),
(2,2),(0.,0.005,0.01,0.015,0.02,0.025,0.03,0.035,0.04,0.045,0.05,0.055,
0.06,0.065,0.07,0.075,0.08,0.085,0.09,0.095,0.1,0.105,0.11,0.115,0.12,0.125,
0.13,0.135,0.14,0.145,0.15,0.155,0.16,0.165,0.17,0.175,0.18,0.185,0.19,
0.195,0.2,0.205,0.21,0.215,0.22,0.225,0.23,0.235,0.24,0.245,0.25,0.255,
0.26,0.265,0.27,0.275,0.28,0.285,0.29,0.295,0.3,0.305,0.31,0.315,0.32,0.325,
0.33,0.335,0.34,0.345,0.35,0.355,0.36,0.365,0.37,0.375,0.38,0.385,0.39,
0.395,0.4,0.405,0.41,0.415,0.42,0.425,0.43,0.435,0.44,0.445,0.45,0.455,
0.46,0.465,0.47,0.475,0.48,0.485,0.49,0.495,0.5,0.505,0.51,0.515,0.52,0.525,
0.53,0.535,0.54,0.545,0.55,0.555,0.56,0.565,0.57,0.575,0.58,0.585,0.59,
0.595,0.6,0.605,0.61,0.615,0.62,0.625,0.63,0.635,0.64,0.645,0.65,0.655,
0.66,0.665,0.67,0.675,0.68,0.685,0.690000000000001,0.695000000000001,0.700000000000001,
0.705000000000001,0.710000000000001,0.715000000000001,0.720000000000001,
0.725000000000001,0.730000000000001,0.735000000000001,0.740000000000001,
0.745000000000001,0.750000000000001,0.755000000000001,0.760000000000001,
0.765000000000001,0.770000000000001,0.775000000000001,0.780000000000001,
0.785000000000001,0.790000000000001,0.795000000000001,0.800000000000001,
0.805000000000001,0.810000000000001,0.815000000000001,0.820000000000001,
0.825000000000001,0.830000000000001,0.835000000000001,0.840000000000001,
0.845000000000001,0.850000000000001,0.855000000000001,0.860000000000001,
0.865000000000001,0.870000000000001,0.875000000000001,0.880000000000001,
0.885000000000001,0.890000000000001,0.895000000000001,0.900000000000001,
0.905000000000001,0.910000000000001,0.915000000000001,0.920000000000001,
0.925000000000001,0.930000000000001,0.935000000000001,0.940000000000001,
0.945000000000001,0.950000000000001,0.955000000000001,0.960000000000001,
0.965000000000001,0.970000000000001,0.975000000000001,0.980000000000001,
0.985000000000001,0.990000000000001,0.995000000000001,1.),(0.,1.2),
 .UNSPECIFIED.)
GEOMETRIC_REPRESENTATION_ITEM()
RATIONAL_B_SPLINE_SURFACE(((1.,1.),(1.,1.),(1.,1.),(1.,1.),(1.,1.),(1.,
1.),(1.,1.),(1.,1.),(1.,1.),(1.,1.),(1.,1.),(1.,1.),(1.,1.),(1.,1.),(1.,
1.),(1.,1.),(1.,1.),(1.,1.),(1.,1.),(1.,1.),(1.,1.),(1.,1.),(1.,1.),(1.,
1.),(1.,1.),(1.,1.),(1.,1.),(1.,1.),(1.,1.),(1.,1.),(1.,1.),(1.,1.),(1.,
1.),(1.,1.),(1.,1.),(1.,1.),(1.,1.),(1.,1.),(1.,1.),(1.,1.),(1.,1.),(1.,
1.),(1.,1.),(1.,1.),(1.,1.),(1.,1.),(1.,1.),(1.,1.),(1.,1.),(1.,1.),(1.,
1.),(1.,1.),(1.,1.),(1.,1.),(1.,1.),(1.,1.),(1.,1.),(1.,1.),(1.,1.),(1.,
1.),(1.,1.),(1.,1.),(1.,1.),(1.,1.),(1.,1.),(1.,1.),(1.,1.),(1.,1.),(1.,
1.),(1.,1.),(1.,1.),(1.,1.),(1.,1.),(1.,1.),(1.,1.),(1.,1.),(1.,1.),(1.,
1.),(1.,1.),(1.,1.),(1.,1.),(1.,1.),(1.,1.),(1.,1.),(1.,1.),(1.,1.),(1.,
1.),(1.,1.),(1.,1.),(1.,1.),(1.,1.),(1.,1.),(1.,1.),(1.,1.),(1.,1.),(1.,
1.),(1.,1.),(1.,1.),(1.,1.),(1.,1.),(1.,1.),(1.,1.),(1.,1.),(1.,1.),(1.,
1.),(1.,1.),(1.,1.),(1.,1.),(1.,1.),(1.,1.),(1.,1.),(1.,1.),(1.,1.),(1.,
1.),(1.,1.),(1.,1.),(1.,1.),(1.,1.),(1.,1.),(1.,1.),(1.,1.),(1.,1.),(1.,
1.),(1.,1.),(1.,1.),(1.,1.),(1.,1.),(1.,1.),(1.,1.),(1.,1.),(1.,1.),(1.,
1.),(1.,1.),(1.,1.),(1.,1.),(1.,1.),(1.,1.),(1.,1.),(1.,1.),(1.,1.),(1.,
1.),(1.,1.),(1.,1.),(1.,1.),(1.,1.),(1.,1.),(1.,1.),(1.,1.),(1.,1.),(1.,
1.),(1.,1.),(1.,1.),(1.,1.),(1.,1.),(1.,1.),(1.,1.),(1.,1.),(1.,1.),(1.,
1.),(1.,1.),(1.,1.),(1.,1.),(1.,1.),(1.,1.),(1.,1.),(1.,1.),(1.,1.),(1.,
1.),(1.,1.),(1.,1.),(1.,1.),(1.,1.),(1.,1.),(1.,1.),(1.,1.),(1.,1.),(1.,
1.),(1.,1.),(1.,1.),(1.,1.),(1.,1.),(1.,1.),(1.,1.),(1.,1.),(1.,1.),(1.,
1.),(1.,1.),(1.,1.),(1.,1.),(1.,1.),(1.,1.),(1.,1.),(1.,1.),(1.,1.),(1.,
1.),(1.,1.),(1.,1.),(1.,1.),(1.,1.),(1.,1.),(1.,1.),(1.,1.),(1.,1.),(1.,
1.),(1.,1.)))
REPRESENTATION_ITEM('')
SURFACE()
);
#910=(
BOUNDED_SURFACE()
B_SPLINE_SURFACE(5,1,((#76814,#76815),(#76816,#76817),(#76818,#76819),(#76820,
#76821),(#76822,#76823),(#76824,#76825),(#76826,#76827),(#76828,#76829),
(#76830,#76831),(#76832,#76833),(#76834,#76835),(#76836,#76837),(#76838,
#76839),(#76840,#76841),(#76842,#76843),(#76844,#76845),(#76846,#76847),
(#76848,#76849),(#76850,#76851),(#76852,#76853),(#76854,#76855),(#76856,
#76857),(#76858,#76859),(#76860,#76861),(#76862,#76863),(#76864,#76865),
(#76866,#76867),(#76868,#76869),(#76870,#76871),(#76872,#76873),(#76874,
#76875),(#76876,#76877),(#76878,#76879),(#76880,#76881),(#76882,#76883),
(#76884,#76885),(#76886,#76887),(#76888,#76889),(#76890,#76891),(#76892,
#76893),(#76894,#76895),(#76896,#76897),(#76898,#76899),(#76900,#76901),
(#76902,#76903),(#76904,#76905),(#76906,#76907),(#76908,#76909),(#76910,
#76911),(#76912,#76913),(#76914,#76915),(#76916,#76917),(#76918,#76919),
(#76920,#76921),(#76922,#76923),(#76924,#76925),(#76926,#76927),(#76928,
#76929),(#76930,#76931),(#76932,#76933),(#76934,#76935),(#76936,#76937),
(#76938,#76939),(#76940,#76941),(#76942,#76943),(#76944,#76945),(#76946,
#76947),(#76948,#76949),(#76950,#76951),(#76952,#76953),(#76954,#76955),
(#76956,#76957),(#76958,#76959),(#76960,#76961),(#76962,#76963),(#76964,
#76965),(#76966,#76967),(#76968,#76969),(#76970,#76971),(#76972,#76973),
(#76974,#76975),(#76976,#76977),(#76978,#76979),(#76980,#76981),(#76982,
#76983),(#76984,#76985),(#76986,#76987),(#76988,#76989),(#76990,#76991),
(#76992,#76993),(#76994,#76995),(#76996,#76997),(#76998,#76999),(#77000,
#77001),(#77002,#77003),(#77004,#77005),(#77006,#77007),(#77008,#77009),
(#77010,#77011),(#77012,#77013),(#77014,#77015),(#77016,#77017),(#77018,
#77019),(#77020,#77021),(#77022,#77023),(#77024,#77025),(#77026,#77027),
(#77028,#77029),(#77030,#77031),(#77032,#77033),(#77034,#77035),(#77036,
#77037),(#77038,#77039),(#77040,#77041),(#77042,#77043),(#77044,#77045),
(#77046,#77047),(#77048,#77049),(#77050,#77051),(#77052,#77053),(#77054,
#77055),(#77056,#77057),(#77058,#77059),(#77060,#77061),(#77062,#77063),
(#77064,#77065),(#77066,#77067),(#77068,#77069),(#77070,#77071),(#77072,
#77073),(#77074,#77075),(#77076,#77077),(#77078,#77079),(#77080,#77081),
(#77082,#77083),(#77084,#77085),(#77086,#77087),(#77088,#77089),(#77090,
#77091),(#77092,#77093),(#77094,#77095),(#77096,#77097),(#77098,#77099),
(#77100,#77101),(#77102,#77103),(#77104,#77105),(#77106,#77107),(#77108,
#77109),(#77110,#77111),(#77112,#77113),(#77114,#77115),(#77116,#77117),
(#77118,#77119),(#77120,#77121),(#77122,#77123),(#77124,#77125),(#77126,
#77127),(#77128,#77129),(#77130,#77131),(#77132,#77133),(#77134,#77135),
(#77136,#77137),(#77138,#77139),(#77140,#77141),(#77142,#77143),(#77144,
#77145),(#77146,#77147),(#77148,#77149),(#77150,#77151),(#77152,#77153),
(#77154,#77155),(#77156,#77157),(#77158,#77159),(#77160,#77161),(#77162,
#77163),(#77164,#77165),(#77166,#77167),(#77168,#77169),(#77170,#77171),
(#77172,#77173),(#77174,#77175),(#77176,#77177),(#77178,#77179),(#77180,
#77181),(#77182,#77183),(#77184,#77185),(#77186,#77187),(#77188,#77189),
(#77190,#77191),(#77192,#77193),(#77194,#77195),(#77196,#77197),(#77198,
#77199),(#77200,#77201),(#77202,#77203),(#77204,#77205),(#77206,#77207),
(#77208,#77209),(#77210,#77211),(#77212,#77213),(#77214,#77215),(#77216,
#77217),(#77218,#77219),(#77220,#77221),(#77222,#77223)),.UNSPECIFIED.,
 .F.,.F.,.F.)
B_SPLINE_SURFACE_WITH_KNOTS((6,1,1,1,1,1,1,1,1,1,1,1,1,1,1,1,1,1,1,1,1,
1,1,1,1,1,1,1,1,1,1,1,1,1,1,1,1,1,1,1,1,1,1,1,1,1,1,1,1,1,1,1,1,1,1,1,1,
1,1,1,1,1,1,1,1,1,1,1,1,1,1,1,1,1,1,1,1,1,1,1,1,1,1,1,1,1,1,1,1,1,1,1,1,
1,1,1,1,1,1,1,1,1,1,1,1,1,1,1,1,1,1,1,1,1,1,1,1,1,1,1,1,1,1,1,1,1,1,1,1,
1,1,1,1,1,1,1,1,1,1,1,1,1,1,1,1,1,1,1,1,1,1,1,1,1,1,1,1,1,1,1,1,1,1,1,1,
1,1,1,1,1,1,1,1,1,1,1,1,1,1,1,1,1,1,1,1,1,1,1,1,1,1,1,1,1,1,1,1,1,1,1,6),
(2,2),(0.,0.005,0.01,0.015,0.02,0.025,0.03,0.035,0.04,0.045,0.05,0.055,
0.06,0.065,0.07,0.075,0.08,0.085,0.09,0.095,0.1,0.105,0.11,0.115,0.12,0.125,
0.13,0.135,0.14,0.145,0.15,0.155,0.16,0.165,0.17,0.175,0.18,0.185,0.19,
0.195,0.2,0.205,0.21,0.215,0.22,0.225,0.23,0.235,0.24,0.245,0.25,0.255,
0.26,0.265,0.27,0.275,0.28,0.285,0.29,0.295,0.3,0.305,0.31,0.315,0.32,0.325,
0.33,0.335,0.34,0.345,0.35,0.355,0.36,0.365,0.37,0.375,0.38,0.385,0.39,
0.395,0.4,0.405,0.41,0.415,0.42,0.425,0.43,0.435,0.44,0.445,0.45,0.455,
0.46,0.465,0.47,0.475,0.48,0.485,0.49,0.495,0.5,0.505,0.51,0.515,0.52,0.525,
0.53,0.535,0.54,0.545,0.55,0.555,0.56,0.565,0.57,0.575,0.58,0.585,0.59,
0.595,0.6,0.605,0.61,0.615,0.62,0.625,0.63,0.635,0.64,0.645,0.65,0.655,
0.66,0.665,0.67,0.675,0.68,0.685,0.690000000000001,0.695000000000001,0.700000000000001,
0.705000000000001,0.710000000000001,0.715000000000001,0.720000000000001,
0.725000000000001,0.730000000000001,0.735000000000001,0.740000000000001,
0.745000000000001,0.750000000000001,0.755000000000001,0.760000000000001,
0.765000000000001,0.770000000000001,0.775000000000001,0.780000000000001,
0.785000000000001,0.790000000000001,0.795000000000001,0.800000000000001,
0.805000000000001,0.810000000000001,0.815000000000001,0.820000000000001,
0.825000000000001,0.830000000000001,0.835000000000001,0.840000000000001,
0.845000000000001,0.850000000000001,0.855000000000001,0.860000000000001,
0.865000000000001,0.870000000000001,0.875000000000001,0.880000000000001,
0.885000000000001,0.890000000000001,0.895000000000001,0.900000000000001,
0.905000000000001,0.910000000000001,0.915000000000001,0.920000000000001,
0.925000000000001,0.930000000000001,0.935000000000001,0.940000000000001,
0.945000000000001,0.950000000000001,0.955000000000001,0.960000000000001,
0.965000000000001,0.970000000000001,0.975000000000001,0.980000000000001,
0.985000000000001,0.990000000000001,0.995000000000001,1.),(0.,1.2),
 .UNSPECIFIED.)
GEOMETRIC_REPRESENTATION_ITEM()
RATIONAL_B_SPLINE_SURFACE(((1.,1.),(1.,1.),(1.,1.),(1.,1.),(1.,1.),(1.,
1.),(1.,1.),(1.,1.),(1.,1.),(1.,1.),(1.,1.),(1.,1.),(1.,1.),(1.,1.),(1.,
1.),(1.,1.),(1.,1.),(1.,1.),(1.,1.),(1.,1.),(1.,1.),(1.,1.),(1.,1.),(1.,
1.),(1.,1.),(1.,1.),(1.,1.),(1.,1.),(1.,1.),(1.,1.),(1.,1.),(1.,1.),(1.,
1.),(1.,1.),(1.,1.),(1.,1.),(1.,1.),(1.,1.),(1.,1.),(1.,1.),(1.,1.),(1.,
1.),(1.,1.),(1.,1.),(1.,1.),(1.,1.),(1.,1.),(1.,1.),(1.,1.),(1.,1.),(1.,
1.),(1.,1.),(1.,1.),(1.,1.),(1.,1.),(1.,1.),(1.,1.),(1.,1.),(1.,1.),(1.,
1.),(1.,1.),(1.,1.),(1.,1.),(1.,1.),(1.,1.),(1.,1.),(1.,1.),(1.,1.),(1.,
1.),(1.,1.),(1.,1.),(1.,1.),(1.,1.),(1.,1.),(1.,1.),(1.,1.),(1.,1.),(1.,
1.),(1.,1.),(1.,1.),(1.,1.),(1.,1.),(1.,1.),(1.,1.),(1.,1.),(1.,1.),(1.,
1.),(1.,1.),(1.,1.),(1.,1.),(1.,1.),(1.,1.),(1.,1.),(1.,1.),(1.,1.),(1.,
1.),(1.,1.),(1.,1.),(1.,1.),(1.,1.),(1.,1.),(1.,1.),(1.,1.),(1.,1.),(1.,
1.),(1.,1.),(1.,1.),(1.,1.),(1.,1.),(1.,1.),(1.,1.),(1.,1.),(1.,1.),(1.,
1.),(1.,1.),(1.,1.),(1.,1.),(1.,1.),(1.,1.),(1.,1.),(1.,1.),(1.,1.),(1.,
1.),(1.,1.),(1.,1.),(1.,1.),(1.,1.),(1.,1.),(1.,1.),(1.,1.),(1.,1.),(1.,
1.),(1.,1.),(1.,1.),(1.,1.),(1.,1.),(1.,1.),(1.,1.),(1.,1.),(1.,1.),(1.,
1.),(1.,1.),(1.,1.),(1.,1.),(1.,1.),(1.,1.),(1.,1.),(1.,1.),(1.,1.),(1.,
1.),(1.,1.),(1.,1.),(1.,1.),(1.,1.),(1.,1.),(1.,1.),(1.,1.),(1.,1.),(1.,
1.),(1.,1.),(1.,1.),(1.,1.),(1.,1.),(1.,1.),(1.,1.),(1.,1.),(1.,1.),(1.,
1.),(1.,1.),(1.,1.),(1.,1.),(1.,1.),(1.,1.),(1.,1.),(1.,1.),(1.,1.),(1.,
1.),(1.,1.),(1.,1.),(1.,1.),(1.,1.),(1.,1.),(1.,1.),(1.,1.),(1.,1.),(1.,
1.),(1.,1.),(1.,1.),(1.,1.),(1.,1.),(1.,1.),(1.,1.),(1.,1.),(1.,1.),(1.,
1.),(1.,1.),(1.,1.),(1.,1.),(1.,1.),(1.,1.),(1.,1.),(1.,1.),(1.,1.),(1.,
1.),(1.,1.)))
REPRESENTATION_ITEM('')
SURFACE()
);
#911=(
BOUNDED_SURFACE()
B_SPLINE_SURFACE(5,1,((#77710,#77711),(#77712,#77713),(#77714,#77715),(#77716,
#77717),(#77718,#77719),(#77720,#77721),(#77722,#77723),(#77724,#77725),
(#77726,#77727),(#77728,#77729),(#77730,#77731),(#77732,#77733),(#77734,
#77735),(#77736,#77737),(#77738,#77739),(#77740,#77741),(#77742,#77743),
(#77744,#77745),(#77746,#77747),(#77748,#77749),(#77750,#77751),(#77752,
#77753),(#77754,#77755),(#77756,#77757),(#77758,#77759),(#77760,#77761),
(#77762,#77763),(#77764,#77765),(#77766,#77767),(#77768,#77769),(#77770,
#77771),(#77772,#77773),(#77774,#77775),(#77776,#77777),(#77778,#77779),
(#77780,#77781),(#77782,#77783),(#77784,#77785),(#77786,#77787),(#77788,
#77789),(#77790,#77791),(#77792,#77793),(#77794,#77795),(#77796,#77797),
(#77798,#77799),(#77800,#77801),(#77802,#77803),(#77804,#77805),(#77806,
#77807),(#77808,#77809),(#77810,#77811),(#77812,#77813),(#77814,#77815),
(#77816,#77817),(#77818,#77819),(#77820,#77821),(#77822,#77823),(#77824,
#77825),(#77826,#77827),(#77828,#77829),(#77830,#77831),(#77832,#77833),
(#77834,#77835),(#77836,#77837),(#77838,#77839),(#77840,#77841),(#77842,
#77843),(#77844,#77845),(#77846,#77847),(#77848,#77849),(#77850,#77851),
(#77852,#77853),(#77854,#77855),(#77856,#77857),(#77858,#77859),(#77860,
#77861),(#77862,#77863),(#77864,#77865),(#77866,#77867),(#77868,#77869),
(#77870,#77871),(#77872,#77873),(#77874,#77875),(#77876,#77877),(#77878,
#77879),(#77880,#77881),(#77882,#77883),(#77884,#77885),(#77886,#77887),
(#77888,#77889),(#77890,#77891),(#77892,#77893),(#77894,#77895),(#77896,
#77897),(#77898,#77899),(#77900,#77901),(#77902,#77903),(#77904,#77905),
(#77906,#77907),(#77908,#77909),(#77910,#77911),(#77912,#77913),(#77914,
#77915),(#77916,#77917),(#77918,#77919),(#77920,#77921),(#77922,#77923),
(#77924,#77925),(#77926,#77927),(#77928,#77929),(#77930,#77931),(#77932,
#77933),(#77934,#77935),(#77936,#77937),(#77938,#77939),(#77940,#77941),
(#77942,#77943),(#77944,#77945),(#77946,#77947),(#77948,#77949),(#77950,
#77951),(#77952,#77953),(#77954,#77955),(#77956,#77957),(#77958,#77959),
(#77960,#77961),(#77962,#77963),(#77964,#77965),(#77966,#77967),(#77968,
#77969),(#77970,#77971),(#77972,#77973),(#77974,#77975),(#77976,#77977),
(#77978,#77979),(#77980,#77981),(#77982,#77983),(#77984,#77985),(#77986,
#77987),(#77988,#77989),(#77990,#77991),(#77992,#77993),(#77994,#77995),
(#77996,#77997),(#77998,#77999),(#78000,#78001),(#78002,#78003),(#78004,
#78005),(#78006,#78007),(#78008,#78009),(#78010,#78011),(#78012,#78013),
(#78014,#78015),(#78016,#78017),(#78018,#78019),(#78020,#78021),(#78022,
#78023),(#78024,#78025),(#78026,#78027),(#78028,#78029),(#78030,#78031),
(#78032,#78033),(#78034,#78035),(#78036,#78037),(#78038,#78039),(#78040,
#78041),(#78042,#78043),(#78044,#78045),(#78046,#78047),(#78048,#78049),
(#78050,#78051),(#78052,#78053),(#78054,#78055),(#78056,#78057),(#78058,
#78059),(#78060,#78061),(#78062,#78063),(#78064,#78065),(#78066,#78067),
(#78068,#78069),(#78070,#78071),(#78072,#78073),(#78074,#78075),(#78076,
#78077),(#78078,#78079),(#78080,#78081),(#78082,#78083),(#78084,#78085),
(#78086,#78087),(#78088,#78089),(#78090,#78091),(#78092,#78093),(#78094,
#78095),(#78096,#78097),(#78098,#78099),(#78100,#78101),(#78102,#78103),
(#78104,#78105),(#78106,#78107),(#78108,#78109),(#78110,#78111),(#78112,
#78113),(#78114,#78115),(#78116,#78117),(#78118,#78119)),.UNSPECIFIED.,
 .F.,.F.,.F.)
B_SPLINE_SURFACE_WITH_KNOTS((6,1,1,1,1,1,1,1,1,1,1,1,1,1,1,1,1,1,1,1,1,
1,1,1,1,1,1,1,1,1,1,1,1,1,1,1,1,1,1,1,1,1,1,1,1,1,1,1,1,1,1,1,1,1,1,1,1,
1,1,1,1,1,1,1,1,1,1,1,1,1,1,1,1,1,1,1,1,1,1,1,1,1,1,1,1,1,1,1,1,1,1,1,1,
1,1,1,1,1,1,1,1,1,1,1,1,1,1,1,1,1,1,1,1,1,1,1,1,1,1,1,1,1,1,1,1,1,1,1,1,
1,1,1,1,1,1,1,1,1,1,1,1,1,1,1,1,1,1,1,1,1,1,1,1,1,1,1,1,1,1,1,1,1,1,1,1,
1,1,1,1,1,1,1,1,1,1,1,1,1,1,1,1,1,1,1,1,1,1,1,1,1,1,1,1,1,1,1,1,1,1,1,6),
(2,2),(0.,0.005,0.01,0.015,0.02,0.025,0.03,0.035,0.04,0.045,0.05,0.055,
0.06,0.065,0.07,0.075,0.08,0.085,0.09,0.095,0.1,0.105,0.11,0.115,0.12,0.125,
0.13,0.135,0.14,0.145,0.15,0.155,0.16,0.165,0.17,0.175,0.18,0.185,0.19,
0.195,0.2,0.205,0.21,0.215,0.22,0.225,0.23,0.235,0.24,0.245,0.25,0.255,
0.26,0.265,0.27,0.275,0.28,0.285,0.29,0.295,0.3,0.305,0.31,0.315,0.32,0.325,
0.33,0.335,0.34,0.345,0.35,0.355,0.36,0.365,0.37,0.375,0.38,0.385,0.39,
0.395,0.4,0.405,0.41,0.415,0.42,0.425,0.43,0.435,0.44,0.445,0.45,0.455,
0.46,0.465,0.47,0.475,0.48,0.485,0.49,0.495,0.5,0.505,0.51,0.515,0.52,0.525,
0.53,0.535,0.54,0.545,0.55,0.555,0.56,0.565,0.57,0.575,0.58,0.585,0.59,
0.595,0.6,0.605,0.61,0.615,0.62,0.625,0.63,0.635,0.64,0.645,0.65,0.655,
0.66,0.665,0.67,0.675,0.68,0.685,0.690000000000001,0.695000000000001,0.700000000000001,
0.705000000000001,0.710000000000001,0.715000000000001,0.720000000000001,
0.725000000000001,0.730000000000001,0.735000000000001,0.740000000000001,
0.745000000000001,0.750000000000001,0.755000000000001,0.760000000000001,
0.765000000000001,0.770000000000001,0.775000000000001,0.780000000000001,
0.785000000000001,0.790000000000001,0.795000000000001,0.800000000000001,
0.805000000000001,0.810000000000001,0.815000000000001,0.820000000000001,
0.825000000000001,0.830000000000001,0.835000000000001,0.840000000000001,
0.845000000000001,0.850000000000001,0.855000000000001,0.860000000000001,
0.865000000000001,0.870000000000001,0.875000000000001,0.880000000000001,
0.885000000000001,0.890000000000001,0.895000000000001,0.900000000000001,
0.905000000000001,0.910000000000001,0.915000000000001,0.920000000000001,
0.925000000000001,0.930000000000001,0.935000000000001,0.940000000000001,
0.945000000000001,0.950000000000001,0.955000000000001,0.960000000000001,
0.965000000000001,0.970000000000001,0.975000000000001,0.980000000000001,
0.985000000000001,0.990000000000001,0.995000000000001,1.),(0.,1.2),
 .UNSPECIFIED.)
GEOMETRIC_REPRESENTATION_ITEM()
RATIONAL_B_SPLINE_SURFACE(((1.,1.),(1.,1.),(1.,1.),(1.,1.),(1.,1.),(1.,
1.),(1.,1.),(1.,1.),(1.,1.),(1.,1.),(1.,1.),(1.,1.),(1.,1.),(1.,1.),(1.,
1.),(1.,1.),(1.,1.),(1.,1.),(1.,1.),(1.,1.),(1.,1.),(1.,1.),(1.,1.),(1.,
1.),(1.,1.),(1.,1.),(1.,1.),(1.,1.),(1.,1.),(1.,1.),(1.,1.),(1.,1.),(1.,
1.),(1.,1.),(1.,1.),(1.,1.),(1.,1.),(1.,1.),(1.,1.),(1.,1.),(1.,1.),(1.,
1.),(1.,1.),(1.,1.),(1.,1.),(1.,1.),(1.,1.),(1.,1.),(1.,1.),(1.,1.),(1.,
1.),(1.,1.),(1.,1.),(1.,1.),(1.,1.),(1.,1.),(1.,1.),(1.,1.),(1.,1.),(1.,
1.),(1.,1.),(1.,1.),(1.,1.),(1.,1.),(1.,1.),(1.,1.),(1.,1.),(1.,1.),(1.,
1.),(1.,1.),(1.,1.),(1.,1.),(1.,1.),(1.,1.),(1.,1.),(1.,1.),(1.,1.),(1.,
1.),(1.,1.),(1.,1.),(1.,1.),(1.,1.),(1.,1.),(1.,1.),(1.,1.),(1.,1.),(1.,
1.),(1.,1.),(1.,1.),(1.,1.),(1.,1.),(1.,1.),(1.,1.),(1.,1.),(1.,1.),(1.,
1.),(1.,1.),(1.,1.),(1.,1.),(1.,1.),(1.,1.),(1.,1.),(1.,1.),(1.,1.),(1.,
1.),(1.,1.),(1.,1.),(1.,1.),(1.,1.),(1.,1.),(1.,1.),(1.,1.),(1.,1.),(1.,
1.),(1.,1.),(1.,1.),(1.,1.),(1.,1.),(1.,1.),(1.,1.),(1.,1.),(1.,1.),(1.,
1.),(1.,1.),(1.,1.),(1.,1.),(1.,1.),(1.,1.),(1.,1.),(1.,1.),(1.,1.),(1.,
1.),(1.,1.),(1.,1.),(1.,1.),(1.,1.),(1.,1.),(1.,1.),(1.,1.),(1.,1.),(1.,
1.),(1.,1.),(1.,1.),(1.,1.),(1.,1.),(1.,1.),(1.,1.),(1.,1.),(1.,1.),(1.,
1.),(1.,1.),(1.,1.),(1.,1.),(1.,1.),(1.,1.),(1.,1.),(1.,1.),(1.,1.),(1.,
1.),(1.,1.),(1.,1.),(1.,1.),(1.,1.),(1.,1.),(1.,1.),(1.,1.),(1.,1.),(1.,
1.),(1.,1.),(1.,1.),(1.,1.),(1.,1.),(1.,1.),(1.,1.),(1.,1.),(1.,1.),(1.,
1.),(1.,1.),(1.,1.),(1.,1.),(1.,1.),(1.,1.),(1.,1.),(1.,1.),(1.,1.),(1.,
1.),(1.,1.),(1.,1.),(1.,1.),(1.,1.),(1.,1.),(1.,1.),(1.,1.),(1.,1.),(1.,
1.),(1.,1.),(1.,1.),(1.,1.),(1.,1.),(1.,1.),(1.,1.),(1.,1.),(1.,1.),(1.,
1.),(1.,1.)))
REPRESENTATION_ITEM('')
SURFACE()
);
#912=(
BOUNDED_SURFACE()
B_SPLINE_SURFACE(5,1,((#78606,#78607),(#78608,#78609),(#78610,#78611),(#78612,
#78613),(#78614,#78615),(#78616,#78617),(#78618,#78619),(#78620,#78621),
(#78622,#78623),(#78624,#78625),(#78626,#78627),(#78628,#78629),(#78630,
#78631),(#78632,#78633),(#78634,#78635),(#78636,#78637),(#78638,#78639),
(#78640,#78641),(#78642,#78643),(#78644,#78645),(#78646,#78647),(#78648,
#78649),(#78650,#78651),(#78652,#78653),(#78654,#78655),(#78656,#78657),
(#78658,#78659),(#78660,#78661),(#78662,#78663),(#78664,#78665),(#78666,
#78667),(#78668,#78669),(#78670,#78671),(#78672,#78673),(#78674,#78675),
(#78676,#78677),(#78678,#78679),(#78680,#78681),(#78682,#78683),(#78684,
#78685),(#78686,#78687),(#78688,#78689),(#78690,#78691),(#78692,#78693),
(#78694,#78695),(#78696,#78697),(#78698,#78699),(#78700,#78701),(#78702,
#78703),(#78704,#78705),(#78706,#78707),(#78708,#78709),(#78710,#78711),
(#78712,#78713),(#78714,#78715),(#78716,#78717),(#78718,#78719),(#78720,
#78721),(#78722,#78723),(#78724,#78725),(#78726,#78727),(#78728,#78729),
(#78730,#78731),(#78732,#78733),(#78734,#78735),(#78736,#78737),(#78738,
#78739),(#78740,#78741),(#78742,#78743),(#78744,#78745),(#78746,#78747),
(#78748,#78749),(#78750,#78751),(#78752,#78753),(#78754,#78755),(#78756,
#78757),(#78758,#78759),(#78760,#78761),(#78762,#78763),(#78764,#78765),
(#78766,#78767),(#78768,#78769),(#78770,#78771),(#78772,#78773),(#78774,
#78775),(#78776,#78777),(#78778,#78779),(#78780,#78781),(#78782,#78783),
(#78784,#78785),(#78786,#78787),(#78788,#78789),(#78790,#78791),(#78792,
#78793),(#78794,#78795),(#78796,#78797),(#78798,#78799),(#78800,#78801),
(#78802,#78803),(#78804,#78805),(#78806,#78807),(#78808,#78809),(#78810,
#78811),(#78812,#78813),(#78814,#78815),(#78816,#78817),(#78818,#78819),
(#78820,#78821),(#78822,#78823),(#78824,#78825),(#78826,#78827),(#78828,
#78829),(#78830,#78831),(#78832,#78833),(#78834,#78835),(#78836,#78837),
(#78838,#78839),(#78840,#78841),(#78842,#78843),(#78844,#78845),(#78846,
#78847),(#78848,#78849),(#78850,#78851),(#78852,#78853),(#78854,#78855),
(#78856,#78857),(#78858,#78859),(#78860,#78861),(#78862,#78863),(#78864,
#78865),(#78866,#78867),(#78868,#78869),(#78870,#78871),(#78872,#78873),
(#78874,#78875),(#78876,#78877),(#78878,#78879),(#78880,#78881),(#78882,
#78883),(#78884,#78885),(#78886,#78887),(#78888,#78889),(#78890,#78891),
(#78892,#78893),(#78894,#78895),(#78896,#78897),(#78898,#78899),(#78900,
#78901),(#78902,#78903),(#78904,#78905),(#78906,#78907),(#78908,#78909),
(#78910,#78911),(#78912,#78913),(#78914,#78915),(#78916,#78917),(#78918,
#78919),(#78920,#78921),(#78922,#78923),(#78924,#78925),(#78926,#78927),
(#78928,#78929),(#78930,#78931),(#78932,#78933),(#78934,#78935),(#78936,
#78937),(#78938,#78939),(#78940,#78941),(#78942,#78943),(#78944,#78945),
(#78946,#78947),(#78948,#78949),(#78950,#78951),(#78952,#78953),(#78954,
#78955),(#78956,#78957),(#78958,#78959),(#78960,#78961),(#78962,#78963),
(#78964,#78965),(#78966,#78967),(#78968,#78969),(#78970,#78971),(#78972,
#78973),(#78974,#78975),(#78976,#78977),(#78978,#78979),(#78980,#78981),
(#78982,#78983),(#78984,#78985),(#78986,#78987),(#78988,#78989),(#78990,
#78991),(#78992,#78993),(#78994,#78995),(#78996,#78997),(#78998,#78999),
(#79000,#79001),(#79002,#79003),(#79004,#79005),(#79006,#79007),(#79008,
#79009),(#79010,#79011),(#79012,#79013),(#79014,#79015)),.UNSPECIFIED.,
 .F.,.F.,.F.)
B_SPLINE_SURFACE_WITH_KNOTS((6,1,1,1,1,1,1,1,1,1,1,1,1,1,1,1,1,1,1,1,1,
1,1,1,1,1,1,1,1,1,1,1,1,1,1,1,1,1,1,1,1,1,1,1,1,1,1,1,1,1,1,1,1,1,1,1,1,
1,1,1,1,1,1,1,1,1,1,1,1,1,1,1,1,1,1,1,1,1,1,1,1,1,1,1,1,1,1,1,1,1,1,1,1,
1,1,1,1,1,1,1,1,1,1,1,1,1,1,1,1,1,1,1,1,1,1,1,1,1,1,1,1,1,1,1,1,1,1,1,1,
1,1,1,1,1,1,1,1,1,1,1,1,1,1,1,1,1,1,1,1,1,1,1,1,1,1,1,1,1,1,1,1,1,1,1,1,
1,1,1,1,1,1,1,1,1,1,1,1,1,1,1,1,1,1,1,1,1,1,1,1,1,1,1,1,1,1,1,1,1,1,1,6),
(2,2),(0.,0.005,0.01,0.015,0.02,0.025,0.03,0.035,0.04,0.045,0.05,0.055,
0.06,0.065,0.07,0.075,0.08,0.085,0.09,0.095,0.1,0.105,0.11,0.115,0.12,0.125,
0.13,0.135,0.14,0.145,0.15,0.155,0.16,0.165,0.17,0.175,0.18,0.185,0.19,
0.195,0.2,0.205,0.21,0.215,0.22,0.225,0.23,0.235,0.24,0.245,0.25,0.255,
0.26,0.265,0.27,0.275,0.28,0.285,0.29,0.295,0.3,0.305,0.31,0.315,0.32,0.325,
0.33,0.335,0.34,0.345,0.35,0.355,0.36,0.365,0.37,0.375,0.38,0.385,0.39,
0.395,0.4,0.405,0.41,0.415,0.42,0.425,0.43,0.435,0.44,0.445,0.45,0.455,
0.46,0.465,0.47,0.475,0.48,0.485,0.49,0.495,0.5,0.505,0.51,0.515,0.52,0.525,
0.53,0.535,0.54,0.545,0.55,0.555,0.56,0.565,0.57,0.575,0.58,0.585,0.59,
0.595,0.6,0.605,0.61,0.615,0.62,0.625,0.63,0.635,0.64,0.645,0.65,0.655,
0.66,0.665,0.67,0.675,0.68,0.685,0.690000000000001,0.695000000000001,0.700000000000001,
0.705000000000001,0.710000000000001,0.715000000000001,0.720000000000001,
0.725000000000001,0.730000000000001,0.735000000000001,0.740000000000001,
0.745000000000001,0.750000000000001,0.755000000000001,0.760000000000001,
0.765000000000001,0.770000000000001,0.775000000000001,0.780000000000001,
0.785000000000001,0.790000000000001,0.795000000000001,0.800000000000001,
0.805000000000001,0.810000000000001,0.815000000000001,0.820000000000001,
0.825000000000001,0.830000000000001,0.835000000000001,0.840000000000001,
0.845000000000001,0.850000000000001,0.855000000000001,0.860000000000001,
0.865000000000001,0.870000000000001,0.875000000000001,0.880000000000001,
0.885000000000001,0.890000000000001,0.895000000000001,0.900000000000001,
0.905000000000001,0.910000000000001,0.915000000000001,0.920000000000001,
0.925000000000001,0.930000000000001,0.935000000000001,0.940000000000001,
0.945000000000001,0.950000000000001,0.955000000000001,0.960000000000001,
0.965000000000001,0.970000000000001,0.975000000000001,0.980000000000001,
0.985000000000001,0.990000000000001,0.995000000000001,1.),(0.,1.2),
 .UNSPECIFIED.)
GEOMETRIC_REPRESENTATION_ITEM()
RATIONAL_B_SPLINE_SURFACE(((1.,1.),(1.,1.),(1.,1.),(1.,1.),(1.,1.),(1.,
1.),(1.,1.),(1.,1.),(1.,1.),(1.,1.),(1.,1.),(1.,1.),(1.,1.),(1.,1.),(1.,
1.),(1.,1.),(1.,1.),(1.,1.),(1.,1.),(1.,1.),(1.,1.),(1.,1.),(1.,1.),(1.,
1.),(1.,1.),(1.,1.),(1.,1.),(1.,1.),(1.,1.),(1.,1.),(1.,1.),(1.,1.),(1.,
1.),(1.,1.),(1.,1.),(1.,1.),(1.,1.),(1.,1.),(1.,1.),(1.,1.),(1.,1.),(1.,
1.),(1.,1.),(1.,1.),(1.,1.),(1.,1.),(1.,1.),(1.,1.),(1.,1.),(1.,1.),(1.,
1.),(1.,1.),(1.,1.),(1.,1.),(1.,1.),(1.,1.),(1.,1.),(1.,1.),(1.,1.),(1.,
1.),(1.,1.),(1.,1.),(1.,1.),(1.,1.),(1.,1.),(1.,1.),(1.,1.),(1.,1.),(1.,
1.),(1.,1.),(1.,1.),(1.,1.),(1.,1.),(1.,1.),(1.,1.),(1.,1.),(1.,1.),(1.,
1.),(1.,1.),(1.,1.),(1.,1.),(1.,1.),(1.,1.),(1.,1.),(1.,1.),(1.,1.),(1.,
1.),(1.,1.),(1.,1.),(1.,1.),(1.,1.),(1.,1.),(1.,1.),(1.,1.),(1.,1.),(1.,
1.),(1.,1.),(1.,1.),(1.,1.),(1.,1.),(1.,1.),(1.,1.),(1.,1.),(1.,1.),(1.,
1.),(1.,1.),(1.,1.),(1.,1.),(1.,1.),(1.,1.),(1.,1.),(1.,1.),(1.,1.),(1.,
1.),(1.,1.),(1.,1.),(1.,1.),(1.,1.),(1.,1.),(1.,1.),(1.,1.),(1.,1.),(1.,
1.),(1.,1.),(1.,1.),(1.,1.),(1.,1.),(1.,1.),(1.,1.),(1.,1.),(1.,1.),(1.,
1.),(1.,1.),(1.,1.),(1.,1.),(1.,1.),(1.,1.),(1.,1.),(1.,1.),(1.,1.),(1.,
1.),(1.,1.),(1.,1.),(1.,1.),(1.,1.),(1.,1.),(1.,1.),(1.,1.),(1.,1.),(1.,
1.),(1.,1.),(1.,1.),(1.,1.),(1.,1.),(1.,1.),(1.,1.),(1.,1.),(1.,1.),(1.,
1.),(1.,1.),(1.,1.),(1.,1.),(1.,1.),(1.,1.),(1.,1.),(1.,1.),(1.,1.),(1.,
1.),(1.,1.),(1.,1.),(1.,1.),(1.,1.),(1.,1.),(1.,1.),(1.,1.),(1.,1.),(1.,
1.),(1.,1.),(1.,1.),(1.,1.),(1.,1.),(1.,1.),(1.,1.),(1.,1.),(1.,1.),(1.,
1.),(1.,1.),(1.,1.),(1.,1.),(1.,1.),(1.,1.),(1.,1.),(1.,1.),(1.,1.),(1.,
1.),(1.,1.),(1.,1.),(1.,1.),(1.,1.),(1.,1.),(1.,1.),(1.,1.),(1.,1.),(1.,
1.),(1.,1.)))
REPRESENTATION_ITEM('')
SURFACE()
);
#913=(
BOUNDED_SURFACE()
B_SPLINE_SURFACE(5,1,((#79502,#79503),(#79504,#79505),(#79506,#79507),(#79508,
#79509),(#79510,#79511),(#79512,#79513),(#79514,#79515),(#79516,#79517),
(#79518,#79519),(#79520,#79521),(#79522,#79523),(#79524,#79525),(#79526,
#79527),(#79528,#79529),(#79530,#79531),(#79532,#79533),(#79534,#79535),
(#79536,#79537),(#79538,#79539),(#79540,#79541),(#79542,#79543),(#79544,
#79545),(#79546,#79547),(#79548,#79549),(#79550,#79551),(#79552,#79553),
(#79554,#79555),(#79556,#79557),(#79558,#79559),(#79560,#79561),(#79562,
#79563),(#79564,#79565),(#79566,#79567),(#79568,#79569),(#79570,#79571),
(#79572,#79573),(#79574,#79575),(#79576,#79577),(#79578,#79579),(#79580,
#79581),(#79582,#79583),(#79584,#79585),(#79586,#79587),(#79588,#79589),
(#79590,#79591),(#79592,#79593),(#79594,#79595),(#79596,#79597),(#79598,
#79599),(#79600,#79601),(#79602,#79603),(#79604,#79605),(#79606,#79607),
(#79608,#79609),(#79610,#79611),(#79612,#79613),(#79614,#79615),(#79616,
#79617),(#79618,#79619),(#79620,#79621),(#79622,#79623),(#79624,#79625),
(#79626,#79627),(#79628,#79629),(#79630,#79631),(#79632,#79633),(#79634,
#79635),(#79636,#79637),(#79638,#79639),(#79640,#79641),(#79642,#79643),
(#79644,#79645),(#79646,#79647),(#79648,#79649),(#79650,#79651),(#79652,
#79653),(#79654,#79655),(#79656,#79657),(#79658,#79659),(#79660,#79661),
(#79662,#79663),(#79664,#79665),(#79666,#79667),(#79668,#79669),(#79670,
#79671),(#79672,#79673),(#79674,#79675),(#79676,#79677),(#79678,#79679),
(#79680,#79681),(#79682,#79683),(#79684,#79685),(#79686,#79687),(#79688,
#79689),(#79690,#79691),(#79692,#79693),(#79694,#79695),(#79696,#79697),
(#79698,#79699),(#79700,#79701),(#79702,#79703),(#79704,#79705),(#79706,
#79707),(#79708,#79709),(#79710,#79711),(#79712,#79713),(#79714,#79715),
(#79716,#79717),(#79718,#79719),(#79720,#79721),(#79722,#79723),(#79724,
#79725),(#79726,#79727),(#79728,#79729),(#79730,#79731),(#79732,#79733),
(#79734,#79735),(#79736,#79737),(#79738,#79739),(#79740,#79741),(#79742,
#79743),(#79744,#79745),(#79746,#79747),(#79748,#79749),(#79750,#79751),
(#79752,#79753),(#79754,#79755),(#79756,#79757),(#79758,#79759),(#79760,
#79761),(#79762,#79763),(#79764,#79765),(#79766,#79767),(#79768,#79769),
(#79770,#79771),(#79772,#79773),(#79774,#79775),(#79776,#79777),(#79778,
#79779),(#79780,#79781),(#79782,#79783),(#79784,#79785),(#79786,#79787),
(#79788,#79789),(#79790,#79791),(#79792,#79793),(#79794,#79795),(#79796,
#79797),(#79798,#79799),(#79800,#79801),(#79802,#79803),(#79804,#79805),
(#79806,#79807),(#79808,#79809),(#79810,#79811),(#79812,#79813),(#79814,
#79815),(#79816,#79817),(#79818,#79819),(#79820,#79821),(#79822,#79823),
(#79824,#79825),(#79826,#79827),(#79828,#79829),(#79830,#79831),(#79832,
#79833),(#79834,#79835),(#79836,#79837),(#79838,#79839),(#79840,#79841),
(#79842,#79843),(#79844,#79845),(#79846,#79847),(#79848,#79849),(#79850,
#79851),(#79852,#79853),(#79854,#79855),(#79856,#79857),(#79858,#79859),
(#79860,#79861),(#79862,#79863),(#79864,#79865),(#79866,#79867),(#79868,
#79869),(#79870,#79871),(#79872,#79873),(#79874,#79875),(#79876,#79877),
(#79878,#79879),(#79880,#79881),(#79882,#79883),(#79884,#79885),(#79886,
#79887),(#79888,#79889),(#79890,#79891),(#79892,#79893),(#79894,#79895),
(#79896,#79897),(#79898,#79899),(#79900,#79901),(#79902,#79903),(#79904,
#79905),(#79906,#79907),(#79908,#79909),(#79910,#79911)),.UNSPECIFIED.,
 .F.,.F.,.F.)
B_SPLINE_SURFACE_WITH_KNOTS((6,1,1,1,1,1,1,1,1,1,1,1,1,1,1,1,1,1,1,1,1,
1,1,1,1,1,1,1,1,1,1,1,1,1,1,1,1,1,1,1,1,1,1,1,1,1,1,1,1,1,1,1,1,1,1,1,1,
1,1,1,1,1,1,1,1,1,1,1,1,1,1,1,1,1,1,1,1,1,1,1,1,1,1,1,1,1,1,1,1,1,1,1,1,
1,1,1,1,1,1,1,1,1,1,1,1,1,1,1,1,1,1,1,1,1,1,1,1,1,1,1,1,1,1,1,1,1,1,1,1,
1,1,1,1,1,1,1,1,1,1,1,1,1,1,1,1,1,1,1,1,1,1,1,1,1,1,1,1,1,1,1,1,1,1,1,1,
1,1,1,1,1,1,1,1,1,1,1,1,1,1,1,1,1,1,1,1,1,1,1,1,1,1,1,1,1,1,1,1,1,1,1,6),
(2,2),(0.,0.005,0.01,0.015,0.02,0.025,0.03,0.035,0.04,0.045,0.05,0.055,
0.06,0.065,0.07,0.075,0.08,0.085,0.09,0.095,0.1,0.105,0.11,0.115,0.12,0.125,
0.13,0.135,0.14,0.145,0.15,0.155,0.16,0.165,0.17,0.175,0.18,0.185,0.19,
0.195,0.2,0.205,0.21,0.215,0.22,0.225,0.23,0.235,0.24,0.245,0.25,0.255,
0.26,0.265,0.27,0.275,0.28,0.285,0.29,0.295,0.3,0.305,0.31,0.315,0.32,0.325,
0.33,0.335,0.34,0.345,0.35,0.355,0.36,0.365,0.37,0.375,0.38,0.385,0.39,
0.395,0.4,0.405,0.41,0.415,0.42,0.425,0.43,0.435,0.44,0.445,0.45,0.455,
0.46,0.465,0.47,0.475,0.48,0.485,0.49,0.495,0.5,0.505,0.51,0.515,0.52,0.525,
0.53,0.535,0.54,0.545,0.55,0.555,0.56,0.565,0.57,0.575,0.58,0.585,0.59,
0.595,0.6,0.605,0.61,0.615,0.62,0.625,0.63,0.635,0.64,0.645,0.65,0.655,
0.66,0.665,0.67,0.675,0.68,0.685,0.690000000000001,0.695000000000001,0.700000000000001,
0.705000000000001,0.710000000000001,0.715000000000001,0.720000000000001,
0.725000000000001,0.730000000000001,0.735000000000001,0.740000000000001,
0.745000000000001,0.750000000000001,0.755000000000001,0.760000000000001,
0.765000000000001,0.770000000000001,0.775000000000001,0.780000000000001,
0.785000000000001,0.790000000000001,0.795000000000001,0.800000000000001,
0.805000000000001,0.810000000000001,0.815000000000001,0.820000000000001,
0.825000000000001,0.830000000000001,0.835000000000001,0.840000000000001,
0.845000000000001,0.850000000000001,0.855000000000001,0.860000000000001,
0.865000000000001,0.870000000000001,0.875000000000001,0.880000000000001,
0.885000000000001,0.890000000000001,0.895000000000001,0.900000000000001,
0.905000000000001,0.910000000000001,0.915000000000001,0.920000000000001,
0.925000000000001,0.930000000000001,0.935000000000001,0.940000000000001,
0.945000000000001,0.950000000000001,0.955000000000001,0.960000000000001,
0.965000000000001,0.970000000000001,0.975000000000001,0.980000000000001,
0.985000000000001,0.990000000000001,0.995000000000001,1.),(0.,1.2),
 .UNSPECIFIED.)
GEOMETRIC_REPRESENTATION_ITEM()
RATIONAL_B_SPLINE_SURFACE(((1.,1.),(1.,1.),(1.,1.),(1.,1.),(1.,1.),(1.,
1.),(1.,1.),(1.,1.),(1.,1.),(1.,1.),(1.,1.),(1.,1.),(1.,1.),(1.,1.),(1.,
1.),(1.,1.),(1.,1.),(1.,1.),(1.,1.),(1.,1.),(1.,1.),(1.,1.),(1.,1.),(1.,
1.),(1.,1.),(1.,1.),(1.,1.),(1.,1.),(1.,1.),(1.,1.),(1.,1.),(1.,1.),(1.,
1.),(1.,1.),(1.,1.),(1.,1.),(1.,1.),(1.,1.),(1.,1.),(1.,1.),(1.,1.),(1.,
1.),(1.,1.),(1.,1.),(1.,1.),(1.,1.),(1.,1.),(1.,1.),(1.,1.),(1.,1.),(1.,
1.),(1.,1.),(1.,1.),(1.,1.),(1.,1.),(1.,1.),(1.,1.),(1.,1.),(1.,1.),(1.,
1.),(1.,1.),(1.,1.),(1.,1.),(1.,1.),(1.,1.),(1.,1.),(1.,1.),(1.,1.),(1.,
1.),(1.,1.),(1.,1.),(1.,1.),(1.,1.),(1.,1.),(1.,1.),(1.,1.),(1.,1.),(1.,
1.),(1.,1.),(1.,1.),(1.,1.),(1.,1.),(1.,1.),(1.,1.),(1.,1.),(1.,1.),(1.,
1.),(1.,1.),(1.,1.),(1.,1.),(1.,1.),(1.,1.),(1.,1.),(1.,1.),(1.,1.),(1.,
1.),(1.,1.),(1.,1.),(1.,1.),(1.,1.),(1.,1.),(1.,1.),(1.,1.),(1.,1.),(1.,
1.),(1.,1.),(1.,1.),(1.,1.),(1.,1.),(1.,1.),(1.,1.),(1.,1.),(1.,1.),(1.,
1.),(1.,1.),(1.,1.),(1.,1.),(1.,1.),(1.,1.),(1.,1.),(1.,1.),(1.,1.),(1.,
1.),(1.,1.),(1.,1.),(1.,1.),(1.,1.),(1.,1.),(1.,1.),(1.,1.),(1.,1.),(1.,
1.),(1.,1.),(1.,1.),(1.,1.),(1.,1.),(1.,1.),(1.,1.),(1.,1.),(1.,1.),(1.,
1.),(1.,1.),(1.,1.),(1.,1.),(1.,1.),(1.,1.),(1.,1.),(1.,1.),(1.,1.),(1.,
1.),(1.,1.),(1.,1.),(1.,1.),(1.,1.),(1.,1.),(1.,1.),(1.,1.),(1.,1.),(1.,
1.),(1.,1.),(1.,1.),(1.,1.),(1.,1.),(1.,1.),(1.,1.),(1.,1.),(1.,1.),(1.,
1.),(1.,1.),(1.,1.),(1.,1.),(1.,1.),(1.,1.),(1.,1.),(1.,1.),(1.,1.),(1.,
1.),(1.,1.),(1.,1.),(1.,1.),(1.,1.),(1.,1.),(1.,1.),(1.,1.),(1.,1.),(1.,
1.),(1.,1.),(1.,1.),(1.,1.),(1.,1.),(1.,1.),(1.,1.),(1.,1.),(1.,1.),(1.,
1.),(1.,1.),(1.,1.),(1.,1.),(1.,1.),(1.,1.),(1.,1.),(1.,1.),(1.,1.),(1.,
1.),(1.,1.)))
REPRESENTATION_ITEM('')
SURFACE()
);
#914=(
BOUNDED_SURFACE()
B_SPLINE_SURFACE(5,1,((#80398,#80399),(#80400,#80401),(#80402,#80403),(#80404,
#80405),(#80406,#80407),(#80408,#80409),(#80410,#80411),(#80412,#80413),
(#80414,#80415),(#80416,#80417),(#80418,#80419),(#80420,#80421),(#80422,
#80423),(#80424,#80425),(#80426,#80427),(#80428,#80429),(#80430,#80431),
(#80432,#80433),(#80434,#80435),(#80436,#80437),(#80438,#80439),(#80440,
#80441),(#80442,#80443),(#80444,#80445),(#80446,#80447),(#80448,#80449),
(#80450,#80451),(#80452,#80453),(#80454,#80455),(#80456,#80457),(#80458,
#80459),(#80460,#80461),(#80462,#80463),(#80464,#80465),(#80466,#80467),
(#80468,#80469),(#80470,#80471),(#80472,#80473),(#80474,#80475),(#80476,
#80477),(#80478,#80479),(#80480,#80481),(#80482,#80483),(#80484,#80485),
(#80486,#80487),(#80488,#80489),(#80490,#80491),(#80492,#80493),(#80494,
#80495),(#80496,#80497),(#80498,#80499),(#80500,#80501),(#80502,#80503),
(#80504,#80505),(#80506,#80507),(#80508,#80509),(#80510,#80511),(#80512,
#80513),(#80514,#80515),(#80516,#80517),(#80518,#80519),(#80520,#80521),
(#80522,#80523),(#80524,#80525),(#80526,#80527),(#80528,#80529),(#80530,
#80531),(#80532,#80533),(#80534,#80535),(#80536,#80537),(#80538,#80539),
(#80540,#80541),(#80542,#80543),(#80544,#80545),(#80546,#80547),(#80548,
#80549),(#80550,#80551),(#80552,#80553),(#80554,#80555),(#80556,#80557),
(#80558,#80559),(#80560,#80561),(#80562,#80563),(#80564,#80565),(#80566,
#80567),(#80568,#80569),(#80570,#80571),(#80572,#80573),(#80574,#80575),
(#80576,#80577),(#80578,#80579),(#80580,#80581),(#80582,#80583),(#80584,
#80585),(#80586,#80587),(#80588,#80589),(#80590,#80591),(#80592,#80593),
(#80594,#80595),(#80596,#80597),(#80598,#80599),(#80600,#80601),(#80602,
#80603),(#80604,#80605),(#80606,#80607),(#80608,#80609),(#80610,#80611),
(#80612,#80613),(#80614,#80615),(#80616,#80617),(#80618,#80619),(#80620,
#80621),(#80622,#80623),(#80624,#80625),(#80626,#80627),(#80628,#80629),
(#80630,#80631),(#80632,#80633),(#80634,#80635),(#80636,#80637),(#80638,
#80639),(#80640,#80641),(#80642,#80643),(#80644,#80645),(#80646,#80647),
(#80648,#80649),(#80650,#80651),(#80652,#80653),(#80654,#80655),(#80656,
#80657),(#80658,#80659),(#80660,#80661),(#80662,#80663),(#80664,#80665),
(#80666,#80667),(#80668,#80669),(#80670,#80671),(#80672,#80673),(#80674,
#80675),(#80676,#80677),(#80678,#80679),(#80680,#80681),(#80682,#80683),
(#80684,#80685),(#80686,#80687),(#80688,#80689),(#80690,#80691),(#80692,
#80693),(#80694,#80695),(#80696,#80697),(#80698,#80699),(#80700,#80701),
(#80702,#80703),(#80704,#80705),(#80706,#80707),(#80708,#80709),(#80710,
#80711),(#80712,#80713),(#80714,#80715),(#80716,#80717),(#80718,#80719),
(#80720,#80721),(#80722,#80723),(#80724,#80725),(#80726,#80727),(#80728,
#80729),(#80730,#80731),(#80732,#80733),(#80734,#80735),(#80736,#80737),
(#80738,#80739),(#80740,#80741),(#80742,#80743),(#80744,#80745),(#80746,
#80747),(#80748,#80749),(#80750,#80751),(#80752,#80753),(#80754,#80755),
(#80756,#80757),(#80758,#80759),(#80760,#80761),(#80762,#80763),(#80764,
#80765),(#80766,#80767),(#80768,#80769),(#80770,#80771),(#80772,#80773),
(#80774,#80775),(#80776,#80777),(#80778,#80779),(#80780,#80781),(#80782,
#80783),(#80784,#80785),(#80786,#80787),(#80788,#80789),(#80790,#80791),
(#80792,#80793),(#80794,#80795),(#80796,#80797),(#80798,#80799),(#80800,
#80801),(#80802,#80803),(#80804,#80805),(#80806,#80807)),.UNSPECIFIED.,
 .F.,.F.,.F.)
B_SPLINE_SURFACE_WITH_KNOTS((6,1,1,1,1,1,1,1,1,1,1,1,1,1,1,1,1,1,1,1,1,
1,1,1,1,1,1,1,1,1,1,1,1,1,1,1,1,1,1,1,1,1,1,1,1,1,1,1,1,1,1,1,1,1,1,1,1,
1,1,1,1,1,1,1,1,1,1,1,1,1,1,1,1,1,1,1,1,1,1,1,1,1,1,1,1,1,1,1,1,1,1,1,1,
1,1,1,1,1,1,1,1,1,1,1,1,1,1,1,1,1,1,1,1,1,1,1,1,1,1,1,1,1,1,1,1,1,1,1,1,
1,1,1,1,1,1,1,1,1,1,1,1,1,1,1,1,1,1,1,1,1,1,1,1,1,1,1,1,1,1,1,1,1,1,1,1,
1,1,1,1,1,1,1,1,1,1,1,1,1,1,1,1,1,1,1,1,1,1,1,1,1,1,1,1,1,1,1,1,1,1,1,6),
(2,2),(0.,0.005,0.01,0.015,0.02,0.025,0.03,0.035,0.04,0.045,0.05,0.055,
0.06,0.065,0.07,0.075,0.08,0.085,0.09,0.095,0.1,0.105,0.11,0.115,0.12,0.125,
0.13,0.135,0.14,0.145,0.15,0.155,0.16,0.165,0.17,0.175,0.18,0.185,0.19,
0.195,0.2,0.205,0.21,0.215,0.22,0.225,0.23,0.235,0.24,0.245,0.25,0.255,
0.26,0.265,0.27,0.275,0.28,0.285,0.29,0.295,0.3,0.305,0.31,0.315,0.32,0.325,
0.33,0.335,0.34,0.345,0.35,0.355,0.36,0.365,0.37,0.375,0.38,0.385,0.39,
0.395,0.4,0.405,0.41,0.415,0.42,0.425,0.43,0.435,0.44,0.445,0.45,0.455,
0.46,0.465,0.47,0.475,0.48,0.485,0.49,0.495,0.5,0.505,0.51,0.515,0.52,0.525,
0.53,0.535,0.54,0.545,0.55,0.555,0.56,0.565,0.57,0.575,0.58,0.585,0.59,
0.595,0.6,0.605,0.61,0.615,0.62,0.625,0.63,0.635,0.64,0.645,0.65,0.655,
0.66,0.665,0.67,0.675,0.68,0.685,0.690000000000001,0.695000000000001,0.700000000000001,
0.705000000000001,0.710000000000001,0.715000000000001,0.720000000000001,
0.725000000000001,0.730000000000001,0.735000000000001,0.740000000000001,
0.745000000000001,0.750000000000001,0.755000000000001,0.760000000000001,
0.765000000000001,0.770000000000001,0.775000000000001,0.780000000000001,
0.785000000000001,0.790000000000001,0.795000000000001,0.800000000000001,
0.805000000000001,0.810000000000001,0.815000000000001,0.820000000000001,
0.825000000000001,0.830000000000001,0.835000000000001,0.840000000000001,
0.845000000000001,0.850000000000001,0.855000000000001,0.860000000000001,
0.865000000000001,0.870000000000001,0.875000000000001,0.880000000000001,
0.885000000000001,0.890000000000001,0.895000000000001,0.900000000000001,
0.905000000000001,0.910000000000001,0.915000000000001,0.920000000000001,
0.925000000000001,0.930000000000001,0.935000000000001,0.940000000000001,
0.945000000000001,0.950000000000001,0.955000000000001,0.960000000000001,
0.965000000000001,0.970000000000001,0.975000000000001,0.980000000000001,
0.985000000000001,0.990000000000001,0.995000000000001,1.),(0.,1.2),
 .UNSPECIFIED.)
GEOMETRIC_REPRESENTATION_ITEM()
RATIONAL_B_SPLINE_SURFACE(((1.,1.),(1.,1.),(1.,1.),(1.,1.),(1.,1.),(1.,
1.),(1.,1.),(1.,1.),(1.,1.),(1.,1.),(1.,1.),(1.,1.),(1.,1.),(1.,1.),(1.,
1.),(1.,1.),(1.,1.),(1.,1.),(1.,1.),(1.,1.),(1.,1.),(1.,1.),(1.,1.),(1.,
1.),(1.,1.),(1.,1.),(1.,1.),(1.,1.),(1.,1.),(1.,1.),(1.,1.),(1.,1.),(1.,
1.),(1.,1.),(1.,1.),(1.,1.),(1.,1.),(1.,1.),(1.,1.),(1.,1.),(1.,1.),(1.,
1.),(1.,1.),(1.,1.),(1.,1.),(1.,1.),(1.,1.),(1.,1.),(1.,1.),(1.,1.),(1.,
1.),(1.,1.),(1.,1.),(1.,1.),(1.,1.),(1.,1.),(1.,1.),(1.,1.),(1.,1.),(1.,
1.),(1.,1.),(1.,1.),(1.,1.),(1.,1.),(1.,1.),(1.,1.),(1.,1.),(1.,1.),(1.,
1.),(1.,1.),(1.,1.),(1.,1.),(1.,1.),(1.,1.),(1.,1.),(1.,1.),(1.,1.),(1.,
1.),(1.,1.),(1.,1.),(1.,1.),(1.,1.),(1.,1.),(1.,1.),(1.,1.),(1.,1.),(1.,
1.),(1.,1.),(1.,1.),(1.,1.),(1.,1.),(1.,1.),(1.,1.),(1.,1.),(1.,1.),(1.,
1.),(1.,1.),(1.,1.),(1.,1.),(1.,1.),(1.,1.),(1.,1.),(1.,1.),(1.,1.),(1.,
1.),(1.,1.),(1.,1.),(1.,1.),(1.,1.),(1.,1.),(1.,1.),(1.,1.),(1.,1.),(1.,
1.),(1.,1.),(1.,1.),(1.,1.),(1.,1.),(1.,1.),(1.,1.),(1.,1.),(1.,1.),(1.,
1.),(1.,1.),(1.,1.),(1.,1.),(1.,1.),(1.,1.),(1.,1.),(1.,1.),(1.,1.),(1.,
1.),(1.,1.),(1.,1.),(1.,1.),(1.,1.),(1.,1.),(1.,1.),(1.,1.),(1.,1.),(1.,
1.),(1.,1.),(1.,1.),(1.,1.),(1.,1.),(1.,1.),(1.,1.),(1.,1.),(1.,1.),(1.,
1.),(1.,1.),(1.,1.),(1.,1.),(1.,1.),(1.,1.),(1.,1.),(1.,1.),(1.,1.),(1.,
1.),(1.,1.),(1.,1.),(1.,1.),(1.,1.),(1.,1.),(1.,1.),(1.,1.),(1.,1.),(1.,
1.),(1.,1.),(1.,1.),(1.,1.),(1.,1.),(1.,1.),(1.,1.),(1.,1.),(1.,1.),(1.,
1.),(1.,1.),(1.,1.),(1.,1.),(1.,1.),(1.,1.),(1.,1.),(1.,1.),(1.,1.),(1.,
1.),(1.,1.),(1.,1.),(1.,1.),(1.,1.),(1.,1.),(1.,1.),(1.,1.),(1.,1.),(1.,
1.),(1.,1.),(1.,1.),(1.,1.),(1.,1.),(1.,1.),(1.,1.),(1.,1.),(1.,1.),(1.,
1.),(1.,1.)))
REPRESENTATION_ITEM('')
SURFACE()
);
#915=(
BOUNDED_SURFACE()
B_SPLINE_SURFACE(5,1,((#81294,#81295),(#81296,#81297),(#81298,#81299),(#81300,
#81301),(#81302,#81303),(#81304,#81305),(#81306,#81307),(#81308,#81309),
(#81310,#81311),(#81312,#81313),(#81314,#81315),(#81316,#81317),(#81318,
#81319),(#81320,#81321),(#81322,#81323),(#81324,#81325),(#81326,#81327),
(#81328,#81329),(#81330,#81331),(#81332,#81333),(#81334,#81335),(#81336,
#81337),(#81338,#81339),(#81340,#81341),(#81342,#81343),(#81344,#81345),
(#81346,#81347),(#81348,#81349),(#81350,#81351),(#81352,#81353),(#81354,
#81355),(#81356,#81357),(#81358,#81359),(#81360,#81361),(#81362,#81363),
(#81364,#81365),(#81366,#81367),(#81368,#81369),(#81370,#81371),(#81372,
#81373),(#81374,#81375),(#81376,#81377),(#81378,#81379),(#81380,#81381),
(#81382,#81383),(#81384,#81385),(#81386,#81387),(#81388,#81389),(#81390,
#81391),(#81392,#81393),(#81394,#81395),(#81396,#81397),(#81398,#81399),
(#81400,#81401),(#81402,#81403),(#81404,#81405),(#81406,#81407),(#81408,
#81409),(#81410,#81411),(#81412,#81413),(#81414,#81415),(#81416,#81417),
(#81418,#81419),(#81420,#81421),(#81422,#81423),(#81424,#81425),(#81426,
#81427),(#81428,#81429),(#81430,#81431),(#81432,#81433),(#81434,#81435),
(#81436,#81437),(#81438,#81439),(#81440,#81441),(#81442,#81443),(#81444,
#81445),(#81446,#81447),(#81448,#81449),(#81450,#81451),(#81452,#81453),
(#81454,#81455),(#81456,#81457),(#81458,#81459),(#81460,#81461),(#81462,
#81463),(#81464,#81465),(#81466,#81467),(#81468,#81469),(#81470,#81471),
(#81472,#81473),(#81474,#81475),(#81476,#81477),(#81478,#81479),(#81480,
#81481),(#81482,#81483),(#81484,#81485),(#81486,#81487),(#81488,#81489),
(#81490,#81491),(#81492,#81493),(#81494,#81495),(#81496,#81497),(#81498,
#81499),(#81500,#81501),(#81502,#81503),(#81504,#81505),(#81506,#81507),
(#81508,#81509),(#81510,#81511),(#81512,#81513),(#81514,#81515),(#81516,
#81517),(#81518,#81519),(#81520,#81521),(#81522,#81523),(#81524,#81525),
(#81526,#81527),(#81528,#81529),(#81530,#81531),(#81532,#81533),(#81534,
#81535),(#81536,#81537),(#81538,#81539),(#81540,#81541),(#81542,#81543),
(#81544,#81545),(#81546,#81547),(#81548,#81549),(#81550,#81551),(#81552,
#81553),(#81554,#81555),(#81556,#81557),(#81558,#81559),(#81560,#81561),
(#81562,#81563),(#81564,#81565),(#81566,#81567),(#81568,#81569),(#81570,
#81571),(#81572,#81573),(#81574,#81575),(#81576,#81577),(#81578,#81579),
(#81580,#81581),(#81582,#81583),(#81584,#81585),(#81586,#81587),(#81588,
#81589),(#81590,#81591),(#81592,#81593),(#81594,#81595),(#81596,#81597),
(#81598,#81599),(#81600,#81601),(#81602,#81603),(#81604,#81605),(#81606,
#81607),(#81608,#81609),(#81610,#81611),(#81612,#81613),(#81614,#81615),
(#81616,#81617),(#81618,#81619),(#81620,#81621),(#81622,#81623),(#81624,
#81625),(#81626,#81627),(#81628,#81629),(#81630,#81631),(#81632,#81633),
(#81634,#81635),(#81636,#81637),(#81638,#81639),(#81640,#81641),(#81642,
#81643),(#81644,#81645),(#81646,#81647),(#81648,#81649),(#81650,#81651),
(#81652,#81653),(#81654,#81655),(#81656,#81657),(#81658,#81659),(#81660,
#81661),(#81662,#81663),(#81664,#81665),(#81666,#81667),(#81668,#81669),
(#81670,#81671),(#81672,#81673),(#81674,#81675),(#81676,#81677),(#81678,
#81679),(#81680,#81681),(#81682,#81683),(#81684,#81685),(#81686,#81687),
(#81688,#81689),(#81690,#81691),(#81692,#81693),(#81694,#81695),(#81696,
#81697),(#81698,#81699),(#81700,#81701),(#81702,#81703)),.UNSPECIFIED.,
 .F.,.F.,.F.)
B_SPLINE_SURFACE_WITH_KNOTS((6,1,1,1,1,1,1,1,1,1,1,1,1,1,1,1,1,1,1,1,1,
1,1,1,1,1,1,1,1,1,1,1,1,1,1,1,1,1,1,1,1,1,1,1,1,1,1,1,1,1,1,1,1,1,1,1,1,
1,1,1,1,1,1,1,1,1,1,1,1,1,1,1,1,1,1,1,1,1,1,1,1,1,1,1,1,1,1,1,1,1,1,1,1,
1,1,1,1,1,1,1,1,1,1,1,1,1,1,1,1,1,1,1,1,1,1,1,1,1,1,1,1,1,1,1,1,1,1,1,1,
1,1,1,1,1,1,1,1,1,1,1,1,1,1,1,1,1,1,1,1,1,1,1,1,1,1,1,1,1,1,1,1,1,1,1,1,
1,1,1,1,1,1,1,1,1,1,1,1,1,1,1,1,1,1,1,1,1,1,1,1,1,1,1,1,1,1,1,1,1,1,1,6),
(2,2),(0.,0.005,0.01,0.015,0.02,0.025,0.03,0.035,0.04,0.045,0.05,0.055,
0.06,0.065,0.07,0.075,0.08,0.085,0.09,0.095,0.1,0.105,0.11,0.115,0.12,0.125,
0.13,0.135,0.14,0.145,0.15,0.155,0.16,0.165,0.17,0.175,0.18,0.185,0.19,
0.195,0.2,0.205,0.21,0.215,0.22,0.225,0.23,0.235,0.24,0.245,0.25,0.255,
0.26,0.265,0.27,0.275,0.28,0.285,0.29,0.295,0.3,0.305,0.31,0.315,0.32,0.325,
0.33,0.335,0.34,0.345,0.35,0.355,0.36,0.365,0.37,0.375,0.38,0.385,0.39,
0.395,0.4,0.405,0.41,0.415,0.42,0.425,0.43,0.435,0.44,0.445,0.45,0.455,
0.46,0.465,0.47,0.475,0.48,0.485,0.49,0.495,0.5,0.505,0.51,0.515,0.52,0.525,
0.53,0.535,0.54,0.545,0.55,0.555,0.56,0.565,0.57,0.575,0.58,0.585,0.59,
0.595,0.6,0.605,0.61,0.615,0.62,0.625,0.63,0.635,0.64,0.645,0.65,0.655,
0.66,0.665,0.67,0.675,0.68,0.685,0.690000000000001,0.695000000000001,0.700000000000001,
0.705000000000001,0.710000000000001,0.715000000000001,0.720000000000001,
0.725000000000001,0.730000000000001,0.735000000000001,0.740000000000001,
0.745000000000001,0.750000000000001,0.755000000000001,0.760000000000001,
0.765000000000001,0.770000000000001,0.775000000000001,0.780000000000001,
0.785000000000001,0.790000000000001,0.795000000000001,0.800000000000001,
0.805000000000001,0.810000000000001,0.815000000000001,0.820000000000001,
0.825000000000001,0.830000000000001,0.835000000000001,0.840000000000001,
0.845000000000001,0.850000000000001,0.855000000000001,0.860000000000001,
0.865000000000001,0.870000000000001,0.875000000000001,0.880000000000001,
0.885000000000001,0.890000000000001,0.895000000000001,0.900000000000001,
0.905000000000001,0.910000000000001,0.915000000000001,0.920000000000001,
0.925000000000001,0.930000000000001,0.935000000000001,0.940000000000001,
0.945000000000001,0.950000000000001,0.955000000000001,0.960000000000001,
0.965000000000001,0.970000000000001,0.975000000000001,0.980000000000001,
0.985000000000001,0.990000000000001,0.995000000000001,1.),(0.,1.2),
 .UNSPECIFIED.)
GEOMETRIC_REPRESENTATION_ITEM()
RATIONAL_B_SPLINE_SURFACE(((1.,1.),(1.,1.),(1.,1.),(1.,1.),(1.,1.),(1.,
1.),(1.,1.),(1.,1.),(1.,1.),(1.,1.),(1.,1.),(1.,1.),(1.,1.),(1.,1.),(1.,
1.),(1.,1.),(1.,1.),(1.,1.),(1.,1.),(1.,1.),(1.,1.),(1.,1.),(1.,1.),(1.,
1.),(1.,1.),(1.,1.),(1.,1.),(1.,1.),(1.,1.),(1.,1.),(1.,1.),(1.,1.),(1.,
1.),(1.,1.),(1.,1.),(1.,1.),(1.,1.),(1.,1.),(1.,1.),(1.,1.),(1.,1.),(1.,
1.),(1.,1.),(1.,1.),(1.,1.),(1.,1.),(1.,1.),(1.,1.),(1.,1.),(1.,1.),(1.,
1.),(1.,1.),(1.,1.),(1.,1.),(1.,1.),(1.,1.),(1.,1.),(1.,1.),(1.,1.),(1.,
1.),(1.,1.),(1.,1.),(1.,1.),(1.,1.),(1.,1.),(1.,1.),(1.,1.),(1.,1.),(1.,
1.),(1.,1.),(1.,1.),(1.,1.),(1.,1.),(1.,1.),(1.,1.),(1.,1.),(1.,1.),(1.,
1.),(1.,1.),(1.,1.),(1.,1.),(1.,1.),(1.,1.),(1.,1.),(1.,1.),(1.,1.),(1.,
1.),(1.,1.),(1.,1.),(1.,1.),(1.,1.),(1.,1.),(1.,1.),(1.,1.),(1.,1.),(1.,
1.),(1.,1.),(1.,1.),(1.,1.),(1.,1.),(1.,1.),(1.,1.),(1.,1.),(1.,1.),(1.,
1.),(1.,1.),(1.,1.),(1.,1.),(1.,1.),(1.,1.),(1.,1.),(1.,1.),(1.,1.),(1.,
1.),(1.,1.),(1.,1.),(1.,1.),(1.,1.),(1.,1.),(1.,1.),(1.,1.),(1.,1.),(1.,
1.),(1.,1.),(1.,1.),(1.,1.),(1.,1.),(1.,1.),(1.,1.),(1.,1.),(1.,1.),(1.,
1.),(1.,1.),(1.,1.),(1.,1.),(1.,1.),(1.,1.),(1.,1.),(1.,1.),(1.,1.),(1.,
1.),(1.,1.),(1.,1.),(1.,1.),(1.,1.),(1.,1.),(1.,1.),(1.,1.),(1.,1.),(1.,
1.),(1.,1.),(1.,1.),(1.,1.),(1.,1.),(1.,1.),(1.,1.),(1.,1.),(1.,1.),(1.,
1.),(1.,1.),(1.,1.),(1.,1.),(1.,1.),(1.,1.),(1.,1.),(1.,1.),(1.,1.),(1.,
1.),(1.,1.),(1.,1.),(1.,1.),(1.,1.),(1.,1.),(1.,1.),(1.,1.),(1.,1.),(1.,
1.),(1.,1.),(1.,1.),(1.,1.),(1.,1.),(1.,1.),(1.,1.),(1.,1.),(1.,1.),(1.,
1.),(1.,1.),(1.,1.),(1.,1.),(1.,1.),(1.,1.),(1.,1.),(1.,1.),(1.,1.),(1.,
1.),(1.,1.),(1.,1.),(1.,1.),(1.,1.),(1.,1.),(1.,1.),(1.,1.),(1.,1.),(1.,
1.),(1.,1.)))
REPRESENTATION_ITEM('')
SURFACE()
);
#916=(
BOUNDED_SURFACE()
B_SPLINE_SURFACE(5,1,((#82190,#82191),(#82192,#82193),(#82194,#82195),(#82196,
#82197),(#82198,#82199),(#82200,#82201),(#82202,#82203),(#82204,#82205),
(#82206,#82207),(#82208,#82209),(#82210,#82211),(#82212,#82213),(#82214,
#82215),(#82216,#82217),(#82218,#82219),(#82220,#82221),(#82222,#82223),
(#82224,#82225),(#82226,#82227),(#82228,#82229),(#82230,#82231),(#82232,
#82233),(#82234,#82235),(#82236,#82237),(#82238,#82239),(#82240,#82241),
(#82242,#82243),(#82244,#82245),(#82246,#82247),(#82248,#82249),(#82250,
#82251),(#82252,#82253),(#82254,#82255),(#82256,#82257),(#82258,#82259),
(#82260,#82261),(#82262,#82263),(#82264,#82265),(#82266,#82267),(#82268,
#82269),(#82270,#82271),(#82272,#82273),(#82274,#82275),(#82276,#82277),
(#82278,#82279),(#82280,#82281),(#82282,#82283),(#82284,#82285),(#82286,
#82287),(#82288,#82289),(#82290,#82291),(#82292,#82293),(#82294,#82295),
(#82296,#82297),(#82298,#82299),(#82300,#82301),(#82302,#82303),(#82304,
#82305),(#82306,#82307),(#82308,#82309),(#82310,#82311),(#82312,#82313),
(#82314,#82315),(#82316,#82317),(#82318,#82319),(#82320,#82321),(#82322,
#82323),(#82324,#82325),(#82326,#82327),(#82328,#82329),(#82330,#82331),
(#82332,#82333),(#82334,#82335),(#82336,#82337),(#82338,#82339),(#82340,
#82341),(#82342,#82343),(#82344,#82345),(#82346,#82347),(#82348,#82349),
(#82350,#82351),(#82352,#82353),(#82354,#82355),(#82356,#82357),(#82358,
#82359),(#82360,#82361),(#82362,#82363),(#82364,#82365),(#82366,#82367),
(#82368,#82369),(#82370,#82371),(#82372,#82373),(#82374,#82375),(#82376,
#82377),(#82378,#82379),(#82380,#82381),(#82382,#82383),(#82384,#82385),
(#82386,#82387),(#82388,#82389),(#82390,#82391),(#82392,#82393),(#82394,
#82395),(#82396,#82397),(#82398,#82399),(#82400,#82401),(#82402,#82403),
(#82404,#82405),(#82406,#82407),(#82408,#82409),(#82410,#82411),(#82412,
#82413),(#82414,#82415),(#82416,#82417),(#82418,#82419),(#82420,#82421),
(#82422,#82423),(#82424,#82425),(#82426,#82427),(#82428,#82429),(#82430,
#82431),(#82432,#82433),(#82434,#82435),(#82436,#82437),(#82438,#82439),
(#82440,#82441),(#82442,#82443),(#82444,#82445),(#82446,#82447),(#82448,
#82449),(#82450,#82451),(#82452,#82453),(#82454,#82455),(#82456,#82457),
(#82458,#82459),(#82460,#82461),(#82462,#82463),(#82464,#82465),(#82466,
#82467),(#82468,#82469),(#82470,#82471),(#82472,#82473),(#82474,#82475),
(#82476,#82477),(#82478,#82479),(#82480,#82481),(#82482,#82483),(#82484,
#82485),(#82486,#82487),(#82488,#82489),(#82490,#82491),(#82492,#82493),
(#82494,#82495),(#82496,#82497),(#82498,#82499),(#82500,#82501),(#82502,
#82503),(#82504,#82505),(#82506,#82507),(#82508,#82509),(#82510,#82511),
(#82512,#82513),(#82514,#82515),(#82516,#82517),(#82518,#82519),(#82520,
#82521),(#82522,#82523),(#82524,#82525),(#82526,#82527),(#82528,#82529),
(#82530,#82531),(#82532,#82533),(#82534,#82535),(#82536,#82537),(#82538,
#82539),(#82540,#82541),(#82542,#82543),(#82544,#82545),(#82546,#82547),
(#82548,#82549),(#82550,#82551),(#82552,#82553),(#82554,#82555),(#82556,
#82557),(#82558,#82559),(#82560,#82561),(#82562,#82563),(#82564,#82565),
(#82566,#82567),(#82568,#82569),(#82570,#82571),(#82572,#82573),(#82574,
#82575),(#82576,#82577),(#82578,#82579),(#82580,#82581),(#82582,#82583),
(#82584,#82585),(#82586,#82587),(#82588,#82589),(#82590,#82591),(#82592,
#82593),(#82594,#82595),(#82596,#82597),(#82598,#82599)),.UNSPECIFIED.,
 .F.,.F.,.F.)
B_SPLINE_SURFACE_WITH_KNOTS((6,1,1,1,1,1,1,1,1,1,1,1,1,1,1,1,1,1,1,1,1,
1,1,1,1,1,1,1,1,1,1,1,1,1,1,1,1,1,1,1,1,1,1,1,1,1,1,1,1,1,1,1,1,1,1,1,1,
1,1,1,1,1,1,1,1,1,1,1,1,1,1,1,1,1,1,1,1,1,1,1,1,1,1,1,1,1,1,1,1,1,1,1,1,
1,1,1,1,1,1,1,1,1,1,1,1,1,1,1,1,1,1,1,1,1,1,1,1,1,1,1,1,1,1,1,1,1,1,1,1,
1,1,1,1,1,1,1,1,1,1,1,1,1,1,1,1,1,1,1,1,1,1,1,1,1,1,1,1,1,1,1,1,1,1,1,1,
1,1,1,1,1,1,1,1,1,1,1,1,1,1,1,1,1,1,1,1,1,1,1,1,1,1,1,1,1,1,1,1,1,1,1,6),
(2,2),(0.,0.005,0.01,0.015,0.02,0.025,0.03,0.035,0.04,0.045,0.05,0.055,
0.06,0.065,0.07,0.075,0.08,0.085,0.09,0.095,0.1,0.105,0.11,0.115,0.12,0.125,
0.13,0.135,0.14,0.145,0.15,0.155,0.16,0.165,0.17,0.175,0.18,0.185,0.19,
0.195,0.2,0.205,0.21,0.215,0.22,0.225,0.23,0.235,0.24,0.245,0.25,0.255,
0.26,0.265,0.27,0.275,0.28,0.285,0.29,0.295,0.3,0.305,0.31,0.315,0.32,0.325,
0.33,0.335,0.34,0.345,0.35,0.355,0.36,0.365,0.37,0.375,0.38,0.385,0.39,
0.395,0.4,0.405,0.41,0.415,0.42,0.425,0.43,0.435,0.44,0.445,0.45,0.455,
0.46,0.465,0.47,0.475,0.48,0.485,0.49,0.495,0.5,0.505,0.51,0.515,0.52,0.525,
0.53,0.535,0.54,0.545,0.55,0.555,0.56,0.565,0.57,0.575,0.58,0.585,0.59,
0.595,0.6,0.605,0.61,0.615,0.62,0.625,0.63,0.635,0.64,0.645,0.65,0.655,
0.66,0.665,0.67,0.675,0.68,0.685,0.690000000000001,0.695000000000001,0.700000000000001,
0.705000000000001,0.710000000000001,0.715000000000001,0.720000000000001,
0.725000000000001,0.730000000000001,0.735000000000001,0.740000000000001,
0.745000000000001,0.750000000000001,0.755000000000001,0.760000000000001,
0.765000000000001,0.770000000000001,0.775000000000001,0.780000000000001,
0.785000000000001,0.790000000000001,0.795000000000001,0.800000000000001,
0.805000000000001,0.810000000000001,0.815000000000001,0.820000000000001,
0.825000000000001,0.830000000000001,0.835000000000001,0.840000000000001,
0.845000000000001,0.850000000000001,0.855000000000001,0.860000000000001,
0.865000000000001,0.870000000000001,0.875000000000001,0.880000000000001,
0.885000000000001,0.890000000000001,0.895000000000001,0.900000000000001,
0.905000000000001,0.910000000000001,0.915000000000001,0.920000000000001,
0.925000000000001,0.930000000000001,0.935000000000001,0.940000000000001,
0.945000000000001,0.950000000000001,0.955000000000001,0.960000000000001,
0.965000000000001,0.970000000000001,0.975000000000001,0.980000000000001,
0.985000000000001,0.990000000000001,0.995000000000001,1.),(0.,1.2),
 .UNSPECIFIED.)
GEOMETRIC_REPRESENTATION_ITEM()
RATIONAL_B_SPLINE_SURFACE(((1.,1.),(1.,1.),(1.,1.),(1.,1.),(1.,1.),(1.,
1.),(1.,1.),(1.,1.),(1.,1.),(1.,1.),(1.,1.),(1.,1.),(1.,1.),(1.,1.),(1.,
1.),(1.,1.),(1.,1.),(1.,1.),(1.,1.),(1.,1.),(1.,1.),(1.,1.),(1.,1.),(1.,
1.),(1.,1.),(1.,1.),(1.,1.),(1.,1.),(1.,1.),(1.,1.),(1.,1.),(1.,1.),(1.,
1.),(1.,1.),(1.,1.),(1.,1.),(1.,1.),(1.,1.),(1.,1.),(1.,1.),(1.,1.),(1.,
1.),(1.,1.),(1.,1.),(1.,1.),(1.,1.),(1.,1.),(1.,1.),(1.,1.),(1.,1.),(1.,
1.),(1.,1.),(1.,1.),(1.,1.),(1.,1.),(1.,1.),(1.,1.),(1.,1.),(1.,1.),(1.,
1.),(1.,1.),(1.,1.),(1.,1.),(1.,1.),(1.,1.),(1.,1.),(1.,1.),(1.,1.),(1.,
1.),(1.,1.),(1.,1.),(1.,1.),(1.,1.),(1.,1.),(1.,1.),(1.,1.),(1.,1.),(1.,
1.),(1.,1.),(1.,1.),(1.,1.),(1.,1.),(1.,1.),(1.,1.),(1.,1.),(1.,1.),(1.,
1.),(1.,1.),(1.,1.),(1.,1.),(1.,1.),(1.,1.),(1.,1.),(1.,1.),(1.,1.),(1.,
1.),(1.,1.),(1.,1.),(1.,1.),(1.,1.),(1.,1.),(1.,1.),(1.,1.),(1.,1.),(1.,
1.),(1.,1.),(1.,1.),(1.,1.),(1.,1.),(1.,1.),(1.,1.),(1.,1.),(1.,1.),(1.,
1.),(1.,1.),(1.,1.),(1.,1.),(1.,1.),(1.,1.),(1.,1.),(1.,1.),(1.,1.),(1.,
1.),(1.,1.),(1.,1.),(1.,1.),(1.,1.),(1.,1.),(1.,1.),(1.,1.),(1.,1.),(1.,
1.),(1.,1.),(1.,1.),(1.,1.),(1.,1.),(1.,1.),(1.,1.),(1.,1.),(1.,1.),(1.,
1.),(1.,1.),(1.,1.),(1.,1.),(1.,1.),(1.,1.),(1.,1.),(1.,1.),(1.,1.),(1.,
1.),(1.,1.),(1.,1.),(1.,1.),(1.,1.),(1.,1.),(1.,1.),(1.,1.),(1.,1.),(1.,
1.),(1.,1.),(1.,1.),(1.,1.),(1.,1.),(1.,1.),(1.,1.),(1.,1.),(1.,1.),(1.,
1.),(1.,1.),(1.,1.),(1.,1.),(1.,1.),(1.,1.),(1.,1.),(1.,1.),(1.,1.),(1.,
1.),(1.,1.),(1.,1.),(1.,1.),(1.,1.),(1.,1.),(1.,1.),(1.,1.),(1.,1.),(1.,
1.),(1.,1.),(1.,1.),(1.,1.),(1.,1.),(1.,1.),(1.,1.),(1.,1.),(1.,1.),(1.,
1.),(1.,1.),(1.,1.),(1.,1.),(1.,1.),(1.,1.),(1.,1.),(1.,1.),(1.,1.),(1.,
1.),(1.,1.)))
REPRESENTATION_ITEM('')
SURFACE()
);
#917=(
BOUNDED_SURFACE()
B_SPLINE_SURFACE(5,1,((#83086,#83087),(#83088,#83089),(#83090,#83091),(#83092,
#83093),(#83094,#83095),(#83096,#83097),(#83098,#83099),(#83100,#83101),
(#83102,#83103),(#83104,#83105),(#83106,#83107),(#83108,#83109),(#83110,
#83111),(#83112,#83113),(#83114,#83115),(#83116,#83117),(#83118,#83119),
(#83120,#83121),(#83122,#83123),(#83124,#83125),(#83126,#83127),(#83128,
#83129),(#83130,#83131),(#83132,#83133),(#83134,#83135),(#83136,#83137),
(#83138,#83139),(#83140,#83141),(#83142,#83143),(#83144,#83145),(#83146,
#83147),(#83148,#83149),(#83150,#83151),(#83152,#83153),(#83154,#83155),
(#83156,#83157),(#83158,#83159),(#83160,#83161),(#83162,#83163),(#83164,
#83165),(#83166,#83167),(#83168,#83169),(#83170,#83171),(#83172,#83173),
(#83174,#83175),(#83176,#83177),(#83178,#83179),(#83180,#83181),(#83182,
#83183),(#83184,#83185),(#83186,#83187),(#83188,#83189),(#83190,#83191),
(#83192,#83193),(#83194,#83195),(#83196,#83197),(#83198,#83199),(#83200,
#83201),(#83202,#83203),(#83204,#83205),(#83206,#83207),(#83208,#83209),
(#83210,#83211),(#83212,#83213),(#83214,#83215),(#83216,#83217),(#83218,
#83219),(#83220,#83221),(#83222,#83223),(#83224,#83225),(#83226,#83227),
(#83228,#83229),(#83230,#83231),(#83232,#83233),(#83234,#83235),(#83236,
#83237),(#83238,#83239),(#83240,#83241),(#83242,#83243),(#83244,#83245),
(#83246,#83247),(#83248,#83249),(#83250,#83251),(#83252,#83253),(#83254,
#83255),(#83256,#83257),(#83258,#83259),(#83260,#83261),(#83262,#83263),
(#83264,#83265),(#83266,#83267),(#83268,#83269),(#83270,#83271),(#83272,
#83273),(#83274,#83275),(#83276,#83277),(#83278,#83279),(#83280,#83281),
(#83282,#83283),(#83284,#83285),(#83286,#83287),(#83288,#83289),(#83290,
#83291),(#83292,#83293),(#83294,#83295),(#83296,#83297),(#83298,#83299),
(#83300,#83301),(#83302,#83303),(#83304,#83305),(#83306,#83307),(#83308,
#83309),(#83310,#83311),(#83312,#83313),(#83314,#83315),(#83316,#83317),
(#83318,#83319),(#83320,#83321),(#83322,#83323),(#83324,#83325),(#83326,
#83327),(#83328,#83329),(#83330,#83331),(#83332,#83333),(#83334,#83335),
(#83336,#83337),(#83338,#83339),(#83340,#83341),(#83342,#83343),(#83344,
#83345),(#83346,#83347),(#83348,#83349),(#83350,#83351),(#83352,#83353),
(#83354,#83355),(#83356,#83357),(#83358,#83359),(#83360,#83361),(#83362,
#83363),(#83364,#83365),(#83366,#83367),(#83368,#83369),(#83370,#83371),
(#83372,#83373),(#83374,#83375),(#83376,#83377),(#83378,#83379),(#83380,
#83381),(#83382,#83383),(#83384,#83385),(#83386,#83387),(#83388,#83389),
(#83390,#83391),(#83392,#83393),(#83394,#83395),(#83396,#83397),(#83398,
#83399),(#83400,#83401),(#83402,#83403),(#83404,#83405),(#83406,#83407),
(#83408,#83409),(#83410,#83411),(#83412,#83413),(#83414,#83415),(#83416,
#83417),(#83418,#83419),(#83420,#83421),(#83422,#83423),(#83424,#83425),
(#83426,#83427),(#83428,#83429),(#83430,#83431),(#83432,#83433),(#83434,
#83435),(#83436,#83437),(#83438,#83439),(#83440,#83441),(#83442,#83443),
(#83444,#83445),(#83446,#83447),(#83448,#83449),(#83450,#83451),(#83452,
#83453),(#83454,#83455),(#83456,#83457),(#83458,#83459),(#83460,#83461),
(#83462,#83463),(#83464,#83465),(#83466,#83467),(#83468,#83469),(#83470,
#83471),(#83472,#83473),(#83474,#83475),(#83476,#83477),(#83478,#83479),
(#83480,#83481),(#83482,#83483),(#83484,#83485),(#83486,#83487),(#83488,
#83489),(#83490,#83491),(#83492,#83493),(#83494,#83495)),.UNSPECIFIED.,
 .F.,.F.,.F.)
B_SPLINE_SURFACE_WITH_KNOTS((6,1,1,1,1,1,1,1,1,1,1,1,1,1,1,1,1,1,1,1,1,
1,1,1,1,1,1,1,1,1,1,1,1,1,1,1,1,1,1,1,1,1,1,1,1,1,1,1,1,1,1,1,1,1,1,1,1,
1,1,1,1,1,1,1,1,1,1,1,1,1,1,1,1,1,1,1,1,1,1,1,1,1,1,1,1,1,1,1,1,1,1,1,1,
1,1,1,1,1,1,1,1,1,1,1,1,1,1,1,1,1,1,1,1,1,1,1,1,1,1,1,1,1,1,1,1,1,1,1,1,
1,1,1,1,1,1,1,1,1,1,1,1,1,1,1,1,1,1,1,1,1,1,1,1,1,1,1,1,1,1,1,1,1,1,1,1,
1,1,1,1,1,1,1,1,1,1,1,1,1,1,1,1,1,1,1,1,1,1,1,1,1,1,1,1,1,1,1,1,1,1,1,6),
(2,2),(0.,0.005,0.01,0.015,0.02,0.025,0.03,0.035,0.04,0.045,0.05,0.055,
0.06,0.065,0.07,0.075,0.08,0.085,0.09,0.095,0.1,0.105,0.11,0.115,0.12,0.125,
0.13,0.135,0.14,0.145,0.15,0.155,0.16,0.165,0.17,0.175,0.18,0.185,0.19,
0.195,0.2,0.205,0.21,0.215,0.22,0.225,0.23,0.235,0.24,0.245,0.25,0.255,
0.26,0.265,0.27,0.275,0.28,0.285,0.29,0.295,0.3,0.305,0.31,0.315,0.32,0.325,
0.33,0.335,0.34,0.345,0.35,0.355,0.36,0.365,0.37,0.375,0.38,0.385,0.39,
0.395,0.4,0.405,0.41,0.415,0.42,0.425,0.43,0.435,0.44,0.445,0.45,0.455,
0.46,0.465,0.47,0.475,0.48,0.485,0.49,0.495,0.5,0.505,0.51,0.515,0.52,0.525,
0.53,0.535,0.54,0.545,0.55,0.555,0.56,0.565,0.57,0.575,0.58,0.585,0.59,
0.595,0.6,0.605,0.61,0.615,0.62,0.625,0.63,0.635,0.64,0.645,0.65,0.655,
0.66,0.665,0.67,0.675,0.68,0.685,0.690000000000001,0.695000000000001,0.700000000000001,
0.705000000000001,0.710000000000001,0.715000000000001,0.720000000000001,
0.725000000000001,0.730000000000001,0.735000000000001,0.740000000000001,
0.745000000000001,0.750000000000001,0.755000000000001,0.760000000000001,
0.765000000000001,0.770000000000001,0.775000000000001,0.780000000000001,
0.785000000000001,0.790000000000001,0.795000000000001,0.800000000000001,
0.805000000000001,0.810000000000001,0.815000000000001,0.820000000000001,
0.825000000000001,0.830000000000001,0.835000000000001,0.840000000000001,
0.845000000000001,0.850000000000001,0.855000000000001,0.860000000000001,
0.865000000000001,0.870000000000001,0.875000000000001,0.880000000000001,
0.885000000000001,0.890000000000001,0.895000000000001,0.900000000000001,
0.905000000000001,0.910000000000001,0.915000000000001,0.920000000000001,
0.925000000000001,0.930000000000001,0.935000000000001,0.940000000000001,
0.945000000000001,0.950000000000001,0.955000000000001,0.960000000000001,
0.965000000000001,0.970000000000001,0.975000000000001,0.980000000000001,
0.985000000000001,0.990000000000001,0.995000000000001,1.),(0.,1.2),
 .UNSPECIFIED.)
GEOMETRIC_REPRESENTATION_ITEM()
RATIONAL_B_SPLINE_SURFACE(((1.,1.),(1.,1.),(1.,1.),(1.,1.),(1.,1.),(1.,
1.),(1.,1.),(1.,1.),(1.,1.),(1.,1.),(1.,1.),(1.,1.),(1.,1.),(1.,1.),(1.,
1.),(1.,1.),(1.,1.),(1.,1.),(1.,1.),(1.,1.),(1.,1.),(1.,1.),(1.,1.),(1.,
1.),(1.,1.),(1.,1.),(1.,1.),(1.,1.),(1.,1.),(1.,1.),(1.,1.),(1.,1.),(1.,
1.),(1.,1.),(1.,1.),(1.,1.),(1.,1.),(1.,1.),(1.,1.),(1.,1.),(1.,1.),(1.,
1.),(1.,1.),(1.,1.),(1.,1.),(1.,1.),(1.,1.),(1.,1.),(1.,1.),(1.,1.),(1.,
1.),(1.,1.),(1.,1.),(1.,1.),(1.,1.),(1.,1.),(1.,1.),(1.,1.),(1.,1.),(1.,
1.),(1.,1.),(1.,1.),(1.,1.),(1.,1.),(1.,1.),(1.,1.),(1.,1.),(1.,1.),(1.,
1.),(1.,1.),(1.,1.),(1.,1.),(1.,1.),(1.,1.),(1.,1.),(1.,1.),(1.,1.),(1.,
1.),(1.,1.),(1.,1.),(1.,1.),(1.,1.),(1.,1.),(1.,1.),(1.,1.),(1.,1.),(1.,
1.),(1.,1.),(1.,1.),(1.,1.),(1.,1.),(1.,1.),(1.,1.),(1.,1.),(1.,1.),(1.,
1.),(1.,1.),(1.,1.),(1.,1.),(1.,1.),(1.,1.),(1.,1.),(1.,1.),(1.,1.),(1.,
1.),(1.,1.),(1.,1.),(1.,1.),(1.,1.),(1.,1.),(1.,1.),(1.,1.),(1.,1.),(1.,
1.),(1.,1.),(1.,1.),(1.,1.),(1.,1.),(1.,1.),(1.,1.),(1.,1.),(1.,1.),(1.,
1.),(1.,1.),(1.,1.),(1.,1.),(1.,1.),(1.,1.),(1.,1.),(1.,1.),(1.,1.),(1.,
1.),(1.,1.),(1.,1.),(1.,1.),(1.,1.),(1.,1.),(1.,1.),(1.,1.),(1.,1.),(1.,
1.),(1.,1.),(1.,1.),(1.,1.),(1.,1.),(1.,1.),(1.,1.),(1.,1.),(1.,1.),(1.,
1.),(1.,1.),(1.,1.),(1.,1.),(1.,1.),(1.,1.),(1.,1.),(1.,1.),(1.,1.),(1.,
1.),(1.,1.),(1.,1.),(1.,1.),(1.,1.),(1.,1.),(1.,1.),(1.,1.),(1.,1.),(1.,
1.),(1.,1.),(1.,1.),(1.,1.),(1.,1.),(1.,1.),(1.,1.),(1.,1.),(1.,1.),(1.,
1.),(1.,1.),(1.,1.),(1.,1.),(1.,1.),(1.,1.),(1.,1.),(1.,1.),(1.,1.),(1.,
1.),(1.,1.),(1.,1.),(1.,1.),(1.,1.),(1.,1.),(1.,1.),(1.,1.),(1.,1.),(1.,
1.),(1.,1.),(1.,1.),(1.,1.),(1.,1.),(1.,1.),(1.,1.),(1.,1.),(1.,1.),(1.,
1.),(1.,1.)))
REPRESENTATION_ITEM('')
SURFACE()
);
#918=(
BOUNDED_SURFACE()
B_SPLINE_SURFACE(5,1,((#83982,#83983),(#83984,#83985),(#83986,#83987),(#83988,
#83989),(#83990,#83991),(#83992,#83993),(#83994,#83995),(#83996,#83997),
(#83998,#83999),(#84000,#84001),(#84002,#84003),(#84004,#84005),(#84006,
#84007),(#84008,#84009),(#84010,#84011),(#84012,#84013),(#84014,#84015),
(#84016,#84017),(#84018,#84019),(#84020,#84021),(#84022,#84023),(#84024,
#84025),(#84026,#84027),(#84028,#84029),(#84030,#84031),(#84032,#84033),
(#84034,#84035),(#84036,#84037),(#84038,#84039),(#84040,#84041),(#84042,
#84043),(#84044,#84045),(#84046,#84047),(#84048,#84049),(#84050,#84051),
(#84052,#84053),(#84054,#84055),(#84056,#84057),(#84058,#84059),(#84060,
#84061),(#84062,#84063),(#84064,#84065),(#84066,#84067),(#84068,#84069),
(#84070,#84071),(#84072,#84073),(#84074,#84075),(#84076,#84077),(#84078,
#84079),(#84080,#84081),(#84082,#84083),(#84084,#84085),(#84086,#84087),
(#84088,#84089),(#84090,#84091),(#84092,#84093),(#84094,#84095),(#84096,
#84097),(#84098,#84099),(#84100,#84101),(#84102,#84103),(#84104,#84105),
(#84106,#84107),(#84108,#84109),(#84110,#84111),(#84112,#84113),(#84114,
#84115),(#84116,#84117),(#84118,#84119),(#84120,#84121),(#84122,#84123),
(#84124,#84125),(#84126,#84127),(#84128,#84129),(#84130,#84131),(#84132,
#84133),(#84134,#84135),(#84136,#84137),(#84138,#84139),(#84140,#84141),
(#84142,#84143),(#84144,#84145),(#84146,#84147),(#84148,#84149),(#84150,
#84151),(#84152,#84153),(#84154,#84155),(#84156,#84157),(#84158,#84159),
(#84160,#84161),(#84162,#84163),(#84164,#84165),(#84166,#84167),(#84168,
#84169),(#84170,#84171),(#84172,#84173),(#84174,#84175),(#84176,#84177),
(#84178,#84179),(#84180,#84181),(#84182,#84183),(#84184,#84185),(#84186,
#84187),(#84188,#84189),(#84190,#84191),(#84192,#84193),(#84194,#84195),
(#84196,#84197),(#84198,#84199),(#84200,#84201),(#84202,#84203),(#84204,
#84205),(#84206,#84207),(#84208,#84209),(#84210,#84211),(#84212,#84213),
(#84214,#84215),(#84216,#84217),(#84218,#84219),(#84220,#84221),(#84222,
#84223),(#84224,#84225),(#84226,#84227),(#84228,#84229),(#84230,#84231),
(#84232,#84233),(#84234,#84235),(#84236,#84237),(#84238,#84239),(#84240,
#84241),(#84242,#84243),(#84244,#84245),(#84246,#84247),(#84248,#84249),
(#84250,#84251),(#84252,#84253),(#84254,#84255),(#84256,#84257),(#84258,
#84259),(#84260,#84261),(#84262,#84263),(#84264,#84265),(#84266,#84267),
(#84268,#84269),(#84270,#84271),(#84272,#84273),(#84274,#84275),(#84276,
#84277),(#84278,#84279),(#84280,#84281),(#84282,#84283),(#84284,#84285),
(#84286,#84287),(#84288,#84289),(#84290,#84291),(#84292,#84293),(#84294,
#84295),(#84296,#84297),(#84298,#84299),(#84300,#84301),(#84302,#84303),
(#84304,#84305),(#84306,#84307),(#84308,#84309),(#84310,#84311),(#84312,
#84313),(#84314,#84315),(#84316,#84317),(#84318,#84319),(#84320,#84321),
(#84322,#84323),(#84324,#84325),(#84326,#84327),(#84328,#84329),(#84330,
#84331),(#84332,#84333),(#84334,#84335),(#84336,#84337),(#84338,#84339),
(#84340,#84341),(#84342,#84343),(#84344,#84345),(#84346,#84347),(#84348,
#84349),(#84350,#84351),(#84352,#84353),(#84354,#84355),(#84356,#84357),
(#84358,#84359),(#84360,#84361),(#84362,#84363),(#84364,#84365),(#84366,
#84367),(#84368,#84369),(#84370,#84371),(#84372,#84373),(#84374,#84375),
(#84376,#84377),(#84378,#84379),(#84380,#84381),(#84382,#84383),(#84384,
#84385),(#84386,#84387),(#84388,#84389),(#84390,#84391)),.UNSPECIFIED.,
 .F.,.F.,.F.)
B_SPLINE_SURFACE_WITH_KNOTS((6,1,1,1,1,1,1,1,1,1,1,1,1,1,1,1,1,1,1,1,1,
1,1,1,1,1,1,1,1,1,1,1,1,1,1,1,1,1,1,1,1,1,1,1,1,1,1,1,1,1,1,1,1,1,1,1,1,
1,1,1,1,1,1,1,1,1,1,1,1,1,1,1,1,1,1,1,1,1,1,1,1,1,1,1,1,1,1,1,1,1,1,1,1,
1,1,1,1,1,1,1,1,1,1,1,1,1,1,1,1,1,1,1,1,1,1,1,1,1,1,1,1,1,1,1,1,1,1,1,1,
1,1,1,1,1,1,1,1,1,1,1,1,1,1,1,1,1,1,1,1,1,1,1,1,1,1,1,1,1,1,1,1,1,1,1,1,
1,1,1,1,1,1,1,1,1,1,1,1,1,1,1,1,1,1,1,1,1,1,1,1,1,1,1,1,1,1,1,1,1,1,1,6),
(2,2),(0.,0.005,0.01,0.015,0.02,0.025,0.03,0.035,0.04,0.045,0.05,0.055,
0.06,0.065,0.07,0.075,0.08,0.085,0.09,0.095,0.1,0.105,0.11,0.115,0.12,0.125,
0.13,0.135,0.14,0.145,0.15,0.155,0.16,0.165,0.17,0.175,0.18,0.185,0.19,
0.195,0.2,0.205,0.21,0.215,0.22,0.225,0.23,0.235,0.24,0.245,0.25,0.255,
0.26,0.265,0.27,0.275,0.28,0.285,0.29,0.295,0.3,0.305,0.31,0.315,0.32,0.325,
0.33,0.335,0.34,0.345,0.35,0.355,0.36,0.365,0.37,0.375,0.38,0.385,0.39,
0.395,0.4,0.405,0.41,0.415,0.42,0.425,0.43,0.435,0.44,0.445,0.45,0.455,
0.46,0.465,0.47,0.475,0.48,0.485,0.49,0.495,0.5,0.505,0.51,0.515,0.52,0.525,
0.53,0.535,0.54,0.545,0.55,0.555,0.56,0.565,0.57,0.575,0.58,0.585,0.59,
0.595,0.6,0.605,0.61,0.615,0.62,0.625,0.63,0.635,0.64,0.645,0.65,0.655,
0.66,0.665,0.67,0.675,0.68,0.685,0.690000000000001,0.695000000000001,0.700000000000001,
0.705000000000001,0.710000000000001,0.715000000000001,0.720000000000001,
0.725000000000001,0.730000000000001,0.735000000000001,0.740000000000001,
0.745000000000001,0.750000000000001,0.755000000000001,0.760000000000001,
0.765000000000001,0.770000000000001,0.775000000000001,0.780000000000001,
0.785000000000001,0.790000000000001,0.795000000000001,0.800000000000001,
0.805000000000001,0.810000000000001,0.815000000000001,0.820000000000001,
0.825000000000001,0.830000000000001,0.835000000000001,0.840000000000001,
0.845000000000001,0.850000000000001,0.855000000000001,0.860000000000001,
0.865000000000001,0.870000000000001,0.875000000000001,0.880000000000001,
0.885000000000001,0.890000000000001,0.895000000000001,0.900000000000001,
0.905000000000001,0.910000000000001,0.915000000000001,0.920000000000001,
0.925000000000001,0.930000000000001,0.935000000000001,0.940000000000001,
0.945000000000001,0.950000000000001,0.955000000000001,0.960000000000001,
0.965000000000001,0.970000000000001,0.975000000000001,0.980000000000001,
0.985000000000001,0.990000000000001,0.995000000000001,1.),(0.,1.2),
 .UNSPECIFIED.)
GEOMETRIC_REPRESENTATION_ITEM()
RATIONAL_B_SPLINE_SURFACE(((1.,1.),(1.,1.),(1.,1.),(1.,1.),(1.,1.),(1.,
1.),(1.,1.),(1.,1.),(1.,1.),(1.,1.),(1.,1.),(1.,1.),(1.,1.),(1.,1.),(1.,
1.),(1.,1.),(1.,1.),(1.,1.),(1.,1.),(1.,1.),(1.,1.),(1.,1.),(1.,1.),(1.,
1.),(1.,1.),(1.,1.),(1.,1.),(1.,1.),(1.,1.),(1.,1.),(1.,1.),(1.,1.),(1.,
1.),(1.,1.),(1.,1.),(1.,1.),(1.,1.),(1.,1.),(1.,1.),(1.,1.),(1.,1.),(1.,
1.),(1.,1.),(1.,1.),(1.,1.),(1.,1.),(1.,1.),(1.,1.),(1.,1.),(1.,1.),(1.,
1.),(1.,1.),(1.,1.),(1.,1.),(1.,1.),(1.,1.),(1.,1.),(1.,1.),(1.,1.),(1.,
1.),(1.,1.),(1.,1.),(1.,1.),(1.,1.),(1.,1.),(1.,1.),(1.,1.),(1.,1.),(1.,
1.),(1.,1.),(1.,1.),(1.,1.),(1.,1.),(1.,1.),(1.,1.),(1.,1.),(1.,1.),(1.,
1.),(1.,1.),(1.,1.),(1.,1.),(1.,1.),(1.,1.),(1.,1.),(1.,1.),(1.,1.),(1.,
1.),(1.,1.),(1.,1.),(1.,1.),(1.,1.),(1.,1.),(1.,1.),(1.,1.),(1.,1.),(1.,
1.),(1.,1.),(1.,1.),(1.,1.),(1.,1.),(1.,1.),(1.,1.),(1.,1.),(1.,1.),(1.,
1.),(1.,1.),(1.,1.),(1.,1.),(1.,1.),(1.,1.),(1.,1.),(1.,1.),(1.,1.),(1.,
1.),(1.,1.),(1.,1.),(1.,1.),(1.,1.),(1.,1.),(1.,1.),(1.,1.),(1.,1.),(1.,
1.),(1.,1.),(1.,1.),(1.,1.),(1.,1.),(1.,1.),(1.,1.),(1.,1.),(1.,1.),(1.,
1.),(1.,1.),(1.,1.),(1.,1.),(1.,1.),(1.,1.),(1.,1.),(1.,1.),(1.,1.),(1.,
1.),(1.,1.),(1.,1.),(1.,1.),(1.,1.),(1.,1.),(1.,1.),(1.,1.),(1.,1.),(1.,
1.),(1.,1.),(1.,1.),(1.,1.),(1.,1.),(1.,1.),(1.,1.),(1.,1.),(1.,1.),(1.,
1.),(1.,1.),(1.,1.),(1.,1.),(1.,1.),(1.,1.),(1.,1.),(1.,1.),(1.,1.),(1.,
1.),(1.,1.),(1.,1.),(1.,1.),(1.,1.),(1.,1.),(1.,1.),(1.,1.),(1.,1.),(1.,
1.),(1.,1.),(1.,1.),(1.,1.),(1.,1.),(1.,1.),(1.,1.),(1.,1.),(1.,1.),(1.,
1.),(1.,1.),(1.,1.),(1.,1.),(1.,1.),(1.,1.),(1.,1.),(1.,1.),(1.,1.),(1.,
1.),(1.,1.),(1.,1.),(1.,1.),(1.,1.),(1.,1.),(1.,1.),(1.,1.),(1.,1.),(1.,
1.),(1.,1.)))
REPRESENTATION_ITEM('')
SURFACE()
);
#919=(
BOUNDED_SURFACE()
B_SPLINE_SURFACE(5,1,((#84878,#84879),(#84880,#84881),(#84882,#84883),(#84884,
#84885),(#84886,#84887),(#84888,#84889),(#84890,#84891),(#84892,#84893),
(#84894,#84895),(#84896,#84897),(#84898,#84899),(#84900,#84901),(#84902,
#84903),(#84904,#84905),(#84906,#84907),(#84908,#84909),(#84910,#84911),
(#84912,#84913),(#84914,#84915),(#84916,#84917),(#84918,#84919),(#84920,
#84921),(#84922,#84923),(#84924,#84925),(#84926,#84927),(#84928,#84929),
(#84930,#84931),(#84932,#84933),(#84934,#84935),(#84936,#84937),(#84938,
#84939),(#84940,#84941),(#84942,#84943),(#84944,#84945),(#84946,#84947),
(#84948,#84949),(#84950,#84951),(#84952,#84953),(#84954,#84955),(#84956,
#84957),(#84958,#84959),(#84960,#84961),(#84962,#84963),(#84964,#84965),
(#84966,#84967),(#84968,#84969),(#84970,#84971),(#84972,#84973),(#84974,
#84975),(#84976,#84977),(#84978,#84979),(#84980,#84981),(#84982,#84983),
(#84984,#84985),(#84986,#84987),(#84988,#84989),(#84990,#84991),(#84992,
#84993),(#84994,#84995),(#84996,#84997),(#84998,#84999),(#85000,#85001),
(#85002,#85003),(#85004,#85005),(#85006,#85007),(#85008,#85009),(#85010,
#85011),(#85012,#85013),(#85014,#85015),(#85016,#85017),(#85018,#85019),
(#85020,#85021),(#85022,#85023),(#85024,#85025),(#85026,#85027),(#85028,
#85029),(#85030,#85031),(#85032,#85033),(#85034,#85035),(#85036,#85037),
(#85038,#85039),(#85040,#85041),(#85042,#85043),(#85044,#85045),(#85046,
#85047),(#85048,#85049),(#85050,#85051),(#85052,#85053),(#85054,#85055),
(#85056,#85057),(#85058,#85059),(#85060,#85061),(#85062,#85063),(#85064,
#85065),(#85066,#85067),(#85068,#85069),(#85070,#85071),(#85072,#85073),
(#85074,#85075),(#85076,#85077),(#85078,#85079),(#85080,#85081),(#85082,
#85083),(#85084,#85085),(#85086,#85087),(#85088,#85089),(#85090,#85091),
(#85092,#85093),(#85094,#85095),(#85096,#85097),(#85098,#85099),(#85100,
#85101),(#85102,#85103),(#85104,#85105),(#85106,#85107),(#85108,#85109),
(#85110,#85111),(#85112,#85113),(#85114,#85115),(#85116,#85117),(#85118,
#85119),(#85120,#85121),(#85122,#85123),(#85124,#85125),(#85126,#85127),
(#85128,#85129),(#85130,#85131),(#85132,#85133),(#85134,#85135),(#85136,
#85137),(#85138,#85139),(#85140,#85141),(#85142,#85143),(#85144,#85145),
(#85146,#85147),(#85148,#85149),(#85150,#85151),(#85152,#85153),(#85154,
#85155),(#85156,#85157),(#85158,#85159),(#85160,#85161),(#85162,#85163),
(#85164,#85165),(#85166,#85167),(#85168,#85169),(#85170,#85171),(#85172,
#85173),(#85174,#85175),(#85176,#85177),(#85178,#85179),(#85180,#85181),
(#85182,#85183),(#85184,#85185),(#85186,#85187),(#85188,#85189),(#85190,
#85191),(#85192,#85193),(#85194,#85195),(#85196,#85197),(#85198,#85199),
(#85200,#85201),(#85202,#85203),(#85204,#85205),(#85206,#85207),(#85208,
#85209),(#85210,#85211),(#85212,#85213),(#85214,#85215),(#85216,#85217),
(#85218,#85219),(#85220,#85221),(#85222,#85223),(#85224,#85225),(#85226,
#85227),(#85228,#85229),(#85230,#85231),(#85232,#85233),(#85234,#85235),
(#85236,#85237),(#85238,#85239),(#85240,#85241),(#85242,#85243),(#85244,
#85245),(#85246,#85247),(#85248,#85249),(#85250,#85251),(#85252,#85253),
(#85254,#85255),(#85256,#85257),(#85258,#85259),(#85260,#85261),(#85262,
#85263),(#85264,#85265),(#85266,#85267),(#85268,#85269),(#85270,#85271),
(#85272,#85273),(#85274,#85275),(#85276,#85277),(#85278,#85279),(#85280,
#85281),(#85282,#85283),(#85284,#85285),(#85286,#85287)),.UNSPECIFIED.,
 .F.,.F.,.F.)
B_SPLINE_SURFACE_WITH_KNOTS((6,1,1,1,1,1,1,1,1,1,1,1,1,1,1,1,1,1,1,1,1,
1,1,1,1,1,1,1,1,1,1,1,1,1,1,1,1,1,1,1,1,1,1,1,1,1,1,1,1,1,1,1,1,1,1,1,1,
1,1,1,1,1,1,1,1,1,1,1,1,1,1,1,1,1,1,1,1,1,1,1,1,1,1,1,1,1,1,1,1,1,1,1,1,
1,1,1,1,1,1,1,1,1,1,1,1,1,1,1,1,1,1,1,1,1,1,1,1,1,1,1,1,1,1,1,1,1,1,1,1,
1,1,1,1,1,1,1,1,1,1,1,1,1,1,1,1,1,1,1,1,1,1,1,1,1,1,1,1,1,1,1,1,1,1,1,1,
1,1,1,1,1,1,1,1,1,1,1,1,1,1,1,1,1,1,1,1,1,1,1,1,1,1,1,1,1,1,1,1,1,1,1,6),
(2,2),(0.,0.005,0.01,0.015,0.02,0.025,0.03,0.035,0.04,0.045,0.05,0.055,
0.06,0.065,0.07,0.075,0.08,0.085,0.09,0.095,0.1,0.105,0.11,0.115,0.12,0.125,
0.13,0.135,0.14,0.145,0.15,0.155,0.16,0.165,0.17,0.175,0.18,0.185,0.19,
0.195,0.2,0.205,0.21,0.215,0.22,0.225,0.23,0.235,0.24,0.245,0.25,0.255,
0.26,0.265,0.27,0.275,0.28,0.285,0.29,0.295,0.3,0.305,0.31,0.315,0.32,0.325,
0.33,0.335,0.34,0.345,0.35,0.355,0.36,0.365,0.37,0.375,0.38,0.385,0.39,
0.395,0.4,0.405,0.41,0.415,0.42,0.425,0.43,0.435,0.44,0.445,0.45,0.455,
0.46,0.465,0.47,0.475,0.48,0.485,0.49,0.495,0.5,0.505,0.51,0.515,0.52,0.525,
0.53,0.535,0.54,0.545,0.55,0.555,0.56,0.565,0.57,0.575,0.58,0.585,0.59,
0.595,0.6,0.605,0.61,0.615,0.62,0.625,0.63,0.635,0.64,0.645,0.65,0.655,
0.66,0.665,0.67,0.675,0.68,0.685,0.690000000000001,0.695000000000001,0.700000000000001,
0.705000000000001,0.710000000000001,0.715000000000001,0.720000000000001,
0.725000000000001,0.730000000000001,0.735000000000001,0.740000000000001,
0.745000000000001,0.750000000000001,0.755000000000001,0.760000000000001,
0.765000000000001,0.770000000000001,0.775000000000001,0.780000000000001,
0.785000000000001,0.790000000000001,0.795000000000001,0.800000000000001,
0.805000000000001,0.810000000000001,0.815000000000001,0.820000000000001,
0.825000000000001,0.830000000000001,0.835000000000001,0.840000000000001,
0.845000000000001,0.850000000000001,0.855000000000001,0.860000000000001,
0.865000000000001,0.870000000000001,0.875000000000001,0.880000000000001,
0.885000000000001,0.890000000000001,0.895000000000001,0.900000000000001,
0.905000000000001,0.910000000000001,0.915000000000001,0.920000000000001,
0.925000000000001,0.930000000000001,0.935000000000001,0.940000000000001,
0.945000000000001,0.950000000000001,0.955000000000001,0.960000000000001,
0.965000000000001,0.970000000000001,0.975000000000001,0.980000000000001,
0.985000000000001,0.990000000000001,0.995000000000001,1.),(0.,1.2),
 .UNSPECIFIED.)
GEOMETRIC_REPRESENTATION_ITEM()
RATIONAL_B_SPLINE_SURFACE(((1.,1.),(1.,1.),(1.,1.),(1.,1.),(1.,1.),(1.,
1.),(1.,1.),(1.,1.),(1.,1.),(1.,1.),(1.,1.),(1.,1.),(1.,1.),(1.,1.),(1.,
1.),(1.,1.),(1.,1.),(1.,1.),(1.,1.),(1.,1.),(1.,1.),(1.,1.),(1.,1.),(1.,
1.),(1.,1.),(1.,1.),(1.,1.),(1.,1.),(1.,1.),(1.,1.),(1.,1.),(1.,1.),(1.,
1.),(1.,1.),(1.,1.),(1.,1.),(1.,1.),(1.,1.),(1.,1.),(1.,1.),(1.,1.),(1.,
1.),(1.,1.),(1.,1.),(1.,1.),(1.,1.),(1.,1.),(1.,1.),(1.,1.),(1.,1.),(1.,
1.),(1.,1.),(1.,1.),(1.,1.),(1.,1.),(1.,1.),(1.,1.),(1.,1.),(1.,1.),(1.,
1.),(1.,1.),(1.,1.),(1.,1.),(1.,1.),(1.,1.),(1.,1.),(1.,1.),(1.,1.),(1.,
1.),(1.,1.),(1.,1.),(1.,1.),(1.,1.),(1.,1.),(1.,1.),(1.,1.),(1.,1.),(1.,
1.),(1.,1.),(1.,1.),(1.,1.),(1.,1.),(1.,1.),(1.,1.),(1.,1.),(1.,1.),(1.,
1.),(1.,1.),(1.,1.),(1.,1.),(1.,1.),(1.,1.),(1.,1.),(1.,1.),(1.,1.),(1.,
1.),(1.,1.),(1.,1.),(1.,1.),(1.,1.),(1.,1.),(1.,1.),(1.,1.),(1.,1.),(1.,
1.),(1.,1.),(1.,1.),(1.,1.),(1.,1.),(1.,1.),(1.,1.),(1.,1.),(1.,1.),(1.,
1.),(1.,1.),(1.,1.),(1.,1.),(1.,1.),(1.,1.),(1.,1.),(1.,1.),(1.,1.),(1.,
1.),(1.,1.),(1.,1.),(1.,1.),(1.,1.),(1.,1.),(1.,1.),(1.,1.),(1.,1.),(1.,
1.),(1.,1.),(1.,1.),(1.,1.),(1.,1.),(1.,1.),(1.,1.),(1.,1.),(1.,1.),(1.,
1.),(1.,1.),(1.,1.),(1.,1.),(1.,1.),(1.,1.),(1.,1.),(1.,1.),(1.,1.),(1.,
1.),(1.,1.),(1.,1.),(1.,1.),(1.,1.),(1.,1.),(1.,1.),(1.,1.),(1.,1.),(1.,
1.),(1.,1.),(1.,1.),(1.,1.),(1.,1.),(1.,1.),(1.,1.),(1.,1.),(1.,1.),(1.,
1.),(1.,1.),(1.,1.),(1.,1.),(1.,1.),(1.,1.),(1.,1.),(1.,1.),(1.,1.),(1.,
1.),(1.,1.),(1.,1.),(1.,1.),(1.,1.),(1.,1.),(1.,1.),(1.,1.),(1.,1.),(1.,
1.),(1.,1.),(1.,1.),(1.,1.),(1.,1.),(1.,1.),(1.,1.),(1.,1.),(1.,1.),(1.,
1.),(1.,1.),(1.,1.),(1.,1.),(1.,1.),(1.,1.),(1.,1.),(1.,1.),(1.,1.),(1.,
1.),(1.,1.)))
REPRESENTATION_ITEM('')
SURFACE()
);
#920=(
BOUNDED_SURFACE()
B_SPLINE_SURFACE(5,1,((#85774,#85775),(#85776,#85777),(#85778,#85779),(#85780,
#85781),(#85782,#85783),(#85784,#85785),(#85786,#85787),(#85788,#85789),
(#85790,#85791),(#85792,#85793),(#85794,#85795),(#85796,#85797),(#85798,
#85799),(#85800,#85801),(#85802,#85803),(#85804,#85805),(#85806,#85807),
(#85808,#85809),(#85810,#85811),(#85812,#85813),(#85814,#85815),(#85816,
#85817),(#85818,#85819),(#85820,#85821),(#85822,#85823),(#85824,#85825),
(#85826,#85827),(#85828,#85829),(#85830,#85831),(#85832,#85833),(#85834,
#85835),(#85836,#85837),(#85838,#85839),(#85840,#85841),(#85842,#85843),
(#85844,#85845),(#85846,#85847),(#85848,#85849),(#85850,#85851),(#85852,
#85853),(#85854,#85855),(#85856,#85857),(#85858,#85859),(#85860,#85861),
(#85862,#85863),(#85864,#85865),(#85866,#85867),(#85868,#85869),(#85870,
#85871),(#85872,#85873),(#85874,#85875),(#85876,#85877),(#85878,#85879),
(#85880,#85881),(#85882,#85883),(#85884,#85885),(#85886,#85887),(#85888,
#85889),(#85890,#85891),(#85892,#85893),(#85894,#85895),(#85896,#85897),
(#85898,#85899),(#85900,#85901),(#85902,#85903),(#85904,#85905),(#85906,
#85907),(#85908,#85909),(#85910,#85911),(#85912,#85913),(#85914,#85915),
(#85916,#85917),(#85918,#85919),(#85920,#85921),(#85922,#85923),(#85924,
#85925),(#85926,#85927),(#85928,#85929),(#85930,#85931),(#85932,#85933),
(#85934,#85935),(#85936,#85937),(#85938,#85939),(#85940,#85941),(#85942,
#85943),(#85944,#85945),(#85946,#85947),(#85948,#85949),(#85950,#85951),
(#85952,#85953),(#85954,#85955),(#85956,#85957),(#85958,#85959),(#85960,
#85961),(#85962,#85963),(#85964,#85965),(#85966,#85967),(#85968,#85969),
(#85970,#85971),(#85972,#85973),(#85974,#85975),(#85976,#85977),(#85978,
#85979),(#85980,#85981),(#85982,#85983),(#85984,#85985),(#85986,#85987),
(#85988,#85989),(#85990,#85991),(#85992,#85993),(#85994,#85995),(#85996,
#85997),(#85998,#85999),(#86000,#86001),(#86002,#86003),(#86004,#86005),
(#86006,#86007),(#86008,#86009),(#86010,#86011),(#86012,#86013),(#86014,
#86015),(#86016,#86017),(#86018,#86019),(#86020,#86021),(#86022,#86023),
(#86024,#86025),(#86026,#86027),(#86028,#86029),(#86030,#86031),(#86032,
#86033),(#86034,#86035),(#86036,#86037),(#86038,#86039),(#86040,#86041),
(#86042,#86043),(#86044,#86045),(#86046,#86047),(#86048,#86049),(#86050,
#86051),(#86052,#86053),(#86054,#86055),(#86056,#86057),(#86058,#86059),
(#86060,#86061),(#86062,#86063),(#86064,#86065),(#86066,#86067),(#86068,
#86069),(#86070,#86071),(#86072,#86073),(#86074,#86075),(#86076,#86077),
(#86078,#86079),(#86080,#86081),(#86082,#86083),(#86084,#86085),(#86086,
#86087),(#86088,#86089),(#86090,#86091),(#86092,#86093),(#86094,#86095),
(#86096,#86097),(#86098,#86099),(#86100,#86101),(#86102,#86103),(#86104,
#86105),(#86106,#86107),(#86108,#86109),(#86110,#86111),(#86112,#86113),
(#86114,#86115),(#86116,#86117),(#86118,#86119),(#86120,#86121),(#86122,
#86123),(#86124,#86125),(#86126,#86127),(#86128,#86129),(#86130,#86131),
(#86132,#86133),(#86134,#86135),(#86136,#86137),(#86138,#86139),(#86140,
#86141),(#86142,#86143),(#86144,#86145),(#86146,#86147),(#86148,#86149),
(#86150,#86151),(#86152,#86153),(#86154,#86155),(#86156,#86157),(#86158,
#86159),(#86160,#86161),(#86162,#86163),(#86164,#86165),(#86166,#86167),
(#86168,#86169),(#86170,#86171),(#86172,#86173),(#86174,#86175),(#86176,
#86177),(#86178,#86179),(#86180,#86181),(#86182,#86183)),.UNSPECIFIED.,
 .F.,.F.,.F.)
B_SPLINE_SURFACE_WITH_KNOTS((6,1,1,1,1,1,1,1,1,1,1,1,1,1,1,1,1,1,1,1,1,
1,1,1,1,1,1,1,1,1,1,1,1,1,1,1,1,1,1,1,1,1,1,1,1,1,1,1,1,1,1,1,1,1,1,1,1,
1,1,1,1,1,1,1,1,1,1,1,1,1,1,1,1,1,1,1,1,1,1,1,1,1,1,1,1,1,1,1,1,1,1,1,1,
1,1,1,1,1,1,1,1,1,1,1,1,1,1,1,1,1,1,1,1,1,1,1,1,1,1,1,1,1,1,1,1,1,1,1,1,
1,1,1,1,1,1,1,1,1,1,1,1,1,1,1,1,1,1,1,1,1,1,1,1,1,1,1,1,1,1,1,1,1,1,1,1,
1,1,1,1,1,1,1,1,1,1,1,1,1,1,1,1,1,1,1,1,1,1,1,1,1,1,1,1,1,1,1,1,1,1,1,6),
(2,2),(0.,0.005,0.01,0.015,0.02,0.025,0.03,0.035,0.04,0.045,0.05,0.055,
0.06,0.065,0.07,0.075,0.08,0.085,0.09,0.095,0.1,0.105,0.11,0.115,0.12,0.125,
0.13,0.135,0.14,0.145,0.15,0.155,0.16,0.165,0.17,0.175,0.18,0.185,0.19,
0.195,0.2,0.205,0.21,0.215,0.22,0.225,0.23,0.235,0.24,0.245,0.25,0.255,
0.26,0.265,0.27,0.275,0.28,0.285,0.29,0.295,0.3,0.305,0.31,0.315,0.32,0.325,
0.33,0.335,0.34,0.345,0.35,0.355,0.36,0.365,0.37,0.375,0.38,0.385,0.39,
0.395,0.4,0.405,0.41,0.415,0.42,0.425,0.43,0.435,0.44,0.445,0.45,0.455,
0.46,0.465,0.47,0.475,0.48,0.485,0.49,0.495,0.5,0.505,0.51,0.515,0.52,0.525,
0.53,0.535,0.54,0.545,0.55,0.555,0.56,0.565,0.57,0.575,0.58,0.585,0.59,
0.595,0.6,0.605,0.61,0.615,0.62,0.625,0.63,0.635,0.64,0.645,0.65,0.655,
0.66,0.665,0.67,0.675,0.68,0.685,0.690000000000001,0.695000000000001,0.700000000000001,
0.705000000000001,0.710000000000001,0.715000000000001,0.720000000000001,
0.725000000000001,0.730000000000001,0.735000000000001,0.740000000000001,
0.745000000000001,0.750000000000001,0.755000000000001,0.760000000000001,
0.765000000000001,0.770000000000001,0.775000000000001,0.780000000000001,
0.785000000000001,0.790000000000001,0.795000000000001,0.800000000000001,
0.805000000000001,0.810000000000001,0.815000000000001,0.820000000000001,
0.825000000000001,0.830000000000001,0.835000000000001,0.840000000000001,
0.845000000000001,0.850000000000001,0.855000000000001,0.860000000000001,
0.865000000000001,0.870000000000001,0.875000000000001,0.880000000000001,
0.885000000000001,0.890000000000001,0.895000000000001,0.900000000000001,
0.905000000000001,0.910000000000001,0.915000000000001,0.920000000000001,
0.925000000000001,0.930000000000001,0.935000000000001,0.940000000000001,
0.945000000000001,0.950000000000001,0.955000000000001,0.960000000000001,
0.965000000000001,0.970000000000001,0.975000000000001,0.980000000000001,
0.985000000000001,0.990000000000001,0.995000000000001,1.),(0.,1.2),
 .UNSPECIFIED.)
GEOMETRIC_REPRESENTATION_ITEM()
RATIONAL_B_SPLINE_SURFACE(((1.,1.),(1.,1.),(1.,1.),(1.,1.),(1.,1.),(1.,
1.),(1.,1.),(1.,1.),(1.,1.),(1.,1.),(1.,1.),(1.,1.),(1.,1.),(1.,1.),(1.,
1.),(1.,1.),(1.,1.),(1.,1.),(1.,1.),(1.,1.),(1.,1.),(1.,1.),(1.,1.),(1.,
1.),(1.,1.),(1.,1.),(1.,1.),(1.,1.),(1.,1.),(1.,1.),(1.,1.),(1.,1.),(1.,
1.),(1.,1.),(1.,1.),(1.,1.),(1.,1.),(1.,1.),(1.,1.),(1.,1.),(1.,1.),(1.,
1.),(1.,1.),(1.,1.),(1.,1.),(1.,1.),(1.,1.),(1.,1.),(1.,1.),(1.,1.),(1.,
1.),(1.,1.),(1.,1.),(1.,1.),(1.,1.),(1.,1.),(1.,1.),(1.,1.),(1.,1.),(1.,
1.),(1.,1.),(1.,1.),(1.,1.),(1.,1.),(1.,1.),(1.,1.),(1.,1.),(1.,1.),(1.,
1.),(1.,1.),(1.,1.),(1.,1.),(1.,1.),(1.,1.),(1.,1.),(1.,1.),(1.,1.),(1.,
1.),(1.,1.),(1.,1.),(1.,1.),(1.,1.),(1.,1.),(1.,1.),(1.,1.),(1.,1.),(1.,
1.),(1.,1.),(1.,1.),(1.,1.),(1.,1.),(1.,1.),(1.,1.),(1.,1.),(1.,1.),(1.,
1.),(1.,1.),(1.,1.),(1.,1.),(1.,1.),(1.,1.),(1.,1.),(1.,1.),(1.,1.),(1.,
1.),(1.,1.),(1.,1.),(1.,1.),(1.,1.),(1.,1.),(1.,1.),(1.,1.),(1.,1.),(1.,
1.),(1.,1.),(1.,1.),(1.,1.),(1.,1.),(1.,1.),(1.,1.),(1.,1.),(1.,1.),(1.,
1.),(1.,1.),(1.,1.),(1.,1.),(1.,1.),(1.,1.),(1.,1.),(1.,1.),(1.,1.),(1.,
1.),(1.,1.),(1.,1.),(1.,1.),(1.,1.),(1.,1.),(1.,1.),(1.,1.),(1.,1.),(1.,
1.),(1.,1.),(1.,1.),(1.,1.),(1.,1.),(1.,1.),(1.,1.),(1.,1.),(1.,1.),(1.,
1.),(1.,1.),(1.,1.),(1.,1.),(1.,1.),(1.,1.),(1.,1.),(1.,1.),(1.,1.),(1.,
1.),(1.,1.),(1.,1.),(1.,1.),(1.,1.),(1.,1.),(1.,1.),(1.,1.),(1.,1.),(1.,
1.),(1.,1.),(1.,1.),(1.,1.),(1.,1.),(1.,1.),(1.,1.),(1.,1.),(1.,1.),(1.,
1.),(1.,1.),(1.,1.),(1.,1.),(1.,1.),(1.,1.),(1.,1.),(1.,1.),(1.,1.),(1.,
1.),(1.,1.),(1.,1.),(1.,1.),(1.,1.),(1.,1.),(1.,1.),(1.,1.),(1.,1.),(1.,
1.),(1.,1.),(1.,1.),(1.,1.),(1.,1.),(1.,1.),(1.,1.),(1.,1.),(1.,1.),(1.,
1.),(1.,1.)))
REPRESENTATION_ITEM('')
SURFACE()
);
#921=(
BOUNDED_SURFACE()
B_SPLINE_SURFACE(5,1,((#86670,#86671),(#86672,#86673),(#86674,#86675),(#86676,
#86677),(#86678,#86679),(#86680,#86681),(#86682,#86683),(#86684,#86685),
(#86686,#86687),(#86688,#86689),(#86690,#86691),(#86692,#86693),(#86694,
#86695),(#86696,#86697),(#86698,#86699),(#86700,#86701),(#86702,#86703),
(#86704,#86705),(#86706,#86707),(#86708,#86709),(#86710,#86711),(#86712,
#86713),(#86714,#86715),(#86716,#86717),(#86718,#86719),(#86720,#86721),
(#86722,#86723),(#86724,#86725),(#86726,#86727),(#86728,#86729),(#86730,
#86731),(#86732,#86733),(#86734,#86735),(#86736,#86737),(#86738,#86739),
(#86740,#86741),(#86742,#86743),(#86744,#86745),(#86746,#86747),(#86748,
#86749),(#86750,#86751),(#86752,#86753),(#86754,#86755),(#86756,#86757),
(#86758,#86759),(#86760,#86761),(#86762,#86763),(#86764,#86765),(#86766,
#86767),(#86768,#86769),(#86770,#86771),(#86772,#86773),(#86774,#86775),
(#86776,#86777),(#86778,#86779),(#86780,#86781),(#86782,#86783),(#86784,
#86785),(#86786,#86787),(#86788,#86789),(#86790,#86791),(#86792,#86793),
(#86794,#86795),(#86796,#86797),(#86798,#86799),(#86800,#86801),(#86802,
#86803),(#86804,#86805),(#86806,#86807),(#86808,#86809),(#86810,#86811),
(#86812,#86813),(#86814,#86815),(#86816,#86817),(#86818,#86819),(#86820,
#86821),(#86822,#86823),(#86824,#86825),(#86826,#86827),(#86828,#86829),
(#86830,#86831),(#86832,#86833),(#86834,#86835),(#86836,#86837),(#86838,
#86839),(#86840,#86841),(#86842,#86843),(#86844,#86845),(#86846,#86847),
(#86848,#86849),(#86850,#86851),(#86852,#86853),(#86854,#86855),(#86856,
#86857),(#86858,#86859),(#86860,#86861),(#86862,#86863),(#86864,#86865),
(#86866,#86867),(#86868,#86869),(#86870,#86871),(#86872,#86873),(#86874,
#86875),(#86876,#86877),(#86878,#86879),(#86880,#86881),(#86882,#86883),
(#86884,#86885),(#86886,#86887),(#86888,#86889),(#86890,#86891),(#86892,
#86893),(#86894,#86895),(#86896,#86897),(#86898,#86899),(#86900,#86901),
(#86902,#86903),(#86904,#86905),(#86906,#86907),(#86908,#86909),(#86910,
#86911),(#86912,#86913),(#86914,#86915),(#86916,#86917),(#86918,#86919),
(#86920,#86921),(#86922,#86923),(#86924,#86925),(#86926,#86927),(#86928,
#86929),(#86930,#86931),(#86932,#86933),(#86934,#86935),(#86936,#86937),
(#86938,#86939),(#86940,#86941),(#86942,#86943),(#86944,#86945),(#86946,
#86947),(#86948,#86949),(#86950,#86951),(#86952,#86953),(#86954,#86955),
(#86956,#86957),(#86958,#86959),(#86960,#86961),(#86962,#86963),(#86964,
#86965),(#86966,#86967),(#86968,#86969),(#86970,#86971),(#86972,#86973),
(#86974,#86975),(#86976,#86977),(#86978,#86979),(#86980,#86981),(#86982,
#86983),(#86984,#86985),(#86986,#86987),(#86988,#86989),(#86990,#86991),
(#86992,#86993),(#86994,#86995),(#86996,#86997),(#86998,#86999),(#87000,
#87001),(#87002,#87003),(#87004,#87005),(#87006,#87007),(#87008,#87009),
(#87010,#87011),(#87012,#87013),(#87014,#87015),(#87016,#87017),(#87018,
#87019),(#87020,#87021),(#87022,#87023),(#87024,#87025),(#87026,#87027),
(#87028,#87029),(#87030,#87031),(#87032,#87033),(#87034,#87035),(#87036,
#87037),(#87038,#87039),(#87040,#87041),(#87042,#87043),(#87044,#87045),
(#87046,#87047),(#87048,#87049),(#87050,#87051),(#87052,#87053),(#87054,
#87055),(#87056,#87057),(#87058,#87059),(#87060,#87061),(#87062,#87063),
(#87064,#87065),(#87066,#87067),(#87068,#87069),(#87070,#87071),(#87072,
#87073),(#87074,#87075),(#87076,#87077),(#87078,#87079)),.UNSPECIFIED.,
 .F.,.F.,.F.)
B_SPLINE_SURFACE_WITH_KNOTS((6,1,1,1,1,1,1,1,1,1,1,1,1,1,1,1,1,1,1,1,1,
1,1,1,1,1,1,1,1,1,1,1,1,1,1,1,1,1,1,1,1,1,1,1,1,1,1,1,1,1,1,1,1,1,1,1,1,
1,1,1,1,1,1,1,1,1,1,1,1,1,1,1,1,1,1,1,1,1,1,1,1,1,1,1,1,1,1,1,1,1,1,1,1,
1,1,1,1,1,1,1,1,1,1,1,1,1,1,1,1,1,1,1,1,1,1,1,1,1,1,1,1,1,1,1,1,1,1,1,1,
1,1,1,1,1,1,1,1,1,1,1,1,1,1,1,1,1,1,1,1,1,1,1,1,1,1,1,1,1,1,1,1,1,1,1,1,
1,1,1,1,1,1,1,1,1,1,1,1,1,1,1,1,1,1,1,1,1,1,1,1,1,1,1,1,1,1,1,1,1,1,1,6),
(2,2),(0.,0.005,0.01,0.015,0.02,0.025,0.03,0.035,0.04,0.045,0.05,0.055,
0.06,0.065,0.07,0.075,0.08,0.085,0.09,0.095,0.1,0.105,0.11,0.115,0.12,0.125,
0.13,0.135,0.14,0.145,0.15,0.155,0.16,0.165,0.17,0.175,0.18,0.185,0.19,
0.195,0.2,0.205,0.21,0.215,0.22,0.225,0.23,0.235,0.24,0.245,0.25,0.255,
0.26,0.265,0.27,0.275,0.28,0.285,0.29,0.295,0.3,0.305,0.31,0.315,0.32,0.325,
0.33,0.335,0.34,0.345,0.35,0.355,0.36,0.365,0.37,0.375,0.38,0.385,0.39,
0.395,0.4,0.405,0.41,0.415,0.42,0.425,0.43,0.435,0.44,0.445,0.45,0.455,
0.46,0.465,0.47,0.475,0.48,0.485,0.49,0.495,0.5,0.505,0.51,0.515,0.52,0.525,
0.53,0.535,0.54,0.545,0.55,0.555,0.56,0.565,0.57,0.575,0.58,0.585,0.59,
0.595,0.6,0.605,0.61,0.615,0.62,0.625,0.63,0.635,0.64,0.645,0.65,0.655,
0.66,0.665,0.67,0.675,0.68,0.685,0.690000000000001,0.695000000000001,0.700000000000001,
0.705000000000001,0.710000000000001,0.715000000000001,0.720000000000001,
0.725000000000001,0.730000000000001,0.735000000000001,0.740000000000001,
0.745000000000001,0.750000000000001,0.755000000000001,0.760000000000001,
0.765000000000001,0.770000000000001,0.775000000000001,0.780000000000001,
0.785000000000001,0.790000000000001,0.795000000000001,0.800000000000001,
0.805000000000001,0.810000000000001,0.815000000000001,0.820000000000001,
0.825000000000001,0.830000000000001,0.835000000000001,0.840000000000001,
0.845000000000001,0.850000000000001,0.855000000000001,0.860000000000001,
0.865000000000001,0.870000000000001,0.875000000000001,0.880000000000001,
0.885000000000001,0.890000000000001,0.895000000000001,0.900000000000001,
0.905000000000001,0.910000000000001,0.915000000000001,0.920000000000001,
0.925000000000001,0.930000000000001,0.935000000000001,0.940000000000001,
0.945000000000001,0.950000000000001,0.955000000000001,0.960000000000001,
0.965000000000001,0.970000000000001,0.975000000000001,0.980000000000001,
0.985000000000001,0.990000000000001,0.995000000000001,1.),(0.,1.2),
 .UNSPECIFIED.)
GEOMETRIC_REPRESENTATION_ITEM()
RATIONAL_B_SPLINE_SURFACE(((1.,1.),(1.,1.),(1.,1.),(1.,1.),(1.,1.),(1.,
1.),(1.,1.),(1.,1.),(1.,1.),(1.,1.),(1.,1.),(1.,1.),(1.,1.),(1.,1.),(1.,
1.),(1.,1.),(1.,1.),(1.,1.),(1.,1.),(1.,1.),(1.,1.),(1.,1.),(1.,1.),(1.,
1.),(1.,1.),(1.,1.),(1.,1.),(1.,1.),(1.,1.),(1.,1.),(1.,1.),(1.,1.),(1.,
1.),(1.,1.),(1.,1.),(1.,1.),(1.,1.),(1.,1.),(1.,1.),(1.,1.),(1.,1.),(1.,
1.),(1.,1.),(1.,1.),(1.,1.),(1.,1.),(1.,1.),(1.,1.),(1.,1.),(1.,1.),(1.,
1.),(1.,1.),(1.,1.),(1.,1.),(1.,1.),(1.,1.),(1.,1.),(1.,1.),(1.,1.),(1.,
1.),(1.,1.),(1.,1.),(1.,1.),(1.,1.),(1.,1.),(1.,1.),(1.,1.),(1.,1.),(1.,
1.),(1.,1.),(1.,1.),(1.,1.),(1.,1.),(1.,1.),(1.,1.),(1.,1.),(1.,1.),(1.,
1.),(1.,1.),(1.,1.),(1.,1.),(1.,1.),(1.,1.),(1.,1.),(1.,1.),(1.,1.),(1.,
1.),(1.,1.),(1.,1.),(1.,1.),(1.,1.),(1.,1.),(1.,1.),(1.,1.),(1.,1.),(1.,
1.),(1.,1.),(1.,1.),(1.,1.),(1.,1.),(1.,1.),(1.,1.),(1.,1.),(1.,1.),(1.,
1.),(1.,1.),(1.,1.),(1.,1.),(1.,1.),(1.,1.),(1.,1.),(1.,1.),(1.,1.),(1.,
1.),(1.,1.),(1.,1.),(1.,1.),(1.,1.),(1.,1.),(1.,1.),(1.,1.),(1.,1.),(1.,
1.),(1.,1.),(1.,1.),(1.,1.),(1.,1.),(1.,1.),(1.,1.),(1.,1.),(1.,1.),(1.,
1.),(1.,1.),(1.,1.),(1.,1.),(1.,1.),(1.,1.),(1.,1.),(1.,1.),(1.,1.),(1.,
1.),(1.,1.),(1.,1.),(1.,1.),(1.,1.),(1.,1.),(1.,1.),(1.,1.),(1.,1.),(1.,
1.),(1.,1.),(1.,1.),(1.,1.),(1.,1.),(1.,1.),(1.,1.),(1.,1.),(1.,1.),(1.,
1.),(1.,1.),(1.,1.),(1.,1.),(1.,1.),(1.,1.),(1.,1.),(1.,1.),(1.,1.),(1.,
1.),(1.,1.),(1.,1.),(1.,1.),(1.,1.),(1.,1.),(1.,1.),(1.,1.),(1.,1.),(1.,
1.),(1.,1.),(1.,1.),(1.,1.),(1.,1.),(1.,1.),(1.,1.),(1.,1.),(1.,1.),(1.,
1.),(1.,1.),(1.,1.),(1.,1.),(1.,1.),(1.,1.),(1.,1.),(1.,1.),(1.,1.),(1.,
1.),(1.,1.),(1.,1.),(1.,1.),(1.,1.),(1.,1.),(1.,1.),(1.,1.),(1.,1.),(1.,
1.),(1.,1.)))
REPRESENTATION_ITEM('')
SURFACE()
);
#922=(
BOUNDED_SURFACE()
B_SPLINE_SURFACE(5,1,((#87566,#87567),(#87568,#87569),(#87570,#87571),(#87572,
#87573),(#87574,#87575),(#87576,#87577),(#87578,#87579),(#87580,#87581),
(#87582,#87583),(#87584,#87585),(#87586,#87587),(#87588,#87589),(#87590,
#87591),(#87592,#87593),(#87594,#87595),(#87596,#87597),(#87598,#87599),
(#87600,#87601),(#87602,#87603),(#87604,#87605),(#87606,#87607),(#87608,
#87609),(#87610,#87611),(#87612,#87613),(#87614,#87615),(#87616,#87617),
(#87618,#87619),(#87620,#87621),(#87622,#87623),(#87624,#87625),(#87626,
#87627),(#87628,#87629),(#87630,#87631),(#87632,#87633),(#87634,#87635),
(#87636,#87637),(#87638,#87639),(#87640,#87641),(#87642,#87643),(#87644,
#87645),(#87646,#87647),(#87648,#87649),(#87650,#87651),(#87652,#87653),
(#87654,#87655),(#87656,#87657),(#87658,#87659),(#87660,#87661),(#87662,
#87663),(#87664,#87665),(#87666,#87667),(#87668,#87669),(#87670,#87671),
(#87672,#87673),(#87674,#87675),(#87676,#87677),(#87678,#87679),(#87680,
#87681),(#87682,#87683),(#87684,#87685),(#87686,#87687),(#87688,#87689),
(#87690,#87691),(#87692,#87693),(#87694,#87695),(#87696,#87697),(#87698,
#87699),(#87700,#87701),(#87702,#87703),(#87704,#87705),(#87706,#87707),
(#87708,#87709),(#87710,#87711),(#87712,#87713),(#87714,#87715),(#87716,
#87717),(#87718,#87719),(#87720,#87721),(#87722,#87723),(#87724,#87725),
(#87726,#87727),(#87728,#87729),(#87730,#87731),(#87732,#87733),(#87734,
#87735),(#87736,#87737),(#87738,#87739),(#87740,#87741),(#87742,#87743),
(#87744,#87745),(#87746,#87747),(#87748,#87749),(#87750,#87751),(#87752,
#87753),(#87754,#87755),(#87756,#87757),(#87758,#87759),(#87760,#87761),
(#87762,#87763),(#87764,#87765),(#87766,#87767),(#87768,#87769),(#87770,
#87771),(#87772,#87773),(#87774,#87775),(#87776,#87777),(#87778,#87779),
(#87780,#87781),(#87782,#87783),(#87784,#87785),(#87786,#87787),(#87788,
#87789),(#87790,#87791),(#87792,#87793),(#87794,#87795),(#87796,#87797),
(#87798,#87799),(#87800,#87801),(#87802,#87803),(#87804,#87805),(#87806,
#87807),(#87808,#87809),(#87810,#87811),(#87812,#87813),(#87814,#87815),
(#87816,#87817),(#87818,#87819),(#87820,#87821),(#87822,#87823),(#87824,
#87825),(#87826,#87827),(#87828,#87829),(#87830,#87831),(#87832,#87833),
(#87834,#87835),(#87836,#87837),(#87838,#87839),(#87840,#87841),(#87842,
#87843),(#87844,#87845),(#87846,#87847),(#87848,#87849),(#87850,#87851),
(#87852,#87853),(#87854,#87855),(#87856,#87857),(#87858,#87859),(#87860,
#87861),(#87862,#87863),(#87864,#87865),(#87866,#87867),(#87868,#87869),
(#87870,#87871),(#87872,#87873),(#87874,#87875),(#87876,#87877),(#87878,
#87879),(#87880,#87881),(#87882,#87883),(#87884,#87885),(#87886,#87887),
(#87888,#87889),(#87890,#87891),(#87892,#87893),(#87894,#87895),(#87896,
#87897),(#87898,#87899),(#87900,#87901),(#87902,#87903),(#87904,#87905),
(#87906,#87907),(#87908,#87909),(#87910,#87911),(#87912,#87913),(#87914,
#87915),(#87916,#87917),(#87918,#87919),(#87920,#87921),(#87922,#87923),
(#87924,#87925),(#87926,#87927),(#87928,#87929),(#87930,#87931),(#87932,
#87933),(#87934,#87935),(#87936,#87937),(#87938,#87939),(#87940,#87941),
(#87942,#87943),(#87944,#87945),(#87946,#87947),(#87948,#87949),(#87950,
#87951),(#87952,#87953),(#87954,#87955),(#87956,#87957),(#87958,#87959),
(#87960,#87961),(#87962,#87963),(#87964,#87965),(#87966,#87967),(#87968,
#87969),(#87970,#87971),(#87972,#87973),(#87974,#87975)),.UNSPECIFIED.,
 .F.,.F.,.F.)
B_SPLINE_SURFACE_WITH_KNOTS((6,1,1,1,1,1,1,1,1,1,1,1,1,1,1,1,1,1,1,1,1,
1,1,1,1,1,1,1,1,1,1,1,1,1,1,1,1,1,1,1,1,1,1,1,1,1,1,1,1,1,1,1,1,1,1,1,1,
1,1,1,1,1,1,1,1,1,1,1,1,1,1,1,1,1,1,1,1,1,1,1,1,1,1,1,1,1,1,1,1,1,1,1,1,
1,1,1,1,1,1,1,1,1,1,1,1,1,1,1,1,1,1,1,1,1,1,1,1,1,1,1,1,1,1,1,1,1,1,1,1,
1,1,1,1,1,1,1,1,1,1,1,1,1,1,1,1,1,1,1,1,1,1,1,1,1,1,1,1,1,1,1,1,1,1,1,1,
1,1,1,1,1,1,1,1,1,1,1,1,1,1,1,1,1,1,1,1,1,1,1,1,1,1,1,1,1,1,1,1,1,1,1,6),
(2,2),(0.,0.005,0.01,0.015,0.02,0.025,0.03,0.035,0.04,0.045,0.05,0.055,
0.06,0.065,0.07,0.075,0.08,0.085,0.09,0.095,0.1,0.105,0.11,0.115,0.12,0.125,
0.13,0.135,0.14,0.145,0.15,0.155,0.16,0.165,0.17,0.175,0.18,0.185,0.19,
0.195,0.2,0.205,0.21,0.215,0.22,0.225,0.23,0.235,0.24,0.245,0.25,0.255,
0.26,0.265,0.27,0.275,0.28,0.285,0.29,0.295,0.3,0.305,0.31,0.315,0.32,0.325,
0.33,0.335,0.34,0.345,0.35,0.355,0.36,0.365,0.37,0.375,0.38,0.385,0.39,
0.395,0.4,0.405,0.41,0.415,0.42,0.425,0.43,0.435,0.44,0.445,0.45,0.455,
0.46,0.465,0.47,0.475,0.48,0.485,0.49,0.495,0.5,0.505,0.51,0.515,0.52,0.525,
0.53,0.535,0.54,0.545,0.55,0.555,0.56,0.565,0.57,0.575,0.58,0.585,0.59,
0.595,0.6,0.605,0.61,0.615,0.62,0.625,0.63,0.635,0.64,0.645,0.65,0.655,
0.66,0.665,0.67,0.675,0.68,0.685,0.690000000000001,0.695000000000001,0.700000000000001,
0.705000000000001,0.710000000000001,0.715000000000001,0.720000000000001,
0.725000000000001,0.730000000000001,0.735000000000001,0.740000000000001,
0.745000000000001,0.750000000000001,0.755000000000001,0.760000000000001,
0.765000000000001,0.770000000000001,0.775000000000001,0.780000000000001,
0.785000000000001,0.790000000000001,0.795000000000001,0.800000000000001,
0.805000000000001,0.810000000000001,0.815000000000001,0.820000000000001,
0.825000000000001,0.830000000000001,0.835000000000001,0.840000000000001,
0.845000000000001,0.850000000000001,0.855000000000001,0.860000000000001,
0.865000000000001,0.870000000000001,0.875000000000001,0.880000000000001,
0.885000000000001,0.890000000000001,0.895000000000001,0.900000000000001,
0.905000000000001,0.910000000000001,0.915000000000001,0.920000000000001,
0.925000000000001,0.930000000000001,0.935000000000001,0.940000000000001,
0.945000000000001,0.950000000000001,0.955000000000001,0.960000000000001,
0.965000000000001,0.970000000000001,0.975000000000001,0.980000000000001,
0.985000000000001,0.990000000000001,0.995000000000001,1.),(0.,1.2),
 .UNSPECIFIED.)
GEOMETRIC_REPRESENTATION_ITEM()
RATIONAL_B_SPLINE_SURFACE(((1.,1.),(1.,1.),(1.,1.),(1.,1.),(1.,1.),(1.,
1.),(1.,1.),(1.,1.),(1.,1.),(1.,1.),(1.,1.),(1.,1.),(1.,1.),(1.,1.),(1.,
1.),(1.,1.),(1.,1.),(1.,1.),(1.,1.),(1.,1.),(1.,1.),(1.,1.),(1.,1.),(1.,
1.),(1.,1.),(1.,1.),(1.,1.),(1.,1.),(1.,1.),(1.,1.),(1.,1.),(1.,1.),(1.,
1.),(1.,1.),(1.,1.),(1.,1.),(1.,1.),(1.,1.),(1.,1.),(1.,1.),(1.,1.),(1.,
1.),(1.,1.),(1.,1.),(1.,1.),(1.,1.),(1.,1.),(1.,1.),(1.,1.),(1.,1.),(1.,
1.),(1.,1.),(1.,1.),(1.,1.),(1.,1.),(1.,1.),(1.,1.),(1.,1.),(1.,1.),(1.,
1.),(1.,1.),(1.,1.),(1.,1.),(1.,1.),(1.,1.),(1.,1.),(1.,1.),(1.,1.),(1.,
1.),(1.,1.),(1.,1.),(1.,1.),(1.,1.),(1.,1.),(1.,1.),(1.,1.),(1.,1.),(1.,
1.),(1.,1.),(1.,1.),(1.,1.),(1.,1.),(1.,1.),(1.,1.),(1.,1.),(1.,1.),(1.,
1.),(1.,1.),(1.,1.),(1.,1.),(1.,1.),(1.,1.),(1.,1.),(1.,1.),(1.,1.),(1.,
1.),(1.,1.),(1.,1.),(1.,1.),(1.,1.),(1.,1.),(1.,1.),(1.,1.),(1.,1.),(1.,
1.),(1.,1.),(1.,1.),(1.,1.),(1.,1.),(1.,1.),(1.,1.),(1.,1.),(1.,1.),(1.,
1.),(1.,1.),(1.,1.),(1.,1.),(1.,1.),(1.,1.),(1.,1.),(1.,1.),(1.,1.),(1.,
1.),(1.,1.),(1.,1.),(1.,1.),(1.,1.),(1.,1.),(1.,1.),(1.,1.),(1.,1.),(1.,
1.),(1.,1.),(1.,1.),(1.,1.),(1.,1.),(1.,1.),(1.,1.),(1.,1.),(1.,1.),(1.,
1.),(1.,1.),(1.,1.),(1.,1.),(1.,1.),(1.,1.),(1.,1.),(1.,1.),(1.,1.),(1.,
1.),(1.,1.),(1.,1.),(1.,1.),(1.,1.),(1.,1.),(1.,1.),(1.,1.),(1.,1.),(1.,
1.),(1.,1.),(1.,1.),(1.,1.),(1.,1.),(1.,1.),(1.,1.),(1.,1.),(1.,1.),(1.,
1.),(1.,1.),(1.,1.),(1.,1.),(1.,1.),(1.,1.),(1.,1.),(1.,1.),(1.,1.),(1.,
1.),(1.,1.),(1.,1.),(1.,1.),(1.,1.),(1.,1.),(1.,1.),(1.,1.),(1.,1.),(1.,
1.),(1.,1.),(1.,1.),(1.,1.),(1.,1.),(1.,1.),(1.,1.),(1.,1.),(1.,1.),(1.,
1.),(1.,1.),(1.,1.),(1.,1.),(1.,1.),(1.,1.),(1.,1.),(1.,1.),(1.,1.),(1.,
1.),(1.,1.)))
REPRESENTATION_ITEM('')
SURFACE()
);
#923=(
BOUNDED_SURFACE()
B_SPLINE_SURFACE(5,1,((#88462,#88463),(#88464,#88465),(#88466,#88467),(#88468,
#88469),(#88470,#88471),(#88472,#88473),(#88474,#88475),(#88476,#88477),
(#88478,#88479),(#88480,#88481),(#88482,#88483),(#88484,#88485),(#88486,
#88487),(#88488,#88489),(#88490,#88491),(#88492,#88493),(#88494,#88495),
(#88496,#88497),(#88498,#88499),(#88500,#88501),(#88502,#88503),(#88504,
#88505),(#88506,#88507),(#88508,#88509),(#88510,#88511),(#88512,#88513),
(#88514,#88515),(#88516,#88517),(#88518,#88519),(#88520,#88521),(#88522,
#88523),(#88524,#88525),(#88526,#88527),(#88528,#88529),(#88530,#88531),
(#88532,#88533),(#88534,#88535),(#88536,#88537),(#88538,#88539),(#88540,
#88541),(#88542,#88543),(#88544,#88545),(#88546,#88547),(#88548,#88549),
(#88550,#88551),(#88552,#88553),(#88554,#88555),(#88556,#88557),(#88558,
#88559),(#88560,#88561),(#88562,#88563),(#88564,#88565),(#88566,#88567),
(#88568,#88569),(#88570,#88571),(#88572,#88573),(#88574,#88575),(#88576,
#88577),(#88578,#88579),(#88580,#88581),(#88582,#88583),(#88584,#88585),
(#88586,#88587),(#88588,#88589),(#88590,#88591),(#88592,#88593),(#88594,
#88595),(#88596,#88597),(#88598,#88599),(#88600,#88601),(#88602,#88603),
(#88604,#88605),(#88606,#88607),(#88608,#88609),(#88610,#88611),(#88612,
#88613),(#88614,#88615),(#88616,#88617),(#88618,#88619),(#88620,#88621),
(#88622,#88623),(#88624,#88625),(#88626,#88627),(#88628,#88629),(#88630,
#88631),(#88632,#88633),(#88634,#88635),(#88636,#88637),(#88638,#88639),
(#88640,#88641),(#88642,#88643),(#88644,#88645),(#88646,#88647),(#88648,
#88649),(#88650,#88651),(#88652,#88653),(#88654,#88655),(#88656,#88657),
(#88658,#88659),(#88660,#88661),(#88662,#88663),(#88664,#88665),(#88666,
#88667),(#88668,#88669),(#88670,#88671),(#88672,#88673),(#88674,#88675),
(#88676,#88677),(#88678,#88679),(#88680,#88681),(#88682,#88683),(#88684,
#88685),(#88686,#88687),(#88688,#88689),(#88690,#88691),(#88692,#88693),
(#88694,#88695),(#88696,#88697),(#88698,#88699),(#88700,#88701),(#88702,
#88703),(#88704,#88705),(#88706,#88707),(#88708,#88709),(#88710,#88711),
(#88712,#88713),(#88714,#88715),(#88716,#88717),(#88718,#88719),(#88720,
#88721),(#88722,#88723),(#88724,#88725),(#88726,#88727),(#88728,#88729),
(#88730,#88731),(#88732,#88733),(#88734,#88735),(#88736,#88737),(#88738,
#88739),(#88740,#88741),(#88742,#88743),(#88744,#88745),(#88746,#88747),
(#88748,#88749),(#88750,#88751),(#88752,#88753),(#88754,#88755),(#88756,
#88757),(#88758,#88759),(#88760,#88761),(#88762,#88763),(#88764,#88765),
(#88766,#88767),(#88768,#88769),(#88770,#88771),(#88772,#88773),(#88774,
#88775),(#88776,#88777),(#88778,#88779),(#88780,#88781),(#88782,#88783),
(#88784,#88785),(#88786,#88787),(#88788,#88789),(#88790,#88791),(#88792,
#88793),(#88794,#88795),(#88796,#88797),(#88798,#88799),(#88800,#88801),
(#88802,#88803),(#88804,#88805),(#88806,#88807),(#88808,#88809),(#88810,
#88811),(#88812,#88813),(#88814,#88815),(#88816,#88817),(#88818,#88819),
(#88820,#88821),(#88822,#88823),(#88824,#88825),(#88826,#88827),(#88828,
#88829),(#88830,#88831),(#88832,#88833),(#88834,#88835),(#88836,#88837),
(#88838,#88839),(#88840,#88841),(#88842,#88843),(#88844,#88845),(#88846,
#88847),(#88848,#88849),(#88850,#88851),(#88852,#88853),(#88854,#88855),
(#88856,#88857),(#88858,#88859),(#88860,#88861),(#88862,#88863),(#88864,
#88865),(#88866,#88867),(#88868,#88869),(#88870,#88871)),.UNSPECIFIED.,
 .F.,.F.,.F.)
B_SPLINE_SURFACE_WITH_KNOTS((6,1,1,1,1,1,1,1,1,1,1,1,1,1,1,1,1,1,1,1,1,
1,1,1,1,1,1,1,1,1,1,1,1,1,1,1,1,1,1,1,1,1,1,1,1,1,1,1,1,1,1,1,1,1,1,1,1,
1,1,1,1,1,1,1,1,1,1,1,1,1,1,1,1,1,1,1,1,1,1,1,1,1,1,1,1,1,1,1,1,1,1,1,1,
1,1,1,1,1,1,1,1,1,1,1,1,1,1,1,1,1,1,1,1,1,1,1,1,1,1,1,1,1,1,1,1,1,1,1,1,
1,1,1,1,1,1,1,1,1,1,1,1,1,1,1,1,1,1,1,1,1,1,1,1,1,1,1,1,1,1,1,1,1,1,1,1,
1,1,1,1,1,1,1,1,1,1,1,1,1,1,1,1,1,1,1,1,1,1,1,1,1,1,1,1,1,1,1,1,1,1,1,6),
(2,2),(0.,0.005,0.01,0.015,0.02,0.025,0.03,0.035,0.04,0.045,0.05,0.055,
0.06,0.065,0.07,0.075,0.08,0.085,0.09,0.095,0.1,0.105,0.11,0.115,0.12,0.125,
0.13,0.135,0.14,0.145,0.15,0.155,0.16,0.165,0.17,0.175,0.18,0.185,0.19,
0.195,0.2,0.205,0.21,0.215,0.22,0.225,0.23,0.235,0.24,0.245,0.25,0.255,
0.26,0.265,0.27,0.275,0.28,0.285,0.29,0.295,0.3,0.305,0.31,0.315,0.32,0.325,
0.33,0.335,0.34,0.345,0.35,0.355,0.36,0.365,0.37,0.375,0.38,0.385,0.39,
0.395,0.4,0.405,0.41,0.415,0.42,0.425,0.43,0.435,0.44,0.445,0.45,0.455,
0.46,0.465,0.47,0.475,0.48,0.485,0.49,0.495,0.5,0.505,0.51,0.515,0.52,0.525,
0.53,0.535,0.54,0.545,0.55,0.555,0.56,0.565,0.57,0.575,0.58,0.585,0.59,
0.595,0.6,0.605,0.61,0.615,0.62,0.625,0.63,0.635,0.64,0.645,0.65,0.655,
0.66,0.665,0.67,0.675,0.68,0.685,0.690000000000001,0.695000000000001,0.700000000000001,
0.705000000000001,0.710000000000001,0.715000000000001,0.720000000000001,
0.725000000000001,0.730000000000001,0.735000000000001,0.740000000000001,
0.745000000000001,0.750000000000001,0.755000000000001,0.760000000000001,
0.765000000000001,0.770000000000001,0.775000000000001,0.780000000000001,
0.785000000000001,0.790000000000001,0.795000000000001,0.800000000000001,
0.805000000000001,0.810000000000001,0.815000000000001,0.820000000000001,
0.825000000000001,0.830000000000001,0.835000000000001,0.840000000000001,
0.845000000000001,0.850000000000001,0.855000000000001,0.860000000000001,
0.865000000000001,0.870000000000001,0.875000000000001,0.880000000000001,
0.885000000000001,0.890000000000001,0.895000000000001,0.900000000000001,
0.905000000000001,0.910000000000001,0.915000000000001,0.920000000000001,
0.925000000000001,0.930000000000001,0.935000000000001,0.940000000000001,
0.945000000000001,0.950000000000001,0.955000000000001,0.960000000000001,
0.965000000000001,0.970000000000001,0.975000000000001,0.980000000000001,
0.985000000000001,0.990000000000001,0.995000000000001,1.),(0.,1.2),
 .UNSPECIFIED.)
GEOMETRIC_REPRESENTATION_ITEM()
RATIONAL_B_SPLINE_SURFACE(((1.,1.),(1.,1.),(1.,1.),(1.,1.),(1.,1.),(1.,
1.),(1.,1.),(1.,1.),(1.,1.),(1.,1.),(1.,1.),(1.,1.),(1.,1.),(1.,1.),(1.,
1.),(1.,1.),(1.,1.),(1.,1.),(1.,1.),(1.,1.),(1.,1.),(1.,1.),(1.,1.),(1.,
1.),(1.,1.),(1.,1.),(1.,1.),(1.,1.),(1.,1.),(1.,1.),(1.,1.),(1.,1.),(1.,
1.),(1.,1.),(1.,1.),(1.,1.),(1.,1.),(1.,1.),(1.,1.),(1.,1.),(1.,1.),(1.,
1.),(1.,1.),(1.,1.),(1.,1.),(1.,1.),(1.,1.),(1.,1.),(1.,1.),(1.,1.),(1.,
1.),(1.,1.),(1.,1.),(1.,1.),(1.,1.),(1.,1.),(1.,1.),(1.,1.),(1.,1.),(1.,
1.),(1.,1.),(1.,1.),(1.,1.),(1.,1.),(1.,1.),(1.,1.),(1.,1.),(1.,1.),(1.,
1.),(1.,1.),(1.,1.),(1.,1.),(1.,1.),(1.,1.),(1.,1.),(1.,1.),(1.,1.),(1.,
1.),(1.,1.),(1.,1.),(1.,1.),(1.,1.),(1.,1.),(1.,1.),(1.,1.),(1.,1.),(1.,
1.),(1.,1.),(1.,1.),(1.,1.),(1.,1.),(1.,1.),(1.,1.),(1.,1.),(1.,1.),(1.,
1.),(1.,1.),(1.,1.),(1.,1.),(1.,1.),(1.,1.),(1.,1.),(1.,1.),(1.,1.),(1.,
1.),(1.,1.),(1.,1.),(1.,1.),(1.,1.),(1.,1.),(1.,1.),(1.,1.),(1.,1.),(1.,
1.),(1.,1.),(1.,1.),(1.,1.),(1.,1.),(1.,1.),(1.,1.),(1.,1.),(1.,1.),(1.,
1.),(1.,1.),(1.,1.),(1.,1.),(1.,1.),(1.,1.),(1.,1.),(1.,1.),(1.,1.),(1.,
1.),(1.,1.),(1.,1.),(1.,1.),(1.,1.),(1.,1.),(1.,1.),(1.,1.),(1.,1.),(1.,
1.),(1.,1.),(1.,1.),(1.,1.),(1.,1.),(1.,1.),(1.,1.),(1.,1.),(1.,1.),(1.,
1.),(1.,1.),(1.,1.),(1.,1.),(1.,1.),(1.,1.),(1.,1.),(1.,1.),(1.,1.),(1.,
1.),(1.,1.),(1.,1.),(1.,1.),(1.,1.),(1.,1.),(1.,1.),(1.,1.),(1.,1.),(1.,
1.),(1.,1.),(1.,1.),(1.,1.),(1.,1.),(1.,1.),(1.,1.),(1.,1.),(1.,1.),(1.,
1.),(1.,1.),(1.,1.),(1.,1.),(1.,1.),(1.,1.),(1.,1.),(1.,1.),(1.,1.),(1.,
1.),(1.,1.),(1.,1.),(1.,1.),(1.,1.),(1.,1.),(1.,1.),(1.,1.),(1.,1.),(1.,
1.),(1.,1.),(1.,1.),(1.,1.),(1.,1.),(1.,1.),(1.,1.),(1.,1.),(1.,1.),(1.,
1.),(1.,1.)))
REPRESENTATION_ITEM('')
SURFACE()
);
#924=(
BOUNDED_SURFACE()
B_SPLINE_SURFACE(5,1,((#89358,#89359),(#89360,#89361),(#89362,#89363),(#89364,
#89365),(#89366,#89367),(#89368,#89369),(#89370,#89371),(#89372,#89373),
(#89374,#89375),(#89376,#89377),(#89378,#89379),(#89380,#89381),(#89382,
#89383),(#89384,#89385),(#89386,#89387),(#89388,#89389),(#89390,#89391),
(#89392,#89393),(#89394,#89395),(#89396,#89397),(#89398,#89399),(#89400,
#89401),(#89402,#89403),(#89404,#89405),(#89406,#89407),(#89408,#89409),
(#89410,#89411),(#89412,#89413),(#89414,#89415),(#89416,#89417),(#89418,
#89419),(#89420,#89421),(#89422,#89423),(#89424,#89425),(#89426,#89427),
(#89428,#89429),(#89430,#89431),(#89432,#89433),(#89434,#89435),(#89436,
#89437),(#89438,#89439),(#89440,#89441),(#89442,#89443),(#89444,#89445),
(#89446,#89447),(#89448,#89449),(#89450,#89451),(#89452,#89453),(#89454,
#89455),(#89456,#89457),(#89458,#89459),(#89460,#89461),(#89462,#89463),
(#89464,#89465),(#89466,#89467),(#89468,#89469),(#89470,#89471),(#89472,
#89473),(#89474,#89475),(#89476,#89477),(#89478,#89479),(#89480,#89481),
(#89482,#89483),(#89484,#89485),(#89486,#89487),(#89488,#89489),(#89490,
#89491),(#89492,#89493),(#89494,#89495),(#89496,#89497),(#89498,#89499),
(#89500,#89501),(#89502,#89503),(#89504,#89505),(#89506,#89507),(#89508,
#89509),(#89510,#89511),(#89512,#89513),(#89514,#89515),(#89516,#89517),
(#89518,#89519),(#89520,#89521),(#89522,#89523),(#89524,#89525),(#89526,
#89527),(#89528,#89529),(#89530,#89531),(#89532,#89533),(#89534,#89535),
(#89536,#89537),(#89538,#89539),(#89540,#89541),(#89542,#89543),(#89544,
#89545),(#89546,#89547),(#89548,#89549),(#89550,#89551),(#89552,#89553),
(#89554,#89555),(#89556,#89557),(#89558,#89559),(#89560,#89561),(#89562,
#89563),(#89564,#89565),(#89566,#89567),(#89568,#89569),(#89570,#89571),
(#89572,#89573),(#89574,#89575),(#89576,#89577),(#89578,#89579),(#89580,
#89581),(#89582,#89583),(#89584,#89585),(#89586,#89587),(#89588,#89589),
(#89590,#89591),(#89592,#89593),(#89594,#89595),(#89596,#89597),(#89598,
#89599),(#89600,#89601),(#89602,#89603),(#89604,#89605),(#89606,#89607),
(#89608,#89609),(#89610,#89611),(#89612,#89613),(#89614,#89615),(#89616,
#89617),(#89618,#89619),(#89620,#89621),(#89622,#89623),(#89624,#89625),
(#89626,#89627),(#89628,#89629),(#89630,#89631),(#89632,#89633),(#89634,
#89635),(#89636,#89637),(#89638,#89639),(#89640,#89641),(#89642,#89643),
(#89644,#89645),(#89646,#89647),(#89648,#89649),(#89650,#89651),(#89652,
#89653),(#89654,#89655),(#89656,#89657),(#89658,#89659),(#89660,#89661),
(#89662,#89663),(#89664,#89665),(#89666,#89667),(#89668,#89669),(#89670,
#89671),(#89672,#89673),(#89674,#89675),(#89676,#89677),(#89678,#89679),
(#89680,#89681),(#89682,#89683),(#89684,#89685),(#89686,#89687),(#89688,
#89689),(#89690,#89691),(#89692,#89693),(#89694,#89695),(#89696,#89697),
(#89698,#89699),(#89700,#89701),(#89702,#89703),(#89704,#89705),(#89706,
#89707),(#89708,#89709),(#89710,#89711),(#89712,#89713),(#89714,#89715),
(#89716,#89717),(#89718,#89719),(#89720,#89721),(#89722,#89723),(#89724,
#89725),(#89726,#89727),(#89728,#89729),(#89730,#89731),(#89732,#89733),
(#89734,#89735),(#89736,#89737),(#89738,#89739),(#89740,#89741),(#89742,
#89743),(#89744,#89745),(#89746,#89747),(#89748,#89749),(#89750,#89751),
(#89752,#89753),(#89754,#89755),(#89756,#89757),(#89758,#89759),(#89760,
#89761),(#89762,#89763),(#89764,#89765),(#89766,#89767)),.UNSPECIFIED.,
 .F.,.F.,.F.)
B_SPLINE_SURFACE_WITH_KNOTS((6,1,1,1,1,1,1,1,1,1,1,1,1,1,1,1,1,1,1,1,1,
1,1,1,1,1,1,1,1,1,1,1,1,1,1,1,1,1,1,1,1,1,1,1,1,1,1,1,1,1,1,1,1,1,1,1,1,
1,1,1,1,1,1,1,1,1,1,1,1,1,1,1,1,1,1,1,1,1,1,1,1,1,1,1,1,1,1,1,1,1,1,1,1,
1,1,1,1,1,1,1,1,1,1,1,1,1,1,1,1,1,1,1,1,1,1,1,1,1,1,1,1,1,1,1,1,1,1,1,1,
1,1,1,1,1,1,1,1,1,1,1,1,1,1,1,1,1,1,1,1,1,1,1,1,1,1,1,1,1,1,1,1,1,1,1,1,
1,1,1,1,1,1,1,1,1,1,1,1,1,1,1,1,1,1,1,1,1,1,1,1,1,1,1,1,1,1,1,1,1,1,1,6),
(2,2),(0.,0.005,0.01,0.015,0.02,0.025,0.03,0.035,0.04,0.045,0.05,0.055,
0.06,0.065,0.07,0.075,0.08,0.085,0.09,0.095,0.1,0.105,0.11,0.115,0.12,0.125,
0.13,0.135,0.14,0.145,0.15,0.155,0.16,0.165,0.17,0.175,0.18,0.185,0.19,
0.195,0.2,0.205,0.21,0.215,0.22,0.225,0.23,0.235,0.24,0.245,0.25,0.255,
0.26,0.265,0.27,0.275,0.28,0.285,0.29,0.295,0.3,0.305,0.31,0.315,0.32,0.325,
0.33,0.335,0.34,0.345,0.35,0.355,0.36,0.365,0.37,0.375,0.38,0.385,0.39,
0.395,0.4,0.405,0.41,0.415,0.42,0.425,0.43,0.435,0.44,0.445,0.45,0.455,
0.46,0.465,0.47,0.475,0.48,0.485,0.49,0.495,0.5,0.505,0.51,0.515,0.52,0.525,
0.53,0.535,0.54,0.545,0.55,0.555,0.56,0.565,0.57,0.575,0.58,0.585,0.59,
0.595,0.6,0.605,0.61,0.615,0.62,0.625,0.63,0.635,0.64,0.645,0.65,0.655,
0.66,0.665,0.67,0.675,0.68,0.685,0.690000000000001,0.695000000000001,0.700000000000001,
0.705000000000001,0.710000000000001,0.715000000000001,0.720000000000001,
0.725000000000001,0.730000000000001,0.735000000000001,0.740000000000001,
0.745000000000001,0.750000000000001,0.755000000000001,0.760000000000001,
0.765000000000001,0.770000000000001,0.775000000000001,0.780000000000001,
0.785000000000001,0.790000000000001,0.795000000000001,0.800000000000001,
0.805000000000001,0.810000000000001,0.815000000000001,0.820000000000001,
0.825000000000001,0.830000000000001,0.835000000000001,0.840000000000001,
0.845000000000001,0.850000000000001,0.855000000000001,0.860000000000001,
0.865000000000001,0.870000000000001,0.875000000000001,0.880000000000001,
0.885000000000001,0.890000000000001,0.895000000000001,0.900000000000001,
0.905000000000001,0.910000000000001,0.915000000000001,0.920000000000001,
0.925000000000001,0.930000000000001,0.935000000000001,0.940000000000001,
0.945000000000001,0.950000000000001,0.955000000000001,0.960000000000001,
0.965000000000001,0.970000000000001,0.975000000000001,0.980000000000001,
0.985000000000001,0.990000000000001,0.995000000000001,1.),(0.,1.2),
 .UNSPECIFIED.)
GEOMETRIC_REPRESENTATION_ITEM()
RATIONAL_B_SPLINE_SURFACE(((1.,1.),(1.,1.),(1.,1.),(1.,1.),(1.,1.),(1.,
1.),(1.,1.),(1.,1.),(1.,1.),(1.,1.),(1.,1.),(1.,1.),(1.,1.),(1.,1.),(1.,
1.),(1.,1.),(1.,1.),(1.,1.),(1.,1.),(1.,1.),(1.,1.),(1.,1.),(1.,1.),(1.,
1.),(1.,1.),(1.,1.),(1.,1.),(1.,1.),(1.,1.),(1.,1.),(1.,1.),(1.,1.),(1.,
1.),(1.,1.),(1.,1.),(1.,1.),(1.,1.),(1.,1.),(1.,1.),(1.,1.),(1.,1.),(1.,
1.),(1.,1.),(1.,1.),(1.,1.),(1.,1.),(1.,1.),(1.,1.),(1.,1.),(1.,1.),(1.,
1.),(1.,1.),(1.,1.),(1.,1.),(1.,1.),(1.,1.),(1.,1.),(1.,1.),(1.,1.),(1.,
1.),(1.,1.),(1.,1.),(1.,1.),(1.,1.),(1.,1.),(1.,1.),(1.,1.),(1.,1.),(1.,
1.),(1.,1.),(1.,1.),(1.,1.),(1.,1.),(1.,1.),(1.,1.),(1.,1.),(1.,1.),(1.,
1.),(1.,1.),(1.,1.),(1.,1.),(1.,1.),(1.,1.),(1.,1.),(1.,1.),(1.,1.),(1.,
1.),(1.,1.),(1.,1.),(1.,1.),(1.,1.),(1.,1.),(1.,1.),(1.,1.),(1.,1.),(1.,
1.),(1.,1.),(1.,1.),(1.,1.),(1.,1.),(1.,1.),(1.,1.),(1.,1.),(1.,1.),(1.,
1.),(1.,1.),(1.,1.),(1.,1.),(1.,1.),(1.,1.),(1.,1.),(1.,1.),(1.,1.),(1.,
1.),(1.,1.),(1.,1.),(1.,1.),(1.,1.),(1.,1.),(1.,1.),(1.,1.),(1.,1.),(1.,
1.),(1.,1.),(1.,1.),(1.,1.),(1.,1.),(1.,1.),(1.,1.),(1.,1.),(1.,1.),(1.,
1.),(1.,1.),(1.,1.),(1.,1.),(1.,1.),(1.,1.),(1.,1.),(1.,1.),(1.,1.),(1.,
1.),(1.,1.),(1.,1.),(1.,1.),(1.,1.),(1.,1.),(1.,1.),(1.,1.),(1.,1.),(1.,
1.),(1.,1.),(1.,1.),(1.,1.),(1.,1.),(1.,1.),(1.,1.),(1.,1.),(1.,1.),(1.,
1.),(1.,1.),(1.,1.),(1.,1.),(1.,1.),(1.,1.),(1.,1.),(1.,1.),(1.,1.),(1.,
1.),(1.,1.),(1.,1.),(1.,1.),(1.,1.),(1.,1.),(1.,1.),(1.,1.),(1.,1.),(1.,
1.),(1.,1.),(1.,1.),(1.,1.),(1.,1.),(1.,1.),(1.,1.),(1.,1.),(1.,1.),(1.,
1.),(1.,1.),(1.,1.),(1.,1.),(1.,1.),(1.,1.),(1.,1.),(1.,1.),(1.,1.),(1.,
1.),(1.,1.),(1.,1.),(1.,1.),(1.,1.),(1.,1.),(1.,1.),(1.,1.),(1.,1.),(1.,
1.),(1.,1.)))
REPRESENTATION_ITEM('')
SURFACE()
);
#925=(
BOUNDED_SURFACE()
B_SPLINE_SURFACE(5,1,((#90254,#90255),(#90256,#90257),(#90258,#90259),(#90260,
#90261),(#90262,#90263),(#90264,#90265),(#90266,#90267),(#90268,#90269),
(#90270,#90271),(#90272,#90273),(#90274,#90275),(#90276,#90277),(#90278,
#90279),(#90280,#90281),(#90282,#90283),(#90284,#90285),(#90286,#90287),
(#90288,#90289),(#90290,#90291),(#90292,#90293),(#90294,#90295),(#90296,
#90297),(#90298,#90299),(#90300,#90301),(#90302,#90303),(#90304,#90305),
(#90306,#90307),(#90308,#90309),(#90310,#90311),(#90312,#90313),(#90314,
#90315),(#90316,#90317),(#90318,#90319),(#90320,#90321),(#90322,#90323),
(#90324,#90325),(#90326,#90327),(#90328,#90329),(#90330,#90331),(#90332,
#90333),(#90334,#90335),(#90336,#90337),(#90338,#90339),(#90340,#90341),
(#90342,#90343),(#90344,#90345),(#90346,#90347),(#90348,#90349),(#90350,
#90351),(#90352,#90353),(#90354,#90355),(#90356,#90357),(#90358,#90359),
(#90360,#90361),(#90362,#90363),(#90364,#90365),(#90366,#90367),(#90368,
#90369),(#90370,#90371),(#90372,#90373),(#90374,#90375),(#90376,#90377),
(#90378,#90379),(#90380,#90381),(#90382,#90383),(#90384,#90385),(#90386,
#90387),(#90388,#90389),(#90390,#90391),(#90392,#90393),(#90394,#90395),
(#90396,#90397),(#90398,#90399),(#90400,#90401),(#90402,#90403),(#90404,
#90405),(#90406,#90407),(#90408,#90409),(#90410,#90411),(#90412,#90413),
(#90414,#90415),(#90416,#90417),(#90418,#90419),(#90420,#90421),(#90422,
#90423),(#90424,#90425),(#90426,#90427),(#90428,#90429),(#90430,#90431),
(#90432,#90433),(#90434,#90435),(#90436,#90437),(#90438,#90439),(#90440,
#90441),(#90442,#90443),(#90444,#90445),(#90446,#90447),(#90448,#90449),
(#90450,#90451),(#90452,#90453),(#90454,#90455),(#90456,#90457),(#90458,
#90459),(#90460,#90461),(#90462,#90463),(#90464,#90465),(#90466,#90467),
(#90468,#90469),(#90470,#90471),(#90472,#90473),(#90474,#90475),(#90476,
#90477),(#90478,#90479),(#90480,#90481),(#90482,#90483),(#90484,#90485),
(#90486,#90487),(#90488,#90489),(#90490,#90491),(#90492,#90493),(#90494,
#90495),(#90496,#90497),(#90498,#90499),(#90500,#90501),(#90502,#90503),
(#90504,#90505),(#90506,#90507),(#90508,#90509),(#90510,#90511),(#90512,
#90513),(#90514,#90515),(#90516,#90517),(#90518,#90519),(#90520,#90521),
(#90522,#90523),(#90524,#90525),(#90526,#90527),(#90528,#90529),(#90530,
#90531),(#90532,#90533),(#90534,#90535),(#90536,#90537),(#90538,#90539),
(#90540,#90541),(#90542,#90543),(#90544,#90545),(#90546,#90547),(#90548,
#90549),(#90550,#90551),(#90552,#90553),(#90554,#90555),(#90556,#90557),
(#90558,#90559),(#90560,#90561),(#90562,#90563),(#90564,#90565),(#90566,
#90567),(#90568,#90569),(#90570,#90571),(#90572,#90573),(#90574,#90575),
(#90576,#90577),(#90578,#90579),(#90580,#90581),(#90582,#90583),(#90584,
#90585),(#90586,#90587),(#90588,#90589),(#90590,#90591),(#90592,#90593),
(#90594,#90595),(#90596,#90597),(#90598,#90599),(#90600,#90601),(#90602,
#90603),(#90604,#90605),(#90606,#90607),(#90608,#90609),(#90610,#90611),
(#90612,#90613),(#90614,#90615),(#90616,#90617),(#90618,#90619),(#90620,
#90621),(#90622,#90623),(#90624,#90625),(#90626,#90627),(#90628,#90629),
(#90630,#90631),(#90632,#90633),(#90634,#90635),(#90636,#90637),(#90638,
#90639),(#90640,#90641),(#90642,#90643),(#90644,#90645),(#90646,#90647),
(#90648,#90649),(#90650,#90651),(#90652,#90653),(#90654,#90655),(#90656,
#90657),(#90658,#90659),(#90660,#90661),(#90662,#90663)),.UNSPECIFIED.,
 .F.,.F.,.F.)
B_SPLINE_SURFACE_WITH_KNOTS((6,1,1,1,1,1,1,1,1,1,1,1,1,1,1,1,1,1,1,1,1,
1,1,1,1,1,1,1,1,1,1,1,1,1,1,1,1,1,1,1,1,1,1,1,1,1,1,1,1,1,1,1,1,1,1,1,1,
1,1,1,1,1,1,1,1,1,1,1,1,1,1,1,1,1,1,1,1,1,1,1,1,1,1,1,1,1,1,1,1,1,1,1,1,
1,1,1,1,1,1,1,1,1,1,1,1,1,1,1,1,1,1,1,1,1,1,1,1,1,1,1,1,1,1,1,1,1,1,1,1,
1,1,1,1,1,1,1,1,1,1,1,1,1,1,1,1,1,1,1,1,1,1,1,1,1,1,1,1,1,1,1,1,1,1,1,1,
1,1,1,1,1,1,1,1,1,1,1,1,1,1,1,1,1,1,1,1,1,1,1,1,1,1,1,1,1,1,1,1,1,1,1,6),
(2,2),(0.,0.005,0.01,0.015,0.02,0.025,0.03,0.035,0.04,0.045,0.05,0.055,
0.06,0.065,0.07,0.075,0.08,0.085,0.09,0.095,0.1,0.105,0.11,0.115,0.12,0.125,
0.13,0.135,0.14,0.145,0.15,0.155,0.16,0.165,0.17,0.175,0.18,0.185,0.19,
0.195,0.2,0.205,0.21,0.215,0.22,0.225,0.23,0.235,0.24,0.245,0.25,0.255,
0.26,0.265,0.27,0.275,0.28,0.285,0.29,0.295,0.3,0.305,0.31,0.315,0.32,0.325,
0.33,0.335,0.34,0.345,0.35,0.355,0.36,0.365,0.37,0.375,0.38,0.385,0.39,
0.395,0.4,0.405,0.41,0.415,0.42,0.425,0.43,0.435,0.44,0.445,0.45,0.455,
0.46,0.465,0.47,0.475,0.48,0.485,0.49,0.495,0.5,0.505,0.51,0.515,0.52,0.525,
0.53,0.535,0.54,0.545,0.55,0.555,0.56,0.565,0.57,0.575,0.58,0.585,0.59,
0.595,0.6,0.605,0.61,0.615,0.62,0.625,0.63,0.635,0.64,0.645,0.65,0.655,
0.66,0.665,0.67,0.675,0.68,0.685,0.690000000000001,0.695000000000001,0.700000000000001,
0.705000000000001,0.710000000000001,0.715000000000001,0.720000000000001,
0.725000000000001,0.730000000000001,0.735000000000001,0.740000000000001,
0.745000000000001,0.750000000000001,0.755000000000001,0.760000000000001,
0.765000000000001,0.770000000000001,0.775000000000001,0.780000000000001,
0.785000000000001,0.790000000000001,0.795000000000001,0.800000000000001,
0.805000000000001,0.810000000000001,0.815000000000001,0.820000000000001,
0.825000000000001,0.830000000000001,0.835000000000001,0.840000000000001,
0.845000000000001,0.850000000000001,0.855000000000001,0.860000000000001,
0.865000000000001,0.870000000000001,0.875000000000001,0.880000000000001,
0.885000000000001,0.890000000000001,0.895000000000001,0.900000000000001,
0.905000000000001,0.910000000000001,0.915000000000001,0.920000000000001,
0.925000000000001,0.930000000000001,0.935000000000001,0.940000000000001,
0.945000000000001,0.950000000000001,0.955000000000001,0.960000000000001,
0.965000000000001,0.970000000000001,0.975000000000001,0.980000000000001,
0.985000000000001,0.990000000000001,0.995000000000001,1.),(0.,1.2),
 .UNSPECIFIED.)
GEOMETRIC_REPRESENTATION_ITEM()
RATIONAL_B_SPLINE_SURFACE(((1.,1.),(1.,1.),(1.,1.),(1.,1.),(1.,1.),(1.,
1.),(1.,1.),(1.,1.),(1.,1.),(1.,1.),(1.,1.),(1.,1.),(1.,1.),(1.,1.),(1.,
1.),(1.,1.),(1.,1.),(1.,1.),(1.,1.),(1.,1.),(1.,1.),(1.,1.),(1.,1.),(1.,
1.),(1.,1.),(1.,1.),(1.,1.),(1.,1.),(1.,1.),(1.,1.),(1.,1.),(1.,1.),(1.,
1.),(1.,1.),(1.,1.),(1.,1.),(1.,1.),(1.,1.),(1.,1.),(1.,1.),(1.,1.),(1.,
1.),(1.,1.),(1.,1.),(1.,1.),(1.,1.),(1.,1.),(1.,1.),(1.,1.),(1.,1.),(1.,
1.),(1.,1.),(1.,1.),(1.,1.),(1.,1.),(1.,1.),(1.,1.),(1.,1.),(1.,1.),(1.,
1.),(1.,1.),(1.,1.),(1.,1.),(1.,1.),(1.,1.),(1.,1.),(1.,1.),(1.,1.),(1.,
1.),(1.,1.),(1.,1.),(1.,1.),(1.,1.),(1.,1.),(1.,1.),(1.,1.),(1.,1.),(1.,
1.),(1.,1.),(1.,1.),(1.,1.),(1.,1.),(1.,1.),(1.,1.),(1.,1.),(1.,1.),(1.,
1.),(1.,1.),(1.,1.),(1.,1.),(1.,1.),(1.,1.),(1.,1.),(1.,1.),(1.,1.),(1.,
1.),(1.,1.),(1.,1.),(1.,1.),(1.,1.),(1.,1.),(1.,1.),(1.,1.),(1.,1.),(1.,
1.),(1.,1.),(1.,1.),(1.,1.),(1.,1.),(1.,1.),(1.,1.),(1.,1.),(1.,1.),(1.,
1.),(1.,1.),(1.,1.),(1.,1.),(1.,1.),(1.,1.),(1.,1.),(1.,1.),(1.,1.),(1.,
1.),(1.,1.),(1.,1.),(1.,1.),(1.,1.),(1.,1.),(1.,1.),(1.,1.),(1.,1.),(1.,
1.),(1.,1.),(1.,1.),(1.,1.),(1.,1.),(1.,1.),(1.,1.),(1.,1.),(1.,1.),(1.,
1.),(1.,1.),(1.,1.),(1.,1.),(1.,1.),(1.,1.),(1.,1.),(1.,1.),(1.,1.),(1.,
1.),(1.,1.),(1.,1.),(1.,1.),(1.,1.),(1.,1.),(1.,1.),(1.,1.),(1.,1.),(1.,
1.),(1.,1.),(1.,1.),(1.,1.),(1.,1.),(1.,1.),(1.,1.),(1.,1.),(1.,1.),(1.,
1.),(1.,1.),(1.,1.),(1.,1.),(1.,1.),(1.,1.),(1.,1.),(1.,1.),(1.,1.),(1.,
1.),(1.,1.),(1.,1.),(1.,1.),(1.,1.),(1.,1.),(1.,1.),(1.,1.),(1.,1.),(1.,
1.),(1.,1.),(1.,1.),(1.,1.),(1.,1.),(1.,1.),(1.,1.),(1.,1.),(1.,1.),(1.,
1.),(1.,1.),(1.,1.),(1.,1.),(1.,1.),(1.,1.),(1.,1.),(1.,1.),(1.,1.),(1.,
1.),(1.,1.)))
REPRESENTATION_ITEM('')
SURFACE()
);
#926=(
BOUNDED_SURFACE()
B_SPLINE_SURFACE(5,1,((#91150,#91151),(#91152,#91153),(#91154,#91155),(#91156,
#91157),(#91158,#91159),(#91160,#91161),(#91162,#91163),(#91164,#91165),
(#91166,#91167),(#91168,#91169),(#91170,#91171),(#91172,#91173),(#91174,
#91175),(#91176,#91177),(#91178,#91179),(#91180,#91181),(#91182,#91183),
(#91184,#91185),(#91186,#91187),(#91188,#91189),(#91190,#91191),(#91192,
#91193),(#91194,#91195),(#91196,#91197),(#91198,#91199),(#91200,#91201),
(#91202,#91203),(#91204,#91205),(#91206,#91207),(#91208,#91209),(#91210,
#91211),(#91212,#91213),(#91214,#91215),(#91216,#91217),(#91218,#91219),
(#91220,#91221),(#91222,#91223),(#91224,#91225),(#91226,#91227),(#91228,
#91229),(#91230,#91231),(#91232,#91233),(#91234,#91235),(#91236,#91237),
(#91238,#91239),(#91240,#91241),(#91242,#91243),(#91244,#91245),(#91246,
#91247),(#91248,#91249),(#91250,#91251),(#91252,#91253),(#91254,#91255),
(#91256,#91257),(#91258,#91259),(#91260,#91261),(#91262,#91263),(#91264,
#91265),(#91266,#91267),(#91268,#91269),(#91270,#91271),(#91272,#91273),
(#91274,#91275),(#91276,#91277),(#91278,#91279),(#91280,#91281),(#91282,
#91283),(#91284,#91285),(#91286,#91287),(#91288,#91289),(#91290,#91291),
(#91292,#91293),(#91294,#91295),(#91296,#91297),(#91298,#91299),(#91300,
#91301),(#91302,#91303),(#91304,#91305),(#91306,#91307),(#91308,#91309),
(#91310,#91311),(#91312,#91313),(#91314,#91315),(#91316,#91317),(#91318,
#91319),(#91320,#91321),(#91322,#91323),(#91324,#91325),(#91326,#91327),
(#91328,#91329),(#91330,#91331),(#91332,#91333),(#91334,#91335),(#91336,
#91337),(#91338,#91339),(#91340,#91341),(#91342,#91343),(#91344,#91345),
(#91346,#91347),(#91348,#91349),(#91350,#91351),(#91352,#91353),(#91354,
#91355),(#91356,#91357),(#91358,#91359),(#91360,#91361),(#91362,#91363),
(#91364,#91365),(#91366,#91367),(#91368,#91369),(#91370,#91371),(#91372,
#91373),(#91374,#91375),(#91376,#91377),(#91378,#91379),(#91380,#91381),
(#91382,#91383),(#91384,#91385),(#91386,#91387),(#91388,#91389),(#91390,
#91391),(#91392,#91393),(#91394,#91395),(#91396,#91397),(#91398,#91399),
(#91400,#91401),(#91402,#91403),(#91404,#91405),(#91406,#91407),(#91408,
#91409),(#91410,#91411),(#91412,#91413),(#91414,#91415),(#91416,#91417),
(#91418,#91419),(#91420,#91421),(#91422,#91423),(#91424,#91425),(#91426,
#91427),(#91428,#91429),(#91430,#91431),(#91432,#91433),(#91434,#91435),
(#91436,#91437),(#91438,#91439),(#91440,#91441),(#91442,#91443),(#91444,
#91445),(#91446,#91447),(#91448,#91449),(#91450,#91451),(#91452,#91453),
(#91454,#91455),(#91456,#91457),(#91458,#91459),(#91460,#91461),(#91462,
#91463),(#91464,#91465),(#91466,#91467),(#91468,#91469),(#91470,#91471),
(#91472,#91473),(#91474,#91475),(#91476,#91477),(#91478,#91479),(#91480,
#91481),(#91482,#91483),(#91484,#91485),(#91486,#91487),(#91488,#91489),
(#91490,#91491),(#91492,#91493),(#91494,#91495),(#91496,#91497),(#91498,
#91499),(#91500,#91501),(#91502,#91503),(#91504,#91505),(#91506,#91507),
(#91508,#91509),(#91510,#91511),(#91512,#91513),(#91514,#91515),(#91516,
#91517),(#91518,#91519),(#91520,#91521),(#91522,#91523),(#91524,#91525),
(#91526,#91527),(#91528,#91529),(#91530,#91531),(#91532,#91533),(#91534,
#91535),(#91536,#91537),(#91538,#91539),(#91540,#91541),(#91542,#91543),
(#91544,#91545),(#91546,#91547),(#91548,#91549),(#91550,#91551),(#91552,
#91553),(#91554,#91555),(#91556,#91557),(#91558,#91559)),.UNSPECIFIED.,
 .F.,.F.,.F.)
B_SPLINE_SURFACE_WITH_KNOTS((6,1,1,1,1,1,1,1,1,1,1,1,1,1,1,1,1,1,1,1,1,
1,1,1,1,1,1,1,1,1,1,1,1,1,1,1,1,1,1,1,1,1,1,1,1,1,1,1,1,1,1,1,1,1,1,1,1,
1,1,1,1,1,1,1,1,1,1,1,1,1,1,1,1,1,1,1,1,1,1,1,1,1,1,1,1,1,1,1,1,1,1,1,1,
1,1,1,1,1,1,1,1,1,1,1,1,1,1,1,1,1,1,1,1,1,1,1,1,1,1,1,1,1,1,1,1,1,1,1,1,
1,1,1,1,1,1,1,1,1,1,1,1,1,1,1,1,1,1,1,1,1,1,1,1,1,1,1,1,1,1,1,1,1,1,1,1,
1,1,1,1,1,1,1,1,1,1,1,1,1,1,1,1,1,1,1,1,1,1,1,1,1,1,1,1,1,1,1,1,1,1,1,6),
(2,2),(0.,0.005,0.01,0.015,0.02,0.025,0.03,0.035,0.04,0.045,0.05,0.055,
0.06,0.065,0.07,0.075,0.08,0.085,0.09,0.095,0.1,0.105,0.11,0.115,0.12,0.125,
0.13,0.135,0.14,0.145,0.15,0.155,0.16,0.165,0.17,0.175,0.18,0.185,0.19,
0.195,0.2,0.205,0.21,0.215,0.22,0.225,0.23,0.235,0.24,0.245,0.25,0.255,
0.26,0.265,0.27,0.275,0.28,0.285,0.29,0.295,0.3,0.305,0.31,0.315,0.32,0.325,
0.33,0.335,0.34,0.345,0.35,0.355,0.36,0.365,0.37,0.375,0.38,0.385,0.39,
0.395,0.4,0.405,0.41,0.415,0.42,0.425,0.43,0.435,0.44,0.445,0.45,0.455,
0.46,0.465,0.47,0.475,0.48,0.485,0.49,0.495,0.5,0.505,0.51,0.515,0.52,0.525,
0.53,0.535,0.54,0.545,0.55,0.555,0.56,0.565,0.57,0.575,0.58,0.585,0.59,
0.595,0.6,0.605,0.61,0.615,0.62,0.625,0.63,0.635,0.64,0.645,0.65,0.655,
0.66,0.665,0.67,0.675,0.68,0.685,0.690000000000001,0.695000000000001,0.700000000000001,
0.705000000000001,0.710000000000001,0.715000000000001,0.720000000000001,
0.725000000000001,0.730000000000001,0.735000000000001,0.740000000000001,
0.745000000000001,0.750000000000001,0.755000000000001,0.760000000000001,
0.765000000000001,0.770000000000001,0.775000000000001,0.780000000000001,
0.785000000000001,0.790000000000001,0.795000000000001,0.800000000000001,
0.805000000000001,0.810000000000001,0.815000000000001,0.820000000000001,
0.825000000000001,0.830000000000001,0.835000000000001,0.840000000000001,
0.845000000000001,0.850000000000001,0.855000000000001,0.860000000000001,
0.865000000000001,0.870000000000001,0.875000000000001,0.880000000000001,
0.885000000000001,0.890000000000001,0.895000000000001,0.900000000000001,
0.905000000000001,0.910000000000001,0.915000000000001,0.920000000000001,
0.925000000000001,0.930000000000001,0.935000000000001,0.940000000000001,
0.945000000000001,0.950000000000001,0.955000000000001,0.960000000000001,
0.965000000000001,0.970000000000001,0.975000000000001,0.980000000000001,
0.985000000000001,0.990000000000001,0.995000000000001,1.),(0.,1.2),
 .UNSPECIFIED.)
GEOMETRIC_REPRESENTATION_ITEM()
RATIONAL_B_SPLINE_SURFACE(((1.,1.),(1.,1.),(1.,1.),(1.,1.),(1.,1.),(1.,
1.),(1.,1.),(1.,1.),(1.,1.),(1.,1.),(1.,1.),(1.,1.),(1.,1.),(1.,1.),(1.,
1.),(1.,1.),(1.,1.),(1.,1.),(1.,1.),(1.,1.),(1.,1.),(1.,1.),(1.,1.),(1.,
1.),(1.,1.),(1.,1.),(1.,1.),(1.,1.),(1.,1.),(1.,1.),(1.,1.),(1.,1.),(1.,
1.),(1.,1.),(1.,1.),(1.,1.),(1.,1.),(1.,1.),(1.,1.),(1.,1.),(1.,1.),(1.,
1.),(1.,1.),(1.,1.),(1.,1.),(1.,1.),(1.,1.),(1.,1.),(1.,1.),(1.,1.),(1.,
1.),(1.,1.),(1.,1.),(1.,1.),(1.,1.),(1.,1.),(1.,1.),(1.,1.),(1.,1.),(1.,
1.),(1.,1.),(1.,1.),(1.,1.),(1.,1.),(1.,1.),(1.,1.),(1.,1.),(1.,1.),(1.,
1.),(1.,1.),(1.,1.),(1.,1.),(1.,1.),(1.,1.),(1.,1.),(1.,1.),(1.,1.),(1.,
1.),(1.,1.),(1.,1.),(1.,1.),(1.,1.),(1.,1.),(1.,1.),(1.,1.),(1.,1.),(1.,
1.),(1.,1.),(1.,1.),(1.,1.),(1.,1.),(1.,1.),(1.,1.),(1.,1.),(1.,1.),(1.,
1.),(1.,1.),(1.,1.),(1.,1.),(1.,1.),(1.,1.),(1.,1.),(1.,1.),(1.,1.),(1.,
1.),(1.,1.),(1.,1.),(1.,1.),(1.,1.),(1.,1.),(1.,1.),(1.,1.),(1.,1.),(1.,
1.),(1.,1.),(1.,1.),(1.,1.),(1.,1.),(1.,1.),(1.,1.),(1.,1.),(1.,1.),(1.,
1.),(1.,1.),(1.,1.),(1.,1.),(1.,1.),(1.,1.),(1.,1.),(1.,1.),(1.,1.),(1.,
1.),(1.,1.),(1.,1.),(1.,1.),(1.,1.),(1.,1.),(1.,1.),(1.,1.),(1.,1.),(1.,
1.),(1.,1.),(1.,1.),(1.,1.),(1.,1.),(1.,1.),(1.,1.),(1.,1.),(1.,1.),(1.,
1.),(1.,1.),(1.,1.),(1.,1.),(1.,1.),(1.,1.),(1.,1.),(1.,1.),(1.,1.),(1.,
1.),(1.,1.),(1.,1.),(1.,1.),(1.,1.),(1.,1.),(1.,1.),(1.,1.),(1.,1.),(1.,
1.),(1.,1.),(1.,1.),(1.,1.),(1.,1.),(1.,1.),(1.,1.),(1.,1.),(1.,1.),(1.,
1.),(1.,1.),(1.,1.),(1.,1.),(1.,1.),(1.,1.),(1.,1.),(1.,1.),(1.,1.),(1.,
1.),(1.,1.),(1.,1.),(1.,1.),(1.,1.),(1.,1.),(1.,1.),(1.,1.),(1.,1.),(1.,
1.),(1.,1.),(1.,1.),(1.,1.),(1.,1.),(1.,1.),(1.,1.),(1.,1.),(1.,1.),(1.,
1.),(1.,1.)))
REPRESENTATION_ITEM('')
SURFACE()
);
#927=(
BOUNDED_SURFACE()
B_SPLINE_SURFACE(5,1,((#92046,#92047),(#92048,#92049),(#92050,#92051),(#92052,
#92053),(#92054,#92055),(#92056,#92057),(#92058,#92059),(#92060,#92061),
(#92062,#92063),(#92064,#92065),(#92066,#92067),(#92068,#92069),(#92070,
#92071),(#92072,#92073),(#92074,#92075),(#92076,#92077),(#92078,#92079),
(#92080,#92081),(#92082,#92083),(#92084,#92085),(#92086,#92087),(#92088,
#92089),(#92090,#92091),(#92092,#92093),(#92094,#92095),(#92096,#92097),
(#92098,#92099),(#92100,#92101),(#92102,#92103),(#92104,#92105),(#92106,
#92107),(#92108,#92109),(#92110,#92111),(#92112,#92113),(#92114,#92115),
(#92116,#92117),(#92118,#92119),(#92120,#92121),(#92122,#92123),(#92124,
#92125),(#92126,#92127),(#92128,#92129),(#92130,#92131),(#92132,#92133),
(#92134,#92135),(#92136,#92137),(#92138,#92139),(#92140,#92141),(#92142,
#92143),(#92144,#92145),(#92146,#92147),(#92148,#92149),(#92150,#92151),
(#92152,#92153),(#92154,#92155),(#92156,#92157),(#92158,#92159),(#92160,
#92161),(#92162,#92163),(#92164,#92165),(#92166,#92167),(#92168,#92169),
(#92170,#92171),(#92172,#92173),(#92174,#92175),(#92176,#92177),(#92178,
#92179),(#92180,#92181),(#92182,#92183),(#92184,#92185),(#92186,#92187),
(#92188,#92189),(#92190,#92191),(#92192,#92193),(#92194,#92195),(#92196,
#92197),(#92198,#92199),(#92200,#92201),(#92202,#92203),(#92204,#92205),
(#92206,#92207),(#92208,#92209),(#92210,#92211),(#92212,#92213),(#92214,
#92215),(#92216,#92217),(#92218,#92219),(#92220,#92221),(#92222,#92223),
(#92224,#92225),(#92226,#92227),(#92228,#92229),(#92230,#92231),(#92232,
#92233),(#92234,#92235),(#92236,#92237),(#92238,#92239),(#92240,#92241),
(#92242,#92243),(#92244,#92245),(#92246,#92247),(#92248,#92249),(#92250,
#92251),(#92252,#92253),(#92254,#92255),(#92256,#92257),(#92258,#92259),
(#92260,#92261),(#92262,#92263),(#92264,#92265),(#92266,#92267),(#92268,
#92269),(#92270,#92271),(#92272,#92273),(#92274,#92275),(#92276,#92277),
(#92278,#92279),(#92280,#92281),(#92282,#92283),(#92284,#92285),(#92286,
#92287),(#92288,#92289),(#92290,#92291),(#92292,#92293),(#92294,#92295),
(#92296,#92297),(#92298,#92299),(#92300,#92301),(#92302,#92303),(#92304,
#92305),(#92306,#92307),(#92308,#92309),(#92310,#92311),(#92312,#92313),
(#92314,#92315),(#92316,#92317),(#92318,#92319),(#92320,#92321),(#92322,
#92323),(#92324,#92325),(#92326,#92327),(#92328,#92329),(#92330,#92331),
(#92332,#92333),(#92334,#92335),(#92336,#92337),(#92338,#92339),(#92340,
#92341),(#92342,#92343),(#92344,#92345),(#92346,#92347),(#92348,#92349),
(#92350,#92351),(#92352,#92353),(#92354,#92355),(#92356,#92357),(#92358,
#92359),(#92360,#92361),(#92362,#92363),(#92364,#92365),(#92366,#92367),
(#92368,#92369),(#92370,#92371),(#92372,#92373),(#92374,#92375),(#92376,
#92377),(#92378,#92379),(#92380,#92381),(#92382,#92383),(#92384,#92385),
(#92386,#92387),(#92388,#92389),(#92390,#92391),(#92392,#92393),(#92394,
#92395),(#92396,#92397),(#92398,#92399),(#92400,#92401),(#92402,#92403),
(#92404,#92405),(#92406,#92407),(#92408,#92409),(#92410,#92411),(#92412,
#92413),(#92414,#92415),(#92416,#92417),(#92418,#92419),(#92420,#92421),
(#92422,#92423),(#92424,#92425),(#92426,#92427),(#92428,#92429),(#92430,
#92431),(#92432,#92433),(#92434,#92435),(#92436,#92437),(#92438,#92439),
(#92440,#92441),(#92442,#92443),(#92444,#92445),(#92446,#92447),(#92448,
#92449),(#92450,#92451),(#92452,#92453),(#92454,#92455)),.UNSPECIFIED.,
 .F.,.F.,.F.)
B_SPLINE_SURFACE_WITH_KNOTS((6,1,1,1,1,1,1,1,1,1,1,1,1,1,1,1,1,1,1,1,1,
1,1,1,1,1,1,1,1,1,1,1,1,1,1,1,1,1,1,1,1,1,1,1,1,1,1,1,1,1,1,1,1,1,1,1,1,
1,1,1,1,1,1,1,1,1,1,1,1,1,1,1,1,1,1,1,1,1,1,1,1,1,1,1,1,1,1,1,1,1,1,1,1,
1,1,1,1,1,1,1,1,1,1,1,1,1,1,1,1,1,1,1,1,1,1,1,1,1,1,1,1,1,1,1,1,1,1,1,1,
1,1,1,1,1,1,1,1,1,1,1,1,1,1,1,1,1,1,1,1,1,1,1,1,1,1,1,1,1,1,1,1,1,1,1,1,
1,1,1,1,1,1,1,1,1,1,1,1,1,1,1,1,1,1,1,1,1,1,1,1,1,1,1,1,1,1,1,1,1,1,1,6),
(2,2),(0.,0.005,0.01,0.015,0.02,0.025,0.03,0.035,0.04,0.045,0.05,0.055,
0.06,0.065,0.07,0.075,0.08,0.085,0.09,0.095,0.1,0.105,0.11,0.115,0.12,0.125,
0.13,0.135,0.14,0.145,0.15,0.155,0.16,0.165,0.17,0.175,0.18,0.185,0.19,
0.195,0.2,0.205,0.21,0.215,0.22,0.225,0.23,0.235,0.24,0.245,0.25,0.255,
0.26,0.265,0.27,0.275,0.28,0.285,0.29,0.295,0.3,0.305,0.31,0.315,0.32,0.325,
0.33,0.335,0.34,0.345,0.35,0.355,0.36,0.365,0.37,0.375,0.38,0.385,0.39,
0.395,0.4,0.405,0.41,0.415,0.42,0.425,0.43,0.435,0.44,0.445,0.45,0.455,
0.46,0.465,0.47,0.475,0.48,0.485,0.49,0.495,0.5,0.505,0.51,0.515,0.52,0.525,
0.53,0.535,0.54,0.545,0.55,0.555,0.56,0.565,0.57,0.575,0.58,0.585,0.59,
0.595,0.6,0.605,0.61,0.615,0.62,0.625,0.63,0.635,0.64,0.645,0.65,0.655,
0.66,0.665,0.67,0.675,0.68,0.685,0.690000000000001,0.695000000000001,0.700000000000001,
0.705000000000001,0.710000000000001,0.715000000000001,0.720000000000001,
0.725000000000001,0.730000000000001,0.735000000000001,0.740000000000001,
0.745000000000001,0.750000000000001,0.755000000000001,0.760000000000001,
0.765000000000001,0.770000000000001,0.775000000000001,0.780000000000001,
0.785000000000001,0.790000000000001,0.795000000000001,0.800000000000001,
0.805000000000001,0.810000000000001,0.815000000000001,0.820000000000001,
0.825000000000001,0.830000000000001,0.835000000000001,0.840000000000001,
0.845000000000001,0.850000000000001,0.855000000000001,0.860000000000001,
0.865000000000001,0.870000000000001,0.875000000000001,0.880000000000001,
0.885000000000001,0.890000000000001,0.895000000000001,0.900000000000001,
0.905000000000001,0.910000000000001,0.915000000000001,0.920000000000001,
0.925000000000001,0.930000000000001,0.935000000000001,0.940000000000001,
0.945000000000001,0.950000000000001,0.955000000000001,0.960000000000001,
0.965000000000001,0.970000000000001,0.975000000000001,0.980000000000001,
0.985000000000001,0.990000000000001,0.995000000000001,1.),(0.,1.2),
 .UNSPECIFIED.)
GEOMETRIC_REPRESENTATION_ITEM()
RATIONAL_B_SPLINE_SURFACE(((1.,1.),(1.,1.),(1.,1.),(1.,1.),(1.,1.),(1.,
1.),(1.,1.),(1.,1.),(1.,1.),(1.,1.),(1.,1.),(1.,1.),(1.,1.),(1.,1.),(1.,
1.),(1.,1.),(1.,1.),(1.,1.),(1.,1.),(1.,1.),(1.,1.),(1.,1.),(1.,1.),(1.,
1.),(1.,1.),(1.,1.),(1.,1.),(1.,1.),(1.,1.),(1.,1.),(1.,1.),(1.,1.),(1.,
1.),(1.,1.),(1.,1.),(1.,1.),(1.,1.),(1.,1.),(1.,1.),(1.,1.),(1.,1.),(1.,
1.),(1.,1.),(1.,1.),(1.,1.),(1.,1.),(1.,1.),(1.,1.),(1.,1.),(1.,1.),(1.,
1.),(1.,1.),(1.,1.),(1.,1.),(1.,1.),(1.,1.),(1.,1.),(1.,1.),(1.,1.),(1.,
1.),(1.,1.),(1.,1.),(1.,1.),(1.,1.),(1.,1.),(1.,1.),(1.,1.),(1.,1.),(1.,
1.),(1.,1.),(1.,1.),(1.,1.),(1.,1.),(1.,1.),(1.,1.),(1.,1.),(1.,1.),(1.,
1.),(1.,1.),(1.,1.),(1.,1.),(1.,1.),(1.,1.),(1.,1.),(1.,1.),(1.,1.),(1.,
1.),(1.,1.),(1.,1.),(1.,1.),(1.,1.),(1.,1.),(1.,1.),(1.,1.),(1.,1.),(1.,
1.),(1.,1.),(1.,1.),(1.,1.),(1.,1.),(1.,1.),(1.,1.),(1.,1.),(1.,1.),(1.,
1.),(1.,1.),(1.,1.),(1.,1.),(1.,1.),(1.,1.),(1.,1.),(1.,1.),(1.,1.),(1.,
1.),(1.,1.),(1.,1.),(1.,1.),(1.,1.),(1.,1.),(1.,1.),(1.,1.),(1.,1.),(1.,
1.),(1.,1.),(1.,1.),(1.,1.),(1.,1.),(1.,1.),(1.,1.),(1.,1.),(1.,1.),(1.,
1.),(1.,1.),(1.,1.),(1.,1.),(1.,1.),(1.,1.),(1.,1.),(1.,1.),(1.,1.),(1.,
1.),(1.,1.),(1.,1.),(1.,1.),(1.,1.),(1.,1.),(1.,1.),(1.,1.),(1.,1.),(1.,
1.),(1.,1.),(1.,1.),(1.,1.),(1.,1.),(1.,1.),(1.,1.),(1.,1.),(1.,1.),(1.,
1.),(1.,1.),(1.,1.),(1.,1.),(1.,1.),(1.,1.),(1.,1.),(1.,1.),(1.,1.),(1.,
1.),(1.,1.),(1.,1.),(1.,1.),(1.,1.),(1.,1.),(1.,1.),(1.,1.),(1.,1.),(1.,
1.),(1.,1.),(1.,1.),(1.,1.),(1.,1.),(1.,1.),(1.,1.),(1.,1.),(1.,1.),(1.,
1.),(1.,1.),(1.,1.),(1.,1.),(1.,1.),(1.,1.),(1.,1.),(1.,1.),(1.,1.),(1.,
1.),(1.,1.),(1.,1.),(1.,1.),(1.,1.),(1.,1.),(1.,1.),(1.,1.),(1.,1.),(1.,
1.),(1.,1.)))
REPRESENTATION_ITEM('')
SURFACE()
);
#928=(
BOUNDED_SURFACE()
B_SPLINE_SURFACE(5,1,((#92942,#92943),(#92944,#92945),(#92946,#92947),(#92948,
#92949),(#92950,#92951),(#92952,#92953),(#92954,#92955),(#92956,#92957),
(#92958,#92959),(#92960,#92961),(#92962,#92963),(#92964,#92965),(#92966,
#92967),(#92968,#92969),(#92970,#92971),(#92972,#92973),(#92974,#92975),
(#92976,#92977),(#92978,#92979),(#92980,#92981),(#92982,#92983),(#92984,
#92985),(#92986,#92987),(#92988,#92989),(#92990,#92991),(#92992,#92993),
(#92994,#92995),(#92996,#92997),(#92998,#92999),(#93000,#93001),(#93002,
#93003),(#93004,#93005),(#93006,#93007),(#93008,#93009),(#93010,#93011),
(#93012,#93013),(#93014,#93015),(#93016,#93017),(#93018,#93019),(#93020,
#93021),(#93022,#93023),(#93024,#93025),(#93026,#93027),(#93028,#93029),
(#93030,#93031),(#93032,#93033),(#93034,#93035),(#93036,#93037),(#93038,
#93039),(#93040,#93041),(#93042,#93043),(#93044,#93045),(#93046,#93047),
(#93048,#93049),(#93050,#93051),(#93052,#93053),(#93054,#93055),(#93056,
#93057),(#93058,#93059),(#93060,#93061),(#93062,#93063),(#93064,#93065),
(#93066,#93067),(#93068,#93069),(#93070,#93071),(#93072,#93073),(#93074,
#93075),(#93076,#93077),(#93078,#93079),(#93080,#93081),(#93082,#93083),
(#93084,#93085),(#93086,#93087),(#93088,#93089),(#93090,#93091),(#93092,
#93093),(#93094,#93095),(#93096,#93097),(#93098,#93099),(#93100,#93101),
(#93102,#93103),(#93104,#93105),(#93106,#93107),(#93108,#93109),(#93110,
#93111),(#93112,#93113),(#93114,#93115),(#93116,#93117),(#93118,#93119),
(#93120,#93121),(#93122,#93123),(#93124,#93125),(#93126,#93127),(#93128,
#93129),(#93130,#93131),(#93132,#93133),(#93134,#93135),(#93136,#93137),
(#93138,#93139),(#93140,#93141),(#93142,#93143),(#93144,#93145),(#93146,
#93147),(#93148,#93149),(#93150,#93151),(#93152,#93153),(#93154,#93155),
(#93156,#93157),(#93158,#93159),(#93160,#93161),(#93162,#93163),(#93164,
#93165),(#93166,#93167),(#93168,#93169),(#93170,#93171),(#93172,#93173),
(#93174,#93175),(#93176,#93177),(#93178,#93179),(#93180,#93181),(#93182,
#93183),(#93184,#93185),(#93186,#93187),(#93188,#93189),(#93190,#93191),
(#93192,#93193),(#93194,#93195),(#93196,#93197),(#93198,#93199),(#93200,
#93201),(#93202,#93203),(#93204,#93205),(#93206,#93207),(#93208,#93209),
(#93210,#93211),(#93212,#93213),(#93214,#93215),(#93216,#93217),(#93218,
#93219),(#93220,#93221),(#93222,#93223),(#93224,#93225),(#93226,#93227),
(#93228,#93229),(#93230,#93231),(#93232,#93233),(#93234,#93235),(#93236,
#93237),(#93238,#93239),(#93240,#93241),(#93242,#93243),(#93244,#93245),
(#93246,#93247),(#93248,#93249),(#93250,#93251),(#93252,#93253),(#93254,
#93255),(#93256,#93257),(#93258,#93259),(#93260,#93261),(#93262,#93263),
(#93264,#93265),(#93266,#93267),(#93268,#93269),(#93270,#93271),(#93272,
#93273),(#93274,#93275),(#93276,#93277),(#93278,#93279),(#93280,#93281),
(#93282,#93283),(#93284,#93285),(#93286,#93287),(#93288,#93289),(#93290,
#93291),(#93292,#93293),(#93294,#93295),(#93296,#93297),(#93298,#93299),
(#93300,#93301),(#93302,#93303),(#93304,#93305),(#93306,#93307),(#93308,
#93309),(#93310,#93311),(#93312,#93313),(#93314,#93315),(#93316,#93317),
(#93318,#93319),(#93320,#93321),(#93322,#93323),(#93324,#93325),(#93326,
#93327),(#93328,#93329),(#93330,#93331),(#93332,#93333),(#93334,#93335),
(#93336,#93337),(#93338,#93339),(#93340,#93341),(#93342,#93343),(#93344,
#93345),(#93346,#93347),(#93348,#93349),(#93350,#93351)),.UNSPECIFIED.,
 .F.,.F.,.F.)
B_SPLINE_SURFACE_WITH_KNOTS((6,1,1,1,1,1,1,1,1,1,1,1,1,1,1,1,1,1,1,1,1,
1,1,1,1,1,1,1,1,1,1,1,1,1,1,1,1,1,1,1,1,1,1,1,1,1,1,1,1,1,1,1,1,1,1,1,1,
1,1,1,1,1,1,1,1,1,1,1,1,1,1,1,1,1,1,1,1,1,1,1,1,1,1,1,1,1,1,1,1,1,1,1,1,
1,1,1,1,1,1,1,1,1,1,1,1,1,1,1,1,1,1,1,1,1,1,1,1,1,1,1,1,1,1,1,1,1,1,1,1,
1,1,1,1,1,1,1,1,1,1,1,1,1,1,1,1,1,1,1,1,1,1,1,1,1,1,1,1,1,1,1,1,1,1,1,1,
1,1,1,1,1,1,1,1,1,1,1,1,1,1,1,1,1,1,1,1,1,1,1,1,1,1,1,1,1,1,1,1,1,1,1,6),
(2,2),(0.,0.005,0.01,0.015,0.02,0.025,0.03,0.035,0.04,0.045,0.05,0.055,
0.06,0.065,0.07,0.075,0.08,0.085,0.09,0.095,0.1,0.105,0.11,0.115,0.12,0.125,
0.13,0.135,0.14,0.145,0.15,0.155,0.16,0.165,0.17,0.175,0.18,0.185,0.19,
0.195,0.2,0.205,0.21,0.215,0.22,0.225,0.23,0.235,0.24,0.245,0.25,0.255,
0.26,0.265,0.27,0.275,0.28,0.285,0.29,0.295,0.3,0.305,0.31,0.315,0.32,0.325,
0.33,0.335,0.34,0.345,0.35,0.355,0.36,0.365,0.37,0.375,0.38,0.385,0.39,
0.395,0.4,0.405,0.41,0.415,0.42,0.425,0.43,0.435,0.44,0.445,0.45,0.455,
0.46,0.465,0.47,0.475,0.48,0.485,0.49,0.495,0.5,0.505,0.51,0.515,0.52,0.525,
0.53,0.535,0.54,0.545,0.55,0.555,0.56,0.565,0.57,0.575,0.58,0.585,0.59,
0.595,0.6,0.605,0.61,0.615,0.62,0.625,0.63,0.635,0.64,0.645,0.65,0.655,
0.66,0.665,0.67,0.675,0.68,0.685,0.690000000000001,0.695000000000001,0.700000000000001,
0.705000000000001,0.710000000000001,0.715000000000001,0.720000000000001,
0.725000000000001,0.730000000000001,0.735000000000001,0.740000000000001,
0.745000000000001,0.750000000000001,0.755000000000001,0.760000000000001,
0.765000000000001,0.770000000000001,0.775000000000001,0.780000000000001,
0.785000000000001,0.790000000000001,0.795000000000001,0.800000000000001,
0.805000000000001,0.810000000000001,0.815000000000001,0.820000000000001,
0.825000000000001,0.830000000000001,0.835000000000001,0.840000000000001,
0.845000000000001,0.850000000000001,0.855000000000001,0.860000000000001,
0.865000000000001,0.870000000000001,0.875000000000001,0.880000000000001,
0.885000000000001,0.890000000000001,0.895000000000001,0.900000000000001,
0.905000000000001,0.910000000000001,0.915000000000001,0.920000000000001,
0.925000000000001,0.930000000000001,0.935000000000001,0.940000000000001,
0.945000000000001,0.950000000000001,0.955000000000001,0.960000000000001,
0.965000000000001,0.970000000000001,0.975000000000001,0.980000000000001,
0.985000000000001,0.990000000000001,0.995000000000001,1.),(0.,1.2),
 .UNSPECIFIED.)
GEOMETRIC_REPRESENTATION_ITEM()
RATIONAL_B_SPLINE_SURFACE(((1.,1.),(1.,1.),(1.,1.),(1.,1.),(1.,1.),(1.,
1.),(1.,1.),(1.,1.),(1.,1.),(1.,1.),(1.,1.),(1.,1.),(1.,1.),(1.,1.),(1.,
1.),(1.,1.),(1.,1.),(1.,1.),(1.,1.),(1.,1.),(1.,1.),(1.,1.),(1.,1.),(1.,
1.),(1.,1.),(1.,1.),(1.,1.),(1.,1.),(1.,1.),(1.,1.),(1.,1.),(1.,1.),(1.,
1.),(1.,1.),(1.,1.),(1.,1.),(1.,1.),(1.,1.),(1.,1.),(1.,1.),(1.,1.),(1.,
1.),(1.,1.),(1.,1.),(1.,1.),(1.,1.),(1.,1.),(1.,1.),(1.,1.),(1.,1.),(1.,
1.),(1.,1.),(1.,1.),(1.,1.),(1.,1.),(1.,1.),(1.,1.),(1.,1.),(1.,1.),(1.,
1.),(1.,1.),(1.,1.),(1.,1.),(1.,1.),(1.,1.),(1.,1.),(1.,1.),(1.,1.),(1.,
1.),(1.,1.),(1.,1.),(1.,1.),(1.,1.),(1.,1.),(1.,1.),(1.,1.),(1.,1.),(1.,
1.),(1.,1.),(1.,1.),(1.,1.),(1.,1.),(1.,1.),(1.,1.),(1.,1.),(1.,1.),(1.,
1.),(1.,1.),(1.,1.),(1.,1.),(1.,1.),(1.,1.),(1.,1.),(1.,1.),(1.,1.),(1.,
1.),(1.,1.),(1.,1.),(1.,1.),(1.,1.),(1.,1.),(1.,1.),(1.,1.),(1.,1.),(1.,
1.),(1.,1.),(1.,1.),(1.,1.),(1.,1.),(1.,1.),(1.,1.),(1.,1.),(1.,1.),(1.,
1.),(1.,1.),(1.,1.),(1.,1.),(1.,1.),(1.,1.),(1.,1.),(1.,1.),(1.,1.),(1.,
1.),(1.,1.),(1.,1.),(1.,1.),(1.,1.),(1.,1.),(1.,1.),(1.,1.),(1.,1.),(1.,
1.),(1.,1.),(1.,1.),(1.,1.),(1.,1.),(1.,1.),(1.,1.),(1.,1.),(1.,1.),(1.,
1.),(1.,1.),(1.,1.),(1.,1.),(1.,1.),(1.,1.),(1.,1.),(1.,1.),(1.,1.),(1.,
1.),(1.,1.),(1.,1.),(1.,1.),(1.,1.),(1.,1.),(1.,1.),(1.,1.),(1.,1.),(1.,
1.),(1.,1.),(1.,1.),(1.,1.),(1.,1.),(1.,1.),(1.,1.),(1.,1.),(1.,1.),(1.,
1.),(1.,1.),(1.,1.),(1.,1.),(1.,1.),(1.,1.),(1.,1.),(1.,1.),(1.,1.),(1.,
1.),(1.,1.),(1.,1.),(1.,1.),(1.,1.),(1.,1.),(1.,1.),(1.,1.),(1.,1.),(1.,
1.),(1.,1.),(1.,1.),(1.,1.),(1.,1.),(1.,1.),(1.,1.),(1.,1.),(1.,1.),(1.,
1.),(1.,1.),(1.,1.),(1.,1.),(1.,1.),(1.,1.),(1.,1.),(1.,1.),(1.,1.),(1.,
1.),(1.,1.)))
REPRESENTATION_ITEM('')
SURFACE()
);
#929=(
BOUNDED_SURFACE()
B_SPLINE_SURFACE(5,1,((#93838,#93839),(#93840,#93841),(#93842,#93843),(#93844,
#93845),(#93846,#93847),(#93848,#93849),(#93850,#93851),(#93852,#93853),
(#93854,#93855),(#93856,#93857),(#93858,#93859),(#93860,#93861),(#93862,
#93863),(#93864,#93865),(#93866,#93867),(#93868,#93869),(#93870,#93871),
(#93872,#93873),(#93874,#93875),(#93876,#93877),(#93878,#93879),(#93880,
#93881),(#93882,#93883),(#93884,#93885),(#93886,#93887),(#93888,#93889),
(#93890,#93891),(#93892,#93893),(#93894,#93895),(#93896,#93897),(#93898,
#93899),(#93900,#93901),(#93902,#93903),(#93904,#93905),(#93906,#93907),
(#93908,#93909),(#93910,#93911),(#93912,#93913),(#93914,#93915),(#93916,
#93917),(#93918,#93919),(#93920,#93921),(#93922,#93923),(#93924,#93925),
(#93926,#93927),(#93928,#93929),(#93930,#93931),(#93932,#93933),(#93934,
#93935),(#93936,#93937),(#93938,#93939),(#93940,#93941),(#93942,#93943),
(#93944,#93945),(#93946,#93947),(#93948,#93949),(#93950,#93951),(#93952,
#93953),(#93954,#93955),(#93956,#93957),(#93958,#93959),(#93960,#93961),
(#93962,#93963),(#93964,#93965),(#93966,#93967),(#93968,#93969),(#93970,
#93971),(#93972,#93973),(#93974,#93975),(#93976,#93977),(#93978,#93979),
(#93980,#93981),(#93982,#93983),(#93984,#93985),(#93986,#93987),(#93988,
#93989),(#93990,#93991),(#93992,#93993),(#93994,#93995),(#93996,#93997),
(#93998,#93999),(#94000,#94001),(#94002,#94003),(#94004,#94005),(#94006,
#94007),(#94008,#94009),(#94010,#94011),(#94012,#94013),(#94014,#94015),
(#94016,#94017),(#94018,#94019),(#94020,#94021),(#94022,#94023),(#94024,
#94025),(#94026,#94027),(#94028,#94029),(#94030,#94031),(#94032,#94033),
(#94034,#94035),(#94036,#94037),(#94038,#94039),(#94040,#94041),(#94042,
#94043),(#94044,#94045),(#94046,#94047),(#94048,#94049),(#94050,#94051),
(#94052,#94053),(#94054,#94055),(#94056,#94057),(#94058,#94059),(#94060,
#94061),(#94062,#94063),(#94064,#94065),(#94066,#94067),(#94068,#94069),
(#94070,#94071),(#94072,#94073),(#94074,#94075),(#94076,#94077),(#94078,
#94079),(#94080,#94081),(#94082,#94083),(#94084,#94085),(#94086,#94087),
(#94088,#94089),(#94090,#94091),(#94092,#94093),(#94094,#94095),(#94096,
#94097),(#94098,#94099),(#94100,#94101),(#94102,#94103),(#94104,#94105),
(#94106,#94107),(#94108,#94109),(#94110,#94111),(#94112,#94113),(#94114,
#94115),(#94116,#94117),(#94118,#94119),(#94120,#94121),(#94122,#94123),
(#94124,#94125),(#94126,#94127),(#94128,#94129),(#94130,#94131),(#94132,
#94133),(#94134,#94135),(#94136,#94137),(#94138,#94139),(#94140,#94141),
(#94142,#94143),(#94144,#94145),(#94146,#94147),(#94148,#94149),(#94150,
#94151),(#94152,#94153),(#94154,#94155),(#94156,#94157),(#94158,#94159),
(#94160,#94161),(#94162,#94163),(#94164,#94165),(#94166,#94167),(#94168,
#94169),(#94170,#94171),(#94172,#94173),(#94174,#94175),(#94176,#94177),
(#94178,#94179),(#94180,#94181),(#94182,#94183),(#94184,#94185),(#94186,
#94187),(#94188,#94189),(#94190,#94191),(#94192,#94193),(#94194,#94195),
(#94196,#94197),(#94198,#94199),(#94200,#94201),(#94202,#94203),(#94204,
#94205),(#94206,#94207),(#94208,#94209),(#94210,#94211),(#94212,#94213),
(#94214,#94215),(#94216,#94217),(#94218,#94219),(#94220,#94221),(#94222,
#94223),(#94224,#94225),(#94226,#94227),(#94228,#94229),(#94230,#94231),
(#94232,#94233),(#94234,#94235),(#94236,#94237),(#94238,#94239),(#94240,
#94241),(#94242,#94243),(#94244,#94245),(#94246,#94247)),.UNSPECIFIED.,
 .F.,.F.,.F.)
B_SPLINE_SURFACE_WITH_KNOTS((6,1,1,1,1,1,1,1,1,1,1,1,1,1,1,1,1,1,1,1,1,
1,1,1,1,1,1,1,1,1,1,1,1,1,1,1,1,1,1,1,1,1,1,1,1,1,1,1,1,1,1,1,1,1,1,1,1,
1,1,1,1,1,1,1,1,1,1,1,1,1,1,1,1,1,1,1,1,1,1,1,1,1,1,1,1,1,1,1,1,1,1,1,1,
1,1,1,1,1,1,1,1,1,1,1,1,1,1,1,1,1,1,1,1,1,1,1,1,1,1,1,1,1,1,1,1,1,1,1,1,
1,1,1,1,1,1,1,1,1,1,1,1,1,1,1,1,1,1,1,1,1,1,1,1,1,1,1,1,1,1,1,1,1,1,1,1,
1,1,1,1,1,1,1,1,1,1,1,1,1,1,1,1,1,1,1,1,1,1,1,1,1,1,1,1,1,1,1,1,1,1,1,6),
(2,2),(0.,0.005,0.01,0.015,0.02,0.025,0.03,0.035,0.04,0.045,0.05,0.055,
0.06,0.065,0.07,0.075,0.08,0.085,0.09,0.095,0.1,0.105,0.11,0.115,0.12,0.125,
0.13,0.135,0.14,0.145,0.15,0.155,0.16,0.165,0.17,0.175,0.18,0.185,0.19,
0.195,0.2,0.205,0.21,0.215,0.22,0.225,0.23,0.235,0.24,0.245,0.25,0.255,
0.26,0.265,0.27,0.275,0.28,0.285,0.29,0.295,0.3,0.305,0.31,0.315,0.32,0.325,
0.33,0.335,0.34,0.345,0.35,0.355,0.36,0.365,0.37,0.375,0.38,0.385,0.39,
0.395,0.4,0.405,0.41,0.415,0.42,0.425,0.43,0.435,0.44,0.445,0.45,0.455,
0.46,0.465,0.47,0.475,0.48,0.485,0.49,0.495,0.5,0.505,0.51,0.515,0.52,0.525,
0.53,0.535,0.54,0.545,0.55,0.555,0.56,0.565,0.57,0.575,0.58,0.585,0.59,
0.595,0.6,0.605,0.61,0.615,0.62,0.625,0.63,0.635,0.64,0.645,0.65,0.655,
0.66,0.665,0.67,0.675,0.68,0.685,0.690000000000001,0.695000000000001,0.700000000000001,
0.705000000000001,0.710000000000001,0.715000000000001,0.720000000000001,
0.725000000000001,0.730000000000001,0.735000000000001,0.740000000000001,
0.745000000000001,0.750000000000001,0.755000000000001,0.760000000000001,
0.765000000000001,0.770000000000001,0.775000000000001,0.780000000000001,
0.785000000000001,0.790000000000001,0.795000000000001,0.800000000000001,
0.805000000000001,0.810000000000001,0.815000000000001,0.820000000000001,
0.825000000000001,0.830000000000001,0.835000000000001,0.840000000000001,
0.845000000000001,0.850000000000001,0.855000000000001,0.860000000000001,
0.865000000000001,0.870000000000001,0.875000000000001,0.880000000000001,
0.885000000000001,0.890000000000001,0.895000000000001,0.900000000000001,
0.905000000000001,0.910000000000001,0.915000000000001,0.920000000000001,
0.925000000000001,0.930000000000001,0.935000000000001,0.940000000000001,
0.945000000000001,0.950000000000001,0.955000000000001,0.960000000000001,
0.965000000000001,0.970000000000001,0.975000000000001,0.980000000000001,
0.985000000000001,0.990000000000001,0.995000000000001,1.),(0.,1.2),
 .UNSPECIFIED.)
GEOMETRIC_REPRESENTATION_ITEM()
RATIONAL_B_SPLINE_SURFACE(((1.,1.),(1.,1.),(1.,1.),(1.,1.),(1.,1.),(1.,
1.),(1.,1.),(1.,1.),(1.,1.),(1.,1.),(1.,1.),(1.,1.),(1.,1.),(1.,1.),(1.,
1.),(1.,1.),(1.,1.),(1.,1.),(1.,1.),(1.,1.),(1.,1.),(1.,1.),(1.,1.),(1.,
1.),(1.,1.),(1.,1.),(1.,1.),(1.,1.),(1.,1.),(1.,1.),(1.,1.),(1.,1.),(1.,
1.),(1.,1.),(1.,1.),(1.,1.),(1.,1.),(1.,1.),(1.,1.),(1.,1.),(1.,1.),(1.,
1.),(1.,1.),(1.,1.),(1.,1.),(1.,1.),(1.,1.),(1.,1.),(1.,1.),(1.,1.),(1.,
1.),(1.,1.),(1.,1.),(1.,1.),(1.,1.),(1.,1.),(1.,1.),(1.,1.),(1.,1.),(1.,
1.),(1.,1.),(1.,1.),(1.,1.),(1.,1.),(1.,1.),(1.,1.),(1.,1.),(1.,1.),(1.,
1.),(1.,1.),(1.,1.),(1.,1.),(1.,1.),(1.,1.),(1.,1.),(1.,1.),(1.,1.),(1.,
1.),(1.,1.),(1.,1.),(1.,1.),(1.,1.),(1.,1.),(1.,1.),(1.,1.),(1.,1.),(1.,
1.),(1.,1.),(1.,1.),(1.,1.),(1.,1.),(1.,1.),(1.,1.),(1.,1.),(1.,1.),(1.,
1.),(1.,1.),(1.,1.),(1.,1.),(1.,1.),(1.,1.),(1.,1.),(1.,1.),(1.,1.),(1.,
1.),(1.,1.),(1.,1.),(1.,1.),(1.,1.),(1.,1.),(1.,1.),(1.,1.),(1.,1.),(1.,
1.),(1.,1.),(1.,1.),(1.,1.),(1.,1.),(1.,1.),(1.,1.),(1.,1.),(1.,1.),(1.,
1.),(1.,1.),(1.,1.),(1.,1.),(1.,1.),(1.,1.),(1.,1.),(1.,1.),(1.,1.),(1.,
1.),(1.,1.),(1.,1.),(1.,1.),(1.,1.),(1.,1.),(1.,1.),(1.,1.),(1.,1.),(1.,
1.),(1.,1.),(1.,1.),(1.,1.),(1.,1.),(1.,1.),(1.,1.),(1.,1.),(1.,1.),(1.,
1.),(1.,1.),(1.,1.),(1.,1.),(1.,1.),(1.,1.),(1.,1.),(1.,1.),(1.,1.),(1.,
1.),(1.,1.),(1.,1.),(1.,1.),(1.,1.),(1.,1.),(1.,1.),(1.,1.),(1.,1.),(1.,
1.),(1.,1.),(1.,1.),(1.,1.),(1.,1.),(1.,1.),(1.,1.),(1.,1.),(1.,1.),(1.,
1.),(1.,1.),(1.,1.),(1.,1.),(1.,1.),(1.,1.),(1.,1.),(1.,1.),(1.,1.),(1.,
1.),(1.,1.),(1.,1.),(1.,1.),(1.,1.),(1.,1.),(1.,1.),(1.,1.),(1.,1.),(1.,
1.),(1.,1.),(1.,1.),(1.,1.),(1.,1.),(1.,1.),(1.,1.),(1.,1.),(1.,1.),(1.,
1.),(1.,1.)))
REPRESENTATION_ITEM('')
SURFACE()
);
#930=(
BOUNDED_SURFACE()
B_SPLINE_SURFACE(5,1,((#94734,#94735),(#94736,#94737),(#94738,#94739),(#94740,
#94741),(#94742,#94743),(#94744,#94745),(#94746,#94747),(#94748,#94749),
(#94750,#94751),(#94752,#94753),(#94754,#94755),(#94756,#94757),(#94758,
#94759),(#94760,#94761),(#94762,#94763),(#94764,#94765),(#94766,#94767),
(#94768,#94769),(#94770,#94771),(#94772,#94773),(#94774,#94775),(#94776,
#94777),(#94778,#94779),(#94780,#94781),(#94782,#94783),(#94784,#94785),
(#94786,#94787),(#94788,#94789),(#94790,#94791),(#94792,#94793),(#94794,
#94795),(#94796,#94797),(#94798,#94799),(#94800,#94801),(#94802,#94803),
(#94804,#94805),(#94806,#94807),(#94808,#94809),(#94810,#94811),(#94812,
#94813),(#94814,#94815),(#94816,#94817),(#94818,#94819),(#94820,#94821),
(#94822,#94823),(#94824,#94825),(#94826,#94827),(#94828,#94829),(#94830,
#94831),(#94832,#94833),(#94834,#94835),(#94836,#94837),(#94838,#94839),
(#94840,#94841),(#94842,#94843),(#94844,#94845),(#94846,#94847),(#94848,
#94849),(#94850,#94851),(#94852,#94853),(#94854,#94855),(#94856,#94857),
(#94858,#94859),(#94860,#94861),(#94862,#94863),(#94864,#94865),(#94866,
#94867),(#94868,#94869),(#94870,#94871),(#94872,#94873),(#94874,#94875),
(#94876,#94877),(#94878,#94879),(#94880,#94881),(#94882,#94883),(#94884,
#94885),(#94886,#94887),(#94888,#94889),(#94890,#94891),(#94892,#94893),
(#94894,#94895),(#94896,#94897),(#94898,#94899),(#94900,#94901),(#94902,
#94903),(#94904,#94905),(#94906,#94907),(#94908,#94909),(#94910,#94911),
(#94912,#94913),(#94914,#94915),(#94916,#94917),(#94918,#94919),(#94920,
#94921),(#94922,#94923),(#94924,#94925),(#94926,#94927),(#94928,#94929),
(#94930,#94931),(#94932,#94933),(#94934,#94935),(#94936,#94937),(#94938,
#94939),(#94940,#94941),(#94942,#94943),(#94944,#94945),(#94946,#94947),
(#94948,#94949),(#94950,#94951),(#94952,#94953),(#94954,#94955),(#94956,
#94957),(#94958,#94959),(#94960,#94961),(#94962,#94963),(#94964,#94965),
(#94966,#94967),(#94968,#94969),(#94970,#94971),(#94972,#94973),(#94974,
#94975),(#94976,#94977),(#94978,#94979),(#94980,#94981),(#94982,#94983),
(#94984,#94985),(#94986,#94987),(#94988,#94989),(#94990,#94991),(#94992,
#94993),(#94994,#94995),(#94996,#94997),(#94998,#94999),(#95000,#95001),
(#95002,#95003),(#95004,#95005),(#95006,#95007),(#95008,#95009),(#95010,
#95011),(#95012,#95013),(#95014,#95015),(#95016,#95017),(#95018,#95019),
(#95020,#95021),(#95022,#95023),(#95024,#95025),(#95026,#95027),(#95028,
#95029),(#95030,#95031),(#95032,#95033),(#95034,#95035),(#95036,#95037),
(#95038,#95039),(#95040,#95041),(#95042,#95043),(#95044,#95045),(#95046,
#95047),(#95048,#95049),(#95050,#95051),(#95052,#95053),(#95054,#95055),
(#95056,#95057),(#95058,#95059),(#95060,#95061),(#95062,#95063),(#95064,
#95065),(#95066,#95067),(#95068,#95069),(#95070,#95071),(#95072,#95073),
(#95074,#95075),(#95076,#95077),(#95078,#95079),(#95080,#95081),(#95082,
#95083),(#95084,#95085),(#95086,#95087),(#95088,#95089),(#95090,#95091),
(#95092,#95093),(#95094,#95095),(#95096,#95097),(#95098,#95099),(#95100,
#95101),(#95102,#95103),(#95104,#95105),(#95106,#95107),(#95108,#95109),
(#95110,#95111),(#95112,#95113),(#95114,#95115),(#95116,#95117),(#95118,
#95119),(#95120,#95121),(#95122,#95123),(#95124,#95125),(#95126,#95127),
(#95128,#95129),(#95130,#95131),(#95132,#95133),(#95134,#95135),(#95136,
#95137),(#95138,#95139),(#95140,#95141),(#95142,#95143)),.UNSPECIFIED.,
 .F.,.F.,.F.)
B_SPLINE_SURFACE_WITH_KNOTS((6,1,1,1,1,1,1,1,1,1,1,1,1,1,1,1,1,1,1,1,1,
1,1,1,1,1,1,1,1,1,1,1,1,1,1,1,1,1,1,1,1,1,1,1,1,1,1,1,1,1,1,1,1,1,1,1,1,
1,1,1,1,1,1,1,1,1,1,1,1,1,1,1,1,1,1,1,1,1,1,1,1,1,1,1,1,1,1,1,1,1,1,1,1,
1,1,1,1,1,1,1,1,1,1,1,1,1,1,1,1,1,1,1,1,1,1,1,1,1,1,1,1,1,1,1,1,1,1,1,1,
1,1,1,1,1,1,1,1,1,1,1,1,1,1,1,1,1,1,1,1,1,1,1,1,1,1,1,1,1,1,1,1,1,1,1,1,
1,1,1,1,1,1,1,1,1,1,1,1,1,1,1,1,1,1,1,1,1,1,1,1,1,1,1,1,1,1,1,1,1,1,1,6),
(2,2),(0.,0.005,0.01,0.015,0.02,0.025,0.03,0.035,0.04,0.045,0.05,0.055,
0.06,0.065,0.07,0.075,0.08,0.085,0.09,0.095,0.1,0.105,0.11,0.115,0.12,0.125,
0.13,0.135,0.14,0.145,0.15,0.155,0.16,0.165,0.17,0.175,0.18,0.185,0.19,
0.195,0.2,0.205,0.21,0.215,0.22,0.225,0.23,0.235,0.24,0.245,0.25,0.255,
0.26,0.265,0.27,0.275,0.28,0.285,0.29,0.295,0.3,0.305,0.31,0.315,0.32,0.325,
0.33,0.335,0.34,0.345,0.35,0.355,0.36,0.365,0.37,0.375,0.38,0.385,0.39,
0.395,0.4,0.405,0.41,0.415,0.42,0.425,0.43,0.435,0.44,0.445,0.45,0.455,
0.46,0.465,0.47,0.475,0.48,0.485,0.49,0.495,0.5,0.505,0.51,0.515,0.52,0.525,
0.53,0.535,0.54,0.545,0.55,0.555,0.56,0.565,0.57,0.575,0.58,0.585,0.59,
0.595,0.6,0.605,0.61,0.615,0.62,0.625,0.63,0.635,0.64,0.645,0.65,0.655,
0.66,0.665,0.67,0.675,0.68,0.685,0.690000000000001,0.695000000000001,0.700000000000001,
0.705000000000001,0.710000000000001,0.715000000000001,0.720000000000001,
0.725000000000001,0.730000000000001,0.735000000000001,0.740000000000001,
0.745000000000001,0.750000000000001,0.755000000000001,0.760000000000001,
0.765000000000001,0.770000000000001,0.775000000000001,0.780000000000001,
0.785000000000001,0.790000000000001,0.795000000000001,0.800000000000001,
0.805000000000001,0.810000000000001,0.815000000000001,0.820000000000001,
0.825000000000001,0.830000000000001,0.835000000000001,0.840000000000001,
0.845000000000001,0.850000000000001,0.855000000000001,0.860000000000001,
0.865000000000001,0.870000000000001,0.875000000000001,0.880000000000001,
0.885000000000001,0.890000000000001,0.895000000000001,0.900000000000001,
0.905000000000001,0.910000000000001,0.915000000000001,0.920000000000001,
0.925000000000001,0.930000000000001,0.935000000000001,0.940000000000001,
0.945000000000001,0.950000000000001,0.955000000000001,0.960000000000001,
0.965000000000001,0.970000000000001,0.975000000000001,0.980000000000001,
0.985000000000001,0.990000000000001,0.995000000000001,1.),(0.,1.2),
 .UNSPECIFIED.)
GEOMETRIC_REPRESENTATION_ITEM()
RATIONAL_B_SPLINE_SURFACE(((1.,1.),(1.,1.),(1.,1.),(1.,1.),(1.,1.),(1.,
1.),(1.,1.),(1.,1.),(1.,1.),(1.,1.),(1.,1.),(1.,1.),(1.,1.),(1.,1.),(1.,
1.),(1.,1.),(1.,1.),(1.,1.),(1.,1.),(1.,1.),(1.,1.),(1.,1.),(1.,1.),(1.,
1.),(1.,1.),(1.,1.),(1.,1.),(1.,1.),(1.,1.),(1.,1.),(1.,1.),(1.,1.),(1.,
1.),(1.,1.),(1.,1.),(1.,1.),(1.,1.),(1.,1.),(1.,1.),(1.,1.),(1.,1.),(1.,
1.),(1.,1.),(1.,1.),(1.,1.),(1.,1.),(1.,1.),(1.,1.),(1.,1.),(1.,1.),(1.,
1.),(1.,1.),(1.,1.),(1.,1.),(1.,1.),(1.,1.),(1.,1.),(1.,1.),(1.,1.),(1.,
1.),(1.,1.),(1.,1.),(1.,1.),(1.,1.),(1.,1.),(1.,1.),(1.,1.),(1.,1.),(1.,
1.),(1.,1.),(1.,1.),(1.,1.),(1.,1.),(1.,1.),(1.,1.),(1.,1.),(1.,1.),(1.,
1.),(1.,1.),(1.,1.),(1.,1.),(1.,1.),(1.,1.),(1.,1.),(1.,1.),(1.,1.),(1.,
1.),(1.,1.),(1.,1.),(1.,1.),(1.,1.),(1.,1.),(1.,1.),(1.,1.),(1.,1.),(1.,
1.),(1.,1.),(1.,1.),(1.,1.),(1.,1.),(1.,1.),(1.,1.),(1.,1.),(1.,1.),(1.,
1.),(1.,1.),(1.,1.),(1.,1.),(1.,1.),(1.,1.),(1.,1.),(1.,1.),(1.,1.),(1.,
1.),(1.,1.),(1.,1.),(1.,1.),(1.,1.),(1.,1.),(1.,1.),(1.,1.),(1.,1.),(1.,
1.),(1.,1.),(1.,1.),(1.,1.),(1.,1.),(1.,1.),(1.,1.),(1.,1.),(1.,1.),(1.,
1.),(1.,1.),(1.,1.),(1.,1.),(1.,1.),(1.,1.),(1.,1.),(1.,1.),(1.,1.),(1.,
1.),(1.,1.),(1.,1.),(1.,1.),(1.,1.),(1.,1.),(1.,1.),(1.,1.),(1.,1.),(1.,
1.),(1.,1.),(1.,1.),(1.,1.),(1.,1.),(1.,1.),(1.,1.),(1.,1.),(1.,1.),(1.,
1.),(1.,1.),(1.,1.),(1.,1.),(1.,1.),(1.,1.),(1.,1.),(1.,1.),(1.,1.),(1.,
1.),(1.,1.),(1.,1.),(1.,1.),(1.,1.),(1.,1.),(1.,1.),(1.,1.),(1.,1.),(1.,
1.),(1.,1.),(1.,1.),(1.,1.),(1.,1.),(1.,1.),(1.,1.),(1.,1.),(1.,1.),(1.,
1.),(1.,1.),(1.,1.),(1.,1.),(1.,1.),(1.,1.),(1.,1.),(1.,1.),(1.,1.),(1.,
1.),(1.,1.),(1.,1.),(1.,1.),(1.,1.),(1.,1.),(1.,1.),(1.,1.),(1.,1.),(1.,
1.),(1.,1.)))
REPRESENTATION_ITEM('')
SURFACE()
);
#931=(
BOUNDED_SURFACE()
B_SPLINE_SURFACE(5,1,((#95630,#95631),(#95632,#95633),(#95634,#95635),(#95636,
#95637),(#95638,#95639),(#95640,#95641),(#95642,#95643),(#95644,#95645),
(#95646,#95647),(#95648,#95649),(#95650,#95651),(#95652,#95653),(#95654,
#95655),(#95656,#95657),(#95658,#95659),(#95660,#95661),(#95662,#95663),
(#95664,#95665),(#95666,#95667),(#95668,#95669),(#95670,#95671),(#95672,
#95673),(#95674,#95675),(#95676,#95677),(#95678,#95679),(#95680,#95681),
(#95682,#95683),(#95684,#95685),(#95686,#95687),(#95688,#95689),(#95690,
#95691),(#95692,#95693),(#95694,#95695),(#95696,#95697),(#95698,#95699),
(#95700,#95701),(#95702,#95703),(#95704,#95705),(#95706,#95707),(#95708,
#95709),(#95710,#95711),(#95712,#95713),(#95714,#95715),(#95716,#95717),
(#95718,#95719),(#95720,#95721),(#95722,#95723),(#95724,#95725),(#95726,
#95727),(#95728,#95729),(#95730,#95731),(#95732,#95733),(#95734,#95735),
(#95736,#95737),(#95738,#95739),(#95740,#95741),(#95742,#95743),(#95744,
#95745),(#95746,#95747),(#95748,#95749),(#95750,#95751),(#95752,#95753),
(#95754,#95755),(#95756,#95757),(#95758,#95759),(#95760,#95761),(#95762,
#95763),(#95764,#95765),(#95766,#95767),(#95768,#95769),(#95770,#95771),
(#95772,#95773),(#95774,#95775),(#95776,#95777),(#95778,#95779),(#95780,
#95781),(#95782,#95783),(#95784,#95785),(#95786,#95787),(#95788,#95789),
(#95790,#95791),(#95792,#95793),(#95794,#95795),(#95796,#95797),(#95798,
#95799),(#95800,#95801),(#95802,#95803),(#95804,#95805),(#95806,#95807),
(#95808,#95809),(#95810,#95811),(#95812,#95813),(#95814,#95815),(#95816,
#95817),(#95818,#95819),(#95820,#95821),(#95822,#95823),(#95824,#95825),
(#95826,#95827),(#95828,#95829),(#95830,#95831),(#95832,#95833),(#95834,
#95835),(#95836,#95837),(#95838,#95839),(#95840,#95841),(#95842,#95843),
(#95844,#95845),(#95846,#95847),(#95848,#95849),(#95850,#95851),(#95852,
#95853),(#95854,#95855),(#95856,#95857),(#95858,#95859),(#95860,#95861),
(#95862,#95863),(#95864,#95865),(#95866,#95867),(#95868,#95869),(#95870,
#95871),(#95872,#95873),(#95874,#95875),(#95876,#95877),(#95878,#95879),
(#95880,#95881),(#95882,#95883),(#95884,#95885),(#95886,#95887),(#95888,
#95889),(#95890,#95891),(#95892,#95893),(#95894,#95895),(#95896,#95897),
(#95898,#95899),(#95900,#95901),(#95902,#95903),(#95904,#95905),(#95906,
#95907),(#95908,#95909),(#95910,#95911),(#95912,#95913),(#95914,#95915),
(#95916,#95917),(#95918,#95919),(#95920,#95921),(#95922,#95923),(#95924,
#95925),(#95926,#95927),(#95928,#95929),(#95930,#95931),(#95932,#95933),
(#95934,#95935),(#95936,#95937),(#95938,#95939),(#95940,#95941),(#95942,
#95943),(#95944,#95945),(#95946,#95947),(#95948,#95949),(#95950,#95951),
(#95952,#95953),(#95954,#95955),(#95956,#95957),(#95958,#95959),(#95960,
#95961),(#95962,#95963),(#95964,#95965),(#95966,#95967),(#95968,#95969),
(#95970,#95971),(#95972,#95973),(#95974,#95975),(#95976,#95977),(#95978,
#95979),(#95980,#95981),(#95982,#95983),(#95984,#95985),(#95986,#95987),
(#95988,#95989),(#95990,#95991),(#95992,#95993),(#95994,#95995),(#95996,
#95997),(#95998,#95999),(#96000,#96001),(#96002,#96003),(#96004,#96005),
(#96006,#96007),(#96008,#96009),(#96010,#96011),(#96012,#96013),(#96014,
#96015),(#96016,#96017),(#96018,#96019),(#96020,#96021),(#96022,#96023),
(#96024,#96025),(#96026,#96027),(#96028,#96029),(#96030,#96031),(#96032,
#96033),(#96034,#96035),(#96036,#96037),(#96038,#96039)),.UNSPECIFIED.,
 .F.,.F.,.F.)
B_SPLINE_SURFACE_WITH_KNOTS((6,1,1,1,1,1,1,1,1,1,1,1,1,1,1,1,1,1,1,1,1,
1,1,1,1,1,1,1,1,1,1,1,1,1,1,1,1,1,1,1,1,1,1,1,1,1,1,1,1,1,1,1,1,1,1,1,1,
1,1,1,1,1,1,1,1,1,1,1,1,1,1,1,1,1,1,1,1,1,1,1,1,1,1,1,1,1,1,1,1,1,1,1,1,
1,1,1,1,1,1,1,1,1,1,1,1,1,1,1,1,1,1,1,1,1,1,1,1,1,1,1,1,1,1,1,1,1,1,1,1,
1,1,1,1,1,1,1,1,1,1,1,1,1,1,1,1,1,1,1,1,1,1,1,1,1,1,1,1,1,1,1,1,1,1,1,1,
1,1,1,1,1,1,1,1,1,1,1,1,1,1,1,1,1,1,1,1,1,1,1,1,1,1,1,1,1,1,1,1,1,1,1,6),
(2,2),(0.,0.005,0.01,0.015,0.02,0.025,0.03,0.035,0.04,0.045,0.05,0.055,
0.06,0.065,0.07,0.075,0.08,0.085,0.09,0.095,0.1,0.105,0.11,0.115,0.12,0.125,
0.13,0.135,0.14,0.145,0.15,0.155,0.16,0.165,0.17,0.175,0.18,0.185,0.19,
0.195,0.2,0.205,0.21,0.215,0.22,0.225,0.23,0.235,0.24,0.245,0.25,0.255,
0.26,0.265,0.27,0.275,0.28,0.285,0.29,0.295,0.3,0.305,0.31,0.315,0.32,0.325,
0.33,0.335,0.34,0.345,0.35,0.355,0.36,0.365,0.37,0.375,0.38,0.385,0.39,
0.395,0.4,0.405,0.41,0.415,0.42,0.425,0.43,0.435,0.44,0.445,0.45,0.455,
0.46,0.465,0.47,0.475,0.48,0.485,0.49,0.495,0.5,0.505,0.51,0.515,0.52,0.525,
0.53,0.535,0.54,0.545,0.55,0.555,0.56,0.565,0.57,0.575,0.58,0.585,0.59,
0.595,0.6,0.605,0.61,0.615,0.62,0.625,0.63,0.635,0.64,0.645,0.65,0.655,
0.66,0.665,0.67,0.675,0.68,0.685,0.690000000000001,0.695000000000001,0.700000000000001,
0.705000000000001,0.710000000000001,0.715000000000001,0.720000000000001,
0.725000000000001,0.730000000000001,0.735000000000001,0.740000000000001,
0.745000000000001,0.750000000000001,0.755000000000001,0.760000000000001,
0.765000000000001,0.770000000000001,0.775000000000001,0.780000000000001,
0.785000000000001,0.790000000000001,0.795000000000001,0.800000000000001,
0.805000000000001,0.810000000000001,0.815000000000001,0.820000000000001,
0.825000000000001,0.830000000000001,0.835000000000001,0.840000000000001,
0.845000000000001,0.850000000000001,0.855000000000001,0.860000000000001,
0.865000000000001,0.870000000000001,0.875000000000001,0.880000000000001,
0.885000000000001,0.890000000000001,0.895000000000001,0.900000000000001,
0.905000000000001,0.910000000000001,0.915000000000001,0.920000000000001,
0.925000000000001,0.930000000000001,0.935000000000001,0.940000000000001,
0.945000000000001,0.950000000000001,0.955000000000001,0.960000000000001,
0.965000000000001,0.970000000000001,0.975000000000001,0.980000000000001,
0.985000000000001,0.990000000000001,0.995000000000001,1.),(0.,1.2),
 .UNSPECIFIED.)
GEOMETRIC_REPRESENTATION_ITEM()
RATIONAL_B_SPLINE_SURFACE(((1.,1.),(1.,1.),(1.,1.),(1.,1.),(1.,1.),(1.,
1.),(1.,1.),(1.,1.),(1.,1.),(1.,1.),(1.,1.),(1.,1.),(1.,1.),(1.,1.),(1.,
1.),(1.,1.),(1.,1.),(1.,1.),(1.,1.),(1.,1.),(1.,1.),(1.,1.),(1.,1.),(1.,
1.),(1.,1.),(1.,1.),(1.,1.),(1.,1.),(1.,1.),(1.,1.),(1.,1.),(1.,1.),(1.,
1.),(1.,1.),(1.,1.),(1.,1.),(1.,1.),(1.,1.),(1.,1.),(1.,1.),(1.,1.),(1.,
1.),(1.,1.),(1.,1.),(1.,1.),(1.,1.),(1.,1.),(1.,1.),(1.,1.),(1.,1.),(1.,
1.),(1.,1.),(1.,1.),(1.,1.),(1.,1.),(1.,1.),(1.,1.),(1.,1.),(1.,1.),(1.,
1.),(1.,1.),(1.,1.),(1.,1.),(1.,1.),(1.,1.),(1.,1.),(1.,1.),(1.,1.),(1.,
1.),(1.,1.),(1.,1.),(1.,1.),(1.,1.),(1.,1.),(1.,1.),(1.,1.),(1.,1.),(1.,
1.),(1.,1.),(1.,1.),(1.,1.),(1.,1.),(1.,1.),(1.,1.),(1.,1.),(1.,1.),(1.,
1.),(1.,1.),(1.,1.),(1.,1.),(1.,1.),(1.,1.),(1.,1.),(1.,1.),(1.,1.),(1.,
1.),(1.,1.),(1.,1.),(1.,1.),(1.,1.),(1.,1.),(1.,1.),(1.,1.),(1.,1.),(1.,
1.),(1.,1.),(1.,1.),(1.,1.),(1.,1.),(1.,1.),(1.,1.),(1.,1.),(1.,1.),(1.,
1.),(1.,1.),(1.,1.),(1.,1.),(1.,1.),(1.,1.),(1.,1.),(1.,1.),(1.,1.),(1.,
1.),(1.,1.),(1.,1.),(1.,1.),(1.,1.),(1.,1.),(1.,1.),(1.,1.),(1.,1.),(1.,
1.),(1.,1.),(1.,1.),(1.,1.),(1.,1.),(1.,1.),(1.,1.),(1.,1.),(1.,1.),(1.,
1.),(1.,1.),(1.,1.),(1.,1.),(1.,1.),(1.,1.),(1.,1.),(1.,1.),(1.,1.),(1.,
1.),(1.,1.),(1.,1.),(1.,1.),(1.,1.),(1.,1.),(1.,1.),(1.,1.),(1.,1.),(1.,
1.),(1.,1.),(1.,1.),(1.,1.),(1.,1.),(1.,1.),(1.,1.),(1.,1.),(1.,1.),(1.,
1.),(1.,1.),(1.,1.),(1.,1.),(1.,1.),(1.,1.),(1.,1.),(1.,1.),(1.,1.),(1.,
1.),(1.,1.),(1.,1.),(1.,1.),(1.,1.),(1.,1.),(1.,1.),(1.,1.),(1.,1.),(1.,
1.),(1.,1.),(1.,1.),(1.,1.),(1.,1.),(1.,1.),(1.,1.),(1.,1.),(1.,1.),(1.,
1.),(1.,1.),(1.,1.),(1.,1.),(1.,1.),(1.,1.),(1.,1.),(1.,1.),(1.,1.),(1.,
1.),(1.,1.)))
REPRESENTATION_ITEM('')
SURFACE()
);
#932=(
BOUNDED_SURFACE()
B_SPLINE_SURFACE(5,1,((#96526,#96527),(#96528,#96529),(#96530,#96531),(#96532,
#96533),(#96534,#96535),(#96536,#96537),(#96538,#96539),(#96540,#96541),
(#96542,#96543),(#96544,#96545),(#96546,#96547),(#96548,#96549),(#96550,
#96551),(#96552,#96553),(#96554,#96555),(#96556,#96557),(#96558,#96559),
(#96560,#96561),(#96562,#96563),(#96564,#96565),(#96566,#96567),(#96568,
#96569),(#96570,#96571),(#96572,#96573),(#96574,#96575),(#96576,#96577),
(#96578,#96579),(#96580,#96581),(#96582,#96583),(#96584,#96585),(#96586,
#96587),(#96588,#96589),(#96590,#96591),(#96592,#96593),(#96594,#96595),
(#96596,#96597),(#96598,#96599),(#96600,#96601),(#96602,#96603),(#96604,
#96605),(#96606,#96607),(#96608,#96609),(#96610,#96611),(#96612,#96613),
(#96614,#96615),(#96616,#96617),(#96618,#96619),(#96620,#96621),(#96622,
#96623),(#96624,#96625),(#96626,#96627),(#96628,#96629),(#96630,#96631),
(#96632,#96633),(#96634,#96635),(#96636,#96637),(#96638,#96639),(#96640,
#96641),(#96642,#96643),(#96644,#96645),(#96646,#96647),(#96648,#96649),
(#96650,#96651),(#96652,#96653),(#96654,#96655),(#96656,#96657),(#96658,
#96659),(#96660,#96661),(#96662,#96663),(#96664,#96665),(#96666,#96667),
(#96668,#96669),(#96670,#96671),(#96672,#96673),(#96674,#96675),(#96676,
#96677),(#96678,#96679),(#96680,#96681),(#96682,#96683),(#96684,#96685),
(#96686,#96687),(#96688,#96689),(#96690,#96691),(#96692,#96693),(#96694,
#96695),(#96696,#96697),(#96698,#96699),(#96700,#96701),(#96702,#96703),
(#96704,#96705),(#96706,#96707),(#96708,#96709),(#96710,#96711),(#96712,
#96713),(#96714,#96715),(#96716,#96717),(#96718,#96719),(#96720,#96721),
(#96722,#96723),(#96724,#96725),(#96726,#96727),(#96728,#96729),(#96730,
#96731),(#96732,#96733),(#96734,#96735),(#96736,#96737),(#96738,#96739),
(#96740,#96741),(#96742,#96743),(#96744,#96745),(#96746,#96747),(#96748,
#96749),(#96750,#96751),(#96752,#96753),(#96754,#96755),(#96756,#96757),
(#96758,#96759),(#96760,#96761),(#96762,#96763),(#96764,#96765),(#96766,
#96767),(#96768,#96769),(#96770,#96771),(#96772,#96773),(#96774,#96775),
(#96776,#96777),(#96778,#96779),(#96780,#96781),(#96782,#96783),(#96784,
#96785),(#96786,#96787),(#96788,#96789),(#96790,#96791),(#96792,#96793),
(#96794,#96795),(#96796,#96797),(#96798,#96799),(#96800,#96801),(#96802,
#96803),(#96804,#96805),(#96806,#96807),(#96808,#96809),(#96810,#96811),
(#96812,#96813),(#96814,#96815),(#96816,#96817),(#96818,#96819),(#96820,
#96821),(#96822,#96823),(#96824,#96825),(#96826,#96827),(#96828,#96829),
(#96830,#96831),(#96832,#96833),(#96834,#96835),(#96836,#96837),(#96838,
#96839),(#96840,#96841),(#96842,#96843),(#96844,#96845),(#96846,#96847),
(#96848,#96849),(#96850,#96851),(#96852,#96853),(#96854,#96855),(#96856,
#96857),(#96858,#96859),(#96860,#96861),(#96862,#96863),(#96864,#96865),
(#96866,#96867),(#96868,#96869),(#96870,#96871),(#96872,#96873),(#96874,
#96875),(#96876,#96877),(#96878,#96879),(#96880,#96881),(#96882,#96883),
(#96884,#96885),(#96886,#96887),(#96888,#96889),(#96890,#96891),(#96892,
#96893),(#96894,#96895),(#96896,#96897),(#96898,#96899),(#96900,#96901),
(#96902,#96903),(#96904,#96905),(#96906,#96907),(#96908,#96909),(#96910,
#96911),(#96912,#96913),(#96914,#96915),(#96916,#96917),(#96918,#96919),
(#96920,#96921),(#96922,#96923),(#96924,#96925),(#96926,#96927),(#96928,
#96929),(#96930,#96931),(#96932,#96933),(#96934,#96935)),.UNSPECIFIED.,
 .F.,.F.,.F.)
B_SPLINE_SURFACE_WITH_KNOTS((6,1,1,1,1,1,1,1,1,1,1,1,1,1,1,1,1,1,1,1,1,
1,1,1,1,1,1,1,1,1,1,1,1,1,1,1,1,1,1,1,1,1,1,1,1,1,1,1,1,1,1,1,1,1,1,1,1,
1,1,1,1,1,1,1,1,1,1,1,1,1,1,1,1,1,1,1,1,1,1,1,1,1,1,1,1,1,1,1,1,1,1,1,1,
1,1,1,1,1,1,1,1,1,1,1,1,1,1,1,1,1,1,1,1,1,1,1,1,1,1,1,1,1,1,1,1,1,1,1,1,
1,1,1,1,1,1,1,1,1,1,1,1,1,1,1,1,1,1,1,1,1,1,1,1,1,1,1,1,1,1,1,1,1,1,1,1,
1,1,1,1,1,1,1,1,1,1,1,1,1,1,1,1,1,1,1,1,1,1,1,1,1,1,1,1,1,1,1,1,1,1,1,6),
(2,2),(0.,0.005,0.01,0.015,0.02,0.025,0.03,0.035,0.04,0.045,0.05,0.055,
0.06,0.065,0.07,0.075,0.08,0.085,0.09,0.095,0.1,0.105,0.11,0.115,0.12,0.125,
0.13,0.135,0.14,0.145,0.15,0.155,0.16,0.165,0.17,0.175,0.18,0.185,0.19,
0.195,0.2,0.205,0.21,0.215,0.22,0.225,0.23,0.235,0.24,0.245,0.25,0.255,
0.26,0.265,0.27,0.275,0.28,0.285,0.29,0.295,0.3,0.305,0.31,0.315,0.32,0.325,
0.33,0.335,0.34,0.345,0.35,0.355,0.36,0.365,0.37,0.375,0.38,0.385,0.39,
0.395,0.4,0.405,0.41,0.415,0.42,0.425,0.43,0.435,0.44,0.445,0.45,0.455,
0.46,0.465,0.47,0.475,0.48,0.485,0.49,0.495,0.5,0.505,0.51,0.515,0.52,0.525,
0.53,0.535,0.54,0.545,0.55,0.555,0.56,0.565,0.57,0.575,0.58,0.585,0.59,
0.595,0.6,0.605,0.61,0.615,0.62,0.625,0.63,0.635,0.64,0.645,0.65,0.655,
0.66,0.665,0.67,0.675,0.68,0.685,0.690000000000001,0.695000000000001,0.700000000000001,
0.705000000000001,0.710000000000001,0.715000000000001,0.720000000000001,
0.725000000000001,0.730000000000001,0.735000000000001,0.740000000000001,
0.745000000000001,0.750000000000001,0.755000000000001,0.760000000000001,
0.765000000000001,0.770000000000001,0.775000000000001,0.780000000000001,
0.785000000000001,0.790000000000001,0.795000000000001,0.800000000000001,
0.805000000000001,0.810000000000001,0.815000000000001,0.820000000000001,
0.825000000000001,0.830000000000001,0.835000000000001,0.840000000000001,
0.845000000000001,0.850000000000001,0.855000000000001,0.860000000000001,
0.865000000000001,0.870000000000001,0.875000000000001,0.880000000000001,
0.885000000000001,0.890000000000001,0.895000000000001,0.900000000000001,
0.905000000000001,0.910000000000001,0.915000000000001,0.920000000000001,
0.925000000000001,0.930000000000001,0.935000000000001,0.940000000000001,
0.945000000000001,0.950000000000001,0.955000000000001,0.960000000000001,
0.965000000000001,0.970000000000001,0.975000000000001,0.980000000000001,
0.985000000000001,0.990000000000001,0.995000000000001,1.),(0.,1.2),
 .UNSPECIFIED.)
GEOMETRIC_REPRESENTATION_ITEM()
RATIONAL_B_SPLINE_SURFACE(((1.,1.),(1.,1.),(1.,1.),(1.,1.),(1.,1.),(1.,
1.),(1.,1.),(1.,1.),(1.,1.),(1.,1.),(1.,1.),(1.,1.),(1.,1.),(1.,1.),(1.,
1.),(1.,1.),(1.,1.),(1.,1.),(1.,1.),(1.,1.),(1.,1.),(1.,1.),(1.,1.),(1.,
1.),(1.,1.),(1.,1.),(1.,1.),(1.,1.),(1.,1.),(1.,1.),(1.,1.),(1.,1.),(1.,
1.),(1.,1.),(1.,1.),(1.,1.),(1.,1.),(1.,1.),(1.,1.),(1.,1.),(1.,1.),(1.,
1.),(1.,1.),(1.,1.),(1.,1.),(1.,1.),(1.,1.),(1.,1.),(1.,1.),(1.,1.),(1.,
1.),(1.,1.),(1.,1.),(1.,1.),(1.,1.),(1.,1.),(1.,1.),(1.,1.),(1.,1.),(1.,
1.),(1.,1.),(1.,1.),(1.,1.),(1.,1.),(1.,1.),(1.,1.),(1.,1.),(1.,1.),(1.,
1.),(1.,1.),(1.,1.),(1.,1.),(1.,1.),(1.,1.),(1.,1.),(1.,1.),(1.,1.),(1.,
1.),(1.,1.),(1.,1.),(1.,1.),(1.,1.),(1.,1.),(1.,1.),(1.,1.),(1.,1.),(1.,
1.),(1.,1.),(1.,1.),(1.,1.),(1.,1.),(1.,1.),(1.,1.),(1.,1.),(1.,1.),(1.,
1.),(1.,1.),(1.,1.),(1.,1.),(1.,1.),(1.,1.),(1.,1.),(1.,1.),(1.,1.),(1.,
1.),(1.,1.),(1.,1.),(1.,1.),(1.,1.),(1.,1.),(1.,1.),(1.,1.),(1.,1.),(1.,
1.),(1.,1.),(1.,1.),(1.,1.),(1.,1.),(1.,1.),(1.,1.),(1.,1.),(1.,1.),(1.,
1.),(1.,1.),(1.,1.),(1.,1.),(1.,1.),(1.,1.),(1.,1.),(1.,1.),(1.,1.),(1.,
1.),(1.,1.),(1.,1.),(1.,1.),(1.,1.),(1.,1.),(1.,1.),(1.,1.),(1.,1.),(1.,
1.),(1.,1.),(1.,1.),(1.,1.),(1.,1.),(1.,1.),(1.,1.),(1.,1.),(1.,1.),(1.,
1.),(1.,1.),(1.,1.),(1.,1.),(1.,1.),(1.,1.),(1.,1.),(1.,1.),(1.,1.),(1.,
1.),(1.,1.),(1.,1.),(1.,1.),(1.,1.),(1.,1.),(1.,1.),(1.,1.),(1.,1.),(1.,
1.),(1.,1.),(1.,1.),(1.,1.),(1.,1.),(1.,1.),(1.,1.),(1.,1.),(1.,1.),(1.,
1.),(1.,1.),(1.,1.),(1.,1.),(1.,1.),(1.,1.),(1.,1.),(1.,1.),(1.,1.),(1.,
1.),(1.,1.),(1.,1.),(1.,1.),(1.,1.),(1.,1.),(1.,1.),(1.,1.),(1.,1.),(1.,
1.),(1.,1.),(1.,1.),(1.,1.),(1.,1.),(1.,1.),(1.,1.),(1.,1.),(1.,1.),(1.,
1.),(1.,1.)))
REPRESENTATION_ITEM('')
SURFACE()
);
#933=(
BOUNDED_SURFACE()
B_SPLINE_SURFACE(5,1,((#97422,#97423),(#97424,#97425),(#97426,#97427),(#97428,
#97429),(#97430,#97431),(#97432,#97433),(#97434,#97435),(#97436,#97437),
(#97438,#97439),(#97440,#97441),(#97442,#97443),(#97444,#97445),(#97446,
#97447),(#97448,#97449),(#97450,#97451),(#97452,#97453),(#97454,#97455),
(#97456,#97457),(#97458,#97459),(#97460,#97461),(#97462,#97463),(#97464,
#97465),(#97466,#97467),(#97468,#97469),(#97470,#97471),(#97472,#97473),
(#97474,#97475),(#97476,#97477),(#97478,#97479),(#97480,#97481),(#97482,
#97483),(#97484,#97485),(#97486,#97487),(#97488,#97489),(#97490,#97491),
(#97492,#97493),(#97494,#97495),(#97496,#97497),(#97498,#97499),(#97500,
#97501),(#97502,#97503),(#97504,#97505),(#97506,#97507),(#97508,#97509),
(#97510,#97511),(#97512,#97513),(#97514,#97515),(#97516,#97517),(#97518,
#97519),(#97520,#97521),(#97522,#97523),(#97524,#97525),(#97526,#97527),
(#97528,#97529),(#97530,#97531),(#97532,#97533),(#97534,#97535),(#97536,
#97537),(#97538,#97539),(#97540,#97541),(#97542,#97543),(#97544,#97545),
(#97546,#97547),(#97548,#97549),(#97550,#97551),(#97552,#97553),(#97554,
#97555),(#97556,#97557),(#97558,#97559),(#97560,#97561),(#97562,#97563),
(#97564,#97565),(#97566,#97567),(#97568,#97569),(#97570,#97571),(#97572,
#97573),(#97574,#97575),(#97576,#97577),(#97578,#97579),(#97580,#97581),
(#97582,#97583),(#97584,#97585),(#97586,#97587),(#97588,#97589),(#97590,
#97591),(#97592,#97593),(#97594,#97595),(#97596,#97597),(#97598,#97599),
(#97600,#97601),(#97602,#97603),(#97604,#97605),(#97606,#97607),(#97608,
#97609),(#97610,#97611),(#97612,#97613),(#97614,#97615),(#97616,#97617),
(#97618,#97619),(#97620,#97621),(#97622,#97623),(#97624,#97625),(#97626,
#97627),(#97628,#97629),(#97630,#97631),(#97632,#97633),(#97634,#97635),
(#97636,#97637),(#97638,#97639),(#97640,#97641),(#97642,#97643),(#97644,
#97645),(#97646,#97647),(#97648,#97649),(#97650,#97651),(#97652,#97653),
(#97654,#97655),(#97656,#97657),(#97658,#97659),(#97660,#97661),(#97662,
#97663),(#97664,#97665),(#97666,#97667),(#97668,#97669),(#97670,#97671),
(#97672,#97673),(#97674,#97675),(#97676,#97677),(#97678,#97679),(#97680,
#97681),(#97682,#97683),(#97684,#97685),(#97686,#97687),(#97688,#97689),
(#97690,#97691),(#97692,#97693),(#97694,#97695),(#97696,#97697),(#97698,
#97699),(#97700,#97701),(#97702,#97703),(#97704,#97705),(#97706,#97707),
(#97708,#97709),(#97710,#97711),(#97712,#97713),(#97714,#97715),(#97716,
#97717),(#97718,#97719),(#97720,#97721),(#97722,#97723),(#97724,#97725),
(#97726,#97727),(#97728,#97729),(#97730,#97731),(#97732,#97733),(#97734,
#97735),(#97736,#97737),(#97738,#97739),(#97740,#97741),(#97742,#97743),
(#97744,#97745),(#97746,#97747),(#97748,#97749),(#97750,#97751),(#97752,
#97753),(#97754,#97755),(#97756,#97757),(#97758,#97759),(#97760,#97761),
(#97762,#97763),(#97764,#97765),(#97766,#97767),(#97768,#97769),(#97770,
#97771),(#97772,#97773),(#97774,#97775),(#97776,#97777),(#97778,#97779),
(#97780,#97781),(#97782,#97783),(#97784,#97785),(#97786,#97787),(#97788,
#97789),(#97790,#97791),(#97792,#97793),(#97794,#97795),(#97796,#97797),
(#97798,#97799),(#97800,#97801),(#97802,#97803),(#97804,#97805),(#97806,
#97807),(#97808,#97809),(#97810,#97811),(#97812,#97813),(#97814,#97815),
(#97816,#97817),(#97818,#97819),(#97820,#97821),(#97822,#97823),(#97824,
#97825),(#97826,#97827),(#97828,#97829),(#97830,#97831)),.UNSPECIFIED.,
 .F.,.F.,.F.)
B_SPLINE_SURFACE_WITH_KNOTS((6,1,1,1,1,1,1,1,1,1,1,1,1,1,1,1,1,1,1,1,1,
1,1,1,1,1,1,1,1,1,1,1,1,1,1,1,1,1,1,1,1,1,1,1,1,1,1,1,1,1,1,1,1,1,1,1,1,
1,1,1,1,1,1,1,1,1,1,1,1,1,1,1,1,1,1,1,1,1,1,1,1,1,1,1,1,1,1,1,1,1,1,1,1,
1,1,1,1,1,1,1,1,1,1,1,1,1,1,1,1,1,1,1,1,1,1,1,1,1,1,1,1,1,1,1,1,1,1,1,1,
1,1,1,1,1,1,1,1,1,1,1,1,1,1,1,1,1,1,1,1,1,1,1,1,1,1,1,1,1,1,1,1,1,1,1,1,
1,1,1,1,1,1,1,1,1,1,1,1,1,1,1,1,1,1,1,1,1,1,1,1,1,1,1,1,1,1,1,1,1,1,1,6),
(2,2),(0.,0.005,0.01,0.015,0.02,0.025,0.03,0.035,0.04,0.045,0.05,0.055,
0.06,0.065,0.07,0.075,0.08,0.085,0.09,0.095,0.1,0.105,0.11,0.115,0.12,0.125,
0.13,0.135,0.14,0.145,0.15,0.155,0.16,0.165,0.17,0.175,0.18,0.185,0.19,
0.195,0.2,0.205,0.21,0.215,0.22,0.225,0.23,0.235,0.24,0.245,0.25,0.255,
0.26,0.265,0.27,0.275,0.28,0.285,0.29,0.295,0.3,0.305,0.31,0.315,0.32,0.325,
0.33,0.335,0.34,0.345,0.35,0.355,0.36,0.365,0.37,0.375,0.38,0.385,0.39,
0.395,0.4,0.405,0.41,0.415,0.42,0.425,0.43,0.435,0.44,0.445,0.45,0.455,
0.46,0.465,0.47,0.475,0.48,0.485,0.49,0.495,0.5,0.505,0.51,0.515,0.52,0.525,
0.53,0.535,0.54,0.545,0.55,0.555,0.56,0.565,0.57,0.575,0.58,0.585,0.59,
0.595,0.6,0.605,0.61,0.615,0.62,0.625,0.63,0.635,0.64,0.645,0.65,0.655,
0.66,0.665,0.67,0.675,0.68,0.685,0.690000000000001,0.695000000000001,0.700000000000001,
0.705000000000001,0.710000000000001,0.715000000000001,0.720000000000001,
0.725000000000001,0.730000000000001,0.735000000000001,0.740000000000001,
0.745000000000001,0.750000000000001,0.755000000000001,0.760000000000001,
0.765000000000001,0.770000000000001,0.775000000000001,0.780000000000001,
0.785000000000001,0.790000000000001,0.795000000000001,0.800000000000001,
0.805000000000001,0.810000000000001,0.815000000000001,0.820000000000001,
0.825000000000001,0.830000000000001,0.835000000000001,0.840000000000001,
0.845000000000001,0.850000000000001,0.855000000000001,0.860000000000001,
0.865000000000001,0.870000000000001,0.875000000000001,0.880000000000001,
0.885000000000001,0.890000000000001,0.895000000000001,0.900000000000001,
0.905000000000001,0.910000000000001,0.915000000000001,0.920000000000001,
0.925000000000001,0.930000000000001,0.935000000000001,0.940000000000001,
0.945000000000001,0.950000000000001,0.955000000000001,0.960000000000001,
0.965000000000001,0.970000000000001,0.975000000000001,0.980000000000001,
0.985000000000001,0.990000000000001,0.995000000000001,1.),(0.,1.2),
 .UNSPECIFIED.)
GEOMETRIC_REPRESENTATION_ITEM()
RATIONAL_B_SPLINE_SURFACE(((1.,1.),(1.,1.),(1.,1.),(1.,1.),(1.,1.),(1.,
1.),(1.,1.),(1.,1.),(1.,1.),(1.,1.),(1.,1.),(1.,1.),(1.,1.),(1.,1.),(1.,
1.),(1.,1.),(1.,1.),(1.,1.),(1.,1.),(1.,1.),(1.,1.),(1.,1.),(1.,1.),(1.,
1.),(1.,1.),(1.,1.),(1.,1.),(1.,1.),(1.,1.),(1.,1.),(1.,1.),(1.,1.),(1.,
1.),(1.,1.),(1.,1.),(1.,1.),(1.,1.),(1.,1.),(1.,1.),(1.,1.),(1.,1.),(1.,
1.),(1.,1.),(1.,1.),(1.,1.),(1.,1.),(1.,1.),(1.,1.),(1.,1.),(1.,1.),(1.,
1.),(1.,1.),(1.,1.),(1.,1.),(1.,1.),(1.,1.),(1.,1.),(1.,1.),(1.,1.),(1.,
1.),(1.,1.),(1.,1.),(1.,1.),(1.,1.),(1.,1.),(1.,1.),(1.,1.),(1.,1.),(1.,
1.),(1.,1.),(1.,1.),(1.,1.),(1.,1.),(1.,1.),(1.,1.),(1.,1.),(1.,1.),(1.,
1.),(1.,1.),(1.,1.),(1.,1.),(1.,1.),(1.,1.),(1.,1.),(1.,1.),(1.,1.),(1.,
1.),(1.,1.),(1.,1.),(1.,1.),(1.,1.),(1.,1.),(1.,1.),(1.,1.),(1.,1.),(1.,
1.),(1.,1.),(1.,1.),(1.,1.),(1.,1.),(1.,1.),(1.,1.),(1.,1.),(1.,1.),(1.,
1.),(1.,1.),(1.,1.),(1.,1.),(1.,1.),(1.,1.),(1.,1.),(1.,1.),(1.,1.),(1.,
1.),(1.,1.),(1.,1.),(1.,1.),(1.,1.),(1.,1.),(1.,1.),(1.,1.),(1.,1.),(1.,
1.),(1.,1.),(1.,1.),(1.,1.),(1.,1.),(1.,1.),(1.,1.),(1.,1.),(1.,1.),(1.,
1.),(1.,1.),(1.,1.),(1.,1.),(1.,1.),(1.,1.),(1.,1.),(1.,1.),(1.,1.),(1.,
1.),(1.,1.),(1.,1.),(1.,1.),(1.,1.),(1.,1.),(1.,1.),(1.,1.),(1.,1.),(1.,
1.),(1.,1.),(1.,1.),(1.,1.),(1.,1.),(1.,1.),(1.,1.),(1.,1.),(1.,1.),(1.,
1.),(1.,1.),(1.,1.),(1.,1.),(1.,1.),(1.,1.),(1.,1.),(1.,1.),(1.,1.),(1.,
1.),(1.,1.),(1.,1.),(1.,1.),(1.,1.),(1.,1.),(1.,1.),(1.,1.),(1.,1.),(1.,
1.),(1.,1.),(1.,1.),(1.,1.),(1.,1.),(1.,1.),(1.,1.),(1.,1.),(1.,1.),(1.,
1.),(1.,1.),(1.,1.),(1.,1.),(1.,1.),(1.,1.),(1.,1.),(1.,1.),(1.,1.),(1.,
1.),(1.,1.),(1.,1.),(1.,1.),(1.,1.),(1.,1.),(1.,1.),(1.,1.),(1.,1.),(1.,
1.),(1.,1.)))
REPRESENTATION_ITEM('')
SURFACE()
);
#934=(
BOUNDED_SURFACE()
B_SPLINE_SURFACE(5,1,((#98318,#98319),(#98320,#98321),(#98322,#98323),(#98324,
#98325),(#98326,#98327),(#98328,#98329),(#98330,#98331),(#98332,#98333),
(#98334,#98335),(#98336,#98337),(#98338,#98339),(#98340,#98341),(#98342,
#98343),(#98344,#98345),(#98346,#98347),(#98348,#98349),(#98350,#98351),
(#98352,#98353),(#98354,#98355),(#98356,#98357),(#98358,#98359),(#98360,
#98361),(#98362,#98363),(#98364,#98365),(#98366,#98367),(#98368,#98369),
(#98370,#98371),(#98372,#98373),(#98374,#98375),(#98376,#98377),(#98378,
#98379),(#98380,#98381),(#98382,#98383),(#98384,#98385),(#98386,#98387),
(#98388,#98389),(#98390,#98391),(#98392,#98393),(#98394,#98395),(#98396,
#98397),(#98398,#98399),(#98400,#98401),(#98402,#98403),(#98404,#98405),
(#98406,#98407),(#98408,#98409),(#98410,#98411),(#98412,#98413),(#98414,
#98415),(#98416,#98417),(#98418,#98419),(#98420,#98421),(#98422,#98423),
(#98424,#98425),(#98426,#98427),(#98428,#98429),(#98430,#98431),(#98432,
#98433),(#98434,#98435),(#98436,#98437),(#98438,#98439),(#98440,#98441),
(#98442,#98443),(#98444,#98445),(#98446,#98447),(#98448,#98449),(#98450,
#98451),(#98452,#98453),(#98454,#98455),(#98456,#98457),(#98458,#98459),
(#98460,#98461),(#98462,#98463),(#98464,#98465),(#98466,#98467),(#98468,
#98469),(#98470,#98471),(#98472,#98473),(#98474,#98475),(#98476,#98477),
(#98478,#98479),(#98480,#98481),(#98482,#98483),(#98484,#98485),(#98486,
#98487),(#98488,#98489),(#98490,#98491),(#98492,#98493),(#98494,#98495),
(#98496,#98497),(#98498,#98499),(#98500,#98501),(#98502,#98503),(#98504,
#98505),(#98506,#98507),(#98508,#98509),(#98510,#98511),(#98512,#98513),
(#98514,#98515),(#98516,#98517),(#98518,#98519),(#98520,#98521),(#98522,
#98523),(#98524,#98525),(#98526,#98527),(#98528,#98529),(#98530,#98531),
(#98532,#98533),(#98534,#98535),(#98536,#98537),(#98538,#98539),(#98540,
#98541),(#98542,#98543),(#98544,#98545),(#98546,#98547),(#98548,#98549),
(#98550,#98551),(#98552,#98553),(#98554,#98555),(#98556,#98557),(#98558,
#98559),(#98560,#98561),(#98562,#98563),(#98564,#98565),(#98566,#98567),
(#98568,#98569),(#98570,#98571),(#98572,#98573),(#98574,#98575),(#98576,
#98577),(#98578,#98579),(#98580,#98581),(#98582,#98583),(#98584,#98585),
(#98586,#98587),(#98588,#98589),(#98590,#98591),(#98592,#98593),(#98594,
#98595),(#98596,#98597),(#98598,#98599),(#98600,#98601),(#98602,#98603),
(#98604,#98605),(#98606,#98607),(#98608,#98609),(#98610,#98611),(#98612,
#98613),(#98614,#98615),(#98616,#98617),(#98618,#98619),(#98620,#98621),
(#98622,#98623),(#98624,#98625),(#98626,#98627),(#98628,#98629),(#98630,
#98631),(#98632,#98633),(#98634,#98635),(#98636,#98637),(#98638,#98639),
(#98640,#98641),(#98642,#98643),(#98644,#98645),(#98646,#98647),(#98648,
#98649),(#98650,#98651),(#98652,#98653),(#98654,#98655),(#98656,#98657),
(#98658,#98659),(#98660,#98661),(#98662,#98663),(#98664,#98665),(#98666,
#98667),(#98668,#98669),(#98670,#98671),(#98672,#98673),(#98674,#98675),
(#98676,#98677),(#98678,#98679),(#98680,#98681),(#98682,#98683),(#98684,
#98685),(#98686,#98687),(#98688,#98689),(#98690,#98691),(#98692,#98693),
(#98694,#98695),(#98696,#98697),(#98698,#98699),(#98700,#98701),(#98702,
#98703),(#98704,#98705),(#98706,#98707),(#98708,#98709),(#98710,#98711),
(#98712,#98713),(#98714,#98715),(#98716,#98717),(#98718,#98719),(#98720,
#98721),(#98722,#98723),(#98724,#98725),(#98726,#98727)),.UNSPECIFIED.,
 .F.,.F.,.F.)
B_SPLINE_SURFACE_WITH_KNOTS((6,1,1,1,1,1,1,1,1,1,1,1,1,1,1,1,1,1,1,1,1,
1,1,1,1,1,1,1,1,1,1,1,1,1,1,1,1,1,1,1,1,1,1,1,1,1,1,1,1,1,1,1,1,1,1,1,1,
1,1,1,1,1,1,1,1,1,1,1,1,1,1,1,1,1,1,1,1,1,1,1,1,1,1,1,1,1,1,1,1,1,1,1,1,
1,1,1,1,1,1,1,1,1,1,1,1,1,1,1,1,1,1,1,1,1,1,1,1,1,1,1,1,1,1,1,1,1,1,1,1,
1,1,1,1,1,1,1,1,1,1,1,1,1,1,1,1,1,1,1,1,1,1,1,1,1,1,1,1,1,1,1,1,1,1,1,1,
1,1,1,1,1,1,1,1,1,1,1,1,1,1,1,1,1,1,1,1,1,1,1,1,1,1,1,1,1,1,1,1,1,1,1,6),
(2,2),(0.,0.005,0.01,0.015,0.02,0.025,0.03,0.035,0.04,0.045,0.05,0.055,
0.06,0.065,0.07,0.075,0.08,0.085,0.09,0.095,0.1,0.105,0.11,0.115,0.12,0.125,
0.13,0.135,0.14,0.145,0.15,0.155,0.16,0.165,0.17,0.175,0.18,0.185,0.19,
0.195,0.2,0.205,0.21,0.215,0.22,0.225,0.23,0.235,0.24,0.245,0.25,0.255,
0.26,0.265,0.27,0.275,0.28,0.285,0.29,0.295,0.3,0.305,0.31,0.315,0.32,0.325,
0.33,0.335,0.34,0.345,0.35,0.355,0.36,0.365,0.37,0.375,0.38,0.385,0.39,
0.395,0.4,0.405,0.41,0.415,0.42,0.425,0.43,0.435,0.44,0.445,0.45,0.455,
0.46,0.465,0.47,0.475,0.48,0.485,0.49,0.495,0.5,0.505,0.51,0.515,0.52,0.525,
0.53,0.535,0.54,0.545,0.55,0.555,0.56,0.565,0.57,0.575,0.58,0.585,0.59,
0.595,0.6,0.605,0.61,0.615,0.62,0.625,0.63,0.635,0.64,0.645,0.65,0.655,
0.66,0.665,0.67,0.675,0.68,0.685,0.690000000000001,0.695000000000001,0.700000000000001,
0.705000000000001,0.710000000000001,0.715000000000001,0.720000000000001,
0.725000000000001,0.730000000000001,0.735000000000001,0.740000000000001,
0.745000000000001,0.750000000000001,0.755000000000001,0.760000000000001,
0.765000000000001,0.770000000000001,0.775000000000001,0.780000000000001,
0.785000000000001,0.790000000000001,0.795000000000001,0.800000000000001,
0.805000000000001,0.810000000000001,0.815000000000001,0.820000000000001,
0.825000000000001,0.830000000000001,0.835000000000001,0.840000000000001,
0.845000000000001,0.850000000000001,0.855000000000001,0.860000000000001,
0.865000000000001,0.870000000000001,0.875000000000001,0.880000000000001,
0.885000000000001,0.890000000000001,0.895000000000001,0.900000000000001,
0.905000000000001,0.910000000000001,0.915000000000001,0.920000000000001,
0.925000000000001,0.930000000000001,0.935000000000001,0.940000000000001,
0.945000000000001,0.950000000000001,0.955000000000001,0.960000000000001,
0.965000000000001,0.970000000000001,0.975000000000001,0.980000000000001,
0.985000000000001,0.990000000000001,0.995000000000001,1.),(0.,1.2),
 .UNSPECIFIED.)
GEOMETRIC_REPRESENTATION_ITEM()
RATIONAL_B_SPLINE_SURFACE(((1.,1.),(1.,1.),(1.,1.),(1.,1.),(1.,1.),(1.,
1.),(1.,1.),(1.,1.),(1.,1.),(1.,1.),(1.,1.),(1.,1.),(1.,1.),(1.,1.),(1.,
1.),(1.,1.),(1.,1.),(1.,1.),(1.,1.),(1.,1.),(1.,1.),(1.,1.),(1.,1.),(1.,
1.),(1.,1.),(1.,1.),(1.,1.),(1.,1.),(1.,1.),(1.,1.),(1.,1.),(1.,1.),(1.,
1.),(1.,1.),(1.,1.),(1.,1.),(1.,1.),(1.,1.),(1.,1.),(1.,1.),(1.,1.),(1.,
1.),(1.,1.),(1.,1.),(1.,1.),(1.,1.),(1.,1.),(1.,1.),(1.,1.),(1.,1.),(1.,
1.),(1.,1.),(1.,1.),(1.,1.),(1.,1.),(1.,1.),(1.,1.),(1.,1.),(1.,1.),(1.,
1.),(1.,1.),(1.,1.),(1.,1.),(1.,1.),(1.,1.),(1.,1.),(1.,1.),(1.,1.),(1.,
1.),(1.,1.),(1.,1.),(1.,1.),(1.,1.),(1.,1.),(1.,1.),(1.,1.),(1.,1.),(1.,
1.),(1.,1.),(1.,1.),(1.,1.),(1.,1.),(1.,1.),(1.,1.),(1.,1.),(1.,1.),(1.,
1.),(1.,1.),(1.,1.),(1.,1.),(1.,1.),(1.,1.),(1.,1.),(1.,1.),(1.,1.),(1.,
1.),(1.,1.),(1.,1.),(1.,1.),(1.,1.),(1.,1.),(1.,1.),(1.,1.),(1.,1.),(1.,
1.),(1.,1.),(1.,1.),(1.,1.),(1.,1.),(1.,1.),(1.,1.),(1.,1.),(1.,1.),(1.,
1.),(1.,1.),(1.,1.),(1.,1.),(1.,1.),(1.,1.),(1.,1.),(1.,1.),(1.,1.),(1.,
1.),(1.,1.),(1.,1.),(1.,1.),(1.,1.),(1.,1.),(1.,1.),(1.,1.),(1.,1.),(1.,
1.),(1.,1.),(1.,1.),(1.,1.),(1.,1.),(1.,1.),(1.,1.),(1.,1.),(1.,1.),(1.,
1.),(1.,1.),(1.,1.),(1.,1.),(1.,1.),(1.,1.),(1.,1.),(1.,1.),(1.,1.),(1.,
1.),(1.,1.),(1.,1.),(1.,1.),(1.,1.),(1.,1.),(1.,1.),(1.,1.),(1.,1.),(1.,
1.),(1.,1.),(1.,1.),(1.,1.),(1.,1.),(1.,1.),(1.,1.),(1.,1.),(1.,1.),(1.,
1.),(1.,1.),(1.,1.),(1.,1.),(1.,1.),(1.,1.),(1.,1.),(1.,1.),(1.,1.),(1.,
1.),(1.,1.),(1.,1.),(1.,1.),(1.,1.),(1.,1.),(1.,1.),(1.,1.),(1.,1.),(1.,
1.),(1.,1.),(1.,1.),(1.,1.),(1.,1.),(1.,1.),(1.,1.),(1.,1.),(1.,1.),(1.,
1.),(1.,1.),(1.,1.),(1.,1.),(1.,1.),(1.,1.),(1.,1.),(1.,1.),(1.,1.),(1.,
1.),(1.,1.)))
REPRESENTATION_ITEM('')
SURFACE()
);
#935=(
BOUNDED_SURFACE()
B_SPLINE_SURFACE(5,1,((#99214,#99215),(#99216,#99217),(#99218,#99219),(#99220,
#99221),(#99222,#99223),(#99224,#99225),(#99226,#99227),(#99228,#99229),
(#99230,#99231),(#99232,#99233),(#99234,#99235),(#99236,#99237),(#99238,
#99239),(#99240,#99241),(#99242,#99243),(#99244,#99245),(#99246,#99247),
(#99248,#99249),(#99250,#99251),(#99252,#99253),(#99254,#99255),(#99256,
#99257),(#99258,#99259),(#99260,#99261),(#99262,#99263),(#99264,#99265),
(#99266,#99267),(#99268,#99269),(#99270,#99271),(#99272,#99273),(#99274,
#99275),(#99276,#99277),(#99278,#99279),(#99280,#99281),(#99282,#99283),
(#99284,#99285),(#99286,#99287),(#99288,#99289),(#99290,#99291),(#99292,
#99293),(#99294,#99295),(#99296,#99297),(#99298,#99299),(#99300,#99301),
(#99302,#99303),(#99304,#99305),(#99306,#99307),(#99308,#99309),(#99310,
#99311),(#99312,#99313),(#99314,#99315),(#99316,#99317),(#99318,#99319),
(#99320,#99321),(#99322,#99323),(#99324,#99325),(#99326,#99327),(#99328,
#99329),(#99330,#99331),(#99332,#99333),(#99334,#99335),(#99336,#99337),
(#99338,#99339),(#99340,#99341),(#99342,#99343),(#99344,#99345),(#99346,
#99347),(#99348,#99349),(#99350,#99351),(#99352,#99353),(#99354,#99355),
(#99356,#99357),(#99358,#99359),(#99360,#99361),(#99362,#99363),(#99364,
#99365),(#99366,#99367),(#99368,#99369),(#99370,#99371),(#99372,#99373),
(#99374,#99375),(#99376,#99377),(#99378,#99379),(#99380,#99381),(#99382,
#99383),(#99384,#99385),(#99386,#99387),(#99388,#99389),(#99390,#99391),
(#99392,#99393),(#99394,#99395),(#99396,#99397),(#99398,#99399),(#99400,
#99401),(#99402,#99403),(#99404,#99405),(#99406,#99407),(#99408,#99409),
(#99410,#99411),(#99412,#99413),(#99414,#99415),(#99416,#99417),(#99418,
#99419),(#99420,#99421),(#99422,#99423),(#99424,#99425),(#99426,#99427),
(#99428,#99429),(#99430,#99431),(#99432,#99433),(#99434,#99435),(#99436,
#99437),(#99438,#99439),(#99440,#99441),(#99442,#99443),(#99444,#99445),
(#99446,#99447),(#99448,#99449),(#99450,#99451),(#99452,#99453),(#99454,
#99455),(#99456,#99457),(#99458,#99459),(#99460,#99461),(#99462,#99463),
(#99464,#99465),(#99466,#99467),(#99468,#99469),(#99470,#99471),(#99472,
#99473),(#99474,#99475),(#99476,#99477),(#99478,#99479),(#99480,#99481),
(#99482,#99483),(#99484,#99485),(#99486,#99487),(#99488,#99489),(#99490,
#99491),(#99492,#99493),(#99494,#99495),(#99496,#99497),(#99498,#99499),
(#99500,#99501),(#99502,#99503),(#99504,#99505),(#99506,#99507),(#99508,
#99509),(#99510,#99511),(#99512,#99513),(#99514,#99515),(#99516,#99517),
(#99518,#99519),(#99520,#99521),(#99522,#99523),(#99524,#99525),(#99526,
#99527),(#99528,#99529),(#99530,#99531),(#99532,#99533),(#99534,#99535),
(#99536,#99537),(#99538,#99539),(#99540,#99541),(#99542,#99543),(#99544,
#99545),(#99546,#99547),(#99548,#99549),(#99550,#99551),(#99552,#99553),
(#99554,#99555),(#99556,#99557),(#99558,#99559),(#99560,#99561),(#99562,
#99563),(#99564,#99565),(#99566,#99567),(#99568,#99569),(#99570,#99571),
(#99572,#99573),(#99574,#99575),(#99576,#99577),(#99578,#99579),(#99580,
#99581),(#99582,#99583),(#99584,#99585),(#99586,#99587),(#99588,#99589),
(#99590,#99591),(#99592,#99593),(#99594,#99595),(#99596,#99597),(#99598,
#99599),(#99600,#99601),(#99602,#99603),(#99604,#99605),(#99606,#99607),
(#99608,#99609),(#99610,#99611),(#99612,#99613),(#99614,#99615),(#99616,
#99617),(#99618,#99619),(#99620,#99621),(#99622,#99623)),.UNSPECIFIED.,
 .F.,.F.,.F.)
B_SPLINE_SURFACE_WITH_KNOTS((6,1,1,1,1,1,1,1,1,1,1,1,1,1,1,1,1,1,1,1,1,
1,1,1,1,1,1,1,1,1,1,1,1,1,1,1,1,1,1,1,1,1,1,1,1,1,1,1,1,1,1,1,1,1,1,1,1,
1,1,1,1,1,1,1,1,1,1,1,1,1,1,1,1,1,1,1,1,1,1,1,1,1,1,1,1,1,1,1,1,1,1,1,1,
1,1,1,1,1,1,1,1,1,1,1,1,1,1,1,1,1,1,1,1,1,1,1,1,1,1,1,1,1,1,1,1,1,1,1,1,
1,1,1,1,1,1,1,1,1,1,1,1,1,1,1,1,1,1,1,1,1,1,1,1,1,1,1,1,1,1,1,1,1,1,1,1,
1,1,1,1,1,1,1,1,1,1,1,1,1,1,1,1,1,1,1,1,1,1,1,1,1,1,1,1,1,1,1,1,1,1,1,6),
(2,2),(0.,0.005,0.01,0.015,0.02,0.025,0.03,0.035,0.04,0.045,0.05,0.055,
0.06,0.065,0.07,0.075,0.08,0.085,0.09,0.095,0.1,0.105,0.11,0.115,0.12,0.125,
0.13,0.135,0.14,0.145,0.15,0.155,0.16,0.165,0.17,0.175,0.18,0.185,0.19,
0.195,0.2,0.205,0.21,0.215,0.22,0.225,0.23,0.235,0.24,0.245,0.25,0.255,
0.26,0.265,0.27,0.275,0.28,0.285,0.29,0.295,0.3,0.305,0.31,0.315,0.32,0.325,
0.33,0.335,0.34,0.345,0.35,0.355,0.36,0.365,0.37,0.375,0.38,0.385,0.39,
0.395,0.4,0.405,0.41,0.415,0.42,0.425,0.43,0.435,0.44,0.445,0.45,0.455,
0.46,0.465,0.47,0.475,0.48,0.485,0.49,0.495,0.5,0.505,0.51,0.515,0.52,0.525,
0.53,0.535,0.54,0.545,0.55,0.555,0.56,0.565,0.57,0.575,0.58,0.585,0.59,
0.595,0.6,0.605,0.61,0.615,0.62,0.625,0.63,0.635,0.64,0.645,0.65,0.655,
0.66,0.665,0.67,0.675,0.68,0.685,0.690000000000001,0.695000000000001,0.700000000000001,
0.705000000000001,0.710000000000001,0.715000000000001,0.720000000000001,
0.725000000000001,0.730000000000001,0.735000000000001,0.740000000000001,
0.745000000000001,0.750000000000001,0.755000000000001,0.760000000000001,
0.765000000000001,0.770000000000001,0.775000000000001,0.780000000000001,
0.785000000000001,0.790000000000001,0.795000000000001,0.800000000000001,
0.805000000000001,0.810000000000001,0.815000000000001,0.820000000000001,
0.825000000000001,0.830000000000001,0.835000000000001,0.840000000000001,
0.845000000000001,0.850000000000001,0.855000000000001,0.860000000000001,
0.865000000000001,0.870000000000001,0.875000000000001,0.880000000000001,
0.885000000000001,0.890000000000001,0.895000000000001,0.900000000000001,
0.905000000000001,0.910000000000001,0.915000000000001,0.920000000000001,
0.925000000000001,0.930000000000001,0.935000000000001,0.940000000000001,
0.945000000000001,0.950000000000001,0.955000000000001,0.960000000000001,
0.965000000000001,0.970000000000001,0.975000000000001,0.980000000000001,
0.985000000000001,0.990000000000001,0.995000000000001,1.),(0.,1.2),
 .UNSPECIFIED.)
GEOMETRIC_REPRESENTATION_ITEM()
RATIONAL_B_SPLINE_SURFACE(((1.,1.),(1.,1.),(1.,1.),(1.,1.),(1.,1.),(1.,
1.),(1.,1.),(1.,1.),(1.,1.),(1.,1.),(1.,1.),(1.,1.),(1.,1.),(1.,1.),(1.,
1.),(1.,1.),(1.,1.),(1.,1.),(1.,1.),(1.,1.),(1.,1.),(1.,1.),(1.,1.),(1.,
1.),(1.,1.),(1.,1.),(1.,1.),(1.,1.),(1.,1.),(1.,1.),(1.,1.),(1.,1.),(1.,
1.),(1.,1.),(1.,1.),(1.,1.),(1.,1.),(1.,1.),(1.,1.),(1.,1.),(1.,1.),(1.,
1.),(1.,1.),(1.,1.),(1.,1.),(1.,1.),(1.,1.),(1.,1.),(1.,1.),(1.,1.),(1.,
1.),(1.,1.),(1.,1.),(1.,1.),(1.,1.),(1.,1.),(1.,1.),(1.,1.),(1.,1.),(1.,
1.),(1.,1.),(1.,1.),(1.,1.),(1.,1.),(1.,1.),(1.,1.),(1.,1.),(1.,1.),(1.,
1.),(1.,1.),(1.,1.),(1.,1.),(1.,1.),(1.,1.),(1.,1.),(1.,1.),(1.,1.),(1.,
1.),(1.,1.),(1.,1.),(1.,1.),(1.,1.),(1.,1.),(1.,1.),(1.,1.),(1.,1.),(1.,
1.),(1.,1.),(1.,1.),(1.,1.),(1.,1.),(1.,1.),(1.,1.),(1.,1.),(1.,1.),(1.,
1.),(1.,1.),(1.,1.),(1.,1.),(1.,1.),(1.,1.),(1.,1.),(1.,1.),(1.,1.),(1.,
1.),(1.,1.),(1.,1.),(1.,1.),(1.,1.),(1.,1.),(1.,1.),(1.,1.),(1.,1.),(1.,
1.),(1.,1.),(1.,1.),(1.,1.),(1.,1.),(1.,1.),(1.,1.),(1.,1.),(1.,1.),(1.,
1.),(1.,1.),(1.,1.),(1.,1.),(1.,1.),(1.,1.),(1.,1.),(1.,1.),(1.,1.),(1.,
1.),(1.,1.),(1.,1.),(1.,1.),(1.,1.),(1.,1.),(1.,1.),(1.,1.),(1.,1.),(1.,
1.),(1.,1.),(1.,1.),(1.,1.),(1.,1.),(1.,1.),(1.,1.),(1.,1.),(1.,1.),(1.,
1.),(1.,1.),(1.,1.),(1.,1.),(1.,1.),(1.,1.),(1.,1.),(1.,1.),(1.,1.),(1.,
1.),(1.,1.),(1.,1.),(1.,1.),(1.,1.),(1.,1.),(1.,1.),(1.,1.),(1.,1.),(1.,
1.),(1.,1.),(1.,1.),(1.,1.),(1.,1.),(1.,1.),(1.,1.),(1.,1.),(1.,1.),(1.,
1.),(1.,1.),(1.,1.),(1.,1.),(1.,1.),(1.,1.),(1.,1.),(1.,1.),(1.,1.),(1.,
1.),(1.,1.),(1.,1.),(1.,1.),(1.,1.),(1.,1.),(1.,1.),(1.,1.),(1.,1.),(1.,
1.),(1.,1.),(1.,1.),(1.,1.),(1.,1.),(1.,1.),(1.,1.),(1.,1.),(1.,1.),(1.,
1.),(1.,1.)))
REPRESENTATION_ITEM('')
SURFACE()
);
#936=(
BOUNDED_SURFACE()
B_SPLINE_SURFACE(5,1,((#100110,#100111),(#100112,#100113),(#100114,#100115),
(#100116,#100117),(#100118,#100119),(#100120,#100121),(#100122,#100123),
(#100124,#100125),(#100126,#100127),(#100128,#100129),(#100130,#100131),
(#100132,#100133),(#100134,#100135),(#100136,#100137),(#100138,#100139),
(#100140,#100141),(#100142,#100143),(#100144,#100145),(#100146,#100147),
(#100148,#100149),(#100150,#100151),(#100152,#100153),(#100154,#100155),
(#100156,#100157),(#100158,#100159),(#100160,#100161),(#100162,#100163),
(#100164,#100165),(#100166,#100167),(#100168,#100169),(#100170,#100171),
(#100172,#100173),(#100174,#100175),(#100176,#100177),(#100178,#100179),
(#100180,#100181),(#100182,#100183),(#100184,#100185),(#100186,#100187),
(#100188,#100189),(#100190,#100191),(#100192,#100193),(#100194,#100195),
(#100196,#100197),(#100198,#100199),(#100200,#100201),(#100202,#100203),
(#100204,#100205),(#100206,#100207),(#100208,#100209),(#100210,#100211),
(#100212,#100213),(#100214,#100215),(#100216,#100217),(#100218,#100219),
(#100220,#100221),(#100222,#100223),(#100224,#100225),(#100226,#100227),
(#100228,#100229),(#100230,#100231),(#100232,#100233),(#100234,#100235),
(#100236,#100237),(#100238,#100239),(#100240,#100241),(#100242,#100243),
(#100244,#100245),(#100246,#100247),(#100248,#100249),(#100250,#100251),
(#100252,#100253),(#100254,#100255),(#100256,#100257),(#100258,#100259),
(#100260,#100261),(#100262,#100263),(#100264,#100265),(#100266,#100267),
(#100268,#100269),(#100270,#100271),(#100272,#100273),(#100274,#100275),
(#100276,#100277),(#100278,#100279),(#100280,#100281),(#100282,#100283),
(#100284,#100285),(#100286,#100287),(#100288,#100289),(#100290,#100291),
(#100292,#100293),(#100294,#100295),(#100296,#100297),(#100298,#100299),
(#100300,#100301),(#100302,#100303),(#100304,#100305),(#100306,#100307),
(#100308,#100309),(#100310,#100311),(#100312,#100313),(#100314,#100315),
(#100316,#100317),(#100318,#100319),(#100320,#100321),(#100322,#100323),
(#100324,#100325),(#100326,#100327),(#100328,#100329),(#100330,#100331),
(#100332,#100333),(#100334,#100335),(#100336,#100337),(#100338,#100339),
(#100340,#100341),(#100342,#100343),(#100344,#100345),(#100346,#100347),
(#100348,#100349),(#100350,#100351),(#100352,#100353),(#100354,#100355),
(#100356,#100357),(#100358,#100359),(#100360,#100361),(#100362,#100363),
(#100364,#100365),(#100366,#100367),(#100368,#100369),(#100370,#100371),
(#100372,#100373),(#100374,#100375),(#100376,#100377),(#100378,#100379),
(#100380,#100381),(#100382,#100383),(#100384,#100385),(#100386,#100387),
(#100388,#100389),(#100390,#100391),(#100392,#100393),(#100394,#100395),
(#100396,#100397),(#100398,#100399),(#100400,#100401),(#100402,#100403),
(#100404,#100405),(#100406,#100407),(#100408,#100409),(#100410,#100411),
(#100412,#100413),(#100414,#100415),(#100416,#100417),(#100418,#100419),
(#100420,#100421),(#100422,#100423),(#100424,#100425),(#100426,#100427),
(#100428,#100429),(#100430,#100431),(#100432,#100433),(#100434,#100435),
(#100436,#100437),(#100438,#100439),(#100440,#100441),(#100442,#100443),
(#100444,#100445),(#100446,#100447),(#100448,#100449),(#100450,#100451),
(#100452,#100453),(#100454,#100455),(#100456,#100457),(#100458,#100459),
(#100460,#100461),(#100462,#100463),(#100464,#100465),(#100466,#100467),
(#100468,#100469),(#100470,#100471),(#100472,#100473),(#100474,#100475),
(#100476,#100477),(#100478,#100479),(#100480,#100481),(#100482,#100483),
(#100484,#100485),(#100486,#100487),(#100488,#100489),(#100490,#100491),
(#100492,#100493),(#100494,#100495),(#100496,#100497),(#100498,#100499),
(#100500,#100501),(#100502,#100503),(#100504,#100505),(#100506,#100507),
(#100508,#100509),(#100510,#100511),(#100512,#100513),(#100514,#100515),
(#100516,#100517),(#100518,#100519)),.UNSPECIFIED.,.F.,.F.,.F.)
B_SPLINE_SURFACE_WITH_KNOTS((6,1,1,1,1,1,1,1,1,1,1,1,1,1,1,1,1,1,1,1,1,
1,1,1,1,1,1,1,1,1,1,1,1,1,1,1,1,1,1,1,1,1,1,1,1,1,1,1,1,1,1,1,1,1,1,1,1,
1,1,1,1,1,1,1,1,1,1,1,1,1,1,1,1,1,1,1,1,1,1,1,1,1,1,1,1,1,1,1,1,1,1,1,1,
1,1,1,1,1,1,1,1,1,1,1,1,1,1,1,1,1,1,1,1,1,1,1,1,1,1,1,1,1,1,1,1,1,1,1,1,
1,1,1,1,1,1,1,1,1,1,1,1,1,1,1,1,1,1,1,1,1,1,1,1,1,1,1,1,1,1,1,1,1,1,1,1,
1,1,1,1,1,1,1,1,1,1,1,1,1,1,1,1,1,1,1,1,1,1,1,1,1,1,1,1,1,1,1,1,1,1,1,6),
(2,2),(0.,0.005,0.01,0.015,0.02,0.025,0.03,0.035,0.04,0.045,0.05,0.055,
0.06,0.065,0.07,0.075,0.08,0.085,0.09,0.095,0.1,0.105,0.11,0.115,0.12,0.125,
0.13,0.135,0.14,0.145,0.15,0.155,0.16,0.165,0.17,0.175,0.18,0.185,0.19,
0.195,0.2,0.205,0.21,0.215,0.22,0.225,0.23,0.235,0.24,0.245,0.25,0.255,
0.26,0.265,0.27,0.275,0.28,0.285,0.29,0.295,0.3,0.305,0.31,0.315,0.32,0.325,
0.33,0.335,0.34,0.345,0.35,0.355,0.36,0.365,0.37,0.375,0.38,0.385,0.39,
0.395,0.4,0.405,0.41,0.415,0.42,0.425,0.43,0.435,0.44,0.445,0.45,0.455,
0.46,0.465,0.47,0.475,0.48,0.485,0.49,0.495,0.5,0.505,0.51,0.515,0.52,0.525,
0.53,0.535,0.54,0.545,0.55,0.555,0.56,0.565,0.57,0.575,0.58,0.585,0.59,
0.595,0.6,0.605,0.61,0.615,0.62,0.625,0.63,0.635,0.64,0.645,0.65,0.655,
0.66,0.665,0.67,0.675,0.68,0.685,0.690000000000001,0.695000000000001,0.700000000000001,
0.705000000000001,0.710000000000001,0.715000000000001,0.720000000000001,
0.725000000000001,0.730000000000001,0.735000000000001,0.740000000000001,
0.745000000000001,0.750000000000001,0.755000000000001,0.760000000000001,
0.765000000000001,0.770000000000001,0.775000000000001,0.780000000000001,
0.785000000000001,0.790000000000001,0.795000000000001,0.800000000000001,
0.805000000000001,0.810000000000001,0.815000000000001,0.820000000000001,
0.825000000000001,0.830000000000001,0.835000000000001,0.840000000000001,
0.845000000000001,0.850000000000001,0.855000000000001,0.860000000000001,
0.865000000000001,0.870000000000001,0.875000000000001,0.880000000000001,
0.885000000000001,0.890000000000001,0.895000000000001,0.900000000000001,
0.905000000000001,0.910000000000001,0.915000000000001,0.920000000000001,
0.925000000000001,0.930000000000001,0.935000000000001,0.940000000000001,
0.945000000000001,0.950000000000001,0.955000000000001,0.960000000000001,
0.965000000000001,0.970000000000001,0.975000000000001,0.980000000000001,
0.985000000000001,0.990000000000001,0.995000000000001,1.),(0.,1.2),
 .UNSPECIFIED.)
GEOMETRIC_REPRESENTATION_ITEM()
RATIONAL_B_SPLINE_SURFACE(((1.,1.),(1.,1.),(1.,1.),(1.,1.),(1.,1.),(1.,
1.),(1.,1.),(1.,1.),(1.,1.),(1.,1.),(1.,1.),(1.,1.),(1.,1.),(1.,1.),(1.,
1.),(1.,1.),(1.,1.),(1.,1.),(1.,1.),(1.,1.),(1.,1.),(1.,1.),(1.,1.),(1.,
1.),(1.,1.),(1.,1.),(1.,1.),(1.,1.),(1.,1.),(1.,1.),(1.,1.),(1.,1.),(1.,
1.),(1.,1.),(1.,1.),(1.,1.),(1.,1.),(1.,1.),(1.,1.),(1.,1.),(1.,1.),(1.,
1.),(1.,1.),(1.,1.),(1.,1.),(1.,1.),(1.,1.),(1.,1.),(1.,1.),(1.,1.),(1.,
1.),(1.,1.),(1.,1.),(1.,1.),(1.,1.),(1.,1.),(1.,1.),(1.,1.),(1.,1.),(1.,
1.),(1.,1.),(1.,1.),(1.,1.),(1.,1.),(1.,1.),(1.,1.),(1.,1.),(1.,1.),(1.,
1.),(1.,1.),(1.,1.),(1.,1.),(1.,1.),(1.,1.),(1.,1.),(1.,1.),(1.,1.),(1.,
1.),(1.,1.),(1.,1.),(1.,1.),(1.,1.),(1.,1.),(1.,1.),(1.,1.),(1.,1.),(1.,
1.),(1.,1.),(1.,1.),(1.,1.),(1.,1.),(1.,1.),(1.,1.),(1.,1.),(1.,1.),(1.,
1.),(1.,1.),(1.,1.),(1.,1.),(1.,1.),(1.,1.),(1.,1.),(1.,1.),(1.,1.),(1.,
1.),(1.,1.),(1.,1.),(1.,1.),(1.,1.),(1.,1.),(1.,1.),(1.,1.),(1.,1.),(1.,
1.),(1.,1.),(1.,1.),(1.,1.),(1.,1.),(1.,1.),(1.,1.),(1.,1.),(1.,1.),(1.,
1.),(1.,1.),(1.,1.),(1.,1.),(1.,1.),(1.,1.),(1.,1.),(1.,1.),(1.,1.),(1.,
1.),(1.,1.),(1.,1.),(1.,1.),(1.,1.),(1.,1.),(1.,1.),(1.,1.),(1.,1.),(1.,
1.),(1.,1.),(1.,1.),(1.,1.),(1.,1.),(1.,1.),(1.,1.),(1.,1.),(1.,1.),(1.,
1.),(1.,1.),(1.,1.),(1.,1.),(1.,1.),(1.,1.),(1.,1.),(1.,1.),(1.,1.),(1.,
1.),(1.,1.),(1.,1.),(1.,1.),(1.,1.),(1.,1.),(1.,1.),(1.,1.),(1.,1.),(1.,
1.),(1.,1.),(1.,1.),(1.,1.),(1.,1.),(1.,1.),(1.,1.),(1.,1.),(1.,1.),(1.,
1.),(1.,1.),(1.,1.),(1.,1.),(1.,1.),(1.,1.),(1.,1.),(1.,1.),(1.,1.),(1.,
1.),(1.,1.),(1.,1.),(1.,1.),(1.,1.),(1.,1.),(1.,1.),(1.,1.),(1.,1.),(1.,
1.),(1.,1.),(1.,1.),(1.,1.),(1.,1.),(1.,1.),(1.,1.),(1.,1.),(1.,1.),(1.,
1.),(1.,1.)))
REPRESENTATION_ITEM('')
SURFACE()
);
#937=(
BOUNDED_SURFACE()
B_SPLINE_SURFACE(5,1,((#101006,#101007),(#101008,#101009),(#101010,#101011),
(#101012,#101013),(#101014,#101015),(#101016,#101017),(#101018,#101019),
(#101020,#101021),(#101022,#101023),(#101024,#101025),(#101026,#101027),
(#101028,#101029),(#101030,#101031),(#101032,#101033),(#101034,#101035),
(#101036,#101037),(#101038,#101039),(#101040,#101041),(#101042,#101043),
(#101044,#101045),(#101046,#101047),(#101048,#101049),(#101050,#101051),
(#101052,#101053),(#101054,#101055),(#101056,#101057),(#101058,#101059),
(#101060,#101061),(#101062,#101063),(#101064,#101065),(#101066,#101067),
(#101068,#101069),(#101070,#101071),(#101072,#101073),(#101074,#101075),
(#101076,#101077),(#101078,#101079),(#101080,#101081),(#101082,#101083),
(#101084,#101085),(#101086,#101087),(#101088,#101089),(#101090,#101091),
(#101092,#101093),(#101094,#101095),(#101096,#101097),(#101098,#101099),
(#101100,#101101),(#101102,#101103),(#101104,#101105),(#101106,#101107),
(#101108,#101109),(#101110,#101111),(#101112,#101113),(#101114,#101115),
(#101116,#101117),(#101118,#101119),(#101120,#101121),(#101122,#101123),
(#101124,#101125),(#101126,#101127),(#101128,#101129),(#101130,#101131),
(#101132,#101133),(#101134,#101135),(#101136,#101137),(#101138,#101139),
(#101140,#101141),(#101142,#101143),(#101144,#101145),(#101146,#101147),
(#101148,#101149),(#101150,#101151),(#101152,#101153),(#101154,#101155),
(#101156,#101157),(#101158,#101159),(#101160,#101161),(#101162,#101163),
(#101164,#101165),(#101166,#101167),(#101168,#101169),(#101170,#101171),
(#101172,#101173),(#101174,#101175),(#101176,#101177),(#101178,#101179),
(#101180,#101181),(#101182,#101183),(#101184,#101185),(#101186,#101187),
(#101188,#101189),(#101190,#101191),(#101192,#101193),(#101194,#101195),
(#101196,#101197),(#101198,#101199),(#101200,#101201),(#101202,#101203),
(#101204,#101205),(#101206,#101207),(#101208,#101209),(#101210,#101211),
(#101212,#101213),(#101214,#101215),(#101216,#101217),(#101218,#101219),
(#101220,#101221),(#101222,#101223),(#101224,#101225),(#101226,#101227),
(#101228,#101229),(#101230,#101231),(#101232,#101233),(#101234,#101235),
(#101236,#101237),(#101238,#101239),(#101240,#101241),(#101242,#101243),
(#101244,#101245),(#101246,#101247),(#101248,#101249),(#101250,#101251),
(#101252,#101253),(#101254,#101255),(#101256,#101257),(#101258,#101259),
(#101260,#101261),(#101262,#101263),(#101264,#101265),(#101266,#101267),
(#101268,#101269),(#101270,#101271),(#101272,#101273),(#101274,#101275),
(#101276,#101277),(#101278,#101279),(#101280,#101281),(#101282,#101283),
(#101284,#101285),(#101286,#101287),(#101288,#101289),(#101290,#101291),
(#101292,#101293),(#101294,#101295),(#101296,#101297),(#101298,#101299),
(#101300,#101301),(#101302,#101303),(#101304,#101305),(#101306,#101307),
(#101308,#101309),(#101310,#101311),(#101312,#101313),(#101314,#101315),
(#101316,#101317),(#101318,#101319),(#101320,#101321),(#101322,#101323),
(#101324,#101325),(#101326,#101327),(#101328,#101329),(#101330,#101331),
(#101332,#101333),(#101334,#101335),(#101336,#101337),(#101338,#101339),
(#101340,#101341),(#101342,#101343),(#101344,#101345),(#101346,#101347),
(#101348,#101349),(#101350,#101351),(#101352,#101353),(#101354,#101355),
(#101356,#101357),(#101358,#101359),(#101360,#101361),(#101362,#101363),
(#101364,#101365),(#101366,#101367),(#101368,#101369),(#101370,#101371),
(#101372,#101373),(#101374,#101375),(#101376,#101377),(#101378,#101379),
(#101380,#101381),(#101382,#101383),(#101384,#101385),(#101386,#101387),
(#101388,#101389),(#101390,#101391),(#101392,#101393),(#101394,#101395),
(#101396,#101397),(#101398,#101399),(#101400,#101401),(#101402,#101403),
(#101404,#101405),(#101406,#101407),(#101408,#101409),(#101410,#101411),
(#101412,#101413),(#101414,#101415)),.UNSPECIFIED.,.F.,.F.,.F.)
B_SPLINE_SURFACE_WITH_KNOTS((6,1,1,1,1,1,1,1,1,1,1,1,1,1,1,1,1,1,1,1,1,
1,1,1,1,1,1,1,1,1,1,1,1,1,1,1,1,1,1,1,1,1,1,1,1,1,1,1,1,1,1,1,1,1,1,1,1,
1,1,1,1,1,1,1,1,1,1,1,1,1,1,1,1,1,1,1,1,1,1,1,1,1,1,1,1,1,1,1,1,1,1,1,1,
1,1,1,1,1,1,1,1,1,1,1,1,1,1,1,1,1,1,1,1,1,1,1,1,1,1,1,1,1,1,1,1,1,1,1,1,
1,1,1,1,1,1,1,1,1,1,1,1,1,1,1,1,1,1,1,1,1,1,1,1,1,1,1,1,1,1,1,1,1,1,1,1,
1,1,1,1,1,1,1,1,1,1,1,1,1,1,1,1,1,1,1,1,1,1,1,1,1,1,1,1,1,1,1,1,1,1,1,6),
(2,2),(0.,0.005,0.01,0.015,0.02,0.025,0.03,0.035,0.04,0.045,0.05,0.055,
0.06,0.065,0.07,0.075,0.08,0.085,0.09,0.095,0.1,0.105,0.11,0.115,0.12,0.125,
0.13,0.135,0.14,0.145,0.15,0.155,0.16,0.165,0.17,0.175,0.18,0.185,0.19,
0.195,0.2,0.205,0.21,0.215,0.22,0.225,0.23,0.235,0.24,0.245,0.25,0.255,
0.26,0.265,0.27,0.275,0.28,0.285,0.29,0.295,0.3,0.305,0.31,0.315,0.32,0.325,
0.33,0.335,0.34,0.345,0.35,0.355,0.36,0.365,0.37,0.375,0.38,0.385,0.39,
0.395,0.4,0.405,0.41,0.415,0.42,0.425,0.43,0.435,0.44,0.445,0.45,0.455,
0.46,0.465,0.47,0.475,0.48,0.485,0.49,0.495,0.5,0.505,0.51,0.515,0.52,0.525,
0.53,0.535,0.54,0.545,0.55,0.555,0.56,0.565,0.57,0.575,0.58,0.585,0.59,
0.595,0.6,0.605,0.61,0.615,0.62,0.625,0.63,0.635,0.64,0.645,0.65,0.655,
0.66,0.665,0.67,0.675,0.68,0.685,0.690000000000001,0.695000000000001,0.700000000000001,
0.705000000000001,0.710000000000001,0.715000000000001,0.720000000000001,
0.725000000000001,0.730000000000001,0.735000000000001,0.740000000000001,
0.745000000000001,0.750000000000001,0.755000000000001,0.760000000000001,
0.765000000000001,0.770000000000001,0.775000000000001,0.780000000000001,
0.785000000000001,0.790000000000001,0.795000000000001,0.800000000000001,
0.805000000000001,0.810000000000001,0.815000000000001,0.820000000000001,
0.825000000000001,0.830000000000001,0.835000000000001,0.840000000000001,
0.845000000000001,0.850000000000001,0.855000000000001,0.860000000000001,
0.865000000000001,0.870000000000001,0.875000000000001,0.880000000000001,
0.885000000000001,0.890000000000001,0.895000000000001,0.900000000000001,
0.905000000000001,0.910000000000001,0.915000000000001,0.920000000000001,
0.925000000000001,0.930000000000001,0.935000000000001,0.940000000000001,
0.945000000000001,0.950000000000001,0.955000000000001,0.960000000000001,
0.965000000000001,0.970000000000001,0.975000000000001,0.980000000000001,
0.985000000000001,0.990000000000001,0.995000000000001,1.),(0.,1.2),
 .UNSPECIFIED.)
GEOMETRIC_REPRESENTATION_ITEM()
RATIONAL_B_SPLINE_SURFACE(((1.,1.),(1.,1.),(1.,1.),(1.,1.),(1.,1.),(1.,
1.),(1.,1.),(1.,1.),(1.,1.),(1.,1.),(1.,1.),(1.,1.),(1.,1.),(1.,1.),(1.,
1.),(1.,1.),(1.,1.),(1.,1.),(1.,1.),(1.,1.),(1.,1.),(1.,1.),(1.,1.),(1.,
1.),(1.,1.),(1.,1.),(1.,1.),(1.,1.),(1.,1.),(1.,1.),(1.,1.),(1.,1.),(1.,
1.),(1.,1.),(1.,1.),(1.,1.),(1.,1.),(1.,1.),(1.,1.),(1.,1.),(1.,1.),(1.,
1.),(1.,1.),(1.,1.),(1.,1.),(1.,1.),(1.,1.),(1.,1.),(1.,1.),(1.,1.),(1.,
1.),(1.,1.),(1.,1.),(1.,1.),(1.,1.),(1.,1.),(1.,1.),(1.,1.),(1.,1.),(1.,
1.),(1.,1.),(1.,1.),(1.,1.),(1.,1.),(1.,1.),(1.,1.),(1.,1.),(1.,1.),(1.,
1.),(1.,1.),(1.,1.),(1.,1.),(1.,1.),(1.,1.),(1.,1.),(1.,1.),(1.,1.),(1.,
1.),(1.,1.),(1.,1.),(1.,1.),(1.,1.),(1.,1.),(1.,1.),(1.,1.),(1.,1.),(1.,
1.),(1.,1.),(1.,1.),(1.,1.),(1.,1.),(1.,1.),(1.,1.),(1.,1.),(1.,1.),(1.,
1.),(1.,1.),(1.,1.),(1.,1.),(1.,1.),(1.,1.),(1.,1.),(1.,1.),(1.,1.),(1.,
1.),(1.,1.),(1.,1.),(1.,1.),(1.,1.),(1.,1.),(1.,1.),(1.,1.),(1.,1.),(1.,
1.),(1.,1.),(1.,1.),(1.,1.),(1.,1.),(1.,1.),(1.,1.),(1.,1.),(1.,1.),(1.,
1.),(1.,1.),(1.,1.),(1.,1.),(1.,1.),(1.,1.),(1.,1.),(1.,1.),(1.,1.),(1.,
1.),(1.,1.),(1.,1.),(1.,1.),(1.,1.),(1.,1.),(1.,1.),(1.,1.),(1.,1.),(1.,
1.),(1.,1.),(1.,1.),(1.,1.),(1.,1.),(1.,1.),(1.,1.),(1.,1.),(1.,1.),(1.,
1.),(1.,1.),(1.,1.),(1.,1.),(1.,1.),(1.,1.),(1.,1.),(1.,1.),(1.,1.),(1.,
1.),(1.,1.),(1.,1.),(1.,1.),(1.,1.),(1.,1.),(1.,1.),(1.,1.),(1.,1.),(1.,
1.),(1.,1.),(1.,1.),(1.,1.),(1.,1.),(1.,1.),(1.,1.),(1.,1.),(1.,1.),(1.,
1.),(1.,1.),(1.,1.),(1.,1.),(1.,1.),(1.,1.),(1.,1.),(1.,1.),(1.,1.),(1.,
1.),(1.,1.),(1.,1.),(1.,1.),(1.,1.),(1.,1.),(1.,1.),(1.,1.),(1.,1.),(1.,
1.),(1.,1.),(1.,1.),(1.,1.),(1.,1.),(1.,1.),(1.,1.),(1.,1.),(1.,1.),(1.,
1.),(1.,1.)))
REPRESENTATION_ITEM('')
SURFACE()
);
#938=(
BOUNDED_SURFACE()
B_SPLINE_SURFACE(5,1,((#101902,#101903),(#101904,#101905),(#101906,#101907),
(#101908,#101909),(#101910,#101911),(#101912,#101913),(#101914,#101915),
(#101916,#101917),(#101918,#101919),(#101920,#101921),(#101922,#101923),
(#101924,#101925),(#101926,#101927),(#101928,#101929),(#101930,#101931),
(#101932,#101933),(#101934,#101935),(#101936,#101937),(#101938,#101939),
(#101940,#101941),(#101942,#101943),(#101944,#101945),(#101946,#101947),
(#101948,#101949),(#101950,#101951),(#101952,#101953),(#101954,#101955),
(#101956,#101957),(#101958,#101959),(#101960,#101961),(#101962,#101963),
(#101964,#101965),(#101966,#101967),(#101968,#101969),(#101970,#101971),
(#101972,#101973),(#101974,#101975),(#101976,#101977),(#101978,#101979),
(#101980,#101981),(#101982,#101983),(#101984,#101985),(#101986,#101987),
(#101988,#101989),(#101990,#101991),(#101992,#101993),(#101994,#101995),
(#101996,#101997),(#101998,#101999),(#102000,#102001),(#102002,#102003),
(#102004,#102005),(#102006,#102007),(#102008,#102009),(#102010,#102011),
(#102012,#102013),(#102014,#102015),(#102016,#102017),(#102018,#102019),
(#102020,#102021),(#102022,#102023),(#102024,#102025),(#102026,#102027),
(#102028,#102029),(#102030,#102031),(#102032,#102033),(#102034,#102035),
(#102036,#102037),(#102038,#102039),(#102040,#102041),(#102042,#102043),
(#102044,#102045),(#102046,#102047),(#102048,#102049),(#102050,#102051),
(#102052,#102053),(#102054,#102055),(#102056,#102057),(#102058,#102059),
(#102060,#102061),(#102062,#102063),(#102064,#102065),(#102066,#102067),
(#102068,#102069),(#102070,#102071),(#102072,#102073),(#102074,#102075),
(#102076,#102077),(#102078,#102079),(#102080,#102081),(#102082,#102083),
(#102084,#102085),(#102086,#102087),(#102088,#102089),(#102090,#102091),
(#102092,#102093),(#102094,#102095),(#102096,#102097),(#102098,#102099),
(#102100,#102101),(#102102,#102103),(#102104,#102105),(#102106,#102107),
(#102108,#102109),(#102110,#102111),(#102112,#102113),(#102114,#102115),
(#102116,#102117),(#102118,#102119),(#102120,#102121),(#102122,#102123),
(#102124,#102125),(#102126,#102127),(#102128,#102129),(#102130,#102131),
(#102132,#102133),(#102134,#102135),(#102136,#102137),(#102138,#102139),
(#102140,#102141),(#102142,#102143),(#102144,#102145),(#102146,#102147),
(#102148,#102149),(#102150,#102151),(#102152,#102153),(#102154,#102155),
(#102156,#102157),(#102158,#102159),(#102160,#102161),(#102162,#102163),
(#102164,#102165),(#102166,#102167),(#102168,#102169),(#102170,#102171),
(#102172,#102173),(#102174,#102175),(#102176,#102177),(#102178,#102179),
(#102180,#102181),(#102182,#102183),(#102184,#102185),(#102186,#102187),
(#102188,#102189),(#102190,#102191),(#102192,#102193),(#102194,#102195),
(#102196,#102197),(#102198,#102199),(#102200,#102201),(#102202,#102203),
(#102204,#102205),(#102206,#102207),(#102208,#102209),(#102210,#102211),
(#102212,#102213),(#102214,#102215),(#102216,#102217),(#102218,#102219),
(#102220,#102221),(#102222,#102223),(#102224,#102225),(#102226,#102227),
(#102228,#102229),(#102230,#102231),(#102232,#102233),(#102234,#102235),
(#102236,#102237),(#102238,#102239),(#102240,#102241),(#102242,#102243),
(#102244,#102245),(#102246,#102247),(#102248,#102249),(#102250,#102251),
(#102252,#102253),(#102254,#102255),(#102256,#102257),(#102258,#102259),
(#102260,#102261),(#102262,#102263),(#102264,#102265),(#102266,#102267),
(#102268,#102269),(#102270,#102271),(#102272,#102273),(#102274,#102275),
(#102276,#102277),(#102278,#102279),(#102280,#102281),(#102282,#102283),
(#102284,#102285),(#102286,#102287),(#102288,#102289),(#102290,#102291),
(#102292,#102293),(#102294,#102295),(#102296,#102297),(#102298,#102299),
(#102300,#102301),(#102302,#102303),(#102304,#102305),(#102306,#102307),
(#102308,#102309),(#102310,#102311)),.UNSPECIFIED.,.F.,.F.,.F.)
B_SPLINE_SURFACE_WITH_KNOTS((6,1,1,1,1,1,1,1,1,1,1,1,1,1,1,1,1,1,1,1,1,
1,1,1,1,1,1,1,1,1,1,1,1,1,1,1,1,1,1,1,1,1,1,1,1,1,1,1,1,1,1,1,1,1,1,1,1,
1,1,1,1,1,1,1,1,1,1,1,1,1,1,1,1,1,1,1,1,1,1,1,1,1,1,1,1,1,1,1,1,1,1,1,1,
1,1,1,1,1,1,1,1,1,1,1,1,1,1,1,1,1,1,1,1,1,1,1,1,1,1,1,1,1,1,1,1,1,1,1,1,
1,1,1,1,1,1,1,1,1,1,1,1,1,1,1,1,1,1,1,1,1,1,1,1,1,1,1,1,1,1,1,1,1,1,1,1,
1,1,1,1,1,1,1,1,1,1,1,1,1,1,1,1,1,1,1,1,1,1,1,1,1,1,1,1,1,1,1,1,1,1,1,6),
(2,2),(0.,0.005,0.01,0.015,0.02,0.025,0.03,0.035,0.04,0.045,0.05,0.055,
0.06,0.065,0.07,0.075,0.08,0.085,0.09,0.095,0.1,0.105,0.11,0.115,0.12,0.125,
0.13,0.135,0.14,0.145,0.15,0.155,0.16,0.165,0.17,0.175,0.18,0.185,0.19,
0.195,0.2,0.205,0.21,0.215,0.22,0.225,0.23,0.235,0.24,0.245,0.25,0.255,
0.26,0.265,0.27,0.275,0.28,0.285,0.29,0.295,0.3,0.305,0.31,0.315,0.32,0.325,
0.33,0.335,0.34,0.345,0.35,0.355,0.36,0.365,0.37,0.375,0.38,0.385,0.39,
0.395,0.4,0.405,0.41,0.415,0.42,0.425,0.43,0.435,0.44,0.445,0.45,0.455,
0.46,0.465,0.47,0.475,0.48,0.485,0.49,0.495,0.5,0.505,0.51,0.515,0.52,0.525,
0.53,0.535,0.54,0.545,0.55,0.555,0.56,0.565,0.57,0.575,0.58,0.585,0.59,
0.595,0.6,0.605,0.61,0.615,0.62,0.625,0.63,0.635,0.64,0.645,0.65,0.655,
0.66,0.665,0.67,0.675,0.68,0.685,0.690000000000001,0.695000000000001,0.700000000000001,
0.705000000000001,0.710000000000001,0.715000000000001,0.720000000000001,
0.725000000000001,0.730000000000001,0.735000000000001,0.740000000000001,
0.745000000000001,0.750000000000001,0.755000000000001,0.760000000000001,
0.765000000000001,0.770000000000001,0.775000000000001,0.780000000000001,
0.785000000000001,0.790000000000001,0.795000000000001,0.800000000000001,
0.805000000000001,0.810000000000001,0.815000000000001,0.820000000000001,
0.825000000000001,0.830000000000001,0.835000000000001,0.840000000000001,
0.845000000000001,0.850000000000001,0.855000000000001,0.860000000000001,
0.865000000000001,0.870000000000001,0.875000000000001,0.880000000000001,
0.885000000000001,0.890000000000001,0.895000000000001,0.900000000000001,
0.905000000000001,0.910000000000001,0.915000000000001,0.920000000000001,
0.925000000000001,0.930000000000001,0.935000000000001,0.940000000000001,
0.945000000000001,0.950000000000001,0.955000000000001,0.960000000000001,
0.965000000000001,0.970000000000001,0.975000000000001,0.980000000000001,
0.985000000000001,0.990000000000001,0.995000000000001,1.),(0.,1.2),
 .UNSPECIFIED.)
GEOMETRIC_REPRESENTATION_ITEM()
RATIONAL_B_SPLINE_SURFACE(((1.,1.),(1.,1.),(1.,1.),(1.,1.),(1.,1.),(1.,
1.),(1.,1.),(1.,1.),(1.,1.),(1.,1.),(1.,1.),(1.,1.),(1.,1.),(1.,1.),(1.,
1.),(1.,1.),(1.,1.),(1.,1.),(1.,1.),(1.,1.),(1.,1.),(1.,1.),(1.,1.),(1.,
1.),(1.,1.),(1.,1.),(1.,1.),(1.,1.),(1.,1.),(1.,1.),(1.,1.),(1.,1.),(1.,
1.),(1.,1.),(1.,1.),(1.,1.),(1.,1.),(1.,1.),(1.,1.),(1.,1.),(1.,1.),(1.,
1.),(1.,1.),(1.,1.),(1.,1.),(1.,1.),(1.,1.),(1.,1.),(1.,1.),(1.,1.),(1.,
1.),(1.,1.),(1.,1.),(1.,1.),(1.,1.),(1.,1.),(1.,1.),(1.,1.),(1.,1.),(1.,
1.),(1.,1.),(1.,1.),(1.,1.),(1.,1.),(1.,1.),(1.,1.),(1.,1.),(1.,1.),(1.,
1.),(1.,1.),(1.,1.),(1.,1.),(1.,1.),(1.,1.),(1.,1.),(1.,1.),(1.,1.),(1.,
1.),(1.,1.),(1.,1.),(1.,1.),(1.,1.),(1.,1.),(1.,1.),(1.,1.),(1.,1.),(1.,
1.),(1.,1.),(1.,1.),(1.,1.),(1.,1.),(1.,1.),(1.,1.),(1.,1.),(1.,1.),(1.,
1.),(1.,1.),(1.,1.),(1.,1.),(1.,1.),(1.,1.),(1.,1.),(1.,1.),(1.,1.),(1.,
1.),(1.,1.),(1.,1.),(1.,1.),(1.,1.),(1.,1.),(1.,1.),(1.,1.),(1.,1.),(1.,
1.),(1.,1.),(1.,1.),(1.,1.),(1.,1.),(1.,1.),(1.,1.),(1.,1.),(1.,1.),(1.,
1.),(1.,1.),(1.,1.),(1.,1.),(1.,1.),(1.,1.),(1.,1.),(1.,1.),(1.,1.),(1.,
1.),(1.,1.),(1.,1.),(1.,1.),(1.,1.),(1.,1.),(1.,1.),(1.,1.),(1.,1.),(1.,
1.),(1.,1.),(1.,1.),(1.,1.),(1.,1.),(1.,1.),(1.,1.),(1.,1.),(1.,1.),(1.,
1.),(1.,1.),(1.,1.),(1.,1.),(1.,1.),(1.,1.),(1.,1.),(1.,1.),(1.,1.),(1.,
1.),(1.,1.),(1.,1.),(1.,1.),(1.,1.),(1.,1.),(1.,1.),(1.,1.),(1.,1.),(1.,
1.),(1.,1.),(1.,1.),(1.,1.),(1.,1.),(1.,1.),(1.,1.),(1.,1.),(1.,1.),(1.,
1.),(1.,1.),(1.,1.),(1.,1.),(1.,1.),(1.,1.),(1.,1.),(1.,1.),(1.,1.),(1.,
1.),(1.,1.),(1.,1.),(1.,1.),(1.,1.),(1.,1.),(1.,1.),(1.,1.),(1.,1.),(1.,
1.),(1.,1.),(1.,1.),(1.,1.),(1.,1.),(1.,1.),(1.,1.),(1.,1.),(1.,1.),(1.,
1.),(1.,1.)))
REPRESENTATION_ITEM('')
SURFACE()
);
#939=(
BOUNDED_SURFACE()
B_SPLINE_SURFACE(5,1,((#102798,#102799),(#102800,#102801),(#102802,#102803),
(#102804,#102805),(#102806,#102807),(#102808,#102809),(#102810,#102811),
(#102812,#102813),(#102814,#102815),(#102816,#102817),(#102818,#102819),
(#102820,#102821),(#102822,#102823),(#102824,#102825),(#102826,#102827),
(#102828,#102829),(#102830,#102831),(#102832,#102833),(#102834,#102835),
(#102836,#102837),(#102838,#102839),(#102840,#102841),(#102842,#102843),
(#102844,#102845),(#102846,#102847),(#102848,#102849),(#102850,#102851),
(#102852,#102853),(#102854,#102855),(#102856,#102857),(#102858,#102859),
(#102860,#102861),(#102862,#102863),(#102864,#102865),(#102866,#102867),
(#102868,#102869),(#102870,#102871),(#102872,#102873),(#102874,#102875),
(#102876,#102877),(#102878,#102879),(#102880,#102881),(#102882,#102883),
(#102884,#102885),(#102886,#102887),(#102888,#102889),(#102890,#102891),
(#102892,#102893),(#102894,#102895),(#102896,#102897),(#102898,#102899),
(#102900,#102901),(#102902,#102903),(#102904,#102905),(#102906,#102907),
(#102908,#102909),(#102910,#102911),(#102912,#102913),(#102914,#102915),
(#102916,#102917),(#102918,#102919),(#102920,#102921),(#102922,#102923),
(#102924,#102925),(#102926,#102927),(#102928,#102929),(#102930,#102931),
(#102932,#102933),(#102934,#102935),(#102936,#102937),(#102938,#102939),
(#102940,#102941),(#102942,#102943),(#102944,#102945),(#102946,#102947),
(#102948,#102949),(#102950,#102951),(#102952,#102953),(#102954,#102955),
(#102956,#102957),(#102958,#102959),(#102960,#102961),(#102962,#102963),
(#102964,#102965),(#102966,#102967),(#102968,#102969),(#102970,#102971),
(#102972,#102973),(#102974,#102975),(#102976,#102977),(#102978,#102979),
(#102980,#102981),(#102982,#102983),(#102984,#102985),(#102986,#102987),
(#102988,#102989),(#102990,#102991),(#102992,#102993),(#102994,#102995),
(#102996,#102997),(#102998,#102999),(#103000,#103001),(#103002,#103003),
(#103004,#103005),(#103006,#103007),(#103008,#103009),(#103010,#103011),
(#103012,#103013),(#103014,#103015),(#103016,#103017),(#103018,#103019),
(#103020,#103021),(#103022,#103023),(#103024,#103025),(#103026,#103027),
(#103028,#103029),(#103030,#103031),(#103032,#103033),(#103034,#103035),
(#103036,#103037),(#103038,#103039),(#103040,#103041),(#103042,#103043),
(#103044,#103045),(#103046,#103047),(#103048,#103049),(#103050,#103051),
(#103052,#103053),(#103054,#103055),(#103056,#103057),(#103058,#103059),
(#103060,#103061),(#103062,#103063),(#103064,#103065),(#103066,#103067),
(#103068,#103069),(#103070,#103071),(#103072,#103073),(#103074,#103075),
(#103076,#103077),(#103078,#103079),(#103080,#103081),(#103082,#103083),
(#103084,#103085),(#103086,#103087),(#103088,#103089),(#103090,#103091),
(#103092,#103093),(#103094,#103095),(#103096,#103097),(#103098,#103099),
(#103100,#103101),(#103102,#103103),(#103104,#103105),(#103106,#103107),
(#103108,#103109),(#103110,#103111),(#103112,#103113),(#103114,#103115),
(#103116,#103117),(#103118,#103119),(#103120,#103121),(#103122,#103123),
(#103124,#103125),(#103126,#103127),(#103128,#103129),(#103130,#103131),
(#103132,#103133),(#103134,#103135),(#103136,#103137),(#103138,#103139),
(#103140,#103141),(#103142,#103143),(#103144,#103145),(#103146,#103147),
(#103148,#103149),(#103150,#103151),(#103152,#103153),(#103154,#103155),
(#103156,#103157),(#103158,#103159),(#103160,#103161),(#103162,#103163),
(#103164,#103165),(#103166,#103167),(#103168,#103169),(#103170,#103171),
(#103172,#103173),(#103174,#103175),(#103176,#103177),(#103178,#103179),
(#103180,#103181),(#103182,#103183),(#103184,#103185),(#103186,#103187),
(#103188,#103189),(#103190,#103191),(#103192,#103193),(#103194,#103195),
(#103196,#103197),(#103198,#103199),(#103200,#103201),(#103202,#103203),
(#103204,#103205),(#103206,#103207)),.UNSPECIFIED.,.F.,.F.,.F.)
B_SPLINE_SURFACE_WITH_KNOTS((6,1,1,1,1,1,1,1,1,1,1,1,1,1,1,1,1,1,1,1,1,
1,1,1,1,1,1,1,1,1,1,1,1,1,1,1,1,1,1,1,1,1,1,1,1,1,1,1,1,1,1,1,1,1,1,1,1,
1,1,1,1,1,1,1,1,1,1,1,1,1,1,1,1,1,1,1,1,1,1,1,1,1,1,1,1,1,1,1,1,1,1,1,1,
1,1,1,1,1,1,1,1,1,1,1,1,1,1,1,1,1,1,1,1,1,1,1,1,1,1,1,1,1,1,1,1,1,1,1,1,
1,1,1,1,1,1,1,1,1,1,1,1,1,1,1,1,1,1,1,1,1,1,1,1,1,1,1,1,1,1,1,1,1,1,1,1,
1,1,1,1,1,1,1,1,1,1,1,1,1,1,1,1,1,1,1,1,1,1,1,1,1,1,1,1,1,1,1,1,1,1,1,6),
(2,2),(0.,0.005,0.01,0.015,0.02,0.025,0.03,0.035,0.04,0.045,0.05,0.055,
0.06,0.065,0.07,0.075,0.08,0.085,0.09,0.095,0.1,0.105,0.11,0.115,0.12,0.125,
0.13,0.135,0.14,0.145,0.15,0.155,0.16,0.165,0.17,0.175,0.18,0.185,0.19,
0.195,0.2,0.205,0.21,0.215,0.22,0.225,0.23,0.235,0.24,0.245,0.25,0.255,
0.26,0.265,0.27,0.275,0.28,0.285,0.29,0.295,0.3,0.305,0.31,0.315,0.32,0.325,
0.33,0.335,0.34,0.345,0.35,0.355,0.36,0.365,0.37,0.375,0.38,0.385,0.39,
0.395,0.4,0.405,0.41,0.415,0.42,0.425,0.43,0.435,0.44,0.445,0.45,0.455,
0.46,0.465,0.47,0.475,0.48,0.485,0.49,0.495,0.5,0.505,0.51,0.515,0.52,0.525,
0.53,0.535,0.54,0.545,0.55,0.555,0.56,0.565,0.57,0.575,0.58,0.585,0.59,
0.595,0.6,0.605,0.61,0.615,0.62,0.625,0.63,0.635,0.64,0.645,0.65,0.655,
0.66,0.665,0.67,0.675,0.68,0.685,0.690000000000001,0.695000000000001,0.700000000000001,
0.705000000000001,0.710000000000001,0.715000000000001,0.720000000000001,
0.725000000000001,0.730000000000001,0.735000000000001,0.740000000000001,
0.745000000000001,0.750000000000001,0.755000000000001,0.760000000000001,
0.765000000000001,0.770000000000001,0.775000000000001,0.780000000000001,
0.785000000000001,0.790000000000001,0.795000000000001,0.800000000000001,
0.805000000000001,0.810000000000001,0.815000000000001,0.820000000000001,
0.825000000000001,0.830000000000001,0.835000000000001,0.840000000000001,
0.845000000000001,0.850000000000001,0.855000000000001,0.860000000000001,
0.865000000000001,0.870000000000001,0.875000000000001,0.880000000000001,
0.885000000000001,0.890000000000001,0.895000000000001,0.900000000000001,
0.905000000000001,0.910000000000001,0.915000000000001,0.920000000000001,
0.925000000000001,0.930000000000001,0.935000000000001,0.940000000000001,
0.945000000000001,0.950000000000001,0.955000000000001,0.960000000000001,
0.965000000000001,0.970000000000001,0.975000000000001,0.980000000000001,
0.985000000000001,0.990000000000001,0.995000000000001,1.),(0.,1.2),
 .UNSPECIFIED.)
GEOMETRIC_REPRESENTATION_ITEM()
RATIONAL_B_SPLINE_SURFACE(((1.,1.),(1.,1.),(1.,1.),(1.,1.),(1.,1.),(1.,
1.),(1.,1.),(1.,1.),(1.,1.),(1.,1.),(1.,1.),(1.,1.),(1.,1.),(1.,1.),(1.,
1.),(1.,1.),(1.,1.),(1.,1.),(1.,1.),(1.,1.),(1.,1.),(1.,1.),(1.,1.),(1.,
1.),(1.,1.),(1.,1.),(1.,1.),(1.,1.),(1.,1.),(1.,1.),(1.,1.),(1.,1.),(1.,
1.),(1.,1.),(1.,1.),(1.,1.),(1.,1.),(1.,1.),(1.,1.),(1.,1.),(1.,1.),(1.,
1.),(1.,1.),(1.,1.),(1.,1.),(1.,1.),(1.,1.),(1.,1.),(1.,1.),(1.,1.),(1.,
1.),(1.,1.),(1.,1.),(1.,1.),(1.,1.),(1.,1.),(1.,1.),(1.,1.),(1.,1.),(1.,
1.),(1.,1.),(1.,1.),(1.,1.),(1.,1.),(1.,1.),(1.,1.),(1.,1.),(1.,1.),(1.,
1.),(1.,1.),(1.,1.),(1.,1.),(1.,1.),(1.,1.),(1.,1.),(1.,1.),(1.,1.),(1.,
1.),(1.,1.),(1.,1.),(1.,1.),(1.,1.),(1.,1.),(1.,1.),(1.,1.),(1.,1.),(1.,
1.),(1.,1.),(1.,1.),(1.,1.),(1.,1.),(1.,1.),(1.,1.),(1.,1.),(1.,1.),(1.,
1.),(1.,1.),(1.,1.),(1.,1.),(1.,1.),(1.,1.),(1.,1.),(1.,1.),(1.,1.),(1.,
1.),(1.,1.),(1.,1.),(1.,1.),(1.,1.),(1.,1.),(1.,1.),(1.,1.),(1.,1.),(1.,
1.),(1.,1.),(1.,1.),(1.,1.),(1.,1.),(1.,1.),(1.,1.),(1.,1.),(1.,1.),(1.,
1.),(1.,1.),(1.,1.),(1.,1.),(1.,1.),(1.,1.),(1.,1.),(1.,1.),(1.,1.),(1.,
1.),(1.,1.),(1.,1.),(1.,1.),(1.,1.),(1.,1.),(1.,1.),(1.,1.),(1.,1.),(1.,
1.),(1.,1.),(1.,1.),(1.,1.),(1.,1.),(1.,1.),(1.,1.),(1.,1.),(1.,1.),(1.,
1.),(1.,1.),(1.,1.),(1.,1.),(1.,1.),(1.,1.),(1.,1.),(1.,1.),(1.,1.),(1.,
1.),(1.,1.),(1.,1.),(1.,1.),(1.,1.),(1.,1.),(1.,1.),(1.,1.),(1.,1.),(1.,
1.),(1.,1.),(1.,1.),(1.,1.),(1.,1.),(1.,1.),(1.,1.),(1.,1.),(1.,1.),(1.,
1.),(1.,1.),(1.,1.),(1.,1.),(1.,1.),(1.,1.),(1.,1.),(1.,1.),(1.,1.),(1.,
1.),(1.,1.),(1.,1.),(1.,1.),(1.,1.),(1.,1.),(1.,1.),(1.,1.),(1.,1.),(1.,
1.),(1.,1.),(1.,1.),(1.,1.),(1.,1.),(1.,1.),(1.,1.),(1.,1.),(1.,1.),(1.,
1.),(1.,1.)))
REPRESENTATION_ITEM('')
SURFACE()
);
#940=(
BOUNDED_SURFACE()
B_SPLINE_SURFACE(5,1,((#103694,#103695),(#103696,#103697),(#103698,#103699),
(#103700,#103701),(#103702,#103703),(#103704,#103705),(#103706,#103707),
(#103708,#103709),(#103710,#103711),(#103712,#103713),(#103714,#103715),
(#103716,#103717),(#103718,#103719),(#103720,#103721),(#103722,#103723),
(#103724,#103725),(#103726,#103727),(#103728,#103729),(#103730,#103731),
(#103732,#103733),(#103734,#103735),(#103736,#103737),(#103738,#103739),
(#103740,#103741),(#103742,#103743),(#103744,#103745),(#103746,#103747),
(#103748,#103749),(#103750,#103751),(#103752,#103753),(#103754,#103755),
(#103756,#103757),(#103758,#103759),(#103760,#103761),(#103762,#103763),
(#103764,#103765),(#103766,#103767),(#103768,#103769),(#103770,#103771),
(#103772,#103773),(#103774,#103775),(#103776,#103777),(#103778,#103779),
(#103780,#103781),(#103782,#103783),(#103784,#103785),(#103786,#103787),
(#103788,#103789),(#103790,#103791),(#103792,#103793),(#103794,#103795),
(#103796,#103797),(#103798,#103799),(#103800,#103801),(#103802,#103803),
(#103804,#103805),(#103806,#103807),(#103808,#103809),(#103810,#103811),
(#103812,#103813),(#103814,#103815),(#103816,#103817),(#103818,#103819),
(#103820,#103821),(#103822,#103823),(#103824,#103825),(#103826,#103827),
(#103828,#103829),(#103830,#103831),(#103832,#103833),(#103834,#103835),
(#103836,#103837),(#103838,#103839),(#103840,#103841),(#103842,#103843),
(#103844,#103845),(#103846,#103847),(#103848,#103849),(#103850,#103851),
(#103852,#103853),(#103854,#103855),(#103856,#103857),(#103858,#103859),
(#103860,#103861),(#103862,#103863),(#103864,#103865),(#103866,#103867),
(#103868,#103869),(#103870,#103871),(#103872,#103873),(#103874,#103875),
(#103876,#103877),(#103878,#103879),(#103880,#103881),(#103882,#103883),
(#103884,#103885),(#103886,#103887),(#103888,#103889),(#103890,#103891),
(#103892,#103893),(#103894,#103895),(#103896,#103897),(#103898,#103899),
(#103900,#103901),(#103902,#103903),(#103904,#103905),(#103906,#103907),
(#103908,#103909),(#103910,#103911),(#103912,#103913),(#103914,#103915),
(#103916,#103917),(#103918,#103919),(#103920,#103921),(#103922,#103923),
(#103924,#103925),(#103926,#103927),(#103928,#103929),(#103930,#103931),
(#103932,#103933),(#103934,#103935),(#103936,#103937),(#103938,#103939),
(#103940,#103941),(#103942,#103943),(#103944,#103945),(#103946,#103947),
(#103948,#103949),(#103950,#103951),(#103952,#103953),(#103954,#103955),
(#103956,#103957),(#103958,#103959),(#103960,#103961),(#103962,#103963),
(#103964,#103965),(#103966,#103967),(#103968,#103969),(#103970,#103971),
(#103972,#103973),(#103974,#103975),(#103976,#103977),(#103978,#103979),
(#103980,#103981),(#103982,#103983),(#103984,#103985),(#103986,#103987),
(#103988,#103989),(#103990,#103991),(#103992,#103993),(#103994,#103995),
(#103996,#103997),(#103998,#103999),(#104000,#104001),(#104002,#104003),
(#104004,#104005),(#104006,#104007),(#104008,#104009),(#104010,#104011),
(#104012,#104013),(#104014,#104015),(#104016,#104017),(#104018,#104019),
(#104020,#104021),(#104022,#104023),(#104024,#104025),(#104026,#104027),
(#104028,#104029),(#104030,#104031),(#104032,#104033),(#104034,#104035),
(#104036,#104037),(#104038,#104039),(#104040,#104041),(#104042,#104043),
(#104044,#104045),(#104046,#104047),(#104048,#104049),(#104050,#104051),
(#104052,#104053),(#104054,#104055),(#104056,#104057),(#104058,#104059),
(#104060,#104061),(#104062,#104063),(#104064,#104065),(#104066,#104067),
(#104068,#104069),(#104070,#104071),(#104072,#104073),(#104074,#104075),
(#104076,#104077),(#104078,#104079),(#104080,#104081),(#104082,#104083),
(#104084,#104085),(#104086,#104087),(#104088,#104089),(#104090,#104091),
(#104092,#104093),(#104094,#104095),(#104096,#104097),(#104098,#104099),
(#104100,#104101),(#104102,#104103)),.UNSPECIFIED.,.F.,.F.,.F.)
B_SPLINE_SURFACE_WITH_KNOTS((6,1,1,1,1,1,1,1,1,1,1,1,1,1,1,1,1,1,1,1,1,
1,1,1,1,1,1,1,1,1,1,1,1,1,1,1,1,1,1,1,1,1,1,1,1,1,1,1,1,1,1,1,1,1,1,1,1,
1,1,1,1,1,1,1,1,1,1,1,1,1,1,1,1,1,1,1,1,1,1,1,1,1,1,1,1,1,1,1,1,1,1,1,1,
1,1,1,1,1,1,1,1,1,1,1,1,1,1,1,1,1,1,1,1,1,1,1,1,1,1,1,1,1,1,1,1,1,1,1,1,
1,1,1,1,1,1,1,1,1,1,1,1,1,1,1,1,1,1,1,1,1,1,1,1,1,1,1,1,1,1,1,1,1,1,1,1,
1,1,1,1,1,1,1,1,1,1,1,1,1,1,1,1,1,1,1,1,1,1,1,1,1,1,1,1,1,1,1,1,1,1,1,6),
(2,2),(0.,0.005,0.01,0.015,0.02,0.025,0.03,0.035,0.04,0.045,0.05,0.055,
0.06,0.065,0.07,0.075,0.08,0.085,0.09,0.095,0.1,0.105,0.11,0.115,0.12,0.125,
0.13,0.135,0.14,0.145,0.15,0.155,0.16,0.165,0.17,0.175,0.18,0.185,0.19,
0.195,0.2,0.205,0.21,0.215,0.22,0.225,0.23,0.235,0.24,0.245,0.25,0.255,
0.26,0.265,0.27,0.275,0.28,0.285,0.29,0.295,0.3,0.305,0.31,0.315,0.32,0.325,
0.33,0.335,0.34,0.345,0.35,0.355,0.36,0.365,0.37,0.375,0.38,0.385,0.39,
0.395,0.4,0.405,0.41,0.415,0.42,0.425,0.43,0.435,0.44,0.445,0.45,0.455,
0.46,0.465,0.47,0.475,0.48,0.485,0.49,0.495,0.5,0.505,0.51,0.515,0.52,0.525,
0.53,0.535,0.54,0.545,0.55,0.555,0.56,0.565,0.57,0.575,0.58,0.585,0.59,
0.595,0.6,0.605,0.61,0.615,0.62,0.625,0.63,0.635,0.64,0.645,0.65,0.655,
0.66,0.665,0.67,0.675,0.68,0.685,0.690000000000001,0.695000000000001,0.700000000000001,
0.705000000000001,0.710000000000001,0.715000000000001,0.720000000000001,
0.725000000000001,0.730000000000001,0.735000000000001,0.740000000000001,
0.745000000000001,0.750000000000001,0.755000000000001,0.760000000000001,
0.765000000000001,0.770000000000001,0.775000000000001,0.780000000000001,
0.785000000000001,0.790000000000001,0.795000000000001,0.800000000000001,
0.805000000000001,0.810000000000001,0.815000000000001,0.820000000000001,
0.825000000000001,0.830000000000001,0.835000000000001,0.840000000000001,
0.845000000000001,0.850000000000001,0.855000000000001,0.860000000000001,
0.865000000000001,0.870000000000001,0.875000000000001,0.880000000000001,
0.885000000000001,0.890000000000001,0.895000000000001,0.900000000000001,
0.905000000000001,0.910000000000001,0.915000000000001,0.920000000000001,
0.925000000000001,0.930000000000001,0.935000000000001,0.940000000000001,
0.945000000000001,0.950000000000001,0.955000000000001,0.960000000000001,
0.965000000000001,0.970000000000001,0.975000000000001,0.980000000000001,
0.985000000000001,0.990000000000001,0.995000000000001,1.),(0.,1.2),
 .UNSPECIFIED.)
GEOMETRIC_REPRESENTATION_ITEM()
RATIONAL_B_SPLINE_SURFACE(((1.,1.),(1.,1.),(1.,1.),(1.,1.),(1.,1.),(1.,
1.),(1.,1.),(1.,1.),(1.,1.),(1.,1.),(1.,1.),(1.,1.),(1.,1.),(1.,1.),(1.,
1.),(1.,1.),(1.,1.),(1.,1.),(1.,1.),(1.,1.),(1.,1.),(1.,1.),(1.,1.),(1.,
1.),(1.,1.),(1.,1.),(1.,1.),(1.,1.),(1.,1.),(1.,1.),(1.,1.),(1.,1.),(1.,
1.),(1.,1.),(1.,1.),(1.,1.),(1.,1.),(1.,1.),(1.,1.),(1.,1.),(1.,1.),(1.,
1.),(1.,1.),(1.,1.),(1.,1.),(1.,1.),(1.,1.),(1.,1.),(1.,1.),(1.,1.),(1.,
1.),(1.,1.),(1.,1.),(1.,1.),(1.,1.),(1.,1.),(1.,1.),(1.,1.),(1.,1.),(1.,
1.),(1.,1.),(1.,1.),(1.,1.),(1.,1.),(1.,1.),(1.,1.),(1.,1.),(1.,1.),(1.,
1.),(1.,1.),(1.,1.),(1.,1.),(1.,1.),(1.,1.),(1.,1.),(1.,1.),(1.,1.),(1.,
1.),(1.,1.),(1.,1.),(1.,1.),(1.,1.),(1.,1.),(1.,1.),(1.,1.),(1.,1.),(1.,
1.),(1.,1.),(1.,1.),(1.,1.),(1.,1.),(1.,1.),(1.,1.),(1.,1.),(1.,1.),(1.,
1.),(1.,1.),(1.,1.),(1.,1.),(1.,1.),(1.,1.),(1.,1.),(1.,1.),(1.,1.),(1.,
1.),(1.,1.),(1.,1.),(1.,1.),(1.,1.),(1.,1.),(1.,1.),(1.,1.),(1.,1.),(1.,
1.),(1.,1.),(1.,1.),(1.,1.),(1.,1.),(1.,1.),(1.,1.),(1.,1.),(1.,1.),(1.,
1.),(1.,1.),(1.,1.),(1.,1.),(1.,1.),(1.,1.),(1.,1.),(1.,1.),(1.,1.),(1.,
1.),(1.,1.),(1.,1.),(1.,1.),(1.,1.),(1.,1.),(1.,1.),(1.,1.),(1.,1.),(1.,
1.),(1.,1.),(1.,1.),(1.,1.),(1.,1.),(1.,1.),(1.,1.),(1.,1.),(1.,1.),(1.,
1.),(1.,1.),(1.,1.),(1.,1.),(1.,1.),(1.,1.),(1.,1.),(1.,1.),(1.,1.),(1.,
1.),(1.,1.),(1.,1.),(1.,1.),(1.,1.),(1.,1.),(1.,1.),(1.,1.),(1.,1.),(1.,
1.),(1.,1.),(1.,1.),(1.,1.),(1.,1.),(1.,1.),(1.,1.),(1.,1.),(1.,1.),(1.,
1.),(1.,1.),(1.,1.),(1.,1.),(1.,1.),(1.,1.),(1.,1.),(1.,1.),(1.,1.),(1.,
1.),(1.,1.),(1.,1.),(1.,1.),(1.,1.),(1.,1.),(1.,1.),(1.,1.),(1.,1.),(1.,
1.),(1.,1.),(1.,1.),(1.,1.),(1.,1.),(1.,1.),(1.,1.),(1.,1.),(1.,1.),(1.,
1.),(1.,1.)))
REPRESENTATION_ITEM('')
SURFACE()
);
#941=(
BOUNDED_SURFACE()
B_SPLINE_SURFACE(5,1,((#104590,#104591),(#104592,#104593),(#104594,#104595),
(#104596,#104597),(#104598,#104599),(#104600,#104601),(#104602,#104603),
(#104604,#104605),(#104606,#104607),(#104608,#104609),(#104610,#104611),
(#104612,#104613),(#104614,#104615),(#104616,#104617),(#104618,#104619),
(#104620,#104621),(#104622,#104623),(#104624,#104625),(#104626,#104627),
(#104628,#104629),(#104630,#104631),(#104632,#104633),(#104634,#104635),
(#104636,#104637),(#104638,#104639),(#104640,#104641),(#104642,#104643),
(#104644,#104645),(#104646,#104647),(#104648,#104649),(#104650,#104651),
(#104652,#104653),(#104654,#104655),(#104656,#104657),(#104658,#104659),
(#104660,#104661),(#104662,#104663),(#104664,#104665),(#104666,#104667),
(#104668,#104669),(#104670,#104671),(#104672,#104673),(#104674,#104675),
(#104676,#104677),(#104678,#104679),(#104680,#104681),(#104682,#104683),
(#104684,#104685),(#104686,#104687),(#104688,#104689),(#104690,#104691),
(#104692,#104693),(#104694,#104695),(#104696,#104697),(#104698,#104699),
(#104700,#104701),(#104702,#104703),(#104704,#104705),(#104706,#104707),
(#104708,#104709),(#104710,#104711),(#104712,#104713),(#104714,#104715),
(#104716,#104717),(#104718,#104719),(#104720,#104721),(#104722,#104723),
(#104724,#104725),(#104726,#104727),(#104728,#104729),(#104730,#104731),
(#104732,#104733),(#104734,#104735),(#104736,#104737),(#104738,#104739),
(#104740,#104741),(#104742,#104743),(#104744,#104745),(#104746,#104747),
(#104748,#104749),(#104750,#104751),(#104752,#104753),(#104754,#104755),
(#104756,#104757),(#104758,#104759),(#104760,#104761),(#104762,#104763),
(#104764,#104765),(#104766,#104767),(#104768,#104769),(#104770,#104771),
(#104772,#104773),(#104774,#104775),(#104776,#104777),(#104778,#104779),
(#104780,#104781),(#104782,#104783),(#104784,#104785),(#104786,#104787),
(#104788,#104789),(#104790,#104791),(#104792,#104793),(#104794,#104795),
(#104796,#104797),(#104798,#104799),(#104800,#104801),(#104802,#104803),
(#104804,#104805),(#104806,#104807),(#104808,#104809),(#104810,#104811),
(#104812,#104813),(#104814,#104815),(#104816,#104817),(#104818,#104819),
(#104820,#104821),(#104822,#104823),(#104824,#104825),(#104826,#104827),
(#104828,#104829),(#104830,#104831),(#104832,#104833),(#104834,#104835),
(#104836,#104837),(#104838,#104839),(#104840,#104841),(#104842,#104843),
(#104844,#104845),(#104846,#104847),(#104848,#104849),(#104850,#104851),
(#104852,#104853),(#104854,#104855),(#104856,#104857),(#104858,#104859),
(#104860,#104861),(#104862,#104863),(#104864,#104865),(#104866,#104867),
(#104868,#104869),(#104870,#104871),(#104872,#104873),(#104874,#104875),
(#104876,#104877),(#104878,#104879),(#104880,#104881),(#104882,#104883),
(#104884,#104885),(#104886,#104887),(#104888,#104889),(#104890,#104891),
(#104892,#104893),(#104894,#104895),(#104896,#104897),(#104898,#104899),
(#104900,#104901),(#104902,#104903),(#104904,#104905),(#104906,#104907),
(#104908,#104909),(#104910,#104911),(#104912,#104913),(#104914,#104915),
(#104916,#104917),(#104918,#104919),(#104920,#104921),(#104922,#104923),
(#104924,#104925),(#104926,#104927),(#104928,#104929),(#104930,#104931),
(#104932,#104933),(#104934,#104935),(#104936,#104937),(#104938,#104939),
(#104940,#104941),(#104942,#104943),(#104944,#104945),(#104946,#104947),
(#104948,#104949),(#104950,#104951),(#104952,#104953),(#104954,#104955),
(#104956,#104957),(#104958,#104959),(#104960,#104961),(#104962,#104963),
(#104964,#104965),(#104966,#104967),(#104968,#104969),(#104970,#104971),
(#104972,#104973),(#104974,#104975),(#104976,#104977),(#104978,#104979),
(#104980,#104981),(#104982,#104983),(#104984,#104985),(#104986,#104987),
(#104988,#104989),(#104990,#104991),(#104992,#104993),(#104994,#104995),
(#104996,#104997),(#104998,#104999)),.UNSPECIFIED.,.F.,.F.,.F.)
B_SPLINE_SURFACE_WITH_KNOTS((6,1,1,1,1,1,1,1,1,1,1,1,1,1,1,1,1,1,1,1,1,
1,1,1,1,1,1,1,1,1,1,1,1,1,1,1,1,1,1,1,1,1,1,1,1,1,1,1,1,1,1,1,1,1,1,1,1,
1,1,1,1,1,1,1,1,1,1,1,1,1,1,1,1,1,1,1,1,1,1,1,1,1,1,1,1,1,1,1,1,1,1,1,1,
1,1,1,1,1,1,1,1,1,1,1,1,1,1,1,1,1,1,1,1,1,1,1,1,1,1,1,1,1,1,1,1,1,1,1,1,
1,1,1,1,1,1,1,1,1,1,1,1,1,1,1,1,1,1,1,1,1,1,1,1,1,1,1,1,1,1,1,1,1,1,1,1,
1,1,1,1,1,1,1,1,1,1,1,1,1,1,1,1,1,1,1,1,1,1,1,1,1,1,1,1,1,1,1,1,1,1,1,6),
(2,2),(0.,0.005,0.01,0.015,0.02,0.025,0.03,0.035,0.04,0.045,0.05,0.055,
0.06,0.065,0.07,0.075,0.08,0.085,0.09,0.095,0.1,0.105,0.11,0.115,0.12,0.125,
0.13,0.135,0.14,0.145,0.15,0.155,0.16,0.165,0.17,0.175,0.18,0.185,0.19,
0.195,0.2,0.205,0.21,0.215,0.22,0.225,0.23,0.235,0.24,0.245,0.25,0.255,
0.26,0.265,0.27,0.275,0.28,0.285,0.29,0.295,0.3,0.305,0.31,0.315,0.32,0.325,
0.33,0.335,0.34,0.345,0.35,0.355,0.36,0.365,0.37,0.375,0.38,0.385,0.39,
0.395,0.4,0.405,0.41,0.415,0.42,0.425,0.43,0.435,0.44,0.445,0.45,0.455,
0.46,0.465,0.47,0.475,0.48,0.485,0.49,0.495,0.5,0.505,0.51,0.515,0.52,0.525,
0.53,0.535,0.54,0.545,0.55,0.555,0.56,0.565,0.57,0.575,0.58,0.585,0.59,
0.595,0.6,0.605,0.61,0.615,0.62,0.625,0.63,0.635,0.64,0.645,0.65,0.655,
0.66,0.665,0.67,0.675,0.68,0.685,0.690000000000001,0.695000000000001,0.700000000000001,
0.705000000000001,0.710000000000001,0.715000000000001,0.720000000000001,
0.725000000000001,0.730000000000001,0.735000000000001,0.740000000000001,
0.745000000000001,0.750000000000001,0.755000000000001,0.760000000000001,
0.765000000000001,0.770000000000001,0.775000000000001,0.780000000000001,
0.785000000000001,0.790000000000001,0.795000000000001,0.800000000000001,
0.805000000000001,0.810000000000001,0.815000000000001,0.820000000000001,
0.825000000000001,0.830000000000001,0.835000000000001,0.840000000000001,
0.845000000000001,0.850000000000001,0.855000000000001,0.860000000000001,
0.865000000000001,0.870000000000001,0.875000000000001,0.880000000000001,
0.885000000000001,0.890000000000001,0.895000000000001,0.900000000000001,
0.905000000000001,0.910000000000001,0.915000000000001,0.920000000000001,
0.925000000000001,0.930000000000001,0.935000000000001,0.940000000000001,
0.945000000000001,0.950000000000001,0.955000000000001,0.960000000000001,
0.965000000000001,0.970000000000001,0.975000000000001,0.980000000000001,
0.985000000000001,0.990000000000001,0.995000000000001,1.),(0.,1.2),
 .UNSPECIFIED.)
GEOMETRIC_REPRESENTATION_ITEM()
RATIONAL_B_SPLINE_SURFACE(((1.,1.),(1.,1.),(1.,1.),(1.,1.),(1.,1.),(1.,
1.),(1.,1.),(1.,1.),(1.,1.),(1.,1.),(1.,1.),(1.,1.),(1.,1.),(1.,1.),(1.,
1.),(1.,1.),(1.,1.),(1.,1.),(1.,1.),(1.,1.),(1.,1.),(1.,1.),(1.,1.),(1.,
1.),(1.,1.),(1.,1.),(1.,1.),(1.,1.),(1.,1.),(1.,1.),(1.,1.),(1.,1.),(1.,
1.),(1.,1.),(1.,1.),(1.,1.),(1.,1.),(1.,1.),(1.,1.),(1.,1.),(1.,1.),(1.,
1.),(1.,1.),(1.,1.),(1.,1.),(1.,1.),(1.,1.),(1.,1.),(1.,1.),(1.,1.),(1.,
1.),(1.,1.),(1.,1.),(1.,1.),(1.,1.),(1.,1.),(1.,1.),(1.,1.),(1.,1.),(1.,
1.),(1.,1.),(1.,1.),(1.,1.),(1.,1.),(1.,1.),(1.,1.),(1.,1.),(1.,1.),(1.,
1.),(1.,1.),(1.,1.),(1.,1.),(1.,1.),(1.,1.),(1.,1.),(1.,1.),(1.,1.),(1.,
1.),(1.,1.),(1.,1.),(1.,1.),(1.,1.),(1.,1.),(1.,1.),(1.,1.),(1.,1.),(1.,
1.),(1.,1.),(1.,1.),(1.,1.),(1.,1.),(1.,1.),(1.,1.),(1.,1.),(1.,1.),(1.,
1.),(1.,1.),(1.,1.),(1.,1.),(1.,1.),(1.,1.),(1.,1.),(1.,1.),(1.,1.),(1.,
1.),(1.,1.),(1.,1.),(1.,1.),(1.,1.),(1.,1.),(1.,1.),(1.,1.),(1.,1.),(1.,
1.),(1.,1.),(1.,1.),(1.,1.),(1.,1.),(1.,1.),(1.,1.),(1.,1.),(1.,1.),(1.,
1.),(1.,1.),(1.,1.),(1.,1.),(1.,1.),(1.,1.),(1.,1.),(1.,1.),(1.,1.),(1.,
1.),(1.,1.),(1.,1.),(1.,1.),(1.,1.),(1.,1.),(1.,1.),(1.,1.),(1.,1.),(1.,
1.),(1.,1.),(1.,1.),(1.,1.),(1.,1.),(1.,1.),(1.,1.),(1.,1.),(1.,1.),(1.,
1.),(1.,1.),(1.,1.),(1.,1.),(1.,1.),(1.,1.),(1.,1.),(1.,1.),(1.,1.),(1.,
1.),(1.,1.),(1.,1.),(1.,1.),(1.,1.),(1.,1.),(1.,1.),(1.,1.),(1.,1.),(1.,
1.),(1.,1.),(1.,1.),(1.,1.),(1.,1.),(1.,1.),(1.,1.),(1.,1.),(1.,1.),(1.,
1.),(1.,1.),(1.,1.),(1.,1.),(1.,1.),(1.,1.),(1.,1.),(1.,1.),(1.,1.),(1.,
1.),(1.,1.),(1.,1.),(1.,1.),(1.,1.),(1.,1.),(1.,1.),(1.,1.),(1.,1.),(1.,
1.),(1.,1.),(1.,1.),(1.,1.),(1.,1.),(1.,1.),(1.,1.),(1.,1.),(1.,1.),(1.,
1.),(1.,1.)))
REPRESENTATION_ITEM('')
SURFACE()
);
#942=(
BOUNDED_SURFACE()
B_SPLINE_SURFACE(5,1,((#105486,#105487),(#105488,#105489),(#105490,#105491),
(#105492,#105493),(#105494,#105495),(#105496,#105497),(#105498,#105499),
(#105500,#105501),(#105502,#105503),(#105504,#105505),(#105506,#105507),
(#105508,#105509),(#105510,#105511),(#105512,#105513),(#105514,#105515),
(#105516,#105517),(#105518,#105519),(#105520,#105521),(#105522,#105523),
(#105524,#105525),(#105526,#105527),(#105528,#105529),(#105530,#105531),
(#105532,#105533),(#105534,#105535),(#105536,#105537),(#105538,#105539),
(#105540,#105541),(#105542,#105543),(#105544,#105545),(#105546,#105547),
(#105548,#105549),(#105550,#105551),(#105552,#105553),(#105554,#105555),
(#105556,#105557),(#105558,#105559),(#105560,#105561),(#105562,#105563),
(#105564,#105565),(#105566,#105567),(#105568,#105569),(#105570,#105571),
(#105572,#105573),(#105574,#105575),(#105576,#105577),(#105578,#105579),
(#105580,#105581),(#105582,#105583),(#105584,#105585),(#105586,#105587),
(#105588,#105589),(#105590,#105591),(#105592,#105593),(#105594,#105595),
(#105596,#105597),(#105598,#105599),(#105600,#105601),(#105602,#105603),
(#105604,#105605),(#105606,#105607),(#105608,#105609),(#105610,#105611),
(#105612,#105613),(#105614,#105615),(#105616,#105617),(#105618,#105619),
(#105620,#105621),(#105622,#105623),(#105624,#105625),(#105626,#105627),
(#105628,#105629),(#105630,#105631),(#105632,#105633),(#105634,#105635),
(#105636,#105637),(#105638,#105639),(#105640,#105641),(#105642,#105643),
(#105644,#105645),(#105646,#105647),(#105648,#105649),(#105650,#105651),
(#105652,#105653),(#105654,#105655),(#105656,#105657),(#105658,#105659),
(#105660,#105661),(#105662,#105663),(#105664,#105665),(#105666,#105667),
(#105668,#105669),(#105670,#105671),(#105672,#105673),(#105674,#105675),
(#105676,#105677),(#105678,#105679),(#105680,#105681),(#105682,#105683),
(#105684,#105685),(#105686,#105687),(#105688,#105689),(#105690,#105691),
(#105692,#105693),(#105694,#105695),(#105696,#105697),(#105698,#105699),
(#105700,#105701),(#105702,#105703),(#105704,#105705),(#105706,#105707),
(#105708,#105709),(#105710,#105711),(#105712,#105713),(#105714,#105715),
(#105716,#105717),(#105718,#105719),(#105720,#105721),(#105722,#105723),
(#105724,#105725),(#105726,#105727),(#105728,#105729),(#105730,#105731),
(#105732,#105733),(#105734,#105735),(#105736,#105737),(#105738,#105739),
(#105740,#105741),(#105742,#105743),(#105744,#105745),(#105746,#105747),
(#105748,#105749),(#105750,#105751),(#105752,#105753),(#105754,#105755),
(#105756,#105757),(#105758,#105759),(#105760,#105761),(#105762,#105763),
(#105764,#105765),(#105766,#105767),(#105768,#105769),(#105770,#105771),
(#105772,#105773),(#105774,#105775),(#105776,#105777),(#105778,#105779),
(#105780,#105781),(#105782,#105783),(#105784,#105785),(#105786,#105787),
(#105788,#105789),(#105790,#105791),(#105792,#105793),(#105794,#105795),
(#105796,#105797),(#105798,#105799),(#105800,#105801),(#105802,#105803),
(#105804,#105805),(#105806,#105807),(#105808,#105809),(#105810,#105811),
(#105812,#105813),(#105814,#105815),(#105816,#105817),(#105818,#105819),
(#105820,#105821),(#105822,#105823),(#105824,#105825),(#105826,#105827),
(#105828,#105829),(#105830,#105831),(#105832,#105833),(#105834,#105835),
(#105836,#105837),(#105838,#105839),(#105840,#105841),(#105842,#105843),
(#105844,#105845),(#105846,#105847),(#105848,#105849),(#105850,#105851),
(#105852,#105853),(#105854,#105855),(#105856,#105857),(#105858,#105859),
(#105860,#105861),(#105862,#105863),(#105864,#105865),(#105866,#105867),
(#105868,#105869),(#105870,#105871),(#105872,#105873),(#105874,#105875),
(#105876,#105877),(#105878,#105879),(#105880,#105881),(#105882,#105883),
(#105884,#105885),(#105886,#105887),(#105888,#105889),(#105890,#105891),
(#105892,#105893),(#105894,#105895)),.UNSPECIFIED.,.F.,.F.,.F.)
B_SPLINE_SURFACE_WITH_KNOTS((6,1,1,1,1,1,1,1,1,1,1,1,1,1,1,1,1,1,1,1,1,
1,1,1,1,1,1,1,1,1,1,1,1,1,1,1,1,1,1,1,1,1,1,1,1,1,1,1,1,1,1,1,1,1,1,1,1,
1,1,1,1,1,1,1,1,1,1,1,1,1,1,1,1,1,1,1,1,1,1,1,1,1,1,1,1,1,1,1,1,1,1,1,1,
1,1,1,1,1,1,1,1,1,1,1,1,1,1,1,1,1,1,1,1,1,1,1,1,1,1,1,1,1,1,1,1,1,1,1,1,
1,1,1,1,1,1,1,1,1,1,1,1,1,1,1,1,1,1,1,1,1,1,1,1,1,1,1,1,1,1,1,1,1,1,1,1,
1,1,1,1,1,1,1,1,1,1,1,1,1,1,1,1,1,1,1,1,1,1,1,1,1,1,1,1,1,1,1,1,1,1,1,6),
(2,2),(0.,0.005,0.01,0.015,0.02,0.025,0.03,0.035,0.04,0.045,0.05,0.055,
0.06,0.065,0.07,0.075,0.08,0.085,0.09,0.095,0.1,0.105,0.11,0.115,0.12,0.125,
0.13,0.135,0.14,0.145,0.15,0.155,0.16,0.165,0.17,0.175,0.18,0.185,0.19,
0.195,0.2,0.205,0.21,0.215,0.22,0.225,0.23,0.235,0.24,0.245,0.25,0.255,
0.26,0.265,0.27,0.275,0.28,0.285,0.29,0.295,0.3,0.305,0.31,0.315,0.32,0.325,
0.33,0.335,0.34,0.345,0.35,0.355,0.36,0.365,0.37,0.375,0.38,0.385,0.39,
0.395,0.4,0.405,0.41,0.415,0.42,0.425,0.43,0.435,0.44,0.445,0.45,0.455,
0.46,0.465,0.47,0.475,0.48,0.485,0.49,0.495,0.5,0.505,0.51,0.515,0.52,0.525,
0.53,0.535,0.54,0.545,0.55,0.555,0.56,0.565,0.57,0.575,0.58,0.585,0.59,
0.595,0.6,0.605,0.61,0.615,0.62,0.625,0.63,0.635,0.64,0.645,0.65,0.655,
0.66,0.665,0.67,0.675,0.68,0.685,0.690000000000001,0.695000000000001,0.700000000000001,
0.705000000000001,0.710000000000001,0.715000000000001,0.720000000000001,
0.725000000000001,0.730000000000001,0.735000000000001,0.740000000000001,
0.745000000000001,0.750000000000001,0.755000000000001,0.760000000000001,
0.765000000000001,0.770000000000001,0.775000000000001,0.780000000000001,
0.785000000000001,0.790000000000001,0.795000000000001,0.800000000000001,
0.805000000000001,0.810000000000001,0.815000000000001,0.820000000000001,
0.825000000000001,0.830000000000001,0.835000000000001,0.840000000000001,
0.845000000000001,0.850000000000001,0.855000000000001,0.860000000000001,
0.865000000000001,0.870000000000001,0.875000000000001,0.880000000000001,
0.885000000000001,0.890000000000001,0.895000000000001,0.900000000000001,
0.905000000000001,0.910000000000001,0.915000000000001,0.920000000000001,
0.925000000000001,0.930000000000001,0.935000000000001,0.940000000000001,
0.945000000000001,0.950000000000001,0.955000000000001,0.960000000000001,
0.965000000000001,0.970000000000001,0.975000000000001,0.980000000000001,
0.985000000000001,0.990000000000001,0.995000000000001,1.),(0.,1.2),
 .UNSPECIFIED.)
GEOMETRIC_REPRESENTATION_ITEM()
RATIONAL_B_SPLINE_SURFACE(((1.,1.),(1.,1.),(1.,1.),(1.,1.),(1.,1.),(1.,
1.),(1.,1.),(1.,1.),(1.,1.),(1.,1.),(1.,1.),(1.,1.),(1.,1.),(1.,1.),(1.,
1.),(1.,1.),(1.,1.),(1.,1.),(1.,1.),(1.,1.),(1.,1.),(1.,1.),(1.,1.),(1.,
1.),(1.,1.),(1.,1.),(1.,1.),(1.,1.),(1.,1.),(1.,1.),(1.,1.),(1.,1.),(1.,
1.),(1.,1.),(1.,1.),(1.,1.),(1.,1.),(1.,1.),(1.,1.),(1.,1.),(1.,1.),(1.,
1.),(1.,1.),(1.,1.),(1.,1.),(1.,1.),(1.,1.),(1.,1.),(1.,1.),(1.,1.),(1.,
1.),(1.,1.),(1.,1.),(1.,1.),(1.,1.),(1.,1.),(1.,1.),(1.,1.),(1.,1.),(1.,
1.),(1.,1.),(1.,1.),(1.,1.),(1.,1.),(1.,1.),(1.,1.),(1.,1.),(1.,1.),(1.,
1.),(1.,1.),(1.,1.),(1.,1.),(1.,1.),(1.,1.),(1.,1.),(1.,1.),(1.,1.),(1.,
1.),(1.,1.),(1.,1.),(1.,1.),(1.,1.),(1.,1.),(1.,1.),(1.,1.),(1.,1.),(1.,
1.),(1.,1.),(1.,1.),(1.,1.),(1.,1.),(1.,1.),(1.,1.),(1.,1.),(1.,1.),(1.,
1.),(1.,1.),(1.,1.),(1.,1.),(1.,1.),(1.,1.),(1.,1.),(1.,1.),(1.,1.),(1.,
1.),(1.,1.),(1.,1.),(1.,1.),(1.,1.),(1.,1.),(1.,1.),(1.,1.),(1.,1.),(1.,
1.),(1.,1.),(1.,1.),(1.,1.),(1.,1.),(1.,1.),(1.,1.),(1.,1.),(1.,1.),(1.,
1.),(1.,1.),(1.,1.),(1.,1.),(1.,1.),(1.,1.),(1.,1.),(1.,1.),(1.,1.),(1.,
1.),(1.,1.),(1.,1.),(1.,1.),(1.,1.),(1.,1.),(1.,1.),(1.,1.),(1.,1.),(1.,
1.),(1.,1.),(1.,1.),(1.,1.),(1.,1.),(1.,1.),(1.,1.),(1.,1.),(1.,1.),(1.,
1.),(1.,1.),(1.,1.),(1.,1.),(1.,1.),(1.,1.),(1.,1.),(1.,1.),(1.,1.),(1.,
1.),(1.,1.),(1.,1.),(1.,1.),(1.,1.),(1.,1.),(1.,1.),(1.,1.),(1.,1.),(1.,
1.),(1.,1.),(1.,1.),(1.,1.),(1.,1.),(1.,1.),(1.,1.),(1.,1.),(1.,1.),(1.,
1.),(1.,1.),(1.,1.),(1.,1.),(1.,1.),(1.,1.),(1.,1.),(1.,1.),(1.,1.),(1.,
1.),(1.,1.),(1.,1.),(1.,1.),(1.,1.),(1.,1.),(1.,1.),(1.,1.),(1.,1.),(1.,
1.),(1.,1.),(1.,1.),(1.,1.),(1.,1.),(1.,1.),(1.,1.),(1.,1.),(1.,1.),(1.,
1.),(1.,1.)))
REPRESENTATION_ITEM('')
SURFACE()
);
#943=(
BOUNDED_SURFACE()
B_SPLINE_SURFACE(5,1,((#106382,#106383),(#106384,#106385),(#106386,#106387),
(#106388,#106389),(#106390,#106391),(#106392,#106393),(#106394,#106395),
(#106396,#106397),(#106398,#106399),(#106400,#106401),(#106402,#106403),
(#106404,#106405),(#106406,#106407),(#106408,#106409),(#106410,#106411),
(#106412,#106413),(#106414,#106415),(#106416,#106417),(#106418,#106419),
(#106420,#106421),(#106422,#106423),(#106424,#106425),(#106426,#106427),
(#106428,#106429),(#106430,#106431),(#106432,#106433),(#106434,#106435),
(#106436,#106437),(#106438,#106439),(#106440,#106441),(#106442,#106443),
(#106444,#106445),(#106446,#106447),(#106448,#106449),(#106450,#106451),
(#106452,#106453),(#106454,#106455),(#106456,#106457),(#106458,#106459),
(#106460,#106461),(#106462,#106463),(#106464,#106465),(#106466,#106467),
(#106468,#106469),(#106470,#106471),(#106472,#106473),(#106474,#106475),
(#106476,#106477),(#106478,#106479),(#106480,#106481),(#106482,#106483),
(#106484,#106485),(#106486,#106487),(#106488,#106489),(#106490,#106491),
(#106492,#106493),(#106494,#106495),(#106496,#106497),(#106498,#106499),
(#106500,#106501),(#106502,#106503),(#106504,#106505),(#106506,#106507),
(#106508,#106509),(#106510,#106511),(#106512,#106513),(#106514,#106515),
(#106516,#106517),(#106518,#106519),(#106520,#106521),(#106522,#106523),
(#106524,#106525),(#106526,#106527),(#106528,#106529),(#106530,#106531),
(#106532,#106533),(#106534,#106535),(#106536,#106537),(#106538,#106539),
(#106540,#106541),(#106542,#106543),(#106544,#106545),(#106546,#106547),
(#106548,#106549),(#106550,#106551),(#106552,#106553),(#106554,#106555),
(#106556,#106557),(#106558,#106559),(#106560,#106561),(#106562,#106563),
(#106564,#106565),(#106566,#106567),(#106568,#106569),(#106570,#106571),
(#106572,#106573),(#106574,#106575),(#106576,#106577),(#106578,#106579),
(#106580,#106581),(#106582,#106583),(#106584,#106585),(#106586,#106587),
(#106588,#106589),(#106590,#106591),(#106592,#106593),(#106594,#106595),
(#106596,#106597),(#106598,#106599),(#106600,#106601),(#106602,#106603),
(#106604,#106605),(#106606,#106607),(#106608,#106609),(#106610,#106611),
(#106612,#106613),(#106614,#106615),(#106616,#106617),(#106618,#106619),
(#106620,#106621),(#106622,#106623),(#106624,#106625),(#106626,#106627),
(#106628,#106629),(#106630,#106631),(#106632,#106633),(#106634,#106635),
(#106636,#106637),(#106638,#106639),(#106640,#106641),(#106642,#106643),
(#106644,#106645),(#106646,#106647),(#106648,#106649),(#106650,#106651),
(#106652,#106653),(#106654,#106655),(#106656,#106657),(#106658,#106659),
(#106660,#106661),(#106662,#106663),(#106664,#106665),(#106666,#106667),
(#106668,#106669),(#106670,#106671),(#106672,#106673),(#106674,#106675),
(#106676,#106677),(#106678,#106679),(#106680,#106681),(#106682,#106683),
(#106684,#106685),(#106686,#106687),(#106688,#106689),(#106690,#106691),
(#106692,#106693),(#106694,#106695),(#106696,#106697),(#106698,#106699),
(#106700,#106701),(#106702,#106703),(#106704,#106705),(#106706,#106707),
(#106708,#106709),(#106710,#106711),(#106712,#106713),(#106714,#106715),
(#106716,#106717),(#106718,#106719),(#106720,#106721),(#106722,#106723),
(#106724,#106725),(#106726,#106727),(#106728,#106729),(#106730,#106731),
(#106732,#106733),(#106734,#106735),(#106736,#106737),(#106738,#106739),
(#106740,#106741),(#106742,#106743),(#106744,#106745),(#106746,#106747),
(#106748,#106749),(#106750,#106751),(#106752,#106753),(#106754,#106755),
(#106756,#106757),(#106758,#106759),(#106760,#106761),(#106762,#106763),
(#106764,#106765),(#106766,#106767),(#106768,#106769),(#106770,#106771),
(#106772,#106773),(#106774,#106775),(#106776,#106777),(#106778,#106779),
(#106780,#106781),(#106782,#106783),(#106784,#106785),(#106786,#106787),
(#106788,#106789),(#106790,#106791)),.UNSPECIFIED.,.F.,.F.,.F.)
B_SPLINE_SURFACE_WITH_KNOTS((6,1,1,1,1,1,1,1,1,1,1,1,1,1,1,1,1,1,1,1,1,
1,1,1,1,1,1,1,1,1,1,1,1,1,1,1,1,1,1,1,1,1,1,1,1,1,1,1,1,1,1,1,1,1,1,1,1,
1,1,1,1,1,1,1,1,1,1,1,1,1,1,1,1,1,1,1,1,1,1,1,1,1,1,1,1,1,1,1,1,1,1,1,1,
1,1,1,1,1,1,1,1,1,1,1,1,1,1,1,1,1,1,1,1,1,1,1,1,1,1,1,1,1,1,1,1,1,1,1,1,
1,1,1,1,1,1,1,1,1,1,1,1,1,1,1,1,1,1,1,1,1,1,1,1,1,1,1,1,1,1,1,1,1,1,1,1,
1,1,1,1,1,1,1,1,1,1,1,1,1,1,1,1,1,1,1,1,1,1,1,1,1,1,1,1,1,1,1,1,1,1,1,6),
(2,2),(0.,0.005,0.01,0.015,0.02,0.025,0.03,0.035,0.04,0.045,0.05,0.055,
0.06,0.065,0.07,0.075,0.08,0.085,0.09,0.095,0.1,0.105,0.11,0.115,0.12,0.125,
0.13,0.135,0.14,0.145,0.15,0.155,0.16,0.165,0.17,0.175,0.18,0.185,0.19,
0.195,0.2,0.205,0.21,0.215,0.22,0.225,0.23,0.235,0.24,0.245,0.25,0.255,
0.26,0.265,0.27,0.275,0.28,0.285,0.29,0.295,0.3,0.305,0.31,0.315,0.32,0.325,
0.33,0.335,0.34,0.345,0.35,0.355,0.36,0.365,0.37,0.375,0.38,0.385,0.39,
0.395,0.4,0.405,0.41,0.415,0.42,0.425,0.43,0.435,0.44,0.445,0.45,0.455,
0.46,0.465,0.47,0.475,0.48,0.485,0.49,0.495,0.5,0.505,0.51,0.515,0.52,0.525,
0.53,0.535,0.54,0.545,0.55,0.555,0.56,0.565,0.57,0.575,0.58,0.585,0.59,
0.595,0.6,0.605,0.61,0.615,0.62,0.625,0.63,0.635,0.64,0.645,0.65,0.655,
0.66,0.665,0.67,0.675,0.68,0.685,0.690000000000001,0.695000000000001,0.700000000000001,
0.705000000000001,0.710000000000001,0.715000000000001,0.720000000000001,
0.725000000000001,0.730000000000001,0.735000000000001,0.740000000000001,
0.745000000000001,0.750000000000001,0.755000000000001,0.760000000000001,
0.765000000000001,0.770000000000001,0.775000000000001,0.780000000000001,
0.785000000000001,0.790000000000001,0.795000000000001,0.800000000000001,
0.805000000000001,0.810000000000001,0.815000000000001,0.820000000000001,
0.825000000000001,0.830000000000001,0.835000000000001,0.840000000000001,
0.845000000000001,0.850000000000001,0.855000000000001,0.860000000000001,
0.865000000000001,0.870000000000001,0.875000000000001,0.880000000000001,
0.885000000000001,0.890000000000001,0.895000000000001,0.900000000000001,
0.905000000000001,0.910000000000001,0.915000000000001,0.920000000000001,
0.925000000000001,0.930000000000001,0.935000000000001,0.940000000000001,
0.945000000000001,0.950000000000001,0.955000000000001,0.960000000000001,
0.965000000000001,0.970000000000001,0.975000000000001,0.980000000000001,
0.985000000000001,0.990000000000001,0.995000000000001,1.),(0.,1.2),
 .UNSPECIFIED.)
GEOMETRIC_REPRESENTATION_ITEM()
RATIONAL_B_SPLINE_SURFACE(((1.,1.),(1.,1.),(1.,1.),(1.,1.),(1.,1.),(1.,
1.),(1.,1.),(1.,1.),(1.,1.),(1.,1.),(1.,1.),(1.,1.),(1.,1.),(1.,1.),(1.,
1.),(1.,1.),(1.,1.),(1.,1.),(1.,1.),(1.,1.),(1.,1.),(1.,1.),(1.,1.),(1.,
1.),(1.,1.),(1.,1.),(1.,1.),(1.,1.),(1.,1.),(1.,1.),(1.,1.),(1.,1.),(1.,
1.),(1.,1.),(1.,1.),(1.,1.),(1.,1.),(1.,1.),(1.,1.),(1.,1.),(1.,1.),(1.,
1.),(1.,1.),(1.,1.),(1.,1.),(1.,1.),(1.,1.),(1.,1.),(1.,1.),(1.,1.),(1.,
1.),(1.,1.),(1.,1.),(1.,1.),(1.,1.),(1.,1.),(1.,1.),(1.,1.),(1.,1.),(1.,
1.),(1.,1.),(1.,1.),(1.,1.),(1.,1.),(1.,1.),(1.,1.),(1.,1.),(1.,1.),(1.,
1.),(1.,1.),(1.,1.),(1.,1.),(1.,1.),(1.,1.),(1.,1.),(1.,1.),(1.,1.),(1.,
1.),(1.,1.),(1.,1.),(1.,1.),(1.,1.),(1.,1.),(1.,1.),(1.,1.),(1.,1.),(1.,
1.),(1.,1.),(1.,1.),(1.,1.),(1.,1.),(1.,1.),(1.,1.),(1.,1.),(1.,1.),(1.,
1.),(1.,1.),(1.,1.),(1.,1.),(1.,1.),(1.,1.),(1.,1.),(1.,1.),(1.,1.),(1.,
1.),(1.,1.),(1.,1.),(1.,1.),(1.,1.),(1.,1.),(1.,1.),(1.,1.),(1.,1.),(1.,
1.),(1.,1.),(1.,1.),(1.,1.),(1.,1.),(1.,1.),(1.,1.),(1.,1.),(1.,1.),(1.,
1.),(1.,1.),(1.,1.),(1.,1.),(1.,1.),(1.,1.),(1.,1.),(1.,1.),(1.,1.),(1.,
1.),(1.,1.),(1.,1.),(1.,1.),(1.,1.),(1.,1.),(1.,1.),(1.,1.),(1.,1.),(1.,
1.),(1.,1.),(1.,1.),(1.,1.),(1.,1.),(1.,1.),(1.,1.),(1.,1.),(1.,1.),(1.,
1.),(1.,1.),(1.,1.),(1.,1.),(1.,1.),(1.,1.),(1.,1.),(1.,1.),(1.,1.),(1.,
1.),(1.,1.),(1.,1.),(1.,1.),(1.,1.),(1.,1.),(1.,1.),(1.,1.),(1.,1.),(1.,
1.),(1.,1.),(1.,1.),(1.,1.),(1.,1.),(1.,1.),(1.,1.),(1.,1.),(1.,1.),(1.,
1.),(1.,1.),(1.,1.),(1.,1.),(1.,1.),(1.,1.),(1.,1.),(1.,1.),(1.,1.),(1.,
1.),(1.,1.),(1.,1.),(1.,1.),(1.,1.),(1.,1.),(1.,1.),(1.,1.),(1.,1.),(1.,
1.),(1.,1.),(1.,1.),(1.,1.),(1.,1.),(1.,1.),(1.,1.),(1.,1.),(1.,1.),(1.,
1.),(1.,1.)))
REPRESENTATION_ITEM('')
SURFACE()
);
#944=(
BOUNDED_SURFACE()
B_SPLINE_SURFACE(5,1,((#107278,#107279),(#107280,#107281),(#107282,#107283),
(#107284,#107285),(#107286,#107287),(#107288,#107289),(#107290,#107291),
(#107292,#107293),(#107294,#107295),(#107296,#107297),(#107298,#107299),
(#107300,#107301),(#107302,#107303),(#107304,#107305),(#107306,#107307),
(#107308,#107309),(#107310,#107311),(#107312,#107313),(#107314,#107315),
(#107316,#107317),(#107318,#107319),(#107320,#107321),(#107322,#107323),
(#107324,#107325),(#107326,#107327),(#107328,#107329),(#107330,#107331),
(#107332,#107333),(#107334,#107335),(#107336,#107337),(#107338,#107339),
(#107340,#107341),(#107342,#107343),(#107344,#107345),(#107346,#107347),
(#107348,#107349),(#107350,#107351),(#107352,#107353),(#107354,#107355),
(#107356,#107357),(#107358,#107359),(#107360,#107361),(#107362,#107363),
(#107364,#107365),(#107366,#107367),(#107368,#107369),(#107370,#107371),
(#107372,#107373),(#107374,#107375),(#107376,#107377),(#107378,#107379),
(#107380,#107381),(#107382,#107383),(#107384,#107385),(#107386,#107387),
(#107388,#107389),(#107390,#107391),(#107392,#107393),(#107394,#107395),
(#107396,#107397),(#107398,#107399),(#107400,#107401),(#107402,#107403),
(#107404,#107405),(#107406,#107407),(#107408,#107409),(#107410,#107411),
(#107412,#107413),(#107414,#107415),(#107416,#107417),(#107418,#107419),
(#107420,#107421),(#107422,#107423),(#107424,#107425),(#107426,#107427),
(#107428,#107429),(#107430,#107431),(#107432,#107433),(#107434,#107435),
(#107436,#107437),(#107438,#107439),(#107440,#107441),(#107442,#107443),
(#107444,#107445),(#107446,#107447),(#107448,#107449),(#107450,#107451),
(#107452,#107453),(#107454,#107455),(#107456,#107457),(#107458,#107459),
(#107460,#107461),(#107462,#107463),(#107464,#107465),(#107466,#107467),
(#107468,#107469),(#107470,#107471),(#107472,#107473),(#107474,#107475),
(#107476,#107477),(#107478,#107479),(#107480,#107481),(#107482,#107483),
(#107484,#107485),(#107486,#107487),(#107488,#107489),(#107490,#107491),
(#107492,#107493),(#107494,#107495),(#107496,#107497),(#107498,#107499),
(#107500,#107501),(#107502,#107503),(#107504,#107505),(#107506,#107507),
(#107508,#107509),(#107510,#107511),(#107512,#107513),(#107514,#107515),
(#107516,#107517),(#107518,#107519),(#107520,#107521),(#107522,#107523),
(#107524,#107525),(#107526,#107527),(#107528,#107529),(#107530,#107531),
(#107532,#107533),(#107534,#107535),(#107536,#107537),(#107538,#107539),
(#107540,#107541),(#107542,#107543),(#107544,#107545),(#107546,#107547),
(#107548,#107549),(#107550,#107551),(#107552,#107553),(#107554,#107555),
(#107556,#107557),(#107558,#107559),(#107560,#107561),(#107562,#107563),
(#107564,#107565),(#107566,#107567),(#107568,#107569),(#107570,#107571),
(#107572,#107573),(#107574,#107575),(#107576,#107577),(#107578,#107579),
(#107580,#107581),(#107582,#107583),(#107584,#107585),(#107586,#107587),
(#107588,#107589),(#107590,#107591),(#107592,#107593),(#107594,#107595),
(#107596,#107597),(#107598,#107599),(#107600,#107601),(#107602,#107603),
(#107604,#107605),(#107606,#107607),(#107608,#107609),(#107610,#107611),
(#107612,#107613),(#107614,#107615),(#107616,#107617),(#107618,#107619),
(#107620,#107621),(#107622,#107623),(#107624,#107625),(#107626,#107627),
(#107628,#107629),(#107630,#107631),(#107632,#107633),(#107634,#107635),
(#107636,#107637),(#107638,#107639),(#107640,#107641),(#107642,#107643),
(#107644,#107645),(#107646,#107647),(#107648,#107649),(#107650,#107651),
(#107652,#107653),(#107654,#107655),(#107656,#107657),(#107658,#107659),
(#107660,#107661),(#107662,#107663),(#107664,#107665),(#107666,#107667),
(#107668,#107669),(#107670,#107671),(#107672,#107673),(#107674,#107675),
(#107676,#107677),(#107678,#107679),(#107680,#107681),(#107682,#107683),
(#107684,#107685),(#107686,#107687)),.UNSPECIFIED.,.F.,.F.,.F.)
B_SPLINE_SURFACE_WITH_KNOTS((6,1,1,1,1,1,1,1,1,1,1,1,1,1,1,1,1,1,1,1,1,
1,1,1,1,1,1,1,1,1,1,1,1,1,1,1,1,1,1,1,1,1,1,1,1,1,1,1,1,1,1,1,1,1,1,1,1,
1,1,1,1,1,1,1,1,1,1,1,1,1,1,1,1,1,1,1,1,1,1,1,1,1,1,1,1,1,1,1,1,1,1,1,1,
1,1,1,1,1,1,1,1,1,1,1,1,1,1,1,1,1,1,1,1,1,1,1,1,1,1,1,1,1,1,1,1,1,1,1,1,
1,1,1,1,1,1,1,1,1,1,1,1,1,1,1,1,1,1,1,1,1,1,1,1,1,1,1,1,1,1,1,1,1,1,1,1,
1,1,1,1,1,1,1,1,1,1,1,1,1,1,1,1,1,1,1,1,1,1,1,1,1,1,1,1,1,1,1,1,1,1,1,6),
(2,2),(0.,0.005,0.01,0.015,0.02,0.025,0.03,0.035,0.04,0.045,0.05,0.055,
0.06,0.065,0.07,0.075,0.08,0.085,0.09,0.095,0.1,0.105,0.11,0.115,0.12,0.125,
0.13,0.135,0.14,0.145,0.15,0.155,0.16,0.165,0.17,0.175,0.18,0.185,0.19,
0.195,0.2,0.205,0.21,0.215,0.22,0.225,0.23,0.235,0.24,0.245,0.25,0.255,
0.26,0.265,0.27,0.275,0.28,0.285,0.29,0.295,0.3,0.305,0.31,0.315,0.32,0.325,
0.33,0.335,0.34,0.345,0.35,0.355,0.36,0.365,0.37,0.375,0.38,0.385,0.39,
0.395,0.4,0.405,0.41,0.415,0.42,0.425,0.43,0.435,0.44,0.445,0.45,0.455,
0.46,0.465,0.47,0.475,0.48,0.485,0.49,0.495,0.5,0.505,0.51,0.515,0.52,0.525,
0.53,0.535,0.54,0.545,0.55,0.555,0.56,0.565,0.57,0.575,0.58,0.585,0.59,
0.595,0.6,0.605,0.61,0.615,0.62,0.625,0.63,0.635,0.64,0.645,0.65,0.655,
0.66,0.665,0.67,0.675,0.68,0.685,0.690000000000001,0.695000000000001,0.700000000000001,
0.705000000000001,0.710000000000001,0.715000000000001,0.720000000000001,
0.725000000000001,0.730000000000001,0.735000000000001,0.740000000000001,
0.745000000000001,0.750000000000001,0.755000000000001,0.760000000000001,
0.765000000000001,0.770000000000001,0.775000000000001,0.780000000000001,
0.785000000000001,0.790000000000001,0.795000000000001,0.800000000000001,
0.805000000000001,0.810000000000001,0.815000000000001,0.820000000000001,
0.825000000000001,0.830000000000001,0.835000000000001,0.840000000000001,
0.845000000000001,0.850000000000001,0.855000000000001,0.860000000000001,
0.865000000000001,0.870000000000001,0.875000000000001,0.880000000000001,
0.885000000000001,0.890000000000001,0.895000000000001,0.900000000000001,
0.905000000000001,0.910000000000001,0.915000000000001,0.920000000000001,
0.925000000000001,0.930000000000001,0.935000000000001,0.940000000000001,
0.945000000000001,0.950000000000001,0.955000000000001,0.960000000000001,
0.965000000000001,0.970000000000001,0.975000000000001,0.980000000000001,
0.985000000000001,0.990000000000001,0.995000000000001,1.),(0.,1.2),
 .UNSPECIFIED.)
GEOMETRIC_REPRESENTATION_ITEM()
RATIONAL_B_SPLINE_SURFACE(((1.,1.),(1.,1.),(1.,1.),(1.,1.),(1.,1.),(1.,
1.),(1.,1.),(1.,1.),(1.,1.),(1.,1.),(1.,1.),(1.,1.),(1.,1.),(1.,1.),(1.,
1.),(1.,1.),(1.,1.),(1.,1.),(1.,1.),(1.,1.),(1.,1.),(1.,1.),(1.,1.),(1.,
1.),(1.,1.),(1.,1.),(1.,1.),(1.,1.),(1.,1.),(1.,1.),(1.,1.),(1.,1.),(1.,
1.),(1.,1.),(1.,1.),(1.,1.),(1.,1.),(1.,1.),(1.,1.),(1.,1.),(1.,1.),(1.,
1.),(1.,1.),(1.,1.),(1.,1.),(1.,1.),(1.,1.),(1.,1.),(1.,1.),(1.,1.),(1.,
1.),(1.,1.),(1.,1.),(1.,1.),(1.,1.),(1.,1.),(1.,1.),(1.,1.),(1.,1.),(1.,
1.),(1.,1.),(1.,1.),(1.,1.),(1.,1.),(1.,1.),(1.,1.),(1.,1.),(1.,1.),(1.,
1.),(1.,1.),(1.,1.),(1.,1.),(1.,1.),(1.,1.),(1.,1.),(1.,1.),(1.,1.),(1.,
1.),(1.,1.),(1.,1.),(1.,1.),(1.,1.),(1.,1.),(1.,1.),(1.,1.),(1.,1.),(1.,
1.),(1.,1.),(1.,1.),(1.,1.),(1.,1.),(1.,1.),(1.,1.),(1.,1.),(1.,1.),(1.,
1.),(1.,1.),(1.,1.),(1.,1.),(1.,1.),(1.,1.),(1.,1.),(1.,1.),(1.,1.),(1.,
1.),(1.,1.),(1.,1.),(1.,1.),(1.,1.),(1.,1.),(1.,1.),(1.,1.),(1.,1.),(1.,
1.),(1.,1.),(1.,1.),(1.,1.),(1.,1.),(1.,1.),(1.,1.),(1.,1.),(1.,1.),(1.,
1.),(1.,1.),(1.,1.),(1.,1.),(1.,1.),(1.,1.),(1.,1.),(1.,1.),(1.,1.),(1.,
1.),(1.,1.),(1.,1.),(1.,1.),(1.,1.),(1.,1.),(1.,1.),(1.,1.),(1.,1.),(1.,
1.),(1.,1.),(1.,1.),(1.,1.),(1.,1.),(1.,1.),(1.,1.),(1.,1.),(1.,1.),(1.,
1.),(1.,1.),(1.,1.),(1.,1.),(1.,1.),(1.,1.),(1.,1.),(1.,1.),(1.,1.),(1.,
1.),(1.,1.),(1.,1.),(1.,1.),(1.,1.),(1.,1.),(1.,1.),(1.,1.),(1.,1.),(1.,
1.),(1.,1.),(1.,1.),(1.,1.),(1.,1.),(1.,1.),(1.,1.),(1.,1.),(1.,1.),(1.,
1.),(1.,1.),(1.,1.),(1.,1.),(1.,1.),(1.,1.),(1.,1.),(1.,1.),(1.,1.),(1.,
1.),(1.,1.),(1.,1.),(1.,1.),(1.,1.),(1.,1.),(1.,1.),(1.,1.),(1.,1.),(1.,
1.),(1.,1.),(1.,1.),(1.,1.),(1.,1.),(1.,1.),(1.,1.),(1.,1.),(1.,1.),(1.,
1.),(1.,1.)))
REPRESENTATION_ITEM('')
SURFACE()
);
#945=(
BOUNDED_SURFACE()
B_SPLINE_SURFACE(5,1,((#108174,#108175),(#108176,#108177),(#108178,#108179),
(#108180,#108181),(#108182,#108183),(#108184,#108185),(#108186,#108187),
(#108188,#108189),(#108190,#108191),(#108192,#108193),(#108194,#108195),
(#108196,#108197),(#108198,#108199),(#108200,#108201),(#108202,#108203),
(#108204,#108205),(#108206,#108207),(#108208,#108209),(#108210,#108211),
(#108212,#108213),(#108214,#108215),(#108216,#108217),(#108218,#108219),
(#108220,#108221),(#108222,#108223),(#108224,#108225),(#108226,#108227),
(#108228,#108229),(#108230,#108231),(#108232,#108233),(#108234,#108235),
(#108236,#108237),(#108238,#108239),(#108240,#108241),(#108242,#108243),
(#108244,#108245),(#108246,#108247),(#108248,#108249),(#108250,#108251),
(#108252,#108253),(#108254,#108255),(#108256,#108257),(#108258,#108259),
(#108260,#108261),(#108262,#108263),(#108264,#108265),(#108266,#108267),
(#108268,#108269),(#108270,#108271),(#108272,#108273),(#108274,#108275),
(#108276,#108277),(#108278,#108279),(#108280,#108281),(#108282,#108283),
(#108284,#108285),(#108286,#108287),(#108288,#108289),(#108290,#108291),
(#108292,#108293),(#108294,#108295),(#108296,#108297),(#108298,#108299),
(#108300,#108301),(#108302,#108303),(#108304,#108305),(#108306,#108307),
(#108308,#108309),(#108310,#108311),(#108312,#108313),(#108314,#108315),
(#108316,#108317),(#108318,#108319),(#108320,#108321),(#108322,#108323),
(#108324,#108325),(#108326,#108327),(#108328,#108329),(#108330,#108331),
(#108332,#108333),(#108334,#108335),(#108336,#108337),(#108338,#108339),
(#108340,#108341),(#108342,#108343),(#108344,#108345),(#108346,#108347),
(#108348,#108349),(#108350,#108351),(#108352,#108353),(#108354,#108355),
(#108356,#108357),(#108358,#108359),(#108360,#108361),(#108362,#108363),
(#108364,#108365),(#108366,#108367),(#108368,#108369),(#108370,#108371),
(#108372,#108373),(#108374,#108375),(#108376,#108377),(#108378,#108379),
(#108380,#108381),(#108382,#108383),(#108384,#108385),(#108386,#108387),
(#108388,#108389),(#108390,#108391),(#108392,#108393),(#108394,#108395),
(#108396,#108397),(#108398,#108399),(#108400,#108401),(#108402,#108403),
(#108404,#108405),(#108406,#108407),(#108408,#108409),(#108410,#108411),
(#108412,#108413),(#108414,#108415),(#108416,#108417),(#108418,#108419),
(#108420,#108421),(#108422,#108423),(#108424,#108425),(#108426,#108427),
(#108428,#108429),(#108430,#108431),(#108432,#108433),(#108434,#108435),
(#108436,#108437),(#108438,#108439),(#108440,#108441),(#108442,#108443),
(#108444,#108445),(#108446,#108447),(#108448,#108449),(#108450,#108451),
(#108452,#108453),(#108454,#108455),(#108456,#108457),(#108458,#108459),
(#108460,#108461),(#108462,#108463),(#108464,#108465),(#108466,#108467),
(#108468,#108469),(#108470,#108471),(#108472,#108473),(#108474,#108475),
(#108476,#108477),(#108478,#108479),(#108480,#108481),(#108482,#108483),
(#108484,#108485),(#108486,#108487),(#108488,#108489),(#108490,#108491),
(#108492,#108493),(#108494,#108495),(#108496,#108497),(#108498,#108499),
(#108500,#108501),(#108502,#108503),(#108504,#108505),(#108506,#108507),
(#108508,#108509),(#108510,#108511),(#108512,#108513),(#108514,#108515),
(#108516,#108517),(#108518,#108519),(#108520,#108521),(#108522,#108523),
(#108524,#108525),(#108526,#108527),(#108528,#108529),(#108530,#108531),
(#108532,#108533),(#108534,#108535),(#108536,#108537),(#108538,#108539),
(#108540,#108541),(#108542,#108543),(#108544,#108545),(#108546,#108547),
(#108548,#108549),(#108550,#108551),(#108552,#108553),(#108554,#108555),
(#108556,#108557),(#108558,#108559),(#108560,#108561),(#108562,#108563),
(#108564,#108565),(#108566,#108567),(#108568,#108569),(#108570,#108571),
(#108572,#108573),(#108574,#108575),(#108576,#108577),(#108578,#108579),
(#108580,#108581),(#108582,#108583)),.UNSPECIFIED.,.F.,.F.,.F.)
B_SPLINE_SURFACE_WITH_KNOTS((6,1,1,1,1,1,1,1,1,1,1,1,1,1,1,1,1,1,1,1,1,
1,1,1,1,1,1,1,1,1,1,1,1,1,1,1,1,1,1,1,1,1,1,1,1,1,1,1,1,1,1,1,1,1,1,1,1,
1,1,1,1,1,1,1,1,1,1,1,1,1,1,1,1,1,1,1,1,1,1,1,1,1,1,1,1,1,1,1,1,1,1,1,1,
1,1,1,1,1,1,1,1,1,1,1,1,1,1,1,1,1,1,1,1,1,1,1,1,1,1,1,1,1,1,1,1,1,1,1,1,
1,1,1,1,1,1,1,1,1,1,1,1,1,1,1,1,1,1,1,1,1,1,1,1,1,1,1,1,1,1,1,1,1,1,1,1,
1,1,1,1,1,1,1,1,1,1,1,1,1,1,1,1,1,1,1,1,1,1,1,1,1,1,1,1,1,1,1,1,1,1,1,6),
(2,2),(0.,0.005,0.01,0.015,0.02,0.025,0.03,0.035,0.04,0.045,0.05,0.055,
0.06,0.065,0.07,0.075,0.08,0.085,0.09,0.095,0.1,0.105,0.11,0.115,0.12,0.125,
0.13,0.135,0.14,0.145,0.15,0.155,0.16,0.165,0.17,0.175,0.18,0.185,0.19,
0.195,0.2,0.205,0.21,0.215,0.22,0.225,0.23,0.235,0.24,0.245,0.25,0.255,
0.26,0.265,0.27,0.275,0.28,0.285,0.29,0.295,0.3,0.305,0.31,0.315,0.32,0.325,
0.33,0.335,0.34,0.345,0.35,0.355,0.36,0.365,0.37,0.375,0.38,0.385,0.39,
0.395,0.4,0.405,0.41,0.415,0.42,0.425,0.43,0.435,0.44,0.445,0.45,0.455,
0.46,0.465,0.47,0.475,0.48,0.485,0.49,0.495,0.5,0.505,0.51,0.515,0.52,0.525,
0.53,0.535,0.54,0.545,0.55,0.555,0.56,0.565,0.57,0.575,0.58,0.585,0.59,
0.595,0.6,0.605,0.61,0.615,0.62,0.625,0.63,0.635,0.64,0.645,0.65,0.655,
0.66,0.665,0.67,0.675,0.68,0.685,0.690000000000001,0.695000000000001,0.700000000000001,
0.705000000000001,0.710000000000001,0.715000000000001,0.720000000000001,
0.725000000000001,0.730000000000001,0.735000000000001,0.740000000000001,
0.745000000000001,0.750000000000001,0.755000000000001,0.760000000000001,
0.765000000000001,0.770000000000001,0.775000000000001,0.780000000000001,
0.785000000000001,0.790000000000001,0.795000000000001,0.800000000000001,
0.805000000000001,0.810000000000001,0.815000000000001,0.820000000000001,
0.825000000000001,0.830000000000001,0.835000000000001,0.840000000000001,
0.845000000000001,0.850000000000001,0.855000000000001,0.860000000000001,
0.865000000000001,0.870000000000001,0.875000000000001,0.880000000000001,
0.885000000000001,0.890000000000001,0.895000000000001,0.900000000000001,
0.905000000000001,0.910000000000001,0.915000000000001,0.920000000000001,
0.925000000000001,0.930000000000001,0.935000000000001,0.940000000000001,
0.945000000000001,0.950000000000001,0.955000000000001,0.960000000000001,
0.965000000000001,0.970000000000001,0.975000000000001,0.980000000000001,
0.985000000000001,0.990000000000001,0.995000000000001,1.),(0.,1.2),
 .UNSPECIFIED.)
GEOMETRIC_REPRESENTATION_ITEM()
RATIONAL_B_SPLINE_SURFACE(((1.,1.),(1.,1.),(1.,1.),(1.,1.),(1.,1.),(1.,
1.),(1.,1.),(1.,1.),(1.,1.),(1.,1.),(1.,1.),(1.,1.),(1.,1.),(1.,1.),(1.,
1.),(1.,1.),(1.,1.),(1.,1.),(1.,1.),(1.,1.),(1.,1.),(1.,1.),(1.,1.),(1.,
1.),(1.,1.),(1.,1.),(1.,1.),(1.,1.),(1.,1.),(1.,1.),(1.,1.),(1.,1.),(1.,
1.),(1.,1.),(1.,1.),(1.,1.),(1.,1.),(1.,1.),(1.,1.),(1.,1.),(1.,1.),(1.,
1.),(1.,1.),(1.,1.),(1.,1.),(1.,1.),(1.,1.),(1.,1.),(1.,1.),(1.,1.),(1.,
1.),(1.,1.),(1.,1.),(1.,1.),(1.,1.),(1.,1.),(1.,1.),(1.,1.),(1.,1.),(1.,
1.),(1.,1.),(1.,1.),(1.,1.),(1.,1.),(1.,1.),(1.,1.),(1.,1.),(1.,1.),(1.,
1.),(1.,1.),(1.,1.),(1.,1.),(1.,1.),(1.,1.),(1.,1.),(1.,1.),(1.,1.),(1.,
1.),(1.,1.),(1.,1.),(1.,1.),(1.,1.),(1.,1.),(1.,1.),(1.,1.),(1.,1.),(1.,
1.),(1.,1.),(1.,1.),(1.,1.),(1.,1.),(1.,1.),(1.,1.),(1.,1.),(1.,1.),(1.,
1.),(1.,1.),(1.,1.),(1.,1.),(1.,1.),(1.,1.),(1.,1.),(1.,1.),(1.,1.),(1.,
1.),(1.,1.),(1.,1.),(1.,1.),(1.,1.),(1.,1.),(1.,1.),(1.,1.),(1.,1.),(1.,
1.),(1.,1.),(1.,1.),(1.,1.),(1.,1.),(1.,1.),(1.,1.),(1.,1.),(1.,1.),(1.,
1.),(1.,1.),(1.,1.),(1.,1.),(1.,1.),(1.,1.),(1.,1.),(1.,1.),(1.,1.),(1.,
1.),(1.,1.),(1.,1.),(1.,1.),(1.,1.),(1.,1.),(1.,1.),(1.,1.),(1.,1.),(1.,
1.),(1.,1.),(1.,1.),(1.,1.),(1.,1.),(1.,1.),(1.,1.),(1.,1.),(1.,1.),(1.,
1.),(1.,1.),(1.,1.),(1.,1.),(1.,1.),(1.,1.),(1.,1.),(1.,1.),(1.,1.),(1.,
1.),(1.,1.),(1.,1.),(1.,1.),(1.,1.),(1.,1.),(1.,1.),(1.,1.),(1.,1.),(1.,
1.),(1.,1.),(1.,1.),(1.,1.),(1.,1.),(1.,1.),(1.,1.),(1.,1.),(1.,1.),(1.,
1.),(1.,1.),(1.,1.),(1.,1.),(1.,1.),(1.,1.),(1.,1.),(1.,1.),(1.,1.),(1.,
1.),(1.,1.),(1.,1.),(1.,1.),(1.,1.),(1.,1.),(1.,1.),(1.,1.),(1.,1.),(1.,
1.),(1.,1.),(1.,1.),(1.,1.),(1.,1.),(1.,1.),(1.,1.),(1.,1.),(1.,1.),(1.,
1.),(1.,1.)))
REPRESENTATION_ITEM('')
SURFACE()
);
#946=(
BOUNDED_SURFACE()
B_SPLINE_SURFACE(5,1,((#109070,#109071),(#109072,#109073),(#109074,#109075),
(#109076,#109077),(#109078,#109079),(#109080,#109081),(#109082,#109083),
(#109084,#109085),(#109086,#109087),(#109088,#109089),(#109090,#109091),
(#109092,#109093),(#109094,#109095),(#109096,#109097),(#109098,#109099),
(#109100,#109101),(#109102,#109103),(#109104,#109105),(#109106,#109107),
(#109108,#109109),(#109110,#109111),(#109112,#109113),(#109114,#109115),
(#109116,#109117),(#109118,#109119),(#109120,#109121),(#109122,#109123),
(#109124,#109125),(#109126,#109127),(#109128,#109129),(#109130,#109131),
(#109132,#109133),(#109134,#109135),(#109136,#109137),(#109138,#109139),
(#109140,#109141),(#109142,#109143),(#109144,#109145),(#109146,#109147),
(#109148,#109149),(#109150,#109151),(#109152,#109153),(#109154,#109155),
(#109156,#109157),(#109158,#109159),(#109160,#109161),(#109162,#109163),
(#109164,#109165),(#109166,#109167),(#109168,#109169),(#109170,#109171),
(#109172,#109173),(#109174,#109175),(#109176,#109177),(#109178,#109179),
(#109180,#109181),(#109182,#109183),(#109184,#109185),(#109186,#109187),
(#109188,#109189),(#109190,#109191),(#109192,#109193),(#109194,#109195),
(#109196,#109197),(#109198,#109199),(#109200,#109201),(#109202,#109203),
(#109204,#109205),(#109206,#109207),(#109208,#109209),(#109210,#109211),
(#109212,#109213),(#109214,#109215),(#109216,#109217),(#109218,#109219),
(#109220,#109221),(#109222,#109223),(#109224,#109225),(#109226,#109227),
(#109228,#109229),(#109230,#109231),(#109232,#109233),(#109234,#109235),
(#109236,#109237),(#109238,#109239),(#109240,#109241),(#109242,#109243),
(#109244,#109245),(#109246,#109247),(#109248,#109249),(#109250,#109251),
(#109252,#109253),(#109254,#109255),(#109256,#109257),(#109258,#109259),
(#109260,#109261),(#109262,#109263),(#109264,#109265),(#109266,#109267),
(#109268,#109269),(#109270,#109271),(#109272,#109273),(#109274,#109275),
(#109276,#109277),(#109278,#109279),(#109280,#109281),(#109282,#109283),
(#109284,#109285),(#109286,#109287),(#109288,#109289),(#109290,#109291),
(#109292,#109293),(#109294,#109295),(#109296,#109297),(#109298,#109299),
(#109300,#109301),(#109302,#109303),(#109304,#109305),(#109306,#109307),
(#109308,#109309),(#109310,#109311),(#109312,#109313),(#109314,#109315),
(#109316,#109317),(#109318,#109319),(#109320,#109321),(#109322,#109323),
(#109324,#109325),(#109326,#109327),(#109328,#109329),(#109330,#109331),
(#109332,#109333),(#109334,#109335),(#109336,#109337),(#109338,#109339),
(#109340,#109341),(#109342,#109343),(#109344,#109345),(#109346,#109347),
(#109348,#109349),(#109350,#109351),(#109352,#109353),(#109354,#109355),
(#109356,#109357),(#109358,#109359),(#109360,#109361),(#109362,#109363),
(#109364,#109365),(#109366,#109367),(#109368,#109369),(#109370,#109371),
(#109372,#109373),(#109374,#109375),(#109376,#109377),(#109378,#109379),
(#109380,#109381),(#109382,#109383),(#109384,#109385),(#109386,#109387),
(#109388,#109389),(#109390,#109391),(#109392,#109393),(#109394,#109395),
(#109396,#109397),(#109398,#109399),(#109400,#109401),(#109402,#109403),
(#109404,#109405),(#109406,#109407),(#109408,#109409),(#109410,#109411),
(#109412,#109413),(#109414,#109415),(#109416,#109417),(#109418,#109419),
(#109420,#109421),(#109422,#109423),(#109424,#109425),(#109426,#109427),
(#109428,#109429),(#109430,#109431),(#109432,#109433),(#109434,#109435),
(#109436,#109437),(#109438,#109439),(#109440,#109441),(#109442,#109443),
(#109444,#109445),(#109446,#109447),(#109448,#109449),(#109450,#109451),
(#109452,#109453),(#109454,#109455),(#109456,#109457),(#109458,#109459),
(#109460,#109461),(#109462,#109463),(#109464,#109465),(#109466,#109467),
(#109468,#109469),(#109470,#109471),(#109472,#109473),(#109474,#109475),
(#109476,#109477),(#109478,#109479)),.UNSPECIFIED.,.F.,.F.,.F.)
B_SPLINE_SURFACE_WITH_KNOTS((6,1,1,1,1,1,1,1,1,1,1,1,1,1,1,1,1,1,1,1,1,
1,1,1,1,1,1,1,1,1,1,1,1,1,1,1,1,1,1,1,1,1,1,1,1,1,1,1,1,1,1,1,1,1,1,1,1,
1,1,1,1,1,1,1,1,1,1,1,1,1,1,1,1,1,1,1,1,1,1,1,1,1,1,1,1,1,1,1,1,1,1,1,1,
1,1,1,1,1,1,1,1,1,1,1,1,1,1,1,1,1,1,1,1,1,1,1,1,1,1,1,1,1,1,1,1,1,1,1,1,
1,1,1,1,1,1,1,1,1,1,1,1,1,1,1,1,1,1,1,1,1,1,1,1,1,1,1,1,1,1,1,1,1,1,1,1,
1,1,1,1,1,1,1,1,1,1,1,1,1,1,1,1,1,1,1,1,1,1,1,1,1,1,1,1,1,1,1,1,1,1,1,6),
(2,2),(0.,0.005,0.01,0.015,0.02,0.025,0.03,0.035,0.04,0.045,0.05,0.055,
0.06,0.065,0.07,0.075,0.08,0.085,0.09,0.095,0.1,0.105,0.11,0.115,0.12,0.125,
0.13,0.135,0.14,0.145,0.15,0.155,0.16,0.165,0.17,0.175,0.18,0.185,0.19,
0.195,0.2,0.205,0.21,0.215,0.22,0.225,0.23,0.235,0.24,0.245,0.25,0.255,
0.26,0.265,0.27,0.275,0.28,0.285,0.29,0.295,0.3,0.305,0.31,0.315,0.32,0.325,
0.33,0.335,0.34,0.345,0.35,0.355,0.36,0.365,0.37,0.375,0.38,0.385,0.39,
0.395,0.4,0.405,0.41,0.415,0.42,0.425,0.43,0.435,0.44,0.445,0.45,0.455,
0.46,0.465,0.47,0.475,0.48,0.485,0.49,0.495,0.5,0.505,0.51,0.515,0.52,0.525,
0.53,0.535,0.54,0.545,0.55,0.555,0.56,0.565,0.57,0.575,0.58,0.585,0.59,
0.595,0.6,0.605,0.61,0.615,0.62,0.625,0.63,0.635,0.64,0.645,0.65,0.655,
0.66,0.665,0.67,0.675,0.68,0.685,0.690000000000001,0.695000000000001,0.700000000000001,
0.705000000000001,0.710000000000001,0.715000000000001,0.720000000000001,
0.725000000000001,0.730000000000001,0.735000000000001,0.740000000000001,
0.745000000000001,0.750000000000001,0.755000000000001,0.760000000000001,
0.765000000000001,0.770000000000001,0.775000000000001,0.780000000000001,
0.785000000000001,0.790000000000001,0.795000000000001,0.800000000000001,
0.805000000000001,0.810000000000001,0.815000000000001,0.820000000000001,
0.825000000000001,0.830000000000001,0.835000000000001,0.840000000000001,
0.845000000000001,0.850000000000001,0.855000000000001,0.860000000000001,
0.865000000000001,0.870000000000001,0.875000000000001,0.880000000000001,
0.885000000000001,0.890000000000001,0.895000000000001,0.900000000000001,
0.905000000000001,0.910000000000001,0.915000000000001,0.920000000000001,
0.925000000000001,0.930000000000001,0.935000000000001,0.940000000000001,
0.945000000000001,0.950000000000001,0.955000000000001,0.960000000000001,
0.965000000000001,0.970000000000001,0.975000000000001,0.980000000000001,
0.985000000000001,0.990000000000001,0.995000000000001,1.),(0.,1.2),
 .UNSPECIFIED.)
GEOMETRIC_REPRESENTATION_ITEM()
RATIONAL_B_SPLINE_SURFACE(((1.,1.),(1.,1.),(1.,1.),(1.,1.),(1.,1.),(1.,
1.),(1.,1.),(1.,1.),(1.,1.),(1.,1.),(1.,1.),(1.,1.),(1.,1.),(1.,1.),(1.,
1.),(1.,1.),(1.,1.),(1.,1.),(1.,1.),(1.,1.),(1.,1.),(1.,1.),(1.,1.),(1.,
1.),(1.,1.),(1.,1.),(1.,1.),(1.,1.),(1.,1.),(1.,1.),(1.,1.),(1.,1.),(1.,
1.),(1.,1.),(1.,1.),(1.,1.),(1.,1.),(1.,1.),(1.,1.),(1.,1.),(1.,1.),(1.,
1.),(1.,1.),(1.,1.),(1.,1.),(1.,1.),(1.,1.),(1.,1.),(1.,1.),(1.,1.),(1.,
1.),(1.,1.),(1.,1.),(1.,1.),(1.,1.),(1.,1.),(1.,1.),(1.,1.),(1.,1.),(1.,
1.),(1.,1.),(1.,1.),(1.,1.),(1.,1.),(1.,1.),(1.,1.),(1.,1.),(1.,1.),(1.,
1.),(1.,1.),(1.,1.),(1.,1.),(1.,1.),(1.,1.),(1.,1.),(1.,1.),(1.,1.),(1.,
1.),(1.,1.),(1.,1.),(1.,1.),(1.,1.),(1.,1.),(1.,1.),(1.,1.),(1.,1.),(1.,
1.),(1.,1.),(1.,1.),(1.,1.),(1.,1.),(1.,1.),(1.,1.),(1.,1.),(1.,1.),(1.,
1.),(1.,1.),(1.,1.),(1.,1.),(1.,1.),(1.,1.),(1.,1.),(1.,1.),(1.,1.),(1.,
1.),(1.,1.),(1.,1.),(1.,1.),(1.,1.),(1.,1.),(1.,1.),(1.,1.),(1.,1.),(1.,
1.),(1.,1.),(1.,1.),(1.,1.),(1.,1.),(1.,1.),(1.,1.),(1.,1.),(1.,1.),(1.,
1.),(1.,1.),(1.,1.),(1.,1.),(1.,1.),(1.,1.),(1.,1.),(1.,1.),(1.,1.),(1.,
1.),(1.,1.),(1.,1.),(1.,1.),(1.,1.),(1.,1.),(1.,1.),(1.,1.),(1.,1.),(1.,
1.),(1.,1.),(1.,1.),(1.,1.),(1.,1.),(1.,1.),(1.,1.),(1.,1.),(1.,1.),(1.,
1.),(1.,1.),(1.,1.),(1.,1.),(1.,1.),(1.,1.),(1.,1.),(1.,1.),(1.,1.),(1.,
1.),(1.,1.),(1.,1.),(1.,1.),(1.,1.),(1.,1.),(1.,1.),(1.,1.),(1.,1.),(1.,
1.),(1.,1.),(1.,1.),(1.,1.),(1.,1.),(1.,1.),(1.,1.),(1.,1.),(1.,1.),(1.,
1.),(1.,1.),(1.,1.),(1.,1.),(1.,1.),(1.,1.),(1.,1.),(1.,1.),(1.,1.),(1.,
1.),(1.,1.),(1.,1.),(1.,1.),(1.,1.),(1.,1.),(1.,1.),(1.,1.),(1.,1.),(1.,
1.),(1.,1.),(1.,1.),(1.,1.),(1.,1.),(1.,1.),(1.,1.),(1.,1.),(1.,1.),(1.,
1.),(1.,1.)))
REPRESENTATION_ITEM('')
SURFACE()
);
#947=(
BOUNDED_SURFACE()
B_SPLINE_SURFACE(5,1,((#109966,#109967),(#109968,#109969),(#109970,#109971),
(#109972,#109973),(#109974,#109975),(#109976,#109977),(#109978,#109979),
(#109980,#109981),(#109982,#109983),(#109984,#109985),(#109986,#109987),
(#109988,#109989),(#109990,#109991),(#109992,#109993),(#109994,#109995),
(#109996,#109997),(#109998,#109999),(#110000,#110001),(#110002,#110003),
(#110004,#110005),(#110006,#110007),(#110008,#110009),(#110010,#110011),
(#110012,#110013),(#110014,#110015),(#110016,#110017),(#110018,#110019),
(#110020,#110021),(#110022,#110023),(#110024,#110025),(#110026,#110027),
(#110028,#110029),(#110030,#110031),(#110032,#110033),(#110034,#110035),
(#110036,#110037),(#110038,#110039),(#110040,#110041),(#110042,#110043),
(#110044,#110045),(#110046,#110047),(#110048,#110049),(#110050,#110051),
(#110052,#110053),(#110054,#110055),(#110056,#110057),(#110058,#110059),
(#110060,#110061),(#110062,#110063),(#110064,#110065),(#110066,#110067),
(#110068,#110069),(#110070,#110071),(#110072,#110073),(#110074,#110075),
(#110076,#110077),(#110078,#110079),(#110080,#110081),(#110082,#110083),
(#110084,#110085),(#110086,#110087),(#110088,#110089),(#110090,#110091),
(#110092,#110093),(#110094,#110095),(#110096,#110097),(#110098,#110099),
(#110100,#110101),(#110102,#110103),(#110104,#110105),(#110106,#110107),
(#110108,#110109),(#110110,#110111),(#110112,#110113),(#110114,#110115),
(#110116,#110117),(#110118,#110119),(#110120,#110121),(#110122,#110123),
(#110124,#110125),(#110126,#110127),(#110128,#110129),(#110130,#110131),
(#110132,#110133),(#110134,#110135),(#110136,#110137),(#110138,#110139),
(#110140,#110141),(#110142,#110143),(#110144,#110145),(#110146,#110147),
(#110148,#110149),(#110150,#110151),(#110152,#110153),(#110154,#110155),
(#110156,#110157),(#110158,#110159),(#110160,#110161),(#110162,#110163),
(#110164,#110165),(#110166,#110167),(#110168,#110169),(#110170,#110171),
(#110172,#110173),(#110174,#110175),(#110176,#110177),(#110178,#110179),
(#110180,#110181),(#110182,#110183),(#110184,#110185),(#110186,#110187),
(#110188,#110189),(#110190,#110191),(#110192,#110193),(#110194,#110195),
(#110196,#110197),(#110198,#110199),(#110200,#110201),(#110202,#110203),
(#110204,#110205),(#110206,#110207),(#110208,#110209),(#110210,#110211),
(#110212,#110213),(#110214,#110215),(#110216,#110217),(#110218,#110219),
(#110220,#110221),(#110222,#110223),(#110224,#110225),(#110226,#110227),
(#110228,#110229),(#110230,#110231),(#110232,#110233),(#110234,#110235),
(#110236,#110237),(#110238,#110239),(#110240,#110241),(#110242,#110243),
(#110244,#110245),(#110246,#110247),(#110248,#110249),(#110250,#110251),
(#110252,#110253),(#110254,#110255),(#110256,#110257),(#110258,#110259),
(#110260,#110261),(#110262,#110263),(#110264,#110265),(#110266,#110267),
(#110268,#110269),(#110270,#110271),(#110272,#110273),(#110274,#110275),
(#110276,#110277),(#110278,#110279),(#110280,#110281),(#110282,#110283),
(#110284,#110285),(#110286,#110287),(#110288,#110289),(#110290,#110291),
(#110292,#110293),(#110294,#110295),(#110296,#110297),(#110298,#110299),
(#110300,#110301),(#110302,#110303),(#110304,#110305),(#110306,#110307),
(#110308,#110309),(#110310,#110311),(#110312,#110313),(#110314,#110315),
(#110316,#110317),(#110318,#110319),(#110320,#110321),(#110322,#110323),
(#110324,#110325),(#110326,#110327),(#110328,#110329),(#110330,#110331),
(#110332,#110333),(#110334,#110335),(#110336,#110337),(#110338,#110339),
(#110340,#110341),(#110342,#110343),(#110344,#110345),(#110346,#110347),
(#110348,#110349),(#110350,#110351),(#110352,#110353),(#110354,#110355),
(#110356,#110357),(#110358,#110359),(#110360,#110361),(#110362,#110363),
(#110364,#110365),(#110366,#110367),(#110368,#110369),(#110370,#110371),
(#110372,#110373),(#110374,#110375)),.UNSPECIFIED.,.F.,.F.,.F.)
B_SPLINE_SURFACE_WITH_KNOTS((6,1,1,1,1,1,1,1,1,1,1,1,1,1,1,1,1,1,1,1,1,
1,1,1,1,1,1,1,1,1,1,1,1,1,1,1,1,1,1,1,1,1,1,1,1,1,1,1,1,1,1,1,1,1,1,1,1,
1,1,1,1,1,1,1,1,1,1,1,1,1,1,1,1,1,1,1,1,1,1,1,1,1,1,1,1,1,1,1,1,1,1,1,1,
1,1,1,1,1,1,1,1,1,1,1,1,1,1,1,1,1,1,1,1,1,1,1,1,1,1,1,1,1,1,1,1,1,1,1,1,
1,1,1,1,1,1,1,1,1,1,1,1,1,1,1,1,1,1,1,1,1,1,1,1,1,1,1,1,1,1,1,1,1,1,1,1,
1,1,1,1,1,1,1,1,1,1,1,1,1,1,1,1,1,1,1,1,1,1,1,1,1,1,1,1,1,1,1,1,1,1,1,6),
(2,2),(0.,0.005,0.01,0.015,0.02,0.025,0.03,0.035,0.04,0.045,0.05,0.055,
0.06,0.065,0.07,0.075,0.08,0.085,0.09,0.095,0.1,0.105,0.11,0.115,0.12,0.125,
0.13,0.135,0.14,0.145,0.15,0.155,0.16,0.165,0.17,0.175,0.18,0.185,0.19,
0.195,0.2,0.205,0.21,0.215,0.22,0.225,0.23,0.235,0.24,0.245,0.25,0.255,
0.26,0.265,0.27,0.275,0.28,0.285,0.29,0.295,0.3,0.305,0.31,0.315,0.32,0.325,
0.33,0.335,0.34,0.345,0.35,0.355,0.36,0.365,0.37,0.375,0.38,0.385,0.39,
0.395,0.4,0.405,0.41,0.415,0.42,0.425,0.43,0.435,0.44,0.445,0.45,0.455,
0.46,0.465,0.47,0.475,0.48,0.485,0.49,0.495,0.5,0.505,0.51,0.515,0.52,0.525,
0.53,0.535,0.54,0.545,0.55,0.555,0.56,0.565,0.57,0.575,0.58,0.585,0.59,
0.595,0.6,0.605,0.61,0.615,0.62,0.625,0.63,0.635,0.64,0.645,0.65,0.655,
0.66,0.665,0.67,0.675,0.68,0.685,0.690000000000001,0.695000000000001,0.700000000000001,
0.705000000000001,0.710000000000001,0.715000000000001,0.720000000000001,
0.725000000000001,0.730000000000001,0.735000000000001,0.740000000000001,
0.745000000000001,0.750000000000001,0.755000000000001,0.760000000000001,
0.765000000000001,0.770000000000001,0.775000000000001,0.780000000000001,
0.785000000000001,0.790000000000001,0.795000000000001,0.800000000000001,
0.805000000000001,0.810000000000001,0.815000000000001,0.820000000000001,
0.825000000000001,0.830000000000001,0.835000000000001,0.840000000000001,
0.845000000000001,0.850000000000001,0.855000000000001,0.860000000000001,
0.865000000000001,0.870000000000001,0.875000000000001,0.880000000000001,
0.885000000000001,0.890000000000001,0.895000000000001,0.900000000000001,
0.905000000000001,0.910000000000001,0.915000000000001,0.920000000000001,
0.925000000000001,0.930000000000001,0.935000000000001,0.940000000000001,
0.945000000000001,0.950000000000001,0.955000000000001,0.960000000000001,
0.965000000000001,0.970000000000001,0.975000000000001,0.980000000000001,
0.985000000000001,0.990000000000001,0.995000000000001,1.),(0.,1.2),
 .UNSPECIFIED.)
GEOMETRIC_REPRESENTATION_ITEM()
RATIONAL_B_SPLINE_SURFACE(((1.,1.),(1.,1.),(1.,1.),(1.,1.),(1.,1.),(1.,
1.),(1.,1.),(1.,1.),(1.,1.),(1.,1.),(1.,1.),(1.,1.),(1.,1.),(1.,1.),(1.,
1.),(1.,1.),(1.,1.),(1.,1.),(1.,1.),(1.,1.),(1.,1.),(1.,1.),(1.,1.),(1.,
1.),(1.,1.),(1.,1.),(1.,1.),(1.,1.),(1.,1.),(1.,1.),(1.,1.),(1.,1.),(1.,
1.),(1.,1.),(1.,1.),(1.,1.),(1.,1.),(1.,1.),(1.,1.),(1.,1.),(1.,1.),(1.,
1.),(1.,1.),(1.,1.),(1.,1.),(1.,1.),(1.,1.),(1.,1.),(1.,1.),(1.,1.),(1.,
1.),(1.,1.),(1.,1.),(1.,1.),(1.,1.),(1.,1.),(1.,1.),(1.,1.),(1.,1.),(1.,
1.),(1.,1.),(1.,1.),(1.,1.),(1.,1.),(1.,1.),(1.,1.),(1.,1.),(1.,1.),(1.,
1.),(1.,1.),(1.,1.),(1.,1.),(1.,1.),(1.,1.),(1.,1.),(1.,1.),(1.,1.),(1.,
1.),(1.,1.),(1.,1.),(1.,1.),(1.,1.),(1.,1.),(1.,1.),(1.,1.),(1.,1.),(1.,
1.),(1.,1.),(1.,1.),(1.,1.),(1.,1.),(1.,1.),(1.,1.),(1.,1.),(1.,1.),(1.,
1.),(1.,1.),(1.,1.),(1.,1.),(1.,1.),(1.,1.),(1.,1.),(1.,1.),(1.,1.),(1.,
1.),(1.,1.),(1.,1.),(1.,1.),(1.,1.),(1.,1.),(1.,1.),(1.,1.),(1.,1.),(1.,
1.),(1.,1.),(1.,1.),(1.,1.),(1.,1.),(1.,1.),(1.,1.),(1.,1.),(1.,1.),(1.,
1.),(1.,1.),(1.,1.),(1.,1.),(1.,1.),(1.,1.),(1.,1.),(1.,1.),(1.,1.),(1.,
1.),(1.,1.),(1.,1.),(1.,1.),(1.,1.),(1.,1.),(1.,1.),(1.,1.),(1.,1.),(1.,
1.),(1.,1.),(1.,1.),(1.,1.),(1.,1.),(1.,1.),(1.,1.),(1.,1.),(1.,1.),(1.,
1.),(1.,1.),(1.,1.),(1.,1.),(1.,1.),(1.,1.),(1.,1.),(1.,1.),(1.,1.),(1.,
1.),(1.,1.),(1.,1.),(1.,1.),(1.,1.),(1.,1.),(1.,1.),(1.,1.),(1.,1.),(1.,
1.),(1.,1.),(1.,1.),(1.,1.),(1.,1.),(1.,1.),(1.,1.),(1.,1.),(1.,1.),(1.,
1.),(1.,1.),(1.,1.),(1.,1.),(1.,1.),(1.,1.),(1.,1.),(1.,1.),(1.,1.),(1.,
1.),(1.,1.),(1.,1.),(1.,1.),(1.,1.),(1.,1.),(1.,1.),(1.,1.),(1.,1.),(1.,
1.),(1.,1.),(1.,1.),(1.,1.),(1.,1.),(1.,1.),(1.,1.),(1.,1.),(1.,1.),(1.,
1.),(1.,1.)))
REPRESENTATION_ITEM('')
SURFACE()
);
#948=(
BOUNDED_SURFACE()
B_SPLINE_SURFACE(5,1,((#110862,#110863),(#110864,#110865),(#110866,#110867),
(#110868,#110869),(#110870,#110871),(#110872,#110873),(#110874,#110875),
(#110876,#110877),(#110878,#110879),(#110880,#110881),(#110882,#110883),
(#110884,#110885),(#110886,#110887),(#110888,#110889),(#110890,#110891),
(#110892,#110893),(#110894,#110895),(#110896,#110897),(#110898,#110899),
(#110900,#110901),(#110902,#110903),(#110904,#110905),(#110906,#110907),
(#110908,#110909),(#110910,#110911),(#110912,#110913),(#110914,#110915),
(#110916,#110917),(#110918,#110919),(#110920,#110921),(#110922,#110923),
(#110924,#110925),(#110926,#110927),(#110928,#110929),(#110930,#110931),
(#110932,#110933),(#110934,#110935),(#110936,#110937),(#110938,#110939),
(#110940,#110941),(#110942,#110943),(#110944,#110945),(#110946,#110947),
(#110948,#110949),(#110950,#110951),(#110952,#110953),(#110954,#110955),
(#110956,#110957),(#110958,#110959),(#110960,#110961),(#110962,#110963),
(#110964,#110965),(#110966,#110967),(#110968,#110969),(#110970,#110971),
(#110972,#110973),(#110974,#110975),(#110976,#110977),(#110978,#110979),
(#110980,#110981),(#110982,#110983),(#110984,#110985),(#110986,#110987),
(#110988,#110989),(#110990,#110991),(#110992,#110993),(#110994,#110995),
(#110996,#110997),(#110998,#110999),(#111000,#111001),(#111002,#111003),
(#111004,#111005),(#111006,#111007),(#111008,#111009),(#111010,#111011),
(#111012,#111013),(#111014,#111015),(#111016,#111017),(#111018,#111019),
(#111020,#111021),(#111022,#111023),(#111024,#111025),(#111026,#111027),
(#111028,#111029),(#111030,#111031),(#111032,#111033),(#111034,#111035),
(#111036,#111037),(#111038,#111039),(#111040,#111041),(#111042,#111043),
(#111044,#111045),(#111046,#111047),(#111048,#111049),(#111050,#111051),
(#111052,#111053),(#111054,#111055),(#111056,#111057),(#111058,#111059),
(#111060,#111061),(#111062,#111063),(#111064,#111065),(#111066,#111067),
(#111068,#111069),(#111070,#111071),(#111072,#111073),(#111074,#111075),
(#111076,#111077),(#111078,#111079),(#111080,#111081),(#111082,#111083),
(#111084,#111085),(#111086,#111087),(#111088,#111089),(#111090,#111091),
(#111092,#111093),(#111094,#111095),(#111096,#111097),(#111098,#111099),
(#111100,#111101),(#111102,#111103),(#111104,#111105),(#111106,#111107),
(#111108,#111109),(#111110,#111111),(#111112,#111113),(#111114,#111115),
(#111116,#111117),(#111118,#111119),(#111120,#111121),(#111122,#111123),
(#111124,#111125),(#111126,#111127),(#111128,#111129),(#111130,#111131),
(#111132,#111133),(#111134,#111135),(#111136,#111137),(#111138,#111139),
(#111140,#111141),(#111142,#111143),(#111144,#111145),(#111146,#111147),
(#111148,#111149),(#111150,#111151),(#111152,#111153),(#111154,#111155),
(#111156,#111157),(#111158,#111159),(#111160,#111161),(#111162,#111163),
(#111164,#111165),(#111166,#111167),(#111168,#111169),(#111170,#111171),
(#111172,#111173),(#111174,#111175),(#111176,#111177),(#111178,#111179),
(#111180,#111181),(#111182,#111183),(#111184,#111185),(#111186,#111187),
(#111188,#111189),(#111190,#111191),(#111192,#111193),(#111194,#111195),
(#111196,#111197),(#111198,#111199),(#111200,#111201),(#111202,#111203),
(#111204,#111205),(#111206,#111207),(#111208,#111209),(#111210,#111211),
(#111212,#111213),(#111214,#111215),(#111216,#111217),(#111218,#111219),
(#111220,#111221),(#111222,#111223),(#111224,#111225),(#111226,#111227),
(#111228,#111229),(#111230,#111231),(#111232,#111233),(#111234,#111235),
(#111236,#111237),(#111238,#111239),(#111240,#111241),(#111242,#111243),
(#111244,#111245),(#111246,#111247),(#111248,#111249),(#111250,#111251),
(#111252,#111253),(#111254,#111255),(#111256,#111257),(#111258,#111259),
(#111260,#111261),(#111262,#111263),(#111264,#111265),(#111266,#111267),
(#111268,#111269),(#111270,#111271)),.UNSPECIFIED.,.F.,.F.,.F.)
B_SPLINE_SURFACE_WITH_KNOTS((6,1,1,1,1,1,1,1,1,1,1,1,1,1,1,1,1,1,1,1,1,
1,1,1,1,1,1,1,1,1,1,1,1,1,1,1,1,1,1,1,1,1,1,1,1,1,1,1,1,1,1,1,1,1,1,1,1,
1,1,1,1,1,1,1,1,1,1,1,1,1,1,1,1,1,1,1,1,1,1,1,1,1,1,1,1,1,1,1,1,1,1,1,1,
1,1,1,1,1,1,1,1,1,1,1,1,1,1,1,1,1,1,1,1,1,1,1,1,1,1,1,1,1,1,1,1,1,1,1,1,
1,1,1,1,1,1,1,1,1,1,1,1,1,1,1,1,1,1,1,1,1,1,1,1,1,1,1,1,1,1,1,1,1,1,1,1,
1,1,1,1,1,1,1,1,1,1,1,1,1,1,1,1,1,1,1,1,1,1,1,1,1,1,1,1,1,1,1,1,1,1,1,6),
(2,2),(0.,0.005,0.01,0.015,0.02,0.025,0.03,0.035,0.04,0.045,0.05,0.055,
0.06,0.065,0.07,0.075,0.08,0.085,0.09,0.095,0.1,0.105,0.11,0.115,0.12,0.125,
0.13,0.135,0.14,0.145,0.15,0.155,0.16,0.165,0.17,0.175,0.18,0.185,0.19,
0.195,0.2,0.205,0.21,0.215,0.22,0.225,0.23,0.235,0.24,0.245,0.25,0.255,
0.26,0.265,0.27,0.275,0.28,0.285,0.29,0.295,0.3,0.305,0.31,0.315,0.32,0.325,
0.33,0.335,0.34,0.345,0.35,0.355,0.36,0.365,0.37,0.375,0.38,0.385,0.39,
0.395,0.4,0.405,0.41,0.415,0.42,0.425,0.43,0.435,0.44,0.445,0.45,0.455,
0.46,0.465,0.47,0.475,0.48,0.485,0.49,0.495,0.5,0.505,0.51,0.515,0.52,0.525,
0.53,0.535,0.54,0.545,0.55,0.555,0.56,0.565,0.57,0.575,0.58,0.585,0.59,
0.595,0.6,0.605,0.61,0.615,0.62,0.625,0.63,0.635,0.64,0.645,0.65,0.655,
0.66,0.665,0.67,0.675,0.68,0.685,0.690000000000001,0.695000000000001,0.700000000000001,
0.705000000000001,0.710000000000001,0.715000000000001,0.720000000000001,
0.725000000000001,0.730000000000001,0.735000000000001,0.740000000000001,
0.745000000000001,0.750000000000001,0.755000000000001,0.760000000000001,
0.765000000000001,0.770000000000001,0.775000000000001,0.780000000000001,
0.785000000000001,0.790000000000001,0.795000000000001,0.800000000000001,
0.805000000000001,0.810000000000001,0.815000000000001,0.820000000000001,
0.825000000000001,0.830000000000001,0.835000000000001,0.840000000000001,
0.845000000000001,0.850000000000001,0.855000000000001,0.860000000000001,
0.865000000000001,0.870000000000001,0.875000000000001,0.880000000000001,
0.885000000000001,0.890000000000001,0.895000000000001,0.900000000000001,
0.905000000000001,0.910000000000001,0.915000000000001,0.920000000000001,
0.925000000000001,0.930000000000001,0.935000000000001,0.940000000000001,
0.945000000000001,0.950000000000001,0.955000000000001,0.960000000000001,
0.965000000000001,0.970000000000001,0.975000000000001,0.980000000000001,
0.985000000000001,0.990000000000001,0.995000000000001,1.),(0.,1.2),
 .UNSPECIFIED.)
GEOMETRIC_REPRESENTATION_ITEM()
RATIONAL_B_SPLINE_SURFACE(((1.,1.),(1.,1.),(1.,1.),(1.,1.),(1.,1.),(1.,
1.),(1.,1.),(1.,1.),(1.,1.),(1.,1.),(1.,1.),(1.,1.),(1.,1.),(1.,1.),(1.,
1.),(1.,1.),(1.,1.),(1.,1.),(1.,1.),(1.,1.),(1.,1.),(1.,1.),(1.,1.),(1.,
1.),(1.,1.),(1.,1.),(1.,1.),(1.,1.),(1.,1.),(1.,1.),(1.,1.),(1.,1.),(1.,
1.),(1.,1.),(1.,1.),(1.,1.),(1.,1.),(1.,1.),(1.,1.),(1.,1.),(1.,1.),(1.,
1.),(1.,1.),(1.,1.),(1.,1.),(1.,1.),(1.,1.),(1.,1.),(1.,1.),(1.,1.),(1.,
1.),(1.,1.),(1.,1.),(1.,1.),(1.,1.),(1.,1.),(1.,1.),(1.,1.),(1.,1.),(1.,
1.),(1.,1.),(1.,1.),(1.,1.),(1.,1.),(1.,1.),(1.,1.),(1.,1.),(1.,1.),(1.,
1.),(1.,1.),(1.,1.),(1.,1.),(1.,1.),(1.,1.),(1.,1.),(1.,1.),(1.,1.),(1.,
1.),(1.,1.),(1.,1.),(1.,1.),(1.,1.),(1.,1.),(1.,1.),(1.,1.),(1.,1.),(1.,
1.),(1.,1.),(1.,1.),(1.,1.),(1.,1.),(1.,1.),(1.,1.),(1.,1.),(1.,1.),(1.,
1.),(1.,1.),(1.,1.),(1.,1.),(1.,1.),(1.,1.),(1.,1.),(1.,1.),(1.,1.),(1.,
1.),(1.,1.),(1.,1.),(1.,1.),(1.,1.),(1.,1.),(1.,1.),(1.,1.),(1.,1.),(1.,
1.),(1.,1.),(1.,1.),(1.,1.),(1.,1.),(1.,1.),(1.,1.),(1.,1.),(1.,1.),(1.,
1.),(1.,1.),(1.,1.),(1.,1.),(1.,1.),(1.,1.),(1.,1.),(1.,1.),(1.,1.),(1.,
1.),(1.,1.),(1.,1.),(1.,1.),(1.,1.),(1.,1.),(1.,1.),(1.,1.),(1.,1.),(1.,
1.),(1.,1.),(1.,1.),(1.,1.),(1.,1.),(1.,1.),(1.,1.),(1.,1.),(1.,1.),(1.,
1.),(1.,1.),(1.,1.),(1.,1.),(1.,1.),(1.,1.),(1.,1.),(1.,1.),(1.,1.),(1.,
1.),(1.,1.),(1.,1.),(1.,1.),(1.,1.),(1.,1.),(1.,1.),(1.,1.),(1.,1.),(1.,
1.),(1.,1.),(1.,1.),(1.,1.),(1.,1.),(1.,1.),(1.,1.),(1.,1.),(1.,1.),(1.,
1.),(1.,1.),(1.,1.),(1.,1.),(1.,1.),(1.,1.),(1.,1.),(1.,1.),(1.,1.),(1.,
1.),(1.,1.),(1.,1.),(1.,1.),(1.,1.),(1.,1.),(1.,1.),(1.,1.),(1.,1.),(1.,
1.),(1.,1.),(1.,1.),(1.,1.),(1.,1.),(1.,1.),(1.,1.),(1.,1.),(1.,1.),(1.,
1.),(1.,1.)))
REPRESENTATION_ITEM('')
SURFACE()
);
#949=(
BOUNDED_SURFACE()
B_SPLINE_SURFACE(5,1,((#111758,#111759),(#111760,#111761),(#111762,#111763),
(#111764,#111765),(#111766,#111767),(#111768,#111769),(#111770,#111771),
(#111772,#111773),(#111774,#111775),(#111776,#111777),(#111778,#111779),
(#111780,#111781),(#111782,#111783),(#111784,#111785),(#111786,#111787),
(#111788,#111789),(#111790,#111791),(#111792,#111793),(#111794,#111795),
(#111796,#111797),(#111798,#111799),(#111800,#111801),(#111802,#111803),
(#111804,#111805),(#111806,#111807),(#111808,#111809),(#111810,#111811),
(#111812,#111813),(#111814,#111815),(#111816,#111817),(#111818,#111819),
(#111820,#111821),(#111822,#111823),(#111824,#111825),(#111826,#111827),
(#111828,#111829),(#111830,#111831),(#111832,#111833),(#111834,#111835),
(#111836,#111837),(#111838,#111839),(#111840,#111841),(#111842,#111843),
(#111844,#111845),(#111846,#111847),(#111848,#111849),(#111850,#111851),
(#111852,#111853),(#111854,#111855),(#111856,#111857),(#111858,#111859),
(#111860,#111861),(#111862,#111863),(#111864,#111865),(#111866,#111867),
(#111868,#111869),(#111870,#111871),(#111872,#111873),(#111874,#111875),
(#111876,#111877),(#111878,#111879),(#111880,#111881),(#111882,#111883),
(#111884,#111885),(#111886,#111887),(#111888,#111889),(#111890,#111891),
(#111892,#111893),(#111894,#111895),(#111896,#111897),(#111898,#111899),
(#111900,#111901),(#111902,#111903),(#111904,#111905),(#111906,#111907),
(#111908,#111909),(#111910,#111911),(#111912,#111913),(#111914,#111915),
(#111916,#111917),(#111918,#111919),(#111920,#111921),(#111922,#111923),
(#111924,#111925),(#111926,#111927),(#111928,#111929),(#111930,#111931),
(#111932,#111933),(#111934,#111935),(#111936,#111937),(#111938,#111939),
(#111940,#111941),(#111942,#111943),(#111944,#111945),(#111946,#111947),
(#111948,#111949),(#111950,#111951),(#111952,#111953),(#111954,#111955),
(#111956,#111957),(#111958,#111959),(#111960,#111961),(#111962,#111963),
(#111964,#111965),(#111966,#111967),(#111968,#111969),(#111970,#111971),
(#111972,#111973),(#111974,#111975),(#111976,#111977),(#111978,#111979),
(#111980,#111981),(#111982,#111983),(#111984,#111985),(#111986,#111987),
(#111988,#111989),(#111990,#111991),(#111992,#111993),(#111994,#111995),
(#111996,#111997),(#111998,#111999),(#112000,#112001),(#112002,#112003),
(#112004,#112005),(#112006,#112007),(#112008,#112009),(#112010,#112011),
(#112012,#112013),(#112014,#112015),(#112016,#112017),(#112018,#112019),
(#112020,#112021),(#112022,#112023),(#112024,#112025),(#112026,#112027),
(#112028,#112029),(#112030,#112031),(#112032,#112033),(#112034,#112035),
(#112036,#112037),(#112038,#112039),(#112040,#112041),(#112042,#112043),
(#112044,#112045),(#112046,#112047),(#112048,#112049),(#112050,#112051),
(#112052,#112053),(#112054,#112055),(#112056,#112057),(#112058,#112059),
(#112060,#112061),(#112062,#112063),(#112064,#112065),(#112066,#112067),
(#112068,#112069),(#112070,#112071),(#112072,#112073),(#112074,#112075),
(#112076,#112077),(#112078,#112079),(#112080,#112081),(#112082,#112083),
(#112084,#112085),(#112086,#112087),(#112088,#112089),(#112090,#112091),
(#112092,#112093),(#112094,#112095),(#112096,#112097),(#112098,#112099),
(#112100,#112101),(#112102,#112103),(#112104,#112105),(#112106,#112107),
(#112108,#112109),(#112110,#112111),(#112112,#112113),(#112114,#112115),
(#112116,#112117),(#112118,#112119),(#112120,#112121),(#112122,#112123),
(#112124,#112125),(#112126,#112127),(#112128,#112129),(#112130,#112131),
(#112132,#112133),(#112134,#112135),(#112136,#112137),(#112138,#112139),
(#112140,#112141),(#112142,#112143),(#112144,#112145),(#112146,#112147),
(#112148,#112149),(#112150,#112151),(#112152,#112153),(#112154,#112155),
(#112156,#112157),(#112158,#112159),(#112160,#112161),(#112162,#112163),
(#112164,#112165),(#112166,#112167)),.UNSPECIFIED.,.F.,.F.,.F.)
B_SPLINE_SURFACE_WITH_KNOTS((6,1,1,1,1,1,1,1,1,1,1,1,1,1,1,1,1,1,1,1,1,
1,1,1,1,1,1,1,1,1,1,1,1,1,1,1,1,1,1,1,1,1,1,1,1,1,1,1,1,1,1,1,1,1,1,1,1,
1,1,1,1,1,1,1,1,1,1,1,1,1,1,1,1,1,1,1,1,1,1,1,1,1,1,1,1,1,1,1,1,1,1,1,1,
1,1,1,1,1,1,1,1,1,1,1,1,1,1,1,1,1,1,1,1,1,1,1,1,1,1,1,1,1,1,1,1,1,1,1,1,
1,1,1,1,1,1,1,1,1,1,1,1,1,1,1,1,1,1,1,1,1,1,1,1,1,1,1,1,1,1,1,1,1,1,1,1,
1,1,1,1,1,1,1,1,1,1,1,1,1,1,1,1,1,1,1,1,1,1,1,1,1,1,1,1,1,1,1,1,1,1,1,6),
(2,2),(0.,0.005,0.01,0.015,0.02,0.025,0.03,0.035,0.04,0.045,0.05,0.055,
0.06,0.065,0.07,0.075,0.08,0.085,0.09,0.095,0.1,0.105,0.11,0.115,0.12,0.125,
0.13,0.135,0.14,0.145,0.15,0.155,0.16,0.165,0.17,0.175,0.18,0.185,0.19,
0.195,0.2,0.205,0.21,0.215,0.22,0.225,0.23,0.235,0.24,0.245,0.25,0.255,
0.26,0.265,0.27,0.275,0.28,0.285,0.29,0.295,0.3,0.305,0.31,0.315,0.32,0.325,
0.33,0.335,0.34,0.345,0.35,0.355,0.36,0.365,0.37,0.375,0.38,0.385,0.39,
0.395,0.4,0.405,0.41,0.415,0.42,0.425,0.43,0.435,0.44,0.445,0.45,0.455,
0.46,0.465,0.47,0.475,0.48,0.485,0.49,0.495,0.5,0.505,0.51,0.515,0.52,0.525,
0.53,0.535,0.54,0.545,0.55,0.555,0.56,0.565,0.57,0.575,0.58,0.585,0.59,
0.595,0.6,0.605,0.61,0.615,0.62,0.625,0.63,0.635,0.64,0.645,0.65,0.655,
0.66,0.665,0.67,0.675,0.68,0.685,0.690000000000001,0.695000000000001,0.700000000000001,
0.705000000000001,0.710000000000001,0.715000000000001,0.720000000000001,
0.725000000000001,0.730000000000001,0.735000000000001,0.740000000000001,
0.745000000000001,0.750000000000001,0.755000000000001,0.760000000000001,
0.765000000000001,0.770000000000001,0.775000000000001,0.780000000000001,
0.785000000000001,0.790000000000001,0.795000000000001,0.800000000000001,
0.805000000000001,0.810000000000001,0.815000000000001,0.820000000000001,
0.825000000000001,0.830000000000001,0.835000000000001,0.840000000000001,
0.845000000000001,0.850000000000001,0.855000000000001,0.860000000000001,
0.865000000000001,0.870000000000001,0.875000000000001,0.880000000000001,
0.885000000000001,0.890000000000001,0.895000000000001,0.900000000000001,
0.905000000000001,0.910000000000001,0.915000000000001,0.920000000000001,
0.925000000000001,0.930000000000001,0.935000000000001,0.940000000000001,
0.945000000000001,0.950000000000001,0.955000000000001,0.960000000000001,
0.965000000000001,0.970000000000001,0.975000000000001,0.980000000000001,
0.985000000000001,0.990000000000001,0.995000000000001,1.),(0.,1.2),
 .UNSPECIFIED.)
GEOMETRIC_REPRESENTATION_ITEM()
RATIONAL_B_SPLINE_SURFACE(((1.,1.),(1.,1.),(1.,1.),(1.,1.),(1.,1.),(1.,
1.),(1.,1.),(1.,1.),(1.,1.),(1.,1.),(1.,1.),(1.,1.),(1.,1.),(1.,1.),(1.,
1.),(1.,1.),(1.,1.),(1.,1.),(1.,1.),(1.,1.),(1.,1.),(1.,1.),(1.,1.),(1.,
1.),(1.,1.),(1.,1.),(1.,1.),(1.,1.),(1.,1.),(1.,1.),(1.,1.),(1.,1.),(1.,
1.),(1.,1.),(1.,1.),(1.,1.),(1.,1.),(1.,1.),(1.,1.),(1.,1.),(1.,1.),(1.,
1.),(1.,1.),(1.,1.),(1.,1.),(1.,1.),(1.,1.),(1.,1.),(1.,1.),(1.,1.),(1.,
1.),(1.,1.),(1.,1.),(1.,1.),(1.,1.),(1.,1.),(1.,1.),(1.,1.),(1.,1.),(1.,
1.),(1.,1.),(1.,1.),(1.,1.),(1.,1.),(1.,1.),(1.,1.),(1.,1.),(1.,1.),(1.,
1.),(1.,1.),(1.,1.),(1.,1.),(1.,1.),(1.,1.),(1.,1.),(1.,1.),(1.,1.),(1.,
1.),(1.,1.),(1.,1.),(1.,1.),(1.,1.),(1.,1.),(1.,1.),(1.,1.),(1.,1.),(1.,
1.),(1.,1.),(1.,1.),(1.,1.),(1.,1.),(1.,1.),(1.,1.),(1.,1.),(1.,1.),(1.,
1.),(1.,1.),(1.,1.),(1.,1.),(1.,1.),(1.,1.),(1.,1.),(1.,1.),(1.,1.),(1.,
1.),(1.,1.),(1.,1.),(1.,1.),(1.,1.),(1.,1.),(1.,1.),(1.,1.),(1.,1.),(1.,
1.),(1.,1.),(1.,1.),(1.,1.),(1.,1.),(1.,1.),(1.,1.),(1.,1.),(1.,1.),(1.,
1.),(1.,1.),(1.,1.),(1.,1.),(1.,1.),(1.,1.),(1.,1.),(1.,1.),(1.,1.),(1.,
1.),(1.,1.),(1.,1.),(1.,1.),(1.,1.),(1.,1.),(1.,1.),(1.,1.),(1.,1.),(1.,
1.),(1.,1.),(1.,1.),(1.,1.),(1.,1.),(1.,1.),(1.,1.),(1.,1.),(1.,1.),(1.,
1.),(1.,1.),(1.,1.),(1.,1.),(1.,1.),(1.,1.),(1.,1.),(1.,1.),(1.,1.),(1.,
1.),(1.,1.),(1.,1.),(1.,1.),(1.,1.),(1.,1.),(1.,1.),(1.,1.),(1.,1.),(1.,
1.),(1.,1.),(1.,1.),(1.,1.),(1.,1.),(1.,1.),(1.,1.),(1.,1.),(1.,1.),(1.,
1.),(1.,1.),(1.,1.),(1.,1.),(1.,1.),(1.,1.),(1.,1.),(1.,1.),(1.,1.),(1.,
1.),(1.,1.),(1.,1.),(1.,1.),(1.,1.),(1.,1.),(1.,1.),(1.,1.),(1.,1.),(1.,
1.),(1.,1.),(1.,1.),(1.,1.),(1.,1.),(1.,1.),(1.,1.),(1.,1.),(1.,1.),(1.,
1.),(1.,1.)))
REPRESENTATION_ITEM('')
SURFACE()
);
#950=(
BOUNDED_SURFACE()
B_SPLINE_SURFACE(5,1,((#112654,#112655),(#112656,#112657),(#112658,#112659),
(#112660,#112661),(#112662,#112663),(#112664,#112665),(#112666,#112667),
(#112668,#112669),(#112670,#112671),(#112672,#112673),(#112674,#112675),
(#112676,#112677),(#112678,#112679),(#112680,#112681),(#112682,#112683),
(#112684,#112685),(#112686,#112687),(#112688,#112689),(#112690,#112691),
(#112692,#112693),(#112694,#112695),(#112696,#112697),(#112698,#112699),
(#112700,#112701),(#112702,#112703),(#112704,#112705),(#112706,#112707),
(#112708,#112709),(#112710,#112711),(#112712,#112713),(#112714,#112715),
(#112716,#112717),(#112718,#112719),(#112720,#112721),(#112722,#112723),
(#112724,#112725),(#112726,#112727),(#112728,#112729),(#112730,#112731),
(#112732,#112733),(#112734,#112735),(#112736,#112737),(#112738,#112739),
(#112740,#112741),(#112742,#112743),(#112744,#112745),(#112746,#112747),
(#112748,#112749),(#112750,#112751),(#112752,#112753),(#112754,#112755),
(#112756,#112757),(#112758,#112759),(#112760,#112761),(#112762,#112763),
(#112764,#112765),(#112766,#112767),(#112768,#112769),(#112770,#112771),
(#112772,#112773),(#112774,#112775),(#112776,#112777),(#112778,#112779),
(#112780,#112781),(#112782,#112783),(#112784,#112785),(#112786,#112787),
(#112788,#112789),(#112790,#112791),(#112792,#112793),(#112794,#112795),
(#112796,#112797),(#112798,#112799),(#112800,#112801),(#112802,#112803),
(#112804,#112805),(#112806,#112807),(#112808,#112809),(#112810,#112811),
(#112812,#112813),(#112814,#112815),(#112816,#112817),(#112818,#112819),
(#112820,#112821),(#112822,#112823),(#112824,#112825),(#112826,#112827),
(#112828,#112829),(#112830,#112831),(#112832,#112833),(#112834,#112835),
(#112836,#112837),(#112838,#112839),(#112840,#112841),(#112842,#112843),
(#112844,#112845),(#112846,#112847),(#112848,#112849),(#112850,#112851),
(#112852,#112853),(#112854,#112855),(#112856,#112857),(#112858,#112859),
(#112860,#112861),(#112862,#112863),(#112864,#112865),(#112866,#112867),
(#112868,#112869),(#112870,#112871),(#112872,#112873),(#112874,#112875),
(#112876,#112877),(#112878,#112879),(#112880,#112881),(#112882,#112883),
(#112884,#112885),(#112886,#112887),(#112888,#112889),(#112890,#112891),
(#112892,#112893),(#112894,#112895),(#112896,#112897),(#112898,#112899),
(#112900,#112901),(#112902,#112903),(#112904,#112905),(#112906,#112907),
(#112908,#112909),(#112910,#112911),(#112912,#112913),(#112914,#112915),
(#112916,#112917),(#112918,#112919),(#112920,#112921),(#112922,#112923),
(#112924,#112925),(#112926,#112927),(#112928,#112929),(#112930,#112931),
(#112932,#112933),(#112934,#112935),(#112936,#112937),(#112938,#112939),
(#112940,#112941),(#112942,#112943),(#112944,#112945),(#112946,#112947),
(#112948,#112949),(#112950,#112951),(#112952,#112953),(#112954,#112955),
(#112956,#112957),(#112958,#112959),(#112960,#112961),(#112962,#112963),
(#112964,#112965),(#112966,#112967),(#112968,#112969),(#112970,#112971),
(#112972,#112973),(#112974,#112975),(#112976,#112977),(#112978,#112979),
(#112980,#112981),(#112982,#112983),(#112984,#112985),(#112986,#112987),
(#112988,#112989),(#112990,#112991),(#112992,#112993),(#112994,#112995),
(#112996,#112997),(#112998,#112999),(#113000,#113001),(#113002,#113003),
(#113004,#113005),(#113006,#113007),(#113008,#113009),(#113010,#113011),
(#113012,#113013),(#113014,#113015),(#113016,#113017),(#113018,#113019),
(#113020,#113021),(#113022,#113023),(#113024,#113025),(#113026,#113027),
(#113028,#113029),(#113030,#113031),(#113032,#113033),(#113034,#113035),
(#113036,#113037),(#113038,#113039),(#113040,#113041),(#113042,#113043),
(#113044,#113045),(#113046,#113047),(#113048,#113049),(#113050,#113051),
(#113052,#113053),(#113054,#113055),(#113056,#113057),(#113058,#113059),
(#113060,#113061),(#113062,#113063)),.UNSPECIFIED.,.F.,.F.,.F.)
B_SPLINE_SURFACE_WITH_KNOTS((6,1,1,1,1,1,1,1,1,1,1,1,1,1,1,1,1,1,1,1,1,
1,1,1,1,1,1,1,1,1,1,1,1,1,1,1,1,1,1,1,1,1,1,1,1,1,1,1,1,1,1,1,1,1,1,1,1,
1,1,1,1,1,1,1,1,1,1,1,1,1,1,1,1,1,1,1,1,1,1,1,1,1,1,1,1,1,1,1,1,1,1,1,1,
1,1,1,1,1,1,1,1,1,1,1,1,1,1,1,1,1,1,1,1,1,1,1,1,1,1,1,1,1,1,1,1,1,1,1,1,
1,1,1,1,1,1,1,1,1,1,1,1,1,1,1,1,1,1,1,1,1,1,1,1,1,1,1,1,1,1,1,1,1,1,1,1,
1,1,1,1,1,1,1,1,1,1,1,1,1,1,1,1,1,1,1,1,1,1,1,1,1,1,1,1,1,1,1,1,1,1,1,6),
(2,2),(0.,0.005,0.01,0.015,0.02,0.025,0.03,0.035,0.04,0.045,0.05,0.055,
0.06,0.065,0.07,0.075,0.08,0.085,0.09,0.095,0.1,0.105,0.11,0.115,0.12,0.125,
0.13,0.135,0.14,0.145,0.15,0.155,0.16,0.165,0.17,0.175,0.18,0.185,0.19,
0.195,0.2,0.205,0.21,0.215,0.22,0.225,0.23,0.235,0.24,0.245,0.25,0.255,
0.26,0.265,0.27,0.275,0.28,0.285,0.29,0.295,0.3,0.305,0.31,0.315,0.32,0.325,
0.33,0.335,0.34,0.345,0.35,0.355,0.36,0.365,0.37,0.375,0.38,0.385,0.39,
0.395,0.4,0.405,0.41,0.415,0.42,0.425,0.43,0.435,0.44,0.445,0.45,0.455,
0.46,0.465,0.47,0.475,0.48,0.485,0.49,0.495,0.5,0.505,0.51,0.515,0.52,0.525,
0.53,0.535,0.54,0.545,0.55,0.555,0.56,0.565,0.57,0.575,0.58,0.585,0.59,
0.595,0.6,0.605,0.61,0.615,0.62,0.625,0.63,0.635,0.64,0.645,0.65,0.655,
0.66,0.665,0.67,0.675,0.68,0.685,0.690000000000001,0.695000000000001,0.700000000000001,
0.705000000000001,0.710000000000001,0.715000000000001,0.720000000000001,
0.725000000000001,0.730000000000001,0.735000000000001,0.740000000000001,
0.745000000000001,0.750000000000001,0.755000000000001,0.760000000000001,
0.765000000000001,0.770000000000001,0.775000000000001,0.780000000000001,
0.785000000000001,0.790000000000001,0.795000000000001,0.800000000000001,
0.805000000000001,0.810000000000001,0.815000000000001,0.820000000000001,
0.825000000000001,0.830000000000001,0.835000000000001,0.840000000000001,
0.845000000000001,0.850000000000001,0.855000000000001,0.860000000000001,
0.865000000000001,0.870000000000001,0.875000000000001,0.880000000000001,
0.885000000000001,0.890000000000001,0.895000000000001,0.900000000000001,
0.905000000000001,0.910000000000001,0.915000000000001,0.920000000000001,
0.925000000000001,0.930000000000001,0.935000000000001,0.940000000000001,
0.945000000000001,0.950000000000001,0.955000000000001,0.960000000000001,
0.965000000000001,0.970000000000001,0.975000000000001,0.980000000000001,
0.985000000000001,0.990000000000001,0.995000000000001,1.),(0.,1.2),
 .UNSPECIFIED.)
GEOMETRIC_REPRESENTATION_ITEM()
RATIONAL_B_SPLINE_SURFACE(((1.,1.),(1.,1.),(1.,1.),(1.,1.),(1.,1.),(1.,
1.),(1.,1.),(1.,1.),(1.,1.),(1.,1.),(1.,1.),(1.,1.),(1.,1.),(1.,1.),(1.,
1.),(1.,1.),(1.,1.),(1.,1.),(1.,1.),(1.,1.),(1.,1.),(1.,1.),(1.,1.),(1.,
1.),(1.,1.),(1.,1.),(1.,1.),(1.,1.),(1.,1.),(1.,1.),(1.,1.),(1.,1.),(1.,
1.),(1.,1.),(1.,1.),(1.,1.),(1.,1.),(1.,1.),(1.,1.),(1.,1.),(1.,1.),(1.,
1.),(1.,1.),(1.,1.),(1.,1.),(1.,1.),(1.,1.),(1.,1.),(1.,1.),(1.,1.),(1.,
1.),(1.,1.),(1.,1.),(1.,1.),(1.,1.),(1.,1.),(1.,1.),(1.,1.),(1.,1.),(1.,
1.),(1.,1.),(1.,1.),(1.,1.),(1.,1.),(1.,1.),(1.,1.),(1.,1.),(1.,1.),(1.,
1.),(1.,1.),(1.,1.),(1.,1.),(1.,1.),(1.,1.),(1.,1.),(1.,1.),(1.,1.),(1.,
1.),(1.,1.),(1.,1.),(1.,1.),(1.,1.),(1.,1.),(1.,1.),(1.,1.),(1.,1.),(1.,
1.),(1.,1.),(1.,1.),(1.,1.),(1.,1.),(1.,1.),(1.,1.),(1.,1.),(1.,1.),(1.,
1.),(1.,1.),(1.,1.),(1.,1.),(1.,1.),(1.,1.),(1.,1.),(1.,1.),(1.,1.),(1.,
1.),(1.,1.),(1.,1.),(1.,1.),(1.,1.),(1.,1.),(1.,1.),(1.,1.),(1.,1.),(1.,
1.),(1.,1.),(1.,1.),(1.,1.),(1.,1.),(1.,1.),(1.,1.),(1.,1.),(1.,1.),(1.,
1.),(1.,1.),(1.,1.),(1.,1.),(1.,1.),(1.,1.),(1.,1.),(1.,1.),(1.,1.),(1.,
1.),(1.,1.),(1.,1.),(1.,1.),(1.,1.),(1.,1.),(1.,1.),(1.,1.),(1.,1.),(1.,
1.),(1.,1.),(1.,1.),(1.,1.),(1.,1.),(1.,1.),(1.,1.),(1.,1.),(1.,1.),(1.,
1.),(1.,1.),(1.,1.),(1.,1.),(1.,1.),(1.,1.),(1.,1.),(1.,1.),(1.,1.),(1.,
1.),(1.,1.),(1.,1.),(1.,1.),(1.,1.),(1.,1.),(1.,1.),(1.,1.),(1.,1.),(1.,
1.),(1.,1.),(1.,1.),(1.,1.),(1.,1.),(1.,1.),(1.,1.),(1.,1.),(1.,1.),(1.,
1.),(1.,1.),(1.,1.),(1.,1.),(1.,1.),(1.,1.),(1.,1.),(1.,1.),(1.,1.),(1.,
1.),(1.,1.),(1.,1.),(1.,1.),(1.,1.),(1.,1.),(1.,1.),(1.,1.),(1.,1.),(1.,
1.),(1.,1.),(1.,1.),(1.,1.),(1.,1.),(1.,1.),(1.,1.),(1.,1.),(1.,1.),(1.,
1.),(1.,1.)))
REPRESENTATION_ITEM('')
SURFACE()
);
#951=(
BOUNDED_SURFACE()
B_SPLINE_SURFACE(5,1,((#113550,#113551),(#113552,#113553),(#113554,#113555),
(#113556,#113557),(#113558,#113559),(#113560,#113561),(#113562,#113563),
(#113564,#113565),(#113566,#113567),(#113568,#113569),(#113570,#113571),
(#113572,#113573),(#113574,#113575),(#113576,#113577),(#113578,#113579),
(#113580,#113581),(#113582,#113583),(#113584,#113585),(#113586,#113587),
(#113588,#113589),(#113590,#113591),(#113592,#113593),(#113594,#113595),
(#113596,#113597),(#113598,#113599),(#113600,#113601),(#113602,#113603),
(#113604,#113605),(#113606,#113607),(#113608,#113609),(#113610,#113611),
(#113612,#113613),(#113614,#113615),(#113616,#113617),(#113618,#113619),
(#113620,#113621),(#113622,#113623),(#113624,#113625),(#113626,#113627),
(#113628,#113629),(#113630,#113631),(#113632,#113633),(#113634,#113635),
(#113636,#113637),(#113638,#113639),(#113640,#113641),(#113642,#113643),
(#113644,#113645),(#113646,#113647),(#113648,#113649),(#113650,#113651),
(#113652,#113653),(#113654,#113655),(#113656,#113657),(#113658,#113659),
(#113660,#113661),(#113662,#113663),(#113664,#113665),(#113666,#113667),
(#113668,#113669),(#113670,#113671),(#113672,#113673),(#113674,#113675),
(#113676,#113677),(#113678,#113679),(#113680,#113681),(#113682,#113683),
(#113684,#113685),(#113686,#113687),(#113688,#113689),(#113690,#113691),
(#113692,#113693),(#113694,#113695),(#113696,#113697),(#113698,#113699),
(#113700,#113701),(#113702,#113703),(#113704,#113705),(#113706,#113707),
(#113708,#113709),(#113710,#113711),(#113712,#113713),(#113714,#113715),
(#113716,#113717),(#113718,#113719),(#113720,#113721),(#113722,#113723),
(#113724,#113725),(#113726,#113727),(#113728,#113729),(#113730,#113731),
(#113732,#113733),(#113734,#113735),(#113736,#113737),(#113738,#113739),
(#113740,#113741),(#113742,#113743),(#113744,#113745),(#113746,#113747),
(#113748,#113749),(#113750,#113751),(#113752,#113753),(#113754,#113755),
(#113756,#113757),(#113758,#113759),(#113760,#113761),(#113762,#113763),
(#113764,#113765),(#113766,#113767),(#113768,#113769),(#113770,#113771),
(#113772,#113773),(#113774,#113775),(#113776,#113777),(#113778,#113779),
(#113780,#113781),(#113782,#113783),(#113784,#113785),(#113786,#113787),
(#113788,#113789),(#113790,#113791),(#113792,#113793),(#113794,#113795),
(#113796,#113797),(#113798,#113799),(#113800,#113801),(#113802,#113803),
(#113804,#113805),(#113806,#113807),(#113808,#113809),(#113810,#113811),
(#113812,#113813),(#113814,#113815),(#113816,#113817),(#113818,#113819),
(#113820,#113821),(#113822,#113823),(#113824,#113825),(#113826,#113827),
(#113828,#113829),(#113830,#113831),(#113832,#113833),(#113834,#113835),
(#113836,#113837),(#113838,#113839),(#113840,#113841),(#113842,#113843),
(#113844,#113845),(#113846,#113847),(#113848,#113849),(#113850,#113851),
(#113852,#113853),(#113854,#113855),(#113856,#113857),(#113858,#113859),
(#113860,#113861),(#113862,#113863),(#113864,#113865),(#113866,#113867),
(#113868,#113869),(#113870,#113871),(#113872,#113873),(#113874,#113875),
(#113876,#113877),(#113878,#113879),(#113880,#113881),(#113882,#113883),
(#113884,#113885),(#113886,#113887),(#113888,#113889),(#113890,#113891),
(#113892,#113893),(#113894,#113895),(#113896,#113897),(#113898,#113899),
(#113900,#113901),(#113902,#113903),(#113904,#113905),(#113906,#113907),
(#113908,#113909),(#113910,#113911),(#113912,#113913),(#113914,#113915),
(#113916,#113917),(#113918,#113919),(#113920,#113921),(#113922,#113923),
(#113924,#113925),(#113926,#113927),(#113928,#113929),(#113930,#113931),
(#113932,#113933),(#113934,#113935),(#113936,#113937),(#113938,#113939),
(#113940,#113941),(#113942,#113943),(#113944,#113945),(#113946,#113947),
(#113948,#113949),(#113950,#113951),(#113952,#113953),(#113954,#113955),
(#113956,#113957),(#113958,#113959)),.UNSPECIFIED.,.F.,.F.,.F.)
B_SPLINE_SURFACE_WITH_KNOTS((6,1,1,1,1,1,1,1,1,1,1,1,1,1,1,1,1,1,1,1,1,
1,1,1,1,1,1,1,1,1,1,1,1,1,1,1,1,1,1,1,1,1,1,1,1,1,1,1,1,1,1,1,1,1,1,1,1,
1,1,1,1,1,1,1,1,1,1,1,1,1,1,1,1,1,1,1,1,1,1,1,1,1,1,1,1,1,1,1,1,1,1,1,1,
1,1,1,1,1,1,1,1,1,1,1,1,1,1,1,1,1,1,1,1,1,1,1,1,1,1,1,1,1,1,1,1,1,1,1,1,
1,1,1,1,1,1,1,1,1,1,1,1,1,1,1,1,1,1,1,1,1,1,1,1,1,1,1,1,1,1,1,1,1,1,1,1,
1,1,1,1,1,1,1,1,1,1,1,1,1,1,1,1,1,1,1,1,1,1,1,1,1,1,1,1,1,1,1,1,1,1,1,6),
(2,2),(0.,0.005,0.01,0.015,0.02,0.025,0.03,0.035,0.04,0.045,0.05,0.055,
0.06,0.065,0.07,0.075,0.08,0.085,0.09,0.095,0.1,0.105,0.11,0.115,0.12,0.125,
0.13,0.135,0.14,0.145,0.15,0.155,0.16,0.165,0.17,0.175,0.18,0.185,0.19,
0.195,0.2,0.205,0.21,0.215,0.22,0.225,0.23,0.235,0.24,0.245,0.25,0.255,
0.26,0.265,0.27,0.275,0.28,0.285,0.29,0.295,0.3,0.305,0.31,0.315,0.32,0.325,
0.33,0.335,0.34,0.345,0.35,0.355,0.36,0.365,0.37,0.375,0.38,0.385,0.39,
0.395,0.4,0.405,0.41,0.415,0.42,0.425,0.43,0.435,0.44,0.445,0.45,0.455,
0.46,0.465,0.47,0.475,0.48,0.485,0.49,0.495,0.5,0.505,0.51,0.515,0.52,0.525,
0.53,0.535,0.54,0.545,0.55,0.555,0.56,0.565,0.57,0.575,0.58,0.585,0.59,
0.595,0.6,0.605,0.61,0.615,0.62,0.625,0.63,0.635,0.64,0.645,0.65,0.655,
0.66,0.665,0.67,0.675,0.68,0.685,0.690000000000001,0.695000000000001,0.700000000000001,
0.705000000000001,0.710000000000001,0.715000000000001,0.720000000000001,
0.725000000000001,0.730000000000001,0.735000000000001,0.740000000000001,
0.745000000000001,0.750000000000001,0.755000000000001,0.760000000000001,
0.765000000000001,0.770000000000001,0.775000000000001,0.780000000000001,
0.785000000000001,0.790000000000001,0.795000000000001,0.800000000000001,
0.805000000000001,0.810000000000001,0.815000000000001,0.820000000000001,
0.825000000000001,0.830000000000001,0.835000000000001,0.840000000000001,
0.845000000000001,0.850000000000001,0.855000000000001,0.860000000000001,
0.865000000000001,0.870000000000001,0.875000000000001,0.880000000000001,
0.885000000000001,0.890000000000001,0.895000000000001,0.900000000000001,
0.905000000000001,0.910000000000001,0.915000000000001,0.920000000000001,
0.925000000000001,0.930000000000001,0.935000000000001,0.940000000000001,
0.945000000000001,0.950000000000001,0.955000000000001,0.960000000000001,
0.965000000000001,0.970000000000001,0.975000000000001,0.980000000000001,
0.985000000000001,0.990000000000001,0.995000000000001,1.),(0.,1.2),
 .UNSPECIFIED.)
GEOMETRIC_REPRESENTATION_ITEM()
RATIONAL_B_SPLINE_SURFACE(((1.,1.),(1.,1.),(1.,1.),(1.,1.),(1.,1.),(1.,
1.),(1.,1.),(1.,1.),(1.,1.),(1.,1.),(1.,1.),(1.,1.),(1.,1.),(1.,1.),(1.,
1.),(1.,1.),(1.,1.),(1.,1.),(1.,1.),(1.,1.),(1.,1.),(1.,1.),(1.,1.),(1.,
1.),(1.,1.),(1.,1.),(1.,1.),(1.,1.),(1.,1.),(1.,1.),(1.,1.),(1.,1.),(1.,
1.),(1.,1.),(1.,1.),(1.,1.),(1.,1.),(1.,1.),(1.,1.),(1.,1.),(1.,1.),(1.,
1.),(1.,1.),(1.,1.),(1.,1.),(1.,1.),(1.,1.),(1.,1.),(1.,1.),(1.,1.),(1.,
1.),(1.,1.),(1.,1.),(1.,1.),(1.,1.),(1.,1.),(1.,1.),(1.,1.),(1.,1.),(1.,
1.),(1.,1.),(1.,1.),(1.,1.),(1.,1.),(1.,1.),(1.,1.),(1.,1.),(1.,1.),(1.,
1.),(1.,1.),(1.,1.),(1.,1.),(1.,1.),(1.,1.),(1.,1.),(1.,1.),(1.,1.),(1.,
1.),(1.,1.),(1.,1.),(1.,1.),(1.,1.),(1.,1.),(1.,1.),(1.,1.),(1.,1.),(1.,
1.),(1.,1.),(1.,1.),(1.,1.),(1.,1.),(1.,1.),(1.,1.),(1.,1.),(1.,1.),(1.,
1.),(1.,1.),(1.,1.),(1.,1.),(1.,1.),(1.,1.),(1.,1.),(1.,1.),(1.,1.),(1.,
1.),(1.,1.),(1.,1.),(1.,1.),(1.,1.),(1.,1.),(1.,1.),(1.,1.),(1.,1.),(1.,
1.),(1.,1.),(1.,1.),(1.,1.),(1.,1.),(1.,1.),(1.,1.),(1.,1.),(1.,1.),(1.,
1.),(1.,1.),(1.,1.),(1.,1.),(1.,1.),(1.,1.),(1.,1.),(1.,1.),(1.,1.),(1.,
1.),(1.,1.),(1.,1.),(1.,1.),(1.,1.),(1.,1.),(1.,1.),(1.,1.),(1.,1.),(1.,
1.),(1.,1.),(1.,1.),(1.,1.),(1.,1.),(1.,1.),(1.,1.),(1.,1.),(1.,1.),(1.,
1.),(1.,1.),(1.,1.),(1.,1.),(1.,1.),(1.,1.),(1.,1.),(1.,1.),(1.,1.),(1.,
1.),(1.,1.),(1.,1.),(1.,1.),(1.,1.),(1.,1.),(1.,1.),(1.,1.),(1.,1.),(1.,
1.),(1.,1.),(1.,1.),(1.,1.),(1.,1.),(1.,1.),(1.,1.),(1.,1.),(1.,1.),(1.,
1.),(1.,1.),(1.,1.),(1.,1.),(1.,1.),(1.,1.),(1.,1.),(1.,1.),(1.,1.),(1.,
1.),(1.,1.),(1.,1.),(1.,1.),(1.,1.),(1.,1.),(1.,1.),(1.,1.),(1.,1.),(1.,
1.),(1.,1.),(1.,1.),(1.,1.),(1.,1.),(1.,1.),(1.,1.),(1.,1.),(1.,1.),(1.,
1.),(1.,1.)))
REPRESENTATION_ITEM('')
SURFACE()
);
#952=(
BOUNDED_SURFACE()
B_SPLINE_SURFACE(5,1,((#114446,#114447),(#114448,#114449),(#114450,#114451),
(#114452,#114453),(#114454,#114455),(#114456,#114457),(#114458,#114459),
(#114460,#114461),(#114462,#114463),(#114464,#114465),(#114466,#114467),
(#114468,#114469),(#114470,#114471),(#114472,#114473),(#114474,#114475),
(#114476,#114477),(#114478,#114479),(#114480,#114481),(#114482,#114483),
(#114484,#114485),(#114486,#114487),(#114488,#114489),(#114490,#114491),
(#114492,#114493),(#114494,#114495),(#114496,#114497),(#114498,#114499),
(#114500,#114501),(#114502,#114503),(#114504,#114505),(#114506,#114507),
(#114508,#114509),(#114510,#114511),(#114512,#114513),(#114514,#114515),
(#114516,#114517),(#114518,#114519),(#114520,#114521),(#114522,#114523),
(#114524,#114525),(#114526,#114527),(#114528,#114529),(#114530,#114531),
(#114532,#114533),(#114534,#114535),(#114536,#114537),(#114538,#114539),
(#114540,#114541),(#114542,#114543),(#114544,#114545),(#114546,#114547),
(#114548,#114549),(#114550,#114551),(#114552,#114553),(#114554,#114555),
(#114556,#114557),(#114558,#114559),(#114560,#114561),(#114562,#114563),
(#114564,#114565),(#114566,#114567),(#114568,#114569),(#114570,#114571),
(#114572,#114573),(#114574,#114575),(#114576,#114577),(#114578,#114579),
(#114580,#114581),(#114582,#114583),(#114584,#114585),(#114586,#114587),
(#114588,#114589),(#114590,#114591),(#114592,#114593),(#114594,#114595),
(#114596,#114597),(#114598,#114599),(#114600,#114601),(#114602,#114603),
(#114604,#114605),(#114606,#114607),(#114608,#114609),(#114610,#114611),
(#114612,#114613),(#114614,#114615),(#114616,#114617),(#114618,#114619),
(#114620,#114621),(#114622,#114623),(#114624,#114625),(#114626,#114627),
(#114628,#114629),(#114630,#114631),(#114632,#114633),(#114634,#114635),
(#114636,#114637),(#114638,#114639),(#114640,#114641),(#114642,#114643),
(#114644,#114645),(#114646,#114647),(#114648,#114649),(#114650,#114651),
(#114652,#114653),(#114654,#114655),(#114656,#114657),(#114658,#114659),
(#114660,#114661),(#114662,#114663),(#114664,#114665),(#114666,#114667),
(#114668,#114669),(#114670,#114671),(#114672,#114673),(#114674,#114675),
(#114676,#114677),(#114678,#114679),(#114680,#114681),(#114682,#114683),
(#114684,#114685),(#114686,#114687),(#114688,#114689),(#114690,#114691),
(#114692,#114693),(#114694,#114695),(#114696,#114697),(#114698,#114699),
(#114700,#114701),(#114702,#114703),(#114704,#114705),(#114706,#114707),
(#114708,#114709),(#114710,#114711),(#114712,#114713),(#114714,#114715),
(#114716,#114717),(#114718,#114719),(#114720,#114721),(#114722,#114723),
(#114724,#114725),(#114726,#114727),(#114728,#114729),(#114730,#114731),
(#114732,#114733),(#114734,#114735),(#114736,#114737),(#114738,#114739),
(#114740,#114741),(#114742,#114743),(#114744,#114745),(#114746,#114747),
(#114748,#114749),(#114750,#114751),(#114752,#114753),(#114754,#114755),
(#114756,#114757),(#114758,#114759),(#114760,#114761),(#114762,#114763),
(#114764,#114765),(#114766,#114767),(#114768,#114769),(#114770,#114771),
(#114772,#114773),(#114774,#114775),(#114776,#114777),(#114778,#114779),
(#114780,#114781),(#114782,#114783),(#114784,#114785),(#114786,#114787),
(#114788,#114789),(#114790,#114791),(#114792,#114793),(#114794,#114795),
(#114796,#114797),(#114798,#114799),(#114800,#114801),(#114802,#114803),
(#114804,#114805),(#114806,#114807),(#114808,#114809),(#114810,#114811),
(#114812,#114813),(#114814,#114815),(#114816,#114817),(#114818,#114819),
(#114820,#114821),(#114822,#114823),(#114824,#114825),(#114826,#114827),
(#114828,#114829),(#114830,#114831),(#114832,#114833),(#114834,#114835),
(#114836,#114837),(#114838,#114839),(#114840,#114841),(#114842,#114843),
(#114844,#114845),(#114846,#114847),(#114848,#114849),(#114850,#114851),
(#114852,#114853),(#114854,#114855)),.UNSPECIFIED.,.F.,.F.,.F.)
B_SPLINE_SURFACE_WITH_KNOTS((6,1,1,1,1,1,1,1,1,1,1,1,1,1,1,1,1,1,1,1,1,
1,1,1,1,1,1,1,1,1,1,1,1,1,1,1,1,1,1,1,1,1,1,1,1,1,1,1,1,1,1,1,1,1,1,1,1,
1,1,1,1,1,1,1,1,1,1,1,1,1,1,1,1,1,1,1,1,1,1,1,1,1,1,1,1,1,1,1,1,1,1,1,1,
1,1,1,1,1,1,1,1,1,1,1,1,1,1,1,1,1,1,1,1,1,1,1,1,1,1,1,1,1,1,1,1,1,1,1,1,
1,1,1,1,1,1,1,1,1,1,1,1,1,1,1,1,1,1,1,1,1,1,1,1,1,1,1,1,1,1,1,1,1,1,1,1,
1,1,1,1,1,1,1,1,1,1,1,1,1,1,1,1,1,1,1,1,1,1,1,1,1,1,1,1,1,1,1,1,1,1,1,6),
(2,2),(0.,0.005,0.01,0.015,0.02,0.025,0.03,0.035,0.04,0.045,0.05,0.055,
0.06,0.065,0.07,0.075,0.08,0.085,0.09,0.095,0.1,0.105,0.11,0.115,0.12,0.125,
0.13,0.135,0.14,0.145,0.15,0.155,0.16,0.165,0.17,0.175,0.18,0.185,0.19,
0.195,0.2,0.205,0.21,0.215,0.22,0.225,0.23,0.235,0.24,0.245,0.25,0.255,
0.26,0.265,0.27,0.275,0.28,0.285,0.29,0.295,0.3,0.305,0.31,0.315,0.32,0.325,
0.33,0.335,0.34,0.345,0.35,0.355,0.36,0.365,0.37,0.375,0.38,0.385,0.39,
0.395,0.4,0.405,0.41,0.415,0.42,0.425,0.43,0.435,0.44,0.445,0.45,0.455,
0.46,0.465,0.47,0.475,0.48,0.485,0.49,0.495,0.5,0.505,0.51,0.515,0.52,0.525,
0.53,0.535,0.54,0.545,0.55,0.555,0.56,0.565,0.57,0.575,0.58,0.585,0.59,
0.595,0.6,0.605,0.61,0.615,0.62,0.625,0.63,0.635,0.64,0.645,0.65,0.655,
0.66,0.665,0.67,0.675,0.68,0.685,0.690000000000001,0.695000000000001,0.700000000000001,
0.705000000000001,0.710000000000001,0.715000000000001,0.720000000000001,
0.725000000000001,0.730000000000001,0.735000000000001,0.740000000000001,
0.745000000000001,0.750000000000001,0.755000000000001,0.760000000000001,
0.765000000000001,0.770000000000001,0.775000000000001,0.780000000000001,
0.785000000000001,0.790000000000001,0.795000000000001,0.800000000000001,
0.805000000000001,0.810000000000001,0.815000000000001,0.820000000000001,
0.825000000000001,0.830000000000001,0.835000000000001,0.840000000000001,
0.845000000000001,0.850000000000001,0.855000000000001,0.860000000000001,
0.865000000000001,0.870000000000001,0.875000000000001,0.880000000000001,
0.885000000000001,0.890000000000001,0.895000000000001,0.900000000000001,
0.905000000000001,0.910000000000001,0.915000000000001,0.920000000000001,
0.925000000000001,0.930000000000001,0.935000000000001,0.940000000000001,
0.945000000000001,0.950000000000001,0.955000000000001,0.960000000000001,
0.965000000000001,0.970000000000001,0.975000000000001,0.980000000000001,
0.985000000000001,0.990000000000001,0.995000000000001,1.),(0.,1.2),
 .UNSPECIFIED.)
GEOMETRIC_REPRESENTATION_ITEM()
RATIONAL_B_SPLINE_SURFACE(((1.,1.),(1.,1.),(1.,1.),(1.,1.),(1.,1.),(1.,
1.),(1.,1.),(1.,1.),(1.,1.),(1.,1.),(1.,1.),(1.,1.),(1.,1.),(1.,1.),(1.,
1.),(1.,1.),(1.,1.),(1.,1.),(1.,1.),(1.,1.),(1.,1.),(1.,1.),(1.,1.),(1.,
1.),(1.,1.),(1.,1.),(1.,1.),(1.,1.),(1.,1.),(1.,1.),(1.,1.),(1.,1.),(1.,
1.),(1.,1.),(1.,1.),(1.,1.),(1.,1.),(1.,1.),(1.,1.),(1.,1.),(1.,1.),(1.,
1.),(1.,1.),(1.,1.),(1.,1.),(1.,1.),(1.,1.),(1.,1.),(1.,1.),(1.,1.),(1.,
1.),(1.,1.),(1.,1.),(1.,1.),(1.,1.),(1.,1.),(1.,1.),(1.,1.),(1.,1.),(1.,
1.),(1.,1.),(1.,1.),(1.,1.),(1.,1.),(1.,1.),(1.,1.),(1.,1.),(1.,1.),(1.,
1.),(1.,1.),(1.,1.),(1.,1.),(1.,1.),(1.,1.),(1.,1.),(1.,1.),(1.,1.),(1.,
1.),(1.,1.),(1.,1.),(1.,1.),(1.,1.),(1.,1.),(1.,1.),(1.,1.),(1.,1.),(1.,
1.),(1.,1.),(1.,1.),(1.,1.),(1.,1.),(1.,1.),(1.,1.),(1.,1.),(1.,1.),(1.,
1.),(1.,1.),(1.,1.),(1.,1.),(1.,1.),(1.,1.),(1.,1.),(1.,1.),(1.,1.),(1.,
1.),(1.,1.),(1.,1.),(1.,1.),(1.,1.),(1.,1.),(1.,1.),(1.,1.),(1.,1.),(1.,
1.),(1.,1.),(1.,1.),(1.,1.),(1.,1.),(1.,1.),(1.,1.),(1.,1.),(1.,1.),(1.,
1.),(1.,1.),(1.,1.),(1.,1.),(1.,1.),(1.,1.),(1.,1.),(1.,1.),(1.,1.),(1.,
1.),(1.,1.),(1.,1.),(1.,1.),(1.,1.),(1.,1.),(1.,1.),(1.,1.),(1.,1.),(1.,
1.),(1.,1.),(1.,1.),(1.,1.),(1.,1.),(1.,1.),(1.,1.),(1.,1.),(1.,1.),(1.,
1.),(1.,1.),(1.,1.),(1.,1.),(1.,1.),(1.,1.),(1.,1.),(1.,1.),(1.,1.),(1.,
1.),(1.,1.),(1.,1.),(1.,1.),(1.,1.),(1.,1.),(1.,1.),(1.,1.),(1.,1.),(1.,
1.),(1.,1.),(1.,1.),(1.,1.),(1.,1.),(1.,1.),(1.,1.),(1.,1.),(1.,1.),(1.,
1.),(1.,1.),(1.,1.),(1.,1.),(1.,1.),(1.,1.),(1.,1.),(1.,1.),(1.,1.),(1.,
1.),(1.,1.),(1.,1.),(1.,1.),(1.,1.),(1.,1.),(1.,1.),(1.,1.),(1.,1.),(1.,
1.),(1.,1.),(1.,1.),(1.,1.),(1.,1.),(1.,1.),(1.,1.),(1.,1.),(1.,1.),(1.,
1.),(1.,1.)))
REPRESENTATION_ITEM('')
SURFACE()
);
#953=(
BOUNDED_SURFACE()
B_SPLINE_SURFACE(5,1,((#115342,#115343),(#115344,#115345),(#115346,#115347),
(#115348,#115349),(#115350,#115351),(#115352,#115353),(#115354,#115355),
(#115356,#115357),(#115358,#115359),(#115360,#115361),(#115362,#115363),
(#115364,#115365),(#115366,#115367),(#115368,#115369),(#115370,#115371),
(#115372,#115373),(#115374,#115375),(#115376,#115377),(#115378,#115379),
(#115380,#115381),(#115382,#115383),(#115384,#115385),(#115386,#115387),
(#115388,#115389),(#115390,#115391),(#115392,#115393),(#115394,#115395),
(#115396,#115397),(#115398,#115399),(#115400,#115401),(#115402,#115403),
(#115404,#115405),(#115406,#115407),(#115408,#115409),(#115410,#115411),
(#115412,#115413),(#115414,#115415),(#115416,#115417),(#115418,#115419),
(#115420,#115421),(#115422,#115423),(#115424,#115425),(#115426,#115427),
(#115428,#115429),(#115430,#115431),(#115432,#115433),(#115434,#115435),
(#115436,#115437),(#115438,#115439),(#115440,#115441),(#115442,#115443),
(#115444,#115445),(#115446,#115447),(#115448,#115449),(#115450,#115451),
(#115452,#115453),(#115454,#115455),(#115456,#115457),(#115458,#115459),
(#115460,#115461),(#115462,#115463),(#115464,#115465),(#115466,#115467),
(#115468,#115469),(#115470,#115471),(#115472,#115473),(#115474,#115475),
(#115476,#115477),(#115478,#115479),(#115480,#115481),(#115482,#115483),
(#115484,#115485),(#115486,#115487),(#115488,#115489),(#115490,#115491),
(#115492,#115493),(#115494,#115495),(#115496,#115497),(#115498,#115499),
(#115500,#115501),(#115502,#115503),(#115504,#115505),(#115506,#115507),
(#115508,#115509),(#115510,#115511),(#115512,#115513),(#115514,#115515),
(#115516,#115517),(#115518,#115519),(#115520,#115521),(#115522,#115523),
(#115524,#115525),(#115526,#115527),(#115528,#115529),(#115530,#115531),
(#115532,#115533),(#115534,#115535),(#115536,#115537),(#115538,#115539),
(#115540,#115541),(#115542,#115543),(#115544,#115545),(#115546,#115547),
(#115548,#115549),(#115550,#115551),(#115552,#115553),(#115554,#115555),
(#115556,#115557),(#115558,#115559),(#115560,#115561),(#115562,#115563),
(#115564,#115565),(#115566,#115567),(#115568,#115569),(#115570,#115571),
(#115572,#115573),(#115574,#115575),(#115576,#115577),(#115578,#115579),
(#115580,#115581),(#115582,#115583),(#115584,#115585),(#115586,#115587),
(#115588,#115589),(#115590,#115591),(#115592,#115593),(#115594,#115595),
(#115596,#115597),(#115598,#115599),(#115600,#115601),(#115602,#115603),
(#115604,#115605),(#115606,#115607),(#115608,#115609),(#115610,#115611),
(#115612,#115613),(#115614,#115615),(#115616,#115617),(#115618,#115619),
(#115620,#115621),(#115622,#115623),(#115624,#115625),(#115626,#115627),
(#115628,#115629),(#115630,#115631),(#115632,#115633),(#115634,#115635),
(#115636,#115637),(#115638,#115639),(#115640,#115641),(#115642,#115643),
(#115644,#115645),(#115646,#115647),(#115648,#115649),(#115650,#115651),
(#115652,#115653),(#115654,#115655),(#115656,#115657),(#115658,#115659),
(#115660,#115661),(#115662,#115663),(#115664,#115665),(#115666,#115667),
(#115668,#115669),(#115670,#115671),(#115672,#115673),(#115674,#115675),
(#115676,#115677),(#115678,#115679),(#115680,#115681),(#115682,#115683),
(#115684,#115685),(#115686,#115687),(#115688,#115689),(#115690,#115691),
(#115692,#115693),(#115694,#115695),(#115696,#115697),(#115698,#115699),
(#115700,#115701),(#115702,#115703),(#115704,#115705),(#115706,#115707),
(#115708,#115709),(#115710,#115711),(#115712,#115713),(#115714,#115715),
(#115716,#115717),(#115718,#115719),(#115720,#115721),(#115722,#115723),
(#115724,#115725),(#115726,#115727),(#115728,#115729),(#115730,#115731),
(#115732,#115733),(#115734,#115735),(#115736,#115737),(#115738,#115739),
(#115740,#115741),(#115742,#115743),(#115744,#115745),(#115746,#115747),
(#115748,#115749),(#115750,#115751)),.UNSPECIFIED.,.F.,.F.,.F.)
B_SPLINE_SURFACE_WITH_KNOTS((6,1,1,1,1,1,1,1,1,1,1,1,1,1,1,1,1,1,1,1,1,
1,1,1,1,1,1,1,1,1,1,1,1,1,1,1,1,1,1,1,1,1,1,1,1,1,1,1,1,1,1,1,1,1,1,1,1,
1,1,1,1,1,1,1,1,1,1,1,1,1,1,1,1,1,1,1,1,1,1,1,1,1,1,1,1,1,1,1,1,1,1,1,1,
1,1,1,1,1,1,1,1,1,1,1,1,1,1,1,1,1,1,1,1,1,1,1,1,1,1,1,1,1,1,1,1,1,1,1,1,
1,1,1,1,1,1,1,1,1,1,1,1,1,1,1,1,1,1,1,1,1,1,1,1,1,1,1,1,1,1,1,1,1,1,1,1,
1,1,1,1,1,1,1,1,1,1,1,1,1,1,1,1,1,1,1,1,1,1,1,1,1,1,1,1,1,1,1,1,1,1,1,6),
(2,2),(0.,0.005,0.01,0.015,0.02,0.025,0.03,0.035,0.04,0.045,0.05,0.055,
0.06,0.065,0.07,0.075,0.08,0.085,0.09,0.095,0.1,0.105,0.11,0.115,0.12,0.125,
0.13,0.135,0.14,0.145,0.15,0.155,0.16,0.165,0.17,0.175,0.18,0.185,0.19,
0.195,0.2,0.205,0.21,0.215,0.22,0.225,0.23,0.235,0.24,0.245,0.25,0.255,
0.26,0.265,0.27,0.275,0.28,0.285,0.29,0.295,0.3,0.305,0.31,0.315,0.32,0.325,
0.33,0.335,0.34,0.345,0.35,0.355,0.36,0.365,0.37,0.375,0.38,0.385,0.39,
0.395,0.4,0.405,0.41,0.415,0.42,0.425,0.43,0.435,0.44,0.445,0.45,0.455,
0.46,0.465,0.47,0.475,0.48,0.485,0.49,0.495,0.5,0.505,0.51,0.515,0.52,0.525,
0.53,0.535,0.54,0.545,0.55,0.555,0.56,0.565,0.57,0.575,0.58,0.585,0.59,
0.595,0.6,0.605,0.61,0.615,0.62,0.625,0.63,0.635,0.64,0.645,0.65,0.655,
0.66,0.665,0.67,0.675,0.68,0.685,0.690000000000001,0.695000000000001,0.700000000000001,
0.705000000000001,0.710000000000001,0.715000000000001,0.720000000000001,
0.725000000000001,0.730000000000001,0.735000000000001,0.740000000000001,
0.745000000000001,0.750000000000001,0.755000000000001,0.760000000000001,
0.765000000000001,0.770000000000001,0.775000000000001,0.780000000000001,
0.785000000000001,0.790000000000001,0.795000000000001,0.800000000000001,
0.805000000000001,0.810000000000001,0.815000000000001,0.820000000000001,
0.825000000000001,0.830000000000001,0.835000000000001,0.840000000000001,
0.845000000000001,0.850000000000001,0.855000000000001,0.860000000000001,
0.865000000000001,0.870000000000001,0.875000000000001,0.880000000000001,
0.885000000000001,0.890000000000001,0.895000000000001,0.900000000000001,
0.905000000000001,0.910000000000001,0.915000000000001,0.920000000000001,
0.925000000000001,0.930000000000001,0.935000000000001,0.940000000000001,
0.945000000000001,0.950000000000001,0.955000000000001,0.960000000000001,
0.965000000000001,0.970000000000001,0.975000000000001,0.980000000000001,
0.985000000000001,0.990000000000001,0.995000000000001,1.),(0.,1.2),
 .UNSPECIFIED.)
GEOMETRIC_REPRESENTATION_ITEM()
RATIONAL_B_SPLINE_SURFACE(((1.,1.),(1.,1.),(1.,1.),(1.,1.),(1.,1.),(1.,
1.),(1.,1.),(1.,1.),(1.,1.),(1.,1.),(1.,1.),(1.,1.),(1.,1.),(1.,1.),(1.,
1.),(1.,1.),(1.,1.),(1.,1.),(1.,1.),(1.,1.),(1.,1.),(1.,1.),(1.,1.),(1.,
1.),(1.,1.),(1.,1.),(1.,1.),(1.,1.),(1.,1.),(1.,1.),(1.,1.),(1.,1.),(1.,
1.),(1.,1.),(1.,1.),(1.,1.),(1.,1.),(1.,1.),(1.,1.),(1.,1.),(1.,1.),(1.,
1.),(1.,1.),(1.,1.),(1.,1.),(1.,1.),(1.,1.),(1.,1.),(1.,1.),(1.,1.),(1.,
1.),(1.,1.),(1.,1.),(1.,1.),(1.,1.),(1.,1.),(1.,1.),(1.,1.),(1.,1.),(1.,
1.),(1.,1.),(1.,1.),(1.,1.),(1.,1.),(1.,1.),(1.,1.),(1.,1.),(1.,1.),(1.,
1.),(1.,1.),(1.,1.),(1.,1.),(1.,1.),(1.,1.),(1.,1.),(1.,1.),(1.,1.),(1.,
1.),(1.,1.),(1.,1.),(1.,1.),(1.,1.),(1.,1.),(1.,1.),(1.,1.),(1.,1.),(1.,
1.),(1.,1.),(1.,1.),(1.,1.),(1.,1.),(1.,1.),(1.,1.),(1.,1.),(1.,1.),(1.,
1.),(1.,1.),(1.,1.),(1.,1.),(1.,1.),(1.,1.),(1.,1.),(1.,1.),(1.,1.),(1.,
1.),(1.,1.),(1.,1.),(1.,1.),(1.,1.),(1.,1.),(1.,1.),(1.,1.),(1.,1.),(1.,
1.),(1.,1.),(1.,1.),(1.,1.),(1.,1.),(1.,1.),(1.,1.),(1.,1.),(1.,1.),(1.,
1.),(1.,1.),(1.,1.),(1.,1.),(1.,1.),(1.,1.),(1.,1.),(1.,1.),(1.,1.),(1.,
1.),(1.,1.),(1.,1.),(1.,1.),(1.,1.),(1.,1.),(1.,1.),(1.,1.),(1.,1.),(1.,
1.),(1.,1.),(1.,1.),(1.,1.),(1.,1.),(1.,1.),(1.,1.),(1.,1.),(1.,1.),(1.,
1.),(1.,1.),(1.,1.),(1.,1.),(1.,1.),(1.,1.),(1.,1.),(1.,1.),(1.,1.),(1.,
1.),(1.,1.),(1.,1.),(1.,1.),(1.,1.),(1.,1.),(1.,1.),(1.,1.),(1.,1.),(1.,
1.),(1.,1.),(1.,1.),(1.,1.),(1.,1.),(1.,1.),(1.,1.),(1.,1.),(1.,1.),(1.,
1.),(1.,1.),(1.,1.),(1.,1.),(1.,1.),(1.,1.),(1.,1.),(1.,1.),(1.,1.),(1.,
1.),(1.,1.),(1.,1.),(1.,1.),(1.,1.),(1.,1.),(1.,1.),(1.,1.),(1.,1.),(1.,
1.),(1.,1.),(1.,1.),(1.,1.),(1.,1.),(1.,1.),(1.,1.),(1.,1.),(1.,1.),(1.,
1.),(1.,1.)))
REPRESENTATION_ITEM('')
SURFACE()
);
#954=(
BOUNDED_SURFACE()
B_SPLINE_SURFACE(5,1,((#116192,#116193),(#116194,#116195),(#116196,#116197),
(#116198,#116199),(#116200,#116201),(#116202,#116203),(#116204,#116205),
(#116206,#116207),(#116208,#116209),(#116210,#116211),(#116212,#116213),
(#116214,#116215),(#116216,#116217),(#116218,#116219),(#116220,#116221),
(#116222,#116223),(#116224,#116225),(#116226,#116227),(#116228,#116229),
(#116230,#116231),(#116232,#116233),(#116234,#116235),(#116236,#116237),
(#116238,#116239),(#116240,#116241),(#116242,#116243),(#116244,#116245),
(#116246,#116247),(#116248,#116249),(#116250,#116251),(#116252,#116253),
(#116254,#116255),(#116256,#116257),(#116258,#116259),(#116260,#116261),
(#116262,#116263),(#116264,#116265),(#116266,#116267),(#116268,#116269),
(#116270,#116271),(#116272,#116273),(#116274,#116275),(#116276,#116277),
(#116278,#116279),(#116280,#116281),(#116282,#116283),(#116284,#116285),
(#116286,#116287),(#116288,#116289),(#116290,#116291),(#116292,#116293),
(#116294,#116295),(#116296,#116297),(#116298,#116299),(#116300,#116301),
(#116302,#116303),(#116304,#116305),(#116306,#116307),(#116308,#116309),
(#116310,#116311),(#116312,#116313),(#116314,#116315),(#116316,#116317),
(#116318,#116319),(#116320,#116321),(#116322,#116323),(#116324,#116325),
(#116326,#116327),(#116328,#116329),(#116330,#116331),(#116332,#116333),
(#116334,#116335),(#116336,#116337),(#116338,#116339),(#116340,#116341),
(#116342,#116343),(#116344,#116345),(#116346,#116347),(#116348,#116349),
(#116350,#116351),(#116352,#116353),(#116354,#116355),(#116356,#116357),
(#116358,#116359),(#116360,#116361),(#116362,#116363),(#116364,#116365),
(#116366,#116367),(#116368,#116369),(#116370,#116371),(#116372,#116373),
(#116374,#116375),(#116376,#116377),(#116378,#116379),(#116380,#116381),
(#116382,#116383),(#116384,#116385),(#116386,#116387),(#116388,#116389),
(#116390,#116391),(#116392,#116393),(#116394,#116395),(#116396,#116397),
(#116398,#116399),(#116400,#116401),(#116402,#116403),(#116404,#116405),
(#116406,#116407),(#116408,#116409),(#116410,#116411),(#116412,#116413),
(#116414,#116415),(#116416,#116417),(#116418,#116419),(#116420,#116421),
(#116422,#116423),(#116424,#116425),(#116426,#116427),(#116428,#116429),
(#116430,#116431),(#116432,#116433),(#116434,#116435),(#116436,#116437),
(#116438,#116439),(#116440,#116441),(#116442,#116443),(#116444,#116445),
(#116446,#116447),(#116448,#116449),(#116450,#116451),(#116452,#116453),
(#116454,#116455),(#116456,#116457),(#116458,#116459),(#116460,#116461),
(#116462,#116463),(#116464,#116465),(#116466,#116467),(#116468,#116469),
(#116470,#116471),(#116472,#116473),(#116474,#116475),(#116476,#116477),
(#116478,#116479),(#116480,#116481),(#116482,#116483),(#116484,#116485),
(#116486,#116487),(#116488,#116489),(#116490,#116491),(#116492,#116493),
(#116494,#116495),(#116496,#116497),(#116498,#116499),(#116500,#116501),
(#116502,#116503),(#116504,#116505),(#116506,#116507),(#116508,#116509),
(#116510,#116511),(#116512,#116513),(#116514,#116515),(#116516,#116517),
(#116518,#116519),(#116520,#116521),(#116522,#116523),(#116524,#116525),
(#116526,#116527),(#116528,#116529),(#116530,#116531),(#116532,#116533),
(#116534,#116535),(#116536,#116537),(#116538,#116539),(#116540,#116541),
(#116542,#116543),(#116544,#116545),(#116546,#116547),(#116548,#116549),
(#116550,#116551),(#116552,#116553),(#116554,#116555),(#116556,#116557),
(#116558,#116559),(#116560,#116561),(#116562,#116563),(#116564,#116565),
(#116566,#116567),(#116568,#116569),(#116570,#116571),(#116572,#116573),
(#116574,#116575),(#116576,#116577),(#116578,#116579),(#116580,#116581),
(#116582,#116583),(#116584,#116585),(#116586,#116587),(#116588,#116589),
(#116590,#116591),(#116592,#116593),(#116594,#116595),(#116596,#116597),
(#116598,#116599),(#116600,#116601)),.UNSPECIFIED.,.F.,.F.,.F.)
B_SPLINE_SURFACE_WITH_KNOTS((6,1,1,1,1,1,1,1,1,1,1,1,1,1,1,1,1,1,1,1,1,
1,1,1,1,1,1,1,1,1,1,1,1,1,1,1,1,1,1,1,1,1,1,1,1,1,1,1,1,1,1,1,1,1,1,1,1,
1,1,1,1,1,1,1,1,1,1,1,1,1,1,1,1,1,1,1,1,1,1,1,1,1,1,1,1,1,1,1,1,1,1,1,1,
1,1,1,1,1,1,1,1,1,1,1,1,1,1,1,1,1,1,1,1,1,1,1,1,1,1,1,1,1,1,1,1,1,1,1,1,
1,1,1,1,1,1,1,1,1,1,1,1,1,1,1,1,1,1,1,1,1,1,1,1,1,1,1,1,1,1,1,1,1,1,1,1,
1,1,1,1,1,1,1,1,1,1,1,1,1,1,1,1,1,1,1,1,1,1,1,1,1,1,1,1,1,1,1,1,1,1,1,6),
(2,2),(-1.,-0.995000000000001,-0.990000000000001,-0.985000000000001,-0.980000000000001,
-0.975000000000001,-0.970000000000001,-0.965000000000001,-0.960000000000001,
-0.955000000000001,-0.950000000000001,-0.945000000000001,-0.940000000000001,
-0.935000000000001,-0.930000000000001,-0.925000000000001,-0.920000000000001,
-0.915000000000001,-0.910000000000001,-0.905000000000001,-0.900000000000001,
-0.895000000000001,-0.890000000000001,-0.885000000000001,-0.880000000000001,
-0.875000000000001,-0.870000000000001,-0.865000000000001,-0.860000000000001,
-0.855000000000001,-0.850000000000001,-0.845000000000001,-0.840000000000001,
-0.835000000000001,-0.830000000000001,-0.825000000000001,-0.820000000000001,
-0.815000000000001,-0.810000000000001,-0.805000000000001,-0.800000000000001,
-0.795000000000001,-0.790000000000001,-0.785000000000001,-0.780000000000001,
-0.775000000000001,-0.770000000000001,-0.765000000000001,-0.760000000000001,
-0.755000000000001,-0.750000000000001,-0.745000000000001,-0.740000000000001,
-0.735000000000001,-0.730000000000001,-0.725000000000001,-0.720000000000001,
-0.715000000000001,-0.710000000000001,-0.705000000000001,-0.700000000000001,
-0.695000000000001,-0.690000000000001,-0.685,-0.68,-0.675,-0.67,-0.665,
-0.66,-0.655,-0.65,-0.645,-0.64,-0.635,-0.63,-0.625,-0.62,-0.615,-0.61,
-0.605,-0.6,-0.595,-0.59,-0.585,-0.58,-0.575,-0.57,-0.565,-0.56,-0.555,
-0.55,-0.545,-0.54,-0.535,-0.53,-0.525,-0.52,-0.515,-0.51,-0.505,-0.5,-0.495,
-0.49,-0.485,-0.48,-0.475,-0.47,-0.465,-0.46,-0.455,-0.45,-0.445,-0.44,
-0.435,-0.43,-0.425,-0.42,-0.415,-0.41,-0.405,-0.4,-0.395,-0.39,-0.385,
-0.38,-0.375,-0.37,-0.365,-0.36,-0.355,-0.35,-0.345,-0.34,-0.335,-0.33,
-0.325,-0.32,-0.315,-0.31,-0.305,-0.3,-0.295,-0.29,-0.285,-0.28,-0.275,
-0.27,-0.265,-0.26,-0.255,-0.25,-0.245,-0.24,-0.235,-0.23,-0.225,-0.22,
-0.215,-0.21,-0.205,-0.2,-0.195,-0.19,-0.185,-0.18,-0.175,-0.17,-0.165,
-0.16,-0.155,-0.15,-0.145,-0.14,-0.135,-0.13,-0.125,-0.12,-0.115,-0.11,
-0.105,-0.1,-0.095,-0.09,-0.085,-0.08,-0.075,-0.07,-0.065,-0.06,-0.055,
-0.05,-0.045,-0.04,-0.035,-0.03,-0.025,-0.02,-0.015,-0.01,-0.005,0.),(0.,
1.2),.UNSPECIFIED.)
GEOMETRIC_REPRESENTATION_ITEM()
RATIONAL_B_SPLINE_SURFACE(((1.,1.),(1.,1.),(1.,1.),(1.,1.),(1.,1.),(1.,
1.),(1.,1.),(1.,1.),(1.,1.),(1.,1.),(1.,1.),(1.,1.),(1.,1.),(1.,1.),(1.,
1.),(1.,1.),(1.,1.),(1.,1.),(1.,1.),(1.,1.),(1.,1.),(1.,1.),(1.,1.),(1.,
1.),(1.,1.),(1.,1.),(1.,1.),(1.,1.),(1.,1.),(1.,1.),(1.,1.),(1.,1.),(1.,
1.),(1.,1.),(1.,1.),(1.,1.),(1.,1.),(1.,1.),(1.,1.),(1.,1.),(1.,1.),(1.,
1.),(1.,1.),(1.,1.),(1.,1.),(1.,1.),(1.,1.),(1.,1.),(1.,1.),(1.,1.),(1.,
1.),(1.,1.),(1.,1.),(1.,1.),(1.,1.),(1.,1.),(1.,1.),(1.,1.),(1.,1.),(1.,
1.),(1.,1.),(1.,1.),(1.,1.),(1.,1.),(1.,1.),(1.,1.),(1.,1.),(1.,1.),(1.,
1.),(1.,1.),(1.,1.),(1.,1.),(1.,1.),(1.,1.),(1.,1.),(1.,1.),(1.,1.),(1.,
1.),(1.,1.),(1.,1.),(1.,1.),(1.,1.),(1.,1.),(1.,1.),(1.,1.),(1.,1.),(1.,
1.),(1.,1.),(1.,1.),(1.,1.),(1.,1.),(1.,1.),(1.,1.),(1.,1.),(1.,1.),(1.,
1.),(1.,1.),(1.,1.),(1.,1.),(1.,1.),(1.,1.),(1.,1.),(1.,1.),(1.,1.),(1.,
1.),(1.,1.),(1.,1.),(1.,1.),(1.,1.),(1.,1.),(1.,1.),(1.,1.),(1.,1.),(1.,
1.),(1.,1.),(1.,1.),(1.,1.),(1.,1.),(1.,1.),(1.,1.),(1.,1.),(1.,1.),(1.,
1.),(1.,1.),(1.,1.),(1.,1.),(1.,1.),(1.,1.),(1.,1.),(1.,1.),(1.,1.),(1.,
1.),(1.,1.),(1.,1.),(1.,1.),(1.,1.),(1.,1.),(1.,1.),(1.,1.),(1.,1.),(1.,
1.),(1.,1.),(1.,1.),(1.,1.),(1.,1.),(1.,1.),(1.,1.),(1.,1.),(1.,1.),(1.,
1.),(1.,1.),(1.,1.),(1.,1.),(1.,1.),(1.,1.),(1.,1.),(1.,1.),(1.,1.),(1.,
1.),(1.,1.),(1.,1.),(1.,1.),(1.,1.),(1.,1.),(1.,1.),(1.,1.),(1.,1.),(1.,
1.),(1.,1.),(1.,1.),(1.,1.),(1.,1.),(1.,1.),(1.,1.),(1.,1.),(1.,1.),(1.,
1.),(1.,1.),(1.,1.),(1.,1.),(1.,1.),(1.,1.),(1.,1.),(1.,1.),(1.,1.),(1.,
1.),(1.,1.),(1.,1.),(1.,1.),(1.,1.),(1.,1.),(1.,1.),(1.,1.),(1.,1.),(1.,
1.),(1.,1.),(1.,1.),(1.,1.),(1.,1.),(1.,1.),(1.,1.),(1.,1.),(1.,1.),(1.,
1.),(1.,1.)))
REPRESENTATION_ITEM('')
SURFACE()
);
#955=(
BOUNDED_SURFACE()
B_SPLINE_SURFACE(5,1,((#116993,#116994),(#116995,#116996),(#116997,#116998),
(#116999,#117000),(#117001,#117002),(#117003,#117004),(#117005,#117006),
(#117007,#117008),(#117009,#117010),(#117011,#117012),(#117013,#117014),
(#117015,#117016),(#117017,#117018),(#117019,#117020),(#117021,#117022),
(#117023,#117024),(#117025,#117026),(#117027,#117028),(#117029,#117030),
(#117031,#117032),(#117033,#117034),(#117035,#117036),(#117037,#117038),
(#117039,#117040),(#117041,#117042),(#117043,#117044),(#117045,#117046),
(#117047,#117048),(#117049,#117050),(#117051,#117052),(#117053,#117054),
(#117055,#117056),(#117057,#117058),(#117059,#117060),(#117061,#117062),
(#117063,#117064),(#117065,#117066),(#117067,#117068),(#117069,#117070),
(#117071,#117072),(#117073,#117074),(#117075,#117076),(#117077,#117078),
(#117079,#117080),(#117081,#117082),(#117083,#117084),(#117085,#117086),
(#117087,#117088),(#117089,#117090),(#117091,#117092),(#117093,#117094),
(#117095,#117096),(#117097,#117098),(#117099,#117100),(#117101,#117102),
(#117103,#117104),(#117105,#117106),(#117107,#117108),(#117109,#117110),
(#117111,#117112),(#117113,#117114),(#117115,#117116),(#117117,#117118),
(#117119,#117120),(#117121,#117122),(#117123,#117124),(#117125,#117126),
(#117127,#117128),(#117129,#117130),(#117131,#117132),(#117133,#117134),
(#117135,#117136),(#117137,#117138),(#117139,#117140),(#117141,#117142),
(#117143,#117144),(#117145,#117146),(#117147,#117148),(#117149,#117150),
(#117151,#117152),(#117153,#117154),(#117155,#117156),(#117157,#117158),
(#117159,#117160),(#117161,#117162),(#117163,#117164),(#117165,#117166),
(#117167,#117168),(#117169,#117170),(#117171,#117172),(#117173,#117174),
(#117175,#117176),(#117177,#117178),(#117179,#117180),(#117181,#117182),
(#117183,#117184),(#117185,#117186),(#117187,#117188),(#117189,#117190),
(#117191,#117192),(#117193,#117194),(#117195,#117196),(#117197,#117198),
(#117199,#117200),(#117201,#117202),(#117203,#117204),(#117205,#117206),
(#117207,#117208),(#117209,#117210),(#117211,#117212),(#117213,#117214),
(#117215,#117216),(#117217,#117218),(#117219,#117220),(#117221,#117222),
(#117223,#117224),(#117225,#117226),(#117227,#117228),(#117229,#117230),
(#117231,#117232),(#117233,#117234),(#117235,#117236),(#117237,#117238),
(#117239,#117240),(#117241,#117242),(#117243,#117244),(#117245,#117246),
(#117247,#117248),(#117249,#117250),(#117251,#117252),(#117253,#117254),
(#117255,#117256),(#117257,#117258),(#117259,#117260),(#117261,#117262),
(#117263,#117264),(#117265,#117266),(#117267,#117268),(#117269,#117270),
(#117271,#117272),(#117273,#117274),(#117275,#117276),(#117277,#117278),
(#117279,#117280),(#117281,#117282),(#117283,#117284),(#117285,#117286),
(#117287,#117288),(#117289,#117290),(#117291,#117292),(#117293,#117294),
(#117295,#117296),(#117297,#117298),(#117299,#117300),(#117301,#117302),
(#117303,#117304),(#117305,#117306),(#117307,#117308),(#117309,#117310),
(#117311,#117312),(#117313,#117314),(#117315,#117316),(#117317,#117318),
(#117319,#117320),(#117321,#117322),(#117323,#117324),(#117325,#117326),
(#117327,#117328),(#117329,#117330),(#117331,#117332),(#117333,#117334),
(#117335,#117336),(#117337,#117338),(#117339,#117340),(#117341,#117342),
(#117343,#117344),(#117345,#117346),(#117347,#117348),(#117349,#117350),
(#117351,#117352),(#117353,#117354),(#117355,#117356),(#117357,#117358),
(#117359,#117360),(#117361,#117362),(#117363,#117364),(#117365,#117366),
(#117367,#117368),(#117369,#117370),(#117371,#117372),(#117373,#117374),
(#117375,#117376),(#117377,#117378),(#117379,#117380),(#117381,#117382),
(#117383,#117384),(#117385,#117386),(#117387,#117388),(#117389,#117390),
(#117391,#117392),(#117393,#117394),(#117395,#117396),(#117397,#117398),
(#117399,#117400),(#117401,#117402)),.UNSPECIFIED.,.F.,.F.,.F.)
B_SPLINE_SURFACE_WITH_KNOTS((6,1,1,1,1,1,1,1,1,1,1,1,1,1,1,1,1,1,1,1,1,
1,1,1,1,1,1,1,1,1,1,1,1,1,1,1,1,1,1,1,1,1,1,1,1,1,1,1,1,1,1,1,1,1,1,1,1,
1,1,1,1,1,1,1,1,1,1,1,1,1,1,1,1,1,1,1,1,1,1,1,1,1,1,1,1,1,1,1,1,1,1,1,1,
1,1,1,1,1,1,1,1,1,1,1,1,1,1,1,1,1,1,1,1,1,1,1,1,1,1,1,1,1,1,1,1,1,1,1,1,
1,1,1,1,1,1,1,1,1,1,1,1,1,1,1,1,1,1,1,1,1,1,1,1,1,1,1,1,1,1,1,1,1,1,1,1,
1,1,1,1,1,1,1,1,1,1,1,1,1,1,1,1,1,1,1,1,1,1,1,1,1,1,1,1,1,1,1,1,1,1,1,6),
(2,2),(-1.,-0.995000000000001,-0.990000000000001,-0.985000000000001,-0.980000000000001,
-0.975000000000001,-0.970000000000001,-0.965000000000001,-0.960000000000001,
-0.955000000000001,-0.950000000000001,-0.945000000000001,-0.940000000000001,
-0.935000000000001,-0.930000000000001,-0.925000000000001,-0.920000000000001,
-0.915000000000001,-0.910000000000001,-0.905000000000001,-0.900000000000001,
-0.895000000000001,-0.890000000000001,-0.885000000000001,-0.880000000000001,
-0.875000000000001,-0.870000000000001,-0.865000000000001,-0.860000000000001,
-0.855000000000001,-0.850000000000001,-0.845000000000001,-0.840000000000001,
-0.835000000000001,-0.830000000000001,-0.825000000000001,-0.820000000000001,
-0.815000000000001,-0.810000000000001,-0.805000000000001,-0.800000000000001,
-0.795000000000001,-0.790000000000001,-0.785000000000001,-0.780000000000001,
-0.775000000000001,-0.770000000000001,-0.765000000000001,-0.760000000000001,
-0.755000000000001,-0.750000000000001,-0.745000000000001,-0.740000000000001,
-0.735000000000001,-0.730000000000001,-0.725000000000001,-0.720000000000001,
-0.715000000000001,-0.710000000000001,-0.705000000000001,-0.700000000000001,
-0.695000000000001,-0.690000000000001,-0.685,-0.68,-0.675,-0.67,-0.665,
-0.66,-0.655,-0.65,-0.645,-0.64,-0.635,-0.63,-0.625,-0.62,-0.615,-0.61,
-0.605,-0.6,-0.595,-0.59,-0.585,-0.58,-0.575,-0.57,-0.565,-0.56,-0.555,
-0.55,-0.545,-0.54,-0.535,-0.53,-0.525,-0.52,-0.515,-0.51,-0.505,-0.5,-0.495,
-0.49,-0.485,-0.48,-0.475,-0.47,-0.465,-0.46,-0.455,-0.45,-0.445,-0.44,
-0.435,-0.43,-0.425,-0.42,-0.415,-0.41,-0.405,-0.4,-0.395,-0.39,-0.385,
-0.38,-0.375,-0.37,-0.365,-0.36,-0.355,-0.35,-0.345,-0.34,-0.335,-0.33,
-0.325,-0.32,-0.315,-0.31,-0.305,-0.3,-0.295,-0.29,-0.285,-0.28,-0.275,
-0.27,-0.265,-0.26,-0.255,-0.25,-0.245,-0.24,-0.235,-0.23,-0.225,-0.22,
-0.215,-0.21,-0.205,-0.2,-0.195,-0.19,-0.185,-0.18,-0.175,-0.17,-0.165,
-0.16,-0.155,-0.15,-0.145,-0.14,-0.135,-0.13,-0.125,-0.12,-0.115,-0.11,
-0.105,-0.1,-0.095,-0.09,-0.085,-0.08,-0.075,-0.07,-0.065,-0.06,-0.055,
-0.05,-0.045,-0.04,-0.035,-0.03,-0.025,-0.02,-0.015,-0.01,-0.005,0.),(0.,
1.2),.UNSPECIFIED.)
GEOMETRIC_REPRESENTATION_ITEM()
RATIONAL_B_SPLINE_SURFACE(((1.,1.),(1.,1.),(1.,1.),(1.,1.),(1.,1.),(1.,
1.),(1.,1.),(1.,1.),(1.,1.),(1.,1.),(1.,1.),(1.,1.),(1.,1.),(1.,1.),(1.,
1.),(1.,1.),(1.,1.),(1.,1.),(1.,1.),(1.,1.),(1.,1.),(1.,1.),(1.,1.),(1.,
1.),(1.,1.),(1.,1.),(1.,1.),(1.,1.),(1.,1.),(1.,1.),(1.,1.),(1.,1.),(1.,
1.),(1.,1.),(1.,1.),(1.,1.),(1.,1.),(1.,1.),(1.,1.),(1.,1.),(1.,1.),(1.,
1.),(1.,1.),(1.,1.),(1.,1.),(1.,1.),(1.,1.),(1.,1.),(1.,1.),(1.,1.),(1.,
1.),(1.,1.),(1.,1.),(1.,1.),(1.,1.),(1.,1.),(1.,1.),(1.,1.),(1.,1.),(1.,
1.),(1.,1.),(1.,1.),(1.,1.),(1.,1.),(1.,1.),(1.,1.),(1.,1.),(1.,1.),(1.,
1.),(1.,1.),(1.,1.),(1.,1.),(1.,1.),(1.,1.),(1.,1.),(1.,1.),(1.,1.),(1.,
1.),(1.,1.),(1.,1.),(1.,1.),(1.,1.),(1.,1.),(1.,1.),(1.,1.),(1.,1.),(1.,
1.),(1.,1.),(1.,1.),(1.,1.),(1.,1.),(1.,1.),(1.,1.),(1.,1.),(1.,1.),(1.,
1.),(1.,1.),(1.,1.),(1.,1.),(1.,1.),(1.,1.),(1.,1.),(1.,1.),(1.,1.),(1.,
1.),(1.,1.),(1.,1.),(1.,1.),(1.,1.),(1.,1.),(1.,1.),(1.,1.),(1.,1.),(1.,
1.),(1.,1.),(1.,1.),(1.,1.),(1.,1.),(1.,1.),(1.,1.),(1.,1.),(1.,1.),(1.,
1.),(1.,1.),(1.,1.),(1.,1.),(1.,1.),(1.,1.),(1.,1.),(1.,1.),(1.,1.),(1.,
1.),(1.,1.),(1.,1.),(1.,1.),(1.,1.),(1.,1.),(1.,1.),(1.,1.),(1.,1.),(1.,
1.),(1.,1.),(1.,1.),(1.,1.),(1.,1.),(1.,1.),(1.,1.),(1.,1.),(1.,1.),(1.,
1.),(1.,1.),(1.,1.),(1.,1.),(1.,1.),(1.,1.),(1.,1.),(1.,1.),(1.,1.),(1.,
1.),(1.,1.),(1.,1.),(1.,1.),(1.,1.),(1.,1.),(1.,1.),(1.,1.),(1.,1.),(1.,
1.),(1.,1.),(1.,1.),(1.,1.),(1.,1.),(1.,1.),(1.,1.),(1.,1.),(1.,1.),(1.,
1.),(1.,1.),(1.,1.),(1.,1.),(1.,1.),(1.,1.),(1.,1.),(1.,1.),(1.,1.),(1.,
1.),(1.,1.),(1.,1.),(1.,1.),(1.,1.),(1.,1.),(1.,1.),(1.,1.),(1.,1.),(1.,
1.),(1.,1.),(1.,1.),(1.,1.),(1.,1.),(1.,1.),(1.,1.),(1.,1.),(1.,1.),(1.,
1.),(1.,1.)))
REPRESENTATION_ITEM('')
SURFACE()
);
#956=(
BOUNDED_SURFACE()
B_SPLINE_SURFACE(5,1,((#117794,#117795),(#117796,#117797),(#117798,#117799),
(#117800,#117801),(#117802,#117803),(#117804,#117805),(#117806,#117807),
(#117808,#117809),(#117810,#117811),(#117812,#117813),(#117814,#117815),
(#117816,#117817),(#117818,#117819),(#117820,#117821),(#117822,#117823),
(#117824,#117825),(#117826,#117827),(#117828,#117829),(#117830,#117831),
(#117832,#117833),(#117834,#117835),(#117836,#117837),(#117838,#117839),
(#117840,#117841),(#117842,#117843),(#117844,#117845),(#117846,#117847),
(#117848,#117849),(#117850,#117851),(#117852,#117853),(#117854,#117855),
(#117856,#117857),(#117858,#117859),(#117860,#117861),(#117862,#117863),
(#117864,#117865),(#117866,#117867),(#117868,#117869),(#117870,#117871),
(#117872,#117873),(#117874,#117875),(#117876,#117877),(#117878,#117879),
(#117880,#117881),(#117882,#117883),(#117884,#117885),(#117886,#117887),
(#117888,#117889),(#117890,#117891),(#117892,#117893),(#117894,#117895),
(#117896,#117897),(#117898,#117899),(#117900,#117901),(#117902,#117903),
(#117904,#117905),(#117906,#117907),(#117908,#117909),(#117910,#117911),
(#117912,#117913),(#117914,#117915),(#117916,#117917),(#117918,#117919),
(#117920,#117921),(#117922,#117923),(#117924,#117925),(#117926,#117927),
(#117928,#117929),(#117930,#117931),(#117932,#117933),(#117934,#117935),
(#117936,#117937),(#117938,#117939),(#117940,#117941),(#117942,#117943),
(#117944,#117945),(#117946,#117947),(#117948,#117949),(#117950,#117951),
(#117952,#117953),(#117954,#117955),(#117956,#117957),(#117958,#117959),
(#117960,#117961),(#117962,#117963),(#117964,#117965),(#117966,#117967),
(#117968,#117969),(#117970,#117971),(#117972,#117973),(#117974,#117975),
(#117976,#117977),(#117978,#117979),(#117980,#117981),(#117982,#117983),
(#117984,#117985),(#117986,#117987),(#117988,#117989),(#117990,#117991),
(#117992,#117993),(#117994,#117995),(#117996,#117997),(#117998,#117999),
(#118000,#118001),(#118002,#118003),(#118004,#118005),(#118006,#118007),
(#118008,#118009),(#118010,#118011),(#118012,#118013),(#118014,#118015),
(#118016,#118017),(#118018,#118019),(#118020,#118021),(#118022,#118023),
(#118024,#118025),(#118026,#118027),(#118028,#118029),(#118030,#118031),
(#118032,#118033),(#118034,#118035),(#118036,#118037),(#118038,#118039),
(#118040,#118041),(#118042,#118043),(#118044,#118045),(#118046,#118047),
(#118048,#118049),(#118050,#118051),(#118052,#118053),(#118054,#118055),
(#118056,#118057),(#118058,#118059),(#118060,#118061),(#118062,#118063),
(#118064,#118065),(#118066,#118067),(#118068,#118069),(#118070,#118071),
(#118072,#118073),(#118074,#118075),(#118076,#118077),(#118078,#118079),
(#118080,#118081),(#118082,#118083),(#118084,#118085),(#118086,#118087),
(#118088,#118089),(#118090,#118091),(#118092,#118093),(#118094,#118095),
(#118096,#118097),(#118098,#118099),(#118100,#118101),(#118102,#118103),
(#118104,#118105),(#118106,#118107),(#118108,#118109),(#118110,#118111),
(#118112,#118113),(#118114,#118115),(#118116,#118117),(#118118,#118119),
(#118120,#118121),(#118122,#118123),(#118124,#118125),(#118126,#118127),
(#118128,#118129),(#118130,#118131),(#118132,#118133),(#118134,#118135),
(#118136,#118137),(#118138,#118139),(#118140,#118141),(#118142,#118143),
(#118144,#118145),(#118146,#118147),(#118148,#118149),(#118150,#118151),
(#118152,#118153),(#118154,#118155),(#118156,#118157),(#118158,#118159),
(#118160,#118161),(#118162,#118163),(#118164,#118165),(#118166,#118167),
(#118168,#118169),(#118170,#118171),(#118172,#118173),(#118174,#118175),
(#118176,#118177),(#118178,#118179),(#118180,#118181),(#118182,#118183),
(#118184,#118185),(#118186,#118187),(#118188,#118189),(#118190,#118191),
(#118192,#118193),(#118194,#118195),(#118196,#118197),(#118198,#118199),
(#118200,#118201),(#118202,#118203)),.UNSPECIFIED.,.F.,.F.,.F.)
B_SPLINE_SURFACE_WITH_KNOTS((6,1,1,1,1,1,1,1,1,1,1,1,1,1,1,1,1,1,1,1,1,
1,1,1,1,1,1,1,1,1,1,1,1,1,1,1,1,1,1,1,1,1,1,1,1,1,1,1,1,1,1,1,1,1,1,1,1,
1,1,1,1,1,1,1,1,1,1,1,1,1,1,1,1,1,1,1,1,1,1,1,1,1,1,1,1,1,1,1,1,1,1,1,1,
1,1,1,1,1,1,1,1,1,1,1,1,1,1,1,1,1,1,1,1,1,1,1,1,1,1,1,1,1,1,1,1,1,1,1,1,
1,1,1,1,1,1,1,1,1,1,1,1,1,1,1,1,1,1,1,1,1,1,1,1,1,1,1,1,1,1,1,1,1,1,1,1,
1,1,1,1,1,1,1,1,1,1,1,1,1,1,1,1,1,1,1,1,1,1,1,1,1,1,1,1,1,1,1,1,1,1,1,6),
(2,2),(-1.,-0.995000000000001,-0.990000000000001,-0.985000000000001,-0.980000000000001,
-0.975000000000001,-0.970000000000001,-0.965000000000001,-0.960000000000001,
-0.955000000000001,-0.950000000000001,-0.945000000000001,-0.940000000000001,
-0.935000000000001,-0.930000000000001,-0.925000000000001,-0.920000000000001,
-0.915000000000001,-0.910000000000001,-0.905000000000001,-0.900000000000001,
-0.895000000000001,-0.890000000000001,-0.885000000000001,-0.880000000000001,
-0.875000000000001,-0.870000000000001,-0.865000000000001,-0.860000000000001,
-0.855000000000001,-0.850000000000001,-0.845000000000001,-0.840000000000001,
-0.835000000000001,-0.830000000000001,-0.825000000000001,-0.820000000000001,
-0.815000000000001,-0.810000000000001,-0.805000000000001,-0.800000000000001,
-0.795000000000001,-0.790000000000001,-0.785000000000001,-0.780000000000001,
-0.775000000000001,-0.770000000000001,-0.765000000000001,-0.760000000000001,
-0.755000000000001,-0.750000000000001,-0.745000000000001,-0.740000000000001,
-0.735000000000001,-0.730000000000001,-0.725000000000001,-0.720000000000001,
-0.715000000000001,-0.710000000000001,-0.705000000000001,-0.700000000000001,
-0.695000000000001,-0.690000000000001,-0.685,-0.68,-0.675,-0.67,-0.665,
-0.66,-0.655,-0.65,-0.645,-0.64,-0.635,-0.63,-0.625,-0.62,-0.615,-0.61,
-0.605,-0.6,-0.595,-0.59,-0.585,-0.58,-0.575,-0.57,-0.565,-0.56,-0.555,
-0.55,-0.545,-0.54,-0.535,-0.53,-0.525,-0.52,-0.515,-0.51,-0.505,-0.5,-0.495,
-0.49,-0.485,-0.48,-0.475,-0.47,-0.465,-0.46,-0.455,-0.45,-0.445,-0.44,
-0.435,-0.43,-0.425,-0.42,-0.415,-0.41,-0.405,-0.4,-0.395,-0.39,-0.385,
-0.38,-0.375,-0.37,-0.365,-0.36,-0.355,-0.35,-0.345,-0.34,-0.335,-0.33,
-0.325,-0.32,-0.315,-0.31,-0.305,-0.3,-0.295,-0.29,-0.285,-0.28,-0.275,
-0.27,-0.265,-0.26,-0.255,-0.25,-0.245,-0.24,-0.235,-0.23,-0.225,-0.22,
-0.215,-0.21,-0.205,-0.2,-0.195,-0.19,-0.185,-0.18,-0.175,-0.17,-0.165,
-0.16,-0.155,-0.15,-0.145,-0.14,-0.135,-0.13,-0.125,-0.12,-0.115,-0.11,
-0.105,-0.1,-0.095,-0.09,-0.085,-0.08,-0.075,-0.07,-0.065,-0.06,-0.055,
-0.05,-0.045,-0.04,-0.035,-0.03,-0.025,-0.02,-0.015,-0.01,-0.005,0.),(0.,
1.2),.UNSPECIFIED.)
GEOMETRIC_REPRESENTATION_ITEM()
RATIONAL_B_SPLINE_SURFACE(((1.,1.),(1.,1.),(1.,1.),(1.,1.),(1.,1.),(1.,
1.),(1.,1.),(1.,1.),(1.,1.),(1.,1.),(1.,1.),(1.,1.),(1.,1.),(1.,1.),(1.,
1.),(1.,1.),(1.,1.),(1.,1.),(1.,1.),(1.,1.),(1.,1.),(1.,1.),(1.,1.),(1.,
1.),(1.,1.),(1.,1.),(1.,1.),(1.,1.),(1.,1.),(1.,1.),(1.,1.),(1.,1.),(1.,
1.),(1.,1.),(1.,1.),(1.,1.),(1.,1.),(1.,1.),(1.,1.),(1.,1.),(1.,1.),(1.,
1.),(1.,1.),(1.,1.),(1.,1.),(1.,1.),(1.,1.),(1.,1.),(1.,1.),(1.,1.),(1.,
1.),(1.,1.),(1.,1.),(1.,1.),(1.,1.),(1.,1.),(1.,1.),(1.,1.),(1.,1.),(1.,
1.),(1.,1.),(1.,1.),(1.,1.),(1.,1.),(1.,1.),(1.,1.),(1.,1.),(1.,1.),(1.,
1.),(1.,1.),(1.,1.),(1.,1.),(1.,1.),(1.,1.),(1.,1.),(1.,1.),(1.,1.),(1.,
1.),(1.,1.),(1.,1.),(1.,1.),(1.,1.),(1.,1.),(1.,1.),(1.,1.),(1.,1.),(1.,
1.),(1.,1.),(1.,1.),(1.,1.),(1.,1.),(1.,1.),(1.,1.),(1.,1.),(1.,1.),(1.,
1.),(1.,1.),(1.,1.),(1.,1.),(1.,1.),(1.,1.),(1.,1.),(1.,1.),(1.,1.),(1.,
1.),(1.,1.),(1.,1.),(1.,1.),(1.,1.),(1.,1.),(1.,1.),(1.,1.),(1.,1.),(1.,
1.),(1.,1.),(1.,1.),(1.,1.),(1.,1.),(1.,1.),(1.,1.),(1.,1.),(1.,1.),(1.,
1.),(1.,1.),(1.,1.),(1.,1.),(1.,1.),(1.,1.),(1.,1.),(1.,1.),(1.,1.),(1.,
1.),(1.,1.),(1.,1.),(1.,1.),(1.,1.),(1.,1.),(1.,1.),(1.,1.),(1.,1.),(1.,
1.),(1.,1.),(1.,1.),(1.,1.),(1.,1.),(1.,1.),(1.,1.),(1.,1.),(1.,1.),(1.,
1.),(1.,1.),(1.,1.),(1.,1.),(1.,1.),(1.,1.),(1.,1.),(1.,1.),(1.,1.),(1.,
1.),(1.,1.),(1.,1.),(1.,1.),(1.,1.),(1.,1.),(1.,1.),(1.,1.),(1.,1.),(1.,
1.),(1.,1.),(1.,1.),(1.,1.),(1.,1.),(1.,1.),(1.,1.),(1.,1.),(1.,1.),(1.,
1.),(1.,1.),(1.,1.),(1.,1.),(1.,1.),(1.,1.),(1.,1.),(1.,1.),(1.,1.),(1.,
1.),(1.,1.),(1.,1.),(1.,1.),(1.,1.),(1.,1.),(1.,1.),(1.,1.),(1.,1.),(1.,
1.),(1.,1.),(1.,1.),(1.,1.),(1.,1.),(1.,1.),(1.,1.),(1.,1.),(1.,1.),(1.,
1.),(1.,1.)))
REPRESENTATION_ITEM('')
SURFACE()
);
#957=(
BOUNDED_SURFACE()
B_SPLINE_SURFACE(5,1,((#118595,#118596),(#118597,#118598),(#118599,#118600),
(#118601,#118602),(#118603,#118604),(#118605,#118606),(#118607,#118608),
(#118609,#118610),(#118611,#118612),(#118613,#118614),(#118615,#118616),
(#118617,#118618),(#118619,#118620),(#118621,#118622),(#118623,#118624),
(#118625,#118626),(#118627,#118628),(#118629,#118630),(#118631,#118632),
(#118633,#118634),(#118635,#118636),(#118637,#118638),(#118639,#118640),
(#118641,#118642),(#118643,#118644),(#118645,#118646),(#118647,#118648),
(#118649,#118650),(#118651,#118652),(#118653,#118654),(#118655,#118656),
(#118657,#118658),(#118659,#118660),(#118661,#118662),(#118663,#118664),
(#118665,#118666),(#118667,#118668),(#118669,#118670),(#118671,#118672),
(#118673,#118674),(#118675,#118676),(#118677,#118678),(#118679,#118680),
(#118681,#118682),(#118683,#118684),(#118685,#118686),(#118687,#118688),
(#118689,#118690),(#118691,#118692),(#118693,#118694),(#118695,#118696),
(#118697,#118698),(#118699,#118700),(#118701,#118702),(#118703,#118704),
(#118705,#118706),(#118707,#118708),(#118709,#118710),(#118711,#118712),
(#118713,#118714),(#118715,#118716),(#118717,#118718),(#118719,#118720),
(#118721,#118722),(#118723,#118724),(#118725,#118726),(#118727,#118728),
(#118729,#118730),(#118731,#118732),(#118733,#118734),(#118735,#118736),
(#118737,#118738),(#118739,#118740),(#118741,#118742),(#118743,#118744),
(#118745,#118746),(#118747,#118748),(#118749,#118750),(#118751,#118752),
(#118753,#118754),(#118755,#118756),(#118757,#118758),(#118759,#118760),
(#118761,#118762),(#118763,#118764),(#118765,#118766),(#118767,#118768),
(#118769,#118770),(#118771,#118772),(#118773,#118774),(#118775,#118776),
(#118777,#118778),(#118779,#118780),(#118781,#118782),(#118783,#118784),
(#118785,#118786),(#118787,#118788),(#118789,#118790),(#118791,#118792),
(#118793,#118794),(#118795,#118796),(#118797,#118798),(#118799,#118800),
(#118801,#118802),(#118803,#118804),(#118805,#118806),(#118807,#118808),
(#118809,#118810),(#118811,#118812),(#118813,#118814),(#118815,#118816),
(#118817,#118818),(#118819,#118820),(#118821,#118822),(#118823,#118824),
(#118825,#118826),(#118827,#118828),(#118829,#118830),(#118831,#118832),
(#118833,#118834),(#118835,#118836),(#118837,#118838),(#118839,#118840),
(#118841,#118842),(#118843,#118844),(#118845,#118846),(#118847,#118848),
(#118849,#118850),(#118851,#118852),(#118853,#118854),(#118855,#118856),
(#118857,#118858),(#118859,#118860),(#118861,#118862),(#118863,#118864),
(#118865,#118866),(#118867,#118868),(#118869,#118870),(#118871,#118872),
(#118873,#118874),(#118875,#118876),(#118877,#118878),(#118879,#118880),
(#118881,#118882),(#118883,#118884),(#118885,#118886),(#118887,#118888),
(#118889,#118890),(#118891,#118892),(#118893,#118894),(#118895,#118896),
(#118897,#118898),(#118899,#118900),(#118901,#118902),(#118903,#118904),
(#118905,#118906),(#118907,#118908),(#118909,#118910),(#118911,#118912),
(#118913,#118914),(#118915,#118916),(#118917,#118918),(#118919,#118920),
(#118921,#118922),(#118923,#118924),(#118925,#118926),(#118927,#118928),
(#118929,#118930),(#118931,#118932),(#118933,#118934),(#118935,#118936),
(#118937,#118938),(#118939,#118940),(#118941,#118942),(#118943,#118944),
(#118945,#118946),(#118947,#118948),(#118949,#118950),(#118951,#118952),
(#118953,#118954),(#118955,#118956),(#118957,#118958),(#118959,#118960),
(#118961,#118962),(#118963,#118964),(#118965,#118966),(#118967,#118968),
(#118969,#118970),(#118971,#118972),(#118973,#118974),(#118975,#118976),
(#118977,#118978),(#118979,#118980),(#118981,#118982),(#118983,#118984),
(#118985,#118986),(#118987,#118988),(#118989,#118990),(#118991,#118992),
(#118993,#118994),(#118995,#118996),(#118997,#118998),(#118999,#119000),
(#119001,#119002),(#119003,#119004)),.UNSPECIFIED.,.F.,.F.,.F.)
B_SPLINE_SURFACE_WITH_KNOTS((6,1,1,1,1,1,1,1,1,1,1,1,1,1,1,1,1,1,1,1,1,
1,1,1,1,1,1,1,1,1,1,1,1,1,1,1,1,1,1,1,1,1,1,1,1,1,1,1,1,1,1,1,1,1,1,1,1,
1,1,1,1,1,1,1,1,1,1,1,1,1,1,1,1,1,1,1,1,1,1,1,1,1,1,1,1,1,1,1,1,1,1,1,1,
1,1,1,1,1,1,1,1,1,1,1,1,1,1,1,1,1,1,1,1,1,1,1,1,1,1,1,1,1,1,1,1,1,1,1,1,
1,1,1,1,1,1,1,1,1,1,1,1,1,1,1,1,1,1,1,1,1,1,1,1,1,1,1,1,1,1,1,1,1,1,1,1,
1,1,1,1,1,1,1,1,1,1,1,1,1,1,1,1,1,1,1,1,1,1,1,1,1,1,1,1,1,1,1,1,1,1,1,6),
(2,2),(-1.,-0.995000000000001,-0.990000000000001,-0.985000000000001,-0.980000000000001,
-0.975000000000001,-0.970000000000001,-0.965000000000001,-0.960000000000001,
-0.955000000000001,-0.950000000000001,-0.945000000000001,-0.940000000000001,
-0.935000000000001,-0.930000000000001,-0.925000000000001,-0.920000000000001,
-0.915000000000001,-0.910000000000001,-0.905000000000001,-0.900000000000001,
-0.895000000000001,-0.890000000000001,-0.885000000000001,-0.880000000000001,
-0.875000000000001,-0.870000000000001,-0.865000000000001,-0.860000000000001,
-0.855000000000001,-0.850000000000001,-0.845000000000001,-0.840000000000001,
-0.835000000000001,-0.830000000000001,-0.825000000000001,-0.820000000000001,
-0.815000000000001,-0.810000000000001,-0.805000000000001,-0.800000000000001,
-0.795000000000001,-0.790000000000001,-0.785000000000001,-0.780000000000001,
-0.775000000000001,-0.770000000000001,-0.765000000000001,-0.760000000000001,
-0.755000000000001,-0.750000000000001,-0.745000000000001,-0.740000000000001,
-0.735000000000001,-0.730000000000001,-0.725000000000001,-0.720000000000001,
-0.715000000000001,-0.710000000000001,-0.705000000000001,-0.700000000000001,
-0.695000000000001,-0.690000000000001,-0.685,-0.68,-0.675,-0.67,-0.665,
-0.66,-0.655,-0.65,-0.645,-0.64,-0.635,-0.63,-0.625,-0.62,-0.615,-0.61,
-0.605,-0.6,-0.595,-0.59,-0.585,-0.58,-0.575,-0.57,-0.565,-0.56,-0.555,
-0.55,-0.545,-0.54,-0.535,-0.53,-0.525,-0.52,-0.515,-0.51,-0.505,-0.5,-0.495,
-0.49,-0.485,-0.48,-0.475,-0.47,-0.465,-0.46,-0.455,-0.45,-0.445,-0.44,
-0.435,-0.43,-0.425,-0.42,-0.415,-0.41,-0.405,-0.4,-0.395,-0.39,-0.385,
-0.38,-0.375,-0.37,-0.365,-0.36,-0.355,-0.35,-0.345,-0.34,-0.335,-0.33,
-0.325,-0.32,-0.315,-0.31,-0.305,-0.3,-0.295,-0.29,-0.285,-0.28,-0.275,
-0.27,-0.265,-0.26,-0.255,-0.25,-0.245,-0.24,-0.235,-0.23,-0.225,-0.22,
-0.215,-0.21,-0.205,-0.2,-0.195,-0.19,-0.185,-0.18,-0.175,-0.17,-0.165,
-0.16,-0.155,-0.15,-0.145,-0.14,-0.135,-0.13,-0.125,-0.12,-0.115,-0.11,
-0.105,-0.1,-0.095,-0.09,-0.085,-0.08,-0.075,-0.07,-0.065,-0.06,-0.055,
-0.05,-0.045,-0.04,-0.035,-0.03,-0.025,-0.02,-0.015,-0.01,-0.005,0.),(0.,
1.2),.UNSPECIFIED.)
GEOMETRIC_REPRESENTATION_ITEM()
RATIONAL_B_SPLINE_SURFACE(((1.,1.),(1.,1.),(1.,1.),(1.,1.),(1.,1.),(1.,
1.),(1.,1.),(1.,1.),(1.,1.),(1.,1.),(1.,1.),(1.,1.),(1.,1.),(1.,1.),(1.,
1.),(1.,1.),(1.,1.),(1.,1.),(1.,1.),(1.,1.),(1.,1.),(1.,1.),(1.,1.),(1.,
1.),(1.,1.),(1.,1.),(1.,1.),(1.,1.),(1.,1.),(1.,1.),(1.,1.),(1.,1.),(1.,
1.),(1.,1.),(1.,1.),(1.,1.),(1.,1.),(1.,1.),(1.,1.),(1.,1.),(1.,1.),(1.,
1.),(1.,1.),(1.,1.),(1.,1.),(1.,1.),(1.,1.),(1.,1.),(1.,1.),(1.,1.),(1.,
1.),(1.,1.),(1.,1.),(1.,1.),(1.,1.),(1.,1.),(1.,1.),(1.,1.),(1.,1.),(1.,
1.),(1.,1.),(1.,1.),(1.,1.),(1.,1.),(1.,1.),(1.,1.),(1.,1.),(1.,1.),(1.,
1.),(1.,1.),(1.,1.),(1.,1.),(1.,1.),(1.,1.),(1.,1.),(1.,1.),(1.,1.),(1.,
1.),(1.,1.),(1.,1.),(1.,1.),(1.,1.),(1.,1.),(1.,1.),(1.,1.),(1.,1.),(1.,
1.),(1.,1.),(1.,1.),(1.,1.),(1.,1.),(1.,1.),(1.,1.),(1.,1.),(1.,1.),(1.,
1.),(1.,1.),(1.,1.),(1.,1.),(1.,1.),(1.,1.),(1.,1.),(1.,1.),(1.,1.),(1.,
1.),(1.,1.),(1.,1.),(1.,1.),(1.,1.),(1.,1.),(1.,1.),(1.,1.),(1.,1.),(1.,
1.),(1.,1.),(1.,1.),(1.,1.),(1.,1.),(1.,1.),(1.,1.),(1.,1.),(1.,1.),(1.,
1.),(1.,1.),(1.,1.),(1.,1.),(1.,1.),(1.,1.),(1.,1.),(1.,1.),(1.,1.),(1.,
1.),(1.,1.),(1.,1.),(1.,1.),(1.,1.),(1.,1.),(1.,1.),(1.,1.),(1.,1.),(1.,
1.),(1.,1.),(1.,1.),(1.,1.),(1.,1.),(1.,1.),(1.,1.),(1.,1.),(1.,1.),(1.,
1.),(1.,1.),(1.,1.),(1.,1.),(1.,1.),(1.,1.),(1.,1.),(1.,1.),(1.,1.),(1.,
1.),(1.,1.),(1.,1.),(1.,1.),(1.,1.),(1.,1.),(1.,1.),(1.,1.),(1.,1.),(1.,
1.),(1.,1.),(1.,1.),(1.,1.),(1.,1.),(1.,1.),(1.,1.),(1.,1.),(1.,1.),(1.,
1.),(1.,1.),(1.,1.),(1.,1.),(1.,1.),(1.,1.),(1.,1.),(1.,1.),(1.,1.),(1.,
1.),(1.,1.),(1.,1.),(1.,1.),(1.,1.),(1.,1.),(1.,1.),(1.,1.),(1.,1.),(1.,
1.),(1.,1.),(1.,1.),(1.,1.),(1.,1.),(1.,1.),(1.,1.),(1.,1.),(1.,1.),(1.,
1.),(1.,1.)))
REPRESENTATION_ITEM('')
SURFACE()
);
#958=(
BOUNDED_SURFACE()
B_SPLINE_SURFACE(5,1,((#119396,#119397),(#119398,#119399),(#119400,#119401),
(#119402,#119403),(#119404,#119405),(#119406,#119407),(#119408,#119409),
(#119410,#119411),(#119412,#119413),(#119414,#119415),(#119416,#119417),
(#119418,#119419),(#119420,#119421),(#119422,#119423),(#119424,#119425),
(#119426,#119427),(#119428,#119429),(#119430,#119431),(#119432,#119433),
(#119434,#119435),(#119436,#119437),(#119438,#119439),(#119440,#119441),
(#119442,#119443),(#119444,#119445),(#119446,#119447),(#119448,#119449),
(#119450,#119451),(#119452,#119453),(#119454,#119455),(#119456,#119457),
(#119458,#119459),(#119460,#119461),(#119462,#119463),(#119464,#119465),
(#119466,#119467),(#119468,#119469),(#119470,#119471),(#119472,#119473),
(#119474,#119475),(#119476,#119477),(#119478,#119479),(#119480,#119481),
(#119482,#119483),(#119484,#119485),(#119486,#119487),(#119488,#119489),
(#119490,#119491),(#119492,#119493),(#119494,#119495),(#119496,#119497),
(#119498,#119499),(#119500,#119501),(#119502,#119503),(#119504,#119505),
(#119506,#119507),(#119508,#119509),(#119510,#119511),(#119512,#119513),
(#119514,#119515),(#119516,#119517),(#119518,#119519),(#119520,#119521),
(#119522,#119523),(#119524,#119525),(#119526,#119527),(#119528,#119529),
(#119530,#119531),(#119532,#119533),(#119534,#119535),(#119536,#119537),
(#119538,#119539),(#119540,#119541),(#119542,#119543),(#119544,#119545),
(#119546,#119547),(#119548,#119549),(#119550,#119551),(#119552,#119553),
(#119554,#119555),(#119556,#119557),(#119558,#119559),(#119560,#119561),
(#119562,#119563),(#119564,#119565),(#119566,#119567),(#119568,#119569),
(#119570,#119571),(#119572,#119573),(#119574,#119575),(#119576,#119577),
(#119578,#119579),(#119580,#119581),(#119582,#119583),(#119584,#119585),
(#119586,#119587),(#119588,#119589),(#119590,#119591),(#119592,#119593),
(#119594,#119595),(#119596,#119597),(#119598,#119599),(#119600,#119601),
(#119602,#119603),(#119604,#119605),(#119606,#119607),(#119608,#119609),
(#119610,#119611),(#119612,#119613),(#119614,#119615),(#119616,#119617),
(#119618,#119619),(#119620,#119621),(#119622,#119623),(#119624,#119625),
(#119626,#119627),(#119628,#119629),(#119630,#119631),(#119632,#119633),
(#119634,#119635),(#119636,#119637),(#119638,#119639),(#119640,#119641),
(#119642,#119643),(#119644,#119645),(#119646,#119647),(#119648,#119649),
(#119650,#119651),(#119652,#119653),(#119654,#119655),(#119656,#119657),
(#119658,#119659),(#119660,#119661),(#119662,#119663),(#119664,#119665),
(#119666,#119667),(#119668,#119669),(#119670,#119671),(#119672,#119673),
(#119674,#119675),(#119676,#119677),(#119678,#119679),(#119680,#119681),
(#119682,#119683),(#119684,#119685),(#119686,#119687),(#119688,#119689),
(#119690,#119691),(#119692,#119693),(#119694,#119695),(#119696,#119697),
(#119698,#119699),(#119700,#119701),(#119702,#119703),(#119704,#119705),
(#119706,#119707),(#119708,#119709),(#119710,#119711),(#119712,#119713),
(#119714,#119715),(#119716,#119717),(#119718,#119719),(#119720,#119721),
(#119722,#119723),(#119724,#119725),(#119726,#119727),(#119728,#119729),
(#119730,#119731),(#119732,#119733),(#119734,#119735),(#119736,#119737),
(#119738,#119739),(#119740,#119741),(#119742,#119743),(#119744,#119745),
(#119746,#119747),(#119748,#119749),(#119750,#119751),(#119752,#119753),
(#119754,#119755),(#119756,#119757),(#119758,#119759),(#119760,#119761),
(#119762,#119763),(#119764,#119765),(#119766,#119767),(#119768,#119769),
(#119770,#119771),(#119772,#119773),(#119774,#119775),(#119776,#119777),
(#119778,#119779),(#119780,#119781),(#119782,#119783),(#119784,#119785),
(#119786,#119787),(#119788,#119789),(#119790,#119791),(#119792,#119793),
(#119794,#119795),(#119796,#119797),(#119798,#119799),(#119800,#119801),
(#119802,#119803),(#119804,#119805)),.UNSPECIFIED.,.F.,.F.,.F.)
B_SPLINE_SURFACE_WITH_KNOTS((6,1,1,1,1,1,1,1,1,1,1,1,1,1,1,1,1,1,1,1,1,
1,1,1,1,1,1,1,1,1,1,1,1,1,1,1,1,1,1,1,1,1,1,1,1,1,1,1,1,1,1,1,1,1,1,1,1,
1,1,1,1,1,1,1,1,1,1,1,1,1,1,1,1,1,1,1,1,1,1,1,1,1,1,1,1,1,1,1,1,1,1,1,1,
1,1,1,1,1,1,1,1,1,1,1,1,1,1,1,1,1,1,1,1,1,1,1,1,1,1,1,1,1,1,1,1,1,1,1,1,
1,1,1,1,1,1,1,1,1,1,1,1,1,1,1,1,1,1,1,1,1,1,1,1,1,1,1,1,1,1,1,1,1,1,1,1,
1,1,1,1,1,1,1,1,1,1,1,1,1,1,1,1,1,1,1,1,1,1,1,1,1,1,1,1,1,1,1,1,1,1,1,6),
(2,2),(-1.,-0.995000000000001,-0.990000000000001,-0.985000000000001,-0.980000000000001,
-0.975000000000001,-0.970000000000001,-0.965000000000001,-0.960000000000001,
-0.955000000000001,-0.950000000000001,-0.945000000000001,-0.940000000000001,
-0.935000000000001,-0.930000000000001,-0.925000000000001,-0.920000000000001,
-0.915000000000001,-0.910000000000001,-0.905000000000001,-0.900000000000001,
-0.895000000000001,-0.890000000000001,-0.885000000000001,-0.880000000000001,
-0.875000000000001,-0.870000000000001,-0.865000000000001,-0.860000000000001,
-0.855000000000001,-0.850000000000001,-0.845000000000001,-0.840000000000001,
-0.835000000000001,-0.830000000000001,-0.825000000000001,-0.820000000000001,
-0.815000000000001,-0.810000000000001,-0.805000000000001,-0.800000000000001,
-0.795000000000001,-0.790000000000001,-0.785000000000001,-0.780000000000001,
-0.775000000000001,-0.770000000000001,-0.765000000000001,-0.760000000000001,
-0.755000000000001,-0.750000000000001,-0.745000000000001,-0.740000000000001,
-0.735000000000001,-0.730000000000001,-0.725000000000001,-0.720000000000001,
-0.715000000000001,-0.710000000000001,-0.705000000000001,-0.700000000000001,
-0.695000000000001,-0.690000000000001,-0.685,-0.68,-0.675,-0.67,-0.665,
-0.66,-0.655,-0.65,-0.645,-0.64,-0.635,-0.63,-0.625,-0.62,-0.615,-0.61,
-0.605,-0.6,-0.595,-0.59,-0.585,-0.58,-0.575,-0.57,-0.565,-0.56,-0.555,
-0.55,-0.545,-0.54,-0.535,-0.53,-0.525,-0.52,-0.515,-0.51,-0.505,-0.5,-0.495,
-0.49,-0.485,-0.48,-0.475,-0.47,-0.465,-0.46,-0.455,-0.45,-0.445,-0.44,
-0.435,-0.43,-0.425,-0.42,-0.415,-0.41,-0.405,-0.4,-0.395,-0.39,-0.385,
-0.38,-0.375,-0.37,-0.365,-0.36,-0.355,-0.35,-0.345,-0.34,-0.335,-0.33,
-0.325,-0.32,-0.315,-0.31,-0.305,-0.3,-0.295,-0.29,-0.285,-0.28,-0.275,
-0.27,-0.265,-0.26,-0.255,-0.25,-0.245,-0.24,-0.235,-0.23,-0.225,-0.22,
-0.215,-0.21,-0.205,-0.2,-0.195,-0.19,-0.185,-0.18,-0.175,-0.17,-0.165,
-0.16,-0.155,-0.15,-0.145,-0.14,-0.135,-0.13,-0.125,-0.12,-0.115,-0.11,
-0.105,-0.1,-0.095,-0.09,-0.085,-0.08,-0.075,-0.07,-0.065,-0.06,-0.055,
-0.05,-0.045,-0.04,-0.035,-0.03,-0.025,-0.02,-0.015,-0.01,-0.005,0.),(0.,
1.2),.UNSPECIFIED.)
GEOMETRIC_REPRESENTATION_ITEM()
RATIONAL_B_SPLINE_SURFACE(((1.,1.),(1.,1.),(1.,1.),(1.,1.),(1.,1.),(1.,
1.),(1.,1.),(1.,1.),(1.,1.),(1.,1.),(1.,1.),(1.,1.),(1.,1.),(1.,1.),(1.,
1.),(1.,1.),(1.,1.),(1.,1.),(1.,1.),(1.,1.),(1.,1.),(1.,1.),(1.,1.),(1.,
1.),(1.,1.),(1.,1.),(1.,1.),(1.,1.),(1.,1.),(1.,1.),(1.,1.),(1.,1.),(1.,
1.),(1.,1.),(1.,1.),(1.,1.),(1.,1.),(1.,1.),(1.,1.),(1.,1.),(1.,1.),(1.,
1.),(1.,1.),(1.,1.),(1.,1.),(1.,1.),(1.,1.),(1.,1.),(1.,1.),(1.,1.),(1.,
1.),(1.,1.),(1.,1.),(1.,1.),(1.,1.),(1.,1.),(1.,1.),(1.,1.),(1.,1.),(1.,
1.),(1.,1.),(1.,1.),(1.,1.),(1.,1.),(1.,1.),(1.,1.),(1.,1.),(1.,1.),(1.,
1.),(1.,1.),(1.,1.),(1.,1.),(1.,1.),(1.,1.),(1.,1.),(1.,1.),(1.,1.),(1.,
1.),(1.,1.),(1.,1.),(1.,1.),(1.,1.),(1.,1.),(1.,1.),(1.,1.),(1.,1.),(1.,
1.),(1.,1.),(1.,1.),(1.,1.),(1.,1.),(1.,1.),(1.,1.),(1.,1.),(1.,1.),(1.,
1.),(1.,1.),(1.,1.),(1.,1.),(1.,1.),(1.,1.),(1.,1.),(1.,1.),(1.,1.),(1.,
1.),(1.,1.),(1.,1.),(1.,1.),(1.,1.),(1.,1.),(1.,1.),(1.,1.),(1.,1.),(1.,
1.),(1.,1.),(1.,1.),(1.,1.),(1.,1.),(1.,1.),(1.,1.),(1.,1.),(1.,1.),(1.,
1.),(1.,1.),(1.,1.),(1.,1.),(1.,1.),(1.,1.),(1.,1.),(1.,1.),(1.,1.),(1.,
1.),(1.,1.),(1.,1.),(1.,1.),(1.,1.),(1.,1.),(1.,1.),(1.,1.),(1.,1.),(1.,
1.),(1.,1.),(1.,1.),(1.,1.),(1.,1.),(1.,1.),(1.,1.),(1.,1.),(1.,1.),(1.,
1.),(1.,1.),(1.,1.),(1.,1.),(1.,1.),(1.,1.),(1.,1.),(1.,1.),(1.,1.),(1.,
1.),(1.,1.),(1.,1.),(1.,1.),(1.,1.),(1.,1.),(1.,1.),(1.,1.),(1.,1.),(1.,
1.),(1.,1.),(1.,1.),(1.,1.),(1.,1.),(1.,1.),(1.,1.),(1.,1.),(1.,1.),(1.,
1.),(1.,1.),(1.,1.),(1.,1.),(1.,1.),(1.,1.),(1.,1.),(1.,1.),(1.,1.),(1.,
1.),(1.,1.),(1.,1.),(1.,1.),(1.,1.),(1.,1.),(1.,1.),(1.,1.),(1.,1.),(1.,
1.),(1.,1.),(1.,1.),(1.,1.),(1.,1.),(1.,1.),(1.,1.),(1.,1.),(1.,1.),(1.,
1.),(1.,1.)))
REPRESENTATION_ITEM('')
SURFACE()
);
#959=(
BOUNDED_SURFACE()
B_SPLINE_SURFACE(5,1,((#120197,#120198),(#120199,#120200),(#120201,#120202),
(#120203,#120204),(#120205,#120206),(#120207,#120208),(#120209,#120210),
(#120211,#120212),(#120213,#120214),(#120215,#120216),(#120217,#120218),
(#120219,#120220),(#120221,#120222),(#120223,#120224),(#120225,#120226),
(#120227,#120228),(#120229,#120230),(#120231,#120232),(#120233,#120234),
(#120235,#120236),(#120237,#120238),(#120239,#120240),(#120241,#120242),
(#120243,#120244),(#120245,#120246),(#120247,#120248),(#120249,#120250),
(#120251,#120252),(#120253,#120254),(#120255,#120256),(#120257,#120258),
(#120259,#120260),(#120261,#120262),(#120263,#120264),(#120265,#120266),
(#120267,#120268),(#120269,#120270),(#120271,#120272),(#120273,#120274),
(#120275,#120276),(#120277,#120278),(#120279,#120280),(#120281,#120282),
(#120283,#120284),(#120285,#120286),(#120287,#120288),(#120289,#120290),
(#120291,#120292),(#120293,#120294),(#120295,#120296),(#120297,#120298),
(#120299,#120300),(#120301,#120302),(#120303,#120304),(#120305,#120306),
(#120307,#120308),(#120309,#120310),(#120311,#120312),(#120313,#120314),
(#120315,#120316),(#120317,#120318),(#120319,#120320),(#120321,#120322),
(#120323,#120324),(#120325,#120326),(#120327,#120328),(#120329,#120330),
(#120331,#120332),(#120333,#120334),(#120335,#120336),(#120337,#120338),
(#120339,#120340),(#120341,#120342),(#120343,#120344),(#120345,#120346),
(#120347,#120348),(#120349,#120350),(#120351,#120352),(#120353,#120354),
(#120355,#120356),(#120357,#120358),(#120359,#120360),(#120361,#120362),
(#120363,#120364),(#120365,#120366),(#120367,#120368),(#120369,#120370),
(#120371,#120372),(#120373,#120374),(#120375,#120376),(#120377,#120378),
(#120379,#120380),(#120381,#120382),(#120383,#120384),(#120385,#120386),
(#120387,#120388),(#120389,#120390),(#120391,#120392),(#120393,#120394),
(#120395,#120396),(#120397,#120398),(#120399,#120400),(#120401,#120402),
(#120403,#120404),(#120405,#120406),(#120407,#120408),(#120409,#120410),
(#120411,#120412),(#120413,#120414),(#120415,#120416),(#120417,#120418),
(#120419,#120420),(#120421,#120422),(#120423,#120424),(#120425,#120426),
(#120427,#120428),(#120429,#120430),(#120431,#120432),(#120433,#120434),
(#120435,#120436),(#120437,#120438),(#120439,#120440),(#120441,#120442),
(#120443,#120444),(#120445,#120446),(#120447,#120448),(#120449,#120450),
(#120451,#120452),(#120453,#120454),(#120455,#120456),(#120457,#120458),
(#120459,#120460),(#120461,#120462),(#120463,#120464),(#120465,#120466),
(#120467,#120468),(#120469,#120470),(#120471,#120472),(#120473,#120474),
(#120475,#120476),(#120477,#120478),(#120479,#120480),(#120481,#120482),
(#120483,#120484),(#120485,#120486),(#120487,#120488),(#120489,#120490),
(#120491,#120492),(#120493,#120494),(#120495,#120496),(#120497,#120498),
(#120499,#120500),(#120501,#120502),(#120503,#120504),(#120505,#120506),
(#120507,#120508),(#120509,#120510),(#120511,#120512),(#120513,#120514),
(#120515,#120516),(#120517,#120518),(#120519,#120520),(#120521,#120522),
(#120523,#120524),(#120525,#120526),(#120527,#120528),(#120529,#120530),
(#120531,#120532),(#120533,#120534),(#120535,#120536),(#120537,#120538),
(#120539,#120540),(#120541,#120542),(#120543,#120544),(#120545,#120546),
(#120547,#120548),(#120549,#120550),(#120551,#120552),(#120553,#120554),
(#120555,#120556),(#120557,#120558),(#120559,#120560),(#120561,#120562),
(#120563,#120564),(#120565,#120566),(#120567,#120568),(#120569,#120570),
(#120571,#120572),(#120573,#120574),(#120575,#120576),(#120577,#120578),
(#120579,#120580),(#120581,#120582),(#120583,#120584),(#120585,#120586),
(#120587,#120588),(#120589,#120590),(#120591,#120592),(#120593,#120594),
(#120595,#120596),(#120597,#120598),(#120599,#120600),(#120601,#120602),
(#120603,#120604),(#120605,#120606)),.UNSPECIFIED.,.F.,.F.,.F.)
B_SPLINE_SURFACE_WITH_KNOTS((6,1,1,1,1,1,1,1,1,1,1,1,1,1,1,1,1,1,1,1,1,
1,1,1,1,1,1,1,1,1,1,1,1,1,1,1,1,1,1,1,1,1,1,1,1,1,1,1,1,1,1,1,1,1,1,1,1,
1,1,1,1,1,1,1,1,1,1,1,1,1,1,1,1,1,1,1,1,1,1,1,1,1,1,1,1,1,1,1,1,1,1,1,1,
1,1,1,1,1,1,1,1,1,1,1,1,1,1,1,1,1,1,1,1,1,1,1,1,1,1,1,1,1,1,1,1,1,1,1,1,
1,1,1,1,1,1,1,1,1,1,1,1,1,1,1,1,1,1,1,1,1,1,1,1,1,1,1,1,1,1,1,1,1,1,1,1,
1,1,1,1,1,1,1,1,1,1,1,1,1,1,1,1,1,1,1,1,1,1,1,1,1,1,1,1,1,1,1,1,1,1,1,6),
(2,2),(-1.,-0.995000000000001,-0.990000000000001,-0.985000000000001,-0.980000000000001,
-0.975000000000001,-0.970000000000001,-0.965000000000001,-0.960000000000001,
-0.955000000000001,-0.950000000000001,-0.945000000000001,-0.940000000000001,
-0.935000000000001,-0.930000000000001,-0.925000000000001,-0.920000000000001,
-0.915000000000001,-0.910000000000001,-0.905000000000001,-0.900000000000001,
-0.895000000000001,-0.890000000000001,-0.885000000000001,-0.880000000000001,
-0.875000000000001,-0.870000000000001,-0.865000000000001,-0.860000000000001,
-0.855000000000001,-0.850000000000001,-0.845000000000001,-0.840000000000001,
-0.835000000000001,-0.830000000000001,-0.825000000000001,-0.820000000000001,
-0.815000000000001,-0.810000000000001,-0.805000000000001,-0.800000000000001,
-0.795000000000001,-0.790000000000001,-0.785000000000001,-0.780000000000001,
-0.775000000000001,-0.770000000000001,-0.765000000000001,-0.760000000000001,
-0.755000000000001,-0.750000000000001,-0.745000000000001,-0.740000000000001,
-0.735000000000001,-0.730000000000001,-0.725000000000001,-0.720000000000001,
-0.715000000000001,-0.710000000000001,-0.705000000000001,-0.700000000000001,
-0.695000000000001,-0.690000000000001,-0.685,-0.68,-0.675,-0.67,-0.665,
-0.66,-0.655,-0.65,-0.645,-0.64,-0.635,-0.63,-0.625,-0.62,-0.615,-0.61,
-0.605,-0.6,-0.595,-0.59,-0.585,-0.58,-0.575,-0.57,-0.565,-0.56,-0.555,
-0.55,-0.545,-0.54,-0.535,-0.53,-0.525,-0.52,-0.515,-0.51,-0.505,-0.5,-0.495,
-0.49,-0.485,-0.48,-0.475,-0.47,-0.465,-0.46,-0.455,-0.45,-0.445,-0.44,
-0.435,-0.43,-0.425,-0.42,-0.415,-0.41,-0.405,-0.4,-0.395,-0.39,-0.385,
-0.38,-0.375,-0.37,-0.365,-0.36,-0.355,-0.35,-0.345,-0.34,-0.335,-0.33,
-0.325,-0.32,-0.315,-0.31,-0.305,-0.3,-0.295,-0.29,-0.285,-0.28,-0.275,
-0.27,-0.265,-0.26,-0.255,-0.25,-0.245,-0.24,-0.235,-0.23,-0.225,-0.22,
-0.215,-0.21,-0.205,-0.2,-0.195,-0.19,-0.185,-0.18,-0.175,-0.17,-0.165,
-0.16,-0.155,-0.15,-0.145,-0.14,-0.135,-0.13,-0.125,-0.12,-0.115,-0.11,
-0.105,-0.1,-0.095,-0.09,-0.085,-0.08,-0.075,-0.07,-0.065,-0.06,-0.055,
-0.05,-0.045,-0.04,-0.035,-0.03,-0.025,-0.02,-0.015,-0.01,-0.005,0.),(0.,
1.2),.UNSPECIFIED.)
GEOMETRIC_REPRESENTATION_ITEM()
RATIONAL_B_SPLINE_SURFACE(((1.,1.),(1.,1.),(1.,1.),(1.,1.),(1.,1.),(1.,
1.),(1.,1.),(1.,1.),(1.,1.),(1.,1.),(1.,1.),(1.,1.),(1.,1.),(1.,1.),(1.,
1.),(1.,1.),(1.,1.),(1.,1.),(1.,1.),(1.,1.),(1.,1.),(1.,1.),(1.,1.),(1.,
1.),(1.,1.),(1.,1.),(1.,1.),(1.,1.),(1.,1.),(1.,1.),(1.,1.),(1.,1.),(1.,
1.),(1.,1.),(1.,1.),(1.,1.),(1.,1.),(1.,1.),(1.,1.),(1.,1.),(1.,1.),(1.,
1.),(1.,1.),(1.,1.),(1.,1.),(1.,1.),(1.,1.),(1.,1.),(1.,1.),(1.,1.),(1.,
1.),(1.,1.),(1.,1.),(1.,1.),(1.,1.),(1.,1.),(1.,1.),(1.,1.),(1.,1.),(1.,
1.),(1.,1.),(1.,1.),(1.,1.),(1.,1.),(1.,1.),(1.,1.),(1.,1.),(1.,1.),(1.,
1.),(1.,1.),(1.,1.),(1.,1.),(1.,1.),(1.,1.),(1.,1.),(1.,1.),(1.,1.),(1.,
1.),(1.,1.),(1.,1.),(1.,1.),(1.,1.),(1.,1.),(1.,1.),(1.,1.),(1.,1.),(1.,
1.),(1.,1.),(1.,1.),(1.,1.),(1.,1.),(1.,1.),(1.,1.),(1.,1.),(1.,1.),(1.,
1.),(1.,1.),(1.,1.),(1.,1.),(1.,1.),(1.,1.),(1.,1.),(1.,1.),(1.,1.),(1.,
1.),(1.,1.),(1.,1.),(1.,1.),(1.,1.),(1.,1.),(1.,1.),(1.,1.),(1.,1.),(1.,
1.),(1.,1.),(1.,1.),(1.,1.),(1.,1.),(1.,1.),(1.,1.),(1.,1.),(1.,1.),(1.,
1.),(1.,1.),(1.,1.),(1.,1.),(1.,1.),(1.,1.),(1.,1.),(1.,1.),(1.,1.),(1.,
1.),(1.,1.),(1.,1.),(1.,1.),(1.,1.),(1.,1.),(1.,1.),(1.,1.),(1.,1.),(1.,
1.),(1.,1.),(1.,1.),(1.,1.),(1.,1.),(1.,1.),(1.,1.),(1.,1.),(1.,1.),(1.,
1.),(1.,1.),(1.,1.),(1.,1.),(1.,1.),(1.,1.),(1.,1.),(1.,1.),(1.,1.),(1.,
1.),(1.,1.),(1.,1.),(1.,1.),(1.,1.),(1.,1.),(1.,1.),(1.,1.),(1.,1.),(1.,
1.),(1.,1.),(1.,1.),(1.,1.),(1.,1.),(1.,1.),(1.,1.),(1.,1.),(1.,1.),(1.,
1.),(1.,1.),(1.,1.),(1.,1.),(1.,1.),(1.,1.),(1.,1.),(1.,1.),(1.,1.),(1.,
1.),(1.,1.),(1.,1.),(1.,1.),(1.,1.),(1.,1.),(1.,1.),(1.,1.),(1.,1.),(1.,
1.),(1.,1.),(1.,1.),(1.,1.),(1.,1.),(1.,1.),(1.,1.),(1.,1.),(1.,1.),(1.,
1.),(1.,1.)))
REPRESENTATION_ITEM('')
SURFACE()
);
#960=(
BOUNDED_SURFACE()
B_SPLINE_SURFACE(5,1,((#120998,#120999),(#121000,#121001),(#121002,#121003),
(#121004,#121005),(#121006,#121007),(#121008,#121009),(#121010,#121011),
(#121012,#121013),(#121014,#121015),(#121016,#121017),(#121018,#121019),
(#121020,#121021),(#121022,#121023),(#121024,#121025),(#121026,#121027),
(#121028,#121029),(#121030,#121031),(#121032,#121033),(#121034,#121035),
(#121036,#121037),(#121038,#121039),(#121040,#121041),(#121042,#121043),
(#121044,#121045),(#121046,#121047),(#121048,#121049),(#121050,#121051),
(#121052,#121053),(#121054,#121055),(#121056,#121057),(#121058,#121059),
(#121060,#121061),(#121062,#121063),(#121064,#121065),(#121066,#121067),
(#121068,#121069),(#121070,#121071),(#121072,#121073),(#121074,#121075),
(#121076,#121077),(#121078,#121079),(#121080,#121081),(#121082,#121083),
(#121084,#121085),(#121086,#121087),(#121088,#121089),(#121090,#121091),
(#121092,#121093),(#121094,#121095),(#121096,#121097),(#121098,#121099),
(#121100,#121101),(#121102,#121103),(#121104,#121105),(#121106,#121107),
(#121108,#121109),(#121110,#121111),(#121112,#121113),(#121114,#121115),
(#121116,#121117),(#121118,#121119),(#121120,#121121),(#121122,#121123),
(#121124,#121125),(#121126,#121127),(#121128,#121129),(#121130,#121131),
(#121132,#121133),(#121134,#121135),(#121136,#121137),(#121138,#121139),
(#121140,#121141),(#121142,#121143),(#121144,#121145),(#121146,#121147),
(#121148,#121149),(#121150,#121151),(#121152,#121153),(#121154,#121155),
(#121156,#121157),(#121158,#121159),(#121160,#121161),(#121162,#121163),
(#121164,#121165),(#121166,#121167),(#121168,#121169),(#121170,#121171),
(#121172,#121173),(#121174,#121175),(#121176,#121177),(#121178,#121179),
(#121180,#121181),(#121182,#121183),(#121184,#121185),(#121186,#121187),
(#121188,#121189),(#121190,#121191),(#121192,#121193),(#121194,#121195),
(#121196,#121197),(#121198,#121199),(#121200,#121201),(#121202,#121203),
(#121204,#121205),(#121206,#121207),(#121208,#121209),(#121210,#121211),
(#121212,#121213),(#121214,#121215),(#121216,#121217),(#121218,#121219),
(#121220,#121221),(#121222,#121223),(#121224,#121225),(#121226,#121227),
(#121228,#121229),(#121230,#121231),(#121232,#121233),(#121234,#121235),
(#121236,#121237),(#121238,#121239),(#121240,#121241),(#121242,#121243),
(#121244,#121245),(#121246,#121247),(#121248,#121249),(#121250,#121251),
(#121252,#121253),(#121254,#121255),(#121256,#121257),(#121258,#121259),
(#121260,#121261),(#121262,#121263),(#121264,#121265),(#121266,#121267),
(#121268,#121269),(#121270,#121271),(#121272,#121273),(#121274,#121275),
(#121276,#121277),(#121278,#121279),(#121280,#121281),(#121282,#121283),
(#121284,#121285),(#121286,#121287),(#121288,#121289),(#121290,#121291),
(#121292,#121293),(#121294,#121295),(#121296,#121297),(#121298,#121299),
(#121300,#121301),(#121302,#121303),(#121304,#121305),(#121306,#121307),
(#121308,#121309),(#121310,#121311),(#121312,#121313),(#121314,#121315),
(#121316,#121317),(#121318,#121319),(#121320,#121321),(#121322,#121323),
(#121324,#121325),(#121326,#121327),(#121328,#121329),(#121330,#121331),
(#121332,#121333),(#121334,#121335),(#121336,#121337),(#121338,#121339),
(#121340,#121341),(#121342,#121343),(#121344,#121345),(#121346,#121347),
(#121348,#121349),(#121350,#121351),(#121352,#121353),(#121354,#121355),
(#121356,#121357),(#121358,#121359),(#121360,#121361),(#121362,#121363),
(#121364,#121365),(#121366,#121367),(#121368,#121369),(#121370,#121371),
(#121372,#121373),(#121374,#121375),(#121376,#121377),(#121378,#121379),
(#121380,#121381),(#121382,#121383),(#121384,#121385),(#121386,#121387),
(#121388,#121389),(#121390,#121391),(#121392,#121393),(#121394,#121395),
(#121396,#121397),(#121398,#121399),(#121400,#121401),(#121402,#121403),
(#121404,#121405),(#121406,#121407)),.UNSPECIFIED.,.F.,.F.,.F.)
B_SPLINE_SURFACE_WITH_KNOTS((6,1,1,1,1,1,1,1,1,1,1,1,1,1,1,1,1,1,1,1,1,
1,1,1,1,1,1,1,1,1,1,1,1,1,1,1,1,1,1,1,1,1,1,1,1,1,1,1,1,1,1,1,1,1,1,1,1,
1,1,1,1,1,1,1,1,1,1,1,1,1,1,1,1,1,1,1,1,1,1,1,1,1,1,1,1,1,1,1,1,1,1,1,1,
1,1,1,1,1,1,1,1,1,1,1,1,1,1,1,1,1,1,1,1,1,1,1,1,1,1,1,1,1,1,1,1,1,1,1,1,
1,1,1,1,1,1,1,1,1,1,1,1,1,1,1,1,1,1,1,1,1,1,1,1,1,1,1,1,1,1,1,1,1,1,1,1,
1,1,1,1,1,1,1,1,1,1,1,1,1,1,1,1,1,1,1,1,1,1,1,1,1,1,1,1,1,1,1,1,1,1,1,6),
(2,2),(-1.,-0.995000000000001,-0.990000000000001,-0.985000000000001,-0.980000000000001,
-0.975000000000001,-0.970000000000001,-0.965000000000001,-0.960000000000001,
-0.955000000000001,-0.950000000000001,-0.945000000000001,-0.940000000000001,
-0.935000000000001,-0.930000000000001,-0.925000000000001,-0.920000000000001,
-0.915000000000001,-0.910000000000001,-0.905000000000001,-0.900000000000001,
-0.895000000000001,-0.890000000000001,-0.885000000000001,-0.880000000000001,
-0.875000000000001,-0.870000000000001,-0.865000000000001,-0.860000000000001,
-0.855000000000001,-0.850000000000001,-0.845000000000001,-0.840000000000001,
-0.835000000000001,-0.830000000000001,-0.825000000000001,-0.820000000000001,
-0.815000000000001,-0.810000000000001,-0.805000000000001,-0.800000000000001,
-0.795000000000001,-0.790000000000001,-0.785000000000001,-0.780000000000001,
-0.775000000000001,-0.770000000000001,-0.765000000000001,-0.760000000000001,
-0.755000000000001,-0.750000000000001,-0.745000000000001,-0.740000000000001,
-0.735000000000001,-0.730000000000001,-0.725000000000001,-0.720000000000001,
-0.715000000000001,-0.710000000000001,-0.705000000000001,-0.700000000000001,
-0.695000000000001,-0.690000000000001,-0.685,-0.68,-0.675,-0.67,-0.665,
-0.66,-0.655,-0.65,-0.645,-0.64,-0.635,-0.63,-0.625,-0.62,-0.615,-0.61,
-0.605,-0.6,-0.595,-0.59,-0.585,-0.58,-0.575,-0.57,-0.565,-0.56,-0.555,
-0.55,-0.545,-0.54,-0.535,-0.53,-0.525,-0.52,-0.515,-0.51,-0.505,-0.5,-0.495,
-0.49,-0.485,-0.48,-0.475,-0.47,-0.465,-0.46,-0.455,-0.45,-0.445,-0.44,
-0.435,-0.43,-0.425,-0.42,-0.415,-0.41,-0.405,-0.4,-0.395,-0.39,-0.385,
-0.38,-0.375,-0.37,-0.365,-0.36,-0.355,-0.35,-0.345,-0.34,-0.335,-0.33,
-0.325,-0.32,-0.315,-0.31,-0.305,-0.3,-0.295,-0.29,-0.285,-0.28,-0.275,
-0.27,-0.265,-0.26,-0.255,-0.25,-0.245,-0.24,-0.235,-0.23,-0.225,-0.22,
-0.215,-0.21,-0.205,-0.2,-0.195,-0.19,-0.185,-0.18,-0.175,-0.17,-0.165,
-0.16,-0.155,-0.15,-0.145,-0.14,-0.135,-0.13,-0.125,-0.12,-0.115,-0.11,
-0.105,-0.1,-0.095,-0.09,-0.085,-0.08,-0.075,-0.07,-0.065,-0.06,-0.055,
-0.05,-0.045,-0.04,-0.035,-0.03,-0.025,-0.02,-0.015,-0.01,-0.005,0.),(0.,
1.2),.UNSPECIFIED.)
GEOMETRIC_REPRESENTATION_ITEM()
RATIONAL_B_SPLINE_SURFACE(((1.,1.),(1.,1.),(1.,1.),(1.,1.),(1.,1.),(1.,
1.),(1.,1.),(1.,1.),(1.,1.),(1.,1.),(1.,1.),(1.,1.),(1.,1.),(1.,1.),(1.,
1.),(1.,1.),(1.,1.),(1.,1.),(1.,1.),(1.,1.),(1.,1.),(1.,1.),(1.,1.),(1.,
1.),(1.,1.),(1.,1.),(1.,1.),(1.,1.),(1.,1.),(1.,1.),(1.,1.),(1.,1.),(1.,
1.),(1.,1.),(1.,1.),(1.,1.),(1.,1.),(1.,1.),(1.,1.),(1.,1.),(1.,1.),(1.,
1.),(1.,1.),(1.,1.),(1.,1.),(1.,1.),(1.,1.),(1.,1.),(1.,1.),(1.,1.),(1.,
1.),(1.,1.),(1.,1.),(1.,1.),(1.,1.),(1.,1.),(1.,1.),(1.,1.),(1.,1.),(1.,
1.),(1.,1.),(1.,1.),(1.,1.),(1.,1.),(1.,1.),(1.,1.),(1.,1.),(1.,1.),(1.,
1.),(1.,1.),(1.,1.),(1.,1.),(1.,1.),(1.,1.),(1.,1.),(1.,1.),(1.,1.),(1.,
1.),(1.,1.),(1.,1.),(1.,1.),(1.,1.),(1.,1.),(1.,1.),(1.,1.),(1.,1.),(1.,
1.),(1.,1.),(1.,1.),(1.,1.),(1.,1.),(1.,1.),(1.,1.),(1.,1.),(1.,1.),(1.,
1.),(1.,1.),(1.,1.),(1.,1.),(1.,1.),(1.,1.),(1.,1.),(1.,1.),(1.,1.),(1.,
1.),(1.,1.),(1.,1.),(1.,1.),(1.,1.),(1.,1.),(1.,1.),(1.,1.),(1.,1.),(1.,
1.),(1.,1.),(1.,1.),(1.,1.),(1.,1.),(1.,1.),(1.,1.),(1.,1.),(1.,1.),(1.,
1.),(1.,1.),(1.,1.),(1.,1.),(1.,1.),(1.,1.),(1.,1.),(1.,1.),(1.,1.),(1.,
1.),(1.,1.),(1.,1.),(1.,1.),(1.,1.),(1.,1.),(1.,1.),(1.,1.),(1.,1.),(1.,
1.),(1.,1.),(1.,1.),(1.,1.),(1.,1.),(1.,1.),(1.,1.),(1.,1.),(1.,1.),(1.,
1.),(1.,1.),(1.,1.),(1.,1.),(1.,1.),(1.,1.),(1.,1.),(1.,1.),(1.,1.),(1.,
1.),(1.,1.),(1.,1.),(1.,1.),(1.,1.),(1.,1.),(1.,1.),(1.,1.),(1.,1.),(1.,
1.),(1.,1.),(1.,1.),(1.,1.),(1.,1.),(1.,1.),(1.,1.),(1.,1.),(1.,1.),(1.,
1.),(1.,1.),(1.,1.),(1.,1.),(1.,1.),(1.,1.),(1.,1.),(1.,1.),(1.,1.),(1.,
1.),(1.,1.),(1.,1.),(1.,1.),(1.,1.),(1.,1.),(1.,1.),(1.,1.),(1.,1.),(1.,
1.),(1.,1.),(1.,1.),(1.,1.),(1.,1.),(1.,1.),(1.,1.),(1.,1.),(1.,1.),(1.,
1.),(1.,1.)))
REPRESENTATION_ITEM('')
SURFACE()
);
#961=(
BOUNDED_SURFACE()
B_SPLINE_SURFACE(5,1,((#121799,#121800),(#121801,#121802),(#121803,#121804),
(#121805,#121806),(#121807,#121808),(#121809,#121810),(#121811,#121812),
(#121813,#121814),(#121815,#121816),(#121817,#121818),(#121819,#121820),
(#121821,#121822),(#121823,#121824),(#121825,#121826),(#121827,#121828),
(#121829,#121830),(#121831,#121832),(#121833,#121834),(#121835,#121836),
(#121837,#121838),(#121839,#121840),(#121841,#121842),(#121843,#121844),
(#121845,#121846),(#121847,#121848),(#121849,#121850),(#121851,#121852),
(#121853,#121854),(#121855,#121856),(#121857,#121858),(#121859,#121860),
(#121861,#121862),(#121863,#121864),(#121865,#121866),(#121867,#121868),
(#121869,#121870),(#121871,#121872),(#121873,#121874),(#121875,#121876),
(#121877,#121878),(#121879,#121880),(#121881,#121882),(#121883,#121884),
(#121885,#121886),(#121887,#121888),(#121889,#121890),(#121891,#121892),
(#121893,#121894),(#121895,#121896),(#121897,#121898),(#121899,#121900),
(#121901,#121902),(#121903,#121904),(#121905,#121906),(#121907,#121908),
(#121909,#121910),(#121911,#121912),(#121913,#121914),(#121915,#121916),
(#121917,#121918),(#121919,#121920),(#121921,#121922),(#121923,#121924),
(#121925,#121926),(#121927,#121928),(#121929,#121930),(#121931,#121932),
(#121933,#121934),(#121935,#121936),(#121937,#121938),(#121939,#121940),
(#121941,#121942),(#121943,#121944),(#121945,#121946),(#121947,#121948),
(#121949,#121950),(#121951,#121952),(#121953,#121954),(#121955,#121956),
(#121957,#121958),(#121959,#121960),(#121961,#121962),(#121963,#121964),
(#121965,#121966),(#121967,#121968),(#121969,#121970),(#121971,#121972),
(#121973,#121974),(#121975,#121976),(#121977,#121978),(#121979,#121980),
(#121981,#121982),(#121983,#121984),(#121985,#121986),(#121987,#121988),
(#121989,#121990),(#121991,#121992),(#121993,#121994),(#121995,#121996),
(#121997,#121998),(#121999,#122000),(#122001,#122002),(#122003,#122004),
(#122005,#122006),(#122007,#122008),(#122009,#122010),(#122011,#122012),
(#122013,#122014),(#122015,#122016),(#122017,#122018),(#122019,#122020),
(#122021,#122022),(#122023,#122024),(#122025,#122026),(#122027,#122028),
(#122029,#122030),(#122031,#122032),(#122033,#122034),(#122035,#122036),
(#122037,#122038),(#122039,#122040),(#122041,#122042),(#122043,#122044),
(#122045,#122046),(#122047,#122048),(#122049,#122050),(#122051,#122052),
(#122053,#122054),(#122055,#122056),(#122057,#122058),(#122059,#122060),
(#122061,#122062),(#122063,#122064),(#122065,#122066),(#122067,#122068),
(#122069,#122070),(#122071,#122072),(#122073,#122074),(#122075,#122076),
(#122077,#122078),(#122079,#122080),(#122081,#122082),(#122083,#122084),
(#122085,#122086),(#122087,#122088),(#122089,#122090),(#122091,#122092),
(#122093,#122094),(#122095,#122096),(#122097,#122098),(#122099,#122100),
(#122101,#122102),(#122103,#122104),(#122105,#122106),(#122107,#122108),
(#122109,#122110),(#122111,#122112),(#122113,#122114),(#122115,#122116),
(#122117,#122118),(#122119,#122120),(#122121,#122122),(#122123,#122124),
(#122125,#122126),(#122127,#122128),(#122129,#122130),(#122131,#122132),
(#122133,#122134),(#122135,#122136),(#122137,#122138),(#122139,#122140),
(#122141,#122142),(#122143,#122144),(#122145,#122146),(#122147,#122148),
(#122149,#122150),(#122151,#122152),(#122153,#122154),(#122155,#122156),
(#122157,#122158),(#122159,#122160),(#122161,#122162),(#122163,#122164),
(#122165,#122166),(#122167,#122168),(#122169,#122170),(#122171,#122172),
(#122173,#122174),(#122175,#122176),(#122177,#122178),(#122179,#122180),
(#122181,#122182),(#122183,#122184),(#122185,#122186),(#122187,#122188),
(#122189,#122190),(#122191,#122192),(#122193,#122194),(#122195,#122196),
(#122197,#122198),(#122199,#122200),(#122201,#122202),(#122203,#122204),
(#122205,#122206),(#122207,#122208)),.UNSPECIFIED.,.F.,.F.,.F.)
B_SPLINE_SURFACE_WITH_KNOTS((6,1,1,1,1,1,1,1,1,1,1,1,1,1,1,1,1,1,1,1,1,
1,1,1,1,1,1,1,1,1,1,1,1,1,1,1,1,1,1,1,1,1,1,1,1,1,1,1,1,1,1,1,1,1,1,1,1,
1,1,1,1,1,1,1,1,1,1,1,1,1,1,1,1,1,1,1,1,1,1,1,1,1,1,1,1,1,1,1,1,1,1,1,1,
1,1,1,1,1,1,1,1,1,1,1,1,1,1,1,1,1,1,1,1,1,1,1,1,1,1,1,1,1,1,1,1,1,1,1,1,
1,1,1,1,1,1,1,1,1,1,1,1,1,1,1,1,1,1,1,1,1,1,1,1,1,1,1,1,1,1,1,1,1,1,1,1,
1,1,1,1,1,1,1,1,1,1,1,1,1,1,1,1,1,1,1,1,1,1,1,1,1,1,1,1,1,1,1,1,1,1,1,6),
(2,2),(-1.,-0.995000000000001,-0.990000000000001,-0.985000000000001,-0.980000000000001,
-0.975000000000001,-0.970000000000001,-0.965000000000001,-0.960000000000001,
-0.955000000000001,-0.950000000000001,-0.945000000000001,-0.940000000000001,
-0.935000000000001,-0.930000000000001,-0.925000000000001,-0.920000000000001,
-0.915000000000001,-0.910000000000001,-0.905000000000001,-0.900000000000001,
-0.895000000000001,-0.890000000000001,-0.885000000000001,-0.880000000000001,
-0.875000000000001,-0.870000000000001,-0.865000000000001,-0.860000000000001,
-0.855000000000001,-0.850000000000001,-0.845000000000001,-0.840000000000001,
-0.835000000000001,-0.830000000000001,-0.825000000000001,-0.820000000000001,
-0.815000000000001,-0.810000000000001,-0.805000000000001,-0.800000000000001,
-0.795000000000001,-0.790000000000001,-0.785000000000001,-0.780000000000001,
-0.775000000000001,-0.770000000000001,-0.765000000000001,-0.760000000000001,
-0.755000000000001,-0.750000000000001,-0.745000000000001,-0.740000000000001,
-0.735000000000001,-0.730000000000001,-0.725000000000001,-0.720000000000001,
-0.715000000000001,-0.710000000000001,-0.705000000000001,-0.700000000000001,
-0.695000000000001,-0.690000000000001,-0.685,-0.68,-0.675,-0.67,-0.665,
-0.66,-0.655,-0.65,-0.645,-0.64,-0.635,-0.63,-0.625,-0.62,-0.615,-0.61,
-0.605,-0.6,-0.595,-0.59,-0.585,-0.58,-0.575,-0.57,-0.565,-0.56,-0.555,
-0.55,-0.545,-0.54,-0.535,-0.53,-0.525,-0.52,-0.515,-0.51,-0.505,-0.5,-0.495,
-0.49,-0.485,-0.48,-0.475,-0.47,-0.465,-0.46,-0.455,-0.45,-0.445,-0.44,
-0.435,-0.43,-0.425,-0.42,-0.415,-0.41,-0.405,-0.4,-0.395,-0.39,-0.385,
-0.38,-0.375,-0.37,-0.365,-0.36,-0.355,-0.35,-0.345,-0.34,-0.335,-0.33,
-0.325,-0.32,-0.315,-0.31,-0.305,-0.3,-0.295,-0.29,-0.285,-0.28,-0.275,
-0.27,-0.265,-0.26,-0.255,-0.25,-0.245,-0.24,-0.235,-0.23,-0.225,-0.22,
-0.215,-0.21,-0.205,-0.2,-0.195,-0.19,-0.185,-0.18,-0.175,-0.17,-0.165,
-0.16,-0.155,-0.15,-0.145,-0.14,-0.135,-0.13,-0.125,-0.12,-0.115,-0.11,
-0.105,-0.1,-0.095,-0.09,-0.085,-0.08,-0.075,-0.07,-0.065,-0.06,-0.055,
-0.05,-0.045,-0.04,-0.035,-0.03,-0.025,-0.02,-0.015,-0.01,-0.005,0.),(0.,
1.2),.UNSPECIFIED.)
GEOMETRIC_REPRESENTATION_ITEM()
RATIONAL_B_SPLINE_SURFACE(((1.,1.),(1.,1.),(1.,1.),(1.,1.),(1.,1.),(1.,
1.),(1.,1.),(1.,1.),(1.,1.),(1.,1.),(1.,1.),(1.,1.),(1.,1.),(1.,1.),(1.,
1.),(1.,1.),(1.,1.),(1.,1.),(1.,1.),(1.,1.),(1.,1.),(1.,1.),(1.,1.),(1.,
1.),(1.,1.),(1.,1.),(1.,1.),(1.,1.),(1.,1.),(1.,1.),(1.,1.),(1.,1.),(1.,
1.),(1.,1.),(1.,1.),(1.,1.),(1.,1.),(1.,1.),(1.,1.),(1.,1.),(1.,1.),(1.,
1.),(1.,1.),(1.,1.),(1.,1.),(1.,1.),(1.,1.),(1.,1.),(1.,1.),(1.,1.),(1.,
1.),(1.,1.),(1.,1.),(1.,1.),(1.,1.),(1.,1.),(1.,1.),(1.,1.),(1.,1.),(1.,
1.),(1.,1.),(1.,1.),(1.,1.),(1.,1.),(1.,1.),(1.,1.),(1.,1.),(1.,1.),(1.,
1.),(1.,1.),(1.,1.),(1.,1.),(1.,1.),(1.,1.),(1.,1.),(1.,1.),(1.,1.),(1.,
1.),(1.,1.),(1.,1.),(1.,1.),(1.,1.),(1.,1.),(1.,1.),(1.,1.),(1.,1.),(1.,
1.),(1.,1.),(1.,1.),(1.,1.),(1.,1.),(1.,1.),(1.,1.),(1.,1.),(1.,1.),(1.,
1.),(1.,1.),(1.,1.),(1.,1.),(1.,1.),(1.,1.),(1.,1.),(1.,1.),(1.,1.),(1.,
1.),(1.,1.),(1.,1.),(1.,1.),(1.,1.),(1.,1.),(1.,1.),(1.,1.),(1.,1.),(1.,
1.),(1.,1.),(1.,1.),(1.,1.),(1.,1.),(1.,1.),(1.,1.),(1.,1.),(1.,1.),(1.,
1.),(1.,1.),(1.,1.),(1.,1.),(1.,1.),(1.,1.),(1.,1.),(1.,1.),(1.,1.),(1.,
1.),(1.,1.),(1.,1.),(1.,1.),(1.,1.),(1.,1.),(1.,1.),(1.,1.),(1.,1.),(1.,
1.),(1.,1.),(1.,1.),(1.,1.),(1.,1.),(1.,1.),(1.,1.),(1.,1.),(1.,1.),(1.,
1.),(1.,1.),(1.,1.),(1.,1.),(1.,1.),(1.,1.),(1.,1.),(1.,1.),(1.,1.),(1.,
1.),(1.,1.),(1.,1.),(1.,1.),(1.,1.),(1.,1.),(1.,1.),(1.,1.),(1.,1.),(1.,
1.),(1.,1.),(1.,1.),(1.,1.),(1.,1.),(1.,1.),(1.,1.),(1.,1.),(1.,1.),(1.,
1.),(1.,1.),(1.,1.),(1.,1.),(1.,1.),(1.,1.),(1.,1.),(1.,1.),(1.,1.),(1.,
1.),(1.,1.),(1.,1.),(1.,1.),(1.,1.),(1.,1.),(1.,1.),(1.,1.),(1.,1.),(1.,
1.),(1.,1.),(1.,1.),(1.,1.),(1.,1.),(1.,1.),(1.,1.),(1.,1.),(1.,1.),(1.,
1.),(1.,1.)))
REPRESENTATION_ITEM('')
SURFACE()
);
#962=(
BOUNDED_SURFACE()
B_SPLINE_SURFACE(5,1,((#122600,#122601),(#122602,#122603),(#122604,#122605),
(#122606,#122607),(#122608,#122609),(#122610,#122611),(#122612,#122613),
(#122614,#122615),(#122616,#122617),(#122618,#122619),(#122620,#122621),
(#122622,#122623),(#122624,#122625),(#122626,#122627),(#122628,#122629),
(#122630,#122631),(#122632,#122633),(#122634,#122635),(#122636,#122637),
(#122638,#122639),(#122640,#122641),(#122642,#122643),(#122644,#122645),
(#122646,#122647),(#122648,#122649),(#122650,#122651),(#122652,#122653),
(#122654,#122655),(#122656,#122657),(#122658,#122659),(#122660,#122661),
(#122662,#122663),(#122664,#122665),(#122666,#122667),(#122668,#122669),
(#122670,#122671),(#122672,#122673),(#122674,#122675),(#122676,#122677),
(#122678,#122679),(#122680,#122681),(#122682,#122683),(#122684,#122685),
(#122686,#122687),(#122688,#122689),(#122690,#122691),(#122692,#122693),
(#122694,#122695),(#122696,#122697),(#122698,#122699),(#122700,#122701),
(#122702,#122703),(#122704,#122705),(#122706,#122707),(#122708,#122709),
(#122710,#122711),(#122712,#122713),(#122714,#122715),(#122716,#122717),
(#122718,#122719),(#122720,#122721),(#122722,#122723),(#122724,#122725),
(#122726,#122727),(#122728,#122729),(#122730,#122731),(#122732,#122733),
(#122734,#122735),(#122736,#122737),(#122738,#122739),(#122740,#122741),
(#122742,#122743),(#122744,#122745),(#122746,#122747),(#122748,#122749),
(#122750,#122751),(#122752,#122753),(#122754,#122755),(#122756,#122757),
(#122758,#122759),(#122760,#122761),(#122762,#122763),(#122764,#122765),
(#122766,#122767),(#122768,#122769),(#122770,#122771),(#122772,#122773),
(#122774,#122775),(#122776,#122777),(#122778,#122779),(#122780,#122781),
(#122782,#122783),(#122784,#122785),(#122786,#122787),(#122788,#122789),
(#122790,#122791),(#122792,#122793),(#122794,#122795),(#122796,#122797),
(#122798,#122799),(#122800,#122801),(#122802,#122803),(#122804,#122805),
(#122806,#122807),(#122808,#122809),(#122810,#122811),(#122812,#122813),
(#122814,#122815),(#122816,#122817),(#122818,#122819),(#122820,#122821),
(#122822,#122823),(#122824,#122825),(#122826,#122827),(#122828,#122829),
(#122830,#122831),(#122832,#122833),(#122834,#122835),(#122836,#122837),
(#122838,#122839),(#122840,#122841),(#122842,#122843),(#122844,#122845),
(#122846,#122847),(#122848,#122849),(#122850,#122851),(#122852,#122853),
(#122854,#122855),(#122856,#122857),(#122858,#122859),(#122860,#122861),
(#122862,#122863),(#122864,#122865),(#122866,#122867),(#122868,#122869),
(#122870,#122871),(#122872,#122873),(#122874,#122875),(#122876,#122877),
(#122878,#122879),(#122880,#122881),(#122882,#122883),(#122884,#122885),
(#122886,#122887),(#122888,#122889),(#122890,#122891),(#122892,#122893),
(#122894,#122895),(#122896,#122897),(#122898,#122899),(#122900,#122901),
(#122902,#122903),(#122904,#122905),(#122906,#122907),(#122908,#122909),
(#122910,#122911),(#122912,#122913),(#122914,#122915),(#122916,#122917),
(#122918,#122919),(#122920,#122921),(#122922,#122923),(#122924,#122925),
(#122926,#122927),(#122928,#122929),(#122930,#122931),(#122932,#122933),
(#122934,#122935),(#122936,#122937),(#122938,#122939),(#122940,#122941),
(#122942,#122943),(#122944,#122945),(#122946,#122947),(#122948,#122949),
(#122950,#122951),(#122952,#122953),(#122954,#122955),(#122956,#122957),
(#122958,#122959),(#122960,#122961),(#122962,#122963),(#122964,#122965),
(#122966,#122967),(#122968,#122969),(#122970,#122971),(#122972,#122973),
(#122974,#122975),(#122976,#122977),(#122978,#122979),(#122980,#122981),
(#122982,#122983),(#122984,#122985),(#122986,#122987),(#122988,#122989),
(#122990,#122991),(#122992,#122993),(#122994,#122995),(#122996,#122997),
(#122998,#122999),(#123000,#123001),(#123002,#123003),(#123004,#123005),
(#123006,#123007),(#123008,#123009)),.UNSPECIFIED.,.F.,.F.,.F.)
B_SPLINE_SURFACE_WITH_KNOTS((6,1,1,1,1,1,1,1,1,1,1,1,1,1,1,1,1,1,1,1,1,
1,1,1,1,1,1,1,1,1,1,1,1,1,1,1,1,1,1,1,1,1,1,1,1,1,1,1,1,1,1,1,1,1,1,1,1,
1,1,1,1,1,1,1,1,1,1,1,1,1,1,1,1,1,1,1,1,1,1,1,1,1,1,1,1,1,1,1,1,1,1,1,1,
1,1,1,1,1,1,1,1,1,1,1,1,1,1,1,1,1,1,1,1,1,1,1,1,1,1,1,1,1,1,1,1,1,1,1,1,
1,1,1,1,1,1,1,1,1,1,1,1,1,1,1,1,1,1,1,1,1,1,1,1,1,1,1,1,1,1,1,1,1,1,1,1,
1,1,1,1,1,1,1,1,1,1,1,1,1,1,1,1,1,1,1,1,1,1,1,1,1,1,1,1,1,1,1,1,1,1,1,6),
(2,2),(-1.,-0.995000000000001,-0.990000000000001,-0.985000000000001,-0.980000000000001,
-0.975000000000001,-0.970000000000001,-0.965000000000001,-0.960000000000001,
-0.955000000000001,-0.950000000000001,-0.945000000000001,-0.940000000000001,
-0.935000000000001,-0.930000000000001,-0.925000000000001,-0.920000000000001,
-0.915000000000001,-0.910000000000001,-0.905000000000001,-0.900000000000001,
-0.895000000000001,-0.890000000000001,-0.885000000000001,-0.880000000000001,
-0.875000000000001,-0.870000000000001,-0.865000000000001,-0.860000000000001,
-0.855000000000001,-0.850000000000001,-0.845000000000001,-0.840000000000001,
-0.835000000000001,-0.830000000000001,-0.825000000000001,-0.820000000000001,
-0.815000000000001,-0.810000000000001,-0.805000000000001,-0.800000000000001,
-0.795000000000001,-0.790000000000001,-0.785000000000001,-0.780000000000001,
-0.775000000000001,-0.770000000000001,-0.765000000000001,-0.760000000000001,
-0.755000000000001,-0.750000000000001,-0.745000000000001,-0.740000000000001,
-0.735000000000001,-0.730000000000001,-0.725000000000001,-0.720000000000001,
-0.715000000000001,-0.710000000000001,-0.705000000000001,-0.700000000000001,
-0.695000000000001,-0.690000000000001,-0.685,-0.68,-0.675,-0.67,-0.665,
-0.66,-0.655,-0.65,-0.645,-0.64,-0.635,-0.63,-0.625,-0.62,-0.615,-0.61,
-0.605,-0.6,-0.595,-0.59,-0.585,-0.58,-0.575,-0.57,-0.565,-0.56,-0.555,
-0.55,-0.545,-0.54,-0.535,-0.53,-0.525,-0.52,-0.515,-0.51,-0.505,-0.5,-0.495,
-0.49,-0.485,-0.48,-0.475,-0.47,-0.465,-0.46,-0.455,-0.45,-0.445,-0.44,
-0.435,-0.43,-0.425,-0.42,-0.415,-0.41,-0.405,-0.4,-0.395,-0.39,-0.385,
-0.38,-0.375,-0.37,-0.365,-0.36,-0.355,-0.35,-0.345,-0.34,-0.335,-0.33,
-0.325,-0.32,-0.315,-0.31,-0.305,-0.3,-0.295,-0.29,-0.285,-0.28,-0.275,
-0.27,-0.265,-0.26,-0.255,-0.25,-0.245,-0.24,-0.235,-0.23,-0.225,-0.22,
-0.215,-0.21,-0.205,-0.2,-0.195,-0.19,-0.185,-0.18,-0.175,-0.17,-0.165,
-0.16,-0.155,-0.15,-0.145,-0.14,-0.135,-0.13,-0.125,-0.12,-0.115,-0.11,
-0.105,-0.1,-0.095,-0.09,-0.085,-0.08,-0.075,-0.07,-0.065,-0.06,-0.055,
-0.05,-0.045,-0.04,-0.035,-0.03,-0.025,-0.02,-0.015,-0.01,-0.005,0.),(0.,
1.2),.UNSPECIFIED.)
GEOMETRIC_REPRESENTATION_ITEM()
RATIONAL_B_SPLINE_SURFACE(((1.,1.),(1.,1.),(1.,1.),(1.,1.),(1.,1.),(1.,
1.),(1.,1.),(1.,1.),(1.,1.),(1.,1.),(1.,1.),(1.,1.),(1.,1.),(1.,1.),(1.,
1.),(1.,1.),(1.,1.),(1.,1.),(1.,1.),(1.,1.),(1.,1.),(1.,1.),(1.,1.),(1.,
1.),(1.,1.),(1.,1.),(1.,1.),(1.,1.),(1.,1.),(1.,1.),(1.,1.),(1.,1.),(1.,
1.),(1.,1.),(1.,1.),(1.,1.),(1.,1.),(1.,1.),(1.,1.),(1.,1.),(1.,1.),(1.,
1.),(1.,1.),(1.,1.),(1.,1.),(1.,1.),(1.,1.),(1.,1.),(1.,1.),(1.,1.),(1.,
1.),(1.,1.),(1.,1.),(1.,1.),(1.,1.),(1.,1.),(1.,1.),(1.,1.),(1.,1.),(1.,
1.),(1.,1.),(1.,1.),(1.,1.),(1.,1.),(1.,1.),(1.,1.),(1.,1.),(1.,1.),(1.,
1.),(1.,1.),(1.,1.),(1.,1.),(1.,1.),(1.,1.),(1.,1.),(1.,1.),(1.,1.),(1.,
1.),(1.,1.),(1.,1.),(1.,1.),(1.,1.),(1.,1.),(1.,1.),(1.,1.),(1.,1.),(1.,
1.),(1.,1.),(1.,1.),(1.,1.),(1.,1.),(1.,1.),(1.,1.),(1.,1.),(1.,1.),(1.,
1.),(1.,1.),(1.,1.),(1.,1.),(1.,1.),(1.,1.),(1.,1.),(1.,1.),(1.,1.),(1.,
1.),(1.,1.),(1.,1.),(1.,1.),(1.,1.),(1.,1.),(1.,1.),(1.,1.),(1.,1.),(1.,
1.),(1.,1.),(1.,1.),(1.,1.),(1.,1.),(1.,1.),(1.,1.),(1.,1.),(1.,1.),(1.,
1.),(1.,1.),(1.,1.),(1.,1.),(1.,1.),(1.,1.),(1.,1.),(1.,1.),(1.,1.),(1.,
1.),(1.,1.),(1.,1.),(1.,1.),(1.,1.),(1.,1.),(1.,1.),(1.,1.),(1.,1.),(1.,
1.),(1.,1.),(1.,1.),(1.,1.),(1.,1.),(1.,1.),(1.,1.),(1.,1.),(1.,1.),(1.,
1.),(1.,1.),(1.,1.),(1.,1.),(1.,1.),(1.,1.),(1.,1.),(1.,1.),(1.,1.),(1.,
1.),(1.,1.),(1.,1.),(1.,1.),(1.,1.),(1.,1.),(1.,1.),(1.,1.),(1.,1.),(1.,
1.),(1.,1.),(1.,1.),(1.,1.),(1.,1.),(1.,1.),(1.,1.),(1.,1.),(1.,1.),(1.,
1.),(1.,1.),(1.,1.),(1.,1.),(1.,1.),(1.,1.),(1.,1.),(1.,1.),(1.,1.),(1.,
1.),(1.,1.),(1.,1.),(1.,1.),(1.,1.),(1.,1.),(1.,1.),(1.,1.),(1.,1.),(1.,
1.),(1.,1.),(1.,1.),(1.,1.),(1.,1.),(1.,1.),(1.,1.),(1.,1.),(1.,1.),(1.,
1.),(1.,1.)))
REPRESENTATION_ITEM('')
SURFACE()
);
#963=(
BOUNDED_SURFACE()
B_SPLINE_SURFACE(5,1,((#123401,#123402),(#123403,#123404),(#123405,#123406),
(#123407,#123408),(#123409,#123410),(#123411,#123412),(#123413,#123414),
(#123415,#123416),(#123417,#123418),(#123419,#123420),(#123421,#123422),
(#123423,#123424),(#123425,#123426),(#123427,#123428),(#123429,#123430),
(#123431,#123432),(#123433,#123434),(#123435,#123436),(#123437,#123438),
(#123439,#123440),(#123441,#123442),(#123443,#123444),(#123445,#123446),
(#123447,#123448),(#123449,#123450),(#123451,#123452),(#123453,#123454),
(#123455,#123456),(#123457,#123458),(#123459,#123460),(#123461,#123462),
(#123463,#123464),(#123465,#123466),(#123467,#123468),(#123469,#123470),
(#123471,#123472),(#123473,#123474),(#123475,#123476),(#123477,#123478),
(#123479,#123480),(#123481,#123482),(#123483,#123484),(#123485,#123486),
(#123487,#123488),(#123489,#123490),(#123491,#123492),(#123493,#123494),
(#123495,#123496),(#123497,#123498),(#123499,#123500),(#123501,#123502),
(#123503,#123504),(#123505,#123506),(#123507,#123508),(#123509,#123510),
(#123511,#123512),(#123513,#123514),(#123515,#123516),(#123517,#123518),
(#123519,#123520),(#123521,#123522),(#123523,#123524),(#123525,#123526),
(#123527,#123528),(#123529,#123530),(#123531,#123532),(#123533,#123534),
(#123535,#123536),(#123537,#123538),(#123539,#123540),(#123541,#123542),
(#123543,#123544),(#123545,#123546),(#123547,#123548),(#123549,#123550),
(#123551,#123552),(#123553,#123554),(#123555,#123556),(#123557,#123558),
(#123559,#123560),(#123561,#123562),(#123563,#123564),(#123565,#123566),
(#123567,#123568),(#123569,#123570),(#123571,#123572),(#123573,#123574),
(#123575,#123576),(#123577,#123578),(#123579,#123580),(#123581,#123582),
(#123583,#123584),(#123585,#123586),(#123587,#123588),(#123589,#123590),
(#123591,#123592),(#123593,#123594),(#123595,#123596),(#123597,#123598),
(#123599,#123600),(#123601,#123602),(#123603,#123604),(#123605,#123606),
(#123607,#123608),(#123609,#123610),(#123611,#123612),(#123613,#123614),
(#123615,#123616),(#123617,#123618),(#123619,#123620),(#123621,#123622),
(#123623,#123624),(#123625,#123626),(#123627,#123628),(#123629,#123630),
(#123631,#123632),(#123633,#123634),(#123635,#123636),(#123637,#123638),
(#123639,#123640),(#123641,#123642),(#123643,#123644),(#123645,#123646),
(#123647,#123648),(#123649,#123650),(#123651,#123652),(#123653,#123654),
(#123655,#123656),(#123657,#123658),(#123659,#123660),(#123661,#123662),
(#123663,#123664),(#123665,#123666),(#123667,#123668),(#123669,#123670),
(#123671,#123672),(#123673,#123674),(#123675,#123676),(#123677,#123678),
(#123679,#123680),(#123681,#123682),(#123683,#123684),(#123685,#123686),
(#123687,#123688),(#123689,#123690),(#123691,#123692),(#123693,#123694),
(#123695,#123696),(#123697,#123698),(#123699,#123700),(#123701,#123702),
(#123703,#123704),(#123705,#123706),(#123707,#123708),(#123709,#123710),
(#123711,#123712),(#123713,#123714),(#123715,#123716),(#123717,#123718),
(#123719,#123720),(#123721,#123722),(#123723,#123724),(#123725,#123726),
(#123727,#123728),(#123729,#123730),(#123731,#123732),(#123733,#123734),
(#123735,#123736),(#123737,#123738),(#123739,#123740),(#123741,#123742),
(#123743,#123744),(#123745,#123746),(#123747,#123748),(#123749,#123750),
(#123751,#123752),(#123753,#123754),(#123755,#123756),(#123757,#123758),
(#123759,#123760),(#123761,#123762),(#123763,#123764),(#123765,#123766),
(#123767,#123768),(#123769,#123770),(#123771,#123772),(#123773,#123774),
(#123775,#123776),(#123777,#123778),(#123779,#123780),(#123781,#123782),
(#123783,#123784),(#123785,#123786),(#123787,#123788),(#123789,#123790),
(#123791,#123792),(#123793,#123794),(#123795,#123796),(#123797,#123798),
(#123799,#123800),(#123801,#123802),(#123803,#123804),(#123805,#123806),
(#123807,#123808),(#123809,#123810)),.UNSPECIFIED.,.F.,.F.,.F.)
B_SPLINE_SURFACE_WITH_KNOTS((6,1,1,1,1,1,1,1,1,1,1,1,1,1,1,1,1,1,1,1,1,
1,1,1,1,1,1,1,1,1,1,1,1,1,1,1,1,1,1,1,1,1,1,1,1,1,1,1,1,1,1,1,1,1,1,1,1,
1,1,1,1,1,1,1,1,1,1,1,1,1,1,1,1,1,1,1,1,1,1,1,1,1,1,1,1,1,1,1,1,1,1,1,1,
1,1,1,1,1,1,1,1,1,1,1,1,1,1,1,1,1,1,1,1,1,1,1,1,1,1,1,1,1,1,1,1,1,1,1,1,
1,1,1,1,1,1,1,1,1,1,1,1,1,1,1,1,1,1,1,1,1,1,1,1,1,1,1,1,1,1,1,1,1,1,1,1,
1,1,1,1,1,1,1,1,1,1,1,1,1,1,1,1,1,1,1,1,1,1,1,1,1,1,1,1,1,1,1,1,1,1,1,6),
(2,2),(-1.,-0.995000000000001,-0.990000000000001,-0.985000000000001,-0.980000000000001,
-0.975000000000001,-0.970000000000001,-0.965000000000001,-0.960000000000001,
-0.955000000000001,-0.950000000000001,-0.945000000000001,-0.940000000000001,
-0.935000000000001,-0.930000000000001,-0.925000000000001,-0.920000000000001,
-0.915000000000001,-0.910000000000001,-0.905000000000001,-0.900000000000001,
-0.895000000000001,-0.890000000000001,-0.885000000000001,-0.880000000000001,
-0.875000000000001,-0.870000000000001,-0.865000000000001,-0.860000000000001,
-0.855000000000001,-0.850000000000001,-0.845000000000001,-0.840000000000001,
-0.835000000000001,-0.830000000000001,-0.825000000000001,-0.820000000000001,
-0.815000000000001,-0.810000000000001,-0.805000000000001,-0.800000000000001,
-0.795000000000001,-0.790000000000001,-0.785000000000001,-0.780000000000001,
-0.775000000000001,-0.770000000000001,-0.765000000000001,-0.760000000000001,
-0.755000000000001,-0.750000000000001,-0.745000000000001,-0.740000000000001,
-0.735000000000001,-0.730000000000001,-0.725000000000001,-0.720000000000001,
-0.715000000000001,-0.710000000000001,-0.705000000000001,-0.700000000000001,
-0.695000000000001,-0.690000000000001,-0.685,-0.68,-0.675,-0.67,-0.665,
-0.66,-0.655,-0.65,-0.645,-0.64,-0.635,-0.63,-0.625,-0.62,-0.615,-0.61,
-0.605,-0.6,-0.595,-0.59,-0.585,-0.58,-0.575,-0.57,-0.565,-0.56,-0.555,
-0.55,-0.545,-0.54,-0.535,-0.53,-0.525,-0.52,-0.515,-0.51,-0.505,-0.5,-0.495,
-0.49,-0.485,-0.48,-0.475,-0.47,-0.465,-0.46,-0.455,-0.45,-0.445,-0.44,
-0.435,-0.43,-0.425,-0.42,-0.415,-0.41,-0.405,-0.4,-0.395,-0.39,-0.385,
-0.38,-0.375,-0.37,-0.365,-0.36,-0.355,-0.35,-0.345,-0.34,-0.335,-0.33,
-0.325,-0.32,-0.315,-0.31,-0.305,-0.3,-0.295,-0.29,-0.285,-0.28,-0.275,
-0.27,-0.265,-0.26,-0.255,-0.25,-0.245,-0.24,-0.235,-0.23,-0.225,-0.22,
-0.215,-0.21,-0.205,-0.2,-0.195,-0.19,-0.185,-0.18,-0.175,-0.17,-0.165,
-0.16,-0.155,-0.15,-0.145,-0.14,-0.135,-0.13,-0.125,-0.12,-0.115,-0.11,
-0.105,-0.1,-0.095,-0.09,-0.085,-0.08,-0.075,-0.07,-0.065,-0.06,-0.055,
-0.05,-0.045,-0.04,-0.035,-0.03,-0.025,-0.02,-0.015,-0.01,-0.005,0.),(0.,
1.2),.UNSPECIFIED.)
GEOMETRIC_REPRESENTATION_ITEM()
RATIONAL_B_SPLINE_SURFACE(((1.,1.),(1.,1.),(1.,1.),(1.,1.),(1.,1.),(1.,
1.),(1.,1.),(1.,1.),(1.,1.),(1.,1.),(1.,1.),(1.,1.),(1.,1.),(1.,1.),(1.,
1.),(1.,1.),(1.,1.),(1.,1.),(1.,1.),(1.,1.),(1.,1.),(1.,1.),(1.,1.),(1.,
1.),(1.,1.),(1.,1.),(1.,1.),(1.,1.),(1.,1.),(1.,1.),(1.,1.),(1.,1.),(1.,
1.),(1.,1.),(1.,1.),(1.,1.),(1.,1.),(1.,1.),(1.,1.),(1.,1.),(1.,1.),(1.,
1.),(1.,1.),(1.,1.),(1.,1.),(1.,1.),(1.,1.),(1.,1.),(1.,1.),(1.,1.),(1.,
1.),(1.,1.),(1.,1.),(1.,1.),(1.,1.),(1.,1.),(1.,1.),(1.,1.),(1.,1.),(1.,
1.),(1.,1.),(1.,1.),(1.,1.),(1.,1.),(1.,1.),(1.,1.),(1.,1.),(1.,1.),(1.,
1.),(1.,1.),(1.,1.),(1.,1.),(1.,1.),(1.,1.),(1.,1.),(1.,1.),(1.,1.),(1.,
1.),(1.,1.),(1.,1.),(1.,1.),(1.,1.),(1.,1.),(1.,1.),(1.,1.),(1.,1.),(1.,
1.),(1.,1.),(1.,1.),(1.,1.),(1.,1.),(1.,1.),(1.,1.),(1.,1.),(1.,1.),(1.,
1.),(1.,1.),(1.,1.),(1.,1.),(1.,1.),(1.,1.),(1.,1.),(1.,1.),(1.,1.),(1.,
1.),(1.,1.),(1.,1.),(1.,1.),(1.,1.),(1.,1.),(1.,1.),(1.,1.),(1.,1.),(1.,
1.),(1.,1.),(1.,1.),(1.,1.),(1.,1.),(1.,1.),(1.,1.),(1.,1.),(1.,1.),(1.,
1.),(1.,1.),(1.,1.),(1.,1.),(1.,1.),(1.,1.),(1.,1.),(1.,1.),(1.,1.),(1.,
1.),(1.,1.),(1.,1.),(1.,1.),(1.,1.),(1.,1.),(1.,1.),(1.,1.),(1.,1.),(1.,
1.),(1.,1.),(1.,1.),(1.,1.),(1.,1.),(1.,1.),(1.,1.),(1.,1.),(1.,1.),(1.,
1.),(1.,1.),(1.,1.),(1.,1.),(1.,1.),(1.,1.),(1.,1.),(1.,1.),(1.,1.),(1.,
1.),(1.,1.),(1.,1.),(1.,1.),(1.,1.),(1.,1.),(1.,1.),(1.,1.),(1.,1.),(1.,
1.),(1.,1.),(1.,1.),(1.,1.),(1.,1.),(1.,1.),(1.,1.),(1.,1.),(1.,1.),(1.,
1.),(1.,1.),(1.,1.),(1.,1.),(1.,1.),(1.,1.),(1.,1.),(1.,1.),(1.,1.),(1.,
1.),(1.,1.),(1.,1.),(1.,1.),(1.,1.),(1.,1.),(1.,1.),(1.,1.),(1.,1.),(1.,
1.),(1.,1.),(1.,1.),(1.,1.),(1.,1.),(1.,1.),(1.,1.),(1.,1.),(1.,1.),(1.,
1.),(1.,1.)))
REPRESENTATION_ITEM('')
SURFACE()
);
#964=(
BOUNDED_SURFACE()
B_SPLINE_SURFACE(5,1,((#124202,#124203),(#124204,#124205),(#124206,#124207),
(#124208,#124209),(#124210,#124211),(#124212,#124213),(#124214,#124215),
(#124216,#124217),(#124218,#124219),(#124220,#124221),(#124222,#124223),
(#124224,#124225),(#124226,#124227),(#124228,#124229),(#124230,#124231),
(#124232,#124233),(#124234,#124235),(#124236,#124237),(#124238,#124239),
(#124240,#124241),(#124242,#124243),(#124244,#124245),(#124246,#124247),
(#124248,#124249),(#124250,#124251),(#124252,#124253),(#124254,#124255),
(#124256,#124257),(#124258,#124259),(#124260,#124261),(#124262,#124263),
(#124264,#124265),(#124266,#124267),(#124268,#124269),(#124270,#124271),
(#124272,#124273),(#124274,#124275),(#124276,#124277),(#124278,#124279),
(#124280,#124281),(#124282,#124283),(#124284,#124285),(#124286,#124287),
(#124288,#124289),(#124290,#124291),(#124292,#124293),(#124294,#124295),
(#124296,#124297),(#124298,#124299),(#124300,#124301),(#124302,#124303),
(#124304,#124305),(#124306,#124307),(#124308,#124309),(#124310,#124311),
(#124312,#124313),(#124314,#124315),(#124316,#124317),(#124318,#124319),
(#124320,#124321),(#124322,#124323),(#124324,#124325),(#124326,#124327),
(#124328,#124329),(#124330,#124331),(#124332,#124333),(#124334,#124335),
(#124336,#124337),(#124338,#124339),(#124340,#124341),(#124342,#124343),
(#124344,#124345),(#124346,#124347),(#124348,#124349),(#124350,#124351),
(#124352,#124353),(#124354,#124355),(#124356,#124357),(#124358,#124359),
(#124360,#124361),(#124362,#124363),(#124364,#124365),(#124366,#124367),
(#124368,#124369),(#124370,#124371),(#124372,#124373),(#124374,#124375),
(#124376,#124377),(#124378,#124379),(#124380,#124381),(#124382,#124383),
(#124384,#124385),(#124386,#124387),(#124388,#124389),(#124390,#124391),
(#124392,#124393),(#124394,#124395),(#124396,#124397),(#124398,#124399),
(#124400,#124401),(#124402,#124403),(#124404,#124405),(#124406,#124407),
(#124408,#124409),(#124410,#124411),(#124412,#124413),(#124414,#124415),
(#124416,#124417),(#124418,#124419),(#124420,#124421),(#124422,#124423),
(#124424,#124425),(#124426,#124427),(#124428,#124429),(#124430,#124431),
(#124432,#124433),(#124434,#124435),(#124436,#124437),(#124438,#124439),
(#124440,#124441),(#124442,#124443),(#124444,#124445),(#124446,#124447),
(#124448,#124449),(#124450,#124451),(#124452,#124453),(#124454,#124455),
(#124456,#124457),(#124458,#124459),(#124460,#124461),(#124462,#124463),
(#124464,#124465),(#124466,#124467),(#124468,#124469),(#124470,#124471),
(#124472,#124473),(#124474,#124475),(#124476,#124477),(#124478,#124479),
(#124480,#124481),(#124482,#124483),(#124484,#124485),(#124486,#124487),
(#124488,#124489),(#124490,#124491),(#124492,#124493),(#124494,#124495),
(#124496,#124497),(#124498,#124499),(#124500,#124501),(#124502,#124503),
(#124504,#124505),(#124506,#124507),(#124508,#124509),(#124510,#124511),
(#124512,#124513),(#124514,#124515),(#124516,#124517),(#124518,#124519),
(#124520,#124521),(#124522,#124523),(#124524,#124525),(#124526,#124527),
(#124528,#124529),(#124530,#124531),(#124532,#124533),(#124534,#124535),
(#124536,#124537),(#124538,#124539),(#124540,#124541),(#124542,#124543),
(#124544,#124545),(#124546,#124547),(#124548,#124549),(#124550,#124551),
(#124552,#124553),(#124554,#124555),(#124556,#124557),(#124558,#124559),
(#124560,#124561),(#124562,#124563),(#124564,#124565),(#124566,#124567),
(#124568,#124569),(#124570,#124571),(#124572,#124573),(#124574,#124575),
(#124576,#124577),(#124578,#124579),(#124580,#124581),(#124582,#124583),
(#124584,#124585),(#124586,#124587),(#124588,#124589),(#124590,#124591),
(#124592,#124593),(#124594,#124595),(#124596,#124597),(#124598,#124599),
(#124600,#124601),(#124602,#124603),(#124604,#124605),(#124606,#124607),
(#124608,#124609),(#124610,#124611)),.UNSPECIFIED.,.F.,.F.,.F.)
B_SPLINE_SURFACE_WITH_KNOTS((6,1,1,1,1,1,1,1,1,1,1,1,1,1,1,1,1,1,1,1,1,
1,1,1,1,1,1,1,1,1,1,1,1,1,1,1,1,1,1,1,1,1,1,1,1,1,1,1,1,1,1,1,1,1,1,1,1,
1,1,1,1,1,1,1,1,1,1,1,1,1,1,1,1,1,1,1,1,1,1,1,1,1,1,1,1,1,1,1,1,1,1,1,1,
1,1,1,1,1,1,1,1,1,1,1,1,1,1,1,1,1,1,1,1,1,1,1,1,1,1,1,1,1,1,1,1,1,1,1,1,
1,1,1,1,1,1,1,1,1,1,1,1,1,1,1,1,1,1,1,1,1,1,1,1,1,1,1,1,1,1,1,1,1,1,1,1,
1,1,1,1,1,1,1,1,1,1,1,1,1,1,1,1,1,1,1,1,1,1,1,1,1,1,1,1,1,1,1,1,1,1,1,6),
(2,2),(-1.,-0.995000000000001,-0.990000000000001,-0.985000000000001,-0.980000000000001,
-0.975000000000001,-0.970000000000001,-0.965000000000001,-0.960000000000001,
-0.955000000000001,-0.950000000000001,-0.945000000000001,-0.940000000000001,
-0.935000000000001,-0.930000000000001,-0.925000000000001,-0.920000000000001,
-0.915000000000001,-0.910000000000001,-0.905000000000001,-0.900000000000001,
-0.895000000000001,-0.890000000000001,-0.885000000000001,-0.880000000000001,
-0.875000000000001,-0.870000000000001,-0.865000000000001,-0.860000000000001,
-0.855000000000001,-0.850000000000001,-0.845000000000001,-0.840000000000001,
-0.835000000000001,-0.830000000000001,-0.825000000000001,-0.820000000000001,
-0.815000000000001,-0.810000000000001,-0.805000000000001,-0.800000000000001,
-0.795000000000001,-0.790000000000001,-0.785000000000001,-0.780000000000001,
-0.775000000000001,-0.770000000000001,-0.765000000000001,-0.760000000000001,
-0.755000000000001,-0.750000000000001,-0.745000000000001,-0.740000000000001,
-0.735000000000001,-0.730000000000001,-0.725000000000001,-0.720000000000001,
-0.715000000000001,-0.710000000000001,-0.705000000000001,-0.700000000000001,
-0.695000000000001,-0.690000000000001,-0.685,-0.68,-0.675,-0.67,-0.665,
-0.66,-0.655,-0.65,-0.645,-0.64,-0.635,-0.63,-0.625,-0.62,-0.615,-0.61,
-0.605,-0.6,-0.595,-0.59,-0.585,-0.58,-0.575,-0.57,-0.565,-0.56,-0.555,
-0.55,-0.545,-0.54,-0.535,-0.53,-0.525,-0.52,-0.515,-0.51,-0.505,-0.5,-0.495,
-0.49,-0.485,-0.48,-0.475,-0.47,-0.465,-0.46,-0.455,-0.45,-0.445,-0.44,
-0.435,-0.43,-0.425,-0.42,-0.415,-0.41,-0.405,-0.4,-0.395,-0.39,-0.385,
-0.38,-0.375,-0.37,-0.365,-0.36,-0.355,-0.35,-0.345,-0.34,-0.335,-0.33,
-0.325,-0.32,-0.315,-0.31,-0.305,-0.3,-0.295,-0.29,-0.285,-0.28,-0.275,
-0.27,-0.265,-0.26,-0.255,-0.25,-0.245,-0.24,-0.235,-0.23,-0.225,-0.22,
-0.215,-0.21,-0.205,-0.2,-0.195,-0.19,-0.185,-0.18,-0.175,-0.17,-0.165,
-0.16,-0.155,-0.15,-0.145,-0.14,-0.135,-0.13,-0.125,-0.12,-0.115,-0.11,
-0.105,-0.1,-0.095,-0.09,-0.085,-0.08,-0.075,-0.07,-0.065,-0.06,-0.055,
-0.05,-0.045,-0.04,-0.035,-0.03,-0.025,-0.02,-0.015,-0.01,-0.005,0.),(0.,
1.2),.UNSPECIFIED.)
GEOMETRIC_REPRESENTATION_ITEM()
RATIONAL_B_SPLINE_SURFACE(((1.,1.),(1.,1.),(1.,1.),(1.,1.),(1.,1.),(1.,
1.),(1.,1.),(1.,1.),(1.,1.),(1.,1.),(1.,1.),(1.,1.),(1.,1.),(1.,1.),(1.,
1.),(1.,1.),(1.,1.),(1.,1.),(1.,1.),(1.,1.),(1.,1.),(1.,1.),(1.,1.),(1.,
1.),(1.,1.),(1.,1.),(1.,1.),(1.,1.),(1.,1.),(1.,1.),(1.,1.),(1.,1.),(1.,
1.),(1.,1.),(1.,1.),(1.,1.),(1.,1.),(1.,1.),(1.,1.),(1.,1.),(1.,1.),(1.,
1.),(1.,1.),(1.,1.),(1.,1.),(1.,1.),(1.,1.),(1.,1.),(1.,1.),(1.,1.),(1.,
1.),(1.,1.),(1.,1.),(1.,1.),(1.,1.),(1.,1.),(1.,1.),(1.,1.),(1.,1.),(1.,
1.),(1.,1.),(1.,1.),(1.,1.),(1.,1.),(1.,1.),(1.,1.),(1.,1.),(1.,1.),(1.,
1.),(1.,1.),(1.,1.),(1.,1.),(1.,1.),(1.,1.),(1.,1.),(1.,1.),(1.,1.),(1.,
1.),(1.,1.),(1.,1.),(1.,1.),(1.,1.),(1.,1.),(1.,1.),(1.,1.),(1.,1.),(1.,
1.),(1.,1.),(1.,1.),(1.,1.),(1.,1.),(1.,1.),(1.,1.),(1.,1.),(1.,1.),(1.,
1.),(1.,1.),(1.,1.),(1.,1.),(1.,1.),(1.,1.),(1.,1.),(1.,1.),(1.,1.),(1.,
1.),(1.,1.),(1.,1.),(1.,1.),(1.,1.),(1.,1.),(1.,1.),(1.,1.),(1.,1.),(1.,
1.),(1.,1.),(1.,1.),(1.,1.),(1.,1.),(1.,1.),(1.,1.),(1.,1.),(1.,1.),(1.,
1.),(1.,1.),(1.,1.),(1.,1.),(1.,1.),(1.,1.),(1.,1.),(1.,1.),(1.,1.),(1.,
1.),(1.,1.),(1.,1.),(1.,1.),(1.,1.),(1.,1.),(1.,1.),(1.,1.),(1.,1.),(1.,
1.),(1.,1.),(1.,1.),(1.,1.),(1.,1.),(1.,1.),(1.,1.),(1.,1.),(1.,1.),(1.,
1.),(1.,1.),(1.,1.),(1.,1.),(1.,1.),(1.,1.),(1.,1.),(1.,1.),(1.,1.),(1.,
1.),(1.,1.),(1.,1.),(1.,1.),(1.,1.),(1.,1.),(1.,1.),(1.,1.),(1.,1.),(1.,
1.),(1.,1.),(1.,1.),(1.,1.),(1.,1.),(1.,1.),(1.,1.),(1.,1.),(1.,1.),(1.,
1.),(1.,1.),(1.,1.),(1.,1.),(1.,1.),(1.,1.),(1.,1.),(1.,1.),(1.,1.),(1.,
1.),(1.,1.),(1.,1.),(1.,1.),(1.,1.),(1.,1.),(1.,1.),(1.,1.),(1.,1.),(1.,
1.),(1.,1.),(1.,1.),(1.,1.),(1.,1.),(1.,1.),(1.,1.),(1.,1.),(1.,1.),(1.,
1.),(1.,1.)))
REPRESENTATION_ITEM('')
SURFACE()
);
#965=(
BOUNDED_SURFACE()
B_SPLINE_SURFACE(5,1,((#125003,#125004),(#125005,#125006),(#125007,#125008),
(#125009,#125010),(#125011,#125012),(#125013,#125014),(#125015,#125016),
(#125017,#125018),(#125019,#125020),(#125021,#125022),(#125023,#125024),
(#125025,#125026),(#125027,#125028),(#125029,#125030),(#125031,#125032),
(#125033,#125034),(#125035,#125036),(#125037,#125038),(#125039,#125040),
(#125041,#125042),(#125043,#125044),(#125045,#125046),(#125047,#125048),
(#125049,#125050),(#125051,#125052),(#125053,#125054),(#125055,#125056),
(#125057,#125058),(#125059,#125060),(#125061,#125062),(#125063,#125064),
(#125065,#125066),(#125067,#125068),(#125069,#125070),(#125071,#125072),
(#125073,#125074),(#125075,#125076),(#125077,#125078),(#125079,#125080),
(#125081,#125082),(#125083,#125084),(#125085,#125086),(#125087,#125088),
(#125089,#125090),(#125091,#125092),(#125093,#125094),(#125095,#125096),
(#125097,#125098),(#125099,#125100),(#125101,#125102),(#125103,#125104),
(#125105,#125106),(#125107,#125108),(#125109,#125110),(#125111,#125112),
(#125113,#125114),(#125115,#125116),(#125117,#125118),(#125119,#125120),
(#125121,#125122),(#125123,#125124),(#125125,#125126),(#125127,#125128),
(#125129,#125130),(#125131,#125132),(#125133,#125134),(#125135,#125136),
(#125137,#125138),(#125139,#125140),(#125141,#125142),(#125143,#125144),
(#125145,#125146),(#125147,#125148),(#125149,#125150),(#125151,#125152),
(#125153,#125154),(#125155,#125156),(#125157,#125158),(#125159,#125160),
(#125161,#125162),(#125163,#125164),(#125165,#125166),(#125167,#125168),
(#125169,#125170),(#125171,#125172),(#125173,#125174),(#125175,#125176),
(#125177,#125178),(#125179,#125180),(#125181,#125182),(#125183,#125184),
(#125185,#125186),(#125187,#125188),(#125189,#125190),(#125191,#125192),
(#125193,#125194),(#125195,#125196),(#125197,#125198),(#125199,#125200),
(#125201,#125202),(#125203,#125204),(#125205,#125206),(#125207,#125208),
(#125209,#125210),(#125211,#125212),(#125213,#125214),(#125215,#125216),
(#125217,#125218),(#125219,#125220),(#125221,#125222),(#125223,#125224),
(#125225,#125226),(#125227,#125228),(#125229,#125230),(#125231,#125232),
(#125233,#125234),(#125235,#125236),(#125237,#125238),(#125239,#125240),
(#125241,#125242),(#125243,#125244),(#125245,#125246),(#125247,#125248),
(#125249,#125250),(#125251,#125252),(#125253,#125254),(#125255,#125256),
(#125257,#125258),(#125259,#125260),(#125261,#125262),(#125263,#125264),
(#125265,#125266),(#125267,#125268),(#125269,#125270),(#125271,#125272),
(#125273,#125274),(#125275,#125276),(#125277,#125278),(#125279,#125280),
(#125281,#125282),(#125283,#125284),(#125285,#125286),(#125287,#125288),
(#125289,#125290),(#125291,#125292),(#125293,#125294),(#125295,#125296),
(#125297,#125298),(#125299,#125300),(#125301,#125302),(#125303,#125304),
(#125305,#125306),(#125307,#125308),(#125309,#125310),(#125311,#125312),
(#125313,#125314),(#125315,#125316),(#125317,#125318),(#125319,#125320),
(#125321,#125322),(#125323,#125324),(#125325,#125326),(#125327,#125328),
(#125329,#125330),(#125331,#125332),(#125333,#125334),(#125335,#125336),
(#125337,#125338),(#125339,#125340),(#125341,#125342),(#125343,#125344),
(#125345,#125346),(#125347,#125348),(#125349,#125350),(#125351,#125352),
(#125353,#125354),(#125355,#125356),(#125357,#125358),(#125359,#125360),
(#125361,#125362),(#125363,#125364),(#125365,#125366),(#125367,#125368),
(#125369,#125370),(#125371,#125372),(#125373,#125374),(#125375,#125376),
(#125377,#125378),(#125379,#125380),(#125381,#125382),(#125383,#125384),
(#125385,#125386),(#125387,#125388),(#125389,#125390),(#125391,#125392),
(#125393,#125394),(#125395,#125396),(#125397,#125398),(#125399,#125400),
(#125401,#125402),(#125403,#125404),(#125405,#125406),(#125407,#125408),
(#125409,#125410),(#125411,#125412)),.UNSPECIFIED.,.F.,.F.,.F.)
B_SPLINE_SURFACE_WITH_KNOTS((6,1,1,1,1,1,1,1,1,1,1,1,1,1,1,1,1,1,1,1,1,
1,1,1,1,1,1,1,1,1,1,1,1,1,1,1,1,1,1,1,1,1,1,1,1,1,1,1,1,1,1,1,1,1,1,1,1,
1,1,1,1,1,1,1,1,1,1,1,1,1,1,1,1,1,1,1,1,1,1,1,1,1,1,1,1,1,1,1,1,1,1,1,1,
1,1,1,1,1,1,1,1,1,1,1,1,1,1,1,1,1,1,1,1,1,1,1,1,1,1,1,1,1,1,1,1,1,1,1,1,
1,1,1,1,1,1,1,1,1,1,1,1,1,1,1,1,1,1,1,1,1,1,1,1,1,1,1,1,1,1,1,1,1,1,1,1,
1,1,1,1,1,1,1,1,1,1,1,1,1,1,1,1,1,1,1,1,1,1,1,1,1,1,1,1,1,1,1,1,1,1,1,6),
(2,2),(-1.,-0.995000000000001,-0.990000000000001,-0.985000000000001,-0.980000000000001,
-0.975000000000001,-0.970000000000001,-0.965000000000001,-0.960000000000001,
-0.955000000000001,-0.950000000000001,-0.945000000000001,-0.940000000000001,
-0.935000000000001,-0.930000000000001,-0.925000000000001,-0.920000000000001,
-0.915000000000001,-0.910000000000001,-0.905000000000001,-0.900000000000001,
-0.895000000000001,-0.890000000000001,-0.885000000000001,-0.880000000000001,
-0.875000000000001,-0.870000000000001,-0.865000000000001,-0.860000000000001,
-0.855000000000001,-0.850000000000001,-0.845000000000001,-0.840000000000001,
-0.835000000000001,-0.830000000000001,-0.825000000000001,-0.820000000000001,
-0.815000000000001,-0.810000000000001,-0.805000000000001,-0.800000000000001,
-0.795000000000001,-0.790000000000001,-0.785000000000001,-0.780000000000001,
-0.775000000000001,-0.770000000000001,-0.765000000000001,-0.760000000000001,
-0.755000000000001,-0.750000000000001,-0.745000000000001,-0.740000000000001,
-0.735000000000001,-0.730000000000001,-0.725000000000001,-0.720000000000001,
-0.715000000000001,-0.710000000000001,-0.705000000000001,-0.700000000000001,
-0.695000000000001,-0.690000000000001,-0.685,-0.68,-0.675,-0.67,-0.665,
-0.66,-0.655,-0.65,-0.645,-0.64,-0.635,-0.63,-0.625,-0.62,-0.615,-0.61,
-0.605,-0.6,-0.595,-0.59,-0.585,-0.58,-0.575,-0.57,-0.565,-0.56,-0.555,
-0.55,-0.545,-0.54,-0.535,-0.53,-0.525,-0.52,-0.515,-0.51,-0.505,-0.5,-0.495,
-0.49,-0.485,-0.48,-0.475,-0.47,-0.465,-0.46,-0.455,-0.45,-0.445,-0.44,
-0.435,-0.43,-0.425,-0.42,-0.415,-0.41,-0.405,-0.4,-0.395,-0.39,-0.385,
-0.38,-0.375,-0.37,-0.365,-0.36,-0.355,-0.35,-0.345,-0.34,-0.335,-0.33,
-0.325,-0.32,-0.315,-0.31,-0.305,-0.3,-0.295,-0.29,-0.285,-0.28,-0.275,
-0.27,-0.265,-0.26,-0.255,-0.25,-0.245,-0.24,-0.235,-0.23,-0.225,-0.22,
-0.215,-0.21,-0.205,-0.2,-0.195,-0.19,-0.185,-0.18,-0.175,-0.17,-0.165,
-0.16,-0.155,-0.15,-0.145,-0.14,-0.135,-0.13,-0.125,-0.12,-0.115,-0.11,
-0.105,-0.1,-0.095,-0.09,-0.085,-0.08,-0.075,-0.07,-0.065,-0.06,-0.055,
-0.05,-0.045,-0.04,-0.035,-0.03,-0.025,-0.02,-0.015,-0.01,-0.005,0.),(0.,
1.2),.UNSPECIFIED.)
GEOMETRIC_REPRESENTATION_ITEM()
RATIONAL_B_SPLINE_SURFACE(((1.,1.),(1.,1.),(1.,1.),(1.,1.),(1.,1.),(1.,
1.),(1.,1.),(1.,1.),(1.,1.),(1.,1.),(1.,1.),(1.,1.),(1.,1.),(1.,1.),(1.,
1.),(1.,1.),(1.,1.),(1.,1.),(1.,1.),(1.,1.),(1.,1.),(1.,1.),(1.,1.),(1.,
1.),(1.,1.),(1.,1.),(1.,1.),(1.,1.),(1.,1.),(1.,1.),(1.,1.),(1.,1.),(1.,
1.),(1.,1.),(1.,1.),(1.,1.),(1.,1.),(1.,1.),(1.,1.),(1.,1.),(1.,1.),(1.,
1.),(1.,1.),(1.,1.),(1.,1.),(1.,1.),(1.,1.),(1.,1.),(1.,1.),(1.,1.),(1.,
1.),(1.,1.),(1.,1.),(1.,1.),(1.,1.),(1.,1.),(1.,1.),(1.,1.),(1.,1.),(1.,
1.),(1.,1.),(1.,1.),(1.,1.),(1.,1.),(1.,1.),(1.,1.),(1.,1.),(1.,1.),(1.,
1.),(1.,1.),(1.,1.),(1.,1.),(1.,1.),(1.,1.),(1.,1.),(1.,1.),(1.,1.),(1.,
1.),(1.,1.),(1.,1.),(1.,1.),(1.,1.),(1.,1.),(1.,1.),(1.,1.),(1.,1.),(1.,
1.),(1.,1.),(1.,1.),(1.,1.),(1.,1.),(1.,1.),(1.,1.),(1.,1.),(1.,1.),(1.,
1.),(1.,1.),(1.,1.),(1.,1.),(1.,1.),(1.,1.),(1.,1.),(1.,1.),(1.,1.),(1.,
1.),(1.,1.),(1.,1.),(1.,1.),(1.,1.),(1.,1.),(1.,1.),(1.,1.),(1.,1.),(1.,
1.),(1.,1.),(1.,1.),(1.,1.),(1.,1.),(1.,1.),(1.,1.),(1.,1.),(1.,1.),(1.,
1.),(1.,1.),(1.,1.),(1.,1.),(1.,1.),(1.,1.),(1.,1.),(1.,1.),(1.,1.),(1.,
1.),(1.,1.),(1.,1.),(1.,1.),(1.,1.),(1.,1.),(1.,1.),(1.,1.),(1.,1.),(1.,
1.),(1.,1.),(1.,1.),(1.,1.),(1.,1.),(1.,1.),(1.,1.),(1.,1.),(1.,1.),(1.,
1.),(1.,1.),(1.,1.),(1.,1.),(1.,1.),(1.,1.),(1.,1.),(1.,1.),(1.,1.),(1.,
1.),(1.,1.),(1.,1.),(1.,1.),(1.,1.),(1.,1.),(1.,1.),(1.,1.),(1.,1.),(1.,
1.),(1.,1.),(1.,1.),(1.,1.),(1.,1.),(1.,1.),(1.,1.),(1.,1.),(1.,1.),(1.,
1.),(1.,1.),(1.,1.),(1.,1.),(1.,1.),(1.,1.),(1.,1.),(1.,1.),(1.,1.),(1.,
1.),(1.,1.),(1.,1.),(1.,1.),(1.,1.),(1.,1.),(1.,1.),(1.,1.),(1.,1.),(1.,
1.),(1.,1.),(1.,1.),(1.,1.),(1.,1.),(1.,1.),(1.,1.),(1.,1.),(1.,1.),(1.,
1.),(1.,1.)))
REPRESENTATION_ITEM('')
SURFACE()
);
#966=(
BOUNDED_SURFACE()
B_SPLINE_SURFACE(5,1,((#125804,#125805),(#125806,#125807),(#125808,#125809),
(#125810,#125811),(#125812,#125813),(#125814,#125815),(#125816,#125817),
(#125818,#125819),(#125820,#125821),(#125822,#125823),(#125824,#125825),
(#125826,#125827),(#125828,#125829),(#125830,#125831),(#125832,#125833),
(#125834,#125835),(#125836,#125837),(#125838,#125839),(#125840,#125841),
(#125842,#125843),(#125844,#125845),(#125846,#125847),(#125848,#125849),
(#125850,#125851),(#125852,#125853),(#125854,#125855),(#125856,#125857),
(#125858,#125859),(#125860,#125861),(#125862,#125863),(#125864,#125865),
(#125866,#125867),(#125868,#125869),(#125870,#125871),(#125872,#125873),
(#125874,#125875),(#125876,#125877),(#125878,#125879),(#125880,#125881),
(#125882,#125883),(#125884,#125885),(#125886,#125887),(#125888,#125889),
(#125890,#125891),(#125892,#125893),(#125894,#125895),(#125896,#125897),
(#125898,#125899),(#125900,#125901),(#125902,#125903),(#125904,#125905),
(#125906,#125907),(#125908,#125909),(#125910,#125911),(#125912,#125913),
(#125914,#125915),(#125916,#125917),(#125918,#125919),(#125920,#125921),
(#125922,#125923),(#125924,#125925),(#125926,#125927),(#125928,#125929),
(#125930,#125931),(#125932,#125933),(#125934,#125935),(#125936,#125937),
(#125938,#125939),(#125940,#125941),(#125942,#125943),(#125944,#125945),
(#125946,#125947),(#125948,#125949),(#125950,#125951),(#125952,#125953),
(#125954,#125955),(#125956,#125957),(#125958,#125959),(#125960,#125961),
(#125962,#125963),(#125964,#125965),(#125966,#125967),(#125968,#125969),
(#125970,#125971),(#125972,#125973),(#125974,#125975),(#125976,#125977),
(#125978,#125979),(#125980,#125981),(#125982,#125983),(#125984,#125985),
(#125986,#125987),(#125988,#125989),(#125990,#125991),(#125992,#125993),
(#125994,#125995),(#125996,#125997),(#125998,#125999),(#126000,#126001),
(#126002,#126003),(#126004,#126005),(#126006,#126007),(#126008,#126009),
(#126010,#126011),(#126012,#126013),(#126014,#126015),(#126016,#126017),
(#126018,#126019),(#126020,#126021),(#126022,#126023),(#126024,#126025),
(#126026,#126027),(#126028,#126029),(#126030,#126031),(#126032,#126033),
(#126034,#126035),(#126036,#126037),(#126038,#126039),(#126040,#126041),
(#126042,#126043),(#126044,#126045),(#126046,#126047),(#126048,#126049),
(#126050,#126051),(#126052,#126053),(#126054,#126055),(#126056,#126057),
(#126058,#126059),(#126060,#126061),(#126062,#126063),(#126064,#126065),
(#126066,#126067),(#126068,#126069),(#126070,#126071),(#126072,#126073),
(#126074,#126075),(#126076,#126077),(#126078,#126079),(#126080,#126081),
(#126082,#126083),(#126084,#126085),(#126086,#126087),(#126088,#126089),
(#126090,#126091),(#126092,#126093),(#126094,#126095),(#126096,#126097),
(#126098,#126099),(#126100,#126101),(#126102,#126103),(#126104,#126105),
(#126106,#126107),(#126108,#126109),(#126110,#126111),(#126112,#126113),
(#126114,#126115),(#126116,#126117),(#126118,#126119),(#126120,#126121),
(#126122,#126123),(#126124,#126125),(#126126,#126127),(#126128,#126129),
(#126130,#126131),(#126132,#126133),(#126134,#126135),(#126136,#126137),
(#126138,#126139),(#126140,#126141),(#126142,#126143),(#126144,#126145),
(#126146,#126147),(#126148,#126149),(#126150,#126151),(#126152,#126153),
(#126154,#126155),(#126156,#126157),(#126158,#126159),(#126160,#126161),
(#126162,#126163),(#126164,#126165),(#126166,#126167),(#126168,#126169),
(#126170,#126171),(#126172,#126173),(#126174,#126175),(#126176,#126177),
(#126178,#126179),(#126180,#126181),(#126182,#126183),(#126184,#126185),
(#126186,#126187),(#126188,#126189),(#126190,#126191),(#126192,#126193),
(#126194,#126195),(#126196,#126197),(#126198,#126199),(#126200,#126201),
(#126202,#126203),(#126204,#126205),(#126206,#126207),(#126208,#126209),
(#126210,#126211),(#126212,#126213)),.UNSPECIFIED.,.F.,.F.,.F.)
B_SPLINE_SURFACE_WITH_KNOTS((6,1,1,1,1,1,1,1,1,1,1,1,1,1,1,1,1,1,1,1,1,
1,1,1,1,1,1,1,1,1,1,1,1,1,1,1,1,1,1,1,1,1,1,1,1,1,1,1,1,1,1,1,1,1,1,1,1,
1,1,1,1,1,1,1,1,1,1,1,1,1,1,1,1,1,1,1,1,1,1,1,1,1,1,1,1,1,1,1,1,1,1,1,1,
1,1,1,1,1,1,1,1,1,1,1,1,1,1,1,1,1,1,1,1,1,1,1,1,1,1,1,1,1,1,1,1,1,1,1,1,
1,1,1,1,1,1,1,1,1,1,1,1,1,1,1,1,1,1,1,1,1,1,1,1,1,1,1,1,1,1,1,1,1,1,1,1,
1,1,1,1,1,1,1,1,1,1,1,1,1,1,1,1,1,1,1,1,1,1,1,1,1,1,1,1,1,1,1,1,1,1,1,6),
(2,2),(-1.,-0.995000000000001,-0.990000000000001,-0.985000000000001,-0.980000000000001,
-0.975000000000001,-0.970000000000001,-0.965000000000001,-0.960000000000001,
-0.955000000000001,-0.950000000000001,-0.945000000000001,-0.940000000000001,
-0.935000000000001,-0.930000000000001,-0.925000000000001,-0.920000000000001,
-0.915000000000001,-0.910000000000001,-0.905000000000001,-0.900000000000001,
-0.895000000000001,-0.890000000000001,-0.885000000000001,-0.880000000000001,
-0.875000000000001,-0.870000000000001,-0.865000000000001,-0.860000000000001,
-0.855000000000001,-0.850000000000001,-0.845000000000001,-0.840000000000001,
-0.835000000000001,-0.830000000000001,-0.825000000000001,-0.820000000000001,
-0.815000000000001,-0.810000000000001,-0.805000000000001,-0.800000000000001,
-0.795000000000001,-0.790000000000001,-0.785000000000001,-0.780000000000001,
-0.775000000000001,-0.770000000000001,-0.765000000000001,-0.760000000000001,
-0.755000000000001,-0.750000000000001,-0.745000000000001,-0.740000000000001,
-0.735000000000001,-0.730000000000001,-0.725000000000001,-0.720000000000001,
-0.715000000000001,-0.710000000000001,-0.705000000000001,-0.700000000000001,
-0.695000000000001,-0.690000000000001,-0.685,-0.68,-0.675,-0.67,-0.665,
-0.66,-0.655,-0.65,-0.645,-0.64,-0.635,-0.63,-0.625,-0.62,-0.615,-0.61,
-0.605,-0.6,-0.595,-0.59,-0.585,-0.58,-0.575,-0.57,-0.565,-0.56,-0.555,
-0.55,-0.545,-0.54,-0.535,-0.53,-0.525,-0.52,-0.515,-0.51,-0.505,-0.5,-0.495,
-0.49,-0.485,-0.48,-0.475,-0.47,-0.465,-0.46,-0.455,-0.45,-0.445,-0.44,
-0.435,-0.43,-0.425,-0.42,-0.415,-0.41,-0.405,-0.4,-0.395,-0.39,-0.385,
-0.38,-0.375,-0.37,-0.365,-0.36,-0.355,-0.35,-0.345,-0.34,-0.335,-0.33,
-0.325,-0.32,-0.315,-0.31,-0.305,-0.3,-0.295,-0.29,-0.285,-0.28,-0.275,
-0.27,-0.265,-0.26,-0.255,-0.25,-0.245,-0.24,-0.235,-0.23,-0.225,-0.22,
-0.215,-0.21,-0.205,-0.2,-0.195,-0.19,-0.185,-0.18,-0.175,-0.17,-0.165,
-0.16,-0.155,-0.15,-0.145,-0.14,-0.135,-0.13,-0.125,-0.12,-0.115,-0.11,
-0.105,-0.1,-0.095,-0.09,-0.085,-0.08,-0.075,-0.07,-0.065,-0.06,-0.055,
-0.05,-0.045,-0.04,-0.035,-0.03,-0.025,-0.02,-0.015,-0.01,-0.005,0.),(0.,
1.2),.UNSPECIFIED.)
GEOMETRIC_REPRESENTATION_ITEM()
RATIONAL_B_SPLINE_SURFACE(((1.,1.),(1.,1.),(1.,1.),(1.,1.),(1.,1.),(1.,
1.),(1.,1.),(1.,1.),(1.,1.),(1.,1.),(1.,1.),(1.,1.),(1.,1.),(1.,1.),(1.,
1.),(1.,1.),(1.,1.),(1.,1.),(1.,1.),(1.,1.),(1.,1.),(1.,1.),(1.,1.),(1.,
1.),(1.,1.),(1.,1.),(1.,1.),(1.,1.),(1.,1.),(1.,1.),(1.,1.),(1.,1.),(1.,
1.),(1.,1.),(1.,1.),(1.,1.),(1.,1.),(1.,1.),(1.,1.),(1.,1.),(1.,1.),(1.,
1.),(1.,1.),(1.,1.),(1.,1.),(1.,1.),(1.,1.),(1.,1.),(1.,1.),(1.,1.),(1.,
1.),(1.,1.),(1.,1.),(1.,1.),(1.,1.),(1.,1.),(1.,1.),(1.,1.),(1.,1.),(1.,
1.),(1.,1.),(1.,1.),(1.,1.),(1.,1.),(1.,1.),(1.,1.),(1.,1.),(1.,1.),(1.,
1.),(1.,1.),(1.,1.),(1.,1.),(1.,1.),(1.,1.),(1.,1.),(1.,1.),(1.,1.),(1.,
1.),(1.,1.),(1.,1.),(1.,1.),(1.,1.),(1.,1.),(1.,1.),(1.,1.),(1.,1.),(1.,
1.),(1.,1.),(1.,1.),(1.,1.),(1.,1.),(1.,1.),(1.,1.),(1.,1.),(1.,1.),(1.,
1.),(1.,1.),(1.,1.),(1.,1.),(1.,1.),(1.,1.),(1.,1.),(1.,1.),(1.,1.),(1.,
1.),(1.,1.),(1.,1.),(1.,1.),(1.,1.),(1.,1.),(1.,1.),(1.,1.),(1.,1.),(1.,
1.),(1.,1.),(1.,1.),(1.,1.),(1.,1.),(1.,1.),(1.,1.),(1.,1.),(1.,1.),(1.,
1.),(1.,1.),(1.,1.),(1.,1.),(1.,1.),(1.,1.),(1.,1.),(1.,1.),(1.,1.),(1.,
1.),(1.,1.),(1.,1.),(1.,1.),(1.,1.),(1.,1.),(1.,1.),(1.,1.),(1.,1.),(1.,
1.),(1.,1.),(1.,1.),(1.,1.),(1.,1.),(1.,1.),(1.,1.),(1.,1.),(1.,1.),(1.,
1.),(1.,1.),(1.,1.),(1.,1.),(1.,1.),(1.,1.),(1.,1.),(1.,1.),(1.,1.),(1.,
1.),(1.,1.),(1.,1.),(1.,1.),(1.,1.),(1.,1.),(1.,1.),(1.,1.),(1.,1.),(1.,
1.),(1.,1.),(1.,1.),(1.,1.),(1.,1.),(1.,1.),(1.,1.),(1.,1.),(1.,1.),(1.,
1.),(1.,1.),(1.,1.),(1.,1.),(1.,1.),(1.,1.),(1.,1.),(1.,1.),(1.,1.),(1.,
1.),(1.,1.),(1.,1.),(1.,1.),(1.,1.),(1.,1.),(1.,1.),(1.,1.),(1.,1.),(1.,
1.),(1.,1.),(1.,1.),(1.,1.),(1.,1.),(1.,1.),(1.,1.),(1.,1.),(1.,1.),(1.,
1.),(1.,1.)))
REPRESENTATION_ITEM('')
SURFACE()
);
#967=(
BOUNDED_SURFACE()
B_SPLINE_SURFACE(5,1,((#126605,#126606),(#126607,#126608),(#126609,#126610),
(#126611,#126612),(#126613,#126614),(#126615,#126616),(#126617,#126618),
(#126619,#126620),(#126621,#126622),(#126623,#126624),(#126625,#126626),
(#126627,#126628),(#126629,#126630),(#126631,#126632),(#126633,#126634),
(#126635,#126636),(#126637,#126638),(#126639,#126640),(#126641,#126642),
(#126643,#126644),(#126645,#126646),(#126647,#126648),(#126649,#126650),
(#126651,#126652),(#126653,#126654),(#126655,#126656),(#126657,#126658),
(#126659,#126660),(#126661,#126662),(#126663,#126664),(#126665,#126666),
(#126667,#126668),(#126669,#126670),(#126671,#126672),(#126673,#126674),
(#126675,#126676),(#126677,#126678),(#126679,#126680),(#126681,#126682),
(#126683,#126684),(#126685,#126686),(#126687,#126688),(#126689,#126690),
(#126691,#126692),(#126693,#126694),(#126695,#126696),(#126697,#126698),
(#126699,#126700),(#126701,#126702),(#126703,#126704),(#126705,#126706),
(#126707,#126708),(#126709,#126710),(#126711,#126712),(#126713,#126714),
(#126715,#126716),(#126717,#126718),(#126719,#126720),(#126721,#126722),
(#126723,#126724),(#126725,#126726),(#126727,#126728),(#126729,#126730),
(#126731,#126732),(#126733,#126734),(#126735,#126736),(#126737,#126738),
(#126739,#126740),(#126741,#126742),(#126743,#126744),(#126745,#126746),
(#126747,#126748),(#126749,#126750),(#126751,#126752),(#126753,#126754),
(#126755,#126756),(#126757,#126758),(#126759,#126760),(#126761,#126762),
(#126763,#126764),(#126765,#126766),(#126767,#126768),(#126769,#126770),
(#126771,#126772),(#126773,#126774),(#126775,#126776),(#126777,#126778),
(#126779,#126780),(#126781,#126782),(#126783,#126784),(#126785,#126786),
(#126787,#126788),(#126789,#126790),(#126791,#126792),(#126793,#126794),
(#126795,#126796),(#126797,#126798),(#126799,#126800),(#126801,#126802),
(#126803,#126804),(#126805,#126806),(#126807,#126808),(#126809,#126810),
(#126811,#126812),(#126813,#126814),(#126815,#126816),(#126817,#126818),
(#126819,#126820),(#126821,#126822),(#126823,#126824),(#126825,#126826),
(#126827,#126828),(#126829,#126830),(#126831,#126832),(#126833,#126834),
(#126835,#126836),(#126837,#126838),(#126839,#126840),(#126841,#126842),
(#126843,#126844),(#126845,#126846),(#126847,#126848),(#126849,#126850),
(#126851,#126852),(#126853,#126854),(#126855,#126856),(#126857,#126858),
(#126859,#126860),(#126861,#126862),(#126863,#126864),(#126865,#126866),
(#126867,#126868),(#126869,#126870),(#126871,#126872),(#126873,#126874),
(#126875,#126876),(#126877,#126878),(#126879,#126880),(#126881,#126882),
(#126883,#126884),(#126885,#126886),(#126887,#126888),(#126889,#126890),
(#126891,#126892),(#126893,#126894),(#126895,#126896),(#126897,#126898),
(#126899,#126900),(#126901,#126902),(#126903,#126904),(#126905,#126906),
(#126907,#126908),(#126909,#126910),(#126911,#126912),(#126913,#126914),
(#126915,#126916),(#126917,#126918),(#126919,#126920),(#126921,#126922),
(#126923,#126924),(#126925,#126926),(#126927,#126928),(#126929,#126930),
(#126931,#126932),(#126933,#126934),(#126935,#126936),(#126937,#126938),
(#126939,#126940),(#126941,#126942),(#126943,#126944),(#126945,#126946),
(#126947,#126948),(#126949,#126950),(#126951,#126952),(#126953,#126954),
(#126955,#126956),(#126957,#126958),(#126959,#126960),(#126961,#126962),
(#126963,#126964),(#126965,#126966),(#126967,#126968),(#126969,#126970),
(#126971,#126972),(#126973,#126974),(#126975,#126976),(#126977,#126978),
(#126979,#126980),(#126981,#126982),(#126983,#126984),(#126985,#126986),
(#126987,#126988),(#126989,#126990),(#126991,#126992),(#126993,#126994),
(#126995,#126996),(#126997,#126998),(#126999,#127000),(#127001,#127002),
(#127003,#127004),(#127005,#127006),(#127007,#127008),(#127009,#127010),
(#127011,#127012),(#127013,#127014)),.UNSPECIFIED.,.F.,.F.,.F.)
B_SPLINE_SURFACE_WITH_KNOTS((6,1,1,1,1,1,1,1,1,1,1,1,1,1,1,1,1,1,1,1,1,
1,1,1,1,1,1,1,1,1,1,1,1,1,1,1,1,1,1,1,1,1,1,1,1,1,1,1,1,1,1,1,1,1,1,1,1,
1,1,1,1,1,1,1,1,1,1,1,1,1,1,1,1,1,1,1,1,1,1,1,1,1,1,1,1,1,1,1,1,1,1,1,1,
1,1,1,1,1,1,1,1,1,1,1,1,1,1,1,1,1,1,1,1,1,1,1,1,1,1,1,1,1,1,1,1,1,1,1,1,
1,1,1,1,1,1,1,1,1,1,1,1,1,1,1,1,1,1,1,1,1,1,1,1,1,1,1,1,1,1,1,1,1,1,1,1,
1,1,1,1,1,1,1,1,1,1,1,1,1,1,1,1,1,1,1,1,1,1,1,1,1,1,1,1,1,1,1,1,1,1,1,6),
(2,2),(-1.,-0.995000000000001,-0.990000000000001,-0.985000000000001,-0.980000000000001,
-0.975000000000001,-0.970000000000001,-0.965000000000001,-0.960000000000001,
-0.955000000000001,-0.950000000000001,-0.945000000000001,-0.940000000000001,
-0.935000000000001,-0.930000000000001,-0.925000000000001,-0.920000000000001,
-0.915000000000001,-0.910000000000001,-0.905000000000001,-0.900000000000001,
-0.895000000000001,-0.890000000000001,-0.885000000000001,-0.880000000000001,
-0.875000000000001,-0.870000000000001,-0.865000000000001,-0.860000000000001,
-0.855000000000001,-0.850000000000001,-0.845000000000001,-0.840000000000001,
-0.835000000000001,-0.830000000000001,-0.825000000000001,-0.820000000000001,
-0.815000000000001,-0.810000000000001,-0.805000000000001,-0.800000000000001,
-0.795000000000001,-0.790000000000001,-0.785000000000001,-0.780000000000001,
-0.775000000000001,-0.770000000000001,-0.765000000000001,-0.760000000000001,
-0.755000000000001,-0.750000000000001,-0.745000000000001,-0.740000000000001,
-0.735000000000001,-0.730000000000001,-0.725000000000001,-0.720000000000001,
-0.715000000000001,-0.710000000000001,-0.705000000000001,-0.700000000000001,
-0.695000000000001,-0.690000000000001,-0.685,-0.68,-0.675,-0.67,-0.665,
-0.66,-0.655,-0.65,-0.645,-0.64,-0.635,-0.63,-0.625,-0.62,-0.615,-0.61,
-0.605,-0.6,-0.595,-0.59,-0.585,-0.58,-0.575,-0.57,-0.565,-0.56,-0.555,
-0.55,-0.545,-0.54,-0.535,-0.53,-0.525,-0.52,-0.515,-0.51,-0.505,-0.5,-0.495,
-0.49,-0.485,-0.48,-0.475,-0.47,-0.465,-0.46,-0.455,-0.45,-0.445,-0.44,
-0.435,-0.43,-0.425,-0.42,-0.415,-0.41,-0.405,-0.4,-0.395,-0.39,-0.385,
-0.38,-0.375,-0.37,-0.365,-0.36,-0.355,-0.35,-0.345,-0.34,-0.335,-0.33,
-0.325,-0.32,-0.315,-0.31,-0.305,-0.3,-0.295,-0.29,-0.285,-0.28,-0.275,
-0.27,-0.265,-0.26,-0.255,-0.25,-0.245,-0.24,-0.235,-0.23,-0.225,-0.22,
-0.215,-0.21,-0.205,-0.2,-0.195,-0.19,-0.185,-0.18,-0.175,-0.17,-0.165,
-0.16,-0.155,-0.15,-0.145,-0.14,-0.135,-0.13,-0.125,-0.12,-0.115,-0.11,
-0.105,-0.1,-0.095,-0.09,-0.085,-0.08,-0.075,-0.07,-0.065,-0.06,-0.055,
-0.05,-0.045,-0.04,-0.035,-0.03,-0.025,-0.02,-0.015,-0.01,-0.005,0.),(0.,
1.2),.UNSPECIFIED.)
GEOMETRIC_REPRESENTATION_ITEM()
RATIONAL_B_SPLINE_SURFACE(((1.,1.),(1.,1.),(1.,1.),(1.,1.),(1.,1.),(1.,
1.),(1.,1.),(1.,1.),(1.,1.),(1.,1.),(1.,1.),(1.,1.),(1.,1.),(1.,1.),(1.,
1.),(1.,1.),(1.,1.),(1.,1.),(1.,1.),(1.,1.),(1.,1.),(1.,1.),(1.,1.),(1.,
1.),(1.,1.),(1.,1.),(1.,1.),(1.,1.),(1.,1.),(1.,1.),(1.,1.),(1.,1.),(1.,
1.),(1.,1.),(1.,1.),(1.,1.),(1.,1.),(1.,1.),(1.,1.),(1.,1.),(1.,1.),(1.,
1.),(1.,1.),(1.,1.),(1.,1.),(1.,1.),(1.,1.),(1.,1.),(1.,1.),(1.,1.),(1.,
1.),(1.,1.),(1.,1.),(1.,1.),(1.,1.),(1.,1.),(1.,1.),(1.,1.),(1.,1.),(1.,
1.),(1.,1.),(1.,1.),(1.,1.),(1.,1.),(1.,1.),(1.,1.),(1.,1.),(1.,1.),(1.,
1.),(1.,1.),(1.,1.),(1.,1.),(1.,1.),(1.,1.),(1.,1.),(1.,1.),(1.,1.),(1.,
1.),(1.,1.),(1.,1.),(1.,1.),(1.,1.),(1.,1.),(1.,1.),(1.,1.),(1.,1.),(1.,
1.),(1.,1.),(1.,1.),(1.,1.),(1.,1.),(1.,1.),(1.,1.),(1.,1.),(1.,1.),(1.,
1.),(1.,1.),(1.,1.),(1.,1.),(1.,1.),(1.,1.),(1.,1.),(1.,1.),(1.,1.),(1.,
1.),(1.,1.),(1.,1.),(1.,1.),(1.,1.),(1.,1.),(1.,1.),(1.,1.),(1.,1.),(1.,
1.),(1.,1.),(1.,1.),(1.,1.),(1.,1.),(1.,1.),(1.,1.),(1.,1.),(1.,1.),(1.,
1.),(1.,1.),(1.,1.),(1.,1.),(1.,1.),(1.,1.),(1.,1.),(1.,1.),(1.,1.),(1.,
1.),(1.,1.),(1.,1.),(1.,1.),(1.,1.),(1.,1.),(1.,1.),(1.,1.),(1.,1.),(1.,
1.),(1.,1.),(1.,1.),(1.,1.),(1.,1.),(1.,1.),(1.,1.),(1.,1.),(1.,1.),(1.,
1.),(1.,1.),(1.,1.),(1.,1.),(1.,1.),(1.,1.),(1.,1.),(1.,1.),(1.,1.),(1.,
1.),(1.,1.),(1.,1.),(1.,1.),(1.,1.),(1.,1.),(1.,1.),(1.,1.),(1.,1.),(1.,
1.),(1.,1.),(1.,1.),(1.,1.),(1.,1.),(1.,1.),(1.,1.),(1.,1.),(1.,1.),(1.,
1.),(1.,1.),(1.,1.),(1.,1.),(1.,1.),(1.,1.),(1.,1.),(1.,1.),(1.,1.),(1.,
1.),(1.,1.),(1.,1.),(1.,1.),(1.,1.),(1.,1.),(1.,1.),(1.,1.),(1.,1.),(1.,
1.),(1.,1.),(1.,1.),(1.,1.),(1.,1.),(1.,1.),(1.,1.),(1.,1.),(1.,1.),(1.,
1.),(1.,1.)))
REPRESENTATION_ITEM('')
SURFACE()
);
#968=(
BOUNDED_SURFACE()
B_SPLINE_SURFACE(5,1,((#127406,#127407),(#127408,#127409),(#127410,#127411),
(#127412,#127413),(#127414,#127415),(#127416,#127417),(#127418,#127419),
(#127420,#127421),(#127422,#127423),(#127424,#127425),(#127426,#127427),
(#127428,#127429),(#127430,#127431),(#127432,#127433),(#127434,#127435),
(#127436,#127437),(#127438,#127439),(#127440,#127441),(#127442,#127443),
(#127444,#127445),(#127446,#127447),(#127448,#127449),(#127450,#127451),
(#127452,#127453),(#127454,#127455),(#127456,#127457),(#127458,#127459),
(#127460,#127461),(#127462,#127463),(#127464,#127465),(#127466,#127467),
(#127468,#127469),(#127470,#127471),(#127472,#127473),(#127474,#127475),
(#127476,#127477),(#127478,#127479),(#127480,#127481),(#127482,#127483),
(#127484,#127485),(#127486,#127487),(#127488,#127489),(#127490,#127491),
(#127492,#127493),(#127494,#127495),(#127496,#127497),(#127498,#127499),
(#127500,#127501),(#127502,#127503),(#127504,#127505),(#127506,#127507),
(#127508,#127509),(#127510,#127511),(#127512,#127513),(#127514,#127515),
(#127516,#127517),(#127518,#127519),(#127520,#127521),(#127522,#127523),
(#127524,#127525),(#127526,#127527),(#127528,#127529),(#127530,#127531),
(#127532,#127533),(#127534,#127535),(#127536,#127537),(#127538,#127539),
(#127540,#127541),(#127542,#127543),(#127544,#127545),(#127546,#127547),
(#127548,#127549),(#127550,#127551),(#127552,#127553),(#127554,#127555),
(#127556,#127557),(#127558,#127559),(#127560,#127561),(#127562,#127563),
(#127564,#127565),(#127566,#127567),(#127568,#127569),(#127570,#127571),
(#127572,#127573),(#127574,#127575),(#127576,#127577),(#127578,#127579),
(#127580,#127581),(#127582,#127583),(#127584,#127585),(#127586,#127587),
(#127588,#127589),(#127590,#127591),(#127592,#127593),(#127594,#127595),
(#127596,#127597),(#127598,#127599),(#127600,#127601),(#127602,#127603),
(#127604,#127605),(#127606,#127607),(#127608,#127609),(#127610,#127611),
(#127612,#127613),(#127614,#127615),(#127616,#127617),(#127618,#127619),
(#127620,#127621),(#127622,#127623),(#127624,#127625),(#127626,#127627),
(#127628,#127629),(#127630,#127631),(#127632,#127633),(#127634,#127635),
(#127636,#127637),(#127638,#127639),(#127640,#127641),(#127642,#127643),
(#127644,#127645),(#127646,#127647),(#127648,#127649),(#127650,#127651),
(#127652,#127653),(#127654,#127655),(#127656,#127657),(#127658,#127659),
(#127660,#127661),(#127662,#127663),(#127664,#127665),(#127666,#127667),
(#127668,#127669),(#127670,#127671),(#127672,#127673),(#127674,#127675),
(#127676,#127677),(#127678,#127679),(#127680,#127681),(#127682,#127683),
(#127684,#127685),(#127686,#127687),(#127688,#127689),(#127690,#127691),
(#127692,#127693),(#127694,#127695),(#127696,#127697),(#127698,#127699),
(#127700,#127701),(#127702,#127703),(#127704,#127705),(#127706,#127707),
(#127708,#127709),(#127710,#127711),(#127712,#127713),(#127714,#127715),
(#127716,#127717),(#127718,#127719),(#127720,#127721),(#127722,#127723),
(#127724,#127725),(#127726,#127727),(#127728,#127729),(#127730,#127731),
(#127732,#127733),(#127734,#127735),(#127736,#127737),(#127738,#127739),
(#127740,#127741),(#127742,#127743),(#127744,#127745),(#127746,#127747),
(#127748,#127749),(#127750,#127751),(#127752,#127753),(#127754,#127755),
(#127756,#127757),(#127758,#127759),(#127760,#127761),(#127762,#127763),
(#127764,#127765),(#127766,#127767),(#127768,#127769),(#127770,#127771),
(#127772,#127773),(#127774,#127775),(#127776,#127777),(#127778,#127779),
(#127780,#127781),(#127782,#127783),(#127784,#127785),(#127786,#127787),
(#127788,#127789),(#127790,#127791),(#127792,#127793),(#127794,#127795),
(#127796,#127797),(#127798,#127799),(#127800,#127801),(#127802,#127803),
(#127804,#127805),(#127806,#127807),(#127808,#127809),(#127810,#127811),
(#127812,#127813),(#127814,#127815)),.UNSPECIFIED.,.F.,.F.,.F.)
B_SPLINE_SURFACE_WITH_KNOTS((6,1,1,1,1,1,1,1,1,1,1,1,1,1,1,1,1,1,1,1,1,
1,1,1,1,1,1,1,1,1,1,1,1,1,1,1,1,1,1,1,1,1,1,1,1,1,1,1,1,1,1,1,1,1,1,1,1,
1,1,1,1,1,1,1,1,1,1,1,1,1,1,1,1,1,1,1,1,1,1,1,1,1,1,1,1,1,1,1,1,1,1,1,1,
1,1,1,1,1,1,1,1,1,1,1,1,1,1,1,1,1,1,1,1,1,1,1,1,1,1,1,1,1,1,1,1,1,1,1,1,
1,1,1,1,1,1,1,1,1,1,1,1,1,1,1,1,1,1,1,1,1,1,1,1,1,1,1,1,1,1,1,1,1,1,1,1,
1,1,1,1,1,1,1,1,1,1,1,1,1,1,1,1,1,1,1,1,1,1,1,1,1,1,1,1,1,1,1,1,1,1,1,6),
(2,2),(-1.,-0.995000000000001,-0.990000000000001,-0.985000000000001,-0.980000000000001,
-0.975000000000001,-0.970000000000001,-0.965000000000001,-0.960000000000001,
-0.955000000000001,-0.950000000000001,-0.945000000000001,-0.940000000000001,
-0.935000000000001,-0.930000000000001,-0.925000000000001,-0.920000000000001,
-0.915000000000001,-0.910000000000001,-0.905000000000001,-0.900000000000001,
-0.895000000000001,-0.890000000000001,-0.885000000000001,-0.880000000000001,
-0.875000000000001,-0.870000000000001,-0.865000000000001,-0.860000000000001,
-0.855000000000001,-0.850000000000001,-0.845000000000001,-0.840000000000001,
-0.835000000000001,-0.830000000000001,-0.825000000000001,-0.820000000000001,
-0.815000000000001,-0.810000000000001,-0.805000000000001,-0.800000000000001,
-0.795000000000001,-0.790000000000001,-0.785000000000001,-0.780000000000001,
-0.775000000000001,-0.770000000000001,-0.765000000000001,-0.760000000000001,
-0.755000000000001,-0.750000000000001,-0.745000000000001,-0.740000000000001,
-0.735000000000001,-0.730000000000001,-0.725000000000001,-0.720000000000001,
-0.715000000000001,-0.710000000000001,-0.705000000000001,-0.700000000000001,
-0.695000000000001,-0.690000000000001,-0.685,-0.68,-0.675,-0.67,-0.665,
-0.66,-0.655,-0.65,-0.645,-0.64,-0.635,-0.63,-0.625,-0.62,-0.615,-0.61,
-0.605,-0.6,-0.595,-0.59,-0.585,-0.58,-0.575,-0.57,-0.565,-0.56,-0.555,
-0.55,-0.545,-0.54,-0.535,-0.53,-0.525,-0.52,-0.515,-0.51,-0.505,-0.5,-0.495,
-0.49,-0.485,-0.48,-0.475,-0.47,-0.465,-0.46,-0.455,-0.45,-0.445,-0.44,
-0.435,-0.43,-0.425,-0.42,-0.415,-0.41,-0.405,-0.4,-0.395,-0.39,-0.385,
-0.38,-0.375,-0.37,-0.365,-0.36,-0.355,-0.35,-0.345,-0.34,-0.335,-0.33,
-0.325,-0.32,-0.315,-0.31,-0.305,-0.3,-0.295,-0.29,-0.285,-0.28,-0.275,
-0.27,-0.265,-0.26,-0.255,-0.25,-0.245,-0.24,-0.235,-0.23,-0.225,-0.22,
-0.215,-0.21,-0.205,-0.2,-0.195,-0.19,-0.185,-0.18,-0.175,-0.17,-0.165,
-0.16,-0.155,-0.15,-0.145,-0.14,-0.135,-0.13,-0.125,-0.12,-0.115,-0.11,
-0.105,-0.1,-0.095,-0.09,-0.085,-0.08,-0.075,-0.07,-0.065,-0.06,-0.055,
-0.05,-0.045,-0.04,-0.035,-0.03,-0.025,-0.02,-0.015,-0.01,-0.005,0.),(0.,
1.2),.UNSPECIFIED.)
GEOMETRIC_REPRESENTATION_ITEM()
RATIONAL_B_SPLINE_SURFACE(((1.,1.),(1.,1.),(1.,1.),(1.,1.),(1.,1.),(1.,
1.),(1.,1.),(1.,1.),(1.,1.),(1.,1.),(1.,1.),(1.,1.),(1.,1.),(1.,1.),(1.,
1.),(1.,1.),(1.,1.),(1.,1.),(1.,1.),(1.,1.),(1.,1.),(1.,1.),(1.,1.),(1.,
1.),(1.,1.),(1.,1.),(1.,1.),(1.,1.),(1.,1.),(1.,1.),(1.,1.),(1.,1.),(1.,
1.),(1.,1.),(1.,1.),(1.,1.),(1.,1.),(1.,1.),(1.,1.),(1.,1.),(1.,1.),(1.,
1.),(1.,1.),(1.,1.),(1.,1.),(1.,1.),(1.,1.),(1.,1.),(1.,1.),(1.,1.),(1.,
1.),(1.,1.),(1.,1.),(1.,1.),(1.,1.),(1.,1.),(1.,1.),(1.,1.),(1.,1.),(1.,
1.),(1.,1.),(1.,1.),(1.,1.),(1.,1.),(1.,1.),(1.,1.),(1.,1.),(1.,1.),(1.,
1.),(1.,1.),(1.,1.),(1.,1.),(1.,1.),(1.,1.),(1.,1.),(1.,1.),(1.,1.),(1.,
1.),(1.,1.),(1.,1.),(1.,1.),(1.,1.),(1.,1.),(1.,1.),(1.,1.),(1.,1.),(1.,
1.),(1.,1.),(1.,1.),(1.,1.),(1.,1.),(1.,1.),(1.,1.),(1.,1.),(1.,1.),(1.,
1.),(1.,1.),(1.,1.),(1.,1.),(1.,1.),(1.,1.),(1.,1.),(1.,1.),(1.,1.),(1.,
1.),(1.,1.),(1.,1.),(1.,1.),(1.,1.),(1.,1.),(1.,1.),(1.,1.),(1.,1.),(1.,
1.),(1.,1.),(1.,1.),(1.,1.),(1.,1.),(1.,1.),(1.,1.),(1.,1.),(1.,1.),(1.,
1.),(1.,1.),(1.,1.),(1.,1.),(1.,1.),(1.,1.),(1.,1.),(1.,1.),(1.,1.),(1.,
1.),(1.,1.),(1.,1.),(1.,1.),(1.,1.),(1.,1.),(1.,1.),(1.,1.),(1.,1.),(1.,
1.),(1.,1.),(1.,1.),(1.,1.),(1.,1.),(1.,1.),(1.,1.),(1.,1.),(1.,1.),(1.,
1.),(1.,1.),(1.,1.),(1.,1.),(1.,1.),(1.,1.),(1.,1.),(1.,1.),(1.,1.),(1.,
1.),(1.,1.),(1.,1.),(1.,1.),(1.,1.),(1.,1.),(1.,1.),(1.,1.),(1.,1.),(1.,
1.),(1.,1.),(1.,1.),(1.,1.),(1.,1.),(1.,1.),(1.,1.),(1.,1.),(1.,1.),(1.,
1.),(1.,1.),(1.,1.),(1.,1.),(1.,1.),(1.,1.),(1.,1.),(1.,1.),(1.,1.),(1.,
1.),(1.,1.),(1.,1.),(1.,1.),(1.,1.),(1.,1.),(1.,1.),(1.,1.),(1.,1.),(1.,
1.),(1.,1.),(1.,1.),(1.,1.),(1.,1.),(1.,1.),(1.,1.),(1.,1.),(1.,1.),(1.,
1.),(1.,1.)))
REPRESENTATION_ITEM('')
SURFACE()
);
#969=(
BOUNDED_SURFACE()
B_SPLINE_SURFACE(5,1,((#128207,#128208),(#128209,#128210),(#128211,#128212),
(#128213,#128214),(#128215,#128216),(#128217,#128218),(#128219,#128220),
(#128221,#128222),(#128223,#128224),(#128225,#128226),(#128227,#128228),
(#128229,#128230),(#128231,#128232),(#128233,#128234),(#128235,#128236),
(#128237,#128238),(#128239,#128240),(#128241,#128242),(#128243,#128244),
(#128245,#128246),(#128247,#128248),(#128249,#128250),(#128251,#128252),
(#128253,#128254),(#128255,#128256),(#128257,#128258),(#128259,#128260),
(#128261,#128262),(#128263,#128264),(#128265,#128266),(#128267,#128268),
(#128269,#128270),(#128271,#128272),(#128273,#128274),(#128275,#128276),
(#128277,#128278),(#128279,#128280),(#128281,#128282),(#128283,#128284),
(#128285,#128286),(#128287,#128288),(#128289,#128290),(#128291,#128292),
(#128293,#128294),(#128295,#128296),(#128297,#128298),(#128299,#128300),
(#128301,#128302),(#128303,#128304),(#128305,#128306),(#128307,#128308),
(#128309,#128310),(#128311,#128312),(#128313,#128314),(#128315,#128316),
(#128317,#128318),(#128319,#128320),(#128321,#128322),(#128323,#128324),
(#128325,#128326),(#128327,#128328),(#128329,#128330),(#128331,#128332),
(#128333,#128334),(#128335,#128336),(#128337,#128338),(#128339,#128340),
(#128341,#128342),(#128343,#128344),(#128345,#128346),(#128347,#128348),
(#128349,#128350),(#128351,#128352),(#128353,#128354),(#128355,#128356),
(#128357,#128358),(#128359,#128360),(#128361,#128362),(#128363,#128364),
(#128365,#128366),(#128367,#128368),(#128369,#128370),(#128371,#128372),
(#128373,#128374),(#128375,#128376),(#128377,#128378),(#128379,#128380),
(#128381,#128382),(#128383,#128384),(#128385,#128386),(#128387,#128388),
(#128389,#128390),(#128391,#128392),(#128393,#128394),(#128395,#128396),
(#128397,#128398),(#128399,#128400),(#128401,#128402),(#128403,#128404),
(#128405,#128406),(#128407,#128408),(#128409,#128410),(#128411,#128412),
(#128413,#128414),(#128415,#128416),(#128417,#128418),(#128419,#128420),
(#128421,#128422),(#128423,#128424),(#128425,#128426),(#128427,#128428),
(#128429,#128430),(#128431,#128432),(#128433,#128434),(#128435,#128436),
(#128437,#128438),(#128439,#128440),(#128441,#128442),(#128443,#128444),
(#128445,#128446),(#128447,#128448),(#128449,#128450),(#128451,#128452),
(#128453,#128454),(#128455,#128456),(#128457,#128458),(#128459,#128460),
(#128461,#128462),(#128463,#128464),(#128465,#128466),(#128467,#128468),
(#128469,#128470),(#128471,#128472),(#128473,#128474),(#128475,#128476),
(#128477,#128478),(#128479,#128480),(#128481,#128482),(#128483,#128484),
(#128485,#128486),(#128487,#128488),(#128489,#128490),(#128491,#128492),
(#128493,#128494),(#128495,#128496),(#128497,#128498),(#128499,#128500),
(#128501,#128502),(#128503,#128504),(#128505,#128506),(#128507,#128508),
(#128509,#128510),(#128511,#128512),(#128513,#128514),(#128515,#128516),
(#128517,#128518),(#128519,#128520),(#128521,#128522),(#128523,#128524),
(#128525,#128526),(#128527,#128528),(#128529,#128530),(#128531,#128532),
(#128533,#128534),(#128535,#128536),(#128537,#128538),(#128539,#128540),
(#128541,#128542),(#128543,#128544),(#128545,#128546),(#128547,#128548),
(#128549,#128550),(#128551,#128552),(#128553,#128554),(#128555,#128556),
(#128557,#128558),(#128559,#128560),(#128561,#128562),(#128563,#128564),
(#128565,#128566),(#128567,#128568),(#128569,#128570),(#128571,#128572),
(#128573,#128574),(#128575,#128576),(#128577,#128578),(#128579,#128580),
(#128581,#128582),(#128583,#128584),(#128585,#128586),(#128587,#128588),
(#128589,#128590),(#128591,#128592),(#128593,#128594),(#128595,#128596),
(#128597,#128598),(#128599,#128600),(#128601,#128602),(#128603,#128604),
(#128605,#128606),(#128607,#128608),(#128609,#128610),(#128611,#128612),
(#128613,#128614),(#128615,#128616)),.UNSPECIFIED.,.F.,.F.,.F.)
B_SPLINE_SURFACE_WITH_KNOTS((6,1,1,1,1,1,1,1,1,1,1,1,1,1,1,1,1,1,1,1,1,
1,1,1,1,1,1,1,1,1,1,1,1,1,1,1,1,1,1,1,1,1,1,1,1,1,1,1,1,1,1,1,1,1,1,1,1,
1,1,1,1,1,1,1,1,1,1,1,1,1,1,1,1,1,1,1,1,1,1,1,1,1,1,1,1,1,1,1,1,1,1,1,1,
1,1,1,1,1,1,1,1,1,1,1,1,1,1,1,1,1,1,1,1,1,1,1,1,1,1,1,1,1,1,1,1,1,1,1,1,
1,1,1,1,1,1,1,1,1,1,1,1,1,1,1,1,1,1,1,1,1,1,1,1,1,1,1,1,1,1,1,1,1,1,1,1,
1,1,1,1,1,1,1,1,1,1,1,1,1,1,1,1,1,1,1,1,1,1,1,1,1,1,1,1,1,1,1,1,1,1,1,6),
(2,2),(-1.,-0.995000000000001,-0.990000000000001,-0.985000000000001,-0.980000000000001,
-0.975000000000001,-0.970000000000001,-0.965000000000001,-0.960000000000001,
-0.955000000000001,-0.950000000000001,-0.945000000000001,-0.940000000000001,
-0.935000000000001,-0.930000000000001,-0.925000000000001,-0.920000000000001,
-0.915000000000001,-0.910000000000001,-0.905000000000001,-0.900000000000001,
-0.895000000000001,-0.890000000000001,-0.885000000000001,-0.880000000000001,
-0.875000000000001,-0.870000000000001,-0.865000000000001,-0.860000000000001,
-0.855000000000001,-0.850000000000001,-0.845000000000001,-0.840000000000001,
-0.835000000000001,-0.830000000000001,-0.825000000000001,-0.820000000000001,
-0.815000000000001,-0.810000000000001,-0.805000000000001,-0.800000000000001,
-0.795000000000001,-0.790000000000001,-0.785000000000001,-0.780000000000001,
-0.775000000000001,-0.770000000000001,-0.765000000000001,-0.760000000000001,
-0.755000000000001,-0.750000000000001,-0.745000000000001,-0.740000000000001,
-0.735000000000001,-0.730000000000001,-0.725000000000001,-0.720000000000001,
-0.715000000000001,-0.710000000000001,-0.705000000000001,-0.700000000000001,
-0.695000000000001,-0.690000000000001,-0.685,-0.68,-0.675,-0.67,-0.665,
-0.66,-0.655,-0.65,-0.645,-0.64,-0.635,-0.63,-0.625,-0.62,-0.615,-0.61,
-0.605,-0.6,-0.595,-0.59,-0.585,-0.58,-0.575,-0.57,-0.565,-0.56,-0.555,
-0.55,-0.545,-0.54,-0.535,-0.53,-0.525,-0.52,-0.515,-0.51,-0.505,-0.5,-0.495,
-0.49,-0.485,-0.48,-0.475,-0.47,-0.465,-0.46,-0.455,-0.45,-0.445,-0.44,
-0.435,-0.43,-0.425,-0.42,-0.415,-0.41,-0.405,-0.4,-0.395,-0.39,-0.385,
-0.38,-0.375,-0.37,-0.365,-0.36,-0.355,-0.35,-0.345,-0.34,-0.335,-0.33,
-0.325,-0.32,-0.315,-0.31,-0.305,-0.3,-0.295,-0.29,-0.285,-0.28,-0.275,
-0.27,-0.265,-0.26,-0.255,-0.25,-0.245,-0.24,-0.235,-0.23,-0.225,-0.22,
-0.215,-0.21,-0.205,-0.2,-0.195,-0.19,-0.185,-0.18,-0.175,-0.17,-0.165,
-0.16,-0.155,-0.15,-0.145,-0.14,-0.135,-0.13,-0.125,-0.12,-0.115,-0.11,
-0.105,-0.1,-0.095,-0.09,-0.085,-0.08,-0.075,-0.07,-0.065,-0.06,-0.055,
-0.05,-0.045,-0.04,-0.035,-0.03,-0.025,-0.02,-0.015,-0.01,-0.005,0.),(0.,
1.2),.UNSPECIFIED.)
GEOMETRIC_REPRESENTATION_ITEM()
RATIONAL_B_SPLINE_SURFACE(((1.,1.),(1.,1.),(1.,1.),(1.,1.),(1.,1.),(1.,
1.),(1.,1.),(1.,1.),(1.,1.),(1.,1.),(1.,1.),(1.,1.),(1.,1.),(1.,1.),(1.,
1.),(1.,1.),(1.,1.),(1.,1.),(1.,1.),(1.,1.),(1.,1.),(1.,1.),(1.,1.),(1.,
1.),(1.,1.),(1.,1.),(1.,1.),(1.,1.),(1.,1.),(1.,1.),(1.,1.),(1.,1.),(1.,
1.),(1.,1.),(1.,1.),(1.,1.),(1.,1.),(1.,1.),(1.,1.),(1.,1.),(1.,1.),(1.,
1.),(1.,1.),(1.,1.),(1.,1.),(1.,1.),(1.,1.),(1.,1.),(1.,1.),(1.,1.),(1.,
1.),(1.,1.),(1.,1.),(1.,1.),(1.,1.),(1.,1.),(1.,1.),(1.,1.),(1.,1.),(1.,
1.),(1.,1.),(1.,1.),(1.,1.),(1.,1.),(1.,1.),(1.,1.),(1.,1.),(1.,1.),(1.,
1.),(1.,1.),(1.,1.),(1.,1.),(1.,1.),(1.,1.),(1.,1.),(1.,1.),(1.,1.),(1.,
1.),(1.,1.),(1.,1.),(1.,1.),(1.,1.),(1.,1.),(1.,1.),(1.,1.),(1.,1.),(1.,
1.),(1.,1.),(1.,1.),(1.,1.),(1.,1.),(1.,1.),(1.,1.),(1.,1.),(1.,1.),(1.,
1.),(1.,1.),(1.,1.),(1.,1.),(1.,1.),(1.,1.),(1.,1.),(1.,1.),(1.,1.),(1.,
1.),(1.,1.),(1.,1.),(1.,1.),(1.,1.),(1.,1.),(1.,1.),(1.,1.),(1.,1.),(1.,
1.),(1.,1.),(1.,1.),(1.,1.),(1.,1.),(1.,1.),(1.,1.),(1.,1.),(1.,1.),(1.,
1.),(1.,1.),(1.,1.),(1.,1.),(1.,1.),(1.,1.),(1.,1.),(1.,1.),(1.,1.),(1.,
1.),(1.,1.),(1.,1.),(1.,1.),(1.,1.),(1.,1.),(1.,1.),(1.,1.),(1.,1.),(1.,
1.),(1.,1.),(1.,1.),(1.,1.),(1.,1.),(1.,1.),(1.,1.),(1.,1.),(1.,1.),(1.,
1.),(1.,1.),(1.,1.),(1.,1.),(1.,1.),(1.,1.),(1.,1.),(1.,1.),(1.,1.),(1.,
1.),(1.,1.),(1.,1.),(1.,1.),(1.,1.),(1.,1.),(1.,1.),(1.,1.),(1.,1.),(1.,
1.),(1.,1.),(1.,1.),(1.,1.),(1.,1.),(1.,1.),(1.,1.),(1.,1.),(1.,1.),(1.,
1.),(1.,1.),(1.,1.),(1.,1.),(1.,1.),(1.,1.),(1.,1.),(1.,1.),(1.,1.),(1.,
1.),(1.,1.),(1.,1.),(1.,1.),(1.,1.),(1.,1.),(1.,1.),(1.,1.),(1.,1.),(1.,
1.),(1.,1.),(1.,1.),(1.,1.),(1.,1.),(1.,1.),(1.,1.),(1.,1.),(1.,1.),(1.,
1.),(1.,1.)))
REPRESENTATION_ITEM('')
SURFACE()
);
#970=(
BOUNDED_SURFACE()
B_SPLINE_SURFACE(5,1,((#129008,#129009),(#129010,#129011),(#129012,#129013),
(#129014,#129015),(#129016,#129017),(#129018,#129019),(#129020,#129021),
(#129022,#129023),(#129024,#129025),(#129026,#129027),(#129028,#129029),
(#129030,#129031),(#129032,#129033),(#129034,#129035),(#129036,#129037),
(#129038,#129039),(#129040,#129041),(#129042,#129043),(#129044,#129045),
(#129046,#129047),(#129048,#129049),(#129050,#129051),(#129052,#129053),
(#129054,#129055),(#129056,#129057),(#129058,#129059),(#129060,#129061),
(#129062,#129063),(#129064,#129065),(#129066,#129067),(#129068,#129069),
(#129070,#129071),(#129072,#129073),(#129074,#129075),(#129076,#129077),
(#129078,#129079),(#129080,#129081),(#129082,#129083),(#129084,#129085),
(#129086,#129087),(#129088,#129089),(#129090,#129091),(#129092,#129093),
(#129094,#129095),(#129096,#129097),(#129098,#129099),(#129100,#129101),
(#129102,#129103),(#129104,#129105),(#129106,#129107),(#129108,#129109),
(#129110,#129111),(#129112,#129113),(#129114,#129115),(#129116,#129117),
(#129118,#129119),(#129120,#129121),(#129122,#129123),(#129124,#129125),
(#129126,#129127),(#129128,#129129),(#129130,#129131),(#129132,#129133),
(#129134,#129135),(#129136,#129137),(#129138,#129139),(#129140,#129141),
(#129142,#129143),(#129144,#129145),(#129146,#129147),(#129148,#129149),
(#129150,#129151),(#129152,#129153),(#129154,#129155),(#129156,#129157),
(#129158,#129159),(#129160,#129161),(#129162,#129163),(#129164,#129165),
(#129166,#129167),(#129168,#129169),(#129170,#129171),(#129172,#129173),
(#129174,#129175),(#129176,#129177),(#129178,#129179),(#129180,#129181),
(#129182,#129183),(#129184,#129185),(#129186,#129187),(#129188,#129189),
(#129190,#129191),(#129192,#129193),(#129194,#129195),(#129196,#129197),
(#129198,#129199),(#129200,#129201),(#129202,#129203),(#129204,#129205),
(#129206,#129207),(#129208,#129209),(#129210,#129211),(#129212,#129213),
(#129214,#129215),(#129216,#129217),(#129218,#129219),(#129220,#129221),
(#129222,#129223),(#129224,#129225),(#129226,#129227),(#129228,#129229),
(#129230,#129231),(#129232,#129233),(#129234,#129235),(#129236,#129237),
(#129238,#129239),(#129240,#129241),(#129242,#129243),(#129244,#129245),
(#129246,#129247),(#129248,#129249),(#129250,#129251),(#129252,#129253),
(#129254,#129255),(#129256,#129257),(#129258,#129259),(#129260,#129261),
(#129262,#129263),(#129264,#129265),(#129266,#129267),(#129268,#129269),
(#129270,#129271),(#129272,#129273),(#129274,#129275),(#129276,#129277),
(#129278,#129279),(#129280,#129281),(#129282,#129283),(#129284,#129285),
(#129286,#129287),(#129288,#129289),(#129290,#129291),(#129292,#129293),
(#129294,#129295),(#129296,#129297),(#129298,#129299),(#129300,#129301),
(#129302,#129303),(#129304,#129305),(#129306,#129307),(#129308,#129309),
(#129310,#129311),(#129312,#129313),(#129314,#129315),(#129316,#129317),
(#129318,#129319),(#129320,#129321),(#129322,#129323),(#129324,#129325),
(#129326,#129327),(#129328,#129329),(#129330,#129331),(#129332,#129333),
(#129334,#129335),(#129336,#129337),(#129338,#129339),(#129340,#129341),
(#129342,#129343),(#129344,#129345),(#129346,#129347),(#129348,#129349),
(#129350,#129351),(#129352,#129353),(#129354,#129355),(#129356,#129357),
(#129358,#129359),(#129360,#129361),(#129362,#129363),(#129364,#129365),
(#129366,#129367),(#129368,#129369),(#129370,#129371),(#129372,#129373),
(#129374,#129375),(#129376,#129377),(#129378,#129379),(#129380,#129381),
(#129382,#129383),(#129384,#129385),(#129386,#129387),(#129388,#129389),
(#129390,#129391),(#129392,#129393),(#129394,#129395),(#129396,#129397),
(#129398,#129399),(#129400,#129401),(#129402,#129403),(#129404,#129405),
(#129406,#129407),(#129408,#129409),(#129410,#129411),(#129412,#129413),
(#129414,#129415),(#129416,#129417)),.UNSPECIFIED.,.F.,.F.,.F.)
B_SPLINE_SURFACE_WITH_KNOTS((6,1,1,1,1,1,1,1,1,1,1,1,1,1,1,1,1,1,1,1,1,
1,1,1,1,1,1,1,1,1,1,1,1,1,1,1,1,1,1,1,1,1,1,1,1,1,1,1,1,1,1,1,1,1,1,1,1,
1,1,1,1,1,1,1,1,1,1,1,1,1,1,1,1,1,1,1,1,1,1,1,1,1,1,1,1,1,1,1,1,1,1,1,1,
1,1,1,1,1,1,1,1,1,1,1,1,1,1,1,1,1,1,1,1,1,1,1,1,1,1,1,1,1,1,1,1,1,1,1,1,
1,1,1,1,1,1,1,1,1,1,1,1,1,1,1,1,1,1,1,1,1,1,1,1,1,1,1,1,1,1,1,1,1,1,1,1,
1,1,1,1,1,1,1,1,1,1,1,1,1,1,1,1,1,1,1,1,1,1,1,1,1,1,1,1,1,1,1,1,1,1,1,6),
(2,2),(-1.,-0.995000000000001,-0.990000000000001,-0.985000000000001,-0.980000000000001,
-0.975000000000001,-0.970000000000001,-0.965000000000001,-0.960000000000001,
-0.955000000000001,-0.950000000000001,-0.945000000000001,-0.940000000000001,
-0.935000000000001,-0.930000000000001,-0.925000000000001,-0.920000000000001,
-0.915000000000001,-0.910000000000001,-0.905000000000001,-0.900000000000001,
-0.895000000000001,-0.890000000000001,-0.885000000000001,-0.880000000000001,
-0.875000000000001,-0.870000000000001,-0.865000000000001,-0.860000000000001,
-0.855000000000001,-0.850000000000001,-0.845000000000001,-0.840000000000001,
-0.835000000000001,-0.830000000000001,-0.825000000000001,-0.820000000000001,
-0.815000000000001,-0.810000000000001,-0.805000000000001,-0.800000000000001,
-0.795000000000001,-0.790000000000001,-0.785000000000001,-0.780000000000001,
-0.775000000000001,-0.770000000000001,-0.765000000000001,-0.760000000000001,
-0.755000000000001,-0.750000000000001,-0.745000000000001,-0.740000000000001,
-0.735000000000001,-0.730000000000001,-0.725000000000001,-0.720000000000001,
-0.715000000000001,-0.710000000000001,-0.705000000000001,-0.700000000000001,
-0.695000000000001,-0.690000000000001,-0.685,-0.68,-0.675,-0.67,-0.665,
-0.66,-0.655,-0.65,-0.645,-0.64,-0.635,-0.63,-0.625,-0.62,-0.615,-0.61,
-0.605,-0.6,-0.595,-0.59,-0.585,-0.58,-0.575,-0.57,-0.565,-0.56,-0.555,
-0.55,-0.545,-0.54,-0.535,-0.53,-0.525,-0.52,-0.515,-0.51,-0.505,-0.5,-0.495,
-0.49,-0.485,-0.48,-0.475,-0.47,-0.465,-0.46,-0.455,-0.45,-0.445,-0.44,
-0.435,-0.43,-0.425,-0.42,-0.415,-0.41,-0.405,-0.4,-0.395,-0.39,-0.385,
-0.38,-0.375,-0.37,-0.365,-0.36,-0.355,-0.35,-0.345,-0.34,-0.335,-0.33,
-0.325,-0.32,-0.315,-0.31,-0.305,-0.3,-0.295,-0.29,-0.285,-0.28,-0.275,
-0.27,-0.265,-0.26,-0.255,-0.25,-0.245,-0.24,-0.235,-0.23,-0.225,-0.22,
-0.215,-0.21,-0.205,-0.2,-0.195,-0.19,-0.185,-0.18,-0.175,-0.17,-0.165,
-0.16,-0.155,-0.15,-0.145,-0.14,-0.135,-0.13,-0.125,-0.12,-0.115,-0.11,
-0.105,-0.1,-0.095,-0.09,-0.085,-0.08,-0.075,-0.07,-0.065,-0.06,-0.055,
-0.05,-0.045,-0.04,-0.035,-0.03,-0.025,-0.02,-0.015,-0.01,-0.005,0.),(0.,
1.2),.UNSPECIFIED.)
GEOMETRIC_REPRESENTATION_ITEM()
RATIONAL_B_SPLINE_SURFACE(((1.,1.),(1.,1.),(1.,1.),(1.,1.),(1.,1.),(1.,
1.),(1.,1.),(1.,1.),(1.,1.),(1.,1.),(1.,1.),(1.,1.),(1.,1.),(1.,1.),(1.,
1.),(1.,1.),(1.,1.),(1.,1.),(1.,1.),(1.,1.),(1.,1.),(1.,1.),(1.,1.),(1.,
1.),(1.,1.),(1.,1.),(1.,1.),(1.,1.),(1.,1.),(1.,1.),(1.,1.),(1.,1.),(1.,
1.),(1.,1.),(1.,1.),(1.,1.),(1.,1.),(1.,1.),(1.,1.),(1.,1.),(1.,1.),(1.,
1.),(1.,1.),(1.,1.),(1.,1.),(1.,1.),(1.,1.),(1.,1.),(1.,1.),(1.,1.),(1.,
1.),(1.,1.),(1.,1.),(1.,1.),(1.,1.),(1.,1.),(1.,1.),(1.,1.),(1.,1.),(1.,
1.),(1.,1.),(1.,1.),(1.,1.),(1.,1.),(1.,1.),(1.,1.),(1.,1.),(1.,1.),(1.,
1.),(1.,1.),(1.,1.),(1.,1.),(1.,1.),(1.,1.),(1.,1.),(1.,1.),(1.,1.),(1.,
1.),(1.,1.),(1.,1.),(1.,1.),(1.,1.),(1.,1.),(1.,1.),(1.,1.),(1.,1.),(1.,
1.),(1.,1.),(1.,1.),(1.,1.),(1.,1.),(1.,1.),(1.,1.),(1.,1.),(1.,1.),(1.,
1.),(1.,1.),(1.,1.),(1.,1.),(1.,1.),(1.,1.),(1.,1.),(1.,1.),(1.,1.),(1.,
1.),(1.,1.),(1.,1.),(1.,1.),(1.,1.),(1.,1.),(1.,1.),(1.,1.),(1.,1.),(1.,
1.),(1.,1.),(1.,1.),(1.,1.),(1.,1.),(1.,1.),(1.,1.),(1.,1.),(1.,1.),(1.,
1.),(1.,1.),(1.,1.),(1.,1.),(1.,1.),(1.,1.),(1.,1.),(1.,1.),(1.,1.),(1.,
1.),(1.,1.),(1.,1.),(1.,1.),(1.,1.),(1.,1.),(1.,1.),(1.,1.),(1.,1.),(1.,
1.),(1.,1.),(1.,1.),(1.,1.),(1.,1.),(1.,1.),(1.,1.),(1.,1.),(1.,1.),(1.,
1.),(1.,1.),(1.,1.),(1.,1.),(1.,1.),(1.,1.),(1.,1.),(1.,1.),(1.,1.),(1.,
1.),(1.,1.),(1.,1.),(1.,1.),(1.,1.),(1.,1.),(1.,1.),(1.,1.),(1.,1.),(1.,
1.),(1.,1.),(1.,1.),(1.,1.),(1.,1.),(1.,1.),(1.,1.),(1.,1.),(1.,1.),(1.,
1.),(1.,1.),(1.,1.),(1.,1.),(1.,1.),(1.,1.),(1.,1.),(1.,1.),(1.,1.),(1.,
1.),(1.,1.),(1.,1.),(1.,1.),(1.,1.),(1.,1.),(1.,1.),(1.,1.),(1.,1.),(1.,
1.),(1.,1.),(1.,1.),(1.,1.),(1.,1.),(1.,1.),(1.,1.),(1.,1.),(1.,1.),(1.,
1.),(1.,1.)))
REPRESENTATION_ITEM('')
SURFACE()
);
#971=(
BOUNDED_SURFACE()
B_SPLINE_SURFACE(5,1,((#129809,#129810),(#129811,#129812),(#129813,#129814),
(#129815,#129816),(#129817,#129818),(#129819,#129820),(#129821,#129822),
(#129823,#129824),(#129825,#129826),(#129827,#129828),(#129829,#129830),
(#129831,#129832),(#129833,#129834),(#129835,#129836),(#129837,#129838),
(#129839,#129840),(#129841,#129842),(#129843,#129844),(#129845,#129846),
(#129847,#129848),(#129849,#129850),(#129851,#129852),(#129853,#129854),
(#129855,#129856),(#129857,#129858),(#129859,#129860),(#129861,#129862),
(#129863,#129864),(#129865,#129866),(#129867,#129868),(#129869,#129870),
(#129871,#129872),(#129873,#129874),(#129875,#129876),(#129877,#129878),
(#129879,#129880),(#129881,#129882),(#129883,#129884),(#129885,#129886),
(#129887,#129888),(#129889,#129890),(#129891,#129892),(#129893,#129894),
(#129895,#129896),(#129897,#129898),(#129899,#129900),(#129901,#129902),
(#129903,#129904),(#129905,#129906),(#129907,#129908),(#129909,#129910),
(#129911,#129912),(#129913,#129914),(#129915,#129916),(#129917,#129918),
(#129919,#129920),(#129921,#129922),(#129923,#129924),(#129925,#129926),
(#129927,#129928),(#129929,#129930),(#129931,#129932),(#129933,#129934),
(#129935,#129936),(#129937,#129938),(#129939,#129940),(#129941,#129942),
(#129943,#129944),(#129945,#129946),(#129947,#129948),(#129949,#129950),
(#129951,#129952),(#129953,#129954),(#129955,#129956),(#129957,#129958),
(#129959,#129960),(#129961,#129962),(#129963,#129964),(#129965,#129966),
(#129967,#129968),(#129969,#129970),(#129971,#129972),(#129973,#129974),
(#129975,#129976),(#129977,#129978),(#129979,#129980),(#129981,#129982),
(#129983,#129984),(#129985,#129986),(#129987,#129988),(#129989,#129990),
(#129991,#129992),(#129993,#129994),(#129995,#129996),(#129997,#129998),
(#129999,#130000),(#130001,#130002),(#130003,#130004),(#130005,#130006),
(#130007,#130008),(#130009,#130010),(#130011,#130012),(#130013,#130014),
(#130015,#130016),(#130017,#130018),(#130019,#130020),(#130021,#130022),
(#130023,#130024),(#130025,#130026),(#130027,#130028),(#130029,#130030),
(#130031,#130032),(#130033,#130034),(#130035,#130036),(#130037,#130038),
(#130039,#130040),(#130041,#130042),(#130043,#130044),(#130045,#130046),
(#130047,#130048),(#130049,#130050),(#130051,#130052),(#130053,#130054),
(#130055,#130056),(#130057,#130058),(#130059,#130060),(#130061,#130062),
(#130063,#130064),(#130065,#130066),(#130067,#130068),(#130069,#130070),
(#130071,#130072),(#130073,#130074),(#130075,#130076),(#130077,#130078),
(#130079,#130080),(#130081,#130082),(#130083,#130084),(#130085,#130086),
(#130087,#130088),(#130089,#130090),(#130091,#130092),(#130093,#130094),
(#130095,#130096),(#130097,#130098),(#130099,#130100),(#130101,#130102),
(#130103,#130104),(#130105,#130106),(#130107,#130108),(#130109,#130110),
(#130111,#130112),(#130113,#130114),(#130115,#130116),(#130117,#130118),
(#130119,#130120),(#130121,#130122),(#130123,#130124),(#130125,#130126),
(#130127,#130128),(#130129,#130130),(#130131,#130132),(#130133,#130134),
(#130135,#130136),(#130137,#130138),(#130139,#130140),(#130141,#130142),
(#130143,#130144),(#130145,#130146),(#130147,#130148),(#130149,#130150),
(#130151,#130152),(#130153,#130154),(#130155,#130156),(#130157,#130158),
(#130159,#130160),(#130161,#130162),(#130163,#130164),(#130165,#130166),
(#130167,#130168),(#130169,#130170),(#130171,#130172),(#130173,#130174),
(#130175,#130176),(#130177,#130178),(#130179,#130180),(#130181,#130182),
(#130183,#130184),(#130185,#130186),(#130187,#130188),(#130189,#130190),
(#130191,#130192),(#130193,#130194),(#130195,#130196),(#130197,#130198),
(#130199,#130200),(#130201,#130202),(#130203,#130204),(#130205,#130206),
(#130207,#130208),(#130209,#130210),(#130211,#130212),(#130213,#130214),
(#130215,#130216),(#130217,#130218)),.UNSPECIFIED.,.F.,.F.,.F.)
B_SPLINE_SURFACE_WITH_KNOTS((6,1,1,1,1,1,1,1,1,1,1,1,1,1,1,1,1,1,1,1,1,
1,1,1,1,1,1,1,1,1,1,1,1,1,1,1,1,1,1,1,1,1,1,1,1,1,1,1,1,1,1,1,1,1,1,1,1,
1,1,1,1,1,1,1,1,1,1,1,1,1,1,1,1,1,1,1,1,1,1,1,1,1,1,1,1,1,1,1,1,1,1,1,1,
1,1,1,1,1,1,1,1,1,1,1,1,1,1,1,1,1,1,1,1,1,1,1,1,1,1,1,1,1,1,1,1,1,1,1,1,
1,1,1,1,1,1,1,1,1,1,1,1,1,1,1,1,1,1,1,1,1,1,1,1,1,1,1,1,1,1,1,1,1,1,1,1,
1,1,1,1,1,1,1,1,1,1,1,1,1,1,1,1,1,1,1,1,1,1,1,1,1,1,1,1,1,1,1,1,1,1,1,6),
(2,2),(-1.,-0.995000000000001,-0.990000000000001,-0.985000000000001,-0.980000000000001,
-0.975000000000001,-0.970000000000001,-0.965000000000001,-0.960000000000001,
-0.955000000000001,-0.950000000000001,-0.945000000000001,-0.940000000000001,
-0.935000000000001,-0.930000000000001,-0.925000000000001,-0.920000000000001,
-0.915000000000001,-0.910000000000001,-0.905000000000001,-0.900000000000001,
-0.895000000000001,-0.890000000000001,-0.885000000000001,-0.880000000000001,
-0.875000000000001,-0.870000000000001,-0.865000000000001,-0.860000000000001,
-0.855000000000001,-0.850000000000001,-0.845000000000001,-0.840000000000001,
-0.835000000000001,-0.830000000000001,-0.825000000000001,-0.820000000000001,
-0.815000000000001,-0.810000000000001,-0.805000000000001,-0.800000000000001,
-0.795000000000001,-0.790000000000001,-0.785000000000001,-0.780000000000001,
-0.775000000000001,-0.770000000000001,-0.765000000000001,-0.760000000000001,
-0.755000000000001,-0.750000000000001,-0.745000000000001,-0.740000000000001,
-0.735000000000001,-0.730000000000001,-0.725000000000001,-0.720000000000001,
-0.715000000000001,-0.710000000000001,-0.705000000000001,-0.700000000000001,
-0.695000000000001,-0.690000000000001,-0.685,-0.68,-0.675,-0.67,-0.665,
-0.66,-0.655,-0.65,-0.645,-0.64,-0.635,-0.63,-0.625,-0.62,-0.615,-0.61,
-0.605,-0.6,-0.595,-0.59,-0.585,-0.58,-0.575,-0.57,-0.565,-0.56,-0.555,
-0.55,-0.545,-0.54,-0.535,-0.53,-0.525,-0.52,-0.515,-0.51,-0.505,-0.5,-0.495,
-0.49,-0.485,-0.48,-0.475,-0.47,-0.465,-0.46,-0.455,-0.45,-0.445,-0.44,
-0.435,-0.43,-0.425,-0.42,-0.415,-0.41,-0.405,-0.4,-0.395,-0.39,-0.385,
-0.38,-0.375,-0.37,-0.365,-0.36,-0.355,-0.35,-0.345,-0.34,-0.335,-0.33,
-0.325,-0.32,-0.315,-0.31,-0.305,-0.3,-0.295,-0.29,-0.285,-0.28,-0.275,
-0.27,-0.265,-0.26,-0.255,-0.25,-0.245,-0.24,-0.235,-0.23,-0.225,-0.22,
-0.215,-0.21,-0.205,-0.2,-0.195,-0.19,-0.185,-0.18,-0.175,-0.17,-0.165,
-0.16,-0.155,-0.15,-0.145,-0.14,-0.135,-0.13,-0.125,-0.12,-0.115,-0.11,
-0.105,-0.1,-0.095,-0.09,-0.085,-0.08,-0.075,-0.07,-0.065,-0.06,-0.055,
-0.05,-0.045,-0.04,-0.035,-0.03,-0.025,-0.02,-0.015,-0.01,-0.005,0.),(0.,
1.2),.UNSPECIFIED.)
GEOMETRIC_REPRESENTATION_ITEM()
RATIONAL_B_SPLINE_SURFACE(((1.,1.),(1.,1.),(1.,1.),(1.,1.),(1.,1.),(1.,
1.),(1.,1.),(1.,1.),(1.,1.),(1.,1.),(1.,1.),(1.,1.),(1.,1.),(1.,1.),(1.,
1.),(1.,1.),(1.,1.),(1.,1.),(1.,1.),(1.,1.),(1.,1.),(1.,1.),(1.,1.),(1.,
1.),(1.,1.),(1.,1.),(1.,1.),(1.,1.),(1.,1.),(1.,1.),(1.,1.),(1.,1.),(1.,
1.),(1.,1.),(1.,1.),(1.,1.),(1.,1.),(1.,1.),(1.,1.),(1.,1.),(1.,1.),(1.,
1.),(1.,1.),(1.,1.),(1.,1.),(1.,1.),(1.,1.),(1.,1.),(1.,1.),(1.,1.),(1.,
1.),(1.,1.),(1.,1.),(1.,1.),(1.,1.),(1.,1.),(1.,1.),(1.,1.),(1.,1.),(1.,
1.),(1.,1.),(1.,1.),(1.,1.),(1.,1.),(1.,1.),(1.,1.),(1.,1.),(1.,1.),(1.,
1.),(1.,1.),(1.,1.),(1.,1.),(1.,1.),(1.,1.),(1.,1.),(1.,1.),(1.,1.),(1.,
1.),(1.,1.),(1.,1.),(1.,1.),(1.,1.),(1.,1.),(1.,1.),(1.,1.),(1.,1.),(1.,
1.),(1.,1.),(1.,1.),(1.,1.),(1.,1.),(1.,1.),(1.,1.),(1.,1.),(1.,1.),(1.,
1.),(1.,1.),(1.,1.),(1.,1.),(1.,1.),(1.,1.),(1.,1.),(1.,1.),(1.,1.),(1.,
1.),(1.,1.),(1.,1.),(1.,1.),(1.,1.),(1.,1.),(1.,1.),(1.,1.),(1.,1.),(1.,
1.),(1.,1.),(1.,1.),(1.,1.),(1.,1.),(1.,1.),(1.,1.),(1.,1.),(1.,1.),(1.,
1.),(1.,1.),(1.,1.),(1.,1.),(1.,1.),(1.,1.),(1.,1.),(1.,1.),(1.,1.),(1.,
1.),(1.,1.),(1.,1.),(1.,1.),(1.,1.),(1.,1.),(1.,1.),(1.,1.),(1.,1.),(1.,
1.),(1.,1.),(1.,1.),(1.,1.),(1.,1.),(1.,1.),(1.,1.),(1.,1.),(1.,1.),(1.,
1.),(1.,1.),(1.,1.),(1.,1.),(1.,1.),(1.,1.),(1.,1.),(1.,1.),(1.,1.),(1.,
1.),(1.,1.),(1.,1.),(1.,1.),(1.,1.),(1.,1.),(1.,1.),(1.,1.),(1.,1.),(1.,
1.),(1.,1.),(1.,1.),(1.,1.),(1.,1.),(1.,1.),(1.,1.),(1.,1.),(1.,1.),(1.,
1.),(1.,1.),(1.,1.),(1.,1.),(1.,1.),(1.,1.),(1.,1.),(1.,1.),(1.,1.),(1.,
1.),(1.,1.),(1.,1.),(1.,1.),(1.,1.),(1.,1.),(1.,1.),(1.,1.),(1.,1.),(1.,
1.),(1.,1.),(1.,1.),(1.,1.),(1.,1.),(1.,1.),(1.,1.),(1.,1.),(1.,1.),(1.,
1.),(1.,1.)))
REPRESENTATION_ITEM('')
SURFACE()
);
#972=(
BOUNDED_SURFACE()
B_SPLINE_SURFACE(5,1,((#130610,#130611),(#130612,#130613),(#130614,#130615),
(#130616,#130617),(#130618,#130619),(#130620,#130621),(#130622,#130623),
(#130624,#130625),(#130626,#130627),(#130628,#130629),(#130630,#130631),
(#130632,#130633),(#130634,#130635),(#130636,#130637),(#130638,#130639),
(#130640,#130641),(#130642,#130643),(#130644,#130645),(#130646,#130647),
(#130648,#130649),(#130650,#130651),(#130652,#130653),(#130654,#130655),
(#130656,#130657),(#130658,#130659),(#130660,#130661),(#130662,#130663),
(#130664,#130665),(#130666,#130667),(#130668,#130669),(#130670,#130671),
(#130672,#130673),(#130674,#130675),(#130676,#130677),(#130678,#130679),
(#130680,#130681),(#130682,#130683),(#130684,#130685),(#130686,#130687),
(#130688,#130689),(#130690,#130691),(#130692,#130693),(#130694,#130695),
(#130696,#130697),(#130698,#130699),(#130700,#130701),(#130702,#130703),
(#130704,#130705),(#130706,#130707),(#130708,#130709),(#130710,#130711),
(#130712,#130713),(#130714,#130715),(#130716,#130717),(#130718,#130719),
(#130720,#130721),(#130722,#130723),(#130724,#130725),(#130726,#130727),
(#130728,#130729),(#130730,#130731),(#130732,#130733),(#130734,#130735),
(#130736,#130737),(#130738,#130739),(#130740,#130741),(#130742,#130743),
(#130744,#130745),(#130746,#130747),(#130748,#130749),(#130750,#130751),
(#130752,#130753),(#130754,#130755),(#130756,#130757),(#130758,#130759),
(#130760,#130761),(#130762,#130763),(#130764,#130765),(#130766,#130767),
(#130768,#130769),(#130770,#130771),(#130772,#130773),(#130774,#130775),
(#130776,#130777),(#130778,#130779),(#130780,#130781),(#130782,#130783),
(#130784,#130785),(#130786,#130787),(#130788,#130789),(#130790,#130791),
(#130792,#130793),(#130794,#130795),(#130796,#130797),(#130798,#130799),
(#130800,#130801),(#130802,#130803),(#130804,#130805),(#130806,#130807),
(#130808,#130809),(#130810,#130811),(#130812,#130813),(#130814,#130815),
(#130816,#130817),(#130818,#130819),(#130820,#130821),(#130822,#130823),
(#130824,#130825),(#130826,#130827),(#130828,#130829),(#130830,#130831),
(#130832,#130833),(#130834,#130835),(#130836,#130837),(#130838,#130839),
(#130840,#130841),(#130842,#130843),(#130844,#130845),(#130846,#130847),
(#130848,#130849),(#130850,#130851),(#130852,#130853),(#130854,#130855),
(#130856,#130857),(#130858,#130859),(#130860,#130861),(#130862,#130863),
(#130864,#130865),(#130866,#130867),(#130868,#130869),(#130870,#130871),
(#130872,#130873),(#130874,#130875),(#130876,#130877),(#130878,#130879),
(#130880,#130881),(#130882,#130883),(#130884,#130885),(#130886,#130887),
(#130888,#130889),(#130890,#130891),(#130892,#130893),(#130894,#130895),
(#130896,#130897),(#130898,#130899),(#130900,#130901),(#130902,#130903),
(#130904,#130905),(#130906,#130907),(#130908,#130909),(#130910,#130911),
(#130912,#130913),(#130914,#130915),(#130916,#130917),(#130918,#130919),
(#130920,#130921),(#130922,#130923),(#130924,#130925),(#130926,#130927),
(#130928,#130929),(#130930,#130931),(#130932,#130933),(#130934,#130935),
(#130936,#130937),(#130938,#130939),(#130940,#130941),(#130942,#130943),
(#130944,#130945),(#130946,#130947),(#130948,#130949),(#130950,#130951),
(#130952,#130953),(#130954,#130955),(#130956,#130957),(#130958,#130959),
(#130960,#130961),(#130962,#130963),(#130964,#130965),(#130966,#130967),
(#130968,#130969),(#130970,#130971),(#130972,#130973),(#130974,#130975),
(#130976,#130977),(#130978,#130979),(#130980,#130981),(#130982,#130983),
(#130984,#130985),(#130986,#130987),(#130988,#130989),(#130990,#130991),
(#130992,#130993),(#130994,#130995),(#130996,#130997),(#130998,#130999),
(#131000,#131001),(#131002,#131003),(#131004,#131005),(#131006,#131007),
(#131008,#131009),(#131010,#131011),(#131012,#131013),(#131014,#131015),
(#131016,#131017),(#131018,#131019)),.UNSPECIFIED.,.F.,.F.,.F.)
B_SPLINE_SURFACE_WITH_KNOTS((6,1,1,1,1,1,1,1,1,1,1,1,1,1,1,1,1,1,1,1,1,
1,1,1,1,1,1,1,1,1,1,1,1,1,1,1,1,1,1,1,1,1,1,1,1,1,1,1,1,1,1,1,1,1,1,1,1,
1,1,1,1,1,1,1,1,1,1,1,1,1,1,1,1,1,1,1,1,1,1,1,1,1,1,1,1,1,1,1,1,1,1,1,1,
1,1,1,1,1,1,1,1,1,1,1,1,1,1,1,1,1,1,1,1,1,1,1,1,1,1,1,1,1,1,1,1,1,1,1,1,
1,1,1,1,1,1,1,1,1,1,1,1,1,1,1,1,1,1,1,1,1,1,1,1,1,1,1,1,1,1,1,1,1,1,1,1,
1,1,1,1,1,1,1,1,1,1,1,1,1,1,1,1,1,1,1,1,1,1,1,1,1,1,1,1,1,1,1,1,1,1,1,6),
(2,2),(-1.,-0.995000000000001,-0.990000000000001,-0.985000000000001,-0.980000000000001,
-0.975000000000001,-0.970000000000001,-0.965000000000001,-0.960000000000001,
-0.955000000000001,-0.950000000000001,-0.945000000000001,-0.940000000000001,
-0.935000000000001,-0.930000000000001,-0.925000000000001,-0.920000000000001,
-0.915000000000001,-0.910000000000001,-0.905000000000001,-0.900000000000001,
-0.895000000000001,-0.890000000000001,-0.885000000000001,-0.880000000000001,
-0.875000000000001,-0.870000000000001,-0.865000000000001,-0.860000000000001,
-0.855000000000001,-0.850000000000001,-0.845000000000001,-0.840000000000001,
-0.835000000000001,-0.830000000000001,-0.825000000000001,-0.820000000000001,
-0.815000000000001,-0.810000000000001,-0.805000000000001,-0.800000000000001,
-0.795000000000001,-0.790000000000001,-0.785000000000001,-0.780000000000001,
-0.775000000000001,-0.770000000000001,-0.765000000000001,-0.760000000000001,
-0.755000000000001,-0.750000000000001,-0.745000000000001,-0.740000000000001,
-0.735000000000001,-0.730000000000001,-0.725000000000001,-0.720000000000001,
-0.715000000000001,-0.710000000000001,-0.705000000000001,-0.700000000000001,
-0.695000000000001,-0.690000000000001,-0.685,-0.68,-0.675,-0.67,-0.665,
-0.66,-0.655,-0.65,-0.645,-0.64,-0.635,-0.63,-0.625,-0.62,-0.615,-0.61,
-0.605,-0.6,-0.595,-0.59,-0.585,-0.58,-0.575,-0.57,-0.565,-0.56,-0.555,
-0.55,-0.545,-0.54,-0.535,-0.53,-0.525,-0.52,-0.515,-0.51,-0.505,-0.5,-0.495,
-0.49,-0.485,-0.48,-0.475,-0.47,-0.465,-0.46,-0.455,-0.45,-0.445,-0.44,
-0.435,-0.43,-0.425,-0.42,-0.415,-0.41,-0.405,-0.4,-0.395,-0.39,-0.385,
-0.38,-0.375,-0.37,-0.365,-0.36,-0.355,-0.35,-0.345,-0.34,-0.335,-0.33,
-0.325,-0.32,-0.315,-0.31,-0.305,-0.3,-0.295,-0.29,-0.285,-0.28,-0.275,
-0.27,-0.265,-0.26,-0.255,-0.25,-0.245,-0.24,-0.235,-0.23,-0.225,-0.22,
-0.215,-0.21,-0.205,-0.2,-0.195,-0.19,-0.185,-0.18,-0.175,-0.17,-0.165,
-0.16,-0.155,-0.15,-0.145,-0.14,-0.135,-0.13,-0.125,-0.12,-0.115,-0.11,
-0.105,-0.1,-0.095,-0.09,-0.085,-0.08,-0.075,-0.07,-0.065,-0.06,-0.055,
-0.05,-0.045,-0.04,-0.035,-0.03,-0.025,-0.02,-0.015,-0.01,-0.005,0.),(0.,
1.2),.UNSPECIFIED.)
GEOMETRIC_REPRESENTATION_ITEM()
RATIONAL_B_SPLINE_SURFACE(((1.,1.),(1.,1.),(1.,1.),(1.,1.),(1.,1.),(1.,
1.),(1.,1.),(1.,1.),(1.,1.),(1.,1.),(1.,1.),(1.,1.),(1.,1.),(1.,1.),(1.,
1.),(1.,1.),(1.,1.),(1.,1.),(1.,1.),(1.,1.),(1.,1.),(1.,1.),(1.,1.),(1.,
1.),(1.,1.),(1.,1.),(1.,1.),(1.,1.),(1.,1.),(1.,1.),(1.,1.),(1.,1.),(1.,
1.),(1.,1.),(1.,1.),(1.,1.),(1.,1.),(1.,1.),(1.,1.),(1.,1.),(1.,1.),(1.,
1.),(1.,1.),(1.,1.),(1.,1.),(1.,1.),(1.,1.),(1.,1.),(1.,1.),(1.,1.),(1.,
1.),(1.,1.),(1.,1.),(1.,1.),(1.,1.),(1.,1.),(1.,1.),(1.,1.),(1.,1.),(1.,
1.),(1.,1.),(1.,1.),(1.,1.),(1.,1.),(1.,1.),(1.,1.),(1.,1.),(1.,1.),(1.,
1.),(1.,1.),(1.,1.),(1.,1.),(1.,1.),(1.,1.),(1.,1.),(1.,1.),(1.,1.),(1.,
1.),(1.,1.),(1.,1.),(1.,1.),(1.,1.),(1.,1.),(1.,1.),(1.,1.),(1.,1.),(1.,
1.),(1.,1.),(1.,1.),(1.,1.),(1.,1.),(1.,1.),(1.,1.),(1.,1.),(1.,1.),(1.,
1.),(1.,1.),(1.,1.),(1.,1.),(1.,1.),(1.,1.),(1.,1.),(1.,1.),(1.,1.),(1.,
1.),(1.,1.),(1.,1.),(1.,1.),(1.,1.),(1.,1.),(1.,1.),(1.,1.),(1.,1.),(1.,
1.),(1.,1.),(1.,1.),(1.,1.),(1.,1.),(1.,1.),(1.,1.),(1.,1.),(1.,1.),(1.,
1.),(1.,1.),(1.,1.),(1.,1.),(1.,1.),(1.,1.),(1.,1.),(1.,1.),(1.,1.),(1.,
1.),(1.,1.),(1.,1.),(1.,1.),(1.,1.),(1.,1.),(1.,1.),(1.,1.),(1.,1.),(1.,
1.),(1.,1.),(1.,1.),(1.,1.),(1.,1.),(1.,1.),(1.,1.),(1.,1.),(1.,1.),(1.,
1.),(1.,1.),(1.,1.),(1.,1.),(1.,1.),(1.,1.),(1.,1.),(1.,1.),(1.,1.),(1.,
1.),(1.,1.),(1.,1.),(1.,1.),(1.,1.),(1.,1.),(1.,1.),(1.,1.),(1.,1.),(1.,
1.),(1.,1.),(1.,1.),(1.,1.),(1.,1.),(1.,1.),(1.,1.),(1.,1.),(1.,1.),(1.,
1.),(1.,1.),(1.,1.),(1.,1.),(1.,1.),(1.,1.),(1.,1.),(1.,1.),(1.,1.),(1.,
1.),(1.,1.),(1.,1.),(1.,1.),(1.,1.),(1.,1.),(1.,1.),(1.,1.),(1.,1.),(1.,
1.),(1.,1.),(1.,1.),(1.,1.),(1.,1.),(1.,1.),(1.,1.),(1.,1.),(1.,1.),(1.,
1.),(1.,1.)))
REPRESENTATION_ITEM('')
SURFACE()
);
#973=(
BOUNDED_SURFACE()
B_SPLINE_SURFACE(5,1,((#131411,#131412),(#131413,#131414),(#131415,#131416),
(#131417,#131418),(#131419,#131420),(#131421,#131422),(#131423,#131424),
(#131425,#131426),(#131427,#131428),(#131429,#131430),(#131431,#131432),
(#131433,#131434),(#131435,#131436),(#131437,#131438),(#131439,#131440),
(#131441,#131442),(#131443,#131444),(#131445,#131446),(#131447,#131448),
(#131449,#131450),(#131451,#131452),(#131453,#131454),(#131455,#131456),
(#131457,#131458),(#131459,#131460),(#131461,#131462),(#131463,#131464),
(#131465,#131466),(#131467,#131468),(#131469,#131470),(#131471,#131472),
(#131473,#131474),(#131475,#131476),(#131477,#131478),(#131479,#131480),
(#131481,#131482),(#131483,#131484),(#131485,#131486),(#131487,#131488),
(#131489,#131490),(#131491,#131492),(#131493,#131494),(#131495,#131496),
(#131497,#131498),(#131499,#131500),(#131501,#131502),(#131503,#131504),
(#131505,#131506),(#131507,#131508),(#131509,#131510),(#131511,#131512),
(#131513,#131514),(#131515,#131516),(#131517,#131518),(#131519,#131520),
(#131521,#131522),(#131523,#131524),(#131525,#131526),(#131527,#131528),
(#131529,#131530),(#131531,#131532),(#131533,#131534),(#131535,#131536),
(#131537,#131538),(#131539,#131540),(#131541,#131542),(#131543,#131544),
(#131545,#131546),(#131547,#131548),(#131549,#131550),(#131551,#131552),
(#131553,#131554),(#131555,#131556),(#131557,#131558),(#131559,#131560),
(#131561,#131562),(#131563,#131564),(#131565,#131566),(#131567,#131568),
(#131569,#131570),(#131571,#131572),(#131573,#131574),(#131575,#131576),
(#131577,#131578),(#131579,#131580),(#131581,#131582),(#131583,#131584),
(#131585,#131586),(#131587,#131588),(#131589,#131590),(#131591,#131592),
(#131593,#131594),(#131595,#131596),(#131597,#131598),(#131599,#131600),
(#131601,#131602),(#131603,#131604),(#131605,#131606),(#131607,#131608),
(#131609,#131610),(#131611,#131612),(#131613,#131614),(#131615,#131616),
(#131617,#131618),(#131619,#131620),(#131621,#131622),(#131623,#131624),
(#131625,#131626),(#131627,#131628),(#131629,#131630),(#131631,#131632),
(#131633,#131634),(#131635,#131636),(#131637,#131638),(#131639,#131640),
(#131641,#131642),(#131643,#131644),(#131645,#131646),(#131647,#131648),
(#131649,#131650),(#131651,#131652),(#131653,#131654),(#131655,#131656),
(#131657,#131658),(#131659,#131660),(#131661,#131662),(#131663,#131664),
(#131665,#131666),(#131667,#131668),(#131669,#131670),(#131671,#131672),
(#131673,#131674),(#131675,#131676),(#131677,#131678),(#131679,#131680),
(#131681,#131682),(#131683,#131684),(#131685,#131686),(#131687,#131688),
(#131689,#131690),(#131691,#131692),(#131693,#131694),(#131695,#131696),
(#131697,#131698),(#131699,#131700),(#131701,#131702),(#131703,#131704),
(#131705,#131706),(#131707,#131708),(#131709,#131710),(#131711,#131712),
(#131713,#131714),(#131715,#131716),(#131717,#131718),(#131719,#131720),
(#131721,#131722),(#131723,#131724),(#131725,#131726),(#131727,#131728),
(#131729,#131730),(#131731,#131732),(#131733,#131734),(#131735,#131736),
(#131737,#131738),(#131739,#131740),(#131741,#131742),(#131743,#131744),
(#131745,#131746),(#131747,#131748),(#131749,#131750),(#131751,#131752),
(#131753,#131754),(#131755,#131756),(#131757,#131758),(#131759,#131760),
(#131761,#131762),(#131763,#131764),(#131765,#131766),(#131767,#131768),
(#131769,#131770),(#131771,#131772),(#131773,#131774),(#131775,#131776),
(#131777,#131778),(#131779,#131780),(#131781,#131782),(#131783,#131784),
(#131785,#131786),(#131787,#131788),(#131789,#131790),(#131791,#131792),
(#131793,#131794),(#131795,#131796),(#131797,#131798),(#131799,#131800),
(#131801,#131802),(#131803,#131804),(#131805,#131806),(#131807,#131808),
(#131809,#131810),(#131811,#131812),(#131813,#131814),(#131815,#131816),
(#131817,#131818),(#131819,#131820)),.UNSPECIFIED.,.F.,.F.,.F.)
B_SPLINE_SURFACE_WITH_KNOTS((6,1,1,1,1,1,1,1,1,1,1,1,1,1,1,1,1,1,1,1,1,
1,1,1,1,1,1,1,1,1,1,1,1,1,1,1,1,1,1,1,1,1,1,1,1,1,1,1,1,1,1,1,1,1,1,1,1,
1,1,1,1,1,1,1,1,1,1,1,1,1,1,1,1,1,1,1,1,1,1,1,1,1,1,1,1,1,1,1,1,1,1,1,1,
1,1,1,1,1,1,1,1,1,1,1,1,1,1,1,1,1,1,1,1,1,1,1,1,1,1,1,1,1,1,1,1,1,1,1,1,
1,1,1,1,1,1,1,1,1,1,1,1,1,1,1,1,1,1,1,1,1,1,1,1,1,1,1,1,1,1,1,1,1,1,1,1,
1,1,1,1,1,1,1,1,1,1,1,1,1,1,1,1,1,1,1,1,1,1,1,1,1,1,1,1,1,1,1,1,1,1,1,6),
(2,2),(-1.,-0.995000000000001,-0.990000000000001,-0.985000000000001,-0.980000000000001,
-0.975000000000001,-0.970000000000001,-0.965000000000001,-0.960000000000001,
-0.955000000000001,-0.950000000000001,-0.945000000000001,-0.940000000000001,
-0.935000000000001,-0.930000000000001,-0.925000000000001,-0.920000000000001,
-0.915000000000001,-0.910000000000001,-0.905000000000001,-0.900000000000001,
-0.895000000000001,-0.890000000000001,-0.885000000000001,-0.880000000000001,
-0.875000000000001,-0.870000000000001,-0.865000000000001,-0.860000000000001,
-0.855000000000001,-0.850000000000001,-0.845000000000001,-0.840000000000001,
-0.835000000000001,-0.830000000000001,-0.825000000000001,-0.820000000000001,
-0.815000000000001,-0.810000000000001,-0.805000000000001,-0.800000000000001,
-0.795000000000001,-0.790000000000001,-0.785000000000001,-0.780000000000001,
-0.775000000000001,-0.770000000000001,-0.765000000000001,-0.760000000000001,
-0.755000000000001,-0.750000000000001,-0.745000000000001,-0.740000000000001,
-0.735000000000001,-0.730000000000001,-0.725000000000001,-0.720000000000001,
-0.715000000000001,-0.710000000000001,-0.705000000000001,-0.700000000000001,
-0.695000000000001,-0.690000000000001,-0.685,-0.68,-0.675,-0.67,-0.665,
-0.66,-0.655,-0.65,-0.645,-0.64,-0.635,-0.63,-0.625,-0.62,-0.615,-0.61,
-0.605,-0.6,-0.595,-0.59,-0.585,-0.58,-0.575,-0.57,-0.565,-0.56,-0.555,
-0.55,-0.545,-0.54,-0.535,-0.53,-0.525,-0.52,-0.515,-0.51,-0.505,-0.5,-0.495,
-0.49,-0.485,-0.48,-0.475,-0.47,-0.465,-0.46,-0.455,-0.45,-0.445,-0.44,
-0.435,-0.43,-0.425,-0.42,-0.415,-0.41,-0.405,-0.4,-0.395,-0.39,-0.385,
-0.38,-0.375,-0.37,-0.365,-0.36,-0.355,-0.35,-0.345,-0.34,-0.335,-0.33,
-0.325,-0.32,-0.315,-0.31,-0.305,-0.3,-0.295,-0.29,-0.285,-0.28,-0.275,
-0.27,-0.265,-0.26,-0.255,-0.25,-0.245,-0.24,-0.235,-0.23,-0.225,-0.22,
-0.215,-0.21,-0.205,-0.2,-0.195,-0.19,-0.185,-0.18,-0.175,-0.17,-0.165,
-0.16,-0.155,-0.15,-0.145,-0.14,-0.135,-0.13,-0.125,-0.12,-0.115,-0.11,
-0.105,-0.1,-0.095,-0.09,-0.085,-0.08,-0.075,-0.07,-0.065,-0.06,-0.055,
-0.05,-0.045,-0.04,-0.035,-0.03,-0.025,-0.02,-0.015,-0.01,-0.005,0.),(0.,
1.2),.UNSPECIFIED.)
GEOMETRIC_REPRESENTATION_ITEM()
RATIONAL_B_SPLINE_SURFACE(((1.,1.),(1.,1.),(1.,1.),(1.,1.),(1.,1.),(1.,
1.),(1.,1.),(1.,1.),(1.,1.),(1.,1.),(1.,1.),(1.,1.),(1.,1.),(1.,1.),(1.,
1.),(1.,1.),(1.,1.),(1.,1.),(1.,1.),(1.,1.),(1.,1.),(1.,1.),(1.,1.),(1.,
1.),(1.,1.),(1.,1.),(1.,1.),(1.,1.),(1.,1.),(1.,1.),(1.,1.),(1.,1.),(1.,
1.),(1.,1.),(1.,1.),(1.,1.),(1.,1.),(1.,1.),(1.,1.),(1.,1.),(1.,1.),(1.,
1.),(1.,1.),(1.,1.),(1.,1.),(1.,1.),(1.,1.),(1.,1.),(1.,1.),(1.,1.),(1.,
1.),(1.,1.),(1.,1.),(1.,1.),(1.,1.),(1.,1.),(1.,1.),(1.,1.),(1.,1.),(1.,
1.),(1.,1.),(1.,1.),(1.,1.),(1.,1.),(1.,1.),(1.,1.),(1.,1.),(1.,1.),(1.,
1.),(1.,1.),(1.,1.),(1.,1.),(1.,1.),(1.,1.),(1.,1.),(1.,1.),(1.,1.),(1.,
1.),(1.,1.),(1.,1.),(1.,1.),(1.,1.),(1.,1.),(1.,1.),(1.,1.),(1.,1.),(1.,
1.),(1.,1.),(1.,1.),(1.,1.),(1.,1.),(1.,1.),(1.,1.),(1.,1.),(1.,1.),(1.,
1.),(1.,1.),(1.,1.),(1.,1.),(1.,1.),(1.,1.),(1.,1.),(1.,1.),(1.,1.),(1.,
1.),(1.,1.),(1.,1.),(1.,1.),(1.,1.),(1.,1.),(1.,1.),(1.,1.),(1.,1.),(1.,
1.),(1.,1.),(1.,1.),(1.,1.),(1.,1.),(1.,1.),(1.,1.),(1.,1.),(1.,1.),(1.,
1.),(1.,1.),(1.,1.),(1.,1.),(1.,1.),(1.,1.),(1.,1.),(1.,1.),(1.,1.),(1.,
1.),(1.,1.),(1.,1.),(1.,1.),(1.,1.),(1.,1.),(1.,1.),(1.,1.),(1.,1.),(1.,
1.),(1.,1.),(1.,1.),(1.,1.),(1.,1.),(1.,1.),(1.,1.),(1.,1.),(1.,1.),(1.,
1.),(1.,1.),(1.,1.),(1.,1.),(1.,1.),(1.,1.),(1.,1.),(1.,1.),(1.,1.),(1.,
1.),(1.,1.),(1.,1.),(1.,1.),(1.,1.),(1.,1.),(1.,1.),(1.,1.),(1.,1.),(1.,
1.),(1.,1.),(1.,1.),(1.,1.),(1.,1.),(1.,1.),(1.,1.),(1.,1.),(1.,1.),(1.,
1.),(1.,1.),(1.,1.),(1.,1.),(1.,1.),(1.,1.),(1.,1.),(1.,1.),(1.,1.),(1.,
1.),(1.,1.),(1.,1.),(1.,1.),(1.,1.),(1.,1.),(1.,1.),(1.,1.),(1.,1.),(1.,
1.),(1.,1.),(1.,1.),(1.,1.),(1.,1.),(1.,1.),(1.,1.),(1.,1.),(1.,1.),(1.,
1.),(1.,1.)))
REPRESENTATION_ITEM('')
SURFACE()
);
#974=(
BOUNDED_SURFACE()
B_SPLINE_SURFACE(5,1,((#132212,#132213),(#132214,#132215),(#132216,#132217),
(#132218,#132219),(#132220,#132221),(#132222,#132223),(#132224,#132225),
(#132226,#132227),(#132228,#132229),(#132230,#132231),(#132232,#132233),
(#132234,#132235),(#132236,#132237),(#132238,#132239),(#132240,#132241),
(#132242,#132243),(#132244,#132245),(#132246,#132247),(#132248,#132249),
(#132250,#132251),(#132252,#132253),(#132254,#132255),(#132256,#132257),
(#132258,#132259),(#132260,#132261),(#132262,#132263),(#132264,#132265),
(#132266,#132267),(#132268,#132269),(#132270,#132271),(#132272,#132273),
(#132274,#132275),(#132276,#132277),(#132278,#132279),(#132280,#132281),
(#132282,#132283),(#132284,#132285),(#132286,#132287),(#132288,#132289),
(#132290,#132291),(#132292,#132293),(#132294,#132295),(#132296,#132297),
(#132298,#132299),(#132300,#132301),(#132302,#132303),(#132304,#132305),
(#132306,#132307),(#132308,#132309),(#132310,#132311),(#132312,#132313),
(#132314,#132315),(#132316,#132317),(#132318,#132319),(#132320,#132321),
(#132322,#132323),(#132324,#132325),(#132326,#132327),(#132328,#132329),
(#132330,#132331),(#132332,#132333),(#132334,#132335),(#132336,#132337),
(#132338,#132339),(#132340,#132341),(#132342,#132343),(#132344,#132345),
(#132346,#132347),(#132348,#132349),(#132350,#132351),(#132352,#132353),
(#132354,#132355),(#132356,#132357),(#132358,#132359),(#132360,#132361),
(#132362,#132363),(#132364,#132365),(#132366,#132367),(#132368,#132369),
(#132370,#132371),(#132372,#132373),(#132374,#132375),(#132376,#132377),
(#132378,#132379),(#132380,#132381),(#132382,#132383),(#132384,#132385),
(#132386,#132387),(#132388,#132389),(#132390,#132391),(#132392,#132393),
(#132394,#132395),(#132396,#132397),(#132398,#132399),(#132400,#132401),
(#132402,#132403),(#132404,#132405),(#132406,#132407),(#132408,#132409),
(#132410,#132411),(#132412,#132413),(#132414,#132415),(#132416,#132417),
(#132418,#132419),(#132420,#132421),(#132422,#132423),(#132424,#132425),
(#132426,#132427),(#132428,#132429),(#132430,#132431),(#132432,#132433),
(#132434,#132435),(#132436,#132437),(#132438,#132439),(#132440,#132441),
(#132442,#132443),(#132444,#132445),(#132446,#132447),(#132448,#132449),
(#132450,#132451),(#132452,#132453),(#132454,#132455),(#132456,#132457),
(#132458,#132459),(#132460,#132461),(#132462,#132463),(#132464,#132465),
(#132466,#132467),(#132468,#132469),(#132470,#132471),(#132472,#132473),
(#132474,#132475),(#132476,#132477),(#132478,#132479),(#132480,#132481),
(#132482,#132483),(#132484,#132485),(#132486,#132487),(#132488,#132489),
(#132490,#132491),(#132492,#132493),(#132494,#132495),(#132496,#132497),
(#132498,#132499),(#132500,#132501),(#132502,#132503),(#132504,#132505),
(#132506,#132507),(#132508,#132509),(#132510,#132511),(#132512,#132513),
(#132514,#132515),(#132516,#132517),(#132518,#132519),(#132520,#132521),
(#132522,#132523),(#132524,#132525),(#132526,#132527),(#132528,#132529),
(#132530,#132531),(#132532,#132533),(#132534,#132535),(#132536,#132537),
(#132538,#132539),(#132540,#132541),(#132542,#132543),(#132544,#132545),
(#132546,#132547),(#132548,#132549),(#132550,#132551),(#132552,#132553),
(#132554,#132555),(#132556,#132557),(#132558,#132559),(#132560,#132561),
(#132562,#132563),(#132564,#132565),(#132566,#132567),(#132568,#132569),
(#132570,#132571),(#132572,#132573),(#132574,#132575),(#132576,#132577),
(#132578,#132579),(#132580,#132581),(#132582,#132583),(#132584,#132585),
(#132586,#132587),(#132588,#132589),(#132590,#132591),(#132592,#132593),
(#132594,#132595),(#132596,#132597),(#132598,#132599),(#132600,#132601),
(#132602,#132603),(#132604,#132605),(#132606,#132607),(#132608,#132609),
(#132610,#132611),(#132612,#132613),(#132614,#132615),(#132616,#132617),
(#132618,#132619),(#132620,#132621)),.UNSPECIFIED.,.F.,.F.,.F.)
B_SPLINE_SURFACE_WITH_KNOTS((6,1,1,1,1,1,1,1,1,1,1,1,1,1,1,1,1,1,1,1,1,
1,1,1,1,1,1,1,1,1,1,1,1,1,1,1,1,1,1,1,1,1,1,1,1,1,1,1,1,1,1,1,1,1,1,1,1,
1,1,1,1,1,1,1,1,1,1,1,1,1,1,1,1,1,1,1,1,1,1,1,1,1,1,1,1,1,1,1,1,1,1,1,1,
1,1,1,1,1,1,1,1,1,1,1,1,1,1,1,1,1,1,1,1,1,1,1,1,1,1,1,1,1,1,1,1,1,1,1,1,
1,1,1,1,1,1,1,1,1,1,1,1,1,1,1,1,1,1,1,1,1,1,1,1,1,1,1,1,1,1,1,1,1,1,1,1,
1,1,1,1,1,1,1,1,1,1,1,1,1,1,1,1,1,1,1,1,1,1,1,1,1,1,1,1,1,1,1,1,1,1,1,6),
(2,2),(-1.,-0.995000000000001,-0.990000000000001,-0.985000000000001,-0.980000000000001,
-0.975000000000001,-0.970000000000001,-0.965000000000001,-0.960000000000001,
-0.955000000000001,-0.950000000000001,-0.945000000000001,-0.940000000000001,
-0.935000000000001,-0.930000000000001,-0.925000000000001,-0.920000000000001,
-0.915000000000001,-0.910000000000001,-0.905000000000001,-0.900000000000001,
-0.895000000000001,-0.890000000000001,-0.885000000000001,-0.880000000000001,
-0.875000000000001,-0.870000000000001,-0.865000000000001,-0.860000000000001,
-0.855000000000001,-0.850000000000001,-0.845000000000001,-0.840000000000001,
-0.835000000000001,-0.830000000000001,-0.825000000000001,-0.820000000000001,
-0.815000000000001,-0.810000000000001,-0.805000000000001,-0.800000000000001,
-0.795000000000001,-0.790000000000001,-0.785000000000001,-0.780000000000001,
-0.775000000000001,-0.770000000000001,-0.765000000000001,-0.760000000000001,
-0.755000000000001,-0.750000000000001,-0.745000000000001,-0.740000000000001,
-0.735000000000001,-0.730000000000001,-0.725000000000001,-0.720000000000001,
-0.715000000000001,-0.710000000000001,-0.705000000000001,-0.700000000000001,
-0.695000000000001,-0.690000000000001,-0.685,-0.68,-0.675,-0.67,-0.665,
-0.66,-0.655,-0.65,-0.645,-0.64,-0.635,-0.63,-0.625,-0.62,-0.615,-0.61,
-0.605,-0.6,-0.595,-0.59,-0.585,-0.58,-0.575,-0.57,-0.565,-0.56,-0.555,
-0.55,-0.545,-0.54,-0.535,-0.53,-0.525,-0.52,-0.515,-0.51,-0.505,-0.5,-0.495,
-0.49,-0.485,-0.48,-0.475,-0.47,-0.465,-0.46,-0.455,-0.45,-0.445,-0.44,
-0.435,-0.43,-0.425,-0.42,-0.415,-0.41,-0.405,-0.4,-0.395,-0.39,-0.385,
-0.38,-0.375,-0.37,-0.365,-0.36,-0.355,-0.35,-0.345,-0.34,-0.335,-0.33,
-0.325,-0.32,-0.315,-0.31,-0.305,-0.3,-0.295,-0.29,-0.285,-0.28,-0.275,
-0.27,-0.265,-0.26,-0.255,-0.25,-0.245,-0.24,-0.235,-0.23,-0.225,-0.22,
-0.215,-0.21,-0.205,-0.2,-0.195,-0.19,-0.185,-0.18,-0.175,-0.17,-0.165,
-0.16,-0.155,-0.15,-0.145,-0.14,-0.135,-0.13,-0.125,-0.12,-0.115,-0.11,
-0.105,-0.1,-0.095,-0.09,-0.085,-0.08,-0.075,-0.07,-0.065,-0.06,-0.055,
-0.05,-0.045,-0.04,-0.035,-0.03,-0.025,-0.02,-0.015,-0.01,-0.005,0.),(0.,
1.2),.UNSPECIFIED.)
GEOMETRIC_REPRESENTATION_ITEM()
RATIONAL_B_SPLINE_SURFACE(((1.,1.),(1.,1.),(1.,1.),(1.,1.),(1.,1.),(1.,
1.),(1.,1.),(1.,1.),(1.,1.),(1.,1.),(1.,1.),(1.,1.),(1.,1.),(1.,1.),(1.,
1.),(1.,1.),(1.,1.),(1.,1.),(1.,1.),(1.,1.),(1.,1.),(1.,1.),(1.,1.),(1.,
1.),(1.,1.),(1.,1.),(1.,1.),(1.,1.),(1.,1.),(1.,1.),(1.,1.),(1.,1.),(1.,
1.),(1.,1.),(1.,1.),(1.,1.),(1.,1.),(1.,1.),(1.,1.),(1.,1.),(1.,1.),(1.,
1.),(1.,1.),(1.,1.),(1.,1.),(1.,1.),(1.,1.),(1.,1.),(1.,1.),(1.,1.),(1.,
1.),(1.,1.),(1.,1.),(1.,1.),(1.,1.),(1.,1.),(1.,1.),(1.,1.),(1.,1.),(1.,
1.),(1.,1.),(1.,1.),(1.,1.),(1.,1.),(1.,1.),(1.,1.),(1.,1.),(1.,1.),(1.,
1.),(1.,1.),(1.,1.),(1.,1.),(1.,1.),(1.,1.),(1.,1.),(1.,1.),(1.,1.),(1.,
1.),(1.,1.),(1.,1.),(1.,1.),(1.,1.),(1.,1.),(1.,1.),(1.,1.),(1.,1.),(1.,
1.),(1.,1.),(1.,1.),(1.,1.),(1.,1.),(1.,1.),(1.,1.),(1.,1.),(1.,1.),(1.,
1.),(1.,1.),(1.,1.),(1.,1.),(1.,1.),(1.,1.),(1.,1.),(1.,1.),(1.,1.),(1.,
1.),(1.,1.),(1.,1.),(1.,1.),(1.,1.),(1.,1.),(1.,1.),(1.,1.),(1.,1.),(1.,
1.),(1.,1.),(1.,1.),(1.,1.),(1.,1.),(1.,1.),(1.,1.),(1.,1.),(1.,1.),(1.,
1.),(1.,1.),(1.,1.),(1.,1.),(1.,1.),(1.,1.),(1.,1.),(1.,1.),(1.,1.),(1.,
1.),(1.,1.),(1.,1.),(1.,1.),(1.,1.),(1.,1.),(1.,1.),(1.,1.),(1.,1.),(1.,
1.),(1.,1.),(1.,1.),(1.,1.),(1.,1.),(1.,1.),(1.,1.),(1.,1.),(1.,1.),(1.,
1.),(1.,1.),(1.,1.),(1.,1.),(1.,1.),(1.,1.),(1.,1.),(1.,1.),(1.,1.),(1.,
1.),(1.,1.),(1.,1.),(1.,1.),(1.,1.),(1.,1.),(1.,1.),(1.,1.),(1.,1.),(1.,
1.),(1.,1.),(1.,1.),(1.,1.),(1.,1.),(1.,1.),(1.,1.),(1.,1.),(1.,1.),(1.,
1.),(1.,1.),(1.,1.),(1.,1.),(1.,1.),(1.,1.),(1.,1.),(1.,1.),(1.,1.),(1.,
1.),(1.,1.),(1.,1.),(1.,1.),(1.,1.),(1.,1.),(1.,1.),(1.,1.),(1.,1.),(1.,
1.),(1.,1.),(1.,1.),(1.,1.),(1.,1.),(1.,1.),(1.,1.),(1.,1.),(1.,1.),(1.,
1.),(1.,1.)))
REPRESENTATION_ITEM('')
SURFACE()
);
#975=(
BOUNDED_SURFACE()
B_SPLINE_SURFACE(5,1,((#133013,#133014),(#133015,#133016),(#133017,#133018),
(#133019,#133020),(#133021,#133022),(#133023,#133024),(#133025,#133026),
(#133027,#133028),(#133029,#133030),(#133031,#133032),(#133033,#133034),
(#133035,#133036),(#133037,#133038),(#133039,#133040),(#133041,#133042),
(#133043,#133044),(#133045,#133046),(#133047,#133048),(#133049,#133050),
(#133051,#133052),(#133053,#133054),(#133055,#133056),(#133057,#133058),
(#133059,#133060),(#133061,#133062),(#133063,#133064),(#133065,#133066),
(#133067,#133068),(#133069,#133070),(#133071,#133072),(#133073,#133074),
(#133075,#133076),(#133077,#133078),(#133079,#133080),(#133081,#133082),
(#133083,#133084),(#133085,#133086),(#133087,#133088),(#133089,#133090),
(#133091,#133092),(#133093,#133094),(#133095,#133096),(#133097,#133098),
(#133099,#133100),(#133101,#133102),(#133103,#133104),(#133105,#133106),
(#133107,#133108),(#133109,#133110),(#133111,#133112),(#133113,#133114),
(#133115,#133116),(#133117,#133118),(#133119,#133120),(#133121,#133122),
(#133123,#133124),(#133125,#133126),(#133127,#133128),(#133129,#133130),
(#133131,#133132),(#133133,#133134),(#133135,#133136),(#133137,#133138),
(#133139,#133140),(#133141,#133142),(#133143,#133144),(#133145,#133146),
(#133147,#133148),(#133149,#133150),(#133151,#133152),(#133153,#133154),
(#133155,#133156),(#133157,#133158),(#133159,#133160),(#133161,#133162),
(#133163,#133164),(#133165,#133166),(#133167,#133168),(#133169,#133170),
(#133171,#133172),(#133173,#133174),(#133175,#133176),(#133177,#133178),
(#133179,#133180),(#133181,#133182),(#133183,#133184),(#133185,#133186),
(#133187,#133188),(#133189,#133190),(#133191,#133192),(#133193,#133194),
(#133195,#133196),(#133197,#133198),(#133199,#133200),(#133201,#133202),
(#133203,#133204),(#133205,#133206),(#133207,#133208),(#133209,#133210),
(#133211,#133212),(#133213,#133214),(#133215,#133216),(#133217,#133218),
(#133219,#133220),(#133221,#133222),(#133223,#133224),(#133225,#133226),
(#133227,#133228),(#133229,#133230),(#133231,#133232),(#133233,#133234),
(#133235,#133236),(#133237,#133238),(#133239,#133240),(#133241,#133242),
(#133243,#133244),(#133245,#133246),(#133247,#133248),(#133249,#133250),
(#133251,#133252),(#133253,#133254),(#133255,#133256),(#133257,#133258),
(#133259,#133260),(#133261,#133262),(#133263,#133264),(#133265,#133266),
(#133267,#133268),(#133269,#133270),(#133271,#133272),(#133273,#133274),
(#133275,#133276),(#133277,#133278),(#133279,#133280),(#133281,#133282),
(#133283,#133284),(#133285,#133286),(#133287,#133288),(#133289,#133290),
(#133291,#133292),(#133293,#133294),(#133295,#133296),(#133297,#133298),
(#133299,#133300),(#133301,#133302),(#133303,#133304),(#133305,#133306),
(#133307,#133308),(#133309,#133310),(#133311,#133312),(#133313,#133314),
(#133315,#133316),(#133317,#133318),(#133319,#133320),(#133321,#133322),
(#133323,#133324),(#133325,#133326),(#133327,#133328),(#133329,#133330),
(#133331,#133332),(#133333,#133334),(#133335,#133336),(#133337,#133338),
(#133339,#133340),(#133341,#133342),(#133343,#133344),(#133345,#133346),
(#133347,#133348),(#133349,#133350),(#133351,#133352),(#133353,#133354),
(#133355,#133356),(#133357,#133358),(#133359,#133360),(#133361,#133362),
(#133363,#133364),(#133365,#133366),(#133367,#133368),(#133369,#133370),
(#133371,#133372),(#133373,#133374),(#133375,#133376),(#133377,#133378),
(#133379,#133380),(#133381,#133382),(#133383,#133384),(#133385,#133386),
(#133387,#133388),(#133389,#133390),(#133391,#133392),(#133393,#133394),
(#133395,#133396),(#133397,#133398),(#133399,#133400),(#133401,#133402),
(#133403,#133404),(#133405,#133406),(#133407,#133408),(#133409,#133410),
(#133411,#133412),(#133413,#133414),(#133415,#133416),(#133417,#133418),
(#133419,#133420),(#133421,#133422)),.UNSPECIFIED.,.F.,.F.,.F.)
B_SPLINE_SURFACE_WITH_KNOTS((6,1,1,1,1,1,1,1,1,1,1,1,1,1,1,1,1,1,1,1,1,
1,1,1,1,1,1,1,1,1,1,1,1,1,1,1,1,1,1,1,1,1,1,1,1,1,1,1,1,1,1,1,1,1,1,1,1,
1,1,1,1,1,1,1,1,1,1,1,1,1,1,1,1,1,1,1,1,1,1,1,1,1,1,1,1,1,1,1,1,1,1,1,1,
1,1,1,1,1,1,1,1,1,1,1,1,1,1,1,1,1,1,1,1,1,1,1,1,1,1,1,1,1,1,1,1,1,1,1,1,
1,1,1,1,1,1,1,1,1,1,1,1,1,1,1,1,1,1,1,1,1,1,1,1,1,1,1,1,1,1,1,1,1,1,1,1,
1,1,1,1,1,1,1,1,1,1,1,1,1,1,1,1,1,1,1,1,1,1,1,1,1,1,1,1,1,1,1,1,1,1,1,6),
(2,2),(-1.,-0.995000000000001,-0.990000000000001,-0.985000000000001,-0.980000000000001,
-0.975000000000001,-0.970000000000001,-0.965000000000001,-0.960000000000001,
-0.955000000000001,-0.950000000000001,-0.945000000000001,-0.940000000000001,
-0.935000000000001,-0.930000000000001,-0.925000000000001,-0.920000000000001,
-0.915000000000001,-0.910000000000001,-0.905000000000001,-0.900000000000001,
-0.895000000000001,-0.890000000000001,-0.885000000000001,-0.880000000000001,
-0.875000000000001,-0.870000000000001,-0.865000000000001,-0.860000000000001,
-0.855000000000001,-0.850000000000001,-0.845000000000001,-0.840000000000001,
-0.835000000000001,-0.830000000000001,-0.825000000000001,-0.820000000000001,
-0.815000000000001,-0.810000000000001,-0.805000000000001,-0.800000000000001,
-0.795000000000001,-0.790000000000001,-0.785000000000001,-0.780000000000001,
-0.775000000000001,-0.770000000000001,-0.765000000000001,-0.760000000000001,
-0.755000000000001,-0.750000000000001,-0.745000000000001,-0.740000000000001,
-0.735000000000001,-0.730000000000001,-0.725000000000001,-0.720000000000001,
-0.715000000000001,-0.710000000000001,-0.705000000000001,-0.700000000000001,
-0.695000000000001,-0.690000000000001,-0.685,-0.68,-0.675,-0.67,-0.665,
-0.66,-0.655,-0.65,-0.645,-0.64,-0.635,-0.63,-0.625,-0.62,-0.615,-0.61,
-0.605,-0.6,-0.595,-0.59,-0.585,-0.58,-0.575,-0.57,-0.565,-0.56,-0.555,
-0.55,-0.545,-0.54,-0.535,-0.53,-0.525,-0.52,-0.515,-0.51,-0.505,-0.5,-0.495,
-0.49,-0.485,-0.48,-0.475,-0.47,-0.465,-0.46,-0.455,-0.45,-0.445,-0.44,
-0.435,-0.43,-0.425,-0.42,-0.415,-0.41,-0.405,-0.4,-0.395,-0.39,-0.385,
-0.38,-0.375,-0.37,-0.365,-0.36,-0.355,-0.35,-0.345,-0.34,-0.335,-0.33,
-0.325,-0.32,-0.315,-0.31,-0.305,-0.3,-0.295,-0.29,-0.285,-0.28,-0.275,
-0.27,-0.265,-0.26,-0.255,-0.25,-0.245,-0.24,-0.235,-0.23,-0.225,-0.22,
-0.215,-0.21,-0.205,-0.2,-0.195,-0.19,-0.185,-0.18,-0.175,-0.17,-0.165,
-0.16,-0.155,-0.15,-0.145,-0.14,-0.135,-0.13,-0.125,-0.12,-0.115,-0.11,
-0.105,-0.1,-0.095,-0.09,-0.085,-0.08,-0.075,-0.07,-0.065,-0.06,-0.055,
-0.05,-0.045,-0.04,-0.035,-0.03,-0.025,-0.02,-0.015,-0.01,-0.005,0.),(0.,
1.2),.UNSPECIFIED.)
GEOMETRIC_REPRESENTATION_ITEM()
RATIONAL_B_SPLINE_SURFACE(((1.,1.),(1.,1.),(1.,1.),(1.,1.),(1.,1.),(1.,
1.),(1.,1.),(1.,1.),(1.,1.),(1.,1.),(1.,1.),(1.,1.),(1.,1.),(1.,1.),(1.,
1.),(1.,1.),(1.,1.),(1.,1.),(1.,1.),(1.,1.),(1.,1.),(1.,1.),(1.,1.),(1.,
1.),(1.,1.),(1.,1.),(1.,1.),(1.,1.),(1.,1.),(1.,1.),(1.,1.),(1.,1.),(1.,
1.),(1.,1.),(1.,1.),(1.,1.),(1.,1.),(1.,1.),(1.,1.),(1.,1.),(1.,1.),(1.,
1.),(1.,1.),(1.,1.),(1.,1.),(1.,1.),(1.,1.),(1.,1.),(1.,1.),(1.,1.),(1.,
1.),(1.,1.),(1.,1.),(1.,1.),(1.,1.),(1.,1.),(1.,1.),(1.,1.),(1.,1.),(1.,
1.),(1.,1.),(1.,1.),(1.,1.),(1.,1.),(1.,1.),(1.,1.),(1.,1.),(1.,1.),(1.,
1.),(1.,1.),(1.,1.),(1.,1.),(1.,1.),(1.,1.),(1.,1.),(1.,1.),(1.,1.),(1.,
1.),(1.,1.),(1.,1.),(1.,1.),(1.,1.),(1.,1.),(1.,1.),(1.,1.),(1.,1.),(1.,
1.),(1.,1.),(1.,1.),(1.,1.),(1.,1.),(1.,1.),(1.,1.),(1.,1.),(1.,1.),(1.,
1.),(1.,1.),(1.,1.),(1.,1.),(1.,1.),(1.,1.),(1.,1.),(1.,1.),(1.,1.),(1.,
1.),(1.,1.),(1.,1.),(1.,1.),(1.,1.),(1.,1.),(1.,1.),(1.,1.),(1.,1.),(1.,
1.),(1.,1.),(1.,1.),(1.,1.),(1.,1.),(1.,1.),(1.,1.),(1.,1.),(1.,1.),(1.,
1.),(1.,1.),(1.,1.),(1.,1.),(1.,1.),(1.,1.),(1.,1.),(1.,1.),(1.,1.),(1.,
1.),(1.,1.),(1.,1.),(1.,1.),(1.,1.),(1.,1.),(1.,1.),(1.,1.),(1.,1.),(1.,
1.),(1.,1.),(1.,1.),(1.,1.),(1.,1.),(1.,1.),(1.,1.),(1.,1.),(1.,1.),(1.,
1.),(1.,1.),(1.,1.),(1.,1.),(1.,1.),(1.,1.),(1.,1.),(1.,1.),(1.,1.),(1.,
1.),(1.,1.),(1.,1.),(1.,1.),(1.,1.),(1.,1.),(1.,1.),(1.,1.),(1.,1.),(1.,
1.),(1.,1.),(1.,1.),(1.,1.),(1.,1.),(1.,1.),(1.,1.),(1.,1.),(1.,1.),(1.,
1.),(1.,1.),(1.,1.),(1.,1.),(1.,1.),(1.,1.),(1.,1.),(1.,1.),(1.,1.),(1.,
1.),(1.,1.),(1.,1.),(1.,1.),(1.,1.),(1.,1.),(1.,1.),(1.,1.),(1.,1.),(1.,
1.),(1.,1.),(1.,1.),(1.,1.),(1.,1.),(1.,1.),(1.,1.),(1.,1.),(1.,1.),(1.,
1.),(1.,1.)))
REPRESENTATION_ITEM('')
SURFACE()
);
#976=(
BOUNDED_SURFACE()
B_SPLINE_SURFACE(5,1,((#133814,#133815),(#133816,#133817),(#133818,#133819),
(#133820,#133821),(#133822,#133823),(#133824,#133825),(#133826,#133827),
(#133828,#133829),(#133830,#133831),(#133832,#133833),(#133834,#133835),
(#133836,#133837),(#133838,#133839),(#133840,#133841),(#133842,#133843),
(#133844,#133845),(#133846,#133847),(#133848,#133849),(#133850,#133851),
(#133852,#133853),(#133854,#133855),(#133856,#133857),(#133858,#133859),
(#133860,#133861),(#133862,#133863),(#133864,#133865),(#133866,#133867),
(#133868,#133869),(#133870,#133871),(#133872,#133873),(#133874,#133875),
(#133876,#133877),(#133878,#133879),(#133880,#133881),(#133882,#133883),
(#133884,#133885),(#133886,#133887),(#133888,#133889),(#133890,#133891),
(#133892,#133893),(#133894,#133895),(#133896,#133897),(#133898,#133899),
(#133900,#133901),(#133902,#133903),(#133904,#133905),(#133906,#133907),
(#133908,#133909),(#133910,#133911),(#133912,#133913),(#133914,#133915),
(#133916,#133917),(#133918,#133919),(#133920,#133921),(#133922,#133923),
(#133924,#133925),(#133926,#133927),(#133928,#133929),(#133930,#133931),
(#133932,#133933),(#133934,#133935),(#133936,#133937),(#133938,#133939),
(#133940,#133941),(#133942,#133943),(#133944,#133945),(#133946,#133947),
(#133948,#133949),(#133950,#133951),(#133952,#133953),(#133954,#133955),
(#133956,#133957),(#133958,#133959),(#133960,#133961),(#133962,#133963),
(#133964,#133965),(#133966,#133967),(#133968,#133969),(#133970,#133971),
(#133972,#133973),(#133974,#133975),(#133976,#133977),(#133978,#133979),
(#133980,#133981),(#133982,#133983),(#133984,#133985),(#133986,#133987),
(#133988,#133989),(#133990,#133991),(#133992,#133993),(#133994,#133995),
(#133996,#133997),(#133998,#133999),(#134000,#134001),(#134002,#134003),
(#134004,#134005),(#134006,#134007),(#134008,#134009),(#134010,#134011),
(#134012,#134013),(#134014,#134015),(#134016,#134017),(#134018,#134019),
(#134020,#134021),(#134022,#134023),(#134024,#134025),(#134026,#134027),
(#134028,#134029),(#134030,#134031),(#134032,#134033),(#134034,#134035),
(#134036,#134037),(#134038,#134039),(#134040,#134041),(#134042,#134043),
(#134044,#134045),(#134046,#134047),(#134048,#134049),(#134050,#134051),
(#134052,#134053),(#134054,#134055),(#134056,#134057),(#134058,#134059),
(#134060,#134061),(#134062,#134063),(#134064,#134065),(#134066,#134067),
(#134068,#134069),(#134070,#134071),(#134072,#134073),(#134074,#134075),
(#134076,#134077),(#134078,#134079),(#134080,#134081),(#134082,#134083),
(#134084,#134085),(#134086,#134087),(#134088,#134089),(#134090,#134091),
(#134092,#134093),(#134094,#134095),(#134096,#134097),(#134098,#134099),
(#134100,#134101),(#134102,#134103),(#134104,#134105),(#134106,#134107),
(#134108,#134109),(#134110,#134111),(#134112,#134113),(#134114,#134115),
(#134116,#134117),(#134118,#134119),(#134120,#134121),(#134122,#134123),
(#134124,#134125),(#134126,#134127),(#134128,#134129),(#134130,#134131),
(#134132,#134133),(#134134,#134135),(#134136,#134137),(#134138,#134139),
(#134140,#134141),(#134142,#134143),(#134144,#134145),(#134146,#134147),
(#134148,#134149),(#134150,#134151),(#134152,#134153),(#134154,#134155),
(#134156,#134157),(#134158,#134159),(#134160,#134161),(#134162,#134163),
(#134164,#134165),(#134166,#134167),(#134168,#134169),(#134170,#134171),
(#134172,#134173),(#134174,#134175),(#134176,#134177),(#134178,#134179),
(#134180,#134181),(#134182,#134183),(#134184,#134185),(#134186,#134187),
(#134188,#134189),(#134190,#134191),(#134192,#134193),(#134194,#134195),
(#134196,#134197),(#134198,#134199),(#134200,#134201),(#134202,#134203),
(#134204,#134205),(#134206,#134207),(#134208,#134209),(#134210,#134211),
(#134212,#134213),(#134214,#134215),(#134216,#134217),(#134218,#134219),
(#134220,#134221),(#134222,#134223)),.UNSPECIFIED.,.F.,.F.,.F.)
B_SPLINE_SURFACE_WITH_KNOTS((6,1,1,1,1,1,1,1,1,1,1,1,1,1,1,1,1,1,1,1,1,
1,1,1,1,1,1,1,1,1,1,1,1,1,1,1,1,1,1,1,1,1,1,1,1,1,1,1,1,1,1,1,1,1,1,1,1,
1,1,1,1,1,1,1,1,1,1,1,1,1,1,1,1,1,1,1,1,1,1,1,1,1,1,1,1,1,1,1,1,1,1,1,1,
1,1,1,1,1,1,1,1,1,1,1,1,1,1,1,1,1,1,1,1,1,1,1,1,1,1,1,1,1,1,1,1,1,1,1,1,
1,1,1,1,1,1,1,1,1,1,1,1,1,1,1,1,1,1,1,1,1,1,1,1,1,1,1,1,1,1,1,1,1,1,1,1,
1,1,1,1,1,1,1,1,1,1,1,1,1,1,1,1,1,1,1,1,1,1,1,1,1,1,1,1,1,1,1,1,1,1,1,6),
(2,2),(-1.,-0.995000000000001,-0.990000000000001,-0.985000000000001,-0.980000000000001,
-0.975000000000001,-0.970000000000001,-0.965000000000001,-0.960000000000001,
-0.955000000000001,-0.950000000000001,-0.945000000000001,-0.940000000000001,
-0.935000000000001,-0.930000000000001,-0.925000000000001,-0.920000000000001,
-0.915000000000001,-0.910000000000001,-0.905000000000001,-0.900000000000001,
-0.895000000000001,-0.890000000000001,-0.885000000000001,-0.880000000000001,
-0.875000000000001,-0.870000000000001,-0.865000000000001,-0.860000000000001,
-0.855000000000001,-0.850000000000001,-0.845000000000001,-0.840000000000001,
-0.835000000000001,-0.830000000000001,-0.825000000000001,-0.820000000000001,
-0.815000000000001,-0.810000000000001,-0.805000000000001,-0.800000000000001,
-0.795000000000001,-0.790000000000001,-0.785000000000001,-0.780000000000001,
-0.775000000000001,-0.770000000000001,-0.765000000000001,-0.760000000000001,
-0.755000000000001,-0.750000000000001,-0.745000000000001,-0.740000000000001,
-0.735000000000001,-0.730000000000001,-0.725000000000001,-0.720000000000001,
-0.715000000000001,-0.710000000000001,-0.705000000000001,-0.700000000000001,
-0.695000000000001,-0.690000000000001,-0.685,-0.68,-0.675,-0.67,-0.665,
-0.66,-0.655,-0.65,-0.645,-0.64,-0.635,-0.63,-0.625,-0.62,-0.615,-0.61,
-0.605,-0.6,-0.595,-0.59,-0.585,-0.58,-0.575,-0.57,-0.565,-0.56,-0.555,
-0.55,-0.545,-0.54,-0.535,-0.53,-0.525,-0.52,-0.515,-0.51,-0.505,-0.5,-0.495,
-0.49,-0.485,-0.48,-0.475,-0.47,-0.465,-0.46,-0.455,-0.45,-0.445,-0.44,
-0.435,-0.43,-0.425,-0.42,-0.415,-0.41,-0.405,-0.4,-0.395,-0.39,-0.385,
-0.38,-0.375,-0.37,-0.365,-0.36,-0.355,-0.35,-0.345,-0.34,-0.335,-0.33,
-0.325,-0.32,-0.315,-0.31,-0.305,-0.3,-0.295,-0.29,-0.285,-0.28,-0.275,
-0.27,-0.265,-0.26,-0.255,-0.25,-0.245,-0.24,-0.235,-0.23,-0.225,-0.22,
-0.215,-0.21,-0.205,-0.2,-0.195,-0.19,-0.185,-0.18,-0.175,-0.17,-0.165,
-0.16,-0.155,-0.15,-0.145,-0.14,-0.135,-0.13,-0.125,-0.12,-0.115,-0.11,
-0.105,-0.1,-0.095,-0.09,-0.085,-0.08,-0.075,-0.07,-0.065,-0.06,-0.055,
-0.05,-0.045,-0.04,-0.035,-0.03,-0.025,-0.02,-0.015,-0.01,-0.005,0.),(0.,
1.2),.UNSPECIFIED.)
GEOMETRIC_REPRESENTATION_ITEM()
RATIONAL_B_SPLINE_SURFACE(((1.,1.),(1.,1.),(1.,1.),(1.,1.),(1.,1.),(1.,
1.),(1.,1.),(1.,1.),(1.,1.),(1.,1.),(1.,1.),(1.,1.),(1.,1.),(1.,1.),(1.,
1.),(1.,1.),(1.,1.),(1.,1.),(1.,1.),(1.,1.),(1.,1.),(1.,1.),(1.,1.),(1.,
1.),(1.,1.),(1.,1.),(1.,1.),(1.,1.),(1.,1.),(1.,1.),(1.,1.),(1.,1.),(1.,
1.),(1.,1.),(1.,1.),(1.,1.),(1.,1.),(1.,1.),(1.,1.),(1.,1.),(1.,1.),(1.,
1.),(1.,1.),(1.,1.),(1.,1.),(1.,1.),(1.,1.),(1.,1.),(1.,1.),(1.,1.),(1.,
1.),(1.,1.),(1.,1.),(1.,1.),(1.,1.),(1.,1.),(1.,1.),(1.,1.),(1.,1.),(1.,
1.),(1.,1.),(1.,1.),(1.,1.),(1.,1.),(1.,1.),(1.,1.),(1.,1.),(1.,1.),(1.,
1.),(1.,1.),(1.,1.),(1.,1.),(1.,1.),(1.,1.),(1.,1.),(1.,1.),(1.,1.),(1.,
1.),(1.,1.),(1.,1.),(1.,1.),(1.,1.),(1.,1.),(1.,1.),(1.,1.),(1.,1.),(1.,
1.),(1.,1.),(1.,1.),(1.,1.),(1.,1.),(1.,1.),(1.,1.),(1.,1.),(1.,1.),(1.,
1.),(1.,1.),(1.,1.),(1.,1.),(1.,1.),(1.,1.),(1.,1.),(1.,1.),(1.,1.),(1.,
1.),(1.,1.),(1.,1.),(1.,1.),(1.,1.),(1.,1.),(1.,1.),(1.,1.),(1.,1.),(1.,
1.),(1.,1.),(1.,1.),(1.,1.),(1.,1.),(1.,1.),(1.,1.),(1.,1.),(1.,1.),(1.,
1.),(1.,1.),(1.,1.),(1.,1.),(1.,1.),(1.,1.),(1.,1.),(1.,1.),(1.,1.),(1.,
1.),(1.,1.),(1.,1.),(1.,1.),(1.,1.),(1.,1.),(1.,1.),(1.,1.),(1.,1.),(1.,
1.),(1.,1.),(1.,1.),(1.,1.),(1.,1.),(1.,1.),(1.,1.),(1.,1.),(1.,1.),(1.,
1.),(1.,1.),(1.,1.),(1.,1.),(1.,1.),(1.,1.),(1.,1.),(1.,1.),(1.,1.),(1.,
1.),(1.,1.),(1.,1.),(1.,1.),(1.,1.),(1.,1.),(1.,1.),(1.,1.),(1.,1.),(1.,
1.),(1.,1.),(1.,1.),(1.,1.),(1.,1.),(1.,1.),(1.,1.),(1.,1.),(1.,1.),(1.,
1.),(1.,1.),(1.,1.),(1.,1.),(1.,1.),(1.,1.),(1.,1.),(1.,1.),(1.,1.),(1.,
1.),(1.,1.),(1.,1.),(1.,1.),(1.,1.),(1.,1.),(1.,1.),(1.,1.),(1.,1.),(1.,
1.),(1.,1.),(1.,1.),(1.,1.),(1.,1.),(1.,1.),(1.,1.),(1.,1.),(1.,1.),(1.,
1.),(1.,1.)))
REPRESENTATION_ITEM('')
SURFACE()
);
#977=(
BOUNDED_SURFACE()
B_SPLINE_SURFACE(5,1,((#134615,#134616),(#134617,#134618),(#134619,#134620),
(#134621,#134622),(#134623,#134624),(#134625,#134626),(#134627,#134628),
(#134629,#134630),(#134631,#134632),(#134633,#134634),(#134635,#134636),
(#134637,#134638),(#134639,#134640),(#134641,#134642),(#134643,#134644),
(#134645,#134646),(#134647,#134648),(#134649,#134650),(#134651,#134652),
(#134653,#134654),(#134655,#134656),(#134657,#134658),(#134659,#134660),
(#134661,#134662),(#134663,#134664),(#134665,#134666),(#134667,#134668),
(#134669,#134670),(#134671,#134672),(#134673,#134674),(#134675,#134676),
(#134677,#134678),(#134679,#134680),(#134681,#134682),(#134683,#134684),
(#134685,#134686),(#134687,#134688),(#134689,#134690),(#134691,#134692),
(#134693,#134694),(#134695,#134696),(#134697,#134698),(#134699,#134700),
(#134701,#134702),(#134703,#134704),(#134705,#134706),(#134707,#134708),
(#134709,#134710),(#134711,#134712),(#134713,#134714),(#134715,#134716),
(#134717,#134718),(#134719,#134720),(#134721,#134722),(#134723,#134724),
(#134725,#134726),(#134727,#134728),(#134729,#134730),(#134731,#134732),
(#134733,#134734),(#134735,#134736),(#134737,#134738),(#134739,#134740),
(#134741,#134742),(#134743,#134744),(#134745,#134746),(#134747,#134748),
(#134749,#134750),(#134751,#134752),(#134753,#134754),(#134755,#134756),
(#134757,#134758),(#134759,#134760),(#134761,#134762),(#134763,#134764),
(#134765,#134766),(#134767,#134768),(#134769,#134770),(#134771,#134772),
(#134773,#134774),(#134775,#134776),(#134777,#134778),(#134779,#134780),
(#134781,#134782),(#134783,#134784),(#134785,#134786),(#134787,#134788),
(#134789,#134790),(#134791,#134792),(#134793,#134794),(#134795,#134796),
(#134797,#134798),(#134799,#134800),(#134801,#134802),(#134803,#134804),
(#134805,#134806),(#134807,#134808),(#134809,#134810),(#134811,#134812),
(#134813,#134814),(#134815,#134816),(#134817,#134818),(#134819,#134820),
(#134821,#134822),(#134823,#134824),(#134825,#134826),(#134827,#134828),
(#134829,#134830),(#134831,#134832),(#134833,#134834),(#134835,#134836),
(#134837,#134838),(#134839,#134840),(#134841,#134842),(#134843,#134844),
(#134845,#134846),(#134847,#134848),(#134849,#134850),(#134851,#134852),
(#134853,#134854),(#134855,#134856),(#134857,#134858),(#134859,#134860),
(#134861,#134862),(#134863,#134864),(#134865,#134866),(#134867,#134868),
(#134869,#134870),(#134871,#134872),(#134873,#134874),(#134875,#134876),
(#134877,#134878),(#134879,#134880),(#134881,#134882),(#134883,#134884),
(#134885,#134886),(#134887,#134888),(#134889,#134890),(#134891,#134892),
(#134893,#134894),(#134895,#134896),(#134897,#134898),(#134899,#134900),
(#134901,#134902),(#134903,#134904),(#134905,#134906),(#134907,#134908),
(#134909,#134910),(#134911,#134912),(#134913,#134914),(#134915,#134916),
(#134917,#134918),(#134919,#134920),(#134921,#134922),(#134923,#134924),
(#134925,#134926),(#134927,#134928),(#134929,#134930),(#134931,#134932),
(#134933,#134934),(#134935,#134936),(#134937,#134938),(#134939,#134940),
(#134941,#134942),(#134943,#134944),(#134945,#134946),(#134947,#134948),
(#134949,#134950),(#134951,#134952),(#134953,#134954),(#134955,#134956),
(#134957,#134958),(#134959,#134960),(#134961,#134962),(#134963,#134964),
(#134965,#134966),(#134967,#134968),(#134969,#134970),(#134971,#134972),
(#134973,#134974),(#134975,#134976),(#134977,#134978),(#134979,#134980),
(#134981,#134982),(#134983,#134984),(#134985,#134986),(#134987,#134988),
(#134989,#134990),(#134991,#134992),(#134993,#134994),(#134995,#134996),
(#134997,#134998),(#134999,#135000),(#135001,#135002),(#135003,#135004),
(#135005,#135006),(#135007,#135008),(#135009,#135010),(#135011,#135012),
(#135013,#135014),(#135015,#135016),(#135017,#135018),(#135019,#135020),
(#135021,#135022),(#135023,#135024)),.UNSPECIFIED.,.F.,.F.,.F.)
B_SPLINE_SURFACE_WITH_KNOTS((6,1,1,1,1,1,1,1,1,1,1,1,1,1,1,1,1,1,1,1,1,
1,1,1,1,1,1,1,1,1,1,1,1,1,1,1,1,1,1,1,1,1,1,1,1,1,1,1,1,1,1,1,1,1,1,1,1,
1,1,1,1,1,1,1,1,1,1,1,1,1,1,1,1,1,1,1,1,1,1,1,1,1,1,1,1,1,1,1,1,1,1,1,1,
1,1,1,1,1,1,1,1,1,1,1,1,1,1,1,1,1,1,1,1,1,1,1,1,1,1,1,1,1,1,1,1,1,1,1,1,
1,1,1,1,1,1,1,1,1,1,1,1,1,1,1,1,1,1,1,1,1,1,1,1,1,1,1,1,1,1,1,1,1,1,1,1,
1,1,1,1,1,1,1,1,1,1,1,1,1,1,1,1,1,1,1,1,1,1,1,1,1,1,1,1,1,1,1,1,1,1,1,6),
(2,2),(-1.,-0.995000000000001,-0.990000000000001,-0.985000000000001,-0.980000000000001,
-0.975000000000001,-0.970000000000001,-0.965000000000001,-0.960000000000001,
-0.955000000000001,-0.950000000000001,-0.945000000000001,-0.940000000000001,
-0.935000000000001,-0.930000000000001,-0.925000000000001,-0.920000000000001,
-0.915000000000001,-0.910000000000001,-0.905000000000001,-0.900000000000001,
-0.895000000000001,-0.890000000000001,-0.885000000000001,-0.880000000000001,
-0.875000000000001,-0.870000000000001,-0.865000000000001,-0.860000000000001,
-0.855000000000001,-0.850000000000001,-0.845000000000001,-0.840000000000001,
-0.835000000000001,-0.830000000000001,-0.825000000000001,-0.820000000000001,
-0.815000000000001,-0.810000000000001,-0.805000000000001,-0.800000000000001,
-0.795000000000001,-0.790000000000001,-0.785000000000001,-0.780000000000001,
-0.775000000000001,-0.770000000000001,-0.765000000000001,-0.760000000000001,
-0.755000000000001,-0.750000000000001,-0.745000000000001,-0.740000000000001,
-0.735000000000001,-0.730000000000001,-0.725000000000001,-0.720000000000001,
-0.715000000000001,-0.710000000000001,-0.705000000000001,-0.700000000000001,
-0.695000000000001,-0.690000000000001,-0.685,-0.68,-0.675,-0.67,-0.665,
-0.66,-0.655,-0.65,-0.645,-0.64,-0.635,-0.63,-0.625,-0.62,-0.615,-0.61,
-0.605,-0.6,-0.595,-0.59,-0.585,-0.58,-0.575,-0.57,-0.565,-0.56,-0.555,
-0.55,-0.545,-0.54,-0.535,-0.53,-0.525,-0.52,-0.515,-0.51,-0.505,-0.5,-0.495,
-0.49,-0.485,-0.48,-0.475,-0.47,-0.465,-0.46,-0.455,-0.45,-0.445,-0.44,
-0.435,-0.43,-0.425,-0.42,-0.415,-0.41,-0.405,-0.4,-0.395,-0.39,-0.385,
-0.38,-0.375,-0.37,-0.365,-0.36,-0.355,-0.35,-0.345,-0.34,-0.335,-0.33,
-0.325,-0.32,-0.315,-0.31,-0.305,-0.3,-0.295,-0.29,-0.285,-0.28,-0.275,
-0.27,-0.265,-0.26,-0.255,-0.25,-0.245,-0.24,-0.235,-0.23,-0.225,-0.22,
-0.215,-0.21,-0.205,-0.2,-0.195,-0.19,-0.185,-0.18,-0.175,-0.17,-0.165,
-0.16,-0.155,-0.15,-0.145,-0.14,-0.135,-0.13,-0.125,-0.12,-0.115,-0.11,
-0.105,-0.1,-0.095,-0.09,-0.085,-0.08,-0.075,-0.07,-0.065,-0.06,-0.055,
-0.05,-0.045,-0.04,-0.035,-0.03,-0.025,-0.02,-0.015,-0.01,-0.005,0.),(0.,
1.2),.UNSPECIFIED.)
GEOMETRIC_REPRESENTATION_ITEM()
RATIONAL_B_SPLINE_SURFACE(((1.,1.),(1.,1.),(1.,1.),(1.,1.),(1.,1.),(1.,
1.),(1.,1.),(1.,1.),(1.,1.),(1.,1.),(1.,1.),(1.,1.),(1.,1.),(1.,1.),(1.,
1.),(1.,1.),(1.,1.),(1.,1.),(1.,1.),(1.,1.),(1.,1.),(1.,1.),(1.,1.),(1.,
1.),(1.,1.),(1.,1.),(1.,1.),(1.,1.),(1.,1.),(1.,1.),(1.,1.),(1.,1.),(1.,
1.),(1.,1.),(1.,1.),(1.,1.),(1.,1.),(1.,1.),(1.,1.),(1.,1.),(1.,1.),(1.,
1.),(1.,1.),(1.,1.),(1.,1.),(1.,1.),(1.,1.),(1.,1.),(1.,1.),(1.,1.),(1.,
1.),(1.,1.),(1.,1.),(1.,1.),(1.,1.),(1.,1.),(1.,1.),(1.,1.),(1.,1.),(1.,
1.),(1.,1.),(1.,1.),(1.,1.),(1.,1.),(1.,1.),(1.,1.),(1.,1.),(1.,1.),(1.,
1.),(1.,1.),(1.,1.),(1.,1.),(1.,1.),(1.,1.),(1.,1.),(1.,1.),(1.,1.),(1.,
1.),(1.,1.),(1.,1.),(1.,1.),(1.,1.),(1.,1.),(1.,1.),(1.,1.),(1.,1.),(1.,
1.),(1.,1.),(1.,1.),(1.,1.),(1.,1.),(1.,1.),(1.,1.),(1.,1.),(1.,1.),(1.,
1.),(1.,1.),(1.,1.),(1.,1.),(1.,1.),(1.,1.),(1.,1.),(1.,1.),(1.,1.),(1.,
1.),(1.,1.),(1.,1.),(1.,1.),(1.,1.),(1.,1.),(1.,1.),(1.,1.),(1.,1.),(1.,
1.),(1.,1.),(1.,1.),(1.,1.),(1.,1.),(1.,1.),(1.,1.),(1.,1.),(1.,1.),(1.,
1.),(1.,1.),(1.,1.),(1.,1.),(1.,1.),(1.,1.),(1.,1.),(1.,1.),(1.,1.),(1.,
1.),(1.,1.),(1.,1.),(1.,1.),(1.,1.),(1.,1.),(1.,1.),(1.,1.),(1.,1.),(1.,
1.),(1.,1.),(1.,1.),(1.,1.),(1.,1.),(1.,1.),(1.,1.),(1.,1.),(1.,1.),(1.,
1.),(1.,1.),(1.,1.),(1.,1.),(1.,1.),(1.,1.),(1.,1.),(1.,1.),(1.,1.),(1.,
1.),(1.,1.),(1.,1.),(1.,1.),(1.,1.),(1.,1.),(1.,1.),(1.,1.),(1.,1.),(1.,
1.),(1.,1.),(1.,1.),(1.,1.),(1.,1.),(1.,1.),(1.,1.),(1.,1.),(1.,1.),(1.,
1.),(1.,1.),(1.,1.),(1.,1.),(1.,1.),(1.,1.),(1.,1.),(1.,1.),(1.,1.),(1.,
1.),(1.,1.),(1.,1.),(1.,1.),(1.,1.),(1.,1.),(1.,1.),(1.,1.),(1.,1.),(1.,
1.),(1.,1.),(1.,1.),(1.,1.),(1.,1.),(1.,1.),(1.,1.),(1.,1.),(1.,1.),(1.,
1.),(1.,1.)))
REPRESENTATION_ITEM('')
SURFACE()
);
#978=(
BOUNDED_SURFACE()
B_SPLINE_SURFACE(5,1,((#135416,#135417),(#135418,#135419),(#135420,#135421),
(#135422,#135423),(#135424,#135425),(#135426,#135427),(#135428,#135429),
(#135430,#135431),(#135432,#135433),(#135434,#135435),(#135436,#135437),
(#135438,#135439),(#135440,#135441),(#135442,#135443),(#135444,#135445),
(#135446,#135447),(#135448,#135449),(#135450,#135451),(#135452,#135453),
(#135454,#135455),(#135456,#135457),(#135458,#135459),(#135460,#135461),
(#135462,#135463),(#135464,#135465),(#135466,#135467),(#135468,#135469),
(#135470,#135471),(#135472,#135473),(#135474,#135475),(#135476,#135477),
(#135478,#135479),(#135480,#135481),(#135482,#135483),(#135484,#135485),
(#135486,#135487),(#135488,#135489),(#135490,#135491),(#135492,#135493),
(#135494,#135495),(#135496,#135497),(#135498,#135499),(#135500,#135501),
(#135502,#135503),(#135504,#135505),(#135506,#135507),(#135508,#135509),
(#135510,#135511),(#135512,#135513),(#135514,#135515),(#135516,#135517),
(#135518,#135519),(#135520,#135521),(#135522,#135523),(#135524,#135525),
(#135526,#135527),(#135528,#135529),(#135530,#135531),(#135532,#135533),
(#135534,#135535),(#135536,#135537),(#135538,#135539),(#135540,#135541),
(#135542,#135543),(#135544,#135545),(#135546,#135547),(#135548,#135549),
(#135550,#135551),(#135552,#135553),(#135554,#135555),(#135556,#135557),
(#135558,#135559),(#135560,#135561),(#135562,#135563),(#135564,#135565),
(#135566,#135567),(#135568,#135569),(#135570,#135571),(#135572,#135573),
(#135574,#135575),(#135576,#135577),(#135578,#135579),(#135580,#135581),
(#135582,#135583),(#135584,#135585),(#135586,#135587),(#135588,#135589),
(#135590,#135591),(#135592,#135593),(#135594,#135595),(#135596,#135597),
(#135598,#135599),(#135600,#135601),(#135602,#135603),(#135604,#135605),
(#135606,#135607),(#135608,#135609),(#135610,#135611),(#135612,#135613),
(#135614,#135615),(#135616,#135617),(#135618,#135619),(#135620,#135621),
(#135622,#135623),(#135624,#135625),(#135626,#135627),(#135628,#135629),
(#135630,#135631),(#135632,#135633),(#135634,#135635),(#135636,#135637),
(#135638,#135639),(#135640,#135641),(#135642,#135643),(#135644,#135645),
(#135646,#135647),(#135648,#135649),(#135650,#135651),(#135652,#135653),
(#135654,#135655),(#135656,#135657),(#135658,#135659),(#135660,#135661),
(#135662,#135663),(#135664,#135665),(#135666,#135667),(#135668,#135669),
(#135670,#135671),(#135672,#135673),(#135674,#135675),(#135676,#135677),
(#135678,#135679),(#135680,#135681),(#135682,#135683),(#135684,#135685),
(#135686,#135687),(#135688,#135689),(#135690,#135691),(#135692,#135693),
(#135694,#135695),(#135696,#135697),(#135698,#135699),(#135700,#135701),
(#135702,#135703),(#135704,#135705),(#135706,#135707),(#135708,#135709),
(#135710,#135711),(#135712,#135713),(#135714,#135715),(#135716,#135717),
(#135718,#135719),(#135720,#135721),(#135722,#135723),(#135724,#135725),
(#135726,#135727),(#135728,#135729),(#135730,#135731),(#135732,#135733),
(#135734,#135735),(#135736,#135737),(#135738,#135739),(#135740,#135741),
(#135742,#135743),(#135744,#135745),(#135746,#135747),(#135748,#135749),
(#135750,#135751),(#135752,#135753),(#135754,#135755),(#135756,#135757),
(#135758,#135759),(#135760,#135761),(#135762,#135763),(#135764,#135765),
(#135766,#135767),(#135768,#135769),(#135770,#135771),(#135772,#135773),
(#135774,#135775),(#135776,#135777),(#135778,#135779),(#135780,#135781),
(#135782,#135783),(#135784,#135785),(#135786,#135787),(#135788,#135789),
(#135790,#135791),(#135792,#135793),(#135794,#135795),(#135796,#135797),
(#135798,#135799),(#135800,#135801),(#135802,#135803),(#135804,#135805),
(#135806,#135807),(#135808,#135809),(#135810,#135811),(#135812,#135813),
(#135814,#135815),(#135816,#135817),(#135818,#135819),(#135820,#135821),
(#135822,#135823),(#135824,#135825)),.UNSPECIFIED.,.F.,.F.,.F.)
B_SPLINE_SURFACE_WITH_KNOTS((6,1,1,1,1,1,1,1,1,1,1,1,1,1,1,1,1,1,1,1,1,
1,1,1,1,1,1,1,1,1,1,1,1,1,1,1,1,1,1,1,1,1,1,1,1,1,1,1,1,1,1,1,1,1,1,1,1,
1,1,1,1,1,1,1,1,1,1,1,1,1,1,1,1,1,1,1,1,1,1,1,1,1,1,1,1,1,1,1,1,1,1,1,1,
1,1,1,1,1,1,1,1,1,1,1,1,1,1,1,1,1,1,1,1,1,1,1,1,1,1,1,1,1,1,1,1,1,1,1,1,
1,1,1,1,1,1,1,1,1,1,1,1,1,1,1,1,1,1,1,1,1,1,1,1,1,1,1,1,1,1,1,1,1,1,1,1,
1,1,1,1,1,1,1,1,1,1,1,1,1,1,1,1,1,1,1,1,1,1,1,1,1,1,1,1,1,1,1,1,1,1,1,6),
(2,2),(-1.,-0.995000000000001,-0.990000000000001,-0.985000000000001,-0.980000000000001,
-0.975000000000001,-0.970000000000001,-0.965000000000001,-0.960000000000001,
-0.955000000000001,-0.950000000000001,-0.945000000000001,-0.940000000000001,
-0.935000000000001,-0.930000000000001,-0.925000000000001,-0.920000000000001,
-0.915000000000001,-0.910000000000001,-0.905000000000001,-0.900000000000001,
-0.895000000000001,-0.890000000000001,-0.885000000000001,-0.880000000000001,
-0.875000000000001,-0.870000000000001,-0.865000000000001,-0.860000000000001,
-0.855000000000001,-0.850000000000001,-0.845000000000001,-0.840000000000001,
-0.835000000000001,-0.830000000000001,-0.825000000000001,-0.820000000000001,
-0.815000000000001,-0.810000000000001,-0.805000000000001,-0.800000000000001,
-0.795000000000001,-0.790000000000001,-0.785000000000001,-0.780000000000001,
-0.775000000000001,-0.770000000000001,-0.765000000000001,-0.760000000000001,
-0.755000000000001,-0.750000000000001,-0.745000000000001,-0.740000000000001,
-0.735000000000001,-0.730000000000001,-0.725000000000001,-0.720000000000001,
-0.715000000000001,-0.710000000000001,-0.705000000000001,-0.700000000000001,
-0.695000000000001,-0.690000000000001,-0.685,-0.68,-0.675,-0.67,-0.665,
-0.66,-0.655,-0.65,-0.645,-0.64,-0.635,-0.63,-0.625,-0.62,-0.615,-0.61,
-0.605,-0.6,-0.595,-0.59,-0.585,-0.58,-0.575,-0.57,-0.565,-0.56,-0.555,
-0.55,-0.545,-0.54,-0.535,-0.53,-0.525,-0.52,-0.515,-0.51,-0.505,-0.5,-0.495,
-0.49,-0.485,-0.48,-0.475,-0.47,-0.465,-0.46,-0.455,-0.45,-0.445,-0.44,
-0.435,-0.43,-0.425,-0.42,-0.415,-0.41,-0.405,-0.4,-0.395,-0.39,-0.385,
-0.38,-0.375,-0.37,-0.365,-0.36,-0.355,-0.35,-0.345,-0.34,-0.335,-0.33,
-0.325,-0.32,-0.315,-0.31,-0.305,-0.3,-0.295,-0.29,-0.285,-0.28,-0.275,
-0.27,-0.265,-0.26,-0.255,-0.25,-0.245,-0.24,-0.235,-0.23,-0.225,-0.22,
-0.215,-0.21,-0.205,-0.2,-0.195,-0.19,-0.185,-0.18,-0.175,-0.17,-0.165,
-0.16,-0.155,-0.15,-0.145,-0.14,-0.135,-0.13,-0.125,-0.12,-0.115,-0.11,
-0.105,-0.1,-0.095,-0.09,-0.085,-0.08,-0.075,-0.07,-0.065,-0.06,-0.055,
-0.05,-0.045,-0.04,-0.035,-0.03,-0.025,-0.02,-0.015,-0.01,-0.005,0.),(0.,
1.2),.UNSPECIFIED.)
GEOMETRIC_REPRESENTATION_ITEM()
RATIONAL_B_SPLINE_SURFACE(((1.,1.),(1.,1.),(1.,1.),(1.,1.),(1.,1.),(1.,
1.),(1.,1.),(1.,1.),(1.,1.),(1.,1.),(1.,1.),(1.,1.),(1.,1.),(1.,1.),(1.,
1.),(1.,1.),(1.,1.),(1.,1.),(1.,1.),(1.,1.),(1.,1.),(1.,1.),(1.,1.),(1.,
1.),(1.,1.),(1.,1.),(1.,1.),(1.,1.),(1.,1.),(1.,1.),(1.,1.),(1.,1.),(1.,
1.),(1.,1.),(1.,1.),(1.,1.),(1.,1.),(1.,1.),(1.,1.),(1.,1.),(1.,1.),(1.,
1.),(1.,1.),(1.,1.),(1.,1.),(1.,1.),(1.,1.),(1.,1.),(1.,1.),(1.,1.),(1.,
1.),(1.,1.),(1.,1.),(1.,1.),(1.,1.),(1.,1.),(1.,1.),(1.,1.),(1.,1.),(1.,
1.),(1.,1.),(1.,1.),(1.,1.),(1.,1.),(1.,1.),(1.,1.),(1.,1.),(1.,1.),(1.,
1.),(1.,1.),(1.,1.),(1.,1.),(1.,1.),(1.,1.),(1.,1.),(1.,1.),(1.,1.),(1.,
1.),(1.,1.),(1.,1.),(1.,1.),(1.,1.),(1.,1.),(1.,1.),(1.,1.),(1.,1.),(1.,
1.),(1.,1.),(1.,1.),(1.,1.),(1.,1.),(1.,1.),(1.,1.),(1.,1.),(1.,1.),(1.,
1.),(1.,1.),(1.,1.),(1.,1.),(1.,1.),(1.,1.),(1.,1.),(1.,1.),(1.,1.),(1.,
1.),(1.,1.),(1.,1.),(1.,1.),(1.,1.),(1.,1.),(1.,1.),(1.,1.),(1.,1.),(1.,
1.),(1.,1.),(1.,1.),(1.,1.),(1.,1.),(1.,1.),(1.,1.),(1.,1.),(1.,1.),(1.,
1.),(1.,1.),(1.,1.),(1.,1.),(1.,1.),(1.,1.),(1.,1.),(1.,1.),(1.,1.),(1.,
1.),(1.,1.),(1.,1.),(1.,1.),(1.,1.),(1.,1.),(1.,1.),(1.,1.),(1.,1.),(1.,
1.),(1.,1.),(1.,1.),(1.,1.),(1.,1.),(1.,1.),(1.,1.),(1.,1.),(1.,1.),(1.,
1.),(1.,1.),(1.,1.),(1.,1.),(1.,1.),(1.,1.),(1.,1.),(1.,1.),(1.,1.),(1.,
1.),(1.,1.),(1.,1.),(1.,1.),(1.,1.),(1.,1.),(1.,1.),(1.,1.),(1.,1.),(1.,
1.),(1.,1.),(1.,1.),(1.,1.),(1.,1.),(1.,1.),(1.,1.),(1.,1.),(1.,1.),(1.,
1.),(1.,1.),(1.,1.),(1.,1.),(1.,1.),(1.,1.),(1.,1.),(1.,1.),(1.,1.),(1.,
1.),(1.,1.),(1.,1.),(1.,1.),(1.,1.),(1.,1.),(1.,1.),(1.,1.),(1.,1.),(1.,
1.),(1.,1.),(1.,1.),(1.,1.),(1.,1.),(1.,1.),(1.,1.),(1.,1.),(1.,1.),(1.,
1.),(1.,1.)))
REPRESENTATION_ITEM('')
SURFACE()
);
#979=(
BOUNDED_SURFACE()
B_SPLINE_SURFACE(5,1,((#136217,#136218),(#136219,#136220),(#136221,#136222),
(#136223,#136224),(#136225,#136226),(#136227,#136228),(#136229,#136230),
(#136231,#136232),(#136233,#136234),(#136235,#136236),(#136237,#136238),
(#136239,#136240),(#136241,#136242),(#136243,#136244),(#136245,#136246),
(#136247,#136248),(#136249,#136250),(#136251,#136252),(#136253,#136254),
(#136255,#136256),(#136257,#136258),(#136259,#136260),(#136261,#136262),
(#136263,#136264),(#136265,#136266),(#136267,#136268),(#136269,#136270),
(#136271,#136272),(#136273,#136274),(#136275,#136276),(#136277,#136278),
(#136279,#136280),(#136281,#136282),(#136283,#136284),(#136285,#136286),
(#136287,#136288),(#136289,#136290),(#136291,#136292),(#136293,#136294),
(#136295,#136296),(#136297,#136298),(#136299,#136300),(#136301,#136302),
(#136303,#136304),(#136305,#136306),(#136307,#136308),(#136309,#136310),
(#136311,#136312),(#136313,#136314),(#136315,#136316),(#136317,#136318),
(#136319,#136320),(#136321,#136322),(#136323,#136324),(#136325,#136326),
(#136327,#136328),(#136329,#136330),(#136331,#136332),(#136333,#136334),
(#136335,#136336),(#136337,#136338),(#136339,#136340),(#136341,#136342),
(#136343,#136344),(#136345,#136346),(#136347,#136348),(#136349,#136350),
(#136351,#136352),(#136353,#136354),(#136355,#136356),(#136357,#136358),
(#136359,#136360),(#136361,#136362),(#136363,#136364),(#136365,#136366),
(#136367,#136368),(#136369,#136370),(#136371,#136372),(#136373,#136374),
(#136375,#136376),(#136377,#136378),(#136379,#136380),(#136381,#136382),
(#136383,#136384),(#136385,#136386),(#136387,#136388),(#136389,#136390),
(#136391,#136392),(#136393,#136394),(#136395,#136396),(#136397,#136398),
(#136399,#136400),(#136401,#136402),(#136403,#136404),(#136405,#136406),
(#136407,#136408),(#136409,#136410),(#136411,#136412),(#136413,#136414),
(#136415,#136416),(#136417,#136418),(#136419,#136420),(#136421,#136422),
(#136423,#136424),(#136425,#136426),(#136427,#136428),(#136429,#136430),
(#136431,#136432),(#136433,#136434),(#136435,#136436),(#136437,#136438),
(#136439,#136440),(#136441,#136442),(#136443,#136444),(#136445,#136446),
(#136447,#136448),(#136449,#136450),(#136451,#136452),(#136453,#136454),
(#136455,#136456),(#136457,#136458),(#136459,#136460),(#136461,#136462),
(#136463,#136464),(#136465,#136466),(#136467,#136468),(#136469,#136470),
(#136471,#136472),(#136473,#136474),(#136475,#136476),(#136477,#136478),
(#136479,#136480),(#136481,#136482),(#136483,#136484),(#136485,#136486),
(#136487,#136488),(#136489,#136490),(#136491,#136492),(#136493,#136494),
(#136495,#136496),(#136497,#136498),(#136499,#136500),(#136501,#136502),
(#136503,#136504),(#136505,#136506),(#136507,#136508),(#136509,#136510),
(#136511,#136512),(#136513,#136514),(#136515,#136516),(#136517,#136518),
(#136519,#136520),(#136521,#136522),(#136523,#136524),(#136525,#136526),
(#136527,#136528),(#136529,#136530),(#136531,#136532),(#136533,#136534),
(#136535,#136536),(#136537,#136538),(#136539,#136540),(#136541,#136542),
(#136543,#136544),(#136545,#136546),(#136547,#136548),(#136549,#136550),
(#136551,#136552),(#136553,#136554),(#136555,#136556),(#136557,#136558),
(#136559,#136560),(#136561,#136562),(#136563,#136564),(#136565,#136566),
(#136567,#136568),(#136569,#136570),(#136571,#136572),(#136573,#136574),
(#136575,#136576),(#136577,#136578),(#136579,#136580),(#136581,#136582),
(#136583,#136584),(#136585,#136586),(#136587,#136588),(#136589,#136590),
(#136591,#136592),(#136593,#136594),(#136595,#136596),(#136597,#136598),
(#136599,#136600),(#136601,#136602),(#136603,#136604),(#136605,#136606),
(#136607,#136608),(#136609,#136610),(#136611,#136612),(#136613,#136614),
(#136615,#136616),(#136617,#136618),(#136619,#136620),(#136621,#136622),
(#136623,#136624),(#136625,#136626)),.UNSPECIFIED.,.F.,.F.,.F.)
B_SPLINE_SURFACE_WITH_KNOTS((6,1,1,1,1,1,1,1,1,1,1,1,1,1,1,1,1,1,1,1,1,
1,1,1,1,1,1,1,1,1,1,1,1,1,1,1,1,1,1,1,1,1,1,1,1,1,1,1,1,1,1,1,1,1,1,1,1,
1,1,1,1,1,1,1,1,1,1,1,1,1,1,1,1,1,1,1,1,1,1,1,1,1,1,1,1,1,1,1,1,1,1,1,1,
1,1,1,1,1,1,1,1,1,1,1,1,1,1,1,1,1,1,1,1,1,1,1,1,1,1,1,1,1,1,1,1,1,1,1,1,
1,1,1,1,1,1,1,1,1,1,1,1,1,1,1,1,1,1,1,1,1,1,1,1,1,1,1,1,1,1,1,1,1,1,1,1,
1,1,1,1,1,1,1,1,1,1,1,1,1,1,1,1,1,1,1,1,1,1,1,1,1,1,1,1,1,1,1,1,1,1,1,6),
(2,2),(-1.,-0.995000000000001,-0.990000000000001,-0.985000000000001,-0.980000000000001,
-0.975000000000001,-0.970000000000001,-0.965000000000001,-0.960000000000001,
-0.955000000000001,-0.950000000000001,-0.945000000000001,-0.940000000000001,
-0.935000000000001,-0.930000000000001,-0.925000000000001,-0.920000000000001,
-0.915000000000001,-0.910000000000001,-0.905000000000001,-0.900000000000001,
-0.895000000000001,-0.890000000000001,-0.885000000000001,-0.880000000000001,
-0.875000000000001,-0.870000000000001,-0.865000000000001,-0.860000000000001,
-0.855000000000001,-0.850000000000001,-0.845000000000001,-0.840000000000001,
-0.835000000000001,-0.830000000000001,-0.825000000000001,-0.820000000000001,
-0.815000000000001,-0.810000000000001,-0.805000000000001,-0.800000000000001,
-0.795000000000001,-0.790000000000001,-0.785000000000001,-0.780000000000001,
-0.775000000000001,-0.770000000000001,-0.765000000000001,-0.760000000000001,
-0.755000000000001,-0.750000000000001,-0.745000000000001,-0.740000000000001,
-0.735000000000001,-0.730000000000001,-0.725000000000001,-0.720000000000001,
-0.715000000000001,-0.710000000000001,-0.705000000000001,-0.700000000000001,
-0.695000000000001,-0.690000000000001,-0.685,-0.68,-0.675,-0.67,-0.665,
-0.66,-0.655,-0.65,-0.645,-0.64,-0.635,-0.63,-0.625,-0.62,-0.615,-0.61,
-0.605,-0.6,-0.595,-0.59,-0.585,-0.58,-0.575,-0.57,-0.565,-0.56,-0.555,
-0.55,-0.545,-0.54,-0.535,-0.53,-0.525,-0.52,-0.515,-0.51,-0.505,-0.5,-0.495,
-0.49,-0.485,-0.48,-0.475,-0.47,-0.465,-0.46,-0.455,-0.45,-0.445,-0.44,
-0.435,-0.43,-0.425,-0.42,-0.415,-0.41,-0.405,-0.4,-0.395,-0.39,-0.385,
-0.38,-0.375,-0.37,-0.365,-0.36,-0.355,-0.35,-0.345,-0.34,-0.335,-0.33,
-0.325,-0.32,-0.315,-0.31,-0.305,-0.3,-0.295,-0.29,-0.285,-0.28,-0.275,
-0.27,-0.265,-0.26,-0.255,-0.25,-0.245,-0.24,-0.235,-0.23,-0.225,-0.22,
-0.215,-0.21,-0.205,-0.2,-0.195,-0.19,-0.185,-0.18,-0.175,-0.17,-0.165,
-0.16,-0.155,-0.15,-0.145,-0.14,-0.135,-0.13,-0.125,-0.12,-0.115,-0.11,
-0.105,-0.1,-0.095,-0.09,-0.085,-0.08,-0.075,-0.07,-0.065,-0.06,-0.055,
-0.05,-0.045,-0.04,-0.035,-0.03,-0.025,-0.02,-0.015,-0.01,-0.005,0.),(0.,
1.2),.UNSPECIFIED.)
GEOMETRIC_REPRESENTATION_ITEM()
RATIONAL_B_SPLINE_SURFACE(((1.,1.),(1.,1.),(1.,1.),(1.,1.),(1.,1.),(1.,
1.),(1.,1.),(1.,1.),(1.,1.),(1.,1.),(1.,1.),(1.,1.),(1.,1.),(1.,1.),(1.,
1.),(1.,1.),(1.,1.),(1.,1.),(1.,1.),(1.,1.),(1.,1.),(1.,1.),(1.,1.),(1.,
1.),(1.,1.),(1.,1.),(1.,1.),(1.,1.),(1.,1.),(1.,1.),(1.,1.),(1.,1.),(1.,
1.),(1.,1.),(1.,1.),(1.,1.),(1.,1.),(1.,1.),(1.,1.),(1.,1.),(1.,1.),(1.,
1.),(1.,1.),(1.,1.),(1.,1.),(1.,1.),(1.,1.),(1.,1.),(1.,1.),(1.,1.),(1.,
1.),(1.,1.),(1.,1.),(1.,1.),(1.,1.),(1.,1.),(1.,1.),(1.,1.),(1.,1.),(1.,
1.),(1.,1.),(1.,1.),(1.,1.),(1.,1.),(1.,1.),(1.,1.),(1.,1.),(1.,1.),(1.,
1.),(1.,1.),(1.,1.),(1.,1.),(1.,1.),(1.,1.),(1.,1.),(1.,1.),(1.,1.),(1.,
1.),(1.,1.),(1.,1.),(1.,1.),(1.,1.),(1.,1.),(1.,1.),(1.,1.),(1.,1.),(1.,
1.),(1.,1.),(1.,1.),(1.,1.),(1.,1.),(1.,1.),(1.,1.),(1.,1.),(1.,1.),(1.,
1.),(1.,1.),(1.,1.),(1.,1.),(1.,1.),(1.,1.),(1.,1.),(1.,1.),(1.,1.),(1.,
1.),(1.,1.),(1.,1.),(1.,1.),(1.,1.),(1.,1.),(1.,1.),(1.,1.),(1.,1.),(1.,
1.),(1.,1.),(1.,1.),(1.,1.),(1.,1.),(1.,1.),(1.,1.),(1.,1.),(1.,1.),(1.,
1.),(1.,1.),(1.,1.),(1.,1.),(1.,1.),(1.,1.),(1.,1.),(1.,1.),(1.,1.),(1.,
1.),(1.,1.),(1.,1.),(1.,1.),(1.,1.),(1.,1.),(1.,1.),(1.,1.),(1.,1.),(1.,
1.),(1.,1.),(1.,1.),(1.,1.),(1.,1.),(1.,1.),(1.,1.),(1.,1.),(1.,1.),(1.,
1.),(1.,1.),(1.,1.),(1.,1.),(1.,1.),(1.,1.),(1.,1.),(1.,1.),(1.,1.),(1.,
1.),(1.,1.),(1.,1.),(1.,1.),(1.,1.),(1.,1.),(1.,1.),(1.,1.),(1.,1.),(1.,
1.),(1.,1.),(1.,1.),(1.,1.),(1.,1.),(1.,1.),(1.,1.),(1.,1.),(1.,1.),(1.,
1.),(1.,1.),(1.,1.),(1.,1.),(1.,1.),(1.,1.),(1.,1.),(1.,1.),(1.,1.),(1.,
1.),(1.,1.),(1.,1.),(1.,1.),(1.,1.),(1.,1.),(1.,1.),(1.,1.),(1.,1.),(1.,
1.),(1.,1.),(1.,1.),(1.,1.),(1.,1.),(1.,1.),(1.,1.),(1.,1.),(1.,1.),(1.,
1.),(1.,1.)))
REPRESENTATION_ITEM('')
SURFACE()
);
#980=(
BOUNDED_SURFACE()
B_SPLINE_SURFACE(5,1,((#137018,#137019),(#137020,#137021),(#137022,#137023),
(#137024,#137025),(#137026,#137027),(#137028,#137029),(#137030,#137031),
(#137032,#137033),(#137034,#137035),(#137036,#137037),(#137038,#137039),
(#137040,#137041),(#137042,#137043),(#137044,#137045),(#137046,#137047),
(#137048,#137049),(#137050,#137051),(#137052,#137053),(#137054,#137055),
(#137056,#137057),(#137058,#137059),(#137060,#137061),(#137062,#137063),
(#137064,#137065),(#137066,#137067),(#137068,#137069),(#137070,#137071),
(#137072,#137073),(#137074,#137075),(#137076,#137077),(#137078,#137079),
(#137080,#137081),(#137082,#137083),(#137084,#137085),(#137086,#137087),
(#137088,#137089),(#137090,#137091),(#137092,#137093),(#137094,#137095),
(#137096,#137097),(#137098,#137099),(#137100,#137101),(#137102,#137103),
(#137104,#137105),(#137106,#137107),(#137108,#137109),(#137110,#137111),
(#137112,#137113),(#137114,#137115),(#137116,#137117),(#137118,#137119),
(#137120,#137121),(#137122,#137123),(#137124,#137125),(#137126,#137127),
(#137128,#137129),(#137130,#137131),(#137132,#137133),(#137134,#137135),
(#137136,#137137),(#137138,#137139),(#137140,#137141),(#137142,#137143),
(#137144,#137145),(#137146,#137147),(#137148,#137149),(#137150,#137151),
(#137152,#137153),(#137154,#137155),(#137156,#137157),(#137158,#137159),
(#137160,#137161),(#137162,#137163),(#137164,#137165),(#137166,#137167),
(#137168,#137169),(#137170,#137171),(#137172,#137173),(#137174,#137175),
(#137176,#137177),(#137178,#137179),(#137180,#137181),(#137182,#137183),
(#137184,#137185),(#137186,#137187),(#137188,#137189),(#137190,#137191),
(#137192,#137193),(#137194,#137195),(#137196,#137197),(#137198,#137199),
(#137200,#137201),(#137202,#137203),(#137204,#137205),(#137206,#137207),
(#137208,#137209),(#137210,#137211),(#137212,#137213),(#137214,#137215),
(#137216,#137217),(#137218,#137219),(#137220,#137221),(#137222,#137223),
(#137224,#137225),(#137226,#137227),(#137228,#137229),(#137230,#137231),
(#137232,#137233),(#137234,#137235),(#137236,#137237),(#137238,#137239),
(#137240,#137241),(#137242,#137243),(#137244,#137245),(#137246,#137247),
(#137248,#137249),(#137250,#137251),(#137252,#137253),(#137254,#137255),
(#137256,#137257),(#137258,#137259),(#137260,#137261),(#137262,#137263),
(#137264,#137265),(#137266,#137267),(#137268,#137269),(#137270,#137271),
(#137272,#137273),(#137274,#137275),(#137276,#137277),(#137278,#137279),
(#137280,#137281),(#137282,#137283),(#137284,#137285),(#137286,#137287),
(#137288,#137289),(#137290,#137291),(#137292,#137293),(#137294,#137295),
(#137296,#137297),(#137298,#137299),(#137300,#137301),(#137302,#137303),
(#137304,#137305),(#137306,#137307),(#137308,#137309),(#137310,#137311),
(#137312,#137313),(#137314,#137315),(#137316,#137317),(#137318,#137319),
(#137320,#137321),(#137322,#137323),(#137324,#137325),(#137326,#137327),
(#137328,#137329),(#137330,#137331),(#137332,#137333),(#137334,#137335),
(#137336,#137337),(#137338,#137339),(#137340,#137341),(#137342,#137343),
(#137344,#137345),(#137346,#137347),(#137348,#137349),(#137350,#137351),
(#137352,#137353),(#137354,#137355),(#137356,#137357),(#137358,#137359),
(#137360,#137361),(#137362,#137363),(#137364,#137365),(#137366,#137367),
(#137368,#137369),(#137370,#137371),(#137372,#137373),(#137374,#137375),
(#137376,#137377),(#137378,#137379),(#137380,#137381),(#137382,#137383),
(#137384,#137385),(#137386,#137387),(#137388,#137389),(#137390,#137391),
(#137392,#137393),(#137394,#137395),(#137396,#137397),(#137398,#137399),
(#137400,#137401),(#137402,#137403),(#137404,#137405),(#137406,#137407),
(#137408,#137409),(#137410,#137411),(#137412,#137413),(#137414,#137415),
(#137416,#137417),(#137418,#137419),(#137420,#137421),(#137422,#137423),
(#137424,#137425),(#137426,#137427)),.UNSPECIFIED.,.F.,.F.,.F.)
B_SPLINE_SURFACE_WITH_KNOTS((6,1,1,1,1,1,1,1,1,1,1,1,1,1,1,1,1,1,1,1,1,
1,1,1,1,1,1,1,1,1,1,1,1,1,1,1,1,1,1,1,1,1,1,1,1,1,1,1,1,1,1,1,1,1,1,1,1,
1,1,1,1,1,1,1,1,1,1,1,1,1,1,1,1,1,1,1,1,1,1,1,1,1,1,1,1,1,1,1,1,1,1,1,1,
1,1,1,1,1,1,1,1,1,1,1,1,1,1,1,1,1,1,1,1,1,1,1,1,1,1,1,1,1,1,1,1,1,1,1,1,
1,1,1,1,1,1,1,1,1,1,1,1,1,1,1,1,1,1,1,1,1,1,1,1,1,1,1,1,1,1,1,1,1,1,1,1,
1,1,1,1,1,1,1,1,1,1,1,1,1,1,1,1,1,1,1,1,1,1,1,1,1,1,1,1,1,1,1,1,1,1,1,6),
(2,2),(-1.,-0.995000000000001,-0.990000000000001,-0.985000000000001,-0.980000000000001,
-0.975000000000001,-0.970000000000001,-0.965000000000001,-0.960000000000001,
-0.955000000000001,-0.950000000000001,-0.945000000000001,-0.940000000000001,
-0.935000000000001,-0.930000000000001,-0.925000000000001,-0.920000000000001,
-0.915000000000001,-0.910000000000001,-0.905000000000001,-0.900000000000001,
-0.895000000000001,-0.890000000000001,-0.885000000000001,-0.880000000000001,
-0.875000000000001,-0.870000000000001,-0.865000000000001,-0.860000000000001,
-0.855000000000001,-0.850000000000001,-0.845000000000001,-0.840000000000001,
-0.835000000000001,-0.830000000000001,-0.825000000000001,-0.820000000000001,
-0.815000000000001,-0.810000000000001,-0.805000000000001,-0.800000000000001,
-0.795000000000001,-0.790000000000001,-0.785000000000001,-0.780000000000001,
-0.775000000000001,-0.770000000000001,-0.765000000000001,-0.760000000000001,
-0.755000000000001,-0.750000000000001,-0.745000000000001,-0.740000000000001,
-0.735000000000001,-0.730000000000001,-0.725000000000001,-0.720000000000001,
-0.715000000000001,-0.710000000000001,-0.705000000000001,-0.700000000000001,
-0.695000000000001,-0.690000000000001,-0.685,-0.68,-0.675,-0.67,-0.665,
-0.66,-0.655,-0.65,-0.645,-0.64,-0.635,-0.63,-0.625,-0.62,-0.615,-0.61,
-0.605,-0.6,-0.595,-0.59,-0.585,-0.58,-0.575,-0.57,-0.565,-0.56,-0.555,
-0.55,-0.545,-0.54,-0.535,-0.53,-0.525,-0.52,-0.515,-0.51,-0.505,-0.5,-0.495,
-0.49,-0.485,-0.48,-0.475,-0.47,-0.465,-0.46,-0.455,-0.45,-0.445,-0.44,
-0.435,-0.43,-0.425,-0.42,-0.415,-0.41,-0.405,-0.4,-0.395,-0.39,-0.385,
-0.38,-0.375,-0.37,-0.365,-0.36,-0.355,-0.35,-0.345,-0.34,-0.335,-0.33,
-0.325,-0.32,-0.315,-0.31,-0.305,-0.3,-0.295,-0.29,-0.285,-0.28,-0.275,
-0.27,-0.265,-0.26,-0.255,-0.25,-0.245,-0.24,-0.235,-0.23,-0.225,-0.22,
-0.215,-0.21,-0.205,-0.2,-0.195,-0.19,-0.185,-0.18,-0.175,-0.17,-0.165,
-0.16,-0.155,-0.15,-0.145,-0.14,-0.135,-0.13,-0.125,-0.12,-0.115,-0.11,
-0.105,-0.1,-0.095,-0.09,-0.085,-0.08,-0.075,-0.07,-0.065,-0.06,-0.055,
-0.05,-0.045,-0.04,-0.035,-0.03,-0.025,-0.02,-0.015,-0.01,-0.005,0.),(0.,
1.2),.UNSPECIFIED.)
GEOMETRIC_REPRESENTATION_ITEM()
RATIONAL_B_SPLINE_SURFACE(((1.,1.),(1.,1.),(1.,1.),(1.,1.),(1.,1.),(1.,
1.),(1.,1.),(1.,1.),(1.,1.),(1.,1.),(1.,1.),(1.,1.),(1.,1.),(1.,1.),(1.,
1.),(1.,1.),(1.,1.),(1.,1.),(1.,1.),(1.,1.),(1.,1.),(1.,1.),(1.,1.),(1.,
1.),(1.,1.),(1.,1.),(1.,1.),(1.,1.),(1.,1.),(1.,1.),(1.,1.),(1.,1.),(1.,
1.),(1.,1.),(1.,1.),(1.,1.),(1.,1.),(1.,1.),(1.,1.),(1.,1.),(1.,1.),(1.,
1.),(1.,1.),(1.,1.),(1.,1.),(1.,1.),(1.,1.),(1.,1.),(1.,1.),(1.,1.),(1.,
1.),(1.,1.),(1.,1.),(1.,1.),(1.,1.),(1.,1.),(1.,1.),(1.,1.),(1.,1.),(1.,
1.),(1.,1.),(1.,1.),(1.,1.),(1.,1.),(1.,1.),(1.,1.),(1.,1.),(1.,1.),(1.,
1.),(1.,1.),(1.,1.),(1.,1.),(1.,1.),(1.,1.),(1.,1.),(1.,1.),(1.,1.),(1.,
1.),(1.,1.),(1.,1.),(1.,1.),(1.,1.),(1.,1.),(1.,1.),(1.,1.),(1.,1.),(1.,
1.),(1.,1.),(1.,1.),(1.,1.),(1.,1.),(1.,1.),(1.,1.),(1.,1.),(1.,1.),(1.,
1.),(1.,1.),(1.,1.),(1.,1.),(1.,1.),(1.,1.),(1.,1.),(1.,1.),(1.,1.),(1.,
1.),(1.,1.),(1.,1.),(1.,1.),(1.,1.),(1.,1.),(1.,1.),(1.,1.),(1.,1.),(1.,
1.),(1.,1.),(1.,1.),(1.,1.),(1.,1.),(1.,1.),(1.,1.),(1.,1.),(1.,1.),(1.,
1.),(1.,1.),(1.,1.),(1.,1.),(1.,1.),(1.,1.),(1.,1.),(1.,1.),(1.,1.),(1.,
1.),(1.,1.),(1.,1.),(1.,1.),(1.,1.),(1.,1.),(1.,1.),(1.,1.),(1.,1.),(1.,
1.),(1.,1.),(1.,1.),(1.,1.),(1.,1.),(1.,1.),(1.,1.),(1.,1.),(1.,1.),(1.,
1.),(1.,1.),(1.,1.),(1.,1.),(1.,1.),(1.,1.),(1.,1.),(1.,1.),(1.,1.),(1.,
1.),(1.,1.),(1.,1.),(1.,1.),(1.,1.),(1.,1.),(1.,1.),(1.,1.),(1.,1.),(1.,
1.),(1.,1.),(1.,1.),(1.,1.),(1.,1.),(1.,1.),(1.,1.),(1.,1.),(1.,1.),(1.,
1.),(1.,1.),(1.,1.),(1.,1.),(1.,1.),(1.,1.),(1.,1.),(1.,1.),(1.,1.),(1.,
1.),(1.,1.),(1.,1.),(1.,1.),(1.,1.),(1.,1.),(1.,1.),(1.,1.),(1.,1.),(1.,
1.),(1.,1.),(1.,1.),(1.,1.),(1.,1.),(1.,1.),(1.,1.),(1.,1.),(1.,1.),(1.,
1.),(1.,1.)))
REPRESENTATION_ITEM('')
SURFACE()
);
#981=(
BOUNDED_SURFACE()
B_SPLINE_SURFACE(5,1,((#137819,#137820),(#137821,#137822),(#137823,#137824),
(#137825,#137826),(#137827,#137828),(#137829,#137830),(#137831,#137832),
(#137833,#137834),(#137835,#137836),(#137837,#137838),(#137839,#137840),
(#137841,#137842),(#137843,#137844),(#137845,#137846),(#137847,#137848),
(#137849,#137850),(#137851,#137852),(#137853,#137854),(#137855,#137856),
(#137857,#137858),(#137859,#137860),(#137861,#137862),(#137863,#137864),
(#137865,#137866),(#137867,#137868),(#137869,#137870),(#137871,#137872),
(#137873,#137874),(#137875,#137876),(#137877,#137878),(#137879,#137880),
(#137881,#137882),(#137883,#137884),(#137885,#137886),(#137887,#137888),
(#137889,#137890),(#137891,#137892),(#137893,#137894),(#137895,#137896),
(#137897,#137898),(#137899,#137900),(#137901,#137902),(#137903,#137904),
(#137905,#137906),(#137907,#137908),(#137909,#137910),(#137911,#137912),
(#137913,#137914),(#137915,#137916),(#137917,#137918),(#137919,#137920),
(#137921,#137922),(#137923,#137924),(#137925,#137926),(#137927,#137928),
(#137929,#137930),(#137931,#137932),(#137933,#137934),(#137935,#137936),
(#137937,#137938),(#137939,#137940),(#137941,#137942),(#137943,#137944),
(#137945,#137946),(#137947,#137948),(#137949,#137950),(#137951,#137952),
(#137953,#137954),(#137955,#137956),(#137957,#137958),(#137959,#137960),
(#137961,#137962),(#137963,#137964),(#137965,#137966),(#137967,#137968),
(#137969,#137970),(#137971,#137972),(#137973,#137974),(#137975,#137976),
(#137977,#137978),(#137979,#137980),(#137981,#137982),(#137983,#137984),
(#137985,#137986),(#137987,#137988),(#137989,#137990),(#137991,#137992),
(#137993,#137994),(#137995,#137996),(#137997,#137998),(#137999,#138000),
(#138001,#138002),(#138003,#138004),(#138005,#138006),(#138007,#138008),
(#138009,#138010),(#138011,#138012),(#138013,#138014),(#138015,#138016),
(#138017,#138018),(#138019,#138020),(#138021,#138022),(#138023,#138024),
(#138025,#138026),(#138027,#138028),(#138029,#138030),(#138031,#138032),
(#138033,#138034),(#138035,#138036),(#138037,#138038),(#138039,#138040),
(#138041,#138042),(#138043,#138044),(#138045,#138046),(#138047,#138048),
(#138049,#138050),(#138051,#138052),(#138053,#138054),(#138055,#138056),
(#138057,#138058),(#138059,#138060),(#138061,#138062),(#138063,#138064),
(#138065,#138066),(#138067,#138068),(#138069,#138070),(#138071,#138072),
(#138073,#138074),(#138075,#138076),(#138077,#138078),(#138079,#138080),
(#138081,#138082),(#138083,#138084),(#138085,#138086),(#138087,#138088),
(#138089,#138090),(#138091,#138092),(#138093,#138094),(#138095,#138096),
(#138097,#138098),(#138099,#138100),(#138101,#138102),(#138103,#138104),
(#138105,#138106),(#138107,#138108),(#138109,#138110),(#138111,#138112),
(#138113,#138114),(#138115,#138116),(#138117,#138118),(#138119,#138120),
(#138121,#138122),(#138123,#138124),(#138125,#138126),(#138127,#138128),
(#138129,#138130),(#138131,#138132),(#138133,#138134),(#138135,#138136),
(#138137,#138138),(#138139,#138140),(#138141,#138142),(#138143,#138144),
(#138145,#138146),(#138147,#138148),(#138149,#138150),(#138151,#138152),
(#138153,#138154),(#138155,#138156),(#138157,#138158),(#138159,#138160),
(#138161,#138162),(#138163,#138164),(#138165,#138166),(#138167,#138168),
(#138169,#138170),(#138171,#138172),(#138173,#138174),(#138175,#138176),
(#138177,#138178),(#138179,#138180),(#138181,#138182),(#138183,#138184),
(#138185,#138186),(#138187,#138188),(#138189,#138190),(#138191,#138192),
(#138193,#138194),(#138195,#138196),(#138197,#138198),(#138199,#138200),
(#138201,#138202),(#138203,#138204),(#138205,#138206),(#138207,#138208),
(#138209,#138210),(#138211,#138212),(#138213,#138214),(#138215,#138216),
(#138217,#138218),(#138219,#138220),(#138221,#138222),(#138223,#138224),
(#138225,#138226),(#138227,#138228)),.UNSPECIFIED.,.F.,.F.,.F.)
B_SPLINE_SURFACE_WITH_KNOTS((6,1,1,1,1,1,1,1,1,1,1,1,1,1,1,1,1,1,1,1,1,
1,1,1,1,1,1,1,1,1,1,1,1,1,1,1,1,1,1,1,1,1,1,1,1,1,1,1,1,1,1,1,1,1,1,1,1,
1,1,1,1,1,1,1,1,1,1,1,1,1,1,1,1,1,1,1,1,1,1,1,1,1,1,1,1,1,1,1,1,1,1,1,1,
1,1,1,1,1,1,1,1,1,1,1,1,1,1,1,1,1,1,1,1,1,1,1,1,1,1,1,1,1,1,1,1,1,1,1,1,
1,1,1,1,1,1,1,1,1,1,1,1,1,1,1,1,1,1,1,1,1,1,1,1,1,1,1,1,1,1,1,1,1,1,1,1,
1,1,1,1,1,1,1,1,1,1,1,1,1,1,1,1,1,1,1,1,1,1,1,1,1,1,1,1,1,1,1,1,1,1,1,6),
(2,2),(-1.,-0.995000000000001,-0.990000000000001,-0.985000000000001,-0.980000000000001,
-0.975000000000001,-0.970000000000001,-0.965000000000001,-0.960000000000001,
-0.955000000000001,-0.950000000000001,-0.945000000000001,-0.940000000000001,
-0.935000000000001,-0.930000000000001,-0.925000000000001,-0.920000000000001,
-0.915000000000001,-0.910000000000001,-0.905000000000001,-0.900000000000001,
-0.895000000000001,-0.890000000000001,-0.885000000000001,-0.880000000000001,
-0.875000000000001,-0.870000000000001,-0.865000000000001,-0.860000000000001,
-0.855000000000001,-0.850000000000001,-0.845000000000001,-0.840000000000001,
-0.835000000000001,-0.830000000000001,-0.825000000000001,-0.820000000000001,
-0.815000000000001,-0.810000000000001,-0.805000000000001,-0.800000000000001,
-0.795000000000001,-0.790000000000001,-0.785000000000001,-0.780000000000001,
-0.775000000000001,-0.770000000000001,-0.765000000000001,-0.760000000000001,
-0.755000000000001,-0.750000000000001,-0.745000000000001,-0.740000000000001,
-0.735000000000001,-0.730000000000001,-0.725000000000001,-0.720000000000001,
-0.715000000000001,-0.710000000000001,-0.705000000000001,-0.700000000000001,
-0.695000000000001,-0.690000000000001,-0.685,-0.68,-0.675,-0.67,-0.665,
-0.66,-0.655,-0.65,-0.645,-0.64,-0.635,-0.63,-0.625,-0.62,-0.615,-0.61,
-0.605,-0.6,-0.595,-0.59,-0.585,-0.58,-0.575,-0.57,-0.565,-0.56,-0.555,
-0.55,-0.545,-0.54,-0.535,-0.53,-0.525,-0.52,-0.515,-0.51,-0.505,-0.5,-0.495,
-0.49,-0.485,-0.48,-0.475,-0.47,-0.465,-0.46,-0.455,-0.45,-0.445,-0.44,
-0.435,-0.43,-0.425,-0.42,-0.415,-0.41,-0.405,-0.4,-0.395,-0.39,-0.385,
-0.38,-0.375,-0.37,-0.365,-0.36,-0.355,-0.35,-0.345,-0.34,-0.335,-0.33,
-0.325,-0.32,-0.315,-0.31,-0.305,-0.3,-0.295,-0.29,-0.285,-0.28,-0.275,
-0.27,-0.265,-0.26,-0.255,-0.25,-0.245,-0.24,-0.235,-0.23,-0.225,-0.22,
-0.215,-0.21,-0.205,-0.2,-0.195,-0.19,-0.185,-0.18,-0.175,-0.17,-0.165,
-0.16,-0.155,-0.15,-0.145,-0.14,-0.135,-0.13,-0.125,-0.12,-0.115,-0.11,
-0.105,-0.1,-0.095,-0.09,-0.085,-0.08,-0.075,-0.07,-0.065,-0.06,-0.055,
-0.05,-0.045,-0.04,-0.035,-0.03,-0.025,-0.02,-0.015,-0.01,-0.005,0.),(0.,
1.2),.UNSPECIFIED.)
GEOMETRIC_REPRESENTATION_ITEM()
RATIONAL_B_SPLINE_SURFACE(((1.,1.),(1.,1.),(1.,1.),(1.,1.),(1.,1.),(1.,
1.),(1.,1.),(1.,1.),(1.,1.),(1.,1.),(1.,1.),(1.,1.),(1.,1.),(1.,1.),(1.,
1.),(1.,1.),(1.,1.),(1.,1.),(1.,1.),(1.,1.),(1.,1.),(1.,1.),(1.,1.),(1.,
1.),(1.,1.),(1.,1.),(1.,1.),(1.,1.),(1.,1.),(1.,1.),(1.,1.),(1.,1.),(1.,
1.),(1.,1.),(1.,1.),(1.,1.),(1.,1.),(1.,1.),(1.,1.),(1.,1.),(1.,1.),(1.,
1.),(1.,1.),(1.,1.),(1.,1.),(1.,1.),(1.,1.),(1.,1.),(1.,1.),(1.,1.),(1.,
1.),(1.,1.),(1.,1.),(1.,1.),(1.,1.),(1.,1.),(1.,1.),(1.,1.),(1.,1.),(1.,
1.),(1.,1.),(1.,1.),(1.,1.),(1.,1.),(1.,1.),(1.,1.),(1.,1.),(1.,1.),(1.,
1.),(1.,1.),(1.,1.),(1.,1.),(1.,1.),(1.,1.),(1.,1.),(1.,1.),(1.,1.),(1.,
1.),(1.,1.),(1.,1.),(1.,1.),(1.,1.),(1.,1.),(1.,1.),(1.,1.),(1.,1.),(1.,
1.),(1.,1.),(1.,1.),(1.,1.),(1.,1.),(1.,1.),(1.,1.),(1.,1.),(1.,1.),(1.,
1.),(1.,1.),(1.,1.),(1.,1.),(1.,1.),(1.,1.),(1.,1.),(1.,1.),(1.,1.),(1.,
1.),(1.,1.),(1.,1.),(1.,1.),(1.,1.),(1.,1.),(1.,1.),(1.,1.),(1.,1.),(1.,
1.),(1.,1.),(1.,1.),(1.,1.),(1.,1.),(1.,1.),(1.,1.),(1.,1.),(1.,1.),(1.,
1.),(1.,1.),(1.,1.),(1.,1.),(1.,1.),(1.,1.),(1.,1.),(1.,1.),(1.,1.),(1.,
1.),(1.,1.),(1.,1.),(1.,1.),(1.,1.),(1.,1.),(1.,1.),(1.,1.),(1.,1.),(1.,
1.),(1.,1.),(1.,1.),(1.,1.),(1.,1.),(1.,1.),(1.,1.),(1.,1.),(1.,1.),(1.,
1.),(1.,1.),(1.,1.),(1.,1.),(1.,1.),(1.,1.),(1.,1.),(1.,1.),(1.,1.),(1.,
1.),(1.,1.),(1.,1.),(1.,1.),(1.,1.),(1.,1.),(1.,1.),(1.,1.),(1.,1.),(1.,
1.),(1.,1.),(1.,1.),(1.,1.),(1.,1.),(1.,1.),(1.,1.),(1.,1.),(1.,1.),(1.,
1.),(1.,1.),(1.,1.),(1.,1.),(1.,1.),(1.,1.),(1.,1.),(1.,1.),(1.,1.),(1.,
1.),(1.,1.),(1.,1.),(1.,1.),(1.,1.),(1.,1.),(1.,1.),(1.,1.),(1.,1.),(1.,
1.),(1.,1.),(1.,1.),(1.,1.),(1.,1.),(1.,1.),(1.,1.),(1.,1.),(1.,1.),(1.,
1.),(1.,1.)))
REPRESENTATION_ITEM('')
SURFACE()
);
#982=(
BOUNDED_SURFACE()
B_SPLINE_SURFACE(5,1,((#138620,#138621),(#138622,#138623),(#138624,#138625),
(#138626,#138627),(#138628,#138629),(#138630,#138631),(#138632,#138633),
(#138634,#138635),(#138636,#138637),(#138638,#138639),(#138640,#138641),
(#138642,#138643),(#138644,#138645),(#138646,#138647),(#138648,#138649),
(#138650,#138651),(#138652,#138653),(#138654,#138655),(#138656,#138657),
(#138658,#138659),(#138660,#138661),(#138662,#138663),(#138664,#138665),
(#138666,#138667),(#138668,#138669),(#138670,#138671),(#138672,#138673),
(#138674,#138675),(#138676,#138677),(#138678,#138679),(#138680,#138681),
(#138682,#138683),(#138684,#138685),(#138686,#138687),(#138688,#138689),
(#138690,#138691),(#138692,#138693),(#138694,#138695),(#138696,#138697),
(#138698,#138699),(#138700,#138701),(#138702,#138703),(#138704,#138705),
(#138706,#138707),(#138708,#138709),(#138710,#138711),(#138712,#138713),
(#138714,#138715),(#138716,#138717),(#138718,#138719),(#138720,#138721),
(#138722,#138723),(#138724,#138725),(#138726,#138727),(#138728,#138729),
(#138730,#138731),(#138732,#138733),(#138734,#138735),(#138736,#138737),
(#138738,#138739),(#138740,#138741),(#138742,#138743),(#138744,#138745),
(#138746,#138747),(#138748,#138749),(#138750,#138751),(#138752,#138753),
(#138754,#138755),(#138756,#138757),(#138758,#138759),(#138760,#138761),
(#138762,#138763),(#138764,#138765),(#138766,#138767),(#138768,#138769),
(#138770,#138771),(#138772,#138773),(#138774,#138775),(#138776,#138777),
(#138778,#138779),(#138780,#138781),(#138782,#138783),(#138784,#138785),
(#138786,#138787),(#138788,#138789),(#138790,#138791),(#138792,#138793),
(#138794,#138795),(#138796,#138797),(#138798,#138799),(#138800,#138801),
(#138802,#138803),(#138804,#138805),(#138806,#138807),(#138808,#138809),
(#138810,#138811),(#138812,#138813),(#138814,#138815),(#138816,#138817),
(#138818,#138819),(#138820,#138821),(#138822,#138823),(#138824,#138825),
(#138826,#138827),(#138828,#138829),(#138830,#138831),(#138832,#138833),
(#138834,#138835),(#138836,#138837),(#138838,#138839),(#138840,#138841),
(#138842,#138843),(#138844,#138845),(#138846,#138847),(#138848,#138849),
(#138850,#138851),(#138852,#138853),(#138854,#138855),(#138856,#138857),
(#138858,#138859),(#138860,#138861),(#138862,#138863),(#138864,#138865),
(#138866,#138867),(#138868,#138869),(#138870,#138871),(#138872,#138873),
(#138874,#138875),(#138876,#138877),(#138878,#138879),(#138880,#138881),
(#138882,#138883),(#138884,#138885),(#138886,#138887),(#138888,#138889),
(#138890,#138891),(#138892,#138893),(#138894,#138895),(#138896,#138897),
(#138898,#138899),(#138900,#138901),(#138902,#138903),(#138904,#138905),
(#138906,#138907),(#138908,#138909),(#138910,#138911),(#138912,#138913),
(#138914,#138915),(#138916,#138917),(#138918,#138919),(#138920,#138921),
(#138922,#138923),(#138924,#138925),(#138926,#138927),(#138928,#138929),
(#138930,#138931),(#138932,#138933),(#138934,#138935),(#138936,#138937),
(#138938,#138939),(#138940,#138941),(#138942,#138943),(#138944,#138945),
(#138946,#138947),(#138948,#138949),(#138950,#138951),(#138952,#138953),
(#138954,#138955),(#138956,#138957),(#138958,#138959),(#138960,#138961),
(#138962,#138963),(#138964,#138965),(#138966,#138967),(#138968,#138969),
(#138970,#138971),(#138972,#138973),(#138974,#138975),(#138976,#138977),
(#138978,#138979),(#138980,#138981),(#138982,#138983),(#138984,#138985),
(#138986,#138987),(#138988,#138989),(#138990,#138991),(#138992,#138993),
(#138994,#138995),(#138996,#138997),(#138998,#138999),(#139000,#139001),
(#139002,#139003),(#139004,#139005),(#139006,#139007),(#139008,#139009),
(#139010,#139011),(#139012,#139013),(#139014,#139015),(#139016,#139017),
(#139018,#139019),(#139020,#139021),(#139022,#139023),(#139024,#139025),
(#139026,#139027),(#139028,#139029)),.UNSPECIFIED.,.F.,.F.,.F.)
B_SPLINE_SURFACE_WITH_KNOTS((6,1,1,1,1,1,1,1,1,1,1,1,1,1,1,1,1,1,1,1,1,
1,1,1,1,1,1,1,1,1,1,1,1,1,1,1,1,1,1,1,1,1,1,1,1,1,1,1,1,1,1,1,1,1,1,1,1,
1,1,1,1,1,1,1,1,1,1,1,1,1,1,1,1,1,1,1,1,1,1,1,1,1,1,1,1,1,1,1,1,1,1,1,1,
1,1,1,1,1,1,1,1,1,1,1,1,1,1,1,1,1,1,1,1,1,1,1,1,1,1,1,1,1,1,1,1,1,1,1,1,
1,1,1,1,1,1,1,1,1,1,1,1,1,1,1,1,1,1,1,1,1,1,1,1,1,1,1,1,1,1,1,1,1,1,1,1,
1,1,1,1,1,1,1,1,1,1,1,1,1,1,1,1,1,1,1,1,1,1,1,1,1,1,1,1,1,1,1,1,1,1,1,6),
(2,2),(-1.,-0.995000000000001,-0.990000000000001,-0.985000000000001,-0.980000000000001,
-0.975000000000001,-0.970000000000001,-0.965000000000001,-0.960000000000001,
-0.955000000000001,-0.950000000000001,-0.945000000000001,-0.940000000000001,
-0.935000000000001,-0.930000000000001,-0.925000000000001,-0.920000000000001,
-0.915000000000001,-0.910000000000001,-0.905000000000001,-0.900000000000001,
-0.895000000000001,-0.890000000000001,-0.885000000000001,-0.880000000000001,
-0.875000000000001,-0.870000000000001,-0.865000000000001,-0.860000000000001,
-0.855000000000001,-0.850000000000001,-0.845000000000001,-0.840000000000001,
-0.835000000000001,-0.830000000000001,-0.825000000000001,-0.820000000000001,
-0.815000000000001,-0.810000000000001,-0.805000000000001,-0.800000000000001,
-0.795000000000001,-0.790000000000001,-0.785000000000001,-0.780000000000001,
-0.775000000000001,-0.770000000000001,-0.765000000000001,-0.760000000000001,
-0.755000000000001,-0.750000000000001,-0.745000000000001,-0.740000000000001,
-0.735000000000001,-0.730000000000001,-0.725000000000001,-0.720000000000001,
-0.715000000000001,-0.710000000000001,-0.705000000000001,-0.700000000000001,
-0.695000000000001,-0.690000000000001,-0.685,-0.68,-0.675,-0.67,-0.665,
-0.66,-0.655,-0.65,-0.645,-0.64,-0.635,-0.63,-0.625,-0.62,-0.615,-0.61,
-0.605,-0.6,-0.595,-0.59,-0.585,-0.58,-0.575,-0.57,-0.565,-0.56,-0.555,
-0.55,-0.545,-0.54,-0.535,-0.53,-0.525,-0.52,-0.515,-0.51,-0.505,-0.5,-0.495,
-0.49,-0.485,-0.48,-0.475,-0.47,-0.465,-0.46,-0.455,-0.45,-0.445,-0.44,
-0.435,-0.43,-0.425,-0.42,-0.415,-0.41,-0.405,-0.4,-0.395,-0.39,-0.385,
-0.38,-0.375,-0.37,-0.365,-0.36,-0.355,-0.35,-0.345,-0.34,-0.335,-0.33,
-0.325,-0.32,-0.315,-0.31,-0.305,-0.3,-0.295,-0.29,-0.285,-0.28,-0.275,
-0.27,-0.265,-0.26,-0.255,-0.25,-0.245,-0.24,-0.235,-0.23,-0.225,-0.22,
-0.215,-0.21,-0.205,-0.2,-0.195,-0.19,-0.185,-0.18,-0.175,-0.17,-0.165,
-0.16,-0.155,-0.15,-0.145,-0.14,-0.135,-0.13,-0.125,-0.12,-0.115,-0.11,
-0.105,-0.1,-0.095,-0.09,-0.085,-0.08,-0.075,-0.07,-0.065,-0.06,-0.055,
-0.05,-0.045,-0.04,-0.035,-0.03,-0.025,-0.02,-0.015,-0.01,-0.005,0.),(0.,
1.2),.UNSPECIFIED.)
GEOMETRIC_REPRESENTATION_ITEM()
RATIONAL_B_SPLINE_SURFACE(((1.,1.),(1.,1.),(1.,1.),(1.,1.),(1.,1.),(1.,
1.),(1.,1.),(1.,1.),(1.,1.),(1.,1.),(1.,1.),(1.,1.),(1.,1.),(1.,1.),(1.,
1.),(1.,1.),(1.,1.),(1.,1.),(1.,1.),(1.,1.),(1.,1.),(1.,1.),(1.,1.),(1.,
1.),(1.,1.),(1.,1.),(1.,1.),(1.,1.),(1.,1.),(1.,1.),(1.,1.),(1.,1.),(1.,
1.),(1.,1.),(1.,1.),(1.,1.),(1.,1.),(1.,1.),(1.,1.),(1.,1.),(1.,1.),(1.,
1.),(1.,1.),(1.,1.),(1.,1.),(1.,1.),(1.,1.),(1.,1.),(1.,1.),(1.,1.),(1.,
1.),(1.,1.),(1.,1.),(1.,1.),(1.,1.),(1.,1.),(1.,1.),(1.,1.),(1.,1.),(1.,
1.),(1.,1.),(1.,1.),(1.,1.),(1.,1.),(1.,1.),(1.,1.),(1.,1.),(1.,1.),(1.,
1.),(1.,1.),(1.,1.),(1.,1.),(1.,1.),(1.,1.),(1.,1.),(1.,1.),(1.,1.),(1.,
1.),(1.,1.),(1.,1.),(1.,1.),(1.,1.),(1.,1.),(1.,1.),(1.,1.),(1.,1.),(1.,
1.),(1.,1.),(1.,1.),(1.,1.),(1.,1.),(1.,1.),(1.,1.),(1.,1.),(1.,1.),(1.,
1.),(1.,1.),(1.,1.),(1.,1.),(1.,1.),(1.,1.),(1.,1.),(1.,1.),(1.,1.),(1.,
1.),(1.,1.),(1.,1.),(1.,1.),(1.,1.),(1.,1.),(1.,1.),(1.,1.),(1.,1.),(1.,
1.),(1.,1.),(1.,1.),(1.,1.),(1.,1.),(1.,1.),(1.,1.),(1.,1.),(1.,1.),(1.,
1.),(1.,1.),(1.,1.),(1.,1.),(1.,1.),(1.,1.),(1.,1.),(1.,1.),(1.,1.),(1.,
1.),(1.,1.),(1.,1.),(1.,1.),(1.,1.),(1.,1.),(1.,1.),(1.,1.),(1.,1.),(1.,
1.),(1.,1.),(1.,1.),(1.,1.),(1.,1.),(1.,1.),(1.,1.),(1.,1.),(1.,1.),(1.,
1.),(1.,1.),(1.,1.),(1.,1.),(1.,1.),(1.,1.),(1.,1.),(1.,1.),(1.,1.),(1.,
1.),(1.,1.),(1.,1.),(1.,1.),(1.,1.),(1.,1.),(1.,1.),(1.,1.),(1.,1.),(1.,
1.),(1.,1.),(1.,1.),(1.,1.),(1.,1.),(1.,1.),(1.,1.),(1.,1.),(1.,1.),(1.,
1.),(1.,1.),(1.,1.),(1.,1.),(1.,1.),(1.,1.),(1.,1.),(1.,1.),(1.,1.),(1.,
1.),(1.,1.),(1.,1.),(1.,1.),(1.,1.),(1.,1.),(1.,1.),(1.,1.),(1.,1.),(1.,
1.),(1.,1.),(1.,1.),(1.,1.),(1.,1.),(1.,1.),(1.,1.),(1.,1.),(1.,1.),(1.,
1.),(1.,1.)))
REPRESENTATION_ITEM('')
SURFACE()
);
#983=(
BOUNDED_SURFACE()
B_SPLINE_SURFACE(5,1,((#139421,#139422),(#139423,#139424),(#139425,#139426),
(#139427,#139428),(#139429,#139430),(#139431,#139432),(#139433,#139434),
(#139435,#139436),(#139437,#139438),(#139439,#139440),(#139441,#139442),
(#139443,#139444),(#139445,#139446),(#139447,#139448),(#139449,#139450),
(#139451,#139452),(#139453,#139454),(#139455,#139456),(#139457,#139458),
(#139459,#139460),(#139461,#139462),(#139463,#139464),(#139465,#139466),
(#139467,#139468),(#139469,#139470),(#139471,#139472),(#139473,#139474),
(#139475,#139476),(#139477,#139478),(#139479,#139480),(#139481,#139482),
(#139483,#139484),(#139485,#139486),(#139487,#139488),(#139489,#139490),
(#139491,#139492),(#139493,#139494),(#139495,#139496),(#139497,#139498),
(#139499,#139500),(#139501,#139502),(#139503,#139504),(#139505,#139506),
(#139507,#139508),(#139509,#139510),(#139511,#139512),(#139513,#139514),
(#139515,#139516),(#139517,#139518),(#139519,#139520),(#139521,#139522),
(#139523,#139524),(#139525,#139526),(#139527,#139528),(#139529,#139530),
(#139531,#139532),(#139533,#139534),(#139535,#139536),(#139537,#139538),
(#139539,#139540),(#139541,#139542),(#139543,#139544),(#139545,#139546),
(#139547,#139548),(#139549,#139550),(#139551,#139552),(#139553,#139554),
(#139555,#139556),(#139557,#139558),(#139559,#139560),(#139561,#139562),
(#139563,#139564),(#139565,#139566),(#139567,#139568),(#139569,#139570),
(#139571,#139572),(#139573,#139574),(#139575,#139576),(#139577,#139578),
(#139579,#139580),(#139581,#139582),(#139583,#139584),(#139585,#139586),
(#139587,#139588),(#139589,#139590),(#139591,#139592),(#139593,#139594),
(#139595,#139596),(#139597,#139598),(#139599,#139600),(#139601,#139602),
(#139603,#139604),(#139605,#139606),(#139607,#139608),(#139609,#139610),
(#139611,#139612),(#139613,#139614),(#139615,#139616),(#139617,#139618),
(#139619,#139620),(#139621,#139622),(#139623,#139624),(#139625,#139626),
(#139627,#139628),(#139629,#139630),(#139631,#139632),(#139633,#139634),
(#139635,#139636),(#139637,#139638),(#139639,#139640),(#139641,#139642),
(#139643,#139644),(#139645,#139646),(#139647,#139648),(#139649,#139650),
(#139651,#139652),(#139653,#139654),(#139655,#139656),(#139657,#139658),
(#139659,#139660),(#139661,#139662),(#139663,#139664),(#139665,#139666),
(#139667,#139668),(#139669,#139670),(#139671,#139672),(#139673,#139674),
(#139675,#139676),(#139677,#139678),(#139679,#139680),(#139681,#139682),
(#139683,#139684),(#139685,#139686),(#139687,#139688),(#139689,#139690),
(#139691,#139692),(#139693,#139694),(#139695,#139696),(#139697,#139698),
(#139699,#139700),(#139701,#139702),(#139703,#139704),(#139705,#139706),
(#139707,#139708),(#139709,#139710),(#139711,#139712),(#139713,#139714),
(#139715,#139716),(#139717,#139718),(#139719,#139720),(#139721,#139722),
(#139723,#139724),(#139725,#139726),(#139727,#139728),(#139729,#139730),
(#139731,#139732),(#139733,#139734),(#139735,#139736),(#139737,#139738),
(#139739,#139740),(#139741,#139742),(#139743,#139744),(#139745,#139746),
(#139747,#139748),(#139749,#139750),(#139751,#139752),(#139753,#139754),
(#139755,#139756),(#139757,#139758),(#139759,#139760),(#139761,#139762),
(#139763,#139764),(#139765,#139766),(#139767,#139768),(#139769,#139770),
(#139771,#139772),(#139773,#139774),(#139775,#139776),(#139777,#139778),
(#139779,#139780),(#139781,#139782),(#139783,#139784),(#139785,#139786),
(#139787,#139788),(#139789,#139790),(#139791,#139792),(#139793,#139794),
(#139795,#139796),(#139797,#139798),(#139799,#139800),(#139801,#139802),
(#139803,#139804),(#139805,#139806),(#139807,#139808),(#139809,#139810),
(#139811,#139812),(#139813,#139814),(#139815,#139816),(#139817,#139818),
(#139819,#139820),(#139821,#139822),(#139823,#139824),(#139825,#139826),
(#139827,#139828),(#139829,#139830)),.UNSPECIFIED.,.F.,.F.,.F.)
B_SPLINE_SURFACE_WITH_KNOTS((6,1,1,1,1,1,1,1,1,1,1,1,1,1,1,1,1,1,1,1,1,
1,1,1,1,1,1,1,1,1,1,1,1,1,1,1,1,1,1,1,1,1,1,1,1,1,1,1,1,1,1,1,1,1,1,1,1,
1,1,1,1,1,1,1,1,1,1,1,1,1,1,1,1,1,1,1,1,1,1,1,1,1,1,1,1,1,1,1,1,1,1,1,1,
1,1,1,1,1,1,1,1,1,1,1,1,1,1,1,1,1,1,1,1,1,1,1,1,1,1,1,1,1,1,1,1,1,1,1,1,
1,1,1,1,1,1,1,1,1,1,1,1,1,1,1,1,1,1,1,1,1,1,1,1,1,1,1,1,1,1,1,1,1,1,1,1,
1,1,1,1,1,1,1,1,1,1,1,1,1,1,1,1,1,1,1,1,1,1,1,1,1,1,1,1,1,1,1,1,1,1,1,6),
(2,2),(-1.,-0.995000000000001,-0.990000000000001,-0.985000000000001,-0.980000000000001,
-0.975000000000001,-0.970000000000001,-0.965000000000001,-0.960000000000001,
-0.955000000000001,-0.950000000000001,-0.945000000000001,-0.940000000000001,
-0.935000000000001,-0.930000000000001,-0.925000000000001,-0.920000000000001,
-0.915000000000001,-0.910000000000001,-0.905000000000001,-0.900000000000001,
-0.895000000000001,-0.890000000000001,-0.885000000000001,-0.880000000000001,
-0.875000000000001,-0.870000000000001,-0.865000000000001,-0.860000000000001,
-0.855000000000001,-0.850000000000001,-0.845000000000001,-0.840000000000001,
-0.835000000000001,-0.830000000000001,-0.825000000000001,-0.820000000000001,
-0.815000000000001,-0.810000000000001,-0.805000000000001,-0.800000000000001,
-0.795000000000001,-0.790000000000001,-0.785000000000001,-0.780000000000001,
-0.775000000000001,-0.770000000000001,-0.765000000000001,-0.760000000000001,
-0.755000000000001,-0.750000000000001,-0.745000000000001,-0.740000000000001,
-0.735000000000001,-0.730000000000001,-0.725000000000001,-0.720000000000001,
-0.715000000000001,-0.710000000000001,-0.705000000000001,-0.700000000000001,
-0.695000000000001,-0.690000000000001,-0.685,-0.68,-0.675,-0.67,-0.665,
-0.66,-0.655,-0.65,-0.645,-0.64,-0.635,-0.63,-0.625,-0.62,-0.615,-0.61,
-0.605,-0.6,-0.595,-0.59,-0.585,-0.58,-0.575,-0.57,-0.565,-0.56,-0.555,
-0.55,-0.545,-0.54,-0.535,-0.53,-0.525,-0.52,-0.515,-0.51,-0.505,-0.5,-0.495,
-0.49,-0.485,-0.48,-0.475,-0.47,-0.465,-0.46,-0.455,-0.45,-0.445,-0.44,
-0.435,-0.43,-0.425,-0.42,-0.415,-0.41,-0.405,-0.4,-0.395,-0.39,-0.385,
-0.38,-0.375,-0.37,-0.365,-0.36,-0.355,-0.35,-0.345,-0.34,-0.335,-0.33,
-0.325,-0.32,-0.315,-0.31,-0.305,-0.3,-0.295,-0.29,-0.285,-0.28,-0.275,
-0.27,-0.265,-0.26,-0.255,-0.25,-0.245,-0.24,-0.235,-0.23,-0.225,-0.22,
-0.215,-0.21,-0.205,-0.2,-0.195,-0.19,-0.185,-0.18,-0.175,-0.17,-0.165,
-0.16,-0.155,-0.15,-0.145,-0.14,-0.135,-0.13,-0.125,-0.12,-0.115,-0.11,
-0.105,-0.1,-0.095,-0.09,-0.085,-0.08,-0.075,-0.07,-0.065,-0.06,-0.055,
-0.05,-0.045,-0.04,-0.035,-0.03,-0.025,-0.02,-0.015,-0.01,-0.005,0.),(0.,
1.2),.UNSPECIFIED.)
GEOMETRIC_REPRESENTATION_ITEM()
RATIONAL_B_SPLINE_SURFACE(((1.,1.),(1.,1.),(1.,1.),(1.,1.),(1.,1.),(1.,
1.),(1.,1.),(1.,1.),(1.,1.),(1.,1.),(1.,1.),(1.,1.),(1.,1.),(1.,1.),(1.,
1.),(1.,1.),(1.,1.),(1.,1.),(1.,1.),(1.,1.),(1.,1.),(1.,1.),(1.,1.),(1.,
1.),(1.,1.),(1.,1.),(1.,1.),(1.,1.),(1.,1.),(1.,1.),(1.,1.),(1.,1.),(1.,
1.),(1.,1.),(1.,1.),(1.,1.),(1.,1.),(1.,1.),(1.,1.),(1.,1.),(1.,1.),(1.,
1.),(1.,1.),(1.,1.),(1.,1.),(1.,1.),(1.,1.),(1.,1.),(1.,1.),(1.,1.),(1.,
1.),(1.,1.),(1.,1.),(1.,1.),(1.,1.),(1.,1.),(1.,1.),(1.,1.),(1.,1.),(1.,
1.),(1.,1.),(1.,1.),(1.,1.),(1.,1.),(1.,1.),(1.,1.),(1.,1.),(1.,1.),(1.,
1.),(1.,1.),(1.,1.),(1.,1.),(1.,1.),(1.,1.),(1.,1.),(1.,1.),(1.,1.),(1.,
1.),(1.,1.),(1.,1.),(1.,1.),(1.,1.),(1.,1.),(1.,1.),(1.,1.),(1.,1.),(1.,
1.),(1.,1.),(1.,1.),(1.,1.),(1.,1.),(1.,1.),(1.,1.),(1.,1.),(1.,1.),(1.,
1.),(1.,1.),(1.,1.),(1.,1.),(1.,1.),(1.,1.),(1.,1.),(1.,1.),(1.,1.),(1.,
1.),(1.,1.),(1.,1.),(1.,1.),(1.,1.),(1.,1.),(1.,1.),(1.,1.),(1.,1.),(1.,
1.),(1.,1.),(1.,1.),(1.,1.),(1.,1.),(1.,1.),(1.,1.),(1.,1.),(1.,1.),(1.,
1.),(1.,1.),(1.,1.),(1.,1.),(1.,1.),(1.,1.),(1.,1.),(1.,1.),(1.,1.),(1.,
1.),(1.,1.),(1.,1.),(1.,1.),(1.,1.),(1.,1.),(1.,1.),(1.,1.),(1.,1.),(1.,
1.),(1.,1.),(1.,1.),(1.,1.),(1.,1.),(1.,1.),(1.,1.),(1.,1.),(1.,1.),(1.,
1.),(1.,1.),(1.,1.),(1.,1.),(1.,1.),(1.,1.),(1.,1.),(1.,1.),(1.,1.),(1.,
1.),(1.,1.),(1.,1.),(1.,1.),(1.,1.),(1.,1.),(1.,1.),(1.,1.),(1.,1.),(1.,
1.),(1.,1.),(1.,1.),(1.,1.),(1.,1.),(1.,1.),(1.,1.),(1.,1.),(1.,1.),(1.,
1.),(1.,1.),(1.,1.),(1.,1.),(1.,1.),(1.,1.),(1.,1.),(1.,1.),(1.,1.),(1.,
1.),(1.,1.),(1.,1.),(1.,1.),(1.,1.),(1.,1.),(1.,1.),(1.,1.),(1.,1.),(1.,
1.),(1.,1.),(1.,1.),(1.,1.),(1.,1.),(1.,1.),(1.,1.),(1.,1.),(1.,1.),(1.,
1.),(1.,1.)))
REPRESENTATION_ITEM('')
SURFACE()
);
#984=(
BOUNDED_SURFACE()
B_SPLINE_SURFACE(5,1,((#140222,#140223),(#140224,#140225),(#140226,#140227),
(#140228,#140229),(#140230,#140231),(#140232,#140233),(#140234,#140235),
(#140236,#140237),(#140238,#140239),(#140240,#140241),(#140242,#140243),
(#140244,#140245),(#140246,#140247),(#140248,#140249),(#140250,#140251),
(#140252,#140253),(#140254,#140255),(#140256,#140257),(#140258,#140259),
(#140260,#140261),(#140262,#140263),(#140264,#140265),(#140266,#140267),
(#140268,#140269),(#140270,#140271),(#140272,#140273),(#140274,#140275),
(#140276,#140277),(#140278,#140279),(#140280,#140281),(#140282,#140283),
(#140284,#140285),(#140286,#140287),(#140288,#140289),(#140290,#140291),
(#140292,#140293),(#140294,#140295),(#140296,#140297),(#140298,#140299),
(#140300,#140301),(#140302,#140303),(#140304,#140305),(#140306,#140307),
(#140308,#140309),(#140310,#140311),(#140312,#140313),(#140314,#140315),
(#140316,#140317),(#140318,#140319),(#140320,#140321),(#140322,#140323),
(#140324,#140325),(#140326,#140327),(#140328,#140329),(#140330,#140331),
(#140332,#140333),(#140334,#140335),(#140336,#140337),(#140338,#140339),
(#140340,#140341),(#140342,#140343),(#140344,#140345),(#140346,#140347),
(#140348,#140349),(#140350,#140351),(#140352,#140353),(#140354,#140355),
(#140356,#140357),(#140358,#140359),(#140360,#140361),(#140362,#140363),
(#140364,#140365),(#140366,#140367),(#140368,#140369),(#140370,#140371),
(#140372,#140373),(#140374,#140375),(#140376,#140377),(#140378,#140379),
(#140380,#140381),(#140382,#140383),(#140384,#140385),(#140386,#140387),
(#140388,#140389),(#140390,#140391),(#140392,#140393),(#140394,#140395),
(#140396,#140397),(#140398,#140399),(#140400,#140401),(#140402,#140403),
(#140404,#140405),(#140406,#140407),(#140408,#140409),(#140410,#140411),
(#140412,#140413),(#140414,#140415),(#140416,#140417),(#140418,#140419),
(#140420,#140421),(#140422,#140423),(#140424,#140425),(#140426,#140427),
(#140428,#140429),(#140430,#140431),(#140432,#140433),(#140434,#140435),
(#140436,#140437),(#140438,#140439),(#140440,#140441),(#140442,#140443),
(#140444,#140445),(#140446,#140447),(#140448,#140449),(#140450,#140451),
(#140452,#140453),(#140454,#140455),(#140456,#140457),(#140458,#140459),
(#140460,#140461),(#140462,#140463),(#140464,#140465),(#140466,#140467),
(#140468,#140469),(#140470,#140471),(#140472,#140473),(#140474,#140475),
(#140476,#140477),(#140478,#140479),(#140480,#140481),(#140482,#140483),
(#140484,#140485),(#140486,#140487),(#140488,#140489),(#140490,#140491),
(#140492,#140493),(#140494,#140495),(#140496,#140497),(#140498,#140499),
(#140500,#140501),(#140502,#140503),(#140504,#140505),(#140506,#140507),
(#140508,#140509),(#140510,#140511),(#140512,#140513),(#140514,#140515),
(#140516,#140517),(#140518,#140519),(#140520,#140521),(#140522,#140523),
(#140524,#140525),(#140526,#140527),(#140528,#140529),(#140530,#140531),
(#140532,#140533),(#140534,#140535),(#140536,#140537),(#140538,#140539),
(#140540,#140541),(#140542,#140543),(#140544,#140545),(#140546,#140547),
(#140548,#140549),(#140550,#140551),(#140552,#140553),(#140554,#140555),
(#140556,#140557),(#140558,#140559),(#140560,#140561),(#140562,#140563),
(#140564,#140565),(#140566,#140567),(#140568,#140569),(#140570,#140571),
(#140572,#140573),(#140574,#140575),(#140576,#140577),(#140578,#140579),
(#140580,#140581),(#140582,#140583),(#140584,#140585),(#140586,#140587),
(#140588,#140589),(#140590,#140591),(#140592,#140593),(#140594,#140595),
(#140596,#140597),(#140598,#140599),(#140600,#140601),(#140602,#140603),
(#140604,#140605),(#140606,#140607),(#140608,#140609),(#140610,#140611),
(#140612,#140613),(#140614,#140615),(#140616,#140617),(#140618,#140619),
(#140620,#140621),(#140622,#140623),(#140624,#140625),(#140626,#140627),
(#140628,#140629),(#140630,#140631)),.UNSPECIFIED.,.F.,.F.,.F.)
B_SPLINE_SURFACE_WITH_KNOTS((6,1,1,1,1,1,1,1,1,1,1,1,1,1,1,1,1,1,1,1,1,
1,1,1,1,1,1,1,1,1,1,1,1,1,1,1,1,1,1,1,1,1,1,1,1,1,1,1,1,1,1,1,1,1,1,1,1,
1,1,1,1,1,1,1,1,1,1,1,1,1,1,1,1,1,1,1,1,1,1,1,1,1,1,1,1,1,1,1,1,1,1,1,1,
1,1,1,1,1,1,1,1,1,1,1,1,1,1,1,1,1,1,1,1,1,1,1,1,1,1,1,1,1,1,1,1,1,1,1,1,
1,1,1,1,1,1,1,1,1,1,1,1,1,1,1,1,1,1,1,1,1,1,1,1,1,1,1,1,1,1,1,1,1,1,1,1,
1,1,1,1,1,1,1,1,1,1,1,1,1,1,1,1,1,1,1,1,1,1,1,1,1,1,1,1,1,1,1,1,1,1,1,6),
(2,2),(-1.,-0.995000000000001,-0.990000000000001,-0.985000000000001,-0.980000000000001,
-0.975000000000001,-0.970000000000001,-0.965000000000001,-0.960000000000001,
-0.955000000000001,-0.950000000000001,-0.945000000000001,-0.940000000000001,
-0.935000000000001,-0.930000000000001,-0.925000000000001,-0.920000000000001,
-0.915000000000001,-0.910000000000001,-0.905000000000001,-0.900000000000001,
-0.895000000000001,-0.890000000000001,-0.885000000000001,-0.880000000000001,
-0.875000000000001,-0.870000000000001,-0.865000000000001,-0.860000000000001,
-0.855000000000001,-0.850000000000001,-0.845000000000001,-0.840000000000001,
-0.835000000000001,-0.830000000000001,-0.825000000000001,-0.820000000000001,
-0.815000000000001,-0.810000000000001,-0.805000000000001,-0.800000000000001,
-0.795000000000001,-0.790000000000001,-0.785000000000001,-0.780000000000001,
-0.775000000000001,-0.770000000000001,-0.765000000000001,-0.760000000000001,
-0.755000000000001,-0.750000000000001,-0.745000000000001,-0.740000000000001,
-0.735000000000001,-0.730000000000001,-0.725000000000001,-0.720000000000001,
-0.715000000000001,-0.710000000000001,-0.705000000000001,-0.700000000000001,
-0.695000000000001,-0.690000000000001,-0.685,-0.68,-0.675,-0.67,-0.665,
-0.66,-0.655,-0.65,-0.645,-0.64,-0.635,-0.63,-0.625,-0.62,-0.615,-0.61,
-0.605,-0.6,-0.595,-0.59,-0.585,-0.58,-0.575,-0.57,-0.565,-0.56,-0.555,
-0.55,-0.545,-0.54,-0.535,-0.53,-0.525,-0.52,-0.515,-0.51,-0.505,-0.5,-0.495,
-0.49,-0.485,-0.48,-0.475,-0.47,-0.465,-0.46,-0.455,-0.45,-0.445,-0.44,
-0.435,-0.43,-0.425,-0.42,-0.415,-0.41,-0.405,-0.4,-0.395,-0.39,-0.385,
-0.38,-0.375,-0.37,-0.365,-0.36,-0.355,-0.35,-0.345,-0.34,-0.335,-0.33,
-0.325,-0.32,-0.315,-0.31,-0.305,-0.3,-0.295,-0.29,-0.285,-0.28,-0.275,
-0.27,-0.265,-0.26,-0.255,-0.25,-0.245,-0.24,-0.235,-0.23,-0.225,-0.22,
-0.215,-0.21,-0.205,-0.2,-0.195,-0.19,-0.185,-0.18,-0.175,-0.17,-0.165,
-0.16,-0.155,-0.15,-0.145,-0.14,-0.135,-0.13,-0.125,-0.12,-0.115,-0.11,
-0.105,-0.1,-0.095,-0.09,-0.085,-0.08,-0.075,-0.07,-0.065,-0.06,-0.055,
-0.05,-0.045,-0.04,-0.035,-0.03,-0.025,-0.02,-0.015,-0.01,-0.005,0.),(0.,
1.2),.UNSPECIFIED.)
GEOMETRIC_REPRESENTATION_ITEM()
RATIONAL_B_SPLINE_SURFACE(((1.,1.),(1.,1.),(1.,1.),(1.,1.),(1.,1.),(1.,
1.),(1.,1.),(1.,1.),(1.,1.),(1.,1.),(1.,1.),(1.,1.),(1.,1.),(1.,1.),(1.,
1.),(1.,1.),(1.,1.),(1.,1.),(1.,1.),(1.,1.),(1.,1.),(1.,1.),(1.,1.),(1.,
1.),(1.,1.),(1.,1.),(1.,1.),(1.,1.),(1.,1.),(1.,1.),(1.,1.),(1.,1.),(1.,
1.),(1.,1.),(1.,1.),(1.,1.),(1.,1.),(1.,1.),(1.,1.),(1.,1.),(1.,1.),(1.,
1.),(1.,1.),(1.,1.),(1.,1.),(1.,1.),(1.,1.),(1.,1.),(1.,1.),(1.,1.),(1.,
1.),(1.,1.),(1.,1.),(1.,1.),(1.,1.),(1.,1.),(1.,1.),(1.,1.),(1.,1.),(1.,
1.),(1.,1.),(1.,1.),(1.,1.),(1.,1.),(1.,1.),(1.,1.),(1.,1.),(1.,1.),(1.,
1.),(1.,1.),(1.,1.),(1.,1.),(1.,1.),(1.,1.),(1.,1.),(1.,1.),(1.,1.),(1.,
1.),(1.,1.),(1.,1.),(1.,1.),(1.,1.),(1.,1.),(1.,1.),(1.,1.),(1.,1.),(1.,
1.),(1.,1.),(1.,1.),(1.,1.),(1.,1.),(1.,1.),(1.,1.),(1.,1.),(1.,1.),(1.,
1.),(1.,1.),(1.,1.),(1.,1.),(1.,1.),(1.,1.),(1.,1.),(1.,1.),(1.,1.),(1.,
1.),(1.,1.),(1.,1.),(1.,1.),(1.,1.),(1.,1.),(1.,1.),(1.,1.),(1.,1.),(1.,
1.),(1.,1.),(1.,1.),(1.,1.),(1.,1.),(1.,1.),(1.,1.),(1.,1.),(1.,1.),(1.,
1.),(1.,1.),(1.,1.),(1.,1.),(1.,1.),(1.,1.),(1.,1.),(1.,1.),(1.,1.),(1.,
1.),(1.,1.),(1.,1.),(1.,1.),(1.,1.),(1.,1.),(1.,1.),(1.,1.),(1.,1.),(1.,
1.),(1.,1.),(1.,1.),(1.,1.),(1.,1.),(1.,1.),(1.,1.),(1.,1.),(1.,1.),(1.,
1.),(1.,1.),(1.,1.),(1.,1.),(1.,1.),(1.,1.),(1.,1.),(1.,1.),(1.,1.),(1.,
1.),(1.,1.),(1.,1.),(1.,1.),(1.,1.),(1.,1.),(1.,1.),(1.,1.),(1.,1.),(1.,
1.),(1.,1.),(1.,1.),(1.,1.),(1.,1.),(1.,1.),(1.,1.),(1.,1.),(1.,1.),(1.,
1.),(1.,1.),(1.,1.),(1.,1.),(1.,1.),(1.,1.),(1.,1.),(1.,1.),(1.,1.),(1.,
1.),(1.,1.),(1.,1.),(1.,1.),(1.,1.),(1.,1.),(1.,1.),(1.,1.),(1.,1.),(1.,
1.),(1.,1.),(1.,1.),(1.,1.),(1.,1.),(1.,1.),(1.,1.),(1.,1.),(1.,1.),(1.,
1.),(1.,1.)))
REPRESENTATION_ITEM('')
SURFACE()
);
#985=(
BOUNDED_SURFACE()
B_SPLINE_SURFACE(5,1,((#141023,#141024),(#141025,#141026),(#141027,#141028),
(#141029,#141030),(#141031,#141032),(#141033,#141034),(#141035,#141036),
(#141037,#141038),(#141039,#141040),(#141041,#141042),(#141043,#141044),
(#141045,#141046),(#141047,#141048),(#141049,#141050),(#141051,#141052),
(#141053,#141054),(#141055,#141056),(#141057,#141058),(#141059,#141060),
(#141061,#141062),(#141063,#141064),(#141065,#141066),(#141067,#141068),
(#141069,#141070),(#141071,#141072),(#141073,#141074),(#141075,#141076),
(#141077,#141078),(#141079,#141080),(#141081,#141082),(#141083,#141084),
(#141085,#141086),(#141087,#141088),(#141089,#141090),(#141091,#141092),
(#141093,#141094),(#141095,#141096),(#141097,#141098),(#141099,#141100),
(#141101,#141102),(#141103,#141104),(#141105,#141106),(#141107,#141108),
(#141109,#141110),(#141111,#141112),(#141113,#141114),(#141115,#141116),
(#141117,#141118),(#141119,#141120),(#141121,#141122),(#141123,#141124),
(#141125,#141126),(#141127,#141128),(#141129,#141130),(#141131,#141132),
(#141133,#141134),(#141135,#141136),(#141137,#141138),(#141139,#141140),
(#141141,#141142),(#141143,#141144),(#141145,#141146),(#141147,#141148),
(#141149,#141150),(#141151,#141152),(#141153,#141154),(#141155,#141156),
(#141157,#141158),(#141159,#141160),(#141161,#141162),(#141163,#141164),
(#141165,#141166),(#141167,#141168),(#141169,#141170),(#141171,#141172),
(#141173,#141174),(#141175,#141176),(#141177,#141178),(#141179,#141180),
(#141181,#141182),(#141183,#141184),(#141185,#141186),(#141187,#141188),
(#141189,#141190),(#141191,#141192),(#141193,#141194),(#141195,#141196),
(#141197,#141198),(#141199,#141200),(#141201,#141202),(#141203,#141204),
(#141205,#141206),(#141207,#141208),(#141209,#141210),(#141211,#141212),
(#141213,#141214),(#141215,#141216),(#141217,#141218),(#141219,#141220),
(#141221,#141222),(#141223,#141224),(#141225,#141226),(#141227,#141228),
(#141229,#141230),(#141231,#141232),(#141233,#141234),(#141235,#141236),
(#141237,#141238),(#141239,#141240),(#141241,#141242),(#141243,#141244),
(#141245,#141246),(#141247,#141248),(#141249,#141250),(#141251,#141252),
(#141253,#141254),(#141255,#141256),(#141257,#141258),(#141259,#141260),
(#141261,#141262),(#141263,#141264),(#141265,#141266),(#141267,#141268),
(#141269,#141270),(#141271,#141272),(#141273,#141274),(#141275,#141276),
(#141277,#141278),(#141279,#141280),(#141281,#141282),(#141283,#141284),
(#141285,#141286),(#141287,#141288),(#141289,#141290),(#141291,#141292),
(#141293,#141294),(#141295,#141296),(#141297,#141298),(#141299,#141300),
(#141301,#141302),(#141303,#141304),(#141305,#141306),(#141307,#141308),
(#141309,#141310),(#141311,#141312),(#141313,#141314),(#141315,#141316),
(#141317,#141318),(#141319,#141320),(#141321,#141322),(#141323,#141324),
(#141325,#141326),(#141327,#141328),(#141329,#141330),(#141331,#141332),
(#141333,#141334),(#141335,#141336),(#141337,#141338),(#141339,#141340),
(#141341,#141342),(#141343,#141344),(#141345,#141346),(#141347,#141348),
(#141349,#141350),(#141351,#141352),(#141353,#141354),(#141355,#141356),
(#141357,#141358),(#141359,#141360),(#141361,#141362),(#141363,#141364),
(#141365,#141366),(#141367,#141368),(#141369,#141370),(#141371,#141372),
(#141373,#141374),(#141375,#141376),(#141377,#141378),(#141379,#141380),
(#141381,#141382),(#141383,#141384),(#141385,#141386),(#141387,#141388),
(#141389,#141390),(#141391,#141392),(#141393,#141394),(#141395,#141396),
(#141397,#141398),(#141399,#141400),(#141401,#141402),(#141403,#141404),
(#141405,#141406),(#141407,#141408),(#141409,#141410),(#141411,#141412),
(#141413,#141414),(#141415,#141416),(#141417,#141418),(#141419,#141420),
(#141421,#141422),(#141423,#141424),(#141425,#141426),(#141427,#141428),
(#141429,#141430),(#141431,#141432)),.UNSPECIFIED.,.F.,.F.,.F.)
B_SPLINE_SURFACE_WITH_KNOTS((6,1,1,1,1,1,1,1,1,1,1,1,1,1,1,1,1,1,1,1,1,
1,1,1,1,1,1,1,1,1,1,1,1,1,1,1,1,1,1,1,1,1,1,1,1,1,1,1,1,1,1,1,1,1,1,1,1,
1,1,1,1,1,1,1,1,1,1,1,1,1,1,1,1,1,1,1,1,1,1,1,1,1,1,1,1,1,1,1,1,1,1,1,1,
1,1,1,1,1,1,1,1,1,1,1,1,1,1,1,1,1,1,1,1,1,1,1,1,1,1,1,1,1,1,1,1,1,1,1,1,
1,1,1,1,1,1,1,1,1,1,1,1,1,1,1,1,1,1,1,1,1,1,1,1,1,1,1,1,1,1,1,1,1,1,1,1,
1,1,1,1,1,1,1,1,1,1,1,1,1,1,1,1,1,1,1,1,1,1,1,1,1,1,1,1,1,1,1,1,1,1,1,6),
(2,2),(-1.,-0.995000000000001,-0.990000000000001,-0.985000000000001,-0.980000000000001,
-0.975000000000001,-0.970000000000001,-0.965000000000001,-0.960000000000001,
-0.955000000000001,-0.950000000000001,-0.945000000000001,-0.940000000000001,
-0.935000000000001,-0.930000000000001,-0.925000000000001,-0.920000000000001,
-0.915000000000001,-0.910000000000001,-0.905000000000001,-0.900000000000001,
-0.895000000000001,-0.890000000000001,-0.885000000000001,-0.880000000000001,
-0.875000000000001,-0.870000000000001,-0.865000000000001,-0.860000000000001,
-0.855000000000001,-0.850000000000001,-0.845000000000001,-0.840000000000001,
-0.835000000000001,-0.830000000000001,-0.825000000000001,-0.820000000000001,
-0.815000000000001,-0.810000000000001,-0.805000000000001,-0.800000000000001,
-0.795000000000001,-0.790000000000001,-0.785000000000001,-0.780000000000001,
-0.775000000000001,-0.770000000000001,-0.765000000000001,-0.760000000000001,
-0.755000000000001,-0.750000000000001,-0.745000000000001,-0.740000000000001,
-0.735000000000001,-0.730000000000001,-0.725000000000001,-0.720000000000001,
-0.715000000000001,-0.710000000000001,-0.705000000000001,-0.700000000000001,
-0.695000000000001,-0.690000000000001,-0.685,-0.68,-0.675,-0.67,-0.665,
-0.66,-0.655,-0.65,-0.645,-0.64,-0.635,-0.63,-0.625,-0.62,-0.615,-0.61,
-0.605,-0.6,-0.595,-0.59,-0.585,-0.58,-0.575,-0.57,-0.565,-0.56,-0.555,
-0.55,-0.545,-0.54,-0.535,-0.53,-0.525,-0.52,-0.515,-0.51,-0.505,-0.5,-0.495,
-0.49,-0.485,-0.48,-0.475,-0.47,-0.465,-0.46,-0.455,-0.45,-0.445,-0.44,
-0.435,-0.43,-0.425,-0.42,-0.415,-0.41,-0.405,-0.4,-0.395,-0.39,-0.385,
-0.38,-0.375,-0.37,-0.365,-0.36,-0.355,-0.35,-0.345,-0.34,-0.335,-0.33,
-0.325,-0.32,-0.315,-0.31,-0.305,-0.3,-0.295,-0.29,-0.285,-0.28,-0.275,
-0.27,-0.265,-0.26,-0.255,-0.25,-0.245,-0.24,-0.235,-0.23,-0.225,-0.22,
-0.215,-0.21,-0.205,-0.2,-0.195,-0.19,-0.185,-0.18,-0.175,-0.17,-0.165,
-0.16,-0.155,-0.15,-0.145,-0.14,-0.135,-0.13,-0.125,-0.12,-0.115,-0.11,
-0.105,-0.1,-0.095,-0.09,-0.085,-0.08,-0.075,-0.07,-0.065,-0.06,-0.055,
-0.05,-0.045,-0.04,-0.035,-0.03,-0.025,-0.02,-0.015,-0.01,-0.005,0.),(0.,
1.2),.UNSPECIFIED.)
GEOMETRIC_REPRESENTATION_ITEM()
RATIONAL_B_SPLINE_SURFACE(((1.,1.),(1.,1.),(1.,1.),(1.,1.),(1.,1.),(1.,
1.),(1.,1.),(1.,1.),(1.,1.),(1.,1.),(1.,1.),(1.,1.),(1.,1.),(1.,1.),(1.,
1.),(1.,1.),(1.,1.),(1.,1.),(1.,1.),(1.,1.),(1.,1.),(1.,1.),(1.,1.),(1.,
1.),(1.,1.),(1.,1.),(1.,1.),(1.,1.),(1.,1.),(1.,1.),(1.,1.),(1.,1.),(1.,
1.),(1.,1.),(1.,1.),(1.,1.),(1.,1.),(1.,1.),(1.,1.),(1.,1.),(1.,1.),(1.,
1.),(1.,1.),(1.,1.),(1.,1.),(1.,1.),(1.,1.),(1.,1.),(1.,1.),(1.,1.),(1.,
1.),(1.,1.),(1.,1.),(1.,1.),(1.,1.),(1.,1.),(1.,1.),(1.,1.),(1.,1.),(1.,
1.),(1.,1.),(1.,1.),(1.,1.),(1.,1.),(1.,1.),(1.,1.),(1.,1.),(1.,1.),(1.,
1.),(1.,1.),(1.,1.),(1.,1.),(1.,1.),(1.,1.),(1.,1.),(1.,1.),(1.,1.),(1.,
1.),(1.,1.),(1.,1.),(1.,1.),(1.,1.),(1.,1.),(1.,1.),(1.,1.),(1.,1.),(1.,
1.),(1.,1.),(1.,1.),(1.,1.),(1.,1.),(1.,1.),(1.,1.),(1.,1.),(1.,1.),(1.,
1.),(1.,1.),(1.,1.),(1.,1.),(1.,1.),(1.,1.),(1.,1.),(1.,1.),(1.,1.),(1.,
1.),(1.,1.),(1.,1.),(1.,1.),(1.,1.),(1.,1.),(1.,1.),(1.,1.),(1.,1.),(1.,
1.),(1.,1.),(1.,1.),(1.,1.),(1.,1.),(1.,1.),(1.,1.),(1.,1.),(1.,1.),(1.,
1.),(1.,1.),(1.,1.),(1.,1.),(1.,1.),(1.,1.),(1.,1.),(1.,1.),(1.,1.),(1.,
1.),(1.,1.),(1.,1.),(1.,1.),(1.,1.),(1.,1.),(1.,1.),(1.,1.),(1.,1.),(1.,
1.),(1.,1.),(1.,1.),(1.,1.),(1.,1.),(1.,1.),(1.,1.),(1.,1.),(1.,1.),(1.,
1.),(1.,1.),(1.,1.),(1.,1.),(1.,1.),(1.,1.),(1.,1.),(1.,1.),(1.,1.),(1.,
1.),(1.,1.),(1.,1.),(1.,1.),(1.,1.),(1.,1.),(1.,1.),(1.,1.),(1.,1.),(1.,
1.),(1.,1.),(1.,1.),(1.,1.),(1.,1.),(1.,1.),(1.,1.),(1.,1.),(1.,1.),(1.,
1.),(1.,1.),(1.,1.),(1.,1.),(1.,1.),(1.,1.),(1.,1.),(1.,1.),(1.,1.),(1.,
1.),(1.,1.),(1.,1.),(1.,1.),(1.,1.),(1.,1.),(1.,1.),(1.,1.),(1.,1.),(1.,
1.),(1.,1.),(1.,1.),(1.,1.),(1.,1.),(1.,1.),(1.,1.),(1.,1.),(1.,1.),(1.,
1.),(1.,1.)))
REPRESENTATION_ITEM('')
SURFACE()
);
#986=(
BOUNDED_SURFACE()
B_SPLINE_SURFACE(5,1,((#141824,#141825),(#141826,#141827),(#141828,#141829),
(#141830,#141831),(#141832,#141833),(#141834,#141835),(#141836,#141837),
(#141838,#141839),(#141840,#141841),(#141842,#141843),(#141844,#141845),
(#141846,#141847),(#141848,#141849),(#141850,#141851),(#141852,#141853),
(#141854,#141855),(#141856,#141857),(#141858,#141859),(#141860,#141861),
(#141862,#141863),(#141864,#141865),(#141866,#141867),(#141868,#141869),
(#141870,#141871),(#141872,#141873),(#141874,#141875),(#141876,#141877),
(#141878,#141879),(#141880,#141881),(#141882,#141883),(#141884,#141885),
(#141886,#141887),(#141888,#141889),(#141890,#141891),(#141892,#141893),
(#141894,#141895),(#141896,#141897),(#141898,#141899),(#141900,#141901),
(#141902,#141903),(#141904,#141905),(#141906,#141907),(#141908,#141909),
(#141910,#141911),(#141912,#141913),(#141914,#141915),(#141916,#141917),
(#141918,#141919),(#141920,#141921),(#141922,#141923),(#141924,#141925),
(#141926,#141927),(#141928,#141929),(#141930,#141931),(#141932,#141933),
(#141934,#141935),(#141936,#141937),(#141938,#141939),(#141940,#141941),
(#141942,#141943),(#141944,#141945),(#141946,#141947),(#141948,#141949),
(#141950,#141951),(#141952,#141953),(#141954,#141955),(#141956,#141957),
(#141958,#141959),(#141960,#141961),(#141962,#141963),(#141964,#141965),
(#141966,#141967),(#141968,#141969),(#141970,#141971),(#141972,#141973),
(#141974,#141975),(#141976,#141977),(#141978,#141979),(#141980,#141981),
(#141982,#141983),(#141984,#141985),(#141986,#141987),(#141988,#141989),
(#141990,#141991),(#141992,#141993),(#141994,#141995),(#141996,#141997),
(#141998,#141999),(#142000,#142001),(#142002,#142003),(#142004,#142005),
(#142006,#142007),(#142008,#142009),(#142010,#142011),(#142012,#142013),
(#142014,#142015),(#142016,#142017),(#142018,#142019),(#142020,#142021),
(#142022,#142023),(#142024,#142025),(#142026,#142027),(#142028,#142029),
(#142030,#142031),(#142032,#142033),(#142034,#142035),(#142036,#142037),
(#142038,#142039),(#142040,#142041),(#142042,#142043),(#142044,#142045),
(#142046,#142047),(#142048,#142049),(#142050,#142051),(#142052,#142053),
(#142054,#142055),(#142056,#142057),(#142058,#142059),(#142060,#142061),
(#142062,#142063),(#142064,#142065),(#142066,#142067),(#142068,#142069),
(#142070,#142071),(#142072,#142073),(#142074,#142075),(#142076,#142077),
(#142078,#142079),(#142080,#142081),(#142082,#142083),(#142084,#142085),
(#142086,#142087),(#142088,#142089),(#142090,#142091),(#142092,#142093),
(#142094,#142095),(#142096,#142097),(#142098,#142099),(#142100,#142101),
(#142102,#142103),(#142104,#142105),(#142106,#142107),(#142108,#142109),
(#142110,#142111),(#142112,#142113),(#142114,#142115),(#142116,#142117),
(#142118,#142119),(#142120,#142121),(#142122,#142123),(#142124,#142125),
(#142126,#142127),(#142128,#142129),(#142130,#142131),(#142132,#142133),
(#142134,#142135),(#142136,#142137),(#142138,#142139),(#142140,#142141),
(#142142,#142143),(#142144,#142145),(#142146,#142147),(#142148,#142149),
(#142150,#142151),(#142152,#142153),(#142154,#142155),(#142156,#142157),
(#142158,#142159),(#142160,#142161),(#142162,#142163),(#142164,#142165),
(#142166,#142167),(#142168,#142169),(#142170,#142171),(#142172,#142173),
(#142174,#142175),(#142176,#142177),(#142178,#142179),(#142180,#142181),
(#142182,#142183),(#142184,#142185),(#142186,#142187),(#142188,#142189),
(#142190,#142191),(#142192,#142193),(#142194,#142195),(#142196,#142197),
(#142198,#142199),(#142200,#142201),(#142202,#142203),(#142204,#142205),
(#142206,#142207),(#142208,#142209),(#142210,#142211),(#142212,#142213),
(#142214,#142215),(#142216,#142217),(#142218,#142219),(#142220,#142221),
(#142222,#142223),(#142224,#142225),(#142226,#142227),(#142228,#142229),
(#142230,#142231),(#142232,#142233)),.UNSPECIFIED.,.F.,.F.,.F.)
B_SPLINE_SURFACE_WITH_KNOTS((6,1,1,1,1,1,1,1,1,1,1,1,1,1,1,1,1,1,1,1,1,
1,1,1,1,1,1,1,1,1,1,1,1,1,1,1,1,1,1,1,1,1,1,1,1,1,1,1,1,1,1,1,1,1,1,1,1,
1,1,1,1,1,1,1,1,1,1,1,1,1,1,1,1,1,1,1,1,1,1,1,1,1,1,1,1,1,1,1,1,1,1,1,1,
1,1,1,1,1,1,1,1,1,1,1,1,1,1,1,1,1,1,1,1,1,1,1,1,1,1,1,1,1,1,1,1,1,1,1,1,
1,1,1,1,1,1,1,1,1,1,1,1,1,1,1,1,1,1,1,1,1,1,1,1,1,1,1,1,1,1,1,1,1,1,1,1,
1,1,1,1,1,1,1,1,1,1,1,1,1,1,1,1,1,1,1,1,1,1,1,1,1,1,1,1,1,1,1,1,1,1,1,6),
(2,2),(-1.,-0.995000000000001,-0.990000000000001,-0.985000000000001,-0.980000000000001,
-0.975000000000001,-0.970000000000001,-0.965000000000001,-0.960000000000001,
-0.955000000000001,-0.950000000000001,-0.945000000000001,-0.940000000000001,
-0.935000000000001,-0.930000000000001,-0.925000000000001,-0.920000000000001,
-0.915000000000001,-0.910000000000001,-0.905000000000001,-0.900000000000001,
-0.895000000000001,-0.890000000000001,-0.885000000000001,-0.880000000000001,
-0.875000000000001,-0.870000000000001,-0.865000000000001,-0.860000000000001,
-0.855000000000001,-0.850000000000001,-0.845000000000001,-0.840000000000001,
-0.835000000000001,-0.830000000000001,-0.825000000000001,-0.820000000000001,
-0.815000000000001,-0.810000000000001,-0.805000000000001,-0.800000000000001,
-0.795000000000001,-0.790000000000001,-0.785000000000001,-0.780000000000001,
-0.775000000000001,-0.770000000000001,-0.765000000000001,-0.760000000000001,
-0.755000000000001,-0.750000000000001,-0.745000000000001,-0.740000000000001,
-0.735000000000001,-0.730000000000001,-0.725000000000001,-0.720000000000001,
-0.715000000000001,-0.710000000000001,-0.705000000000001,-0.700000000000001,
-0.695000000000001,-0.690000000000001,-0.685,-0.68,-0.675,-0.67,-0.665,
-0.66,-0.655,-0.65,-0.645,-0.64,-0.635,-0.63,-0.625,-0.62,-0.615,-0.61,
-0.605,-0.6,-0.595,-0.59,-0.585,-0.58,-0.575,-0.57,-0.565,-0.56,-0.555,
-0.55,-0.545,-0.54,-0.535,-0.53,-0.525,-0.52,-0.515,-0.51,-0.505,-0.5,-0.495,
-0.49,-0.485,-0.48,-0.475,-0.47,-0.465,-0.46,-0.455,-0.45,-0.445,-0.44,
-0.435,-0.43,-0.425,-0.42,-0.415,-0.41,-0.405,-0.4,-0.395,-0.39,-0.385,
-0.38,-0.375,-0.37,-0.365,-0.36,-0.355,-0.35,-0.345,-0.34,-0.335,-0.33,
-0.325,-0.32,-0.315,-0.31,-0.305,-0.3,-0.295,-0.29,-0.285,-0.28,-0.275,
-0.27,-0.265,-0.26,-0.255,-0.25,-0.245,-0.24,-0.235,-0.23,-0.225,-0.22,
-0.215,-0.21,-0.205,-0.2,-0.195,-0.19,-0.185,-0.18,-0.175,-0.17,-0.165,
-0.16,-0.155,-0.15,-0.145,-0.14,-0.135,-0.13,-0.125,-0.12,-0.115,-0.11,
-0.105,-0.1,-0.095,-0.09,-0.085,-0.08,-0.075,-0.07,-0.065,-0.06,-0.055,
-0.05,-0.045,-0.04,-0.035,-0.03,-0.025,-0.02,-0.015,-0.01,-0.005,0.),(0.,
1.2),.UNSPECIFIED.)
GEOMETRIC_REPRESENTATION_ITEM()
RATIONAL_B_SPLINE_SURFACE(((1.,1.),(1.,1.),(1.,1.),(1.,1.),(1.,1.),(1.,
1.),(1.,1.),(1.,1.),(1.,1.),(1.,1.),(1.,1.),(1.,1.),(1.,1.),(1.,1.),(1.,
1.),(1.,1.),(1.,1.),(1.,1.),(1.,1.),(1.,1.),(1.,1.),(1.,1.),(1.,1.),(1.,
1.),(1.,1.),(1.,1.),(1.,1.),(1.,1.),(1.,1.),(1.,1.),(1.,1.),(1.,1.),(1.,
1.),(1.,1.),(1.,1.),(1.,1.),(1.,1.),(1.,1.),(1.,1.),(1.,1.),(1.,1.),(1.,
1.),(1.,1.),(1.,1.),(1.,1.),(1.,1.),(1.,1.),(1.,1.),(1.,1.),(1.,1.),(1.,
1.),(1.,1.),(1.,1.),(1.,1.),(1.,1.),(1.,1.),(1.,1.),(1.,1.),(1.,1.),(1.,
1.),(1.,1.),(1.,1.),(1.,1.),(1.,1.),(1.,1.),(1.,1.),(1.,1.),(1.,1.),(1.,
1.),(1.,1.),(1.,1.),(1.,1.),(1.,1.),(1.,1.),(1.,1.),(1.,1.),(1.,1.),(1.,
1.),(1.,1.),(1.,1.),(1.,1.),(1.,1.),(1.,1.),(1.,1.),(1.,1.),(1.,1.),(1.,
1.),(1.,1.),(1.,1.),(1.,1.),(1.,1.),(1.,1.),(1.,1.),(1.,1.),(1.,1.),(1.,
1.),(1.,1.),(1.,1.),(1.,1.),(1.,1.),(1.,1.),(1.,1.),(1.,1.),(1.,1.),(1.,
1.),(1.,1.),(1.,1.),(1.,1.),(1.,1.),(1.,1.),(1.,1.),(1.,1.),(1.,1.),(1.,
1.),(1.,1.),(1.,1.),(1.,1.),(1.,1.),(1.,1.),(1.,1.),(1.,1.),(1.,1.),(1.,
1.),(1.,1.),(1.,1.),(1.,1.),(1.,1.),(1.,1.),(1.,1.),(1.,1.),(1.,1.),(1.,
1.),(1.,1.),(1.,1.),(1.,1.),(1.,1.),(1.,1.),(1.,1.),(1.,1.),(1.,1.),(1.,
1.),(1.,1.),(1.,1.),(1.,1.),(1.,1.),(1.,1.),(1.,1.),(1.,1.),(1.,1.),(1.,
1.),(1.,1.),(1.,1.),(1.,1.),(1.,1.),(1.,1.),(1.,1.),(1.,1.),(1.,1.),(1.,
1.),(1.,1.),(1.,1.),(1.,1.),(1.,1.),(1.,1.),(1.,1.),(1.,1.),(1.,1.),(1.,
1.),(1.,1.),(1.,1.),(1.,1.),(1.,1.),(1.,1.),(1.,1.),(1.,1.),(1.,1.),(1.,
1.),(1.,1.),(1.,1.),(1.,1.),(1.,1.),(1.,1.),(1.,1.),(1.,1.),(1.,1.),(1.,
1.),(1.,1.),(1.,1.),(1.,1.),(1.,1.),(1.,1.),(1.,1.),(1.,1.),(1.,1.),(1.,
1.),(1.,1.),(1.,1.),(1.,1.),(1.,1.),(1.,1.),(1.,1.),(1.,1.),(1.,1.),(1.,
1.),(1.,1.)))
REPRESENTATION_ITEM('')
SURFACE()
);
#987=(
BOUNDED_SURFACE()
B_SPLINE_SURFACE(5,1,((#142625,#142626),(#142627,#142628),(#142629,#142630),
(#142631,#142632),(#142633,#142634),(#142635,#142636),(#142637,#142638),
(#142639,#142640),(#142641,#142642),(#142643,#142644),(#142645,#142646),
(#142647,#142648),(#142649,#142650),(#142651,#142652),(#142653,#142654),
(#142655,#142656),(#142657,#142658),(#142659,#142660),(#142661,#142662),
(#142663,#142664),(#142665,#142666),(#142667,#142668),(#142669,#142670),
(#142671,#142672),(#142673,#142674),(#142675,#142676),(#142677,#142678),
(#142679,#142680),(#142681,#142682),(#142683,#142684),(#142685,#142686),
(#142687,#142688),(#142689,#142690),(#142691,#142692),(#142693,#142694),
(#142695,#142696),(#142697,#142698),(#142699,#142700),(#142701,#142702),
(#142703,#142704),(#142705,#142706),(#142707,#142708),(#142709,#142710),
(#142711,#142712),(#142713,#142714),(#142715,#142716),(#142717,#142718),
(#142719,#142720),(#142721,#142722),(#142723,#142724),(#142725,#142726),
(#142727,#142728),(#142729,#142730),(#142731,#142732),(#142733,#142734),
(#142735,#142736),(#142737,#142738),(#142739,#142740),(#142741,#142742),
(#142743,#142744),(#142745,#142746),(#142747,#142748),(#142749,#142750),
(#142751,#142752),(#142753,#142754),(#142755,#142756),(#142757,#142758),
(#142759,#142760),(#142761,#142762),(#142763,#142764),(#142765,#142766),
(#142767,#142768),(#142769,#142770),(#142771,#142772),(#142773,#142774),
(#142775,#142776),(#142777,#142778),(#142779,#142780),(#142781,#142782),
(#142783,#142784),(#142785,#142786),(#142787,#142788),(#142789,#142790),
(#142791,#142792),(#142793,#142794),(#142795,#142796),(#142797,#142798),
(#142799,#142800),(#142801,#142802),(#142803,#142804),(#142805,#142806),
(#142807,#142808),(#142809,#142810),(#142811,#142812),(#142813,#142814),
(#142815,#142816),(#142817,#142818),(#142819,#142820),(#142821,#142822),
(#142823,#142824),(#142825,#142826),(#142827,#142828),(#142829,#142830),
(#142831,#142832),(#142833,#142834),(#142835,#142836),(#142837,#142838),
(#142839,#142840),(#142841,#142842),(#142843,#142844),(#142845,#142846),
(#142847,#142848),(#142849,#142850),(#142851,#142852),(#142853,#142854),
(#142855,#142856),(#142857,#142858),(#142859,#142860),(#142861,#142862),
(#142863,#142864),(#142865,#142866),(#142867,#142868),(#142869,#142870),
(#142871,#142872),(#142873,#142874),(#142875,#142876),(#142877,#142878),
(#142879,#142880),(#142881,#142882),(#142883,#142884),(#142885,#142886),
(#142887,#142888),(#142889,#142890),(#142891,#142892),(#142893,#142894),
(#142895,#142896),(#142897,#142898),(#142899,#142900),(#142901,#142902),
(#142903,#142904),(#142905,#142906),(#142907,#142908),(#142909,#142910),
(#142911,#142912),(#142913,#142914),(#142915,#142916),(#142917,#142918),
(#142919,#142920),(#142921,#142922),(#142923,#142924),(#142925,#142926),
(#142927,#142928),(#142929,#142930),(#142931,#142932),(#142933,#142934),
(#142935,#142936),(#142937,#142938),(#142939,#142940),(#142941,#142942),
(#142943,#142944),(#142945,#142946),(#142947,#142948),(#142949,#142950),
(#142951,#142952),(#142953,#142954),(#142955,#142956),(#142957,#142958),
(#142959,#142960),(#142961,#142962),(#142963,#142964),(#142965,#142966),
(#142967,#142968),(#142969,#142970),(#142971,#142972),(#142973,#142974),
(#142975,#142976),(#142977,#142978),(#142979,#142980),(#142981,#142982),
(#142983,#142984),(#142985,#142986),(#142987,#142988),(#142989,#142990),
(#142991,#142992),(#142993,#142994),(#142995,#142996),(#142997,#142998),
(#142999,#143000),(#143001,#143002),(#143003,#143004),(#143005,#143006),
(#143007,#143008),(#143009,#143010),(#143011,#143012),(#143013,#143014),
(#143015,#143016),(#143017,#143018),(#143019,#143020),(#143021,#143022),
(#143023,#143024),(#143025,#143026),(#143027,#143028),(#143029,#143030),
(#143031,#143032),(#143033,#143034)),.UNSPECIFIED.,.F.,.F.,.F.)
B_SPLINE_SURFACE_WITH_KNOTS((6,1,1,1,1,1,1,1,1,1,1,1,1,1,1,1,1,1,1,1,1,
1,1,1,1,1,1,1,1,1,1,1,1,1,1,1,1,1,1,1,1,1,1,1,1,1,1,1,1,1,1,1,1,1,1,1,1,
1,1,1,1,1,1,1,1,1,1,1,1,1,1,1,1,1,1,1,1,1,1,1,1,1,1,1,1,1,1,1,1,1,1,1,1,
1,1,1,1,1,1,1,1,1,1,1,1,1,1,1,1,1,1,1,1,1,1,1,1,1,1,1,1,1,1,1,1,1,1,1,1,
1,1,1,1,1,1,1,1,1,1,1,1,1,1,1,1,1,1,1,1,1,1,1,1,1,1,1,1,1,1,1,1,1,1,1,1,
1,1,1,1,1,1,1,1,1,1,1,1,1,1,1,1,1,1,1,1,1,1,1,1,1,1,1,1,1,1,1,1,1,1,1,6),
(2,2),(-1.,-0.995000000000001,-0.990000000000001,-0.985000000000001,-0.980000000000001,
-0.975000000000001,-0.970000000000001,-0.965000000000001,-0.960000000000001,
-0.955000000000001,-0.950000000000001,-0.945000000000001,-0.940000000000001,
-0.935000000000001,-0.930000000000001,-0.925000000000001,-0.920000000000001,
-0.915000000000001,-0.910000000000001,-0.905000000000001,-0.900000000000001,
-0.895000000000001,-0.890000000000001,-0.885000000000001,-0.880000000000001,
-0.875000000000001,-0.870000000000001,-0.865000000000001,-0.860000000000001,
-0.855000000000001,-0.850000000000001,-0.845000000000001,-0.840000000000001,
-0.835000000000001,-0.830000000000001,-0.825000000000001,-0.820000000000001,
-0.815000000000001,-0.810000000000001,-0.805000000000001,-0.800000000000001,
-0.795000000000001,-0.790000000000001,-0.785000000000001,-0.780000000000001,
-0.775000000000001,-0.770000000000001,-0.765000000000001,-0.760000000000001,
-0.755000000000001,-0.750000000000001,-0.745000000000001,-0.740000000000001,
-0.735000000000001,-0.730000000000001,-0.725000000000001,-0.720000000000001,
-0.715000000000001,-0.710000000000001,-0.705000000000001,-0.700000000000001,
-0.695000000000001,-0.690000000000001,-0.685,-0.68,-0.675,-0.67,-0.665,
-0.66,-0.655,-0.65,-0.645,-0.64,-0.635,-0.63,-0.625,-0.62,-0.615,-0.61,
-0.605,-0.6,-0.595,-0.59,-0.585,-0.58,-0.575,-0.57,-0.565,-0.56,-0.555,
-0.55,-0.545,-0.54,-0.535,-0.53,-0.525,-0.52,-0.515,-0.51,-0.505,-0.5,-0.495,
-0.49,-0.485,-0.48,-0.475,-0.47,-0.465,-0.46,-0.455,-0.45,-0.445,-0.44,
-0.435,-0.43,-0.425,-0.42,-0.415,-0.41,-0.405,-0.4,-0.395,-0.39,-0.385,
-0.38,-0.375,-0.37,-0.365,-0.36,-0.355,-0.35,-0.345,-0.34,-0.335,-0.33,
-0.325,-0.32,-0.315,-0.31,-0.305,-0.3,-0.295,-0.29,-0.285,-0.28,-0.275,
-0.27,-0.265,-0.26,-0.255,-0.25,-0.245,-0.24,-0.235,-0.23,-0.225,-0.22,
-0.215,-0.21,-0.205,-0.2,-0.195,-0.19,-0.185,-0.18,-0.175,-0.17,-0.165,
-0.16,-0.155,-0.15,-0.145,-0.14,-0.135,-0.13,-0.125,-0.12,-0.115,-0.11,
-0.105,-0.1,-0.095,-0.09,-0.085,-0.08,-0.075,-0.07,-0.065,-0.06,-0.055,
-0.05,-0.045,-0.04,-0.035,-0.03,-0.025,-0.02,-0.015,-0.01,-0.005,0.),(0.,
1.2),.UNSPECIFIED.)
GEOMETRIC_REPRESENTATION_ITEM()
RATIONAL_B_SPLINE_SURFACE(((1.,1.),(1.,1.),(1.,1.),(1.,1.),(1.,1.),(1.,
1.),(1.,1.),(1.,1.),(1.,1.),(1.,1.),(1.,1.),(1.,1.),(1.,1.),(1.,1.),(1.,
1.),(1.,1.),(1.,1.),(1.,1.),(1.,1.),(1.,1.),(1.,1.),(1.,1.),(1.,1.),(1.,
1.),(1.,1.),(1.,1.),(1.,1.),(1.,1.),(1.,1.),(1.,1.),(1.,1.),(1.,1.),(1.,
1.),(1.,1.),(1.,1.),(1.,1.),(1.,1.),(1.,1.),(1.,1.),(1.,1.),(1.,1.),(1.,
1.),(1.,1.),(1.,1.),(1.,1.),(1.,1.),(1.,1.),(1.,1.),(1.,1.),(1.,1.),(1.,
1.),(1.,1.),(1.,1.),(1.,1.),(1.,1.),(1.,1.),(1.,1.),(1.,1.),(1.,1.),(1.,
1.),(1.,1.),(1.,1.),(1.,1.),(1.,1.),(1.,1.),(1.,1.),(1.,1.),(1.,1.),(1.,
1.),(1.,1.),(1.,1.),(1.,1.),(1.,1.),(1.,1.),(1.,1.),(1.,1.),(1.,1.),(1.,
1.),(1.,1.),(1.,1.),(1.,1.),(1.,1.),(1.,1.),(1.,1.),(1.,1.),(1.,1.),(1.,
1.),(1.,1.),(1.,1.),(1.,1.),(1.,1.),(1.,1.),(1.,1.),(1.,1.),(1.,1.),(1.,
1.),(1.,1.),(1.,1.),(1.,1.),(1.,1.),(1.,1.),(1.,1.),(1.,1.),(1.,1.),(1.,
1.),(1.,1.),(1.,1.),(1.,1.),(1.,1.),(1.,1.),(1.,1.),(1.,1.),(1.,1.),(1.,
1.),(1.,1.),(1.,1.),(1.,1.),(1.,1.),(1.,1.),(1.,1.),(1.,1.),(1.,1.),(1.,
1.),(1.,1.),(1.,1.),(1.,1.),(1.,1.),(1.,1.),(1.,1.),(1.,1.),(1.,1.),(1.,
1.),(1.,1.),(1.,1.),(1.,1.),(1.,1.),(1.,1.),(1.,1.),(1.,1.),(1.,1.),(1.,
1.),(1.,1.),(1.,1.),(1.,1.),(1.,1.),(1.,1.),(1.,1.),(1.,1.),(1.,1.),(1.,
1.),(1.,1.),(1.,1.),(1.,1.),(1.,1.),(1.,1.),(1.,1.),(1.,1.),(1.,1.),(1.,
1.),(1.,1.),(1.,1.),(1.,1.),(1.,1.),(1.,1.),(1.,1.),(1.,1.),(1.,1.),(1.,
1.),(1.,1.),(1.,1.),(1.,1.),(1.,1.),(1.,1.),(1.,1.),(1.,1.),(1.,1.),(1.,
1.),(1.,1.),(1.,1.),(1.,1.),(1.,1.),(1.,1.),(1.,1.),(1.,1.),(1.,1.),(1.,
1.),(1.,1.),(1.,1.),(1.,1.),(1.,1.),(1.,1.),(1.,1.),(1.,1.),(1.,1.),(1.,
1.),(1.,1.),(1.,1.),(1.,1.),(1.,1.),(1.,1.),(1.,1.),(1.,1.),(1.,1.),(1.,
1.),(1.,1.)))
REPRESENTATION_ITEM('')
SURFACE()
);
#988=(
BOUNDED_SURFACE()
B_SPLINE_SURFACE(5,1,((#143426,#143427),(#143428,#143429),(#143430,#143431),
(#143432,#143433),(#143434,#143435),(#143436,#143437),(#143438,#143439),
(#143440,#143441),(#143442,#143443),(#143444,#143445),(#143446,#143447),
(#143448,#143449),(#143450,#143451),(#143452,#143453),(#143454,#143455),
(#143456,#143457),(#143458,#143459),(#143460,#143461),(#143462,#143463),
(#143464,#143465),(#143466,#143467),(#143468,#143469),(#143470,#143471),
(#143472,#143473),(#143474,#143475),(#143476,#143477),(#143478,#143479),
(#143480,#143481),(#143482,#143483),(#143484,#143485),(#143486,#143487),
(#143488,#143489),(#143490,#143491),(#143492,#143493),(#143494,#143495),
(#143496,#143497),(#143498,#143499),(#143500,#143501),(#143502,#143503),
(#143504,#143505),(#143506,#143507),(#143508,#143509),(#143510,#143511),
(#143512,#143513),(#143514,#143515),(#143516,#143517),(#143518,#143519),
(#143520,#143521),(#143522,#143523),(#143524,#143525),(#143526,#143527),
(#143528,#143529),(#143530,#143531),(#143532,#143533),(#143534,#143535),
(#143536,#143537),(#143538,#143539),(#143540,#143541),(#143542,#143543),
(#143544,#143545),(#143546,#143547),(#143548,#143549),(#143550,#143551),
(#143552,#143553),(#143554,#143555),(#143556,#143557),(#143558,#143559),
(#143560,#143561),(#143562,#143563),(#143564,#143565),(#143566,#143567),
(#143568,#143569),(#143570,#143571),(#143572,#143573),(#143574,#143575),
(#143576,#143577),(#143578,#143579),(#143580,#143581),(#143582,#143583),
(#143584,#143585),(#143586,#143587),(#143588,#143589),(#143590,#143591),
(#143592,#143593),(#143594,#143595),(#143596,#143597),(#143598,#143599),
(#143600,#143601),(#143602,#143603),(#143604,#143605),(#143606,#143607),
(#143608,#143609),(#143610,#143611),(#143612,#143613),(#143614,#143615),
(#143616,#143617),(#143618,#143619),(#143620,#143621),(#143622,#143623),
(#143624,#143625),(#143626,#143627),(#143628,#143629),(#143630,#143631),
(#143632,#143633),(#143634,#143635),(#143636,#143637),(#143638,#143639),
(#143640,#143641),(#143642,#143643),(#143644,#143645),(#143646,#143647),
(#143648,#143649),(#143650,#143651),(#143652,#143653),(#143654,#143655),
(#143656,#143657),(#143658,#143659),(#143660,#143661),(#143662,#143663),
(#143664,#143665),(#143666,#143667),(#143668,#143669),(#143670,#143671),
(#143672,#143673),(#143674,#143675),(#143676,#143677),(#143678,#143679),
(#143680,#143681),(#143682,#143683),(#143684,#143685),(#143686,#143687),
(#143688,#143689),(#143690,#143691),(#143692,#143693),(#143694,#143695),
(#143696,#143697),(#143698,#143699),(#143700,#143701),(#143702,#143703),
(#143704,#143705),(#143706,#143707),(#143708,#143709),(#143710,#143711),
(#143712,#143713),(#143714,#143715),(#143716,#143717),(#143718,#143719),
(#143720,#143721),(#143722,#143723),(#143724,#143725),(#143726,#143727),
(#143728,#143729),(#143730,#143731),(#143732,#143733),(#143734,#143735),
(#143736,#143737),(#143738,#143739),(#143740,#143741),(#143742,#143743),
(#143744,#143745),(#143746,#143747),(#143748,#143749),(#143750,#143751),
(#143752,#143753),(#143754,#143755),(#143756,#143757),(#143758,#143759),
(#143760,#143761),(#143762,#143763),(#143764,#143765),(#143766,#143767),
(#143768,#143769),(#143770,#143771),(#143772,#143773),(#143774,#143775),
(#143776,#143777),(#143778,#143779),(#143780,#143781),(#143782,#143783),
(#143784,#143785),(#143786,#143787),(#143788,#143789),(#143790,#143791),
(#143792,#143793),(#143794,#143795),(#143796,#143797),(#143798,#143799),
(#143800,#143801),(#143802,#143803),(#143804,#143805),(#143806,#143807),
(#143808,#143809),(#143810,#143811),(#143812,#143813),(#143814,#143815),
(#143816,#143817),(#143818,#143819),(#143820,#143821),(#143822,#143823),
(#143824,#143825),(#143826,#143827),(#143828,#143829),(#143830,#143831),
(#143832,#143833),(#143834,#143835)),.UNSPECIFIED.,.F.,.F.,.F.)
B_SPLINE_SURFACE_WITH_KNOTS((6,1,1,1,1,1,1,1,1,1,1,1,1,1,1,1,1,1,1,1,1,
1,1,1,1,1,1,1,1,1,1,1,1,1,1,1,1,1,1,1,1,1,1,1,1,1,1,1,1,1,1,1,1,1,1,1,1,
1,1,1,1,1,1,1,1,1,1,1,1,1,1,1,1,1,1,1,1,1,1,1,1,1,1,1,1,1,1,1,1,1,1,1,1,
1,1,1,1,1,1,1,1,1,1,1,1,1,1,1,1,1,1,1,1,1,1,1,1,1,1,1,1,1,1,1,1,1,1,1,1,
1,1,1,1,1,1,1,1,1,1,1,1,1,1,1,1,1,1,1,1,1,1,1,1,1,1,1,1,1,1,1,1,1,1,1,1,
1,1,1,1,1,1,1,1,1,1,1,1,1,1,1,1,1,1,1,1,1,1,1,1,1,1,1,1,1,1,1,1,1,1,1,6),
(2,2),(-1.,-0.995000000000001,-0.990000000000001,-0.985000000000001,-0.980000000000001,
-0.975000000000001,-0.970000000000001,-0.965000000000001,-0.960000000000001,
-0.955000000000001,-0.950000000000001,-0.945000000000001,-0.940000000000001,
-0.935000000000001,-0.930000000000001,-0.925000000000001,-0.920000000000001,
-0.915000000000001,-0.910000000000001,-0.905000000000001,-0.900000000000001,
-0.895000000000001,-0.890000000000001,-0.885000000000001,-0.880000000000001,
-0.875000000000001,-0.870000000000001,-0.865000000000001,-0.860000000000001,
-0.855000000000001,-0.850000000000001,-0.845000000000001,-0.840000000000001,
-0.835000000000001,-0.830000000000001,-0.825000000000001,-0.820000000000001,
-0.815000000000001,-0.810000000000001,-0.805000000000001,-0.800000000000001,
-0.795000000000001,-0.790000000000001,-0.785000000000001,-0.780000000000001,
-0.775000000000001,-0.770000000000001,-0.765000000000001,-0.760000000000001,
-0.755000000000001,-0.750000000000001,-0.745000000000001,-0.740000000000001,
-0.735000000000001,-0.730000000000001,-0.725000000000001,-0.720000000000001,
-0.715000000000001,-0.710000000000001,-0.705000000000001,-0.700000000000001,
-0.695000000000001,-0.690000000000001,-0.685,-0.68,-0.675,-0.67,-0.665,
-0.66,-0.655,-0.65,-0.645,-0.64,-0.635,-0.63,-0.625,-0.62,-0.615,-0.61,
-0.605,-0.6,-0.595,-0.59,-0.585,-0.58,-0.575,-0.57,-0.565,-0.56,-0.555,
-0.55,-0.545,-0.54,-0.535,-0.53,-0.525,-0.52,-0.515,-0.51,-0.505,-0.5,-0.495,
-0.49,-0.485,-0.48,-0.475,-0.47,-0.465,-0.46,-0.455,-0.45,-0.445,-0.44,
-0.435,-0.43,-0.425,-0.42,-0.415,-0.41,-0.405,-0.4,-0.395,-0.39,-0.385,
-0.38,-0.375,-0.37,-0.365,-0.36,-0.355,-0.35,-0.345,-0.34,-0.335,-0.33,
-0.325,-0.32,-0.315,-0.31,-0.305,-0.3,-0.295,-0.29,-0.285,-0.28,-0.275,
-0.27,-0.265,-0.26,-0.255,-0.25,-0.245,-0.24,-0.235,-0.23,-0.225,-0.22,
-0.215,-0.21,-0.205,-0.2,-0.195,-0.19,-0.185,-0.18,-0.175,-0.17,-0.165,
-0.16,-0.155,-0.15,-0.145,-0.14,-0.135,-0.13,-0.125,-0.12,-0.115,-0.11,
-0.105,-0.1,-0.095,-0.09,-0.085,-0.08,-0.075,-0.07,-0.065,-0.06,-0.055,
-0.05,-0.045,-0.04,-0.035,-0.03,-0.025,-0.02,-0.015,-0.01,-0.005,0.),(0.,
1.2),.UNSPECIFIED.)
GEOMETRIC_REPRESENTATION_ITEM()
RATIONAL_B_SPLINE_SURFACE(((1.,1.),(1.,1.),(1.,1.),(1.,1.),(1.,1.),(1.,
1.),(1.,1.),(1.,1.),(1.,1.),(1.,1.),(1.,1.),(1.,1.),(1.,1.),(1.,1.),(1.,
1.),(1.,1.),(1.,1.),(1.,1.),(1.,1.),(1.,1.),(1.,1.),(1.,1.),(1.,1.),(1.,
1.),(1.,1.),(1.,1.),(1.,1.),(1.,1.),(1.,1.),(1.,1.),(1.,1.),(1.,1.),(1.,
1.),(1.,1.),(1.,1.),(1.,1.),(1.,1.),(1.,1.),(1.,1.),(1.,1.),(1.,1.),(1.,
1.),(1.,1.),(1.,1.),(1.,1.),(1.,1.),(1.,1.),(1.,1.),(1.,1.),(1.,1.),(1.,
1.),(1.,1.),(1.,1.),(1.,1.),(1.,1.),(1.,1.),(1.,1.),(1.,1.),(1.,1.),(1.,
1.),(1.,1.),(1.,1.),(1.,1.),(1.,1.),(1.,1.),(1.,1.),(1.,1.),(1.,1.),(1.,
1.),(1.,1.),(1.,1.),(1.,1.),(1.,1.),(1.,1.),(1.,1.),(1.,1.),(1.,1.),(1.,
1.),(1.,1.),(1.,1.),(1.,1.),(1.,1.),(1.,1.),(1.,1.),(1.,1.),(1.,1.),(1.,
1.),(1.,1.),(1.,1.),(1.,1.),(1.,1.),(1.,1.),(1.,1.),(1.,1.),(1.,1.),(1.,
1.),(1.,1.),(1.,1.),(1.,1.),(1.,1.),(1.,1.),(1.,1.),(1.,1.),(1.,1.),(1.,
1.),(1.,1.),(1.,1.),(1.,1.),(1.,1.),(1.,1.),(1.,1.),(1.,1.),(1.,1.),(1.,
1.),(1.,1.),(1.,1.),(1.,1.),(1.,1.),(1.,1.),(1.,1.),(1.,1.),(1.,1.),(1.,
1.),(1.,1.),(1.,1.),(1.,1.),(1.,1.),(1.,1.),(1.,1.),(1.,1.),(1.,1.),(1.,
1.),(1.,1.),(1.,1.),(1.,1.),(1.,1.),(1.,1.),(1.,1.),(1.,1.),(1.,1.),(1.,
1.),(1.,1.),(1.,1.),(1.,1.),(1.,1.),(1.,1.),(1.,1.),(1.,1.),(1.,1.),(1.,
1.),(1.,1.),(1.,1.),(1.,1.),(1.,1.),(1.,1.),(1.,1.),(1.,1.),(1.,1.),(1.,
1.),(1.,1.),(1.,1.),(1.,1.),(1.,1.),(1.,1.),(1.,1.),(1.,1.),(1.,1.),(1.,
1.),(1.,1.),(1.,1.),(1.,1.),(1.,1.),(1.,1.),(1.,1.),(1.,1.),(1.,1.),(1.,
1.),(1.,1.),(1.,1.),(1.,1.),(1.,1.),(1.,1.),(1.,1.),(1.,1.),(1.,1.),(1.,
1.),(1.,1.),(1.,1.),(1.,1.),(1.,1.),(1.,1.),(1.,1.),(1.,1.),(1.,1.),(1.,
1.),(1.,1.),(1.,1.),(1.,1.),(1.,1.),(1.,1.),(1.,1.),(1.,1.),(1.,1.),(1.,
1.),(1.,1.)))
REPRESENTATION_ITEM('')
SURFACE()
);
#989=(
BOUNDED_SURFACE()
B_SPLINE_SURFACE(5,1,((#144227,#144228),(#144229,#144230),(#144231,#144232),
(#144233,#144234),(#144235,#144236),(#144237,#144238),(#144239,#144240),
(#144241,#144242),(#144243,#144244),(#144245,#144246),(#144247,#144248),
(#144249,#144250),(#144251,#144252),(#144253,#144254),(#144255,#144256),
(#144257,#144258),(#144259,#144260),(#144261,#144262),(#144263,#144264),
(#144265,#144266),(#144267,#144268),(#144269,#144270),(#144271,#144272),
(#144273,#144274),(#144275,#144276),(#144277,#144278),(#144279,#144280),
(#144281,#144282),(#144283,#144284),(#144285,#144286),(#144287,#144288),
(#144289,#144290),(#144291,#144292),(#144293,#144294),(#144295,#144296),
(#144297,#144298),(#144299,#144300),(#144301,#144302),(#144303,#144304),
(#144305,#144306),(#144307,#144308),(#144309,#144310),(#144311,#144312),
(#144313,#144314),(#144315,#144316),(#144317,#144318),(#144319,#144320),
(#144321,#144322),(#144323,#144324),(#144325,#144326),(#144327,#144328),
(#144329,#144330),(#144331,#144332),(#144333,#144334),(#144335,#144336),
(#144337,#144338),(#144339,#144340),(#144341,#144342),(#144343,#144344),
(#144345,#144346),(#144347,#144348),(#144349,#144350),(#144351,#144352),
(#144353,#144354),(#144355,#144356),(#144357,#144358),(#144359,#144360),
(#144361,#144362),(#144363,#144364),(#144365,#144366),(#144367,#144368),
(#144369,#144370),(#144371,#144372),(#144373,#144374),(#144375,#144376),
(#144377,#144378),(#144379,#144380),(#144381,#144382),(#144383,#144384),
(#144385,#144386),(#144387,#144388),(#144389,#144390),(#144391,#144392),
(#144393,#144394),(#144395,#144396),(#144397,#144398),(#144399,#144400),
(#144401,#144402),(#144403,#144404),(#144405,#144406),(#144407,#144408),
(#144409,#144410),(#144411,#144412),(#144413,#144414),(#144415,#144416),
(#144417,#144418),(#144419,#144420),(#144421,#144422),(#144423,#144424),
(#144425,#144426),(#144427,#144428),(#144429,#144430),(#144431,#144432),
(#144433,#144434),(#144435,#144436),(#144437,#144438),(#144439,#144440),
(#144441,#144442),(#144443,#144444),(#144445,#144446),(#144447,#144448),
(#144449,#144450),(#144451,#144452),(#144453,#144454),(#144455,#144456),
(#144457,#144458),(#144459,#144460),(#144461,#144462),(#144463,#144464),
(#144465,#144466),(#144467,#144468),(#144469,#144470),(#144471,#144472),
(#144473,#144474),(#144475,#144476),(#144477,#144478),(#144479,#144480),
(#144481,#144482),(#144483,#144484),(#144485,#144486),(#144487,#144488),
(#144489,#144490),(#144491,#144492),(#144493,#144494),(#144495,#144496),
(#144497,#144498),(#144499,#144500),(#144501,#144502),(#144503,#144504),
(#144505,#144506),(#144507,#144508),(#144509,#144510),(#144511,#144512),
(#144513,#144514),(#144515,#144516),(#144517,#144518),(#144519,#144520),
(#144521,#144522),(#144523,#144524),(#144525,#144526),(#144527,#144528),
(#144529,#144530),(#144531,#144532),(#144533,#144534),(#144535,#144536),
(#144537,#144538),(#144539,#144540),(#144541,#144542),(#144543,#144544),
(#144545,#144546),(#144547,#144548),(#144549,#144550),(#144551,#144552),
(#144553,#144554),(#144555,#144556),(#144557,#144558),(#144559,#144560),
(#144561,#144562),(#144563,#144564),(#144565,#144566),(#144567,#144568),
(#144569,#144570),(#144571,#144572),(#144573,#144574),(#144575,#144576),
(#144577,#144578),(#144579,#144580),(#144581,#144582),(#144583,#144584),
(#144585,#144586),(#144587,#144588),(#144589,#144590),(#144591,#144592),
(#144593,#144594),(#144595,#144596),(#144597,#144598),(#144599,#144600),
(#144601,#144602),(#144603,#144604),(#144605,#144606),(#144607,#144608),
(#144609,#144610),(#144611,#144612),(#144613,#144614),(#144615,#144616),
(#144617,#144618),(#144619,#144620),(#144621,#144622),(#144623,#144624),
(#144625,#144626),(#144627,#144628),(#144629,#144630),(#144631,#144632),
(#144633,#144634),(#144635,#144636)),.UNSPECIFIED.,.F.,.F.,.F.)
B_SPLINE_SURFACE_WITH_KNOTS((6,1,1,1,1,1,1,1,1,1,1,1,1,1,1,1,1,1,1,1,1,
1,1,1,1,1,1,1,1,1,1,1,1,1,1,1,1,1,1,1,1,1,1,1,1,1,1,1,1,1,1,1,1,1,1,1,1,
1,1,1,1,1,1,1,1,1,1,1,1,1,1,1,1,1,1,1,1,1,1,1,1,1,1,1,1,1,1,1,1,1,1,1,1,
1,1,1,1,1,1,1,1,1,1,1,1,1,1,1,1,1,1,1,1,1,1,1,1,1,1,1,1,1,1,1,1,1,1,1,1,
1,1,1,1,1,1,1,1,1,1,1,1,1,1,1,1,1,1,1,1,1,1,1,1,1,1,1,1,1,1,1,1,1,1,1,1,
1,1,1,1,1,1,1,1,1,1,1,1,1,1,1,1,1,1,1,1,1,1,1,1,1,1,1,1,1,1,1,1,1,1,1,6),
(2,2),(-1.,-0.995000000000001,-0.990000000000001,-0.985000000000001,-0.980000000000001,
-0.975000000000001,-0.970000000000001,-0.965000000000001,-0.960000000000001,
-0.955000000000001,-0.950000000000001,-0.945000000000001,-0.940000000000001,
-0.935000000000001,-0.930000000000001,-0.925000000000001,-0.920000000000001,
-0.915000000000001,-0.910000000000001,-0.905000000000001,-0.900000000000001,
-0.895000000000001,-0.890000000000001,-0.885000000000001,-0.880000000000001,
-0.875000000000001,-0.870000000000001,-0.865000000000001,-0.860000000000001,
-0.855000000000001,-0.850000000000001,-0.845000000000001,-0.840000000000001,
-0.835000000000001,-0.830000000000001,-0.825000000000001,-0.820000000000001,
-0.815000000000001,-0.810000000000001,-0.805000000000001,-0.800000000000001,
-0.795000000000001,-0.790000000000001,-0.785000000000001,-0.780000000000001,
-0.775000000000001,-0.770000000000001,-0.765000000000001,-0.760000000000001,
-0.755000000000001,-0.750000000000001,-0.745000000000001,-0.740000000000001,
-0.735000000000001,-0.730000000000001,-0.725000000000001,-0.720000000000001,
-0.715000000000001,-0.710000000000001,-0.705000000000001,-0.700000000000001,
-0.695000000000001,-0.690000000000001,-0.685,-0.68,-0.675,-0.67,-0.665,
-0.66,-0.655,-0.65,-0.645,-0.64,-0.635,-0.63,-0.625,-0.62,-0.615,-0.61,
-0.605,-0.6,-0.595,-0.59,-0.585,-0.58,-0.575,-0.57,-0.565,-0.56,-0.555,
-0.55,-0.545,-0.54,-0.535,-0.53,-0.525,-0.52,-0.515,-0.51,-0.505,-0.5,-0.495,
-0.49,-0.485,-0.48,-0.475,-0.47,-0.465,-0.46,-0.455,-0.45,-0.445,-0.44,
-0.435,-0.43,-0.425,-0.42,-0.415,-0.41,-0.405,-0.4,-0.395,-0.39,-0.385,
-0.38,-0.375,-0.37,-0.365,-0.36,-0.355,-0.35,-0.345,-0.34,-0.335,-0.33,
-0.325,-0.32,-0.315,-0.31,-0.305,-0.3,-0.295,-0.29,-0.285,-0.28,-0.275,
-0.27,-0.265,-0.26,-0.255,-0.25,-0.245,-0.24,-0.235,-0.23,-0.225,-0.22,
-0.215,-0.21,-0.205,-0.2,-0.195,-0.19,-0.185,-0.18,-0.175,-0.17,-0.165,
-0.16,-0.155,-0.15,-0.145,-0.14,-0.135,-0.13,-0.125,-0.12,-0.115,-0.11,
-0.105,-0.1,-0.095,-0.09,-0.085,-0.08,-0.075,-0.07,-0.065,-0.06,-0.055,
-0.05,-0.045,-0.04,-0.035,-0.03,-0.025,-0.02,-0.015,-0.01,-0.005,0.),(0.,
1.2),.UNSPECIFIED.)
GEOMETRIC_REPRESENTATION_ITEM()
RATIONAL_B_SPLINE_SURFACE(((1.,1.),(1.,1.),(1.,1.),(1.,1.),(1.,1.),(1.,
1.),(1.,1.),(1.,1.),(1.,1.),(1.,1.),(1.,1.),(1.,1.),(1.,1.),(1.,1.),(1.,
1.),(1.,1.),(1.,1.),(1.,1.),(1.,1.),(1.,1.),(1.,1.),(1.,1.),(1.,1.),(1.,
1.),(1.,1.),(1.,1.),(1.,1.),(1.,1.),(1.,1.),(1.,1.),(1.,1.),(1.,1.),(1.,
1.),(1.,1.),(1.,1.),(1.,1.),(1.,1.),(1.,1.),(1.,1.),(1.,1.),(1.,1.),(1.,
1.),(1.,1.),(1.,1.),(1.,1.),(1.,1.),(1.,1.),(1.,1.),(1.,1.),(1.,1.),(1.,
1.),(1.,1.),(1.,1.),(1.,1.),(1.,1.),(1.,1.),(1.,1.),(1.,1.),(1.,1.),(1.,
1.),(1.,1.),(1.,1.),(1.,1.),(1.,1.),(1.,1.),(1.,1.),(1.,1.),(1.,1.),(1.,
1.),(1.,1.),(1.,1.),(1.,1.),(1.,1.),(1.,1.),(1.,1.),(1.,1.),(1.,1.),(1.,
1.),(1.,1.),(1.,1.),(1.,1.),(1.,1.),(1.,1.),(1.,1.),(1.,1.),(1.,1.),(1.,
1.),(1.,1.),(1.,1.),(1.,1.),(1.,1.),(1.,1.),(1.,1.),(1.,1.),(1.,1.),(1.,
1.),(1.,1.),(1.,1.),(1.,1.),(1.,1.),(1.,1.),(1.,1.),(1.,1.),(1.,1.),(1.,
1.),(1.,1.),(1.,1.),(1.,1.),(1.,1.),(1.,1.),(1.,1.),(1.,1.),(1.,1.),(1.,
1.),(1.,1.),(1.,1.),(1.,1.),(1.,1.),(1.,1.),(1.,1.),(1.,1.),(1.,1.),(1.,
1.),(1.,1.),(1.,1.),(1.,1.),(1.,1.),(1.,1.),(1.,1.),(1.,1.),(1.,1.),(1.,
1.),(1.,1.),(1.,1.),(1.,1.),(1.,1.),(1.,1.),(1.,1.),(1.,1.),(1.,1.),(1.,
1.),(1.,1.),(1.,1.),(1.,1.),(1.,1.),(1.,1.),(1.,1.),(1.,1.),(1.,1.),(1.,
1.),(1.,1.),(1.,1.),(1.,1.),(1.,1.),(1.,1.),(1.,1.),(1.,1.),(1.,1.),(1.,
1.),(1.,1.),(1.,1.),(1.,1.),(1.,1.),(1.,1.),(1.,1.),(1.,1.),(1.,1.),(1.,
1.),(1.,1.),(1.,1.),(1.,1.),(1.,1.),(1.,1.),(1.,1.),(1.,1.),(1.,1.),(1.,
1.),(1.,1.),(1.,1.),(1.,1.),(1.,1.),(1.,1.),(1.,1.),(1.,1.),(1.,1.),(1.,
1.),(1.,1.),(1.,1.),(1.,1.),(1.,1.),(1.,1.),(1.,1.),(1.,1.),(1.,1.),(1.,
1.),(1.,1.),(1.,1.),(1.,1.),(1.,1.),(1.,1.),(1.,1.),(1.,1.),(1.,1.),(1.,
1.),(1.,1.)))
REPRESENTATION_ITEM('')
SURFACE()
);
#990=(
BOUNDED_SURFACE()
B_SPLINE_SURFACE(5,1,((#145028,#145029),(#145030,#145031),(#145032,#145033),
(#145034,#145035),(#145036,#145037),(#145038,#145039),(#145040,#145041),
(#145042,#145043),(#145044,#145045),(#145046,#145047),(#145048,#145049),
(#145050,#145051),(#145052,#145053),(#145054,#145055),(#145056,#145057),
(#145058,#145059),(#145060,#145061),(#145062,#145063),(#145064,#145065),
(#145066,#145067),(#145068,#145069),(#145070,#145071),(#145072,#145073),
(#145074,#145075),(#145076,#145077),(#145078,#145079),(#145080,#145081),
(#145082,#145083),(#145084,#145085),(#145086,#145087),(#145088,#145089),
(#145090,#145091),(#145092,#145093),(#145094,#145095),(#145096,#145097),
(#145098,#145099),(#145100,#145101),(#145102,#145103),(#145104,#145105),
(#145106,#145107),(#145108,#145109),(#145110,#145111),(#145112,#145113),
(#145114,#145115),(#145116,#145117),(#145118,#145119),(#145120,#145121),
(#145122,#145123),(#145124,#145125),(#145126,#145127),(#145128,#145129),
(#145130,#145131),(#145132,#145133),(#145134,#145135),(#145136,#145137),
(#145138,#145139),(#145140,#145141),(#145142,#145143),(#145144,#145145),
(#145146,#145147),(#145148,#145149),(#145150,#145151),(#145152,#145153),
(#145154,#145155),(#145156,#145157),(#145158,#145159),(#145160,#145161),
(#145162,#145163),(#145164,#145165),(#145166,#145167),(#145168,#145169),
(#145170,#145171),(#145172,#145173),(#145174,#145175),(#145176,#145177),
(#145178,#145179),(#145180,#145181),(#145182,#145183),(#145184,#145185),
(#145186,#145187),(#145188,#145189),(#145190,#145191),(#145192,#145193),
(#145194,#145195),(#145196,#145197),(#145198,#145199),(#145200,#145201),
(#145202,#145203),(#145204,#145205),(#145206,#145207),(#145208,#145209),
(#145210,#145211),(#145212,#145213),(#145214,#145215),(#145216,#145217),
(#145218,#145219),(#145220,#145221),(#145222,#145223),(#145224,#145225),
(#145226,#145227),(#145228,#145229),(#145230,#145231),(#145232,#145233),
(#145234,#145235),(#145236,#145237),(#145238,#145239),(#145240,#145241),
(#145242,#145243),(#145244,#145245),(#145246,#145247),(#145248,#145249),
(#145250,#145251),(#145252,#145253),(#145254,#145255),(#145256,#145257),
(#145258,#145259),(#145260,#145261),(#145262,#145263),(#145264,#145265),
(#145266,#145267),(#145268,#145269),(#145270,#145271),(#145272,#145273),
(#145274,#145275),(#145276,#145277),(#145278,#145279),(#145280,#145281),
(#145282,#145283),(#145284,#145285),(#145286,#145287),(#145288,#145289),
(#145290,#145291),(#145292,#145293),(#145294,#145295),(#145296,#145297),
(#145298,#145299),(#145300,#145301),(#145302,#145303),(#145304,#145305),
(#145306,#145307),(#145308,#145309),(#145310,#145311),(#145312,#145313),
(#145314,#145315),(#145316,#145317),(#145318,#145319),(#145320,#145321),
(#145322,#145323),(#145324,#145325),(#145326,#145327),(#145328,#145329),
(#145330,#145331),(#145332,#145333),(#145334,#145335),(#145336,#145337),
(#145338,#145339),(#145340,#145341),(#145342,#145343),(#145344,#145345),
(#145346,#145347),(#145348,#145349),(#145350,#145351),(#145352,#145353),
(#145354,#145355),(#145356,#145357),(#145358,#145359),(#145360,#145361),
(#145362,#145363),(#145364,#145365),(#145366,#145367),(#145368,#145369),
(#145370,#145371),(#145372,#145373),(#145374,#145375),(#145376,#145377),
(#145378,#145379),(#145380,#145381),(#145382,#145383),(#145384,#145385),
(#145386,#145387),(#145388,#145389),(#145390,#145391),(#145392,#145393),
(#145394,#145395),(#145396,#145397),(#145398,#145399),(#145400,#145401),
(#145402,#145403),(#145404,#145405),(#145406,#145407),(#145408,#145409),
(#145410,#145411),(#145412,#145413),(#145414,#145415),(#145416,#145417),
(#145418,#145419),(#145420,#145421),(#145422,#145423),(#145424,#145425),
(#145426,#145427),(#145428,#145429),(#145430,#145431),(#145432,#145433),
(#145434,#145435),(#145436,#145437)),.UNSPECIFIED.,.F.,.F.,.F.)
B_SPLINE_SURFACE_WITH_KNOTS((6,1,1,1,1,1,1,1,1,1,1,1,1,1,1,1,1,1,1,1,1,
1,1,1,1,1,1,1,1,1,1,1,1,1,1,1,1,1,1,1,1,1,1,1,1,1,1,1,1,1,1,1,1,1,1,1,1,
1,1,1,1,1,1,1,1,1,1,1,1,1,1,1,1,1,1,1,1,1,1,1,1,1,1,1,1,1,1,1,1,1,1,1,1,
1,1,1,1,1,1,1,1,1,1,1,1,1,1,1,1,1,1,1,1,1,1,1,1,1,1,1,1,1,1,1,1,1,1,1,1,
1,1,1,1,1,1,1,1,1,1,1,1,1,1,1,1,1,1,1,1,1,1,1,1,1,1,1,1,1,1,1,1,1,1,1,1,
1,1,1,1,1,1,1,1,1,1,1,1,1,1,1,1,1,1,1,1,1,1,1,1,1,1,1,1,1,1,1,1,1,1,1,6),
(2,2),(-1.,-0.995000000000001,-0.990000000000001,-0.985000000000001,-0.980000000000001,
-0.975000000000001,-0.970000000000001,-0.965000000000001,-0.960000000000001,
-0.955000000000001,-0.950000000000001,-0.945000000000001,-0.940000000000001,
-0.935000000000001,-0.930000000000001,-0.925000000000001,-0.920000000000001,
-0.915000000000001,-0.910000000000001,-0.905000000000001,-0.900000000000001,
-0.895000000000001,-0.890000000000001,-0.885000000000001,-0.880000000000001,
-0.875000000000001,-0.870000000000001,-0.865000000000001,-0.860000000000001,
-0.855000000000001,-0.850000000000001,-0.845000000000001,-0.840000000000001,
-0.835000000000001,-0.830000000000001,-0.825000000000001,-0.820000000000001,
-0.815000000000001,-0.810000000000001,-0.805000000000001,-0.800000000000001,
-0.795000000000001,-0.790000000000001,-0.785000000000001,-0.780000000000001,
-0.775000000000001,-0.770000000000001,-0.765000000000001,-0.760000000000001,
-0.755000000000001,-0.750000000000001,-0.745000000000001,-0.740000000000001,
-0.735000000000001,-0.730000000000001,-0.725000000000001,-0.720000000000001,
-0.715000000000001,-0.710000000000001,-0.705000000000001,-0.700000000000001,
-0.695000000000001,-0.690000000000001,-0.685,-0.68,-0.675,-0.67,-0.665,
-0.66,-0.655,-0.65,-0.645,-0.64,-0.635,-0.63,-0.625,-0.62,-0.615,-0.61,
-0.605,-0.6,-0.595,-0.59,-0.585,-0.58,-0.575,-0.57,-0.565,-0.56,-0.555,
-0.55,-0.545,-0.54,-0.535,-0.53,-0.525,-0.52,-0.515,-0.51,-0.505,-0.5,-0.495,
-0.49,-0.485,-0.48,-0.475,-0.47,-0.465,-0.46,-0.455,-0.45,-0.445,-0.44,
-0.435,-0.43,-0.425,-0.42,-0.415,-0.41,-0.405,-0.4,-0.395,-0.39,-0.385,
-0.38,-0.375,-0.37,-0.365,-0.36,-0.355,-0.35,-0.345,-0.34,-0.335,-0.33,
-0.325,-0.32,-0.315,-0.31,-0.305,-0.3,-0.295,-0.29,-0.285,-0.28,-0.275,
-0.27,-0.265,-0.26,-0.255,-0.25,-0.245,-0.24,-0.235,-0.23,-0.225,-0.22,
-0.215,-0.21,-0.205,-0.2,-0.195,-0.19,-0.185,-0.18,-0.175,-0.17,-0.165,
-0.16,-0.155,-0.15,-0.145,-0.14,-0.135,-0.13,-0.125,-0.12,-0.115,-0.11,
-0.105,-0.1,-0.095,-0.09,-0.085,-0.08,-0.075,-0.07,-0.065,-0.06,-0.055,
-0.05,-0.045,-0.04,-0.035,-0.03,-0.025,-0.02,-0.015,-0.01,-0.005,0.),(0.,
1.2),.UNSPECIFIED.)
GEOMETRIC_REPRESENTATION_ITEM()
RATIONAL_B_SPLINE_SURFACE(((1.,1.),(1.,1.),(1.,1.),(1.,1.),(1.,1.),(1.,
1.),(1.,1.),(1.,1.),(1.,1.),(1.,1.),(1.,1.),(1.,1.),(1.,1.),(1.,1.),(1.,
1.),(1.,1.),(1.,1.),(1.,1.),(1.,1.),(1.,1.),(1.,1.),(1.,1.),(1.,1.),(1.,
1.),(1.,1.),(1.,1.),(1.,1.),(1.,1.),(1.,1.),(1.,1.),(1.,1.),(1.,1.),(1.,
1.),(1.,1.),(1.,1.),(1.,1.),(1.,1.),(1.,1.),(1.,1.),(1.,1.),(1.,1.),(1.,
1.),(1.,1.),(1.,1.),(1.,1.),(1.,1.),(1.,1.),(1.,1.),(1.,1.),(1.,1.),(1.,
1.),(1.,1.),(1.,1.),(1.,1.),(1.,1.),(1.,1.),(1.,1.),(1.,1.),(1.,1.),(1.,
1.),(1.,1.),(1.,1.),(1.,1.),(1.,1.),(1.,1.),(1.,1.),(1.,1.),(1.,1.),(1.,
1.),(1.,1.),(1.,1.),(1.,1.),(1.,1.),(1.,1.),(1.,1.),(1.,1.),(1.,1.),(1.,
1.),(1.,1.),(1.,1.),(1.,1.),(1.,1.),(1.,1.),(1.,1.),(1.,1.),(1.,1.),(1.,
1.),(1.,1.),(1.,1.),(1.,1.),(1.,1.),(1.,1.),(1.,1.),(1.,1.),(1.,1.),(1.,
1.),(1.,1.),(1.,1.),(1.,1.),(1.,1.),(1.,1.),(1.,1.),(1.,1.),(1.,1.),(1.,
1.),(1.,1.),(1.,1.),(1.,1.),(1.,1.),(1.,1.),(1.,1.),(1.,1.),(1.,1.),(1.,
1.),(1.,1.),(1.,1.),(1.,1.),(1.,1.),(1.,1.),(1.,1.),(1.,1.),(1.,1.),(1.,
1.),(1.,1.),(1.,1.),(1.,1.),(1.,1.),(1.,1.),(1.,1.),(1.,1.),(1.,1.),(1.,
1.),(1.,1.),(1.,1.),(1.,1.),(1.,1.),(1.,1.),(1.,1.),(1.,1.),(1.,1.),(1.,
1.),(1.,1.),(1.,1.),(1.,1.),(1.,1.),(1.,1.),(1.,1.),(1.,1.),(1.,1.),(1.,
1.),(1.,1.),(1.,1.),(1.,1.),(1.,1.),(1.,1.),(1.,1.),(1.,1.),(1.,1.),(1.,
1.),(1.,1.),(1.,1.),(1.,1.),(1.,1.),(1.,1.),(1.,1.),(1.,1.),(1.,1.),(1.,
1.),(1.,1.),(1.,1.),(1.,1.),(1.,1.),(1.,1.),(1.,1.),(1.,1.),(1.,1.),(1.,
1.),(1.,1.),(1.,1.),(1.,1.),(1.,1.),(1.,1.),(1.,1.),(1.,1.),(1.,1.),(1.,
1.),(1.,1.),(1.,1.),(1.,1.),(1.,1.),(1.,1.),(1.,1.),(1.,1.),(1.,1.),(1.,
1.),(1.,1.),(1.,1.),(1.,1.),(1.,1.),(1.,1.),(1.,1.),(1.,1.),(1.,1.),(1.,
1.),(1.,1.)))
REPRESENTATION_ITEM('')
SURFACE()
);
#991=(
BOUNDED_SURFACE()
B_SPLINE_SURFACE(5,1,((#145829,#145830),(#145831,#145832),(#145833,#145834),
(#145835,#145836),(#145837,#145838),(#145839,#145840),(#145841,#145842),
(#145843,#145844),(#145845,#145846),(#145847,#145848),(#145849,#145850),
(#145851,#145852),(#145853,#145854),(#145855,#145856),(#145857,#145858),
(#145859,#145860),(#145861,#145862),(#145863,#145864),(#145865,#145866),
(#145867,#145868),(#145869,#145870),(#145871,#145872),(#145873,#145874),
(#145875,#145876),(#145877,#145878),(#145879,#145880),(#145881,#145882),
(#145883,#145884),(#145885,#145886),(#145887,#145888),(#145889,#145890),
(#145891,#145892),(#145893,#145894),(#145895,#145896),(#145897,#145898),
(#145899,#145900),(#145901,#145902),(#145903,#145904),(#145905,#145906),
(#145907,#145908),(#145909,#145910),(#145911,#145912),(#145913,#145914),
(#145915,#145916),(#145917,#145918),(#145919,#145920),(#145921,#145922),
(#145923,#145924),(#145925,#145926),(#145927,#145928),(#145929,#145930),
(#145931,#145932),(#145933,#145934),(#145935,#145936),(#145937,#145938),
(#145939,#145940),(#145941,#145942),(#145943,#145944),(#145945,#145946),
(#145947,#145948),(#145949,#145950),(#145951,#145952),(#145953,#145954),
(#145955,#145956),(#145957,#145958),(#145959,#145960),(#145961,#145962),
(#145963,#145964),(#145965,#145966),(#145967,#145968),(#145969,#145970),
(#145971,#145972),(#145973,#145974),(#145975,#145976),(#145977,#145978),
(#145979,#145980),(#145981,#145982),(#145983,#145984),(#145985,#145986),
(#145987,#145988),(#145989,#145990),(#145991,#145992),(#145993,#145994),
(#145995,#145996),(#145997,#145998),(#145999,#146000),(#146001,#146002),
(#146003,#146004),(#146005,#146006),(#146007,#146008),(#146009,#146010),
(#146011,#146012),(#146013,#146014),(#146015,#146016),(#146017,#146018),
(#146019,#146020),(#146021,#146022),(#146023,#146024),(#146025,#146026),
(#146027,#146028),(#146029,#146030),(#146031,#146032),(#146033,#146034),
(#146035,#146036),(#146037,#146038),(#146039,#146040),(#146041,#146042),
(#146043,#146044),(#146045,#146046),(#146047,#146048),(#146049,#146050),
(#146051,#146052),(#146053,#146054),(#146055,#146056),(#146057,#146058),
(#146059,#146060),(#146061,#146062),(#146063,#146064),(#146065,#146066),
(#146067,#146068),(#146069,#146070),(#146071,#146072),(#146073,#146074),
(#146075,#146076),(#146077,#146078),(#146079,#146080),(#146081,#146082),
(#146083,#146084),(#146085,#146086),(#146087,#146088),(#146089,#146090),
(#146091,#146092),(#146093,#146094),(#146095,#146096),(#146097,#146098),
(#146099,#146100),(#146101,#146102),(#146103,#146104),(#146105,#146106),
(#146107,#146108),(#146109,#146110),(#146111,#146112),(#146113,#146114),
(#146115,#146116),(#146117,#146118),(#146119,#146120),(#146121,#146122),
(#146123,#146124),(#146125,#146126),(#146127,#146128),(#146129,#146130),
(#146131,#146132),(#146133,#146134),(#146135,#146136),(#146137,#146138),
(#146139,#146140),(#146141,#146142),(#146143,#146144),(#146145,#146146),
(#146147,#146148),(#146149,#146150),(#146151,#146152),(#146153,#146154),
(#146155,#146156),(#146157,#146158),(#146159,#146160),(#146161,#146162),
(#146163,#146164),(#146165,#146166),(#146167,#146168),(#146169,#146170),
(#146171,#146172),(#146173,#146174),(#146175,#146176),(#146177,#146178),
(#146179,#146180),(#146181,#146182),(#146183,#146184),(#146185,#146186),
(#146187,#146188),(#146189,#146190),(#146191,#146192),(#146193,#146194),
(#146195,#146196),(#146197,#146198),(#146199,#146200),(#146201,#146202),
(#146203,#146204),(#146205,#146206),(#146207,#146208),(#146209,#146210),
(#146211,#146212),(#146213,#146214),(#146215,#146216),(#146217,#146218),
(#146219,#146220),(#146221,#146222),(#146223,#146224),(#146225,#146226),
(#146227,#146228),(#146229,#146230),(#146231,#146232),(#146233,#146234),
(#146235,#146236),(#146237,#146238)),.UNSPECIFIED.,.F.,.F.,.F.)
B_SPLINE_SURFACE_WITH_KNOTS((6,1,1,1,1,1,1,1,1,1,1,1,1,1,1,1,1,1,1,1,1,
1,1,1,1,1,1,1,1,1,1,1,1,1,1,1,1,1,1,1,1,1,1,1,1,1,1,1,1,1,1,1,1,1,1,1,1,
1,1,1,1,1,1,1,1,1,1,1,1,1,1,1,1,1,1,1,1,1,1,1,1,1,1,1,1,1,1,1,1,1,1,1,1,
1,1,1,1,1,1,1,1,1,1,1,1,1,1,1,1,1,1,1,1,1,1,1,1,1,1,1,1,1,1,1,1,1,1,1,1,
1,1,1,1,1,1,1,1,1,1,1,1,1,1,1,1,1,1,1,1,1,1,1,1,1,1,1,1,1,1,1,1,1,1,1,1,
1,1,1,1,1,1,1,1,1,1,1,1,1,1,1,1,1,1,1,1,1,1,1,1,1,1,1,1,1,1,1,1,1,1,1,6),
(2,2),(-1.,-0.995000000000001,-0.990000000000001,-0.985000000000001,-0.980000000000001,
-0.975000000000001,-0.970000000000001,-0.965000000000001,-0.960000000000001,
-0.955000000000001,-0.950000000000001,-0.945000000000001,-0.940000000000001,
-0.935000000000001,-0.930000000000001,-0.925000000000001,-0.920000000000001,
-0.915000000000001,-0.910000000000001,-0.905000000000001,-0.900000000000001,
-0.895000000000001,-0.890000000000001,-0.885000000000001,-0.880000000000001,
-0.875000000000001,-0.870000000000001,-0.865000000000001,-0.860000000000001,
-0.855000000000001,-0.850000000000001,-0.845000000000001,-0.840000000000001,
-0.835000000000001,-0.830000000000001,-0.825000000000001,-0.820000000000001,
-0.815000000000001,-0.810000000000001,-0.805000000000001,-0.800000000000001,
-0.795000000000001,-0.790000000000001,-0.785000000000001,-0.780000000000001,
-0.775000000000001,-0.770000000000001,-0.765000000000001,-0.760000000000001,
-0.755000000000001,-0.750000000000001,-0.745000000000001,-0.740000000000001,
-0.735000000000001,-0.730000000000001,-0.725000000000001,-0.720000000000001,
-0.715000000000001,-0.710000000000001,-0.705000000000001,-0.700000000000001,
-0.695000000000001,-0.690000000000001,-0.685,-0.68,-0.675,-0.67,-0.665,
-0.66,-0.655,-0.65,-0.645,-0.64,-0.635,-0.63,-0.625,-0.62,-0.615,-0.61,
-0.605,-0.6,-0.595,-0.59,-0.585,-0.58,-0.575,-0.57,-0.565,-0.56,-0.555,
-0.55,-0.545,-0.54,-0.535,-0.53,-0.525,-0.52,-0.515,-0.51,-0.505,-0.5,-0.495,
-0.49,-0.485,-0.48,-0.475,-0.47,-0.465,-0.46,-0.455,-0.45,-0.445,-0.44,
-0.435,-0.43,-0.425,-0.42,-0.415,-0.41,-0.405,-0.4,-0.395,-0.39,-0.385,
-0.38,-0.375,-0.37,-0.365,-0.36,-0.355,-0.35,-0.345,-0.34,-0.335,-0.33,
-0.325,-0.32,-0.315,-0.31,-0.305,-0.3,-0.295,-0.29,-0.285,-0.28,-0.275,
-0.27,-0.265,-0.26,-0.255,-0.25,-0.245,-0.24,-0.235,-0.23,-0.225,-0.22,
-0.215,-0.21,-0.205,-0.2,-0.195,-0.19,-0.185,-0.18,-0.175,-0.17,-0.165,
-0.16,-0.155,-0.15,-0.145,-0.14,-0.135,-0.13,-0.125,-0.12,-0.115,-0.11,
-0.105,-0.1,-0.095,-0.09,-0.085,-0.08,-0.075,-0.07,-0.065,-0.06,-0.055,
-0.05,-0.045,-0.04,-0.035,-0.03,-0.025,-0.02,-0.015,-0.01,-0.005,0.),(0.,
1.2),.UNSPECIFIED.)
GEOMETRIC_REPRESENTATION_ITEM()
RATIONAL_B_SPLINE_SURFACE(((1.,1.),(1.,1.),(1.,1.),(1.,1.),(1.,1.),(1.,
1.),(1.,1.),(1.,1.),(1.,1.),(1.,1.),(1.,1.),(1.,1.),(1.,1.),(1.,1.),(1.,
1.),(1.,1.),(1.,1.),(1.,1.),(1.,1.),(1.,1.),(1.,1.),(1.,1.),(1.,1.),(1.,
1.),(1.,1.),(1.,1.),(1.,1.),(1.,1.),(1.,1.),(1.,1.),(1.,1.),(1.,1.),(1.,
1.),(1.,1.),(1.,1.),(1.,1.),(1.,1.),(1.,1.),(1.,1.),(1.,1.),(1.,1.),(1.,
1.),(1.,1.),(1.,1.),(1.,1.),(1.,1.),(1.,1.),(1.,1.),(1.,1.),(1.,1.),(1.,
1.),(1.,1.),(1.,1.),(1.,1.),(1.,1.),(1.,1.),(1.,1.),(1.,1.),(1.,1.),(1.,
1.),(1.,1.),(1.,1.),(1.,1.),(1.,1.),(1.,1.),(1.,1.),(1.,1.),(1.,1.),(1.,
1.),(1.,1.),(1.,1.),(1.,1.),(1.,1.),(1.,1.),(1.,1.),(1.,1.),(1.,1.),(1.,
1.),(1.,1.),(1.,1.),(1.,1.),(1.,1.),(1.,1.),(1.,1.),(1.,1.),(1.,1.),(1.,
1.),(1.,1.),(1.,1.),(1.,1.),(1.,1.),(1.,1.),(1.,1.),(1.,1.),(1.,1.),(1.,
1.),(1.,1.),(1.,1.),(1.,1.),(1.,1.),(1.,1.),(1.,1.),(1.,1.),(1.,1.),(1.,
1.),(1.,1.),(1.,1.),(1.,1.),(1.,1.),(1.,1.),(1.,1.),(1.,1.),(1.,1.),(1.,
1.),(1.,1.),(1.,1.),(1.,1.),(1.,1.),(1.,1.),(1.,1.),(1.,1.),(1.,1.),(1.,
1.),(1.,1.),(1.,1.),(1.,1.),(1.,1.),(1.,1.),(1.,1.),(1.,1.),(1.,1.),(1.,
1.),(1.,1.),(1.,1.),(1.,1.),(1.,1.),(1.,1.),(1.,1.),(1.,1.),(1.,1.),(1.,
1.),(1.,1.),(1.,1.),(1.,1.),(1.,1.),(1.,1.),(1.,1.),(1.,1.),(1.,1.),(1.,
1.),(1.,1.),(1.,1.),(1.,1.),(1.,1.),(1.,1.),(1.,1.),(1.,1.),(1.,1.),(1.,
1.),(1.,1.),(1.,1.),(1.,1.),(1.,1.),(1.,1.),(1.,1.),(1.,1.),(1.,1.),(1.,
1.),(1.,1.),(1.,1.),(1.,1.),(1.,1.),(1.,1.),(1.,1.),(1.,1.),(1.,1.),(1.,
1.),(1.,1.),(1.,1.),(1.,1.),(1.,1.),(1.,1.),(1.,1.),(1.,1.),(1.,1.),(1.,
1.),(1.,1.),(1.,1.),(1.,1.),(1.,1.),(1.,1.),(1.,1.),(1.,1.),(1.,1.),(1.,
1.),(1.,1.),(1.,1.),(1.,1.),(1.,1.),(1.,1.),(1.,1.),(1.,1.),(1.,1.),(1.,
1.),(1.,1.)))
REPRESENTATION_ITEM('')
SURFACE()
);
#992=(
BOUNDED_SURFACE()
B_SPLINE_SURFACE(5,1,((#146630,#146631),(#146632,#146633),(#146634,#146635),
(#146636,#146637),(#146638,#146639),(#146640,#146641),(#146642,#146643),
(#146644,#146645),(#146646,#146647),(#146648,#146649),(#146650,#146651),
(#146652,#146653),(#146654,#146655),(#146656,#146657),(#146658,#146659),
(#146660,#146661),(#146662,#146663),(#146664,#146665),(#146666,#146667),
(#146668,#146669),(#146670,#146671),(#146672,#146673),(#146674,#146675),
(#146676,#146677),(#146678,#146679),(#146680,#146681),(#146682,#146683),
(#146684,#146685),(#146686,#146687),(#146688,#146689),(#146690,#146691),
(#146692,#146693),(#146694,#146695),(#146696,#146697),(#146698,#146699),
(#146700,#146701),(#146702,#146703),(#146704,#146705),(#146706,#146707),
(#146708,#146709),(#146710,#146711),(#146712,#146713),(#146714,#146715),
(#146716,#146717),(#146718,#146719),(#146720,#146721),(#146722,#146723),
(#146724,#146725),(#146726,#146727),(#146728,#146729),(#146730,#146731),
(#146732,#146733),(#146734,#146735),(#146736,#146737),(#146738,#146739),
(#146740,#146741),(#146742,#146743),(#146744,#146745),(#146746,#146747),
(#146748,#146749),(#146750,#146751),(#146752,#146753),(#146754,#146755),
(#146756,#146757),(#146758,#146759),(#146760,#146761),(#146762,#146763),
(#146764,#146765),(#146766,#146767),(#146768,#146769),(#146770,#146771),
(#146772,#146773),(#146774,#146775),(#146776,#146777),(#146778,#146779),
(#146780,#146781),(#146782,#146783),(#146784,#146785),(#146786,#146787),
(#146788,#146789),(#146790,#146791),(#146792,#146793),(#146794,#146795),
(#146796,#146797),(#146798,#146799),(#146800,#146801),(#146802,#146803),
(#146804,#146805),(#146806,#146807),(#146808,#146809),(#146810,#146811),
(#146812,#146813),(#146814,#146815),(#146816,#146817),(#146818,#146819),
(#146820,#146821),(#146822,#146823),(#146824,#146825),(#146826,#146827),
(#146828,#146829),(#146830,#146831),(#146832,#146833),(#146834,#146835),
(#146836,#146837),(#146838,#146839),(#146840,#146841),(#146842,#146843),
(#146844,#146845),(#146846,#146847),(#146848,#146849),(#146850,#146851),
(#146852,#146853),(#146854,#146855),(#146856,#146857),(#146858,#146859),
(#146860,#146861),(#146862,#146863),(#146864,#146865),(#146866,#146867),
(#146868,#146869),(#146870,#146871),(#146872,#146873),(#146874,#146875),
(#146876,#146877),(#146878,#146879),(#146880,#146881),(#146882,#146883),
(#146884,#146885),(#146886,#146887),(#146888,#146889),(#146890,#146891),
(#146892,#146893),(#146894,#146895),(#146896,#146897),(#146898,#146899),
(#146900,#146901),(#146902,#146903),(#146904,#146905),(#146906,#146907),
(#146908,#146909),(#146910,#146911),(#146912,#146913),(#146914,#146915),
(#146916,#146917),(#146918,#146919),(#146920,#146921),(#146922,#146923),
(#146924,#146925),(#146926,#146927),(#146928,#146929),(#146930,#146931),
(#146932,#146933),(#146934,#146935),(#146936,#146937),(#146938,#146939),
(#146940,#146941),(#146942,#146943),(#146944,#146945),(#146946,#146947),
(#146948,#146949),(#146950,#146951),(#146952,#146953),(#146954,#146955),
(#146956,#146957),(#146958,#146959),(#146960,#146961),(#146962,#146963),
(#146964,#146965),(#146966,#146967),(#146968,#146969),(#146970,#146971),
(#146972,#146973),(#146974,#146975),(#146976,#146977),(#146978,#146979),
(#146980,#146981),(#146982,#146983),(#146984,#146985),(#146986,#146987),
(#146988,#146989),(#146990,#146991),(#146992,#146993),(#146994,#146995),
(#146996,#146997),(#146998,#146999),(#147000,#147001),(#147002,#147003),
(#147004,#147005),(#147006,#147007),(#147008,#147009),(#147010,#147011),
(#147012,#147013),(#147014,#147015),(#147016,#147017),(#147018,#147019),
(#147020,#147021),(#147022,#147023),(#147024,#147025),(#147026,#147027),
(#147028,#147029),(#147030,#147031),(#147032,#147033),(#147034,#147035),
(#147036,#147037),(#147038,#147039)),.UNSPECIFIED.,.F.,.F.,.F.)
B_SPLINE_SURFACE_WITH_KNOTS((6,1,1,1,1,1,1,1,1,1,1,1,1,1,1,1,1,1,1,1,1,
1,1,1,1,1,1,1,1,1,1,1,1,1,1,1,1,1,1,1,1,1,1,1,1,1,1,1,1,1,1,1,1,1,1,1,1,
1,1,1,1,1,1,1,1,1,1,1,1,1,1,1,1,1,1,1,1,1,1,1,1,1,1,1,1,1,1,1,1,1,1,1,1,
1,1,1,1,1,1,1,1,1,1,1,1,1,1,1,1,1,1,1,1,1,1,1,1,1,1,1,1,1,1,1,1,1,1,1,1,
1,1,1,1,1,1,1,1,1,1,1,1,1,1,1,1,1,1,1,1,1,1,1,1,1,1,1,1,1,1,1,1,1,1,1,1,
1,1,1,1,1,1,1,1,1,1,1,1,1,1,1,1,1,1,1,1,1,1,1,1,1,1,1,1,1,1,1,1,1,1,1,6),
(2,2),(-1.,-0.995000000000001,-0.990000000000001,-0.985000000000001,-0.980000000000001,
-0.975000000000001,-0.970000000000001,-0.965000000000001,-0.960000000000001,
-0.955000000000001,-0.950000000000001,-0.945000000000001,-0.940000000000001,
-0.935000000000001,-0.930000000000001,-0.925000000000001,-0.920000000000001,
-0.915000000000001,-0.910000000000001,-0.905000000000001,-0.900000000000001,
-0.895000000000001,-0.890000000000001,-0.885000000000001,-0.880000000000001,
-0.875000000000001,-0.870000000000001,-0.865000000000001,-0.860000000000001,
-0.855000000000001,-0.850000000000001,-0.845000000000001,-0.840000000000001,
-0.835000000000001,-0.830000000000001,-0.825000000000001,-0.820000000000001,
-0.815000000000001,-0.810000000000001,-0.805000000000001,-0.800000000000001,
-0.795000000000001,-0.790000000000001,-0.785000000000001,-0.780000000000001,
-0.775000000000001,-0.770000000000001,-0.765000000000001,-0.760000000000001,
-0.755000000000001,-0.750000000000001,-0.745000000000001,-0.740000000000001,
-0.735000000000001,-0.730000000000001,-0.725000000000001,-0.720000000000001,
-0.715000000000001,-0.710000000000001,-0.705000000000001,-0.700000000000001,
-0.695000000000001,-0.690000000000001,-0.685,-0.68,-0.675,-0.67,-0.665,
-0.66,-0.655,-0.65,-0.645,-0.64,-0.635,-0.63,-0.625,-0.62,-0.615,-0.61,
-0.605,-0.6,-0.595,-0.59,-0.585,-0.58,-0.575,-0.57,-0.565,-0.56,-0.555,
-0.55,-0.545,-0.54,-0.535,-0.53,-0.525,-0.52,-0.515,-0.51,-0.505,-0.5,-0.495,
-0.49,-0.485,-0.48,-0.475,-0.47,-0.465,-0.46,-0.455,-0.45,-0.445,-0.44,
-0.435,-0.43,-0.425,-0.42,-0.415,-0.41,-0.405,-0.4,-0.395,-0.39,-0.385,
-0.38,-0.375,-0.37,-0.365,-0.36,-0.355,-0.35,-0.345,-0.34,-0.335,-0.33,
-0.325,-0.32,-0.315,-0.31,-0.305,-0.3,-0.295,-0.29,-0.285,-0.28,-0.275,
-0.27,-0.265,-0.26,-0.255,-0.25,-0.245,-0.24,-0.235,-0.23,-0.225,-0.22,
-0.215,-0.21,-0.205,-0.2,-0.195,-0.19,-0.185,-0.18,-0.175,-0.17,-0.165,
-0.16,-0.155,-0.15,-0.145,-0.14,-0.135,-0.13,-0.125,-0.12,-0.115,-0.11,
-0.105,-0.1,-0.095,-0.09,-0.085,-0.08,-0.075,-0.07,-0.065,-0.06,-0.055,
-0.05,-0.045,-0.04,-0.035,-0.03,-0.025,-0.02,-0.015,-0.01,-0.005,0.),(0.,
1.2),.UNSPECIFIED.)
GEOMETRIC_REPRESENTATION_ITEM()
RATIONAL_B_SPLINE_SURFACE(((1.,1.),(1.,1.),(1.,1.),(1.,1.),(1.,1.),(1.,
1.),(1.,1.),(1.,1.),(1.,1.),(1.,1.),(1.,1.),(1.,1.),(1.,1.),(1.,1.),(1.,
1.),(1.,1.),(1.,1.),(1.,1.),(1.,1.),(1.,1.),(1.,1.),(1.,1.),(1.,1.),(1.,
1.),(1.,1.),(1.,1.),(1.,1.),(1.,1.),(1.,1.),(1.,1.),(1.,1.),(1.,1.),(1.,
1.),(1.,1.),(1.,1.),(1.,1.),(1.,1.),(1.,1.),(1.,1.),(1.,1.),(1.,1.),(1.,
1.),(1.,1.),(1.,1.),(1.,1.),(1.,1.),(1.,1.),(1.,1.),(1.,1.),(1.,1.),(1.,
1.),(1.,1.),(1.,1.),(1.,1.),(1.,1.),(1.,1.),(1.,1.),(1.,1.),(1.,1.),(1.,
1.),(1.,1.),(1.,1.),(1.,1.),(1.,1.),(1.,1.),(1.,1.),(1.,1.),(1.,1.),(1.,
1.),(1.,1.),(1.,1.),(1.,1.),(1.,1.),(1.,1.),(1.,1.),(1.,1.),(1.,1.),(1.,
1.),(1.,1.),(1.,1.),(1.,1.),(1.,1.),(1.,1.),(1.,1.),(1.,1.),(1.,1.),(1.,
1.),(1.,1.),(1.,1.),(1.,1.),(1.,1.),(1.,1.),(1.,1.),(1.,1.),(1.,1.),(1.,
1.),(1.,1.),(1.,1.),(1.,1.),(1.,1.),(1.,1.),(1.,1.),(1.,1.),(1.,1.),(1.,
1.),(1.,1.),(1.,1.),(1.,1.),(1.,1.),(1.,1.),(1.,1.),(1.,1.),(1.,1.),(1.,
1.),(1.,1.),(1.,1.),(1.,1.),(1.,1.),(1.,1.),(1.,1.),(1.,1.),(1.,1.),(1.,
1.),(1.,1.),(1.,1.),(1.,1.),(1.,1.),(1.,1.),(1.,1.),(1.,1.),(1.,1.),(1.,
1.),(1.,1.),(1.,1.),(1.,1.),(1.,1.),(1.,1.),(1.,1.),(1.,1.),(1.,1.),(1.,
1.),(1.,1.),(1.,1.),(1.,1.),(1.,1.),(1.,1.),(1.,1.),(1.,1.),(1.,1.),(1.,
1.),(1.,1.),(1.,1.),(1.,1.),(1.,1.),(1.,1.),(1.,1.),(1.,1.),(1.,1.),(1.,
1.),(1.,1.),(1.,1.),(1.,1.),(1.,1.),(1.,1.),(1.,1.),(1.,1.),(1.,1.),(1.,
1.),(1.,1.),(1.,1.),(1.,1.),(1.,1.),(1.,1.),(1.,1.),(1.,1.),(1.,1.),(1.,
1.),(1.,1.),(1.,1.),(1.,1.),(1.,1.),(1.,1.),(1.,1.),(1.,1.),(1.,1.),(1.,
1.),(1.,1.),(1.,1.),(1.,1.),(1.,1.),(1.,1.),(1.,1.),(1.,1.),(1.,1.),(1.,
1.),(1.,1.),(1.,1.),(1.,1.),(1.,1.),(1.,1.),(1.,1.),(1.,1.),(1.,1.),(1.,
1.),(1.,1.)))
REPRESENTATION_ITEM('')
SURFACE()
);
#993=(
BOUNDED_SURFACE()
B_SPLINE_SURFACE(5,1,((#147431,#147432),(#147433,#147434),(#147435,#147436),
(#147437,#147438),(#147439,#147440),(#147441,#147442),(#147443,#147444),
(#147445,#147446),(#147447,#147448),(#147449,#147450),(#147451,#147452),
(#147453,#147454),(#147455,#147456),(#147457,#147458),(#147459,#147460),
(#147461,#147462),(#147463,#147464),(#147465,#147466),(#147467,#147468),
(#147469,#147470),(#147471,#147472),(#147473,#147474),(#147475,#147476),
(#147477,#147478),(#147479,#147480),(#147481,#147482),(#147483,#147484),
(#147485,#147486),(#147487,#147488),(#147489,#147490),(#147491,#147492),
(#147493,#147494),(#147495,#147496),(#147497,#147498),(#147499,#147500),
(#147501,#147502),(#147503,#147504),(#147505,#147506),(#147507,#147508),
(#147509,#147510),(#147511,#147512),(#147513,#147514),(#147515,#147516),
(#147517,#147518),(#147519,#147520),(#147521,#147522),(#147523,#147524),
(#147525,#147526),(#147527,#147528),(#147529,#147530),(#147531,#147532),
(#147533,#147534),(#147535,#147536),(#147537,#147538),(#147539,#147540),
(#147541,#147542),(#147543,#147544),(#147545,#147546),(#147547,#147548),
(#147549,#147550),(#147551,#147552),(#147553,#147554),(#147555,#147556),
(#147557,#147558),(#147559,#147560),(#147561,#147562),(#147563,#147564),
(#147565,#147566),(#147567,#147568),(#147569,#147570),(#147571,#147572),
(#147573,#147574),(#147575,#147576),(#147577,#147578),(#147579,#147580),
(#147581,#147582),(#147583,#147584),(#147585,#147586),(#147587,#147588),
(#147589,#147590),(#147591,#147592),(#147593,#147594),(#147595,#147596),
(#147597,#147598),(#147599,#147600),(#147601,#147602),(#147603,#147604),
(#147605,#147606),(#147607,#147608),(#147609,#147610),(#147611,#147612),
(#147613,#147614),(#147615,#147616),(#147617,#147618),(#147619,#147620),
(#147621,#147622),(#147623,#147624),(#147625,#147626),(#147627,#147628),
(#147629,#147630),(#147631,#147632),(#147633,#147634),(#147635,#147636),
(#147637,#147638),(#147639,#147640),(#147641,#147642),(#147643,#147644),
(#147645,#147646),(#147647,#147648),(#147649,#147650),(#147651,#147652),
(#147653,#147654),(#147655,#147656),(#147657,#147658),(#147659,#147660),
(#147661,#147662),(#147663,#147664),(#147665,#147666),(#147667,#147668),
(#147669,#147670),(#147671,#147672),(#147673,#147674),(#147675,#147676),
(#147677,#147678),(#147679,#147680),(#147681,#147682),(#147683,#147684),
(#147685,#147686),(#147687,#147688),(#147689,#147690),(#147691,#147692),
(#147693,#147694),(#147695,#147696),(#147697,#147698),(#147699,#147700),
(#147701,#147702),(#147703,#147704),(#147705,#147706),(#147707,#147708),
(#147709,#147710),(#147711,#147712),(#147713,#147714),(#147715,#147716),
(#147717,#147718),(#147719,#147720),(#147721,#147722),(#147723,#147724),
(#147725,#147726),(#147727,#147728),(#147729,#147730),(#147731,#147732),
(#147733,#147734),(#147735,#147736),(#147737,#147738),(#147739,#147740),
(#147741,#147742),(#147743,#147744),(#147745,#147746),(#147747,#147748),
(#147749,#147750),(#147751,#147752),(#147753,#147754),(#147755,#147756),
(#147757,#147758),(#147759,#147760),(#147761,#147762),(#147763,#147764),
(#147765,#147766),(#147767,#147768),(#147769,#147770),(#147771,#147772),
(#147773,#147774),(#147775,#147776),(#147777,#147778),(#147779,#147780),
(#147781,#147782),(#147783,#147784),(#147785,#147786),(#147787,#147788),
(#147789,#147790),(#147791,#147792),(#147793,#147794),(#147795,#147796),
(#147797,#147798),(#147799,#147800),(#147801,#147802),(#147803,#147804),
(#147805,#147806),(#147807,#147808),(#147809,#147810),(#147811,#147812),
(#147813,#147814),(#147815,#147816),(#147817,#147818),(#147819,#147820),
(#147821,#147822),(#147823,#147824),(#147825,#147826),(#147827,#147828),
(#147829,#147830),(#147831,#147832),(#147833,#147834),(#147835,#147836),
(#147837,#147838),(#147839,#147840)),.UNSPECIFIED.,.F.,.F.,.F.)
B_SPLINE_SURFACE_WITH_KNOTS((6,1,1,1,1,1,1,1,1,1,1,1,1,1,1,1,1,1,1,1,1,
1,1,1,1,1,1,1,1,1,1,1,1,1,1,1,1,1,1,1,1,1,1,1,1,1,1,1,1,1,1,1,1,1,1,1,1,
1,1,1,1,1,1,1,1,1,1,1,1,1,1,1,1,1,1,1,1,1,1,1,1,1,1,1,1,1,1,1,1,1,1,1,1,
1,1,1,1,1,1,1,1,1,1,1,1,1,1,1,1,1,1,1,1,1,1,1,1,1,1,1,1,1,1,1,1,1,1,1,1,
1,1,1,1,1,1,1,1,1,1,1,1,1,1,1,1,1,1,1,1,1,1,1,1,1,1,1,1,1,1,1,1,1,1,1,1,
1,1,1,1,1,1,1,1,1,1,1,1,1,1,1,1,1,1,1,1,1,1,1,1,1,1,1,1,1,1,1,1,1,1,1,6),
(2,2),(-1.,-0.995000000000001,-0.990000000000001,-0.985000000000001,-0.980000000000001,
-0.975000000000001,-0.970000000000001,-0.965000000000001,-0.960000000000001,
-0.955000000000001,-0.950000000000001,-0.945000000000001,-0.940000000000001,
-0.935000000000001,-0.930000000000001,-0.925000000000001,-0.920000000000001,
-0.915000000000001,-0.910000000000001,-0.905000000000001,-0.900000000000001,
-0.895000000000001,-0.890000000000001,-0.885000000000001,-0.880000000000001,
-0.875000000000001,-0.870000000000001,-0.865000000000001,-0.860000000000001,
-0.855000000000001,-0.850000000000001,-0.845000000000001,-0.840000000000001,
-0.835000000000001,-0.830000000000001,-0.825000000000001,-0.820000000000001,
-0.815000000000001,-0.810000000000001,-0.805000000000001,-0.800000000000001,
-0.795000000000001,-0.790000000000001,-0.785000000000001,-0.780000000000001,
-0.775000000000001,-0.770000000000001,-0.765000000000001,-0.760000000000001,
-0.755000000000001,-0.750000000000001,-0.745000000000001,-0.740000000000001,
-0.735000000000001,-0.730000000000001,-0.725000000000001,-0.720000000000001,
-0.715000000000001,-0.710000000000001,-0.705000000000001,-0.700000000000001,
-0.695000000000001,-0.690000000000001,-0.685,-0.68,-0.675,-0.67,-0.665,
-0.66,-0.655,-0.65,-0.645,-0.64,-0.635,-0.63,-0.625,-0.62,-0.615,-0.61,
-0.605,-0.6,-0.595,-0.59,-0.585,-0.58,-0.575,-0.57,-0.565,-0.56,-0.555,
-0.55,-0.545,-0.54,-0.535,-0.53,-0.525,-0.52,-0.515,-0.51,-0.505,-0.5,-0.495,
-0.49,-0.485,-0.48,-0.475,-0.47,-0.465,-0.46,-0.455,-0.45,-0.445,-0.44,
-0.435,-0.43,-0.425,-0.42,-0.415,-0.41,-0.405,-0.4,-0.395,-0.39,-0.385,
-0.38,-0.375,-0.37,-0.365,-0.36,-0.355,-0.35,-0.345,-0.34,-0.335,-0.33,
-0.325,-0.32,-0.315,-0.31,-0.305,-0.3,-0.295,-0.29,-0.285,-0.28,-0.275,
-0.27,-0.265,-0.26,-0.255,-0.25,-0.245,-0.24,-0.235,-0.23,-0.225,-0.22,
-0.215,-0.21,-0.205,-0.2,-0.195,-0.19,-0.185,-0.18,-0.175,-0.17,-0.165,
-0.16,-0.155,-0.15,-0.145,-0.14,-0.135,-0.13,-0.125,-0.12,-0.115,-0.11,
-0.105,-0.1,-0.095,-0.09,-0.085,-0.08,-0.075,-0.07,-0.065,-0.06,-0.055,
-0.05,-0.045,-0.04,-0.035,-0.03,-0.025,-0.02,-0.015,-0.01,-0.005,0.),(0.,
1.2),.UNSPECIFIED.)
GEOMETRIC_REPRESENTATION_ITEM()
RATIONAL_B_SPLINE_SURFACE(((1.,1.),(1.,1.),(1.,1.),(1.,1.),(1.,1.),(1.,
1.),(1.,1.),(1.,1.),(1.,1.),(1.,1.),(1.,1.),(1.,1.),(1.,1.),(1.,1.),(1.,
1.),(1.,1.),(1.,1.),(1.,1.),(1.,1.),(1.,1.),(1.,1.),(1.,1.),(1.,1.),(1.,
1.),(1.,1.),(1.,1.),(1.,1.),(1.,1.),(1.,1.),(1.,1.),(1.,1.),(1.,1.),(1.,
1.),(1.,1.),(1.,1.),(1.,1.),(1.,1.),(1.,1.),(1.,1.),(1.,1.),(1.,1.),(1.,
1.),(1.,1.),(1.,1.),(1.,1.),(1.,1.),(1.,1.),(1.,1.),(1.,1.),(1.,1.),(1.,
1.),(1.,1.),(1.,1.),(1.,1.),(1.,1.),(1.,1.),(1.,1.),(1.,1.),(1.,1.),(1.,
1.),(1.,1.),(1.,1.),(1.,1.),(1.,1.),(1.,1.),(1.,1.),(1.,1.),(1.,1.),(1.,
1.),(1.,1.),(1.,1.),(1.,1.),(1.,1.),(1.,1.),(1.,1.),(1.,1.),(1.,1.),(1.,
1.),(1.,1.),(1.,1.),(1.,1.),(1.,1.),(1.,1.),(1.,1.),(1.,1.),(1.,1.),(1.,
1.),(1.,1.),(1.,1.),(1.,1.),(1.,1.),(1.,1.),(1.,1.),(1.,1.),(1.,1.),(1.,
1.),(1.,1.),(1.,1.),(1.,1.),(1.,1.),(1.,1.),(1.,1.),(1.,1.),(1.,1.),(1.,
1.),(1.,1.),(1.,1.),(1.,1.),(1.,1.),(1.,1.),(1.,1.),(1.,1.),(1.,1.),(1.,
1.),(1.,1.),(1.,1.),(1.,1.),(1.,1.),(1.,1.),(1.,1.),(1.,1.),(1.,1.),(1.,
1.),(1.,1.),(1.,1.),(1.,1.),(1.,1.),(1.,1.),(1.,1.),(1.,1.),(1.,1.),(1.,
1.),(1.,1.),(1.,1.),(1.,1.),(1.,1.),(1.,1.),(1.,1.),(1.,1.),(1.,1.),(1.,
1.),(1.,1.),(1.,1.),(1.,1.),(1.,1.),(1.,1.),(1.,1.),(1.,1.),(1.,1.),(1.,
1.),(1.,1.),(1.,1.),(1.,1.),(1.,1.),(1.,1.),(1.,1.),(1.,1.),(1.,1.),(1.,
1.),(1.,1.),(1.,1.),(1.,1.),(1.,1.),(1.,1.),(1.,1.),(1.,1.),(1.,1.),(1.,
1.),(1.,1.),(1.,1.),(1.,1.),(1.,1.),(1.,1.),(1.,1.),(1.,1.),(1.,1.),(1.,
1.),(1.,1.),(1.,1.),(1.,1.),(1.,1.),(1.,1.),(1.,1.),(1.,1.),(1.,1.),(1.,
1.),(1.,1.),(1.,1.),(1.,1.),(1.,1.),(1.,1.),(1.,1.),(1.,1.),(1.,1.),(1.,
1.),(1.,1.),(1.,1.),(1.,1.),(1.,1.),(1.,1.),(1.,1.),(1.,1.),(1.,1.),(1.,
1.),(1.,1.)))
REPRESENTATION_ITEM('')
SURFACE()
);
#994=(
BOUNDED_SURFACE()
B_SPLINE_SURFACE(5,1,((#148232,#148233),(#148234,#148235),(#148236,#148237),
(#148238,#148239),(#148240,#148241),(#148242,#148243),(#148244,#148245),
(#148246,#148247),(#148248,#148249),(#148250,#148251),(#148252,#148253),
(#148254,#148255),(#148256,#148257),(#148258,#148259),(#148260,#148261),
(#148262,#148263),(#148264,#148265),(#148266,#148267),(#148268,#148269),
(#148270,#148271),(#148272,#148273),(#148274,#148275),(#148276,#148277),
(#148278,#148279),(#148280,#148281),(#148282,#148283),(#148284,#148285),
(#148286,#148287),(#148288,#148289),(#148290,#148291),(#148292,#148293),
(#148294,#148295),(#148296,#148297),(#148298,#148299),(#148300,#148301),
(#148302,#148303),(#148304,#148305),(#148306,#148307),(#148308,#148309),
(#148310,#148311),(#148312,#148313),(#148314,#148315),(#148316,#148317),
(#148318,#148319),(#148320,#148321),(#148322,#148323),(#148324,#148325),
(#148326,#148327),(#148328,#148329),(#148330,#148331),(#148332,#148333),
(#148334,#148335),(#148336,#148337),(#148338,#148339),(#148340,#148341),
(#148342,#148343),(#148344,#148345),(#148346,#148347),(#148348,#148349),
(#148350,#148351),(#148352,#148353),(#148354,#148355),(#148356,#148357),
(#148358,#148359),(#148360,#148361),(#148362,#148363),(#148364,#148365),
(#148366,#148367),(#148368,#148369),(#148370,#148371),(#148372,#148373),
(#148374,#148375),(#148376,#148377),(#148378,#148379),(#148380,#148381),
(#148382,#148383),(#148384,#148385),(#148386,#148387),(#148388,#148389),
(#148390,#148391),(#148392,#148393),(#148394,#148395),(#148396,#148397),
(#148398,#148399),(#148400,#148401),(#148402,#148403),(#148404,#148405),
(#148406,#148407),(#148408,#148409),(#148410,#148411),(#148412,#148413),
(#148414,#148415),(#148416,#148417),(#148418,#148419),(#148420,#148421),
(#148422,#148423),(#148424,#148425),(#148426,#148427),(#148428,#148429),
(#148430,#148431),(#148432,#148433),(#148434,#148435),(#148436,#148437),
(#148438,#148439),(#148440,#148441),(#148442,#148443),(#148444,#148445),
(#148446,#148447),(#148448,#148449),(#148450,#148451),(#148452,#148453),
(#148454,#148455),(#148456,#148457),(#148458,#148459),(#148460,#148461),
(#148462,#148463),(#148464,#148465),(#148466,#148467),(#148468,#148469),
(#148470,#148471),(#148472,#148473),(#148474,#148475),(#148476,#148477),
(#148478,#148479),(#148480,#148481),(#148482,#148483),(#148484,#148485),
(#148486,#148487),(#148488,#148489),(#148490,#148491),(#148492,#148493),
(#148494,#148495),(#148496,#148497),(#148498,#148499),(#148500,#148501),
(#148502,#148503),(#148504,#148505),(#148506,#148507),(#148508,#148509),
(#148510,#148511),(#148512,#148513),(#148514,#148515),(#148516,#148517),
(#148518,#148519),(#148520,#148521),(#148522,#148523),(#148524,#148525),
(#148526,#148527),(#148528,#148529),(#148530,#148531),(#148532,#148533),
(#148534,#148535),(#148536,#148537),(#148538,#148539),(#148540,#148541),
(#148542,#148543),(#148544,#148545),(#148546,#148547),(#148548,#148549),
(#148550,#148551),(#148552,#148553),(#148554,#148555),(#148556,#148557),
(#148558,#148559),(#148560,#148561),(#148562,#148563),(#148564,#148565),
(#148566,#148567),(#148568,#148569),(#148570,#148571),(#148572,#148573),
(#148574,#148575),(#148576,#148577),(#148578,#148579),(#148580,#148581),
(#148582,#148583),(#148584,#148585),(#148586,#148587),(#148588,#148589),
(#148590,#148591),(#148592,#148593),(#148594,#148595),(#148596,#148597),
(#148598,#148599),(#148600,#148601),(#148602,#148603),(#148604,#148605),
(#148606,#148607),(#148608,#148609),(#148610,#148611),(#148612,#148613),
(#148614,#148615),(#148616,#148617),(#148618,#148619),(#148620,#148621),
(#148622,#148623),(#148624,#148625),(#148626,#148627),(#148628,#148629),
(#148630,#148631),(#148632,#148633),(#148634,#148635),(#148636,#148637),
(#148638,#148639),(#148640,#148641)),.UNSPECIFIED.,.F.,.F.,.F.)
B_SPLINE_SURFACE_WITH_KNOTS((6,1,1,1,1,1,1,1,1,1,1,1,1,1,1,1,1,1,1,1,1,
1,1,1,1,1,1,1,1,1,1,1,1,1,1,1,1,1,1,1,1,1,1,1,1,1,1,1,1,1,1,1,1,1,1,1,1,
1,1,1,1,1,1,1,1,1,1,1,1,1,1,1,1,1,1,1,1,1,1,1,1,1,1,1,1,1,1,1,1,1,1,1,1,
1,1,1,1,1,1,1,1,1,1,1,1,1,1,1,1,1,1,1,1,1,1,1,1,1,1,1,1,1,1,1,1,1,1,1,1,
1,1,1,1,1,1,1,1,1,1,1,1,1,1,1,1,1,1,1,1,1,1,1,1,1,1,1,1,1,1,1,1,1,1,1,1,
1,1,1,1,1,1,1,1,1,1,1,1,1,1,1,1,1,1,1,1,1,1,1,1,1,1,1,1,1,1,1,1,1,1,1,6),
(2,2),(-1.,-0.995000000000001,-0.990000000000001,-0.985000000000001,-0.980000000000001,
-0.975000000000001,-0.970000000000001,-0.965000000000001,-0.960000000000001,
-0.955000000000001,-0.950000000000001,-0.945000000000001,-0.940000000000001,
-0.935000000000001,-0.930000000000001,-0.925000000000001,-0.920000000000001,
-0.915000000000001,-0.910000000000001,-0.905000000000001,-0.900000000000001,
-0.895000000000001,-0.890000000000001,-0.885000000000001,-0.880000000000001,
-0.875000000000001,-0.870000000000001,-0.865000000000001,-0.860000000000001,
-0.855000000000001,-0.850000000000001,-0.845000000000001,-0.840000000000001,
-0.835000000000001,-0.830000000000001,-0.825000000000001,-0.820000000000001,
-0.815000000000001,-0.810000000000001,-0.805000000000001,-0.800000000000001,
-0.795000000000001,-0.790000000000001,-0.785000000000001,-0.780000000000001,
-0.775000000000001,-0.770000000000001,-0.765000000000001,-0.760000000000001,
-0.755000000000001,-0.750000000000001,-0.745000000000001,-0.740000000000001,
-0.735000000000001,-0.730000000000001,-0.725000000000001,-0.720000000000001,
-0.715000000000001,-0.710000000000001,-0.705000000000001,-0.700000000000001,
-0.695000000000001,-0.690000000000001,-0.685,-0.68,-0.675,-0.67,-0.665,
-0.66,-0.655,-0.65,-0.645,-0.64,-0.635,-0.63,-0.625,-0.62,-0.615,-0.61,
-0.605,-0.6,-0.595,-0.59,-0.585,-0.58,-0.575,-0.57,-0.565,-0.56,-0.555,
-0.55,-0.545,-0.54,-0.535,-0.53,-0.525,-0.52,-0.515,-0.51,-0.505,-0.5,-0.495,
-0.49,-0.485,-0.48,-0.475,-0.47,-0.465,-0.46,-0.455,-0.45,-0.445,-0.44,
-0.435,-0.43,-0.425,-0.42,-0.415,-0.41,-0.405,-0.4,-0.395,-0.39,-0.385,
-0.38,-0.375,-0.37,-0.365,-0.36,-0.355,-0.35,-0.345,-0.34,-0.335,-0.33,
-0.325,-0.32,-0.315,-0.31,-0.305,-0.3,-0.295,-0.29,-0.285,-0.28,-0.275,
-0.27,-0.265,-0.26,-0.255,-0.25,-0.245,-0.24,-0.235,-0.23,-0.225,-0.22,
-0.215,-0.21,-0.205,-0.2,-0.195,-0.19,-0.185,-0.18,-0.175,-0.17,-0.165,
-0.16,-0.155,-0.15,-0.145,-0.14,-0.135,-0.13,-0.125,-0.12,-0.115,-0.11,
-0.105,-0.1,-0.095,-0.09,-0.085,-0.08,-0.075,-0.07,-0.065,-0.06,-0.055,
-0.05,-0.045,-0.04,-0.035,-0.03,-0.025,-0.02,-0.015,-0.01,-0.005,0.),(0.,
1.2),.UNSPECIFIED.)
GEOMETRIC_REPRESENTATION_ITEM()
RATIONAL_B_SPLINE_SURFACE(((1.,1.),(1.,1.),(1.,1.),(1.,1.),(1.,1.),(1.,
1.),(1.,1.),(1.,1.),(1.,1.),(1.,1.),(1.,1.),(1.,1.),(1.,1.),(1.,1.),(1.,
1.),(1.,1.),(1.,1.),(1.,1.),(1.,1.),(1.,1.),(1.,1.),(1.,1.),(1.,1.),(1.,
1.),(1.,1.),(1.,1.),(1.,1.),(1.,1.),(1.,1.),(1.,1.),(1.,1.),(1.,1.),(1.,
1.),(1.,1.),(1.,1.),(1.,1.),(1.,1.),(1.,1.),(1.,1.),(1.,1.),(1.,1.),(1.,
1.),(1.,1.),(1.,1.),(1.,1.),(1.,1.),(1.,1.),(1.,1.),(1.,1.),(1.,1.),(1.,
1.),(1.,1.),(1.,1.),(1.,1.),(1.,1.),(1.,1.),(1.,1.),(1.,1.),(1.,1.),(1.,
1.),(1.,1.),(1.,1.),(1.,1.),(1.,1.),(1.,1.),(1.,1.),(1.,1.),(1.,1.),(1.,
1.),(1.,1.),(1.,1.),(1.,1.),(1.,1.),(1.,1.),(1.,1.),(1.,1.),(1.,1.),(1.,
1.),(1.,1.),(1.,1.),(1.,1.),(1.,1.),(1.,1.),(1.,1.),(1.,1.),(1.,1.),(1.,
1.),(1.,1.),(1.,1.),(1.,1.),(1.,1.),(1.,1.),(1.,1.),(1.,1.),(1.,1.),(1.,
1.),(1.,1.),(1.,1.),(1.,1.),(1.,1.),(1.,1.),(1.,1.),(1.,1.),(1.,1.),(1.,
1.),(1.,1.),(1.,1.),(1.,1.),(1.,1.),(1.,1.),(1.,1.),(1.,1.),(1.,1.),(1.,
1.),(1.,1.),(1.,1.),(1.,1.),(1.,1.),(1.,1.),(1.,1.),(1.,1.),(1.,1.),(1.,
1.),(1.,1.),(1.,1.),(1.,1.),(1.,1.),(1.,1.),(1.,1.),(1.,1.),(1.,1.),(1.,
1.),(1.,1.),(1.,1.),(1.,1.),(1.,1.),(1.,1.),(1.,1.),(1.,1.),(1.,1.),(1.,
1.),(1.,1.),(1.,1.),(1.,1.),(1.,1.),(1.,1.),(1.,1.),(1.,1.),(1.,1.),(1.,
1.),(1.,1.),(1.,1.),(1.,1.),(1.,1.),(1.,1.),(1.,1.),(1.,1.),(1.,1.),(1.,
1.),(1.,1.),(1.,1.),(1.,1.),(1.,1.),(1.,1.),(1.,1.),(1.,1.),(1.,1.),(1.,
1.),(1.,1.),(1.,1.),(1.,1.),(1.,1.),(1.,1.),(1.,1.),(1.,1.),(1.,1.),(1.,
1.),(1.,1.),(1.,1.),(1.,1.),(1.,1.),(1.,1.),(1.,1.),(1.,1.),(1.,1.),(1.,
1.),(1.,1.),(1.,1.),(1.,1.),(1.,1.),(1.,1.),(1.,1.),(1.,1.),(1.,1.),(1.,
1.),(1.,1.),(1.,1.),(1.,1.),(1.,1.),(1.,1.),(1.,1.),(1.,1.),(1.,1.),(1.,
1.),(1.,1.)))
REPRESENTATION_ITEM('')
SURFACE()
);
#995=(
BOUNDED_SURFACE()
B_SPLINE_SURFACE(5,1,((#149033,#149034),(#149035,#149036),(#149037,#149038),
(#149039,#149040),(#149041,#149042),(#149043,#149044),(#149045,#149046),
(#149047,#149048),(#149049,#149050),(#149051,#149052),(#149053,#149054),
(#149055,#149056),(#149057,#149058),(#149059,#149060),(#149061,#149062),
(#149063,#149064),(#149065,#149066),(#149067,#149068),(#149069,#149070),
(#149071,#149072),(#149073,#149074),(#149075,#149076),(#149077,#149078),
(#149079,#149080),(#149081,#149082),(#149083,#149084),(#149085,#149086),
(#149087,#149088),(#149089,#149090),(#149091,#149092),(#149093,#149094),
(#149095,#149096),(#149097,#149098),(#149099,#149100),(#149101,#149102),
(#149103,#149104),(#149105,#149106),(#149107,#149108),(#149109,#149110),
(#149111,#149112),(#149113,#149114),(#149115,#149116),(#149117,#149118),
(#149119,#149120),(#149121,#149122),(#149123,#149124),(#149125,#149126),
(#149127,#149128),(#149129,#149130),(#149131,#149132),(#149133,#149134),
(#149135,#149136),(#149137,#149138),(#149139,#149140),(#149141,#149142),
(#149143,#149144),(#149145,#149146),(#149147,#149148),(#149149,#149150),
(#149151,#149152),(#149153,#149154),(#149155,#149156),(#149157,#149158),
(#149159,#149160),(#149161,#149162),(#149163,#149164),(#149165,#149166),
(#149167,#149168),(#149169,#149170),(#149171,#149172),(#149173,#149174),
(#149175,#149176),(#149177,#149178),(#149179,#149180),(#149181,#149182),
(#149183,#149184),(#149185,#149186),(#149187,#149188),(#149189,#149190),
(#149191,#149192),(#149193,#149194),(#149195,#149196),(#149197,#149198),
(#149199,#149200),(#149201,#149202),(#149203,#149204),(#149205,#149206),
(#149207,#149208),(#149209,#149210),(#149211,#149212),(#149213,#149214),
(#149215,#149216),(#149217,#149218),(#149219,#149220),(#149221,#149222),
(#149223,#149224),(#149225,#149226),(#149227,#149228),(#149229,#149230),
(#149231,#149232),(#149233,#149234),(#149235,#149236),(#149237,#149238),
(#149239,#149240),(#149241,#149242),(#149243,#149244),(#149245,#149246),
(#149247,#149248),(#149249,#149250),(#149251,#149252),(#149253,#149254),
(#149255,#149256),(#149257,#149258),(#149259,#149260),(#149261,#149262),
(#149263,#149264),(#149265,#149266),(#149267,#149268),(#149269,#149270),
(#149271,#149272),(#149273,#149274),(#149275,#149276),(#149277,#149278),
(#149279,#149280),(#149281,#149282),(#149283,#149284),(#149285,#149286),
(#149287,#149288),(#149289,#149290),(#149291,#149292),(#149293,#149294),
(#149295,#149296),(#149297,#149298),(#149299,#149300),(#149301,#149302),
(#149303,#149304),(#149305,#149306),(#149307,#149308),(#149309,#149310),
(#149311,#149312),(#149313,#149314),(#149315,#149316),(#149317,#149318),
(#149319,#149320),(#149321,#149322),(#149323,#149324),(#149325,#149326),
(#149327,#149328),(#149329,#149330),(#149331,#149332),(#149333,#149334),
(#149335,#149336),(#149337,#149338),(#149339,#149340),(#149341,#149342),
(#149343,#149344),(#149345,#149346),(#149347,#149348),(#149349,#149350),
(#149351,#149352),(#149353,#149354),(#149355,#149356),(#149357,#149358),
(#149359,#149360),(#149361,#149362),(#149363,#149364),(#149365,#149366),
(#149367,#149368),(#149369,#149370),(#149371,#149372),(#149373,#149374),
(#149375,#149376),(#149377,#149378),(#149379,#149380),(#149381,#149382),
(#149383,#149384),(#149385,#149386),(#149387,#149388),(#149389,#149390),
(#149391,#149392),(#149393,#149394),(#149395,#149396),(#149397,#149398),
(#149399,#149400),(#149401,#149402),(#149403,#149404),(#149405,#149406),
(#149407,#149408),(#149409,#149410),(#149411,#149412),(#149413,#149414),
(#149415,#149416),(#149417,#149418),(#149419,#149420),(#149421,#149422),
(#149423,#149424),(#149425,#149426),(#149427,#149428),(#149429,#149430),
(#149431,#149432),(#149433,#149434),(#149435,#149436),(#149437,#149438),
(#149439,#149440),(#149441,#149442)),.UNSPECIFIED.,.F.,.F.,.F.)
B_SPLINE_SURFACE_WITH_KNOTS((6,1,1,1,1,1,1,1,1,1,1,1,1,1,1,1,1,1,1,1,1,
1,1,1,1,1,1,1,1,1,1,1,1,1,1,1,1,1,1,1,1,1,1,1,1,1,1,1,1,1,1,1,1,1,1,1,1,
1,1,1,1,1,1,1,1,1,1,1,1,1,1,1,1,1,1,1,1,1,1,1,1,1,1,1,1,1,1,1,1,1,1,1,1,
1,1,1,1,1,1,1,1,1,1,1,1,1,1,1,1,1,1,1,1,1,1,1,1,1,1,1,1,1,1,1,1,1,1,1,1,
1,1,1,1,1,1,1,1,1,1,1,1,1,1,1,1,1,1,1,1,1,1,1,1,1,1,1,1,1,1,1,1,1,1,1,1,
1,1,1,1,1,1,1,1,1,1,1,1,1,1,1,1,1,1,1,1,1,1,1,1,1,1,1,1,1,1,1,1,1,1,1,6),
(2,2),(-1.,-0.995000000000001,-0.990000000000001,-0.985000000000001,-0.980000000000001,
-0.975000000000001,-0.970000000000001,-0.965000000000001,-0.960000000000001,
-0.955000000000001,-0.950000000000001,-0.945000000000001,-0.940000000000001,
-0.935000000000001,-0.930000000000001,-0.925000000000001,-0.920000000000001,
-0.915000000000001,-0.910000000000001,-0.905000000000001,-0.900000000000001,
-0.895000000000001,-0.890000000000001,-0.885000000000001,-0.880000000000001,
-0.875000000000001,-0.870000000000001,-0.865000000000001,-0.860000000000001,
-0.855000000000001,-0.850000000000001,-0.845000000000001,-0.840000000000001,
-0.835000000000001,-0.830000000000001,-0.825000000000001,-0.820000000000001,
-0.815000000000001,-0.810000000000001,-0.805000000000001,-0.800000000000001,
-0.795000000000001,-0.790000000000001,-0.785000000000001,-0.780000000000001,
-0.775000000000001,-0.770000000000001,-0.765000000000001,-0.760000000000001,
-0.755000000000001,-0.750000000000001,-0.745000000000001,-0.740000000000001,
-0.735000000000001,-0.730000000000001,-0.725000000000001,-0.720000000000001,
-0.715000000000001,-0.710000000000001,-0.705000000000001,-0.700000000000001,
-0.695000000000001,-0.690000000000001,-0.685,-0.68,-0.675,-0.67,-0.665,
-0.66,-0.655,-0.65,-0.645,-0.64,-0.635,-0.63,-0.625,-0.62,-0.615,-0.61,
-0.605,-0.6,-0.595,-0.59,-0.585,-0.58,-0.575,-0.57,-0.565,-0.56,-0.555,
-0.55,-0.545,-0.54,-0.535,-0.53,-0.525,-0.52,-0.515,-0.51,-0.505,-0.5,-0.495,
-0.49,-0.485,-0.48,-0.475,-0.47,-0.465,-0.46,-0.455,-0.45,-0.445,-0.44,
-0.435,-0.43,-0.425,-0.42,-0.415,-0.41,-0.405,-0.4,-0.395,-0.39,-0.385,
-0.38,-0.375,-0.37,-0.365,-0.36,-0.355,-0.35,-0.345,-0.34,-0.335,-0.33,
-0.325,-0.32,-0.315,-0.31,-0.305,-0.3,-0.295,-0.29,-0.285,-0.28,-0.275,
-0.27,-0.265,-0.26,-0.255,-0.25,-0.245,-0.24,-0.235,-0.23,-0.225,-0.22,
-0.215,-0.21,-0.205,-0.2,-0.195,-0.19,-0.185,-0.18,-0.175,-0.17,-0.165,
-0.16,-0.155,-0.15,-0.145,-0.14,-0.135,-0.13,-0.125,-0.12,-0.115,-0.11,
-0.105,-0.1,-0.095,-0.09,-0.085,-0.08,-0.075,-0.07,-0.065,-0.06,-0.055,
-0.05,-0.045,-0.04,-0.035,-0.03,-0.025,-0.02,-0.015,-0.01,-0.005,0.),(0.,
1.2),.UNSPECIFIED.)
GEOMETRIC_REPRESENTATION_ITEM()
RATIONAL_B_SPLINE_SURFACE(((1.,1.),(1.,1.),(1.,1.),(1.,1.),(1.,1.),(1.,
1.),(1.,1.),(1.,1.),(1.,1.),(1.,1.),(1.,1.),(1.,1.),(1.,1.),(1.,1.),(1.,
1.),(1.,1.),(1.,1.),(1.,1.),(1.,1.),(1.,1.),(1.,1.),(1.,1.),(1.,1.),(1.,
1.),(1.,1.),(1.,1.),(1.,1.),(1.,1.),(1.,1.),(1.,1.),(1.,1.),(1.,1.),(1.,
1.),(1.,1.),(1.,1.),(1.,1.),(1.,1.),(1.,1.),(1.,1.),(1.,1.),(1.,1.),(1.,
1.),(1.,1.),(1.,1.),(1.,1.),(1.,1.),(1.,1.),(1.,1.),(1.,1.),(1.,1.),(1.,
1.),(1.,1.),(1.,1.),(1.,1.),(1.,1.),(1.,1.),(1.,1.),(1.,1.),(1.,1.),(1.,
1.),(1.,1.),(1.,1.),(1.,1.),(1.,1.),(1.,1.),(1.,1.),(1.,1.),(1.,1.),(1.,
1.),(1.,1.),(1.,1.),(1.,1.),(1.,1.),(1.,1.),(1.,1.),(1.,1.),(1.,1.),(1.,
1.),(1.,1.),(1.,1.),(1.,1.),(1.,1.),(1.,1.),(1.,1.),(1.,1.),(1.,1.),(1.,
1.),(1.,1.),(1.,1.),(1.,1.),(1.,1.),(1.,1.),(1.,1.),(1.,1.),(1.,1.),(1.,
1.),(1.,1.),(1.,1.),(1.,1.),(1.,1.),(1.,1.),(1.,1.),(1.,1.),(1.,1.),(1.,
1.),(1.,1.),(1.,1.),(1.,1.),(1.,1.),(1.,1.),(1.,1.),(1.,1.),(1.,1.),(1.,
1.),(1.,1.),(1.,1.),(1.,1.),(1.,1.),(1.,1.),(1.,1.),(1.,1.),(1.,1.),(1.,
1.),(1.,1.),(1.,1.),(1.,1.),(1.,1.),(1.,1.),(1.,1.),(1.,1.),(1.,1.),(1.,
1.),(1.,1.),(1.,1.),(1.,1.),(1.,1.),(1.,1.),(1.,1.),(1.,1.),(1.,1.),(1.,
1.),(1.,1.),(1.,1.),(1.,1.),(1.,1.),(1.,1.),(1.,1.),(1.,1.),(1.,1.),(1.,
1.),(1.,1.),(1.,1.),(1.,1.),(1.,1.),(1.,1.),(1.,1.),(1.,1.),(1.,1.),(1.,
1.),(1.,1.),(1.,1.),(1.,1.),(1.,1.),(1.,1.),(1.,1.),(1.,1.),(1.,1.),(1.,
1.),(1.,1.),(1.,1.),(1.,1.),(1.,1.),(1.,1.),(1.,1.),(1.,1.),(1.,1.),(1.,
1.),(1.,1.),(1.,1.),(1.,1.),(1.,1.),(1.,1.),(1.,1.),(1.,1.),(1.,1.),(1.,
1.),(1.,1.),(1.,1.),(1.,1.),(1.,1.),(1.,1.),(1.,1.),(1.,1.),(1.,1.),(1.,
1.),(1.,1.),(1.,1.),(1.,1.),(1.,1.),(1.,1.),(1.,1.),(1.,1.),(1.,1.),(1.,
1.),(1.,1.)))
REPRESENTATION_ITEM('')
SURFACE()
);
#996=(
BOUNDED_SURFACE()
B_SPLINE_SURFACE(5,1,((#149834,#149835),(#149836,#149837),(#149838,#149839),
(#149840,#149841),(#149842,#149843),(#149844,#149845),(#149846,#149847),
(#149848,#149849),(#149850,#149851),(#149852,#149853),(#149854,#149855),
(#149856,#149857),(#149858,#149859),(#149860,#149861),(#149862,#149863),
(#149864,#149865),(#149866,#149867),(#149868,#149869),(#149870,#149871),
(#149872,#149873),(#149874,#149875),(#149876,#149877),(#149878,#149879),
(#149880,#149881),(#149882,#149883),(#149884,#149885),(#149886,#149887),
(#149888,#149889),(#149890,#149891),(#149892,#149893),(#149894,#149895),
(#149896,#149897),(#149898,#149899),(#149900,#149901),(#149902,#149903),
(#149904,#149905),(#149906,#149907),(#149908,#149909),(#149910,#149911),
(#149912,#149913),(#149914,#149915),(#149916,#149917),(#149918,#149919),
(#149920,#149921),(#149922,#149923),(#149924,#149925),(#149926,#149927),
(#149928,#149929),(#149930,#149931),(#149932,#149933),(#149934,#149935),
(#149936,#149937),(#149938,#149939),(#149940,#149941),(#149942,#149943),
(#149944,#149945),(#149946,#149947),(#149948,#149949),(#149950,#149951),
(#149952,#149953),(#149954,#149955),(#149956,#149957),(#149958,#149959),
(#149960,#149961),(#149962,#149963),(#149964,#149965),(#149966,#149967),
(#149968,#149969),(#149970,#149971),(#149972,#149973),(#149974,#149975),
(#149976,#149977),(#149978,#149979),(#149980,#149981),(#149982,#149983),
(#149984,#149985),(#149986,#149987),(#149988,#149989),(#149990,#149991),
(#149992,#149993),(#149994,#149995),(#149996,#149997),(#149998,#149999),
(#150000,#150001),(#150002,#150003),(#150004,#150005),(#150006,#150007),
(#150008,#150009),(#150010,#150011),(#150012,#150013),(#150014,#150015),
(#150016,#150017),(#150018,#150019),(#150020,#150021),(#150022,#150023),
(#150024,#150025),(#150026,#150027),(#150028,#150029),(#150030,#150031),
(#150032,#150033),(#150034,#150035),(#150036,#150037),(#150038,#150039),
(#150040,#150041),(#150042,#150043),(#150044,#150045),(#150046,#150047),
(#150048,#150049),(#150050,#150051),(#150052,#150053),(#150054,#150055),
(#150056,#150057),(#150058,#150059),(#150060,#150061),(#150062,#150063),
(#150064,#150065),(#150066,#150067),(#150068,#150069),(#150070,#150071),
(#150072,#150073),(#150074,#150075),(#150076,#150077),(#150078,#150079),
(#150080,#150081),(#150082,#150083),(#150084,#150085),(#150086,#150087),
(#150088,#150089),(#150090,#150091),(#150092,#150093),(#150094,#150095),
(#150096,#150097),(#150098,#150099),(#150100,#150101),(#150102,#150103),
(#150104,#150105),(#150106,#150107),(#150108,#150109),(#150110,#150111),
(#150112,#150113),(#150114,#150115),(#150116,#150117),(#150118,#150119),
(#150120,#150121),(#150122,#150123),(#150124,#150125),(#150126,#150127),
(#150128,#150129),(#150130,#150131),(#150132,#150133),(#150134,#150135),
(#150136,#150137),(#150138,#150139),(#150140,#150141),(#150142,#150143),
(#150144,#150145),(#150146,#150147),(#150148,#150149),(#150150,#150151),
(#150152,#150153),(#150154,#150155),(#150156,#150157),(#150158,#150159),
(#150160,#150161),(#150162,#150163),(#150164,#150165),(#150166,#150167),
(#150168,#150169),(#150170,#150171),(#150172,#150173),(#150174,#150175),
(#150176,#150177),(#150178,#150179),(#150180,#150181),(#150182,#150183),
(#150184,#150185),(#150186,#150187),(#150188,#150189),(#150190,#150191),
(#150192,#150193),(#150194,#150195),(#150196,#150197),(#150198,#150199),
(#150200,#150201),(#150202,#150203),(#150204,#150205),(#150206,#150207),
(#150208,#150209),(#150210,#150211),(#150212,#150213),(#150214,#150215),
(#150216,#150217),(#150218,#150219),(#150220,#150221),(#150222,#150223),
(#150224,#150225),(#150226,#150227),(#150228,#150229),(#150230,#150231),
(#150232,#150233),(#150234,#150235),(#150236,#150237),(#150238,#150239),
(#150240,#150241),(#150242,#150243)),.UNSPECIFIED.,.F.,.F.,.F.)
B_SPLINE_SURFACE_WITH_KNOTS((6,1,1,1,1,1,1,1,1,1,1,1,1,1,1,1,1,1,1,1,1,
1,1,1,1,1,1,1,1,1,1,1,1,1,1,1,1,1,1,1,1,1,1,1,1,1,1,1,1,1,1,1,1,1,1,1,1,
1,1,1,1,1,1,1,1,1,1,1,1,1,1,1,1,1,1,1,1,1,1,1,1,1,1,1,1,1,1,1,1,1,1,1,1,
1,1,1,1,1,1,1,1,1,1,1,1,1,1,1,1,1,1,1,1,1,1,1,1,1,1,1,1,1,1,1,1,1,1,1,1,
1,1,1,1,1,1,1,1,1,1,1,1,1,1,1,1,1,1,1,1,1,1,1,1,1,1,1,1,1,1,1,1,1,1,1,1,
1,1,1,1,1,1,1,1,1,1,1,1,1,1,1,1,1,1,1,1,1,1,1,1,1,1,1,1,1,1,1,1,1,1,1,6),
(2,2),(-1.,-0.995000000000001,-0.990000000000001,-0.985000000000001,-0.980000000000001,
-0.975000000000001,-0.970000000000001,-0.965000000000001,-0.960000000000001,
-0.955000000000001,-0.950000000000001,-0.945000000000001,-0.940000000000001,
-0.935000000000001,-0.930000000000001,-0.925000000000001,-0.920000000000001,
-0.915000000000001,-0.910000000000001,-0.905000000000001,-0.900000000000001,
-0.895000000000001,-0.890000000000001,-0.885000000000001,-0.880000000000001,
-0.875000000000001,-0.870000000000001,-0.865000000000001,-0.860000000000001,
-0.855000000000001,-0.850000000000001,-0.845000000000001,-0.840000000000001,
-0.835000000000001,-0.830000000000001,-0.825000000000001,-0.820000000000001,
-0.815000000000001,-0.810000000000001,-0.805000000000001,-0.800000000000001,
-0.795000000000001,-0.790000000000001,-0.785000000000001,-0.780000000000001,
-0.775000000000001,-0.770000000000001,-0.765000000000001,-0.760000000000001,
-0.755000000000001,-0.750000000000001,-0.745000000000001,-0.740000000000001,
-0.735000000000001,-0.730000000000001,-0.725000000000001,-0.720000000000001,
-0.715000000000001,-0.710000000000001,-0.705000000000001,-0.700000000000001,
-0.695000000000001,-0.690000000000001,-0.685,-0.68,-0.675,-0.67,-0.665,
-0.66,-0.655,-0.65,-0.645,-0.64,-0.635,-0.63,-0.625,-0.62,-0.615,-0.61,
-0.605,-0.6,-0.595,-0.59,-0.585,-0.58,-0.575,-0.57,-0.565,-0.56,-0.555,
-0.55,-0.545,-0.54,-0.535,-0.53,-0.525,-0.52,-0.515,-0.51,-0.505,-0.5,-0.495,
-0.49,-0.485,-0.48,-0.475,-0.47,-0.465,-0.46,-0.455,-0.45,-0.445,-0.44,
-0.435,-0.43,-0.425,-0.42,-0.415,-0.41,-0.405,-0.4,-0.395,-0.39,-0.385,
-0.38,-0.375,-0.37,-0.365,-0.36,-0.355,-0.35,-0.345,-0.34,-0.335,-0.33,
-0.325,-0.32,-0.315,-0.31,-0.305,-0.3,-0.295,-0.29,-0.285,-0.28,-0.275,
-0.27,-0.265,-0.26,-0.255,-0.25,-0.245,-0.24,-0.235,-0.23,-0.225,-0.22,
-0.215,-0.21,-0.205,-0.2,-0.195,-0.19,-0.185,-0.18,-0.175,-0.17,-0.165,
-0.16,-0.155,-0.15,-0.145,-0.14,-0.135,-0.13,-0.125,-0.12,-0.115,-0.11,
-0.105,-0.1,-0.095,-0.09,-0.085,-0.08,-0.075,-0.07,-0.065,-0.06,-0.055,
-0.05,-0.045,-0.04,-0.035,-0.03,-0.025,-0.02,-0.015,-0.01,-0.005,0.),(0.,
1.2),.UNSPECIFIED.)
GEOMETRIC_REPRESENTATION_ITEM()
RATIONAL_B_SPLINE_SURFACE(((1.,1.),(1.,1.),(1.,1.),(1.,1.),(1.,1.),(1.,
1.),(1.,1.),(1.,1.),(1.,1.),(1.,1.),(1.,1.),(1.,1.),(1.,1.),(1.,1.),(1.,
1.),(1.,1.),(1.,1.),(1.,1.),(1.,1.),(1.,1.),(1.,1.),(1.,1.),(1.,1.),(1.,
1.),(1.,1.),(1.,1.),(1.,1.),(1.,1.),(1.,1.),(1.,1.),(1.,1.),(1.,1.),(1.,
1.),(1.,1.),(1.,1.),(1.,1.),(1.,1.),(1.,1.),(1.,1.),(1.,1.),(1.,1.),(1.,
1.),(1.,1.),(1.,1.),(1.,1.),(1.,1.),(1.,1.),(1.,1.),(1.,1.),(1.,1.),(1.,
1.),(1.,1.),(1.,1.),(1.,1.),(1.,1.),(1.,1.),(1.,1.),(1.,1.),(1.,1.),(1.,
1.),(1.,1.),(1.,1.),(1.,1.),(1.,1.),(1.,1.),(1.,1.),(1.,1.),(1.,1.),(1.,
1.),(1.,1.),(1.,1.),(1.,1.),(1.,1.),(1.,1.),(1.,1.),(1.,1.),(1.,1.),(1.,
1.),(1.,1.),(1.,1.),(1.,1.),(1.,1.),(1.,1.),(1.,1.),(1.,1.),(1.,1.),(1.,
1.),(1.,1.),(1.,1.),(1.,1.),(1.,1.),(1.,1.),(1.,1.),(1.,1.),(1.,1.),(1.,
1.),(1.,1.),(1.,1.),(1.,1.),(1.,1.),(1.,1.),(1.,1.),(1.,1.),(1.,1.),(1.,
1.),(1.,1.),(1.,1.),(1.,1.),(1.,1.),(1.,1.),(1.,1.),(1.,1.),(1.,1.),(1.,
1.),(1.,1.),(1.,1.),(1.,1.),(1.,1.),(1.,1.),(1.,1.),(1.,1.),(1.,1.),(1.,
1.),(1.,1.),(1.,1.),(1.,1.),(1.,1.),(1.,1.),(1.,1.),(1.,1.),(1.,1.),(1.,
1.),(1.,1.),(1.,1.),(1.,1.),(1.,1.),(1.,1.),(1.,1.),(1.,1.),(1.,1.),(1.,
1.),(1.,1.),(1.,1.),(1.,1.),(1.,1.),(1.,1.),(1.,1.),(1.,1.),(1.,1.),(1.,
1.),(1.,1.),(1.,1.),(1.,1.),(1.,1.),(1.,1.),(1.,1.),(1.,1.),(1.,1.),(1.,
1.),(1.,1.),(1.,1.),(1.,1.),(1.,1.),(1.,1.),(1.,1.),(1.,1.),(1.,1.),(1.,
1.),(1.,1.),(1.,1.),(1.,1.),(1.,1.),(1.,1.),(1.,1.),(1.,1.),(1.,1.),(1.,
1.),(1.,1.),(1.,1.),(1.,1.),(1.,1.),(1.,1.),(1.,1.),(1.,1.),(1.,1.),(1.,
1.),(1.,1.),(1.,1.),(1.,1.),(1.,1.),(1.,1.),(1.,1.),(1.,1.),(1.,1.),(1.,
1.),(1.,1.),(1.,1.),(1.,1.),(1.,1.),(1.,1.),(1.,1.),(1.,1.),(1.,1.),(1.,
1.),(1.,1.)))
REPRESENTATION_ITEM('')
SURFACE()
);
#997=(
BOUNDED_SURFACE()
B_SPLINE_SURFACE(5,1,((#150635,#150636),(#150637,#150638),(#150639,#150640),
(#150641,#150642),(#150643,#150644),(#150645,#150646),(#150647,#150648),
(#150649,#150650),(#150651,#150652),(#150653,#150654),(#150655,#150656),
(#150657,#150658),(#150659,#150660),(#150661,#150662),(#150663,#150664),
(#150665,#150666),(#150667,#150668),(#150669,#150670),(#150671,#150672),
(#150673,#150674),(#150675,#150676),(#150677,#150678),(#150679,#150680),
(#150681,#150682),(#150683,#150684),(#150685,#150686),(#150687,#150688),
(#150689,#150690),(#150691,#150692),(#150693,#150694),(#150695,#150696),
(#150697,#150698),(#150699,#150700),(#150701,#150702),(#150703,#150704),
(#150705,#150706),(#150707,#150708),(#150709,#150710),(#150711,#150712),
(#150713,#150714),(#150715,#150716),(#150717,#150718),(#150719,#150720),
(#150721,#150722),(#150723,#150724),(#150725,#150726),(#150727,#150728),
(#150729,#150730),(#150731,#150732),(#150733,#150734),(#150735,#150736),
(#150737,#150738),(#150739,#150740),(#150741,#150742),(#150743,#150744),
(#150745,#150746),(#150747,#150748),(#150749,#150750),(#150751,#150752),
(#150753,#150754),(#150755,#150756),(#150757,#150758),(#150759,#150760),
(#150761,#150762),(#150763,#150764),(#150765,#150766),(#150767,#150768),
(#150769,#150770),(#150771,#150772),(#150773,#150774),(#150775,#150776),
(#150777,#150778),(#150779,#150780),(#150781,#150782),(#150783,#150784),
(#150785,#150786),(#150787,#150788),(#150789,#150790),(#150791,#150792),
(#150793,#150794),(#150795,#150796),(#150797,#150798),(#150799,#150800),
(#150801,#150802),(#150803,#150804),(#150805,#150806),(#150807,#150808),
(#150809,#150810),(#150811,#150812),(#150813,#150814),(#150815,#150816),
(#150817,#150818),(#150819,#150820),(#150821,#150822),(#150823,#150824),
(#150825,#150826),(#150827,#150828),(#150829,#150830),(#150831,#150832),
(#150833,#150834),(#150835,#150836),(#150837,#150838),(#150839,#150840),
(#150841,#150842),(#150843,#150844),(#150845,#150846),(#150847,#150848),
(#150849,#150850),(#150851,#150852),(#150853,#150854),(#150855,#150856),
(#150857,#150858),(#150859,#150860),(#150861,#150862),(#150863,#150864),
(#150865,#150866),(#150867,#150868),(#150869,#150870),(#150871,#150872),
(#150873,#150874),(#150875,#150876),(#150877,#150878),(#150879,#150880),
(#150881,#150882),(#150883,#150884),(#150885,#150886),(#150887,#150888),
(#150889,#150890),(#150891,#150892),(#150893,#150894),(#150895,#150896),
(#150897,#150898),(#150899,#150900),(#150901,#150902),(#150903,#150904),
(#150905,#150906),(#150907,#150908),(#150909,#150910),(#150911,#150912),
(#150913,#150914),(#150915,#150916),(#150917,#150918),(#150919,#150920),
(#150921,#150922),(#150923,#150924),(#150925,#150926),(#150927,#150928),
(#150929,#150930),(#150931,#150932),(#150933,#150934),(#150935,#150936),
(#150937,#150938),(#150939,#150940),(#150941,#150942),(#150943,#150944),
(#150945,#150946),(#150947,#150948),(#150949,#150950),(#150951,#150952),
(#150953,#150954),(#150955,#150956),(#150957,#150958),(#150959,#150960),
(#150961,#150962),(#150963,#150964),(#150965,#150966),(#150967,#150968),
(#150969,#150970),(#150971,#150972),(#150973,#150974),(#150975,#150976),
(#150977,#150978),(#150979,#150980),(#150981,#150982),(#150983,#150984),
(#150985,#150986),(#150987,#150988),(#150989,#150990),(#150991,#150992),
(#150993,#150994),(#150995,#150996),(#150997,#150998),(#150999,#151000),
(#151001,#151002),(#151003,#151004),(#151005,#151006),(#151007,#151008),
(#151009,#151010),(#151011,#151012),(#151013,#151014),(#151015,#151016),
(#151017,#151018),(#151019,#151020),(#151021,#151022),(#151023,#151024),
(#151025,#151026),(#151027,#151028),(#151029,#151030),(#151031,#151032),
(#151033,#151034),(#151035,#151036),(#151037,#151038),(#151039,#151040),
(#151041,#151042),(#151043,#151044)),.UNSPECIFIED.,.F.,.F.,.F.)
B_SPLINE_SURFACE_WITH_KNOTS((6,1,1,1,1,1,1,1,1,1,1,1,1,1,1,1,1,1,1,1,1,
1,1,1,1,1,1,1,1,1,1,1,1,1,1,1,1,1,1,1,1,1,1,1,1,1,1,1,1,1,1,1,1,1,1,1,1,
1,1,1,1,1,1,1,1,1,1,1,1,1,1,1,1,1,1,1,1,1,1,1,1,1,1,1,1,1,1,1,1,1,1,1,1,
1,1,1,1,1,1,1,1,1,1,1,1,1,1,1,1,1,1,1,1,1,1,1,1,1,1,1,1,1,1,1,1,1,1,1,1,
1,1,1,1,1,1,1,1,1,1,1,1,1,1,1,1,1,1,1,1,1,1,1,1,1,1,1,1,1,1,1,1,1,1,1,1,
1,1,1,1,1,1,1,1,1,1,1,1,1,1,1,1,1,1,1,1,1,1,1,1,1,1,1,1,1,1,1,1,1,1,1,6),
(2,2),(-1.,-0.995000000000001,-0.990000000000001,-0.985000000000001,-0.980000000000001,
-0.975000000000001,-0.970000000000001,-0.965000000000001,-0.960000000000001,
-0.955000000000001,-0.950000000000001,-0.945000000000001,-0.940000000000001,
-0.935000000000001,-0.930000000000001,-0.925000000000001,-0.920000000000001,
-0.915000000000001,-0.910000000000001,-0.905000000000001,-0.900000000000001,
-0.895000000000001,-0.890000000000001,-0.885000000000001,-0.880000000000001,
-0.875000000000001,-0.870000000000001,-0.865000000000001,-0.860000000000001,
-0.855000000000001,-0.850000000000001,-0.845000000000001,-0.840000000000001,
-0.835000000000001,-0.830000000000001,-0.825000000000001,-0.820000000000001,
-0.815000000000001,-0.810000000000001,-0.805000000000001,-0.800000000000001,
-0.795000000000001,-0.790000000000001,-0.785000000000001,-0.780000000000001,
-0.775000000000001,-0.770000000000001,-0.765000000000001,-0.760000000000001,
-0.755000000000001,-0.750000000000001,-0.745000000000001,-0.740000000000001,
-0.735000000000001,-0.730000000000001,-0.725000000000001,-0.720000000000001,
-0.715000000000001,-0.710000000000001,-0.705000000000001,-0.700000000000001,
-0.695000000000001,-0.690000000000001,-0.685,-0.68,-0.675,-0.67,-0.665,
-0.66,-0.655,-0.65,-0.645,-0.64,-0.635,-0.63,-0.625,-0.62,-0.615,-0.61,
-0.605,-0.6,-0.595,-0.59,-0.585,-0.58,-0.575,-0.57,-0.565,-0.56,-0.555,
-0.55,-0.545,-0.54,-0.535,-0.53,-0.525,-0.52,-0.515,-0.51,-0.505,-0.5,-0.495,
-0.49,-0.485,-0.48,-0.475,-0.47,-0.465,-0.46,-0.455,-0.45,-0.445,-0.44,
-0.435,-0.43,-0.425,-0.42,-0.415,-0.41,-0.405,-0.4,-0.395,-0.39,-0.385,
-0.38,-0.375,-0.37,-0.365,-0.36,-0.355,-0.35,-0.345,-0.34,-0.335,-0.33,
-0.325,-0.32,-0.315,-0.31,-0.305,-0.3,-0.295,-0.29,-0.285,-0.28,-0.275,
-0.27,-0.265,-0.26,-0.255,-0.25,-0.245,-0.24,-0.235,-0.23,-0.225,-0.22,
-0.215,-0.21,-0.205,-0.2,-0.195,-0.19,-0.185,-0.18,-0.175,-0.17,-0.165,
-0.16,-0.155,-0.15,-0.145,-0.14,-0.135,-0.13,-0.125,-0.12,-0.115,-0.11,
-0.105,-0.1,-0.095,-0.09,-0.085,-0.08,-0.075,-0.07,-0.065,-0.06,-0.055,
-0.05,-0.045,-0.04,-0.035,-0.03,-0.025,-0.02,-0.015,-0.01,-0.005,0.),(0.,
1.2),.UNSPECIFIED.)
GEOMETRIC_REPRESENTATION_ITEM()
RATIONAL_B_SPLINE_SURFACE(((1.,1.),(1.,1.),(1.,1.),(1.,1.),(1.,1.),(1.,
1.),(1.,1.),(1.,1.),(1.,1.),(1.,1.),(1.,1.),(1.,1.),(1.,1.),(1.,1.),(1.,
1.),(1.,1.),(1.,1.),(1.,1.),(1.,1.),(1.,1.),(1.,1.),(1.,1.),(1.,1.),(1.,
1.),(1.,1.),(1.,1.),(1.,1.),(1.,1.),(1.,1.),(1.,1.),(1.,1.),(1.,1.),(1.,
1.),(1.,1.),(1.,1.),(1.,1.),(1.,1.),(1.,1.),(1.,1.),(1.,1.),(1.,1.),(1.,
1.),(1.,1.),(1.,1.),(1.,1.),(1.,1.),(1.,1.),(1.,1.),(1.,1.),(1.,1.),(1.,
1.),(1.,1.),(1.,1.),(1.,1.),(1.,1.),(1.,1.),(1.,1.),(1.,1.),(1.,1.),(1.,
1.),(1.,1.),(1.,1.),(1.,1.),(1.,1.),(1.,1.),(1.,1.),(1.,1.),(1.,1.),(1.,
1.),(1.,1.),(1.,1.),(1.,1.),(1.,1.),(1.,1.),(1.,1.),(1.,1.),(1.,1.),(1.,
1.),(1.,1.),(1.,1.),(1.,1.),(1.,1.),(1.,1.),(1.,1.),(1.,1.),(1.,1.),(1.,
1.),(1.,1.),(1.,1.),(1.,1.),(1.,1.),(1.,1.),(1.,1.),(1.,1.),(1.,1.),(1.,
1.),(1.,1.),(1.,1.),(1.,1.),(1.,1.),(1.,1.),(1.,1.),(1.,1.),(1.,1.),(1.,
1.),(1.,1.),(1.,1.),(1.,1.),(1.,1.),(1.,1.),(1.,1.),(1.,1.),(1.,1.),(1.,
1.),(1.,1.),(1.,1.),(1.,1.),(1.,1.),(1.,1.),(1.,1.),(1.,1.),(1.,1.),(1.,
1.),(1.,1.),(1.,1.),(1.,1.),(1.,1.),(1.,1.),(1.,1.),(1.,1.),(1.,1.),(1.,
1.),(1.,1.),(1.,1.),(1.,1.),(1.,1.),(1.,1.),(1.,1.),(1.,1.),(1.,1.),(1.,
1.),(1.,1.),(1.,1.),(1.,1.),(1.,1.),(1.,1.),(1.,1.),(1.,1.),(1.,1.),(1.,
1.),(1.,1.),(1.,1.),(1.,1.),(1.,1.),(1.,1.),(1.,1.),(1.,1.),(1.,1.),(1.,
1.),(1.,1.),(1.,1.),(1.,1.),(1.,1.),(1.,1.),(1.,1.),(1.,1.),(1.,1.),(1.,
1.),(1.,1.),(1.,1.),(1.,1.),(1.,1.),(1.,1.),(1.,1.),(1.,1.),(1.,1.),(1.,
1.),(1.,1.),(1.,1.),(1.,1.),(1.,1.),(1.,1.),(1.,1.),(1.,1.),(1.,1.),(1.,
1.),(1.,1.),(1.,1.),(1.,1.),(1.,1.),(1.,1.),(1.,1.),(1.,1.),(1.,1.),(1.,
1.),(1.,1.),(1.,1.),(1.,1.),(1.,1.),(1.,1.),(1.,1.),(1.,1.),(1.,1.),(1.,
1.),(1.,1.)))
REPRESENTATION_ITEM('')
SURFACE()
);
#998=(
BOUNDED_SURFACE()
B_SPLINE_SURFACE(5,1,((#151436,#151437),(#151438,#151439),(#151440,#151441),
(#151442,#151443),(#151444,#151445),(#151446,#151447),(#151448,#151449),
(#151450,#151451),(#151452,#151453),(#151454,#151455),(#151456,#151457),
(#151458,#151459),(#151460,#151461),(#151462,#151463),(#151464,#151465),
(#151466,#151467),(#151468,#151469),(#151470,#151471),(#151472,#151473),
(#151474,#151475),(#151476,#151477),(#151478,#151479),(#151480,#151481),
(#151482,#151483),(#151484,#151485),(#151486,#151487),(#151488,#151489),
(#151490,#151491),(#151492,#151493),(#151494,#151495),(#151496,#151497),
(#151498,#151499),(#151500,#151501),(#151502,#151503),(#151504,#151505),
(#151506,#151507),(#151508,#151509),(#151510,#151511),(#151512,#151513),
(#151514,#151515),(#151516,#151517),(#151518,#151519),(#151520,#151521),
(#151522,#151523),(#151524,#151525),(#151526,#151527),(#151528,#151529),
(#151530,#151531),(#151532,#151533),(#151534,#151535),(#151536,#151537),
(#151538,#151539),(#151540,#151541),(#151542,#151543),(#151544,#151545),
(#151546,#151547),(#151548,#151549),(#151550,#151551),(#151552,#151553),
(#151554,#151555),(#151556,#151557),(#151558,#151559),(#151560,#151561),
(#151562,#151563),(#151564,#151565),(#151566,#151567),(#151568,#151569),
(#151570,#151571),(#151572,#151573),(#151574,#151575),(#151576,#151577),
(#151578,#151579),(#151580,#151581),(#151582,#151583),(#151584,#151585),
(#151586,#151587),(#151588,#151589),(#151590,#151591),(#151592,#151593),
(#151594,#151595),(#151596,#151597),(#151598,#151599),(#151600,#151601),
(#151602,#151603),(#151604,#151605),(#151606,#151607),(#151608,#151609),
(#151610,#151611),(#151612,#151613),(#151614,#151615),(#151616,#151617),
(#151618,#151619),(#151620,#151621),(#151622,#151623),(#151624,#151625),
(#151626,#151627),(#151628,#151629),(#151630,#151631),(#151632,#151633),
(#151634,#151635),(#151636,#151637),(#151638,#151639),(#151640,#151641),
(#151642,#151643),(#151644,#151645),(#151646,#151647),(#151648,#151649),
(#151650,#151651),(#151652,#151653),(#151654,#151655),(#151656,#151657),
(#151658,#151659),(#151660,#151661),(#151662,#151663),(#151664,#151665),
(#151666,#151667),(#151668,#151669),(#151670,#151671),(#151672,#151673),
(#151674,#151675),(#151676,#151677),(#151678,#151679),(#151680,#151681),
(#151682,#151683),(#151684,#151685),(#151686,#151687),(#151688,#151689),
(#151690,#151691),(#151692,#151693),(#151694,#151695),(#151696,#151697),
(#151698,#151699),(#151700,#151701),(#151702,#151703),(#151704,#151705),
(#151706,#151707),(#151708,#151709),(#151710,#151711),(#151712,#151713),
(#151714,#151715),(#151716,#151717),(#151718,#151719),(#151720,#151721),
(#151722,#151723),(#151724,#151725),(#151726,#151727),(#151728,#151729),
(#151730,#151731),(#151732,#151733),(#151734,#151735),(#151736,#151737),
(#151738,#151739),(#151740,#151741),(#151742,#151743),(#151744,#151745),
(#151746,#151747),(#151748,#151749),(#151750,#151751),(#151752,#151753),
(#151754,#151755),(#151756,#151757),(#151758,#151759),(#151760,#151761),
(#151762,#151763),(#151764,#151765),(#151766,#151767),(#151768,#151769),
(#151770,#151771),(#151772,#151773),(#151774,#151775),(#151776,#151777),
(#151778,#151779),(#151780,#151781),(#151782,#151783),(#151784,#151785),
(#151786,#151787),(#151788,#151789),(#151790,#151791),(#151792,#151793),
(#151794,#151795),(#151796,#151797),(#151798,#151799),(#151800,#151801),
(#151802,#151803),(#151804,#151805),(#151806,#151807),(#151808,#151809),
(#151810,#151811),(#151812,#151813),(#151814,#151815),(#151816,#151817),
(#151818,#151819),(#151820,#151821),(#151822,#151823),(#151824,#151825),
(#151826,#151827),(#151828,#151829),(#151830,#151831),(#151832,#151833),
(#151834,#151835),(#151836,#151837),(#151838,#151839),(#151840,#151841),
(#151842,#151843),(#151844,#151845)),.UNSPECIFIED.,.F.,.F.,.F.)
B_SPLINE_SURFACE_WITH_KNOTS((6,1,1,1,1,1,1,1,1,1,1,1,1,1,1,1,1,1,1,1,1,
1,1,1,1,1,1,1,1,1,1,1,1,1,1,1,1,1,1,1,1,1,1,1,1,1,1,1,1,1,1,1,1,1,1,1,1,
1,1,1,1,1,1,1,1,1,1,1,1,1,1,1,1,1,1,1,1,1,1,1,1,1,1,1,1,1,1,1,1,1,1,1,1,
1,1,1,1,1,1,1,1,1,1,1,1,1,1,1,1,1,1,1,1,1,1,1,1,1,1,1,1,1,1,1,1,1,1,1,1,
1,1,1,1,1,1,1,1,1,1,1,1,1,1,1,1,1,1,1,1,1,1,1,1,1,1,1,1,1,1,1,1,1,1,1,1,
1,1,1,1,1,1,1,1,1,1,1,1,1,1,1,1,1,1,1,1,1,1,1,1,1,1,1,1,1,1,1,1,1,1,1,6),
(2,2),(-1.,-0.995000000000001,-0.990000000000001,-0.985000000000001,-0.980000000000001,
-0.975000000000001,-0.970000000000001,-0.965000000000001,-0.960000000000001,
-0.955000000000001,-0.950000000000001,-0.945000000000001,-0.940000000000001,
-0.935000000000001,-0.930000000000001,-0.925000000000001,-0.920000000000001,
-0.915000000000001,-0.910000000000001,-0.905000000000001,-0.900000000000001,
-0.895000000000001,-0.890000000000001,-0.885000000000001,-0.880000000000001,
-0.875000000000001,-0.870000000000001,-0.865000000000001,-0.860000000000001,
-0.855000000000001,-0.850000000000001,-0.845000000000001,-0.840000000000001,
-0.835000000000001,-0.830000000000001,-0.825000000000001,-0.820000000000001,
-0.815000000000001,-0.810000000000001,-0.805000000000001,-0.800000000000001,
-0.795000000000001,-0.790000000000001,-0.785000000000001,-0.780000000000001,
-0.775000000000001,-0.770000000000001,-0.765000000000001,-0.760000000000001,
-0.755000000000001,-0.750000000000001,-0.745000000000001,-0.740000000000001,
-0.735000000000001,-0.730000000000001,-0.725000000000001,-0.720000000000001,
-0.715000000000001,-0.710000000000001,-0.705000000000001,-0.700000000000001,
-0.695000000000001,-0.690000000000001,-0.685,-0.68,-0.675,-0.67,-0.665,
-0.66,-0.655,-0.65,-0.645,-0.64,-0.635,-0.63,-0.625,-0.62,-0.615,-0.61,
-0.605,-0.6,-0.595,-0.59,-0.585,-0.58,-0.575,-0.57,-0.565,-0.56,-0.555,
-0.55,-0.545,-0.54,-0.535,-0.53,-0.525,-0.52,-0.515,-0.51,-0.505,-0.5,-0.495,
-0.49,-0.485,-0.48,-0.475,-0.47,-0.465,-0.46,-0.455,-0.45,-0.445,-0.44,
-0.435,-0.43,-0.425,-0.42,-0.415,-0.41,-0.405,-0.4,-0.395,-0.39,-0.385,
-0.38,-0.375,-0.37,-0.365,-0.36,-0.355,-0.35,-0.345,-0.34,-0.335,-0.33,
-0.325,-0.32,-0.315,-0.31,-0.305,-0.3,-0.295,-0.29,-0.285,-0.28,-0.275,
-0.27,-0.265,-0.26,-0.255,-0.25,-0.245,-0.24,-0.235,-0.23,-0.225,-0.22,
-0.215,-0.21,-0.205,-0.2,-0.195,-0.19,-0.185,-0.18,-0.175,-0.17,-0.165,
-0.16,-0.155,-0.15,-0.145,-0.14,-0.135,-0.13,-0.125,-0.12,-0.115,-0.11,
-0.105,-0.1,-0.095,-0.09,-0.085,-0.08,-0.075,-0.07,-0.065,-0.06,-0.055,
-0.05,-0.045,-0.04,-0.035,-0.03,-0.025,-0.02,-0.015,-0.01,-0.005,0.),(0.,
1.2),.UNSPECIFIED.)
GEOMETRIC_REPRESENTATION_ITEM()
RATIONAL_B_SPLINE_SURFACE(((1.,1.),(1.,1.),(1.,1.),(1.,1.),(1.,1.),(1.,
1.),(1.,1.),(1.,1.),(1.,1.),(1.,1.),(1.,1.),(1.,1.),(1.,1.),(1.,1.),(1.,
1.),(1.,1.),(1.,1.),(1.,1.),(1.,1.),(1.,1.),(1.,1.),(1.,1.),(1.,1.),(1.,
1.),(1.,1.),(1.,1.),(1.,1.),(1.,1.),(1.,1.),(1.,1.),(1.,1.),(1.,1.),(1.,
1.),(1.,1.),(1.,1.),(1.,1.),(1.,1.),(1.,1.),(1.,1.),(1.,1.),(1.,1.),(1.,
1.),(1.,1.),(1.,1.),(1.,1.),(1.,1.),(1.,1.),(1.,1.),(1.,1.),(1.,1.),(1.,
1.),(1.,1.),(1.,1.),(1.,1.),(1.,1.),(1.,1.),(1.,1.),(1.,1.),(1.,1.),(1.,
1.),(1.,1.),(1.,1.),(1.,1.),(1.,1.),(1.,1.),(1.,1.),(1.,1.),(1.,1.),(1.,
1.),(1.,1.),(1.,1.),(1.,1.),(1.,1.),(1.,1.),(1.,1.),(1.,1.),(1.,1.),(1.,
1.),(1.,1.),(1.,1.),(1.,1.),(1.,1.),(1.,1.),(1.,1.),(1.,1.),(1.,1.),(1.,
1.),(1.,1.),(1.,1.),(1.,1.),(1.,1.),(1.,1.),(1.,1.),(1.,1.),(1.,1.),(1.,
1.),(1.,1.),(1.,1.),(1.,1.),(1.,1.),(1.,1.),(1.,1.),(1.,1.),(1.,1.),(1.,
1.),(1.,1.),(1.,1.),(1.,1.),(1.,1.),(1.,1.),(1.,1.),(1.,1.),(1.,1.),(1.,
1.),(1.,1.),(1.,1.),(1.,1.),(1.,1.),(1.,1.),(1.,1.),(1.,1.),(1.,1.),(1.,
1.),(1.,1.),(1.,1.),(1.,1.),(1.,1.),(1.,1.),(1.,1.),(1.,1.),(1.,1.),(1.,
1.),(1.,1.),(1.,1.),(1.,1.),(1.,1.),(1.,1.),(1.,1.),(1.,1.),(1.,1.),(1.,
1.),(1.,1.),(1.,1.),(1.,1.),(1.,1.),(1.,1.),(1.,1.),(1.,1.),(1.,1.),(1.,
1.),(1.,1.),(1.,1.),(1.,1.),(1.,1.),(1.,1.),(1.,1.),(1.,1.),(1.,1.),(1.,
1.),(1.,1.),(1.,1.),(1.,1.),(1.,1.),(1.,1.),(1.,1.),(1.,1.),(1.,1.),(1.,
1.),(1.,1.),(1.,1.),(1.,1.),(1.,1.),(1.,1.),(1.,1.),(1.,1.),(1.,1.),(1.,
1.),(1.,1.),(1.,1.),(1.,1.),(1.,1.),(1.,1.),(1.,1.),(1.,1.),(1.,1.),(1.,
1.),(1.,1.),(1.,1.),(1.,1.),(1.,1.),(1.,1.),(1.,1.),(1.,1.),(1.,1.),(1.,
1.),(1.,1.),(1.,1.),(1.,1.),(1.,1.),(1.,1.),(1.,1.),(1.,1.),(1.,1.),(1.,
1.),(1.,1.)))
REPRESENTATION_ITEM('')
SURFACE()
);
#999=(
BOUNDED_SURFACE()
B_SPLINE_SURFACE(5,1,((#152237,#152238),(#152239,#152240),(#152241,#152242),
(#152243,#152244),(#152245,#152246),(#152247,#152248),(#152249,#152250),
(#152251,#152252),(#152253,#152254),(#152255,#152256),(#152257,#152258),
(#152259,#152260),(#152261,#152262),(#152263,#152264),(#152265,#152266),
(#152267,#152268),(#152269,#152270),(#152271,#152272),(#152273,#152274),
(#152275,#152276),(#152277,#152278),(#152279,#152280),(#152281,#152282),
(#152283,#152284),(#152285,#152286),(#152287,#152288),(#152289,#152290),
(#152291,#152292),(#152293,#152294),(#152295,#152296),(#152297,#152298),
(#152299,#152300),(#152301,#152302),(#152303,#152304),(#152305,#152306),
(#152307,#152308),(#152309,#152310),(#152311,#152312),(#152313,#152314),
(#152315,#152316),(#152317,#152318),(#152319,#152320),(#152321,#152322),
(#152323,#152324),(#152325,#152326),(#152327,#152328),(#152329,#152330),
(#152331,#152332),(#152333,#152334),(#152335,#152336),(#152337,#152338),
(#152339,#152340),(#152341,#152342),(#152343,#152344),(#152345,#152346),
(#152347,#152348),(#152349,#152350),(#152351,#152352),(#152353,#152354),
(#152355,#152356),(#152357,#152358),(#152359,#152360),(#152361,#152362),
(#152363,#152364),(#152365,#152366),(#152367,#152368),(#152369,#152370),
(#152371,#152372),(#152373,#152374),(#152375,#152376),(#152377,#152378),
(#152379,#152380),(#152381,#152382),(#152383,#152384),(#152385,#152386),
(#152387,#152388),(#152389,#152390),(#152391,#152392),(#152393,#152394),
(#152395,#152396),(#152397,#152398),(#152399,#152400),(#152401,#152402),
(#152403,#152404),(#152405,#152406),(#152407,#152408),(#152409,#152410),
(#152411,#152412),(#152413,#152414),(#152415,#152416),(#152417,#152418),
(#152419,#152420),(#152421,#152422),(#152423,#152424),(#152425,#152426),
(#152427,#152428),(#152429,#152430),(#152431,#152432),(#152433,#152434),
(#152435,#152436),(#152437,#152438),(#152439,#152440),(#152441,#152442),
(#152443,#152444),(#152445,#152446),(#152447,#152448),(#152449,#152450),
(#152451,#152452),(#152453,#152454),(#152455,#152456),(#152457,#152458),
(#152459,#152460),(#152461,#152462),(#152463,#152464),(#152465,#152466),
(#152467,#152468),(#152469,#152470),(#152471,#152472),(#152473,#152474),
(#152475,#152476),(#152477,#152478),(#152479,#152480),(#152481,#152482),
(#152483,#152484),(#152485,#152486),(#152487,#152488),(#152489,#152490),
(#152491,#152492),(#152493,#152494),(#152495,#152496),(#152497,#152498),
(#152499,#152500),(#152501,#152502),(#152503,#152504),(#152505,#152506),
(#152507,#152508),(#152509,#152510),(#152511,#152512),(#152513,#152514),
(#152515,#152516),(#152517,#152518),(#152519,#152520),(#152521,#152522),
(#152523,#152524),(#152525,#152526),(#152527,#152528),(#152529,#152530),
(#152531,#152532),(#152533,#152534),(#152535,#152536),(#152537,#152538),
(#152539,#152540),(#152541,#152542),(#152543,#152544),(#152545,#152546),
(#152547,#152548),(#152549,#152550),(#152551,#152552),(#152553,#152554),
(#152555,#152556),(#152557,#152558),(#152559,#152560),(#152561,#152562),
(#152563,#152564),(#152565,#152566),(#152567,#152568),(#152569,#152570),
(#152571,#152572),(#152573,#152574),(#152575,#152576),(#152577,#152578),
(#152579,#152580),(#152581,#152582),(#152583,#152584),(#152585,#152586),
(#152587,#152588),(#152589,#152590),(#152591,#152592),(#152593,#152594),
(#152595,#152596),(#152597,#152598),(#152599,#152600),(#152601,#152602),
(#152603,#152604),(#152605,#152606),(#152607,#152608),(#152609,#152610),
(#152611,#152612),(#152613,#152614),(#152615,#152616),(#152617,#152618),
(#152619,#152620),(#152621,#152622),(#152623,#152624),(#152625,#152626),
(#152627,#152628),(#152629,#152630),(#152631,#152632),(#152633,#152634),
(#152635,#152636),(#152637,#152638),(#152639,#152640),(#152641,#152642),
(#152643,#152644),(#152645,#152646)),.UNSPECIFIED.,.F.,.F.,.F.)
B_SPLINE_SURFACE_WITH_KNOTS((6,1,1,1,1,1,1,1,1,1,1,1,1,1,1,1,1,1,1,1,1,
1,1,1,1,1,1,1,1,1,1,1,1,1,1,1,1,1,1,1,1,1,1,1,1,1,1,1,1,1,1,1,1,1,1,1,1,
1,1,1,1,1,1,1,1,1,1,1,1,1,1,1,1,1,1,1,1,1,1,1,1,1,1,1,1,1,1,1,1,1,1,1,1,
1,1,1,1,1,1,1,1,1,1,1,1,1,1,1,1,1,1,1,1,1,1,1,1,1,1,1,1,1,1,1,1,1,1,1,1,
1,1,1,1,1,1,1,1,1,1,1,1,1,1,1,1,1,1,1,1,1,1,1,1,1,1,1,1,1,1,1,1,1,1,1,1,
1,1,1,1,1,1,1,1,1,1,1,1,1,1,1,1,1,1,1,1,1,1,1,1,1,1,1,1,1,1,1,1,1,1,1,6),
(2,2),(-1.,-0.995000000000001,-0.990000000000001,-0.985000000000001,-0.980000000000001,
-0.975000000000001,-0.970000000000001,-0.965000000000001,-0.960000000000001,
-0.955000000000001,-0.950000000000001,-0.945000000000001,-0.940000000000001,
-0.935000000000001,-0.930000000000001,-0.925000000000001,-0.920000000000001,
-0.915000000000001,-0.910000000000001,-0.905000000000001,-0.900000000000001,
-0.895000000000001,-0.890000000000001,-0.885000000000001,-0.880000000000001,
-0.875000000000001,-0.870000000000001,-0.865000000000001,-0.860000000000001,
-0.855000000000001,-0.850000000000001,-0.845000000000001,-0.840000000000001,
-0.835000000000001,-0.830000000000001,-0.825000000000001,-0.820000000000001,
-0.815000000000001,-0.810000000000001,-0.805000000000001,-0.800000000000001,
-0.795000000000001,-0.790000000000001,-0.785000000000001,-0.780000000000001,
-0.775000000000001,-0.770000000000001,-0.765000000000001,-0.760000000000001,
-0.755000000000001,-0.750000000000001,-0.745000000000001,-0.740000000000001,
-0.735000000000001,-0.730000000000001,-0.725000000000001,-0.720000000000001,
-0.715000000000001,-0.710000000000001,-0.705000000000001,-0.700000000000001,
-0.695000000000001,-0.690000000000001,-0.685,-0.68,-0.675,-0.67,-0.665,
-0.66,-0.655,-0.65,-0.645,-0.64,-0.635,-0.63,-0.625,-0.62,-0.615,-0.61,
-0.605,-0.6,-0.595,-0.59,-0.585,-0.58,-0.575,-0.57,-0.565,-0.56,-0.555,
-0.55,-0.545,-0.54,-0.535,-0.53,-0.525,-0.52,-0.515,-0.51,-0.505,-0.5,-0.495,
-0.49,-0.485,-0.48,-0.475,-0.47,-0.465,-0.46,-0.455,-0.45,-0.445,-0.44,
-0.435,-0.43,-0.425,-0.42,-0.415,-0.41,-0.405,-0.4,-0.395,-0.39,-0.385,
-0.38,-0.375,-0.37,-0.365,-0.36,-0.355,-0.35,-0.345,-0.34,-0.335,-0.33,
-0.325,-0.32,-0.315,-0.31,-0.305,-0.3,-0.295,-0.29,-0.285,-0.28,-0.275,
-0.27,-0.265,-0.26,-0.255,-0.25,-0.245,-0.24,-0.235,-0.23,-0.225,-0.22,
-0.215,-0.21,-0.205,-0.2,-0.195,-0.19,-0.185,-0.18,-0.175,-0.17,-0.165,
-0.16,-0.155,-0.15,-0.145,-0.14,-0.135,-0.13,-0.125,-0.12,-0.115,-0.11,
-0.105,-0.1,-0.095,-0.09,-0.085,-0.08,-0.075,-0.07,-0.065,-0.06,-0.055,
-0.05,-0.045,-0.04,-0.035,-0.03,-0.025,-0.02,-0.015,-0.01,-0.005,0.),(0.,
1.2),.UNSPECIFIED.)
GEOMETRIC_REPRESENTATION_ITEM()
RATIONAL_B_SPLINE_SURFACE(((1.,1.),(1.,1.),(1.,1.),(1.,1.),(1.,1.),(1.,
1.),(1.,1.),(1.,1.),(1.,1.),(1.,1.),(1.,1.),(1.,1.),(1.,1.),(1.,1.),(1.,
1.),(1.,1.),(1.,1.),(1.,1.),(1.,1.),(1.,1.),(1.,1.),(1.,1.),(1.,1.),(1.,
1.),(1.,1.),(1.,1.),(1.,1.),(1.,1.),(1.,1.),(1.,1.),(1.,1.),(1.,1.),(1.,
1.),(1.,1.),(1.,1.),(1.,1.),(1.,1.),(1.,1.),(1.,1.),(1.,1.),(1.,1.),(1.,
1.),(1.,1.),(1.,1.),(1.,1.),(1.,1.),(1.,1.),(1.,1.),(1.,1.),(1.,1.),(1.,
1.),(1.,1.),(1.,1.),(1.,1.),(1.,1.),(1.,1.),(1.,1.),(1.,1.),(1.,1.),(1.,
1.),(1.,1.),(1.,1.),(1.,1.),(1.,1.),(1.,1.),(1.,1.),(1.,1.),(1.,1.),(1.,
1.),(1.,1.),(1.,1.),(1.,1.),(1.,1.),(1.,1.),(1.,1.),(1.,1.),(1.,1.),(1.,
1.),(1.,1.),(1.,1.),(1.,1.),(1.,1.),(1.,1.),(1.,1.),(1.,1.),(1.,1.),(1.,
1.),(1.,1.),(1.,1.),(1.,1.),(1.,1.),(1.,1.),(1.,1.),(1.,1.),(1.,1.),(1.,
1.),(1.,1.),(1.,1.),(1.,1.),(1.,1.),(1.,1.),(1.,1.),(1.,1.),(1.,1.),(1.,
1.),(1.,1.),(1.,1.),(1.,1.),(1.,1.),(1.,1.),(1.,1.),(1.,1.),(1.,1.),(1.,
1.),(1.,1.),(1.,1.),(1.,1.),(1.,1.),(1.,1.),(1.,1.),(1.,1.),(1.,1.),(1.,
1.),(1.,1.),(1.,1.),(1.,1.),(1.,1.),(1.,1.),(1.,1.),(1.,1.),(1.,1.),(1.,
1.),(1.,1.),(1.,1.),(1.,1.),(1.,1.),(1.,1.),(1.,1.),(1.,1.),(1.,1.),(1.,
1.),(1.,1.),(1.,1.),(1.,1.),(1.,1.),(1.,1.),(1.,1.),(1.,1.),(1.,1.),(1.,
1.),(1.,1.),(1.,1.),(1.,1.),(1.,1.),(1.,1.),(1.,1.),(1.,1.),(1.,1.),(1.,
1.),(1.,1.),(1.,1.),(1.,1.),(1.,1.),(1.,1.),(1.,1.),(1.,1.),(1.,1.),(1.,
1.),(1.,1.),(1.,1.),(1.,1.),(1.,1.),(1.,1.),(1.,1.),(1.,1.),(1.,1.),(1.,
1.),(1.,1.),(1.,1.),(1.,1.),(1.,1.),(1.,1.),(1.,1.),(1.,1.),(1.,1.),(1.,
1.),(1.,1.),(1.,1.),(1.,1.),(1.,1.),(1.,1.),(1.,1.),(1.,1.),(1.,1.),(1.,
1.),(1.,1.),(1.,1.),(1.,1.),(1.,1.),(1.,1.),(1.,1.),(1.,1.),(1.,1.),(1.,
1.),(1.,1.)))
REPRESENTATION_ITEM('')
SURFACE()
);
#1000=(
BOUNDED_SURFACE()
B_SPLINE_SURFACE(5,1,((#153038,#153039),(#153040,#153041),(#153042,#153043),
(#153044,#153045),(#153046,#153047),(#153048,#153049),(#153050,#153051),
(#153052,#153053),(#153054,#153055),(#153056,#153057),(#153058,#153059),
(#153060,#153061),(#153062,#153063),(#153064,#153065),(#153066,#153067),
(#153068,#153069),(#153070,#153071),(#153072,#153073),(#153074,#153075),
(#153076,#153077),(#153078,#153079),(#153080,#153081),(#153082,#153083),
(#153084,#153085),(#153086,#153087),(#153088,#153089),(#153090,#153091),
(#153092,#153093),(#153094,#153095),(#153096,#153097),(#153098,#153099),
(#153100,#153101),(#153102,#153103),(#153104,#153105),(#153106,#153107),
(#153108,#153109),(#153110,#153111),(#153112,#153113),(#153114,#153115),
(#153116,#153117),(#153118,#153119),(#153120,#153121),(#153122,#153123),
(#153124,#153125),(#153126,#153127),(#153128,#153129),(#153130,#153131),
(#153132,#153133),(#153134,#153135),(#153136,#153137),(#153138,#153139),
(#153140,#153141),(#153142,#153143),(#153144,#153145),(#153146,#153147),
(#153148,#153149),(#153150,#153151),(#153152,#153153),(#153154,#153155),
(#153156,#153157),(#153158,#153159),(#153160,#153161),(#153162,#153163),
(#153164,#153165),(#153166,#153167),(#153168,#153169),(#153170,#153171),
(#153172,#153173),(#153174,#153175),(#153176,#153177),(#153178,#153179),
(#153180,#153181),(#153182,#153183),(#153184,#153185),(#153186,#153187),
(#153188,#153189),(#153190,#153191),(#153192,#153193),(#153194,#153195),
(#153196,#153197),(#153198,#153199),(#153200,#153201),(#153202,#153203),
(#153204,#153205),(#153206,#153207),(#153208,#153209),(#153210,#153211),
(#153212,#153213),(#153214,#153215),(#153216,#153217),(#153218,#153219),
(#153220,#153221),(#153222,#153223),(#153224,#153225),(#153226,#153227),
(#153228,#153229),(#153230,#153231),(#153232,#153233),(#153234,#153235),
(#153236,#153237),(#153238,#153239),(#153240,#153241),(#153242,#153243),
(#153244,#153245),(#153246,#153247),(#153248,#153249),(#153250,#153251),
(#153252,#153253),(#153254,#153255),(#153256,#153257),(#153258,#153259),
(#153260,#153261),(#153262,#153263),(#153264,#153265),(#153266,#153267),
(#153268,#153269),(#153270,#153271),(#153272,#153273),(#153274,#153275),
(#153276,#153277),(#153278,#153279),(#153280,#153281),(#153282,#153283),
(#153284,#153285),(#153286,#153287),(#153288,#153289),(#153290,#153291),
(#153292,#153293),(#153294,#153295),(#153296,#153297),(#153298,#153299),
(#153300,#153301),(#153302,#153303),(#153304,#153305),(#153306,#153307),
(#153308,#153309),(#153310,#153311),(#153312,#153313),(#153314,#153315),
(#153316,#153317),(#153318,#153319),(#153320,#153321),(#153322,#153323),
(#153324,#153325),(#153326,#153327),(#153328,#153329),(#153330,#153331),
(#153332,#153333),(#153334,#153335),(#153336,#153337),(#153338,#153339),
(#153340,#153341),(#153342,#153343),(#153344,#153345),(#153346,#153347),
(#153348,#153349),(#153350,#153351),(#153352,#153353),(#153354,#153355),
(#153356,#153357),(#153358,#153359),(#153360,#153361),(#153362,#153363),
(#153364,#153365),(#153366,#153367),(#153368,#153369),(#153370,#153371),
(#153372,#153373),(#153374,#153375),(#153376,#153377),(#153378,#153379),
(#153380,#153381),(#153382,#153383),(#153384,#153385),(#153386,#153387),
(#153388,#153389),(#153390,#153391),(#153392,#153393),(#153394,#153395),
(#153396,#153397),(#153398,#153399),(#153400,#153401),(#153402,#153403),
(#153404,#153405),(#153406,#153407),(#153408,#153409),(#153410,#153411),
(#153412,#153413),(#153414,#153415),(#153416,#153417),(#153418,#153419),
(#153420,#153421),(#153422,#153423),(#153424,#153425),(#153426,#153427),
(#153428,#153429),(#153430,#153431),(#153432,#153433),(#153434,#153435),
(#153436,#153437),(#153438,#153439),(#153440,#153441),(#153442,#153443),
(#153444,#153445),(#153446,#153447)),.UNSPECIFIED.,.F.,.F.,.F.)
B_SPLINE_SURFACE_WITH_KNOTS((6,1,1,1,1,1,1,1,1,1,1,1,1,1,1,1,1,1,1,1,1,
1,1,1,1,1,1,1,1,1,1,1,1,1,1,1,1,1,1,1,1,1,1,1,1,1,1,1,1,1,1,1,1,1,1,1,1,
1,1,1,1,1,1,1,1,1,1,1,1,1,1,1,1,1,1,1,1,1,1,1,1,1,1,1,1,1,1,1,1,1,1,1,1,
1,1,1,1,1,1,1,1,1,1,1,1,1,1,1,1,1,1,1,1,1,1,1,1,1,1,1,1,1,1,1,1,1,1,1,1,
1,1,1,1,1,1,1,1,1,1,1,1,1,1,1,1,1,1,1,1,1,1,1,1,1,1,1,1,1,1,1,1,1,1,1,1,
1,1,1,1,1,1,1,1,1,1,1,1,1,1,1,1,1,1,1,1,1,1,1,1,1,1,1,1,1,1,1,1,1,1,1,6),
(2,2),(-1.,-0.995000000000001,-0.990000000000001,-0.985000000000001,-0.980000000000001,
-0.975000000000001,-0.970000000000001,-0.965000000000001,-0.960000000000001,
-0.955000000000001,-0.950000000000001,-0.945000000000001,-0.940000000000001,
-0.935000000000001,-0.930000000000001,-0.925000000000001,-0.920000000000001,
-0.915000000000001,-0.910000000000001,-0.905000000000001,-0.900000000000001,
-0.895000000000001,-0.890000000000001,-0.885000000000001,-0.880000000000001,
-0.875000000000001,-0.870000000000001,-0.865000000000001,-0.860000000000001,
-0.855000000000001,-0.850000000000001,-0.845000000000001,-0.840000000000001,
-0.835000000000001,-0.830000000000001,-0.825000000000001,-0.820000000000001,
-0.815000000000001,-0.810000000000001,-0.805000000000001,-0.800000000000001,
-0.795000000000001,-0.790000000000001,-0.785000000000001,-0.780000000000001,
-0.775000000000001,-0.770000000000001,-0.765000000000001,-0.760000000000001,
-0.755000000000001,-0.750000000000001,-0.745000000000001,-0.740000000000001,
-0.735000000000001,-0.730000000000001,-0.725000000000001,-0.720000000000001,
-0.715000000000001,-0.710000000000001,-0.705000000000001,-0.700000000000001,
-0.695000000000001,-0.690000000000001,-0.685,-0.68,-0.675,-0.67,-0.665,
-0.66,-0.655,-0.65,-0.645,-0.64,-0.635,-0.63,-0.625,-0.62,-0.615,-0.61,
-0.605,-0.6,-0.595,-0.59,-0.585,-0.58,-0.575,-0.57,-0.565,-0.56,-0.555,
-0.55,-0.545,-0.54,-0.535,-0.53,-0.525,-0.52,-0.515,-0.51,-0.505,-0.5,-0.495,
-0.49,-0.485,-0.48,-0.475,-0.47,-0.465,-0.46,-0.455,-0.45,-0.445,-0.44,
-0.435,-0.43,-0.425,-0.42,-0.415,-0.41,-0.405,-0.4,-0.395,-0.39,-0.385,
-0.38,-0.375,-0.37,-0.365,-0.36,-0.355,-0.35,-0.345,-0.34,-0.335,-0.33,
-0.325,-0.32,-0.315,-0.31,-0.305,-0.3,-0.295,-0.29,-0.285,-0.28,-0.275,
-0.27,-0.265,-0.26,-0.255,-0.25,-0.245,-0.24,-0.235,-0.23,-0.225,-0.22,
-0.215,-0.21,-0.205,-0.2,-0.195,-0.19,-0.185,-0.18,-0.175,-0.17,-0.165,
-0.16,-0.155,-0.15,-0.145,-0.14,-0.135,-0.13,-0.125,-0.12,-0.115,-0.11,
-0.105,-0.1,-0.095,-0.09,-0.085,-0.08,-0.075,-0.07,-0.065,-0.06,-0.055,
-0.05,-0.045,-0.04,-0.035,-0.03,-0.025,-0.02,-0.015,-0.01,-0.005,0.),(0.,
1.2),.UNSPECIFIED.)
GEOMETRIC_REPRESENTATION_ITEM()
RATIONAL_B_SPLINE_SURFACE(((1.,1.),(1.,1.),(1.,1.),(1.,1.),(1.,1.),(1.,
1.),(1.,1.),(1.,1.),(1.,1.),(1.,1.),(1.,1.),(1.,1.),(1.,1.),(1.,1.),(1.,
1.),(1.,1.),(1.,1.),(1.,1.),(1.,1.),(1.,1.),(1.,1.),(1.,1.),(1.,1.),(1.,
1.),(1.,1.),(1.,1.),(1.,1.),(1.,1.),(1.,1.),(1.,1.),(1.,1.),(1.,1.),(1.,
1.),(1.,1.),(1.,1.),(1.,1.),(1.,1.),(1.,1.),(1.,1.),(1.,1.),(1.,1.),(1.,
1.),(1.,1.),(1.,1.),(1.,1.),(1.,1.),(1.,1.),(1.,1.),(1.,1.),(1.,1.),(1.,
1.),(1.,1.),(1.,1.),(1.,1.),(1.,1.),(1.,1.),(1.,1.),(1.,1.),(1.,1.),(1.,
1.),(1.,1.),(1.,1.),(1.,1.),(1.,1.),(1.,1.),(1.,1.),(1.,1.),(1.,1.),(1.,
1.),(1.,1.),(1.,1.),(1.,1.),(1.,1.),(1.,1.),(1.,1.),(1.,1.),(1.,1.),(1.,
1.),(1.,1.),(1.,1.),(1.,1.),(1.,1.),(1.,1.),(1.,1.),(1.,1.),(1.,1.),(1.,
1.),(1.,1.),(1.,1.),(1.,1.),(1.,1.),(1.,1.),(1.,1.),(1.,1.),(1.,1.),(1.,
1.),(1.,1.),(1.,1.),(1.,1.),(1.,1.),(1.,1.),(1.,1.),(1.,1.),(1.,1.),(1.,
1.),(1.,1.),(1.,1.),(1.,1.),(1.,1.),(1.,1.),(1.,1.),(1.,1.),(1.,1.),(1.,
1.),(1.,1.),(1.,1.),(1.,1.),(1.,1.),(1.,1.),(1.,1.),(1.,1.),(1.,1.),(1.,
1.),(1.,1.),(1.,1.),(1.,1.),(1.,1.),(1.,1.),(1.,1.),(1.,1.),(1.,1.),(1.,
1.),(1.,1.),(1.,1.),(1.,1.),(1.,1.),(1.,1.),(1.,1.),(1.,1.),(1.,1.),(1.,
1.),(1.,1.),(1.,1.),(1.,1.),(1.,1.),(1.,1.),(1.,1.),(1.,1.),(1.,1.),(1.,
1.),(1.,1.),(1.,1.),(1.,1.),(1.,1.),(1.,1.),(1.,1.),(1.,1.),(1.,1.),(1.,
1.),(1.,1.),(1.,1.),(1.,1.),(1.,1.),(1.,1.),(1.,1.),(1.,1.),(1.,1.),(1.,
1.),(1.,1.),(1.,1.),(1.,1.),(1.,1.),(1.,1.),(1.,1.),(1.,1.),(1.,1.),(1.,
1.),(1.,1.),(1.,1.),(1.,1.),(1.,1.),(1.,1.),(1.,1.),(1.,1.),(1.,1.),(1.,
1.),(1.,1.),(1.,1.),(1.,1.),(1.,1.),(1.,1.),(1.,1.),(1.,1.),(1.,1.),(1.,
1.),(1.,1.),(1.,1.),(1.,1.),(1.,1.),(1.,1.),(1.,1.),(1.,1.),(1.,1.),(1.,
1.),(1.,1.)))
REPRESENTATION_ITEM('')
SURFACE()
);
#1001=(
BOUNDED_SURFACE()
B_SPLINE_SURFACE(5,1,((#153839,#153840),(#153841,#153842),(#153843,#153844),
(#153845,#153846),(#153847,#153848),(#153849,#153850),(#153851,#153852),
(#153853,#153854),(#153855,#153856),(#153857,#153858),(#153859,#153860),
(#153861,#153862),(#153863,#153864),(#153865,#153866),(#153867,#153868),
(#153869,#153870),(#153871,#153872),(#153873,#153874),(#153875,#153876),
(#153877,#153878),(#153879,#153880),(#153881,#153882),(#153883,#153884),
(#153885,#153886),(#153887,#153888),(#153889,#153890),(#153891,#153892),
(#153893,#153894),(#153895,#153896),(#153897,#153898),(#153899,#153900),
(#153901,#153902),(#153903,#153904),(#153905,#153906),(#153907,#153908),
(#153909,#153910),(#153911,#153912),(#153913,#153914),(#153915,#153916),
(#153917,#153918),(#153919,#153920),(#153921,#153922),(#153923,#153924),
(#153925,#153926),(#153927,#153928),(#153929,#153930),(#153931,#153932),
(#153933,#153934),(#153935,#153936),(#153937,#153938),(#153939,#153940),
(#153941,#153942),(#153943,#153944),(#153945,#153946),(#153947,#153948),
(#153949,#153950),(#153951,#153952),(#153953,#153954),(#153955,#153956),
(#153957,#153958),(#153959,#153960),(#153961,#153962),(#153963,#153964),
(#153965,#153966),(#153967,#153968),(#153969,#153970),(#153971,#153972),
(#153973,#153974),(#153975,#153976),(#153977,#153978),(#153979,#153980),
(#153981,#153982),(#153983,#153984),(#153985,#153986),(#153987,#153988),
(#153989,#153990),(#153991,#153992),(#153993,#153994),(#153995,#153996),
(#153997,#153998),(#153999,#154000),(#154001,#154002),(#154003,#154004),
(#154005,#154006),(#154007,#154008),(#154009,#154010),(#154011,#154012),
(#154013,#154014),(#154015,#154016),(#154017,#154018),(#154019,#154020),
(#154021,#154022),(#154023,#154024),(#154025,#154026),(#154027,#154028),
(#154029,#154030),(#154031,#154032),(#154033,#154034),(#154035,#154036),
(#154037,#154038),(#154039,#154040),(#154041,#154042),(#154043,#154044),
(#154045,#154046),(#154047,#154048),(#154049,#154050),(#154051,#154052),
(#154053,#154054),(#154055,#154056),(#154057,#154058),(#154059,#154060),
(#154061,#154062),(#154063,#154064),(#154065,#154066),(#154067,#154068),
(#154069,#154070),(#154071,#154072),(#154073,#154074),(#154075,#154076),
(#154077,#154078),(#154079,#154080),(#154081,#154082),(#154083,#154084),
(#154085,#154086),(#154087,#154088),(#154089,#154090),(#154091,#154092),
(#154093,#154094),(#154095,#154096),(#154097,#154098),(#154099,#154100),
(#154101,#154102),(#154103,#154104),(#154105,#154106),(#154107,#154108),
(#154109,#154110),(#154111,#154112),(#154113,#154114),(#154115,#154116),
(#154117,#154118),(#154119,#154120),(#154121,#154122),(#154123,#154124),
(#154125,#154126),(#154127,#154128),(#154129,#154130),(#154131,#154132),
(#154133,#154134),(#154135,#154136),(#154137,#154138),(#154139,#154140),
(#154141,#154142),(#154143,#154144),(#154145,#154146),(#154147,#154148),
(#154149,#154150),(#154151,#154152),(#154153,#154154),(#154155,#154156),
(#154157,#154158),(#154159,#154160),(#154161,#154162),(#154163,#154164),
(#154165,#154166),(#154167,#154168),(#154169,#154170),(#154171,#154172),
(#154173,#154174),(#154175,#154176),(#154177,#154178),(#154179,#154180),
(#154181,#154182),(#154183,#154184),(#154185,#154186),(#154187,#154188),
(#154189,#154190),(#154191,#154192),(#154193,#154194),(#154195,#154196),
(#154197,#154198),(#154199,#154200),(#154201,#154202),(#154203,#154204),
(#154205,#154206),(#154207,#154208),(#154209,#154210),(#154211,#154212),
(#154213,#154214),(#154215,#154216),(#154217,#154218),(#154219,#154220),
(#154221,#154222),(#154223,#154224),(#154225,#154226),(#154227,#154228),
(#154229,#154230),(#154231,#154232),(#154233,#154234),(#154235,#154236),
(#154237,#154238),(#154239,#154240),(#154241,#154242),(#154243,#154244),
(#154245,#154246),(#154247,#154248)),.UNSPECIFIED.,.F.,.F.,.F.)
B_SPLINE_SURFACE_WITH_KNOTS((6,1,1,1,1,1,1,1,1,1,1,1,1,1,1,1,1,1,1,1,1,
1,1,1,1,1,1,1,1,1,1,1,1,1,1,1,1,1,1,1,1,1,1,1,1,1,1,1,1,1,1,1,1,1,1,1,1,
1,1,1,1,1,1,1,1,1,1,1,1,1,1,1,1,1,1,1,1,1,1,1,1,1,1,1,1,1,1,1,1,1,1,1,1,
1,1,1,1,1,1,1,1,1,1,1,1,1,1,1,1,1,1,1,1,1,1,1,1,1,1,1,1,1,1,1,1,1,1,1,1,
1,1,1,1,1,1,1,1,1,1,1,1,1,1,1,1,1,1,1,1,1,1,1,1,1,1,1,1,1,1,1,1,1,1,1,1,
1,1,1,1,1,1,1,1,1,1,1,1,1,1,1,1,1,1,1,1,1,1,1,1,1,1,1,1,1,1,1,1,1,1,1,6),
(2,2),(-1.,-0.995000000000001,-0.990000000000001,-0.985000000000001,-0.980000000000001,
-0.975000000000001,-0.970000000000001,-0.965000000000001,-0.960000000000001,
-0.955000000000001,-0.950000000000001,-0.945000000000001,-0.940000000000001,
-0.935000000000001,-0.930000000000001,-0.925000000000001,-0.920000000000001,
-0.915000000000001,-0.910000000000001,-0.905000000000001,-0.900000000000001,
-0.895000000000001,-0.890000000000001,-0.885000000000001,-0.880000000000001,
-0.875000000000001,-0.870000000000001,-0.865000000000001,-0.860000000000001,
-0.855000000000001,-0.850000000000001,-0.845000000000001,-0.840000000000001,
-0.835000000000001,-0.830000000000001,-0.825000000000001,-0.820000000000001,
-0.815000000000001,-0.810000000000001,-0.805000000000001,-0.800000000000001,
-0.795000000000001,-0.790000000000001,-0.785000000000001,-0.780000000000001,
-0.775000000000001,-0.770000000000001,-0.765000000000001,-0.760000000000001,
-0.755000000000001,-0.750000000000001,-0.745000000000001,-0.740000000000001,
-0.735000000000001,-0.730000000000001,-0.725000000000001,-0.720000000000001,
-0.715000000000001,-0.710000000000001,-0.705000000000001,-0.700000000000001,
-0.695000000000001,-0.690000000000001,-0.685,-0.68,-0.675,-0.67,-0.665,
-0.66,-0.655,-0.65,-0.645,-0.64,-0.635,-0.63,-0.625,-0.62,-0.615,-0.61,
-0.605,-0.6,-0.595,-0.59,-0.585,-0.58,-0.575,-0.57,-0.565,-0.56,-0.555,
-0.55,-0.545,-0.54,-0.535,-0.53,-0.525,-0.52,-0.515,-0.51,-0.505,-0.5,-0.495,
-0.49,-0.485,-0.48,-0.475,-0.47,-0.465,-0.46,-0.455,-0.45,-0.445,-0.44,
-0.435,-0.43,-0.425,-0.42,-0.415,-0.41,-0.405,-0.4,-0.395,-0.39,-0.385,
-0.38,-0.375,-0.37,-0.365,-0.36,-0.355,-0.35,-0.345,-0.34,-0.335,-0.33,
-0.325,-0.32,-0.315,-0.31,-0.305,-0.3,-0.295,-0.29,-0.285,-0.28,-0.275,
-0.27,-0.265,-0.26,-0.255,-0.25,-0.245,-0.24,-0.235,-0.23,-0.225,-0.22,
-0.215,-0.21,-0.205,-0.2,-0.195,-0.19,-0.185,-0.18,-0.175,-0.17,-0.165,
-0.16,-0.155,-0.15,-0.145,-0.14,-0.135,-0.13,-0.125,-0.12,-0.115,-0.11,
-0.105,-0.1,-0.095,-0.09,-0.085,-0.08,-0.075,-0.07,-0.065,-0.06,-0.055,
-0.05,-0.045,-0.04,-0.035,-0.03,-0.025,-0.02,-0.015,-0.01,-0.005,0.),(0.,
1.2),.UNSPECIFIED.)
GEOMETRIC_REPRESENTATION_ITEM()
RATIONAL_B_SPLINE_SURFACE(((1.,1.),(1.,1.),(1.,1.),(1.,1.),(1.,1.),(1.,
1.),(1.,1.),(1.,1.),(1.,1.),(1.,1.),(1.,1.),(1.,1.),(1.,1.),(1.,1.),(1.,
1.),(1.,1.),(1.,1.),(1.,1.),(1.,1.),(1.,1.),(1.,1.),(1.,1.),(1.,1.),(1.,
1.),(1.,1.),(1.,1.),(1.,1.),(1.,1.),(1.,1.),(1.,1.),(1.,1.),(1.,1.),(1.,
1.),(1.,1.),(1.,1.),(1.,1.),(1.,1.),(1.,1.),(1.,1.),(1.,1.),(1.,1.),(1.,
1.),(1.,1.),(1.,1.),(1.,1.),(1.,1.),(1.,1.),(1.,1.),(1.,1.),(1.,1.),(1.,
1.),(1.,1.),(1.,1.),(1.,1.),(1.,1.),(1.,1.),(1.,1.),(1.,1.),(1.,1.),(1.,
1.),(1.,1.),(1.,1.),(1.,1.),(1.,1.),(1.,1.),(1.,1.),(1.,1.),(1.,1.),(1.,
1.),(1.,1.),(1.,1.),(1.,1.),(1.,1.),(1.,1.),(1.,1.),(1.,1.),(1.,1.),(1.,
1.),(1.,1.),(1.,1.),(1.,1.),(1.,1.),(1.,1.),(1.,1.),(1.,1.),(1.,1.),(1.,
1.),(1.,1.),(1.,1.),(1.,1.),(1.,1.),(1.,1.),(1.,1.),(1.,1.),(1.,1.),(1.,
1.),(1.,1.),(1.,1.),(1.,1.),(1.,1.),(1.,1.),(1.,1.),(1.,1.),(1.,1.),(1.,
1.),(1.,1.),(1.,1.),(1.,1.),(1.,1.),(1.,1.),(1.,1.),(1.,1.),(1.,1.),(1.,
1.),(1.,1.),(1.,1.),(1.,1.),(1.,1.),(1.,1.),(1.,1.),(1.,1.),(1.,1.),(1.,
1.),(1.,1.),(1.,1.),(1.,1.),(1.,1.),(1.,1.),(1.,1.),(1.,1.),(1.,1.),(1.,
1.),(1.,1.),(1.,1.),(1.,1.),(1.,1.),(1.,1.),(1.,1.),(1.,1.),(1.,1.),(1.,
1.),(1.,1.),(1.,1.),(1.,1.),(1.,1.),(1.,1.),(1.,1.),(1.,1.),(1.,1.),(1.,
1.),(1.,1.),(1.,1.),(1.,1.),(1.,1.),(1.,1.),(1.,1.),(1.,1.),(1.,1.),(1.,
1.),(1.,1.),(1.,1.),(1.,1.),(1.,1.),(1.,1.),(1.,1.),(1.,1.),(1.,1.),(1.,
1.),(1.,1.),(1.,1.),(1.,1.),(1.,1.),(1.,1.),(1.,1.),(1.,1.),(1.,1.),(1.,
1.),(1.,1.),(1.,1.),(1.,1.),(1.,1.),(1.,1.),(1.,1.),(1.,1.),(1.,1.),(1.,
1.),(1.,1.),(1.,1.),(1.,1.),(1.,1.),(1.,1.),(1.,1.),(1.,1.),(1.,1.),(1.,
1.),(1.,1.),(1.,1.),(1.,1.),(1.,1.),(1.,1.),(1.,1.),(1.,1.),(1.,1.),(1.,
1.),(1.,1.)))
REPRESENTATION_ITEM('')
SURFACE()
);
#1002=(
BOUNDED_SURFACE()
B_SPLINE_SURFACE(5,1,((#154640,#154641),(#154642,#154643),(#154644,#154645),
(#154646,#154647),(#154648,#154649),(#154650,#154651),(#154652,#154653),
(#154654,#154655),(#154656,#154657),(#154658,#154659),(#154660,#154661),
(#154662,#154663),(#154664,#154665),(#154666,#154667),(#154668,#154669),
(#154670,#154671),(#154672,#154673),(#154674,#154675),(#154676,#154677),
(#154678,#154679),(#154680,#154681),(#154682,#154683),(#154684,#154685),
(#154686,#154687),(#154688,#154689),(#154690,#154691),(#154692,#154693),
(#154694,#154695),(#154696,#154697),(#154698,#154699),(#154700,#154701),
(#154702,#154703),(#154704,#154705),(#154706,#154707),(#154708,#154709),
(#154710,#154711),(#154712,#154713),(#154714,#154715),(#154716,#154717),
(#154718,#154719),(#154720,#154721),(#154722,#154723),(#154724,#154725),
(#154726,#154727),(#154728,#154729),(#154730,#154731),(#154732,#154733),
(#154734,#154735),(#154736,#154737),(#154738,#154739),(#154740,#154741),
(#154742,#154743),(#154744,#154745),(#154746,#154747),(#154748,#154749),
(#154750,#154751),(#154752,#154753),(#154754,#154755),(#154756,#154757),
(#154758,#154759),(#154760,#154761),(#154762,#154763),(#154764,#154765),
(#154766,#154767),(#154768,#154769),(#154770,#154771),(#154772,#154773),
(#154774,#154775),(#154776,#154777),(#154778,#154779),(#154780,#154781),
(#154782,#154783),(#154784,#154785),(#154786,#154787),(#154788,#154789),
(#154790,#154791),(#154792,#154793),(#154794,#154795),(#154796,#154797),
(#154798,#154799),(#154800,#154801),(#154802,#154803),(#154804,#154805),
(#154806,#154807),(#154808,#154809),(#154810,#154811),(#154812,#154813),
(#154814,#154815),(#154816,#154817),(#154818,#154819),(#154820,#154821),
(#154822,#154823),(#154824,#154825),(#154826,#154827),(#154828,#154829),
(#154830,#154831),(#154832,#154833),(#154834,#154835),(#154836,#154837),
(#154838,#154839),(#154840,#154841),(#154842,#154843),(#154844,#154845),
(#154846,#154847),(#154848,#154849),(#154850,#154851),(#154852,#154853),
(#154854,#154855),(#154856,#154857),(#154858,#154859),(#154860,#154861),
(#154862,#154863),(#154864,#154865),(#154866,#154867),(#154868,#154869),
(#154870,#154871),(#154872,#154873),(#154874,#154875),(#154876,#154877),
(#154878,#154879),(#154880,#154881),(#154882,#154883),(#154884,#154885),
(#154886,#154887),(#154888,#154889),(#154890,#154891),(#154892,#154893),
(#154894,#154895),(#154896,#154897),(#154898,#154899),(#154900,#154901),
(#154902,#154903),(#154904,#154905),(#154906,#154907),(#154908,#154909),
(#154910,#154911),(#154912,#154913),(#154914,#154915),(#154916,#154917),
(#154918,#154919),(#154920,#154921),(#154922,#154923),(#154924,#154925),
(#154926,#154927),(#154928,#154929),(#154930,#154931),(#154932,#154933),
(#154934,#154935),(#154936,#154937),(#154938,#154939),(#154940,#154941),
(#154942,#154943),(#154944,#154945),(#154946,#154947),(#154948,#154949),
(#154950,#154951),(#154952,#154953),(#154954,#154955),(#154956,#154957),
(#154958,#154959),(#154960,#154961),(#154962,#154963),(#154964,#154965),
(#154966,#154967),(#154968,#154969),(#154970,#154971),(#154972,#154973),
(#154974,#154975),(#154976,#154977),(#154978,#154979),(#154980,#154981),
(#154982,#154983),(#154984,#154985),(#154986,#154987),(#154988,#154989),
(#154990,#154991),(#154992,#154993),(#154994,#154995),(#154996,#154997),
(#154998,#154999),(#155000,#155001),(#155002,#155003),(#155004,#155005),
(#155006,#155007),(#155008,#155009),(#155010,#155011),(#155012,#155013),
(#155014,#155015),(#155016,#155017),(#155018,#155019),(#155020,#155021),
(#155022,#155023),(#155024,#155025),(#155026,#155027),(#155028,#155029),
(#155030,#155031),(#155032,#155033),(#155034,#155035),(#155036,#155037),
(#155038,#155039),(#155040,#155041),(#155042,#155043),(#155044,#155045),
(#155046,#155047),(#155048,#155049)),.UNSPECIFIED.,.F.,.F.,.F.)
B_SPLINE_SURFACE_WITH_KNOTS((6,1,1,1,1,1,1,1,1,1,1,1,1,1,1,1,1,1,1,1,1,
1,1,1,1,1,1,1,1,1,1,1,1,1,1,1,1,1,1,1,1,1,1,1,1,1,1,1,1,1,1,1,1,1,1,1,1,
1,1,1,1,1,1,1,1,1,1,1,1,1,1,1,1,1,1,1,1,1,1,1,1,1,1,1,1,1,1,1,1,1,1,1,1,
1,1,1,1,1,1,1,1,1,1,1,1,1,1,1,1,1,1,1,1,1,1,1,1,1,1,1,1,1,1,1,1,1,1,1,1,
1,1,1,1,1,1,1,1,1,1,1,1,1,1,1,1,1,1,1,1,1,1,1,1,1,1,1,1,1,1,1,1,1,1,1,1,
1,1,1,1,1,1,1,1,1,1,1,1,1,1,1,1,1,1,1,1,1,1,1,1,1,1,1,1,1,1,1,1,1,1,1,6),
(2,2),(-1.,-0.995000000000001,-0.990000000000001,-0.985000000000001,-0.980000000000001,
-0.975000000000001,-0.970000000000001,-0.965000000000001,-0.960000000000001,
-0.955000000000001,-0.950000000000001,-0.945000000000001,-0.940000000000001,
-0.935000000000001,-0.930000000000001,-0.925000000000001,-0.920000000000001,
-0.915000000000001,-0.910000000000001,-0.905000000000001,-0.900000000000001,
-0.895000000000001,-0.890000000000001,-0.885000000000001,-0.880000000000001,
-0.875000000000001,-0.870000000000001,-0.865000000000001,-0.860000000000001,
-0.855000000000001,-0.850000000000001,-0.845000000000001,-0.840000000000001,
-0.835000000000001,-0.830000000000001,-0.825000000000001,-0.820000000000001,
-0.815000000000001,-0.810000000000001,-0.805000000000001,-0.800000000000001,
-0.795000000000001,-0.790000000000001,-0.785000000000001,-0.780000000000001,
-0.775000000000001,-0.770000000000001,-0.765000000000001,-0.760000000000001,
-0.755000000000001,-0.750000000000001,-0.745000000000001,-0.740000000000001,
-0.735000000000001,-0.730000000000001,-0.725000000000001,-0.720000000000001,
-0.715000000000001,-0.710000000000001,-0.705000000000001,-0.700000000000001,
-0.695000000000001,-0.690000000000001,-0.685,-0.68,-0.675,-0.67,-0.665,
-0.66,-0.655,-0.65,-0.645,-0.64,-0.635,-0.63,-0.625,-0.62,-0.615,-0.61,
-0.605,-0.6,-0.595,-0.59,-0.585,-0.58,-0.575,-0.57,-0.565,-0.56,-0.555,
-0.55,-0.545,-0.54,-0.535,-0.53,-0.525,-0.52,-0.515,-0.51,-0.505,-0.5,-0.495,
-0.49,-0.485,-0.48,-0.475,-0.47,-0.465,-0.46,-0.455,-0.45,-0.445,-0.44,
-0.435,-0.43,-0.425,-0.42,-0.415,-0.41,-0.405,-0.4,-0.395,-0.39,-0.385,
-0.38,-0.375,-0.37,-0.365,-0.36,-0.355,-0.35,-0.345,-0.34,-0.335,-0.33,
-0.325,-0.32,-0.315,-0.31,-0.305,-0.3,-0.295,-0.29,-0.285,-0.28,-0.275,
-0.27,-0.265,-0.26,-0.255,-0.25,-0.245,-0.24,-0.235,-0.23,-0.225,-0.22,
-0.215,-0.21,-0.205,-0.2,-0.195,-0.19,-0.185,-0.18,-0.175,-0.17,-0.165,
-0.16,-0.155,-0.15,-0.145,-0.14,-0.135,-0.13,-0.125,-0.12,-0.115,-0.11,
-0.105,-0.1,-0.095,-0.09,-0.085,-0.08,-0.075,-0.07,-0.065,-0.06,-0.055,
-0.05,-0.045,-0.04,-0.035,-0.03,-0.025,-0.02,-0.015,-0.01,-0.005,0.),(0.,
1.2),.UNSPECIFIED.)
GEOMETRIC_REPRESENTATION_ITEM()
RATIONAL_B_SPLINE_SURFACE(((1.,1.),(1.,1.),(1.,1.),(1.,1.),(1.,1.),(1.,
1.),(1.,1.),(1.,1.),(1.,1.),(1.,1.),(1.,1.),(1.,1.),(1.,1.),(1.,1.),(1.,
1.),(1.,1.),(1.,1.),(1.,1.),(1.,1.),(1.,1.),(1.,1.),(1.,1.),(1.,1.),(1.,
1.),(1.,1.),(1.,1.),(1.,1.),(1.,1.),(1.,1.),(1.,1.),(1.,1.),(1.,1.),(1.,
1.),(1.,1.),(1.,1.),(1.,1.),(1.,1.),(1.,1.),(1.,1.),(1.,1.),(1.,1.),(1.,
1.),(1.,1.),(1.,1.),(1.,1.),(1.,1.),(1.,1.),(1.,1.),(1.,1.),(1.,1.),(1.,
1.),(1.,1.),(1.,1.),(1.,1.),(1.,1.),(1.,1.),(1.,1.),(1.,1.),(1.,1.),(1.,
1.),(1.,1.),(1.,1.),(1.,1.),(1.,1.),(1.,1.),(1.,1.),(1.,1.),(1.,1.),(1.,
1.),(1.,1.),(1.,1.),(1.,1.),(1.,1.),(1.,1.),(1.,1.),(1.,1.),(1.,1.),(1.,
1.),(1.,1.),(1.,1.),(1.,1.),(1.,1.),(1.,1.),(1.,1.),(1.,1.),(1.,1.),(1.,
1.),(1.,1.),(1.,1.),(1.,1.),(1.,1.),(1.,1.),(1.,1.),(1.,1.),(1.,1.),(1.,
1.),(1.,1.),(1.,1.),(1.,1.),(1.,1.),(1.,1.),(1.,1.),(1.,1.),(1.,1.),(1.,
1.),(1.,1.),(1.,1.),(1.,1.),(1.,1.),(1.,1.),(1.,1.),(1.,1.),(1.,1.),(1.,
1.),(1.,1.),(1.,1.),(1.,1.),(1.,1.),(1.,1.),(1.,1.),(1.,1.),(1.,1.),(1.,
1.),(1.,1.),(1.,1.),(1.,1.),(1.,1.),(1.,1.),(1.,1.),(1.,1.),(1.,1.),(1.,
1.),(1.,1.),(1.,1.),(1.,1.),(1.,1.),(1.,1.),(1.,1.),(1.,1.),(1.,1.),(1.,
1.),(1.,1.),(1.,1.),(1.,1.),(1.,1.),(1.,1.),(1.,1.),(1.,1.),(1.,1.),(1.,
1.),(1.,1.),(1.,1.),(1.,1.),(1.,1.),(1.,1.),(1.,1.),(1.,1.),(1.,1.),(1.,
1.),(1.,1.),(1.,1.),(1.,1.),(1.,1.),(1.,1.),(1.,1.),(1.,1.),(1.,1.),(1.,
1.),(1.,1.),(1.,1.),(1.,1.),(1.,1.),(1.,1.),(1.,1.),(1.,1.),(1.,1.),(1.,
1.),(1.,1.),(1.,1.),(1.,1.),(1.,1.),(1.,1.),(1.,1.),(1.,1.),(1.,1.),(1.,
1.),(1.,1.),(1.,1.),(1.,1.),(1.,1.),(1.,1.),(1.,1.),(1.,1.),(1.,1.),(1.,
1.),(1.,1.),(1.,1.),(1.,1.),(1.,1.),(1.,1.),(1.,1.),(1.,1.),(1.,1.),(1.,
1.),(1.,1.)))
REPRESENTATION_ITEM('')
SURFACE()
);
#1003=(
BOUNDED_SURFACE()
B_SPLINE_SURFACE(5,1,((#155441,#155442),(#155443,#155444),(#155445,#155446),
(#155447,#155448),(#155449,#155450),(#155451,#155452),(#155453,#155454),
(#155455,#155456),(#155457,#155458),(#155459,#155460),(#155461,#155462),
(#155463,#155464),(#155465,#155466),(#155467,#155468),(#155469,#155470),
(#155471,#155472),(#155473,#155474),(#155475,#155476),(#155477,#155478),
(#155479,#155480),(#155481,#155482),(#155483,#155484),(#155485,#155486),
(#155487,#155488),(#155489,#155490),(#155491,#155492),(#155493,#155494),
(#155495,#155496),(#155497,#155498),(#155499,#155500),(#155501,#155502),
(#155503,#155504),(#155505,#155506),(#155507,#155508),(#155509,#155510),
(#155511,#155512),(#155513,#155514),(#155515,#155516),(#155517,#155518),
(#155519,#155520),(#155521,#155522),(#155523,#155524),(#155525,#155526),
(#155527,#155528),(#155529,#155530),(#155531,#155532),(#155533,#155534),
(#155535,#155536),(#155537,#155538),(#155539,#155540),(#155541,#155542),
(#155543,#155544),(#155545,#155546),(#155547,#155548),(#155549,#155550),
(#155551,#155552),(#155553,#155554),(#155555,#155556),(#155557,#155558),
(#155559,#155560),(#155561,#155562),(#155563,#155564),(#155565,#155566),
(#155567,#155568),(#155569,#155570),(#155571,#155572),(#155573,#155574),
(#155575,#155576),(#155577,#155578),(#155579,#155580),(#155581,#155582),
(#155583,#155584),(#155585,#155586),(#155587,#155588),(#155589,#155590),
(#155591,#155592),(#155593,#155594),(#155595,#155596),(#155597,#155598),
(#155599,#155600),(#155601,#155602),(#155603,#155604),(#155605,#155606),
(#155607,#155608),(#155609,#155610),(#155611,#155612),(#155613,#155614),
(#155615,#155616),(#155617,#155618),(#155619,#155620),(#155621,#155622),
(#155623,#155624),(#155625,#155626),(#155627,#155628),(#155629,#155630),
(#155631,#155632),(#155633,#155634),(#155635,#155636),(#155637,#155638),
(#155639,#155640),(#155641,#155642),(#155643,#155644),(#155645,#155646),
(#155647,#155648),(#155649,#155650),(#155651,#155652),(#155653,#155654),
(#155655,#155656),(#155657,#155658),(#155659,#155660),(#155661,#155662),
(#155663,#155664),(#155665,#155666),(#155667,#155668),(#155669,#155670),
(#155671,#155672),(#155673,#155674),(#155675,#155676),(#155677,#155678),
(#155679,#155680),(#155681,#155682),(#155683,#155684),(#155685,#155686),
(#155687,#155688),(#155689,#155690),(#155691,#155692),(#155693,#155694),
(#155695,#155696),(#155697,#155698),(#155699,#155700),(#155701,#155702),
(#155703,#155704),(#155705,#155706),(#155707,#155708),(#155709,#155710),
(#155711,#155712),(#155713,#155714),(#155715,#155716),(#155717,#155718),
(#155719,#155720),(#155721,#155722),(#155723,#155724),(#155725,#155726),
(#155727,#155728),(#155729,#155730),(#155731,#155732),(#155733,#155734),
(#155735,#155736),(#155737,#155738),(#155739,#155740),(#155741,#155742),
(#155743,#155744),(#155745,#155746),(#155747,#155748),(#155749,#155750),
(#155751,#155752),(#155753,#155754),(#155755,#155756),(#155757,#155758),
(#155759,#155760),(#155761,#155762),(#155763,#155764),(#155765,#155766),
(#155767,#155768),(#155769,#155770),(#155771,#155772),(#155773,#155774),
(#155775,#155776),(#155777,#155778),(#155779,#155780),(#155781,#155782),
(#155783,#155784),(#155785,#155786),(#155787,#155788),(#155789,#155790),
(#155791,#155792),(#155793,#155794),(#155795,#155796),(#155797,#155798),
(#155799,#155800),(#155801,#155802),(#155803,#155804),(#155805,#155806),
(#155807,#155808),(#155809,#155810),(#155811,#155812),(#155813,#155814),
(#155815,#155816),(#155817,#155818),(#155819,#155820),(#155821,#155822),
(#155823,#155824),(#155825,#155826),(#155827,#155828),(#155829,#155830),
(#155831,#155832),(#155833,#155834),(#155835,#155836),(#155837,#155838),
(#155839,#155840),(#155841,#155842),(#155843,#155844),(#155845,#155846),
(#155847,#155848),(#155849,#155850)),.UNSPECIFIED.,.F.,.F.,.F.)
B_SPLINE_SURFACE_WITH_KNOTS((6,1,1,1,1,1,1,1,1,1,1,1,1,1,1,1,1,1,1,1,1,
1,1,1,1,1,1,1,1,1,1,1,1,1,1,1,1,1,1,1,1,1,1,1,1,1,1,1,1,1,1,1,1,1,1,1,1,
1,1,1,1,1,1,1,1,1,1,1,1,1,1,1,1,1,1,1,1,1,1,1,1,1,1,1,1,1,1,1,1,1,1,1,1,
1,1,1,1,1,1,1,1,1,1,1,1,1,1,1,1,1,1,1,1,1,1,1,1,1,1,1,1,1,1,1,1,1,1,1,1,
1,1,1,1,1,1,1,1,1,1,1,1,1,1,1,1,1,1,1,1,1,1,1,1,1,1,1,1,1,1,1,1,1,1,1,1,
1,1,1,1,1,1,1,1,1,1,1,1,1,1,1,1,1,1,1,1,1,1,1,1,1,1,1,1,1,1,1,1,1,1,1,6),
(2,2),(-1.,-0.995000000000001,-0.990000000000001,-0.985000000000001,-0.980000000000001,
-0.975000000000001,-0.970000000000001,-0.965000000000001,-0.960000000000001,
-0.955000000000001,-0.950000000000001,-0.945000000000001,-0.940000000000001,
-0.935000000000001,-0.930000000000001,-0.925000000000001,-0.920000000000001,
-0.915000000000001,-0.910000000000001,-0.905000000000001,-0.900000000000001,
-0.895000000000001,-0.890000000000001,-0.885000000000001,-0.880000000000001,
-0.875000000000001,-0.870000000000001,-0.865000000000001,-0.860000000000001,
-0.855000000000001,-0.850000000000001,-0.845000000000001,-0.840000000000001,
-0.835000000000001,-0.830000000000001,-0.825000000000001,-0.820000000000001,
-0.815000000000001,-0.810000000000001,-0.805000000000001,-0.800000000000001,
-0.795000000000001,-0.790000000000001,-0.785000000000001,-0.780000000000001,
-0.775000000000001,-0.770000000000001,-0.765000000000001,-0.760000000000001,
-0.755000000000001,-0.750000000000001,-0.745000000000001,-0.740000000000001,
-0.735000000000001,-0.730000000000001,-0.725000000000001,-0.720000000000001,
-0.715000000000001,-0.710000000000001,-0.705000000000001,-0.700000000000001,
-0.695000000000001,-0.690000000000001,-0.685,-0.68,-0.675,-0.67,-0.665,
-0.66,-0.655,-0.65,-0.645,-0.64,-0.635,-0.63,-0.625,-0.62,-0.615,-0.61,
-0.605,-0.6,-0.595,-0.59,-0.585,-0.58,-0.575,-0.57,-0.565,-0.56,-0.555,
-0.55,-0.545,-0.54,-0.535,-0.53,-0.525,-0.52,-0.515,-0.51,-0.505,-0.5,-0.495,
-0.49,-0.485,-0.48,-0.475,-0.47,-0.465,-0.46,-0.455,-0.45,-0.445,-0.44,
-0.435,-0.43,-0.425,-0.42,-0.415,-0.41,-0.405,-0.4,-0.395,-0.39,-0.385,
-0.38,-0.375,-0.37,-0.365,-0.36,-0.355,-0.35,-0.345,-0.34,-0.335,-0.33,
-0.325,-0.32,-0.315,-0.31,-0.305,-0.3,-0.295,-0.29,-0.285,-0.28,-0.275,
-0.27,-0.265,-0.26,-0.255,-0.25,-0.245,-0.24,-0.235,-0.23,-0.225,-0.22,
-0.215,-0.21,-0.205,-0.2,-0.195,-0.19,-0.185,-0.18,-0.175,-0.17,-0.165,
-0.16,-0.155,-0.15,-0.145,-0.14,-0.135,-0.13,-0.125,-0.12,-0.115,-0.11,
-0.105,-0.1,-0.095,-0.09,-0.085,-0.08,-0.075,-0.07,-0.065,-0.06,-0.055,
-0.05,-0.045,-0.04,-0.035,-0.03,-0.025,-0.02,-0.015,-0.01,-0.005,0.),(0.,
1.2),.UNSPECIFIED.)
GEOMETRIC_REPRESENTATION_ITEM()
RATIONAL_B_SPLINE_SURFACE(((1.,1.),(1.,1.),(1.,1.),(1.,1.),(1.,1.),(1.,
1.),(1.,1.),(1.,1.),(1.,1.),(1.,1.),(1.,1.),(1.,1.),(1.,1.),(1.,1.),(1.,
1.),(1.,1.),(1.,1.),(1.,1.),(1.,1.),(1.,1.),(1.,1.),(1.,1.),(1.,1.),(1.,
1.),(1.,1.),(1.,1.),(1.,1.),(1.,1.),(1.,1.),(1.,1.),(1.,1.),(1.,1.),(1.,
1.),(1.,1.),(1.,1.),(1.,1.),(1.,1.),(1.,1.),(1.,1.),(1.,1.),(1.,1.),(1.,
1.),(1.,1.),(1.,1.),(1.,1.),(1.,1.),(1.,1.),(1.,1.),(1.,1.),(1.,1.),(1.,
1.),(1.,1.),(1.,1.),(1.,1.),(1.,1.),(1.,1.),(1.,1.),(1.,1.),(1.,1.),(1.,
1.),(1.,1.),(1.,1.),(1.,1.),(1.,1.),(1.,1.),(1.,1.),(1.,1.),(1.,1.),(1.,
1.),(1.,1.),(1.,1.),(1.,1.),(1.,1.),(1.,1.),(1.,1.),(1.,1.),(1.,1.),(1.,
1.),(1.,1.),(1.,1.),(1.,1.),(1.,1.),(1.,1.),(1.,1.),(1.,1.),(1.,1.),(1.,
1.),(1.,1.),(1.,1.),(1.,1.),(1.,1.),(1.,1.),(1.,1.),(1.,1.),(1.,1.),(1.,
1.),(1.,1.),(1.,1.),(1.,1.),(1.,1.),(1.,1.),(1.,1.),(1.,1.),(1.,1.),(1.,
1.),(1.,1.),(1.,1.),(1.,1.),(1.,1.),(1.,1.),(1.,1.),(1.,1.),(1.,1.),(1.,
1.),(1.,1.),(1.,1.),(1.,1.),(1.,1.),(1.,1.),(1.,1.),(1.,1.),(1.,1.),(1.,
1.),(1.,1.),(1.,1.),(1.,1.),(1.,1.),(1.,1.),(1.,1.),(1.,1.),(1.,1.),(1.,
1.),(1.,1.),(1.,1.),(1.,1.),(1.,1.),(1.,1.),(1.,1.),(1.,1.),(1.,1.),(1.,
1.),(1.,1.),(1.,1.),(1.,1.),(1.,1.),(1.,1.),(1.,1.),(1.,1.),(1.,1.),(1.,
1.),(1.,1.),(1.,1.),(1.,1.),(1.,1.),(1.,1.),(1.,1.),(1.,1.),(1.,1.),(1.,
1.),(1.,1.),(1.,1.),(1.,1.),(1.,1.),(1.,1.),(1.,1.),(1.,1.),(1.,1.),(1.,
1.),(1.,1.),(1.,1.),(1.,1.),(1.,1.),(1.,1.),(1.,1.),(1.,1.),(1.,1.),(1.,
1.),(1.,1.),(1.,1.),(1.,1.),(1.,1.),(1.,1.),(1.,1.),(1.,1.),(1.,1.),(1.,
1.),(1.,1.),(1.,1.),(1.,1.),(1.,1.),(1.,1.),(1.,1.),(1.,1.),(1.,1.),(1.,
1.),(1.,1.),(1.,1.),(1.,1.),(1.,1.),(1.,1.),(1.,1.),(1.,1.),(1.,1.),(1.,
1.),(1.,1.)))
REPRESENTATION_ITEM('')
SURFACE()
);
#1004=(
BOUNDED_SURFACE()
B_SPLINE_SURFACE(5,1,((#156242,#156243),(#156244,#156245),(#156246,#156247),
(#156248,#156249),(#156250,#156251),(#156252,#156253),(#156254,#156255),
(#156256,#156257),(#156258,#156259),(#156260,#156261),(#156262,#156263),
(#156264,#156265),(#156266,#156267),(#156268,#156269),(#156270,#156271),
(#156272,#156273),(#156274,#156275),(#156276,#156277),(#156278,#156279),
(#156280,#156281),(#156282,#156283),(#156284,#156285),(#156286,#156287),
(#156288,#156289),(#156290,#156291),(#156292,#156293),(#156294,#156295),
(#156296,#156297),(#156298,#156299),(#156300,#156301),(#156302,#156303),
(#156304,#156305),(#156306,#156307),(#156308,#156309),(#156310,#156311),
(#156312,#156313),(#156314,#156315),(#156316,#156317),(#156318,#156319),
(#156320,#156321),(#156322,#156323),(#156324,#156325),(#156326,#156327),
(#156328,#156329),(#156330,#156331),(#156332,#156333),(#156334,#156335),
(#156336,#156337),(#156338,#156339),(#156340,#156341),(#156342,#156343),
(#156344,#156345),(#156346,#156347),(#156348,#156349),(#156350,#156351),
(#156352,#156353),(#156354,#156355),(#156356,#156357),(#156358,#156359),
(#156360,#156361),(#156362,#156363),(#156364,#156365),(#156366,#156367),
(#156368,#156369),(#156370,#156371),(#156372,#156373),(#156374,#156375),
(#156376,#156377),(#156378,#156379),(#156380,#156381),(#156382,#156383),
(#156384,#156385),(#156386,#156387),(#156388,#156389),(#156390,#156391),
(#156392,#156393),(#156394,#156395),(#156396,#156397),(#156398,#156399),
(#156400,#156401),(#156402,#156403),(#156404,#156405),(#156406,#156407),
(#156408,#156409),(#156410,#156411),(#156412,#156413),(#156414,#156415),
(#156416,#156417),(#156418,#156419),(#156420,#156421),(#156422,#156423),
(#156424,#156425),(#156426,#156427),(#156428,#156429),(#156430,#156431),
(#156432,#156433),(#156434,#156435),(#156436,#156437),(#156438,#156439),
(#156440,#156441),(#156442,#156443),(#156444,#156445),(#156446,#156447),
(#156448,#156449),(#156450,#156451),(#156452,#156453),(#156454,#156455),
(#156456,#156457),(#156458,#156459),(#156460,#156461),(#156462,#156463),
(#156464,#156465),(#156466,#156467),(#156468,#156469),(#156470,#156471),
(#156472,#156473),(#156474,#156475),(#156476,#156477),(#156478,#156479),
(#156480,#156481),(#156482,#156483),(#156484,#156485),(#156486,#156487),
(#156488,#156489),(#156490,#156491),(#156492,#156493),(#156494,#156495),
(#156496,#156497),(#156498,#156499),(#156500,#156501),(#156502,#156503),
(#156504,#156505),(#156506,#156507),(#156508,#156509),(#156510,#156511),
(#156512,#156513),(#156514,#156515),(#156516,#156517),(#156518,#156519),
(#156520,#156521),(#156522,#156523),(#156524,#156525),(#156526,#156527),
(#156528,#156529),(#156530,#156531),(#156532,#156533),(#156534,#156535),
(#156536,#156537),(#156538,#156539),(#156540,#156541),(#156542,#156543),
(#156544,#156545),(#156546,#156547),(#156548,#156549),(#156550,#156551),
(#156552,#156553),(#156554,#156555),(#156556,#156557),(#156558,#156559),
(#156560,#156561),(#156562,#156563),(#156564,#156565),(#156566,#156567),
(#156568,#156569),(#156570,#156571),(#156572,#156573),(#156574,#156575),
(#156576,#156577),(#156578,#156579),(#156580,#156581),(#156582,#156583),
(#156584,#156585),(#156586,#156587),(#156588,#156589),(#156590,#156591),
(#156592,#156593),(#156594,#156595),(#156596,#156597),(#156598,#156599),
(#156600,#156601),(#156602,#156603),(#156604,#156605),(#156606,#156607),
(#156608,#156609),(#156610,#156611),(#156612,#156613),(#156614,#156615),
(#156616,#156617),(#156618,#156619),(#156620,#156621),(#156622,#156623),
(#156624,#156625),(#156626,#156627),(#156628,#156629),(#156630,#156631),
(#156632,#156633),(#156634,#156635),(#156636,#156637),(#156638,#156639),
(#156640,#156641),(#156642,#156643),(#156644,#156645),(#156646,#156647),
(#156648,#156649),(#156650,#156651)),.UNSPECIFIED.,.F.,.F.,.F.)
B_SPLINE_SURFACE_WITH_KNOTS((6,1,1,1,1,1,1,1,1,1,1,1,1,1,1,1,1,1,1,1,1,
1,1,1,1,1,1,1,1,1,1,1,1,1,1,1,1,1,1,1,1,1,1,1,1,1,1,1,1,1,1,1,1,1,1,1,1,
1,1,1,1,1,1,1,1,1,1,1,1,1,1,1,1,1,1,1,1,1,1,1,1,1,1,1,1,1,1,1,1,1,1,1,1,
1,1,1,1,1,1,1,1,1,1,1,1,1,1,1,1,1,1,1,1,1,1,1,1,1,1,1,1,1,1,1,1,1,1,1,1,
1,1,1,1,1,1,1,1,1,1,1,1,1,1,1,1,1,1,1,1,1,1,1,1,1,1,1,1,1,1,1,1,1,1,1,1,
1,1,1,1,1,1,1,1,1,1,1,1,1,1,1,1,1,1,1,1,1,1,1,1,1,1,1,1,1,1,1,1,1,1,1,6),
(2,2),(-1.,-0.995000000000001,-0.990000000000001,-0.985000000000001,-0.980000000000001,
-0.975000000000001,-0.970000000000001,-0.965000000000001,-0.960000000000001,
-0.955000000000001,-0.950000000000001,-0.945000000000001,-0.940000000000001,
-0.935000000000001,-0.930000000000001,-0.925000000000001,-0.920000000000001,
-0.915000000000001,-0.910000000000001,-0.905000000000001,-0.900000000000001,
-0.895000000000001,-0.890000000000001,-0.885000000000001,-0.880000000000001,
-0.875000000000001,-0.870000000000001,-0.865000000000001,-0.860000000000001,
-0.855000000000001,-0.850000000000001,-0.845000000000001,-0.840000000000001,
-0.835000000000001,-0.830000000000001,-0.825000000000001,-0.820000000000001,
-0.815000000000001,-0.810000000000001,-0.805000000000001,-0.800000000000001,
-0.795000000000001,-0.790000000000001,-0.785000000000001,-0.780000000000001,
-0.775000000000001,-0.770000000000001,-0.765000000000001,-0.760000000000001,
-0.755000000000001,-0.750000000000001,-0.745000000000001,-0.740000000000001,
-0.735000000000001,-0.730000000000001,-0.725000000000001,-0.720000000000001,
-0.715000000000001,-0.710000000000001,-0.705000000000001,-0.700000000000001,
-0.695000000000001,-0.690000000000001,-0.685,-0.68,-0.675,-0.67,-0.665,
-0.66,-0.655,-0.65,-0.645,-0.64,-0.635,-0.63,-0.625,-0.62,-0.615,-0.61,
-0.605,-0.6,-0.595,-0.59,-0.585,-0.58,-0.575,-0.57,-0.565,-0.56,-0.555,
-0.55,-0.545,-0.54,-0.535,-0.53,-0.525,-0.52,-0.515,-0.51,-0.505,-0.5,-0.495,
-0.49,-0.485,-0.48,-0.475,-0.47,-0.465,-0.46,-0.455,-0.45,-0.445,-0.44,
-0.435,-0.43,-0.425,-0.42,-0.415,-0.41,-0.405,-0.4,-0.395,-0.39,-0.385,
-0.38,-0.375,-0.37,-0.365,-0.36,-0.355,-0.35,-0.345,-0.34,-0.335,-0.33,
-0.325,-0.32,-0.315,-0.31,-0.305,-0.3,-0.295,-0.29,-0.285,-0.28,-0.275,
-0.27,-0.265,-0.26,-0.255,-0.25,-0.245,-0.24,-0.235,-0.23,-0.225,-0.22,
-0.215,-0.21,-0.205,-0.2,-0.195,-0.19,-0.185,-0.18,-0.175,-0.17,-0.165,
-0.16,-0.155,-0.15,-0.145,-0.14,-0.135,-0.13,-0.125,-0.12,-0.115,-0.11,
-0.105,-0.1,-0.095,-0.09,-0.085,-0.08,-0.075,-0.07,-0.065,-0.06,-0.055,
-0.05,-0.045,-0.04,-0.035,-0.03,-0.025,-0.02,-0.015,-0.01,-0.005,0.),(0.,
1.2),.UNSPECIFIED.)
GEOMETRIC_REPRESENTATION_ITEM()
RATIONAL_B_SPLINE_SURFACE(((1.,1.),(1.,1.),(1.,1.),(1.,1.),(1.,1.),(1.,
1.),(1.,1.),(1.,1.),(1.,1.),(1.,1.),(1.,1.),(1.,1.),(1.,1.),(1.,1.),(1.,
1.),(1.,1.),(1.,1.),(1.,1.),(1.,1.),(1.,1.),(1.,1.),(1.,1.),(1.,1.),(1.,
1.),(1.,1.),(1.,1.),(1.,1.),(1.,1.),(1.,1.),(1.,1.),(1.,1.),(1.,1.),(1.,
1.),(1.,1.),(1.,1.),(1.,1.),(1.,1.),(1.,1.),(1.,1.),(1.,1.),(1.,1.),(1.,
1.),(1.,1.),(1.,1.),(1.,1.),(1.,1.),(1.,1.),(1.,1.),(1.,1.),(1.,1.),(1.,
1.),(1.,1.),(1.,1.),(1.,1.),(1.,1.),(1.,1.),(1.,1.),(1.,1.),(1.,1.),(1.,
1.),(1.,1.),(1.,1.),(1.,1.),(1.,1.),(1.,1.),(1.,1.),(1.,1.),(1.,1.),(1.,
1.),(1.,1.),(1.,1.),(1.,1.),(1.,1.),(1.,1.),(1.,1.),(1.,1.),(1.,1.),(1.,
1.),(1.,1.),(1.,1.),(1.,1.),(1.,1.),(1.,1.),(1.,1.),(1.,1.),(1.,1.),(1.,
1.),(1.,1.),(1.,1.),(1.,1.),(1.,1.),(1.,1.),(1.,1.),(1.,1.),(1.,1.),(1.,
1.),(1.,1.),(1.,1.),(1.,1.),(1.,1.),(1.,1.),(1.,1.),(1.,1.),(1.,1.),(1.,
1.),(1.,1.),(1.,1.),(1.,1.),(1.,1.),(1.,1.),(1.,1.),(1.,1.),(1.,1.),(1.,
1.),(1.,1.),(1.,1.),(1.,1.),(1.,1.),(1.,1.),(1.,1.),(1.,1.),(1.,1.),(1.,
1.),(1.,1.),(1.,1.),(1.,1.),(1.,1.),(1.,1.),(1.,1.),(1.,1.),(1.,1.),(1.,
1.),(1.,1.),(1.,1.),(1.,1.),(1.,1.),(1.,1.),(1.,1.),(1.,1.),(1.,1.),(1.,
1.),(1.,1.),(1.,1.),(1.,1.),(1.,1.),(1.,1.),(1.,1.),(1.,1.),(1.,1.),(1.,
1.),(1.,1.),(1.,1.),(1.,1.),(1.,1.),(1.,1.),(1.,1.),(1.,1.),(1.,1.),(1.,
1.),(1.,1.),(1.,1.),(1.,1.),(1.,1.),(1.,1.),(1.,1.),(1.,1.),(1.,1.),(1.,
1.),(1.,1.),(1.,1.),(1.,1.),(1.,1.),(1.,1.),(1.,1.),(1.,1.),(1.,1.),(1.,
1.),(1.,1.),(1.,1.),(1.,1.),(1.,1.),(1.,1.),(1.,1.),(1.,1.),(1.,1.),(1.,
1.),(1.,1.),(1.,1.),(1.,1.),(1.,1.),(1.,1.),(1.,1.),(1.,1.),(1.,1.),(1.,
1.),(1.,1.),(1.,1.),(1.,1.),(1.,1.),(1.,1.),(1.,1.),(1.,1.),(1.,1.),(1.,
1.),(1.,1.)))
REPRESENTATION_ITEM('')
SURFACE()
);
#1005=(
BOUNDED_SURFACE()
B_SPLINE_SURFACE(5,1,((#157043,#157044),(#157045,#157046),(#157047,#157048),
(#157049,#157050),(#157051,#157052),(#157053,#157054),(#157055,#157056),
(#157057,#157058),(#157059,#157060),(#157061,#157062),(#157063,#157064),
(#157065,#157066),(#157067,#157068),(#157069,#157070),(#157071,#157072),
(#157073,#157074),(#157075,#157076),(#157077,#157078),(#157079,#157080),
(#157081,#157082),(#157083,#157084),(#157085,#157086),(#157087,#157088),
(#157089,#157090),(#157091,#157092),(#157093,#157094),(#157095,#157096),
(#157097,#157098),(#157099,#157100),(#157101,#157102),(#157103,#157104),
(#157105,#157106),(#157107,#157108),(#157109,#157110),(#157111,#157112),
(#157113,#157114),(#157115,#157116),(#157117,#157118),(#157119,#157120),
(#157121,#157122),(#157123,#157124),(#157125,#157126),(#157127,#157128),
(#157129,#157130),(#157131,#157132),(#157133,#157134),(#157135,#157136),
(#157137,#157138),(#157139,#157140),(#157141,#157142),(#157143,#157144),
(#157145,#157146),(#157147,#157148),(#157149,#157150),(#157151,#157152),
(#157153,#157154),(#157155,#157156),(#157157,#157158),(#157159,#157160),
(#157161,#157162),(#157163,#157164),(#157165,#157166),(#157167,#157168),
(#157169,#157170),(#157171,#157172),(#157173,#157174),(#157175,#157176),
(#157177,#157178),(#157179,#157180),(#157181,#157182),(#157183,#157184),
(#157185,#157186),(#157187,#157188),(#157189,#157190),(#157191,#157192),
(#157193,#157194),(#157195,#157196),(#157197,#157198),(#157199,#157200),
(#157201,#157202),(#157203,#157204),(#157205,#157206),(#157207,#157208),
(#157209,#157210),(#157211,#157212),(#157213,#157214),(#157215,#157216),
(#157217,#157218),(#157219,#157220),(#157221,#157222),(#157223,#157224),
(#157225,#157226),(#157227,#157228),(#157229,#157230),(#157231,#157232),
(#157233,#157234),(#157235,#157236),(#157237,#157238),(#157239,#157240),
(#157241,#157242),(#157243,#157244),(#157245,#157246),(#157247,#157248),
(#157249,#157250),(#157251,#157252),(#157253,#157254),(#157255,#157256),
(#157257,#157258),(#157259,#157260),(#157261,#157262),(#157263,#157264),
(#157265,#157266),(#157267,#157268),(#157269,#157270),(#157271,#157272),
(#157273,#157274),(#157275,#157276),(#157277,#157278),(#157279,#157280),
(#157281,#157282),(#157283,#157284),(#157285,#157286),(#157287,#157288),
(#157289,#157290),(#157291,#157292),(#157293,#157294),(#157295,#157296),
(#157297,#157298),(#157299,#157300),(#157301,#157302),(#157303,#157304),
(#157305,#157306),(#157307,#157308),(#157309,#157310),(#157311,#157312),
(#157313,#157314),(#157315,#157316),(#157317,#157318),(#157319,#157320),
(#157321,#157322),(#157323,#157324),(#157325,#157326),(#157327,#157328),
(#157329,#157330),(#157331,#157332),(#157333,#157334),(#157335,#157336),
(#157337,#157338),(#157339,#157340),(#157341,#157342),(#157343,#157344),
(#157345,#157346),(#157347,#157348),(#157349,#157350),(#157351,#157352),
(#157353,#157354),(#157355,#157356),(#157357,#157358),(#157359,#157360),
(#157361,#157362),(#157363,#157364),(#157365,#157366),(#157367,#157368),
(#157369,#157370),(#157371,#157372),(#157373,#157374),(#157375,#157376),
(#157377,#157378),(#157379,#157380),(#157381,#157382),(#157383,#157384),
(#157385,#157386),(#157387,#157388),(#157389,#157390),(#157391,#157392),
(#157393,#157394),(#157395,#157396),(#157397,#157398),(#157399,#157400),
(#157401,#157402),(#157403,#157404),(#157405,#157406),(#157407,#157408),
(#157409,#157410),(#157411,#157412),(#157413,#157414),(#157415,#157416),
(#157417,#157418),(#157419,#157420),(#157421,#157422),(#157423,#157424),
(#157425,#157426),(#157427,#157428),(#157429,#157430),(#157431,#157432),
(#157433,#157434),(#157435,#157436),(#157437,#157438),(#157439,#157440),
(#157441,#157442),(#157443,#157444),(#157445,#157446),(#157447,#157448),
(#157449,#157450),(#157451,#157452)),.UNSPECIFIED.,.F.,.F.,.F.)
B_SPLINE_SURFACE_WITH_KNOTS((6,1,1,1,1,1,1,1,1,1,1,1,1,1,1,1,1,1,1,1,1,
1,1,1,1,1,1,1,1,1,1,1,1,1,1,1,1,1,1,1,1,1,1,1,1,1,1,1,1,1,1,1,1,1,1,1,1,
1,1,1,1,1,1,1,1,1,1,1,1,1,1,1,1,1,1,1,1,1,1,1,1,1,1,1,1,1,1,1,1,1,1,1,1,
1,1,1,1,1,1,1,1,1,1,1,1,1,1,1,1,1,1,1,1,1,1,1,1,1,1,1,1,1,1,1,1,1,1,1,1,
1,1,1,1,1,1,1,1,1,1,1,1,1,1,1,1,1,1,1,1,1,1,1,1,1,1,1,1,1,1,1,1,1,1,1,1,
1,1,1,1,1,1,1,1,1,1,1,1,1,1,1,1,1,1,1,1,1,1,1,1,1,1,1,1,1,1,1,1,1,1,1,6),
(2,2),(-1.,-0.995000000000001,-0.990000000000001,-0.985000000000001,-0.980000000000001,
-0.975000000000001,-0.970000000000001,-0.965000000000001,-0.960000000000001,
-0.955000000000001,-0.950000000000001,-0.945000000000001,-0.940000000000001,
-0.935000000000001,-0.930000000000001,-0.925000000000001,-0.920000000000001,
-0.915000000000001,-0.910000000000001,-0.905000000000001,-0.900000000000001,
-0.895000000000001,-0.890000000000001,-0.885000000000001,-0.880000000000001,
-0.875000000000001,-0.870000000000001,-0.865000000000001,-0.860000000000001,
-0.855000000000001,-0.850000000000001,-0.845000000000001,-0.840000000000001,
-0.835000000000001,-0.830000000000001,-0.825000000000001,-0.820000000000001,
-0.815000000000001,-0.810000000000001,-0.805000000000001,-0.800000000000001,
-0.795000000000001,-0.790000000000001,-0.785000000000001,-0.780000000000001,
-0.775000000000001,-0.770000000000001,-0.765000000000001,-0.760000000000001,
-0.755000000000001,-0.750000000000001,-0.745000000000001,-0.740000000000001,
-0.735000000000001,-0.730000000000001,-0.725000000000001,-0.720000000000001,
-0.715000000000001,-0.710000000000001,-0.705000000000001,-0.700000000000001,
-0.695000000000001,-0.690000000000001,-0.685,-0.68,-0.675,-0.67,-0.665,
-0.66,-0.655,-0.65,-0.645,-0.64,-0.635,-0.63,-0.625,-0.62,-0.615,-0.61,
-0.605,-0.6,-0.595,-0.59,-0.585,-0.58,-0.575,-0.57,-0.565,-0.56,-0.555,
-0.55,-0.545,-0.54,-0.535,-0.53,-0.525,-0.52,-0.515,-0.51,-0.505,-0.5,-0.495,
-0.49,-0.485,-0.48,-0.475,-0.47,-0.465,-0.46,-0.455,-0.45,-0.445,-0.44,
-0.435,-0.43,-0.425,-0.42,-0.415,-0.41,-0.405,-0.4,-0.395,-0.39,-0.385,
-0.38,-0.375,-0.37,-0.365,-0.36,-0.355,-0.35,-0.345,-0.34,-0.335,-0.33,
-0.325,-0.32,-0.315,-0.31,-0.305,-0.3,-0.295,-0.29,-0.285,-0.28,-0.275,
-0.27,-0.265,-0.26,-0.255,-0.25,-0.245,-0.24,-0.235,-0.23,-0.225,-0.22,
-0.215,-0.21,-0.205,-0.2,-0.195,-0.19,-0.185,-0.18,-0.175,-0.17,-0.165,
-0.16,-0.155,-0.15,-0.145,-0.14,-0.135,-0.13,-0.125,-0.12,-0.115,-0.11,
-0.105,-0.1,-0.095,-0.09,-0.085,-0.08,-0.075,-0.07,-0.065,-0.06,-0.055,
-0.05,-0.045,-0.04,-0.035,-0.03,-0.025,-0.02,-0.015,-0.01,-0.005,0.),(0.,
1.2),.UNSPECIFIED.)
GEOMETRIC_REPRESENTATION_ITEM()
RATIONAL_B_SPLINE_SURFACE(((1.,1.),(1.,1.),(1.,1.),(1.,1.),(1.,1.),(1.,
1.),(1.,1.),(1.,1.),(1.,1.),(1.,1.),(1.,1.),(1.,1.),(1.,1.),(1.,1.),(1.,
1.),(1.,1.),(1.,1.),(1.,1.),(1.,1.),(1.,1.),(1.,1.),(1.,1.),(1.,1.),(1.,
1.),(1.,1.),(1.,1.),(1.,1.),(1.,1.),(1.,1.),(1.,1.),(1.,1.),(1.,1.),(1.,
1.),(1.,1.),(1.,1.),(1.,1.),(1.,1.),(1.,1.),(1.,1.),(1.,1.),(1.,1.),(1.,
1.),(1.,1.),(1.,1.),(1.,1.),(1.,1.),(1.,1.),(1.,1.),(1.,1.),(1.,1.),(1.,
1.),(1.,1.),(1.,1.),(1.,1.),(1.,1.),(1.,1.),(1.,1.),(1.,1.),(1.,1.),(1.,
1.),(1.,1.),(1.,1.),(1.,1.),(1.,1.),(1.,1.),(1.,1.),(1.,1.),(1.,1.),(1.,
1.),(1.,1.),(1.,1.),(1.,1.),(1.,1.),(1.,1.),(1.,1.),(1.,1.),(1.,1.),(1.,
1.),(1.,1.),(1.,1.),(1.,1.),(1.,1.),(1.,1.),(1.,1.),(1.,1.),(1.,1.),(1.,
1.),(1.,1.),(1.,1.),(1.,1.),(1.,1.),(1.,1.),(1.,1.),(1.,1.),(1.,1.),(1.,
1.),(1.,1.),(1.,1.),(1.,1.),(1.,1.),(1.,1.),(1.,1.),(1.,1.),(1.,1.),(1.,
1.),(1.,1.),(1.,1.),(1.,1.),(1.,1.),(1.,1.),(1.,1.),(1.,1.),(1.,1.),(1.,
1.),(1.,1.),(1.,1.),(1.,1.),(1.,1.),(1.,1.),(1.,1.),(1.,1.),(1.,1.),(1.,
1.),(1.,1.),(1.,1.),(1.,1.),(1.,1.),(1.,1.),(1.,1.),(1.,1.),(1.,1.),(1.,
1.),(1.,1.),(1.,1.),(1.,1.),(1.,1.),(1.,1.),(1.,1.),(1.,1.),(1.,1.),(1.,
1.),(1.,1.),(1.,1.),(1.,1.),(1.,1.),(1.,1.),(1.,1.),(1.,1.),(1.,1.),(1.,
1.),(1.,1.),(1.,1.),(1.,1.),(1.,1.),(1.,1.),(1.,1.),(1.,1.),(1.,1.),(1.,
1.),(1.,1.),(1.,1.),(1.,1.),(1.,1.),(1.,1.),(1.,1.),(1.,1.),(1.,1.),(1.,
1.),(1.,1.),(1.,1.),(1.,1.),(1.,1.),(1.,1.),(1.,1.),(1.,1.),(1.,1.),(1.,
1.),(1.,1.),(1.,1.),(1.,1.),(1.,1.),(1.,1.),(1.,1.),(1.,1.),(1.,1.),(1.,
1.),(1.,1.),(1.,1.),(1.,1.),(1.,1.),(1.,1.),(1.,1.),(1.,1.),(1.,1.),(1.,
1.),(1.,1.),(1.,1.),(1.,1.),(1.,1.),(1.,1.),(1.,1.),(1.,1.),(1.,1.),(1.,
1.),(1.,1.)))
REPRESENTATION_ITEM('')
SURFACE()
);
#1006=(
BOUNDED_SURFACE()
B_SPLINE_SURFACE(5,1,((#157844,#157845),(#157846,#157847),(#157848,#157849),
(#157850,#157851),(#157852,#157853),(#157854,#157855),(#157856,#157857),
(#157858,#157859),(#157860,#157861),(#157862,#157863),(#157864,#157865),
(#157866,#157867),(#157868,#157869),(#157870,#157871),(#157872,#157873),
(#157874,#157875),(#157876,#157877),(#157878,#157879),(#157880,#157881),
(#157882,#157883),(#157884,#157885),(#157886,#157887),(#157888,#157889),
(#157890,#157891),(#157892,#157893),(#157894,#157895),(#157896,#157897),
(#157898,#157899),(#157900,#157901),(#157902,#157903),(#157904,#157905),
(#157906,#157907),(#157908,#157909),(#157910,#157911),(#157912,#157913),
(#157914,#157915),(#157916,#157917),(#157918,#157919),(#157920,#157921),
(#157922,#157923),(#157924,#157925),(#157926,#157927),(#157928,#157929),
(#157930,#157931),(#157932,#157933),(#157934,#157935),(#157936,#157937),
(#157938,#157939),(#157940,#157941),(#157942,#157943),(#157944,#157945),
(#157946,#157947),(#157948,#157949),(#157950,#157951),(#157952,#157953),
(#157954,#157955),(#157956,#157957),(#157958,#157959),(#157960,#157961),
(#157962,#157963),(#157964,#157965),(#157966,#157967),(#157968,#157969),
(#157970,#157971),(#157972,#157973),(#157974,#157975),(#157976,#157977),
(#157978,#157979),(#157980,#157981),(#157982,#157983),(#157984,#157985),
(#157986,#157987),(#157988,#157989),(#157990,#157991),(#157992,#157993),
(#157994,#157995),(#157996,#157997),(#157998,#157999),(#158000,#158001),
(#158002,#158003),(#158004,#158005),(#158006,#158007),(#158008,#158009),
(#158010,#158011),(#158012,#158013),(#158014,#158015),(#158016,#158017),
(#158018,#158019),(#158020,#158021),(#158022,#158023),(#158024,#158025),
(#158026,#158027),(#158028,#158029),(#158030,#158031),(#158032,#158033),
(#158034,#158035),(#158036,#158037),(#158038,#158039),(#158040,#158041),
(#158042,#158043),(#158044,#158045),(#158046,#158047),(#158048,#158049),
(#158050,#158051),(#158052,#158053),(#158054,#158055),(#158056,#158057),
(#158058,#158059),(#158060,#158061),(#158062,#158063),(#158064,#158065),
(#158066,#158067),(#158068,#158069),(#158070,#158071),(#158072,#158073),
(#158074,#158075),(#158076,#158077),(#158078,#158079),(#158080,#158081),
(#158082,#158083),(#158084,#158085),(#158086,#158087),(#158088,#158089),
(#158090,#158091),(#158092,#158093),(#158094,#158095),(#158096,#158097),
(#158098,#158099),(#158100,#158101),(#158102,#158103),(#158104,#158105),
(#158106,#158107),(#158108,#158109),(#158110,#158111),(#158112,#158113),
(#158114,#158115),(#158116,#158117),(#158118,#158119),(#158120,#158121),
(#158122,#158123),(#158124,#158125),(#158126,#158127),(#158128,#158129),
(#158130,#158131),(#158132,#158133),(#158134,#158135),(#158136,#158137),
(#158138,#158139),(#158140,#158141),(#158142,#158143),(#158144,#158145),
(#158146,#158147),(#158148,#158149),(#158150,#158151),(#158152,#158153),
(#158154,#158155),(#158156,#158157),(#158158,#158159),(#158160,#158161),
(#158162,#158163),(#158164,#158165),(#158166,#158167),(#158168,#158169),
(#158170,#158171),(#158172,#158173),(#158174,#158175),(#158176,#158177),
(#158178,#158179),(#158180,#158181),(#158182,#158183),(#158184,#158185),
(#158186,#158187),(#158188,#158189),(#158190,#158191),(#158192,#158193),
(#158194,#158195),(#158196,#158197),(#158198,#158199),(#158200,#158201),
(#158202,#158203),(#158204,#158205),(#158206,#158207),(#158208,#158209),
(#158210,#158211),(#158212,#158213),(#158214,#158215),(#158216,#158217),
(#158218,#158219),(#158220,#158221),(#158222,#158223),(#158224,#158225),
(#158226,#158227),(#158228,#158229),(#158230,#158231),(#158232,#158233),
(#158234,#158235),(#158236,#158237),(#158238,#158239),(#158240,#158241),
(#158242,#158243),(#158244,#158245),(#158246,#158247),(#158248,#158249),
(#158250,#158251),(#158252,#158253)),.UNSPECIFIED.,.F.,.F.,.F.)
B_SPLINE_SURFACE_WITH_KNOTS((6,1,1,1,1,1,1,1,1,1,1,1,1,1,1,1,1,1,1,1,1,
1,1,1,1,1,1,1,1,1,1,1,1,1,1,1,1,1,1,1,1,1,1,1,1,1,1,1,1,1,1,1,1,1,1,1,1,
1,1,1,1,1,1,1,1,1,1,1,1,1,1,1,1,1,1,1,1,1,1,1,1,1,1,1,1,1,1,1,1,1,1,1,1,
1,1,1,1,1,1,1,1,1,1,1,1,1,1,1,1,1,1,1,1,1,1,1,1,1,1,1,1,1,1,1,1,1,1,1,1,
1,1,1,1,1,1,1,1,1,1,1,1,1,1,1,1,1,1,1,1,1,1,1,1,1,1,1,1,1,1,1,1,1,1,1,1,
1,1,1,1,1,1,1,1,1,1,1,1,1,1,1,1,1,1,1,1,1,1,1,1,1,1,1,1,1,1,1,1,1,1,1,6),
(2,2),(-1.,-0.995000000000001,-0.990000000000001,-0.985000000000001,-0.980000000000001,
-0.975000000000001,-0.970000000000001,-0.965000000000001,-0.960000000000001,
-0.955000000000001,-0.950000000000001,-0.945000000000001,-0.940000000000001,
-0.935000000000001,-0.930000000000001,-0.925000000000001,-0.920000000000001,
-0.915000000000001,-0.910000000000001,-0.905000000000001,-0.900000000000001,
-0.895000000000001,-0.890000000000001,-0.885000000000001,-0.880000000000001,
-0.875000000000001,-0.870000000000001,-0.865000000000001,-0.860000000000001,
-0.855000000000001,-0.850000000000001,-0.845000000000001,-0.840000000000001,
-0.835000000000001,-0.830000000000001,-0.825000000000001,-0.820000000000001,
-0.815000000000001,-0.810000000000001,-0.805000000000001,-0.800000000000001,
-0.795000000000001,-0.790000000000001,-0.785000000000001,-0.780000000000001,
-0.775000000000001,-0.770000000000001,-0.765000000000001,-0.760000000000001,
-0.755000000000001,-0.750000000000001,-0.745000000000001,-0.740000000000001,
-0.735000000000001,-0.730000000000001,-0.725000000000001,-0.720000000000001,
-0.715000000000001,-0.710000000000001,-0.705000000000001,-0.700000000000001,
-0.695000000000001,-0.690000000000001,-0.685,-0.68,-0.675,-0.67,-0.665,
-0.66,-0.655,-0.65,-0.645,-0.64,-0.635,-0.63,-0.625,-0.62,-0.615,-0.61,
-0.605,-0.6,-0.595,-0.59,-0.585,-0.58,-0.575,-0.57,-0.565,-0.56,-0.555,
-0.55,-0.545,-0.54,-0.535,-0.53,-0.525,-0.52,-0.515,-0.51,-0.505,-0.5,-0.495,
-0.49,-0.485,-0.48,-0.475,-0.47,-0.465,-0.46,-0.455,-0.45,-0.445,-0.44,
-0.435,-0.43,-0.425,-0.42,-0.415,-0.41,-0.405,-0.4,-0.395,-0.39,-0.385,
-0.38,-0.375,-0.37,-0.365,-0.36,-0.355,-0.35,-0.345,-0.34,-0.335,-0.33,
-0.325,-0.32,-0.315,-0.31,-0.305,-0.3,-0.295,-0.29,-0.285,-0.28,-0.275,
-0.27,-0.265,-0.26,-0.255,-0.25,-0.245,-0.24,-0.235,-0.23,-0.225,-0.22,
-0.215,-0.21,-0.205,-0.2,-0.195,-0.19,-0.185,-0.18,-0.175,-0.17,-0.165,
-0.16,-0.155,-0.15,-0.145,-0.14,-0.135,-0.13,-0.125,-0.12,-0.115,-0.11,
-0.105,-0.1,-0.095,-0.09,-0.085,-0.08,-0.075,-0.07,-0.065,-0.06,-0.055,
-0.05,-0.045,-0.04,-0.035,-0.03,-0.025,-0.02,-0.015,-0.01,-0.005,0.),(0.,
1.2),.UNSPECIFIED.)
GEOMETRIC_REPRESENTATION_ITEM()
RATIONAL_B_SPLINE_SURFACE(((1.,1.),(1.,1.),(1.,1.),(1.,1.),(1.,1.),(1.,
1.),(1.,1.),(1.,1.),(1.,1.),(1.,1.),(1.,1.),(1.,1.),(1.,1.),(1.,1.),(1.,
1.),(1.,1.),(1.,1.),(1.,1.),(1.,1.),(1.,1.),(1.,1.),(1.,1.),(1.,1.),(1.,
1.),(1.,1.),(1.,1.),(1.,1.),(1.,1.),(1.,1.),(1.,1.),(1.,1.),(1.,1.),(1.,
1.),(1.,1.),(1.,1.),(1.,1.),(1.,1.),(1.,1.),(1.,1.),(1.,1.),(1.,1.),(1.,
1.),(1.,1.),(1.,1.),(1.,1.),(1.,1.),(1.,1.),(1.,1.),(1.,1.),(1.,1.),(1.,
1.),(1.,1.),(1.,1.),(1.,1.),(1.,1.),(1.,1.),(1.,1.),(1.,1.),(1.,1.),(1.,
1.),(1.,1.),(1.,1.),(1.,1.),(1.,1.),(1.,1.),(1.,1.),(1.,1.),(1.,1.),(1.,
1.),(1.,1.),(1.,1.),(1.,1.),(1.,1.),(1.,1.),(1.,1.),(1.,1.),(1.,1.),(1.,
1.),(1.,1.),(1.,1.),(1.,1.),(1.,1.),(1.,1.),(1.,1.),(1.,1.),(1.,1.),(1.,
1.),(1.,1.),(1.,1.),(1.,1.),(1.,1.),(1.,1.),(1.,1.),(1.,1.),(1.,1.),(1.,
1.),(1.,1.),(1.,1.),(1.,1.),(1.,1.),(1.,1.),(1.,1.),(1.,1.),(1.,1.),(1.,
1.),(1.,1.),(1.,1.),(1.,1.),(1.,1.),(1.,1.),(1.,1.),(1.,1.),(1.,1.),(1.,
1.),(1.,1.),(1.,1.),(1.,1.),(1.,1.),(1.,1.),(1.,1.),(1.,1.),(1.,1.),(1.,
1.),(1.,1.),(1.,1.),(1.,1.),(1.,1.),(1.,1.),(1.,1.),(1.,1.),(1.,1.),(1.,
1.),(1.,1.),(1.,1.),(1.,1.),(1.,1.),(1.,1.),(1.,1.),(1.,1.),(1.,1.),(1.,
1.),(1.,1.),(1.,1.),(1.,1.),(1.,1.),(1.,1.),(1.,1.),(1.,1.),(1.,1.),(1.,
1.),(1.,1.),(1.,1.),(1.,1.),(1.,1.),(1.,1.),(1.,1.),(1.,1.),(1.,1.),(1.,
1.),(1.,1.),(1.,1.),(1.,1.),(1.,1.),(1.,1.),(1.,1.),(1.,1.),(1.,1.),(1.,
1.),(1.,1.),(1.,1.),(1.,1.),(1.,1.),(1.,1.),(1.,1.),(1.,1.),(1.,1.),(1.,
1.),(1.,1.),(1.,1.),(1.,1.),(1.,1.),(1.,1.),(1.,1.),(1.,1.),(1.,1.),(1.,
1.),(1.,1.),(1.,1.),(1.,1.),(1.,1.),(1.,1.),(1.,1.),(1.,1.),(1.,1.),(1.,
1.),(1.,1.),(1.,1.),(1.,1.),(1.,1.),(1.,1.),(1.,1.),(1.,1.),(1.,1.),(1.,
1.),(1.,1.)))
REPRESENTATION_ITEM('')
SURFACE()
);
#1007=(
BOUNDED_SURFACE()
B_SPLINE_SURFACE(5,1,((#158645,#158646),(#158647,#158648),(#158649,#158650),
(#158651,#158652),(#158653,#158654),(#158655,#158656),(#158657,#158658),
(#158659,#158660),(#158661,#158662),(#158663,#158664),(#158665,#158666),
(#158667,#158668),(#158669,#158670),(#158671,#158672),(#158673,#158674),
(#158675,#158676),(#158677,#158678),(#158679,#158680),(#158681,#158682),
(#158683,#158684),(#158685,#158686),(#158687,#158688),(#158689,#158690),
(#158691,#158692),(#158693,#158694),(#158695,#158696),(#158697,#158698),
(#158699,#158700),(#158701,#158702),(#158703,#158704),(#158705,#158706),
(#158707,#158708),(#158709,#158710),(#158711,#158712),(#158713,#158714),
(#158715,#158716),(#158717,#158718),(#158719,#158720),(#158721,#158722),
(#158723,#158724),(#158725,#158726),(#158727,#158728),(#158729,#158730),
(#158731,#158732),(#158733,#158734),(#158735,#158736),(#158737,#158738),
(#158739,#158740),(#158741,#158742),(#158743,#158744),(#158745,#158746),
(#158747,#158748),(#158749,#158750),(#158751,#158752),(#158753,#158754),
(#158755,#158756),(#158757,#158758),(#158759,#158760),(#158761,#158762),
(#158763,#158764),(#158765,#158766),(#158767,#158768),(#158769,#158770),
(#158771,#158772),(#158773,#158774),(#158775,#158776),(#158777,#158778),
(#158779,#158780),(#158781,#158782),(#158783,#158784),(#158785,#158786),
(#158787,#158788),(#158789,#158790),(#158791,#158792),(#158793,#158794),
(#158795,#158796),(#158797,#158798),(#158799,#158800),(#158801,#158802),
(#158803,#158804),(#158805,#158806),(#158807,#158808),(#158809,#158810),
(#158811,#158812),(#158813,#158814),(#158815,#158816),(#158817,#158818),
(#158819,#158820),(#158821,#158822),(#158823,#158824),(#158825,#158826),
(#158827,#158828),(#158829,#158830),(#158831,#158832),(#158833,#158834),
(#158835,#158836),(#158837,#158838),(#158839,#158840),(#158841,#158842),
(#158843,#158844),(#158845,#158846),(#158847,#158848),(#158849,#158850),
(#158851,#158852),(#158853,#158854),(#158855,#158856),(#158857,#158858),
(#158859,#158860),(#158861,#158862),(#158863,#158864),(#158865,#158866),
(#158867,#158868),(#158869,#158870),(#158871,#158872),(#158873,#158874),
(#158875,#158876),(#158877,#158878),(#158879,#158880),(#158881,#158882),
(#158883,#158884),(#158885,#158886),(#158887,#158888),(#158889,#158890),
(#158891,#158892),(#158893,#158894),(#158895,#158896),(#158897,#158898),
(#158899,#158900),(#158901,#158902),(#158903,#158904),(#158905,#158906),
(#158907,#158908),(#158909,#158910),(#158911,#158912),(#158913,#158914),
(#158915,#158916),(#158917,#158918),(#158919,#158920),(#158921,#158922),
(#158923,#158924),(#158925,#158926),(#158927,#158928),(#158929,#158930),
(#158931,#158932),(#158933,#158934),(#158935,#158936),(#158937,#158938),
(#158939,#158940),(#158941,#158942),(#158943,#158944),(#158945,#158946),
(#158947,#158948),(#158949,#158950),(#158951,#158952),(#158953,#158954),
(#158955,#158956),(#158957,#158958),(#158959,#158960),(#158961,#158962),
(#158963,#158964),(#158965,#158966),(#158967,#158968),(#158969,#158970),
(#158971,#158972),(#158973,#158974),(#158975,#158976),(#158977,#158978),
(#158979,#158980),(#158981,#158982),(#158983,#158984),(#158985,#158986),
(#158987,#158988),(#158989,#158990),(#158991,#158992),(#158993,#158994),
(#158995,#158996),(#158997,#158998),(#158999,#159000),(#159001,#159002),
(#159003,#159004),(#159005,#159006),(#159007,#159008),(#159009,#159010),
(#159011,#159012),(#159013,#159014),(#159015,#159016),(#159017,#159018),
(#159019,#159020),(#159021,#159022),(#159023,#159024),(#159025,#159026),
(#159027,#159028),(#159029,#159030),(#159031,#159032),(#159033,#159034),
(#159035,#159036),(#159037,#159038),(#159039,#159040),(#159041,#159042),
(#159043,#159044),(#159045,#159046),(#159047,#159048),(#159049,#159050),
(#159051,#159052),(#159053,#159054)),.UNSPECIFIED.,.F.,.F.,.F.)
B_SPLINE_SURFACE_WITH_KNOTS((6,1,1,1,1,1,1,1,1,1,1,1,1,1,1,1,1,1,1,1,1,
1,1,1,1,1,1,1,1,1,1,1,1,1,1,1,1,1,1,1,1,1,1,1,1,1,1,1,1,1,1,1,1,1,1,1,1,
1,1,1,1,1,1,1,1,1,1,1,1,1,1,1,1,1,1,1,1,1,1,1,1,1,1,1,1,1,1,1,1,1,1,1,1,
1,1,1,1,1,1,1,1,1,1,1,1,1,1,1,1,1,1,1,1,1,1,1,1,1,1,1,1,1,1,1,1,1,1,1,1,
1,1,1,1,1,1,1,1,1,1,1,1,1,1,1,1,1,1,1,1,1,1,1,1,1,1,1,1,1,1,1,1,1,1,1,1,
1,1,1,1,1,1,1,1,1,1,1,1,1,1,1,1,1,1,1,1,1,1,1,1,1,1,1,1,1,1,1,1,1,1,1,6),
(2,2),(-1.,-0.995000000000001,-0.990000000000001,-0.985000000000001,-0.980000000000001,
-0.975000000000001,-0.970000000000001,-0.965000000000001,-0.960000000000001,
-0.955000000000001,-0.950000000000001,-0.945000000000001,-0.940000000000001,
-0.935000000000001,-0.930000000000001,-0.925000000000001,-0.920000000000001,
-0.915000000000001,-0.910000000000001,-0.905000000000001,-0.900000000000001,
-0.895000000000001,-0.890000000000001,-0.885000000000001,-0.880000000000001,
-0.875000000000001,-0.870000000000001,-0.865000000000001,-0.860000000000001,
-0.855000000000001,-0.850000000000001,-0.845000000000001,-0.840000000000001,
-0.835000000000001,-0.830000000000001,-0.825000000000001,-0.820000000000001,
-0.815000000000001,-0.810000000000001,-0.805000000000001,-0.800000000000001,
-0.795000000000001,-0.790000000000001,-0.785000000000001,-0.780000000000001,
-0.775000000000001,-0.770000000000001,-0.765000000000001,-0.760000000000001,
-0.755000000000001,-0.750000000000001,-0.745000000000001,-0.740000000000001,
-0.735000000000001,-0.730000000000001,-0.725000000000001,-0.720000000000001,
-0.715000000000001,-0.710000000000001,-0.705000000000001,-0.700000000000001,
-0.695000000000001,-0.690000000000001,-0.685,-0.68,-0.675,-0.67,-0.665,
-0.66,-0.655,-0.65,-0.645,-0.64,-0.635,-0.63,-0.625,-0.62,-0.615,-0.61,
-0.605,-0.6,-0.595,-0.59,-0.585,-0.58,-0.575,-0.57,-0.565,-0.56,-0.555,
-0.55,-0.545,-0.54,-0.535,-0.53,-0.525,-0.52,-0.515,-0.51,-0.505,-0.5,-0.495,
-0.49,-0.485,-0.48,-0.475,-0.47,-0.465,-0.46,-0.455,-0.45,-0.445,-0.44,
-0.435,-0.43,-0.425,-0.42,-0.415,-0.41,-0.405,-0.4,-0.395,-0.39,-0.385,
-0.38,-0.375,-0.37,-0.365,-0.36,-0.355,-0.35,-0.345,-0.34,-0.335,-0.33,
-0.325,-0.32,-0.315,-0.31,-0.305,-0.3,-0.295,-0.29,-0.285,-0.28,-0.275,
-0.27,-0.265,-0.26,-0.255,-0.25,-0.245,-0.24,-0.235,-0.23,-0.225,-0.22,
-0.215,-0.21,-0.205,-0.2,-0.195,-0.19,-0.185,-0.18,-0.175,-0.17,-0.165,
-0.16,-0.155,-0.15,-0.145,-0.14,-0.135,-0.13,-0.125,-0.12,-0.115,-0.11,
-0.105,-0.1,-0.095,-0.09,-0.085,-0.08,-0.075,-0.07,-0.065,-0.06,-0.055,
-0.05,-0.045,-0.04,-0.035,-0.03,-0.025,-0.02,-0.015,-0.01,-0.005,0.),(0.,
1.2),.UNSPECIFIED.)
GEOMETRIC_REPRESENTATION_ITEM()
RATIONAL_B_SPLINE_SURFACE(((1.,1.),(1.,1.),(1.,1.),(1.,1.),(1.,1.),(1.,
1.),(1.,1.),(1.,1.),(1.,1.),(1.,1.),(1.,1.),(1.,1.),(1.,1.),(1.,1.),(1.,
1.),(1.,1.),(1.,1.),(1.,1.),(1.,1.),(1.,1.),(1.,1.),(1.,1.),(1.,1.),(1.,
1.),(1.,1.),(1.,1.),(1.,1.),(1.,1.),(1.,1.),(1.,1.),(1.,1.),(1.,1.),(1.,
1.),(1.,1.),(1.,1.),(1.,1.),(1.,1.),(1.,1.),(1.,1.),(1.,1.),(1.,1.),(1.,
1.),(1.,1.),(1.,1.),(1.,1.),(1.,1.),(1.,1.),(1.,1.),(1.,1.),(1.,1.),(1.,
1.),(1.,1.),(1.,1.),(1.,1.),(1.,1.),(1.,1.),(1.,1.),(1.,1.),(1.,1.),(1.,
1.),(1.,1.),(1.,1.),(1.,1.),(1.,1.),(1.,1.),(1.,1.),(1.,1.),(1.,1.),(1.,
1.),(1.,1.),(1.,1.),(1.,1.),(1.,1.),(1.,1.),(1.,1.),(1.,1.),(1.,1.),(1.,
1.),(1.,1.),(1.,1.),(1.,1.),(1.,1.),(1.,1.),(1.,1.),(1.,1.),(1.,1.),(1.,
1.),(1.,1.),(1.,1.),(1.,1.),(1.,1.),(1.,1.),(1.,1.),(1.,1.),(1.,1.),(1.,
1.),(1.,1.),(1.,1.),(1.,1.),(1.,1.),(1.,1.),(1.,1.),(1.,1.),(1.,1.),(1.,
1.),(1.,1.),(1.,1.),(1.,1.),(1.,1.),(1.,1.),(1.,1.),(1.,1.),(1.,1.),(1.,
1.),(1.,1.),(1.,1.),(1.,1.),(1.,1.),(1.,1.),(1.,1.),(1.,1.),(1.,1.),(1.,
1.),(1.,1.),(1.,1.),(1.,1.),(1.,1.),(1.,1.),(1.,1.),(1.,1.),(1.,1.),(1.,
1.),(1.,1.),(1.,1.),(1.,1.),(1.,1.),(1.,1.),(1.,1.),(1.,1.),(1.,1.),(1.,
1.),(1.,1.),(1.,1.),(1.,1.),(1.,1.),(1.,1.),(1.,1.),(1.,1.),(1.,1.),(1.,
1.),(1.,1.),(1.,1.),(1.,1.),(1.,1.),(1.,1.),(1.,1.),(1.,1.),(1.,1.),(1.,
1.),(1.,1.),(1.,1.),(1.,1.),(1.,1.),(1.,1.),(1.,1.),(1.,1.),(1.,1.),(1.,
1.),(1.,1.),(1.,1.),(1.,1.),(1.,1.),(1.,1.),(1.,1.),(1.,1.),(1.,1.),(1.,
1.),(1.,1.),(1.,1.),(1.,1.),(1.,1.),(1.,1.),(1.,1.),(1.,1.),(1.,1.),(1.,
1.),(1.,1.),(1.,1.),(1.,1.),(1.,1.),(1.,1.),(1.,1.),(1.,1.),(1.,1.),(1.,
1.),(1.,1.),(1.,1.),(1.,1.),(1.,1.),(1.,1.),(1.,1.),(1.,1.),(1.,1.),(1.,
1.),(1.,1.)))
REPRESENTATION_ITEM('')
SURFACE()
);
#1008=(
BOUNDED_SURFACE()
B_SPLINE_SURFACE(5,1,((#159446,#159447),(#159448,#159449),(#159450,#159451),
(#159452,#159453),(#159454,#159455),(#159456,#159457),(#159458,#159459),
(#159460,#159461),(#159462,#159463),(#159464,#159465),(#159466,#159467),
(#159468,#159469),(#159470,#159471),(#159472,#159473),(#159474,#159475),
(#159476,#159477),(#159478,#159479),(#159480,#159481),(#159482,#159483),
(#159484,#159485),(#159486,#159487),(#159488,#159489),(#159490,#159491),
(#159492,#159493),(#159494,#159495),(#159496,#159497),(#159498,#159499),
(#159500,#159501),(#159502,#159503),(#159504,#159505),(#159506,#159507),
(#159508,#159509),(#159510,#159511),(#159512,#159513),(#159514,#159515),
(#159516,#159517),(#159518,#159519),(#159520,#159521),(#159522,#159523),
(#159524,#159525),(#159526,#159527),(#159528,#159529),(#159530,#159531),
(#159532,#159533),(#159534,#159535),(#159536,#159537),(#159538,#159539),
(#159540,#159541),(#159542,#159543),(#159544,#159545),(#159546,#159547),
(#159548,#159549),(#159550,#159551),(#159552,#159553),(#159554,#159555),
(#159556,#159557),(#159558,#159559),(#159560,#159561),(#159562,#159563),
(#159564,#159565),(#159566,#159567),(#159568,#159569),(#159570,#159571),
(#159572,#159573),(#159574,#159575),(#159576,#159577),(#159578,#159579),
(#159580,#159581),(#159582,#159583),(#159584,#159585),(#159586,#159587),
(#159588,#159589),(#159590,#159591),(#159592,#159593),(#159594,#159595),
(#159596,#159597),(#159598,#159599),(#159600,#159601),(#159602,#159603),
(#159604,#159605),(#159606,#159607),(#159608,#159609),(#159610,#159611),
(#159612,#159613),(#159614,#159615),(#159616,#159617),(#159618,#159619),
(#159620,#159621),(#159622,#159623),(#159624,#159625),(#159626,#159627),
(#159628,#159629),(#159630,#159631),(#159632,#159633),(#159634,#159635),
(#159636,#159637),(#159638,#159639),(#159640,#159641),(#159642,#159643),
(#159644,#159645),(#159646,#159647),(#159648,#159649),(#159650,#159651),
(#159652,#159653),(#159654,#159655),(#159656,#159657),(#159658,#159659),
(#159660,#159661),(#159662,#159663),(#159664,#159665),(#159666,#159667),
(#159668,#159669),(#159670,#159671),(#159672,#159673),(#159674,#159675),
(#159676,#159677),(#159678,#159679),(#159680,#159681),(#159682,#159683),
(#159684,#159685),(#159686,#159687),(#159688,#159689),(#159690,#159691),
(#159692,#159693),(#159694,#159695),(#159696,#159697),(#159698,#159699),
(#159700,#159701),(#159702,#159703),(#159704,#159705),(#159706,#159707),
(#159708,#159709),(#159710,#159711),(#159712,#159713),(#159714,#159715),
(#159716,#159717),(#159718,#159719),(#159720,#159721),(#159722,#159723),
(#159724,#159725),(#159726,#159727),(#159728,#159729),(#159730,#159731),
(#159732,#159733),(#159734,#159735),(#159736,#159737),(#159738,#159739),
(#159740,#159741),(#159742,#159743),(#159744,#159745),(#159746,#159747),
(#159748,#159749),(#159750,#159751),(#159752,#159753),(#159754,#159755),
(#159756,#159757),(#159758,#159759),(#159760,#159761),(#159762,#159763),
(#159764,#159765),(#159766,#159767),(#159768,#159769),(#159770,#159771),
(#159772,#159773),(#159774,#159775),(#159776,#159777),(#159778,#159779),
(#159780,#159781),(#159782,#159783),(#159784,#159785),(#159786,#159787),
(#159788,#159789),(#159790,#159791),(#159792,#159793),(#159794,#159795),
(#159796,#159797),(#159798,#159799),(#159800,#159801),(#159802,#159803),
(#159804,#159805),(#159806,#159807),(#159808,#159809),(#159810,#159811),
(#159812,#159813),(#159814,#159815),(#159816,#159817),(#159818,#159819),
(#159820,#159821),(#159822,#159823),(#159824,#159825),(#159826,#159827),
(#159828,#159829),(#159830,#159831),(#159832,#159833),(#159834,#159835),
(#159836,#159837),(#159838,#159839),(#159840,#159841),(#159842,#159843),
(#159844,#159845),(#159846,#159847),(#159848,#159849),(#159850,#159851),
(#159852,#159853),(#159854,#159855)),.UNSPECIFIED.,.F.,.F.,.F.)
B_SPLINE_SURFACE_WITH_KNOTS((6,1,1,1,1,1,1,1,1,1,1,1,1,1,1,1,1,1,1,1,1,
1,1,1,1,1,1,1,1,1,1,1,1,1,1,1,1,1,1,1,1,1,1,1,1,1,1,1,1,1,1,1,1,1,1,1,1,
1,1,1,1,1,1,1,1,1,1,1,1,1,1,1,1,1,1,1,1,1,1,1,1,1,1,1,1,1,1,1,1,1,1,1,1,
1,1,1,1,1,1,1,1,1,1,1,1,1,1,1,1,1,1,1,1,1,1,1,1,1,1,1,1,1,1,1,1,1,1,1,1,
1,1,1,1,1,1,1,1,1,1,1,1,1,1,1,1,1,1,1,1,1,1,1,1,1,1,1,1,1,1,1,1,1,1,1,1,
1,1,1,1,1,1,1,1,1,1,1,1,1,1,1,1,1,1,1,1,1,1,1,1,1,1,1,1,1,1,1,1,1,1,1,6),
(2,2),(-1.,-0.995000000000001,-0.990000000000001,-0.985000000000001,-0.980000000000001,
-0.975000000000001,-0.970000000000001,-0.965000000000001,-0.960000000000001,
-0.955000000000001,-0.950000000000001,-0.945000000000001,-0.940000000000001,
-0.935000000000001,-0.930000000000001,-0.925000000000001,-0.920000000000001,
-0.915000000000001,-0.910000000000001,-0.905000000000001,-0.900000000000001,
-0.895000000000001,-0.890000000000001,-0.885000000000001,-0.880000000000001,
-0.875000000000001,-0.870000000000001,-0.865000000000001,-0.860000000000001,
-0.855000000000001,-0.850000000000001,-0.845000000000001,-0.840000000000001,
-0.835000000000001,-0.830000000000001,-0.825000000000001,-0.820000000000001,
-0.815000000000001,-0.810000000000001,-0.805000000000001,-0.800000000000001,
-0.795000000000001,-0.790000000000001,-0.785000000000001,-0.780000000000001,
-0.775000000000001,-0.770000000000001,-0.765000000000001,-0.760000000000001,
-0.755000000000001,-0.750000000000001,-0.745000000000001,-0.740000000000001,
-0.735000000000001,-0.730000000000001,-0.725000000000001,-0.720000000000001,
-0.715000000000001,-0.710000000000001,-0.705000000000001,-0.700000000000001,
-0.695000000000001,-0.690000000000001,-0.685,-0.68,-0.675,-0.67,-0.665,
-0.66,-0.655,-0.65,-0.645,-0.64,-0.635,-0.63,-0.625,-0.62,-0.615,-0.61,
-0.605,-0.6,-0.595,-0.59,-0.585,-0.58,-0.575,-0.57,-0.565,-0.56,-0.555,
-0.55,-0.545,-0.54,-0.535,-0.53,-0.525,-0.52,-0.515,-0.51,-0.505,-0.5,-0.495,
-0.49,-0.485,-0.48,-0.475,-0.47,-0.465,-0.46,-0.455,-0.45,-0.445,-0.44,
-0.435,-0.43,-0.425,-0.42,-0.415,-0.41,-0.405,-0.4,-0.395,-0.39,-0.385,
-0.38,-0.375,-0.37,-0.365,-0.36,-0.355,-0.35,-0.345,-0.34,-0.335,-0.33,
-0.325,-0.32,-0.315,-0.31,-0.305,-0.3,-0.295,-0.29,-0.285,-0.28,-0.275,
-0.27,-0.265,-0.26,-0.255,-0.25,-0.245,-0.24,-0.235,-0.23,-0.225,-0.22,
-0.215,-0.21,-0.205,-0.2,-0.195,-0.19,-0.185,-0.18,-0.175,-0.17,-0.165,
-0.16,-0.155,-0.15,-0.145,-0.14,-0.135,-0.13,-0.125,-0.12,-0.115,-0.11,
-0.105,-0.1,-0.095,-0.09,-0.085,-0.08,-0.075,-0.07,-0.065,-0.06,-0.055,
-0.05,-0.045,-0.04,-0.035,-0.03,-0.025,-0.02,-0.015,-0.01,-0.005,0.),(0.,
1.2),.UNSPECIFIED.)
GEOMETRIC_REPRESENTATION_ITEM()
RATIONAL_B_SPLINE_SURFACE(((1.,1.),(1.,1.),(1.,1.),(1.,1.),(1.,1.),(1.,
1.),(1.,1.),(1.,1.),(1.,1.),(1.,1.),(1.,1.),(1.,1.),(1.,1.),(1.,1.),(1.,
1.),(1.,1.),(1.,1.),(1.,1.),(1.,1.),(1.,1.),(1.,1.),(1.,1.),(1.,1.),(1.,
1.),(1.,1.),(1.,1.),(1.,1.),(1.,1.),(1.,1.),(1.,1.),(1.,1.),(1.,1.),(1.,
1.),(1.,1.),(1.,1.),(1.,1.),(1.,1.),(1.,1.),(1.,1.),(1.,1.),(1.,1.),(1.,
1.),(1.,1.),(1.,1.),(1.,1.),(1.,1.),(1.,1.),(1.,1.),(1.,1.),(1.,1.),(1.,
1.),(1.,1.),(1.,1.),(1.,1.),(1.,1.),(1.,1.),(1.,1.),(1.,1.),(1.,1.),(1.,
1.),(1.,1.),(1.,1.),(1.,1.),(1.,1.),(1.,1.),(1.,1.),(1.,1.),(1.,1.),(1.,
1.),(1.,1.),(1.,1.),(1.,1.),(1.,1.),(1.,1.),(1.,1.),(1.,1.),(1.,1.),(1.,
1.),(1.,1.),(1.,1.),(1.,1.),(1.,1.),(1.,1.),(1.,1.),(1.,1.),(1.,1.),(1.,
1.),(1.,1.),(1.,1.),(1.,1.),(1.,1.),(1.,1.),(1.,1.),(1.,1.),(1.,1.),(1.,
1.),(1.,1.),(1.,1.),(1.,1.),(1.,1.),(1.,1.),(1.,1.),(1.,1.),(1.,1.),(1.,
1.),(1.,1.),(1.,1.),(1.,1.),(1.,1.),(1.,1.),(1.,1.),(1.,1.),(1.,1.),(1.,
1.),(1.,1.),(1.,1.),(1.,1.),(1.,1.),(1.,1.),(1.,1.),(1.,1.),(1.,1.),(1.,
1.),(1.,1.),(1.,1.),(1.,1.),(1.,1.),(1.,1.),(1.,1.),(1.,1.),(1.,1.),(1.,
1.),(1.,1.),(1.,1.),(1.,1.),(1.,1.),(1.,1.),(1.,1.),(1.,1.),(1.,1.),(1.,
1.),(1.,1.),(1.,1.),(1.,1.),(1.,1.),(1.,1.),(1.,1.),(1.,1.),(1.,1.),(1.,
1.),(1.,1.),(1.,1.),(1.,1.),(1.,1.),(1.,1.),(1.,1.),(1.,1.),(1.,1.),(1.,
1.),(1.,1.),(1.,1.),(1.,1.),(1.,1.),(1.,1.),(1.,1.),(1.,1.),(1.,1.),(1.,
1.),(1.,1.),(1.,1.),(1.,1.),(1.,1.),(1.,1.),(1.,1.),(1.,1.),(1.,1.),(1.,
1.),(1.,1.),(1.,1.),(1.,1.),(1.,1.),(1.,1.),(1.,1.),(1.,1.),(1.,1.),(1.,
1.),(1.,1.),(1.,1.),(1.,1.),(1.,1.),(1.,1.),(1.,1.),(1.,1.),(1.,1.),(1.,
1.),(1.,1.),(1.,1.),(1.,1.),(1.,1.),(1.,1.),(1.,1.),(1.,1.),(1.,1.),(1.,
1.),(1.,1.)))
REPRESENTATION_ITEM('')
SURFACE()
);
#1009=(
BOUNDED_SURFACE()
B_SPLINE_SURFACE(5,1,((#160247,#160248),(#160249,#160250),(#160251,#160252),
(#160253,#160254),(#160255,#160256),(#160257,#160258),(#160259,#160260),
(#160261,#160262),(#160263,#160264),(#160265,#160266),(#160267,#160268),
(#160269,#160270),(#160271,#160272),(#160273,#160274),(#160275,#160276),
(#160277,#160278),(#160279,#160280),(#160281,#160282),(#160283,#160284),
(#160285,#160286),(#160287,#160288),(#160289,#160290),(#160291,#160292),
(#160293,#160294),(#160295,#160296),(#160297,#160298),(#160299,#160300),
(#160301,#160302),(#160303,#160304),(#160305,#160306),(#160307,#160308),
(#160309,#160310),(#160311,#160312),(#160313,#160314),(#160315,#160316),
(#160317,#160318),(#160319,#160320),(#160321,#160322),(#160323,#160324),
(#160325,#160326),(#160327,#160328),(#160329,#160330),(#160331,#160332),
(#160333,#160334),(#160335,#160336),(#160337,#160338),(#160339,#160340),
(#160341,#160342),(#160343,#160344),(#160345,#160346),(#160347,#160348),
(#160349,#160350),(#160351,#160352),(#160353,#160354),(#160355,#160356),
(#160357,#160358),(#160359,#160360),(#160361,#160362),(#160363,#160364),
(#160365,#160366),(#160367,#160368),(#160369,#160370),(#160371,#160372),
(#160373,#160374),(#160375,#160376),(#160377,#160378),(#160379,#160380),
(#160381,#160382),(#160383,#160384),(#160385,#160386),(#160387,#160388),
(#160389,#160390),(#160391,#160392),(#160393,#160394),(#160395,#160396),
(#160397,#160398),(#160399,#160400),(#160401,#160402),(#160403,#160404),
(#160405,#160406),(#160407,#160408),(#160409,#160410),(#160411,#160412),
(#160413,#160414),(#160415,#160416),(#160417,#160418),(#160419,#160420),
(#160421,#160422),(#160423,#160424),(#160425,#160426),(#160427,#160428),
(#160429,#160430),(#160431,#160432),(#160433,#160434),(#160435,#160436),
(#160437,#160438),(#160439,#160440),(#160441,#160442),(#160443,#160444),
(#160445,#160446),(#160447,#160448),(#160449,#160450),(#160451,#160452),
(#160453,#160454),(#160455,#160456),(#160457,#160458),(#160459,#160460),
(#160461,#160462),(#160463,#160464),(#160465,#160466),(#160467,#160468),
(#160469,#160470),(#160471,#160472),(#160473,#160474),(#160475,#160476),
(#160477,#160478),(#160479,#160480),(#160481,#160482),(#160483,#160484),
(#160485,#160486),(#160487,#160488),(#160489,#160490),(#160491,#160492),
(#160493,#160494),(#160495,#160496),(#160497,#160498),(#160499,#160500),
(#160501,#160502),(#160503,#160504),(#160505,#160506),(#160507,#160508),
(#160509,#160510),(#160511,#160512),(#160513,#160514),(#160515,#160516),
(#160517,#160518),(#160519,#160520),(#160521,#160522),(#160523,#160524),
(#160525,#160526),(#160527,#160528),(#160529,#160530),(#160531,#160532),
(#160533,#160534),(#160535,#160536),(#160537,#160538),(#160539,#160540),
(#160541,#160542),(#160543,#160544),(#160545,#160546),(#160547,#160548),
(#160549,#160550),(#160551,#160552),(#160553,#160554),(#160555,#160556),
(#160557,#160558),(#160559,#160560),(#160561,#160562),(#160563,#160564),
(#160565,#160566),(#160567,#160568),(#160569,#160570),(#160571,#160572),
(#160573,#160574),(#160575,#160576),(#160577,#160578),(#160579,#160580),
(#160581,#160582),(#160583,#160584),(#160585,#160586),(#160587,#160588),
(#160589,#160590),(#160591,#160592),(#160593,#160594),(#160595,#160596),
(#160597,#160598),(#160599,#160600),(#160601,#160602),(#160603,#160604),
(#160605,#160606),(#160607,#160608),(#160609,#160610),(#160611,#160612),
(#160613,#160614),(#160615,#160616),(#160617,#160618),(#160619,#160620),
(#160621,#160622),(#160623,#160624),(#160625,#160626),(#160627,#160628),
(#160629,#160630),(#160631,#160632),(#160633,#160634),(#160635,#160636),
(#160637,#160638),(#160639,#160640),(#160641,#160642),(#160643,#160644),
(#160645,#160646),(#160647,#160648),(#160649,#160650),(#160651,#160652),
(#160653,#160654),(#160655,#160656)),.UNSPECIFIED.,.F.,.F.,.F.)
B_SPLINE_SURFACE_WITH_KNOTS((6,1,1,1,1,1,1,1,1,1,1,1,1,1,1,1,1,1,1,1,1,
1,1,1,1,1,1,1,1,1,1,1,1,1,1,1,1,1,1,1,1,1,1,1,1,1,1,1,1,1,1,1,1,1,1,1,1,
1,1,1,1,1,1,1,1,1,1,1,1,1,1,1,1,1,1,1,1,1,1,1,1,1,1,1,1,1,1,1,1,1,1,1,1,
1,1,1,1,1,1,1,1,1,1,1,1,1,1,1,1,1,1,1,1,1,1,1,1,1,1,1,1,1,1,1,1,1,1,1,1,
1,1,1,1,1,1,1,1,1,1,1,1,1,1,1,1,1,1,1,1,1,1,1,1,1,1,1,1,1,1,1,1,1,1,1,1,
1,1,1,1,1,1,1,1,1,1,1,1,1,1,1,1,1,1,1,1,1,1,1,1,1,1,1,1,1,1,1,1,1,1,1,6),
(2,2),(-1.,-0.995000000000001,-0.990000000000001,-0.985000000000001,-0.980000000000001,
-0.975000000000001,-0.970000000000001,-0.965000000000001,-0.960000000000001,
-0.955000000000001,-0.950000000000001,-0.945000000000001,-0.940000000000001,
-0.935000000000001,-0.930000000000001,-0.925000000000001,-0.920000000000001,
-0.915000000000001,-0.910000000000001,-0.905000000000001,-0.900000000000001,
-0.895000000000001,-0.890000000000001,-0.885000000000001,-0.880000000000001,
-0.875000000000001,-0.870000000000001,-0.865000000000001,-0.860000000000001,
-0.855000000000001,-0.850000000000001,-0.845000000000001,-0.840000000000001,
-0.835000000000001,-0.830000000000001,-0.825000000000001,-0.820000000000001,
-0.815000000000001,-0.810000000000001,-0.805000000000001,-0.800000000000001,
-0.795000000000001,-0.790000000000001,-0.785000000000001,-0.780000000000001,
-0.775000000000001,-0.770000000000001,-0.765000000000001,-0.760000000000001,
-0.755000000000001,-0.750000000000001,-0.745000000000001,-0.740000000000001,
-0.735000000000001,-0.730000000000001,-0.725000000000001,-0.720000000000001,
-0.715000000000001,-0.710000000000001,-0.705000000000001,-0.700000000000001,
-0.695000000000001,-0.690000000000001,-0.685,-0.68,-0.675,-0.67,-0.665,
-0.66,-0.655,-0.65,-0.645,-0.64,-0.635,-0.63,-0.625,-0.62,-0.615,-0.61,
-0.605,-0.6,-0.595,-0.59,-0.585,-0.58,-0.575,-0.57,-0.565,-0.56,-0.555,
-0.55,-0.545,-0.54,-0.535,-0.53,-0.525,-0.52,-0.515,-0.51,-0.505,-0.5,-0.495,
-0.49,-0.485,-0.48,-0.475,-0.47,-0.465,-0.46,-0.455,-0.45,-0.445,-0.44,
-0.435,-0.43,-0.425,-0.42,-0.415,-0.41,-0.405,-0.4,-0.395,-0.39,-0.385,
-0.38,-0.375,-0.37,-0.365,-0.36,-0.355,-0.35,-0.345,-0.34,-0.335,-0.33,
-0.325,-0.32,-0.315,-0.31,-0.305,-0.3,-0.295,-0.29,-0.285,-0.28,-0.275,
-0.27,-0.265,-0.26,-0.255,-0.25,-0.245,-0.24,-0.235,-0.23,-0.225,-0.22,
-0.215,-0.21,-0.205,-0.2,-0.195,-0.19,-0.185,-0.18,-0.175,-0.17,-0.165,
-0.16,-0.155,-0.15,-0.145,-0.14,-0.135,-0.13,-0.125,-0.12,-0.115,-0.11,
-0.105,-0.1,-0.095,-0.09,-0.085,-0.08,-0.075,-0.07,-0.065,-0.06,-0.055,
-0.05,-0.045,-0.04,-0.035,-0.03,-0.025,-0.02,-0.015,-0.01,-0.005,0.),(0.,
1.2),.UNSPECIFIED.)
GEOMETRIC_REPRESENTATION_ITEM()
RATIONAL_B_SPLINE_SURFACE(((1.,1.),(1.,1.),(1.,1.),(1.,1.),(1.,1.),(1.,
1.),(1.,1.),(1.,1.),(1.,1.),(1.,1.),(1.,1.),(1.,1.),(1.,1.),(1.,1.),(1.,
1.),(1.,1.),(1.,1.),(1.,1.),(1.,1.),(1.,1.),(1.,1.),(1.,1.),(1.,1.),(1.,
1.),(1.,1.),(1.,1.),(1.,1.),(1.,1.),(1.,1.),(1.,1.),(1.,1.),(1.,1.),(1.,
1.),(1.,1.),(1.,1.),(1.,1.),(1.,1.),(1.,1.),(1.,1.),(1.,1.),(1.,1.),(1.,
1.),(1.,1.),(1.,1.),(1.,1.),(1.,1.),(1.,1.),(1.,1.),(1.,1.),(1.,1.),(1.,
1.),(1.,1.),(1.,1.),(1.,1.),(1.,1.),(1.,1.),(1.,1.),(1.,1.),(1.,1.),(1.,
1.),(1.,1.),(1.,1.),(1.,1.),(1.,1.),(1.,1.),(1.,1.),(1.,1.),(1.,1.),(1.,
1.),(1.,1.),(1.,1.),(1.,1.),(1.,1.),(1.,1.),(1.,1.),(1.,1.),(1.,1.),(1.,
1.),(1.,1.),(1.,1.),(1.,1.),(1.,1.),(1.,1.),(1.,1.),(1.,1.),(1.,1.),(1.,
1.),(1.,1.),(1.,1.),(1.,1.),(1.,1.),(1.,1.),(1.,1.),(1.,1.),(1.,1.),(1.,
1.),(1.,1.),(1.,1.),(1.,1.),(1.,1.),(1.,1.),(1.,1.),(1.,1.),(1.,1.),(1.,
1.),(1.,1.),(1.,1.),(1.,1.),(1.,1.),(1.,1.),(1.,1.),(1.,1.),(1.,1.),(1.,
1.),(1.,1.),(1.,1.),(1.,1.),(1.,1.),(1.,1.),(1.,1.),(1.,1.),(1.,1.),(1.,
1.),(1.,1.),(1.,1.),(1.,1.),(1.,1.),(1.,1.),(1.,1.),(1.,1.),(1.,1.),(1.,
1.),(1.,1.),(1.,1.),(1.,1.),(1.,1.),(1.,1.),(1.,1.),(1.,1.),(1.,1.),(1.,
1.),(1.,1.),(1.,1.),(1.,1.),(1.,1.),(1.,1.),(1.,1.),(1.,1.),(1.,1.),(1.,
1.),(1.,1.),(1.,1.),(1.,1.),(1.,1.),(1.,1.),(1.,1.),(1.,1.),(1.,1.),(1.,
1.),(1.,1.),(1.,1.),(1.,1.),(1.,1.),(1.,1.),(1.,1.),(1.,1.),(1.,1.),(1.,
1.),(1.,1.),(1.,1.),(1.,1.),(1.,1.),(1.,1.),(1.,1.),(1.,1.),(1.,1.),(1.,
1.),(1.,1.),(1.,1.),(1.,1.),(1.,1.),(1.,1.),(1.,1.),(1.,1.),(1.,1.),(1.,
1.),(1.,1.),(1.,1.),(1.,1.),(1.,1.),(1.,1.),(1.,1.),(1.,1.),(1.,1.),(1.,
1.),(1.,1.),(1.,1.),(1.,1.),(1.,1.),(1.,1.),(1.,1.),(1.,1.),(1.,1.),(1.,
1.),(1.,1.)))
REPRESENTATION_ITEM('')
SURFACE()
);
#1010=(
BOUNDED_SURFACE()
B_SPLINE_SURFACE(5,1,((#161048,#161049),(#161050,#161051),(#161052,#161053),
(#161054,#161055),(#161056,#161057),(#161058,#161059),(#161060,#161061),
(#161062,#161063),(#161064,#161065),(#161066,#161067),(#161068,#161069),
(#161070,#161071),(#161072,#161073),(#161074,#161075),(#161076,#161077),
(#161078,#161079),(#161080,#161081),(#161082,#161083),(#161084,#161085),
(#161086,#161087),(#161088,#161089),(#161090,#161091),(#161092,#161093),
(#161094,#161095),(#161096,#161097),(#161098,#161099),(#161100,#161101),
(#161102,#161103),(#161104,#161105),(#161106,#161107),(#161108,#161109),
(#161110,#161111),(#161112,#161113),(#161114,#161115),(#161116,#161117),
(#161118,#161119),(#161120,#161121),(#161122,#161123),(#161124,#161125),
(#161126,#161127),(#161128,#161129),(#161130,#161131),(#161132,#161133),
(#161134,#161135),(#161136,#161137),(#161138,#161139),(#161140,#161141),
(#161142,#161143),(#161144,#161145),(#161146,#161147),(#161148,#161149),
(#161150,#161151),(#161152,#161153),(#161154,#161155),(#161156,#161157),
(#161158,#161159),(#161160,#161161),(#161162,#161163),(#161164,#161165),
(#161166,#161167),(#161168,#161169),(#161170,#161171),(#161172,#161173),
(#161174,#161175),(#161176,#161177),(#161178,#161179),(#161180,#161181),
(#161182,#161183),(#161184,#161185),(#161186,#161187),(#161188,#161189),
(#161190,#161191),(#161192,#161193),(#161194,#161195),(#161196,#161197),
(#161198,#161199),(#161200,#161201),(#161202,#161203),(#161204,#161205),
(#161206,#161207),(#161208,#161209),(#161210,#161211),(#161212,#161213),
(#161214,#161215),(#161216,#161217),(#161218,#161219),(#161220,#161221),
(#161222,#161223),(#161224,#161225),(#161226,#161227),(#161228,#161229),
(#161230,#161231),(#161232,#161233),(#161234,#161235),(#161236,#161237),
(#161238,#161239),(#161240,#161241),(#161242,#161243),(#161244,#161245),
(#161246,#161247),(#161248,#161249),(#161250,#161251),(#161252,#161253),
(#161254,#161255),(#161256,#161257),(#161258,#161259),(#161260,#161261),
(#161262,#161263),(#161264,#161265),(#161266,#161267),(#161268,#161269),
(#161270,#161271),(#161272,#161273),(#161274,#161275),(#161276,#161277),
(#161278,#161279),(#161280,#161281),(#161282,#161283),(#161284,#161285),
(#161286,#161287),(#161288,#161289),(#161290,#161291),(#161292,#161293),
(#161294,#161295),(#161296,#161297),(#161298,#161299),(#161300,#161301),
(#161302,#161303),(#161304,#161305),(#161306,#161307),(#161308,#161309),
(#161310,#161311),(#161312,#161313),(#161314,#161315),(#161316,#161317),
(#161318,#161319),(#161320,#161321),(#161322,#161323),(#161324,#161325),
(#161326,#161327),(#161328,#161329),(#161330,#161331),(#161332,#161333),
(#161334,#161335),(#161336,#161337),(#161338,#161339),(#161340,#161341),
(#161342,#161343),(#161344,#161345),(#161346,#161347),(#161348,#161349),
(#161350,#161351),(#161352,#161353),(#161354,#161355),(#161356,#161357),
(#161358,#161359),(#161360,#161361),(#161362,#161363),(#161364,#161365),
(#161366,#161367),(#161368,#161369),(#161370,#161371),(#161372,#161373),
(#161374,#161375),(#161376,#161377),(#161378,#161379),(#161380,#161381),
(#161382,#161383),(#161384,#161385),(#161386,#161387),(#161388,#161389),
(#161390,#161391),(#161392,#161393),(#161394,#161395),(#161396,#161397),
(#161398,#161399),(#161400,#161401),(#161402,#161403),(#161404,#161405),
(#161406,#161407),(#161408,#161409),(#161410,#161411),(#161412,#161413),
(#161414,#161415),(#161416,#161417),(#161418,#161419),(#161420,#161421),
(#161422,#161423),(#161424,#161425),(#161426,#161427),(#161428,#161429),
(#161430,#161431),(#161432,#161433),(#161434,#161435),(#161436,#161437),
(#161438,#161439),(#161440,#161441),(#161442,#161443),(#161444,#161445),
(#161446,#161447),(#161448,#161449),(#161450,#161451),(#161452,#161453),
(#161454,#161455),(#161456,#161457)),.UNSPECIFIED.,.F.,.F.,.F.)
B_SPLINE_SURFACE_WITH_KNOTS((6,1,1,1,1,1,1,1,1,1,1,1,1,1,1,1,1,1,1,1,1,
1,1,1,1,1,1,1,1,1,1,1,1,1,1,1,1,1,1,1,1,1,1,1,1,1,1,1,1,1,1,1,1,1,1,1,1,
1,1,1,1,1,1,1,1,1,1,1,1,1,1,1,1,1,1,1,1,1,1,1,1,1,1,1,1,1,1,1,1,1,1,1,1,
1,1,1,1,1,1,1,1,1,1,1,1,1,1,1,1,1,1,1,1,1,1,1,1,1,1,1,1,1,1,1,1,1,1,1,1,
1,1,1,1,1,1,1,1,1,1,1,1,1,1,1,1,1,1,1,1,1,1,1,1,1,1,1,1,1,1,1,1,1,1,1,1,
1,1,1,1,1,1,1,1,1,1,1,1,1,1,1,1,1,1,1,1,1,1,1,1,1,1,1,1,1,1,1,1,1,1,1,6),
(2,2),(-1.,-0.995000000000001,-0.990000000000001,-0.985000000000001,-0.980000000000001,
-0.975000000000001,-0.970000000000001,-0.965000000000001,-0.960000000000001,
-0.955000000000001,-0.950000000000001,-0.945000000000001,-0.940000000000001,
-0.935000000000001,-0.930000000000001,-0.925000000000001,-0.920000000000001,
-0.915000000000001,-0.910000000000001,-0.905000000000001,-0.900000000000001,
-0.895000000000001,-0.890000000000001,-0.885000000000001,-0.880000000000001,
-0.875000000000001,-0.870000000000001,-0.865000000000001,-0.860000000000001,
-0.855000000000001,-0.850000000000001,-0.845000000000001,-0.840000000000001,
-0.835000000000001,-0.830000000000001,-0.825000000000001,-0.820000000000001,
-0.815000000000001,-0.810000000000001,-0.805000000000001,-0.800000000000001,
-0.795000000000001,-0.790000000000001,-0.785000000000001,-0.780000000000001,
-0.775000000000001,-0.770000000000001,-0.765000000000001,-0.760000000000001,
-0.755000000000001,-0.750000000000001,-0.745000000000001,-0.740000000000001,
-0.735000000000001,-0.730000000000001,-0.725000000000001,-0.720000000000001,
-0.715000000000001,-0.710000000000001,-0.705000000000001,-0.700000000000001,
-0.695000000000001,-0.690000000000001,-0.685,-0.68,-0.675,-0.67,-0.665,
-0.66,-0.655,-0.65,-0.645,-0.64,-0.635,-0.63,-0.625,-0.62,-0.615,-0.61,
-0.605,-0.6,-0.595,-0.59,-0.585,-0.58,-0.575,-0.57,-0.565,-0.56,-0.555,
-0.55,-0.545,-0.54,-0.535,-0.53,-0.525,-0.52,-0.515,-0.51,-0.505,-0.5,-0.495,
-0.49,-0.485,-0.48,-0.475,-0.47,-0.465,-0.46,-0.455,-0.45,-0.445,-0.44,
-0.435,-0.43,-0.425,-0.42,-0.415,-0.41,-0.405,-0.4,-0.395,-0.39,-0.385,
-0.38,-0.375,-0.37,-0.365,-0.36,-0.355,-0.35,-0.345,-0.34,-0.335,-0.33,
-0.325,-0.32,-0.315,-0.31,-0.305,-0.3,-0.295,-0.29,-0.285,-0.28,-0.275,
-0.27,-0.265,-0.26,-0.255,-0.25,-0.245,-0.24,-0.235,-0.23,-0.225,-0.22,
-0.215,-0.21,-0.205,-0.2,-0.195,-0.19,-0.185,-0.18,-0.175,-0.17,-0.165,
-0.16,-0.155,-0.15,-0.145,-0.14,-0.135,-0.13,-0.125,-0.12,-0.115,-0.11,
-0.105,-0.1,-0.095,-0.09,-0.085,-0.08,-0.075,-0.07,-0.065,-0.06,-0.055,
-0.05,-0.045,-0.04,-0.035,-0.03,-0.025,-0.02,-0.015,-0.01,-0.005,0.),(0.,
1.2),.UNSPECIFIED.)
GEOMETRIC_REPRESENTATION_ITEM()
RATIONAL_B_SPLINE_SURFACE(((1.,1.),(1.,1.),(1.,1.),(1.,1.),(1.,1.),(1.,
1.),(1.,1.),(1.,1.),(1.,1.),(1.,1.),(1.,1.),(1.,1.),(1.,1.),(1.,1.),(1.,
1.),(1.,1.),(1.,1.),(1.,1.),(1.,1.),(1.,1.),(1.,1.),(1.,1.),(1.,1.),(1.,
1.),(1.,1.),(1.,1.),(1.,1.),(1.,1.),(1.,1.),(1.,1.),(1.,1.),(1.,1.),(1.,
1.),(1.,1.),(1.,1.),(1.,1.),(1.,1.),(1.,1.),(1.,1.),(1.,1.),(1.,1.),(1.,
1.),(1.,1.),(1.,1.),(1.,1.),(1.,1.),(1.,1.),(1.,1.),(1.,1.),(1.,1.),(1.,
1.),(1.,1.),(1.,1.),(1.,1.),(1.,1.),(1.,1.),(1.,1.),(1.,1.),(1.,1.),(1.,
1.),(1.,1.),(1.,1.),(1.,1.),(1.,1.),(1.,1.),(1.,1.),(1.,1.),(1.,1.),(1.,
1.),(1.,1.),(1.,1.),(1.,1.),(1.,1.),(1.,1.),(1.,1.),(1.,1.),(1.,1.),(1.,
1.),(1.,1.),(1.,1.),(1.,1.),(1.,1.),(1.,1.),(1.,1.),(1.,1.),(1.,1.),(1.,
1.),(1.,1.),(1.,1.),(1.,1.),(1.,1.),(1.,1.),(1.,1.),(1.,1.),(1.,1.),(1.,
1.),(1.,1.),(1.,1.),(1.,1.),(1.,1.),(1.,1.),(1.,1.),(1.,1.),(1.,1.),(1.,
1.),(1.,1.),(1.,1.),(1.,1.),(1.,1.),(1.,1.),(1.,1.),(1.,1.),(1.,1.),(1.,
1.),(1.,1.),(1.,1.),(1.,1.),(1.,1.),(1.,1.),(1.,1.),(1.,1.),(1.,1.),(1.,
1.),(1.,1.),(1.,1.),(1.,1.),(1.,1.),(1.,1.),(1.,1.),(1.,1.),(1.,1.),(1.,
1.),(1.,1.),(1.,1.),(1.,1.),(1.,1.),(1.,1.),(1.,1.),(1.,1.),(1.,1.),(1.,
1.),(1.,1.),(1.,1.),(1.,1.),(1.,1.),(1.,1.),(1.,1.),(1.,1.),(1.,1.),(1.,
1.),(1.,1.),(1.,1.),(1.,1.),(1.,1.),(1.,1.),(1.,1.),(1.,1.),(1.,1.),(1.,
1.),(1.,1.),(1.,1.),(1.,1.),(1.,1.),(1.,1.),(1.,1.),(1.,1.),(1.,1.),(1.,
1.),(1.,1.),(1.,1.),(1.,1.),(1.,1.),(1.,1.),(1.,1.),(1.,1.),(1.,1.),(1.,
1.),(1.,1.),(1.,1.),(1.,1.),(1.,1.),(1.,1.),(1.,1.),(1.,1.),(1.,1.),(1.,
1.),(1.,1.),(1.,1.),(1.,1.),(1.,1.),(1.,1.),(1.,1.),(1.,1.),(1.,1.),(1.,
1.),(1.,1.),(1.,1.),(1.,1.),(1.,1.),(1.,1.),(1.,1.),(1.,1.),(1.,1.),(1.,
1.),(1.,1.)))
REPRESENTATION_ITEM('')
SURFACE()
);
#1011=(
BOUNDED_SURFACE()
B_SPLINE_SURFACE(5,1,((#161849,#161850),(#161851,#161852),(#161853,#161854),
(#161855,#161856),(#161857,#161858),(#161859,#161860),(#161861,#161862),
(#161863,#161864),(#161865,#161866),(#161867,#161868),(#161869,#161870),
(#161871,#161872),(#161873,#161874),(#161875,#161876),(#161877,#161878),
(#161879,#161880),(#161881,#161882),(#161883,#161884),(#161885,#161886),
(#161887,#161888),(#161889,#161890),(#161891,#161892),(#161893,#161894),
(#161895,#161896),(#161897,#161898),(#161899,#161900),(#161901,#161902),
(#161903,#161904),(#161905,#161906),(#161907,#161908),(#161909,#161910),
(#161911,#161912),(#161913,#161914),(#161915,#161916),(#161917,#161918),
(#161919,#161920),(#161921,#161922),(#161923,#161924),(#161925,#161926),
(#161927,#161928),(#161929,#161930),(#161931,#161932),(#161933,#161934),
(#161935,#161936),(#161937,#161938),(#161939,#161940),(#161941,#161942),
(#161943,#161944),(#161945,#161946),(#161947,#161948),(#161949,#161950),
(#161951,#161952),(#161953,#161954),(#161955,#161956),(#161957,#161958),
(#161959,#161960),(#161961,#161962),(#161963,#161964),(#161965,#161966),
(#161967,#161968),(#161969,#161970),(#161971,#161972),(#161973,#161974),
(#161975,#161976),(#161977,#161978),(#161979,#161980),(#161981,#161982),
(#161983,#161984),(#161985,#161986),(#161987,#161988),(#161989,#161990),
(#161991,#161992),(#161993,#161994),(#161995,#161996),(#161997,#161998),
(#161999,#162000),(#162001,#162002),(#162003,#162004),(#162005,#162006),
(#162007,#162008),(#162009,#162010),(#162011,#162012),(#162013,#162014),
(#162015,#162016),(#162017,#162018),(#162019,#162020),(#162021,#162022),
(#162023,#162024),(#162025,#162026),(#162027,#162028),(#162029,#162030),
(#162031,#162032),(#162033,#162034),(#162035,#162036),(#162037,#162038),
(#162039,#162040),(#162041,#162042),(#162043,#162044),(#162045,#162046),
(#162047,#162048),(#162049,#162050),(#162051,#162052),(#162053,#162054),
(#162055,#162056),(#162057,#162058),(#162059,#162060),(#162061,#162062),
(#162063,#162064),(#162065,#162066),(#162067,#162068),(#162069,#162070),
(#162071,#162072),(#162073,#162074),(#162075,#162076),(#162077,#162078),
(#162079,#162080),(#162081,#162082),(#162083,#162084),(#162085,#162086),
(#162087,#162088),(#162089,#162090),(#162091,#162092),(#162093,#162094),
(#162095,#162096),(#162097,#162098),(#162099,#162100),(#162101,#162102),
(#162103,#162104),(#162105,#162106),(#162107,#162108),(#162109,#162110),
(#162111,#162112),(#162113,#162114),(#162115,#162116),(#162117,#162118),
(#162119,#162120),(#162121,#162122),(#162123,#162124),(#162125,#162126),
(#162127,#162128),(#162129,#162130),(#162131,#162132),(#162133,#162134),
(#162135,#162136),(#162137,#162138),(#162139,#162140),(#162141,#162142),
(#162143,#162144),(#162145,#162146),(#162147,#162148),(#162149,#162150),
(#162151,#162152),(#162153,#162154),(#162155,#162156),(#162157,#162158),
(#162159,#162160),(#162161,#162162),(#162163,#162164),(#162165,#162166),
(#162167,#162168),(#162169,#162170),(#162171,#162172),(#162173,#162174),
(#162175,#162176),(#162177,#162178),(#162179,#162180),(#162181,#162182),
(#162183,#162184),(#162185,#162186),(#162187,#162188),(#162189,#162190),
(#162191,#162192),(#162193,#162194),(#162195,#162196),(#162197,#162198),
(#162199,#162200),(#162201,#162202),(#162203,#162204),(#162205,#162206),
(#162207,#162208),(#162209,#162210),(#162211,#162212),(#162213,#162214),
(#162215,#162216),(#162217,#162218),(#162219,#162220),(#162221,#162222),
(#162223,#162224),(#162225,#162226),(#162227,#162228),(#162229,#162230),
(#162231,#162232),(#162233,#162234),(#162235,#162236),(#162237,#162238),
(#162239,#162240),(#162241,#162242),(#162243,#162244),(#162245,#162246),
(#162247,#162248),(#162249,#162250),(#162251,#162252),(#162253,#162254),
(#162255,#162256),(#162257,#162258)),.UNSPECIFIED.,.F.,.F.,.F.)
B_SPLINE_SURFACE_WITH_KNOTS((6,1,1,1,1,1,1,1,1,1,1,1,1,1,1,1,1,1,1,1,1,
1,1,1,1,1,1,1,1,1,1,1,1,1,1,1,1,1,1,1,1,1,1,1,1,1,1,1,1,1,1,1,1,1,1,1,1,
1,1,1,1,1,1,1,1,1,1,1,1,1,1,1,1,1,1,1,1,1,1,1,1,1,1,1,1,1,1,1,1,1,1,1,1,
1,1,1,1,1,1,1,1,1,1,1,1,1,1,1,1,1,1,1,1,1,1,1,1,1,1,1,1,1,1,1,1,1,1,1,1,
1,1,1,1,1,1,1,1,1,1,1,1,1,1,1,1,1,1,1,1,1,1,1,1,1,1,1,1,1,1,1,1,1,1,1,1,
1,1,1,1,1,1,1,1,1,1,1,1,1,1,1,1,1,1,1,1,1,1,1,1,1,1,1,1,1,1,1,1,1,1,1,6),
(2,2),(-1.,-0.995000000000001,-0.990000000000001,-0.985000000000001,-0.980000000000001,
-0.975000000000001,-0.970000000000001,-0.965000000000001,-0.960000000000001,
-0.955000000000001,-0.950000000000001,-0.945000000000001,-0.940000000000001,
-0.935000000000001,-0.930000000000001,-0.925000000000001,-0.920000000000001,
-0.915000000000001,-0.910000000000001,-0.905000000000001,-0.900000000000001,
-0.895000000000001,-0.890000000000001,-0.885000000000001,-0.880000000000001,
-0.875000000000001,-0.870000000000001,-0.865000000000001,-0.860000000000001,
-0.855000000000001,-0.850000000000001,-0.845000000000001,-0.840000000000001,
-0.835000000000001,-0.830000000000001,-0.825000000000001,-0.820000000000001,
-0.815000000000001,-0.810000000000001,-0.805000000000001,-0.800000000000001,
-0.795000000000001,-0.790000000000001,-0.785000000000001,-0.780000000000001,
-0.775000000000001,-0.770000000000001,-0.765000000000001,-0.760000000000001,
-0.755000000000001,-0.750000000000001,-0.745000000000001,-0.740000000000001,
-0.735000000000001,-0.730000000000001,-0.725000000000001,-0.720000000000001,
-0.715000000000001,-0.710000000000001,-0.705000000000001,-0.700000000000001,
-0.695000000000001,-0.690000000000001,-0.685,-0.68,-0.675,-0.67,-0.665,
-0.66,-0.655,-0.65,-0.645,-0.64,-0.635,-0.63,-0.625,-0.62,-0.615,-0.61,
-0.605,-0.6,-0.595,-0.59,-0.585,-0.58,-0.575,-0.57,-0.565,-0.56,-0.555,
-0.55,-0.545,-0.54,-0.535,-0.53,-0.525,-0.52,-0.515,-0.51,-0.505,-0.5,-0.495,
-0.49,-0.485,-0.48,-0.475,-0.47,-0.465,-0.46,-0.455,-0.45,-0.445,-0.44,
-0.435,-0.43,-0.425,-0.42,-0.415,-0.41,-0.405,-0.4,-0.395,-0.39,-0.385,
-0.38,-0.375,-0.37,-0.365,-0.36,-0.355,-0.35,-0.345,-0.34,-0.335,-0.33,
-0.325,-0.32,-0.315,-0.31,-0.305,-0.3,-0.295,-0.29,-0.285,-0.28,-0.275,
-0.27,-0.265,-0.26,-0.255,-0.25,-0.245,-0.24,-0.235,-0.23,-0.225,-0.22,
-0.215,-0.21,-0.205,-0.2,-0.195,-0.19,-0.185,-0.18,-0.175,-0.17,-0.165,
-0.16,-0.155,-0.15,-0.145,-0.14,-0.135,-0.13,-0.125,-0.12,-0.115,-0.11,
-0.105,-0.1,-0.095,-0.09,-0.085,-0.08,-0.075,-0.07,-0.065,-0.06,-0.055,
-0.05,-0.045,-0.04,-0.035,-0.03,-0.025,-0.02,-0.015,-0.01,-0.005,0.),(0.,
1.2),.UNSPECIFIED.)
GEOMETRIC_REPRESENTATION_ITEM()
RATIONAL_B_SPLINE_SURFACE(((1.,1.),(1.,1.),(1.,1.),(1.,1.),(1.,1.),(1.,
1.),(1.,1.),(1.,1.),(1.,1.),(1.,1.),(1.,1.),(1.,1.),(1.,1.),(1.,1.),(1.,
1.),(1.,1.),(1.,1.),(1.,1.),(1.,1.),(1.,1.),(1.,1.),(1.,1.),(1.,1.),(1.,
1.),(1.,1.),(1.,1.),(1.,1.),(1.,1.),(1.,1.),(1.,1.),(1.,1.),(1.,1.),(1.,
1.),(1.,1.),(1.,1.),(1.,1.),(1.,1.),(1.,1.),(1.,1.),(1.,1.),(1.,1.),(1.,
1.),(1.,1.),(1.,1.),(1.,1.),(1.,1.),(1.,1.),(1.,1.),(1.,1.),(1.,1.),(1.,
1.),(1.,1.),(1.,1.),(1.,1.),(1.,1.),(1.,1.),(1.,1.),(1.,1.),(1.,1.),(1.,
1.),(1.,1.),(1.,1.),(1.,1.),(1.,1.),(1.,1.),(1.,1.),(1.,1.),(1.,1.),(1.,
1.),(1.,1.),(1.,1.),(1.,1.),(1.,1.),(1.,1.),(1.,1.),(1.,1.),(1.,1.),(1.,
1.),(1.,1.),(1.,1.),(1.,1.),(1.,1.),(1.,1.),(1.,1.),(1.,1.),(1.,1.),(1.,
1.),(1.,1.),(1.,1.),(1.,1.),(1.,1.),(1.,1.),(1.,1.),(1.,1.),(1.,1.),(1.,
1.),(1.,1.),(1.,1.),(1.,1.),(1.,1.),(1.,1.),(1.,1.),(1.,1.),(1.,1.),(1.,
1.),(1.,1.),(1.,1.),(1.,1.),(1.,1.),(1.,1.),(1.,1.),(1.,1.),(1.,1.),(1.,
1.),(1.,1.),(1.,1.),(1.,1.),(1.,1.),(1.,1.),(1.,1.),(1.,1.),(1.,1.),(1.,
1.),(1.,1.),(1.,1.),(1.,1.),(1.,1.),(1.,1.),(1.,1.),(1.,1.),(1.,1.),(1.,
1.),(1.,1.),(1.,1.),(1.,1.),(1.,1.),(1.,1.),(1.,1.),(1.,1.),(1.,1.),(1.,
1.),(1.,1.),(1.,1.),(1.,1.),(1.,1.),(1.,1.),(1.,1.),(1.,1.),(1.,1.),(1.,
1.),(1.,1.),(1.,1.),(1.,1.),(1.,1.),(1.,1.),(1.,1.),(1.,1.),(1.,1.),(1.,
1.),(1.,1.),(1.,1.),(1.,1.),(1.,1.),(1.,1.),(1.,1.),(1.,1.),(1.,1.),(1.,
1.),(1.,1.),(1.,1.),(1.,1.),(1.,1.),(1.,1.),(1.,1.),(1.,1.),(1.,1.),(1.,
1.),(1.,1.),(1.,1.),(1.,1.),(1.,1.),(1.,1.),(1.,1.),(1.,1.),(1.,1.),(1.,
1.),(1.,1.),(1.,1.),(1.,1.),(1.,1.),(1.,1.),(1.,1.),(1.,1.),(1.,1.),(1.,
1.),(1.,1.),(1.,1.),(1.,1.),(1.,1.),(1.,1.),(1.,1.),(1.,1.),(1.,1.),(1.,
1.),(1.,1.)))
REPRESENTATION_ITEM('')
SURFACE()
);
#1012=(
BOUNDED_SURFACE()
B_SPLINE_SURFACE(5,1,((#162650,#162651),(#162652,#162653),(#162654,#162655),
(#162656,#162657),(#162658,#162659),(#162660,#162661),(#162662,#162663),
(#162664,#162665),(#162666,#162667),(#162668,#162669),(#162670,#162671),
(#162672,#162673),(#162674,#162675),(#162676,#162677),(#162678,#162679),
(#162680,#162681),(#162682,#162683),(#162684,#162685),(#162686,#162687),
(#162688,#162689),(#162690,#162691),(#162692,#162693),(#162694,#162695),
(#162696,#162697),(#162698,#162699),(#162700,#162701),(#162702,#162703),
(#162704,#162705),(#162706,#162707),(#162708,#162709),(#162710,#162711),
(#162712,#162713),(#162714,#162715),(#162716,#162717),(#162718,#162719),
(#162720,#162721),(#162722,#162723),(#162724,#162725),(#162726,#162727),
(#162728,#162729),(#162730,#162731),(#162732,#162733),(#162734,#162735),
(#162736,#162737),(#162738,#162739),(#162740,#162741),(#162742,#162743),
(#162744,#162745),(#162746,#162747),(#162748,#162749),(#162750,#162751),
(#162752,#162753),(#162754,#162755),(#162756,#162757),(#162758,#162759),
(#162760,#162761),(#162762,#162763),(#162764,#162765),(#162766,#162767),
(#162768,#162769),(#162770,#162771),(#162772,#162773),(#162774,#162775),
(#162776,#162777),(#162778,#162779),(#162780,#162781),(#162782,#162783),
(#162784,#162785),(#162786,#162787),(#162788,#162789),(#162790,#162791),
(#162792,#162793),(#162794,#162795),(#162796,#162797),(#162798,#162799),
(#162800,#162801),(#162802,#162803),(#162804,#162805),(#162806,#162807),
(#162808,#162809),(#162810,#162811),(#162812,#162813),(#162814,#162815),
(#162816,#162817),(#162818,#162819),(#162820,#162821),(#162822,#162823),
(#162824,#162825),(#162826,#162827),(#162828,#162829),(#162830,#162831),
(#162832,#162833),(#162834,#162835),(#162836,#162837),(#162838,#162839),
(#162840,#162841),(#162842,#162843),(#162844,#162845),(#162846,#162847),
(#162848,#162849),(#162850,#162851),(#162852,#162853),(#162854,#162855),
(#162856,#162857),(#162858,#162859),(#162860,#162861),(#162862,#162863),
(#162864,#162865),(#162866,#162867),(#162868,#162869),(#162870,#162871),
(#162872,#162873),(#162874,#162875),(#162876,#162877),(#162878,#162879),
(#162880,#162881),(#162882,#162883),(#162884,#162885),(#162886,#162887),
(#162888,#162889),(#162890,#162891),(#162892,#162893),(#162894,#162895),
(#162896,#162897),(#162898,#162899),(#162900,#162901),(#162902,#162903),
(#162904,#162905),(#162906,#162907),(#162908,#162909),(#162910,#162911),
(#162912,#162913),(#162914,#162915),(#162916,#162917),(#162918,#162919),
(#162920,#162921),(#162922,#162923),(#162924,#162925),(#162926,#162927),
(#162928,#162929),(#162930,#162931),(#162932,#162933),(#162934,#162935),
(#162936,#162937),(#162938,#162939),(#162940,#162941),(#162942,#162943),
(#162944,#162945),(#162946,#162947),(#162948,#162949),(#162950,#162951),
(#162952,#162953),(#162954,#162955),(#162956,#162957),(#162958,#162959),
(#162960,#162961),(#162962,#162963),(#162964,#162965),(#162966,#162967),
(#162968,#162969),(#162970,#162971),(#162972,#162973),(#162974,#162975),
(#162976,#162977),(#162978,#162979),(#162980,#162981),(#162982,#162983),
(#162984,#162985),(#162986,#162987),(#162988,#162989),(#162990,#162991),
(#162992,#162993),(#162994,#162995),(#162996,#162997),(#162998,#162999),
(#163000,#163001),(#163002,#163003),(#163004,#163005),(#163006,#163007),
(#163008,#163009),(#163010,#163011),(#163012,#163013),(#163014,#163015),
(#163016,#163017),(#163018,#163019),(#163020,#163021),(#163022,#163023),
(#163024,#163025),(#163026,#163027),(#163028,#163029),(#163030,#163031),
(#163032,#163033),(#163034,#163035),(#163036,#163037),(#163038,#163039),
(#163040,#163041),(#163042,#163043),(#163044,#163045),(#163046,#163047),
(#163048,#163049),(#163050,#163051),(#163052,#163053),(#163054,#163055),
(#163056,#163057),(#163058,#163059)),.UNSPECIFIED.,.F.,.F.,.F.)
B_SPLINE_SURFACE_WITH_KNOTS((6,1,1,1,1,1,1,1,1,1,1,1,1,1,1,1,1,1,1,1,1,
1,1,1,1,1,1,1,1,1,1,1,1,1,1,1,1,1,1,1,1,1,1,1,1,1,1,1,1,1,1,1,1,1,1,1,1,
1,1,1,1,1,1,1,1,1,1,1,1,1,1,1,1,1,1,1,1,1,1,1,1,1,1,1,1,1,1,1,1,1,1,1,1,
1,1,1,1,1,1,1,1,1,1,1,1,1,1,1,1,1,1,1,1,1,1,1,1,1,1,1,1,1,1,1,1,1,1,1,1,
1,1,1,1,1,1,1,1,1,1,1,1,1,1,1,1,1,1,1,1,1,1,1,1,1,1,1,1,1,1,1,1,1,1,1,1,
1,1,1,1,1,1,1,1,1,1,1,1,1,1,1,1,1,1,1,1,1,1,1,1,1,1,1,1,1,1,1,1,1,1,1,6),
(2,2),(-1.,-0.995000000000001,-0.990000000000001,-0.985000000000001,-0.980000000000001,
-0.975000000000001,-0.970000000000001,-0.965000000000001,-0.960000000000001,
-0.955000000000001,-0.950000000000001,-0.945000000000001,-0.940000000000001,
-0.935000000000001,-0.930000000000001,-0.925000000000001,-0.920000000000001,
-0.915000000000001,-0.910000000000001,-0.905000000000001,-0.900000000000001,
-0.895000000000001,-0.890000000000001,-0.885000000000001,-0.880000000000001,
-0.875000000000001,-0.870000000000001,-0.865000000000001,-0.860000000000001,
-0.855000000000001,-0.850000000000001,-0.845000000000001,-0.840000000000001,
-0.835000000000001,-0.830000000000001,-0.825000000000001,-0.820000000000001,
-0.815000000000001,-0.810000000000001,-0.805000000000001,-0.800000000000001,
-0.795000000000001,-0.790000000000001,-0.785000000000001,-0.780000000000001,
-0.775000000000001,-0.770000000000001,-0.765000000000001,-0.760000000000001,
-0.755000000000001,-0.750000000000001,-0.745000000000001,-0.740000000000001,
-0.735000000000001,-0.730000000000001,-0.725000000000001,-0.720000000000001,
-0.715000000000001,-0.710000000000001,-0.705000000000001,-0.700000000000001,
-0.695000000000001,-0.690000000000001,-0.685,-0.68,-0.675,-0.67,-0.665,
-0.66,-0.655,-0.65,-0.645,-0.64,-0.635,-0.63,-0.625,-0.62,-0.615,-0.61,
-0.605,-0.6,-0.595,-0.59,-0.585,-0.58,-0.575,-0.57,-0.565,-0.56,-0.555,
-0.55,-0.545,-0.54,-0.535,-0.53,-0.525,-0.52,-0.515,-0.51,-0.505,-0.5,-0.495,
-0.49,-0.485,-0.48,-0.475,-0.47,-0.465,-0.46,-0.455,-0.45,-0.445,-0.44,
-0.435,-0.43,-0.425,-0.42,-0.415,-0.41,-0.405,-0.4,-0.395,-0.39,-0.385,
-0.38,-0.375,-0.37,-0.365,-0.36,-0.355,-0.35,-0.345,-0.34,-0.335,-0.33,
-0.325,-0.32,-0.315,-0.31,-0.305,-0.3,-0.295,-0.29,-0.285,-0.28,-0.275,
-0.27,-0.265,-0.26,-0.255,-0.25,-0.245,-0.24,-0.235,-0.23,-0.225,-0.22,
-0.215,-0.21,-0.205,-0.2,-0.195,-0.19,-0.185,-0.18,-0.175,-0.17,-0.165,
-0.16,-0.155,-0.15,-0.145,-0.14,-0.135,-0.13,-0.125,-0.12,-0.115,-0.11,
-0.105,-0.1,-0.095,-0.09,-0.085,-0.08,-0.075,-0.07,-0.065,-0.06,-0.055,
-0.05,-0.045,-0.04,-0.035,-0.03,-0.025,-0.02,-0.015,-0.01,-0.005,0.),(0.,
1.2),.UNSPECIFIED.)
GEOMETRIC_REPRESENTATION_ITEM()
RATIONAL_B_SPLINE_SURFACE(((1.,1.),(1.,1.),(1.,1.),(1.,1.),(1.,1.),(1.,
1.),(1.,1.),(1.,1.),(1.,1.),(1.,1.),(1.,1.),(1.,1.),(1.,1.),(1.,1.),(1.,
1.),(1.,1.),(1.,1.),(1.,1.),(1.,1.),(1.,1.),(1.,1.),(1.,1.),(1.,1.),(1.,
1.),(1.,1.),(1.,1.),(1.,1.),(1.,1.),(1.,1.),(1.,1.),(1.,1.),(1.,1.),(1.,
1.),(1.,1.),(1.,1.),(1.,1.),(1.,1.),(1.,1.),(1.,1.),(1.,1.),(1.,1.),(1.,
1.),(1.,1.),(1.,1.),(1.,1.),(1.,1.),(1.,1.),(1.,1.),(1.,1.),(1.,1.),(1.,
1.),(1.,1.),(1.,1.),(1.,1.),(1.,1.),(1.,1.),(1.,1.),(1.,1.),(1.,1.),(1.,
1.),(1.,1.),(1.,1.),(1.,1.),(1.,1.),(1.,1.),(1.,1.),(1.,1.),(1.,1.),(1.,
1.),(1.,1.),(1.,1.),(1.,1.),(1.,1.),(1.,1.),(1.,1.),(1.,1.),(1.,1.),(1.,
1.),(1.,1.),(1.,1.),(1.,1.),(1.,1.),(1.,1.),(1.,1.),(1.,1.),(1.,1.),(1.,
1.),(1.,1.),(1.,1.),(1.,1.),(1.,1.),(1.,1.),(1.,1.),(1.,1.),(1.,1.),(1.,
1.),(1.,1.),(1.,1.),(1.,1.),(1.,1.),(1.,1.),(1.,1.),(1.,1.),(1.,1.),(1.,
1.),(1.,1.),(1.,1.),(1.,1.),(1.,1.),(1.,1.),(1.,1.),(1.,1.),(1.,1.),(1.,
1.),(1.,1.),(1.,1.),(1.,1.),(1.,1.),(1.,1.),(1.,1.),(1.,1.),(1.,1.),(1.,
1.),(1.,1.),(1.,1.),(1.,1.),(1.,1.),(1.,1.),(1.,1.),(1.,1.),(1.,1.),(1.,
1.),(1.,1.),(1.,1.),(1.,1.),(1.,1.),(1.,1.),(1.,1.),(1.,1.),(1.,1.),(1.,
1.),(1.,1.),(1.,1.),(1.,1.),(1.,1.),(1.,1.),(1.,1.),(1.,1.),(1.,1.),(1.,
1.),(1.,1.),(1.,1.),(1.,1.),(1.,1.),(1.,1.),(1.,1.),(1.,1.),(1.,1.),(1.,
1.),(1.,1.),(1.,1.),(1.,1.),(1.,1.),(1.,1.),(1.,1.),(1.,1.),(1.,1.),(1.,
1.),(1.,1.),(1.,1.),(1.,1.),(1.,1.),(1.,1.),(1.,1.),(1.,1.),(1.,1.),(1.,
1.),(1.,1.),(1.,1.),(1.,1.),(1.,1.),(1.,1.),(1.,1.),(1.,1.),(1.,1.),(1.,
1.),(1.,1.),(1.,1.),(1.,1.),(1.,1.),(1.,1.),(1.,1.),(1.,1.),(1.,1.),(1.,
1.),(1.,1.),(1.,1.),(1.,1.),(1.,1.),(1.,1.),(1.,1.),(1.,1.),(1.,1.),(1.,
1.),(1.,1.)))
REPRESENTATION_ITEM('')
SURFACE()
);
#1013=(
BOUNDED_SURFACE()
B_SPLINE_SURFACE(5,1,((#163451,#163452),(#163453,#163454),(#163455,#163456),
(#163457,#163458),(#163459,#163460),(#163461,#163462),(#163463,#163464),
(#163465,#163466),(#163467,#163468),(#163469,#163470),(#163471,#163472),
(#163473,#163474),(#163475,#163476),(#163477,#163478),(#163479,#163480),
(#163481,#163482),(#163483,#163484),(#163485,#163486),(#163487,#163488),
(#163489,#163490),(#163491,#163492),(#163493,#163494),(#163495,#163496),
(#163497,#163498),(#163499,#163500),(#163501,#163502),(#163503,#163504),
(#163505,#163506),(#163507,#163508),(#163509,#163510),(#163511,#163512),
(#163513,#163514),(#163515,#163516),(#163517,#163518),(#163519,#163520),
(#163521,#163522),(#163523,#163524),(#163525,#163526),(#163527,#163528),
(#163529,#163530),(#163531,#163532),(#163533,#163534),(#163535,#163536),
(#163537,#163538),(#163539,#163540),(#163541,#163542),(#163543,#163544),
(#163545,#163546),(#163547,#163548),(#163549,#163550),(#163551,#163552),
(#163553,#163554),(#163555,#163556),(#163557,#163558),(#163559,#163560),
(#163561,#163562),(#163563,#163564),(#163565,#163566),(#163567,#163568),
(#163569,#163570),(#163571,#163572),(#163573,#163574),(#163575,#163576),
(#163577,#163578),(#163579,#163580),(#163581,#163582),(#163583,#163584),
(#163585,#163586),(#163587,#163588),(#163589,#163590),(#163591,#163592),
(#163593,#163594),(#163595,#163596),(#163597,#163598),(#163599,#163600),
(#163601,#163602),(#163603,#163604),(#163605,#163606),(#163607,#163608),
(#163609,#163610),(#163611,#163612),(#163613,#163614),(#163615,#163616),
(#163617,#163618),(#163619,#163620),(#163621,#163622),(#163623,#163624),
(#163625,#163626),(#163627,#163628),(#163629,#163630),(#163631,#163632),
(#163633,#163634),(#163635,#163636),(#163637,#163638),(#163639,#163640),
(#163641,#163642),(#163643,#163644),(#163645,#163646),(#163647,#163648),
(#163649,#163650),(#163651,#163652),(#163653,#163654),(#163655,#163656),
(#163657,#163658),(#163659,#163660),(#163661,#163662),(#163663,#163664),
(#163665,#163666),(#163667,#163668),(#163669,#163670),(#163671,#163672),
(#163673,#163674),(#163675,#163676),(#163677,#163678),(#163679,#163680),
(#163681,#163682),(#163683,#163684),(#163685,#163686),(#163687,#163688),
(#163689,#163690),(#163691,#163692),(#163693,#163694),(#163695,#163696),
(#163697,#163698),(#163699,#163700),(#163701,#163702),(#163703,#163704),
(#163705,#163706),(#163707,#163708),(#163709,#163710),(#163711,#163712),
(#163713,#163714),(#163715,#163716),(#163717,#163718),(#163719,#163720),
(#163721,#163722),(#163723,#163724),(#163725,#163726),(#163727,#163728),
(#163729,#163730),(#163731,#163732),(#163733,#163734),(#163735,#163736),
(#163737,#163738),(#163739,#163740),(#163741,#163742),(#163743,#163744),
(#163745,#163746),(#163747,#163748),(#163749,#163750),(#163751,#163752),
(#163753,#163754),(#163755,#163756),(#163757,#163758),(#163759,#163760),
(#163761,#163762),(#163763,#163764),(#163765,#163766),(#163767,#163768),
(#163769,#163770),(#163771,#163772),(#163773,#163774),(#163775,#163776),
(#163777,#163778),(#163779,#163780),(#163781,#163782),(#163783,#163784),
(#163785,#163786),(#163787,#163788),(#163789,#163790),(#163791,#163792),
(#163793,#163794),(#163795,#163796),(#163797,#163798),(#163799,#163800),
(#163801,#163802),(#163803,#163804),(#163805,#163806),(#163807,#163808),
(#163809,#163810),(#163811,#163812),(#163813,#163814),(#163815,#163816),
(#163817,#163818),(#163819,#163820),(#163821,#163822),(#163823,#163824),
(#163825,#163826),(#163827,#163828),(#163829,#163830),(#163831,#163832),
(#163833,#163834),(#163835,#163836),(#163837,#163838),(#163839,#163840),
(#163841,#163842),(#163843,#163844),(#163845,#163846),(#163847,#163848),
(#163849,#163850),(#163851,#163852),(#163853,#163854),(#163855,#163856),
(#163857,#163858),(#163859,#163860)),.UNSPECIFIED.,.F.,.F.,.F.)
B_SPLINE_SURFACE_WITH_KNOTS((6,1,1,1,1,1,1,1,1,1,1,1,1,1,1,1,1,1,1,1,1,
1,1,1,1,1,1,1,1,1,1,1,1,1,1,1,1,1,1,1,1,1,1,1,1,1,1,1,1,1,1,1,1,1,1,1,1,
1,1,1,1,1,1,1,1,1,1,1,1,1,1,1,1,1,1,1,1,1,1,1,1,1,1,1,1,1,1,1,1,1,1,1,1,
1,1,1,1,1,1,1,1,1,1,1,1,1,1,1,1,1,1,1,1,1,1,1,1,1,1,1,1,1,1,1,1,1,1,1,1,
1,1,1,1,1,1,1,1,1,1,1,1,1,1,1,1,1,1,1,1,1,1,1,1,1,1,1,1,1,1,1,1,1,1,1,1,
1,1,1,1,1,1,1,1,1,1,1,1,1,1,1,1,1,1,1,1,1,1,1,1,1,1,1,1,1,1,1,1,1,1,1,6),
(2,2),(-1.,-0.995000000000001,-0.990000000000001,-0.985000000000001,-0.980000000000001,
-0.975000000000001,-0.970000000000001,-0.965000000000001,-0.960000000000001,
-0.955000000000001,-0.950000000000001,-0.945000000000001,-0.940000000000001,
-0.935000000000001,-0.930000000000001,-0.925000000000001,-0.920000000000001,
-0.915000000000001,-0.910000000000001,-0.905000000000001,-0.900000000000001,
-0.895000000000001,-0.890000000000001,-0.885000000000001,-0.880000000000001,
-0.875000000000001,-0.870000000000001,-0.865000000000001,-0.860000000000001,
-0.855000000000001,-0.850000000000001,-0.845000000000001,-0.840000000000001,
-0.835000000000001,-0.830000000000001,-0.825000000000001,-0.820000000000001,
-0.815000000000001,-0.810000000000001,-0.805000000000001,-0.800000000000001,
-0.795000000000001,-0.790000000000001,-0.785000000000001,-0.780000000000001,
-0.775000000000001,-0.770000000000001,-0.765000000000001,-0.760000000000001,
-0.755000000000001,-0.750000000000001,-0.745000000000001,-0.740000000000001,
-0.735000000000001,-0.730000000000001,-0.725000000000001,-0.720000000000001,
-0.715000000000001,-0.710000000000001,-0.705000000000001,-0.700000000000001,
-0.695000000000001,-0.690000000000001,-0.685,-0.68,-0.675,-0.67,-0.665,
-0.66,-0.655,-0.65,-0.645,-0.64,-0.635,-0.63,-0.625,-0.62,-0.615,-0.61,
-0.605,-0.6,-0.595,-0.59,-0.585,-0.58,-0.575,-0.57,-0.565,-0.56,-0.555,
-0.55,-0.545,-0.54,-0.535,-0.53,-0.525,-0.52,-0.515,-0.51,-0.505,-0.5,-0.495,
-0.49,-0.485,-0.48,-0.475,-0.47,-0.465,-0.46,-0.455,-0.45,-0.445,-0.44,
-0.435,-0.43,-0.425,-0.42,-0.415,-0.41,-0.405,-0.4,-0.395,-0.39,-0.385,
-0.38,-0.375,-0.37,-0.365,-0.36,-0.355,-0.35,-0.345,-0.34,-0.335,-0.33,
-0.325,-0.32,-0.315,-0.31,-0.305,-0.3,-0.295,-0.29,-0.285,-0.28,-0.275,
-0.27,-0.265,-0.26,-0.255,-0.25,-0.245,-0.24,-0.235,-0.23,-0.225,-0.22,
-0.215,-0.21,-0.205,-0.2,-0.195,-0.19,-0.185,-0.18,-0.175,-0.17,-0.165,
-0.16,-0.155,-0.15,-0.145,-0.14,-0.135,-0.13,-0.125,-0.12,-0.115,-0.11,
-0.105,-0.1,-0.095,-0.09,-0.085,-0.08,-0.075,-0.07,-0.065,-0.06,-0.055,
-0.05,-0.045,-0.04,-0.035,-0.03,-0.025,-0.02,-0.015,-0.01,-0.005,0.),(0.,
1.2),.UNSPECIFIED.)
GEOMETRIC_REPRESENTATION_ITEM()
RATIONAL_B_SPLINE_SURFACE(((1.,1.),(1.,1.),(1.,1.),(1.,1.),(1.,1.),(1.,
1.),(1.,1.),(1.,1.),(1.,1.),(1.,1.),(1.,1.),(1.,1.),(1.,1.),(1.,1.),(1.,
1.),(1.,1.),(1.,1.),(1.,1.),(1.,1.),(1.,1.),(1.,1.),(1.,1.),(1.,1.),(1.,
1.),(1.,1.),(1.,1.),(1.,1.),(1.,1.),(1.,1.),(1.,1.),(1.,1.),(1.,1.),(1.,
1.),(1.,1.),(1.,1.),(1.,1.),(1.,1.),(1.,1.),(1.,1.),(1.,1.),(1.,1.),(1.,
1.),(1.,1.),(1.,1.),(1.,1.),(1.,1.),(1.,1.),(1.,1.),(1.,1.),(1.,1.),(1.,
1.),(1.,1.),(1.,1.),(1.,1.),(1.,1.),(1.,1.),(1.,1.),(1.,1.),(1.,1.),(1.,
1.),(1.,1.),(1.,1.),(1.,1.),(1.,1.),(1.,1.),(1.,1.),(1.,1.),(1.,1.),(1.,
1.),(1.,1.),(1.,1.),(1.,1.),(1.,1.),(1.,1.),(1.,1.),(1.,1.),(1.,1.),(1.,
1.),(1.,1.),(1.,1.),(1.,1.),(1.,1.),(1.,1.),(1.,1.),(1.,1.),(1.,1.),(1.,
1.),(1.,1.),(1.,1.),(1.,1.),(1.,1.),(1.,1.),(1.,1.),(1.,1.),(1.,1.),(1.,
1.),(1.,1.),(1.,1.),(1.,1.),(1.,1.),(1.,1.),(1.,1.),(1.,1.),(1.,1.),(1.,
1.),(1.,1.),(1.,1.),(1.,1.),(1.,1.),(1.,1.),(1.,1.),(1.,1.),(1.,1.),(1.,
1.),(1.,1.),(1.,1.),(1.,1.),(1.,1.),(1.,1.),(1.,1.),(1.,1.),(1.,1.),(1.,
1.),(1.,1.),(1.,1.),(1.,1.),(1.,1.),(1.,1.),(1.,1.),(1.,1.),(1.,1.),(1.,
1.),(1.,1.),(1.,1.),(1.,1.),(1.,1.),(1.,1.),(1.,1.),(1.,1.),(1.,1.),(1.,
1.),(1.,1.),(1.,1.),(1.,1.),(1.,1.),(1.,1.),(1.,1.),(1.,1.),(1.,1.),(1.,
1.),(1.,1.),(1.,1.),(1.,1.),(1.,1.),(1.,1.),(1.,1.),(1.,1.),(1.,1.),(1.,
1.),(1.,1.),(1.,1.),(1.,1.),(1.,1.),(1.,1.),(1.,1.),(1.,1.),(1.,1.),(1.,
1.),(1.,1.),(1.,1.),(1.,1.),(1.,1.),(1.,1.),(1.,1.),(1.,1.),(1.,1.),(1.,
1.),(1.,1.),(1.,1.),(1.,1.),(1.,1.),(1.,1.),(1.,1.),(1.,1.),(1.,1.),(1.,
1.),(1.,1.),(1.,1.),(1.,1.),(1.,1.),(1.,1.),(1.,1.),(1.,1.),(1.,1.),(1.,
1.),(1.,1.),(1.,1.),(1.,1.),(1.,1.),(1.,1.),(1.,1.),(1.,1.),(1.,1.),(1.,
1.),(1.,1.)))
REPRESENTATION_ITEM('')
SURFACE()
);
#1014=(
BOUNDED_SURFACE()
B_SPLINE_SURFACE(5,1,((#164252,#164253),(#164254,#164255),(#164256,#164257),
(#164258,#164259),(#164260,#164261),(#164262,#164263),(#164264,#164265),
(#164266,#164267),(#164268,#164269),(#164270,#164271),(#164272,#164273),
(#164274,#164275),(#164276,#164277),(#164278,#164279),(#164280,#164281),
(#164282,#164283),(#164284,#164285),(#164286,#164287),(#164288,#164289),
(#164290,#164291),(#164292,#164293),(#164294,#164295),(#164296,#164297),
(#164298,#164299),(#164300,#164301),(#164302,#164303),(#164304,#164305),
(#164306,#164307),(#164308,#164309),(#164310,#164311),(#164312,#164313),
(#164314,#164315),(#164316,#164317),(#164318,#164319),(#164320,#164321),
(#164322,#164323),(#164324,#164325),(#164326,#164327),(#164328,#164329),
(#164330,#164331),(#164332,#164333),(#164334,#164335),(#164336,#164337),
(#164338,#164339),(#164340,#164341),(#164342,#164343),(#164344,#164345),
(#164346,#164347),(#164348,#164349),(#164350,#164351),(#164352,#164353),
(#164354,#164355),(#164356,#164357),(#164358,#164359),(#164360,#164361),
(#164362,#164363),(#164364,#164365),(#164366,#164367),(#164368,#164369),
(#164370,#164371),(#164372,#164373),(#164374,#164375),(#164376,#164377),
(#164378,#164379),(#164380,#164381),(#164382,#164383),(#164384,#164385),
(#164386,#164387),(#164388,#164389),(#164390,#164391),(#164392,#164393),
(#164394,#164395),(#164396,#164397),(#164398,#164399),(#164400,#164401),
(#164402,#164403),(#164404,#164405),(#164406,#164407),(#164408,#164409),
(#164410,#164411),(#164412,#164413),(#164414,#164415),(#164416,#164417),
(#164418,#164419),(#164420,#164421),(#164422,#164423),(#164424,#164425),
(#164426,#164427),(#164428,#164429),(#164430,#164431),(#164432,#164433),
(#164434,#164435),(#164436,#164437),(#164438,#164439),(#164440,#164441),
(#164442,#164443),(#164444,#164445),(#164446,#164447),(#164448,#164449),
(#164450,#164451),(#164452,#164453),(#164454,#164455),(#164456,#164457),
(#164458,#164459),(#164460,#164461),(#164462,#164463),(#164464,#164465),
(#164466,#164467),(#164468,#164469),(#164470,#164471),(#164472,#164473),
(#164474,#164475),(#164476,#164477),(#164478,#164479),(#164480,#164481),
(#164482,#164483),(#164484,#164485),(#164486,#164487),(#164488,#164489),
(#164490,#164491),(#164492,#164493),(#164494,#164495),(#164496,#164497),
(#164498,#164499),(#164500,#164501),(#164502,#164503),(#164504,#164505),
(#164506,#164507),(#164508,#164509),(#164510,#164511),(#164512,#164513),
(#164514,#164515),(#164516,#164517),(#164518,#164519),(#164520,#164521),
(#164522,#164523),(#164524,#164525),(#164526,#164527),(#164528,#164529),
(#164530,#164531),(#164532,#164533),(#164534,#164535),(#164536,#164537),
(#164538,#164539),(#164540,#164541),(#164542,#164543),(#164544,#164545),
(#164546,#164547),(#164548,#164549),(#164550,#164551),(#164552,#164553),
(#164554,#164555),(#164556,#164557),(#164558,#164559),(#164560,#164561),
(#164562,#164563),(#164564,#164565),(#164566,#164567),(#164568,#164569),
(#164570,#164571),(#164572,#164573),(#164574,#164575),(#164576,#164577),
(#164578,#164579),(#164580,#164581),(#164582,#164583),(#164584,#164585),
(#164586,#164587),(#164588,#164589),(#164590,#164591),(#164592,#164593),
(#164594,#164595),(#164596,#164597),(#164598,#164599),(#164600,#164601),
(#164602,#164603),(#164604,#164605),(#164606,#164607),(#164608,#164609),
(#164610,#164611),(#164612,#164613),(#164614,#164615),(#164616,#164617),
(#164618,#164619),(#164620,#164621),(#164622,#164623),(#164624,#164625),
(#164626,#164627),(#164628,#164629),(#164630,#164631),(#164632,#164633),
(#164634,#164635),(#164636,#164637),(#164638,#164639),(#164640,#164641),
(#164642,#164643),(#164644,#164645),(#164646,#164647),(#164648,#164649),
(#164650,#164651),(#164652,#164653),(#164654,#164655),(#164656,#164657),
(#164658,#164659),(#164660,#164661)),.UNSPECIFIED.,.F.,.F.,.F.)
B_SPLINE_SURFACE_WITH_KNOTS((6,1,1,1,1,1,1,1,1,1,1,1,1,1,1,1,1,1,1,1,1,
1,1,1,1,1,1,1,1,1,1,1,1,1,1,1,1,1,1,1,1,1,1,1,1,1,1,1,1,1,1,1,1,1,1,1,1,
1,1,1,1,1,1,1,1,1,1,1,1,1,1,1,1,1,1,1,1,1,1,1,1,1,1,1,1,1,1,1,1,1,1,1,1,
1,1,1,1,1,1,1,1,1,1,1,1,1,1,1,1,1,1,1,1,1,1,1,1,1,1,1,1,1,1,1,1,1,1,1,1,
1,1,1,1,1,1,1,1,1,1,1,1,1,1,1,1,1,1,1,1,1,1,1,1,1,1,1,1,1,1,1,1,1,1,1,1,
1,1,1,1,1,1,1,1,1,1,1,1,1,1,1,1,1,1,1,1,1,1,1,1,1,1,1,1,1,1,1,1,1,1,1,6),
(2,2),(-1.,-0.995000000000001,-0.990000000000001,-0.985000000000001,-0.980000000000001,
-0.975000000000001,-0.970000000000001,-0.965000000000001,-0.960000000000001,
-0.955000000000001,-0.950000000000001,-0.945000000000001,-0.940000000000001,
-0.935000000000001,-0.930000000000001,-0.925000000000001,-0.920000000000001,
-0.915000000000001,-0.910000000000001,-0.905000000000001,-0.900000000000001,
-0.895000000000001,-0.890000000000001,-0.885000000000001,-0.880000000000001,
-0.875000000000001,-0.870000000000001,-0.865000000000001,-0.860000000000001,
-0.855000000000001,-0.850000000000001,-0.845000000000001,-0.840000000000001,
-0.835000000000001,-0.830000000000001,-0.825000000000001,-0.820000000000001,
-0.815000000000001,-0.810000000000001,-0.805000000000001,-0.800000000000001,
-0.795000000000001,-0.790000000000001,-0.785000000000001,-0.780000000000001,
-0.775000000000001,-0.770000000000001,-0.765000000000001,-0.760000000000001,
-0.755000000000001,-0.750000000000001,-0.745000000000001,-0.740000000000001,
-0.735000000000001,-0.730000000000001,-0.725000000000001,-0.720000000000001,
-0.715000000000001,-0.710000000000001,-0.705000000000001,-0.700000000000001,
-0.695000000000001,-0.690000000000001,-0.685,-0.68,-0.675,-0.67,-0.665,
-0.66,-0.655,-0.65,-0.645,-0.64,-0.635,-0.63,-0.625,-0.62,-0.615,-0.61,
-0.605,-0.6,-0.595,-0.59,-0.585,-0.58,-0.575,-0.57,-0.565,-0.56,-0.555,
-0.55,-0.545,-0.54,-0.535,-0.53,-0.525,-0.52,-0.515,-0.51,-0.505,-0.5,-0.495,
-0.49,-0.485,-0.48,-0.475,-0.47,-0.465,-0.46,-0.455,-0.45,-0.445,-0.44,
-0.435,-0.43,-0.425,-0.42,-0.415,-0.41,-0.405,-0.4,-0.395,-0.39,-0.385,
-0.38,-0.375,-0.37,-0.365,-0.36,-0.355,-0.35,-0.345,-0.34,-0.335,-0.33,
-0.325,-0.32,-0.315,-0.31,-0.305,-0.3,-0.295,-0.29,-0.285,-0.28,-0.275,
-0.27,-0.265,-0.26,-0.255,-0.25,-0.245,-0.24,-0.235,-0.23,-0.225,-0.22,
-0.215,-0.21,-0.205,-0.2,-0.195,-0.19,-0.185,-0.18,-0.175,-0.17,-0.165,
-0.16,-0.155,-0.15,-0.145,-0.14,-0.135,-0.13,-0.125,-0.12,-0.115,-0.11,
-0.105,-0.1,-0.095,-0.09,-0.085,-0.08,-0.075,-0.07,-0.065,-0.06,-0.055,
-0.05,-0.045,-0.04,-0.035,-0.03,-0.025,-0.02,-0.015,-0.01,-0.005,0.),(0.,
1.2),.UNSPECIFIED.)
GEOMETRIC_REPRESENTATION_ITEM()
RATIONAL_B_SPLINE_SURFACE(((1.,1.),(1.,1.),(1.,1.),(1.,1.),(1.,1.),(1.,
1.),(1.,1.),(1.,1.),(1.,1.),(1.,1.),(1.,1.),(1.,1.),(1.,1.),(1.,1.),(1.,
1.),(1.,1.),(1.,1.),(1.,1.),(1.,1.),(1.,1.),(1.,1.),(1.,1.),(1.,1.),(1.,
1.),(1.,1.),(1.,1.),(1.,1.),(1.,1.),(1.,1.),(1.,1.),(1.,1.),(1.,1.),(1.,
1.),(1.,1.),(1.,1.),(1.,1.),(1.,1.),(1.,1.),(1.,1.),(1.,1.),(1.,1.),(1.,
1.),(1.,1.),(1.,1.),(1.,1.),(1.,1.),(1.,1.),(1.,1.),(1.,1.),(1.,1.),(1.,
1.),(1.,1.),(1.,1.),(1.,1.),(1.,1.),(1.,1.),(1.,1.),(1.,1.),(1.,1.),(1.,
1.),(1.,1.),(1.,1.),(1.,1.),(1.,1.),(1.,1.),(1.,1.),(1.,1.),(1.,1.),(1.,
1.),(1.,1.),(1.,1.),(1.,1.),(1.,1.),(1.,1.),(1.,1.),(1.,1.),(1.,1.),(1.,
1.),(1.,1.),(1.,1.),(1.,1.),(1.,1.),(1.,1.),(1.,1.),(1.,1.),(1.,1.),(1.,
1.),(1.,1.),(1.,1.),(1.,1.),(1.,1.),(1.,1.),(1.,1.),(1.,1.),(1.,1.),(1.,
1.),(1.,1.),(1.,1.),(1.,1.),(1.,1.),(1.,1.),(1.,1.),(1.,1.),(1.,1.),(1.,
1.),(1.,1.),(1.,1.),(1.,1.),(1.,1.),(1.,1.),(1.,1.),(1.,1.),(1.,1.),(1.,
1.),(1.,1.),(1.,1.),(1.,1.),(1.,1.),(1.,1.),(1.,1.),(1.,1.),(1.,1.),(1.,
1.),(1.,1.),(1.,1.),(1.,1.),(1.,1.),(1.,1.),(1.,1.),(1.,1.),(1.,1.),(1.,
1.),(1.,1.),(1.,1.),(1.,1.),(1.,1.),(1.,1.),(1.,1.),(1.,1.),(1.,1.),(1.,
1.),(1.,1.),(1.,1.),(1.,1.),(1.,1.),(1.,1.),(1.,1.),(1.,1.),(1.,1.),(1.,
1.),(1.,1.),(1.,1.),(1.,1.),(1.,1.),(1.,1.),(1.,1.),(1.,1.),(1.,1.),(1.,
1.),(1.,1.),(1.,1.),(1.,1.),(1.,1.),(1.,1.),(1.,1.),(1.,1.),(1.,1.),(1.,
1.),(1.,1.),(1.,1.),(1.,1.),(1.,1.),(1.,1.),(1.,1.),(1.,1.),(1.,1.),(1.,
1.),(1.,1.),(1.,1.),(1.,1.),(1.,1.),(1.,1.),(1.,1.),(1.,1.),(1.,1.),(1.,
1.),(1.,1.),(1.,1.),(1.,1.),(1.,1.),(1.,1.),(1.,1.),(1.,1.),(1.,1.),(1.,
1.),(1.,1.),(1.,1.),(1.,1.),(1.,1.),(1.,1.),(1.,1.),(1.,1.),(1.,1.),(1.,
1.),(1.,1.)))
REPRESENTATION_ITEM('')
SURFACE()
);
#1015=(
BOUNDED_SURFACE()
B_SPLINE_SURFACE(5,1,((#165053,#165054),(#165055,#165056),(#165057,#165058),
(#165059,#165060),(#165061,#165062),(#165063,#165064),(#165065,#165066),
(#165067,#165068),(#165069,#165070),(#165071,#165072),(#165073,#165074),
(#165075,#165076),(#165077,#165078),(#165079,#165080),(#165081,#165082),
(#165083,#165084),(#165085,#165086),(#165087,#165088),(#165089,#165090),
(#165091,#165092),(#165093,#165094),(#165095,#165096),(#165097,#165098),
(#165099,#165100),(#165101,#165102),(#165103,#165104),(#165105,#165106),
(#165107,#165108),(#165109,#165110),(#165111,#165112),(#165113,#165114),
(#165115,#165116),(#165117,#165118),(#165119,#165120),(#165121,#165122),
(#165123,#165124),(#165125,#165126),(#165127,#165128),(#165129,#165130),
(#165131,#165132),(#165133,#165134),(#165135,#165136),(#165137,#165138),
(#165139,#165140),(#165141,#165142),(#165143,#165144),(#165145,#165146),
(#165147,#165148),(#165149,#165150),(#165151,#165152),(#165153,#165154),
(#165155,#165156),(#165157,#165158),(#165159,#165160),(#165161,#165162),
(#165163,#165164),(#165165,#165166),(#165167,#165168),(#165169,#165170),
(#165171,#165172),(#165173,#165174),(#165175,#165176),(#165177,#165178),
(#165179,#165180),(#165181,#165182),(#165183,#165184),(#165185,#165186),
(#165187,#165188),(#165189,#165190),(#165191,#165192),(#165193,#165194),
(#165195,#165196),(#165197,#165198),(#165199,#165200),(#165201,#165202),
(#165203,#165204),(#165205,#165206),(#165207,#165208),(#165209,#165210),
(#165211,#165212),(#165213,#165214),(#165215,#165216),(#165217,#165218),
(#165219,#165220),(#165221,#165222),(#165223,#165224),(#165225,#165226),
(#165227,#165228),(#165229,#165230),(#165231,#165232),(#165233,#165234),
(#165235,#165236),(#165237,#165238),(#165239,#165240),(#165241,#165242),
(#165243,#165244),(#165245,#165246),(#165247,#165248),(#165249,#165250),
(#165251,#165252),(#165253,#165254),(#165255,#165256),(#165257,#165258),
(#165259,#165260),(#165261,#165262),(#165263,#165264),(#165265,#165266),
(#165267,#165268),(#165269,#165270),(#165271,#165272),(#165273,#165274),
(#165275,#165276),(#165277,#165278),(#165279,#165280),(#165281,#165282),
(#165283,#165284),(#165285,#165286),(#165287,#165288),(#165289,#165290),
(#165291,#165292),(#165293,#165294),(#165295,#165296),(#165297,#165298),
(#165299,#165300),(#165301,#165302),(#165303,#165304),(#165305,#165306),
(#165307,#165308),(#165309,#165310),(#165311,#165312),(#165313,#165314),
(#165315,#165316),(#165317,#165318),(#165319,#165320),(#165321,#165322),
(#165323,#165324),(#165325,#165326),(#165327,#165328),(#165329,#165330),
(#165331,#165332),(#165333,#165334),(#165335,#165336),(#165337,#165338),
(#165339,#165340),(#165341,#165342),(#165343,#165344),(#165345,#165346),
(#165347,#165348),(#165349,#165350),(#165351,#165352),(#165353,#165354),
(#165355,#165356),(#165357,#165358),(#165359,#165360),(#165361,#165362),
(#165363,#165364),(#165365,#165366),(#165367,#165368),(#165369,#165370),
(#165371,#165372),(#165373,#165374),(#165375,#165376),(#165377,#165378),
(#165379,#165380),(#165381,#165382),(#165383,#165384),(#165385,#165386),
(#165387,#165388),(#165389,#165390),(#165391,#165392),(#165393,#165394),
(#165395,#165396),(#165397,#165398),(#165399,#165400),(#165401,#165402),
(#165403,#165404),(#165405,#165406),(#165407,#165408),(#165409,#165410),
(#165411,#165412),(#165413,#165414),(#165415,#165416),(#165417,#165418),
(#165419,#165420),(#165421,#165422),(#165423,#165424),(#165425,#165426),
(#165427,#165428),(#165429,#165430),(#165431,#165432),(#165433,#165434),
(#165435,#165436),(#165437,#165438),(#165439,#165440),(#165441,#165442),
(#165443,#165444),(#165445,#165446),(#165447,#165448),(#165449,#165450),
(#165451,#165452),(#165453,#165454),(#165455,#165456),(#165457,#165458),
(#165459,#165460),(#165461,#165462)),.UNSPECIFIED.,.F.,.F.,.F.)
B_SPLINE_SURFACE_WITH_KNOTS((6,1,1,1,1,1,1,1,1,1,1,1,1,1,1,1,1,1,1,1,1,
1,1,1,1,1,1,1,1,1,1,1,1,1,1,1,1,1,1,1,1,1,1,1,1,1,1,1,1,1,1,1,1,1,1,1,1,
1,1,1,1,1,1,1,1,1,1,1,1,1,1,1,1,1,1,1,1,1,1,1,1,1,1,1,1,1,1,1,1,1,1,1,1,
1,1,1,1,1,1,1,1,1,1,1,1,1,1,1,1,1,1,1,1,1,1,1,1,1,1,1,1,1,1,1,1,1,1,1,1,
1,1,1,1,1,1,1,1,1,1,1,1,1,1,1,1,1,1,1,1,1,1,1,1,1,1,1,1,1,1,1,1,1,1,1,1,
1,1,1,1,1,1,1,1,1,1,1,1,1,1,1,1,1,1,1,1,1,1,1,1,1,1,1,1,1,1,1,1,1,1,1,6),
(2,2),(-1.,-0.995000000000001,-0.990000000000001,-0.985000000000001,-0.980000000000001,
-0.975000000000001,-0.970000000000001,-0.965000000000001,-0.960000000000001,
-0.955000000000001,-0.950000000000001,-0.945000000000001,-0.940000000000001,
-0.935000000000001,-0.930000000000001,-0.925000000000001,-0.920000000000001,
-0.915000000000001,-0.910000000000001,-0.905000000000001,-0.900000000000001,
-0.895000000000001,-0.890000000000001,-0.885000000000001,-0.880000000000001,
-0.875000000000001,-0.870000000000001,-0.865000000000001,-0.860000000000001,
-0.855000000000001,-0.850000000000001,-0.845000000000001,-0.840000000000001,
-0.835000000000001,-0.830000000000001,-0.825000000000001,-0.820000000000001,
-0.815000000000001,-0.810000000000001,-0.805000000000001,-0.800000000000001,
-0.795000000000001,-0.790000000000001,-0.785000000000001,-0.780000000000001,
-0.775000000000001,-0.770000000000001,-0.765000000000001,-0.760000000000001,
-0.755000000000001,-0.750000000000001,-0.745000000000001,-0.740000000000001,
-0.735000000000001,-0.730000000000001,-0.725000000000001,-0.720000000000001,
-0.715000000000001,-0.710000000000001,-0.705000000000001,-0.700000000000001,
-0.695000000000001,-0.690000000000001,-0.685,-0.68,-0.675,-0.67,-0.665,
-0.66,-0.655,-0.65,-0.645,-0.64,-0.635,-0.63,-0.625,-0.62,-0.615,-0.61,
-0.605,-0.6,-0.595,-0.59,-0.585,-0.58,-0.575,-0.57,-0.565,-0.56,-0.555,
-0.55,-0.545,-0.54,-0.535,-0.53,-0.525,-0.52,-0.515,-0.51,-0.505,-0.5,-0.495,
-0.49,-0.485,-0.48,-0.475,-0.47,-0.465,-0.46,-0.455,-0.45,-0.445,-0.44,
-0.435,-0.43,-0.425,-0.42,-0.415,-0.41,-0.405,-0.4,-0.395,-0.39,-0.385,
-0.38,-0.375,-0.37,-0.365,-0.36,-0.355,-0.35,-0.345,-0.34,-0.335,-0.33,
-0.325,-0.32,-0.315,-0.31,-0.305,-0.3,-0.295,-0.29,-0.285,-0.28,-0.275,
-0.27,-0.265,-0.26,-0.255,-0.25,-0.245,-0.24,-0.235,-0.23,-0.225,-0.22,
-0.215,-0.21,-0.205,-0.2,-0.195,-0.19,-0.185,-0.18,-0.175,-0.17,-0.165,
-0.16,-0.155,-0.15,-0.145,-0.14,-0.135,-0.13,-0.125,-0.12,-0.115,-0.11,
-0.105,-0.1,-0.095,-0.09,-0.085,-0.08,-0.075,-0.07,-0.065,-0.06,-0.055,
-0.05,-0.045,-0.04,-0.035,-0.03,-0.025,-0.02,-0.015,-0.01,-0.005,0.),(0.,
1.2),.UNSPECIFIED.)
GEOMETRIC_REPRESENTATION_ITEM()
RATIONAL_B_SPLINE_SURFACE(((1.,1.),(1.,1.),(1.,1.),(1.,1.),(1.,1.),(1.,
1.),(1.,1.),(1.,1.),(1.,1.),(1.,1.),(1.,1.),(1.,1.),(1.,1.),(1.,1.),(1.,
1.),(1.,1.),(1.,1.),(1.,1.),(1.,1.),(1.,1.),(1.,1.),(1.,1.),(1.,1.),(1.,
1.),(1.,1.),(1.,1.),(1.,1.),(1.,1.),(1.,1.),(1.,1.),(1.,1.),(1.,1.),(1.,
1.),(1.,1.),(1.,1.),(1.,1.),(1.,1.),(1.,1.),(1.,1.),(1.,1.),(1.,1.),(1.,
1.),(1.,1.),(1.,1.),(1.,1.),(1.,1.),(1.,1.),(1.,1.),(1.,1.),(1.,1.),(1.,
1.),(1.,1.),(1.,1.),(1.,1.),(1.,1.),(1.,1.),(1.,1.),(1.,1.),(1.,1.),(1.,
1.),(1.,1.),(1.,1.),(1.,1.),(1.,1.),(1.,1.),(1.,1.),(1.,1.),(1.,1.),(1.,
1.),(1.,1.),(1.,1.),(1.,1.),(1.,1.),(1.,1.),(1.,1.),(1.,1.),(1.,1.),(1.,
1.),(1.,1.),(1.,1.),(1.,1.),(1.,1.),(1.,1.),(1.,1.),(1.,1.),(1.,1.),(1.,
1.),(1.,1.),(1.,1.),(1.,1.),(1.,1.),(1.,1.),(1.,1.),(1.,1.),(1.,1.),(1.,
1.),(1.,1.),(1.,1.),(1.,1.),(1.,1.),(1.,1.),(1.,1.),(1.,1.),(1.,1.),(1.,
1.),(1.,1.),(1.,1.),(1.,1.),(1.,1.),(1.,1.),(1.,1.),(1.,1.),(1.,1.),(1.,
1.),(1.,1.),(1.,1.),(1.,1.),(1.,1.),(1.,1.),(1.,1.),(1.,1.),(1.,1.),(1.,
1.),(1.,1.),(1.,1.),(1.,1.),(1.,1.),(1.,1.),(1.,1.),(1.,1.),(1.,1.),(1.,
1.),(1.,1.),(1.,1.),(1.,1.),(1.,1.),(1.,1.),(1.,1.),(1.,1.),(1.,1.),(1.,
1.),(1.,1.),(1.,1.),(1.,1.),(1.,1.),(1.,1.),(1.,1.),(1.,1.),(1.,1.),(1.,
1.),(1.,1.),(1.,1.),(1.,1.),(1.,1.),(1.,1.),(1.,1.),(1.,1.),(1.,1.),(1.,
1.),(1.,1.),(1.,1.),(1.,1.),(1.,1.),(1.,1.),(1.,1.),(1.,1.),(1.,1.),(1.,
1.),(1.,1.),(1.,1.),(1.,1.),(1.,1.),(1.,1.),(1.,1.),(1.,1.),(1.,1.),(1.,
1.),(1.,1.),(1.,1.),(1.,1.),(1.,1.),(1.,1.),(1.,1.),(1.,1.),(1.,1.),(1.,
1.),(1.,1.),(1.,1.),(1.,1.),(1.,1.),(1.,1.),(1.,1.),(1.,1.),(1.,1.),(1.,
1.),(1.,1.),(1.,1.),(1.,1.),(1.,1.),(1.,1.),(1.,1.),(1.,1.),(1.,1.),(1.,
1.),(1.,1.)))
REPRESENTATION_ITEM('')
SURFACE()
);
#1016=(
BOUNDED_SURFACE()
B_SPLINE_SURFACE(5,1,((#165854,#165855),(#165856,#165857),(#165858,#165859),
(#165860,#165861),(#165862,#165863),(#165864,#165865),(#165866,#165867),
(#165868,#165869),(#165870,#165871),(#165872,#165873),(#165874,#165875),
(#165876,#165877),(#165878,#165879),(#165880,#165881),(#165882,#165883),
(#165884,#165885),(#165886,#165887),(#165888,#165889),(#165890,#165891),
(#165892,#165893),(#165894,#165895),(#165896,#165897),(#165898,#165899),
(#165900,#165901),(#165902,#165903),(#165904,#165905),(#165906,#165907),
(#165908,#165909),(#165910,#165911),(#165912,#165913),(#165914,#165915),
(#165916,#165917),(#165918,#165919),(#165920,#165921),(#165922,#165923),
(#165924,#165925),(#165926,#165927),(#165928,#165929),(#165930,#165931),
(#165932,#165933),(#165934,#165935),(#165936,#165937),(#165938,#165939),
(#165940,#165941),(#165942,#165943),(#165944,#165945),(#165946,#165947),
(#165948,#165949),(#165950,#165951),(#165952,#165953),(#165954,#165955),
(#165956,#165957),(#165958,#165959),(#165960,#165961),(#165962,#165963),
(#165964,#165965),(#165966,#165967),(#165968,#165969),(#165970,#165971),
(#165972,#165973),(#165974,#165975),(#165976,#165977),(#165978,#165979),
(#165980,#165981),(#165982,#165983),(#165984,#165985),(#165986,#165987),
(#165988,#165989),(#165990,#165991),(#165992,#165993),(#165994,#165995),
(#165996,#165997),(#165998,#165999),(#166000,#166001),(#166002,#166003),
(#166004,#166005),(#166006,#166007),(#166008,#166009),(#166010,#166011),
(#166012,#166013),(#166014,#166015),(#166016,#166017),(#166018,#166019),
(#166020,#166021),(#166022,#166023),(#166024,#166025),(#166026,#166027),
(#166028,#166029),(#166030,#166031),(#166032,#166033),(#166034,#166035),
(#166036,#166037),(#166038,#166039),(#166040,#166041),(#166042,#166043),
(#166044,#166045),(#166046,#166047),(#166048,#166049),(#166050,#166051),
(#166052,#166053),(#166054,#166055),(#166056,#166057),(#166058,#166059),
(#166060,#166061),(#166062,#166063),(#166064,#166065),(#166066,#166067),
(#166068,#166069),(#166070,#166071),(#166072,#166073),(#166074,#166075),
(#166076,#166077),(#166078,#166079),(#166080,#166081),(#166082,#166083),
(#166084,#166085),(#166086,#166087),(#166088,#166089),(#166090,#166091),
(#166092,#166093),(#166094,#166095),(#166096,#166097),(#166098,#166099),
(#166100,#166101),(#166102,#166103),(#166104,#166105),(#166106,#166107),
(#166108,#166109),(#166110,#166111),(#166112,#166113),(#166114,#166115),
(#166116,#166117),(#166118,#166119),(#166120,#166121),(#166122,#166123),
(#166124,#166125),(#166126,#166127),(#166128,#166129),(#166130,#166131),
(#166132,#166133),(#166134,#166135),(#166136,#166137),(#166138,#166139),
(#166140,#166141),(#166142,#166143),(#166144,#166145),(#166146,#166147),
(#166148,#166149),(#166150,#166151),(#166152,#166153),(#166154,#166155),
(#166156,#166157),(#166158,#166159),(#166160,#166161),(#166162,#166163),
(#166164,#166165),(#166166,#166167),(#166168,#166169),(#166170,#166171),
(#166172,#166173),(#166174,#166175),(#166176,#166177),(#166178,#166179),
(#166180,#166181),(#166182,#166183),(#166184,#166185),(#166186,#166187),
(#166188,#166189),(#166190,#166191),(#166192,#166193),(#166194,#166195),
(#166196,#166197),(#166198,#166199),(#166200,#166201),(#166202,#166203),
(#166204,#166205),(#166206,#166207),(#166208,#166209),(#166210,#166211),
(#166212,#166213),(#166214,#166215),(#166216,#166217),(#166218,#166219),
(#166220,#166221),(#166222,#166223),(#166224,#166225),(#166226,#166227),
(#166228,#166229),(#166230,#166231),(#166232,#166233),(#166234,#166235),
(#166236,#166237),(#166238,#166239),(#166240,#166241),(#166242,#166243),
(#166244,#166245),(#166246,#166247),(#166248,#166249),(#166250,#166251),
(#166252,#166253),(#166254,#166255),(#166256,#166257),(#166258,#166259),
(#166260,#166261),(#166262,#166263)),.UNSPECIFIED.,.F.,.F.,.F.)
B_SPLINE_SURFACE_WITH_KNOTS((6,1,1,1,1,1,1,1,1,1,1,1,1,1,1,1,1,1,1,1,1,
1,1,1,1,1,1,1,1,1,1,1,1,1,1,1,1,1,1,1,1,1,1,1,1,1,1,1,1,1,1,1,1,1,1,1,1,
1,1,1,1,1,1,1,1,1,1,1,1,1,1,1,1,1,1,1,1,1,1,1,1,1,1,1,1,1,1,1,1,1,1,1,1,
1,1,1,1,1,1,1,1,1,1,1,1,1,1,1,1,1,1,1,1,1,1,1,1,1,1,1,1,1,1,1,1,1,1,1,1,
1,1,1,1,1,1,1,1,1,1,1,1,1,1,1,1,1,1,1,1,1,1,1,1,1,1,1,1,1,1,1,1,1,1,1,1,
1,1,1,1,1,1,1,1,1,1,1,1,1,1,1,1,1,1,1,1,1,1,1,1,1,1,1,1,1,1,1,1,1,1,1,6),
(2,2),(-1.,-0.995000000000001,-0.990000000000001,-0.985000000000001,-0.980000000000001,
-0.975000000000001,-0.970000000000001,-0.965000000000001,-0.960000000000001,
-0.955000000000001,-0.950000000000001,-0.945000000000001,-0.940000000000001,
-0.935000000000001,-0.930000000000001,-0.925000000000001,-0.920000000000001,
-0.915000000000001,-0.910000000000001,-0.905000000000001,-0.900000000000001,
-0.895000000000001,-0.890000000000001,-0.885000000000001,-0.880000000000001,
-0.875000000000001,-0.870000000000001,-0.865000000000001,-0.860000000000001,
-0.855000000000001,-0.850000000000001,-0.845000000000001,-0.840000000000001,
-0.835000000000001,-0.830000000000001,-0.825000000000001,-0.820000000000001,
-0.815000000000001,-0.810000000000001,-0.805000000000001,-0.800000000000001,
-0.795000000000001,-0.790000000000001,-0.785000000000001,-0.780000000000001,
-0.775000000000001,-0.770000000000001,-0.765000000000001,-0.760000000000001,
-0.755000000000001,-0.750000000000001,-0.745000000000001,-0.740000000000001,
-0.735000000000001,-0.730000000000001,-0.725000000000001,-0.720000000000001,
-0.715000000000001,-0.710000000000001,-0.705000000000001,-0.700000000000001,
-0.695000000000001,-0.690000000000001,-0.685,-0.68,-0.675,-0.67,-0.665,
-0.66,-0.655,-0.65,-0.645,-0.64,-0.635,-0.63,-0.625,-0.62,-0.615,-0.61,
-0.605,-0.6,-0.595,-0.59,-0.585,-0.58,-0.575,-0.57,-0.565,-0.56,-0.555,
-0.55,-0.545,-0.54,-0.535,-0.53,-0.525,-0.52,-0.515,-0.51,-0.505,-0.5,-0.495,
-0.49,-0.485,-0.48,-0.475,-0.47,-0.465,-0.46,-0.455,-0.45,-0.445,-0.44,
-0.435,-0.43,-0.425,-0.42,-0.415,-0.41,-0.405,-0.4,-0.395,-0.39,-0.385,
-0.38,-0.375,-0.37,-0.365,-0.36,-0.355,-0.35,-0.345,-0.34,-0.335,-0.33,
-0.325,-0.32,-0.315,-0.31,-0.305,-0.3,-0.295,-0.29,-0.285,-0.28,-0.275,
-0.27,-0.265,-0.26,-0.255,-0.25,-0.245,-0.24,-0.235,-0.23,-0.225,-0.22,
-0.215,-0.21,-0.205,-0.2,-0.195,-0.19,-0.185,-0.18,-0.175,-0.17,-0.165,
-0.16,-0.155,-0.15,-0.145,-0.14,-0.135,-0.13,-0.125,-0.12,-0.115,-0.11,
-0.105,-0.1,-0.095,-0.09,-0.085,-0.08,-0.075,-0.07,-0.065,-0.06,-0.055,
-0.05,-0.045,-0.04,-0.035,-0.03,-0.025,-0.02,-0.015,-0.01,-0.005,0.),(0.,
1.2),.UNSPECIFIED.)
GEOMETRIC_REPRESENTATION_ITEM()
RATIONAL_B_SPLINE_SURFACE(((1.,1.),(1.,1.),(1.,1.),(1.,1.),(1.,1.),(1.,
1.),(1.,1.),(1.,1.),(1.,1.),(1.,1.),(1.,1.),(1.,1.),(1.,1.),(1.,1.),(1.,
1.),(1.,1.),(1.,1.),(1.,1.),(1.,1.),(1.,1.),(1.,1.),(1.,1.),(1.,1.),(1.,
1.),(1.,1.),(1.,1.),(1.,1.),(1.,1.),(1.,1.),(1.,1.),(1.,1.),(1.,1.),(1.,
1.),(1.,1.),(1.,1.),(1.,1.),(1.,1.),(1.,1.),(1.,1.),(1.,1.),(1.,1.),(1.,
1.),(1.,1.),(1.,1.),(1.,1.),(1.,1.),(1.,1.),(1.,1.),(1.,1.),(1.,1.),(1.,
1.),(1.,1.),(1.,1.),(1.,1.),(1.,1.),(1.,1.),(1.,1.),(1.,1.),(1.,1.),(1.,
1.),(1.,1.),(1.,1.),(1.,1.),(1.,1.),(1.,1.),(1.,1.),(1.,1.),(1.,1.),(1.,
1.),(1.,1.),(1.,1.),(1.,1.),(1.,1.),(1.,1.),(1.,1.),(1.,1.),(1.,1.),(1.,
1.),(1.,1.),(1.,1.),(1.,1.),(1.,1.),(1.,1.),(1.,1.),(1.,1.),(1.,1.),(1.,
1.),(1.,1.),(1.,1.),(1.,1.),(1.,1.),(1.,1.),(1.,1.),(1.,1.),(1.,1.),(1.,
1.),(1.,1.),(1.,1.),(1.,1.),(1.,1.),(1.,1.),(1.,1.),(1.,1.),(1.,1.),(1.,
1.),(1.,1.),(1.,1.),(1.,1.),(1.,1.),(1.,1.),(1.,1.),(1.,1.),(1.,1.),(1.,
1.),(1.,1.),(1.,1.),(1.,1.),(1.,1.),(1.,1.),(1.,1.),(1.,1.),(1.,1.),(1.,
1.),(1.,1.),(1.,1.),(1.,1.),(1.,1.),(1.,1.),(1.,1.),(1.,1.),(1.,1.),(1.,
1.),(1.,1.),(1.,1.),(1.,1.),(1.,1.),(1.,1.),(1.,1.),(1.,1.),(1.,1.),(1.,
1.),(1.,1.),(1.,1.),(1.,1.),(1.,1.),(1.,1.),(1.,1.),(1.,1.),(1.,1.),(1.,
1.),(1.,1.),(1.,1.),(1.,1.),(1.,1.),(1.,1.),(1.,1.),(1.,1.),(1.,1.),(1.,
1.),(1.,1.),(1.,1.),(1.,1.),(1.,1.),(1.,1.),(1.,1.),(1.,1.),(1.,1.),(1.,
1.),(1.,1.),(1.,1.),(1.,1.),(1.,1.),(1.,1.),(1.,1.),(1.,1.),(1.,1.),(1.,
1.),(1.,1.),(1.,1.),(1.,1.),(1.,1.),(1.,1.),(1.,1.),(1.,1.),(1.,1.),(1.,
1.),(1.,1.),(1.,1.),(1.,1.),(1.,1.),(1.,1.),(1.,1.),(1.,1.),(1.,1.),(1.,
1.),(1.,1.),(1.,1.),(1.,1.),(1.,1.),(1.,1.),(1.,1.),(1.,1.),(1.,1.),(1.,
1.),(1.,1.)))
REPRESENTATION_ITEM('')
SURFACE()
);
#1017=(
BOUNDED_SURFACE()
B_SPLINE_SURFACE(5,1,((#166655,#166656),(#166657,#166658),(#166659,#166660),
(#166661,#166662),(#166663,#166664),(#166665,#166666),(#166667,#166668),
(#166669,#166670),(#166671,#166672),(#166673,#166674),(#166675,#166676),
(#166677,#166678),(#166679,#166680),(#166681,#166682),(#166683,#166684),
(#166685,#166686),(#166687,#166688),(#166689,#166690),(#166691,#166692),
(#166693,#166694),(#166695,#166696),(#166697,#166698),(#166699,#166700),
(#166701,#166702),(#166703,#166704),(#166705,#166706),(#166707,#166708),
(#166709,#166710),(#166711,#166712),(#166713,#166714),(#166715,#166716),
(#166717,#166718),(#166719,#166720),(#166721,#166722),(#166723,#166724),
(#166725,#166726),(#166727,#166728),(#166729,#166730),(#166731,#166732),
(#166733,#166734),(#166735,#166736),(#166737,#166738),(#166739,#166740),
(#166741,#166742),(#166743,#166744),(#166745,#166746),(#166747,#166748),
(#166749,#166750),(#166751,#166752),(#166753,#166754),(#166755,#166756),
(#166757,#166758),(#166759,#166760),(#166761,#166762),(#166763,#166764),
(#166765,#166766),(#166767,#166768),(#166769,#166770),(#166771,#166772),
(#166773,#166774),(#166775,#166776),(#166777,#166778),(#166779,#166780),
(#166781,#166782),(#166783,#166784),(#166785,#166786),(#166787,#166788),
(#166789,#166790),(#166791,#166792),(#166793,#166794),(#166795,#166796),
(#166797,#166798),(#166799,#166800),(#166801,#166802),(#166803,#166804),
(#166805,#166806),(#166807,#166808),(#166809,#166810),(#166811,#166812),
(#166813,#166814),(#166815,#166816),(#166817,#166818),(#166819,#166820),
(#166821,#166822),(#166823,#166824),(#166825,#166826),(#166827,#166828),
(#166829,#166830),(#166831,#166832),(#166833,#166834),(#166835,#166836),
(#166837,#166838),(#166839,#166840),(#166841,#166842),(#166843,#166844),
(#166845,#166846),(#166847,#166848),(#166849,#166850),(#166851,#166852),
(#166853,#166854),(#166855,#166856),(#166857,#166858),(#166859,#166860),
(#166861,#166862),(#166863,#166864),(#166865,#166866),(#166867,#166868),
(#166869,#166870),(#166871,#166872),(#166873,#166874),(#166875,#166876),
(#166877,#166878),(#166879,#166880),(#166881,#166882),(#166883,#166884),
(#166885,#166886),(#166887,#166888),(#166889,#166890),(#166891,#166892),
(#166893,#166894),(#166895,#166896),(#166897,#166898),(#166899,#166900),
(#166901,#166902),(#166903,#166904),(#166905,#166906),(#166907,#166908),
(#166909,#166910),(#166911,#166912),(#166913,#166914),(#166915,#166916),
(#166917,#166918),(#166919,#166920),(#166921,#166922),(#166923,#166924),
(#166925,#166926),(#166927,#166928),(#166929,#166930),(#166931,#166932),
(#166933,#166934),(#166935,#166936),(#166937,#166938),(#166939,#166940),
(#166941,#166942),(#166943,#166944),(#166945,#166946),(#166947,#166948),
(#166949,#166950),(#166951,#166952),(#166953,#166954),(#166955,#166956),
(#166957,#166958),(#166959,#166960),(#166961,#166962),(#166963,#166964),
(#166965,#166966),(#166967,#166968),(#166969,#166970),(#166971,#166972),
(#166973,#166974),(#166975,#166976),(#166977,#166978),(#166979,#166980),
(#166981,#166982),(#166983,#166984),(#166985,#166986),(#166987,#166988),
(#166989,#166990),(#166991,#166992),(#166993,#166994),(#166995,#166996),
(#166997,#166998),(#166999,#167000),(#167001,#167002),(#167003,#167004),
(#167005,#167006),(#167007,#167008),(#167009,#167010),(#167011,#167012),
(#167013,#167014),(#167015,#167016),(#167017,#167018),(#167019,#167020),
(#167021,#167022),(#167023,#167024),(#167025,#167026),(#167027,#167028),
(#167029,#167030),(#167031,#167032),(#167033,#167034),(#167035,#167036),
(#167037,#167038),(#167039,#167040),(#167041,#167042),(#167043,#167044),
(#167045,#167046),(#167047,#167048),(#167049,#167050),(#167051,#167052),
(#167053,#167054),(#167055,#167056),(#167057,#167058),(#167059,#167060),
(#167061,#167062),(#167063,#167064)),.UNSPECIFIED.,.F.,.F.,.F.)
B_SPLINE_SURFACE_WITH_KNOTS((6,1,1,1,1,1,1,1,1,1,1,1,1,1,1,1,1,1,1,1,1,
1,1,1,1,1,1,1,1,1,1,1,1,1,1,1,1,1,1,1,1,1,1,1,1,1,1,1,1,1,1,1,1,1,1,1,1,
1,1,1,1,1,1,1,1,1,1,1,1,1,1,1,1,1,1,1,1,1,1,1,1,1,1,1,1,1,1,1,1,1,1,1,1,
1,1,1,1,1,1,1,1,1,1,1,1,1,1,1,1,1,1,1,1,1,1,1,1,1,1,1,1,1,1,1,1,1,1,1,1,
1,1,1,1,1,1,1,1,1,1,1,1,1,1,1,1,1,1,1,1,1,1,1,1,1,1,1,1,1,1,1,1,1,1,1,1,
1,1,1,1,1,1,1,1,1,1,1,1,1,1,1,1,1,1,1,1,1,1,1,1,1,1,1,1,1,1,1,1,1,1,1,6),
(2,2),(-1.,-0.995000000000001,-0.990000000000001,-0.985000000000001,-0.980000000000001,
-0.975000000000001,-0.970000000000001,-0.965000000000001,-0.960000000000001,
-0.955000000000001,-0.950000000000001,-0.945000000000001,-0.940000000000001,
-0.935000000000001,-0.930000000000001,-0.925000000000001,-0.920000000000001,
-0.915000000000001,-0.910000000000001,-0.905000000000001,-0.900000000000001,
-0.895000000000001,-0.890000000000001,-0.885000000000001,-0.880000000000001,
-0.875000000000001,-0.870000000000001,-0.865000000000001,-0.860000000000001,
-0.855000000000001,-0.850000000000001,-0.845000000000001,-0.840000000000001,
-0.835000000000001,-0.830000000000001,-0.825000000000001,-0.820000000000001,
-0.815000000000001,-0.810000000000001,-0.805000000000001,-0.800000000000001,
-0.795000000000001,-0.790000000000001,-0.785000000000001,-0.780000000000001,
-0.775000000000001,-0.770000000000001,-0.765000000000001,-0.760000000000001,
-0.755000000000001,-0.750000000000001,-0.745000000000001,-0.740000000000001,
-0.735000000000001,-0.730000000000001,-0.725000000000001,-0.720000000000001,
-0.715000000000001,-0.710000000000001,-0.705000000000001,-0.700000000000001,
-0.695000000000001,-0.690000000000001,-0.685,-0.68,-0.675,-0.67,-0.665,
-0.66,-0.655,-0.65,-0.645,-0.64,-0.635,-0.63,-0.625,-0.62,-0.615,-0.61,
-0.605,-0.6,-0.595,-0.59,-0.585,-0.58,-0.575,-0.57,-0.565,-0.56,-0.555,
-0.55,-0.545,-0.54,-0.535,-0.53,-0.525,-0.52,-0.515,-0.51,-0.505,-0.5,-0.495,
-0.49,-0.485,-0.48,-0.475,-0.47,-0.465,-0.46,-0.455,-0.45,-0.445,-0.44,
-0.435,-0.43,-0.425,-0.42,-0.415,-0.41,-0.405,-0.4,-0.395,-0.39,-0.385,
-0.38,-0.375,-0.37,-0.365,-0.36,-0.355,-0.35,-0.345,-0.34,-0.335,-0.33,
-0.325,-0.32,-0.315,-0.31,-0.305,-0.3,-0.295,-0.29,-0.285,-0.28,-0.275,
-0.27,-0.265,-0.26,-0.255,-0.25,-0.245,-0.24,-0.235,-0.23,-0.225,-0.22,
-0.215,-0.21,-0.205,-0.2,-0.195,-0.19,-0.185,-0.18,-0.175,-0.17,-0.165,
-0.16,-0.155,-0.15,-0.145,-0.14,-0.135,-0.13,-0.125,-0.12,-0.115,-0.11,
-0.105,-0.1,-0.095,-0.09,-0.085,-0.08,-0.075,-0.07,-0.065,-0.06,-0.055,
-0.05,-0.045,-0.04,-0.035,-0.03,-0.025,-0.02,-0.015,-0.01,-0.005,0.),(0.,
1.2),.UNSPECIFIED.)
GEOMETRIC_REPRESENTATION_ITEM()
RATIONAL_B_SPLINE_SURFACE(((1.,1.),(1.,1.),(1.,1.),(1.,1.),(1.,1.),(1.,
1.),(1.,1.),(1.,1.),(1.,1.),(1.,1.),(1.,1.),(1.,1.),(1.,1.),(1.,1.),(1.,
1.),(1.,1.),(1.,1.),(1.,1.),(1.,1.),(1.,1.),(1.,1.),(1.,1.),(1.,1.),(1.,
1.),(1.,1.),(1.,1.),(1.,1.),(1.,1.),(1.,1.),(1.,1.),(1.,1.),(1.,1.),(1.,
1.),(1.,1.),(1.,1.),(1.,1.),(1.,1.),(1.,1.),(1.,1.),(1.,1.),(1.,1.),(1.,
1.),(1.,1.),(1.,1.),(1.,1.),(1.,1.),(1.,1.),(1.,1.),(1.,1.),(1.,1.),(1.,
1.),(1.,1.),(1.,1.),(1.,1.),(1.,1.),(1.,1.),(1.,1.),(1.,1.),(1.,1.),(1.,
1.),(1.,1.),(1.,1.),(1.,1.),(1.,1.),(1.,1.),(1.,1.),(1.,1.),(1.,1.),(1.,
1.),(1.,1.),(1.,1.),(1.,1.),(1.,1.),(1.,1.),(1.,1.),(1.,1.),(1.,1.),(1.,
1.),(1.,1.),(1.,1.),(1.,1.),(1.,1.),(1.,1.),(1.,1.),(1.,1.),(1.,1.),(1.,
1.),(1.,1.),(1.,1.),(1.,1.),(1.,1.),(1.,1.),(1.,1.),(1.,1.),(1.,1.),(1.,
1.),(1.,1.),(1.,1.),(1.,1.),(1.,1.),(1.,1.),(1.,1.),(1.,1.),(1.,1.),(1.,
1.),(1.,1.),(1.,1.),(1.,1.),(1.,1.),(1.,1.),(1.,1.),(1.,1.),(1.,1.),(1.,
1.),(1.,1.),(1.,1.),(1.,1.),(1.,1.),(1.,1.),(1.,1.),(1.,1.),(1.,1.),(1.,
1.),(1.,1.),(1.,1.),(1.,1.),(1.,1.),(1.,1.),(1.,1.),(1.,1.),(1.,1.),(1.,
1.),(1.,1.),(1.,1.),(1.,1.),(1.,1.),(1.,1.),(1.,1.),(1.,1.),(1.,1.),(1.,
1.),(1.,1.),(1.,1.),(1.,1.),(1.,1.),(1.,1.),(1.,1.),(1.,1.),(1.,1.),(1.,
1.),(1.,1.),(1.,1.),(1.,1.),(1.,1.),(1.,1.),(1.,1.),(1.,1.),(1.,1.),(1.,
1.),(1.,1.),(1.,1.),(1.,1.),(1.,1.),(1.,1.),(1.,1.),(1.,1.),(1.,1.),(1.,
1.),(1.,1.),(1.,1.),(1.,1.),(1.,1.),(1.,1.),(1.,1.),(1.,1.),(1.,1.),(1.,
1.),(1.,1.),(1.,1.),(1.,1.),(1.,1.),(1.,1.),(1.,1.),(1.,1.),(1.,1.),(1.,
1.),(1.,1.),(1.,1.),(1.,1.),(1.,1.),(1.,1.),(1.,1.),(1.,1.),(1.,1.),(1.,
1.),(1.,1.),(1.,1.),(1.,1.),(1.,1.),(1.,1.),(1.,1.),(1.,1.),(1.,1.),(1.,
1.),(1.,1.)))
REPRESENTATION_ITEM('')
SURFACE()
);
#1018=(
BOUNDED_SURFACE()
B_SPLINE_SURFACE(5,1,((#167456,#167457),(#167458,#167459),(#167460,#167461),
(#167462,#167463),(#167464,#167465),(#167466,#167467),(#167468,#167469),
(#167470,#167471),(#167472,#167473),(#167474,#167475),(#167476,#167477),
(#167478,#167479),(#167480,#167481),(#167482,#167483),(#167484,#167485),
(#167486,#167487),(#167488,#167489),(#167490,#167491),(#167492,#167493),
(#167494,#167495),(#167496,#167497),(#167498,#167499),(#167500,#167501),
(#167502,#167503),(#167504,#167505),(#167506,#167507),(#167508,#167509),
(#167510,#167511),(#167512,#167513),(#167514,#167515),(#167516,#167517),
(#167518,#167519),(#167520,#167521),(#167522,#167523),(#167524,#167525),
(#167526,#167527),(#167528,#167529),(#167530,#167531),(#167532,#167533),
(#167534,#167535),(#167536,#167537),(#167538,#167539),(#167540,#167541),
(#167542,#167543),(#167544,#167545),(#167546,#167547),(#167548,#167549),
(#167550,#167551),(#167552,#167553),(#167554,#167555),(#167556,#167557),
(#167558,#167559),(#167560,#167561),(#167562,#167563),(#167564,#167565),
(#167566,#167567),(#167568,#167569),(#167570,#167571),(#167572,#167573),
(#167574,#167575),(#167576,#167577),(#167578,#167579),(#167580,#167581),
(#167582,#167583),(#167584,#167585),(#167586,#167587),(#167588,#167589),
(#167590,#167591),(#167592,#167593),(#167594,#167595),(#167596,#167597),
(#167598,#167599),(#167600,#167601),(#167602,#167603),(#167604,#167605),
(#167606,#167607),(#167608,#167609),(#167610,#167611),(#167612,#167613),
(#167614,#167615),(#167616,#167617),(#167618,#167619),(#167620,#167621),
(#167622,#167623),(#167624,#167625),(#167626,#167627),(#167628,#167629),
(#167630,#167631),(#167632,#167633),(#167634,#167635),(#167636,#167637),
(#167638,#167639),(#167640,#167641),(#167642,#167643),(#167644,#167645),
(#167646,#167647),(#167648,#167649),(#167650,#167651),(#167652,#167653),
(#167654,#167655),(#167656,#167657),(#167658,#167659),(#167660,#167661),
(#167662,#167663),(#167664,#167665),(#167666,#167667),(#167668,#167669),
(#167670,#167671),(#167672,#167673),(#167674,#167675),(#167676,#167677),
(#167678,#167679),(#167680,#167681),(#167682,#167683),(#167684,#167685),
(#167686,#167687),(#167688,#167689),(#167690,#167691),(#167692,#167693),
(#167694,#167695),(#167696,#167697),(#167698,#167699),(#167700,#167701),
(#167702,#167703),(#167704,#167705),(#167706,#167707),(#167708,#167709),
(#167710,#167711),(#167712,#167713),(#167714,#167715),(#167716,#167717),
(#167718,#167719),(#167720,#167721),(#167722,#167723),(#167724,#167725),
(#167726,#167727),(#167728,#167729),(#167730,#167731),(#167732,#167733),
(#167734,#167735),(#167736,#167737),(#167738,#167739),(#167740,#167741),
(#167742,#167743),(#167744,#167745),(#167746,#167747),(#167748,#167749),
(#167750,#167751),(#167752,#167753),(#167754,#167755),(#167756,#167757),
(#167758,#167759),(#167760,#167761),(#167762,#167763),(#167764,#167765),
(#167766,#167767),(#167768,#167769),(#167770,#167771),(#167772,#167773),
(#167774,#167775),(#167776,#167777),(#167778,#167779),(#167780,#167781),
(#167782,#167783),(#167784,#167785),(#167786,#167787),(#167788,#167789),
(#167790,#167791),(#167792,#167793),(#167794,#167795),(#167796,#167797),
(#167798,#167799),(#167800,#167801),(#167802,#167803),(#167804,#167805),
(#167806,#167807),(#167808,#167809),(#167810,#167811),(#167812,#167813),
(#167814,#167815),(#167816,#167817),(#167818,#167819),(#167820,#167821),
(#167822,#167823),(#167824,#167825),(#167826,#167827),(#167828,#167829),
(#167830,#167831),(#167832,#167833),(#167834,#167835),(#167836,#167837),
(#167838,#167839),(#167840,#167841),(#167842,#167843),(#167844,#167845),
(#167846,#167847),(#167848,#167849),(#167850,#167851),(#167852,#167853),
(#167854,#167855),(#167856,#167857),(#167858,#167859),(#167860,#167861),
(#167862,#167863),(#167864,#167865)),.UNSPECIFIED.,.F.,.F.,.F.)
B_SPLINE_SURFACE_WITH_KNOTS((6,1,1,1,1,1,1,1,1,1,1,1,1,1,1,1,1,1,1,1,1,
1,1,1,1,1,1,1,1,1,1,1,1,1,1,1,1,1,1,1,1,1,1,1,1,1,1,1,1,1,1,1,1,1,1,1,1,
1,1,1,1,1,1,1,1,1,1,1,1,1,1,1,1,1,1,1,1,1,1,1,1,1,1,1,1,1,1,1,1,1,1,1,1,
1,1,1,1,1,1,1,1,1,1,1,1,1,1,1,1,1,1,1,1,1,1,1,1,1,1,1,1,1,1,1,1,1,1,1,1,
1,1,1,1,1,1,1,1,1,1,1,1,1,1,1,1,1,1,1,1,1,1,1,1,1,1,1,1,1,1,1,1,1,1,1,1,
1,1,1,1,1,1,1,1,1,1,1,1,1,1,1,1,1,1,1,1,1,1,1,1,1,1,1,1,1,1,1,1,1,1,1,6),
(2,2),(-1.,-0.995000000000001,-0.990000000000001,-0.985000000000001,-0.980000000000001,
-0.975000000000001,-0.970000000000001,-0.965000000000001,-0.960000000000001,
-0.955000000000001,-0.950000000000001,-0.945000000000001,-0.940000000000001,
-0.935000000000001,-0.930000000000001,-0.925000000000001,-0.920000000000001,
-0.915000000000001,-0.910000000000001,-0.905000000000001,-0.900000000000001,
-0.895000000000001,-0.890000000000001,-0.885000000000001,-0.880000000000001,
-0.875000000000001,-0.870000000000001,-0.865000000000001,-0.860000000000001,
-0.855000000000001,-0.850000000000001,-0.845000000000001,-0.840000000000001,
-0.835000000000001,-0.830000000000001,-0.825000000000001,-0.820000000000001,
-0.815000000000001,-0.810000000000001,-0.805000000000001,-0.800000000000001,
-0.795000000000001,-0.790000000000001,-0.785000000000001,-0.780000000000001,
-0.775000000000001,-0.770000000000001,-0.765000000000001,-0.760000000000001,
-0.755000000000001,-0.750000000000001,-0.745000000000001,-0.740000000000001,
-0.735000000000001,-0.730000000000001,-0.725000000000001,-0.720000000000001,
-0.715000000000001,-0.710000000000001,-0.705000000000001,-0.700000000000001,
-0.695000000000001,-0.690000000000001,-0.685,-0.68,-0.675,-0.67,-0.665,
-0.66,-0.655,-0.65,-0.645,-0.64,-0.635,-0.63,-0.625,-0.62,-0.615,-0.61,
-0.605,-0.6,-0.595,-0.59,-0.585,-0.58,-0.575,-0.57,-0.565,-0.56,-0.555,
-0.55,-0.545,-0.54,-0.535,-0.53,-0.525,-0.52,-0.515,-0.51,-0.505,-0.5,-0.495,
-0.49,-0.485,-0.48,-0.475,-0.47,-0.465,-0.46,-0.455,-0.45,-0.445,-0.44,
-0.435,-0.43,-0.425,-0.42,-0.415,-0.41,-0.405,-0.4,-0.395,-0.39,-0.385,
-0.38,-0.375,-0.37,-0.365,-0.36,-0.355,-0.35,-0.345,-0.34,-0.335,-0.33,
-0.325,-0.32,-0.315,-0.31,-0.305,-0.3,-0.295,-0.29,-0.285,-0.28,-0.275,
-0.27,-0.265,-0.26,-0.255,-0.25,-0.245,-0.24,-0.235,-0.23,-0.225,-0.22,
-0.215,-0.21,-0.205,-0.2,-0.195,-0.19,-0.185,-0.18,-0.175,-0.17,-0.165,
-0.16,-0.155,-0.15,-0.145,-0.14,-0.135,-0.13,-0.125,-0.12,-0.115,-0.11,
-0.105,-0.1,-0.095,-0.09,-0.085,-0.08,-0.075,-0.07,-0.065,-0.06,-0.055,
-0.05,-0.045,-0.04,-0.035,-0.03,-0.025,-0.02,-0.015,-0.01,-0.005,0.),(0.,
1.2),.UNSPECIFIED.)
GEOMETRIC_REPRESENTATION_ITEM()
RATIONAL_B_SPLINE_SURFACE(((1.,1.),(1.,1.),(1.,1.),(1.,1.),(1.,1.),(1.,
1.),(1.,1.),(1.,1.),(1.,1.),(1.,1.),(1.,1.),(1.,1.),(1.,1.),(1.,1.),(1.,
1.),(1.,1.),(1.,1.),(1.,1.),(1.,1.),(1.,1.),(1.,1.),(1.,1.),(1.,1.),(1.,
1.),(1.,1.),(1.,1.),(1.,1.),(1.,1.),(1.,1.),(1.,1.),(1.,1.),(1.,1.),(1.,
1.),(1.,1.),(1.,1.),(1.,1.),(1.,1.),(1.,1.),(1.,1.),(1.,1.),(1.,1.),(1.,
1.),(1.,1.),(1.,1.),(1.,1.),(1.,1.),(1.,1.),(1.,1.),(1.,1.),(1.,1.),(1.,
1.),(1.,1.),(1.,1.),(1.,1.),(1.,1.),(1.,1.),(1.,1.),(1.,1.),(1.,1.),(1.,
1.),(1.,1.),(1.,1.),(1.,1.),(1.,1.),(1.,1.),(1.,1.),(1.,1.),(1.,1.),(1.,
1.),(1.,1.),(1.,1.),(1.,1.),(1.,1.),(1.,1.),(1.,1.),(1.,1.),(1.,1.),(1.,
1.),(1.,1.),(1.,1.),(1.,1.),(1.,1.),(1.,1.),(1.,1.),(1.,1.),(1.,1.),(1.,
1.),(1.,1.),(1.,1.),(1.,1.),(1.,1.),(1.,1.),(1.,1.),(1.,1.),(1.,1.),(1.,
1.),(1.,1.),(1.,1.),(1.,1.),(1.,1.),(1.,1.),(1.,1.),(1.,1.),(1.,1.),(1.,
1.),(1.,1.),(1.,1.),(1.,1.),(1.,1.),(1.,1.),(1.,1.),(1.,1.),(1.,1.),(1.,
1.),(1.,1.),(1.,1.),(1.,1.),(1.,1.),(1.,1.),(1.,1.),(1.,1.),(1.,1.),(1.,
1.),(1.,1.),(1.,1.),(1.,1.),(1.,1.),(1.,1.),(1.,1.),(1.,1.),(1.,1.),(1.,
1.),(1.,1.),(1.,1.),(1.,1.),(1.,1.),(1.,1.),(1.,1.),(1.,1.),(1.,1.),(1.,
1.),(1.,1.),(1.,1.),(1.,1.),(1.,1.),(1.,1.),(1.,1.),(1.,1.),(1.,1.),(1.,
1.),(1.,1.),(1.,1.),(1.,1.),(1.,1.),(1.,1.),(1.,1.),(1.,1.),(1.,1.),(1.,
1.),(1.,1.),(1.,1.),(1.,1.),(1.,1.),(1.,1.),(1.,1.),(1.,1.),(1.,1.),(1.,
1.),(1.,1.),(1.,1.),(1.,1.),(1.,1.),(1.,1.),(1.,1.),(1.,1.),(1.,1.),(1.,
1.),(1.,1.),(1.,1.),(1.,1.),(1.,1.),(1.,1.),(1.,1.),(1.,1.),(1.,1.),(1.,
1.),(1.,1.),(1.,1.),(1.,1.),(1.,1.),(1.,1.),(1.,1.),(1.,1.),(1.,1.),(1.,
1.),(1.,1.),(1.,1.),(1.,1.),(1.,1.),(1.,1.),(1.,1.),(1.,1.),(1.,1.),(1.,
1.),(1.,1.)))
REPRESENTATION_ITEM('')
SURFACE()
);
#1019=(
BOUNDED_SURFACE()
B_SPLINE_SURFACE(5,1,((#168257,#168258),(#168259,#168260),(#168261,#168262),
(#168263,#168264),(#168265,#168266),(#168267,#168268),(#168269,#168270),
(#168271,#168272),(#168273,#168274),(#168275,#168276),(#168277,#168278),
(#168279,#168280),(#168281,#168282),(#168283,#168284),(#168285,#168286),
(#168287,#168288),(#168289,#168290),(#168291,#168292),(#168293,#168294),
(#168295,#168296),(#168297,#168298),(#168299,#168300),(#168301,#168302),
(#168303,#168304),(#168305,#168306),(#168307,#168308),(#168309,#168310),
(#168311,#168312),(#168313,#168314),(#168315,#168316),(#168317,#168318),
(#168319,#168320),(#168321,#168322),(#168323,#168324),(#168325,#168326),
(#168327,#168328),(#168329,#168330),(#168331,#168332),(#168333,#168334),
(#168335,#168336),(#168337,#168338),(#168339,#168340),(#168341,#168342),
(#168343,#168344),(#168345,#168346),(#168347,#168348),(#168349,#168350),
(#168351,#168352),(#168353,#168354),(#168355,#168356),(#168357,#168358),
(#168359,#168360),(#168361,#168362),(#168363,#168364),(#168365,#168366),
(#168367,#168368),(#168369,#168370),(#168371,#168372),(#168373,#168374),
(#168375,#168376),(#168377,#168378),(#168379,#168380),(#168381,#168382),
(#168383,#168384),(#168385,#168386),(#168387,#168388),(#168389,#168390),
(#168391,#168392),(#168393,#168394),(#168395,#168396),(#168397,#168398),
(#168399,#168400),(#168401,#168402),(#168403,#168404),(#168405,#168406),
(#168407,#168408),(#168409,#168410),(#168411,#168412),(#168413,#168414),
(#168415,#168416),(#168417,#168418),(#168419,#168420),(#168421,#168422),
(#168423,#168424),(#168425,#168426),(#168427,#168428),(#168429,#168430),
(#168431,#168432),(#168433,#168434),(#168435,#168436),(#168437,#168438),
(#168439,#168440),(#168441,#168442),(#168443,#168444),(#168445,#168446),
(#168447,#168448),(#168449,#168450),(#168451,#168452),(#168453,#168454),
(#168455,#168456),(#168457,#168458),(#168459,#168460),(#168461,#168462),
(#168463,#168464),(#168465,#168466),(#168467,#168468),(#168469,#168470),
(#168471,#168472),(#168473,#168474),(#168475,#168476),(#168477,#168478),
(#168479,#168480),(#168481,#168482),(#168483,#168484),(#168485,#168486),
(#168487,#168488),(#168489,#168490),(#168491,#168492),(#168493,#168494),
(#168495,#168496),(#168497,#168498),(#168499,#168500),(#168501,#168502),
(#168503,#168504),(#168505,#168506),(#168507,#168508),(#168509,#168510),
(#168511,#168512),(#168513,#168514),(#168515,#168516),(#168517,#168518),
(#168519,#168520),(#168521,#168522),(#168523,#168524),(#168525,#168526),
(#168527,#168528),(#168529,#168530),(#168531,#168532),(#168533,#168534),
(#168535,#168536),(#168537,#168538),(#168539,#168540),(#168541,#168542),
(#168543,#168544),(#168545,#168546),(#168547,#168548),(#168549,#168550),
(#168551,#168552),(#168553,#168554),(#168555,#168556),(#168557,#168558),
(#168559,#168560),(#168561,#168562),(#168563,#168564),(#168565,#168566),
(#168567,#168568),(#168569,#168570),(#168571,#168572),(#168573,#168574),
(#168575,#168576),(#168577,#168578),(#168579,#168580),(#168581,#168582),
(#168583,#168584),(#168585,#168586),(#168587,#168588),(#168589,#168590),
(#168591,#168592),(#168593,#168594),(#168595,#168596),(#168597,#168598),
(#168599,#168600),(#168601,#168602),(#168603,#168604),(#168605,#168606),
(#168607,#168608),(#168609,#168610),(#168611,#168612),(#168613,#168614),
(#168615,#168616),(#168617,#168618),(#168619,#168620),(#168621,#168622),
(#168623,#168624),(#168625,#168626),(#168627,#168628),(#168629,#168630),
(#168631,#168632),(#168633,#168634),(#168635,#168636),(#168637,#168638),
(#168639,#168640),(#168641,#168642),(#168643,#168644),(#168645,#168646),
(#168647,#168648),(#168649,#168650),(#168651,#168652),(#168653,#168654),
(#168655,#168656),(#168657,#168658),(#168659,#168660),(#168661,#168662),
(#168663,#168664),(#168665,#168666)),.UNSPECIFIED.,.F.,.F.,.F.)
B_SPLINE_SURFACE_WITH_KNOTS((6,1,1,1,1,1,1,1,1,1,1,1,1,1,1,1,1,1,1,1,1,
1,1,1,1,1,1,1,1,1,1,1,1,1,1,1,1,1,1,1,1,1,1,1,1,1,1,1,1,1,1,1,1,1,1,1,1,
1,1,1,1,1,1,1,1,1,1,1,1,1,1,1,1,1,1,1,1,1,1,1,1,1,1,1,1,1,1,1,1,1,1,1,1,
1,1,1,1,1,1,1,1,1,1,1,1,1,1,1,1,1,1,1,1,1,1,1,1,1,1,1,1,1,1,1,1,1,1,1,1,
1,1,1,1,1,1,1,1,1,1,1,1,1,1,1,1,1,1,1,1,1,1,1,1,1,1,1,1,1,1,1,1,1,1,1,1,
1,1,1,1,1,1,1,1,1,1,1,1,1,1,1,1,1,1,1,1,1,1,1,1,1,1,1,1,1,1,1,1,1,1,1,6),
(2,2),(-1.,-0.995000000000001,-0.990000000000001,-0.985000000000001,-0.980000000000001,
-0.975000000000001,-0.970000000000001,-0.965000000000001,-0.960000000000001,
-0.955000000000001,-0.950000000000001,-0.945000000000001,-0.940000000000001,
-0.935000000000001,-0.930000000000001,-0.925000000000001,-0.920000000000001,
-0.915000000000001,-0.910000000000001,-0.905000000000001,-0.900000000000001,
-0.895000000000001,-0.890000000000001,-0.885000000000001,-0.880000000000001,
-0.875000000000001,-0.870000000000001,-0.865000000000001,-0.860000000000001,
-0.855000000000001,-0.850000000000001,-0.845000000000001,-0.840000000000001,
-0.835000000000001,-0.830000000000001,-0.825000000000001,-0.820000000000001,
-0.815000000000001,-0.810000000000001,-0.805000000000001,-0.800000000000001,
-0.795000000000001,-0.790000000000001,-0.785000000000001,-0.780000000000001,
-0.775000000000001,-0.770000000000001,-0.765000000000001,-0.760000000000001,
-0.755000000000001,-0.750000000000001,-0.745000000000001,-0.740000000000001,
-0.735000000000001,-0.730000000000001,-0.725000000000001,-0.720000000000001,
-0.715000000000001,-0.710000000000001,-0.705000000000001,-0.700000000000001,
-0.695000000000001,-0.690000000000001,-0.685,-0.68,-0.675,-0.67,-0.665,
-0.66,-0.655,-0.65,-0.645,-0.64,-0.635,-0.63,-0.625,-0.62,-0.615,-0.61,
-0.605,-0.6,-0.595,-0.59,-0.585,-0.58,-0.575,-0.57,-0.565,-0.56,-0.555,
-0.55,-0.545,-0.54,-0.535,-0.53,-0.525,-0.52,-0.515,-0.51,-0.505,-0.5,-0.495,
-0.49,-0.485,-0.48,-0.475,-0.47,-0.465,-0.46,-0.455,-0.45,-0.445,-0.44,
-0.435,-0.43,-0.425,-0.42,-0.415,-0.41,-0.405,-0.4,-0.395,-0.39,-0.385,
-0.38,-0.375,-0.37,-0.365,-0.36,-0.355,-0.35,-0.345,-0.34,-0.335,-0.33,
-0.325,-0.32,-0.315,-0.31,-0.305,-0.3,-0.295,-0.29,-0.285,-0.28,-0.275,
-0.27,-0.265,-0.26,-0.255,-0.25,-0.245,-0.24,-0.235,-0.23,-0.225,-0.22,
-0.215,-0.21,-0.205,-0.2,-0.195,-0.19,-0.185,-0.18,-0.175,-0.17,-0.165,
-0.16,-0.155,-0.15,-0.145,-0.14,-0.135,-0.13,-0.125,-0.12,-0.115,-0.11,
-0.105,-0.1,-0.095,-0.09,-0.085,-0.08,-0.075,-0.07,-0.065,-0.06,-0.055,
-0.05,-0.045,-0.04,-0.035,-0.03,-0.025,-0.02,-0.015,-0.01,-0.005,0.),(0.,
1.2),.UNSPECIFIED.)
GEOMETRIC_REPRESENTATION_ITEM()
RATIONAL_B_SPLINE_SURFACE(((1.,1.),(1.,1.),(1.,1.),(1.,1.),(1.,1.),(1.,
1.),(1.,1.),(1.,1.),(1.,1.),(1.,1.),(1.,1.),(1.,1.),(1.,1.),(1.,1.),(1.,
1.),(1.,1.),(1.,1.),(1.,1.),(1.,1.),(1.,1.),(1.,1.),(1.,1.),(1.,1.),(1.,
1.),(1.,1.),(1.,1.),(1.,1.),(1.,1.),(1.,1.),(1.,1.),(1.,1.),(1.,1.),(1.,
1.),(1.,1.),(1.,1.),(1.,1.),(1.,1.),(1.,1.),(1.,1.),(1.,1.),(1.,1.),(1.,
1.),(1.,1.),(1.,1.),(1.,1.),(1.,1.),(1.,1.),(1.,1.),(1.,1.),(1.,1.),(1.,
1.),(1.,1.),(1.,1.),(1.,1.),(1.,1.),(1.,1.),(1.,1.),(1.,1.),(1.,1.),(1.,
1.),(1.,1.),(1.,1.),(1.,1.),(1.,1.),(1.,1.),(1.,1.),(1.,1.),(1.,1.),(1.,
1.),(1.,1.),(1.,1.),(1.,1.),(1.,1.),(1.,1.),(1.,1.),(1.,1.),(1.,1.),(1.,
1.),(1.,1.),(1.,1.),(1.,1.),(1.,1.),(1.,1.),(1.,1.),(1.,1.),(1.,1.),(1.,
1.),(1.,1.),(1.,1.),(1.,1.),(1.,1.),(1.,1.),(1.,1.),(1.,1.),(1.,1.),(1.,
1.),(1.,1.),(1.,1.),(1.,1.),(1.,1.),(1.,1.),(1.,1.),(1.,1.),(1.,1.),(1.,
1.),(1.,1.),(1.,1.),(1.,1.),(1.,1.),(1.,1.),(1.,1.),(1.,1.),(1.,1.),(1.,
1.),(1.,1.),(1.,1.),(1.,1.),(1.,1.),(1.,1.),(1.,1.),(1.,1.),(1.,1.),(1.,
1.),(1.,1.),(1.,1.),(1.,1.),(1.,1.),(1.,1.),(1.,1.),(1.,1.),(1.,1.),(1.,
1.),(1.,1.),(1.,1.),(1.,1.),(1.,1.),(1.,1.),(1.,1.),(1.,1.),(1.,1.),(1.,
1.),(1.,1.),(1.,1.),(1.,1.),(1.,1.),(1.,1.),(1.,1.),(1.,1.),(1.,1.),(1.,
1.),(1.,1.),(1.,1.),(1.,1.),(1.,1.),(1.,1.),(1.,1.),(1.,1.),(1.,1.),(1.,
1.),(1.,1.),(1.,1.),(1.,1.),(1.,1.),(1.,1.),(1.,1.),(1.,1.),(1.,1.),(1.,
1.),(1.,1.),(1.,1.),(1.,1.),(1.,1.),(1.,1.),(1.,1.),(1.,1.),(1.,1.),(1.,
1.),(1.,1.),(1.,1.),(1.,1.),(1.,1.),(1.,1.),(1.,1.),(1.,1.),(1.,1.),(1.,
1.),(1.,1.),(1.,1.),(1.,1.),(1.,1.),(1.,1.),(1.,1.),(1.,1.),(1.,1.),(1.,
1.),(1.,1.),(1.,1.),(1.,1.),(1.,1.),(1.,1.),(1.,1.),(1.,1.),(1.,1.),(1.,
1.),(1.,1.)))
REPRESENTATION_ITEM('')
SURFACE()
);
#1020=(
BOUNDED_SURFACE()
B_SPLINE_SURFACE(5,1,((#169058,#169059),(#169060,#169061),(#169062,#169063),
(#169064,#169065),(#169066,#169067),(#169068,#169069),(#169070,#169071),
(#169072,#169073),(#169074,#169075),(#169076,#169077),(#169078,#169079),
(#169080,#169081),(#169082,#169083),(#169084,#169085),(#169086,#169087),
(#169088,#169089),(#169090,#169091),(#169092,#169093),(#169094,#169095),
(#169096,#169097),(#169098,#169099),(#169100,#169101),(#169102,#169103),
(#169104,#169105),(#169106,#169107),(#169108,#169109),(#169110,#169111),
(#169112,#169113),(#169114,#169115),(#169116,#169117),(#169118,#169119),
(#169120,#169121),(#169122,#169123),(#169124,#169125),(#169126,#169127),
(#169128,#169129),(#169130,#169131),(#169132,#169133),(#169134,#169135),
(#169136,#169137),(#169138,#169139),(#169140,#169141),(#169142,#169143),
(#169144,#169145),(#169146,#169147),(#169148,#169149),(#169150,#169151),
(#169152,#169153),(#169154,#169155),(#169156,#169157),(#169158,#169159),
(#169160,#169161),(#169162,#169163),(#169164,#169165),(#169166,#169167),
(#169168,#169169),(#169170,#169171),(#169172,#169173),(#169174,#169175),
(#169176,#169177),(#169178,#169179),(#169180,#169181),(#169182,#169183),
(#169184,#169185),(#169186,#169187),(#169188,#169189),(#169190,#169191),
(#169192,#169193),(#169194,#169195),(#169196,#169197),(#169198,#169199),
(#169200,#169201),(#169202,#169203),(#169204,#169205),(#169206,#169207),
(#169208,#169209),(#169210,#169211),(#169212,#169213),(#169214,#169215),
(#169216,#169217),(#169218,#169219),(#169220,#169221),(#169222,#169223),
(#169224,#169225),(#169226,#169227),(#169228,#169229),(#169230,#169231),
(#169232,#169233),(#169234,#169235),(#169236,#169237),(#169238,#169239),
(#169240,#169241),(#169242,#169243),(#169244,#169245),(#169246,#169247),
(#169248,#169249),(#169250,#169251),(#169252,#169253),(#169254,#169255),
(#169256,#169257),(#169258,#169259),(#169260,#169261),(#169262,#169263),
(#169264,#169265),(#169266,#169267),(#169268,#169269),(#169270,#169271),
(#169272,#169273),(#169274,#169275),(#169276,#169277),(#169278,#169279),
(#169280,#169281),(#169282,#169283),(#169284,#169285),(#169286,#169287),
(#169288,#169289),(#169290,#169291),(#169292,#169293),(#169294,#169295),
(#169296,#169297),(#169298,#169299),(#169300,#169301),(#169302,#169303),
(#169304,#169305),(#169306,#169307),(#169308,#169309),(#169310,#169311),
(#169312,#169313),(#169314,#169315),(#169316,#169317),(#169318,#169319),
(#169320,#169321),(#169322,#169323),(#169324,#169325),(#169326,#169327),
(#169328,#169329),(#169330,#169331),(#169332,#169333),(#169334,#169335),
(#169336,#169337),(#169338,#169339),(#169340,#169341),(#169342,#169343),
(#169344,#169345),(#169346,#169347),(#169348,#169349),(#169350,#169351),
(#169352,#169353),(#169354,#169355),(#169356,#169357),(#169358,#169359),
(#169360,#169361),(#169362,#169363),(#169364,#169365),(#169366,#169367),
(#169368,#169369),(#169370,#169371),(#169372,#169373),(#169374,#169375),
(#169376,#169377),(#169378,#169379),(#169380,#169381),(#169382,#169383),
(#169384,#169385),(#169386,#169387),(#169388,#169389),(#169390,#169391),
(#169392,#169393),(#169394,#169395),(#169396,#169397),(#169398,#169399),
(#169400,#169401),(#169402,#169403),(#169404,#169405),(#169406,#169407),
(#169408,#169409),(#169410,#169411),(#169412,#169413),(#169414,#169415),
(#169416,#169417),(#169418,#169419),(#169420,#169421),(#169422,#169423),
(#169424,#169425),(#169426,#169427),(#169428,#169429),(#169430,#169431),
(#169432,#169433),(#169434,#169435),(#169436,#169437),(#169438,#169439),
(#169440,#169441),(#169442,#169443),(#169444,#169445),(#169446,#169447),
(#169448,#169449),(#169450,#169451),(#169452,#169453),(#169454,#169455),
(#169456,#169457),(#169458,#169459),(#169460,#169461),(#169462,#169463),
(#169464,#169465),(#169466,#169467)),.UNSPECIFIED.,.F.,.F.,.F.)
B_SPLINE_SURFACE_WITH_KNOTS((6,1,1,1,1,1,1,1,1,1,1,1,1,1,1,1,1,1,1,1,1,
1,1,1,1,1,1,1,1,1,1,1,1,1,1,1,1,1,1,1,1,1,1,1,1,1,1,1,1,1,1,1,1,1,1,1,1,
1,1,1,1,1,1,1,1,1,1,1,1,1,1,1,1,1,1,1,1,1,1,1,1,1,1,1,1,1,1,1,1,1,1,1,1,
1,1,1,1,1,1,1,1,1,1,1,1,1,1,1,1,1,1,1,1,1,1,1,1,1,1,1,1,1,1,1,1,1,1,1,1,
1,1,1,1,1,1,1,1,1,1,1,1,1,1,1,1,1,1,1,1,1,1,1,1,1,1,1,1,1,1,1,1,1,1,1,1,
1,1,1,1,1,1,1,1,1,1,1,1,1,1,1,1,1,1,1,1,1,1,1,1,1,1,1,1,1,1,1,1,1,1,1,6),
(2,2),(-1.,-0.995000000000001,-0.990000000000001,-0.985000000000001,-0.980000000000001,
-0.975000000000001,-0.970000000000001,-0.965000000000001,-0.960000000000001,
-0.955000000000001,-0.950000000000001,-0.945000000000001,-0.940000000000001,
-0.935000000000001,-0.930000000000001,-0.925000000000001,-0.920000000000001,
-0.915000000000001,-0.910000000000001,-0.905000000000001,-0.900000000000001,
-0.895000000000001,-0.890000000000001,-0.885000000000001,-0.880000000000001,
-0.875000000000001,-0.870000000000001,-0.865000000000001,-0.860000000000001,
-0.855000000000001,-0.850000000000001,-0.845000000000001,-0.840000000000001,
-0.835000000000001,-0.830000000000001,-0.825000000000001,-0.820000000000001,
-0.815000000000001,-0.810000000000001,-0.805000000000001,-0.800000000000001,
-0.795000000000001,-0.790000000000001,-0.785000000000001,-0.780000000000001,
-0.775000000000001,-0.770000000000001,-0.765000000000001,-0.760000000000001,
-0.755000000000001,-0.750000000000001,-0.745000000000001,-0.740000000000001,
-0.735000000000001,-0.730000000000001,-0.725000000000001,-0.720000000000001,
-0.715000000000001,-0.710000000000001,-0.705000000000001,-0.700000000000001,
-0.695000000000001,-0.690000000000001,-0.685,-0.68,-0.675,-0.67,-0.665,
-0.66,-0.655,-0.65,-0.645,-0.64,-0.635,-0.63,-0.625,-0.62,-0.615,-0.61,
-0.605,-0.6,-0.595,-0.59,-0.585,-0.58,-0.575,-0.57,-0.565,-0.56,-0.555,
-0.55,-0.545,-0.54,-0.535,-0.53,-0.525,-0.52,-0.515,-0.51,-0.505,-0.5,-0.495,
-0.49,-0.485,-0.48,-0.475,-0.47,-0.465,-0.46,-0.455,-0.45,-0.445,-0.44,
-0.435,-0.43,-0.425,-0.42,-0.415,-0.41,-0.405,-0.4,-0.395,-0.39,-0.385,
-0.38,-0.375,-0.37,-0.365,-0.36,-0.355,-0.35,-0.345,-0.34,-0.335,-0.33,
-0.325,-0.32,-0.315,-0.31,-0.305,-0.3,-0.295,-0.29,-0.285,-0.28,-0.275,
-0.27,-0.265,-0.26,-0.255,-0.25,-0.245,-0.24,-0.235,-0.23,-0.225,-0.22,
-0.215,-0.21,-0.205,-0.2,-0.195,-0.19,-0.185,-0.18,-0.175,-0.17,-0.165,
-0.16,-0.155,-0.15,-0.145,-0.14,-0.135,-0.13,-0.125,-0.12,-0.115,-0.11,
-0.105,-0.1,-0.095,-0.09,-0.085,-0.08,-0.075,-0.07,-0.065,-0.06,-0.055,
-0.05,-0.045,-0.04,-0.035,-0.03,-0.025,-0.02,-0.015,-0.01,-0.005,0.),(0.,
1.2),.UNSPECIFIED.)
GEOMETRIC_REPRESENTATION_ITEM()
RATIONAL_B_SPLINE_SURFACE(((1.,1.),(1.,1.),(1.,1.),(1.,1.),(1.,1.),(1.,
1.),(1.,1.),(1.,1.),(1.,1.),(1.,1.),(1.,1.),(1.,1.),(1.,1.),(1.,1.),(1.,
1.),(1.,1.),(1.,1.),(1.,1.),(1.,1.),(1.,1.),(1.,1.),(1.,1.),(1.,1.),(1.,
1.),(1.,1.),(1.,1.),(1.,1.),(1.,1.),(1.,1.),(1.,1.),(1.,1.),(1.,1.),(1.,
1.),(1.,1.),(1.,1.),(1.,1.),(1.,1.),(1.,1.),(1.,1.),(1.,1.),(1.,1.),(1.,
1.),(1.,1.),(1.,1.),(1.,1.),(1.,1.),(1.,1.),(1.,1.),(1.,1.),(1.,1.),(1.,
1.),(1.,1.),(1.,1.),(1.,1.),(1.,1.),(1.,1.),(1.,1.),(1.,1.),(1.,1.),(1.,
1.),(1.,1.),(1.,1.),(1.,1.),(1.,1.),(1.,1.),(1.,1.),(1.,1.),(1.,1.),(1.,
1.),(1.,1.),(1.,1.),(1.,1.),(1.,1.),(1.,1.),(1.,1.),(1.,1.),(1.,1.),(1.,
1.),(1.,1.),(1.,1.),(1.,1.),(1.,1.),(1.,1.),(1.,1.),(1.,1.),(1.,1.),(1.,
1.),(1.,1.),(1.,1.),(1.,1.),(1.,1.),(1.,1.),(1.,1.),(1.,1.),(1.,1.),(1.,
1.),(1.,1.),(1.,1.),(1.,1.),(1.,1.),(1.,1.),(1.,1.),(1.,1.),(1.,1.),(1.,
1.),(1.,1.),(1.,1.),(1.,1.),(1.,1.),(1.,1.),(1.,1.),(1.,1.),(1.,1.),(1.,
1.),(1.,1.),(1.,1.),(1.,1.),(1.,1.),(1.,1.),(1.,1.),(1.,1.),(1.,1.),(1.,
1.),(1.,1.),(1.,1.),(1.,1.),(1.,1.),(1.,1.),(1.,1.),(1.,1.),(1.,1.),(1.,
1.),(1.,1.),(1.,1.),(1.,1.),(1.,1.),(1.,1.),(1.,1.),(1.,1.),(1.,1.),(1.,
1.),(1.,1.),(1.,1.),(1.,1.),(1.,1.),(1.,1.),(1.,1.),(1.,1.),(1.,1.),(1.,
1.),(1.,1.),(1.,1.),(1.,1.),(1.,1.),(1.,1.),(1.,1.),(1.,1.),(1.,1.),(1.,
1.),(1.,1.),(1.,1.),(1.,1.),(1.,1.),(1.,1.),(1.,1.),(1.,1.),(1.,1.),(1.,
1.),(1.,1.),(1.,1.),(1.,1.),(1.,1.),(1.,1.),(1.,1.),(1.,1.),(1.,1.),(1.,
1.),(1.,1.),(1.,1.),(1.,1.),(1.,1.),(1.,1.),(1.,1.),(1.,1.),(1.,1.),(1.,
1.),(1.,1.),(1.,1.),(1.,1.),(1.,1.),(1.,1.),(1.,1.),(1.,1.),(1.,1.),(1.,
1.),(1.,1.),(1.,1.),(1.,1.),(1.,1.),(1.,1.),(1.,1.),(1.,1.),(1.,1.),(1.,
1.),(1.,1.)))
REPRESENTATION_ITEM('')
SURFACE()
);
#1021=(
BOUNDED_SURFACE()
B_SPLINE_SURFACE(5,1,((#169859,#169860),(#169861,#169862),(#169863,#169864),
(#169865,#169866),(#169867,#169868),(#169869,#169870),(#169871,#169872),
(#169873,#169874),(#169875,#169876),(#169877,#169878),(#169879,#169880),
(#169881,#169882),(#169883,#169884),(#169885,#169886),(#169887,#169888),
(#169889,#169890),(#169891,#169892),(#169893,#169894),(#169895,#169896),
(#169897,#169898),(#169899,#169900),(#169901,#169902),(#169903,#169904),
(#169905,#169906),(#169907,#169908),(#169909,#169910),(#169911,#169912),
(#169913,#169914),(#169915,#169916),(#169917,#169918),(#169919,#169920),
(#169921,#169922),(#169923,#169924),(#169925,#169926),(#169927,#169928),
(#169929,#169930),(#169931,#169932),(#169933,#169934),(#169935,#169936),
(#169937,#169938),(#169939,#169940),(#169941,#169942),(#169943,#169944),
(#169945,#169946),(#169947,#169948),(#169949,#169950),(#169951,#169952),
(#169953,#169954),(#169955,#169956),(#169957,#169958),(#169959,#169960),
(#169961,#169962),(#169963,#169964),(#169965,#169966),(#169967,#169968),
(#169969,#169970),(#169971,#169972),(#169973,#169974),(#169975,#169976),
(#169977,#169978),(#169979,#169980),(#169981,#169982),(#169983,#169984),
(#169985,#169986),(#169987,#169988),(#169989,#169990),(#169991,#169992),
(#169993,#169994),(#169995,#169996),(#169997,#169998),(#169999,#170000),
(#170001,#170002),(#170003,#170004),(#170005,#170006),(#170007,#170008),
(#170009,#170010),(#170011,#170012),(#170013,#170014),(#170015,#170016),
(#170017,#170018),(#170019,#170020),(#170021,#170022),(#170023,#170024),
(#170025,#170026),(#170027,#170028),(#170029,#170030),(#170031,#170032),
(#170033,#170034),(#170035,#170036),(#170037,#170038),(#170039,#170040),
(#170041,#170042),(#170043,#170044),(#170045,#170046),(#170047,#170048),
(#170049,#170050),(#170051,#170052),(#170053,#170054),(#170055,#170056),
(#170057,#170058),(#170059,#170060),(#170061,#170062),(#170063,#170064),
(#170065,#170066),(#170067,#170068),(#170069,#170070),(#170071,#170072),
(#170073,#170074),(#170075,#170076),(#170077,#170078),(#170079,#170080),
(#170081,#170082),(#170083,#170084),(#170085,#170086),(#170087,#170088),
(#170089,#170090),(#170091,#170092),(#170093,#170094),(#170095,#170096),
(#170097,#170098),(#170099,#170100),(#170101,#170102),(#170103,#170104),
(#170105,#170106),(#170107,#170108),(#170109,#170110),(#170111,#170112),
(#170113,#170114),(#170115,#170116),(#170117,#170118),(#170119,#170120),
(#170121,#170122),(#170123,#170124),(#170125,#170126),(#170127,#170128),
(#170129,#170130),(#170131,#170132),(#170133,#170134),(#170135,#170136),
(#170137,#170138),(#170139,#170140),(#170141,#170142),(#170143,#170144),
(#170145,#170146),(#170147,#170148),(#170149,#170150),(#170151,#170152),
(#170153,#170154),(#170155,#170156),(#170157,#170158),(#170159,#170160),
(#170161,#170162),(#170163,#170164),(#170165,#170166),(#170167,#170168),
(#170169,#170170),(#170171,#170172),(#170173,#170174),(#170175,#170176),
(#170177,#170178),(#170179,#170180),(#170181,#170182),(#170183,#170184),
(#170185,#170186),(#170187,#170188),(#170189,#170190),(#170191,#170192),
(#170193,#170194),(#170195,#170196),(#170197,#170198),(#170199,#170200),
(#170201,#170202),(#170203,#170204),(#170205,#170206),(#170207,#170208),
(#170209,#170210),(#170211,#170212),(#170213,#170214),(#170215,#170216),
(#170217,#170218),(#170219,#170220),(#170221,#170222),(#170223,#170224),
(#170225,#170226),(#170227,#170228),(#170229,#170230),(#170231,#170232),
(#170233,#170234),(#170235,#170236),(#170237,#170238),(#170239,#170240),
(#170241,#170242),(#170243,#170244),(#170245,#170246),(#170247,#170248),
(#170249,#170250),(#170251,#170252),(#170253,#170254),(#170255,#170256),
(#170257,#170258),(#170259,#170260),(#170261,#170262),(#170263,#170264),
(#170265,#170266),(#170267,#170268)),.UNSPECIFIED.,.F.,.F.,.F.)
B_SPLINE_SURFACE_WITH_KNOTS((6,1,1,1,1,1,1,1,1,1,1,1,1,1,1,1,1,1,1,1,1,
1,1,1,1,1,1,1,1,1,1,1,1,1,1,1,1,1,1,1,1,1,1,1,1,1,1,1,1,1,1,1,1,1,1,1,1,
1,1,1,1,1,1,1,1,1,1,1,1,1,1,1,1,1,1,1,1,1,1,1,1,1,1,1,1,1,1,1,1,1,1,1,1,
1,1,1,1,1,1,1,1,1,1,1,1,1,1,1,1,1,1,1,1,1,1,1,1,1,1,1,1,1,1,1,1,1,1,1,1,
1,1,1,1,1,1,1,1,1,1,1,1,1,1,1,1,1,1,1,1,1,1,1,1,1,1,1,1,1,1,1,1,1,1,1,1,
1,1,1,1,1,1,1,1,1,1,1,1,1,1,1,1,1,1,1,1,1,1,1,1,1,1,1,1,1,1,1,1,1,1,1,6),
(2,2),(-1.,-0.995000000000001,-0.990000000000001,-0.985000000000001,-0.980000000000001,
-0.975000000000001,-0.970000000000001,-0.965000000000001,-0.960000000000001,
-0.955000000000001,-0.950000000000001,-0.945000000000001,-0.940000000000001,
-0.935000000000001,-0.930000000000001,-0.925000000000001,-0.920000000000001,
-0.915000000000001,-0.910000000000001,-0.905000000000001,-0.900000000000001,
-0.895000000000001,-0.890000000000001,-0.885000000000001,-0.880000000000001,
-0.875000000000001,-0.870000000000001,-0.865000000000001,-0.860000000000001,
-0.855000000000001,-0.850000000000001,-0.845000000000001,-0.840000000000001,
-0.835000000000001,-0.830000000000001,-0.825000000000001,-0.820000000000001,
-0.815000000000001,-0.810000000000001,-0.805000000000001,-0.800000000000001,
-0.795000000000001,-0.790000000000001,-0.785000000000001,-0.780000000000001,
-0.775000000000001,-0.770000000000001,-0.765000000000001,-0.760000000000001,
-0.755000000000001,-0.750000000000001,-0.745000000000001,-0.740000000000001,
-0.735000000000001,-0.730000000000001,-0.725000000000001,-0.720000000000001,
-0.715000000000001,-0.710000000000001,-0.705000000000001,-0.700000000000001,
-0.695000000000001,-0.690000000000001,-0.685,-0.68,-0.675,-0.67,-0.665,
-0.66,-0.655,-0.65,-0.645,-0.64,-0.635,-0.63,-0.625,-0.62,-0.615,-0.61,
-0.605,-0.6,-0.595,-0.59,-0.585,-0.58,-0.575,-0.57,-0.565,-0.56,-0.555,
-0.55,-0.545,-0.54,-0.535,-0.53,-0.525,-0.52,-0.515,-0.51,-0.505,-0.5,-0.495,
-0.49,-0.485,-0.48,-0.475,-0.47,-0.465,-0.46,-0.455,-0.45,-0.445,-0.44,
-0.435,-0.43,-0.425,-0.42,-0.415,-0.41,-0.405,-0.4,-0.395,-0.39,-0.385,
-0.38,-0.375,-0.37,-0.365,-0.36,-0.355,-0.35,-0.345,-0.34,-0.335,-0.33,
-0.325,-0.32,-0.315,-0.31,-0.305,-0.3,-0.295,-0.29,-0.285,-0.28,-0.275,
-0.27,-0.265,-0.26,-0.255,-0.25,-0.245,-0.24,-0.235,-0.23,-0.225,-0.22,
-0.215,-0.21,-0.205,-0.2,-0.195,-0.19,-0.185,-0.18,-0.175,-0.17,-0.165,
-0.16,-0.155,-0.15,-0.145,-0.14,-0.135,-0.13,-0.125,-0.12,-0.115,-0.11,
-0.105,-0.1,-0.095,-0.09,-0.085,-0.08,-0.075,-0.07,-0.065,-0.06,-0.055,
-0.05,-0.045,-0.04,-0.035,-0.03,-0.025,-0.02,-0.015,-0.01,-0.005,0.),(0.,
1.2),.UNSPECIFIED.)
GEOMETRIC_REPRESENTATION_ITEM()
RATIONAL_B_SPLINE_SURFACE(((1.,1.),(1.,1.),(1.,1.),(1.,1.),(1.,1.),(1.,
1.),(1.,1.),(1.,1.),(1.,1.),(1.,1.),(1.,1.),(1.,1.),(1.,1.),(1.,1.),(1.,
1.),(1.,1.),(1.,1.),(1.,1.),(1.,1.),(1.,1.),(1.,1.),(1.,1.),(1.,1.),(1.,
1.),(1.,1.),(1.,1.),(1.,1.),(1.,1.),(1.,1.),(1.,1.),(1.,1.),(1.,1.),(1.,
1.),(1.,1.),(1.,1.),(1.,1.),(1.,1.),(1.,1.),(1.,1.),(1.,1.),(1.,1.),(1.,
1.),(1.,1.),(1.,1.),(1.,1.),(1.,1.),(1.,1.),(1.,1.),(1.,1.),(1.,1.),(1.,
1.),(1.,1.),(1.,1.),(1.,1.),(1.,1.),(1.,1.),(1.,1.),(1.,1.),(1.,1.),(1.,
1.),(1.,1.),(1.,1.),(1.,1.),(1.,1.),(1.,1.),(1.,1.),(1.,1.),(1.,1.),(1.,
1.),(1.,1.),(1.,1.),(1.,1.),(1.,1.),(1.,1.),(1.,1.),(1.,1.),(1.,1.),(1.,
1.),(1.,1.),(1.,1.),(1.,1.),(1.,1.),(1.,1.),(1.,1.),(1.,1.),(1.,1.),(1.,
1.),(1.,1.),(1.,1.),(1.,1.),(1.,1.),(1.,1.),(1.,1.),(1.,1.),(1.,1.),(1.,
1.),(1.,1.),(1.,1.),(1.,1.),(1.,1.),(1.,1.),(1.,1.),(1.,1.),(1.,1.),(1.,
1.),(1.,1.),(1.,1.),(1.,1.),(1.,1.),(1.,1.),(1.,1.),(1.,1.),(1.,1.),(1.,
1.),(1.,1.),(1.,1.),(1.,1.),(1.,1.),(1.,1.),(1.,1.),(1.,1.),(1.,1.),(1.,
1.),(1.,1.),(1.,1.),(1.,1.),(1.,1.),(1.,1.),(1.,1.),(1.,1.),(1.,1.),(1.,
1.),(1.,1.),(1.,1.),(1.,1.),(1.,1.),(1.,1.),(1.,1.),(1.,1.),(1.,1.),(1.,
1.),(1.,1.),(1.,1.),(1.,1.),(1.,1.),(1.,1.),(1.,1.),(1.,1.),(1.,1.),(1.,
1.),(1.,1.),(1.,1.),(1.,1.),(1.,1.),(1.,1.),(1.,1.),(1.,1.),(1.,1.),(1.,
1.),(1.,1.),(1.,1.),(1.,1.),(1.,1.),(1.,1.),(1.,1.),(1.,1.),(1.,1.),(1.,
1.),(1.,1.),(1.,1.),(1.,1.),(1.,1.),(1.,1.),(1.,1.),(1.,1.),(1.,1.),(1.,
1.),(1.,1.),(1.,1.),(1.,1.),(1.,1.),(1.,1.),(1.,1.),(1.,1.),(1.,1.),(1.,
1.),(1.,1.),(1.,1.),(1.,1.),(1.,1.),(1.,1.),(1.,1.),(1.,1.),(1.,1.),(1.,
1.),(1.,1.),(1.,1.),(1.,1.),(1.,1.),(1.,1.),(1.,1.),(1.,1.),(1.,1.),(1.,
1.),(1.,1.)))
REPRESENTATION_ITEM('')
SURFACE()
);
#1022=(
BOUNDED_SURFACE()
B_SPLINE_SURFACE(5,1,((#170660,#170661),(#170662,#170663),(#170664,#170665),
(#170666,#170667),(#170668,#170669),(#170670,#170671),(#170672,#170673),
(#170674,#170675),(#170676,#170677),(#170678,#170679),(#170680,#170681),
(#170682,#170683),(#170684,#170685),(#170686,#170687),(#170688,#170689),
(#170690,#170691),(#170692,#170693),(#170694,#170695),(#170696,#170697),
(#170698,#170699),(#170700,#170701),(#170702,#170703),(#170704,#170705),
(#170706,#170707),(#170708,#170709),(#170710,#170711),(#170712,#170713),
(#170714,#170715),(#170716,#170717),(#170718,#170719),(#170720,#170721),
(#170722,#170723),(#170724,#170725),(#170726,#170727),(#170728,#170729),
(#170730,#170731),(#170732,#170733),(#170734,#170735),(#170736,#170737),
(#170738,#170739),(#170740,#170741),(#170742,#170743),(#170744,#170745),
(#170746,#170747),(#170748,#170749),(#170750,#170751),(#170752,#170753),
(#170754,#170755),(#170756,#170757),(#170758,#170759),(#170760,#170761),
(#170762,#170763),(#170764,#170765),(#170766,#170767),(#170768,#170769),
(#170770,#170771),(#170772,#170773),(#170774,#170775),(#170776,#170777),
(#170778,#170779),(#170780,#170781),(#170782,#170783),(#170784,#170785),
(#170786,#170787),(#170788,#170789),(#170790,#170791),(#170792,#170793),
(#170794,#170795),(#170796,#170797),(#170798,#170799),(#170800,#170801),
(#170802,#170803),(#170804,#170805),(#170806,#170807),(#170808,#170809),
(#170810,#170811),(#170812,#170813),(#170814,#170815),(#170816,#170817),
(#170818,#170819),(#170820,#170821),(#170822,#170823),(#170824,#170825),
(#170826,#170827),(#170828,#170829),(#170830,#170831),(#170832,#170833),
(#170834,#170835),(#170836,#170837),(#170838,#170839),(#170840,#170841),
(#170842,#170843),(#170844,#170845),(#170846,#170847),(#170848,#170849),
(#170850,#170851),(#170852,#170853),(#170854,#170855),(#170856,#170857),
(#170858,#170859),(#170860,#170861),(#170862,#170863),(#170864,#170865),
(#170866,#170867),(#170868,#170869),(#170870,#170871),(#170872,#170873),
(#170874,#170875),(#170876,#170877),(#170878,#170879),(#170880,#170881),
(#170882,#170883),(#170884,#170885),(#170886,#170887),(#170888,#170889),
(#170890,#170891),(#170892,#170893),(#170894,#170895),(#170896,#170897),
(#170898,#170899),(#170900,#170901),(#170902,#170903),(#170904,#170905),
(#170906,#170907),(#170908,#170909),(#170910,#170911),(#170912,#170913),
(#170914,#170915),(#170916,#170917),(#170918,#170919),(#170920,#170921),
(#170922,#170923),(#170924,#170925),(#170926,#170927),(#170928,#170929),
(#170930,#170931),(#170932,#170933),(#170934,#170935),(#170936,#170937),
(#170938,#170939),(#170940,#170941),(#170942,#170943),(#170944,#170945),
(#170946,#170947),(#170948,#170949),(#170950,#170951),(#170952,#170953),
(#170954,#170955),(#170956,#170957),(#170958,#170959),(#170960,#170961),
(#170962,#170963),(#170964,#170965),(#170966,#170967),(#170968,#170969),
(#170970,#170971),(#170972,#170973),(#170974,#170975),(#170976,#170977),
(#170978,#170979),(#170980,#170981),(#170982,#170983),(#170984,#170985),
(#170986,#170987),(#170988,#170989),(#170990,#170991),(#170992,#170993),
(#170994,#170995),(#170996,#170997),(#170998,#170999),(#171000,#171001),
(#171002,#171003),(#171004,#171005),(#171006,#171007),(#171008,#171009),
(#171010,#171011),(#171012,#171013),(#171014,#171015),(#171016,#171017),
(#171018,#171019),(#171020,#171021),(#171022,#171023),(#171024,#171025),
(#171026,#171027),(#171028,#171029),(#171030,#171031),(#171032,#171033),
(#171034,#171035),(#171036,#171037),(#171038,#171039),(#171040,#171041),
(#171042,#171043),(#171044,#171045),(#171046,#171047),(#171048,#171049),
(#171050,#171051),(#171052,#171053),(#171054,#171055),(#171056,#171057),
(#171058,#171059),(#171060,#171061),(#171062,#171063),(#171064,#171065),
(#171066,#171067),(#171068,#171069)),.UNSPECIFIED.,.F.,.F.,.F.)
B_SPLINE_SURFACE_WITH_KNOTS((6,1,1,1,1,1,1,1,1,1,1,1,1,1,1,1,1,1,1,1,1,
1,1,1,1,1,1,1,1,1,1,1,1,1,1,1,1,1,1,1,1,1,1,1,1,1,1,1,1,1,1,1,1,1,1,1,1,
1,1,1,1,1,1,1,1,1,1,1,1,1,1,1,1,1,1,1,1,1,1,1,1,1,1,1,1,1,1,1,1,1,1,1,1,
1,1,1,1,1,1,1,1,1,1,1,1,1,1,1,1,1,1,1,1,1,1,1,1,1,1,1,1,1,1,1,1,1,1,1,1,
1,1,1,1,1,1,1,1,1,1,1,1,1,1,1,1,1,1,1,1,1,1,1,1,1,1,1,1,1,1,1,1,1,1,1,1,
1,1,1,1,1,1,1,1,1,1,1,1,1,1,1,1,1,1,1,1,1,1,1,1,1,1,1,1,1,1,1,1,1,1,1,6),
(2,2),(-1.,-0.995000000000001,-0.990000000000001,-0.985000000000001,-0.980000000000001,
-0.975000000000001,-0.970000000000001,-0.965000000000001,-0.960000000000001,
-0.955000000000001,-0.950000000000001,-0.945000000000001,-0.940000000000001,
-0.935000000000001,-0.930000000000001,-0.925000000000001,-0.920000000000001,
-0.915000000000001,-0.910000000000001,-0.905000000000001,-0.900000000000001,
-0.895000000000001,-0.890000000000001,-0.885000000000001,-0.880000000000001,
-0.875000000000001,-0.870000000000001,-0.865000000000001,-0.860000000000001,
-0.855000000000001,-0.850000000000001,-0.845000000000001,-0.840000000000001,
-0.835000000000001,-0.830000000000001,-0.825000000000001,-0.820000000000001,
-0.815000000000001,-0.810000000000001,-0.805000000000001,-0.800000000000001,
-0.795000000000001,-0.790000000000001,-0.785000000000001,-0.780000000000001,
-0.775000000000001,-0.770000000000001,-0.765000000000001,-0.760000000000001,
-0.755000000000001,-0.750000000000001,-0.745000000000001,-0.740000000000001,
-0.735000000000001,-0.730000000000001,-0.725000000000001,-0.720000000000001,
-0.715000000000001,-0.710000000000001,-0.705000000000001,-0.700000000000001,
-0.695000000000001,-0.690000000000001,-0.685,-0.68,-0.675,-0.67,-0.665,
-0.66,-0.655,-0.65,-0.645,-0.64,-0.635,-0.63,-0.625,-0.62,-0.615,-0.61,
-0.605,-0.6,-0.595,-0.59,-0.585,-0.58,-0.575,-0.57,-0.565,-0.56,-0.555,
-0.55,-0.545,-0.54,-0.535,-0.53,-0.525,-0.52,-0.515,-0.51,-0.505,-0.5,-0.495,
-0.49,-0.485,-0.48,-0.475,-0.47,-0.465,-0.46,-0.455,-0.45,-0.445,-0.44,
-0.435,-0.43,-0.425,-0.42,-0.415,-0.41,-0.405,-0.4,-0.395,-0.39,-0.385,
-0.38,-0.375,-0.37,-0.365,-0.36,-0.355,-0.35,-0.345,-0.34,-0.335,-0.33,
-0.325,-0.32,-0.315,-0.31,-0.305,-0.3,-0.295,-0.29,-0.285,-0.28,-0.275,
-0.27,-0.265,-0.26,-0.255,-0.25,-0.245,-0.24,-0.235,-0.23,-0.225,-0.22,
-0.215,-0.21,-0.205,-0.2,-0.195,-0.19,-0.185,-0.18,-0.175,-0.17,-0.165,
-0.16,-0.155,-0.15,-0.145,-0.14,-0.135,-0.13,-0.125,-0.12,-0.115,-0.11,
-0.105,-0.1,-0.095,-0.09,-0.085,-0.08,-0.075,-0.07,-0.065,-0.06,-0.055,
-0.05,-0.045,-0.04,-0.035,-0.03,-0.025,-0.02,-0.015,-0.01,-0.005,0.),(0.,
1.2),.UNSPECIFIED.)
GEOMETRIC_REPRESENTATION_ITEM()
RATIONAL_B_SPLINE_SURFACE(((1.,1.),(1.,1.),(1.,1.),(1.,1.),(1.,1.),(1.,
1.),(1.,1.),(1.,1.),(1.,1.),(1.,1.),(1.,1.),(1.,1.),(1.,1.),(1.,1.),(1.,
1.),(1.,1.),(1.,1.),(1.,1.),(1.,1.),(1.,1.),(1.,1.),(1.,1.),(1.,1.),(1.,
1.),(1.,1.),(1.,1.),(1.,1.),(1.,1.),(1.,1.),(1.,1.),(1.,1.),(1.,1.),(1.,
1.),(1.,1.),(1.,1.),(1.,1.),(1.,1.),(1.,1.),(1.,1.),(1.,1.),(1.,1.),(1.,
1.),(1.,1.),(1.,1.),(1.,1.),(1.,1.),(1.,1.),(1.,1.),(1.,1.),(1.,1.),(1.,
1.),(1.,1.),(1.,1.),(1.,1.),(1.,1.),(1.,1.),(1.,1.),(1.,1.),(1.,1.),(1.,
1.),(1.,1.),(1.,1.),(1.,1.),(1.,1.),(1.,1.),(1.,1.),(1.,1.),(1.,1.),(1.,
1.),(1.,1.),(1.,1.),(1.,1.),(1.,1.),(1.,1.),(1.,1.),(1.,1.),(1.,1.),(1.,
1.),(1.,1.),(1.,1.),(1.,1.),(1.,1.),(1.,1.),(1.,1.),(1.,1.),(1.,1.),(1.,
1.),(1.,1.),(1.,1.),(1.,1.),(1.,1.),(1.,1.),(1.,1.),(1.,1.),(1.,1.),(1.,
1.),(1.,1.),(1.,1.),(1.,1.),(1.,1.),(1.,1.),(1.,1.),(1.,1.),(1.,1.),(1.,
1.),(1.,1.),(1.,1.),(1.,1.),(1.,1.),(1.,1.),(1.,1.),(1.,1.),(1.,1.),(1.,
1.),(1.,1.),(1.,1.),(1.,1.),(1.,1.),(1.,1.),(1.,1.),(1.,1.),(1.,1.),(1.,
1.),(1.,1.),(1.,1.),(1.,1.),(1.,1.),(1.,1.),(1.,1.),(1.,1.),(1.,1.),(1.,
1.),(1.,1.),(1.,1.),(1.,1.),(1.,1.),(1.,1.),(1.,1.),(1.,1.),(1.,1.),(1.,
1.),(1.,1.),(1.,1.),(1.,1.),(1.,1.),(1.,1.),(1.,1.),(1.,1.),(1.,1.),(1.,
1.),(1.,1.),(1.,1.),(1.,1.),(1.,1.),(1.,1.),(1.,1.),(1.,1.),(1.,1.),(1.,
1.),(1.,1.),(1.,1.),(1.,1.),(1.,1.),(1.,1.),(1.,1.),(1.,1.),(1.,1.),(1.,
1.),(1.,1.),(1.,1.),(1.,1.),(1.,1.),(1.,1.),(1.,1.),(1.,1.),(1.,1.),(1.,
1.),(1.,1.),(1.,1.),(1.,1.),(1.,1.),(1.,1.),(1.,1.),(1.,1.),(1.,1.),(1.,
1.),(1.,1.),(1.,1.),(1.,1.),(1.,1.),(1.,1.),(1.,1.),(1.,1.),(1.,1.),(1.,
1.),(1.,1.),(1.,1.),(1.,1.),(1.,1.),(1.,1.),(1.,1.),(1.,1.),(1.,1.),(1.,
1.),(1.,1.)))
REPRESENTATION_ITEM('')
SURFACE()
);
#1023=(
BOUNDED_SURFACE()
B_SPLINE_SURFACE(5,1,((#171461,#171462),(#171463,#171464),(#171465,#171466),
(#171467,#171468),(#171469,#171470),(#171471,#171472),(#171473,#171474),
(#171475,#171476),(#171477,#171478),(#171479,#171480),(#171481,#171482),
(#171483,#171484),(#171485,#171486),(#171487,#171488),(#171489,#171490),
(#171491,#171492),(#171493,#171494),(#171495,#171496),(#171497,#171498),
(#171499,#171500),(#171501,#171502),(#171503,#171504),(#171505,#171506),
(#171507,#171508),(#171509,#171510),(#171511,#171512),(#171513,#171514),
(#171515,#171516),(#171517,#171518),(#171519,#171520),(#171521,#171522),
(#171523,#171524),(#171525,#171526),(#171527,#171528),(#171529,#171530),
(#171531,#171532),(#171533,#171534),(#171535,#171536),(#171537,#171538),
(#171539,#171540),(#171541,#171542),(#171543,#171544),(#171545,#171546),
(#171547,#171548),(#171549,#171550),(#171551,#171552),(#171553,#171554),
(#171555,#171556),(#171557,#171558),(#171559,#171560),(#171561,#171562),
(#171563,#171564),(#171565,#171566),(#171567,#171568),(#171569,#171570),
(#171571,#171572),(#171573,#171574),(#171575,#171576),(#171577,#171578),
(#171579,#171580),(#171581,#171582),(#171583,#171584),(#171585,#171586),
(#171587,#171588),(#171589,#171590),(#171591,#171592),(#171593,#171594),
(#171595,#171596),(#171597,#171598),(#171599,#171600),(#171601,#171602),
(#171603,#171604),(#171605,#171606),(#171607,#171608),(#171609,#171610),
(#171611,#171612),(#171613,#171614),(#171615,#171616),(#171617,#171618),
(#171619,#171620),(#171621,#171622),(#171623,#171624),(#171625,#171626),
(#171627,#171628),(#171629,#171630),(#171631,#171632),(#171633,#171634),
(#171635,#171636),(#171637,#171638),(#171639,#171640),(#171641,#171642),
(#171643,#171644),(#171645,#171646),(#171647,#171648),(#171649,#171650),
(#171651,#171652),(#171653,#171654),(#171655,#171656),(#171657,#171658),
(#171659,#171660),(#171661,#171662),(#171663,#171664),(#171665,#171666),
(#171667,#171668),(#171669,#171670),(#171671,#171672),(#171673,#171674),
(#171675,#171676),(#171677,#171678),(#171679,#171680),(#171681,#171682),
(#171683,#171684),(#171685,#171686),(#171687,#171688),(#171689,#171690),
(#171691,#171692),(#171693,#171694),(#171695,#171696),(#171697,#171698),
(#171699,#171700),(#171701,#171702),(#171703,#171704),(#171705,#171706),
(#171707,#171708),(#171709,#171710),(#171711,#171712),(#171713,#171714),
(#171715,#171716),(#171717,#171718),(#171719,#171720),(#171721,#171722),
(#171723,#171724),(#171725,#171726),(#171727,#171728),(#171729,#171730),
(#171731,#171732),(#171733,#171734),(#171735,#171736),(#171737,#171738),
(#171739,#171740),(#171741,#171742),(#171743,#171744),(#171745,#171746),
(#171747,#171748),(#171749,#171750),(#171751,#171752),(#171753,#171754),
(#171755,#171756),(#171757,#171758),(#171759,#171760),(#171761,#171762),
(#171763,#171764),(#171765,#171766),(#171767,#171768),(#171769,#171770),
(#171771,#171772),(#171773,#171774),(#171775,#171776),(#171777,#171778),
(#171779,#171780),(#171781,#171782),(#171783,#171784),(#171785,#171786),
(#171787,#171788),(#171789,#171790),(#171791,#171792),(#171793,#171794),
(#171795,#171796),(#171797,#171798),(#171799,#171800),(#171801,#171802),
(#171803,#171804),(#171805,#171806),(#171807,#171808),(#171809,#171810),
(#171811,#171812),(#171813,#171814),(#171815,#171816),(#171817,#171818),
(#171819,#171820),(#171821,#171822),(#171823,#171824),(#171825,#171826),
(#171827,#171828),(#171829,#171830),(#171831,#171832),(#171833,#171834),
(#171835,#171836),(#171837,#171838),(#171839,#171840),(#171841,#171842),
(#171843,#171844),(#171845,#171846),(#171847,#171848),(#171849,#171850),
(#171851,#171852),(#171853,#171854),(#171855,#171856),(#171857,#171858),
(#171859,#171860),(#171861,#171862),(#171863,#171864),(#171865,#171866),
(#171867,#171868),(#171869,#171870)),.UNSPECIFIED.,.F.,.F.,.F.)
B_SPLINE_SURFACE_WITH_KNOTS((6,1,1,1,1,1,1,1,1,1,1,1,1,1,1,1,1,1,1,1,1,
1,1,1,1,1,1,1,1,1,1,1,1,1,1,1,1,1,1,1,1,1,1,1,1,1,1,1,1,1,1,1,1,1,1,1,1,
1,1,1,1,1,1,1,1,1,1,1,1,1,1,1,1,1,1,1,1,1,1,1,1,1,1,1,1,1,1,1,1,1,1,1,1,
1,1,1,1,1,1,1,1,1,1,1,1,1,1,1,1,1,1,1,1,1,1,1,1,1,1,1,1,1,1,1,1,1,1,1,1,
1,1,1,1,1,1,1,1,1,1,1,1,1,1,1,1,1,1,1,1,1,1,1,1,1,1,1,1,1,1,1,1,1,1,1,1,
1,1,1,1,1,1,1,1,1,1,1,1,1,1,1,1,1,1,1,1,1,1,1,1,1,1,1,1,1,1,1,1,1,1,1,6),
(2,2),(-1.,-0.995000000000001,-0.990000000000001,-0.985000000000001,-0.980000000000001,
-0.975000000000001,-0.970000000000001,-0.965000000000001,-0.960000000000001,
-0.955000000000001,-0.950000000000001,-0.945000000000001,-0.940000000000001,
-0.935000000000001,-0.930000000000001,-0.925000000000001,-0.920000000000001,
-0.915000000000001,-0.910000000000001,-0.905000000000001,-0.900000000000001,
-0.895000000000001,-0.890000000000001,-0.885000000000001,-0.880000000000001,
-0.875000000000001,-0.870000000000001,-0.865000000000001,-0.860000000000001,
-0.855000000000001,-0.850000000000001,-0.845000000000001,-0.840000000000001,
-0.835000000000001,-0.830000000000001,-0.825000000000001,-0.820000000000001,
-0.815000000000001,-0.810000000000001,-0.805000000000001,-0.800000000000001,
-0.795000000000001,-0.790000000000001,-0.785000000000001,-0.780000000000001,
-0.775000000000001,-0.770000000000001,-0.765000000000001,-0.760000000000001,
-0.755000000000001,-0.750000000000001,-0.745000000000001,-0.740000000000001,
-0.735000000000001,-0.730000000000001,-0.725000000000001,-0.720000000000001,
-0.715000000000001,-0.710000000000001,-0.705000000000001,-0.700000000000001,
-0.695000000000001,-0.690000000000001,-0.685,-0.68,-0.675,-0.67,-0.665,
-0.66,-0.655,-0.65,-0.645,-0.64,-0.635,-0.63,-0.625,-0.62,-0.615,-0.61,
-0.605,-0.6,-0.595,-0.59,-0.585,-0.58,-0.575,-0.57,-0.565,-0.56,-0.555,
-0.55,-0.545,-0.54,-0.535,-0.53,-0.525,-0.52,-0.515,-0.51,-0.505,-0.5,-0.495,
-0.49,-0.485,-0.48,-0.475,-0.47,-0.465,-0.46,-0.455,-0.45,-0.445,-0.44,
-0.435,-0.43,-0.425,-0.42,-0.415,-0.41,-0.405,-0.4,-0.395,-0.39,-0.385,
-0.38,-0.375,-0.37,-0.365,-0.36,-0.355,-0.35,-0.345,-0.34,-0.335,-0.33,
-0.325,-0.32,-0.315,-0.31,-0.305,-0.3,-0.295,-0.29,-0.285,-0.28,-0.275,
-0.27,-0.265,-0.26,-0.255,-0.25,-0.245,-0.24,-0.235,-0.23,-0.225,-0.22,
-0.215,-0.21,-0.205,-0.2,-0.195,-0.19,-0.185,-0.18,-0.175,-0.17,-0.165,
-0.16,-0.155,-0.15,-0.145,-0.14,-0.135,-0.13,-0.125,-0.12,-0.115,-0.11,
-0.105,-0.1,-0.095,-0.09,-0.085,-0.08,-0.075,-0.07,-0.065,-0.06,-0.055,
-0.05,-0.045,-0.04,-0.035,-0.03,-0.025,-0.02,-0.015,-0.01,-0.005,0.),(0.,
1.2),.UNSPECIFIED.)
GEOMETRIC_REPRESENTATION_ITEM()
RATIONAL_B_SPLINE_SURFACE(((1.,1.),(1.,1.),(1.,1.),(1.,1.),(1.,1.),(1.,
1.),(1.,1.),(1.,1.),(1.,1.),(1.,1.),(1.,1.),(1.,1.),(1.,1.),(1.,1.),(1.,
1.),(1.,1.),(1.,1.),(1.,1.),(1.,1.),(1.,1.),(1.,1.),(1.,1.),(1.,1.),(1.,
1.),(1.,1.),(1.,1.),(1.,1.),(1.,1.),(1.,1.),(1.,1.),(1.,1.),(1.,1.),(1.,
1.),(1.,1.),(1.,1.),(1.,1.),(1.,1.),(1.,1.),(1.,1.),(1.,1.),(1.,1.),(1.,
1.),(1.,1.),(1.,1.),(1.,1.),(1.,1.),(1.,1.),(1.,1.),(1.,1.),(1.,1.),(1.,
1.),(1.,1.),(1.,1.),(1.,1.),(1.,1.),(1.,1.),(1.,1.),(1.,1.),(1.,1.),(1.,
1.),(1.,1.),(1.,1.),(1.,1.),(1.,1.),(1.,1.),(1.,1.),(1.,1.),(1.,1.),(1.,
1.),(1.,1.),(1.,1.),(1.,1.),(1.,1.),(1.,1.),(1.,1.),(1.,1.),(1.,1.),(1.,
1.),(1.,1.),(1.,1.),(1.,1.),(1.,1.),(1.,1.),(1.,1.),(1.,1.),(1.,1.),(1.,
1.),(1.,1.),(1.,1.),(1.,1.),(1.,1.),(1.,1.),(1.,1.),(1.,1.),(1.,1.),(1.,
1.),(1.,1.),(1.,1.),(1.,1.),(1.,1.),(1.,1.),(1.,1.),(1.,1.),(1.,1.),(1.,
1.),(1.,1.),(1.,1.),(1.,1.),(1.,1.),(1.,1.),(1.,1.),(1.,1.),(1.,1.),(1.,
1.),(1.,1.),(1.,1.),(1.,1.),(1.,1.),(1.,1.),(1.,1.),(1.,1.),(1.,1.),(1.,
1.),(1.,1.),(1.,1.),(1.,1.),(1.,1.),(1.,1.),(1.,1.),(1.,1.),(1.,1.),(1.,
1.),(1.,1.),(1.,1.),(1.,1.),(1.,1.),(1.,1.),(1.,1.),(1.,1.),(1.,1.),(1.,
1.),(1.,1.),(1.,1.),(1.,1.),(1.,1.),(1.,1.),(1.,1.),(1.,1.),(1.,1.),(1.,
1.),(1.,1.),(1.,1.),(1.,1.),(1.,1.),(1.,1.),(1.,1.),(1.,1.),(1.,1.),(1.,
1.),(1.,1.),(1.,1.),(1.,1.),(1.,1.),(1.,1.),(1.,1.),(1.,1.),(1.,1.),(1.,
1.),(1.,1.),(1.,1.),(1.,1.),(1.,1.),(1.,1.),(1.,1.),(1.,1.),(1.,1.),(1.,
1.),(1.,1.),(1.,1.),(1.,1.),(1.,1.),(1.,1.),(1.,1.),(1.,1.),(1.,1.),(1.,
1.),(1.,1.),(1.,1.),(1.,1.),(1.,1.),(1.,1.),(1.,1.),(1.,1.),(1.,1.),(1.,
1.),(1.,1.),(1.,1.),(1.,1.),(1.,1.),(1.,1.),(1.,1.),(1.,1.),(1.,1.),(1.,
1.),(1.,1.)))
REPRESENTATION_ITEM('')
SURFACE()
);
#1024=(
BOUNDED_SURFACE()
B_SPLINE_SURFACE(5,1,((#172262,#172263),(#172264,#172265),(#172266,#172267),
(#172268,#172269),(#172270,#172271),(#172272,#172273),(#172274,#172275),
(#172276,#172277),(#172278,#172279),(#172280,#172281),(#172282,#172283),
(#172284,#172285),(#172286,#172287),(#172288,#172289),(#172290,#172291),
(#172292,#172293),(#172294,#172295),(#172296,#172297),(#172298,#172299),
(#172300,#172301),(#172302,#172303),(#172304,#172305),(#172306,#172307),
(#172308,#172309),(#172310,#172311),(#172312,#172313),(#172314,#172315),
(#172316,#172317),(#172318,#172319),(#172320,#172321),(#172322,#172323),
(#172324,#172325),(#172326,#172327),(#172328,#172329),(#172330,#172331),
(#172332,#172333),(#172334,#172335),(#172336,#172337),(#172338,#172339),
(#172340,#172341),(#172342,#172343),(#172344,#172345),(#172346,#172347),
(#172348,#172349),(#172350,#172351),(#172352,#172353),(#172354,#172355),
(#172356,#172357),(#172358,#172359),(#172360,#172361),(#172362,#172363),
(#172364,#172365),(#172366,#172367),(#172368,#172369),(#172370,#172371),
(#172372,#172373),(#172374,#172375),(#172376,#172377),(#172378,#172379),
(#172380,#172381),(#172382,#172383),(#172384,#172385),(#172386,#172387),
(#172388,#172389),(#172390,#172391),(#172392,#172393),(#172394,#172395),
(#172396,#172397),(#172398,#172399),(#172400,#172401),(#172402,#172403),
(#172404,#172405),(#172406,#172407),(#172408,#172409),(#172410,#172411),
(#172412,#172413),(#172414,#172415),(#172416,#172417),(#172418,#172419),
(#172420,#172421),(#172422,#172423),(#172424,#172425),(#172426,#172427),
(#172428,#172429),(#172430,#172431),(#172432,#172433),(#172434,#172435),
(#172436,#172437),(#172438,#172439),(#172440,#172441),(#172442,#172443),
(#172444,#172445),(#172446,#172447),(#172448,#172449),(#172450,#172451),
(#172452,#172453),(#172454,#172455),(#172456,#172457),(#172458,#172459),
(#172460,#172461),(#172462,#172463),(#172464,#172465),(#172466,#172467),
(#172468,#172469),(#172470,#172471),(#172472,#172473),(#172474,#172475),
(#172476,#172477),(#172478,#172479),(#172480,#172481),(#172482,#172483),
(#172484,#172485),(#172486,#172487),(#172488,#172489),(#172490,#172491),
(#172492,#172493),(#172494,#172495),(#172496,#172497),(#172498,#172499),
(#172500,#172501),(#172502,#172503),(#172504,#172505),(#172506,#172507),
(#172508,#172509),(#172510,#172511),(#172512,#172513),(#172514,#172515),
(#172516,#172517),(#172518,#172519),(#172520,#172521),(#172522,#172523),
(#172524,#172525),(#172526,#172527),(#172528,#172529),(#172530,#172531),
(#172532,#172533),(#172534,#172535),(#172536,#172537),(#172538,#172539),
(#172540,#172541),(#172542,#172543),(#172544,#172545),(#172546,#172547),
(#172548,#172549),(#172550,#172551),(#172552,#172553),(#172554,#172555),
(#172556,#172557),(#172558,#172559),(#172560,#172561),(#172562,#172563),
(#172564,#172565),(#172566,#172567),(#172568,#172569),(#172570,#172571),
(#172572,#172573),(#172574,#172575),(#172576,#172577),(#172578,#172579),
(#172580,#172581),(#172582,#172583),(#172584,#172585),(#172586,#172587),
(#172588,#172589),(#172590,#172591),(#172592,#172593),(#172594,#172595),
(#172596,#172597),(#172598,#172599),(#172600,#172601),(#172602,#172603),
(#172604,#172605),(#172606,#172607),(#172608,#172609),(#172610,#172611),
(#172612,#172613),(#172614,#172615),(#172616,#172617),(#172618,#172619),
(#172620,#172621),(#172622,#172623),(#172624,#172625),(#172626,#172627),
(#172628,#172629),(#172630,#172631),(#172632,#172633),(#172634,#172635),
(#172636,#172637),(#172638,#172639),(#172640,#172641),(#172642,#172643),
(#172644,#172645),(#172646,#172647),(#172648,#172649),(#172650,#172651),
(#172652,#172653),(#172654,#172655),(#172656,#172657),(#172658,#172659),
(#172660,#172661),(#172662,#172663),(#172664,#172665),(#172666,#172667),
(#172668,#172669),(#172670,#172671)),.UNSPECIFIED.,.F.,.F.,.F.)
B_SPLINE_SURFACE_WITH_KNOTS((6,1,1,1,1,1,1,1,1,1,1,1,1,1,1,1,1,1,1,1,1,
1,1,1,1,1,1,1,1,1,1,1,1,1,1,1,1,1,1,1,1,1,1,1,1,1,1,1,1,1,1,1,1,1,1,1,1,
1,1,1,1,1,1,1,1,1,1,1,1,1,1,1,1,1,1,1,1,1,1,1,1,1,1,1,1,1,1,1,1,1,1,1,1,
1,1,1,1,1,1,1,1,1,1,1,1,1,1,1,1,1,1,1,1,1,1,1,1,1,1,1,1,1,1,1,1,1,1,1,1,
1,1,1,1,1,1,1,1,1,1,1,1,1,1,1,1,1,1,1,1,1,1,1,1,1,1,1,1,1,1,1,1,1,1,1,1,
1,1,1,1,1,1,1,1,1,1,1,1,1,1,1,1,1,1,1,1,1,1,1,1,1,1,1,1,1,1,1,1,1,1,1,6),
(2,2),(-1.,-0.995000000000001,-0.990000000000001,-0.985000000000001,-0.980000000000001,
-0.975000000000001,-0.970000000000001,-0.965000000000001,-0.960000000000001,
-0.955000000000001,-0.950000000000001,-0.945000000000001,-0.940000000000001,
-0.935000000000001,-0.930000000000001,-0.925000000000001,-0.920000000000001,
-0.915000000000001,-0.910000000000001,-0.905000000000001,-0.900000000000001,
-0.895000000000001,-0.890000000000001,-0.885000000000001,-0.880000000000001,
-0.875000000000001,-0.870000000000001,-0.865000000000001,-0.860000000000001,
-0.855000000000001,-0.850000000000001,-0.845000000000001,-0.840000000000001,
-0.835000000000001,-0.830000000000001,-0.825000000000001,-0.820000000000001,
-0.815000000000001,-0.810000000000001,-0.805000000000001,-0.800000000000001,
-0.795000000000001,-0.790000000000001,-0.785000000000001,-0.780000000000001,
-0.775000000000001,-0.770000000000001,-0.765000000000001,-0.760000000000001,
-0.755000000000001,-0.750000000000001,-0.745000000000001,-0.740000000000001,
-0.735000000000001,-0.730000000000001,-0.725000000000001,-0.720000000000001,
-0.715000000000001,-0.710000000000001,-0.705000000000001,-0.700000000000001,
-0.695000000000001,-0.690000000000001,-0.685,-0.68,-0.675,-0.67,-0.665,
-0.66,-0.655,-0.65,-0.645,-0.64,-0.635,-0.63,-0.625,-0.62,-0.615,-0.61,
-0.605,-0.6,-0.595,-0.59,-0.585,-0.58,-0.575,-0.57,-0.565,-0.56,-0.555,
-0.55,-0.545,-0.54,-0.535,-0.53,-0.525,-0.52,-0.515,-0.51,-0.505,-0.5,-0.495,
-0.49,-0.485,-0.48,-0.475,-0.47,-0.465,-0.46,-0.455,-0.45,-0.445,-0.44,
-0.435,-0.43,-0.425,-0.42,-0.415,-0.41,-0.405,-0.4,-0.395,-0.39,-0.385,
-0.38,-0.375,-0.37,-0.365,-0.36,-0.355,-0.35,-0.345,-0.34,-0.335,-0.33,
-0.325,-0.32,-0.315,-0.31,-0.305,-0.3,-0.295,-0.29,-0.285,-0.28,-0.275,
-0.27,-0.265,-0.26,-0.255,-0.25,-0.245,-0.24,-0.235,-0.23,-0.225,-0.22,
-0.215,-0.21,-0.205,-0.2,-0.195,-0.19,-0.185,-0.18,-0.175,-0.17,-0.165,
-0.16,-0.155,-0.15,-0.145,-0.14,-0.135,-0.13,-0.125,-0.12,-0.115,-0.11,
-0.105,-0.1,-0.095,-0.09,-0.085,-0.08,-0.075,-0.07,-0.065,-0.06,-0.055,
-0.05,-0.045,-0.04,-0.035,-0.03,-0.025,-0.02,-0.015,-0.01,-0.005,0.),(0.,
1.2),.UNSPECIFIED.)
GEOMETRIC_REPRESENTATION_ITEM()
RATIONAL_B_SPLINE_SURFACE(((1.,1.),(1.,1.),(1.,1.),(1.,1.),(1.,1.),(1.,
1.),(1.,1.),(1.,1.),(1.,1.),(1.,1.),(1.,1.),(1.,1.),(1.,1.),(1.,1.),(1.,
1.),(1.,1.),(1.,1.),(1.,1.),(1.,1.),(1.,1.),(1.,1.),(1.,1.),(1.,1.),(1.,
1.),(1.,1.),(1.,1.),(1.,1.),(1.,1.),(1.,1.),(1.,1.),(1.,1.),(1.,1.),(1.,
1.),(1.,1.),(1.,1.),(1.,1.),(1.,1.),(1.,1.),(1.,1.),(1.,1.),(1.,1.),(1.,
1.),(1.,1.),(1.,1.),(1.,1.),(1.,1.),(1.,1.),(1.,1.),(1.,1.),(1.,1.),(1.,
1.),(1.,1.),(1.,1.),(1.,1.),(1.,1.),(1.,1.),(1.,1.),(1.,1.),(1.,1.),(1.,
1.),(1.,1.),(1.,1.),(1.,1.),(1.,1.),(1.,1.),(1.,1.),(1.,1.),(1.,1.),(1.,
1.),(1.,1.),(1.,1.),(1.,1.),(1.,1.),(1.,1.),(1.,1.),(1.,1.),(1.,1.),(1.,
1.),(1.,1.),(1.,1.),(1.,1.),(1.,1.),(1.,1.),(1.,1.),(1.,1.),(1.,1.),(1.,
1.),(1.,1.),(1.,1.),(1.,1.),(1.,1.),(1.,1.),(1.,1.),(1.,1.),(1.,1.),(1.,
1.),(1.,1.),(1.,1.),(1.,1.),(1.,1.),(1.,1.),(1.,1.),(1.,1.),(1.,1.),(1.,
1.),(1.,1.),(1.,1.),(1.,1.),(1.,1.),(1.,1.),(1.,1.),(1.,1.),(1.,1.),(1.,
1.),(1.,1.),(1.,1.),(1.,1.),(1.,1.),(1.,1.),(1.,1.),(1.,1.),(1.,1.),(1.,
1.),(1.,1.),(1.,1.),(1.,1.),(1.,1.),(1.,1.),(1.,1.),(1.,1.),(1.,1.),(1.,
1.),(1.,1.),(1.,1.),(1.,1.),(1.,1.),(1.,1.),(1.,1.),(1.,1.),(1.,1.),(1.,
1.),(1.,1.),(1.,1.),(1.,1.),(1.,1.),(1.,1.),(1.,1.),(1.,1.),(1.,1.),(1.,
1.),(1.,1.),(1.,1.),(1.,1.),(1.,1.),(1.,1.),(1.,1.),(1.,1.),(1.,1.),(1.,
1.),(1.,1.),(1.,1.),(1.,1.),(1.,1.),(1.,1.),(1.,1.),(1.,1.),(1.,1.),(1.,
1.),(1.,1.),(1.,1.),(1.,1.),(1.,1.),(1.,1.),(1.,1.),(1.,1.),(1.,1.),(1.,
1.),(1.,1.),(1.,1.),(1.,1.),(1.,1.),(1.,1.),(1.,1.),(1.,1.),(1.,1.),(1.,
1.),(1.,1.),(1.,1.),(1.,1.),(1.,1.),(1.,1.),(1.,1.),(1.,1.),(1.,1.),(1.,
1.),(1.,1.),(1.,1.),(1.,1.),(1.,1.),(1.,1.),(1.,1.),(1.,1.),(1.,1.),(1.,
1.),(1.,1.)))
REPRESENTATION_ITEM('')
SURFACE()
);
#1025=(
BOUNDED_SURFACE()
B_SPLINE_SURFACE(5,1,((#173328,#173329),(#173330,#173331),(#173332,#173333),
(#173334,#173335),(#173336,#173337),(#173338,#173339),(#173340,#173341),
(#173342,#173343),(#173344,#173345),(#173346,#173347),(#173348,#173349),
(#173350,#173351),(#173352,#173353),(#173354,#173355),(#173356,#173357),
(#173358,#173359),(#173360,#173361),(#173362,#173363),(#173364,#173365),
(#173366,#173367),(#173368,#173369),(#173370,#173371),(#173372,#173373),
(#173374,#173375),(#173376,#173377),(#173378,#173379),(#173380,#173381),
(#173382,#173383),(#173384,#173385),(#173386,#173387),(#173388,#173389),
(#173390,#173391),(#173392,#173393),(#173394,#173395),(#173396,#173397),
(#173398,#173399),(#173400,#173401),(#173402,#173403),(#173404,#173405),
(#173406,#173407),(#173408,#173409),(#173410,#173411),(#173412,#173413),
(#173414,#173415),(#173416,#173417),(#173418,#173419),(#173420,#173421),
(#173422,#173423),(#173424,#173425),(#173426,#173427),(#173428,#173429),
(#173430,#173431),(#173432,#173433),(#173434,#173435),(#173436,#173437),
(#173438,#173439),(#173440,#173441),(#173442,#173443),(#173444,#173445),
(#173446,#173447),(#173448,#173449),(#173450,#173451),(#173452,#173453),
(#173454,#173455),(#173456,#173457),(#173458,#173459),(#173460,#173461),
(#173462,#173463),(#173464,#173465),(#173466,#173467),(#173468,#173469),
(#173470,#173471),(#173472,#173473),(#173474,#173475),(#173476,#173477),
(#173478,#173479),(#173480,#173481),(#173482,#173483),(#173484,#173485),
(#173486,#173487),(#173488,#173489),(#173490,#173491),(#173492,#173493),
(#173494,#173495),(#173496,#173497),(#173498,#173499),(#173500,#173501),
(#173502,#173503),(#173504,#173505),(#173506,#173507),(#173508,#173509),
(#173510,#173511),(#173512,#173513),(#173514,#173515),(#173516,#173517),
(#173518,#173519),(#173520,#173521),(#173522,#173523),(#173524,#173525),
(#173526,#173527),(#173528,#173529),(#173530,#173531),(#173532,#173533),
(#173534,#173535),(#173536,#173537),(#173538,#173539),(#173540,#173541),
(#173542,#173543),(#173544,#173545),(#173546,#173547),(#173548,#173549),
(#173550,#173551),(#173552,#173553),(#173554,#173555),(#173556,#173557),
(#173558,#173559),(#173560,#173561),(#173562,#173563),(#173564,#173565),
(#173566,#173567),(#173568,#173569),(#173570,#173571),(#173572,#173573),
(#173574,#173575),(#173576,#173577),(#173578,#173579),(#173580,#173581),
(#173582,#173583),(#173584,#173585),(#173586,#173587),(#173588,#173589),
(#173590,#173591),(#173592,#173593),(#173594,#173595),(#173596,#173597),
(#173598,#173599),(#173600,#173601),(#173602,#173603),(#173604,#173605),
(#173606,#173607),(#173608,#173609),(#173610,#173611),(#173612,#173613),
(#173614,#173615),(#173616,#173617),(#173618,#173619),(#173620,#173621),
(#173622,#173623),(#173624,#173625),(#173626,#173627),(#173628,#173629),
(#173630,#173631),(#173632,#173633),(#173634,#173635),(#173636,#173637),
(#173638,#173639),(#173640,#173641),(#173642,#173643),(#173644,#173645),
(#173646,#173647),(#173648,#173649),(#173650,#173651),(#173652,#173653),
(#173654,#173655),(#173656,#173657),(#173658,#173659),(#173660,#173661),
(#173662,#173663),(#173664,#173665),(#173666,#173667),(#173668,#173669),
(#173670,#173671),(#173672,#173673),(#173674,#173675),(#173676,#173677),
(#173678,#173679),(#173680,#173681),(#173682,#173683),(#173684,#173685),
(#173686,#173687),(#173688,#173689),(#173690,#173691),(#173692,#173693),
(#173694,#173695),(#173696,#173697),(#173698,#173699),(#173700,#173701),
(#173702,#173703),(#173704,#173705),(#173706,#173707),(#173708,#173709),
(#173710,#173711),(#173712,#173713),(#173714,#173715),(#173716,#173717),
(#173718,#173719),(#173720,#173721),(#173722,#173723),(#173724,#173725),
(#173726,#173727),(#173728,#173729),(#173730,#173731),(#173732,#173733),
(#173734,#173735),(#173736,#173737)),.UNSPECIFIED.,.F.,.F.,.F.)
B_SPLINE_SURFACE_WITH_KNOTS((6,1,1,1,1,1,1,1,1,1,1,1,1,1,1,1,1,1,1,1,1,
1,1,1,1,1,1,1,1,1,1,1,1,1,1,1,1,1,1,1,1,1,1,1,1,1,1,1,1,1,1,1,1,1,1,1,1,
1,1,1,1,1,1,1,1,1,1,1,1,1,1,1,1,1,1,1,1,1,1,1,1,1,1,1,1,1,1,1,1,1,1,1,1,
1,1,1,1,1,1,1,1,1,1,1,1,1,1,1,1,1,1,1,1,1,1,1,1,1,1,1,1,1,1,1,1,1,1,1,1,
1,1,1,1,1,1,1,1,1,1,1,1,1,1,1,1,1,1,1,1,1,1,1,1,1,1,1,1,1,1,1,1,1,1,1,1,
1,1,1,1,1,1,1,1,1,1,1,1,1,1,1,1,1,1,1,1,1,1,1,1,1,1,1,1,1,1,1,1,1,1,1,6),
(2,2),(0.,0.005,0.01,0.015,0.02,0.025,0.03,0.035,0.04,0.045,0.05,0.055,
0.06,0.065,0.07,0.075,0.08,0.085,0.09,0.095,0.1,0.105,0.11,0.115,0.12,0.125,
0.13,0.135,0.14,0.145,0.15,0.155,0.16,0.165,0.17,0.175,0.18,0.185,0.19,
0.195,0.2,0.205,0.21,0.215,0.22,0.225,0.23,0.235,0.24,0.245,0.25,0.255,
0.26,0.265,0.27,0.275,0.28,0.285,0.29,0.295,0.3,0.305,0.31,0.315,0.32,0.325,
0.33,0.335,0.34,0.345,0.35,0.355,0.36,0.365,0.37,0.375,0.38,0.385,0.39,
0.395,0.4,0.405,0.41,0.415,0.42,0.425,0.43,0.435,0.44,0.445,0.45,0.455,
0.46,0.465,0.47,0.475,0.48,0.485,0.49,0.495,0.5,0.505,0.51,0.515,0.52,0.525,
0.53,0.535,0.54,0.545,0.55,0.555,0.56,0.565,0.57,0.575,0.58,0.585,0.59,
0.595,0.6,0.605,0.61,0.615,0.62,0.625,0.63,0.635,0.64,0.645,0.65,0.655,
0.66,0.665,0.67,0.675,0.68,0.685,0.690000000000001,0.695000000000001,0.700000000000001,
0.705000000000001,0.710000000000001,0.715000000000001,0.720000000000001,
0.725000000000001,0.730000000000001,0.735000000000001,0.740000000000001,
0.745000000000001,0.750000000000001,0.755000000000001,0.760000000000001,
0.765000000000001,0.770000000000001,0.775000000000001,0.780000000000001,
0.785000000000001,0.790000000000001,0.795000000000001,0.800000000000001,
0.805000000000001,0.810000000000001,0.815000000000001,0.820000000000001,
0.825000000000001,0.830000000000001,0.835000000000001,0.840000000000001,
0.845000000000001,0.850000000000001,0.855000000000001,0.860000000000001,
0.865000000000001,0.870000000000001,0.875000000000001,0.880000000000001,
0.885000000000001,0.890000000000001,0.895000000000001,0.900000000000001,
0.905000000000001,0.910000000000001,0.915000000000001,0.920000000000001,
0.925000000000001,0.930000000000001,0.935000000000001,0.940000000000001,
0.945000000000001,0.950000000000001,0.955000000000001,0.960000000000001,
0.965000000000001,0.970000000000001,0.975000000000001,0.980000000000001,
0.985000000000001,0.990000000000001,0.995000000000001,1.),(0.,1.2),
 .UNSPECIFIED.)
GEOMETRIC_REPRESENTATION_ITEM()
RATIONAL_B_SPLINE_SURFACE(((1.,1.),(1.,1.),(1.,1.),(1.,1.),(1.,1.),(1.,
1.),(1.,1.),(1.,1.),(1.,1.),(1.,1.),(1.,1.),(1.,1.),(1.,1.),(1.,1.),(1.,
1.),(1.,1.),(1.,1.),(1.,1.),(1.,1.),(1.,1.),(1.,1.),(1.,1.),(1.,1.),(1.,
1.),(1.,1.),(1.,1.),(1.,1.),(1.,1.),(1.,1.),(1.,1.),(1.,1.),(1.,1.),(1.,
1.),(1.,1.),(1.,1.),(1.,1.),(1.,1.),(1.,1.),(1.,1.),(1.,1.),(1.,1.),(1.,
1.),(1.,1.),(1.,1.),(1.,1.),(1.,1.),(1.,1.),(1.,1.),(1.,1.),(1.,1.),(1.,
1.),(1.,1.),(1.,1.),(1.,1.),(1.,1.),(1.,1.),(1.,1.),(1.,1.),(1.,1.),(1.,
1.),(1.,1.),(1.,1.),(1.,1.),(1.,1.),(1.,1.),(1.,1.),(1.,1.),(1.,1.),(1.,
1.),(1.,1.),(1.,1.),(1.,1.),(1.,1.),(1.,1.),(1.,1.),(1.,1.),(1.,1.),(1.,
1.),(1.,1.),(1.,1.),(1.,1.),(1.,1.),(1.,1.),(1.,1.),(1.,1.),(1.,1.),(1.,
1.),(1.,1.),(1.,1.),(1.,1.),(1.,1.),(1.,1.),(1.,1.),(1.,1.),(1.,1.),(1.,
1.),(1.,1.),(1.,1.),(1.,1.),(1.,1.),(1.,1.),(1.,1.),(1.,1.),(1.,1.),(1.,
1.),(1.,1.),(1.,1.),(1.,1.),(1.,1.),(1.,1.),(1.,1.),(1.,1.),(1.,1.),(1.,
1.),(1.,1.),(1.,1.),(1.,1.),(1.,1.),(1.,1.),(1.,1.),(1.,1.),(1.,1.),(1.,
1.),(1.,1.),(1.,1.),(1.,1.),(1.,1.),(1.,1.),(1.,1.),(1.,1.),(1.,1.),(1.,
1.),(1.,1.),(1.,1.),(1.,1.),(1.,1.),(1.,1.),(1.,1.),(1.,1.),(1.,1.),(1.,
1.),(1.,1.),(1.,1.),(1.,1.),(1.,1.),(1.,1.),(1.,1.),(1.,1.),(1.,1.),(1.,
1.),(1.,1.),(1.,1.),(1.,1.),(1.,1.),(1.,1.),(1.,1.),(1.,1.),(1.,1.),(1.,
1.),(1.,1.),(1.,1.),(1.,1.),(1.,1.),(1.,1.),(1.,1.),(1.,1.),(1.,1.),(1.,
1.),(1.,1.),(1.,1.),(1.,1.),(1.,1.),(1.,1.),(1.,1.),(1.,1.),(1.,1.),(1.,
1.),(1.,1.),(1.,1.),(1.,1.),(1.,1.),(1.,1.),(1.,1.),(1.,1.),(1.,1.),(1.,
1.),(1.,1.),(1.,1.),(1.,1.),(1.,1.),(1.,1.),(1.,1.),(1.,1.),(1.,1.),(1.,
1.),(1.,1.),(1.,1.),(1.,1.),(1.,1.),(1.,1.),(1.,1.),(1.,1.),(1.,1.),(1.,
1.),(1.,1.)))
REPRESENTATION_ITEM('')
SURFACE()
);
#1026=(
BOUNDED_SURFACE()
B_SPLINE_SURFACE(5,1,((#174175,#174176),(#174177,#174178),(#174179,#174180),
(#174181,#174182),(#174183,#174184),(#174185,#174186),(#174187,#174188),
(#174189,#174190),(#174191,#174192),(#174193,#174194),(#174195,#174196),
(#174197,#174198),(#174199,#174200),(#174201,#174202),(#174203,#174204),
(#174205,#174206),(#174207,#174208),(#174209,#174210),(#174211,#174212),
(#174213,#174214),(#174215,#174216),(#174217,#174218),(#174219,#174220),
(#174221,#174222),(#174223,#174224),(#174225,#174226),(#174227,#174228),
(#174229,#174230),(#174231,#174232),(#174233,#174234),(#174235,#174236),
(#174237,#174238),(#174239,#174240),(#174241,#174242),(#174243,#174244),
(#174245,#174246),(#174247,#174248),(#174249,#174250),(#174251,#174252),
(#174253,#174254),(#174255,#174256),(#174257,#174258),(#174259,#174260),
(#174261,#174262),(#174263,#174264),(#174265,#174266),(#174267,#174268),
(#174269,#174270),(#174271,#174272),(#174273,#174274),(#174275,#174276),
(#174277,#174278),(#174279,#174280),(#174281,#174282),(#174283,#174284),
(#174285,#174286),(#174287,#174288),(#174289,#174290),(#174291,#174292),
(#174293,#174294),(#174295,#174296),(#174297,#174298),(#174299,#174300),
(#174301,#174302),(#174303,#174304),(#174305,#174306),(#174307,#174308),
(#174309,#174310),(#174311,#174312),(#174313,#174314),(#174315,#174316),
(#174317,#174318),(#174319,#174320),(#174321,#174322),(#174323,#174324),
(#174325,#174326),(#174327,#174328),(#174329,#174330),(#174331,#174332),
(#174333,#174334),(#174335,#174336),(#174337,#174338),(#174339,#174340),
(#174341,#174342),(#174343,#174344),(#174345,#174346),(#174347,#174348),
(#174349,#174350),(#174351,#174352),(#174353,#174354),(#174355,#174356),
(#174357,#174358),(#174359,#174360),(#174361,#174362),(#174363,#174364),
(#174365,#174366),(#174367,#174368),(#174369,#174370),(#174371,#174372),
(#174373,#174374),(#174375,#174376),(#174377,#174378),(#174379,#174380),
(#174381,#174382),(#174383,#174384),(#174385,#174386),(#174387,#174388),
(#174389,#174390),(#174391,#174392),(#174393,#174394),(#174395,#174396),
(#174397,#174398),(#174399,#174400),(#174401,#174402),(#174403,#174404),
(#174405,#174406),(#174407,#174408),(#174409,#174410),(#174411,#174412),
(#174413,#174414),(#174415,#174416),(#174417,#174418),(#174419,#174420),
(#174421,#174422),(#174423,#174424),(#174425,#174426),(#174427,#174428),
(#174429,#174430),(#174431,#174432),(#174433,#174434),(#174435,#174436),
(#174437,#174438),(#174439,#174440),(#174441,#174442),(#174443,#174444),
(#174445,#174446),(#174447,#174448),(#174449,#174450),(#174451,#174452),
(#174453,#174454),(#174455,#174456),(#174457,#174458),(#174459,#174460),
(#174461,#174462),(#174463,#174464),(#174465,#174466),(#174467,#174468),
(#174469,#174470),(#174471,#174472),(#174473,#174474),(#174475,#174476),
(#174477,#174478),(#174479,#174480),(#174481,#174482),(#174483,#174484),
(#174485,#174486),(#174487,#174488),(#174489,#174490),(#174491,#174492),
(#174493,#174494),(#174495,#174496),(#174497,#174498),(#174499,#174500),
(#174501,#174502),(#174503,#174504),(#174505,#174506),(#174507,#174508),
(#174509,#174510),(#174511,#174512),(#174513,#174514),(#174515,#174516),
(#174517,#174518),(#174519,#174520),(#174521,#174522),(#174523,#174524),
(#174525,#174526),(#174527,#174528),(#174529,#174530),(#174531,#174532),
(#174533,#174534),(#174535,#174536),(#174537,#174538),(#174539,#174540),
(#174541,#174542),(#174543,#174544),(#174545,#174546),(#174547,#174548),
(#174549,#174550),(#174551,#174552),(#174553,#174554),(#174555,#174556),
(#174557,#174558),(#174559,#174560),(#174561,#174562),(#174563,#174564),
(#174565,#174566),(#174567,#174568),(#174569,#174570),(#174571,#174572),
(#174573,#174574),(#174575,#174576),(#174577,#174578),(#174579,#174580),
(#174581,#174582),(#174583,#174584)),.UNSPECIFIED.,.F.,.F.,.F.)
B_SPLINE_SURFACE_WITH_KNOTS((6,1,1,1,1,1,1,1,1,1,1,1,1,1,1,1,1,1,1,1,1,
1,1,1,1,1,1,1,1,1,1,1,1,1,1,1,1,1,1,1,1,1,1,1,1,1,1,1,1,1,1,1,1,1,1,1,1,
1,1,1,1,1,1,1,1,1,1,1,1,1,1,1,1,1,1,1,1,1,1,1,1,1,1,1,1,1,1,1,1,1,1,1,1,
1,1,1,1,1,1,1,1,1,1,1,1,1,1,1,1,1,1,1,1,1,1,1,1,1,1,1,1,1,1,1,1,1,1,1,1,
1,1,1,1,1,1,1,1,1,1,1,1,1,1,1,1,1,1,1,1,1,1,1,1,1,1,1,1,1,1,1,1,1,1,1,1,
1,1,1,1,1,1,1,1,1,1,1,1,1,1,1,1,1,1,1,1,1,1,1,1,1,1,1,1,1,1,1,1,1,1,1,6),
(2,2),(-1.,-0.995000000000001,-0.990000000000001,-0.985000000000001,-0.980000000000001,
-0.975000000000001,-0.970000000000001,-0.965000000000001,-0.960000000000001,
-0.955000000000001,-0.950000000000001,-0.945000000000001,-0.940000000000001,
-0.935000000000001,-0.930000000000001,-0.925000000000001,-0.920000000000001,
-0.915000000000001,-0.910000000000001,-0.905000000000001,-0.900000000000001,
-0.895000000000001,-0.890000000000001,-0.885000000000001,-0.880000000000001,
-0.875000000000001,-0.870000000000001,-0.865000000000001,-0.860000000000001,
-0.855000000000001,-0.850000000000001,-0.845000000000001,-0.840000000000001,
-0.835000000000001,-0.830000000000001,-0.825000000000001,-0.820000000000001,
-0.815000000000001,-0.810000000000001,-0.805000000000001,-0.800000000000001,
-0.795000000000001,-0.790000000000001,-0.785000000000001,-0.780000000000001,
-0.775000000000001,-0.770000000000001,-0.765000000000001,-0.760000000000001,
-0.755000000000001,-0.750000000000001,-0.745000000000001,-0.740000000000001,
-0.735000000000001,-0.730000000000001,-0.725000000000001,-0.720000000000001,
-0.715000000000001,-0.710000000000001,-0.705000000000001,-0.700000000000001,
-0.695000000000001,-0.690000000000001,-0.685,-0.68,-0.675,-0.67,-0.665,
-0.66,-0.655,-0.65,-0.645,-0.64,-0.635,-0.63,-0.625,-0.62,-0.615,-0.61,
-0.605,-0.6,-0.595,-0.59,-0.585,-0.58,-0.575,-0.57,-0.565,-0.56,-0.555,
-0.55,-0.545,-0.54,-0.535,-0.53,-0.525,-0.52,-0.515,-0.51,-0.505,-0.5,-0.495,
-0.49,-0.485,-0.48,-0.475,-0.47,-0.465,-0.46,-0.455,-0.45,-0.445,-0.44,
-0.435,-0.43,-0.425,-0.42,-0.415,-0.41,-0.405,-0.4,-0.395,-0.39,-0.385,
-0.38,-0.375,-0.37,-0.365,-0.36,-0.355,-0.35,-0.345,-0.34,-0.335,-0.33,
-0.325,-0.32,-0.315,-0.31,-0.305,-0.3,-0.295,-0.29,-0.285,-0.28,-0.275,
-0.27,-0.265,-0.26,-0.255,-0.25,-0.245,-0.24,-0.235,-0.23,-0.225,-0.22,
-0.215,-0.21,-0.205,-0.2,-0.195,-0.19,-0.185,-0.18,-0.175,-0.17,-0.165,
-0.16,-0.155,-0.15,-0.145,-0.14,-0.135,-0.13,-0.125,-0.12,-0.115,-0.11,
-0.105,-0.1,-0.095,-0.09,-0.085,-0.08,-0.075,-0.07,-0.065,-0.06,-0.055,
-0.05,-0.045,-0.04,-0.035,-0.03,-0.025,-0.02,-0.015,-0.01,-0.005,0.),(0.,
1.2),.UNSPECIFIED.)
GEOMETRIC_REPRESENTATION_ITEM()
RATIONAL_B_SPLINE_SURFACE(((1.,1.),(1.,1.),(1.,1.),(1.,1.),(1.,1.),(1.,
1.),(1.,1.),(1.,1.),(1.,1.),(1.,1.),(1.,1.),(1.,1.),(1.,1.),(1.,1.),(1.,
1.),(1.,1.),(1.,1.),(1.,1.),(1.,1.),(1.,1.),(1.,1.),(1.,1.),(1.,1.),(1.,
1.),(1.,1.),(1.,1.),(1.,1.),(1.,1.),(1.,1.),(1.,1.),(1.,1.),(1.,1.),(1.,
1.),(1.,1.),(1.,1.),(1.,1.),(1.,1.),(1.,1.),(1.,1.),(1.,1.),(1.,1.),(1.,
1.),(1.,1.),(1.,1.),(1.,1.),(1.,1.),(1.,1.),(1.,1.),(1.,1.),(1.,1.),(1.,
1.),(1.,1.),(1.,1.),(1.,1.),(1.,1.),(1.,1.),(1.,1.),(1.,1.),(1.,1.),(1.,
1.),(1.,1.),(1.,1.),(1.,1.),(1.,1.),(1.,1.),(1.,1.),(1.,1.),(1.,1.),(1.,
1.),(1.,1.),(1.,1.),(1.,1.),(1.,1.),(1.,1.),(1.,1.),(1.,1.),(1.,1.),(1.,
1.),(1.,1.),(1.,1.),(1.,1.),(1.,1.),(1.,1.),(1.,1.),(1.,1.),(1.,1.),(1.,
1.),(1.,1.),(1.,1.),(1.,1.),(1.,1.),(1.,1.),(1.,1.),(1.,1.),(1.,1.),(1.,
1.),(1.,1.),(1.,1.),(1.,1.),(1.,1.),(1.,1.),(1.,1.),(1.,1.),(1.,1.),(1.,
1.),(1.,1.),(1.,1.),(1.,1.),(1.,1.),(1.,1.),(1.,1.),(1.,1.),(1.,1.),(1.,
1.),(1.,1.),(1.,1.),(1.,1.),(1.,1.),(1.,1.),(1.,1.),(1.,1.),(1.,1.),(1.,
1.),(1.,1.),(1.,1.),(1.,1.),(1.,1.),(1.,1.),(1.,1.),(1.,1.),(1.,1.),(1.,
1.),(1.,1.),(1.,1.),(1.,1.),(1.,1.),(1.,1.),(1.,1.),(1.,1.),(1.,1.),(1.,
1.),(1.,1.),(1.,1.),(1.,1.),(1.,1.),(1.,1.),(1.,1.),(1.,1.),(1.,1.),(1.,
1.),(1.,1.),(1.,1.),(1.,1.),(1.,1.),(1.,1.),(1.,1.),(1.,1.),(1.,1.),(1.,
1.),(1.,1.),(1.,1.),(1.,1.),(1.,1.),(1.,1.),(1.,1.),(1.,1.),(1.,1.),(1.,
1.),(1.,1.),(1.,1.),(1.,1.),(1.,1.),(1.,1.),(1.,1.),(1.,1.),(1.,1.),(1.,
1.),(1.,1.),(1.,1.),(1.,1.),(1.,1.),(1.,1.),(1.,1.),(1.,1.),(1.,1.),(1.,
1.),(1.,1.),(1.,1.),(1.,1.),(1.,1.),(1.,1.),(1.,1.),(1.,1.),(1.,1.),(1.,
1.),(1.,1.),(1.,1.),(1.,1.),(1.,1.),(1.,1.),(1.,1.),(1.,1.),(1.,1.),(1.,
1.),(1.,1.)))
REPRESENTATION_ITEM('')
SURFACE()
);
#1027=(
BOUNDED_SURFACE()
B_SPLINE_SURFACE(5,1,((#185605,#185606),(#185607,#185608),(#185609,#185610),
(#185611,#185612),(#185613,#185614),(#185615,#185616),(#185617,#185618),
(#185619,#185620),(#185621,#185622),(#185623,#185624),(#185625,#185626),
(#185627,#185628),(#185629,#185630),(#185631,#185632),(#185633,#185634),
(#185635,#185636),(#185637,#185638),(#185639,#185640),(#185641,#185642),
(#185643,#185644),(#185645,#185646),(#185647,#185648),(#185649,#185650),
(#185651,#185652),(#185653,#185654),(#185655,#185656),(#185657,#185658),
(#185659,#185660),(#185661,#185662),(#185663,#185664),(#185665,#185666),
(#185667,#185668),(#185669,#185670),(#185671,#185672),(#185673,#185674),
(#185675,#185676),(#185677,#185678),(#185679,#185680),(#185681,#185682),
(#185683,#185684),(#185685,#185686),(#185687,#185688),(#185689,#185690),
(#185691,#185692),(#185693,#185694),(#185695,#185696),(#185697,#185698),
(#185699,#185700),(#185701,#185702),(#185703,#185704),(#185705,#185706),
(#185707,#185708),(#185709,#185710),(#185711,#185712),(#185713,#185714),
(#185715,#185716),(#185717,#185718),(#185719,#185720),(#185721,#185722),
(#185723,#185724),(#185725,#185726),(#185727,#185728),(#185729,#185730),
(#185731,#185732),(#185733,#185734),(#185735,#185736),(#185737,#185738),
(#185739,#185740),(#185741,#185742),(#185743,#185744),(#185745,#185746),
(#185747,#185748),(#185749,#185750),(#185751,#185752),(#185753,#185754),
(#185755,#185756),(#185757,#185758),(#185759,#185760),(#185761,#185762),
(#185763,#185764),(#185765,#185766),(#185767,#185768),(#185769,#185770),
(#185771,#185772),(#185773,#185774),(#185775,#185776),(#185777,#185778),
(#185779,#185780),(#185781,#185782),(#185783,#185784),(#185785,#185786),
(#185787,#185788),(#185789,#185790),(#185791,#185792),(#185793,#185794),
(#185795,#185796),(#185797,#185798),(#185799,#185800),(#185801,#185802),
(#185803,#185804),(#185805,#185806),(#185807,#185808),(#185809,#185810),
(#185811,#185812),(#185813,#185814),(#185815,#185816),(#185817,#185818),
(#185819,#185820),(#185821,#185822),(#185823,#185824),(#185825,#185826),
(#185827,#185828),(#185829,#185830),(#185831,#185832),(#185833,#185834),
(#185835,#185836),(#185837,#185838),(#185839,#185840),(#185841,#185842),
(#185843,#185844),(#185845,#185846),(#185847,#185848),(#185849,#185850),
(#185851,#185852),(#185853,#185854),(#185855,#185856),(#185857,#185858),
(#185859,#185860),(#185861,#185862),(#185863,#185864),(#185865,#185866),
(#185867,#185868),(#185869,#185870),(#185871,#185872),(#185873,#185874),
(#185875,#185876),(#185877,#185878),(#185879,#185880),(#185881,#185882),
(#185883,#185884),(#185885,#185886),(#185887,#185888),(#185889,#185890),
(#185891,#185892),(#185893,#185894),(#185895,#185896),(#185897,#185898),
(#185899,#185900),(#185901,#185902),(#185903,#185904),(#185905,#185906),
(#185907,#185908),(#185909,#185910),(#185911,#185912),(#185913,#185914),
(#185915,#185916),(#185917,#185918),(#185919,#185920),(#185921,#185922),
(#185923,#185924),(#185925,#185926),(#185927,#185928),(#185929,#185930),
(#185931,#185932),(#185933,#185934),(#185935,#185936),(#185937,#185938),
(#185939,#185940),(#185941,#185942),(#185943,#185944),(#185945,#185946),
(#185947,#185948),(#185949,#185950),(#185951,#185952),(#185953,#185954),
(#185955,#185956),(#185957,#185958),(#185959,#185960),(#185961,#185962),
(#185963,#185964),(#185965,#185966),(#185967,#185968),(#185969,#185970),
(#185971,#185972),(#185973,#185974),(#185975,#185976),(#185977,#185978),
(#185979,#185980),(#185981,#185982),(#185983,#185984),(#185985,#185986),
(#185987,#185988),(#185989,#185990),(#185991,#185992),(#185993,#185994),
(#185995,#185996),(#185997,#185998),(#185999,#186000),(#186001,#186002),
(#186003,#186004),(#186005,#186006),(#186007,#186008),(#186009,#186010),
(#186011,#186012),(#186013,#186014)),.UNSPECIFIED.,.F.,.F.,.F.)
B_SPLINE_SURFACE_WITH_KNOTS((6,1,1,1,1,1,1,1,1,1,1,1,1,1,1,1,1,1,1,1,1,
1,1,1,1,1,1,1,1,1,1,1,1,1,1,1,1,1,1,1,1,1,1,1,1,1,1,1,1,1,1,1,1,1,1,1,1,
1,1,1,1,1,1,1,1,1,1,1,1,1,1,1,1,1,1,1,1,1,1,1,1,1,1,1,1,1,1,1,1,1,1,1,1,
1,1,1,1,1,1,1,1,1,1,1,1,1,1,1,1,1,1,1,1,1,1,1,1,1,1,1,1,1,1,1,1,1,1,1,1,
1,1,1,1,1,1,1,1,1,1,1,1,1,1,1,1,1,1,1,1,1,1,1,1,1,1,1,1,1,1,1,1,1,1,1,1,
1,1,1,1,1,1,1,1,1,1,1,1,1,1,1,1,1,1,1,1,1,1,1,1,1,1,1,1,1,1,1,1,1,1,1,6),
(2,2),(-1.,-0.995000000000001,-0.990000000000001,-0.985000000000001,-0.980000000000001,
-0.975000000000001,-0.970000000000001,-0.965000000000001,-0.960000000000001,
-0.955000000000001,-0.950000000000001,-0.945000000000001,-0.940000000000001,
-0.935000000000001,-0.930000000000001,-0.925000000000001,-0.920000000000001,
-0.915000000000001,-0.910000000000001,-0.905000000000001,-0.900000000000001,
-0.895000000000001,-0.890000000000001,-0.885000000000001,-0.880000000000001,
-0.875000000000001,-0.870000000000001,-0.865000000000001,-0.860000000000001,
-0.855000000000001,-0.850000000000001,-0.845000000000001,-0.840000000000001,
-0.835000000000001,-0.830000000000001,-0.825000000000001,-0.820000000000001,
-0.815000000000001,-0.810000000000001,-0.805000000000001,-0.800000000000001,
-0.795000000000001,-0.790000000000001,-0.785000000000001,-0.780000000000001,
-0.775000000000001,-0.770000000000001,-0.765000000000001,-0.760000000000001,
-0.755000000000001,-0.750000000000001,-0.745000000000001,-0.740000000000001,
-0.735000000000001,-0.730000000000001,-0.725000000000001,-0.720000000000001,
-0.715000000000001,-0.710000000000001,-0.705000000000001,-0.700000000000001,
-0.695000000000001,-0.690000000000001,-0.685,-0.68,-0.675,-0.67,-0.665,
-0.66,-0.655,-0.65,-0.645,-0.64,-0.635,-0.63,-0.625,-0.62,-0.615,-0.61,
-0.605,-0.6,-0.595,-0.59,-0.585,-0.58,-0.575,-0.57,-0.565,-0.56,-0.555,
-0.55,-0.545,-0.54,-0.535,-0.53,-0.525,-0.52,-0.515,-0.51,-0.505,-0.5,-0.495,
-0.49,-0.485,-0.48,-0.475,-0.47,-0.465,-0.46,-0.455,-0.45,-0.445,-0.44,
-0.435,-0.43,-0.425,-0.42,-0.415,-0.41,-0.405,-0.4,-0.395,-0.39,-0.385,
-0.38,-0.375,-0.37,-0.365,-0.36,-0.355,-0.35,-0.345,-0.34,-0.335,-0.33,
-0.325,-0.32,-0.315,-0.31,-0.305,-0.3,-0.295,-0.29,-0.285,-0.28,-0.275,
-0.27,-0.265,-0.26,-0.255,-0.25,-0.245,-0.24,-0.235,-0.23,-0.225,-0.22,
-0.215,-0.21,-0.205,-0.2,-0.195,-0.19,-0.185,-0.18,-0.175,-0.17,-0.165,
-0.16,-0.155,-0.15,-0.145,-0.14,-0.135,-0.13,-0.125,-0.12,-0.115,-0.11,
-0.105,-0.1,-0.095,-0.09,-0.085,-0.08,-0.075,-0.07,-0.065,-0.06,-0.055,
-0.05,-0.045,-0.04,-0.035,-0.03,-0.025,-0.02,-0.015,-0.01,-0.005,0.),(0.,
1.2),.UNSPECIFIED.)
GEOMETRIC_REPRESENTATION_ITEM()
RATIONAL_B_SPLINE_SURFACE(((1.,1.),(1.,1.),(1.,1.),(1.,1.),(1.,1.),(1.,
1.),(1.,1.),(1.,1.),(1.,1.),(1.,1.),(1.,1.),(1.,1.),(1.,1.),(1.,1.),(1.,
1.),(1.,1.),(1.,1.),(1.,1.),(1.,1.),(1.,1.),(1.,1.),(1.,1.),(1.,1.),(1.,
1.),(1.,1.),(1.,1.),(1.,1.),(1.,1.),(1.,1.),(1.,1.),(1.,1.),(1.,1.),(1.,
1.),(1.,1.),(1.,1.),(1.,1.),(1.,1.),(1.,1.),(1.,1.),(1.,1.),(1.,1.),(1.,
1.),(1.,1.),(1.,1.),(1.,1.),(1.,1.),(1.,1.),(1.,1.),(1.,1.),(1.,1.),(1.,
1.),(1.,1.),(1.,1.),(1.,1.),(1.,1.),(1.,1.),(1.,1.),(1.,1.),(1.,1.),(1.,
1.),(1.,1.),(1.,1.),(1.,1.),(1.,1.),(1.,1.),(1.,1.),(1.,1.),(1.,1.),(1.,
1.),(1.,1.),(1.,1.),(1.,1.),(1.,1.),(1.,1.),(1.,1.),(1.,1.),(1.,1.),(1.,
1.),(1.,1.),(1.,1.),(1.,1.),(1.,1.),(1.,1.),(1.,1.),(1.,1.),(1.,1.),(1.,
1.),(1.,1.),(1.,1.),(1.,1.),(1.,1.),(1.,1.),(1.,1.),(1.,1.),(1.,1.),(1.,
1.),(1.,1.),(1.,1.),(1.,1.),(1.,1.),(1.,1.),(1.,1.),(1.,1.),(1.,1.),(1.,
1.),(1.,1.),(1.,1.),(1.,1.),(1.,1.),(1.,1.),(1.,1.),(1.,1.),(1.,1.),(1.,
1.),(1.,1.),(1.,1.),(1.,1.),(1.,1.),(1.,1.),(1.,1.),(1.,1.),(1.,1.),(1.,
1.),(1.,1.),(1.,1.),(1.,1.),(1.,1.),(1.,1.),(1.,1.),(1.,1.),(1.,1.),(1.,
1.),(1.,1.),(1.,1.),(1.,1.),(1.,1.),(1.,1.),(1.,1.),(1.,1.),(1.,1.),(1.,
1.),(1.,1.),(1.,1.),(1.,1.),(1.,1.),(1.,1.),(1.,1.),(1.,1.),(1.,1.),(1.,
1.),(1.,1.),(1.,1.),(1.,1.),(1.,1.),(1.,1.),(1.,1.),(1.,1.),(1.,1.),(1.,
1.),(1.,1.),(1.,1.),(1.,1.),(1.,1.),(1.,1.),(1.,1.),(1.,1.),(1.,1.),(1.,
1.),(1.,1.),(1.,1.),(1.,1.),(1.,1.),(1.,1.),(1.,1.),(1.,1.),(1.,1.),(1.,
1.),(1.,1.),(1.,1.),(1.,1.),(1.,1.),(1.,1.),(1.,1.),(1.,1.),(1.,1.),(1.,
1.),(1.,1.),(1.,1.),(1.,1.),(1.,1.),(1.,1.),(1.,1.),(1.,1.),(1.,1.),(1.,
1.),(1.,1.),(1.,1.),(1.,1.),(1.,1.),(1.,1.),(1.,1.),(1.,1.),(1.,1.),(1.,
1.),(1.,1.)))
REPRESENTATION_ITEM('')
SURFACE()
);
#1028=(
BOUNDED_SURFACE()
B_SPLINE_SURFACE(5,1,((#186222,#186223),(#186224,#186225),(#186226,#186227),
(#186228,#186229),(#186230,#186231),(#186232,#186233),(#186234,#186235),
(#186236,#186237),(#186238,#186239),(#186240,#186241),(#186242,#186243),
(#186244,#186245),(#186246,#186247),(#186248,#186249),(#186250,#186251),
(#186252,#186253),(#186254,#186255),(#186256,#186257),(#186258,#186259),
(#186260,#186261),(#186262,#186263),(#186264,#186265),(#186266,#186267),
(#186268,#186269),(#186270,#186271),(#186272,#186273),(#186274,#186275),
(#186276,#186277),(#186278,#186279),(#186280,#186281),(#186282,#186283),
(#186284,#186285),(#186286,#186287),(#186288,#186289),(#186290,#186291),
(#186292,#186293),(#186294,#186295),(#186296,#186297),(#186298,#186299),
(#186300,#186301),(#186302,#186303),(#186304,#186305),(#186306,#186307),
(#186308,#186309),(#186310,#186311),(#186312,#186313),(#186314,#186315),
(#186316,#186317),(#186318,#186319),(#186320,#186321),(#186322,#186323),
(#186324,#186325),(#186326,#186327),(#186328,#186329),(#186330,#186331),
(#186332,#186333),(#186334,#186335),(#186336,#186337),(#186338,#186339),
(#186340,#186341),(#186342,#186343),(#186344,#186345),(#186346,#186347),
(#186348,#186349),(#186350,#186351),(#186352,#186353),(#186354,#186355),
(#186356,#186357),(#186358,#186359),(#186360,#186361),(#186362,#186363),
(#186364,#186365),(#186366,#186367),(#186368,#186369),(#186370,#186371),
(#186372,#186373),(#186374,#186375),(#186376,#186377),(#186378,#186379),
(#186380,#186381),(#186382,#186383),(#186384,#186385),(#186386,#186387),
(#186388,#186389),(#186390,#186391),(#186392,#186393),(#186394,#186395),
(#186396,#186397),(#186398,#186399),(#186400,#186401),(#186402,#186403),
(#186404,#186405),(#186406,#186407),(#186408,#186409),(#186410,#186411),
(#186412,#186413),(#186414,#186415),(#186416,#186417),(#186418,#186419),
(#186420,#186421),(#186422,#186423),(#186424,#186425),(#186426,#186427),
(#186428,#186429),(#186430,#186431),(#186432,#186433),(#186434,#186435),
(#186436,#186437),(#186438,#186439),(#186440,#186441),(#186442,#186443),
(#186444,#186445),(#186446,#186447),(#186448,#186449),(#186450,#186451),
(#186452,#186453),(#186454,#186455),(#186456,#186457),(#186458,#186459),
(#186460,#186461),(#186462,#186463),(#186464,#186465),(#186466,#186467),
(#186468,#186469),(#186470,#186471),(#186472,#186473),(#186474,#186475),
(#186476,#186477),(#186478,#186479),(#186480,#186481),(#186482,#186483),
(#186484,#186485),(#186486,#186487),(#186488,#186489),(#186490,#186491),
(#186492,#186493),(#186494,#186495),(#186496,#186497),(#186498,#186499),
(#186500,#186501),(#186502,#186503),(#186504,#186505),(#186506,#186507),
(#186508,#186509),(#186510,#186511),(#186512,#186513),(#186514,#186515),
(#186516,#186517),(#186518,#186519),(#186520,#186521),(#186522,#186523),
(#186524,#186525),(#186526,#186527),(#186528,#186529),(#186530,#186531),
(#186532,#186533),(#186534,#186535),(#186536,#186537),(#186538,#186539),
(#186540,#186541),(#186542,#186543),(#186544,#186545),(#186546,#186547),
(#186548,#186549),(#186550,#186551),(#186552,#186553),(#186554,#186555),
(#186556,#186557),(#186558,#186559),(#186560,#186561),(#186562,#186563),
(#186564,#186565),(#186566,#186567),(#186568,#186569),(#186570,#186571),
(#186572,#186573),(#186574,#186575),(#186576,#186577),(#186578,#186579),
(#186580,#186581),(#186582,#186583),(#186584,#186585),(#186586,#186587),
(#186588,#186589),(#186590,#186591),(#186592,#186593),(#186594,#186595),
(#186596,#186597),(#186598,#186599),(#186600,#186601),(#186602,#186603),
(#186604,#186605),(#186606,#186607),(#186608,#186609),(#186610,#186611),
(#186612,#186613),(#186614,#186615),(#186616,#186617),(#186618,#186619),
(#186620,#186621),(#186622,#186623),(#186624,#186625),(#186626,#186627),
(#186628,#186629),(#186630,#186631)),.UNSPECIFIED.,.F.,.F.,.F.)
B_SPLINE_SURFACE_WITH_KNOTS((6,1,1,1,1,1,1,1,1,1,1,1,1,1,1,1,1,1,1,1,1,
1,1,1,1,1,1,1,1,1,1,1,1,1,1,1,1,1,1,1,1,1,1,1,1,1,1,1,1,1,1,1,1,1,1,1,1,
1,1,1,1,1,1,1,1,1,1,1,1,1,1,1,1,1,1,1,1,1,1,1,1,1,1,1,1,1,1,1,1,1,1,1,1,
1,1,1,1,1,1,1,1,1,1,1,1,1,1,1,1,1,1,1,1,1,1,1,1,1,1,1,1,1,1,1,1,1,1,1,1,
1,1,1,1,1,1,1,1,1,1,1,1,1,1,1,1,1,1,1,1,1,1,1,1,1,1,1,1,1,1,1,1,1,1,1,1,
1,1,1,1,1,1,1,1,1,1,1,1,1,1,1,1,1,1,1,1,1,1,1,1,1,1,1,1,1,1,1,1,1,1,1,6),
(2,2),(0.,0.005,0.01,0.015,0.02,0.025,0.03,0.035,0.04,0.045,0.05,0.055,
0.06,0.065,0.07,0.075,0.08,0.085,0.09,0.095,0.1,0.105,0.11,0.115,0.12,0.125,
0.13,0.135,0.14,0.145,0.15,0.155,0.16,0.165,0.17,0.175,0.18,0.185,0.19,
0.195,0.2,0.205,0.21,0.215,0.22,0.225,0.23,0.235,0.24,0.245,0.25,0.255,
0.26,0.265,0.27,0.275,0.28,0.285,0.29,0.295,0.3,0.305,0.31,0.315,0.32,0.325,
0.33,0.335,0.34,0.345,0.35,0.355,0.36,0.365,0.37,0.375,0.38,0.385,0.39,
0.395,0.4,0.405,0.41,0.415,0.42,0.425,0.43,0.435,0.44,0.445,0.45,0.455,
0.46,0.465,0.47,0.475,0.48,0.485,0.49,0.495,0.5,0.505,0.51,0.515,0.52,0.525,
0.53,0.535,0.54,0.545,0.55,0.555,0.56,0.565,0.57,0.575,0.58,0.585,0.59,
0.595,0.6,0.605,0.61,0.615,0.62,0.625,0.63,0.635,0.64,0.645,0.65,0.655,
0.66,0.665,0.67,0.675,0.68,0.685,0.690000000000001,0.695000000000001,0.700000000000001,
0.705000000000001,0.710000000000001,0.715000000000001,0.720000000000001,
0.725000000000001,0.730000000000001,0.735000000000001,0.740000000000001,
0.745000000000001,0.750000000000001,0.755000000000001,0.760000000000001,
0.765000000000001,0.770000000000001,0.775000000000001,0.780000000000001,
0.785000000000001,0.790000000000001,0.795000000000001,0.800000000000001,
0.805000000000001,0.810000000000001,0.815000000000001,0.820000000000001,
0.825000000000001,0.830000000000001,0.835000000000001,0.840000000000001,
0.845000000000001,0.850000000000001,0.855000000000001,0.860000000000001,
0.865000000000001,0.870000000000001,0.875000000000001,0.880000000000001,
0.885000000000001,0.890000000000001,0.895000000000001,0.900000000000001,
0.905000000000001,0.910000000000001,0.915000000000001,0.920000000000001,
0.925000000000001,0.930000000000001,0.935000000000001,0.940000000000001,
0.945000000000001,0.950000000000001,0.955000000000001,0.960000000000001,
0.965000000000001,0.970000000000001,0.975000000000001,0.980000000000001,
0.985000000000001,0.990000000000001,0.995000000000001,1.),(0.,1.2),
 .UNSPECIFIED.)
GEOMETRIC_REPRESENTATION_ITEM()
RATIONAL_B_SPLINE_SURFACE(((1.,1.),(1.,1.),(1.,1.),(1.,1.),(1.,1.),(1.,
1.),(1.,1.),(1.,1.),(1.,1.),(1.,1.),(1.,1.),(1.,1.),(1.,1.),(1.,1.),(1.,
1.),(1.,1.),(1.,1.),(1.,1.),(1.,1.),(1.,1.),(1.,1.),(1.,1.),(1.,1.),(1.,
1.),(1.,1.),(1.,1.),(1.,1.),(1.,1.),(1.,1.),(1.,1.),(1.,1.),(1.,1.),(1.,
1.),(1.,1.),(1.,1.),(1.,1.),(1.,1.),(1.,1.),(1.,1.),(1.,1.),(1.,1.),(1.,
1.),(1.,1.),(1.,1.),(1.,1.),(1.,1.),(1.,1.),(1.,1.),(1.,1.),(1.,1.),(1.,
1.),(1.,1.),(1.,1.),(1.,1.),(1.,1.),(1.,1.),(1.,1.),(1.,1.),(1.,1.),(1.,
1.),(1.,1.),(1.,1.),(1.,1.),(1.,1.),(1.,1.),(1.,1.),(1.,1.),(1.,1.),(1.,
1.),(1.,1.),(1.,1.),(1.,1.),(1.,1.),(1.,1.),(1.,1.),(1.,1.),(1.,1.),(1.,
1.),(1.,1.),(1.,1.),(1.,1.),(1.,1.),(1.,1.),(1.,1.),(1.,1.),(1.,1.),(1.,
1.),(1.,1.),(1.,1.),(1.,1.),(1.,1.),(1.,1.),(1.,1.),(1.,1.),(1.,1.),(1.,
1.),(1.,1.),(1.,1.),(1.,1.),(1.,1.),(1.,1.),(1.,1.),(1.,1.),(1.,1.),(1.,
1.),(1.,1.),(1.,1.),(1.,1.),(1.,1.),(1.,1.),(1.,1.),(1.,1.),(1.,1.),(1.,
1.),(1.,1.),(1.,1.),(1.,1.),(1.,1.),(1.,1.),(1.,1.),(1.,1.),(1.,1.),(1.,
1.),(1.,1.),(1.,1.),(1.,1.),(1.,1.),(1.,1.),(1.,1.),(1.,1.),(1.,1.),(1.,
1.),(1.,1.),(1.,1.),(1.,1.),(1.,1.),(1.,1.),(1.,1.),(1.,1.),(1.,1.),(1.,
1.),(1.,1.),(1.,1.),(1.,1.),(1.,1.),(1.,1.),(1.,1.),(1.,1.),(1.,1.),(1.,
1.),(1.,1.),(1.,1.),(1.,1.),(1.,1.),(1.,1.),(1.,1.),(1.,1.),(1.,1.),(1.,
1.),(1.,1.),(1.,1.),(1.,1.),(1.,1.),(1.,1.),(1.,1.),(1.,1.),(1.,1.),(1.,
1.),(1.,1.),(1.,1.),(1.,1.),(1.,1.),(1.,1.),(1.,1.),(1.,1.),(1.,1.),(1.,
1.),(1.,1.),(1.,1.),(1.,1.),(1.,1.),(1.,1.),(1.,1.),(1.,1.),(1.,1.),(1.,
1.),(1.,1.),(1.,1.),(1.,1.),(1.,1.),(1.,1.),(1.,1.),(1.,1.),(1.,1.),(1.,
1.),(1.,1.),(1.,1.),(1.,1.),(1.,1.),(1.,1.),(1.,1.),(1.,1.),(1.,1.),(1.,
1.),(1.,1.)))
REPRESENTATION_ITEM('')
SURFACE()
);
#1029=(
BOUNDED_SURFACE()
B_SPLINE_SURFACE(5,1,((#186843,#186844),(#186845,#186846),(#186847,#186848),
(#186849,#186850),(#186851,#186852),(#186853,#186854),(#186855,#186856),
(#186857,#186858),(#186859,#186860),(#186861,#186862),(#186863,#186864),
(#186865,#186866),(#186867,#186868),(#186869,#186870),(#186871,#186872),
(#186873,#186874),(#186875,#186876),(#186877,#186878),(#186879,#186880),
(#186881,#186882),(#186883,#186884),(#186885,#186886),(#186887,#186888),
(#186889,#186890),(#186891,#186892),(#186893,#186894),(#186895,#186896),
(#186897,#186898),(#186899,#186900),(#186901,#186902),(#186903,#186904),
(#186905,#186906),(#186907,#186908),(#186909,#186910),(#186911,#186912),
(#186913,#186914),(#186915,#186916),(#186917,#186918),(#186919,#186920),
(#186921,#186922),(#186923,#186924),(#186925,#186926),(#186927,#186928),
(#186929,#186930),(#186931,#186932),(#186933,#186934),(#186935,#186936),
(#186937,#186938),(#186939,#186940),(#186941,#186942),(#186943,#186944),
(#186945,#186946),(#186947,#186948),(#186949,#186950),(#186951,#186952),
(#186953,#186954),(#186955,#186956),(#186957,#186958),(#186959,#186960),
(#186961,#186962),(#186963,#186964),(#186965,#186966),(#186967,#186968),
(#186969,#186970),(#186971,#186972),(#186973,#186974),(#186975,#186976),
(#186977,#186978),(#186979,#186980),(#186981,#186982),(#186983,#186984),
(#186985,#186986),(#186987,#186988),(#186989,#186990),(#186991,#186992),
(#186993,#186994),(#186995,#186996),(#186997,#186998),(#186999,#187000),
(#187001,#187002),(#187003,#187004),(#187005,#187006),(#187007,#187008),
(#187009,#187010),(#187011,#187012),(#187013,#187014),(#187015,#187016),
(#187017,#187018),(#187019,#187020),(#187021,#187022),(#187023,#187024),
(#187025,#187026),(#187027,#187028),(#187029,#187030),(#187031,#187032),
(#187033,#187034),(#187035,#187036),(#187037,#187038),(#187039,#187040),
(#187041,#187042),(#187043,#187044),(#187045,#187046),(#187047,#187048),
(#187049,#187050),(#187051,#187052),(#187053,#187054),(#187055,#187056),
(#187057,#187058),(#187059,#187060),(#187061,#187062),(#187063,#187064),
(#187065,#187066),(#187067,#187068),(#187069,#187070),(#187071,#187072),
(#187073,#187074),(#187075,#187076),(#187077,#187078),(#187079,#187080),
(#187081,#187082),(#187083,#187084),(#187085,#187086),(#187087,#187088),
(#187089,#187090),(#187091,#187092),(#187093,#187094),(#187095,#187096),
(#187097,#187098),(#187099,#187100),(#187101,#187102),(#187103,#187104),
(#187105,#187106),(#187107,#187108),(#187109,#187110),(#187111,#187112),
(#187113,#187114),(#187115,#187116),(#187117,#187118),(#187119,#187120),
(#187121,#187122),(#187123,#187124),(#187125,#187126),(#187127,#187128),
(#187129,#187130),(#187131,#187132),(#187133,#187134),(#187135,#187136),
(#187137,#187138),(#187139,#187140),(#187141,#187142),(#187143,#187144),
(#187145,#187146),(#187147,#187148),(#187149,#187150),(#187151,#187152),
(#187153,#187154),(#187155,#187156),(#187157,#187158),(#187159,#187160),
(#187161,#187162),(#187163,#187164),(#187165,#187166),(#187167,#187168),
(#187169,#187170),(#187171,#187172),(#187173,#187174),(#187175,#187176),
(#187177,#187178),(#187179,#187180),(#187181,#187182),(#187183,#187184),
(#187185,#187186),(#187187,#187188),(#187189,#187190),(#187191,#187192),
(#187193,#187194),(#187195,#187196),(#187197,#187198),(#187199,#187200),
(#187201,#187202),(#187203,#187204),(#187205,#187206),(#187207,#187208),
(#187209,#187210),(#187211,#187212),(#187213,#187214),(#187215,#187216),
(#187217,#187218),(#187219,#187220),(#187221,#187222),(#187223,#187224),
(#187225,#187226),(#187227,#187228),(#187229,#187230),(#187231,#187232),
(#187233,#187234),(#187235,#187236),(#187237,#187238),(#187239,#187240),
(#187241,#187242),(#187243,#187244),(#187245,#187246),(#187247,#187248),
(#187249,#187250),(#187251,#187252)),.UNSPECIFIED.,.F.,.F.,.F.)
B_SPLINE_SURFACE_WITH_KNOTS((6,1,1,1,1,1,1,1,1,1,1,1,1,1,1,1,1,1,1,1,1,
1,1,1,1,1,1,1,1,1,1,1,1,1,1,1,1,1,1,1,1,1,1,1,1,1,1,1,1,1,1,1,1,1,1,1,1,
1,1,1,1,1,1,1,1,1,1,1,1,1,1,1,1,1,1,1,1,1,1,1,1,1,1,1,1,1,1,1,1,1,1,1,1,
1,1,1,1,1,1,1,1,1,1,1,1,1,1,1,1,1,1,1,1,1,1,1,1,1,1,1,1,1,1,1,1,1,1,1,1,
1,1,1,1,1,1,1,1,1,1,1,1,1,1,1,1,1,1,1,1,1,1,1,1,1,1,1,1,1,1,1,1,1,1,1,1,
1,1,1,1,1,1,1,1,1,1,1,1,1,1,1,1,1,1,1,1,1,1,1,1,1,1,1,1,1,1,1,1,1,1,1,6),
(2,2),(-1.,-0.995000000000001,-0.990000000000001,-0.985000000000001,-0.980000000000001,
-0.975000000000001,-0.970000000000001,-0.965000000000001,-0.960000000000001,
-0.955000000000001,-0.950000000000001,-0.945000000000001,-0.940000000000001,
-0.935000000000001,-0.930000000000001,-0.925000000000001,-0.920000000000001,
-0.915000000000001,-0.910000000000001,-0.905000000000001,-0.900000000000001,
-0.895000000000001,-0.890000000000001,-0.885000000000001,-0.880000000000001,
-0.875000000000001,-0.870000000000001,-0.865000000000001,-0.860000000000001,
-0.855000000000001,-0.850000000000001,-0.845000000000001,-0.840000000000001,
-0.835000000000001,-0.830000000000001,-0.825000000000001,-0.820000000000001,
-0.815000000000001,-0.810000000000001,-0.805000000000001,-0.800000000000001,
-0.795000000000001,-0.790000000000001,-0.785000000000001,-0.780000000000001,
-0.775000000000001,-0.770000000000001,-0.765000000000001,-0.760000000000001,
-0.755000000000001,-0.750000000000001,-0.745000000000001,-0.740000000000001,
-0.735000000000001,-0.730000000000001,-0.725000000000001,-0.720000000000001,
-0.715000000000001,-0.710000000000001,-0.705000000000001,-0.700000000000001,
-0.695000000000001,-0.690000000000001,-0.685,-0.68,-0.675,-0.67,-0.665,
-0.66,-0.655,-0.65,-0.645,-0.64,-0.635,-0.63,-0.625,-0.62,-0.615,-0.61,
-0.605,-0.6,-0.595,-0.59,-0.585,-0.58,-0.575,-0.57,-0.565,-0.56,-0.555,
-0.55,-0.545,-0.54,-0.535,-0.53,-0.525,-0.52,-0.515,-0.51,-0.505,-0.5,-0.495,
-0.49,-0.485,-0.48,-0.475,-0.47,-0.465,-0.46,-0.455,-0.45,-0.445,-0.44,
-0.435,-0.43,-0.425,-0.42,-0.415,-0.41,-0.405,-0.4,-0.395,-0.39,-0.385,
-0.38,-0.375,-0.37,-0.365,-0.36,-0.355,-0.35,-0.345,-0.34,-0.335,-0.33,
-0.325,-0.32,-0.315,-0.31,-0.305,-0.3,-0.295,-0.29,-0.285,-0.28,-0.275,
-0.27,-0.265,-0.26,-0.255,-0.25,-0.245,-0.24,-0.235,-0.23,-0.225,-0.22,
-0.215,-0.21,-0.205,-0.2,-0.195,-0.19,-0.185,-0.18,-0.175,-0.17,-0.165,
-0.16,-0.155,-0.15,-0.145,-0.14,-0.135,-0.13,-0.125,-0.12,-0.115,-0.11,
-0.105,-0.1,-0.095,-0.09,-0.085,-0.08,-0.075,-0.07,-0.065,-0.06,-0.055,
-0.05,-0.045,-0.04,-0.035,-0.03,-0.025,-0.02,-0.015,-0.01,-0.005,0.),(0.,
1.2),.UNSPECIFIED.)
GEOMETRIC_REPRESENTATION_ITEM()
RATIONAL_B_SPLINE_SURFACE(((1.,1.),(1.,1.),(1.,1.),(1.,1.),(1.,1.),(1.,
1.),(1.,1.),(1.,1.),(1.,1.),(1.,1.),(1.,1.),(1.,1.),(1.,1.),(1.,1.),(1.,
1.),(1.,1.),(1.,1.),(1.,1.),(1.,1.),(1.,1.),(1.,1.),(1.,1.),(1.,1.),(1.,
1.),(1.,1.),(1.,1.),(1.,1.),(1.,1.),(1.,1.),(1.,1.),(1.,1.),(1.,1.),(1.,
1.),(1.,1.),(1.,1.),(1.,1.),(1.,1.),(1.,1.),(1.,1.),(1.,1.),(1.,1.),(1.,
1.),(1.,1.),(1.,1.),(1.,1.),(1.,1.),(1.,1.),(1.,1.),(1.,1.),(1.,1.),(1.,
1.),(1.,1.),(1.,1.),(1.,1.),(1.,1.),(1.,1.),(1.,1.),(1.,1.),(1.,1.),(1.,
1.),(1.,1.),(1.,1.),(1.,1.),(1.,1.),(1.,1.),(1.,1.),(1.,1.),(1.,1.),(1.,
1.),(1.,1.),(1.,1.),(1.,1.),(1.,1.),(1.,1.),(1.,1.),(1.,1.),(1.,1.),(1.,
1.),(1.,1.),(1.,1.),(1.,1.),(1.,1.),(1.,1.),(1.,1.),(1.,1.),(1.,1.),(1.,
1.),(1.,1.),(1.,1.),(1.,1.),(1.,1.),(1.,1.),(1.,1.),(1.,1.),(1.,1.),(1.,
1.),(1.,1.),(1.,1.),(1.,1.),(1.,1.),(1.,1.),(1.,1.),(1.,1.),(1.,1.),(1.,
1.),(1.,1.),(1.,1.),(1.,1.),(1.,1.),(1.,1.),(1.,1.),(1.,1.),(1.,1.),(1.,
1.),(1.,1.),(1.,1.),(1.,1.),(1.,1.),(1.,1.),(1.,1.),(1.,1.),(1.,1.),(1.,
1.),(1.,1.),(1.,1.),(1.,1.),(1.,1.),(1.,1.),(1.,1.),(1.,1.),(1.,1.),(1.,
1.),(1.,1.),(1.,1.),(1.,1.),(1.,1.),(1.,1.),(1.,1.),(1.,1.),(1.,1.),(1.,
1.),(1.,1.),(1.,1.),(1.,1.),(1.,1.),(1.,1.),(1.,1.),(1.,1.),(1.,1.),(1.,
1.),(1.,1.),(1.,1.),(1.,1.),(1.,1.),(1.,1.),(1.,1.),(1.,1.),(1.,1.),(1.,
1.),(1.,1.),(1.,1.),(1.,1.),(1.,1.),(1.,1.),(1.,1.),(1.,1.),(1.,1.),(1.,
1.),(1.,1.),(1.,1.),(1.,1.),(1.,1.),(1.,1.),(1.,1.),(1.,1.),(1.,1.),(1.,
1.),(1.,1.),(1.,1.),(1.,1.),(1.,1.),(1.,1.),(1.,1.),(1.,1.),(1.,1.),(1.,
1.),(1.,1.),(1.,1.),(1.,1.),(1.,1.),(1.,1.),(1.,1.),(1.,1.),(1.,1.),(1.,
1.),(1.,1.),(1.,1.),(1.,1.),(1.,1.),(1.,1.),(1.,1.),(1.,1.),(1.,1.),(1.,
1.),(1.,1.)))
REPRESENTATION_ITEM('')
SURFACE()
);
#1030=(
BOUNDED_SURFACE()
B_SPLINE_SURFACE(5,1,((#187460,#187461),(#187462,#187463),(#187464,#187465),
(#187466,#187467),(#187468,#187469),(#187470,#187471),(#187472,#187473),
(#187474,#187475),(#187476,#187477),(#187478,#187479),(#187480,#187481),
(#187482,#187483),(#187484,#187485),(#187486,#187487),(#187488,#187489),
(#187490,#187491),(#187492,#187493),(#187494,#187495),(#187496,#187497),
(#187498,#187499),(#187500,#187501),(#187502,#187503),(#187504,#187505),
(#187506,#187507),(#187508,#187509),(#187510,#187511),(#187512,#187513),
(#187514,#187515),(#187516,#187517),(#187518,#187519),(#187520,#187521),
(#187522,#187523),(#187524,#187525),(#187526,#187527),(#187528,#187529),
(#187530,#187531),(#187532,#187533),(#187534,#187535),(#187536,#187537),
(#187538,#187539),(#187540,#187541),(#187542,#187543),(#187544,#187545),
(#187546,#187547),(#187548,#187549),(#187550,#187551),(#187552,#187553),
(#187554,#187555),(#187556,#187557),(#187558,#187559),(#187560,#187561),
(#187562,#187563),(#187564,#187565),(#187566,#187567),(#187568,#187569),
(#187570,#187571),(#187572,#187573),(#187574,#187575),(#187576,#187577),
(#187578,#187579),(#187580,#187581),(#187582,#187583),(#187584,#187585),
(#187586,#187587),(#187588,#187589),(#187590,#187591),(#187592,#187593),
(#187594,#187595),(#187596,#187597),(#187598,#187599),(#187600,#187601),
(#187602,#187603),(#187604,#187605),(#187606,#187607),(#187608,#187609),
(#187610,#187611),(#187612,#187613),(#187614,#187615),(#187616,#187617),
(#187618,#187619),(#187620,#187621),(#187622,#187623),(#187624,#187625),
(#187626,#187627),(#187628,#187629),(#187630,#187631),(#187632,#187633),
(#187634,#187635),(#187636,#187637),(#187638,#187639),(#187640,#187641),
(#187642,#187643),(#187644,#187645),(#187646,#187647),(#187648,#187649),
(#187650,#187651),(#187652,#187653),(#187654,#187655),(#187656,#187657),
(#187658,#187659),(#187660,#187661),(#187662,#187663),(#187664,#187665),
(#187666,#187667),(#187668,#187669),(#187670,#187671),(#187672,#187673),
(#187674,#187675),(#187676,#187677),(#187678,#187679),(#187680,#187681),
(#187682,#187683),(#187684,#187685),(#187686,#187687),(#187688,#187689),
(#187690,#187691),(#187692,#187693),(#187694,#187695),(#187696,#187697),
(#187698,#187699),(#187700,#187701),(#187702,#187703),(#187704,#187705),
(#187706,#187707),(#187708,#187709),(#187710,#187711),(#187712,#187713),
(#187714,#187715),(#187716,#187717),(#187718,#187719),(#187720,#187721),
(#187722,#187723),(#187724,#187725),(#187726,#187727),(#187728,#187729),
(#187730,#187731),(#187732,#187733),(#187734,#187735),(#187736,#187737),
(#187738,#187739),(#187740,#187741),(#187742,#187743),(#187744,#187745),
(#187746,#187747),(#187748,#187749),(#187750,#187751),(#187752,#187753),
(#187754,#187755),(#187756,#187757),(#187758,#187759),(#187760,#187761),
(#187762,#187763),(#187764,#187765),(#187766,#187767),(#187768,#187769),
(#187770,#187771),(#187772,#187773),(#187774,#187775),(#187776,#187777),
(#187778,#187779),(#187780,#187781),(#187782,#187783),(#187784,#187785),
(#187786,#187787),(#187788,#187789),(#187790,#187791),(#187792,#187793),
(#187794,#187795),(#187796,#187797),(#187798,#187799),(#187800,#187801),
(#187802,#187803),(#187804,#187805),(#187806,#187807),(#187808,#187809),
(#187810,#187811),(#187812,#187813),(#187814,#187815),(#187816,#187817),
(#187818,#187819),(#187820,#187821),(#187822,#187823),(#187824,#187825),
(#187826,#187827),(#187828,#187829),(#187830,#187831),(#187832,#187833),
(#187834,#187835),(#187836,#187837),(#187838,#187839),(#187840,#187841),
(#187842,#187843),(#187844,#187845),(#187846,#187847),(#187848,#187849),
(#187850,#187851),(#187852,#187853),(#187854,#187855),(#187856,#187857),
(#187858,#187859),(#187860,#187861),(#187862,#187863),(#187864,#187865),
(#187866,#187867),(#187868,#187869)),.UNSPECIFIED.,.F.,.F.,.F.)
B_SPLINE_SURFACE_WITH_KNOTS((6,1,1,1,1,1,1,1,1,1,1,1,1,1,1,1,1,1,1,1,1,
1,1,1,1,1,1,1,1,1,1,1,1,1,1,1,1,1,1,1,1,1,1,1,1,1,1,1,1,1,1,1,1,1,1,1,1,
1,1,1,1,1,1,1,1,1,1,1,1,1,1,1,1,1,1,1,1,1,1,1,1,1,1,1,1,1,1,1,1,1,1,1,1,
1,1,1,1,1,1,1,1,1,1,1,1,1,1,1,1,1,1,1,1,1,1,1,1,1,1,1,1,1,1,1,1,1,1,1,1,
1,1,1,1,1,1,1,1,1,1,1,1,1,1,1,1,1,1,1,1,1,1,1,1,1,1,1,1,1,1,1,1,1,1,1,1,
1,1,1,1,1,1,1,1,1,1,1,1,1,1,1,1,1,1,1,1,1,1,1,1,1,1,1,1,1,1,1,1,1,1,1,6),
(2,2),(0.,0.005,0.01,0.015,0.02,0.025,0.03,0.035,0.04,0.045,0.05,0.055,
0.06,0.065,0.07,0.075,0.08,0.085,0.09,0.095,0.1,0.105,0.11,0.115,0.12,0.125,
0.13,0.135,0.14,0.145,0.15,0.155,0.16,0.165,0.17,0.175,0.18,0.185,0.19,
0.195,0.2,0.205,0.21,0.215,0.22,0.225,0.23,0.235,0.24,0.245,0.25,0.255,
0.26,0.265,0.27,0.275,0.28,0.285,0.29,0.295,0.3,0.305,0.31,0.315,0.32,0.325,
0.33,0.335,0.34,0.345,0.35,0.355,0.36,0.365,0.37,0.375,0.38,0.385,0.39,
0.395,0.4,0.405,0.41,0.415,0.42,0.425,0.43,0.435,0.44,0.445,0.45,0.455,
0.46,0.465,0.47,0.475,0.48,0.485,0.49,0.495,0.5,0.505,0.51,0.515,0.52,0.525,
0.53,0.535,0.54,0.545,0.55,0.555,0.56,0.565,0.57,0.575,0.58,0.585,0.59,
0.595,0.6,0.605,0.61,0.615,0.62,0.625,0.63,0.635,0.64,0.645,0.65,0.655,
0.66,0.665,0.67,0.675,0.68,0.685,0.690000000000001,0.695000000000001,0.700000000000001,
0.705000000000001,0.710000000000001,0.715000000000001,0.720000000000001,
0.725000000000001,0.730000000000001,0.735000000000001,0.740000000000001,
0.745000000000001,0.750000000000001,0.755000000000001,0.760000000000001,
0.765000000000001,0.770000000000001,0.775000000000001,0.780000000000001,
0.785000000000001,0.790000000000001,0.795000000000001,0.800000000000001,
0.805000000000001,0.810000000000001,0.815000000000001,0.820000000000001,
0.825000000000001,0.830000000000001,0.835000000000001,0.840000000000001,
0.845000000000001,0.850000000000001,0.855000000000001,0.860000000000001,
0.865000000000001,0.870000000000001,0.875000000000001,0.880000000000001,
0.885000000000001,0.890000000000001,0.895000000000001,0.900000000000001,
0.905000000000001,0.910000000000001,0.915000000000001,0.920000000000001,
0.925000000000001,0.930000000000001,0.935000000000001,0.940000000000001,
0.945000000000001,0.950000000000001,0.955000000000001,0.960000000000001,
0.965000000000001,0.970000000000001,0.975000000000001,0.980000000000001,
0.985000000000001,0.990000000000001,0.995000000000001,1.),(0.,1.2),
 .UNSPECIFIED.)
GEOMETRIC_REPRESENTATION_ITEM()
RATIONAL_B_SPLINE_SURFACE(((1.,1.),(1.,1.),(1.,1.),(1.,1.),(1.,1.),(1.,
1.),(1.,1.),(1.,1.),(1.,1.),(1.,1.),(1.,1.),(1.,1.),(1.,1.),(1.,1.),(1.,
1.),(1.,1.),(1.,1.),(1.,1.),(1.,1.),(1.,1.),(1.,1.),(1.,1.),(1.,1.),(1.,
1.),(1.,1.),(1.,1.),(1.,1.),(1.,1.),(1.,1.),(1.,1.),(1.,1.),(1.,1.),(1.,
1.),(1.,1.),(1.,1.),(1.,1.),(1.,1.),(1.,1.),(1.,1.),(1.,1.),(1.,1.),(1.,
1.),(1.,1.),(1.,1.),(1.,1.),(1.,1.),(1.,1.),(1.,1.),(1.,1.),(1.,1.),(1.,
1.),(1.,1.),(1.,1.),(1.,1.),(1.,1.),(1.,1.),(1.,1.),(1.,1.),(1.,1.),(1.,
1.),(1.,1.),(1.,1.),(1.,1.),(1.,1.),(1.,1.),(1.,1.),(1.,1.),(1.,1.),(1.,
1.),(1.,1.),(1.,1.),(1.,1.),(1.,1.),(1.,1.),(1.,1.),(1.,1.),(1.,1.),(1.,
1.),(1.,1.),(1.,1.),(1.,1.),(1.,1.),(1.,1.),(1.,1.),(1.,1.),(1.,1.),(1.,
1.),(1.,1.),(1.,1.),(1.,1.),(1.,1.),(1.,1.),(1.,1.),(1.,1.),(1.,1.),(1.,
1.),(1.,1.),(1.,1.),(1.,1.),(1.,1.),(1.,1.),(1.,1.),(1.,1.),(1.,1.),(1.,
1.),(1.,1.),(1.,1.),(1.,1.),(1.,1.),(1.,1.),(1.,1.),(1.,1.),(1.,1.),(1.,
1.),(1.,1.),(1.,1.),(1.,1.),(1.,1.),(1.,1.),(1.,1.),(1.,1.),(1.,1.),(1.,
1.),(1.,1.),(1.,1.),(1.,1.),(1.,1.),(1.,1.),(1.,1.),(1.,1.),(1.,1.),(1.,
1.),(1.,1.),(1.,1.),(1.,1.),(1.,1.),(1.,1.),(1.,1.),(1.,1.),(1.,1.),(1.,
1.),(1.,1.),(1.,1.),(1.,1.),(1.,1.),(1.,1.),(1.,1.),(1.,1.),(1.,1.),(1.,
1.),(1.,1.),(1.,1.),(1.,1.),(1.,1.),(1.,1.),(1.,1.),(1.,1.),(1.,1.),(1.,
1.),(1.,1.),(1.,1.),(1.,1.),(1.,1.),(1.,1.),(1.,1.),(1.,1.),(1.,1.),(1.,
1.),(1.,1.),(1.,1.),(1.,1.),(1.,1.),(1.,1.),(1.,1.),(1.,1.),(1.,1.),(1.,
1.),(1.,1.),(1.,1.),(1.,1.),(1.,1.),(1.,1.),(1.,1.),(1.,1.),(1.,1.),(1.,
1.),(1.,1.),(1.,1.),(1.,1.),(1.,1.),(1.,1.),(1.,1.),(1.,1.),(1.,1.),(1.,
1.),(1.,1.),(1.,1.),(1.,1.),(1.,1.),(1.,1.),(1.,1.),(1.,1.),(1.,1.),(1.,
1.),(1.,1.)))
REPRESENTATION_ITEM('')
SURFACE()
);
#1031=(
BOUNDED_SURFACE()
B_SPLINE_SURFACE(5,1,((#188081,#188082),(#188083,#188084),(#188085,#188086),
(#188087,#188088),(#188089,#188090),(#188091,#188092),(#188093,#188094),
(#188095,#188096),(#188097,#188098),(#188099,#188100),(#188101,#188102),
(#188103,#188104),(#188105,#188106),(#188107,#188108),(#188109,#188110),
(#188111,#188112),(#188113,#188114),(#188115,#188116),(#188117,#188118),
(#188119,#188120),(#188121,#188122),(#188123,#188124),(#188125,#188126),
(#188127,#188128),(#188129,#188130),(#188131,#188132),(#188133,#188134),
(#188135,#188136),(#188137,#188138),(#188139,#188140),(#188141,#188142),
(#188143,#188144),(#188145,#188146),(#188147,#188148),(#188149,#188150),
(#188151,#188152),(#188153,#188154),(#188155,#188156),(#188157,#188158),
(#188159,#188160),(#188161,#188162),(#188163,#188164),(#188165,#188166),
(#188167,#188168),(#188169,#188170),(#188171,#188172),(#188173,#188174),
(#188175,#188176),(#188177,#188178),(#188179,#188180),(#188181,#188182),
(#188183,#188184),(#188185,#188186),(#188187,#188188),(#188189,#188190),
(#188191,#188192),(#188193,#188194),(#188195,#188196),(#188197,#188198),
(#188199,#188200),(#188201,#188202),(#188203,#188204),(#188205,#188206),
(#188207,#188208),(#188209,#188210),(#188211,#188212),(#188213,#188214),
(#188215,#188216),(#188217,#188218),(#188219,#188220),(#188221,#188222),
(#188223,#188224),(#188225,#188226),(#188227,#188228),(#188229,#188230),
(#188231,#188232),(#188233,#188234),(#188235,#188236),(#188237,#188238),
(#188239,#188240),(#188241,#188242),(#188243,#188244),(#188245,#188246),
(#188247,#188248),(#188249,#188250),(#188251,#188252),(#188253,#188254),
(#188255,#188256),(#188257,#188258),(#188259,#188260),(#188261,#188262),
(#188263,#188264),(#188265,#188266),(#188267,#188268),(#188269,#188270),
(#188271,#188272),(#188273,#188274),(#188275,#188276),(#188277,#188278),
(#188279,#188280),(#188281,#188282),(#188283,#188284),(#188285,#188286),
(#188287,#188288),(#188289,#188290),(#188291,#188292),(#188293,#188294),
(#188295,#188296),(#188297,#188298),(#188299,#188300),(#188301,#188302),
(#188303,#188304),(#188305,#188306),(#188307,#188308),(#188309,#188310),
(#188311,#188312),(#188313,#188314),(#188315,#188316),(#188317,#188318),
(#188319,#188320),(#188321,#188322),(#188323,#188324),(#188325,#188326),
(#188327,#188328),(#188329,#188330),(#188331,#188332),(#188333,#188334),
(#188335,#188336),(#188337,#188338),(#188339,#188340),(#188341,#188342),
(#188343,#188344),(#188345,#188346),(#188347,#188348),(#188349,#188350),
(#188351,#188352),(#188353,#188354),(#188355,#188356),(#188357,#188358),
(#188359,#188360),(#188361,#188362),(#188363,#188364),(#188365,#188366),
(#188367,#188368),(#188369,#188370),(#188371,#188372),(#188373,#188374),
(#188375,#188376),(#188377,#188378),(#188379,#188380),(#188381,#188382),
(#188383,#188384),(#188385,#188386),(#188387,#188388),(#188389,#188390),
(#188391,#188392),(#188393,#188394),(#188395,#188396),(#188397,#188398),
(#188399,#188400),(#188401,#188402),(#188403,#188404),(#188405,#188406),
(#188407,#188408),(#188409,#188410),(#188411,#188412),(#188413,#188414),
(#188415,#188416),(#188417,#188418),(#188419,#188420),(#188421,#188422),
(#188423,#188424),(#188425,#188426),(#188427,#188428),(#188429,#188430),
(#188431,#188432),(#188433,#188434),(#188435,#188436),(#188437,#188438),
(#188439,#188440),(#188441,#188442),(#188443,#188444),(#188445,#188446),
(#188447,#188448),(#188449,#188450),(#188451,#188452),(#188453,#188454),
(#188455,#188456),(#188457,#188458),(#188459,#188460),(#188461,#188462),
(#188463,#188464),(#188465,#188466),(#188467,#188468),(#188469,#188470),
(#188471,#188472),(#188473,#188474),(#188475,#188476),(#188477,#188478),
(#188479,#188480),(#188481,#188482),(#188483,#188484),(#188485,#188486),
(#188487,#188488),(#188489,#188490)),.UNSPECIFIED.,.F.,.F.,.F.)
B_SPLINE_SURFACE_WITH_KNOTS((6,1,1,1,1,1,1,1,1,1,1,1,1,1,1,1,1,1,1,1,1,
1,1,1,1,1,1,1,1,1,1,1,1,1,1,1,1,1,1,1,1,1,1,1,1,1,1,1,1,1,1,1,1,1,1,1,1,
1,1,1,1,1,1,1,1,1,1,1,1,1,1,1,1,1,1,1,1,1,1,1,1,1,1,1,1,1,1,1,1,1,1,1,1,
1,1,1,1,1,1,1,1,1,1,1,1,1,1,1,1,1,1,1,1,1,1,1,1,1,1,1,1,1,1,1,1,1,1,1,1,
1,1,1,1,1,1,1,1,1,1,1,1,1,1,1,1,1,1,1,1,1,1,1,1,1,1,1,1,1,1,1,1,1,1,1,1,
1,1,1,1,1,1,1,1,1,1,1,1,1,1,1,1,1,1,1,1,1,1,1,1,1,1,1,1,1,1,1,1,1,1,1,6),
(2,2),(-1.,-0.995000000000001,-0.990000000000001,-0.985000000000001,-0.980000000000001,
-0.975000000000001,-0.970000000000001,-0.965000000000001,-0.960000000000001,
-0.955000000000001,-0.950000000000001,-0.945000000000001,-0.940000000000001,
-0.935000000000001,-0.930000000000001,-0.925000000000001,-0.920000000000001,
-0.915000000000001,-0.910000000000001,-0.905000000000001,-0.900000000000001,
-0.895000000000001,-0.890000000000001,-0.885000000000001,-0.880000000000001,
-0.875000000000001,-0.870000000000001,-0.865000000000001,-0.860000000000001,
-0.855000000000001,-0.850000000000001,-0.845000000000001,-0.840000000000001,
-0.835000000000001,-0.830000000000001,-0.825000000000001,-0.820000000000001,
-0.815000000000001,-0.810000000000001,-0.805000000000001,-0.800000000000001,
-0.795000000000001,-0.790000000000001,-0.785000000000001,-0.780000000000001,
-0.775000000000001,-0.770000000000001,-0.765000000000001,-0.760000000000001,
-0.755000000000001,-0.750000000000001,-0.745000000000001,-0.740000000000001,
-0.735000000000001,-0.730000000000001,-0.725000000000001,-0.720000000000001,
-0.715000000000001,-0.710000000000001,-0.705000000000001,-0.700000000000001,
-0.695000000000001,-0.690000000000001,-0.685,-0.68,-0.675,-0.67,-0.665,
-0.66,-0.655,-0.65,-0.645,-0.64,-0.635,-0.63,-0.625,-0.62,-0.615,-0.61,
-0.605,-0.6,-0.595,-0.59,-0.585,-0.58,-0.575,-0.57,-0.565,-0.56,-0.555,
-0.55,-0.545,-0.54,-0.535,-0.53,-0.525,-0.52,-0.515,-0.51,-0.505,-0.5,-0.495,
-0.49,-0.485,-0.48,-0.475,-0.47,-0.465,-0.46,-0.455,-0.45,-0.445,-0.44,
-0.435,-0.43,-0.425,-0.42,-0.415,-0.41,-0.405,-0.4,-0.395,-0.39,-0.385,
-0.38,-0.375,-0.37,-0.365,-0.36,-0.355,-0.35,-0.345,-0.34,-0.335,-0.33,
-0.325,-0.32,-0.315,-0.31,-0.305,-0.3,-0.295,-0.29,-0.285,-0.28,-0.275,
-0.27,-0.265,-0.26,-0.255,-0.25,-0.245,-0.24,-0.235,-0.23,-0.225,-0.22,
-0.215,-0.21,-0.205,-0.2,-0.195,-0.19,-0.185,-0.18,-0.175,-0.17,-0.165,
-0.16,-0.155,-0.15,-0.145,-0.14,-0.135,-0.13,-0.125,-0.12,-0.115,-0.11,
-0.105,-0.1,-0.095,-0.09,-0.085,-0.08,-0.075,-0.07,-0.065,-0.06,-0.055,
-0.05,-0.045,-0.04,-0.035,-0.03,-0.025,-0.02,-0.015,-0.01,-0.005,0.),(0.,
1.2),.UNSPECIFIED.)
GEOMETRIC_REPRESENTATION_ITEM()
RATIONAL_B_SPLINE_SURFACE(((1.,1.),(1.,1.),(1.,1.),(1.,1.),(1.,1.),(1.,
1.),(1.,1.),(1.,1.),(1.,1.),(1.,1.),(1.,1.),(1.,1.),(1.,1.),(1.,1.),(1.,
1.),(1.,1.),(1.,1.),(1.,1.),(1.,1.),(1.,1.),(1.,1.),(1.,1.),(1.,1.),(1.,
1.),(1.,1.),(1.,1.),(1.,1.),(1.,1.),(1.,1.),(1.,1.),(1.,1.),(1.,1.),(1.,
1.),(1.,1.),(1.,1.),(1.,1.),(1.,1.),(1.,1.),(1.,1.),(1.,1.),(1.,1.),(1.,
1.),(1.,1.),(1.,1.),(1.,1.),(1.,1.),(1.,1.),(1.,1.),(1.,1.),(1.,1.),(1.,
1.),(1.,1.),(1.,1.),(1.,1.),(1.,1.),(1.,1.),(1.,1.),(1.,1.),(1.,1.),(1.,
1.),(1.,1.),(1.,1.),(1.,1.),(1.,1.),(1.,1.),(1.,1.),(1.,1.),(1.,1.),(1.,
1.),(1.,1.),(1.,1.),(1.,1.),(1.,1.),(1.,1.),(1.,1.),(1.,1.),(1.,1.),(1.,
1.),(1.,1.),(1.,1.),(1.,1.),(1.,1.),(1.,1.),(1.,1.),(1.,1.),(1.,1.),(1.,
1.),(1.,1.),(1.,1.),(1.,1.),(1.,1.),(1.,1.),(1.,1.),(1.,1.),(1.,1.),(1.,
1.),(1.,1.),(1.,1.),(1.,1.),(1.,1.),(1.,1.),(1.,1.),(1.,1.),(1.,1.),(1.,
1.),(1.,1.),(1.,1.),(1.,1.),(1.,1.),(1.,1.),(1.,1.),(1.,1.),(1.,1.),(1.,
1.),(1.,1.),(1.,1.),(1.,1.),(1.,1.),(1.,1.),(1.,1.),(1.,1.),(1.,1.),(1.,
1.),(1.,1.),(1.,1.),(1.,1.),(1.,1.),(1.,1.),(1.,1.),(1.,1.),(1.,1.),(1.,
1.),(1.,1.),(1.,1.),(1.,1.),(1.,1.),(1.,1.),(1.,1.),(1.,1.),(1.,1.),(1.,
1.),(1.,1.),(1.,1.),(1.,1.),(1.,1.),(1.,1.),(1.,1.),(1.,1.),(1.,1.),(1.,
1.),(1.,1.),(1.,1.),(1.,1.),(1.,1.),(1.,1.),(1.,1.),(1.,1.),(1.,1.),(1.,
1.),(1.,1.),(1.,1.),(1.,1.),(1.,1.),(1.,1.),(1.,1.),(1.,1.),(1.,1.),(1.,
1.),(1.,1.),(1.,1.),(1.,1.),(1.,1.),(1.,1.),(1.,1.),(1.,1.),(1.,1.),(1.,
1.),(1.,1.),(1.,1.),(1.,1.),(1.,1.),(1.,1.),(1.,1.),(1.,1.),(1.,1.),(1.,
1.),(1.,1.),(1.,1.),(1.,1.),(1.,1.),(1.,1.),(1.,1.),(1.,1.),(1.,1.),(1.,
1.),(1.,1.),(1.,1.),(1.,1.),(1.,1.),(1.,1.),(1.,1.),(1.,1.),(1.,1.),(1.,
1.),(1.,1.)))
REPRESENTATION_ITEM('')
SURFACE()
);
#1032=(
BOUNDED_SURFACE()
B_SPLINE_SURFACE(5,1,((#188698,#188699),(#188700,#188701),(#188702,#188703),
(#188704,#188705),(#188706,#188707),(#188708,#188709),(#188710,#188711),
(#188712,#188713),(#188714,#188715),(#188716,#188717),(#188718,#188719),
(#188720,#188721),(#188722,#188723),(#188724,#188725),(#188726,#188727),
(#188728,#188729),(#188730,#188731),(#188732,#188733),(#188734,#188735),
(#188736,#188737),(#188738,#188739),(#188740,#188741),(#188742,#188743),
(#188744,#188745),(#188746,#188747),(#188748,#188749),(#188750,#188751),
(#188752,#188753),(#188754,#188755),(#188756,#188757),(#188758,#188759),
(#188760,#188761),(#188762,#188763),(#188764,#188765),(#188766,#188767),
(#188768,#188769),(#188770,#188771),(#188772,#188773),(#188774,#188775),
(#188776,#188777),(#188778,#188779),(#188780,#188781),(#188782,#188783),
(#188784,#188785),(#188786,#188787),(#188788,#188789),(#188790,#188791),
(#188792,#188793),(#188794,#188795),(#188796,#188797),(#188798,#188799),
(#188800,#188801),(#188802,#188803),(#188804,#188805),(#188806,#188807),
(#188808,#188809),(#188810,#188811),(#188812,#188813),(#188814,#188815),
(#188816,#188817),(#188818,#188819),(#188820,#188821),(#188822,#188823),
(#188824,#188825),(#188826,#188827),(#188828,#188829),(#188830,#188831),
(#188832,#188833),(#188834,#188835),(#188836,#188837),(#188838,#188839),
(#188840,#188841),(#188842,#188843),(#188844,#188845),(#188846,#188847),
(#188848,#188849),(#188850,#188851),(#188852,#188853),(#188854,#188855),
(#188856,#188857),(#188858,#188859),(#188860,#188861),(#188862,#188863),
(#188864,#188865),(#188866,#188867),(#188868,#188869),(#188870,#188871),
(#188872,#188873),(#188874,#188875),(#188876,#188877),(#188878,#188879),
(#188880,#188881),(#188882,#188883),(#188884,#188885),(#188886,#188887),
(#188888,#188889),(#188890,#188891),(#188892,#188893),(#188894,#188895),
(#188896,#188897),(#188898,#188899),(#188900,#188901),(#188902,#188903),
(#188904,#188905),(#188906,#188907),(#188908,#188909),(#188910,#188911),
(#188912,#188913),(#188914,#188915),(#188916,#188917),(#188918,#188919),
(#188920,#188921),(#188922,#188923),(#188924,#188925),(#188926,#188927),
(#188928,#188929),(#188930,#188931),(#188932,#188933),(#188934,#188935),
(#188936,#188937),(#188938,#188939),(#188940,#188941),(#188942,#188943),
(#188944,#188945),(#188946,#188947),(#188948,#188949),(#188950,#188951),
(#188952,#188953),(#188954,#188955),(#188956,#188957),(#188958,#188959),
(#188960,#188961),(#188962,#188963),(#188964,#188965),(#188966,#188967),
(#188968,#188969),(#188970,#188971),(#188972,#188973),(#188974,#188975),
(#188976,#188977),(#188978,#188979),(#188980,#188981),(#188982,#188983),
(#188984,#188985),(#188986,#188987),(#188988,#188989),(#188990,#188991),
(#188992,#188993),(#188994,#188995),(#188996,#188997),(#188998,#188999),
(#189000,#189001),(#189002,#189003),(#189004,#189005),(#189006,#189007),
(#189008,#189009),(#189010,#189011),(#189012,#189013),(#189014,#189015),
(#189016,#189017),(#189018,#189019),(#189020,#189021),(#189022,#189023),
(#189024,#189025),(#189026,#189027),(#189028,#189029),(#189030,#189031),
(#189032,#189033),(#189034,#189035),(#189036,#189037),(#189038,#189039),
(#189040,#189041),(#189042,#189043),(#189044,#189045),(#189046,#189047),
(#189048,#189049),(#189050,#189051),(#189052,#189053),(#189054,#189055),
(#189056,#189057),(#189058,#189059),(#189060,#189061),(#189062,#189063),
(#189064,#189065),(#189066,#189067),(#189068,#189069),(#189070,#189071),
(#189072,#189073),(#189074,#189075),(#189076,#189077),(#189078,#189079),
(#189080,#189081),(#189082,#189083),(#189084,#189085),(#189086,#189087),
(#189088,#189089),(#189090,#189091),(#189092,#189093),(#189094,#189095),
(#189096,#189097),(#189098,#189099),(#189100,#189101),(#189102,#189103),
(#189104,#189105),(#189106,#189107)),.UNSPECIFIED.,.F.,.F.,.F.)
B_SPLINE_SURFACE_WITH_KNOTS((6,1,1,1,1,1,1,1,1,1,1,1,1,1,1,1,1,1,1,1,1,
1,1,1,1,1,1,1,1,1,1,1,1,1,1,1,1,1,1,1,1,1,1,1,1,1,1,1,1,1,1,1,1,1,1,1,1,
1,1,1,1,1,1,1,1,1,1,1,1,1,1,1,1,1,1,1,1,1,1,1,1,1,1,1,1,1,1,1,1,1,1,1,1,
1,1,1,1,1,1,1,1,1,1,1,1,1,1,1,1,1,1,1,1,1,1,1,1,1,1,1,1,1,1,1,1,1,1,1,1,
1,1,1,1,1,1,1,1,1,1,1,1,1,1,1,1,1,1,1,1,1,1,1,1,1,1,1,1,1,1,1,1,1,1,1,1,
1,1,1,1,1,1,1,1,1,1,1,1,1,1,1,1,1,1,1,1,1,1,1,1,1,1,1,1,1,1,1,1,1,1,1,6),
(2,2),(0.,0.005,0.01,0.015,0.02,0.025,0.03,0.035,0.04,0.045,0.05,0.055,
0.06,0.065,0.07,0.075,0.08,0.085,0.09,0.095,0.1,0.105,0.11,0.115,0.12,0.125,
0.13,0.135,0.14,0.145,0.15,0.155,0.16,0.165,0.17,0.175,0.18,0.185,0.19,
0.195,0.2,0.205,0.21,0.215,0.22,0.225,0.23,0.235,0.24,0.245,0.25,0.255,
0.26,0.265,0.27,0.275,0.28,0.285,0.29,0.295,0.3,0.305,0.31,0.315,0.32,0.325,
0.33,0.335,0.34,0.345,0.35,0.355,0.36,0.365,0.37,0.375,0.38,0.385,0.39,
0.395,0.4,0.405,0.41,0.415,0.42,0.425,0.43,0.435,0.44,0.445,0.45,0.455,
0.46,0.465,0.47,0.475,0.48,0.485,0.49,0.495,0.5,0.505,0.51,0.515,0.52,0.525,
0.53,0.535,0.54,0.545,0.55,0.555,0.56,0.565,0.57,0.575,0.58,0.585,0.59,
0.595,0.6,0.605,0.61,0.615,0.62,0.625,0.63,0.635,0.64,0.645,0.65,0.655,
0.66,0.665,0.67,0.675,0.68,0.685,0.690000000000001,0.695000000000001,0.700000000000001,
0.705000000000001,0.710000000000001,0.715000000000001,0.720000000000001,
0.725000000000001,0.730000000000001,0.735000000000001,0.740000000000001,
0.745000000000001,0.750000000000001,0.755000000000001,0.760000000000001,
0.765000000000001,0.770000000000001,0.775000000000001,0.780000000000001,
0.785000000000001,0.790000000000001,0.795000000000001,0.800000000000001,
0.805000000000001,0.810000000000001,0.815000000000001,0.820000000000001,
0.825000000000001,0.830000000000001,0.835000000000001,0.840000000000001,
0.845000000000001,0.850000000000001,0.855000000000001,0.860000000000001,
0.865000000000001,0.870000000000001,0.875000000000001,0.880000000000001,
0.885000000000001,0.890000000000001,0.895000000000001,0.900000000000001,
0.905000000000001,0.910000000000001,0.915000000000001,0.920000000000001,
0.925000000000001,0.930000000000001,0.935000000000001,0.940000000000001,
0.945000000000001,0.950000000000001,0.955000000000001,0.960000000000001,
0.965000000000001,0.970000000000001,0.975000000000001,0.980000000000001,
0.985000000000001,0.990000000000001,0.995000000000001,1.),(0.,1.2),
 .UNSPECIFIED.)
GEOMETRIC_REPRESENTATION_ITEM()
RATIONAL_B_SPLINE_SURFACE(((1.,1.),(1.,1.),(1.,1.),(1.,1.),(1.,1.),(1.,
1.),(1.,1.),(1.,1.),(1.,1.),(1.,1.),(1.,1.),(1.,1.),(1.,1.),(1.,1.),(1.,
1.),(1.,1.),(1.,1.),(1.,1.),(1.,1.),(1.,1.),(1.,1.),(1.,1.),(1.,1.),(1.,
1.),(1.,1.),(1.,1.),(1.,1.),(1.,1.),(1.,1.),(1.,1.),(1.,1.),(1.,1.),(1.,
1.),(1.,1.),(1.,1.),(1.,1.),(1.,1.),(1.,1.),(1.,1.),(1.,1.),(1.,1.),(1.,
1.),(1.,1.),(1.,1.),(1.,1.),(1.,1.),(1.,1.),(1.,1.),(1.,1.),(1.,1.),(1.,
1.),(1.,1.),(1.,1.),(1.,1.),(1.,1.),(1.,1.),(1.,1.),(1.,1.),(1.,1.),(1.,
1.),(1.,1.),(1.,1.),(1.,1.),(1.,1.),(1.,1.),(1.,1.),(1.,1.),(1.,1.),(1.,
1.),(1.,1.),(1.,1.),(1.,1.),(1.,1.),(1.,1.),(1.,1.),(1.,1.),(1.,1.),(1.,
1.),(1.,1.),(1.,1.),(1.,1.),(1.,1.),(1.,1.),(1.,1.),(1.,1.),(1.,1.),(1.,
1.),(1.,1.),(1.,1.),(1.,1.),(1.,1.),(1.,1.),(1.,1.),(1.,1.),(1.,1.),(1.,
1.),(1.,1.),(1.,1.),(1.,1.),(1.,1.),(1.,1.),(1.,1.),(1.,1.),(1.,1.),(1.,
1.),(1.,1.),(1.,1.),(1.,1.),(1.,1.),(1.,1.),(1.,1.),(1.,1.),(1.,1.),(1.,
1.),(1.,1.),(1.,1.),(1.,1.),(1.,1.),(1.,1.),(1.,1.),(1.,1.),(1.,1.),(1.,
1.),(1.,1.),(1.,1.),(1.,1.),(1.,1.),(1.,1.),(1.,1.),(1.,1.),(1.,1.),(1.,
1.),(1.,1.),(1.,1.),(1.,1.),(1.,1.),(1.,1.),(1.,1.),(1.,1.),(1.,1.),(1.,
1.),(1.,1.),(1.,1.),(1.,1.),(1.,1.),(1.,1.),(1.,1.),(1.,1.),(1.,1.),(1.,
1.),(1.,1.),(1.,1.),(1.,1.),(1.,1.),(1.,1.),(1.,1.),(1.,1.),(1.,1.),(1.,
1.),(1.,1.),(1.,1.),(1.,1.),(1.,1.),(1.,1.),(1.,1.),(1.,1.),(1.,1.),(1.,
1.),(1.,1.),(1.,1.),(1.,1.),(1.,1.),(1.,1.),(1.,1.),(1.,1.),(1.,1.),(1.,
1.),(1.,1.),(1.,1.),(1.,1.),(1.,1.),(1.,1.),(1.,1.),(1.,1.),(1.,1.),(1.,
1.),(1.,1.),(1.,1.),(1.,1.),(1.,1.),(1.,1.),(1.,1.),(1.,1.),(1.,1.),(1.,
1.),(1.,1.),(1.,1.),(1.,1.),(1.,1.),(1.,1.),(1.,1.),(1.,1.),(1.,1.),(1.,
1.),(1.,1.)))
REPRESENTATION_ITEM('')
SURFACE()
);
#1033=(
BOUNDED_SURFACE()
B_SPLINE_SURFACE(5,1,((#189319,#189320),(#189321,#189322),(#189323,#189324),
(#189325,#189326),(#189327,#189328),(#189329,#189330),(#189331,#189332),
(#189333,#189334),(#189335,#189336),(#189337,#189338),(#189339,#189340),
(#189341,#189342),(#189343,#189344),(#189345,#189346),(#189347,#189348),
(#189349,#189350),(#189351,#189352),(#189353,#189354),(#189355,#189356),
(#189357,#189358),(#189359,#189360),(#189361,#189362),(#189363,#189364),
(#189365,#189366),(#189367,#189368),(#189369,#189370),(#189371,#189372),
(#189373,#189374),(#189375,#189376),(#189377,#189378),(#189379,#189380),
(#189381,#189382),(#189383,#189384),(#189385,#189386),(#189387,#189388),
(#189389,#189390),(#189391,#189392),(#189393,#189394),(#189395,#189396),
(#189397,#189398),(#189399,#189400),(#189401,#189402),(#189403,#189404),
(#189405,#189406),(#189407,#189408),(#189409,#189410),(#189411,#189412),
(#189413,#189414),(#189415,#189416),(#189417,#189418),(#189419,#189420),
(#189421,#189422),(#189423,#189424),(#189425,#189426),(#189427,#189428),
(#189429,#189430),(#189431,#189432),(#189433,#189434),(#189435,#189436),
(#189437,#189438),(#189439,#189440),(#189441,#189442),(#189443,#189444),
(#189445,#189446),(#189447,#189448),(#189449,#189450),(#189451,#189452),
(#189453,#189454),(#189455,#189456),(#189457,#189458),(#189459,#189460),
(#189461,#189462),(#189463,#189464),(#189465,#189466),(#189467,#189468),
(#189469,#189470),(#189471,#189472),(#189473,#189474),(#189475,#189476),
(#189477,#189478),(#189479,#189480),(#189481,#189482),(#189483,#189484),
(#189485,#189486),(#189487,#189488),(#189489,#189490),(#189491,#189492),
(#189493,#189494),(#189495,#189496),(#189497,#189498),(#189499,#189500),
(#189501,#189502),(#189503,#189504),(#189505,#189506),(#189507,#189508),
(#189509,#189510),(#189511,#189512),(#189513,#189514),(#189515,#189516),
(#189517,#189518),(#189519,#189520),(#189521,#189522),(#189523,#189524),
(#189525,#189526),(#189527,#189528),(#189529,#189530),(#189531,#189532),
(#189533,#189534),(#189535,#189536),(#189537,#189538),(#189539,#189540),
(#189541,#189542),(#189543,#189544),(#189545,#189546),(#189547,#189548),
(#189549,#189550),(#189551,#189552),(#189553,#189554),(#189555,#189556),
(#189557,#189558),(#189559,#189560),(#189561,#189562),(#189563,#189564),
(#189565,#189566),(#189567,#189568),(#189569,#189570),(#189571,#189572),
(#189573,#189574),(#189575,#189576),(#189577,#189578),(#189579,#189580),
(#189581,#189582),(#189583,#189584),(#189585,#189586),(#189587,#189588),
(#189589,#189590),(#189591,#189592),(#189593,#189594),(#189595,#189596),
(#189597,#189598),(#189599,#189600),(#189601,#189602),(#189603,#189604),
(#189605,#189606),(#189607,#189608),(#189609,#189610),(#189611,#189612),
(#189613,#189614),(#189615,#189616),(#189617,#189618),(#189619,#189620),
(#189621,#189622),(#189623,#189624),(#189625,#189626),(#189627,#189628),
(#189629,#189630),(#189631,#189632),(#189633,#189634),(#189635,#189636),
(#189637,#189638),(#189639,#189640),(#189641,#189642),(#189643,#189644),
(#189645,#189646),(#189647,#189648),(#189649,#189650),(#189651,#189652),
(#189653,#189654),(#189655,#189656),(#189657,#189658),(#189659,#189660),
(#189661,#189662),(#189663,#189664),(#189665,#189666),(#189667,#189668),
(#189669,#189670),(#189671,#189672),(#189673,#189674),(#189675,#189676),
(#189677,#189678),(#189679,#189680),(#189681,#189682),(#189683,#189684),
(#189685,#189686),(#189687,#189688),(#189689,#189690),(#189691,#189692),
(#189693,#189694),(#189695,#189696),(#189697,#189698),(#189699,#189700),
(#189701,#189702),(#189703,#189704),(#189705,#189706),(#189707,#189708),
(#189709,#189710),(#189711,#189712),(#189713,#189714),(#189715,#189716),
(#189717,#189718),(#189719,#189720),(#189721,#189722),(#189723,#189724),
(#189725,#189726),(#189727,#189728)),.UNSPECIFIED.,.F.,.F.,.F.)
B_SPLINE_SURFACE_WITH_KNOTS((6,1,1,1,1,1,1,1,1,1,1,1,1,1,1,1,1,1,1,1,1,
1,1,1,1,1,1,1,1,1,1,1,1,1,1,1,1,1,1,1,1,1,1,1,1,1,1,1,1,1,1,1,1,1,1,1,1,
1,1,1,1,1,1,1,1,1,1,1,1,1,1,1,1,1,1,1,1,1,1,1,1,1,1,1,1,1,1,1,1,1,1,1,1,
1,1,1,1,1,1,1,1,1,1,1,1,1,1,1,1,1,1,1,1,1,1,1,1,1,1,1,1,1,1,1,1,1,1,1,1,
1,1,1,1,1,1,1,1,1,1,1,1,1,1,1,1,1,1,1,1,1,1,1,1,1,1,1,1,1,1,1,1,1,1,1,1,
1,1,1,1,1,1,1,1,1,1,1,1,1,1,1,1,1,1,1,1,1,1,1,1,1,1,1,1,1,1,1,1,1,1,1,6),
(2,2),(-1.,-0.995000000000001,-0.990000000000001,-0.985000000000001,-0.980000000000001,
-0.975000000000001,-0.970000000000001,-0.965000000000001,-0.960000000000001,
-0.955000000000001,-0.950000000000001,-0.945000000000001,-0.940000000000001,
-0.935000000000001,-0.930000000000001,-0.925000000000001,-0.920000000000001,
-0.915000000000001,-0.910000000000001,-0.905000000000001,-0.900000000000001,
-0.895000000000001,-0.890000000000001,-0.885000000000001,-0.880000000000001,
-0.875000000000001,-0.870000000000001,-0.865000000000001,-0.860000000000001,
-0.855000000000001,-0.850000000000001,-0.845000000000001,-0.840000000000001,
-0.835000000000001,-0.830000000000001,-0.825000000000001,-0.820000000000001,
-0.815000000000001,-0.810000000000001,-0.805000000000001,-0.800000000000001,
-0.795000000000001,-0.790000000000001,-0.785000000000001,-0.780000000000001,
-0.775000000000001,-0.770000000000001,-0.765000000000001,-0.760000000000001,
-0.755000000000001,-0.750000000000001,-0.745000000000001,-0.740000000000001,
-0.735000000000001,-0.730000000000001,-0.725000000000001,-0.720000000000001,
-0.715000000000001,-0.710000000000001,-0.705000000000001,-0.700000000000001,
-0.695000000000001,-0.690000000000001,-0.685,-0.68,-0.675,-0.67,-0.665,
-0.66,-0.655,-0.65,-0.645,-0.64,-0.635,-0.63,-0.625,-0.62,-0.615,-0.61,
-0.605,-0.6,-0.595,-0.59,-0.585,-0.58,-0.575,-0.57,-0.565,-0.56,-0.555,
-0.55,-0.545,-0.54,-0.535,-0.53,-0.525,-0.52,-0.515,-0.51,-0.505,-0.5,-0.495,
-0.49,-0.485,-0.48,-0.475,-0.47,-0.465,-0.46,-0.455,-0.45,-0.445,-0.44,
-0.435,-0.43,-0.425,-0.42,-0.415,-0.41,-0.405,-0.4,-0.395,-0.39,-0.385,
-0.38,-0.375,-0.37,-0.365,-0.36,-0.355,-0.35,-0.345,-0.34,-0.335,-0.33,
-0.325,-0.32,-0.315,-0.31,-0.305,-0.3,-0.295,-0.29,-0.285,-0.28,-0.275,
-0.27,-0.265,-0.26,-0.255,-0.25,-0.245,-0.24,-0.235,-0.23,-0.225,-0.22,
-0.215,-0.21,-0.205,-0.2,-0.195,-0.19,-0.185,-0.18,-0.175,-0.17,-0.165,
-0.16,-0.155,-0.15,-0.145,-0.14,-0.135,-0.13,-0.125,-0.12,-0.115,-0.11,
-0.105,-0.1,-0.095,-0.09,-0.085,-0.08,-0.075,-0.07,-0.065,-0.06,-0.055,
-0.05,-0.045,-0.04,-0.035,-0.03,-0.025,-0.02,-0.015,-0.01,-0.005,0.),(0.,
1.2),.UNSPECIFIED.)
GEOMETRIC_REPRESENTATION_ITEM()
RATIONAL_B_SPLINE_SURFACE(((1.,1.),(1.,1.),(1.,1.),(1.,1.),(1.,1.),(1.,
1.),(1.,1.),(1.,1.),(1.,1.),(1.,1.),(1.,1.),(1.,1.),(1.,1.),(1.,1.),(1.,
1.),(1.,1.),(1.,1.),(1.,1.),(1.,1.),(1.,1.),(1.,1.),(1.,1.),(1.,1.),(1.,
1.),(1.,1.),(1.,1.),(1.,1.),(1.,1.),(1.,1.),(1.,1.),(1.,1.),(1.,1.),(1.,
1.),(1.,1.),(1.,1.),(1.,1.),(1.,1.),(1.,1.),(1.,1.),(1.,1.),(1.,1.),(1.,
1.),(1.,1.),(1.,1.),(1.,1.),(1.,1.),(1.,1.),(1.,1.),(1.,1.),(1.,1.),(1.,
1.),(1.,1.),(1.,1.),(1.,1.),(1.,1.),(1.,1.),(1.,1.),(1.,1.),(1.,1.),(1.,
1.),(1.,1.),(1.,1.),(1.,1.),(1.,1.),(1.,1.),(1.,1.),(1.,1.),(1.,1.),(1.,
1.),(1.,1.),(1.,1.),(1.,1.),(1.,1.),(1.,1.),(1.,1.),(1.,1.),(1.,1.),(1.,
1.),(1.,1.),(1.,1.),(1.,1.),(1.,1.),(1.,1.),(1.,1.),(1.,1.),(1.,1.),(1.,
1.),(1.,1.),(1.,1.),(1.,1.),(1.,1.),(1.,1.),(1.,1.),(1.,1.),(1.,1.),(1.,
1.),(1.,1.),(1.,1.),(1.,1.),(1.,1.),(1.,1.),(1.,1.),(1.,1.),(1.,1.),(1.,
1.),(1.,1.),(1.,1.),(1.,1.),(1.,1.),(1.,1.),(1.,1.),(1.,1.),(1.,1.),(1.,
1.),(1.,1.),(1.,1.),(1.,1.),(1.,1.),(1.,1.),(1.,1.),(1.,1.),(1.,1.),(1.,
1.),(1.,1.),(1.,1.),(1.,1.),(1.,1.),(1.,1.),(1.,1.),(1.,1.),(1.,1.),(1.,
1.),(1.,1.),(1.,1.),(1.,1.),(1.,1.),(1.,1.),(1.,1.),(1.,1.),(1.,1.),(1.,
1.),(1.,1.),(1.,1.),(1.,1.),(1.,1.),(1.,1.),(1.,1.),(1.,1.),(1.,1.),(1.,
1.),(1.,1.),(1.,1.),(1.,1.),(1.,1.),(1.,1.),(1.,1.),(1.,1.),(1.,1.),(1.,
1.),(1.,1.),(1.,1.),(1.,1.),(1.,1.),(1.,1.),(1.,1.),(1.,1.),(1.,1.),(1.,
1.),(1.,1.),(1.,1.),(1.,1.),(1.,1.),(1.,1.),(1.,1.),(1.,1.),(1.,1.),(1.,
1.),(1.,1.),(1.,1.),(1.,1.),(1.,1.),(1.,1.),(1.,1.),(1.,1.),(1.,1.),(1.,
1.),(1.,1.),(1.,1.),(1.,1.),(1.,1.),(1.,1.),(1.,1.),(1.,1.),(1.,1.),(1.,
1.),(1.,1.),(1.,1.),(1.,1.),(1.,1.),(1.,1.),(1.,1.),(1.,1.),(1.,1.),(1.,
1.),(1.,1.)))
REPRESENTATION_ITEM('')
SURFACE()
);
#1034=(
BOUNDED_SURFACE()
B_SPLINE_SURFACE(5,1,((#189936,#189937),(#189938,#189939),(#189940,#189941),
(#189942,#189943),(#189944,#189945),(#189946,#189947),(#189948,#189949),
(#189950,#189951),(#189952,#189953),(#189954,#189955),(#189956,#189957),
(#189958,#189959),(#189960,#189961),(#189962,#189963),(#189964,#189965),
(#189966,#189967),(#189968,#189969),(#189970,#189971),(#189972,#189973),
(#189974,#189975),(#189976,#189977),(#189978,#189979),(#189980,#189981),
(#189982,#189983),(#189984,#189985),(#189986,#189987),(#189988,#189989),
(#189990,#189991),(#189992,#189993),(#189994,#189995),(#189996,#189997),
(#189998,#189999),(#190000,#190001),(#190002,#190003),(#190004,#190005),
(#190006,#190007),(#190008,#190009),(#190010,#190011),(#190012,#190013),
(#190014,#190015),(#190016,#190017),(#190018,#190019),(#190020,#190021),
(#190022,#190023),(#190024,#190025),(#190026,#190027),(#190028,#190029),
(#190030,#190031),(#190032,#190033),(#190034,#190035),(#190036,#190037),
(#190038,#190039),(#190040,#190041),(#190042,#190043),(#190044,#190045),
(#190046,#190047),(#190048,#190049),(#190050,#190051),(#190052,#190053),
(#190054,#190055),(#190056,#190057),(#190058,#190059),(#190060,#190061),
(#190062,#190063),(#190064,#190065),(#190066,#190067),(#190068,#190069),
(#190070,#190071),(#190072,#190073),(#190074,#190075),(#190076,#190077),
(#190078,#190079),(#190080,#190081),(#190082,#190083),(#190084,#190085),
(#190086,#190087),(#190088,#190089),(#190090,#190091),(#190092,#190093),
(#190094,#190095),(#190096,#190097),(#190098,#190099),(#190100,#190101),
(#190102,#190103),(#190104,#190105),(#190106,#190107),(#190108,#190109),
(#190110,#190111),(#190112,#190113),(#190114,#190115),(#190116,#190117),
(#190118,#190119),(#190120,#190121),(#190122,#190123),(#190124,#190125),
(#190126,#190127),(#190128,#190129),(#190130,#190131),(#190132,#190133),
(#190134,#190135),(#190136,#190137),(#190138,#190139),(#190140,#190141),
(#190142,#190143),(#190144,#190145),(#190146,#190147),(#190148,#190149),
(#190150,#190151),(#190152,#190153),(#190154,#190155),(#190156,#190157),
(#190158,#190159),(#190160,#190161),(#190162,#190163),(#190164,#190165),
(#190166,#190167),(#190168,#190169),(#190170,#190171),(#190172,#190173),
(#190174,#190175),(#190176,#190177),(#190178,#190179),(#190180,#190181),
(#190182,#190183),(#190184,#190185),(#190186,#190187),(#190188,#190189),
(#190190,#190191),(#190192,#190193),(#190194,#190195),(#190196,#190197),
(#190198,#190199),(#190200,#190201),(#190202,#190203),(#190204,#190205),
(#190206,#190207),(#190208,#190209),(#190210,#190211),(#190212,#190213),
(#190214,#190215),(#190216,#190217),(#190218,#190219),(#190220,#190221),
(#190222,#190223),(#190224,#190225),(#190226,#190227),(#190228,#190229),
(#190230,#190231),(#190232,#190233),(#190234,#190235),(#190236,#190237),
(#190238,#190239),(#190240,#190241),(#190242,#190243),(#190244,#190245),
(#190246,#190247),(#190248,#190249),(#190250,#190251),(#190252,#190253),
(#190254,#190255),(#190256,#190257),(#190258,#190259),(#190260,#190261),
(#190262,#190263),(#190264,#190265),(#190266,#190267),(#190268,#190269),
(#190270,#190271),(#190272,#190273),(#190274,#190275),(#190276,#190277),
(#190278,#190279),(#190280,#190281),(#190282,#190283),(#190284,#190285),
(#190286,#190287),(#190288,#190289),(#190290,#190291),(#190292,#190293),
(#190294,#190295),(#190296,#190297),(#190298,#190299),(#190300,#190301),
(#190302,#190303),(#190304,#190305),(#190306,#190307),(#190308,#190309),
(#190310,#190311),(#190312,#190313),(#190314,#190315),(#190316,#190317),
(#190318,#190319),(#190320,#190321),(#190322,#190323),(#190324,#190325),
(#190326,#190327),(#190328,#190329),(#190330,#190331),(#190332,#190333),
(#190334,#190335),(#190336,#190337),(#190338,#190339),(#190340,#190341),
(#190342,#190343),(#190344,#190345)),.UNSPECIFIED.,.F.,.F.,.F.)
B_SPLINE_SURFACE_WITH_KNOTS((6,1,1,1,1,1,1,1,1,1,1,1,1,1,1,1,1,1,1,1,1,
1,1,1,1,1,1,1,1,1,1,1,1,1,1,1,1,1,1,1,1,1,1,1,1,1,1,1,1,1,1,1,1,1,1,1,1,
1,1,1,1,1,1,1,1,1,1,1,1,1,1,1,1,1,1,1,1,1,1,1,1,1,1,1,1,1,1,1,1,1,1,1,1,
1,1,1,1,1,1,1,1,1,1,1,1,1,1,1,1,1,1,1,1,1,1,1,1,1,1,1,1,1,1,1,1,1,1,1,1,
1,1,1,1,1,1,1,1,1,1,1,1,1,1,1,1,1,1,1,1,1,1,1,1,1,1,1,1,1,1,1,1,1,1,1,1,
1,1,1,1,1,1,1,1,1,1,1,1,1,1,1,1,1,1,1,1,1,1,1,1,1,1,1,1,1,1,1,1,1,1,1,6),
(2,2),(0.,0.005,0.01,0.015,0.02,0.025,0.03,0.035,0.04,0.045,0.05,0.055,
0.06,0.065,0.07,0.075,0.08,0.085,0.09,0.095,0.1,0.105,0.11,0.115,0.12,0.125,
0.13,0.135,0.14,0.145,0.15,0.155,0.16,0.165,0.17,0.175,0.18,0.185,0.19,
0.195,0.2,0.205,0.21,0.215,0.22,0.225,0.23,0.235,0.24,0.245,0.25,0.255,
0.26,0.265,0.27,0.275,0.28,0.285,0.29,0.295,0.3,0.305,0.31,0.315,0.32,0.325,
0.33,0.335,0.34,0.345,0.35,0.355,0.36,0.365,0.37,0.375,0.38,0.385,0.39,
0.395,0.4,0.405,0.41,0.415,0.42,0.425,0.43,0.435,0.44,0.445,0.45,0.455,
0.46,0.465,0.47,0.475,0.48,0.485,0.49,0.495,0.5,0.505,0.51,0.515,0.52,0.525,
0.53,0.535,0.54,0.545,0.55,0.555,0.56,0.565,0.57,0.575,0.58,0.585,0.59,
0.595,0.6,0.605,0.61,0.615,0.62,0.625,0.63,0.635,0.64,0.645,0.65,0.655,
0.66,0.665,0.67,0.675,0.68,0.685,0.690000000000001,0.695000000000001,0.700000000000001,
0.705000000000001,0.710000000000001,0.715000000000001,0.720000000000001,
0.725000000000001,0.730000000000001,0.735000000000001,0.740000000000001,
0.745000000000001,0.750000000000001,0.755000000000001,0.760000000000001,
0.765000000000001,0.770000000000001,0.775000000000001,0.780000000000001,
0.785000000000001,0.790000000000001,0.795000000000001,0.800000000000001,
0.805000000000001,0.810000000000001,0.815000000000001,0.820000000000001,
0.825000000000001,0.830000000000001,0.835000000000001,0.840000000000001,
0.845000000000001,0.850000000000001,0.855000000000001,0.860000000000001,
0.865000000000001,0.870000000000001,0.875000000000001,0.880000000000001,
0.885000000000001,0.890000000000001,0.895000000000001,0.900000000000001,
0.905000000000001,0.910000000000001,0.915000000000001,0.920000000000001,
0.925000000000001,0.930000000000001,0.935000000000001,0.940000000000001,
0.945000000000001,0.950000000000001,0.955000000000001,0.960000000000001,
0.965000000000001,0.970000000000001,0.975000000000001,0.980000000000001,
0.985000000000001,0.990000000000001,0.995000000000001,1.),(0.,1.2),
 .UNSPECIFIED.)
GEOMETRIC_REPRESENTATION_ITEM()
RATIONAL_B_SPLINE_SURFACE(((1.,1.),(1.,1.),(1.,1.),(1.,1.),(1.,1.),(1.,
1.),(1.,1.),(1.,1.),(1.,1.),(1.,1.),(1.,1.),(1.,1.),(1.,1.),(1.,1.),(1.,
1.),(1.,1.),(1.,1.),(1.,1.),(1.,1.),(1.,1.),(1.,1.),(1.,1.),(1.,1.),(1.,
1.),(1.,1.),(1.,1.),(1.,1.),(1.,1.),(1.,1.),(1.,1.),(1.,1.),(1.,1.),(1.,
1.),(1.,1.),(1.,1.),(1.,1.),(1.,1.),(1.,1.),(1.,1.),(1.,1.),(1.,1.),(1.,
1.),(1.,1.),(1.,1.),(1.,1.),(1.,1.),(1.,1.),(1.,1.),(1.,1.),(1.,1.),(1.,
1.),(1.,1.),(1.,1.),(1.,1.),(1.,1.),(1.,1.),(1.,1.),(1.,1.),(1.,1.),(1.,
1.),(1.,1.),(1.,1.),(1.,1.),(1.,1.),(1.,1.),(1.,1.),(1.,1.),(1.,1.),(1.,
1.),(1.,1.),(1.,1.),(1.,1.),(1.,1.),(1.,1.),(1.,1.),(1.,1.),(1.,1.),(1.,
1.),(1.,1.),(1.,1.),(1.,1.),(1.,1.),(1.,1.),(1.,1.),(1.,1.),(1.,1.),(1.,
1.),(1.,1.),(1.,1.),(1.,1.),(1.,1.),(1.,1.),(1.,1.),(1.,1.),(1.,1.),(1.,
1.),(1.,1.),(1.,1.),(1.,1.),(1.,1.),(1.,1.),(1.,1.),(1.,1.),(1.,1.),(1.,
1.),(1.,1.),(1.,1.),(1.,1.),(1.,1.),(1.,1.),(1.,1.),(1.,1.),(1.,1.),(1.,
1.),(1.,1.),(1.,1.),(1.,1.),(1.,1.),(1.,1.),(1.,1.),(1.,1.),(1.,1.),(1.,
1.),(1.,1.),(1.,1.),(1.,1.),(1.,1.),(1.,1.),(1.,1.),(1.,1.),(1.,1.),(1.,
1.),(1.,1.),(1.,1.),(1.,1.),(1.,1.),(1.,1.),(1.,1.),(1.,1.),(1.,1.),(1.,
1.),(1.,1.),(1.,1.),(1.,1.),(1.,1.),(1.,1.),(1.,1.),(1.,1.),(1.,1.),(1.,
1.),(1.,1.),(1.,1.),(1.,1.),(1.,1.),(1.,1.),(1.,1.),(1.,1.),(1.,1.),(1.,
1.),(1.,1.),(1.,1.),(1.,1.),(1.,1.),(1.,1.),(1.,1.),(1.,1.),(1.,1.),(1.,
1.),(1.,1.),(1.,1.),(1.,1.),(1.,1.),(1.,1.),(1.,1.),(1.,1.),(1.,1.),(1.,
1.),(1.,1.),(1.,1.),(1.,1.),(1.,1.),(1.,1.),(1.,1.),(1.,1.),(1.,1.),(1.,
1.),(1.,1.),(1.,1.),(1.,1.),(1.,1.),(1.,1.),(1.,1.),(1.,1.),(1.,1.),(1.,
1.),(1.,1.),(1.,1.),(1.,1.),(1.,1.),(1.,1.),(1.,1.),(1.,1.),(1.,1.),(1.,
1.),(1.,1.)))
REPRESENTATION_ITEM('')
SURFACE()
);
#1035=(
BOUNDED_SURFACE()
B_SPLINE_SURFACE(5,1,((#190557,#190558),(#190559,#190560),(#190561,#190562),
(#190563,#190564),(#190565,#190566),(#190567,#190568),(#190569,#190570),
(#190571,#190572),(#190573,#190574),(#190575,#190576),(#190577,#190578),
(#190579,#190580),(#190581,#190582),(#190583,#190584),(#190585,#190586),
(#190587,#190588),(#190589,#190590),(#190591,#190592),(#190593,#190594),
(#190595,#190596),(#190597,#190598),(#190599,#190600),(#190601,#190602),
(#190603,#190604),(#190605,#190606),(#190607,#190608),(#190609,#190610),
(#190611,#190612),(#190613,#190614),(#190615,#190616),(#190617,#190618),
(#190619,#190620),(#190621,#190622),(#190623,#190624),(#190625,#190626),
(#190627,#190628),(#190629,#190630),(#190631,#190632),(#190633,#190634),
(#190635,#190636),(#190637,#190638),(#190639,#190640),(#190641,#190642),
(#190643,#190644),(#190645,#190646),(#190647,#190648),(#190649,#190650),
(#190651,#190652),(#190653,#190654),(#190655,#190656),(#190657,#190658),
(#190659,#190660),(#190661,#190662),(#190663,#190664),(#190665,#190666),
(#190667,#190668),(#190669,#190670),(#190671,#190672),(#190673,#190674),
(#190675,#190676),(#190677,#190678),(#190679,#190680),(#190681,#190682),
(#190683,#190684),(#190685,#190686),(#190687,#190688),(#190689,#190690),
(#190691,#190692),(#190693,#190694),(#190695,#190696),(#190697,#190698),
(#190699,#190700),(#190701,#190702),(#190703,#190704),(#190705,#190706),
(#190707,#190708),(#190709,#190710),(#190711,#190712),(#190713,#190714),
(#190715,#190716),(#190717,#190718),(#190719,#190720),(#190721,#190722),
(#190723,#190724),(#190725,#190726),(#190727,#190728),(#190729,#190730),
(#190731,#190732),(#190733,#190734),(#190735,#190736),(#190737,#190738),
(#190739,#190740),(#190741,#190742),(#190743,#190744),(#190745,#190746),
(#190747,#190748),(#190749,#190750),(#190751,#190752),(#190753,#190754),
(#190755,#190756),(#190757,#190758),(#190759,#190760),(#190761,#190762),
(#190763,#190764),(#190765,#190766),(#190767,#190768),(#190769,#190770),
(#190771,#190772),(#190773,#190774),(#190775,#190776),(#190777,#190778),
(#190779,#190780),(#190781,#190782),(#190783,#190784),(#190785,#190786),
(#190787,#190788),(#190789,#190790),(#190791,#190792),(#190793,#190794),
(#190795,#190796),(#190797,#190798),(#190799,#190800),(#190801,#190802),
(#190803,#190804),(#190805,#190806),(#190807,#190808),(#190809,#190810),
(#190811,#190812),(#190813,#190814),(#190815,#190816),(#190817,#190818),
(#190819,#190820),(#190821,#190822),(#190823,#190824),(#190825,#190826),
(#190827,#190828),(#190829,#190830),(#190831,#190832),(#190833,#190834),
(#190835,#190836),(#190837,#190838),(#190839,#190840),(#190841,#190842),
(#190843,#190844),(#190845,#190846),(#190847,#190848),(#190849,#190850),
(#190851,#190852),(#190853,#190854),(#190855,#190856),(#190857,#190858),
(#190859,#190860),(#190861,#190862),(#190863,#190864),(#190865,#190866),
(#190867,#190868),(#190869,#190870),(#190871,#190872),(#190873,#190874),
(#190875,#190876),(#190877,#190878),(#190879,#190880),(#190881,#190882),
(#190883,#190884),(#190885,#190886),(#190887,#190888),(#190889,#190890),
(#190891,#190892),(#190893,#190894),(#190895,#190896),(#190897,#190898),
(#190899,#190900),(#190901,#190902),(#190903,#190904),(#190905,#190906),
(#190907,#190908),(#190909,#190910),(#190911,#190912),(#190913,#190914),
(#190915,#190916),(#190917,#190918),(#190919,#190920),(#190921,#190922),
(#190923,#190924),(#190925,#190926),(#190927,#190928),(#190929,#190930),
(#190931,#190932),(#190933,#190934),(#190935,#190936),(#190937,#190938),
(#190939,#190940),(#190941,#190942),(#190943,#190944),(#190945,#190946),
(#190947,#190948),(#190949,#190950),(#190951,#190952),(#190953,#190954),
(#190955,#190956),(#190957,#190958),(#190959,#190960),(#190961,#190962),
(#190963,#190964),(#190965,#190966)),.UNSPECIFIED.,.F.,.F.,.F.)
B_SPLINE_SURFACE_WITH_KNOTS((6,1,1,1,1,1,1,1,1,1,1,1,1,1,1,1,1,1,1,1,1,
1,1,1,1,1,1,1,1,1,1,1,1,1,1,1,1,1,1,1,1,1,1,1,1,1,1,1,1,1,1,1,1,1,1,1,1,
1,1,1,1,1,1,1,1,1,1,1,1,1,1,1,1,1,1,1,1,1,1,1,1,1,1,1,1,1,1,1,1,1,1,1,1,
1,1,1,1,1,1,1,1,1,1,1,1,1,1,1,1,1,1,1,1,1,1,1,1,1,1,1,1,1,1,1,1,1,1,1,1,
1,1,1,1,1,1,1,1,1,1,1,1,1,1,1,1,1,1,1,1,1,1,1,1,1,1,1,1,1,1,1,1,1,1,1,1,
1,1,1,1,1,1,1,1,1,1,1,1,1,1,1,1,1,1,1,1,1,1,1,1,1,1,1,1,1,1,1,1,1,1,1,6),
(2,2),(-1.,-0.995000000000001,-0.990000000000001,-0.985000000000001,-0.980000000000001,
-0.975000000000001,-0.970000000000001,-0.965000000000001,-0.960000000000001,
-0.955000000000001,-0.950000000000001,-0.945000000000001,-0.940000000000001,
-0.935000000000001,-0.930000000000001,-0.925000000000001,-0.920000000000001,
-0.915000000000001,-0.910000000000001,-0.905000000000001,-0.900000000000001,
-0.895000000000001,-0.890000000000001,-0.885000000000001,-0.880000000000001,
-0.875000000000001,-0.870000000000001,-0.865000000000001,-0.860000000000001,
-0.855000000000001,-0.850000000000001,-0.845000000000001,-0.840000000000001,
-0.835000000000001,-0.830000000000001,-0.825000000000001,-0.820000000000001,
-0.815000000000001,-0.810000000000001,-0.805000000000001,-0.800000000000001,
-0.795000000000001,-0.790000000000001,-0.785000000000001,-0.780000000000001,
-0.775000000000001,-0.770000000000001,-0.765000000000001,-0.760000000000001,
-0.755000000000001,-0.750000000000001,-0.745000000000001,-0.740000000000001,
-0.735000000000001,-0.730000000000001,-0.725000000000001,-0.720000000000001,
-0.715000000000001,-0.710000000000001,-0.705000000000001,-0.700000000000001,
-0.695000000000001,-0.690000000000001,-0.685,-0.68,-0.675,-0.67,-0.665,
-0.66,-0.655,-0.65,-0.645,-0.64,-0.635,-0.63,-0.625,-0.62,-0.615,-0.61,
-0.605,-0.6,-0.595,-0.59,-0.585,-0.58,-0.575,-0.57,-0.565,-0.56,-0.555,
-0.55,-0.545,-0.54,-0.535,-0.53,-0.525,-0.52,-0.515,-0.51,-0.505,-0.5,-0.495,
-0.49,-0.485,-0.48,-0.475,-0.47,-0.465,-0.46,-0.455,-0.45,-0.445,-0.44,
-0.435,-0.43,-0.425,-0.42,-0.415,-0.41,-0.405,-0.4,-0.395,-0.39,-0.385,
-0.38,-0.375,-0.37,-0.365,-0.36,-0.355,-0.35,-0.345,-0.34,-0.335,-0.33,
-0.325,-0.32,-0.315,-0.31,-0.305,-0.3,-0.295,-0.29,-0.285,-0.28,-0.275,
-0.27,-0.265,-0.26,-0.255,-0.25,-0.245,-0.24,-0.235,-0.23,-0.225,-0.22,
-0.215,-0.21,-0.205,-0.2,-0.195,-0.19,-0.185,-0.18,-0.175,-0.17,-0.165,
-0.16,-0.155,-0.15,-0.145,-0.14,-0.135,-0.13,-0.125,-0.12,-0.115,-0.11,
-0.105,-0.1,-0.095,-0.09,-0.085,-0.08,-0.075,-0.07,-0.065,-0.06,-0.055,
-0.05,-0.045,-0.04,-0.035,-0.03,-0.025,-0.02,-0.015,-0.01,-0.005,0.),(0.,
1.2),.UNSPECIFIED.)
GEOMETRIC_REPRESENTATION_ITEM()
RATIONAL_B_SPLINE_SURFACE(((1.,1.),(1.,1.),(1.,1.),(1.,1.),(1.,1.),(1.,
1.),(1.,1.),(1.,1.),(1.,1.),(1.,1.),(1.,1.),(1.,1.),(1.,1.),(1.,1.),(1.,
1.),(1.,1.),(1.,1.),(1.,1.),(1.,1.),(1.,1.),(1.,1.),(1.,1.),(1.,1.),(1.,
1.),(1.,1.),(1.,1.),(1.,1.),(1.,1.),(1.,1.),(1.,1.),(1.,1.),(1.,1.),(1.,
1.),(1.,1.),(1.,1.),(1.,1.),(1.,1.),(1.,1.),(1.,1.),(1.,1.),(1.,1.),(1.,
1.),(1.,1.),(1.,1.),(1.,1.),(1.,1.),(1.,1.),(1.,1.),(1.,1.),(1.,1.),(1.,
1.),(1.,1.),(1.,1.),(1.,1.),(1.,1.),(1.,1.),(1.,1.),(1.,1.),(1.,1.),(1.,
1.),(1.,1.),(1.,1.),(1.,1.),(1.,1.),(1.,1.),(1.,1.),(1.,1.),(1.,1.),(1.,
1.),(1.,1.),(1.,1.),(1.,1.),(1.,1.),(1.,1.),(1.,1.),(1.,1.),(1.,1.),(1.,
1.),(1.,1.),(1.,1.),(1.,1.),(1.,1.),(1.,1.),(1.,1.),(1.,1.),(1.,1.),(1.,
1.),(1.,1.),(1.,1.),(1.,1.),(1.,1.),(1.,1.),(1.,1.),(1.,1.),(1.,1.),(1.,
1.),(1.,1.),(1.,1.),(1.,1.),(1.,1.),(1.,1.),(1.,1.),(1.,1.),(1.,1.),(1.,
1.),(1.,1.),(1.,1.),(1.,1.),(1.,1.),(1.,1.),(1.,1.),(1.,1.),(1.,1.),(1.,
1.),(1.,1.),(1.,1.),(1.,1.),(1.,1.),(1.,1.),(1.,1.),(1.,1.),(1.,1.),(1.,
1.),(1.,1.),(1.,1.),(1.,1.),(1.,1.),(1.,1.),(1.,1.),(1.,1.),(1.,1.),(1.,
1.),(1.,1.),(1.,1.),(1.,1.),(1.,1.),(1.,1.),(1.,1.),(1.,1.),(1.,1.),(1.,
1.),(1.,1.),(1.,1.),(1.,1.),(1.,1.),(1.,1.),(1.,1.),(1.,1.),(1.,1.),(1.,
1.),(1.,1.),(1.,1.),(1.,1.),(1.,1.),(1.,1.),(1.,1.),(1.,1.),(1.,1.),(1.,
1.),(1.,1.),(1.,1.),(1.,1.),(1.,1.),(1.,1.),(1.,1.),(1.,1.),(1.,1.),(1.,
1.),(1.,1.),(1.,1.),(1.,1.),(1.,1.),(1.,1.),(1.,1.),(1.,1.),(1.,1.),(1.,
1.),(1.,1.),(1.,1.),(1.,1.),(1.,1.),(1.,1.),(1.,1.),(1.,1.),(1.,1.),(1.,
1.),(1.,1.),(1.,1.),(1.,1.),(1.,1.),(1.,1.),(1.,1.),(1.,1.),(1.,1.),(1.,
1.),(1.,1.),(1.,1.),(1.,1.),(1.,1.),(1.,1.),(1.,1.),(1.,1.),(1.,1.),(1.,
1.),(1.,1.)))
REPRESENTATION_ITEM('')
SURFACE()
);
#1036=(
BOUNDED_SURFACE()
B_SPLINE_SURFACE(5,1,((#191174,#191175),(#191176,#191177),(#191178,#191179),
(#191180,#191181),(#191182,#191183),(#191184,#191185),(#191186,#191187),
(#191188,#191189),(#191190,#191191),(#191192,#191193),(#191194,#191195),
(#191196,#191197),(#191198,#191199),(#191200,#191201),(#191202,#191203),
(#191204,#191205),(#191206,#191207),(#191208,#191209),(#191210,#191211),
(#191212,#191213),(#191214,#191215),(#191216,#191217),(#191218,#191219),
(#191220,#191221),(#191222,#191223),(#191224,#191225),(#191226,#191227),
(#191228,#191229),(#191230,#191231),(#191232,#191233),(#191234,#191235),
(#191236,#191237),(#191238,#191239),(#191240,#191241),(#191242,#191243),
(#191244,#191245),(#191246,#191247),(#191248,#191249),(#191250,#191251),
(#191252,#191253),(#191254,#191255),(#191256,#191257),(#191258,#191259),
(#191260,#191261),(#191262,#191263),(#191264,#191265),(#191266,#191267),
(#191268,#191269),(#191270,#191271),(#191272,#191273),(#191274,#191275),
(#191276,#191277),(#191278,#191279),(#191280,#191281),(#191282,#191283),
(#191284,#191285),(#191286,#191287),(#191288,#191289),(#191290,#191291),
(#191292,#191293),(#191294,#191295),(#191296,#191297),(#191298,#191299),
(#191300,#191301),(#191302,#191303),(#191304,#191305),(#191306,#191307),
(#191308,#191309),(#191310,#191311),(#191312,#191313),(#191314,#191315),
(#191316,#191317),(#191318,#191319),(#191320,#191321),(#191322,#191323),
(#191324,#191325),(#191326,#191327),(#191328,#191329),(#191330,#191331),
(#191332,#191333),(#191334,#191335),(#191336,#191337),(#191338,#191339),
(#191340,#191341),(#191342,#191343),(#191344,#191345),(#191346,#191347),
(#191348,#191349),(#191350,#191351),(#191352,#191353),(#191354,#191355),
(#191356,#191357),(#191358,#191359),(#191360,#191361),(#191362,#191363),
(#191364,#191365),(#191366,#191367),(#191368,#191369),(#191370,#191371),
(#191372,#191373),(#191374,#191375),(#191376,#191377),(#191378,#191379),
(#191380,#191381),(#191382,#191383),(#191384,#191385),(#191386,#191387),
(#191388,#191389),(#191390,#191391),(#191392,#191393),(#191394,#191395),
(#191396,#191397),(#191398,#191399),(#191400,#191401),(#191402,#191403),
(#191404,#191405),(#191406,#191407),(#191408,#191409),(#191410,#191411),
(#191412,#191413),(#191414,#191415),(#191416,#191417),(#191418,#191419),
(#191420,#191421),(#191422,#191423),(#191424,#191425),(#191426,#191427),
(#191428,#191429),(#191430,#191431),(#191432,#191433),(#191434,#191435),
(#191436,#191437),(#191438,#191439),(#191440,#191441),(#191442,#191443),
(#191444,#191445),(#191446,#191447),(#191448,#191449),(#191450,#191451),
(#191452,#191453),(#191454,#191455),(#191456,#191457),(#191458,#191459),
(#191460,#191461),(#191462,#191463),(#191464,#191465),(#191466,#191467),
(#191468,#191469),(#191470,#191471),(#191472,#191473),(#191474,#191475),
(#191476,#191477),(#191478,#191479),(#191480,#191481),(#191482,#191483),
(#191484,#191485),(#191486,#191487),(#191488,#191489),(#191490,#191491),
(#191492,#191493),(#191494,#191495),(#191496,#191497),(#191498,#191499),
(#191500,#191501),(#191502,#191503),(#191504,#191505),(#191506,#191507),
(#191508,#191509),(#191510,#191511),(#191512,#191513),(#191514,#191515),
(#191516,#191517),(#191518,#191519),(#191520,#191521),(#191522,#191523),
(#191524,#191525),(#191526,#191527),(#191528,#191529),(#191530,#191531),
(#191532,#191533),(#191534,#191535),(#191536,#191537),(#191538,#191539),
(#191540,#191541),(#191542,#191543),(#191544,#191545),(#191546,#191547),
(#191548,#191549),(#191550,#191551),(#191552,#191553),(#191554,#191555),
(#191556,#191557),(#191558,#191559),(#191560,#191561),(#191562,#191563),
(#191564,#191565),(#191566,#191567),(#191568,#191569),(#191570,#191571),
(#191572,#191573),(#191574,#191575),(#191576,#191577),(#191578,#191579),
(#191580,#191581),(#191582,#191583)),.UNSPECIFIED.,.F.,.F.,.F.)
B_SPLINE_SURFACE_WITH_KNOTS((6,1,1,1,1,1,1,1,1,1,1,1,1,1,1,1,1,1,1,1,1,
1,1,1,1,1,1,1,1,1,1,1,1,1,1,1,1,1,1,1,1,1,1,1,1,1,1,1,1,1,1,1,1,1,1,1,1,
1,1,1,1,1,1,1,1,1,1,1,1,1,1,1,1,1,1,1,1,1,1,1,1,1,1,1,1,1,1,1,1,1,1,1,1,
1,1,1,1,1,1,1,1,1,1,1,1,1,1,1,1,1,1,1,1,1,1,1,1,1,1,1,1,1,1,1,1,1,1,1,1,
1,1,1,1,1,1,1,1,1,1,1,1,1,1,1,1,1,1,1,1,1,1,1,1,1,1,1,1,1,1,1,1,1,1,1,1,
1,1,1,1,1,1,1,1,1,1,1,1,1,1,1,1,1,1,1,1,1,1,1,1,1,1,1,1,1,1,1,1,1,1,1,6),
(2,2),(0.,0.005,0.01,0.015,0.02,0.025,0.03,0.035,0.04,0.045,0.05,0.055,
0.06,0.065,0.07,0.075,0.08,0.085,0.09,0.095,0.1,0.105,0.11,0.115,0.12,0.125,
0.13,0.135,0.14,0.145,0.15,0.155,0.16,0.165,0.17,0.175,0.18,0.185,0.19,
0.195,0.2,0.205,0.21,0.215,0.22,0.225,0.23,0.235,0.24,0.245,0.25,0.255,
0.26,0.265,0.27,0.275,0.28,0.285,0.29,0.295,0.3,0.305,0.31,0.315,0.32,0.325,
0.33,0.335,0.34,0.345,0.35,0.355,0.36,0.365,0.37,0.375,0.38,0.385,0.39,
0.395,0.4,0.405,0.41,0.415,0.42,0.425,0.43,0.435,0.44,0.445,0.45,0.455,
0.46,0.465,0.47,0.475,0.48,0.485,0.49,0.495,0.5,0.505,0.51,0.515,0.52,0.525,
0.53,0.535,0.54,0.545,0.55,0.555,0.56,0.565,0.57,0.575,0.58,0.585,0.59,
0.595,0.6,0.605,0.61,0.615,0.62,0.625,0.63,0.635,0.64,0.645,0.65,0.655,
0.66,0.665,0.67,0.675,0.68,0.685,0.690000000000001,0.695000000000001,0.700000000000001,
0.705000000000001,0.710000000000001,0.715000000000001,0.720000000000001,
0.725000000000001,0.730000000000001,0.735000000000001,0.740000000000001,
0.745000000000001,0.750000000000001,0.755000000000001,0.760000000000001,
0.765000000000001,0.770000000000001,0.775000000000001,0.780000000000001,
0.785000000000001,0.790000000000001,0.795000000000001,0.800000000000001,
0.805000000000001,0.810000000000001,0.815000000000001,0.820000000000001,
0.825000000000001,0.830000000000001,0.835000000000001,0.840000000000001,
0.845000000000001,0.850000000000001,0.855000000000001,0.860000000000001,
0.865000000000001,0.870000000000001,0.875000000000001,0.880000000000001,
0.885000000000001,0.890000000000001,0.895000000000001,0.900000000000001,
0.905000000000001,0.910000000000001,0.915000000000001,0.920000000000001,
0.925000000000001,0.930000000000001,0.935000000000001,0.940000000000001,
0.945000000000001,0.950000000000001,0.955000000000001,0.960000000000001,
0.965000000000001,0.970000000000001,0.975000000000001,0.980000000000001,
0.985000000000001,0.990000000000001,0.995000000000001,1.),(0.,1.2),
 .UNSPECIFIED.)
GEOMETRIC_REPRESENTATION_ITEM()
RATIONAL_B_SPLINE_SURFACE(((1.,1.),(1.,1.),(1.,1.),(1.,1.),(1.,1.),(1.,
1.),(1.,1.),(1.,1.),(1.,1.),(1.,1.),(1.,1.),(1.,1.),(1.,1.),(1.,1.),(1.,
1.),(1.,1.),(1.,1.),(1.,1.),(1.,1.),(1.,1.),(1.,1.),(1.,1.),(1.,1.),(1.,
1.),(1.,1.),(1.,1.),(1.,1.),(1.,1.),(1.,1.),(1.,1.),(1.,1.),(1.,1.),(1.,
1.),(1.,1.),(1.,1.),(1.,1.),(1.,1.),(1.,1.),(1.,1.),(1.,1.),(1.,1.),(1.,
1.),(1.,1.),(1.,1.),(1.,1.),(1.,1.),(1.,1.),(1.,1.),(1.,1.),(1.,1.),(1.,
1.),(1.,1.),(1.,1.),(1.,1.),(1.,1.),(1.,1.),(1.,1.),(1.,1.),(1.,1.),(1.,
1.),(1.,1.),(1.,1.),(1.,1.),(1.,1.),(1.,1.),(1.,1.),(1.,1.),(1.,1.),(1.,
1.),(1.,1.),(1.,1.),(1.,1.),(1.,1.),(1.,1.),(1.,1.),(1.,1.),(1.,1.),(1.,
1.),(1.,1.),(1.,1.),(1.,1.),(1.,1.),(1.,1.),(1.,1.),(1.,1.),(1.,1.),(1.,
1.),(1.,1.),(1.,1.),(1.,1.),(1.,1.),(1.,1.),(1.,1.),(1.,1.),(1.,1.),(1.,
1.),(1.,1.),(1.,1.),(1.,1.),(1.,1.),(1.,1.),(1.,1.),(1.,1.),(1.,1.),(1.,
1.),(1.,1.),(1.,1.),(1.,1.),(1.,1.),(1.,1.),(1.,1.),(1.,1.),(1.,1.),(1.,
1.),(1.,1.),(1.,1.),(1.,1.),(1.,1.),(1.,1.),(1.,1.),(1.,1.),(1.,1.),(1.,
1.),(1.,1.),(1.,1.),(1.,1.),(1.,1.),(1.,1.),(1.,1.),(1.,1.),(1.,1.),(1.,
1.),(1.,1.),(1.,1.),(1.,1.),(1.,1.),(1.,1.),(1.,1.),(1.,1.),(1.,1.),(1.,
1.),(1.,1.),(1.,1.),(1.,1.),(1.,1.),(1.,1.),(1.,1.),(1.,1.),(1.,1.),(1.,
1.),(1.,1.),(1.,1.),(1.,1.),(1.,1.),(1.,1.),(1.,1.),(1.,1.),(1.,1.),(1.,
1.),(1.,1.),(1.,1.),(1.,1.),(1.,1.),(1.,1.),(1.,1.),(1.,1.),(1.,1.),(1.,
1.),(1.,1.),(1.,1.),(1.,1.),(1.,1.),(1.,1.),(1.,1.),(1.,1.),(1.,1.),(1.,
1.),(1.,1.),(1.,1.),(1.,1.),(1.,1.),(1.,1.),(1.,1.),(1.,1.),(1.,1.),(1.,
1.),(1.,1.),(1.,1.),(1.,1.),(1.,1.),(1.,1.),(1.,1.),(1.,1.),(1.,1.),(1.,
1.),(1.,1.),(1.,1.),(1.,1.),(1.,1.),(1.,1.),(1.,1.),(1.,1.),(1.,1.),(1.,
1.),(1.,1.)))
REPRESENTATION_ITEM('')
SURFACE()
);
#1037=(
BOUNDED_SURFACE()
B_SPLINE_SURFACE(5,1,((#191795,#191796),(#191797,#191798),(#191799,#191800),
(#191801,#191802),(#191803,#191804),(#191805,#191806),(#191807,#191808),
(#191809,#191810),(#191811,#191812),(#191813,#191814),(#191815,#191816),
(#191817,#191818),(#191819,#191820),(#191821,#191822),(#191823,#191824),
(#191825,#191826),(#191827,#191828),(#191829,#191830),(#191831,#191832),
(#191833,#191834),(#191835,#191836),(#191837,#191838),(#191839,#191840),
(#191841,#191842),(#191843,#191844),(#191845,#191846),(#191847,#191848),
(#191849,#191850),(#191851,#191852),(#191853,#191854),(#191855,#191856),
(#191857,#191858),(#191859,#191860),(#191861,#191862),(#191863,#191864),
(#191865,#191866),(#191867,#191868),(#191869,#191870),(#191871,#191872),
(#191873,#191874),(#191875,#191876),(#191877,#191878),(#191879,#191880),
(#191881,#191882),(#191883,#191884),(#191885,#191886),(#191887,#191888),
(#191889,#191890),(#191891,#191892),(#191893,#191894),(#191895,#191896),
(#191897,#191898),(#191899,#191900),(#191901,#191902),(#191903,#191904),
(#191905,#191906),(#191907,#191908),(#191909,#191910),(#191911,#191912),
(#191913,#191914),(#191915,#191916),(#191917,#191918),(#191919,#191920),
(#191921,#191922),(#191923,#191924),(#191925,#191926),(#191927,#191928),
(#191929,#191930),(#191931,#191932),(#191933,#191934),(#191935,#191936),
(#191937,#191938),(#191939,#191940),(#191941,#191942),(#191943,#191944),
(#191945,#191946),(#191947,#191948),(#191949,#191950),(#191951,#191952),
(#191953,#191954),(#191955,#191956),(#191957,#191958),(#191959,#191960),
(#191961,#191962),(#191963,#191964),(#191965,#191966),(#191967,#191968),
(#191969,#191970),(#191971,#191972),(#191973,#191974),(#191975,#191976),
(#191977,#191978),(#191979,#191980),(#191981,#191982),(#191983,#191984),
(#191985,#191986),(#191987,#191988),(#191989,#191990),(#191991,#191992),
(#191993,#191994),(#191995,#191996),(#191997,#191998),(#191999,#192000),
(#192001,#192002),(#192003,#192004),(#192005,#192006),(#192007,#192008),
(#192009,#192010),(#192011,#192012),(#192013,#192014),(#192015,#192016),
(#192017,#192018),(#192019,#192020),(#192021,#192022),(#192023,#192024),
(#192025,#192026),(#192027,#192028),(#192029,#192030),(#192031,#192032),
(#192033,#192034),(#192035,#192036),(#192037,#192038),(#192039,#192040),
(#192041,#192042),(#192043,#192044),(#192045,#192046),(#192047,#192048),
(#192049,#192050),(#192051,#192052),(#192053,#192054),(#192055,#192056),
(#192057,#192058),(#192059,#192060),(#192061,#192062),(#192063,#192064),
(#192065,#192066),(#192067,#192068),(#192069,#192070),(#192071,#192072),
(#192073,#192074),(#192075,#192076),(#192077,#192078),(#192079,#192080),
(#192081,#192082),(#192083,#192084),(#192085,#192086),(#192087,#192088),
(#192089,#192090),(#192091,#192092),(#192093,#192094),(#192095,#192096),
(#192097,#192098),(#192099,#192100),(#192101,#192102),(#192103,#192104),
(#192105,#192106),(#192107,#192108),(#192109,#192110),(#192111,#192112),
(#192113,#192114),(#192115,#192116),(#192117,#192118),(#192119,#192120),
(#192121,#192122),(#192123,#192124),(#192125,#192126),(#192127,#192128),
(#192129,#192130),(#192131,#192132),(#192133,#192134),(#192135,#192136),
(#192137,#192138),(#192139,#192140),(#192141,#192142),(#192143,#192144),
(#192145,#192146),(#192147,#192148),(#192149,#192150),(#192151,#192152),
(#192153,#192154),(#192155,#192156),(#192157,#192158),(#192159,#192160),
(#192161,#192162),(#192163,#192164),(#192165,#192166),(#192167,#192168),
(#192169,#192170),(#192171,#192172),(#192173,#192174),(#192175,#192176),
(#192177,#192178),(#192179,#192180),(#192181,#192182),(#192183,#192184),
(#192185,#192186),(#192187,#192188),(#192189,#192190),(#192191,#192192),
(#192193,#192194),(#192195,#192196),(#192197,#192198),(#192199,#192200),
(#192201,#192202),(#192203,#192204)),.UNSPECIFIED.,.F.,.F.,.F.)
B_SPLINE_SURFACE_WITH_KNOTS((6,1,1,1,1,1,1,1,1,1,1,1,1,1,1,1,1,1,1,1,1,
1,1,1,1,1,1,1,1,1,1,1,1,1,1,1,1,1,1,1,1,1,1,1,1,1,1,1,1,1,1,1,1,1,1,1,1,
1,1,1,1,1,1,1,1,1,1,1,1,1,1,1,1,1,1,1,1,1,1,1,1,1,1,1,1,1,1,1,1,1,1,1,1,
1,1,1,1,1,1,1,1,1,1,1,1,1,1,1,1,1,1,1,1,1,1,1,1,1,1,1,1,1,1,1,1,1,1,1,1,
1,1,1,1,1,1,1,1,1,1,1,1,1,1,1,1,1,1,1,1,1,1,1,1,1,1,1,1,1,1,1,1,1,1,1,1,
1,1,1,1,1,1,1,1,1,1,1,1,1,1,1,1,1,1,1,1,1,1,1,1,1,1,1,1,1,1,1,1,1,1,1,6),
(2,2),(-1.,-0.995000000000001,-0.990000000000001,-0.985000000000001,-0.980000000000001,
-0.975000000000001,-0.970000000000001,-0.965000000000001,-0.960000000000001,
-0.955000000000001,-0.950000000000001,-0.945000000000001,-0.940000000000001,
-0.935000000000001,-0.930000000000001,-0.925000000000001,-0.920000000000001,
-0.915000000000001,-0.910000000000001,-0.905000000000001,-0.900000000000001,
-0.895000000000001,-0.890000000000001,-0.885000000000001,-0.880000000000001,
-0.875000000000001,-0.870000000000001,-0.865000000000001,-0.860000000000001,
-0.855000000000001,-0.850000000000001,-0.845000000000001,-0.840000000000001,
-0.835000000000001,-0.830000000000001,-0.825000000000001,-0.820000000000001,
-0.815000000000001,-0.810000000000001,-0.805000000000001,-0.800000000000001,
-0.795000000000001,-0.790000000000001,-0.785000000000001,-0.780000000000001,
-0.775000000000001,-0.770000000000001,-0.765000000000001,-0.760000000000001,
-0.755000000000001,-0.750000000000001,-0.745000000000001,-0.740000000000001,
-0.735000000000001,-0.730000000000001,-0.725000000000001,-0.720000000000001,
-0.715000000000001,-0.710000000000001,-0.705000000000001,-0.700000000000001,
-0.695000000000001,-0.690000000000001,-0.685,-0.68,-0.675,-0.67,-0.665,
-0.66,-0.655,-0.65,-0.645,-0.64,-0.635,-0.63,-0.625,-0.62,-0.615,-0.61,
-0.605,-0.6,-0.595,-0.59,-0.585,-0.58,-0.575,-0.57,-0.565,-0.56,-0.555,
-0.55,-0.545,-0.54,-0.535,-0.53,-0.525,-0.52,-0.515,-0.51,-0.505,-0.5,-0.495,
-0.49,-0.485,-0.48,-0.475,-0.47,-0.465,-0.46,-0.455,-0.45,-0.445,-0.44,
-0.435,-0.43,-0.425,-0.42,-0.415,-0.41,-0.405,-0.4,-0.395,-0.39,-0.385,
-0.38,-0.375,-0.37,-0.365,-0.36,-0.355,-0.35,-0.345,-0.34,-0.335,-0.33,
-0.325,-0.32,-0.315,-0.31,-0.305,-0.3,-0.295,-0.29,-0.285,-0.28,-0.275,
-0.27,-0.265,-0.26,-0.255,-0.25,-0.245,-0.24,-0.235,-0.23,-0.225,-0.22,
-0.215,-0.21,-0.205,-0.2,-0.195,-0.19,-0.185,-0.18,-0.175,-0.17,-0.165,
-0.16,-0.155,-0.15,-0.145,-0.14,-0.135,-0.13,-0.125,-0.12,-0.115,-0.11,
-0.105,-0.1,-0.095,-0.09,-0.085,-0.08,-0.075,-0.07,-0.065,-0.06,-0.055,
-0.05,-0.045,-0.04,-0.035,-0.03,-0.025,-0.02,-0.015,-0.01,-0.005,0.),(0.,
1.2),.UNSPECIFIED.)
GEOMETRIC_REPRESENTATION_ITEM()
RATIONAL_B_SPLINE_SURFACE(((1.,1.),(1.,1.),(1.,1.),(1.,1.),(1.,1.),(1.,
1.),(1.,1.),(1.,1.),(1.,1.),(1.,1.),(1.,1.),(1.,1.),(1.,1.),(1.,1.),(1.,
1.),(1.,1.),(1.,1.),(1.,1.),(1.,1.),(1.,1.),(1.,1.),(1.,1.),(1.,1.),(1.,
1.),(1.,1.),(1.,1.),(1.,1.),(1.,1.),(1.,1.),(1.,1.),(1.,1.),(1.,1.),(1.,
1.),(1.,1.),(1.,1.),(1.,1.),(1.,1.),(1.,1.),(1.,1.),(1.,1.),(1.,1.),(1.,
1.),(1.,1.),(1.,1.),(1.,1.),(1.,1.),(1.,1.),(1.,1.),(1.,1.),(1.,1.),(1.,
1.),(1.,1.),(1.,1.),(1.,1.),(1.,1.),(1.,1.),(1.,1.),(1.,1.),(1.,1.),(1.,
1.),(1.,1.),(1.,1.),(1.,1.),(1.,1.),(1.,1.),(1.,1.),(1.,1.),(1.,1.),(1.,
1.),(1.,1.),(1.,1.),(1.,1.),(1.,1.),(1.,1.),(1.,1.),(1.,1.),(1.,1.),(1.,
1.),(1.,1.),(1.,1.),(1.,1.),(1.,1.),(1.,1.),(1.,1.),(1.,1.),(1.,1.),(1.,
1.),(1.,1.),(1.,1.),(1.,1.),(1.,1.),(1.,1.),(1.,1.),(1.,1.),(1.,1.),(1.,
1.),(1.,1.),(1.,1.),(1.,1.),(1.,1.),(1.,1.),(1.,1.),(1.,1.),(1.,1.),(1.,
1.),(1.,1.),(1.,1.),(1.,1.),(1.,1.),(1.,1.),(1.,1.),(1.,1.),(1.,1.),(1.,
1.),(1.,1.),(1.,1.),(1.,1.),(1.,1.),(1.,1.),(1.,1.),(1.,1.),(1.,1.),(1.,
1.),(1.,1.),(1.,1.),(1.,1.),(1.,1.),(1.,1.),(1.,1.),(1.,1.),(1.,1.),(1.,
1.),(1.,1.),(1.,1.),(1.,1.),(1.,1.),(1.,1.),(1.,1.),(1.,1.),(1.,1.),(1.,
1.),(1.,1.),(1.,1.),(1.,1.),(1.,1.),(1.,1.),(1.,1.),(1.,1.),(1.,1.),(1.,
1.),(1.,1.),(1.,1.),(1.,1.),(1.,1.),(1.,1.),(1.,1.),(1.,1.),(1.,1.),(1.,
1.),(1.,1.),(1.,1.),(1.,1.),(1.,1.),(1.,1.),(1.,1.),(1.,1.),(1.,1.),(1.,
1.),(1.,1.),(1.,1.),(1.,1.),(1.,1.),(1.,1.),(1.,1.),(1.,1.),(1.,1.),(1.,
1.),(1.,1.),(1.,1.),(1.,1.),(1.,1.),(1.,1.),(1.,1.),(1.,1.),(1.,1.),(1.,
1.),(1.,1.),(1.,1.),(1.,1.),(1.,1.),(1.,1.),(1.,1.),(1.,1.),(1.,1.),(1.,
1.),(1.,1.),(1.,1.),(1.,1.),(1.,1.),(1.,1.),(1.,1.),(1.,1.),(1.,1.),(1.,
1.),(1.,1.)))
REPRESENTATION_ITEM('')
SURFACE()
);
#1038=(
BOUNDED_SURFACE()
B_SPLINE_SURFACE(5,1,((#192412,#192413),(#192414,#192415),(#192416,#192417),
(#192418,#192419),(#192420,#192421),(#192422,#192423),(#192424,#192425),
(#192426,#192427),(#192428,#192429),(#192430,#192431),(#192432,#192433),
(#192434,#192435),(#192436,#192437),(#192438,#192439),(#192440,#192441),
(#192442,#192443),(#192444,#192445),(#192446,#192447),(#192448,#192449),
(#192450,#192451),(#192452,#192453),(#192454,#192455),(#192456,#192457),
(#192458,#192459),(#192460,#192461),(#192462,#192463),(#192464,#192465),
(#192466,#192467),(#192468,#192469),(#192470,#192471),(#192472,#192473),
(#192474,#192475),(#192476,#192477),(#192478,#192479),(#192480,#192481),
(#192482,#192483),(#192484,#192485),(#192486,#192487),(#192488,#192489),
(#192490,#192491),(#192492,#192493),(#192494,#192495),(#192496,#192497),
(#192498,#192499),(#192500,#192501),(#192502,#192503),(#192504,#192505),
(#192506,#192507),(#192508,#192509),(#192510,#192511),(#192512,#192513),
(#192514,#192515),(#192516,#192517),(#192518,#192519),(#192520,#192521),
(#192522,#192523),(#192524,#192525),(#192526,#192527),(#192528,#192529),
(#192530,#192531),(#192532,#192533),(#192534,#192535),(#192536,#192537),
(#192538,#192539),(#192540,#192541),(#192542,#192543),(#192544,#192545),
(#192546,#192547),(#192548,#192549),(#192550,#192551),(#192552,#192553),
(#192554,#192555),(#192556,#192557),(#192558,#192559),(#192560,#192561),
(#192562,#192563),(#192564,#192565),(#192566,#192567),(#192568,#192569),
(#192570,#192571),(#192572,#192573),(#192574,#192575),(#192576,#192577),
(#192578,#192579),(#192580,#192581),(#192582,#192583),(#192584,#192585),
(#192586,#192587),(#192588,#192589),(#192590,#192591),(#192592,#192593),
(#192594,#192595),(#192596,#192597),(#192598,#192599),(#192600,#192601),
(#192602,#192603),(#192604,#192605),(#192606,#192607),(#192608,#192609),
(#192610,#192611),(#192612,#192613),(#192614,#192615),(#192616,#192617),
(#192618,#192619),(#192620,#192621),(#192622,#192623),(#192624,#192625),
(#192626,#192627),(#192628,#192629),(#192630,#192631),(#192632,#192633),
(#192634,#192635),(#192636,#192637),(#192638,#192639),(#192640,#192641),
(#192642,#192643),(#192644,#192645),(#192646,#192647),(#192648,#192649),
(#192650,#192651),(#192652,#192653),(#192654,#192655),(#192656,#192657),
(#192658,#192659),(#192660,#192661),(#192662,#192663),(#192664,#192665),
(#192666,#192667),(#192668,#192669),(#192670,#192671),(#192672,#192673),
(#192674,#192675),(#192676,#192677),(#192678,#192679),(#192680,#192681),
(#192682,#192683),(#192684,#192685),(#192686,#192687),(#192688,#192689),
(#192690,#192691),(#192692,#192693),(#192694,#192695),(#192696,#192697),
(#192698,#192699),(#192700,#192701),(#192702,#192703),(#192704,#192705),
(#192706,#192707),(#192708,#192709),(#192710,#192711),(#192712,#192713),
(#192714,#192715),(#192716,#192717),(#192718,#192719),(#192720,#192721),
(#192722,#192723),(#192724,#192725),(#192726,#192727),(#192728,#192729),
(#192730,#192731),(#192732,#192733),(#192734,#192735),(#192736,#192737),
(#192738,#192739),(#192740,#192741),(#192742,#192743),(#192744,#192745),
(#192746,#192747),(#192748,#192749),(#192750,#192751),(#192752,#192753),
(#192754,#192755),(#192756,#192757),(#192758,#192759),(#192760,#192761),
(#192762,#192763),(#192764,#192765),(#192766,#192767),(#192768,#192769),
(#192770,#192771),(#192772,#192773),(#192774,#192775),(#192776,#192777),
(#192778,#192779),(#192780,#192781),(#192782,#192783),(#192784,#192785),
(#192786,#192787),(#192788,#192789),(#192790,#192791),(#192792,#192793),
(#192794,#192795),(#192796,#192797),(#192798,#192799),(#192800,#192801),
(#192802,#192803),(#192804,#192805),(#192806,#192807),(#192808,#192809),
(#192810,#192811),(#192812,#192813),(#192814,#192815),(#192816,#192817),
(#192818,#192819),(#192820,#192821)),.UNSPECIFIED.,.F.,.F.,.F.)
B_SPLINE_SURFACE_WITH_KNOTS((6,1,1,1,1,1,1,1,1,1,1,1,1,1,1,1,1,1,1,1,1,
1,1,1,1,1,1,1,1,1,1,1,1,1,1,1,1,1,1,1,1,1,1,1,1,1,1,1,1,1,1,1,1,1,1,1,1,
1,1,1,1,1,1,1,1,1,1,1,1,1,1,1,1,1,1,1,1,1,1,1,1,1,1,1,1,1,1,1,1,1,1,1,1,
1,1,1,1,1,1,1,1,1,1,1,1,1,1,1,1,1,1,1,1,1,1,1,1,1,1,1,1,1,1,1,1,1,1,1,1,
1,1,1,1,1,1,1,1,1,1,1,1,1,1,1,1,1,1,1,1,1,1,1,1,1,1,1,1,1,1,1,1,1,1,1,1,
1,1,1,1,1,1,1,1,1,1,1,1,1,1,1,1,1,1,1,1,1,1,1,1,1,1,1,1,1,1,1,1,1,1,1,6),
(2,2),(0.,0.005,0.01,0.015,0.02,0.025,0.03,0.035,0.04,0.045,0.05,0.055,
0.06,0.065,0.07,0.075,0.08,0.085,0.09,0.095,0.1,0.105,0.11,0.115,0.12,0.125,
0.13,0.135,0.14,0.145,0.15,0.155,0.16,0.165,0.17,0.175,0.18,0.185,0.19,
0.195,0.2,0.205,0.21,0.215,0.22,0.225,0.23,0.235,0.24,0.245,0.25,0.255,
0.26,0.265,0.27,0.275,0.28,0.285,0.29,0.295,0.3,0.305,0.31,0.315,0.32,0.325,
0.33,0.335,0.34,0.345,0.35,0.355,0.36,0.365,0.37,0.375,0.38,0.385,0.39,
0.395,0.4,0.405,0.41,0.415,0.42,0.425,0.43,0.435,0.44,0.445,0.45,0.455,
0.46,0.465,0.47,0.475,0.48,0.485,0.49,0.495,0.5,0.505,0.51,0.515,0.52,0.525,
0.53,0.535,0.54,0.545,0.55,0.555,0.56,0.565,0.57,0.575,0.58,0.585,0.59,
0.595,0.6,0.605,0.61,0.615,0.62,0.625,0.63,0.635,0.64,0.645,0.65,0.655,
0.66,0.665,0.67,0.675,0.68,0.685,0.690000000000001,0.695000000000001,0.700000000000001,
0.705000000000001,0.710000000000001,0.715000000000001,0.720000000000001,
0.725000000000001,0.730000000000001,0.735000000000001,0.740000000000001,
0.745000000000001,0.750000000000001,0.755000000000001,0.760000000000001,
0.765000000000001,0.770000000000001,0.775000000000001,0.780000000000001,
0.785000000000001,0.790000000000001,0.795000000000001,0.800000000000001,
0.805000000000001,0.810000000000001,0.815000000000001,0.820000000000001,
0.825000000000001,0.830000000000001,0.835000000000001,0.840000000000001,
0.845000000000001,0.850000000000001,0.855000000000001,0.860000000000001,
0.865000000000001,0.870000000000001,0.875000000000001,0.880000000000001,
0.885000000000001,0.890000000000001,0.895000000000001,0.900000000000001,
0.905000000000001,0.910000000000001,0.915000000000001,0.920000000000001,
0.925000000000001,0.930000000000001,0.935000000000001,0.940000000000001,
0.945000000000001,0.950000000000001,0.955000000000001,0.960000000000001,
0.965000000000001,0.970000000000001,0.975000000000001,0.980000000000001,
0.985000000000001,0.990000000000001,0.995000000000001,1.),(0.,1.2),
 .UNSPECIFIED.)
GEOMETRIC_REPRESENTATION_ITEM()
RATIONAL_B_SPLINE_SURFACE(((1.,1.),(1.,1.),(1.,1.),(1.,1.),(1.,1.),(1.,
1.),(1.,1.),(1.,1.),(1.,1.),(1.,1.),(1.,1.),(1.,1.),(1.,1.),(1.,1.),(1.,
1.),(1.,1.),(1.,1.),(1.,1.),(1.,1.),(1.,1.),(1.,1.),(1.,1.),(1.,1.),(1.,
1.),(1.,1.),(1.,1.),(1.,1.),(1.,1.),(1.,1.),(1.,1.),(1.,1.),(1.,1.),(1.,
1.),(1.,1.),(1.,1.),(1.,1.),(1.,1.),(1.,1.),(1.,1.),(1.,1.),(1.,1.),(1.,
1.),(1.,1.),(1.,1.),(1.,1.),(1.,1.),(1.,1.),(1.,1.),(1.,1.),(1.,1.),(1.,
1.),(1.,1.),(1.,1.),(1.,1.),(1.,1.),(1.,1.),(1.,1.),(1.,1.),(1.,1.),(1.,
1.),(1.,1.),(1.,1.),(1.,1.),(1.,1.),(1.,1.),(1.,1.),(1.,1.),(1.,1.),(1.,
1.),(1.,1.),(1.,1.),(1.,1.),(1.,1.),(1.,1.),(1.,1.),(1.,1.),(1.,1.),(1.,
1.),(1.,1.),(1.,1.),(1.,1.),(1.,1.),(1.,1.),(1.,1.),(1.,1.),(1.,1.),(1.,
1.),(1.,1.),(1.,1.),(1.,1.),(1.,1.),(1.,1.),(1.,1.),(1.,1.),(1.,1.),(1.,
1.),(1.,1.),(1.,1.),(1.,1.),(1.,1.),(1.,1.),(1.,1.),(1.,1.),(1.,1.),(1.,
1.),(1.,1.),(1.,1.),(1.,1.),(1.,1.),(1.,1.),(1.,1.),(1.,1.),(1.,1.),(1.,
1.),(1.,1.),(1.,1.),(1.,1.),(1.,1.),(1.,1.),(1.,1.),(1.,1.),(1.,1.),(1.,
1.),(1.,1.),(1.,1.),(1.,1.),(1.,1.),(1.,1.),(1.,1.),(1.,1.),(1.,1.),(1.,
1.),(1.,1.),(1.,1.),(1.,1.),(1.,1.),(1.,1.),(1.,1.),(1.,1.),(1.,1.),(1.,
1.),(1.,1.),(1.,1.),(1.,1.),(1.,1.),(1.,1.),(1.,1.),(1.,1.),(1.,1.),(1.,
1.),(1.,1.),(1.,1.),(1.,1.),(1.,1.),(1.,1.),(1.,1.),(1.,1.),(1.,1.),(1.,
1.),(1.,1.),(1.,1.),(1.,1.),(1.,1.),(1.,1.),(1.,1.),(1.,1.),(1.,1.),(1.,
1.),(1.,1.),(1.,1.),(1.,1.),(1.,1.),(1.,1.),(1.,1.),(1.,1.),(1.,1.),(1.,
1.),(1.,1.),(1.,1.),(1.,1.),(1.,1.),(1.,1.),(1.,1.),(1.,1.),(1.,1.),(1.,
1.),(1.,1.),(1.,1.),(1.,1.),(1.,1.),(1.,1.),(1.,1.),(1.,1.),(1.,1.),(1.,
1.),(1.,1.),(1.,1.),(1.,1.),(1.,1.),(1.,1.),(1.,1.),(1.,1.),(1.,1.),(1.,
1.),(1.,1.)))
REPRESENTATION_ITEM('')
SURFACE()
);
#1039=(
BOUNDED_SURFACE()
B_SPLINE_SURFACE(5,1,((#193033,#193034),(#193035,#193036),(#193037,#193038),
(#193039,#193040),(#193041,#193042),(#193043,#193044),(#193045,#193046),
(#193047,#193048),(#193049,#193050),(#193051,#193052),(#193053,#193054),
(#193055,#193056),(#193057,#193058),(#193059,#193060),(#193061,#193062),
(#193063,#193064),(#193065,#193066),(#193067,#193068),(#193069,#193070),
(#193071,#193072),(#193073,#193074),(#193075,#193076),(#193077,#193078),
(#193079,#193080),(#193081,#193082),(#193083,#193084),(#193085,#193086),
(#193087,#193088),(#193089,#193090),(#193091,#193092),(#193093,#193094),
(#193095,#193096),(#193097,#193098),(#193099,#193100),(#193101,#193102),
(#193103,#193104),(#193105,#193106),(#193107,#193108),(#193109,#193110),
(#193111,#193112),(#193113,#193114),(#193115,#193116),(#193117,#193118),
(#193119,#193120),(#193121,#193122),(#193123,#193124),(#193125,#193126),
(#193127,#193128),(#193129,#193130),(#193131,#193132),(#193133,#193134),
(#193135,#193136),(#193137,#193138),(#193139,#193140),(#193141,#193142),
(#193143,#193144),(#193145,#193146),(#193147,#193148),(#193149,#193150),
(#193151,#193152),(#193153,#193154),(#193155,#193156),(#193157,#193158),
(#193159,#193160),(#193161,#193162),(#193163,#193164),(#193165,#193166),
(#193167,#193168),(#193169,#193170),(#193171,#193172),(#193173,#193174),
(#193175,#193176),(#193177,#193178),(#193179,#193180),(#193181,#193182),
(#193183,#193184),(#193185,#193186),(#193187,#193188),(#193189,#193190),
(#193191,#193192),(#193193,#193194),(#193195,#193196),(#193197,#193198),
(#193199,#193200),(#193201,#193202),(#193203,#193204),(#193205,#193206),
(#193207,#193208),(#193209,#193210),(#193211,#193212),(#193213,#193214),
(#193215,#193216),(#193217,#193218),(#193219,#193220),(#193221,#193222),
(#193223,#193224),(#193225,#193226),(#193227,#193228),(#193229,#193230),
(#193231,#193232),(#193233,#193234),(#193235,#193236),(#193237,#193238),
(#193239,#193240),(#193241,#193242),(#193243,#193244),(#193245,#193246),
(#193247,#193248),(#193249,#193250),(#193251,#193252),(#193253,#193254),
(#193255,#193256),(#193257,#193258),(#193259,#193260),(#193261,#193262),
(#193263,#193264),(#193265,#193266),(#193267,#193268),(#193269,#193270),
(#193271,#193272),(#193273,#193274),(#193275,#193276),(#193277,#193278),
(#193279,#193280),(#193281,#193282),(#193283,#193284),(#193285,#193286),
(#193287,#193288),(#193289,#193290),(#193291,#193292),(#193293,#193294),
(#193295,#193296),(#193297,#193298),(#193299,#193300),(#193301,#193302),
(#193303,#193304),(#193305,#193306),(#193307,#193308),(#193309,#193310),
(#193311,#193312),(#193313,#193314),(#193315,#193316),(#193317,#193318),
(#193319,#193320),(#193321,#193322),(#193323,#193324),(#193325,#193326),
(#193327,#193328),(#193329,#193330),(#193331,#193332),(#193333,#193334),
(#193335,#193336),(#193337,#193338),(#193339,#193340),(#193341,#193342),
(#193343,#193344),(#193345,#193346),(#193347,#193348),(#193349,#193350),
(#193351,#193352),(#193353,#193354),(#193355,#193356),(#193357,#193358),
(#193359,#193360),(#193361,#193362),(#193363,#193364),(#193365,#193366),
(#193367,#193368),(#193369,#193370),(#193371,#193372),(#193373,#193374),
(#193375,#193376),(#193377,#193378),(#193379,#193380),(#193381,#193382),
(#193383,#193384),(#193385,#193386),(#193387,#193388),(#193389,#193390),
(#193391,#193392),(#193393,#193394),(#193395,#193396),(#193397,#193398),
(#193399,#193400),(#193401,#193402),(#193403,#193404),(#193405,#193406),
(#193407,#193408),(#193409,#193410),(#193411,#193412),(#193413,#193414),
(#193415,#193416),(#193417,#193418),(#193419,#193420),(#193421,#193422),
(#193423,#193424),(#193425,#193426),(#193427,#193428),(#193429,#193430),
(#193431,#193432),(#193433,#193434),(#193435,#193436),(#193437,#193438),
(#193439,#193440),(#193441,#193442)),.UNSPECIFIED.,.F.,.F.,.F.)
B_SPLINE_SURFACE_WITH_KNOTS((6,1,1,1,1,1,1,1,1,1,1,1,1,1,1,1,1,1,1,1,1,
1,1,1,1,1,1,1,1,1,1,1,1,1,1,1,1,1,1,1,1,1,1,1,1,1,1,1,1,1,1,1,1,1,1,1,1,
1,1,1,1,1,1,1,1,1,1,1,1,1,1,1,1,1,1,1,1,1,1,1,1,1,1,1,1,1,1,1,1,1,1,1,1,
1,1,1,1,1,1,1,1,1,1,1,1,1,1,1,1,1,1,1,1,1,1,1,1,1,1,1,1,1,1,1,1,1,1,1,1,
1,1,1,1,1,1,1,1,1,1,1,1,1,1,1,1,1,1,1,1,1,1,1,1,1,1,1,1,1,1,1,1,1,1,1,1,
1,1,1,1,1,1,1,1,1,1,1,1,1,1,1,1,1,1,1,1,1,1,1,1,1,1,1,1,1,1,1,1,1,1,1,6),
(2,2),(-1.,-0.995000000000001,-0.990000000000001,-0.985000000000001,-0.980000000000001,
-0.975000000000001,-0.970000000000001,-0.965000000000001,-0.960000000000001,
-0.955000000000001,-0.950000000000001,-0.945000000000001,-0.940000000000001,
-0.935000000000001,-0.930000000000001,-0.925000000000001,-0.920000000000001,
-0.915000000000001,-0.910000000000001,-0.905000000000001,-0.900000000000001,
-0.895000000000001,-0.890000000000001,-0.885000000000001,-0.880000000000001,
-0.875000000000001,-0.870000000000001,-0.865000000000001,-0.860000000000001,
-0.855000000000001,-0.850000000000001,-0.845000000000001,-0.840000000000001,
-0.835000000000001,-0.830000000000001,-0.825000000000001,-0.820000000000001,
-0.815000000000001,-0.810000000000001,-0.805000000000001,-0.800000000000001,
-0.795000000000001,-0.790000000000001,-0.785000000000001,-0.780000000000001,
-0.775000000000001,-0.770000000000001,-0.765000000000001,-0.760000000000001,
-0.755000000000001,-0.750000000000001,-0.745000000000001,-0.740000000000001,
-0.735000000000001,-0.730000000000001,-0.725000000000001,-0.720000000000001,
-0.715000000000001,-0.710000000000001,-0.705000000000001,-0.700000000000001,
-0.695000000000001,-0.690000000000001,-0.685,-0.68,-0.675,-0.67,-0.665,
-0.66,-0.655,-0.65,-0.645,-0.64,-0.635,-0.63,-0.625,-0.62,-0.615,-0.61,
-0.605,-0.6,-0.595,-0.59,-0.585,-0.58,-0.575,-0.57,-0.565,-0.56,-0.555,
-0.55,-0.545,-0.54,-0.535,-0.53,-0.525,-0.52,-0.515,-0.51,-0.505,-0.5,-0.495,
-0.49,-0.485,-0.48,-0.475,-0.47,-0.465,-0.46,-0.455,-0.45,-0.445,-0.44,
-0.435,-0.43,-0.425,-0.42,-0.415,-0.41,-0.405,-0.4,-0.395,-0.39,-0.385,
-0.38,-0.375,-0.37,-0.365,-0.36,-0.355,-0.35,-0.345,-0.34,-0.335,-0.33,
-0.325,-0.32,-0.315,-0.31,-0.305,-0.3,-0.295,-0.29,-0.285,-0.28,-0.275,
-0.27,-0.265,-0.26,-0.255,-0.25,-0.245,-0.24,-0.235,-0.23,-0.225,-0.22,
-0.215,-0.21,-0.205,-0.2,-0.195,-0.19,-0.185,-0.18,-0.175,-0.17,-0.165,
-0.16,-0.155,-0.15,-0.145,-0.14,-0.135,-0.13,-0.125,-0.12,-0.115,-0.11,
-0.105,-0.1,-0.095,-0.09,-0.085,-0.08,-0.075,-0.07,-0.065,-0.06,-0.055,
-0.05,-0.045,-0.04,-0.035,-0.03,-0.025,-0.02,-0.015,-0.01,-0.005,0.),(0.,
1.2),.UNSPECIFIED.)
GEOMETRIC_REPRESENTATION_ITEM()
RATIONAL_B_SPLINE_SURFACE(((1.,1.),(1.,1.),(1.,1.),(1.,1.),(1.,1.),(1.,
1.),(1.,1.),(1.,1.),(1.,1.),(1.,1.),(1.,1.),(1.,1.),(1.,1.),(1.,1.),(1.,
1.),(1.,1.),(1.,1.),(1.,1.),(1.,1.),(1.,1.),(1.,1.),(1.,1.),(1.,1.),(1.,
1.),(1.,1.),(1.,1.),(1.,1.),(1.,1.),(1.,1.),(1.,1.),(1.,1.),(1.,1.),(1.,
1.),(1.,1.),(1.,1.),(1.,1.),(1.,1.),(1.,1.),(1.,1.),(1.,1.),(1.,1.),(1.,
1.),(1.,1.),(1.,1.),(1.,1.),(1.,1.),(1.,1.),(1.,1.),(1.,1.),(1.,1.),(1.,
1.),(1.,1.),(1.,1.),(1.,1.),(1.,1.),(1.,1.),(1.,1.),(1.,1.),(1.,1.),(1.,
1.),(1.,1.),(1.,1.),(1.,1.),(1.,1.),(1.,1.),(1.,1.),(1.,1.),(1.,1.),(1.,
1.),(1.,1.),(1.,1.),(1.,1.),(1.,1.),(1.,1.),(1.,1.),(1.,1.),(1.,1.),(1.,
1.),(1.,1.),(1.,1.),(1.,1.),(1.,1.),(1.,1.),(1.,1.),(1.,1.),(1.,1.),(1.,
1.),(1.,1.),(1.,1.),(1.,1.),(1.,1.),(1.,1.),(1.,1.),(1.,1.),(1.,1.),(1.,
1.),(1.,1.),(1.,1.),(1.,1.),(1.,1.),(1.,1.),(1.,1.),(1.,1.),(1.,1.),(1.,
1.),(1.,1.),(1.,1.),(1.,1.),(1.,1.),(1.,1.),(1.,1.),(1.,1.),(1.,1.),(1.,
1.),(1.,1.),(1.,1.),(1.,1.),(1.,1.),(1.,1.),(1.,1.),(1.,1.),(1.,1.),(1.,
1.),(1.,1.),(1.,1.),(1.,1.),(1.,1.),(1.,1.),(1.,1.),(1.,1.),(1.,1.),(1.,
1.),(1.,1.),(1.,1.),(1.,1.),(1.,1.),(1.,1.),(1.,1.),(1.,1.),(1.,1.),(1.,
1.),(1.,1.),(1.,1.),(1.,1.),(1.,1.),(1.,1.),(1.,1.),(1.,1.),(1.,1.),(1.,
1.),(1.,1.),(1.,1.),(1.,1.),(1.,1.),(1.,1.),(1.,1.),(1.,1.),(1.,1.),(1.,
1.),(1.,1.),(1.,1.),(1.,1.),(1.,1.),(1.,1.),(1.,1.),(1.,1.),(1.,1.),(1.,
1.),(1.,1.),(1.,1.),(1.,1.),(1.,1.),(1.,1.),(1.,1.),(1.,1.),(1.,1.),(1.,
1.),(1.,1.),(1.,1.),(1.,1.),(1.,1.),(1.,1.),(1.,1.),(1.,1.),(1.,1.),(1.,
1.),(1.,1.),(1.,1.),(1.,1.),(1.,1.),(1.,1.),(1.,1.),(1.,1.),(1.,1.),(1.,
1.),(1.,1.),(1.,1.),(1.,1.),(1.,1.),(1.,1.),(1.,1.),(1.,1.),(1.,1.),(1.,
1.),(1.,1.)))
REPRESENTATION_ITEM('')
SURFACE()
);
#1040=(
BOUNDED_SURFACE()
B_SPLINE_SURFACE(5,1,((#193650,#193651),(#193652,#193653),(#193654,#193655),
(#193656,#193657),(#193658,#193659),(#193660,#193661),(#193662,#193663),
(#193664,#193665),(#193666,#193667),(#193668,#193669),(#193670,#193671),
(#193672,#193673),(#193674,#193675),(#193676,#193677),(#193678,#193679),
(#193680,#193681),(#193682,#193683),(#193684,#193685),(#193686,#193687),
(#193688,#193689),(#193690,#193691),(#193692,#193693),(#193694,#193695),
(#193696,#193697),(#193698,#193699),(#193700,#193701),(#193702,#193703),
(#193704,#193705),(#193706,#193707),(#193708,#193709),(#193710,#193711),
(#193712,#193713),(#193714,#193715),(#193716,#193717),(#193718,#193719),
(#193720,#193721),(#193722,#193723),(#193724,#193725),(#193726,#193727),
(#193728,#193729),(#193730,#193731),(#193732,#193733),(#193734,#193735),
(#193736,#193737),(#193738,#193739),(#193740,#193741),(#193742,#193743),
(#193744,#193745),(#193746,#193747),(#193748,#193749),(#193750,#193751),
(#193752,#193753),(#193754,#193755),(#193756,#193757),(#193758,#193759),
(#193760,#193761),(#193762,#193763),(#193764,#193765),(#193766,#193767),
(#193768,#193769),(#193770,#193771),(#193772,#193773),(#193774,#193775),
(#193776,#193777),(#193778,#193779),(#193780,#193781),(#193782,#193783),
(#193784,#193785),(#193786,#193787),(#193788,#193789),(#193790,#193791),
(#193792,#193793),(#193794,#193795),(#193796,#193797),(#193798,#193799),
(#193800,#193801),(#193802,#193803),(#193804,#193805),(#193806,#193807),
(#193808,#193809),(#193810,#193811),(#193812,#193813),(#193814,#193815),
(#193816,#193817),(#193818,#193819),(#193820,#193821),(#193822,#193823),
(#193824,#193825),(#193826,#193827),(#193828,#193829),(#193830,#193831),
(#193832,#193833),(#193834,#193835),(#193836,#193837),(#193838,#193839),
(#193840,#193841),(#193842,#193843),(#193844,#193845),(#193846,#193847),
(#193848,#193849),(#193850,#193851),(#193852,#193853),(#193854,#193855),
(#193856,#193857),(#193858,#193859),(#193860,#193861),(#193862,#193863),
(#193864,#193865),(#193866,#193867),(#193868,#193869),(#193870,#193871),
(#193872,#193873),(#193874,#193875),(#193876,#193877),(#193878,#193879),
(#193880,#193881),(#193882,#193883),(#193884,#193885),(#193886,#193887),
(#193888,#193889),(#193890,#193891),(#193892,#193893),(#193894,#193895),
(#193896,#193897),(#193898,#193899),(#193900,#193901),(#193902,#193903),
(#193904,#193905),(#193906,#193907),(#193908,#193909),(#193910,#193911),
(#193912,#193913),(#193914,#193915),(#193916,#193917),(#193918,#193919),
(#193920,#193921),(#193922,#193923),(#193924,#193925),(#193926,#193927),
(#193928,#193929),(#193930,#193931),(#193932,#193933),(#193934,#193935),
(#193936,#193937),(#193938,#193939),(#193940,#193941),(#193942,#193943),
(#193944,#193945),(#193946,#193947),(#193948,#193949),(#193950,#193951),
(#193952,#193953),(#193954,#193955),(#193956,#193957),(#193958,#193959),
(#193960,#193961),(#193962,#193963),(#193964,#193965),(#193966,#193967),
(#193968,#193969),(#193970,#193971),(#193972,#193973),(#193974,#193975),
(#193976,#193977),(#193978,#193979),(#193980,#193981),(#193982,#193983),
(#193984,#193985),(#193986,#193987),(#193988,#193989),(#193990,#193991),
(#193992,#193993),(#193994,#193995),(#193996,#193997),(#193998,#193999),
(#194000,#194001),(#194002,#194003),(#194004,#194005),(#194006,#194007),
(#194008,#194009),(#194010,#194011),(#194012,#194013),(#194014,#194015),
(#194016,#194017),(#194018,#194019),(#194020,#194021),(#194022,#194023),
(#194024,#194025),(#194026,#194027),(#194028,#194029),(#194030,#194031),
(#194032,#194033),(#194034,#194035),(#194036,#194037),(#194038,#194039),
(#194040,#194041),(#194042,#194043),(#194044,#194045),(#194046,#194047),
(#194048,#194049),(#194050,#194051),(#194052,#194053),(#194054,#194055),
(#194056,#194057),(#194058,#194059)),.UNSPECIFIED.,.F.,.F.,.F.)
B_SPLINE_SURFACE_WITH_KNOTS((6,1,1,1,1,1,1,1,1,1,1,1,1,1,1,1,1,1,1,1,1,
1,1,1,1,1,1,1,1,1,1,1,1,1,1,1,1,1,1,1,1,1,1,1,1,1,1,1,1,1,1,1,1,1,1,1,1,
1,1,1,1,1,1,1,1,1,1,1,1,1,1,1,1,1,1,1,1,1,1,1,1,1,1,1,1,1,1,1,1,1,1,1,1,
1,1,1,1,1,1,1,1,1,1,1,1,1,1,1,1,1,1,1,1,1,1,1,1,1,1,1,1,1,1,1,1,1,1,1,1,
1,1,1,1,1,1,1,1,1,1,1,1,1,1,1,1,1,1,1,1,1,1,1,1,1,1,1,1,1,1,1,1,1,1,1,1,
1,1,1,1,1,1,1,1,1,1,1,1,1,1,1,1,1,1,1,1,1,1,1,1,1,1,1,1,1,1,1,1,1,1,1,6),
(2,2),(0.,0.005,0.01,0.015,0.02,0.025,0.03,0.035,0.04,0.045,0.05,0.055,
0.06,0.065,0.07,0.075,0.08,0.085,0.09,0.095,0.1,0.105,0.11,0.115,0.12,0.125,
0.13,0.135,0.14,0.145,0.15,0.155,0.16,0.165,0.17,0.175,0.18,0.185,0.19,
0.195,0.2,0.205,0.21,0.215,0.22,0.225,0.23,0.235,0.24,0.245,0.25,0.255,
0.26,0.265,0.27,0.275,0.28,0.285,0.29,0.295,0.3,0.305,0.31,0.315,0.32,0.325,
0.33,0.335,0.34,0.345,0.35,0.355,0.36,0.365,0.37,0.375,0.38,0.385,0.39,
0.395,0.4,0.405,0.41,0.415,0.42,0.425,0.43,0.435,0.44,0.445,0.45,0.455,
0.46,0.465,0.47,0.475,0.48,0.485,0.49,0.495,0.5,0.505,0.51,0.515,0.52,0.525,
0.53,0.535,0.54,0.545,0.55,0.555,0.56,0.565,0.57,0.575,0.58,0.585,0.59,
0.595,0.6,0.605,0.61,0.615,0.62,0.625,0.63,0.635,0.64,0.645,0.65,0.655,
0.66,0.665,0.67,0.675,0.68,0.685,0.690000000000001,0.695000000000001,0.700000000000001,
0.705000000000001,0.710000000000001,0.715000000000001,0.720000000000001,
0.725000000000001,0.730000000000001,0.735000000000001,0.740000000000001,
0.745000000000001,0.750000000000001,0.755000000000001,0.760000000000001,
0.765000000000001,0.770000000000001,0.775000000000001,0.780000000000001,
0.785000000000001,0.790000000000001,0.795000000000001,0.800000000000001,
0.805000000000001,0.810000000000001,0.815000000000001,0.820000000000001,
0.825000000000001,0.830000000000001,0.835000000000001,0.840000000000001,
0.845000000000001,0.850000000000001,0.855000000000001,0.860000000000001,
0.865000000000001,0.870000000000001,0.875000000000001,0.880000000000001,
0.885000000000001,0.890000000000001,0.895000000000001,0.900000000000001,
0.905000000000001,0.910000000000001,0.915000000000001,0.920000000000001,
0.925000000000001,0.930000000000001,0.935000000000001,0.940000000000001,
0.945000000000001,0.950000000000001,0.955000000000001,0.960000000000001,
0.965000000000001,0.970000000000001,0.975000000000001,0.980000000000001,
0.985000000000001,0.990000000000001,0.995000000000001,1.),(0.,1.2),
 .UNSPECIFIED.)
GEOMETRIC_REPRESENTATION_ITEM()
RATIONAL_B_SPLINE_SURFACE(((1.,1.),(1.,1.),(1.,1.),(1.,1.),(1.,1.),(1.,
1.),(1.,1.),(1.,1.),(1.,1.),(1.,1.),(1.,1.),(1.,1.),(1.,1.),(1.,1.),(1.,
1.),(1.,1.),(1.,1.),(1.,1.),(1.,1.),(1.,1.),(1.,1.),(1.,1.),(1.,1.),(1.,
1.),(1.,1.),(1.,1.),(1.,1.),(1.,1.),(1.,1.),(1.,1.),(1.,1.),(1.,1.),(1.,
1.),(1.,1.),(1.,1.),(1.,1.),(1.,1.),(1.,1.),(1.,1.),(1.,1.),(1.,1.),(1.,
1.),(1.,1.),(1.,1.),(1.,1.),(1.,1.),(1.,1.),(1.,1.),(1.,1.),(1.,1.),(1.,
1.),(1.,1.),(1.,1.),(1.,1.),(1.,1.),(1.,1.),(1.,1.),(1.,1.),(1.,1.),(1.,
1.),(1.,1.),(1.,1.),(1.,1.),(1.,1.),(1.,1.),(1.,1.),(1.,1.),(1.,1.),(1.,
1.),(1.,1.),(1.,1.),(1.,1.),(1.,1.),(1.,1.),(1.,1.),(1.,1.),(1.,1.),(1.,
1.),(1.,1.),(1.,1.),(1.,1.),(1.,1.),(1.,1.),(1.,1.),(1.,1.),(1.,1.),(1.,
1.),(1.,1.),(1.,1.),(1.,1.),(1.,1.),(1.,1.),(1.,1.),(1.,1.),(1.,1.),(1.,
1.),(1.,1.),(1.,1.),(1.,1.),(1.,1.),(1.,1.),(1.,1.),(1.,1.),(1.,1.),(1.,
1.),(1.,1.),(1.,1.),(1.,1.),(1.,1.),(1.,1.),(1.,1.),(1.,1.),(1.,1.),(1.,
1.),(1.,1.),(1.,1.),(1.,1.),(1.,1.),(1.,1.),(1.,1.),(1.,1.),(1.,1.),(1.,
1.),(1.,1.),(1.,1.),(1.,1.),(1.,1.),(1.,1.),(1.,1.),(1.,1.),(1.,1.),(1.,
1.),(1.,1.),(1.,1.),(1.,1.),(1.,1.),(1.,1.),(1.,1.),(1.,1.),(1.,1.),(1.,
1.),(1.,1.),(1.,1.),(1.,1.),(1.,1.),(1.,1.),(1.,1.),(1.,1.),(1.,1.),(1.,
1.),(1.,1.),(1.,1.),(1.,1.),(1.,1.),(1.,1.),(1.,1.),(1.,1.),(1.,1.),(1.,
1.),(1.,1.),(1.,1.),(1.,1.),(1.,1.),(1.,1.),(1.,1.),(1.,1.),(1.,1.),(1.,
1.),(1.,1.),(1.,1.),(1.,1.),(1.,1.),(1.,1.),(1.,1.),(1.,1.),(1.,1.),(1.,
1.),(1.,1.),(1.,1.),(1.,1.),(1.,1.),(1.,1.),(1.,1.),(1.,1.),(1.,1.),(1.,
1.),(1.,1.),(1.,1.),(1.,1.),(1.,1.),(1.,1.),(1.,1.),(1.,1.),(1.,1.),(1.,
1.),(1.,1.),(1.,1.),(1.,1.),(1.,1.),(1.,1.),(1.,1.),(1.,1.),(1.,1.),(1.,
1.),(1.,1.)))
REPRESENTATION_ITEM('')
SURFACE()
);
#1041=(
BOUNDED_SURFACE()
B_SPLINE_SURFACE(5,1,((#194271,#194272),(#194273,#194274),(#194275,#194276),
(#194277,#194278),(#194279,#194280),(#194281,#194282),(#194283,#194284),
(#194285,#194286),(#194287,#194288),(#194289,#194290),(#194291,#194292),
(#194293,#194294),(#194295,#194296),(#194297,#194298),(#194299,#194300),
(#194301,#194302),(#194303,#194304),(#194305,#194306),(#194307,#194308),
(#194309,#194310),(#194311,#194312),(#194313,#194314),(#194315,#194316),
(#194317,#194318),(#194319,#194320),(#194321,#194322),(#194323,#194324),
(#194325,#194326),(#194327,#194328),(#194329,#194330),(#194331,#194332),
(#194333,#194334),(#194335,#194336),(#194337,#194338),(#194339,#194340),
(#194341,#194342),(#194343,#194344),(#194345,#194346),(#194347,#194348),
(#194349,#194350),(#194351,#194352),(#194353,#194354),(#194355,#194356),
(#194357,#194358),(#194359,#194360),(#194361,#194362),(#194363,#194364),
(#194365,#194366),(#194367,#194368),(#194369,#194370),(#194371,#194372),
(#194373,#194374),(#194375,#194376),(#194377,#194378),(#194379,#194380),
(#194381,#194382),(#194383,#194384),(#194385,#194386),(#194387,#194388),
(#194389,#194390),(#194391,#194392),(#194393,#194394),(#194395,#194396),
(#194397,#194398),(#194399,#194400),(#194401,#194402),(#194403,#194404),
(#194405,#194406),(#194407,#194408),(#194409,#194410),(#194411,#194412),
(#194413,#194414),(#194415,#194416),(#194417,#194418),(#194419,#194420),
(#194421,#194422),(#194423,#194424),(#194425,#194426),(#194427,#194428),
(#194429,#194430),(#194431,#194432),(#194433,#194434),(#194435,#194436),
(#194437,#194438),(#194439,#194440),(#194441,#194442),(#194443,#194444),
(#194445,#194446),(#194447,#194448),(#194449,#194450),(#194451,#194452),
(#194453,#194454),(#194455,#194456),(#194457,#194458),(#194459,#194460),
(#194461,#194462),(#194463,#194464),(#194465,#194466),(#194467,#194468),
(#194469,#194470),(#194471,#194472),(#194473,#194474),(#194475,#194476),
(#194477,#194478),(#194479,#194480),(#194481,#194482),(#194483,#194484),
(#194485,#194486),(#194487,#194488),(#194489,#194490),(#194491,#194492),
(#194493,#194494),(#194495,#194496),(#194497,#194498),(#194499,#194500),
(#194501,#194502),(#194503,#194504),(#194505,#194506),(#194507,#194508),
(#194509,#194510),(#194511,#194512),(#194513,#194514),(#194515,#194516),
(#194517,#194518),(#194519,#194520),(#194521,#194522),(#194523,#194524),
(#194525,#194526),(#194527,#194528),(#194529,#194530),(#194531,#194532),
(#194533,#194534),(#194535,#194536),(#194537,#194538),(#194539,#194540),
(#194541,#194542),(#194543,#194544),(#194545,#194546),(#194547,#194548),
(#194549,#194550),(#194551,#194552),(#194553,#194554),(#194555,#194556),
(#194557,#194558),(#194559,#194560),(#194561,#194562),(#194563,#194564),
(#194565,#194566),(#194567,#194568),(#194569,#194570),(#194571,#194572),
(#194573,#194574),(#194575,#194576),(#194577,#194578),(#194579,#194580),
(#194581,#194582),(#194583,#194584),(#194585,#194586),(#194587,#194588),
(#194589,#194590),(#194591,#194592),(#194593,#194594),(#194595,#194596),
(#194597,#194598),(#194599,#194600),(#194601,#194602),(#194603,#194604),
(#194605,#194606),(#194607,#194608),(#194609,#194610),(#194611,#194612),
(#194613,#194614),(#194615,#194616),(#194617,#194618),(#194619,#194620),
(#194621,#194622),(#194623,#194624),(#194625,#194626),(#194627,#194628),
(#194629,#194630),(#194631,#194632),(#194633,#194634),(#194635,#194636),
(#194637,#194638),(#194639,#194640),(#194641,#194642),(#194643,#194644),
(#194645,#194646),(#194647,#194648),(#194649,#194650),(#194651,#194652),
(#194653,#194654),(#194655,#194656),(#194657,#194658),(#194659,#194660),
(#194661,#194662),(#194663,#194664),(#194665,#194666),(#194667,#194668),
(#194669,#194670),(#194671,#194672),(#194673,#194674),(#194675,#194676),
(#194677,#194678),(#194679,#194680)),.UNSPECIFIED.,.F.,.F.,.F.)
B_SPLINE_SURFACE_WITH_KNOTS((6,1,1,1,1,1,1,1,1,1,1,1,1,1,1,1,1,1,1,1,1,
1,1,1,1,1,1,1,1,1,1,1,1,1,1,1,1,1,1,1,1,1,1,1,1,1,1,1,1,1,1,1,1,1,1,1,1,
1,1,1,1,1,1,1,1,1,1,1,1,1,1,1,1,1,1,1,1,1,1,1,1,1,1,1,1,1,1,1,1,1,1,1,1,
1,1,1,1,1,1,1,1,1,1,1,1,1,1,1,1,1,1,1,1,1,1,1,1,1,1,1,1,1,1,1,1,1,1,1,1,
1,1,1,1,1,1,1,1,1,1,1,1,1,1,1,1,1,1,1,1,1,1,1,1,1,1,1,1,1,1,1,1,1,1,1,1,
1,1,1,1,1,1,1,1,1,1,1,1,1,1,1,1,1,1,1,1,1,1,1,1,1,1,1,1,1,1,1,1,1,1,1,6),
(2,2),(-1.,-0.995000000000001,-0.990000000000001,-0.985000000000001,-0.980000000000001,
-0.975000000000001,-0.970000000000001,-0.965000000000001,-0.960000000000001,
-0.955000000000001,-0.950000000000001,-0.945000000000001,-0.940000000000001,
-0.935000000000001,-0.930000000000001,-0.925000000000001,-0.920000000000001,
-0.915000000000001,-0.910000000000001,-0.905000000000001,-0.900000000000001,
-0.895000000000001,-0.890000000000001,-0.885000000000001,-0.880000000000001,
-0.875000000000001,-0.870000000000001,-0.865000000000001,-0.860000000000001,
-0.855000000000001,-0.850000000000001,-0.845000000000001,-0.840000000000001,
-0.835000000000001,-0.830000000000001,-0.825000000000001,-0.820000000000001,
-0.815000000000001,-0.810000000000001,-0.805000000000001,-0.800000000000001,
-0.795000000000001,-0.790000000000001,-0.785000000000001,-0.780000000000001,
-0.775000000000001,-0.770000000000001,-0.765000000000001,-0.760000000000001,
-0.755000000000001,-0.750000000000001,-0.745000000000001,-0.740000000000001,
-0.735000000000001,-0.730000000000001,-0.725000000000001,-0.720000000000001,
-0.715000000000001,-0.710000000000001,-0.705000000000001,-0.700000000000001,
-0.695000000000001,-0.690000000000001,-0.685,-0.68,-0.675,-0.67,-0.665,
-0.66,-0.655,-0.65,-0.645,-0.64,-0.635,-0.63,-0.625,-0.62,-0.615,-0.61,
-0.605,-0.6,-0.595,-0.59,-0.585,-0.58,-0.575,-0.57,-0.565,-0.56,-0.555,
-0.55,-0.545,-0.54,-0.535,-0.53,-0.525,-0.52,-0.515,-0.51,-0.505,-0.5,-0.495,
-0.49,-0.485,-0.48,-0.475,-0.47,-0.465,-0.46,-0.455,-0.45,-0.445,-0.44,
-0.435,-0.43,-0.425,-0.42,-0.415,-0.41,-0.405,-0.4,-0.395,-0.39,-0.385,
-0.38,-0.375,-0.37,-0.365,-0.36,-0.355,-0.35,-0.345,-0.34,-0.335,-0.33,
-0.325,-0.32,-0.315,-0.31,-0.305,-0.3,-0.295,-0.29,-0.285,-0.28,-0.275,
-0.27,-0.265,-0.26,-0.255,-0.25,-0.245,-0.24,-0.235,-0.23,-0.225,-0.22,
-0.215,-0.21,-0.205,-0.2,-0.195,-0.19,-0.185,-0.18,-0.175,-0.17,-0.165,
-0.16,-0.155,-0.15,-0.145,-0.14,-0.135,-0.13,-0.125,-0.12,-0.115,-0.11,
-0.105,-0.1,-0.095,-0.09,-0.085,-0.08,-0.075,-0.07,-0.065,-0.06,-0.055,
-0.05,-0.045,-0.04,-0.035,-0.03,-0.025,-0.02,-0.015,-0.01,-0.005,0.),(0.,
1.2),.UNSPECIFIED.)
GEOMETRIC_REPRESENTATION_ITEM()
RATIONAL_B_SPLINE_SURFACE(((1.,1.),(1.,1.),(1.,1.),(1.,1.),(1.,1.),(1.,
1.),(1.,1.),(1.,1.),(1.,1.),(1.,1.),(1.,1.),(1.,1.),(1.,1.),(1.,1.),(1.,
1.),(1.,1.),(1.,1.),(1.,1.),(1.,1.),(1.,1.),(1.,1.),(1.,1.),(1.,1.),(1.,
1.),(1.,1.),(1.,1.),(1.,1.),(1.,1.),(1.,1.),(1.,1.),(1.,1.),(1.,1.),(1.,
1.),(1.,1.),(1.,1.),(1.,1.),(1.,1.),(1.,1.),(1.,1.),(1.,1.),(1.,1.),(1.,
1.),(1.,1.),(1.,1.),(1.,1.),(1.,1.),(1.,1.),(1.,1.),(1.,1.),(1.,1.),(1.,
1.),(1.,1.),(1.,1.),(1.,1.),(1.,1.),(1.,1.),(1.,1.),(1.,1.),(1.,1.),(1.,
1.),(1.,1.),(1.,1.),(1.,1.),(1.,1.),(1.,1.),(1.,1.),(1.,1.),(1.,1.),(1.,
1.),(1.,1.),(1.,1.),(1.,1.),(1.,1.),(1.,1.),(1.,1.),(1.,1.),(1.,1.),(1.,
1.),(1.,1.),(1.,1.),(1.,1.),(1.,1.),(1.,1.),(1.,1.),(1.,1.),(1.,1.),(1.,
1.),(1.,1.),(1.,1.),(1.,1.),(1.,1.),(1.,1.),(1.,1.),(1.,1.),(1.,1.),(1.,
1.),(1.,1.),(1.,1.),(1.,1.),(1.,1.),(1.,1.),(1.,1.),(1.,1.),(1.,1.),(1.,
1.),(1.,1.),(1.,1.),(1.,1.),(1.,1.),(1.,1.),(1.,1.),(1.,1.),(1.,1.),(1.,
1.),(1.,1.),(1.,1.),(1.,1.),(1.,1.),(1.,1.),(1.,1.),(1.,1.),(1.,1.),(1.,
1.),(1.,1.),(1.,1.),(1.,1.),(1.,1.),(1.,1.),(1.,1.),(1.,1.),(1.,1.),(1.,
1.),(1.,1.),(1.,1.),(1.,1.),(1.,1.),(1.,1.),(1.,1.),(1.,1.),(1.,1.),(1.,
1.),(1.,1.),(1.,1.),(1.,1.),(1.,1.),(1.,1.),(1.,1.),(1.,1.),(1.,1.),(1.,
1.),(1.,1.),(1.,1.),(1.,1.),(1.,1.),(1.,1.),(1.,1.),(1.,1.),(1.,1.),(1.,
1.),(1.,1.),(1.,1.),(1.,1.),(1.,1.),(1.,1.),(1.,1.),(1.,1.),(1.,1.),(1.,
1.),(1.,1.),(1.,1.),(1.,1.),(1.,1.),(1.,1.),(1.,1.),(1.,1.),(1.,1.),(1.,
1.),(1.,1.),(1.,1.),(1.,1.),(1.,1.),(1.,1.),(1.,1.),(1.,1.),(1.,1.),(1.,
1.),(1.,1.),(1.,1.),(1.,1.),(1.,1.),(1.,1.),(1.,1.),(1.,1.),(1.,1.),(1.,
1.),(1.,1.),(1.,1.),(1.,1.),(1.,1.),(1.,1.),(1.,1.),(1.,1.),(1.,1.),(1.,
1.),(1.,1.)))
REPRESENTATION_ITEM('')
SURFACE()
);
#1042=(
BOUNDED_SURFACE()
B_SPLINE_SURFACE(5,1,((#194888,#194889),(#194890,#194891),(#194892,#194893),
(#194894,#194895),(#194896,#194897),(#194898,#194899),(#194900,#194901),
(#194902,#194903),(#194904,#194905),(#194906,#194907),(#194908,#194909),
(#194910,#194911),(#194912,#194913),(#194914,#194915),(#194916,#194917),
(#194918,#194919),(#194920,#194921),(#194922,#194923),(#194924,#194925),
(#194926,#194927),(#194928,#194929),(#194930,#194931),(#194932,#194933),
(#194934,#194935),(#194936,#194937),(#194938,#194939),(#194940,#194941),
(#194942,#194943),(#194944,#194945),(#194946,#194947),(#194948,#194949),
(#194950,#194951),(#194952,#194953),(#194954,#194955),(#194956,#194957),
(#194958,#194959),(#194960,#194961),(#194962,#194963),(#194964,#194965),
(#194966,#194967),(#194968,#194969),(#194970,#194971),(#194972,#194973),
(#194974,#194975),(#194976,#194977),(#194978,#194979),(#194980,#194981),
(#194982,#194983),(#194984,#194985),(#194986,#194987),(#194988,#194989),
(#194990,#194991),(#194992,#194993),(#194994,#194995),(#194996,#194997),
(#194998,#194999),(#195000,#195001),(#195002,#195003),(#195004,#195005),
(#195006,#195007),(#195008,#195009),(#195010,#195011),(#195012,#195013),
(#195014,#195015),(#195016,#195017),(#195018,#195019),(#195020,#195021),
(#195022,#195023),(#195024,#195025),(#195026,#195027),(#195028,#195029),
(#195030,#195031),(#195032,#195033),(#195034,#195035),(#195036,#195037),
(#195038,#195039),(#195040,#195041),(#195042,#195043),(#195044,#195045),
(#195046,#195047),(#195048,#195049),(#195050,#195051),(#195052,#195053),
(#195054,#195055),(#195056,#195057),(#195058,#195059),(#195060,#195061),
(#195062,#195063),(#195064,#195065),(#195066,#195067),(#195068,#195069),
(#195070,#195071),(#195072,#195073),(#195074,#195075),(#195076,#195077),
(#195078,#195079),(#195080,#195081),(#195082,#195083),(#195084,#195085),
(#195086,#195087),(#195088,#195089),(#195090,#195091),(#195092,#195093),
(#195094,#195095),(#195096,#195097),(#195098,#195099),(#195100,#195101),
(#195102,#195103),(#195104,#195105),(#195106,#195107),(#195108,#195109),
(#195110,#195111),(#195112,#195113),(#195114,#195115),(#195116,#195117),
(#195118,#195119),(#195120,#195121),(#195122,#195123),(#195124,#195125),
(#195126,#195127),(#195128,#195129),(#195130,#195131),(#195132,#195133),
(#195134,#195135),(#195136,#195137),(#195138,#195139),(#195140,#195141),
(#195142,#195143),(#195144,#195145),(#195146,#195147),(#195148,#195149),
(#195150,#195151),(#195152,#195153),(#195154,#195155),(#195156,#195157),
(#195158,#195159),(#195160,#195161),(#195162,#195163),(#195164,#195165),
(#195166,#195167),(#195168,#195169),(#195170,#195171),(#195172,#195173),
(#195174,#195175),(#195176,#195177),(#195178,#195179),(#195180,#195181),
(#195182,#195183),(#195184,#195185),(#195186,#195187),(#195188,#195189),
(#195190,#195191),(#195192,#195193),(#195194,#195195),(#195196,#195197),
(#195198,#195199),(#195200,#195201),(#195202,#195203),(#195204,#195205),
(#195206,#195207),(#195208,#195209),(#195210,#195211),(#195212,#195213),
(#195214,#195215),(#195216,#195217),(#195218,#195219),(#195220,#195221),
(#195222,#195223),(#195224,#195225),(#195226,#195227),(#195228,#195229),
(#195230,#195231),(#195232,#195233),(#195234,#195235),(#195236,#195237),
(#195238,#195239),(#195240,#195241),(#195242,#195243),(#195244,#195245),
(#195246,#195247),(#195248,#195249),(#195250,#195251),(#195252,#195253),
(#195254,#195255),(#195256,#195257),(#195258,#195259),(#195260,#195261),
(#195262,#195263),(#195264,#195265),(#195266,#195267),(#195268,#195269),
(#195270,#195271),(#195272,#195273),(#195274,#195275),(#195276,#195277),
(#195278,#195279),(#195280,#195281),(#195282,#195283),(#195284,#195285),
(#195286,#195287),(#195288,#195289),(#195290,#195291),(#195292,#195293),
(#195294,#195295),(#195296,#195297)),.UNSPECIFIED.,.F.,.F.,.F.)
B_SPLINE_SURFACE_WITH_KNOTS((6,1,1,1,1,1,1,1,1,1,1,1,1,1,1,1,1,1,1,1,1,
1,1,1,1,1,1,1,1,1,1,1,1,1,1,1,1,1,1,1,1,1,1,1,1,1,1,1,1,1,1,1,1,1,1,1,1,
1,1,1,1,1,1,1,1,1,1,1,1,1,1,1,1,1,1,1,1,1,1,1,1,1,1,1,1,1,1,1,1,1,1,1,1,
1,1,1,1,1,1,1,1,1,1,1,1,1,1,1,1,1,1,1,1,1,1,1,1,1,1,1,1,1,1,1,1,1,1,1,1,
1,1,1,1,1,1,1,1,1,1,1,1,1,1,1,1,1,1,1,1,1,1,1,1,1,1,1,1,1,1,1,1,1,1,1,1,
1,1,1,1,1,1,1,1,1,1,1,1,1,1,1,1,1,1,1,1,1,1,1,1,1,1,1,1,1,1,1,1,1,1,1,6),
(2,2),(0.,0.005,0.01,0.015,0.02,0.025,0.03,0.035,0.04,0.045,0.05,0.055,
0.06,0.065,0.07,0.075,0.08,0.085,0.09,0.095,0.1,0.105,0.11,0.115,0.12,0.125,
0.13,0.135,0.14,0.145,0.15,0.155,0.16,0.165,0.17,0.175,0.18,0.185,0.19,
0.195,0.2,0.205,0.21,0.215,0.22,0.225,0.23,0.235,0.24,0.245,0.25,0.255,
0.26,0.265,0.27,0.275,0.28,0.285,0.29,0.295,0.3,0.305,0.31,0.315,0.32,0.325,
0.33,0.335,0.34,0.345,0.35,0.355,0.36,0.365,0.37,0.375,0.38,0.385,0.39,
0.395,0.4,0.405,0.41,0.415,0.42,0.425,0.43,0.435,0.44,0.445,0.45,0.455,
0.46,0.465,0.47,0.475,0.48,0.485,0.49,0.495,0.5,0.505,0.51,0.515,0.52,0.525,
0.53,0.535,0.54,0.545,0.55,0.555,0.56,0.565,0.57,0.575,0.58,0.585,0.59,
0.595,0.6,0.605,0.61,0.615,0.62,0.625,0.63,0.635,0.64,0.645,0.65,0.655,
0.66,0.665,0.67,0.675,0.68,0.685,0.690000000000001,0.695000000000001,0.700000000000001,
0.705000000000001,0.710000000000001,0.715000000000001,0.720000000000001,
0.725000000000001,0.730000000000001,0.735000000000001,0.740000000000001,
0.745000000000001,0.750000000000001,0.755000000000001,0.760000000000001,
0.765000000000001,0.770000000000001,0.775000000000001,0.780000000000001,
0.785000000000001,0.790000000000001,0.795000000000001,0.800000000000001,
0.805000000000001,0.810000000000001,0.815000000000001,0.820000000000001,
0.825000000000001,0.830000000000001,0.835000000000001,0.840000000000001,
0.845000000000001,0.850000000000001,0.855000000000001,0.860000000000001,
0.865000000000001,0.870000000000001,0.875000000000001,0.880000000000001,
0.885000000000001,0.890000000000001,0.895000000000001,0.900000000000001,
0.905000000000001,0.910000000000001,0.915000000000001,0.920000000000001,
0.925000000000001,0.930000000000001,0.935000000000001,0.940000000000001,
0.945000000000001,0.950000000000001,0.955000000000001,0.960000000000001,
0.965000000000001,0.970000000000001,0.975000000000001,0.980000000000001,
0.985000000000001,0.990000000000001,0.995000000000001,1.),(0.,1.2),
 .UNSPECIFIED.)
GEOMETRIC_REPRESENTATION_ITEM()
RATIONAL_B_SPLINE_SURFACE(((1.,1.),(1.,1.),(1.,1.),(1.,1.),(1.,1.),(1.,
1.),(1.,1.),(1.,1.),(1.,1.),(1.,1.),(1.,1.),(1.,1.),(1.,1.),(1.,1.),(1.,
1.),(1.,1.),(1.,1.),(1.,1.),(1.,1.),(1.,1.),(1.,1.),(1.,1.),(1.,1.),(1.,
1.),(1.,1.),(1.,1.),(1.,1.),(1.,1.),(1.,1.),(1.,1.),(1.,1.),(1.,1.),(1.,
1.),(1.,1.),(1.,1.),(1.,1.),(1.,1.),(1.,1.),(1.,1.),(1.,1.),(1.,1.),(1.,
1.),(1.,1.),(1.,1.),(1.,1.),(1.,1.),(1.,1.),(1.,1.),(1.,1.),(1.,1.),(1.,
1.),(1.,1.),(1.,1.),(1.,1.),(1.,1.),(1.,1.),(1.,1.),(1.,1.),(1.,1.),(1.,
1.),(1.,1.),(1.,1.),(1.,1.),(1.,1.),(1.,1.),(1.,1.),(1.,1.),(1.,1.),(1.,
1.),(1.,1.),(1.,1.),(1.,1.),(1.,1.),(1.,1.),(1.,1.),(1.,1.),(1.,1.),(1.,
1.),(1.,1.),(1.,1.),(1.,1.),(1.,1.),(1.,1.),(1.,1.),(1.,1.),(1.,1.),(1.,
1.),(1.,1.),(1.,1.),(1.,1.),(1.,1.),(1.,1.),(1.,1.),(1.,1.),(1.,1.),(1.,
1.),(1.,1.),(1.,1.),(1.,1.),(1.,1.),(1.,1.),(1.,1.),(1.,1.),(1.,1.),(1.,
1.),(1.,1.),(1.,1.),(1.,1.),(1.,1.),(1.,1.),(1.,1.),(1.,1.),(1.,1.),(1.,
1.),(1.,1.),(1.,1.),(1.,1.),(1.,1.),(1.,1.),(1.,1.),(1.,1.),(1.,1.),(1.,
1.),(1.,1.),(1.,1.),(1.,1.),(1.,1.),(1.,1.),(1.,1.),(1.,1.),(1.,1.),(1.,
1.),(1.,1.),(1.,1.),(1.,1.),(1.,1.),(1.,1.),(1.,1.),(1.,1.),(1.,1.),(1.,
1.),(1.,1.),(1.,1.),(1.,1.),(1.,1.),(1.,1.),(1.,1.),(1.,1.),(1.,1.),(1.,
1.),(1.,1.),(1.,1.),(1.,1.),(1.,1.),(1.,1.),(1.,1.),(1.,1.),(1.,1.),(1.,
1.),(1.,1.),(1.,1.),(1.,1.),(1.,1.),(1.,1.),(1.,1.),(1.,1.),(1.,1.),(1.,
1.),(1.,1.),(1.,1.),(1.,1.),(1.,1.),(1.,1.),(1.,1.),(1.,1.),(1.,1.),(1.,
1.),(1.,1.),(1.,1.),(1.,1.),(1.,1.),(1.,1.),(1.,1.),(1.,1.),(1.,1.),(1.,
1.),(1.,1.),(1.,1.),(1.,1.),(1.,1.),(1.,1.),(1.,1.),(1.,1.),(1.,1.),(1.,
1.),(1.,1.),(1.,1.),(1.,1.),(1.,1.),(1.,1.),(1.,1.),(1.,1.),(1.,1.),(1.,
1.),(1.,1.)))
REPRESENTATION_ITEM('')
SURFACE()
);
#1043=(
BOUNDED_SURFACE()
B_SPLINE_SURFACE(5,1,((#195509,#195510),(#195511,#195512),(#195513,#195514),
(#195515,#195516),(#195517,#195518),(#195519,#195520),(#195521,#195522),
(#195523,#195524),(#195525,#195526),(#195527,#195528),(#195529,#195530),
(#195531,#195532),(#195533,#195534),(#195535,#195536),(#195537,#195538),
(#195539,#195540),(#195541,#195542),(#195543,#195544),(#195545,#195546),
(#195547,#195548),(#195549,#195550),(#195551,#195552),(#195553,#195554),
(#195555,#195556),(#195557,#195558),(#195559,#195560),(#195561,#195562),
(#195563,#195564),(#195565,#195566),(#195567,#195568),(#195569,#195570),
(#195571,#195572),(#195573,#195574),(#195575,#195576),(#195577,#195578),
(#195579,#195580),(#195581,#195582),(#195583,#195584),(#195585,#195586),
(#195587,#195588),(#195589,#195590),(#195591,#195592),(#195593,#195594),
(#195595,#195596),(#195597,#195598),(#195599,#195600),(#195601,#195602),
(#195603,#195604),(#195605,#195606),(#195607,#195608),(#195609,#195610),
(#195611,#195612),(#195613,#195614),(#195615,#195616),(#195617,#195618),
(#195619,#195620),(#195621,#195622),(#195623,#195624),(#195625,#195626),
(#195627,#195628),(#195629,#195630),(#195631,#195632),(#195633,#195634),
(#195635,#195636),(#195637,#195638),(#195639,#195640),(#195641,#195642),
(#195643,#195644),(#195645,#195646),(#195647,#195648),(#195649,#195650),
(#195651,#195652),(#195653,#195654),(#195655,#195656),(#195657,#195658),
(#195659,#195660),(#195661,#195662),(#195663,#195664),(#195665,#195666),
(#195667,#195668),(#195669,#195670),(#195671,#195672),(#195673,#195674),
(#195675,#195676),(#195677,#195678),(#195679,#195680),(#195681,#195682),
(#195683,#195684),(#195685,#195686),(#195687,#195688),(#195689,#195690),
(#195691,#195692),(#195693,#195694),(#195695,#195696),(#195697,#195698),
(#195699,#195700),(#195701,#195702),(#195703,#195704),(#195705,#195706),
(#195707,#195708),(#195709,#195710),(#195711,#195712),(#195713,#195714),
(#195715,#195716),(#195717,#195718),(#195719,#195720),(#195721,#195722),
(#195723,#195724),(#195725,#195726),(#195727,#195728),(#195729,#195730),
(#195731,#195732),(#195733,#195734),(#195735,#195736),(#195737,#195738),
(#195739,#195740),(#195741,#195742),(#195743,#195744),(#195745,#195746),
(#195747,#195748),(#195749,#195750),(#195751,#195752),(#195753,#195754),
(#195755,#195756),(#195757,#195758),(#195759,#195760),(#195761,#195762),
(#195763,#195764),(#195765,#195766),(#195767,#195768),(#195769,#195770),
(#195771,#195772),(#195773,#195774),(#195775,#195776),(#195777,#195778),
(#195779,#195780),(#195781,#195782),(#195783,#195784),(#195785,#195786),
(#195787,#195788),(#195789,#195790),(#195791,#195792),(#195793,#195794),
(#195795,#195796),(#195797,#195798),(#195799,#195800),(#195801,#195802),
(#195803,#195804),(#195805,#195806),(#195807,#195808),(#195809,#195810),
(#195811,#195812),(#195813,#195814),(#195815,#195816),(#195817,#195818),
(#195819,#195820),(#195821,#195822),(#195823,#195824),(#195825,#195826),
(#195827,#195828),(#195829,#195830),(#195831,#195832),(#195833,#195834),
(#195835,#195836),(#195837,#195838),(#195839,#195840),(#195841,#195842),
(#195843,#195844),(#195845,#195846),(#195847,#195848),(#195849,#195850),
(#195851,#195852),(#195853,#195854),(#195855,#195856),(#195857,#195858),
(#195859,#195860),(#195861,#195862),(#195863,#195864),(#195865,#195866),
(#195867,#195868),(#195869,#195870),(#195871,#195872),(#195873,#195874),
(#195875,#195876),(#195877,#195878),(#195879,#195880),(#195881,#195882),
(#195883,#195884),(#195885,#195886),(#195887,#195888),(#195889,#195890),
(#195891,#195892),(#195893,#195894),(#195895,#195896),(#195897,#195898),
(#195899,#195900),(#195901,#195902),(#195903,#195904),(#195905,#195906),
(#195907,#195908),(#195909,#195910),(#195911,#195912),(#195913,#195914),
(#195915,#195916),(#195917,#195918)),.UNSPECIFIED.,.F.,.F.,.F.)
B_SPLINE_SURFACE_WITH_KNOTS((6,1,1,1,1,1,1,1,1,1,1,1,1,1,1,1,1,1,1,1,1,
1,1,1,1,1,1,1,1,1,1,1,1,1,1,1,1,1,1,1,1,1,1,1,1,1,1,1,1,1,1,1,1,1,1,1,1,
1,1,1,1,1,1,1,1,1,1,1,1,1,1,1,1,1,1,1,1,1,1,1,1,1,1,1,1,1,1,1,1,1,1,1,1,
1,1,1,1,1,1,1,1,1,1,1,1,1,1,1,1,1,1,1,1,1,1,1,1,1,1,1,1,1,1,1,1,1,1,1,1,
1,1,1,1,1,1,1,1,1,1,1,1,1,1,1,1,1,1,1,1,1,1,1,1,1,1,1,1,1,1,1,1,1,1,1,1,
1,1,1,1,1,1,1,1,1,1,1,1,1,1,1,1,1,1,1,1,1,1,1,1,1,1,1,1,1,1,1,1,1,1,1,6),
(2,2),(-1.,-0.995000000000001,-0.990000000000001,-0.985000000000001,-0.980000000000001,
-0.975000000000001,-0.970000000000001,-0.965000000000001,-0.960000000000001,
-0.955000000000001,-0.950000000000001,-0.945000000000001,-0.940000000000001,
-0.935000000000001,-0.930000000000001,-0.925000000000001,-0.920000000000001,
-0.915000000000001,-0.910000000000001,-0.905000000000001,-0.900000000000001,
-0.895000000000001,-0.890000000000001,-0.885000000000001,-0.880000000000001,
-0.875000000000001,-0.870000000000001,-0.865000000000001,-0.860000000000001,
-0.855000000000001,-0.850000000000001,-0.845000000000001,-0.840000000000001,
-0.835000000000001,-0.830000000000001,-0.825000000000001,-0.820000000000001,
-0.815000000000001,-0.810000000000001,-0.805000000000001,-0.800000000000001,
-0.795000000000001,-0.790000000000001,-0.785000000000001,-0.780000000000001,
-0.775000000000001,-0.770000000000001,-0.765000000000001,-0.760000000000001,
-0.755000000000001,-0.750000000000001,-0.745000000000001,-0.740000000000001,
-0.735000000000001,-0.730000000000001,-0.725000000000001,-0.720000000000001,
-0.715000000000001,-0.710000000000001,-0.705000000000001,-0.700000000000001,
-0.695000000000001,-0.690000000000001,-0.685,-0.68,-0.675,-0.67,-0.665,
-0.66,-0.655,-0.65,-0.645,-0.64,-0.635,-0.63,-0.625,-0.62,-0.615,-0.61,
-0.605,-0.6,-0.595,-0.59,-0.585,-0.58,-0.575,-0.57,-0.565,-0.56,-0.555,
-0.55,-0.545,-0.54,-0.535,-0.53,-0.525,-0.52,-0.515,-0.51,-0.505,-0.5,-0.495,
-0.49,-0.485,-0.48,-0.475,-0.47,-0.465,-0.46,-0.455,-0.45,-0.445,-0.44,
-0.435,-0.43,-0.425,-0.42,-0.415,-0.41,-0.405,-0.4,-0.395,-0.39,-0.385,
-0.38,-0.375,-0.37,-0.365,-0.36,-0.355,-0.35,-0.345,-0.34,-0.335,-0.33,
-0.325,-0.32,-0.315,-0.31,-0.305,-0.3,-0.295,-0.29,-0.285,-0.28,-0.275,
-0.27,-0.265,-0.26,-0.255,-0.25,-0.245,-0.24,-0.235,-0.23,-0.225,-0.22,
-0.215,-0.21,-0.205,-0.2,-0.195,-0.19,-0.185,-0.18,-0.175,-0.17,-0.165,
-0.16,-0.155,-0.15,-0.145,-0.14,-0.135,-0.13,-0.125,-0.12,-0.115,-0.11,
-0.105,-0.1,-0.095,-0.09,-0.085,-0.08,-0.075,-0.07,-0.065,-0.06,-0.055,
-0.05,-0.045,-0.04,-0.035,-0.03,-0.025,-0.02,-0.015,-0.01,-0.005,0.),(0.,
1.2),.UNSPECIFIED.)
GEOMETRIC_REPRESENTATION_ITEM()
RATIONAL_B_SPLINE_SURFACE(((1.,1.),(1.,1.),(1.,1.),(1.,1.),(1.,1.),(1.,
1.),(1.,1.),(1.,1.),(1.,1.),(1.,1.),(1.,1.),(1.,1.),(1.,1.),(1.,1.),(1.,
1.),(1.,1.),(1.,1.),(1.,1.),(1.,1.),(1.,1.),(1.,1.),(1.,1.),(1.,1.),(1.,
1.),(1.,1.),(1.,1.),(1.,1.),(1.,1.),(1.,1.),(1.,1.),(1.,1.),(1.,1.),(1.,
1.),(1.,1.),(1.,1.),(1.,1.),(1.,1.),(1.,1.),(1.,1.),(1.,1.),(1.,1.),(1.,
1.),(1.,1.),(1.,1.),(1.,1.),(1.,1.),(1.,1.),(1.,1.),(1.,1.),(1.,1.),(1.,
1.),(1.,1.),(1.,1.),(1.,1.),(1.,1.),(1.,1.),(1.,1.),(1.,1.),(1.,1.),(1.,
1.),(1.,1.),(1.,1.),(1.,1.),(1.,1.),(1.,1.),(1.,1.),(1.,1.),(1.,1.),(1.,
1.),(1.,1.),(1.,1.),(1.,1.),(1.,1.),(1.,1.),(1.,1.),(1.,1.),(1.,1.),(1.,
1.),(1.,1.),(1.,1.),(1.,1.),(1.,1.),(1.,1.),(1.,1.),(1.,1.),(1.,1.),(1.,
1.),(1.,1.),(1.,1.),(1.,1.),(1.,1.),(1.,1.),(1.,1.),(1.,1.),(1.,1.),(1.,
1.),(1.,1.),(1.,1.),(1.,1.),(1.,1.),(1.,1.),(1.,1.),(1.,1.),(1.,1.),(1.,
1.),(1.,1.),(1.,1.),(1.,1.),(1.,1.),(1.,1.),(1.,1.),(1.,1.),(1.,1.),(1.,
1.),(1.,1.),(1.,1.),(1.,1.),(1.,1.),(1.,1.),(1.,1.),(1.,1.),(1.,1.),(1.,
1.),(1.,1.),(1.,1.),(1.,1.),(1.,1.),(1.,1.),(1.,1.),(1.,1.),(1.,1.),(1.,
1.),(1.,1.),(1.,1.),(1.,1.),(1.,1.),(1.,1.),(1.,1.),(1.,1.),(1.,1.),(1.,
1.),(1.,1.),(1.,1.),(1.,1.),(1.,1.),(1.,1.),(1.,1.),(1.,1.),(1.,1.),(1.,
1.),(1.,1.),(1.,1.),(1.,1.),(1.,1.),(1.,1.),(1.,1.),(1.,1.),(1.,1.),(1.,
1.),(1.,1.),(1.,1.),(1.,1.),(1.,1.),(1.,1.),(1.,1.),(1.,1.),(1.,1.),(1.,
1.),(1.,1.),(1.,1.),(1.,1.),(1.,1.),(1.,1.),(1.,1.),(1.,1.),(1.,1.),(1.,
1.),(1.,1.),(1.,1.),(1.,1.),(1.,1.),(1.,1.),(1.,1.),(1.,1.),(1.,1.),(1.,
1.),(1.,1.),(1.,1.),(1.,1.),(1.,1.),(1.,1.),(1.,1.),(1.,1.),(1.,1.),(1.,
1.),(1.,1.),(1.,1.),(1.,1.),(1.,1.),(1.,1.),(1.,1.),(1.,1.),(1.,1.),(1.,
1.),(1.,1.)))
REPRESENTATION_ITEM('')
SURFACE()
);
#1044=(
BOUNDED_SURFACE()
B_SPLINE_SURFACE(5,1,((#196126,#196127),(#196128,#196129),(#196130,#196131),
(#196132,#196133),(#196134,#196135),(#196136,#196137),(#196138,#196139),
(#196140,#196141),(#196142,#196143),(#196144,#196145),(#196146,#196147),
(#196148,#196149),(#196150,#196151),(#196152,#196153),(#196154,#196155),
(#196156,#196157),(#196158,#196159),(#196160,#196161),(#196162,#196163),
(#196164,#196165),(#196166,#196167),(#196168,#196169),(#196170,#196171),
(#196172,#196173),(#196174,#196175),(#196176,#196177),(#196178,#196179),
(#196180,#196181),(#196182,#196183),(#196184,#196185),(#196186,#196187),
(#196188,#196189),(#196190,#196191),(#196192,#196193),(#196194,#196195),
(#196196,#196197),(#196198,#196199),(#196200,#196201),(#196202,#196203),
(#196204,#196205),(#196206,#196207),(#196208,#196209),(#196210,#196211),
(#196212,#196213),(#196214,#196215),(#196216,#196217),(#196218,#196219),
(#196220,#196221),(#196222,#196223),(#196224,#196225),(#196226,#196227),
(#196228,#196229),(#196230,#196231),(#196232,#196233),(#196234,#196235),
(#196236,#196237),(#196238,#196239),(#196240,#196241),(#196242,#196243),
(#196244,#196245),(#196246,#196247),(#196248,#196249),(#196250,#196251),
(#196252,#196253),(#196254,#196255),(#196256,#196257),(#196258,#196259),
(#196260,#196261),(#196262,#196263),(#196264,#196265),(#196266,#196267),
(#196268,#196269),(#196270,#196271),(#196272,#196273),(#196274,#196275),
(#196276,#196277),(#196278,#196279),(#196280,#196281),(#196282,#196283),
(#196284,#196285),(#196286,#196287),(#196288,#196289),(#196290,#196291),
(#196292,#196293),(#196294,#196295),(#196296,#196297),(#196298,#196299),
(#196300,#196301),(#196302,#196303),(#196304,#196305),(#196306,#196307),
(#196308,#196309),(#196310,#196311),(#196312,#196313),(#196314,#196315),
(#196316,#196317),(#196318,#196319),(#196320,#196321),(#196322,#196323),
(#196324,#196325),(#196326,#196327),(#196328,#196329),(#196330,#196331),
(#196332,#196333),(#196334,#196335),(#196336,#196337),(#196338,#196339),
(#196340,#196341),(#196342,#196343),(#196344,#196345),(#196346,#196347),
(#196348,#196349),(#196350,#196351),(#196352,#196353),(#196354,#196355),
(#196356,#196357),(#196358,#196359),(#196360,#196361),(#196362,#196363),
(#196364,#196365),(#196366,#196367),(#196368,#196369),(#196370,#196371),
(#196372,#196373),(#196374,#196375),(#196376,#196377),(#196378,#196379),
(#196380,#196381),(#196382,#196383),(#196384,#196385),(#196386,#196387),
(#196388,#196389),(#196390,#196391),(#196392,#196393),(#196394,#196395),
(#196396,#196397),(#196398,#196399),(#196400,#196401),(#196402,#196403),
(#196404,#196405),(#196406,#196407),(#196408,#196409),(#196410,#196411),
(#196412,#196413),(#196414,#196415),(#196416,#196417),(#196418,#196419),
(#196420,#196421),(#196422,#196423),(#196424,#196425),(#196426,#196427),
(#196428,#196429),(#196430,#196431),(#196432,#196433),(#196434,#196435),
(#196436,#196437),(#196438,#196439),(#196440,#196441),(#196442,#196443),
(#196444,#196445),(#196446,#196447),(#196448,#196449),(#196450,#196451),
(#196452,#196453),(#196454,#196455),(#196456,#196457),(#196458,#196459),
(#196460,#196461),(#196462,#196463),(#196464,#196465),(#196466,#196467),
(#196468,#196469),(#196470,#196471),(#196472,#196473),(#196474,#196475),
(#196476,#196477),(#196478,#196479),(#196480,#196481),(#196482,#196483),
(#196484,#196485),(#196486,#196487),(#196488,#196489),(#196490,#196491),
(#196492,#196493),(#196494,#196495),(#196496,#196497),(#196498,#196499),
(#196500,#196501),(#196502,#196503),(#196504,#196505),(#196506,#196507),
(#196508,#196509),(#196510,#196511),(#196512,#196513),(#196514,#196515),
(#196516,#196517),(#196518,#196519),(#196520,#196521),(#196522,#196523),
(#196524,#196525),(#196526,#196527),(#196528,#196529),(#196530,#196531),
(#196532,#196533),(#196534,#196535)),.UNSPECIFIED.,.F.,.F.,.F.)
B_SPLINE_SURFACE_WITH_KNOTS((6,1,1,1,1,1,1,1,1,1,1,1,1,1,1,1,1,1,1,1,1,
1,1,1,1,1,1,1,1,1,1,1,1,1,1,1,1,1,1,1,1,1,1,1,1,1,1,1,1,1,1,1,1,1,1,1,1,
1,1,1,1,1,1,1,1,1,1,1,1,1,1,1,1,1,1,1,1,1,1,1,1,1,1,1,1,1,1,1,1,1,1,1,1,
1,1,1,1,1,1,1,1,1,1,1,1,1,1,1,1,1,1,1,1,1,1,1,1,1,1,1,1,1,1,1,1,1,1,1,1,
1,1,1,1,1,1,1,1,1,1,1,1,1,1,1,1,1,1,1,1,1,1,1,1,1,1,1,1,1,1,1,1,1,1,1,1,
1,1,1,1,1,1,1,1,1,1,1,1,1,1,1,1,1,1,1,1,1,1,1,1,1,1,1,1,1,1,1,1,1,1,1,6),
(2,2),(0.,0.005,0.01,0.015,0.02,0.025,0.03,0.035,0.04,0.045,0.05,0.055,
0.06,0.065,0.07,0.075,0.08,0.085,0.09,0.095,0.1,0.105,0.11,0.115,0.12,0.125,
0.13,0.135,0.14,0.145,0.15,0.155,0.16,0.165,0.17,0.175,0.18,0.185,0.19,
0.195,0.2,0.205,0.21,0.215,0.22,0.225,0.23,0.235,0.24,0.245,0.25,0.255,
0.26,0.265,0.27,0.275,0.28,0.285,0.29,0.295,0.3,0.305,0.31,0.315,0.32,0.325,
0.33,0.335,0.34,0.345,0.35,0.355,0.36,0.365,0.37,0.375,0.38,0.385,0.39,
0.395,0.4,0.405,0.41,0.415,0.42,0.425,0.43,0.435,0.44,0.445,0.45,0.455,
0.46,0.465,0.47,0.475,0.48,0.485,0.49,0.495,0.5,0.505,0.51,0.515,0.52,0.525,
0.53,0.535,0.54,0.545,0.55,0.555,0.56,0.565,0.57,0.575,0.58,0.585,0.59,
0.595,0.6,0.605,0.61,0.615,0.62,0.625,0.63,0.635,0.64,0.645,0.65,0.655,
0.66,0.665,0.67,0.675,0.68,0.685,0.690000000000001,0.695000000000001,0.700000000000001,
0.705000000000001,0.710000000000001,0.715000000000001,0.720000000000001,
0.725000000000001,0.730000000000001,0.735000000000001,0.740000000000001,
0.745000000000001,0.750000000000001,0.755000000000001,0.760000000000001,
0.765000000000001,0.770000000000001,0.775000000000001,0.780000000000001,
0.785000000000001,0.790000000000001,0.795000000000001,0.800000000000001,
0.805000000000001,0.810000000000001,0.815000000000001,0.820000000000001,
0.825000000000001,0.830000000000001,0.835000000000001,0.840000000000001,
0.845000000000001,0.850000000000001,0.855000000000001,0.860000000000001,
0.865000000000001,0.870000000000001,0.875000000000001,0.880000000000001,
0.885000000000001,0.890000000000001,0.895000000000001,0.900000000000001,
0.905000000000001,0.910000000000001,0.915000000000001,0.920000000000001,
0.925000000000001,0.930000000000001,0.935000000000001,0.940000000000001,
0.945000000000001,0.950000000000001,0.955000000000001,0.960000000000001,
0.965000000000001,0.970000000000001,0.975000000000001,0.980000000000001,
0.985000000000001,0.990000000000001,0.995000000000001,1.),(0.,1.2),
 .UNSPECIFIED.)
GEOMETRIC_REPRESENTATION_ITEM()
RATIONAL_B_SPLINE_SURFACE(((1.,1.),(1.,1.),(1.,1.),(1.,1.),(1.,1.),(1.,
1.),(1.,1.),(1.,1.),(1.,1.),(1.,1.),(1.,1.),(1.,1.),(1.,1.),(1.,1.),(1.,
1.),(1.,1.),(1.,1.),(1.,1.),(1.,1.),(1.,1.),(1.,1.),(1.,1.),(1.,1.),(1.,
1.),(1.,1.),(1.,1.),(1.,1.),(1.,1.),(1.,1.),(1.,1.),(1.,1.),(1.,1.),(1.,
1.),(1.,1.),(1.,1.),(1.,1.),(1.,1.),(1.,1.),(1.,1.),(1.,1.),(1.,1.),(1.,
1.),(1.,1.),(1.,1.),(1.,1.),(1.,1.),(1.,1.),(1.,1.),(1.,1.),(1.,1.),(1.,
1.),(1.,1.),(1.,1.),(1.,1.),(1.,1.),(1.,1.),(1.,1.),(1.,1.),(1.,1.),(1.,
1.),(1.,1.),(1.,1.),(1.,1.),(1.,1.),(1.,1.),(1.,1.),(1.,1.),(1.,1.),(1.,
1.),(1.,1.),(1.,1.),(1.,1.),(1.,1.),(1.,1.),(1.,1.),(1.,1.),(1.,1.),(1.,
1.),(1.,1.),(1.,1.),(1.,1.),(1.,1.),(1.,1.),(1.,1.),(1.,1.),(1.,1.),(1.,
1.),(1.,1.),(1.,1.),(1.,1.),(1.,1.),(1.,1.),(1.,1.),(1.,1.),(1.,1.),(1.,
1.),(1.,1.),(1.,1.),(1.,1.),(1.,1.),(1.,1.),(1.,1.),(1.,1.),(1.,1.),(1.,
1.),(1.,1.),(1.,1.),(1.,1.),(1.,1.),(1.,1.),(1.,1.),(1.,1.),(1.,1.),(1.,
1.),(1.,1.),(1.,1.),(1.,1.),(1.,1.),(1.,1.),(1.,1.),(1.,1.),(1.,1.),(1.,
1.),(1.,1.),(1.,1.),(1.,1.),(1.,1.),(1.,1.),(1.,1.),(1.,1.),(1.,1.),(1.,
1.),(1.,1.),(1.,1.),(1.,1.),(1.,1.),(1.,1.),(1.,1.),(1.,1.),(1.,1.),(1.,
1.),(1.,1.),(1.,1.),(1.,1.),(1.,1.),(1.,1.),(1.,1.),(1.,1.),(1.,1.),(1.,
1.),(1.,1.),(1.,1.),(1.,1.),(1.,1.),(1.,1.),(1.,1.),(1.,1.),(1.,1.),(1.,
1.),(1.,1.),(1.,1.),(1.,1.),(1.,1.),(1.,1.),(1.,1.),(1.,1.),(1.,1.),(1.,
1.),(1.,1.),(1.,1.),(1.,1.),(1.,1.),(1.,1.),(1.,1.),(1.,1.),(1.,1.),(1.,
1.),(1.,1.),(1.,1.),(1.,1.),(1.,1.),(1.,1.),(1.,1.),(1.,1.),(1.,1.),(1.,
1.),(1.,1.),(1.,1.),(1.,1.),(1.,1.),(1.,1.),(1.,1.),(1.,1.),(1.,1.),(1.,
1.),(1.,1.),(1.,1.),(1.,1.),(1.,1.),(1.,1.),(1.,1.),(1.,1.),(1.,1.),(1.,
1.),(1.,1.)))
REPRESENTATION_ITEM('')
SURFACE()
);
#1045=(
BOUNDED_SURFACE()
B_SPLINE_SURFACE(5,1,((#196747,#196748),(#196749,#196750),(#196751,#196752),
(#196753,#196754),(#196755,#196756),(#196757,#196758),(#196759,#196760),
(#196761,#196762),(#196763,#196764),(#196765,#196766),(#196767,#196768),
(#196769,#196770),(#196771,#196772),(#196773,#196774),(#196775,#196776),
(#196777,#196778),(#196779,#196780),(#196781,#196782),(#196783,#196784),
(#196785,#196786),(#196787,#196788),(#196789,#196790),(#196791,#196792),
(#196793,#196794),(#196795,#196796),(#196797,#196798),(#196799,#196800),
(#196801,#196802),(#196803,#196804),(#196805,#196806),(#196807,#196808),
(#196809,#196810),(#196811,#196812),(#196813,#196814),(#196815,#196816),
(#196817,#196818),(#196819,#196820),(#196821,#196822),(#196823,#196824),
(#196825,#196826),(#196827,#196828),(#196829,#196830),(#196831,#196832),
(#196833,#196834),(#196835,#196836),(#196837,#196838),(#196839,#196840),
(#196841,#196842),(#196843,#196844),(#196845,#196846),(#196847,#196848),
(#196849,#196850),(#196851,#196852),(#196853,#196854),(#196855,#196856),
(#196857,#196858),(#196859,#196860),(#196861,#196862),(#196863,#196864),
(#196865,#196866),(#196867,#196868),(#196869,#196870),(#196871,#196872),
(#196873,#196874),(#196875,#196876),(#196877,#196878),(#196879,#196880),
(#196881,#196882),(#196883,#196884),(#196885,#196886),(#196887,#196888),
(#196889,#196890),(#196891,#196892),(#196893,#196894),(#196895,#196896),
(#196897,#196898),(#196899,#196900),(#196901,#196902),(#196903,#196904),
(#196905,#196906),(#196907,#196908),(#196909,#196910),(#196911,#196912),
(#196913,#196914),(#196915,#196916),(#196917,#196918),(#196919,#196920),
(#196921,#196922),(#196923,#196924),(#196925,#196926),(#196927,#196928),
(#196929,#196930),(#196931,#196932),(#196933,#196934),(#196935,#196936),
(#196937,#196938),(#196939,#196940),(#196941,#196942),(#196943,#196944),
(#196945,#196946),(#196947,#196948),(#196949,#196950),(#196951,#196952),
(#196953,#196954),(#196955,#196956),(#196957,#196958),(#196959,#196960),
(#196961,#196962),(#196963,#196964),(#196965,#196966),(#196967,#196968),
(#196969,#196970),(#196971,#196972),(#196973,#196974),(#196975,#196976),
(#196977,#196978),(#196979,#196980),(#196981,#196982),(#196983,#196984),
(#196985,#196986),(#196987,#196988),(#196989,#196990),(#196991,#196992),
(#196993,#196994),(#196995,#196996),(#196997,#196998),(#196999,#197000),
(#197001,#197002),(#197003,#197004),(#197005,#197006),(#197007,#197008),
(#197009,#197010),(#197011,#197012),(#197013,#197014),(#197015,#197016),
(#197017,#197018),(#197019,#197020),(#197021,#197022),(#197023,#197024),
(#197025,#197026),(#197027,#197028),(#197029,#197030),(#197031,#197032),
(#197033,#197034),(#197035,#197036),(#197037,#197038),(#197039,#197040),
(#197041,#197042),(#197043,#197044),(#197045,#197046),(#197047,#197048),
(#197049,#197050),(#197051,#197052),(#197053,#197054),(#197055,#197056),
(#197057,#197058),(#197059,#197060),(#197061,#197062),(#197063,#197064),
(#197065,#197066),(#197067,#197068),(#197069,#197070),(#197071,#197072),
(#197073,#197074),(#197075,#197076),(#197077,#197078),(#197079,#197080),
(#197081,#197082),(#197083,#197084),(#197085,#197086),(#197087,#197088),
(#197089,#197090),(#197091,#197092),(#197093,#197094),(#197095,#197096),
(#197097,#197098),(#197099,#197100),(#197101,#197102),(#197103,#197104),
(#197105,#197106),(#197107,#197108),(#197109,#197110),(#197111,#197112),
(#197113,#197114),(#197115,#197116),(#197117,#197118),(#197119,#197120),
(#197121,#197122),(#197123,#197124),(#197125,#197126),(#197127,#197128),
(#197129,#197130),(#197131,#197132),(#197133,#197134),(#197135,#197136),
(#197137,#197138),(#197139,#197140),(#197141,#197142),(#197143,#197144),
(#197145,#197146),(#197147,#197148),(#197149,#197150),(#197151,#197152),
(#197153,#197154),(#197155,#197156)),.UNSPECIFIED.,.F.,.F.,.F.)
B_SPLINE_SURFACE_WITH_KNOTS((6,1,1,1,1,1,1,1,1,1,1,1,1,1,1,1,1,1,1,1,1,
1,1,1,1,1,1,1,1,1,1,1,1,1,1,1,1,1,1,1,1,1,1,1,1,1,1,1,1,1,1,1,1,1,1,1,1,
1,1,1,1,1,1,1,1,1,1,1,1,1,1,1,1,1,1,1,1,1,1,1,1,1,1,1,1,1,1,1,1,1,1,1,1,
1,1,1,1,1,1,1,1,1,1,1,1,1,1,1,1,1,1,1,1,1,1,1,1,1,1,1,1,1,1,1,1,1,1,1,1,
1,1,1,1,1,1,1,1,1,1,1,1,1,1,1,1,1,1,1,1,1,1,1,1,1,1,1,1,1,1,1,1,1,1,1,1,
1,1,1,1,1,1,1,1,1,1,1,1,1,1,1,1,1,1,1,1,1,1,1,1,1,1,1,1,1,1,1,1,1,1,1,6),
(2,2),(-1.,-0.995000000000001,-0.990000000000001,-0.985000000000001,-0.980000000000001,
-0.975000000000001,-0.970000000000001,-0.965000000000001,-0.960000000000001,
-0.955000000000001,-0.950000000000001,-0.945000000000001,-0.940000000000001,
-0.935000000000001,-0.930000000000001,-0.925000000000001,-0.920000000000001,
-0.915000000000001,-0.910000000000001,-0.905000000000001,-0.900000000000001,
-0.895000000000001,-0.890000000000001,-0.885000000000001,-0.880000000000001,
-0.875000000000001,-0.870000000000001,-0.865000000000001,-0.860000000000001,
-0.855000000000001,-0.850000000000001,-0.845000000000001,-0.840000000000001,
-0.835000000000001,-0.830000000000001,-0.825000000000001,-0.820000000000001,
-0.815000000000001,-0.810000000000001,-0.805000000000001,-0.800000000000001,
-0.795000000000001,-0.790000000000001,-0.785000000000001,-0.780000000000001,
-0.775000000000001,-0.770000000000001,-0.765000000000001,-0.760000000000001,
-0.755000000000001,-0.750000000000001,-0.745000000000001,-0.740000000000001,
-0.735000000000001,-0.730000000000001,-0.725000000000001,-0.720000000000001,
-0.715000000000001,-0.710000000000001,-0.705000000000001,-0.700000000000001,
-0.695000000000001,-0.690000000000001,-0.685,-0.68,-0.675,-0.67,-0.665,
-0.66,-0.655,-0.65,-0.645,-0.64,-0.635,-0.63,-0.625,-0.62,-0.615,-0.61,
-0.605,-0.6,-0.595,-0.59,-0.585,-0.58,-0.575,-0.57,-0.565,-0.56,-0.555,
-0.55,-0.545,-0.54,-0.535,-0.53,-0.525,-0.52,-0.515,-0.51,-0.505,-0.5,-0.495,
-0.49,-0.485,-0.48,-0.475,-0.47,-0.465,-0.46,-0.455,-0.45,-0.445,-0.44,
-0.435,-0.43,-0.425,-0.42,-0.415,-0.41,-0.405,-0.4,-0.395,-0.39,-0.385,
-0.38,-0.375,-0.37,-0.365,-0.36,-0.355,-0.35,-0.345,-0.34,-0.335,-0.33,
-0.325,-0.32,-0.315,-0.31,-0.305,-0.3,-0.295,-0.29,-0.285,-0.28,-0.275,
-0.27,-0.265,-0.26,-0.255,-0.25,-0.245,-0.24,-0.235,-0.23,-0.225,-0.22,
-0.215,-0.21,-0.205,-0.2,-0.195,-0.19,-0.185,-0.18,-0.175,-0.17,-0.165,
-0.16,-0.155,-0.15,-0.145,-0.14,-0.135,-0.13,-0.125,-0.12,-0.115,-0.11,
-0.105,-0.1,-0.095,-0.09,-0.085,-0.08,-0.075,-0.07,-0.065,-0.06,-0.055,
-0.05,-0.045,-0.04,-0.035,-0.03,-0.025,-0.02,-0.015,-0.01,-0.005,0.),(0.,
1.2),.UNSPECIFIED.)
GEOMETRIC_REPRESENTATION_ITEM()
RATIONAL_B_SPLINE_SURFACE(((1.,1.),(1.,1.),(1.,1.),(1.,1.),(1.,1.),(1.,
1.),(1.,1.),(1.,1.),(1.,1.),(1.,1.),(1.,1.),(1.,1.),(1.,1.),(1.,1.),(1.,
1.),(1.,1.),(1.,1.),(1.,1.),(1.,1.),(1.,1.),(1.,1.),(1.,1.),(1.,1.),(1.,
1.),(1.,1.),(1.,1.),(1.,1.),(1.,1.),(1.,1.),(1.,1.),(1.,1.),(1.,1.),(1.,
1.),(1.,1.),(1.,1.),(1.,1.),(1.,1.),(1.,1.),(1.,1.),(1.,1.),(1.,1.),(1.,
1.),(1.,1.),(1.,1.),(1.,1.),(1.,1.),(1.,1.),(1.,1.),(1.,1.),(1.,1.),(1.,
1.),(1.,1.),(1.,1.),(1.,1.),(1.,1.),(1.,1.),(1.,1.),(1.,1.),(1.,1.),(1.,
1.),(1.,1.),(1.,1.),(1.,1.),(1.,1.),(1.,1.),(1.,1.),(1.,1.),(1.,1.),(1.,
1.),(1.,1.),(1.,1.),(1.,1.),(1.,1.),(1.,1.),(1.,1.),(1.,1.),(1.,1.),(1.,
1.),(1.,1.),(1.,1.),(1.,1.),(1.,1.),(1.,1.),(1.,1.),(1.,1.),(1.,1.),(1.,
1.),(1.,1.),(1.,1.),(1.,1.),(1.,1.),(1.,1.),(1.,1.),(1.,1.),(1.,1.),(1.,
1.),(1.,1.),(1.,1.),(1.,1.),(1.,1.),(1.,1.),(1.,1.),(1.,1.),(1.,1.),(1.,
1.),(1.,1.),(1.,1.),(1.,1.),(1.,1.),(1.,1.),(1.,1.),(1.,1.),(1.,1.),(1.,
1.),(1.,1.),(1.,1.),(1.,1.),(1.,1.),(1.,1.),(1.,1.),(1.,1.),(1.,1.),(1.,
1.),(1.,1.),(1.,1.),(1.,1.),(1.,1.),(1.,1.),(1.,1.),(1.,1.),(1.,1.),(1.,
1.),(1.,1.),(1.,1.),(1.,1.),(1.,1.),(1.,1.),(1.,1.),(1.,1.),(1.,1.),(1.,
1.),(1.,1.),(1.,1.),(1.,1.),(1.,1.),(1.,1.),(1.,1.),(1.,1.),(1.,1.),(1.,
1.),(1.,1.),(1.,1.),(1.,1.),(1.,1.),(1.,1.),(1.,1.),(1.,1.),(1.,1.),(1.,
1.),(1.,1.),(1.,1.),(1.,1.),(1.,1.),(1.,1.),(1.,1.),(1.,1.),(1.,1.),(1.,
1.),(1.,1.),(1.,1.),(1.,1.),(1.,1.),(1.,1.),(1.,1.),(1.,1.),(1.,1.),(1.,
1.),(1.,1.),(1.,1.),(1.,1.),(1.,1.),(1.,1.),(1.,1.),(1.,1.),(1.,1.),(1.,
1.),(1.,1.),(1.,1.),(1.,1.),(1.,1.),(1.,1.),(1.,1.),(1.,1.),(1.,1.),(1.,
1.),(1.,1.),(1.,1.),(1.,1.),(1.,1.),(1.,1.),(1.,1.),(1.,1.),(1.,1.),(1.,
1.),(1.,1.)))
REPRESENTATION_ITEM('')
SURFACE()
);
#1046=(
BOUNDED_SURFACE()
B_SPLINE_SURFACE(5,1,((#197364,#197365),(#197366,#197367),(#197368,#197369),
(#197370,#197371),(#197372,#197373),(#197374,#197375),(#197376,#197377),
(#197378,#197379),(#197380,#197381),(#197382,#197383),(#197384,#197385),
(#197386,#197387),(#197388,#197389),(#197390,#197391),(#197392,#197393),
(#197394,#197395),(#197396,#197397),(#197398,#197399),(#197400,#197401),
(#197402,#197403),(#197404,#197405),(#197406,#197407),(#197408,#197409),
(#197410,#197411),(#197412,#197413),(#197414,#197415),(#197416,#197417),
(#197418,#197419),(#197420,#197421),(#197422,#197423),(#197424,#197425),
(#197426,#197427),(#197428,#197429),(#197430,#197431),(#197432,#197433),
(#197434,#197435),(#197436,#197437),(#197438,#197439),(#197440,#197441),
(#197442,#197443),(#197444,#197445),(#197446,#197447),(#197448,#197449),
(#197450,#197451),(#197452,#197453),(#197454,#197455),(#197456,#197457),
(#197458,#197459),(#197460,#197461),(#197462,#197463),(#197464,#197465),
(#197466,#197467),(#197468,#197469),(#197470,#197471),(#197472,#197473),
(#197474,#197475),(#197476,#197477),(#197478,#197479),(#197480,#197481),
(#197482,#197483),(#197484,#197485),(#197486,#197487),(#197488,#197489),
(#197490,#197491),(#197492,#197493),(#197494,#197495),(#197496,#197497),
(#197498,#197499),(#197500,#197501),(#197502,#197503),(#197504,#197505),
(#197506,#197507),(#197508,#197509),(#197510,#197511),(#197512,#197513),
(#197514,#197515),(#197516,#197517),(#197518,#197519),(#197520,#197521),
(#197522,#197523),(#197524,#197525),(#197526,#197527),(#197528,#197529),
(#197530,#197531),(#197532,#197533),(#197534,#197535),(#197536,#197537),
(#197538,#197539),(#197540,#197541),(#197542,#197543),(#197544,#197545),
(#197546,#197547),(#197548,#197549),(#197550,#197551),(#197552,#197553),
(#197554,#197555),(#197556,#197557),(#197558,#197559),(#197560,#197561),
(#197562,#197563),(#197564,#197565),(#197566,#197567),(#197568,#197569),
(#197570,#197571),(#197572,#197573),(#197574,#197575),(#197576,#197577),
(#197578,#197579),(#197580,#197581),(#197582,#197583),(#197584,#197585),
(#197586,#197587),(#197588,#197589),(#197590,#197591),(#197592,#197593),
(#197594,#197595),(#197596,#197597),(#197598,#197599),(#197600,#197601),
(#197602,#197603),(#197604,#197605),(#197606,#197607),(#197608,#197609),
(#197610,#197611),(#197612,#197613),(#197614,#197615),(#197616,#197617),
(#197618,#197619),(#197620,#197621),(#197622,#197623),(#197624,#197625),
(#197626,#197627),(#197628,#197629),(#197630,#197631),(#197632,#197633),
(#197634,#197635),(#197636,#197637),(#197638,#197639),(#197640,#197641),
(#197642,#197643),(#197644,#197645),(#197646,#197647),(#197648,#197649),
(#197650,#197651),(#197652,#197653),(#197654,#197655),(#197656,#197657),
(#197658,#197659),(#197660,#197661),(#197662,#197663),(#197664,#197665),
(#197666,#197667),(#197668,#197669),(#197670,#197671),(#197672,#197673),
(#197674,#197675),(#197676,#197677),(#197678,#197679),(#197680,#197681),
(#197682,#197683),(#197684,#197685),(#197686,#197687),(#197688,#197689),
(#197690,#197691),(#197692,#197693),(#197694,#197695),(#197696,#197697),
(#197698,#197699),(#197700,#197701),(#197702,#197703),(#197704,#197705),
(#197706,#197707),(#197708,#197709),(#197710,#197711),(#197712,#197713),
(#197714,#197715),(#197716,#197717),(#197718,#197719),(#197720,#197721),
(#197722,#197723),(#197724,#197725),(#197726,#197727),(#197728,#197729),
(#197730,#197731),(#197732,#197733),(#197734,#197735),(#197736,#197737),
(#197738,#197739),(#197740,#197741),(#197742,#197743),(#197744,#197745),
(#197746,#197747),(#197748,#197749),(#197750,#197751),(#197752,#197753),
(#197754,#197755),(#197756,#197757),(#197758,#197759),(#197760,#197761),
(#197762,#197763),(#197764,#197765),(#197766,#197767),(#197768,#197769),
(#197770,#197771),(#197772,#197773)),.UNSPECIFIED.,.F.,.F.,.F.)
B_SPLINE_SURFACE_WITH_KNOTS((6,1,1,1,1,1,1,1,1,1,1,1,1,1,1,1,1,1,1,1,1,
1,1,1,1,1,1,1,1,1,1,1,1,1,1,1,1,1,1,1,1,1,1,1,1,1,1,1,1,1,1,1,1,1,1,1,1,
1,1,1,1,1,1,1,1,1,1,1,1,1,1,1,1,1,1,1,1,1,1,1,1,1,1,1,1,1,1,1,1,1,1,1,1,
1,1,1,1,1,1,1,1,1,1,1,1,1,1,1,1,1,1,1,1,1,1,1,1,1,1,1,1,1,1,1,1,1,1,1,1,
1,1,1,1,1,1,1,1,1,1,1,1,1,1,1,1,1,1,1,1,1,1,1,1,1,1,1,1,1,1,1,1,1,1,1,1,
1,1,1,1,1,1,1,1,1,1,1,1,1,1,1,1,1,1,1,1,1,1,1,1,1,1,1,1,1,1,1,1,1,1,1,6),
(2,2),(0.,0.005,0.01,0.015,0.02,0.025,0.03,0.035,0.04,0.045,0.05,0.055,
0.06,0.065,0.07,0.075,0.08,0.085,0.09,0.095,0.1,0.105,0.11,0.115,0.12,0.125,
0.13,0.135,0.14,0.145,0.15,0.155,0.16,0.165,0.17,0.175,0.18,0.185,0.19,
0.195,0.2,0.205,0.21,0.215,0.22,0.225,0.23,0.235,0.24,0.245,0.25,0.255,
0.26,0.265,0.27,0.275,0.28,0.285,0.29,0.295,0.3,0.305,0.31,0.315,0.32,0.325,
0.33,0.335,0.34,0.345,0.35,0.355,0.36,0.365,0.37,0.375,0.38,0.385,0.39,
0.395,0.4,0.405,0.41,0.415,0.42,0.425,0.43,0.435,0.44,0.445,0.45,0.455,
0.46,0.465,0.47,0.475,0.48,0.485,0.49,0.495,0.5,0.505,0.51,0.515,0.52,0.525,
0.53,0.535,0.54,0.545,0.55,0.555,0.56,0.565,0.57,0.575,0.58,0.585,0.59,
0.595,0.6,0.605,0.61,0.615,0.62,0.625,0.63,0.635,0.64,0.645,0.65,0.655,
0.66,0.665,0.67,0.675,0.68,0.685,0.690000000000001,0.695000000000001,0.700000000000001,
0.705000000000001,0.710000000000001,0.715000000000001,0.720000000000001,
0.725000000000001,0.730000000000001,0.735000000000001,0.740000000000001,
0.745000000000001,0.750000000000001,0.755000000000001,0.760000000000001,
0.765000000000001,0.770000000000001,0.775000000000001,0.780000000000001,
0.785000000000001,0.790000000000001,0.795000000000001,0.800000000000001,
0.805000000000001,0.810000000000001,0.815000000000001,0.820000000000001,
0.825000000000001,0.830000000000001,0.835000000000001,0.840000000000001,
0.845000000000001,0.850000000000001,0.855000000000001,0.860000000000001,
0.865000000000001,0.870000000000001,0.875000000000001,0.880000000000001,
0.885000000000001,0.890000000000001,0.895000000000001,0.900000000000001,
0.905000000000001,0.910000000000001,0.915000000000001,0.920000000000001,
0.925000000000001,0.930000000000001,0.935000000000001,0.940000000000001,
0.945000000000001,0.950000000000001,0.955000000000001,0.960000000000001,
0.965000000000001,0.970000000000001,0.975000000000001,0.980000000000001,
0.985000000000001,0.990000000000001,0.995000000000001,1.),(0.,1.2),
 .UNSPECIFIED.)
GEOMETRIC_REPRESENTATION_ITEM()
RATIONAL_B_SPLINE_SURFACE(((1.,1.),(1.,1.),(1.,1.),(1.,1.),(1.,1.),(1.,
1.),(1.,1.),(1.,1.),(1.,1.),(1.,1.),(1.,1.),(1.,1.),(1.,1.),(1.,1.),(1.,
1.),(1.,1.),(1.,1.),(1.,1.),(1.,1.),(1.,1.),(1.,1.),(1.,1.),(1.,1.),(1.,
1.),(1.,1.),(1.,1.),(1.,1.),(1.,1.),(1.,1.),(1.,1.),(1.,1.),(1.,1.),(1.,
1.),(1.,1.),(1.,1.),(1.,1.),(1.,1.),(1.,1.),(1.,1.),(1.,1.),(1.,1.),(1.,
1.),(1.,1.),(1.,1.),(1.,1.),(1.,1.),(1.,1.),(1.,1.),(1.,1.),(1.,1.),(1.,
1.),(1.,1.),(1.,1.),(1.,1.),(1.,1.),(1.,1.),(1.,1.),(1.,1.),(1.,1.),(1.,
1.),(1.,1.),(1.,1.),(1.,1.),(1.,1.),(1.,1.),(1.,1.),(1.,1.),(1.,1.),(1.,
1.),(1.,1.),(1.,1.),(1.,1.),(1.,1.),(1.,1.),(1.,1.),(1.,1.),(1.,1.),(1.,
1.),(1.,1.),(1.,1.),(1.,1.),(1.,1.),(1.,1.),(1.,1.),(1.,1.),(1.,1.),(1.,
1.),(1.,1.),(1.,1.),(1.,1.),(1.,1.),(1.,1.),(1.,1.),(1.,1.),(1.,1.),(1.,
1.),(1.,1.),(1.,1.),(1.,1.),(1.,1.),(1.,1.),(1.,1.),(1.,1.),(1.,1.),(1.,
1.),(1.,1.),(1.,1.),(1.,1.),(1.,1.),(1.,1.),(1.,1.),(1.,1.),(1.,1.),(1.,
1.),(1.,1.),(1.,1.),(1.,1.),(1.,1.),(1.,1.),(1.,1.),(1.,1.),(1.,1.),(1.,
1.),(1.,1.),(1.,1.),(1.,1.),(1.,1.),(1.,1.),(1.,1.),(1.,1.),(1.,1.),(1.,
1.),(1.,1.),(1.,1.),(1.,1.),(1.,1.),(1.,1.),(1.,1.),(1.,1.),(1.,1.),(1.,
1.),(1.,1.),(1.,1.),(1.,1.),(1.,1.),(1.,1.),(1.,1.),(1.,1.),(1.,1.),(1.,
1.),(1.,1.),(1.,1.),(1.,1.),(1.,1.),(1.,1.),(1.,1.),(1.,1.),(1.,1.),(1.,
1.),(1.,1.),(1.,1.),(1.,1.),(1.,1.),(1.,1.),(1.,1.),(1.,1.),(1.,1.),(1.,
1.),(1.,1.),(1.,1.),(1.,1.),(1.,1.),(1.,1.),(1.,1.),(1.,1.),(1.,1.),(1.,
1.),(1.,1.),(1.,1.),(1.,1.),(1.,1.),(1.,1.),(1.,1.),(1.,1.),(1.,1.),(1.,
1.),(1.,1.),(1.,1.),(1.,1.),(1.,1.),(1.,1.),(1.,1.),(1.,1.),(1.,1.),(1.,
1.),(1.,1.),(1.,1.),(1.,1.),(1.,1.),(1.,1.),(1.,1.),(1.,1.),(1.,1.),(1.,
1.),(1.,1.)))
REPRESENTATION_ITEM('')
SURFACE()
);
#1047=(
BOUNDED_SURFACE()
B_SPLINE_SURFACE(5,1,((#197985,#197986),(#197987,#197988),(#197989,#197990),
(#197991,#197992),(#197993,#197994),(#197995,#197996),(#197997,#197998),
(#197999,#198000),(#198001,#198002),(#198003,#198004),(#198005,#198006),
(#198007,#198008),(#198009,#198010),(#198011,#198012),(#198013,#198014),
(#198015,#198016),(#198017,#198018),(#198019,#198020),(#198021,#198022),
(#198023,#198024),(#198025,#198026),(#198027,#198028),(#198029,#198030),
(#198031,#198032),(#198033,#198034),(#198035,#198036),(#198037,#198038),
(#198039,#198040),(#198041,#198042),(#198043,#198044),(#198045,#198046),
(#198047,#198048),(#198049,#198050),(#198051,#198052),(#198053,#198054),
(#198055,#198056),(#198057,#198058),(#198059,#198060),(#198061,#198062),
(#198063,#198064),(#198065,#198066),(#198067,#198068),(#198069,#198070),
(#198071,#198072),(#198073,#198074),(#198075,#198076),(#198077,#198078),
(#198079,#198080),(#198081,#198082),(#198083,#198084),(#198085,#198086),
(#198087,#198088),(#198089,#198090),(#198091,#198092),(#198093,#198094),
(#198095,#198096),(#198097,#198098),(#198099,#198100),(#198101,#198102),
(#198103,#198104),(#198105,#198106),(#198107,#198108),(#198109,#198110),
(#198111,#198112),(#198113,#198114),(#198115,#198116),(#198117,#198118),
(#198119,#198120),(#198121,#198122),(#198123,#198124),(#198125,#198126),
(#198127,#198128),(#198129,#198130),(#198131,#198132),(#198133,#198134),
(#198135,#198136),(#198137,#198138),(#198139,#198140),(#198141,#198142),
(#198143,#198144),(#198145,#198146),(#198147,#198148),(#198149,#198150),
(#198151,#198152),(#198153,#198154),(#198155,#198156),(#198157,#198158),
(#198159,#198160),(#198161,#198162),(#198163,#198164),(#198165,#198166),
(#198167,#198168),(#198169,#198170),(#198171,#198172),(#198173,#198174),
(#198175,#198176),(#198177,#198178),(#198179,#198180),(#198181,#198182),
(#198183,#198184),(#198185,#198186),(#198187,#198188),(#198189,#198190),
(#198191,#198192),(#198193,#198194),(#198195,#198196),(#198197,#198198),
(#198199,#198200),(#198201,#198202),(#198203,#198204),(#198205,#198206),
(#198207,#198208),(#198209,#198210),(#198211,#198212),(#198213,#198214),
(#198215,#198216),(#198217,#198218),(#198219,#198220),(#198221,#198222),
(#198223,#198224),(#198225,#198226),(#198227,#198228),(#198229,#198230),
(#198231,#198232),(#198233,#198234),(#198235,#198236),(#198237,#198238),
(#198239,#198240),(#198241,#198242),(#198243,#198244),(#198245,#198246),
(#198247,#198248),(#198249,#198250),(#198251,#198252),(#198253,#198254),
(#198255,#198256),(#198257,#198258),(#198259,#198260),(#198261,#198262),
(#198263,#198264),(#198265,#198266),(#198267,#198268),(#198269,#198270),
(#198271,#198272),(#198273,#198274),(#198275,#198276),(#198277,#198278),
(#198279,#198280),(#198281,#198282),(#198283,#198284),(#198285,#198286),
(#198287,#198288),(#198289,#198290),(#198291,#198292),(#198293,#198294),
(#198295,#198296),(#198297,#198298),(#198299,#198300),(#198301,#198302),
(#198303,#198304),(#198305,#198306),(#198307,#198308),(#198309,#198310),
(#198311,#198312),(#198313,#198314),(#198315,#198316),(#198317,#198318),
(#198319,#198320),(#198321,#198322),(#198323,#198324),(#198325,#198326),
(#198327,#198328),(#198329,#198330),(#198331,#198332),(#198333,#198334),
(#198335,#198336),(#198337,#198338),(#198339,#198340),(#198341,#198342),
(#198343,#198344),(#198345,#198346),(#198347,#198348),(#198349,#198350),
(#198351,#198352),(#198353,#198354),(#198355,#198356),(#198357,#198358),
(#198359,#198360),(#198361,#198362),(#198363,#198364),(#198365,#198366),
(#198367,#198368),(#198369,#198370),(#198371,#198372),(#198373,#198374),
(#198375,#198376),(#198377,#198378),(#198379,#198380),(#198381,#198382),
(#198383,#198384),(#198385,#198386),(#198387,#198388),(#198389,#198390),
(#198391,#198392),(#198393,#198394)),.UNSPECIFIED.,.F.,.F.,.F.)
B_SPLINE_SURFACE_WITH_KNOTS((6,1,1,1,1,1,1,1,1,1,1,1,1,1,1,1,1,1,1,1,1,
1,1,1,1,1,1,1,1,1,1,1,1,1,1,1,1,1,1,1,1,1,1,1,1,1,1,1,1,1,1,1,1,1,1,1,1,
1,1,1,1,1,1,1,1,1,1,1,1,1,1,1,1,1,1,1,1,1,1,1,1,1,1,1,1,1,1,1,1,1,1,1,1,
1,1,1,1,1,1,1,1,1,1,1,1,1,1,1,1,1,1,1,1,1,1,1,1,1,1,1,1,1,1,1,1,1,1,1,1,
1,1,1,1,1,1,1,1,1,1,1,1,1,1,1,1,1,1,1,1,1,1,1,1,1,1,1,1,1,1,1,1,1,1,1,1,
1,1,1,1,1,1,1,1,1,1,1,1,1,1,1,1,1,1,1,1,1,1,1,1,1,1,1,1,1,1,1,1,1,1,1,6),
(2,2),(-1.,-0.995000000000001,-0.990000000000001,-0.985000000000001,-0.980000000000001,
-0.975000000000001,-0.970000000000001,-0.965000000000001,-0.960000000000001,
-0.955000000000001,-0.950000000000001,-0.945000000000001,-0.940000000000001,
-0.935000000000001,-0.930000000000001,-0.925000000000001,-0.920000000000001,
-0.915000000000001,-0.910000000000001,-0.905000000000001,-0.900000000000001,
-0.895000000000001,-0.890000000000001,-0.885000000000001,-0.880000000000001,
-0.875000000000001,-0.870000000000001,-0.865000000000001,-0.860000000000001,
-0.855000000000001,-0.850000000000001,-0.845000000000001,-0.840000000000001,
-0.835000000000001,-0.830000000000001,-0.825000000000001,-0.820000000000001,
-0.815000000000001,-0.810000000000001,-0.805000000000001,-0.800000000000001,
-0.795000000000001,-0.790000000000001,-0.785000000000001,-0.780000000000001,
-0.775000000000001,-0.770000000000001,-0.765000000000001,-0.760000000000001,
-0.755000000000001,-0.750000000000001,-0.745000000000001,-0.740000000000001,
-0.735000000000001,-0.730000000000001,-0.725000000000001,-0.720000000000001,
-0.715000000000001,-0.710000000000001,-0.705000000000001,-0.700000000000001,
-0.695000000000001,-0.690000000000001,-0.685,-0.68,-0.675,-0.67,-0.665,
-0.66,-0.655,-0.65,-0.645,-0.64,-0.635,-0.63,-0.625,-0.62,-0.615,-0.61,
-0.605,-0.6,-0.595,-0.59,-0.585,-0.58,-0.575,-0.57,-0.565,-0.56,-0.555,
-0.55,-0.545,-0.54,-0.535,-0.53,-0.525,-0.52,-0.515,-0.51,-0.505,-0.5,-0.495,
-0.49,-0.485,-0.48,-0.475,-0.47,-0.465,-0.46,-0.455,-0.45,-0.445,-0.44,
-0.435,-0.43,-0.425,-0.42,-0.415,-0.41,-0.405,-0.4,-0.395,-0.39,-0.385,
-0.38,-0.375,-0.37,-0.365,-0.36,-0.355,-0.35,-0.345,-0.34,-0.335,-0.33,
-0.325,-0.32,-0.315,-0.31,-0.305,-0.3,-0.295,-0.29,-0.285,-0.28,-0.275,
-0.27,-0.265,-0.26,-0.255,-0.25,-0.245,-0.24,-0.235,-0.23,-0.225,-0.22,
-0.215,-0.21,-0.205,-0.2,-0.195,-0.19,-0.185,-0.18,-0.175,-0.17,-0.165,
-0.16,-0.155,-0.15,-0.145,-0.14,-0.135,-0.13,-0.125,-0.12,-0.115,-0.11,
-0.105,-0.1,-0.095,-0.09,-0.085,-0.08,-0.075,-0.07,-0.065,-0.06,-0.055,
-0.05,-0.045,-0.04,-0.035,-0.03,-0.025,-0.02,-0.015,-0.01,-0.005,0.),(0.,
1.2),.UNSPECIFIED.)
GEOMETRIC_REPRESENTATION_ITEM()
RATIONAL_B_SPLINE_SURFACE(((1.,1.),(1.,1.),(1.,1.),(1.,1.),(1.,1.),(1.,
1.),(1.,1.),(1.,1.),(1.,1.),(1.,1.),(1.,1.),(1.,1.),(1.,1.),(1.,1.),(1.,
1.),(1.,1.),(1.,1.),(1.,1.),(1.,1.),(1.,1.),(1.,1.),(1.,1.),(1.,1.),(1.,
1.),(1.,1.),(1.,1.),(1.,1.),(1.,1.),(1.,1.),(1.,1.),(1.,1.),(1.,1.),(1.,
1.),(1.,1.),(1.,1.),(1.,1.),(1.,1.),(1.,1.),(1.,1.),(1.,1.),(1.,1.),(1.,
1.),(1.,1.),(1.,1.),(1.,1.),(1.,1.),(1.,1.),(1.,1.),(1.,1.),(1.,1.),(1.,
1.),(1.,1.),(1.,1.),(1.,1.),(1.,1.),(1.,1.),(1.,1.),(1.,1.),(1.,1.),(1.,
1.),(1.,1.),(1.,1.),(1.,1.),(1.,1.),(1.,1.),(1.,1.),(1.,1.),(1.,1.),(1.,
1.),(1.,1.),(1.,1.),(1.,1.),(1.,1.),(1.,1.),(1.,1.),(1.,1.),(1.,1.),(1.,
1.),(1.,1.),(1.,1.),(1.,1.),(1.,1.),(1.,1.),(1.,1.),(1.,1.),(1.,1.),(1.,
1.),(1.,1.),(1.,1.),(1.,1.),(1.,1.),(1.,1.),(1.,1.),(1.,1.),(1.,1.),(1.,
1.),(1.,1.),(1.,1.),(1.,1.),(1.,1.),(1.,1.),(1.,1.),(1.,1.),(1.,1.),(1.,
1.),(1.,1.),(1.,1.),(1.,1.),(1.,1.),(1.,1.),(1.,1.),(1.,1.),(1.,1.),(1.,
1.),(1.,1.),(1.,1.),(1.,1.),(1.,1.),(1.,1.),(1.,1.),(1.,1.),(1.,1.),(1.,
1.),(1.,1.),(1.,1.),(1.,1.),(1.,1.),(1.,1.),(1.,1.),(1.,1.),(1.,1.),(1.,
1.),(1.,1.),(1.,1.),(1.,1.),(1.,1.),(1.,1.),(1.,1.),(1.,1.),(1.,1.),(1.,
1.),(1.,1.),(1.,1.),(1.,1.),(1.,1.),(1.,1.),(1.,1.),(1.,1.),(1.,1.),(1.,
1.),(1.,1.),(1.,1.),(1.,1.),(1.,1.),(1.,1.),(1.,1.),(1.,1.),(1.,1.),(1.,
1.),(1.,1.),(1.,1.),(1.,1.),(1.,1.),(1.,1.),(1.,1.),(1.,1.),(1.,1.),(1.,
1.),(1.,1.),(1.,1.),(1.,1.),(1.,1.),(1.,1.),(1.,1.),(1.,1.),(1.,1.),(1.,
1.),(1.,1.),(1.,1.),(1.,1.),(1.,1.),(1.,1.),(1.,1.),(1.,1.),(1.,1.),(1.,
1.),(1.,1.),(1.,1.),(1.,1.),(1.,1.),(1.,1.),(1.,1.),(1.,1.),(1.,1.),(1.,
1.),(1.,1.),(1.,1.),(1.,1.),(1.,1.),(1.,1.),(1.,1.),(1.,1.),(1.,1.),(1.,
1.),(1.,1.)))
REPRESENTATION_ITEM('')
SURFACE()
);
#1048=(
BOUNDED_SURFACE()
B_SPLINE_SURFACE(5,1,((#198602,#198603),(#198604,#198605),(#198606,#198607),
(#198608,#198609),(#198610,#198611),(#198612,#198613),(#198614,#198615),
(#198616,#198617),(#198618,#198619),(#198620,#198621),(#198622,#198623),
(#198624,#198625),(#198626,#198627),(#198628,#198629),(#198630,#198631),
(#198632,#198633),(#198634,#198635),(#198636,#198637),(#198638,#198639),
(#198640,#198641),(#198642,#198643),(#198644,#198645),(#198646,#198647),
(#198648,#198649),(#198650,#198651),(#198652,#198653),(#198654,#198655),
(#198656,#198657),(#198658,#198659),(#198660,#198661),(#198662,#198663),
(#198664,#198665),(#198666,#198667),(#198668,#198669),(#198670,#198671),
(#198672,#198673),(#198674,#198675),(#198676,#198677),(#198678,#198679),
(#198680,#198681),(#198682,#198683),(#198684,#198685),(#198686,#198687),
(#198688,#198689),(#198690,#198691),(#198692,#198693),(#198694,#198695),
(#198696,#198697),(#198698,#198699),(#198700,#198701),(#198702,#198703),
(#198704,#198705),(#198706,#198707),(#198708,#198709),(#198710,#198711),
(#198712,#198713),(#198714,#198715),(#198716,#198717),(#198718,#198719),
(#198720,#198721),(#198722,#198723),(#198724,#198725),(#198726,#198727),
(#198728,#198729),(#198730,#198731),(#198732,#198733),(#198734,#198735),
(#198736,#198737),(#198738,#198739),(#198740,#198741),(#198742,#198743),
(#198744,#198745),(#198746,#198747),(#198748,#198749),(#198750,#198751),
(#198752,#198753),(#198754,#198755),(#198756,#198757),(#198758,#198759),
(#198760,#198761),(#198762,#198763),(#198764,#198765),(#198766,#198767),
(#198768,#198769),(#198770,#198771),(#198772,#198773),(#198774,#198775),
(#198776,#198777),(#198778,#198779),(#198780,#198781),(#198782,#198783),
(#198784,#198785),(#198786,#198787),(#198788,#198789),(#198790,#198791),
(#198792,#198793),(#198794,#198795),(#198796,#198797),(#198798,#198799),
(#198800,#198801),(#198802,#198803),(#198804,#198805),(#198806,#198807),
(#198808,#198809),(#198810,#198811),(#198812,#198813),(#198814,#198815),
(#198816,#198817),(#198818,#198819),(#198820,#198821),(#198822,#198823),
(#198824,#198825),(#198826,#198827),(#198828,#198829),(#198830,#198831),
(#198832,#198833),(#198834,#198835),(#198836,#198837),(#198838,#198839),
(#198840,#198841),(#198842,#198843),(#198844,#198845),(#198846,#198847),
(#198848,#198849),(#198850,#198851),(#198852,#198853),(#198854,#198855),
(#198856,#198857),(#198858,#198859),(#198860,#198861),(#198862,#198863),
(#198864,#198865),(#198866,#198867),(#198868,#198869),(#198870,#198871),
(#198872,#198873),(#198874,#198875),(#198876,#198877),(#198878,#198879),
(#198880,#198881),(#198882,#198883),(#198884,#198885),(#198886,#198887),
(#198888,#198889),(#198890,#198891),(#198892,#198893),(#198894,#198895),
(#198896,#198897),(#198898,#198899),(#198900,#198901),(#198902,#198903),
(#198904,#198905),(#198906,#198907),(#198908,#198909),(#198910,#198911),
(#198912,#198913),(#198914,#198915),(#198916,#198917),(#198918,#198919),
(#198920,#198921),(#198922,#198923),(#198924,#198925),(#198926,#198927),
(#198928,#198929),(#198930,#198931),(#198932,#198933),(#198934,#198935),
(#198936,#198937),(#198938,#198939),(#198940,#198941),(#198942,#198943),
(#198944,#198945),(#198946,#198947),(#198948,#198949),(#198950,#198951),
(#198952,#198953),(#198954,#198955),(#198956,#198957),(#198958,#198959),
(#198960,#198961),(#198962,#198963),(#198964,#198965),(#198966,#198967),
(#198968,#198969),(#198970,#198971),(#198972,#198973),(#198974,#198975),
(#198976,#198977),(#198978,#198979),(#198980,#198981),(#198982,#198983),
(#198984,#198985),(#198986,#198987),(#198988,#198989),(#198990,#198991),
(#198992,#198993),(#198994,#198995),(#198996,#198997),(#198998,#198999),
(#199000,#199001),(#199002,#199003),(#199004,#199005),(#199006,#199007),
(#199008,#199009),(#199010,#199011)),.UNSPECIFIED.,.F.,.F.,.F.)
B_SPLINE_SURFACE_WITH_KNOTS((6,1,1,1,1,1,1,1,1,1,1,1,1,1,1,1,1,1,1,1,1,
1,1,1,1,1,1,1,1,1,1,1,1,1,1,1,1,1,1,1,1,1,1,1,1,1,1,1,1,1,1,1,1,1,1,1,1,
1,1,1,1,1,1,1,1,1,1,1,1,1,1,1,1,1,1,1,1,1,1,1,1,1,1,1,1,1,1,1,1,1,1,1,1,
1,1,1,1,1,1,1,1,1,1,1,1,1,1,1,1,1,1,1,1,1,1,1,1,1,1,1,1,1,1,1,1,1,1,1,1,
1,1,1,1,1,1,1,1,1,1,1,1,1,1,1,1,1,1,1,1,1,1,1,1,1,1,1,1,1,1,1,1,1,1,1,1,
1,1,1,1,1,1,1,1,1,1,1,1,1,1,1,1,1,1,1,1,1,1,1,1,1,1,1,1,1,1,1,1,1,1,1,6),
(2,2),(0.,0.005,0.01,0.015,0.02,0.025,0.03,0.035,0.04,0.045,0.05,0.055,
0.06,0.065,0.07,0.075,0.08,0.085,0.09,0.095,0.1,0.105,0.11,0.115,0.12,0.125,
0.13,0.135,0.14,0.145,0.15,0.155,0.16,0.165,0.17,0.175,0.18,0.185,0.19,
0.195,0.2,0.205,0.21,0.215,0.22,0.225,0.23,0.235,0.24,0.245,0.25,0.255,
0.26,0.265,0.27,0.275,0.28,0.285,0.29,0.295,0.3,0.305,0.31,0.315,0.32,0.325,
0.33,0.335,0.34,0.345,0.35,0.355,0.36,0.365,0.37,0.375,0.38,0.385,0.39,
0.395,0.4,0.405,0.41,0.415,0.42,0.425,0.43,0.435,0.44,0.445,0.45,0.455,
0.46,0.465,0.47,0.475,0.48,0.485,0.49,0.495,0.5,0.505,0.51,0.515,0.52,0.525,
0.53,0.535,0.54,0.545,0.55,0.555,0.56,0.565,0.57,0.575,0.58,0.585,0.59,
0.595,0.6,0.605,0.61,0.615,0.62,0.625,0.63,0.635,0.64,0.645,0.65,0.655,
0.66,0.665,0.67,0.675,0.68,0.685,0.690000000000001,0.695000000000001,0.700000000000001,
0.705000000000001,0.710000000000001,0.715000000000001,0.720000000000001,
0.725000000000001,0.730000000000001,0.735000000000001,0.740000000000001,
0.745000000000001,0.750000000000001,0.755000000000001,0.760000000000001,
0.765000000000001,0.770000000000001,0.775000000000001,0.780000000000001,
0.785000000000001,0.790000000000001,0.795000000000001,0.800000000000001,
0.805000000000001,0.810000000000001,0.815000000000001,0.820000000000001,
0.825000000000001,0.830000000000001,0.835000000000001,0.840000000000001,
0.845000000000001,0.850000000000001,0.855000000000001,0.860000000000001,
0.865000000000001,0.870000000000001,0.875000000000001,0.880000000000001,
0.885000000000001,0.890000000000001,0.895000000000001,0.900000000000001,
0.905000000000001,0.910000000000001,0.915000000000001,0.920000000000001,
0.925000000000001,0.930000000000001,0.935000000000001,0.940000000000001,
0.945000000000001,0.950000000000001,0.955000000000001,0.960000000000001,
0.965000000000001,0.970000000000001,0.975000000000001,0.980000000000001,
0.985000000000001,0.990000000000001,0.995000000000001,1.),(0.,1.2),
 .UNSPECIFIED.)
GEOMETRIC_REPRESENTATION_ITEM()
RATIONAL_B_SPLINE_SURFACE(((1.,1.),(1.,1.),(1.,1.),(1.,1.),(1.,1.),(1.,
1.),(1.,1.),(1.,1.),(1.,1.),(1.,1.),(1.,1.),(1.,1.),(1.,1.),(1.,1.),(1.,
1.),(1.,1.),(1.,1.),(1.,1.),(1.,1.),(1.,1.),(1.,1.),(1.,1.),(1.,1.),(1.,
1.),(1.,1.),(1.,1.),(1.,1.),(1.,1.),(1.,1.),(1.,1.),(1.,1.),(1.,1.),(1.,
1.),(1.,1.),(1.,1.),(1.,1.),(1.,1.),(1.,1.),(1.,1.),(1.,1.),(1.,1.),(1.,
1.),(1.,1.),(1.,1.),(1.,1.),(1.,1.),(1.,1.),(1.,1.),(1.,1.),(1.,1.),(1.,
1.),(1.,1.),(1.,1.),(1.,1.),(1.,1.),(1.,1.),(1.,1.),(1.,1.),(1.,1.),(1.,
1.),(1.,1.),(1.,1.),(1.,1.),(1.,1.),(1.,1.),(1.,1.),(1.,1.),(1.,1.),(1.,
1.),(1.,1.),(1.,1.),(1.,1.),(1.,1.),(1.,1.),(1.,1.),(1.,1.),(1.,1.),(1.,
1.),(1.,1.),(1.,1.),(1.,1.),(1.,1.),(1.,1.),(1.,1.),(1.,1.),(1.,1.),(1.,
1.),(1.,1.),(1.,1.),(1.,1.),(1.,1.),(1.,1.),(1.,1.),(1.,1.),(1.,1.),(1.,
1.),(1.,1.),(1.,1.),(1.,1.),(1.,1.),(1.,1.),(1.,1.),(1.,1.),(1.,1.),(1.,
1.),(1.,1.),(1.,1.),(1.,1.),(1.,1.),(1.,1.),(1.,1.),(1.,1.),(1.,1.),(1.,
1.),(1.,1.),(1.,1.),(1.,1.),(1.,1.),(1.,1.),(1.,1.),(1.,1.),(1.,1.),(1.,
1.),(1.,1.),(1.,1.),(1.,1.),(1.,1.),(1.,1.),(1.,1.),(1.,1.),(1.,1.),(1.,
1.),(1.,1.),(1.,1.),(1.,1.),(1.,1.),(1.,1.),(1.,1.),(1.,1.),(1.,1.),(1.,
1.),(1.,1.),(1.,1.),(1.,1.),(1.,1.),(1.,1.),(1.,1.),(1.,1.),(1.,1.),(1.,
1.),(1.,1.),(1.,1.),(1.,1.),(1.,1.),(1.,1.),(1.,1.),(1.,1.),(1.,1.),(1.,
1.),(1.,1.),(1.,1.),(1.,1.),(1.,1.),(1.,1.),(1.,1.),(1.,1.),(1.,1.),(1.,
1.),(1.,1.),(1.,1.),(1.,1.),(1.,1.),(1.,1.),(1.,1.),(1.,1.),(1.,1.),(1.,
1.),(1.,1.),(1.,1.),(1.,1.),(1.,1.),(1.,1.),(1.,1.),(1.,1.),(1.,1.),(1.,
1.),(1.,1.),(1.,1.),(1.,1.),(1.,1.),(1.,1.),(1.,1.),(1.,1.),(1.,1.),(1.,
1.),(1.,1.),(1.,1.),(1.,1.),(1.,1.),(1.,1.),(1.,1.),(1.,1.),(1.,1.),(1.,
1.),(1.,1.)))
REPRESENTATION_ITEM('')
SURFACE()
);
#1049=(
BOUNDED_SURFACE()
B_SPLINE_SURFACE(5,1,((#199223,#199224),(#199225,#199226),(#199227,#199228),
(#199229,#199230),(#199231,#199232),(#199233,#199234),(#199235,#199236),
(#199237,#199238),(#199239,#199240),(#199241,#199242),(#199243,#199244),
(#199245,#199246),(#199247,#199248),(#199249,#199250),(#199251,#199252),
(#199253,#199254),(#199255,#199256),(#199257,#199258),(#199259,#199260),
(#199261,#199262),(#199263,#199264),(#199265,#199266),(#199267,#199268),
(#199269,#199270),(#199271,#199272),(#199273,#199274),(#199275,#199276),
(#199277,#199278),(#199279,#199280),(#199281,#199282),(#199283,#199284),
(#199285,#199286),(#199287,#199288),(#199289,#199290),(#199291,#199292),
(#199293,#199294),(#199295,#199296),(#199297,#199298),(#199299,#199300),
(#199301,#199302),(#199303,#199304),(#199305,#199306),(#199307,#199308),
(#199309,#199310),(#199311,#199312),(#199313,#199314),(#199315,#199316),
(#199317,#199318),(#199319,#199320),(#199321,#199322),(#199323,#199324),
(#199325,#199326),(#199327,#199328),(#199329,#199330),(#199331,#199332),
(#199333,#199334),(#199335,#199336),(#199337,#199338),(#199339,#199340),
(#199341,#199342),(#199343,#199344),(#199345,#199346),(#199347,#199348),
(#199349,#199350),(#199351,#199352),(#199353,#199354),(#199355,#199356),
(#199357,#199358),(#199359,#199360),(#199361,#199362),(#199363,#199364),
(#199365,#199366),(#199367,#199368),(#199369,#199370),(#199371,#199372),
(#199373,#199374),(#199375,#199376),(#199377,#199378),(#199379,#199380),
(#199381,#199382),(#199383,#199384),(#199385,#199386),(#199387,#199388),
(#199389,#199390),(#199391,#199392),(#199393,#199394),(#199395,#199396),
(#199397,#199398),(#199399,#199400),(#199401,#199402),(#199403,#199404),
(#199405,#199406),(#199407,#199408),(#199409,#199410),(#199411,#199412),
(#199413,#199414),(#199415,#199416),(#199417,#199418),(#199419,#199420),
(#199421,#199422),(#199423,#199424),(#199425,#199426),(#199427,#199428),
(#199429,#199430),(#199431,#199432),(#199433,#199434),(#199435,#199436),
(#199437,#199438),(#199439,#199440),(#199441,#199442),(#199443,#199444),
(#199445,#199446),(#199447,#199448),(#199449,#199450),(#199451,#199452),
(#199453,#199454),(#199455,#199456),(#199457,#199458),(#199459,#199460),
(#199461,#199462),(#199463,#199464),(#199465,#199466),(#199467,#199468),
(#199469,#199470),(#199471,#199472),(#199473,#199474),(#199475,#199476),
(#199477,#199478),(#199479,#199480),(#199481,#199482),(#199483,#199484),
(#199485,#199486),(#199487,#199488),(#199489,#199490),(#199491,#199492),
(#199493,#199494),(#199495,#199496),(#199497,#199498),(#199499,#199500),
(#199501,#199502),(#199503,#199504),(#199505,#199506),(#199507,#199508),
(#199509,#199510),(#199511,#199512),(#199513,#199514),(#199515,#199516),
(#199517,#199518),(#199519,#199520),(#199521,#199522),(#199523,#199524),
(#199525,#199526),(#199527,#199528),(#199529,#199530),(#199531,#199532),
(#199533,#199534),(#199535,#199536),(#199537,#199538),(#199539,#199540),
(#199541,#199542),(#199543,#199544),(#199545,#199546),(#199547,#199548),
(#199549,#199550),(#199551,#199552),(#199553,#199554),(#199555,#199556),
(#199557,#199558),(#199559,#199560),(#199561,#199562),(#199563,#199564),
(#199565,#199566),(#199567,#199568),(#199569,#199570),(#199571,#199572),
(#199573,#199574),(#199575,#199576),(#199577,#199578),(#199579,#199580),
(#199581,#199582),(#199583,#199584),(#199585,#199586),(#199587,#199588),
(#199589,#199590),(#199591,#199592),(#199593,#199594),(#199595,#199596),
(#199597,#199598),(#199599,#199600),(#199601,#199602),(#199603,#199604),
(#199605,#199606),(#199607,#199608),(#199609,#199610),(#199611,#199612),
(#199613,#199614),(#199615,#199616),(#199617,#199618),(#199619,#199620),
(#199621,#199622),(#199623,#199624),(#199625,#199626),(#199627,#199628),
(#199629,#199630),(#199631,#199632)),.UNSPECIFIED.,.F.,.F.,.F.)
B_SPLINE_SURFACE_WITH_KNOTS((6,1,1,1,1,1,1,1,1,1,1,1,1,1,1,1,1,1,1,1,1,
1,1,1,1,1,1,1,1,1,1,1,1,1,1,1,1,1,1,1,1,1,1,1,1,1,1,1,1,1,1,1,1,1,1,1,1,
1,1,1,1,1,1,1,1,1,1,1,1,1,1,1,1,1,1,1,1,1,1,1,1,1,1,1,1,1,1,1,1,1,1,1,1,
1,1,1,1,1,1,1,1,1,1,1,1,1,1,1,1,1,1,1,1,1,1,1,1,1,1,1,1,1,1,1,1,1,1,1,1,
1,1,1,1,1,1,1,1,1,1,1,1,1,1,1,1,1,1,1,1,1,1,1,1,1,1,1,1,1,1,1,1,1,1,1,1,
1,1,1,1,1,1,1,1,1,1,1,1,1,1,1,1,1,1,1,1,1,1,1,1,1,1,1,1,1,1,1,1,1,1,1,6),
(2,2),(-1.,-0.995000000000001,-0.990000000000001,-0.985000000000001,-0.980000000000001,
-0.975000000000001,-0.970000000000001,-0.965000000000001,-0.960000000000001,
-0.955000000000001,-0.950000000000001,-0.945000000000001,-0.940000000000001,
-0.935000000000001,-0.930000000000001,-0.925000000000001,-0.920000000000001,
-0.915000000000001,-0.910000000000001,-0.905000000000001,-0.900000000000001,
-0.895000000000001,-0.890000000000001,-0.885000000000001,-0.880000000000001,
-0.875000000000001,-0.870000000000001,-0.865000000000001,-0.860000000000001,
-0.855000000000001,-0.850000000000001,-0.845000000000001,-0.840000000000001,
-0.835000000000001,-0.830000000000001,-0.825000000000001,-0.820000000000001,
-0.815000000000001,-0.810000000000001,-0.805000000000001,-0.800000000000001,
-0.795000000000001,-0.790000000000001,-0.785000000000001,-0.780000000000001,
-0.775000000000001,-0.770000000000001,-0.765000000000001,-0.760000000000001,
-0.755000000000001,-0.750000000000001,-0.745000000000001,-0.740000000000001,
-0.735000000000001,-0.730000000000001,-0.725000000000001,-0.720000000000001,
-0.715000000000001,-0.710000000000001,-0.705000000000001,-0.700000000000001,
-0.695000000000001,-0.690000000000001,-0.685,-0.68,-0.675,-0.67,-0.665,
-0.66,-0.655,-0.65,-0.645,-0.64,-0.635,-0.63,-0.625,-0.62,-0.615,-0.61,
-0.605,-0.6,-0.595,-0.59,-0.585,-0.58,-0.575,-0.57,-0.565,-0.56,-0.555,
-0.55,-0.545,-0.54,-0.535,-0.53,-0.525,-0.52,-0.515,-0.51,-0.505,-0.5,-0.495,
-0.49,-0.485,-0.48,-0.475,-0.47,-0.465,-0.46,-0.455,-0.45,-0.445,-0.44,
-0.435,-0.43,-0.425,-0.42,-0.415,-0.41,-0.405,-0.4,-0.395,-0.39,-0.385,
-0.38,-0.375,-0.37,-0.365,-0.36,-0.355,-0.35,-0.345,-0.34,-0.335,-0.33,
-0.325,-0.32,-0.315,-0.31,-0.305,-0.3,-0.295,-0.29,-0.285,-0.28,-0.275,
-0.27,-0.265,-0.26,-0.255,-0.25,-0.245,-0.24,-0.235,-0.23,-0.225,-0.22,
-0.215,-0.21,-0.205,-0.2,-0.195,-0.19,-0.185,-0.18,-0.175,-0.17,-0.165,
-0.16,-0.155,-0.15,-0.145,-0.14,-0.135,-0.13,-0.125,-0.12,-0.115,-0.11,
-0.105,-0.1,-0.095,-0.09,-0.085,-0.08,-0.075,-0.07,-0.065,-0.06,-0.055,
-0.05,-0.045,-0.04,-0.035,-0.03,-0.025,-0.02,-0.015,-0.01,-0.005,0.),(0.,
1.2),.UNSPECIFIED.)
GEOMETRIC_REPRESENTATION_ITEM()
RATIONAL_B_SPLINE_SURFACE(((1.,1.),(1.,1.),(1.,1.),(1.,1.),(1.,1.),(1.,
1.),(1.,1.),(1.,1.),(1.,1.),(1.,1.),(1.,1.),(1.,1.),(1.,1.),(1.,1.),(1.,
1.),(1.,1.),(1.,1.),(1.,1.),(1.,1.),(1.,1.),(1.,1.),(1.,1.),(1.,1.),(1.,
1.),(1.,1.),(1.,1.),(1.,1.),(1.,1.),(1.,1.),(1.,1.),(1.,1.),(1.,1.),(1.,
1.),(1.,1.),(1.,1.),(1.,1.),(1.,1.),(1.,1.),(1.,1.),(1.,1.),(1.,1.),(1.,
1.),(1.,1.),(1.,1.),(1.,1.),(1.,1.),(1.,1.),(1.,1.),(1.,1.),(1.,1.),(1.,
1.),(1.,1.),(1.,1.),(1.,1.),(1.,1.),(1.,1.),(1.,1.),(1.,1.),(1.,1.),(1.,
1.),(1.,1.),(1.,1.),(1.,1.),(1.,1.),(1.,1.),(1.,1.),(1.,1.),(1.,1.),(1.,
1.),(1.,1.),(1.,1.),(1.,1.),(1.,1.),(1.,1.),(1.,1.),(1.,1.),(1.,1.),(1.,
1.),(1.,1.),(1.,1.),(1.,1.),(1.,1.),(1.,1.),(1.,1.),(1.,1.),(1.,1.),(1.,
1.),(1.,1.),(1.,1.),(1.,1.),(1.,1.),(1.,1.),(1.,1.),(1.,1.),(1.,1.),(1.,
1.),(1.,1.),(1.,1.),(1.,1.),(1.,1.),(1.,1.),(1.,1.),(1.,1.),(1.,1.),(1.,
1.),(1.,1.),(1.,1.),(1.,1.),(1.,1.),(1.,1.),(1.,1.),(1.,1.),(1.,1.),(1.,
1.),(1.,1.),(1.,1.),(1.,1.),(1.,1.),(1.,1.),(1.,1.),(1.,1.),(1.,1.),(1.,
1.),(1.,1.),(1.,1.),(1.,1.),(1.,1.),(1.,1.),(1.,1.),(1.,1.),(1.,1.),(1.,
1.),(1.,1.),(1.,1.),(1.,1.),(1.,1.),(1.,1.),(1.,1.),(1.,1.),(1.,1.),(1.,
1.),(1.,1.),(1.,1.),(1.,1.),(1.,1.),(1.,1.),(1.,1.),(1.,1.),(1.,1.),(1.,
1.),(1.,1.),(1.,1.),(1.,1.),(1.,1.),(1.,1.),(1.,1.),(1.,1.),(1.,1.),(1.,
1.),(1.,1.),(1.,1.),(1.,1.),(1.,1.),(1.,1.),(1.,1.),(1.,1.),(1.,1.),(1.,
1.),(1.,1.),(1.,1.),(1.,1.),(1.,1.),(1.,1.),(1.,1.),(1.,1.),(1.,1.),(1.,
1.),(1.,1.),(1.,1.),(1.,1.),(1.,1.),(1.,1.),(1.,1.),(1.,1.),(1.,1.),(1.,
1.),(1.,1.),(1.,1.),(1.,1.),(1.,1.),(1.,1.),(1.,1.),(1.,1.),(1.,1.),(1.,
1.),(1.,1.),(1.,1.),(1.,1.),(1.,1.),(1.,1.),(1.,1.),(1.,1.),(1.,1.),(1.,
1.),(1.,1.)))
REPRESENTATION_ITEM('')
SURFACE()
);
#1050=(
BOUNDED_SURFACE()
B_SPLINE_SURFACE(5,1,((#199840,#199841),(#199842,#199843),(#199844,#199845),
(#199846,#199847),(#199848,#199849),(#199850,#199851),(#199852,#199853),
(#199854,#199855),(#199856,#199857),(#199858,#199859),(#199860,#199861),
(#199862,#199863),(#199864,#199865),(#199866,#199867),(#199868,#199869),
(#199870,#199871),(#199872,#199873),(#199874,#199875),(#199876,#199877),
(#199878,#199879),(#199880,#199881),(#199882,#199883),(#199884,#199885),
(#199886,#199887),(#199888,#199889),(#199890,#199891),(#199892,#199893),
(#199894,#199895),(#199896,#199897),(#199898,#199899),(#199900,#199901),
(#199902,#199903),(#199904,#199905),(#199906,#199907),(#199908,#199909),
(#199910,#199911),(#199912,#199913),(#199914,#199915),(#199916,#199917),
(#199918,#199919),(#199920,#199921),(#199922,#199923),(#199924,#199925),
(#199926,#199927),(#199928,#199929),(#199930,#199931),(#199932,#199933),
(#199934,#199935),(#199936,#199937),(#199938,#199939),(#199940,#199941),
(#199942,#199943),(#199944,#199945),(#199946,#199947),(#199948,#199949),
(#199950,#199951),(#199952,#199953),(#199954,#199955),(#199956,#199957),
(#199958,#199959),(#199960,#199961),(#199962,#199963),(#199964,#199965),
(#199966,#199967),(#199968,#199969),(#199970,#199971),(#199972,#199973),
(#199974,#199975),(#199976,#199977),(#199978,#199979),(#199980,#199981),
(#199982,#199983),(#199984,#199985),(#199986,#199987),(#199988,#199989),
(#199990,#199991),(#199992,#199993),(#199994,#199995),(#199996,#199997),
(#199998,#199999),(#200000,#200001),(#200002,#200003),(#200004,#200005),
(#200006,#200007),(#200008,#200009),(#200010,#200011),(#200012,#200013),
(#200014,#200015),(#200016,#200017),(#200018,#200019),(#200020,#200021),
(#200022,#200023),(#200024,#200025),(#200026,#200027),(#200028,#200029),
(#200030,#200031),(#200032,#200033),(#200034,#200035),(#200036,#200037),
(#200038,#200039),(#200040,#200041),(#200042,#200043),(#200044,#200045),
(#200046,#200047),(#200048,#200049),(#200050,#200051),(#200052,#200053),
(#200054,#200055),(#200056,#200057),(#200058,#200059),(#200060,#200061),
(#200062,#200063),(#200064,#200065),(#200066,#200067),(#200068,#200069),
(#200070,#200071),(#200072,#200073),(#200074,#200075),(#200076,#200077),
(#200078,#200079),(#200080,#200081),(#200082,#200083),(#200084,#200085),
(#200086,#200087),(#200088,#200089),(#200090,#200091),(#200092,#200093),
(#200094,#200095),(#200096,#200097),(#200098,#200099),(#200100,#200101),
(#200102,#200103),(#200104,#200105),(#200106,#200107),(#200108,#200109),
(#200110,#200111),(#200112,#200113),(#200114,#200115),(#200116,#200117),
(#200118,#200119),(#200120,#200121),(#200122,#200123),(#200124,#200125),
(#200126,#200127),(#200128,#200129),(#200130,#200131),(#200132,#200133),
(#200134,#200135),(#200136,#200137),(#200138,#200139),(#200140,#200141),
(#200142,#200143),(#200144,#200145),(#200146,#200147),(#200148,#200149),
(#200150,#200151),(#200152,#200153),(#200154,#200155),(#200156,#200157),
(#200158,#200159),(#200160,#200161),(#200162,#200163),(#200164,#200165),
(#200166,#200167),(#200168,#200169),(#200170,#200171),(#200172,#200173),
(#200174,#200175),(#200176,#200177),(#200178,#200179),(#200180,#200181),
(#200182,#200183),(#200184,#200185),(#200186,#200187),(#200188,#200189),
(#200190,#200191),(#200192,#200193),(#200194,#200195),(#200196,#200197),
(#200198,#200199),(#200200,#200201),(#200202,#200203),(#200204,#200205),
(#200206,#200207),(#200208,#200209),(#200210,#200211),(#200212,#200213),
(#200214,#200215),(#200216,#200217),(#200218,#200219),(#200220,#200221),
(#200222,#200223),(#200224,#200225),(#200226,#200227),(#200228,#200229),
(#200230,#200231),(#200232,#200233),(#200234,#200235),(#200236,#200237),
(#200238,#200239),(#200240,#200241),(#200242,#200243),(#200244,#200245),
(#200246,#200247),(#200248,#200249)),.UNSPECIFIED.,.F.,.F.,.F.)
B_SPLINE_SURFACE_WITH_KNOTS((6,1,1,1,1,1,1,1,1,1,1,1,1,1,1,1,1,1,1,1,1,
1,1,1,1,1,1,1,1,1,1,1,1,1,1,1,1,1,1,1,1,1,1,1,1,1,1,1,1,1,1,1,1,1,1,1,1,
1,1,1,1,1,1,1,1,1,1,1,1,1,1,1,1,1,1,1,1,1,1,1,1,1,1,1,1,1,1,1,1,1,1,1,1,
1,1,1,1,1,1,1,1,1,1,1,1,1,1,1,1,1,1,1,1,1,1,1,1,1,1,1,1,1,1,1,1,1,1,1,1,
1,1,1,1,1,1,1,1,1,1,1,1,1,1,1,1,1,1,1,1,1,1,1,1,1,1,1,1,1,1,1,1,1,1,1,1,
1,1,1,1,1,1,1,1,1,1,1,1,1,1,1,1,1,1,1,1,1,1,1,1,1,1,1,1,1,1,1,1,1,1,1,6),
(2,2),(0.,0.005,0.01,0.015,0.02,0.025,0.03,0.035,0.04,0.045,0.05,0.055,
0.06,0.065,0.07,0.075,0.08,0.085,0.09,0.095,0.1,0.105,0.11,0.115,0.12,0.125,
0.13,0.135,0.14,0.145,0.15,0.155,0.16,0.165,0.17,0.175,0.18,0.185,0.19,
0.195,0.2,0.205,0.21,0.215,0.22,0.225,0.23,0.235,0.24,0.245,0.25,0.255,
0.26,0.265,0.27,0.275,0.28,0.285,0.29,0.295,0.3,0.305,0.31,0.315,0.32,0.325,
0.33,0.335,0.34,0.345,0.35,0.355,0.36,0.365,0.37,0.375,0.38,0.385,0.39,
0.395,0.4,0.405,0.41,0.415,0.42,0.425,0.43,0.435,0.44,0.445,0.45,0.455,
0.46,0.465,0.47,0.475,0.48,0.485,0.49,0.495,0.5,0.505,0.51,0.515,0.52,0.525,
0.53,0.535,0.54,0.545,0.55,0.555,0.56,0.565,0.57,0.575,0.58,0.585,0.59,
0.595,0.6,0.605,0.61,0.615,0.62,0.625,0.63,0.635,0.64,0.645,0.65,0.655,
0.66,0.665,0.67,0.675,0.68,0.685,0.690000000000001,0.695000000000001,0.700000000000001,
0.705000000000001,0.710000000000001,0.715000000000001,0.720000000000001,
0.725000000000001,0.730000000000001,0.735000000000001,0.740000000000001,
0.745000000000001,0.750000000000001,0.755000000000001,0.760000000000001,
0.765000000000001,0.770000000000001,0.775000000000001,0.780000000000001,
0.785000000000001,0.790000000000001,0.795000000000001,0.800000000000001,
0.805000000000001,0.810000000000001,0.815000000000001,0.820000000000001,
0.825000000000001,0.830000000000001,0.835000000000001,0.840000000000001,
0.845000000000001,0.850000000000001,0.855000000000001,0.860000000000001,
0.865000000000001,0.870000000000001,0.875000000000001,0.880000000000001,
0.885000000000001,0.890000000000001,0.895000000000001,0.900000000000001,
0.905000000000001,0.910000000000001,0.915000000000001,0.920000000000001,
0.925000000000001,0.930000000000001,0.935000000000001,0.940000000000001,
0.945000000000001,0.950000000000001,0.955000000000001,0.960000000000001,
0.965000000000001,0.970000000000001,0.975000000000001,0.980000000000001,
0.985000000000001,0.990000000000001,0.995000000000001,1.),(0.,1.2),
 .UNSPECIFIED.)
GEOMETRIC_REPRESENTATION_ITEM()
RATIONAL_B_SPLINE_SURFACE(((1.,1.),(1.,1.),(1.,1.),(1.,1.),(1.,1.),(1.,
1.),(1.,1.),(1.,1.),(1.,1.),(1.,1.),(1.,1.),(1.,1.),(1.,1.),(1.,1.),(1.,
1.),(1.,1.),(1.,1.),(1.,1.),(1.,1.),(1.,1.),(1.,1.),(1.,1.),(1.,1.),(1.,
1.),(1.,1.),(1.,1.),(1.,1.),(1.,1.),(1.,1.),(1.,1.),(1.,1.),(1.,1.),(1.,
1.),(1.,1.),(1.,1.),(1.,1.),(1.,1.),(1.,1.),(1.,1.),(1.,1.),(1.,1.),(1.,
1.),(1.,1.),(1.,1.),(1.,1.),(1.,1.),(1.,1.),(1.,1.),(1.,1.),(1.,1.),(1.,
1.),(1.,1.),(1.,1.),(1.,1.),(1.,1.),(1.,1.),(1.,1.),(1.,1.),(1.,1.),(1.,
1.),(1.,1.),(1.,1.),(1.,1.),(1.,1.),(1.,1.),(1.,1.),(1.,1.),(1.,1.),(1.,
1.),(1.,1.),(1.,1.),(1.,1.),(1.,1.),(1.,1.),(1.,1.),(1.,1.),(1.,1.),(1.,
1.),(1.,1.),(1.,1.),(1.,1.),(1.,1.),(1.,1.),(1.,1.),(1.,1.),(1.,1.),(1.,
1.),(1.,1.),(1.,1.),(1.,1.),(1.,1.),(1.,1.),(1.,1.),(1.,1.),(1.,1.),(1.,
1.),(1.,1.),(1.,1.),(1.,1.),(1.,1.),(1.,1.),(1.,1.),(1.,1.),(1.,1.),(1.,
1.),(1.,1.),(1.,1.),(1.,1.),(1.,1.),(1.,1.),(1.,1.),(1.,1.),(1.,1.),(1.,
1.),(1.,1.),(1.,1.),(1.,1.),(1.,1.),(1.,1.),(1.,1.),(1.,1.),(1.,1.),(1.,
1.),(1.,1.),(1.,1.),(1.,1.),(1.,1.),(1.,1.),(1.,1.),(1.,1.),(1.,1.),(1.,
1.),(1.,1.),(1.,1.),(1.,1.),(1.,1.),(1.,1.),(1.,1.),(1.,1.),(1.,1.),(1.,
1.),(1.,1.),(1.,1.),(1.,1.),(1.,1.),(1.,1.),(1.,1.),(1.,1.),(1.,1.),(1.,
1.),(1.,1.),(1.,1.),(1.,1.),(1.,1.),(1.,1.),(1.,1.),(1.,1.),(1.,1.),(1.,
1.),(1.,1.),(1.,1.),(1.,1.),(1.,1.),(1.,1.),(1.,1.),(1.,1.),(1.,1.),(1.,
1.),(1.,1.),(1.,1.),(1.,1.),(1.,1.),(1.,1.),(1.,1.),(1.,1.),(1.,1.),(1.,
1.),(1.,1.),(1.,1.),(1.,1.),(1.,1.),(1.,1.),(1.,1.),(1.,1.),(1.,1.),(1.,
1.),(1.,1.),(1.,1.),(1.,1.),(1.,1.),(1.,1.),(1.,1.),(1.,1.),(1.,1.),(1.,
1.),(1.,1.),(1.,1.),(1.,1.),(1.,1.),(1.,1.),(1.,1.),(1.,1.),(1.,1.),(1.,
1.),(1.,1.)))
REPRESENTATION_ITEM('')
SURFACE()
);
#1051=(
BOUNDED_SURFACE()
B_SPLINE_SURFACE(5,1,((#200461,#200462),(#200463,#200464),(#200465,#200466),
(#200467,#200468),(#200469,#200470),(#200471,#200472),(#200473,#200474),
(#200475,#200476),(#200477,#200478),(#200479,#200480),(#200481,#200482),
(#200483,#200484),(#200485,#200486),(#200487,#200488),(#200489,#200490),
(#200491,#200492),(#200493,#200494),(#200495,#200496),(#200497,#200498),
(#200499,#200500),(#200501,#200502),(#200503,#200504),(#200505,#200506),
(#200507,#200508),(#200509,#200510),(#200511,#200512),(#200513,#200514),
(#200515,#200516),(#200517,#200518),(#200519,#200520),(#200521,#200522),
(#200523,#200524),(#200525,#200526),(#200527,#200528),(#200529,#200530),
(#200531,#200532),(#200533,#200534),(#200535,#200536),(#200537,#200538),
(#200539,#200540),(#200541,#200542),(#200543,#200544),(#200545,#200546),
(#200547,#200548),(#200549,#200550),(#200551,#200552),(#200553,#200554),
(#200555,#200556),(#200557,#200558),(#200559,#200560),(#200561,#200562),
(#200563,#200564),(#200565,#200566),(#200567,#200568),(#200569,#200570),
(#200571,#200572),(#200573,#200574),(#200575,#200576),(#200577,#200578),
(#200579,#200580),(#200581,#200582),(#200583,#200584),(#200585,#200586),
(#200587,#200588),(#200589,#200590),(#200591,#200592),(#200593,#200594),
(#200595,#200596),(#200597,#200598),(#200599,#200600),(#200601,#200602),
(#200603,#200604),(#200605,#200606),(#200607,#200608),(#200609,#200610),
(#200611,#200612),(#200613,#200614),(#200615,#200616),(#200617,#200618),
(#200619,#200620),(#200621,#200622),(#200623,#200624),(#200625,#200626),
(#200627,#200628),(#200629,#200630),(#200631,#200632),(#200633,#200634),
(#200635,#200636),(#200637,#200638),(#200639,#200640),(#200641,#200642),
(#200643,#200644),(#200645,#200646),(#200647,#200648),(#200649,#200650),
(#200651,#200652),(#200653,#200654),(#200655,#200656),(#200657,#200658),
(#200659,#200660),(#200661,#200662),(#200663,#200664),(#200665,#200666),
(#200667,#200668),(#200669,#200670),(#200671,#200672),(#200673,#200674),
(#200675,#200676),(#200677,#200678),(#200679,#200680),(#200681,#200682),
(#200683,#200684),(#200685,#200686),(#200687,#200688),(#200689,#200690),
(#200691,#200692),(#200693,#200694),(#200695,#200696),(#200697,#200698),
(#200699,#200700),(#200701,#200702),(#200703,#200704),(#200705,#200706),
(#200707,#200708),(#200709,#200710),(#200711,#200712),(#200713,#200714),
(#200715,#200716),(#200717,#200718),(#200719,#200720),(#200721,#200722),
(#200723,#200724),(#200725,#200726),(#200727,#200728),(#200729,#200730),
(#200731,#200732),(#200733,#200734),(#200735,#200736),(#200737,#200738),
(#200739,#200740),(#200741,#200742),(#200743,#200744),(#200745,#200746),
(#200747,#200748),(#200749,#200750),(#200751,#200752),(#200753,#200754),
(#200755,#200756),(#200757,#200758),(#200759,#200760),(#200761,#200762),
(#200763,#200764),(#200765,#200766),(#200767,#200768),(#200769,#200770),
(#200771,#200772),(#200773,#200774),(#200775,#200776),(#200777,#200778),
(#200779,#200780),(#200781,#200782),(#200783,#200784),(#200785,#200786),
(#200787,#200788),(#200789,#200790),(#200791,#200792),(#200793,#200794),
(#200795,#200796),(#200797,#200798),(#200799,#200800),(#200801,#200802),
(#200803,#200804),(#200805,#200806),(#200807,#200808),(#200809,#200810),
(#200811,#200812),(#200813,#200814),(#200815,#200816),(#200817,#200818),
(#200819,#200820),(#200821,#200822),(#200823,#200824),(#200825,#200826),
(#200827,#200828),(#200829,#200830),(#200831,#200832),(#200833,#200834),
(#200835,#200836),(#200837,#200838),(#200839,#200840),(#200841,#200842),
(#200843,#200844),(#200845,#200846),(#200847,#200848),(#200849,#200850),
(#200851,#200852),(#200853,#200854),(#200855,#200856),(#200857,#200858),
(#200859,#200860),(#200861,#200862),(#200863,#200864),(#200865,#200866),
(#200867,#200868),(#200869,#200870)),.UNSPECIFIED.,.F.,.F.,.F.)
B_SPLINE_SURFACE_WITH_KNOTS((6,1,1,1,1,1,1,1,1,1,1,1,1,1,1,1,1,1,1,1,1,
1,1,1,1,1,1,1,1,1,1,1,1,1,1,1,1,1,1,1,1,1,1,1,1,1,1,1,1,1,1,1,1,1,1,1,1,
1,1,1,1,1,1,1,1,1,1,1,1,1,1,1,1,1,1,1,1,1,1,1,1,1,1,1,1,1,1,1,1,1,1,1,1,
1,1,1,1,1,1,1,1,1,1,1,1,1,1,1,1,1,1,1,1,1,1,1,1,1,1,1,1,1,1,1,1,1,1,1,1,
1,1,1,1,1,1,1,1,1,1,1,1,1,1,1,1,1,1,1,1,1,1,1,1,1,1,1,1,1,1,1,1,1,1,1,1,
1,1,1,1,1,1,1,1,1,1,1,1,1,1,1,1,1,1,1,1,1,1,1,1,1,1,1,1,1,1,1,1,1,1,1,6),
(2,2),(-1.,-0.995000000000001,-0.990000000000001,-0.985000000000001,-0.980000000000001,
-0.975000000000001,-0.970000000000001,-0.965000000000001,-0.960000000000001,
-0.955000000000001,-0.950000000000001,-0.945000000000001,-0.940000000000001,
-0.935000000000001,-0.930000000000001,-0.925000000000001,-0.920000000000001,
-0.915000000000001,-0.910000000000001,-0.905000000000001,-0.900000000000001,
-0.895000000000001,-0.890000000000001,-0.885000000000001,-0.880000000000001,
-0.875000000000001,-0.870000000000001,-0.865000000000001,-0.860000000000001,
-0.855000000000001,-0.850000000000001,-0.845000000000001,-0.840000000000001,
-0.835000000000001,-0.830000000000001,-0.825000000000001,-0.820000000000001,
-0.815000000000001,-0.810000000000001,-0.805000000000001,-0.800000000000001,
-0.795000000000001,-0.790000000000001,-0.785000000000001,-0.780000000000001,
-0.775000000000001,-0.770000000000001,-0.765000000000001,-0.760000000000001,
-0.755000000000001,-0.750000000000001,-0.745000000000001,-0.740000000000001,
-0.735000000000001,-0.730000000000001,-0.725000000000001,-0.720000000000001,
-0.715000000000001,-0.710000000000001,-0.705000000000001,-0.700000000000001,
-0.695000000000001,-0.690000000000001,-0.685,-0.68,-0.675,-0.67,-0.665,
-0.66,-0.655,-0.65,-0.645,-0.64,-0.635,-0.63,-0.625,-0.62,-0.615,-0.61,
-0.605,-0.6,-0.595,-0.59,-0.585,-0.58,-0.575,-0.57,-0.565,-0.56,-0.555,
-0.55,-0.545,-0.54,-0.535,-0.53,-0.525,-0.52,-0.515,-0.51,-0.505,-0.5,-0.495,
-0.49,-0.485,-0.48,-0.475,-0.47,-0.465,-0.46,-0.455,-0.45,-0.445,-0.44,
-0.435,-0.43,-0.425,-0.42,-0.415,-0.41,-0.405,-0.4,-0.395,-0.39,-0.385,
-0.38,-0.375,-0.37,-0.365,-0.36,-0.355,-0.35,-0.345,-0.34,-0.335,-0.33,
-0.325,-0.32,-0.315,-0.31,-0.305,-0.3,-0.295,-0.29,-0.285,-0.28,-0.275,
-0.27,-0.265,-0.26,-0.255,-0.25,-0.245,-0.24,-0.235,-0.23,-0.225,-0.22,
-0.215,-0.21,-0.205,-0.2,-0.195,-0.19,-0.185,-0.18,-0.175,-0.17,-0.165,
-0.16,-0.155,-0.15,-0.145,-0.14,-0.135,-0.13,-0.125,-0.12,-0.115,-0.11,
-0.105,-0.1,-0.095,-0.09,-0.085,-0.08,-0.075,-0.07,-0.065,-0.06,-0.055,
-0.05,-0.045,-0.04,-0.035,-0.03,-0.025,-0.02,-0.015,-0.01,-0.005,0.),(0.,
1.2),.UNSPECIFIED.)
GEOMETRIC_REPRESENTATION_ITEM()
RATIONAL_B_SPLINE_SURFACE(((1.,1.),(1.,1.),(1.,1.),(1.,1.),(1.,1.),(1.,
1.),(1.,1.),(1.,1.),(1.,1.),(1.,1.),(1.,1.),(1.,1.),(1.,1.),(1.,1.),(1.,
1.),(1.,1.),(1.,1.),(1.,1.),(1.,1.),(1.,1.),(1.,1.),(1.,1.),(1.,1.),(1.,
1.),(1.,1.),(1.,1.),(1.,1.),(1.,1.),(1.,1.),(1.,1.),(1.,1.),(1.,1.),(1.,
1.),(1.,1.),(1.,1.),(1.,1.),(1.,1.),(1.,1.),(1.,1.),(1.,1.),(1.,1.),(1.,
1.),(1.,1.),(1.,1.),(1.,1.),(1.,1.),(1.,1.),(1.,1.),(1.,1.),(1.,1.),(1.,
1.),(1.,1.),(1.,1.),(1.,1.),(1.,1.),(1.,1.),(1.,1.),(1.,1.),(1.,1.),(1.,
1.),(1.,1.),(1.,1.),(1.,1.),(1.,1.),(1.,1.),(1.,1.),(1.,1.),(1.,1.),(1.,
1.),(1.,1.),(1.,1.),(1.,1.),(1.,1.),(1.,1.),(1.,1.),(1.,1.),(1.,1.),(1.,
1.),(1.,1.),(1.,1.),(1.,1.),(1.,1.),(1.,1.),(1.,1.),(1.,1.),(1.,1.),(1.,
1.),(1.,1.),(1.,1.),(1.,1.),(1.,1.),(1.,1.),(1.,1.),(1.,1.),(1.,1.),(1.,
1.),(1.,1.),(1.,1.),(1.,1.),(1.,1.),(1.,1.),(1.,1.),(1.,1.),(1.,1.),(1.,
1.),(1.,1.),(1.,1.),(1.,1.),(1.,1.),(1.,1.),(1.,1.),(1.,1.),(1.,1.),(1.,
1.),(1.,1.),(1.,1.),(1.,1.),(1.,1.),(1.,1.),(1.,1.),(1.,1.),(1.,1.),(1.,
1.),(1.,1.),(1.,1.),(1.,1.),(1.,1.),(1.,1.),(1.,1.),(1.,1.),(1.,1.),(1.,
1.),(1.,1.),(1.,1.),(1.,1.),(1.,1.),(1.,1.),(1.,1.),(1.,1.),(1.,1.),(1.,
1.),(1.,1.),(1.,1.),(1.,1.),(1.,1.),(1.,1.),(1.,1.),(1.,1.),(1.,1.),(1.,
1.),(1.,1.),(1.,1.),(1.,1.),(1.,1.),(1.,1.),(1.,1.),(1.,1.),(1.,1.),(1.,
1.),(1.,1.),(1.,1.),(1.,1.),(1.,1.),(1.,1.),(1.,1.),(1.,1.),(1.,1.),(1.,
1.),(1.,1.),(1.,1.),(1.,1.),(1.,1.),(1.,1.),(1.,1.),(1.,1.),(1.,1.),(1.,
1.),(1.,1.),(1.,1.),(1.,1.),(1.,1.),(1.,1.),(1.,1.),(1.,1.),(1.,1.),(1.,
1.),(1.,1.),(1.,1.),(1.,1.),(1.,1.),(1.,1.),(1.,1.),(1.,1.),(1.,1.),(1.,
1.),(1.,1.),(1.,1.),(1.,1.),(1.,1.),(1.,1.),(1.,1.),(1.,1.),(1.,1.),(1.,
1.),(1.,1.)))
REPRESENTATION_ITEM('')
SURFACE()
);
#1052=(
BOUNDED_SURFACE()
B_SPLINE_SURFACE(5,1,((#201078,#201079),(#201080,#201081),(#201082,#201083),
(#201084,#201085),(#201086,#201087),(#201088,#201089),(#201090,#201091),
(#201092,#201093),(#201094,#201095),(#201096,#201097),(#201098,#201099),
(#201100,#201101),(#201102,#201103),(#201104,#201105),(#201106,#201107),
(#201108,#201109),(#201110,#201111),(#201112,#201113),(#201114,#201115),
(#201116,#201117),(#201118,#201119),(#201120,#201121),(#201122,#201123),
(#201124,#201125),(#201126,#201127),(#201128,#201129),(#201130,#201131),
(#201132,#201133),(#201134,#201135),(#201136,#201137),(#201138,#201139),
(#201140,#201141),(#201142,#201143),(#201144,#201145),(#201146,#201147),
(#201148,#201149),(#201150,#201151),(#201152,#201153),(#201154,#201155),
(#201156,#201157),(#201158,#201159),(#201160,#201161),(#201162,#201163),
(#201164,#201165),(#201166,#201167),(#201168,#201169),(#201170,#201171),
(#201172,#201173),(#201174,#201175),(#201176,#201177),(#201178,#201179),
(#201180,#201181),(#201182,#201183),(#201184,#201185),(#201186,#201187),
(#201188,#201189),(#201190,#201191),(#201192,#201193),(#201194,#201195),
(#201196,#201197),(#201198,#201199),(#201200,#201201),(#201202,#201203),
(#201204,#201205),(#201206,#201207),(#201208,#201209),(#201210,#201211),
(#201212,#201213),(#201214,#201215),(#201216,#201217),(#201218,#201219),
(#201220,#201221),(#201222,#201223),(#201224,#201225),(#201226,#201227),
(#201228,#201229),(#201230,#201231),(#201232,#201233),(#201234,#201235),
(#201236,#201237),(#201238,#201239),(#201240,#201241),(#201242,#201243),
(#201244,#201245),(#201246,#201247),(#201248,#201249),(#201250,#201251),
(#201252,#201253),(#201254,#201255),(#201256,#201257),(#201258,#201259),
(#201260,#201261),(#201262,#201263),(#201264,#201265),(#201266,#201267),
(#201268,#201269),(#201270,#201271),(#201272,#201273),(#201274,#201275),
(#201276,#201277),(#201278,#201279),(#201280,#201281),(#201282,#201283),
(#201284,#201285),(#201286,#201287),(#201288,#201289),(#201290,#201291),
(#201292,#201293),(#201294,#201295),(#201296,#201297),(#201298,#201299),
(#201300,#201301),(#201302,#201303),(#201304,#201305),(#201306,#201307),
(#201308,#201309),(#201310,#201311),(#201312,#201313),(#201314,#201315),
(#201316,#201317),(#201318,#201319),(#201320,#201321),(#201322,#201323),
(#201324,#201325),(#201326,#201327),(#201328,#201329),(#201330,#201331),
(#201332,#201333),(#201334,#201335),(#201336,#201337),(#201338,#201339),
(#201340,#201341),(#201342,#201343),(#201344,#201345),(#201346,#201347),
(#201348,#201349),(#201350,#201351),(#201352,#201353),(#201354,#201355),
(#201356,#201357),(#201358,#201359),(#201360,#201361),(#201362,#201363),
(#201364,#201365),(#201366,#201367),(#201368,#201369),(#201370,#201371),
(#201372,#201373),(#201374,#201375),(#201376,#201377),(#201378,#201379),
(#201380,#201381),(#201382,#201383),(#201384,#201385),(#201386,#201387),
(#201388,#201389),(#201390,#201391),(#201392,#201393),(#201394,#201395),
(#201396,#201397),(#201398,#201399),(#201400,#201401),(#201402,#201403),
(#201404,#201405),(#201406,#201407),(#201408,#201409),(#201410,#201411),
(#201412,#201413),(#201414,#201415),(#201416,#201417),(#201418,#201419),
(#201420,#201421),(#201422,#201423),(#201424,#201425),(#201426,#201427),
(#201428,#201429),(#201430,#201431),(#201432,#201433),(#201434,#201435),
(#201436,#201437),(#201438,#201439),(#201440,#201441),(#201442,#201443),
(#201444,#201445),(#201446,#201447),(#201448,#201449),(#201450,#201451),
(#201452,#201453),(#201454,#201455),(#201456,#201457),(#201458,#201459),
(#201460,#201461),(#201462,#201463),(#201464,#201465),(#201466,#201467),
(#201468,#201469),(#201470,#201471),(#201472,#201473),(#201474,#201475),
(#201476,#201477),(#201478,#201479),(#201480,#201481),(#201482,#201483),
(#201484,#201485),(#201486,#201487)),.UNSPECIFIED.,.F.,.F.,.F.)
B_SPLINE_SURFACE_WITH_KNOTS((6,1,1,1,1,1,1,1,1,1,1,1,1,1,1,1,1,1,1,1,1,
1,1,1,1,1,1,1,1,1,1,1,1,1,1,1,1,1,1,1,1,1,1,1,1,1,1,1,1,1,1,1,1,1,1,1,1,
1,1,1,1,1,1,1,1,1,1,1,1,1,1,1,1,1,1,1,1,1,1,1,1,1,1,1,1,1,1,1,1,1,1,1,1,
1,1,1,1,1,1,1,1,1,1,1,1,1,1,1,1,1,1,1,1,1,1,1,1,1,1,1,1,1,1,1,1,1,1,1,1,
1,1,1,1,1,1,1,1,1,1,1,1,1,1,1,1,1,1,1,1,1,1,1,1,1,1,1,1,1,1,1,1,1,1,1,1,
1,1,1,1,1,1,1,1,1,1,1,1,1,1,1,1,1,1,1,1,1,1,1,1,1,1,1,1,1,1,1,1,1,1,1,6),
(2,2),(0.,0.005,0.01,0.015,0.02,0.025,0.03,0.035,0.04,0.045,0.05,0.055,
0.06,0.065,0.07,0.075,0.08,0.085,0.09,0.095,0.1,0.105,0.11,0.115,0.12,0.125,
0.13,0.135,0.14,0.145,0.15,0.155,0.16,0.165,0.17,0.175,0.18,0.185,0.19,
0.195,0.2,0.205,0.21,0.215,0.22,0.225,0.23,0.235,0.24,0.245,0.25,0.255,
0.26,0.265,0.27,0.275,0.28,0.285,0.29,0.295,0.3,0.305,0.31,0.315,0.32,0.325,
0.33,0.335,0.34,0.345,0.35,0.355,0.36,0.365,0.37,0.375,0.38,0.385,0.39,
0.395,0.4,0.405,0.41,0.415,0.42,0.425,0.43,0.435,0.44,0.445,0.45,0.455,
0.46,0.465,0.47,0.475,0.48,0.485,0.49,0.495,0.5,0.505,0.51,0.515,0.52,0.525,
0.53,0.535,0.54,0.545,0.55,0.555,0.56,0.565,0.57,0.575,0.58,0.585,0.59,
0.595,0.6,0.605,0.61,0.615,0.62,0.625,0.63,0.635,0.64,0.645,0.65,0.655,
0.66,0.665,0.67,0.675,0.68,0.685,0.690000000000001,0.695000000000001,0.700000000000001,
0.705000000000001,0.710000000000001,0.715000000000001,0.720000000000001,
0.725000000000001,0.730000000000001,0.735000000000001,0.740000000000001,
0.745000000000001,0.750000000000001,0.755000000000001,0.760000000000001,
0.765000000000001,0.770000000000001,0.775000000000001,0.780000000000001,
0.785000000000001,0.790000000000001,0.795000000000001,0.800000000000001,
0.805000000000001,0.810000000000001,0.815000000000001,0.820000000000001,
0.825000000000001,0.830000000000001,0.835000000000001,0.840000000000001,
0.845000000000001,0.850000000000001,0.855000000000001,0.860000000000001,
0.865000000000001,0.870000000000001,0.875000000000001,0.880000000000001,
0.885000000000001,0.890000000000001,0.895000000000001,0.900000000000001,
0.905000000000001,0.910000000000001,0.915000000000001,0.920000000000001,
0.925000000000001,0.930000000000001,0.935000000000001,0.940000000000001,
0.945000000000001,0.950000000000001,0.955000000000001,0.960000000000001,
0.965000000000001,0.970000000000001,0.975000000000001,0.980000000000001,
0.985000000000001,0.990000000000001,0.995000000000001,1.),(0.,1.2),
 .UNSPECIFIED.)
GEOMETRIC_REPRESENTATION_ITEM()
RATIONAL_B_SPLINE_SURFACE(((1.,1.),(1.,1.),(1.,1.),(1.,1.),(1.,1.),(1.,
1.),(1.,1.),(1.,1.),(1.,1.),(1.,1.),(1.,1.),(1.,1.),(1.,1.),(1.,1.),(1.,
1.),(1.,1.),(1.,1.),(1.,1.),(1.,1.),(1.,1.),(1.,1.),(1.,1.),(1.,1.),(1.,
1.),(1.,1.),(1.,1.),(1.,1.),(1.,1.),(1.,1.),(1.,1.),(1.,1.),(1.,1.),(1.,
1.),(1.,1.),(1.,1.),(1.,1.),(1.,1.),(1.,1.),(1.,1.),(1.,1.),(1.,1.),(1.,
1.),(1.,1.),(1.,1.),(1.,1.),(1.,1.),(1.,1.),(1.,1.),(1.,1.),(1.,1.),(1.,
1.),(1.,1.),(1.,1.),(1.,1.),(1.,1.),(1.,1.),(1.,1.),(1.,1.),(1.,1.),(1.,
1.),(1.,1.),(1.,1.),(1.,1.),(1.,1.),(1.,1.),(1.,1.),(1.,1.),(1.,1.),(1.,
1.),(1.,1.),(1.,1.),(1.,1.),(1.,1.),(1.,1.),(1.,1.),(1.,1.),(1.,1.),(1.,
1.),(1.,1.),(1.,1.),(1.,1.),(1.,1.),(1.,1.),(1.,1.),(1.,1.),(1.,1.),(1.,
1.),(1.,1.),(1.,1.),(1.,1.),(1.,1.),(1.,1.),(1.,1.),(1.,1.),(1.,1.),(1.,
1.),(1.,1.),(1.,1.),(1.,1.),(1.,1.),(1.,1.),(1.,1.),(1.,1.),(1.,1.),(1.,
1.),(1.,1.),(1.,1.),(1.,1.),(1.,1.),(1.,1.),(1.,1.),(1.,1.),(1.,1.),(1.,
1.),(1.,1.),(1.,1.),(1.,1.),(1.,1.),(1.,1.),(1.,1.),(1.,1.),(1.,1.),(1.,
1.),(1.,1.),(1.,1.),(1.,1.),(1.,1.),(1.,1.),(1.,1.),(1.,1.),(1.,1.),(1.,
1.),(1.,1.),(1.,1.),(1.,1.),(1.,1.),(1.,1.),(1.,1.),(1.,1.),(1.,1.),(1.,
1.),(1.,1.),(1.,1.),(1.,1.),(1.,1.),(1.,1.),(1.,1.),(1.,1.),(1.,1.),(1.,
1.),(1.,1.),(1.,1.),(1.,1.),(1.,1.),(1.,1.),(1.,1.),(1.,1.),(1.,1.),(1.,
1.),(1.,1.),(1.,1.),(1.,1.),(1.,1.),(1.,1.),(1.,1.),(1.,1.),(1.,1.),(1.,
1.),(1.,1.),(1.,1.),(1.,1.),(1.,1.),(1.,1.),(1.,1.),(1.,1.),(1.,1.),(1.,
1.),(1.,1.),(1.,1.),(1.,1.),(1.,1.),(1.,1.),(1.,1.),(1.,1.),(1.,1.),(1.,
1.),(1.,1.),(1.,1.),(1.,1.),(1.,1.),(1.,1.),(1.,1.),(1.,1.),(1.,1.),(1.,
1.),(1.,1.),(1.,1.),(1.,1.),(1.,1.),(1.,1.),(1.,1.),(1.,1.),(1.,1.),(1.,
1.),(1.,1.)))
REPRESENTATION_ITEM('')
SURFACE()
);
#1053=(
BOUNDED_SURFACE()
B_SPLINE_SURFACE(5,1,((#201699,#201700),(#201701,#201702),(#201703,#201704),
(#201705,#201706),(#201707,#201708),(#201709,#201710),(#201711,#201712),
(#201713,#201714),(#201715,#201716),(#201717,#201718),(#201719,#201720),
(#201721,#201722),(#201723,#201724),(#201725,#201726),(#201727,#201728),
(#201729,#201730),(#201731,#201732),(#201733,#201734),(#201735,#201736),
(#201737,#201738),(#201739,#201740),(#201741,#201742),(#201743,#201744),
(#201745,#201746),(#201747,#201748),(#201749,#201750),(#201751,#201752),
(#201753,#201754),(#201755,#201756),(#201757,#201758),(#201759,#201760),
(#201761,#201762),(#201763,#201764),(#201765,#201766),(#201767,#201768),
(#201769,#201770),(#201771,#201772),(#201773,#201774),(#201775,#201776),
(#201777,#201778),(#201779,#201780),(#201781,#201782),(#201783,#201784),
(#201785,#201786),(#201787,#201788),(#201789,#201790),(#201791,#201792),
(#201793,#201794),(#201795,#201796),(#201797,#201798),(#201799,#201800),
(#201801,#201802),(#201803,#201804),(#201805,#201806),(#201807,#201808),
(#201809,#201810),(#201811,#201812),(#201813,#201814),(#201815,#201816),
(#201817,#201818),(#201819,#201820),(#201821,#201822),(#201823,#201824),
(#201825,#201826),(#201827,#201828),(#201829,#201830),(#201831,#201832),
(#201833,#201834),(#201835,#201836),(#201837,#201838),(#201839,#201840),
(#201841,#201842),(#201843,#201844),(#201845,#201846),(#201847,#201848),
(#201849,#201850),(#201851,#201852),(#201853,#201854),(#201855,#201856),
(#201857,#201858),(#201859,#201860),(#201861,#201862),(#201863,#201864),
(#201865,#201866),(#201867,#201868),(#201869,#201870),(#201871,#201872),
(#201873,#201874),(#201875,#201876),(#201877,#201878),(#201879,#201880),
(#201881,#201882),(#201883,#201884),(#201885,#201886),(#201887,#201888),
(#201889,#201890),(#201891,#201892),(#201893,#201894),(#201895,#201896),
(#201897,#201898),(#201899,#201900),(#201901,#201902),(#201903,#201904),
(#201905,#201906),(#201907,#201908),(#201909,#201910),(#201911,#201912),
(#201913,#201914),(#201915,#201916),(#201917,#201918),(#201919,#201920),
(#201921,#201922),(#201923,#201924),(#201925,#201926),(#201927,#201928),
(#201929,#201930),(#201931,#201932),(#201933,#201934),(#201935,#201936),
(#201937,#201938),(#201939,#201940),(#201941,#201942),(#201943,#201944),
(#201945,#201946),(#201947,#201948),(#201949,#201950),(#201951,#201952),
(#201953,#201954),(#201955,#201956),(#201957,#201958),(#201959,#201960),
(#201961,#201962),(#201963,#201964),(#201965,#201966),(#201967,#201968),
(#201969,#201970),(#201971,#201972),(#201973,#201974),(#201975,#201976),
(#201977,#201978),(#201979,#201980),(#201981,#201982),(#201983,#201984),
(#201985,#201986),(#201987,#201988),(#201989,#201990),(#201991,#201992),
(#201993,#201994),(#201995,#201996),(#201997,#201998),(#201999,#202000),
(#202001,#202002),(#202003,#202004),(#202005,#202006),(#202007,#202008),
(#202009,#202010),(#202011,#202012),(#202013,#202014),(#202015,#202016),
(#202017,#202018),(#202019,#202020),(#202021,#202022),(#202023,#202024),
(#202025,#202026),(#202027,#202028),(#202029,#202030),(#202031,#202032),
(#202033,#202034),(#202035,#202036),(#202037,#202038),(#202039,#202040),
(#202041,#202042),(#202043,#202044),(#202045,#202046),(#202047,#202048),
(#202049,#202050),(#202051,#202052),(#202053,#202054),(#202055,#202056),
(#202057,#202058),(#202059,#202060),(#202061,#202062),(#202063,#202064),
(#202065,#202066),(#202067,#202068),(#202069,#202070),(#202071,#202072),
(#202073,#202074),(#202075,#202076),(#202077,#202078),(#202079,#202080),
(#202081,#202082),(#202083,#202084),(#202085,#202086),(#202087,#202088),
(#202089,#202090),(#202091,#202092),(#202093,#202094),(#202095,#202096),
(#202097,#202098),(#202099,#202100),(#202101,#202102),(#202103,#202104),
(#202105,#202106),(#202107,#202108)),.UNSPECIFIED.,.F.,.F.,.F.)
B_SPLINE_SURFACE_WITH_KNOTS((6,1,1,1,1,1,1,1,1,1,1,1,1,1,1,1,1,1,1,1,1,
1,1,1,1,1,1,1,1,1,1,1,1,1,1,1,1,1,1,1,1,1,1,1,1,1,1,1,1,1,1,1,1,1,1,1,1,
1,1,1,1,1,1,1,1,1,1,1,1,1,1,1,1,1,1,1,1,1,1,1,1,1,1,1,1,1,1,1,1,1,1,1,1,
1,1,1,1,1,1,1,1,1,1,1,1,1,1,1,1,1,1,1,1,1,1,1,1,1,1,1,1,1,1,1,1,1,1,1,1,
1,1,1,1,1,1,1,1,1,1,1,1,1,1,1,1,1,1,1,1,1,1,1,1,1,1,1,1,1,1,1,1,1,1,1,1,
1,1,1,1,1,1,1,1,1,1,1,1,1,1,1,1,1,1,1,1,1,1,1,1,1,1,1,1,1,1,1,1,1,1,1,6),
(2,2),(-1.,-0.995000000000001,-0.990000000000001,-0.985000000000001,-0.980000000000001,
-0.975000000000001,-0.970000000000001,-0.965000000000001,-0.960000000000001,
-0.955000000000001,-0.950000000000001,-0.945000000000001,-0.940000000000001,
-0.935000000000001,-0.930000000000001,-0.925000000000001,-0.920000000000001,
-0.915000000000001,-0.910000000000001,-0.905000000000001,-0.900000000000001,
-0.895000000000001,-0.890000000000001,-0.885000000000001,-0.880000000000001,
-0.875000000000001,-0.870000000000001,-0.865000000000001,-0.860000000000001,
-0.855000000000001,-0.850000000000001,-0.845000000000001,-0.840000000000001,
-0.835000000000001,-0.830000000000001,-0.825000000000001,-0.820000000000001,
-0.815000000000001,-0.810000000000001,-0.805000000000001,-0.800000000000001,
-0.795000000000001,-0.790000000000001,-0.785000000000001,-0.780000000000001,
-0.775000000000001,-0.770000000000001,-0.765000000000001,-0.760000000000001,
-0.755000000000001,-0.750000000000001,-0.745000000000001,-0.740000000000001,
-0.735000000000001,-0.730000000000001,-0.725000000000001,-0.720000000000001,
-0.715000000000001,-0.710000000000001,-0.705000000000001,-0.700000000000001,
-0.695000000000001,-0.690000000000001,-0.685,-0.68,-0.675,-0.67,-0.665,
-0.66,-0.655,-0.65,-0.645,-0.64,-0.635,-0.63,-0.625,-0.62,-0.615,-0.61,
-0.605,-0.6,-0.595,-0.59,-0.585,-0.58,-0.575,-0.57,-0.565,-0.56,-0.555,
-0.55,-0.545,-0.54,-0.535,-0.53,-0.525,-0.52,-0.515,-0.51,-0.505,-0.5,-0.495,
-0.49,-0.485,-0.48,-0.475,-0.47,-0.465,-0.46,-0.455,-0.45,-0.445,-0.44,
-0.435,-0.43,-0.425,-0.42,-0.415,-0.41,-0.405,-0.4,-0.395,-0.39,-0.385,
-0.38,-0.375,-0.37,-0.365,-0.36,-0.355,-0.35,-0.345,-0.34,-0.335,-0.33,
-0.325,-0.32,-0.315,-0.31,-0.305,-0.3,-0.295,-0.29,-0.285,-0.28,-0.275,
-0.27,-0.265,-0.26,-0.255,-0.25,-0.245,-0.24,-0.235,-0.23,-0.225,-0.22,
-0.215,-0.21,-0.205,-0.2,-0.195,-0.19,-0.185,-0.18,-0.175,-0.17,-0.165,
-0.16,-0.155,-0.15,-0.145,-0.14,-0.135,-0.13,-0.125,-0.12,-0.115,-0.11,
-0.105,-0.1,-0.095,-0.09,-0.085,-0.08,-0.075,-0.07,-0.065,-0.06,-0.055,
-0.05,-0.045,-0.04,-0.035,-0.03,-0.025,-0.02,-0.015,-0.01,-0.005,0.),(0.,
1.2),.UNSPECIFIED.)
GEOMETRIC_REPRESENTATION_ITEM()
RATIONAL_B_SPLINE_SURFACE(((1.,1.),(1.,1.),(1.,1.),(1.,1.),(1.,1.),(1.,
1.),(1.,1.),(1.,1.),(1.,1.),(1.,1.),(1.,1.),(1.,1.),(1.,1.),(1.,1.),(1.,
1.),(1.,1.),(1.,1.),(1.,1.),(1.,1.),(1.,1.),(1.,1.),(1.,1.),(1.,1.),(1.,
1.),(1.,1.),(1.,1.),(1.,1.),(1.,1.),(1.,1.),(1.,1.),(1.,1.),(1.,1.),(1.,
1.),(1.,1.),(1.,1.),(1.,1.),(1.,1.),(1.,1.),(1.,1.),(1.,1.),(1.,1.),(1.,
1.),(1.,1.),(1.,1.),(1.,1.),(1.,1.),(1.,1.),(1.,1.),(1.,1.),(1.,1.),(1.,
1.),(1.,1.),(1.,1.),(1.,1.),(1.,1.),(1.,1.),(1.,1.),(1.,1.),(1.,1.),(1.,
1.),(1.,1.),(1.,1.),(1.,1.),(1.,1.),(1.,1.),(1.,1.),(1.,1.),(1.,1.),(1.,
1.),(1.,1.),(1.,1.),(1.,1.),(1.,1.),(1.,1.),(1.,1.),(1.,1.),(1.,1.),(1.,
1.),(1.,1.),(1.,1.),(1.,1.),(1.,1.),(1.,1.),(1.,1.),(1.,1.),(1.,1.),(1.,
1.),(1.,1.),(1.,1.),(1.,1.),(1.,1.),(1.,1.),(1.,1.),(1.,1.),(1.,1.),(1.,
1.),(1.,1.),(1.,1.),(1.,1.),(1.,1.),(1.,1.),(1.,1.),(1.,1.),(1.,1.),(1.,
1.),(1.,1.),(1.,1.),(1.,1.),(1.,1.),(1.,1.),(1.,1.),(1.,1.),(1.,1.),(1.,
1.),(1.,1.),(1.,1.),(1.,1.),(1.,1.),(1.,1.),(1.,1.),(1.,1.),(1.,1.),(1.,
1.),(1.,1.),(1.,1.),(1.,1.),(1.,1.),(1.,1.),(1.,1.),(1.,1.),(1.,1.),(1.,
1.),(1.,1.),(1.,1.),(1.,1.),(1.,1.),(1.,1.),(1.,1.),(1.,1.),(1.,1.),(1.,
1.),(1.,1.),(1.,1.),(1.,1.),(1.,1.),(1.,1.),(1.,1.),(1.,1.),(1.,1.),(1.,
1.),(1.,1.),(1.,1.),(1.,1.),(1.,1.),(1.,1.),(1.,1.),(1.,1.),(1.,1.),(1.,
1.),(1.,1.),(1.,1.),(1.,1.),(1.,1.),(1.,1.),(1.,1.),(1.,1.),(1.,1.),(1.,
1.),(1.,1.),(1.,1.),(1.,1.),(1.,1.),(1.,1.),(1.,1.),(1.,1.),(1.,1.),(1.,
1.),(1.,1.),(1.,1.),(1.,1.),(1.,1.),(1.,1.),(1.,1.),(1.,1.),(1.,1.),(1.,
1.),(1.,1.),(1.,1.),(1.,1.),(1.,1.),(1.,1.),(1.,1.),(1.,1.),(1.,1.),(1.,
1.),(1.,1.),(1.,1.),(1.,1.),(1.,1.),(1.,1.),(1.,1.),(1.,1.),(1.,1.),(1.,
1.),(1.,1.)))
REPRESENTATION_ITEM('')
SURFACE()
);
#1054=(
BOUNDED_SURFACE()
B_SPLINE_SURFACE(5,1,((#202316,#202317),(#202318,#202319),(#202320,#202321),
(#202322,#202323),(#202324,#202325),(#202326,#202327),(#202328,#202329),
(#202330,#202331),(#202332,#202333),(#202334,#202335),(#202336,#202337),
(#202338,#202339),(#202340,#202341),(#202342,#202343),(#202344,#202345),
(#202346,#202347),(#202348,#202349),(#202350,#202351),(#202352,#202353),
(#202354,#202355),(#202356,#202357),(#202358,#202359),(#202360,#202361),
(#202362,#202363),(#202364,#202365),(#202366,#202367),(#202368,#202369),
(#202370,#202371),(#202372,#202373),(#202374,#202375),(#202376,#202377),
(#202378,#202379),(#202380,#202381),(#202382,#202383),(#202384,#202385),
(#202386,#202387),(#202388,#202389),(#202390,#202391),(#202392,#202393),
(#202394,#202395),(#202396,#202397),(#202398,#202399),(#202400,#202401),
(#202402,#202403),(#202404,#202405),(#202406,#202407),(#202408,#202409),
(#202410,#202411),(#202412,#202413),(#202414,#202415),(#202416,#202417),
(#202418,#202419),(#202420,#202421),(#202422,#202423),(#202424,#202425),
(#202426,#202427),(#202428,#202429),(#202430,#202431),(#202432,#202433),
(#202434,#202435),(#202436,#202437),(#202438,#202439),(#202440,#202441),
(#202442,#202443),(#202444,#202445),(#202446,#202447),(#202448,#202449),
(#202450,#202451),(#202452,#202453),(#202454,#202455),(#202456,#202457),
(#202458,#202459),(#202460,#202461),(#202462,#202463),(#202464,#202465),
(#202466,#202467),(#202468,#202469),(#202470,#202471),(#202472,#202473),
(#202474,#202475),(#202476,#202477),(#202478,#202479),(#202480,#202481),
(#202482,#202483),(#202484,#202485),(#202486,#202487),(#202488,#202489),
(#202490,#202491),(#202492,#202493),(#202494,#202495),(#202496,#202497),
(#202498,#202499),(#202500,#202501),(#202502,#202503),(#202504,#202505),
(#202506,#202507),(#202508,#202509),(#202510,#202511),(#202512,#202513),
(#202514,#202515),(#202516,#202517),(#202518,#202519),(#202520,#202521),
(#202522,#202523),(#202524,#202525),(#202526,#202527),(#202528,#202529),
(#202530,#202531),(#202532,#202533),(#202534,#202535),(#202536,#202537),
(#202538,#202539),(#202540,#202541),(#202542,#202543),(#202544,#202545),
(#202546,#202547),(#202548,#202549),(#202550,#202551),(#202552,#202553),
(#202554,#202555),(#202556,#202557),(#202558,#202559),(#202560,#202561),
(#202562,#202563),(#202564,#202565),(#202566,#202567),(#202568,#202569),
(#202570,#202571),(#202572,#202573),(#202574,#202575),(#202576,#202577),
(#202578,#202579),(#202580,#202581),(#202582,#202583),(#202584,#202585),
(#202586,#202587),(#202588,#202589),(#202590,#202591),(#202592,#202593),
(#202594,#202595),(#202596,#202597),(#202598,#202599),(#202600,#202601),
(#202602,#202603),(#202604,#202605),(#202606,#202607),(#202608,#202609),
(#202610,#202611),(#202612,#202613),(#202614,#202615),(#202616,#202617),
(#202618,#202619),(#202620,#202621),(#202622,#202623),(#202624,#202625),
(#202626,#202627),(#202628,#202629),(#202630,#202631),(#202632,#202633),
(#202634,#202635),(#202636,#202637),(#202638,#202639),(#202640,#202641),
(#202642,#202643),(#202644,#202645),(#202646,#202647),(#202648,#202649),
(#202650,#202651),(#202652,#202653),(#202654,#202655),(#202656,#202657),
(#202658,#202659),(#202660,#202661),(#202662,#202663),(#202664,#202665),
(#202666,#202667),(#202668,#202669),(#202670,#202671),(#202672,#202673),
(#202674,#202675),(#202676,#202677),(#202678,#202679),(#202680,#202681),
(#202682,#202683),(#202684,#202685),(#202686,#202687),(#202688,#202689),
(#202690,#202691),(#202692,#202693),(#202694,#202695),(#202696,#202697),
(#202698,#202699),(#202700,#202701),(#202702,#202703),(#202704,#202705),
(#202706,#202707),(#202708,#202709),(#202710,#202711),(#202712,#202713),
(#202714,#202715),(#202716,#202717),(#202718,#202719),(#202720,#202721),
(#202722,#202723),(#202724,#202725)),.UNSPECIFIED.,.F.,.F.,.F.)
B_SPLINE_SURFACE_WITH_KNOTS((6,1,1,1,1,1,1,1,1,1,1,1,1,1,1,1,1,1,1,1,1,
1,1,1,1,1,1,1,1,1,1,1,1,1,1,1,1,1,1,1,1,1,1,1,1,1,1,1,1,1,1,1,1,1,1,1,1,
1,1,1,1,1,1,1,1,1,1,1,1,1,1,1,1,1,1,1,1,1,1,1,1,1,1,1,1,1,1,1,1,1,1,1,1,
1,1,1,1,1,1,1,1,1,1,1,1,1,1,1,1,1,1,1,1,1,1,1,1,1,1,1,1,1,1,1,1,1,1,1,1,
1,1,1,1,1,1,1,1,1,1,1,1,1,1,1,1,1,1,1,1,1,1,1,1,1,1,1,1,1,1,1,1,1,1,1,1,
1,1,1,1,1,1,1,1,1,1,1,1,1,1,1,1,1,1,1,1,1,1,1,1,1,1,1,1,1,1,1,1,1,1,1,6),
(2,2),(0.,0.005,0.01,0.015,0.02,0.025,0.03,0.035,0.04,0.045,0.05,0.055,
0.06,0.065,0.07,0.075,0.08,0.085,0.09,0.095,0.1,0.105,0.11,0.115,0.12,0.125,
0.13,0.135,0.14,0.145,0.15,0.155,0.16,0.165,0.17,0.175,0.18,0.185,0.19,
0.195,0.2,0.205,0.21,0.215,0.22,0.225,0.23,0.235,0.24,0.245,0.25,0.255,
0.26,0.265,0.27,0.275,0.28,0.285,0.29,0.295,0.3,0.305,0.31,0.315,0.32,0.325,
0.33,0.335,0.34,0.345,0.35,0.355,0.36,0.365,0.37,0.375,0.38,0.385,0.39,
0.395,0.4,0.405,0.41,0.415,0.42,0.425,0.43,0.435,0.44,0.445,0.45,0.455,
0.46,0.465,0.47,0.475,0.48,0.485,0.49,0.495,0.5,0.505,0.51,0.515,0.52,0.525,
0.53,0.535,0.54,0.545,0.55,0.555,0.56,0.565,0.57,0.575,0.58,0.585,0.59,
0.595,0.6,0.605,0.61,0.615,0.62,0.625,0.63,0.635,0.64,0.645,0.65,0.655,
0.66,0.665,0.67,0.675,0.68,0.685,0.690000000000001,0.695000000000001,0.700000000000001,
0.705000000000001,0.710000000000001,0.715000000000001,0.720000000000001,
0.725000000000001,0.730000000000001,0.735000000000001,0.740000000000001,
0.745000000000001,0.750000000000001,0.755000000000001,0.760000000000001,
0.765000000000001,0.770000000000001,0.775000000000001,0.780000000000001,
0.785000000000001,0.790000000000001,0.795000000000001,0.800000000000001,
0.805000000000001,0.810000000000001,0.815000000000001,0.820000000000001,
0.825000000000001,0.830000000000001,0.835000000000001,0.840000000000001,
0.845000000000001,0.850000000000001,0.855000000000001,0.860000000000001,
0.865000000000001,0.870000000000001,0.875000000000001,0.880000000000001,
0.885000000000001,0.890000000000001,0.895000000000001,0.900000000000001,
0.905000000000001,0.910000000000001,0.915000000000001,0.920000000000001,
0.925000000000001,0.930000000000001,0.935000000000001,0.940000000000001,
0.945000000000001,0.950000000000001,0.955000000000001,0.960000000000001,
0.965000000000001,0.970000000000001,0.975000000000001,0.980000000000001,
0.985000000000001,0.990000000000001,0.995000000000001,1.),(0.,1.2),
 .UNSPECIFIED.)
GEOMETRIC_REPRESENTATION_ITEM()
RATIONAL_B_SPLINE_SURFACE(((1.,1.),(1.,1.),(1.,1.),(1.,1.),(1.,1.),(1.,
1.),(1.,1.),(1.,1.),(1.,1.),(1.,1.),(1.,1.),(1.,1.),(1.,1.),(1.,1.),(1.,
1.),(1.,1.),(1.,1.),(1.,1.),(1.,1.),(1.,1.),(1.,1.),(1.,1.),(1.,1.),(1.,
1.),(1.,1.),(1.,1.),(1.,1.),(1.,1.),(1.,1.),(1.,1.),(1.,1.),(1.,1.),(1.,
1.),(1.,1.),(1.,1.),(1.,1.),(1.,1.),(1.,1.),(1.,1.),(1.,1.),(1.,1.),(1.,
1.),(1.,1.),(1.,1.),(1.,1.),(1.,1.),(1.,1.),(1.,1.),(1.,1.),(1.,1.),(1.,
1.),(1.,1.),(1.,1.),(1.,1.),(1.,1.),(1.,1.),(1.,1.),(1.,1.),(1.,1.),(1.,
1.),(1.,1.),(1.,1.),(1.,1.),(1.,1.),(1.,1.),(1.,1.),(1.,1.),(1.,1.),(1.,
1.),(1.,1.),(1.,1.),(1.,1.),(1.,1.),(1.,1.),(1.,1.),(1.,1.),(1.,1.),(1.,
1.),(1.,1.),(1.,1.),(1.,1.),(1.,1.),(1.,1.),(1.,1.),(1.,1.),(1.,1.),(1.,
1.),(1.,1.),(1.,1.),(1.,1.),(1.,1.),(1.,1.),(1.,1.),(1.,1.),(1.,1.),(1.,
1.),(1.,1.),(1.,1.),(1.,1.),(1.,1.),(1.,1.),(1.,1.),(1.,1.),(1.,1.),(1.,
1.),(1.,1.),(1.,1.),(1.,1.),(1.,1.),(1.,1.),(1.,1.),(1.,1.),(1.,1.),(1.,
1.),(1.,1.),(1.,1.),(1.,1.),(1.,1.),(1.,1.),(1.,1.),(1.,1.),(1.,1.),(1.,
1.),(1.,1.),(1.,1.),(1.,1.),(1.,1.),(1.,1.),(1.,1.),(1.,1.),(1.,1.),(1.,
1.),(1.,1.),(1.,1.),(1.,1.),(1.,1.),(1.,1.),(1.,1.),(1.,1.),(1.,1.),(1.,
1.),(1.,1.),(1.,1.),(1.,1.),(1.,1.),(1.,1.),(1.,1.),(1.,1.),(1.,1.),(1.,
1.),(1.,1.),(1.,1.),(1.,1.),(1.,1.),(1.,1.),(1.,1.),(1.,1.),(1.,1.),(1.,
1.),(1.,1.),(1.,1.),(1.,1.),(1.,1.),(1.,1.),(1.,1.),(1.,1.),(1.,1.),(1.,
1.),(1.,1.),(1.,1.),(1.,1.),(1.,1.),(1.,1.),(1.,1.),(1.,1.),(1.,1.),(1.,
1.),(1.,1.),(1.,1.),(1.,1.),(1.,1.),(1.,1.),(1.,1.),(1.,1.),(1.,1.),(1.,
1.),(1.,1.),(1.,1.),(1.,1.),(1.,1.),(1.,1.),(1.,1.),(1.,1.),(1.,1.),(1.,
1.),(1.,1.),(1.,1.),(1.,1.),(1.,1.),(1.,1.),(1.,1.),(1.,1.),(1.,1.),(1.,
1.),(1.,1.)))
REPRESENTATION_ITEM('')
SURFACE()
);
#1055=(
BOUNDED_SURFACE()
B_SPLINE_SURFACE(5,1,((#202937,#202938),(#202939,#202940),(#202941,#202942),
(#202943,#202944),(#202945,#202946),(#202947,#202948),(#202949,#202950),
(#202951,#202952),(#202953,#202954),(#202955,#202956),(#202957,#202958),
(#202959,#202960),(#202961,#202962),(#202963,#202964),(#202965,#202966),
(#202967,#202968),(#202969,#202970),(#202971,#202972),(#202973,#202974),
(#202975,#202976),(#202977,#202978),(#202979,#202980),(#202981,#202982),
(#202983,#202984),(#202985,#202986),(#202987,#202988),(#202989,#202990),
(#202991,#202992),(#202993,#202994),(#202995,#202996),(#202997,#202998),
(#202999,#203000),(#203001,#203002),(#203003,#203004),(#203005,#203006),
(#203007,#203008),(#203009,#203010),(#203011,#203012),(#203013,#203014),
(#203015,#203016),(#203017,#203018),(#203019,#203020),(#203021,#203022),
(#203023,#203024),(#203025,#203026),(#203027,#203028),(#203029,#203030),
(#203031,#203032),(#203033,#203034),(#203035,#203036),(#203037,#203038),
(#203039,#203040),(#203041,#203042),(#203043,#203044),(#203045,#203046),
(#203047,#203048),(#203049,#203050),(#203051,#203052),(#203053,#203054),
(#203055,#203056),(#203057,#203058),(#203059,#203060),(#203061,#203062),
(#203063,#203064),(#203065,#203066),(#203067,#203068),(#203069,#203070),
(#203071,#203072),(#203073,#203074),(#203075,#203076),(#203077,#203078),
(#203079,#203080),(#203081,#203082),(#203083,#203084),(#203085,#203086),
(#203087,#203088),(#203089,#203090),(#203091,#203092),(#203093,#203094),
(#203095,#203096),(#203097,#203098),(#203099,#203100),(#203101,#203102),
(#203103,#203104),(#203105,#203106),(#203107,#203108),(#203109,#203110),
(#203111,#203112),(#203113,#203114),(#203115,#203116),(#203117,#203118),
(#203119,#203120),(#203121,#203122),(#203123,#203124),(#203125,#203126),
(#203127,#203128),(#203129,#203130),(#203131,#203132),(#203133,#203134),
(#203135,#203136),(#203137,#203138),(#203139,#203140),(#203141,#203142),
(#203143,#203144),(#203145,#203146),(#203147,#203148),(#203149,#203150),
(#203151,#203152),(#203153,#203154),(#203155,#203156),(#203157,#203158),
(#203159,#203160),(#203161,#203162),(#203163,#203164),(#203165,#203166),
(#203167,#203168),(#203169,#203170),(#203171,#203172),(#203173,#203174),
(#203175,#203176),(#203177,#203178),(#203179,#203180),(#203181,#203182),
(#203183,#203184),(#203185,#203186),(#203187,#203188),(#203189,#203190),
(#203191,#203192),(#203193,#203194),(#203195,#203196),(#203197,#203198),
(#203199,#203200),(#203201,#203202),(#203203,#203204),(#203205,#203206),
(#203207,#203208),(#203209,#203210),(#203211,#203212),(#203213,#203214),
(#203215,#203216),(#203217,#203218),(#203219,#203220),(#203221,#203222),
(#203223,#203224),(#203225,#203226),(#203227,#203228),(#203229,#203230),
(#203231,#203232),(#203233,#203234),(#203235,#203236),(#203237,#203238),
(#203239,#203240),(#203241,#203242),(#203243,#203244),(#203245,#203246),
(#203247,#203248),(#203249,#203250),(#203251,#203252),(#203253,#203254),
(#203255,#203256),(#203257,#203258),(#203259,#203260),(#203261,#203262),
(#203263,#203264),(#203265,#203266),(#203267,#203268),(#203269,#203270),
(#203271,#203272),(#203273,#203274),(#203275,#203276),(#203277,#203278),
(#203279,#203280),(#203281,#203282),(#203283,#203284),(#203285,#203286),
(#203287,#203288),(#203289,#203290),(#203291,#203292),(#203293,#203294),
(#203295,#203296),(#203297,#203298),(#203299,#203300),(#203301,#203302),
(#203303,#203304),(#203305,#203306),(#203307,#203308),(#203309,#203310),
(#203311,#203312),(#203313,#203314),(#203315,#203316),(#203317,#203318),
(#203319,#203320),(#203321,#203322),(#203323,#203324),(#203325,#203326),
(#203327,#203328),(#203329,#203330),(#203331,#203332),(#203333,#203334),
(#203335,#203336),(#203337,#203338),(#203339,#203340),(#203341,#203342),
(#203343,#203344),(#203345,#203346)),.UNSPECIFIED.,.F.,.F.,.F.)
B_SPLINE_SURFACE_WITH_KNOTS((6,1,1,1,1,1,1,1,1,1,1,1,1,1,1,1,1,1,1,1,1,
1,1,1,1,1,1,1,1,1,1,1,1,1,1,1,1,1,1,1,1,1,1,1,1,1,1,1,1,1,1,1,1,1,1,1,1,
1,1,1,1,1,1,1,1,1,1,1,1,1,1,1,1,1,1,1,1,1,1,1,1,1,1,1,1,1,1,1,1,1,1,1,1,
1,1,1,1,1,1,1,1,1,1,1,1,1,1,1,1,1,1,1,1,1,1,1,1,1,1,1,1,1,1,1,1,1,1,1,1,
1,1,1,1,1,1,1,1,1,1,1,1,1,1,1,1,1,1,1,1,1,1,1,1,1,1,1,1,1,1,1,1,1,1,1,1,
1,1,1,1,1,1,1,1,1,1,1,1,1,1,1,1,1,1,1,1,1,1,1,1,1,1,1,1,1,1,1,1,1,1,1,6),
(2,2),(-1.,-0.995000000000001,-0.990000000000001,-0.985000000000001,-0.980000000000001,
-0.975000000000001,-0.970000000000001,-0.965000000000001,-0.960000000000001,
-0.955000000000001,-0.950000000000001,-0.945000000000001,-0.940000000000001,
-0.935000000000001,-0.930000000000001,-0.925000000000001,-0.920000000000001,
-0.915000000000001,-0.910000000000001,-0.905000000000001,-0.900000000000001,
-0.895000000000001,-0.890000000000001,-0.885000000000001,-0.880000000000001,
-0.875000000000001,-0.870000000000001,-0.865000000000001,-0.860000000000001,
-0.855000000000001,-0.850000000000001,-0.845000000000001,-0.840000000000001,
-0.835000000000001,-0.830000000000001,-0.825000000000001,-0.820000000000001,
-0.815000000000001,-0.810000000000001,-0.805000000000001,-0.800000000000001,
-0.795000000000001,-0.790000000000001,-0.785000000000001,-0.780000000000001,
-0.775000000000001,-0.770000000000001,-0.765000000000001,-0.760000000000001,
-0.755000000000001,-0.750000000000001,-0.745000000000001,-0.740000000000001,
-0.735000000000001,-0.730000000000001,-0.725000000000001,-0.720000000000001,
-0.715000000000001,-0.710000000000001,-0.705000000000001,-0.700000000000001,
-0.695000000000001,-0.690000000000001,-0.685,-0.68,-0.675,-0.67,-0.665,
-0.66,-0.655,-0.65,-0.645,-0.64,-0.635,-0.63,-0.625,-0.62,-0.615,-0.61,
-0.605,-0.6,-0.595,-0.59,-0.585,-0.58,-0.575,-0.57,-0.565,-0.56,-0.555,
-0.55,-0.545,-0.54,-0.535,-0.53,-0.525,-0.52,-0.515,-0.51,-0.505,-0.5,-0.495,
-0.49,-0.485,-0.48,-0.475,-0.47,-0.465,-0.46,-0.455,-0.45,-0.445,-0.44,
-0.435,-0.43,-0.425,-0.42,-0.415,-0.41,-0.405,-0.4,-0.395,-0.39,-0.385,
-0.38,-0.375,-0.37,-0.365,-0.36,-0.355,-0.35,-0.345,-0.34,-0.335,-0.33,
-0.325,-0.32,-0.315,-0.31,-0.305,-0.3,-0.295,-0.29,-0.285,-0.28,-0.275,
-0.27,-0.265,-0.26,-0.255,-0.25,-0.245,-0.24,-0.235,-0.23,-0.225,-0.22,
-0.215,-0.21,-0.205,-0.2,-0.195,-0.19,-0.185,-0.18,-0.175,-0.17,-0.165,
-0.16,-0.155,-0.15,-0.145,-0.14,-0.135,-0.13,-0.125,-0.12,-0.115,-0.11,
-0.105,-0.1,-0.095,-0.09,-0.085,-0.08,-0.075,-0.07,-0.065,-0.06,-0.055,
-0.05,-0.045,-0.04,-0.035,-0.03,-0.025,-0.02,-0.015,-0.01,-0.005,0.),(0.,
1.2),.UNSPECIFIED.)
GEOMETRIC_REPRESENTATION_ITEM()
RATIONAL_B_SPLINE_SURFACE(((1.,1.),(1.,1.),(1.,1.),(1.,1.),(1.,1.),(1.,
1.),(1.,1.),(1.,1.),(1.,1.),(1.,1.),(1.,1.),(1.,1.),(1.,1.),(1.,1.),(1.,
1.),(1.,1.),(1.,1.),(1.,1.),(1.,1.),(1.,1.),(1.,1.),(1.,1.),(1.,1.),(1.,
1.),(1.,1.),(1.,1.),(1.,1.),(1.,1.),(1.,1.),(1.,1.),(1.,1.),(1.,1.),(1.,
1.),(1.,1.),(1.,1.),(1.,1.),(1.,1.),(1.,1.),(1.,1.),(1.,1.),(1.,1.),(1.,
1.),(1.,1.),(1.,1.),(1.,1.),(1.,1.),(1.,1.),(1.,1.),(1.,1.),(1.,1.),(1.,
1.),(1.,1.),(1.,1.),(1.,1.),(1.,1.),(1.,1.),(1.,1.),(1.,1.),(1.,1.),(1.,
1.),(1.,1.),(1.,1.),(1.,1.),(1.,1.),(1.,1.),(1.,1.),(1.,1.),(1.,1.),(1.,
1.),(1.,1.),(1.,1.),(1.,1.),(1.,1.),(1.,1.),(1.,1.),(1.,1.),(1.,1.),(1.,
1.),(1.,1.),(1.,1.),(1.,1.),(1.,1.),(1.,1.),(1.,1.),(1.,1.),(1.,1.),(1.,
1.),(1.,1.),(1.,1.),(1.,1.),(1.,1.),(1.,1.),(1.,1.),(1.,1.),(1.,1.),(1.,
1.),(1.,1.),(1.,1.),(1.,1.),(1.,1.),(1.,1.),(1.,1.),(1.,1.),(1.,1.),(1.,
1.),(1.,1.),(1.,1.),(1.,1.),(1.,1.),(1.,1.),(1.,1.),(1.,1.),(1.,1.),(1.,
1.),(1.,1.),(1.,1.),(1.,1.),(1.,1.),(1.,1.),(1.,1.),(1.,1.),(1.,1.),(1.,
1.),(1.,1.),(1.,1.),(1.,1.),(1.,1.),(1.,1.),(1.,1.),(1.,1.),(1.,1.),(1.,
1.),(1.,1.),(1.,1.),(1.,1.),(1.,1.),(1.,1.),(1.,1.),(1.,1.),(1.,1.),(1.,
1.),(1.,1.),(1.,1.),(1.,1.),(1.,1.),(1.,1.),(1.,1.),(1.,1.),(1.,1.),(1.,
1.),(1.,1.),(1.,1.),(1.,1.),(1.,1.),(1.,1.),(1.,1.),(1.,1.),(1.,1.),(1.,
1.),(1.,1.),(1.,1.),(1.,1.),(1.,1.),(1.,1.),(1.,1.),(1.,1.),(1.,1.),(1.,
1.),(1.,1.),(1.,1.),(1.,1.),(1.,1.),(1.,1.),(1.,1.),(1.,1.),(1.,1.),(1.,
1.),(1.,1.),(1.,1.),(1.,1.),(1.,1.),(1.,1.),(1.,1.),(1.,1.),(1.,1.),(1.,
1.),(1.,1.),(1.,1.),(1.,1.),(1.,1.),(1.,1.),(1.,1.),(1.,1.),(1.,1.),(1.,
1.),(1.,1.),(1.,1.),(1.,1.),(1.,1.),(1.,1.),(1.,1.),(1.,1.),(1.,1.),(1.,
1.),(1.,1.)))
REPRESENTATION_ITEM('')
SURFACE()
);
#1056=(
BOUNDED_SURFACE()
B_SPLINE_SURFACE(5,1,((#203554,#203555),(#203556,#203557),(#203558,#203559),
(#203560,#203561),(#203562,#203563),(#203564,#203565),(#203566,#203567),
(#203568,#203569),(#203570,#203571),(#203572,#203573),(#203574,#203575),
(#203576,#203577),(#203578,#203579),(#203580,#203581),(#203582,#203583),
(#203584,#203585),(#203586,#203587),(#203588,#203589),(#203590,#203591),
(#203592,#203593),(#203594,#203595),(#203596,#203597),(#203598,#203599),
(#203600,#203601),(#203602,#203603),(#203604,#203605),(#203606,#203607),
(#203608,#203609),(#203610,#203611),(#203612,#203613),(#203614,#203615),
(#203616,#203617),(#203618,#203619),(#203620,#203621),(#203622,#203623),
(#203624,#203625),(#203626,#203627),(#203628,#203629),(#203630,#203631),
(#203632,#203633),(#203634,#203635),(#203636,#203637),(#203638,#203639),
(#203640,#203641),(#203642,#203643),(#203644,#203645),(#203646,#203647),
(#203648,#203649),(#203650,#203651),(#203652,#203653),(#203654,#203655),
(#203656,#203657),(#203658,#203659),(#203660,#203661),(#203662,#203663),
(#203664,#203665),(#203666,#203667),(#203668,#203669),(#203670,#203671),
(#203672,#203673),(#203674,#203675),(#203676,#203677),(#203678,#203679),
(#203680,#203681),(#203682,#203683),(#203684,#203685),(#203686,#203687),
(#203688,#203689),(#203690,#203691),(#203692,#203693),(#203694,#203695),
(#203696,#203697),(#203698,#203699),(#203700,#203701),(#203702,#203703),
(#203704,#203705),(#203706,#203707),(#203708,#203709),(#203710,#203711),
(#203712,#203713),(#203714,#203715),(#203716,#203717),(#203718,#203719),
(#203720,#203721),(#203722,#203723),(#203724,#203725),(#203726,#203727),
(#203728,#203729),(#203730,#203731),(#203732,#203733),(#203734,#203735),
(#203736,#203737),(#203738,#203739),(#203740,#203741),(#203742,#203743),
(#203744,#203745),(#203746,#203747),(#203748,#203749),(#203750,#203751),
(#203752,#203753),(#203754,#203755),(#203756,#203757),(#203758,#203759),
(#203760,#203761),(#203762,#203763),(#203764,#203765),(#203766,#203767),
(#203768,#203769),(#203770,#203771),(#203772,#203773),(#203774,#203775),
(#203776,#203777),(#203778,#203779),(#203780,#203781),(#203782,#203783),
(#203784,#203785),(#203786,#203787),(#203788,#203789),(#203790,#203791),
(#203792,#203793),(#203794,#203795),(#203796,#203797),(#203798,#203799),
(#203800,#203801),(#203802,#203803),(#203804,#203805),(#203806,#203807),
(#203808,#203809),(#203810,#203811),(#203812,#203813),(#203814,#203815),
(#203816,#203817),(#203818,#203819),(#203820,#203821),(#203822,#203823),
(#203824,#203825),(#203826,#203827),(#203828,#203829),(#203830,#203831),
(#203832,#203833),(#203834,#203835),(#203836,#203837),(#203838,#203839),
(#203840,#203841),(#203842,#203843),(#203844,#203845),(#203846,#203847),
(#203848,#203849),(#203850,#203851),(#203852,#203853),(#203854,#203855),
(#203856,#203857),(#203858,#203859),(#203860,#203861),(#203862,#203863),
(#203864,#203865),(#203866,#203867),(#203868,#203869),(#203870,#203871),
(#203872,#203873),(#203874,#203875),(#203876,#203877),(#203878,#203879),
(#203880,#203881),(#203882,#203883),(#203884,#203885),(#203886,#203887),
(#203888,#203889),(#203890,#203891),(#203892,#203893),(#203894,#203895),
(#203896,#203897),(#203898,#203899),(#203900,#203901),(#203902,#203903),
(#203904,#203905),(#203906,#203907),(#203908,#203909),(#203910,#203911),
(#203912,#203913),(#203914,#203915),(#203916,#203917),(#203918,#203919),
(#203920,#203921),(#203922,#203923),(#203924,#203925),(#203926,#203927),
(#203928,#203929),(#203930,#203931),(#203932,#203933),(#203934,#203935),
(#203936,#203937),(#203938,#203939),(#203940,#203941),(#203942,#203943),
(#203944,#203945),(#203946,#203947),(#203948,#203949),(#203950,#203951),
(#203952,#203953),(#203954,#203955),(#203956,#203957),(#203958,#203959),
(#203960,#203961),(#203962,#203963)),.UNSPECIFIED.,.F.,.F.,.F.)
B_SPLINE_SURFACE_WITH_KNOTS((6,1,1,1,1,1,1,1,1,1,1,1,1,1,1,1,1,1,1,1,1,
1,1,1,1,1,1,1,1,1,1,1,1,1,1,1,1,1,1,1,1,1,1,1,1,1,1,1,1,1,1,1,1,1,1,1,1,
1,1,1,1,1,1,1,1,1,1,1,1,1,1,1,1,1,1,1,1,1,1,1,1,1,1,1,1,1,1,1,1,1,1,1,1,
1,1,1,1,1,1,1,1,1,1,1,1,1,1,1,1,1,1,1,1,1,1,1,1,1,1,1,1,1,1,1,1,1,1,1,1,
1,1,1,1,1,1,1,1,1,1,1,1,1,1,1,1,1,1,1,1,1,1,1,1,1,1,1,1,1,1,1,1,1,1,1,1,
1,1,1,1,1,1,1,1,1,1,1,1,1,1,1,1,1,1,1,1,1,1,1,1,1,1,1,1,1,1,1,1,1,1,1,6),
(2,2),(0.,0.005,0.01,0.015,0.02,0.025,0.03,0.035,0.04,0.045,0.05,0.055,
0.06,0.065,0.07,0.075,0.08,0.085,0.09,0.095,0.1,0.105,0.11,0.115,0.12,0.125,
0.13,0.135,0.14,0.145,0.15,0.155,0.16,0.165,0.17,0.175,0.18,0.185,0.19,
0.195,0.2,0.205,0.21,0.215,0.22,0.225,0.23,0.235,0.24,0.245,0.25,0.255,
0.26,0.265,0.27,0.275,0.28,0.285,0.29,0.295,0.3,0.305,0.31,0.315,0.32,0.325,
0.33,0.335,0.34,0.345,0.35,0.355,0.36,0.365,0.37,0.375,0.38,0.385,0.39,
0.395,0.4,0.405,0.41,0.415,0.42,0.425,0.43,0.435,0.44,0.445,0.45,0.455,
0.46,0.465,0.47,0.475,0.48,0.485,0.49,0.495,0.5,0.505,0.51,0.515,0.52,0.525,
0.53,0.535,0.54,0.545,0.55,0.555,0.56,0.565,0.57,0.575,0.58,0.585,0.59,
0.595,0.6,0.605,0.61,0.615,0.62,0.625,0.63,0.635,0.64,0.645,0.65,0.655,
0.66,0.665,0.67,0.675,0.68,0.685,0.690000000000001,0.695000000000001,0.700000000000001,
0.705000000000001,0.710000000000001,0.715000000000001,0.720000000000001,
0.725000000000001,0.730000000000001,0.735000000000001,0.740000000000001,
0.745000000000001,0.750000000000001,0.755000000000001,0.760000000000001,
0.765000000000001,0.770000000000001,0.775000000000001,0.780000000000001,
0.785000000000001,0.790000000000001,0.795000000000001,0.800000000000001,
0.805000000000001,0.810000000000001,0.815000000000001,0.820000000000001,
0.825000000000001,0.830000000000001,0.835000000000001,0.840000000000001,
0.845000000000001,0.850000000000001,0.855000000000001,0.860000000000001,
0.865000000000001,0.870000000000001,0.875000000000001,0.880000000000001,
0.885000000000001,0.890000000000001,0.895000000000001,0.900000000000001,
0.905000000000001,0.910000000000001,0.915000000000001,0.920000000000001,
0.925000000000001,0.930000000000001,0.935000000000001,0.940000000000001,
0.945000000000001,0.950000000000001,0.955000000000001,0.960000000000001,
0.965000000000001,0.970000000000001,0.975000000000001,0.980000000000001,
0.985000000000001,0.990000000000001,0.995000000000001,1.),(0.,1.2),
 .UNSPECIFIED.)
GEOMETRIC_REPRESENTATION_ITEM()
RATIONAL_B_SPLINE_SURFACE(((1.,1.),(1.,1.),(1.,1.),(1.,1.),(1.,1.),(1.,
1.),(1.,1.),(1.,1.),(1.,1.),(1.,1.),(1.,1.),(1.,1.),(1.,1.),(1.,1.),(1.,
1.),(1.,1.),(1.,1.),(1.,1.),(1.,1.),(1.,1.),(1.,1.),(1.,1.),(1.,1.),(1.,
1.),(1.,1.),(1.,1.),(1.,1.),(1.,1.),(1.,1.),(1.,1.),(1.,1.),(1.,1.),(1.,
1.),(1.,1.),(1.,1.),(1.,1.),(1.,1.),(1.,1.),(1.,1.),(1.,1.),(1.,1.),(1.,
1.),(1.,1.),(1.,1.),(1.,1.),(1.,1.),(1.,1.),(1.,1.),(1.,1.),(1.,1.),(1.,
1.),(1.,1.),(1.,1.),(1.,1.),(1.,1.),(1.,1.),(1.,1.),(1.,1.),(1.,1.),(1.,
1.),(1.,1.),(1.,1.),(1.,1.),(1.,1.),(1.,1.),(1.,1.),(1.,1.),(1.,1.),(1.,
1.),(1.,1.),(1.,1.),(1.,1.),(1.,1.),(1.,1.),(1.,1.),(1.,1.),(1.,1.),(1.,
1.),(1.,1.),(1.,1.),(1.,1.),(1.,1.),(1.,1.),(1.,1.),(1.,1.),(1.,1.),(1.,
1.),(1.,1.),(1.,1.),(1.,1.),(1.,1.),(1.,1.),(1.,1.),(1.,1.),(1.,1.),(1.,
1.),(1.,1.),(1.,1.),(1.,1.),(1.,1.),(1.,1.),(1.,1.),(1.,1.),(1.,1.),(1.,
1.),(1.,1.),(1.,1.),(1.,1.),(1.,1.),(1.,1.),(1.,1.),(1.,1.),(1.,1.),(1.,
1.),(1.,1.),(1.,1.),(1.,1.),(1.,1.),(1.,1.),(1.,1.),(1.,1.),(1.,1.),(1.,
1.),(1.,1.),(1.,1.),(1.,1.),(1.,1.),(1.,1.),(1.,1.),(1.,1.),(1.,1.),(1.,
1.),(1.,1.),(1.,1.),(1.,1.),(1.,1.),(1.,1.),(1.,1.),(1.,1.),(1.,1.),(1.,
1.),(1.,1.),(1.,1.),(1.,1.),(1.,1.),(1.,1.),(1.,1.),(1.,1.),(1.,1.),(1.,
1.),(1.,1.),(1.,1.),(1.,1.),(1.,1.),(1.,1.),(1.,1.),(1.,1.),(1.,1.),(1.,
1.),(1.,1.),(1.,1.),(1.,1.),(1.,1.),(1.,1.),(1.,1.),(1.,1.),(1.,1.),(1.,
1.),(1.,1.),(1.,1.),(1.,1.),(1.,1.),(1.,1.),(1.,1.),(1.,1.),(1.,1.),(1.,
1.),(1.,1.),(1.,1.),(1.,1.),(1.,1.),(1.,1.),(1.,1.),(1.,1.),(1.,1.),(1.,
1.),(1.,1.),(1.,1.),(1.,1.),(1.,1.),(1.,1.),(1.,1.),(1.,1.),(1.,1.),(1.,
1.),(1.,1.),(1.,1.),(1.,1.),(1.,1.),(1.,1.),(1.,1.),(1.,1.),(1.,1.),(1.,
1.),(1.,1.)))
REPRESENTATION_ITEM('')
SURFACE()
);
#1057=(
BOUNDED_SURFACE()
B_SPLINE_SURFACE(5,1,((#204175,#204176),(#204177,#204178),(#204179,#204180),
(#204181,#204182),(#204183,#204184),(#204185,#204186),(#204187,#204188),
(#204189,#204190),(#204191,#204192),(#204193,#204194),(#204195,#204196),
(#204197,#204198),(#204199,#204200),(#204201,#204202),(#204203,#204204),
(#204205,#204206),(#204207,#204208),(#204209,#204210),(#204211,#204212),
(#204213,#204214),(#204215,#204216),(#204217,#204218),(#204219,#204220),
(#204221,#204222),(#204223,#204224),(#204225,#204226),(#204227,#204228),
(#204229,#204230),(#204231,#204232),(#204233,#204234),(#204235,#204236),
(#204237,#204238),(#204239,#204240),(#204241,#204242),(#204243,#204244),
(#204245,#204246),(#204247,#204248),(#204249,#204250),(#204251,#204252),
(#204253,#204254),(#204255,#204256),(#204257,#204258),(#204259,#204260),
(#204261,#204262),(#204263,#204264),(#204265,#204266),(#204267,#204268),
(#204269,#204270),(#204271,#204272),(#204273,#204274),(#204275,#204276),
(#204277,#204278),(#204279,#204280),(#204281,#204282),(#204283,#204284),
(#204285,#204286),(#204287,#204288),(#204289,#204290),(#204291,#204292),
(#204293,#204294),(#204295,#204296),(#204297,#204298),(#204299,#204300),
(#204301,#204302),(#204303,#204304),(#204305,#204306),(#204307,#204308),
(#204309,#204310),(#204311,#204312),(#204313,#204314),(#204315,#204316),
(#204317,#204318),(#204319,#204320),(#204321,#204322),(#204323,#204324),
(#204325,#204326),(#204327,#204328),(#204329,#204330),(#204331,#204332),
(#204333,#204334),(#204335,#204336),(#204337,#204338),(#204339,#204340),
(#204341,#204342),(#204343,#204344),(#204345,#204346),(#204347,#204348),
(#204349,#204350),(#204351,#204352),(#204353,#204354),(#204355,#204356),
(#204357,#204358),(#204359,#204360),(#204361,#204362),(#204363,#204364),
(#204365,#204366),(#204367,#204368),(#204369,#204370),(#204371,#204372),
(#204373,#204374),(#204375,#204376),(#204377,#204378),(#204379,#204380),
(#204381,#204382),(#204383,#204384),(#204385,#204386),(#204387,#204388),
(#204389,#204390),(#204391,#204392),(#204393,#204394),(#204395,#204396),
(#204397,#204398),(#204399,#204400),(#204401,#204402),(#204403,#204404),
(#204405,#204406),(#204407,#204408),(#204409,#204410),(#204411,#204412),
(#204413,#204414),(#204415,#204416),(#204417,#204418),(#204419,#204420),
(#204421,#204422),(#204423,#204424),(#204425,#204426),(#204427,#204428),
(#204429,#204430),(#204431,#204432),(#204433,#204434),(#204435,#204436),
(#204437,#204438),(#204439,#204440),(#204441,#204442),(#204443,#204444),
(#204445,#204446),(#204447,#204448),(#204449,#204450),(#204451,#204452),
(#204453,#204454),(#204455,#204456),(#204457,#204458),(#204459,#204460),
(#204461,#204462),(#204463,#204464),(#204465,#204466),(#204467,#204468),
(#204469,#204470),(#204471,#204472),(#204473,#204474),(#204475,#204476),
(#204477,#204478),(#204479,#204480),(#204481,#204482),(#204483,#204484),
(#204485,#204486),(#204487,#204488),(#204489,#204490),(#204491,#204492),
(#204493,#204494),(#204495,#204496),(#204497,#204498),(#204499,#204500),
(#204501,#204502),(#204503,#204504),(#204505,#204506),(#204507,#204508),
(#204509,#204510),(#204511,#204512),(#204513,#204514),(#204515,#204516),
(#204517,#204518),(#204519,#204520),(#204521,#204522),(#204523,#204524),
(#204525,#204526),(#204527,#204528),(#204529,#204530),(#204531,#204532),
(#204533,#204534),(#204535,#204536),(#204537,#204538),(#204539,#204540),
(#204541,#204542),(#204543,#204544),(#204545,#204546),(#204547,#204548),
(#204549,#204550),(#204551,#204552),(#204553,#204554),(#204555,#204556),
(#204557,#204558),(#204559,#204560),(#204561,#204562),(#204563,#204564),
(#204565,#204566),(#204567,#204568),(#204569,#204570),(#204571,#204572),
(#204573,#204574),(#204575,#204576),(#204577,#204578),(#204579,#204580),
(#204581,#204582),(#204583,#204584)),.UNSPECIFIED.,.F.,.F.,.F.)
B_SPLINE_SURFACE_WITH_KNOTS((6,1,1,1,1,1,1,1,1,1,1,1,1,1,1,1,1,1,1,1,1,
1,1,1,1,1,1,1,1,1,1,1,1,1,1,1,1,1,1,1,1,1,1,1,1,1,1,1,1,1,1,1,1,1,1,1,1,
1,1,1,1,1,1,1,1,1,1,1,1,1,1,1,1,1,1,1,1,1,1,1,1,1,1,1,1,1,1,1,1,1,1,1,1,
1,1,1,1,1,1,1,1,1,1,1,1,1,1,1,1,1,1,1,1,1,1,1,1,1,1,1,1,1,1,1,1,1,1,1,1,
1,1,1,1,1,1,1,1,1,1,1,1,1,1,1,1,1,1,1,1,1,1,1,1,1,1,1,1,1,1,1,1,1,1,1,1,
1,1,1,1,1,1,1,1,1,1,1,1,1,1,1,1,1,1,1,1,1,1,1,1,1,1,1,1,1,1,1,1,1,1,1,6),
(2,2),(-1.,-0.995000000000001,-0.990000000000001,-0.985000000000001,-0.980000000000001,
-0.975000000000001,-0.970000000000001,-0.965000000000001,-0.960000000000001,
-0.955000000000001,-0.950000000000001,-0.945000000000001,-0.940000000000001,
-0.935000000000001,-0.930000000000001,-0.925000000000001,-0.920000000000001,
-0.915000000000001,-0.910000000000001,-0.905000000000001,-0.900000000000001,
-0.895000000000001,-0.890000000000001,-0.885000000000001,-0.880000000000001,
-0.875000000000001,-0.870000000000001,-0.865000000000001,-0.860000000000001,
-0.855000000000001,-0.850000000000001,-0.845000000000001,-0.840000000000001,
-0.835000000000001,-0.830000000000001,-0.825000000000001,-0.820000000000001,
-0.815000000000001,-0.810000000000001,-0.805000000000001,-0.800000000000001,
-0.795000000000001,-0.790000000000001,-0.785000000000001,-0.780000000000001,
-0.775000000000001,-0.770000000000001,-0.765000000000001,-0.760000000000001,
-0.755000000000001,-0.750000000000001,-0.745000000000001,-0.740000000000001,
-0.735000000000001,-0.730000000000001,-0.725000000000001,-0.720000000000001,
-0.715000000000001,-0.710000000000001,-0.705000000000001,-0.700000000000001,
-0.695000000000001,-0.690000000000001,-0.685,-0.68,-0.675,-0.67,-0.665,
-0.66,-0.655,-0.65,-0.645,-0.64,-0.635,-0.63,-0.625,-0.62,-0.615,-0.61,
-0.605,-0.6,-0.595,-0.59,-0.585,-0.58,-0.575,-0.57,-0.565,-0.56,-0.555,
-0.55,-0.545,-0.54,-0.535,-0.53,-0.525,-0.52,-0.515,-0.51,-0.505,-0.5,-0.495,
-0.49,-0.485,-0.48,-0.475,-0.47,-0.465,-0.46,-0.455,-0.45,-0.445,-0.44,
-0.435,-0.43,-0.425,-0.42,-0.415,-0.41,-0.405,-0.4,-0.395,-0.39,-0.385,
-0.38,-0.375,-0.37,-0.365,-0.36,-0.355,-0.35,-0.345,-0.34,-0.335,-0.33,
-0.325,-0.32,-0.315,-0.31,-0.305,-0.3,-0.295,-0.29,-0.285,-0.28,-0.275,
-0.27,-0.265,-0.26,-0.255,-0.25,-0.245,-0.24,-0.235,-0.23,-0.225,-0.22,
-0.215,-0.21,-0.205,-0.2,-0.195,-0.19,-0.185,-0.18,-0.175,-0.17,-0.165,
-0.16,-0.155,-0.15,-0.145,-0.14,-0.135,-0.13,-0.125,-0.12,-0.115,-0.11,
-0.105,-0.1,-0.095,-0.09,-0.085,-0.08,-0.075,-0.07,-0.065,-0.06,-0.055,
-0.05,-0.045,-0.04,-0.035,-0.03,-0.025,-0.02,-0.015,-0.01,-0.005,0.),(0.,
1.2),.UNSPECIFIED.)
GEOMETRIC_REPRESENTATION_ITEM()
RATIONAL_B_SPLINE_SURFACE(((1.,1.),(1.,1.),(1.,1.),(1.,1.),(1.,1.),(1.,
1.),(1.,1.),(1.,1.),(1.,1.),(1.,1.),(1.,1.),(1.,1.),(1.,1.),(1.,1.),(1.,
1.),(1.,1.),(1.,1.),(1.,1.),(1.,1.),(1.,1.),(1.,1.),(1.,1.),(1.,1.),(1.,
1.),(1.,1.),(1.,1.),(1.,1.),(1.,1.),(1.,1.),(1.,1.),(1.,1.),(1.,1.),(1.,
1.),(1.,1.),(1.,1.),(1.,1.),(1.,1.),(1.,1.),(1.,1.),(1.,1.),(1.,1.),(1.,
1.),(1.,1.),(1.,1.),(1.,1.),(1.,1.),(1.,1.),(1.,1.),(1.,1.),(1.,1.),(1.,
1.),(1.,1.),(1.,1.),(1.,1.),(1.,1.),(1.,1.),(1.,1.),(1.,1.),(1.,1.),(1.,
1.),(1.,1.),(1.,1.),(1.,1.),(1.,1.),(1.,1.),(1.,1.),(1.,1.),(1.,1.),(1.,
1.),(1.,1.),(1.,1.),(1.,1.),(1.,1.),(1.,1.),(1.,1.),(1.,1.),(1.,1.),(1.,
1.),(1.,1.),(1.,1.),(1.,1.),(1.,1.),(1.,1.),(1.,1.),(1.,1.),(1.,1.),(1.,
1.),(1.,1.),(1.,1.),(1.,1.),(1.,1.),(1.,1.),(1.,1.),(1.,1.),(1.,1.),(1.,
1.),(1.,1.),(1.,1.),(1.,1.),(1.,1.),(1.,1.),(1.,1.),(1.,1.),(1.,1.),(1.,
1.),(1.,1.),(1.,1.),(1.,1.),(1.,1.),(1.,1.),(1.,1.),(1.,1.),(1.,1.),(1.,
1.),(1.,1.),(1.,1.),(1.,1.),(1.,1.),(1.,1.),(1.,1.),(1.,1.),(1.,1.),(1.,
1.),(1.,1.),(1.,1.),(1.,1.),(1.,1.),(1.,1.),(1.,1.),(1.,1.),(1.,1.),(1.,
1.),(1.,1.),(1.,1.),(1.,1.),(1.,1.),(1.,1.),(1.,1.),(1.,1.),(1.,1.),(1.,
1.),(1.,1.),(1.,1.),(1.,1.),(1.,1.),(1.,1.),(1.,1.),(1.,1.),(1.,1.),(1.,
1.),(1.,1.),(1.,1.),(1.,1.),(1.,1.),(1.,1.),(1.,1.),(1.,1.),(1.,1.),(1.,
1.),(1.,1.),(1.,1.),(1.,1.),(1.,1.),(1.,1.),(1.,1.),(1.,1.),(1.,1.),(1.,
1.),(1.,1.),(1.,1.),(1.,1.),(1.,1.),(1.,1.),(1.,1.),(1.,1.),(1.,1.),(1.,
1.),(1.,1.),(1.,1.),(1.,1.),(1.,1.),(1.,1.),(1.,1.),(1.,1.),(1.,1.),(1.,
1.),(1.,1.),(1.,1.),(1.,1.),(1.,1.),(1.,1.),(1.,1.),(1.,1.),(1.,1.),(1.,
1.),(1.,1.),(1.,1.),(1.,1.),(1.,1.),(1.,1.),(1.,1.),(1.,1.),(1.,1.),(1.,
1.),(1.,1.)))
REPRESENTATION_ITEM('')
SURFACE()
);
#1058=(
BOUNDED_SURFACE()
B_SPLINE_SURFACE(5,1,((#204792,#204793),(#204794,#204795),(#204796,#204797),
(#204798,#204799),(#204800,#204801),(#204802,#204803),(#204804,#204805),
(#204806,#204807),(#204808,#204809),(#204810,#204811),(#204812,#204813),
(#204814,#204815),(#204816,#204817),(#204818,#204819),(#204820,#204821),
(#204822,#204823),(#204824,#204825),(#204826,#204827),(#204828,#204829),
(#204830,#204831),(#204832,#204833),(#204834,#204835),(#204836,#204837),
(#204838,#204839),(#204840,#204841),(#204842,#204843),(#204844,#204845),
(#204846,#204847),(#204848,#204849),(#204850,#204851),(#204852,#204853),
(#204854,#204855),(#204856,#204857),(#204858,#204859),(#204860,#204861),
(#204862,#204863),(#204864,#204865),(#204866,#204867),(#204868,#204869),
(#204870,#204871),(#204872,#204873),(#204874,#204875),(#204876,#204877),
(#204878,#204879),(#204880,#204881),(#204882,#204883),(#204884,#204885),
(#204886,#204887),(#204888,#204889),(#204890,#204891),(#204892,#204893),
(#204894,#204895),(#204896,#204897),(#204898,#204899),(#204900,#204901),
(#204902,#204903),(#204904,#204905),(#204906,#204907),(#204908,#204909),
(#204910,#204911),(#204912,#204913),(#204914,#204915),(#204916,#204917),
(#204918,#204919),(#204920,#204921),(#204922,#204923),(#204924,#204925),
(#204926,#204927),(#204928,#204929),(#204930,#204931),(#204932,#204933),
(#204934,#204935),(#204936,#204937),(#204938,#204939),(#204940,#204941),
(#204942,#204943),(#204944,#204945),(#204946,#204947),(#204948,#204949),
(#204950,#204951),(#204952,#204953),(#204954,#204955),(#204956,#204957),
(#204958,#204959),(#204960,#204961),(#204962,#204963),(#204964,#204965),
(#204966,#204967),(#204968,#204969),(#204970,#204971),(#204972,#204973),
(#204974,#204975),(#204976,#204977),(#204978,#204979),(#204980,#204981),
(#204982,#204983),(#204984,#204985),(#204986,#204987),(#204988,#204989),
(#204990,#204991),(#204992,#204993),(#204994,#204995),(#204996,#204997),
(#204998,#204999),(#205000,#205001),(#205002,#205003),(#205004,#205005),
(#205006,#205007),(#205008,#205009),(#205010,#205011),(#205012,#205013),
(#205014,#205015),(#205016,#205017),(#205018,#205019),(#205020,#205021),
(#205022,#205023),(#205024,#205025),(#205026,#205027),(#205028,#205029),
(#205030,#205031),(#205032,#205033),(#205034,#205035),(#205036,#205037),
(#205038,#205039),(#205040,#205041),(#205042,#205043),(#205044,#205045),
(#205046,#205047),(#205048,#205049),(#205050,#205051),(#205052,#205053),
(#205054,#205055),(#205056,#205057),(#205058,#205059),(#205060,#205061),
(#205062,#205063),(#205064,#205065),(#205066,#205067),(#205068,#205069),
(#205070,#205071),(#205072,#205073),(#205074,#205075),(#205076,#205077),
(#205078,#205079),(#205080,#205081),(#205082,#205083),(#205084,#205085),
(#205086,#205087),(#205088,#205089),(#205090,#205091),(#205092,#205093),
(#205094,#205095),(#205096,#205097),(#205098,#205099),(#205100,#205101),
(#205102,#205103),(#205104,#205105),(#205106,#205107),(#205108,#205109),
(#205110,#205111),(#205112,#205113),(#205114,#205115),(#205116,#205117),
(#205118,#205119),(#205120,#205121),(#205122,#205123),(#205124,#205125),
(#205126,#205127),(#205128,#205129),(#205130,#205131),(#205132,#205133),
(#205134,#205135),(#205136,#205137),(#205138,#205139),(#205140,#205141),
(#205142,#205143),(#205144,#205145),(#205146,#205147),(#205148,#205149),
(#205150,#205151),(#205152,#205153),(#205154,#205155),(#205156,#205157),
(#205158,#205159),(#205160,#205161),(#205162,#205163),(#205164,#205165),
(#205166,#205167),(#205168,#205169),(#205170,#205171),(#205172,#205173),
(#205174,#205175),(#205176,#205177),(#205178,#205179),(#205180,#205181),
(#205182,#205183),(#205184,#205185),(#205186,#205187),(#205188,#205189),
(#205190,#205191),(#205192,#205193),(#205194,#205195),(#205196,#205197),
(#205198,#205199),(#205200,#205201)),.UNSPECIFIED.,.F.,.F.,.F.)
B_SPLINE_SURFACE_WITH_KNOTS((6,1,1,1,1,1,1,1,1,1,1,1,1,1,1,1,1,1,1,1,1,
1,1,1,1,1,1,1,1,1,1,1,1,1,1,1,1,1,1,1,1,1,1,1,1,1,1,1,1,1,1,1,1,1,1,1,1,
1,1,1,1,1,1,1,1,1,1,1,1,1,1,1,1,1,1,1,1,1,1,1,1,1,1,1,1,1,1,1,1,1,1,1,1,
1,1,1,1,1,1,1,1,1,1,1,1,1,1,1,1,1,1,1,1,1,1,1,1,1,1,1,1,1,1,1,1,1,1,1,1,
1,1,1,1,1,1,1,1,1,1,1,1,1,1,1,1,1,1,1,1,1,1,1,1,1,1,1,1,1,1,1,1,1,1,1,1,
1,1,1,1,1,1,1,1,1,1,1,1,1,1,1,1,1,1,1,1,1,1,1,1,1,1,1,1,1,1,1,1,1,1,1,6),
(2,2),(0.,0.005,0.01,0.015,0.02,0.025,0.03,0.035,0.04,0.045,0.05,0.055,
0.06,0.065,0.07,0.075,0.08,0.085,0.09,0.095,0.1,0.105,0.11,0.115,0.12,0.125,
0.13,0.135,0.14,0.145,0.15,0.155,0.16,0.165,0.17,0.175,0.18,0.185,0.19,
0.195,0.2,0.205,0.21,0.215,0.22,0.225,0.23,0.235,0.24,0.245,0.25,0.255,
0.26,0.265,0.27,0.275,0.28,0.285,0.29,0.295,0.3,0.305,0.31,0.315,0.32,0.325,
0.33,0.335,0.34,0.345,0.35,0.355,0.36,0.365,0.37,0.375,0.38,0.385,0.39,
0.395,0.4,0.405,0.41,0.415,0.42,0.425,0.43,0.435,0.44,0.445,0.45,0.455,
0.46,0.465,0.47,0.475,0.48,0.485,0.49,0.495,0.5,0.505,0.51,0.515,0.52,0.525,
0.53,0.535,0.54,0.545,0.55,0.555,0.56,0.565,0.57,0.575,0.58,0.585,0.59,
0.595,0.6,0.605,0.61,0.615,0.62,0.625,0.63,0.635,0.64,0.645,0.65,0.655,
0.66,0.665,0.67,0.675,0.68,0.685,0.690000000000001,0.695000000000001,0.700000000000001,
0.705000000000001,0.710000000000001,0.715000000000001,0.720000000000001,
0.725000000000001,0.730000000000001,0.735000000000001,0.740000000000001,
0.745000000000001,0.750000000000001,0.755000000000001,0.760000000000001,
0.765000000000001,0.770000000000001,0.775000000000001,0.780000000000001,
0.785000000000001,0.790000000000001,0.795000000000001,0.800000000000001,
0.805000000000001,0.810000000000001,0.815000000000001,0.820000000000001,
0.825000000000001,0.830000000000001,0.835000000000001,0.840000000000001,
0.845000000000001,0.850000000000001,0.855000000000001,0.860000000000001,
0.865000000000001,0.870000000000001,0.875000000000001,0.880000000000001,
0.885000000000001,0.890000000000001,0.895000000000001,0.900000000000001,
0.905000000000001,0.910000000000001,0.915000000000001,0.920000000000001,
0.925000000000001,0.930000000000001,0.935000000000001,0.940000000000001,
0.945000000000001,0.950000000000001,0.955000000000001,0.960000000000001,
0.965000000000001,0.970000000000001,0.975000000000001,0.980000000000001,
0.985000000000001,0.990000000000001,0.995000000000001,1.),(0.,1.2),
 .UNSPECIFIED.)
GEOMETRIC_REPRESENTATION_ITEM()
RATIONAL_B_SPLINE_SURFACE(((1.,1.),(1.,1.),(1.,1.),(1.,1.),(1.,1.),(1.,
1.),(1.,1.),(1.,1.),(1.,1.),(1.,1.),(1.,1.),(1.,1.),(1.,1.),(1.,1.),(1.,
1.),(1.,1.),(1.,1.),(1.,1.),(1.,1.),(1.,1.),(1.,1.),(1.,1.),(1.,1.),(1.,
1.),(1.,1.),(1.,1.),(1.,1.),(1.,1.),(1.,1.),(1.,1.),(1.,1.),(1.,1.),(1.,
1.),(1.,1.),(1.,1.),(1.,1.),(1.,1.),(1.,1.),(1.,1.),(1.,1.),(1.,1.),(1.,
1.),(1.,1.),(1.,1.),(1.,1.),(1.,1.),(1.,1.),(1.,1.),(1.,1.),(1.,1.),(1.,
1.),(1.,1.),(1.,1.),(1.,1.),(1.,1.),(1.,1.),(1.,1.),(1.,1.),(1.,1.),(1.,
1.),(1.,1.),(1.,1.),(1.,1.),(1.,1.),(1.,1.),(1.,1.),(1.,1.),(1.,1.),(1.,
1.),(1.,1.),(1.,1.),(1.,1.),(1.,1.),(1.,1.),(1.,1.),(1.,1.),(1.,1.),(1.,
1.),(1.,1.),(1.,1.),(1.,1.),(1.,1.),(1.,1.),(1.,1.),(1.,1.),(1.,1.),(1.,
1.),(1.,1.),(1.,1.),(1.,1.),(1.,1.),(1.,1.),(1.,1.),(1.,1.),(1.,1.),(1.,
1.),(1.,1.),(1.,1.),(1.,1.),(1.,1.),(1.,1.),(1.,1.),(1.,1.),(1.,1.),(1.,
1.),(1.,1.),(1.,1.),(1.,1.),(1.,1.),(1.,1.),(1.,1.),(1.,1.),(1.,1.),(1.,
1.),(1.,1.),(1.,1.),(1.,1.),(1.,1.),(1.,1.),(1.,1.),(1.,1.),(1.,1.),(1.,
1.),(1.,1.),(1.,1.),(1.,1.),(1.,1.),(1.,1.),(1.,1.),(1.,1.),(1.,1.),(1.,
1.),(1.,1.),(1.,1.),(1.,1.),(1.,1.),(1.,1.),(1.,1.),(1.,1.),(1.,1.),(1.,
1.),(1.,1.),(1.,1.),(1.,1.),(1.,1.),(1.,1.),(1.,1.),(1.,1.),(1.,1.),(1.,
1.),(1.,1.),(1.,1.),(1.,1.),(1.,1.),(1.,1.),(1.,1.),(1.,1.),(1.,1.),(1.,
1.),(1.,1.),(1.,1.),(1.,1.),(1.,1.),(1.,1.),(1.,1.),(1.,1.),(1.,1.),(1.,
1.),(1.,1.),(1.,1.),(1.,1.),(1.,1.),(1.,1.),(1.,1.),(1.,1.),(1.,1.),(1.,
1.),(1.,1.),(1.,1.),(1.,1.),(1.,1.),(1.,1.),(1.,1.),(1.,1.),(1.,1.),(1.,
1.),(1.,1.),(1.,1.),(1.,1.),(1.,1.),(1.,1.),(1.,1.),(1.,1.),(1.,1.),(1.,
1.),(1.,1.),(1.,1.),(1.,1.),(1.,1.),(1.,1.),(1.,1.),(1.,1.),(1.,1.),(1.,
1.),(1.,1.)))
REPRESENTATION_ITEM('')
SURFACE()
);
#1059=(
BOUNDED_SURFACE()
B_SPLINE_SURFACE(5,1,((#205413,#205414),(#205415,#205416),(#205417,#205418),
(#205419,#205420),(#205421,#205422),(#205423,#205424),(#205425,#205426),
(#205427,#205428),(#205429,#205430),(#205431,#205432),(#205433,#205434),
(#205435,#205436),(#205437,#205438),(#205439,#205440),(#205441,#205442),
(#205443,#205444),(#205445,#205446),(#205447,#205448),(#205449,#205450),
(#205451,#205452),(#205453,#205454),(#205455,#205456),(#205457,#205458),
(#205459,#205460),(#205461,#205462),(#205463,#205464),(#205465,#205466),
(#205467,#205468),(#205469,#205470),(#205471,#205472),(#205473,#205474),
(#205475,#205476),(#205477,#205478),(#205479,#205480),(#205481,#205482),
(#205483,#205484),(#205485,#205486),(#205487,#205488),(#205489,#205490),
(#205491,#205492),(#205493,#205494),(#205495,#205496),(#205497,#205498),
(#205499,#205500),(#205501,#205502),(#205503,#205504),(#205505,#205506),
(#205507,#205508),(#205509,#205510),(#205511,#205512),(#205513,#205514),
(#205515,#205516),(#205517,#205518),(#205519,#205520),(#205521,#205522),
(#205523,#205524),(#205525,#205526),(#205527,#205528),(#205529,#205530),
(#205531,#205532),(#205533,#205534),(#205535,#205536),(#205537,#205538),
(#205539,#205540),(#205541,#205542),(#205543,#205544),(#205545,#205546),
(#205547,#205548),(#205549,#205550),(#205551,#205552),(#205553,#205554),
(#205555,#205556),(#205557,#205558),(#205559,#205560),(#205561,#205562),
(#205563,#205564),(#205565,#205566),(#205567,#205568),(#205569,#205570),
(#205571,#205572),(#205573,#205574),(#205575,#205576),(#205577,#205578),
(#205579,#205580),(#205581,#205582),(#205583,#205584),(#205585,#205586),
(#205587,#205588),(#205589,#205590),(#205591,#205592),(#205593,#205594),
(#205595,#205596),(#205597,#205598),(#205599,#205600),(#205601,#205602),
(#205603,#205604),(#205605,#205606),(#205607,#205608),(#205609,#205610),
(#205611,#205612),(#205613,#205614),(#205615,#205616),(#205617,#205618),
(#205619,#205620),(#205621,#205622),(#205623,#205624),(#205625,#205626),
(#205627,#205628),(#205629,#205630),(#205631,#205632),(#205633,#205634),
(#205635,#205636),(#205637,#205638),(#205639,#205640),(#205641,#205642),
(#205643,#205644),(#205645,#205646),(#205647,#205648),(#205649,#205650),
(#205651,#205652),(#205653,#205654),(#205655,#205656),(#205657,#205658),
(#205659,#205660),(#205661,#205662),(#205663,#205664),(#205665,#205666),
(#205667,#205668),(#205669,#205670),(#205671,#205672),(#205673,#205674),
(#205675,#205676),(#205677,#205678),(#205679,#205680),(#205681,#205682),
(#205683,#205684),(#205685,#205686),(#205687,#205688),(#205689,#205690),
(#205691,#205692),(#205693,#205694),(#205695,#205696),(#205697,#205698),
(#205699,#205700),(#205701,#205702),(#205703,#205704),(#205705,#205706),
(#205707,#205708),(#205709,#205710),(#205711,#205712),(#205713,#205714),
(#205715,#205716),(#205717,#205718),(#205719,#205720),(#205721,#205722),
(#205723,#205724),(#205725,#205726),(#205727,#205728),(#205729,#205730),
(#205731,#205732),(#205733,#205734),(#205735,#205736),(#205737,#205738),
(#205739,#205740),(#205741,#205742),(#205743,#205744),(#205745,#205746),
(#205747,#205748),(#205749,#205750),(#205751,#205752),(#205753,#205754),
(#205755,#205756),(#205757,#205758),(#205759,#205760),(#205761,#205762),
(#205763,#205764),(#205765,#205766),(#205767,#205768),(#205769,#205770),
(#205771,#205772),(#205773,#205774),(#205775,#205776),(#205777,#205778),
(#205779,#205780),(#205781,#205782),(#205783,#205784),(#205785,#205786),
(#205787,#205788),(#205789,#205790),(#205791,#205792),(#205793,#205794),
(#205795,#205796),(#205797,#205798),(#205799,#205800),(#205801,#205802),
(#205803,#205804),(#205805,#205806),(#205807,#205808),(#205809,#205810),
(#205811,#205812),(#205813,#205814),(#205815,#205816),(#205817,#205818),
(#205819,#205820),(#205821,#205822)),.UNSPECIFIED.,.F.,.F.,.F.)
B_SPLINE_SURFACE_WITH_KNOTS((6,1,1,1,1,1,1,1,1,1,1,1,1,1,1,1,1,1,1,1,1,
1,1,1,1,1,1,1,1,1,1,1,1,1,1,1,1,1,1,1,1,1,1,1,1,1,1,1,1,1,1,1,1,1,1,1,1,
1,1,1,1,1,1,1,1,1,1,1,1,1,1,1,1,1,1,1,1,1,1,1,1,1,1,1,1,1,1,1,1,1,1,1,1,
1,1,1,1,1,1,1,1,1,1,1,1,1,1,1,1,1,1,1,1,1,1,1,1,1,1,1,1,1,1,1,1,1,1,1,1,
1,1,1,1,1,1,1,1,1,1,1,1,1,1,1,1,1,1,1,1,1,1,1,1,1,1,1,1,1,1,1,1,1,1,1,1,
1,1,1,1,1,1,1,1,1,1,1,1,1,1,1,1,1,1,1,1,1,1,1,1,1,1,1,1,1,1,1,1,1,1,1,6),
(2,2),(-1.,-0.995000000000001,-0.990000000000001,-0.985000000000001,-0.980000000000001,
-0.975000000000001,-0.970000000000001,-0.965000000000001,-0.960000000000001,
-0.955000000000001,-0.950000000000001,-0.945000000000001,-0.940000000000001,
-0.935000000000001,-0.930000000000001,-0.925000000000001,-0.920000000000001,
-0.915000000000001,-0.910000000000001,-0.905000000000001,-0.900000000000001,
-0.895000000000001,-0.890000000000001,-0.885000000000001,-0.880000000000001,
-0.875000000000001,-0.870000000000001,-0.865000000000001,-0.860000000000001,
-0.855000000000001,-0.850000000000001,-0.845000000000001,-0.840000000000001,
-0.835000000000001,-0.830000000000001,-0.825000000000001,-0.820000000000001,
-0.815000000000001,-0.810000000000001,-0.805000000000001,-0.800000000000001,
-0.795000000000001,-0.790000000000001,-0.785000000000001,-0.780000000000001,
-0.775000000000001,-0.770000000000001,-0.765000000000001,-0.760000000000001,
-0.755000000000001,-0.750000000000001,-0.745000000000001,-0.740000000000001,
-0.735000000000001,-0.730000000000001,-0.725000000000001,-0.720000000000001,
-0.715000000000001,-0.710000000000001,-0.705000000000001,-0.700000000000001,
-0.695000000000001,-0.690000000000001,-0.685,-0.68,-0.675,-0.67,-0.665,
-0.66,-0.655,-0.65,-0.645,-0.64,-0.635,-0.63,-0.625,-0.62,-0.615,-0.61,
-0.605,-0.6,-0.595,-0.59,-0.585,-0.58,-0.575,-0.57,-0.565,-0.56,-0.555,
-0.55,-0.545,-0.54,-0.535,-0.53,-0.525,-0.52,-0.515,-0.51,-0.505,-0.5,-0.495,
-0.49,-0.485,-0.48,-0.475,-0.47,-0.465,-0.46,-0.455,-0.45,-0.445,-0.44,
-0.435,-0.43,-0.425,-0.42,-0.415,-0.41,-0.405,-0.4,-0.395,-0.39,-0.385,
-0.38,-0.375,-0.37,-0.365,-0.36,-0.355,-0.35,-0.345,-0.34,-0.335,-0.33,
-0.325,-0.32,-0.315,-0.31,-0.305,-0.3,-0.295,-0.29,-0.285,-0.28,-0.275,
-0.27,-0.265,-0.26,-0.255,-0.25,-0.245,-0.24,-0.235,-0.23,-0.225,-0.22,
-0.215,-0.21,-0.205,-0.2,-0.195,-0.19,-0.185,-0.18,-0.175,-0.17,-0.165,
-0.16,-0.155,-0.15,-0.145,-0.14,-0.135,-0.13,-0.125,-0.12,-0.115,-0.11,
-0.105,-0.1,-0.095,-0.09,-0.085,-0.08,-0.075,-0.07,-0.065,-0.06,-0.055,
-0.05,-0.045,-0.04,-0.035,-0.03,-0.025,-0.02,-0.015,-0.01,-0.005,0.),(0.,
1.2),.UNSPECIFIED.)
GEOMETRIC_REPRESENTATION_ITEM()
RATIONAL_B_SPLINE_SURFACE(((1.,1.),(1.,1.),(1.,1.),(1.,1.),(1.,1.),(1.,
1.),(1.,1.),(1.,1.),(1.,1.),(1.,1.),(1.,1.),(1.,1.),(1.,1.),(1.,1.),(1.,
1.),(1.,1.),(1.,1.),(1.,1.),(1.,1.),(1.,1.),(1.,1.),(1.,1.),(1.,1.),(1.,
1.),(1.,1.),(1.,1.),(1.,1.),(1.,1.),(1.,1.),(1.,1.),(1.,1.),(1.,1.),(1.,
1.),(1.,1.),(1.,1.),(1.,1.),(1.,1.),(1.,1.),(1.,1.),(1.,1.),(1.,1.),(1.,
1.),(1.,1.),(1.,1.),(1.,1.),(1.,1.),(1.,1.),(1.,1.),(1.,1.),(1.,1.),(1.,
1.),(1.,1.),(1.,1.),(1.,1.),(1.,1.),(1.,1.),(1.,1.),(1.,1.),(1.,1.),(1.,
1.),(1.,1.),(1.,1.),(1.,1.),(1.,1.),(1.,1.),(1.,1.),(1.,1.),(1.,1.),(1.,
1.),(1.,1.),(1.,1.),(1.,1.),(1.,1.),(1.,1.),(1.,1.),(1.,1.),(1.,1.),(1.,
1.),(1.,1.),(1.,1.),(1.,1.),(1.,1.),(1.,1.),(1.,1.),(1.,1.),(1.,1.),(1.,
1.),(1.,1.),(1.,1.),(1.,1.),(1.,1.),(1.,1.),(1.,1.),(1.,1.),(1.,1.),(1.,
1.),(1.,1.),(1.,1.),(1.,1.),(1.,1.),(1.,1.),(1.,1.),(1.,1.),(1.,1.),(1.,
1.),(1.,1.),(1.,1.),(1.,1.),(1.,1.),(1.,1.),(1.,1.),(1.,1.),(1.,1.),(1.,
1.),(1.,1.),(1.,1.),(1.,1.),(1.,1.),(1.,1.),(1.,1.),(1.,1.),(1.,1.),(1.,
1.),(1.,1.),(1.,1.),(1.,1.),(1.,1.),(1.,1.),(1.,1.),(1.,1.),(1.,1.),(1.,
1.),(1.,1.),(1.,1.),(1.,1.),(1.,1.),(1.,1.),(1.,1.),(1.,1.),(1.,1.),(1.,
1.),(1.,1.),(1.,1.),(1.,1.),(1.,1.),(1.,1.),(1.,1.),(1.,1.),(1.,1.),(1.,
1.),(1.,1.),(1.,1.),(1.,1.),(1.,1.),(1.,1.),(1.,1.),(1.,1.),(1.,1.),(1.,
1.),(1.,1.),(1.,1.),(1.,1.),(1.,1.),(1.,1.),(1.,1.),(1.,1.),(1.,1.),(1.,
1.),(1.,1.),(1.,1.),(1.,1.),(1.,1.),(1.,1.),(1.,1.),(1.,1.),(1.,1.),(1.,
1.),(1.,1.),(1.,1.),(1.,1.),(1.,1.),(1.,1.),(1.,1.),(1.,1.),(1.,1.),(1.,
1.),(1.,1.),(1.,1.),(1.,1.),(1.,1.),(1.,1.),(1.,1.),(1.,1.),(1.,1.),(1.,
1.),(1.,1.),(1.,1.),(1.,1.),(1.,1.),(1.,1.),(1.,1.),(1.,1.),(1.,1.),(1.,
1.),(1.,1.)))
REPRESENTATION_ITEM('')
SURFACE()
);
#1060=(
BOUNDED_SURFACE()
B_SPLINE_SURFACE(5,1,((#206030,#206031),(#206032,#206033),(#206034,#206035),
(#206036,#206037),(#206038,#206039),(#206040,#206041),(#206042,#206043),
(#206044,#206045),(#206046,#206047),(#206048,#206049),(#206050,#206051),
(#206052,#206053),(#206054,#206055),(#206056,#206057),(#206058,#206059),
(#206060,#206061),(#206062,#206063),(#206064,#206065),(#206066,#206067),
(#206068,#206069),(#206070,#206071),(#206072,#206073),(#206074,#206075),
(#206076,#206077),(#206078,#206079),(#206080,#206081),(#206082,#206083),
(#206084,#206085),(#206086,#206087),(#206088,#206089),(#206090,#206091),
(#206092,#206093),(#206094,#206095),(#206096,#206097),(#206098,#206099),
(#206100,#206101),(#206102,#206103),(#206104,#206105),(#206106,#206107),
(#206108,#206109),(#206110,#206111),(#206112,#206113),(#206114,#206115),
(#206116,#206117),(#206118,#206119),(#206120,#206121),(#206122,#206123),
(#206124,#206125),(#206126,#206127),(#206128,#206129),(#206130,#206131),
(#206132,#206133),(#206134,#206135),(#206136,#206137),(#206138,#206139),
(#206140,#206141),(#206142,#206143),(#206144,#206145),(#206146,#206147),
(#206148,#206149),(#206150,#206151),(#206152,#206153),(#206154,#206155),
(#206156,#206157),(#206158,#206159),(#206160,#206161),(#206162,#206163),
(#206164,#206165),(#206166,#206167),(#206168,#206169),(#206170,#206171),
(#206172,#206173),(#206174,#206175),(#206176,#206177),(#206178,#206179),
(#206180,#206181),(#206182,#206183),(#206184,#206185),(#206186,#206187),
(#206188,#206189),(#206190,#206191),(#206192,#206193),(#206194,#206195),
(#206196,#206197),(#206198,#206199),(#206200,#206201),(#206202,#206203),
(#206204,#206205),(#206206,#206207),(#206208,#206209),(#206210,#206211),
(#206212,#206213),(#206214,#206215),(#206216,#206217),(#206218,#206219),
(#206220,#206221),(#206222,#206223),(#206224,#206225),(#206226,#206227),
(#206228,#206229),(#206230,#206231),(#206232,#206233),(#206234,#206235),
(#206236,#206237),(#206238,#206239),(#206240,#206241),(#206242,#206243),
(#206244,#206245),(#206246,#206247),(#206248,#206249),(#206250,#206251),
(#206252,#206253),(#206254,#206255),(#206256,#206257),(#206258,#206259),
(#206260,#206261),(#206262,#206263),(#206264,#206265),(#206266,#206267),
(#206268,#206269),(#206270,#206271),(#206272,#206273),(#206274,#206275),
(#206276,#206277),(#206278,#206279),(#206280,#206281),(#206282,#206283),
(#206284,#206285),(#206286,#206287),(#206288,#206289),(#206290,#206291),
(#206292,#206293),(#206294,#206295),(#206296,#206297),(#206298,#206299),
(#206300,#206301),(#206302,#206303),(#206304,#206305),(#206306,#206307),
(#206308,#206309),(#206310,#206311),(#206312,#206313),(#206314,#206315),
(#206316,#206317),(#206318,#206319),(#206320,#206321),(#206322,#206323),
(#206324,#206325),(#206326,#206327),(#206328,#206329),(#206330,#206331),
(#206332,#206333),(#206334,#206335),(#206336,#206337),(#206338,#206339),
(#206340,#206341),(#206342,#206343),(#206344,#206345),(#206346,#206347),
(#206348,#206349),(#206350,#206351),(#206352,#206353),(#206354,#206355),
(#206356,#206357),(#206358,#206359),(#206360,#206361),(#206362,#206363),
(#206364,#206365),(#206366,#206367),(#206368,#206369),(#206370,#206371),
(#206372,#206373),(#206374,#206375),(#206376,#206377),(#206378,#206379),
(#206380,#206381),(#206382,#206383),(#206384,#206385),(#206386,#206387),
(#206388,#206389),(#206390,#206391),(#206392,#206393),(#206394,#206395),
(#206396,#206397),(#206398,#206399),(#206400,#206401),(#206402,#206403),
(#206404,#206405),(#206406,#206407),(#206408,#206409),(#206410,#206411),
(#206412,#206413),(#206414,#206415),(#206416,#206417),(#206418,#206419),
(#206420,#206421),(#206422,#206423),(#206424,#206425),(#206426,#206427),
(#206428,#206429),(#206430,#206431),(#206432,#206433),(#206434,#206435),
(#206436,#206437),(#206438,#206439)),.UNSPECIFIED.,.F.,.F.,.F.)
B_SPLINE_SURFACE_WITH_KNOTS((6,1,1,1,1,1,1,1,1,1,1,1,1,1,1,1,1,1,1,1,1,
1,1,1,1,1,1,1,1,1,1,1,1,1,1,1,1,1,1,1,1,1,1,1,1,1,1,1,1,1,1,1,1,1,1,1,1,
1,1,1,1,1,1,1,1,1,1,1,1,1,1,1,1,1,1,1,1,1,1,1,1,1,1,1,1,1,1,1,1,1,1,1,1,
1,1,1,1,1,1,1,1,1,1,1,1,1,1,1,1,1,1,1,1,1,1,1,1,1,1,1,1,1,1,1,1,1,1,1,1,
1,1,1,1,1,1,1,1,1,1,1,1,1,1,1,1,1,1,1,1,1,1,1,1,1,1,1,1,1,1,1,1,1,1,1,1,
1,1,1,1,1,1,1,1,1,1,1,1,1,1,1,1,1,1,1,1,1,1,1,1,1,1,1,1,1,1,1,1,1,1,1,6),
(2,2),(0.,0.005,0.01,0.015,0.02,0.025,0.03,0.035,0.04,0.045,0.05,0.055,
0.06,0.065,0.07,0.075,0.08,0.085,0.09,0.095,0.1,0.105,0.11,0.115,0.12,0.125,
0.13,0.135,0.14,0.145,0.15,0.155,0.16,0.165,0.17,0.175,0.18,0.185,0.19,
0.195,0.2,0.205,0.21,0.215,0.22,0.225,0.23,0.235,0.24,0.245,0.25,0.255,
0.26,0.265,0.27,0.275,0.28,0.285,0.29,0.295,0.3,0.305,0.31,0.315,0.32,0.325,
0.33,0.335,0.34,0.345,0.35,0.355,0.36,0.365,0.37,0.375,0.38,0.385,0.39,
0.395,0.4,0.405,0.41,0.415,0.42,0.425,0.43,0.435,0.44,0.445,0.45,0.455,
0.46,0.465,0.47,0.475,0.48,0.485,0.49,0.495,0.5,0.505,0.51,0.515,0.52,0.525,
0.53,0.535,0.54,0.545,0.55,0.555,0.56,0.565,0.57,0.575,0.58,0.585,0.59,
0.595,0.6,0.605,0.61,0.615,0.62,0.625,0.63,0.635,0.64,0.645,0.65,0.655,
0.66,0.665,0.67,0.675,0.68,0.685,0.690000000000001,0.695000000000001,0.700000000000001,
0.705000000000001,0.710000000000001,0.715000000000001,0.720000000000001,
0.725000000000001,0.730000000000001,0.735000000000001,0.740000000000001,
0.745000000000001,0.750000000000001,0.755000000000001,0.760000000000001,
0.765000000000001,0.770000000000001,0.775000000000001,0.780000000000001,
0.785000000000001,0.790000000000001,0.795000000000001,0.800000000000001,
0.805000000000001,0.810000000000001,0.815000000000001,0.820000000000001,
0.825000000000001,0.830000000000001,0.835000000000001,0.840000000000001,
0.845000000000001,0.850000000000001,0.855000000000001,0.860000000000001,
0.865000000000001,0.870000000000001,0.875000000000001,0.880000000000001,
0.885000000000001,0.890000000000001,0.895000000000001,0.900000000000001,
0.905000000000001,0.910000000000001,0.915000000000001,0.920000000000001,
0.925000000000001,0.930000000000001,0.935000000000001,0.940000000000001,
0.945000000000001,0.950000000000001,0.955000000000001,0.960000000000001,
0.965000000000001,0.970000000000001,0.975000000000001,0.980000000000001,
0.985000000000001,0.990000000000001,0.995000000000001,1.),(0.,1.2),
 .UNSPECIFIED.)
GEOMETRIC_REPRESENTATION_ITEM()
RATIONAL_B_SPLINE_SURFACE(((1.,1.),(1.,1.),(1.,1.),(1.,1.),(1.,1.),(1.,
1.),(1.,1.),(1.,1.),(1.,1.),(1.,1.),(1.,1.),(1.,1.),(1.,1.),(1.,1.),(1.,
1.),(1.,1.),(1.,1.),(1.,1.),(1.,1.),(1.,1.),(1.,1.),(1.,1.),(1.,1.),(1.,
1.),(1.,1.),(1.,1.),(1.,1.),(1.,1.),(1.,1.),(1.,1.),(1.,1.),(1.,1.),(1.,
1.),(1.,1.),(1.,1.),(1.,1.),(1.,1.),(1.,1.),(1.,1.),(1.,1.),(1.,1.),(1.,
1.),(1.,1.),(1.,1.),(1.,1.),(1.,1.),(1.,1.),(1.,1.),(1.,1.),(1.,1.),(1.,
1.),(1.,1.),(1.,1.),(1.,1.),(1.,1.),(1.,1.),(1.,1.),(1.,1.),(1.,1.),(1.,
1.),(1.,1.),(1.,1.),(1.,1.),(1.,1.),(1.,1.),(1.,1.),(1.,1.),(1.,1.),(1.,
1.),(1.,1.),(1.,1.),(1.,1.),(1.,1.),(1.,1.),(1.,1.),(1.,1.),(1.,1.),(1.,
1.),(1.,1.),(1.,1.),(1.,1.),(1.,1.),(1.,1.),(1.,1.),(1.,1.),(1.,1.),(1.,
1.),(1.,1.),(1.,1.),(1.,1.),(1.,1.),(1.,1.),(1.,1.),(1.,1.),(1.,1.),(1.,
1.),(1.,1.),(1.,1.),(1.,1.),(1.,1.),(1.,1.),(1.,1.),(1.,1.),(1.,1.),(1.,
1.),(1.,1.),(1.,1.),(1.,1.),(1.,1.),(1.,1.),(1.,1.),(1.,1.),(1.,1.),(1.,
1.),(1.,1.),(1.,1.),(1.,1.),(1.,1.),(1.,1.),(1.,1.),(1.,1.),(1.,1.),(1.,
1.),(1.,1.),(1.,1.),(1.,1.),(1.,1.),(1.,1.),(1.,1.),(1.,1.),(1.,1.),(1.,
1.),(1.,1.),(1.,1.),(1.,1.),(1.,1.),(1.,1.),(1.,1.),(1.,1.),(1.,1.),(1.,
1.),(1.,1.),(1.,1.),(1.,1.),(1.,1.),(1.,1.),(1.,1.),(1.,1.),(1.,1.),(1.,
1.),(1.,1.),(1.,1.),(1.,1.),(1.,1.),(1.,1.),(1.,1.),(1.,1.),(1.,1.),(1.,
1.),(1.,1.),(1.,1.),(1.,1.),(1.,1.),(1.,1.),(1.,1.),(1.,1.),(1.,1.),(1.,
1.),(1.,1.),(1.,1.),(1.,1.),(1.,1.),(1.,1.),(1.,1.),(1.,1.),(1.,1.),(1.,
1.),(1.,1.),(1.,1.),(1.,1.),(1.,1.),(1.,1.),(1.,1.),(1.,1.),(1.,1.),(1.,
1.),(1.,1.),(1.,1.),(1.,1.),(1.,1.),(1.,1.),(1.,1.),(1.,1.),(1.,1.),(1.,
1.),(1.,1.),(1.,1.),(1.,1.),(1.,1.),(1.,1.),(1.,1.),(1.,1.),(1.,1.),(1.,
1.),(1.,1.)))
REPRESENTATION_ITEM('')
SURFACE()
);
#1061=(
BOUNDED_SURFACE()
B_SPLINE_SURFACE(5,1,((#206651,#206652),(#206653,#206654),(#206655,#206656),
(#206657,#206658),(#206659,#206660),(#206661,#206662),(#206663,#206664),
(#206665,#206666),(#206667,#206668),(#206669,#206670),(#206671,#206672),
(#206673,#206674),(#206675,#206676),(#206677,#206678),(#206679,#206680),
(#206681,#206682),(#206683,#206684),(#206685,#206686),(#206687,#206688),
(#206689,#206690),(#206691,#206692),(#206693,#206694),(#206695,#206696),
(#206697,#206698),(#206699,#206700),(#206701,#206702),(#206703,#206704),
(#206705,#206706),(#206707,#206708),(#206709,#206710),(#206711,#206712),
(#206713,#206714),(#206715,#206716),(#206717,#206718),(#206719,#206720),
(#206721,#206722),(#206723,#206724),(#206725,#206726),(#206727,#206728),
(#206729,#206730),(#206731,#206732),(#206733,#206734),(#206735,#206736),
(#206737,#206738),(#206739,#206740),(#206741,#206742),(#206743,#206744),
(#206745,#206746),(#206747,#206748),(#206749,#206750),(#206751,#206752),
(#206753,#206754),(#206755,#206756),(#206757,#206758),(#206759,#206760),
(#206761,#206762),(#206763,#206764),(#206765,#206766),(#206767,#206768),
(#206769,#206770),(#206771,#206772),(#206773,#206774),(#206775,#206776),
(#206777,#206778),(#206779,#206780),(#206781,#206782),(#206783,#206784),
(#206785,#206786),(#206787,#206788),(#206789,#206790),(#206791,#206792),
(#206793,#206794),(#206795,#206796),(#206797,#206798),(#206799,#206800),
(#206801,#206802),(#206803,#206804),(#206805,#206806),(#206807,#206808),
(#206809,#206810),(#206811,#206812),(#206813,#206814),(#206815,#206816),
(#206817,#206818),(#206819,#206820),(#206821,#206822),(#206823,#206824),
(#206825,#206826),(#206827,#206828),(#206829,#206830),(#206831,#206832),
(#206833,#206834),(#206835,#206836),(#206837,#206838),(#206839,#206840),
(#206841,#206842),(#206843,#206844),(#206845,#206846),(#206847,#206848),
(#206849,#206850),(#206851,#206852),(#206853,#206854),(#206855,#206856),
(#206857,#206858),(#206859,#206860),(#206861,#206862),(#206863,#206864),
(#206865,#206866),(#206867,#206868),(#206869,#206870),(#206871,#206872),
(#206873,#206874),(#206875,#206876),(#206877,#206878),(#206879,#206880),
(#206881,#206882),(#206883,#206884),(#206885,#206886),(#206887,#206888),
(#206889,#206890),(#206891,#206892),(#206893,#206894),(#206895,#206896),
(#206897,#206898),(#206899,#206900),(#206901,#206902),(#206903,#206904),
(#206905,#206906),(#206907,#206908),(#206909,#206910),(#206911,#206912),
(#206913,#206914),(#206915,#206916),(#206917,#206918),(#206919,#206920),
(#206921,#206922),(#206923,#206924),(#206925,#206926),(#206927,#206928),
(#206929,#206930),(#206931,#206932),(#206933,#206934),(#206935,#206936),
(#206937,#206938),(#206939,#206940),(#206941,#206942),(#206943,#206944),
(#206945,#206946),(#206947,#206948),(#206949,#206950),(#206951,#206952),
(#206953,#206954),(#206955,#206956),(#206957,#206958),(#206959,#206960),
(#206961,#206962),(#206963,#206964),(#206965,#206966),(#206967,#206968),
(#206969,#206970),(#206971,#206972),(#206973,#206974),(#206975,#206976),
(#206977,#206978),(#206979,#206980),(#206981,#206982),(#206983,#206984),
(#206985,#206986),(#206987,#206988),(#206989,#206990),(#206991,#206992),
(#206993,#206994),(#206995,#206996),(#206997,#206998),(#206999,#207000),
(#207001,#207002),(#207003,#207004),(#207005,#207006),(#207007,#207008),
(#207009,#207010),(#207011,#207012),(#207013,#207014),(#207015,#207016),
(#207017,#207018),(#207019,#207020),(#207021,#207022),(#207023,#207024),
(#207025,#207026),(#207027,#207028),(#207029,#207030),(#207031,#207032),
(#207033,#207034),(#207035,#207036),(#207037,#207038),(#207039,#207040),
(#207041,#207042),(#207043,#207044),(#207045,#207046),(#207047,#207048),
(#207049,#207050),(#207051,#207052),(#207053,#207054),(#207055,#207056),
(#207057,#207058),(#207059,#207060)),.UNSPECIFIED.,.F.,.F.,.F.)
B_SPLINE_SURFACE_WITH_KNOTS((6,1,1,1,1,1,1,1,1,1,1,1,1,1,1,1,1,1,1,1,1,
1,1,1,1,1,1,1,1,1,1,1,1,1,1,1,1,1,1,1,1,1,1,1,1,1,1,1,1,1,1,1,1,1,1,1,1,
1,1,1,1,1,1,1,1,1,1,1,1,1,1,1,1,1,1,1,1,1,1,1,1,1,1,1,1,1,1,1,1,1,1,1,1,
1,1,1,1,1,1,1,1,1,1,1,1,1,1,1,1,1,1,1,1,1,1,1,1,1,1,1,1,1,1,1,1,1,1,1,1,
1,1,1,1,1,1,1,1,1,1,1,1,1,1,1,1,1,1,1,1,1,1,1,1,1,1,1,1,1,1,1,1,1,1,1,1,
1,1,1,1,1,1,1,1,1,1,1,1,1,1,1,1,1,1,1,1,1,1,1,1,1,1,1,1,1,1,1,1,1,1,1,6),
(2,2),(-1.,-0.995000000000001,-0.990000000000001,-0.985000000000001,-0.980000000000001,
-0.975000000000001,-0.970000000000001,-0.965000000000001,-0.960000000000001,
-0.955000000000001,-0.950000000000001,-0.945000000000001,-0.940000000000001,
-0.935000000000001,-0.930000000000001,-0.925000000000001,-0.920000000000001,
-0.915000000000001,-0.910000000000001,-0.905000000000001,-0.900000000000001,
-0.895000000000001,-0.890000000000001,-0.885000000000001,-0.880000000000001,
-0.875000000000001,-0.870000000000001,-0.865000000000001,-0.860000000000001,
-0.855000000000001,-0.850000000000001,-0.845000000000001,-0.840000000000001,
-0.835000000000001,-0.830000000000001,-0.825000000000001,-0.820000000000001,
-0.815000000000001,-0.810000000000001,-0.805000000000001,-0.800000000000001,
-0.795000000000001,-0.790000000000001,-0.785000000000001,-0.780000000000001,
-0.775000000000001,-0.770000000000001,-0.765000000000001,-0.760000000000001,
-0.755000000000001,-0.750000000000001,-0.745000000000001,-0.740000000000001,
-0.735000000000001,-0.730000000000001,-0.725000000000001,-0.720000000000001,
-0.715000000000001,-0.710000000000001,-0.705000000000001,-0.700000000000001,
-0.695000000000001,-0.690000000000001,-0.685,-0.68,-0.675,-0.67,-0.665,
-0.66,-0.655,-0.65,-0.645,-0.64,-0.635,-0.63,-0.625,-0.62,-0.615,-0.61,
-0.605,-0.6,-0.595,-0.59,-0.585,-0.58,-0.575,-0.57,-0.565,-0.56,-0.555,
-0.55,-0.545,-0.54,-0.535,-0.53,-0.525,-0.52,-0.515,-0.51,-0.505,-0.5,-0.495,
-0.49,-0.485,-0.48,-0.475,-0.47,-0.465,-0.46,-0.455,-0.45,-0.445,-0.44,
-0.435,-0.43,-0.425,-0.42,-0.415,-0.41,-0.405,-0.4,-0.395,-0.39,-0.385,
-0.38,-0.375,-0.37,-0.365,-0.36,-0.355,-0.35,-0.345,-0.34,-0.335,-0.33,
-0.325,-0.32,-0.315,-0.31,-0.305,-0.3,-0.295,-0.29,-0.285,-0.28,-0.275,
-0.27,-0.265,-0.26,-0.255,-0.25,-0.245,-0.24,-0.235,-0.23,-0.225,-0.22,
-0.215,-0.21,-0.205,-0.2,-0.195,-0.19,-0.185,-0.18,-0.175,-0.17,-0.165,
-0.16,-0.155,-0.15,-0.145,-0.14,-0.135,-0.13,-0.125,-0.12,-0.115,-0.11,
-0.105,-0.1,-0.095,-0.09,-0.085,-0.08,-0.075,-0.07,-0.065,-0.06,-0.055,
-0.05,-0.045,-0.04,-0.035,-0.03,-0.025,-0.02,-0.015,-0.01,-0.005,0.),(0.,
1.2),.UNSPECIFIED.)
GEOMETRIC_REPRESENTATION_ITEM()
RATIONAL_B_SPLINE_SURFACE(((1.,1.),(1.,1.),(1.,1.),(1.,1.),(1.,1.),(1.,
1.),(1.,1.),(1.,1.),(1.,1.),(1.,1.),(1.,1.),(1.,1.),(1.,1.),(1.,1.),(1.,
1.),(1.,1.),(1.,1.),(1.,1.),(1.,1.),(1.,1.),(1.,1.),(1.,1.),(1.,1.),(1.,
1.),(1.,1.),(1.,1.),(1.,1.),(1.,1.),(1.,1.),(1.,1.),(1.,1.),(1.,1.),(1.,
1.),(1.,1.),(1.,1.),(1.,1.),(1.,1.),(1.,1.),(1.,1.),(1.,1.),(1.,1.),(1.,
1.),(1.,1.),(1.,1.),(1.,1.),(1.,1.),(1.,1.),(1.,1.),(1.,1.),(1.,1.),(1.,
1.),(1.,1.),(1.,1.),(1.,1.),(1.,1.),(1.,1.),(1.,1.),(1.,1.),(1.,1.),(1.,
1.),(1.,1.),(1.,1.),(1.,1.),(1.,1.),(1.,1.),(1.,1.),(1.,1.),(1.,1.),(1.,
1.),(1.,1.),(1.,1.),(1.,1.),(1.,1.),(1.,1.),(1.,1.),(1.,1.),(1.,1.),(1.,
1.),(1.,1.),(1.,1.),(1.,1.),(1.,1.),(1.,1.),(1.,1.),(1.,1.),(1.,1.),(1.,
1.),(1.,1.),(1.,1.),(1.,1.),(1.,1.),(1.,1.),(1.,1.),(1.,1.),(1.,1.),(1.,
1.),(1.,1.),(1.,1.),(1.,1.),(1.,1.),(1.,1.),(1.,1.),(1.,1.),(1.,1.),(1.,
1.),(1.,1.),(1.,1.),(1.,1.),(1.,1.),(1.,1.),(1.,1.),(1.,1.),(1.,1.),(1.,
1.),(1.,1.),(1.,1.),(1.,1.),(1.,1.),(1.,1.),(1.,1.),(1.,1.),(1.,1.),(1.,
1.),(1.,1.),(1.,1.),(1.,1.),(1.,1.),(1.,1.),(1.,1.),(1.,1.),(1.,1.),(1.,
1.),(1.,1.),(1.,1.),(1.,1.),(1.,1.),(1.,1.),(1.,1.),(1.,1.),(1.,1.),(1.,
1.),(1.,1.),(1.,1.),(1.,1.),(1.,1.),(1.,1.),(1.,1.),(1.,1.),(1.,1.),(1.,
1.),(1.,1.),(1.,1.),(1.,1.),(1.,1.),(1.,1.),(1.,1.),(1.,1.),(1.,1.),(1.,
1.),(1.,1.),(1.,1.),(1.,1.),(1.,1.),(1.,1.),(1.,1.),(1.,1.),(1.,1.),(1.,
1.),(1.,1.),(1.,1.),(1.,1.),(1.,1.),(1.,1.),(1.,1.),(1.,1.),(1.,1.),(1.,
1.),(1.,1.),(1.,1.),(1.,1.),(1.,1.),(1.,1.),(1.,1.),(1.,1.),(1.,1.),(1.,
1.),(1.,1.),(1.,1.),(1.,1.),(1.,1.),(1.,1.),(1.,1.),(1.,1.),(1.,1.),(1.,
1.),(1.,1.),(1.,1.),(1.,1.),(1.,1.),(1.,1.),(1.,1.),(1.,1.),(1.,1.),(1.,
1.),(1.,1.)))
REPRESENTATION_ITEM('')
SURFACE()
);
#1062=(
BOUNDED_SURFACE()
B_SPLINE_SURFACE(5,1,((#207268,#207269),(#207270,#207271),(#207272,#207273),
(#207274,#207275),(#207276,#207277),(#207278,#207279),(#207280,#207281),
(#207282,#207283),(#207284,#207285),(#207286,#207287),(#207288,#207289),
(#207290,#207291),(#207292,#207293),(#207294,#207295),(#207296,#207297),
(#207298,#207299),(#207300,#207301),(#207302,#207303),(#207304,#207305),
(#207306,#207307),(#207308,#207309),(#207310,#207311),(#207312,#207313),
(#207314,#207315),(#207316,#207317),(#207318,#207319),(#207320,#207321),
(#207322,#207323),(#207324,#207325),(#207326,#207327),(#207328,#207329),
(#207330,#207331),(#207332,#207333),(#207334,#207335),(#207336,#207337),
(#207338,#207339),(#207340,#207341),(#207342,#207343),(#207344,#207345),
(#207346,#207347),(#207348,#207349),(#207350,#207351),(#207352,#207353),
(#207354,#207355),(#207356,#207357),(#207358,#207359),(#207360,#207361),
(#207362,#207363),(#207364,#207365),(#207366,#207367),(#207368,#207369),
(#207370,#207371),(#207372,#207373),(#207374,#207375),(#207376,#207377),
(#207378,#207379),(#207380,#207381),(#207382,#207383),(#207384,#207385),
(#207386,#207387),(#207388,#207389),(#207390,#207391),(#207392,#207393),
(#207394,#207395),(#207396,#207397),(#207398,#207399),(#207400,#207401),
(#207402,#207403),(#207404,#207405),(#207406,#207407),(#207408,#207409),
(#207410,#207411),(#207412,#207413),(#207414,#207415),(#207416,#207417),
(#207418,#207419),(#207420,#207421),(#207422,#207423),(#207424,#207425),
(#207426,#207427),(#207428,#207429),(#207430,#207431),(#207432,#207433),
(#207434,#207435),(#207436,#207437),(#207438,#207439),(#207440,#207441),
(#207442,#207443),(#207444,#207445),(#207446,#207447),(#207448,#207449),
(#207450,#207451),(#207452,#207453),(#207454,#207455),(#207456,#207457),
(#207458,#207459),(#207460,#207461),(#207462,#207463),(#207464,#207465),
(#207466,#207467),(#207468,#207469),(#207470,#207471),(#207472,#207473),
(#207474,#207475),(#207476,#207477),(#207478,#207479),(#207480,#207481),
(#207482,#207483),(#207484,#207485),(#207486,#207487),(#207488,#207489),
(#207490,#207491),(#207492,#207493),(#207494,#207495),(#207496,#207497),
(#207498,#207499),(#207500,#207501),(#207502,#207503),(#207504,#207505),
(#207506,#207507),(#207508,#207509),(#207510,#207511),(#207512,#207513),
(#207514,#207515),(#207516,#207517),(#207518,#207519),(#207520,#207521),
(#207522,#207523),(#207524,#207525),(#207526,#207527),(#207528,#207529),
(#207530,#207531),(#207532,#207533),(#207534,#207535),(#207536,#207537),
(#207538,#207539),(#207540,#207541),(#207542,#207543),(#207544,#207545),
(#207546,#207547),(#207548,#207549),(#207550,#207551),(#207552,#207553),
(#207554,#207555),(#207556,#207557),(#207558,#207559),(#207560,#207561),
(#207562,#207563),(#207564,#207565),(#207566,#207567),(#207568,#207569),
(#207570,#207571),(#207572,#207573),(#207574,#207575),(#207576,#207577),
(#207578,#207579),(#207580,#207581),(#207582,#207583),(#207584,#207585),
(#207586,#207587),(#207588,#207589),(#207590,#207591),(#207592,#207593),
(#207594,#207595),(#207596,#207597),(#207598,#207599),(#207600,#207601),
(#207602,#207603),(#207604,#207605),(#207606,#207607),(#207608,#207609),
(#207610,#207611),(#207612,#207613),(#207614,#207615),(#207616,#207617),
(#207618,#207619),(#207620,#207621),(#207622,#207623),(#207624,#207625),
(#207626,#207627),(#207628,#207629),(#207630,#207631),(#207632,#207633),
(#207634,#207635),(#207636,#207637),(#207638,#207639),(#207640,#207641),
(#207642,#207643),(#207644,#207645),(#207646,#207647),(#207648,#207649),
(#207650,#207651),(#207652,#207653),(#207654,#207655),(#207656,#207657),
(#207658,#207659),(#207660,#207661),(#207662,#207663),(#207664,#207665),
(#207666,#207667),(#207668,#207669),(#207670,#207671),(#207672,#207673),
(#207674,#207675),(#207676,#207677)),.UNSPECIFIED.,.F.,.F.,.F.)
B_SPLINE_SURFACE_WITH_KNOTS((6,1,1,1,1,1,1,1,1,1,1,1,1,1,1,1,1,1,1,1,1,
1,1,1,1,1,1,1,1,1,1,1,1,1,1,1,1,1,1,1,1,1,1,1,1,1,1,1,1,1,1,1,1,1,1,1,1,
1,1,1,1,1,1,1,1,1,1,1,1,1,1,1,1,1,1,1,1,1,1,1,1,1,1,1,1,1,1,1,1,1,1,1,1,
1,1,1,1,1,1,1,1,1,1,1,1,1,1,1,1,1,1,1,1,1,1,1,1,1,1,1,1,1,1,1,1,1,1,1,1,
1,1,1,1,1,1,1,1,1,1,1,1,1,1,1,1,1,1,1,1,1,1,1,1,1,1,1,1,1,1,1,1,1,1,1,1,
1,1,1,1,1,1,1,1,1,1,1,1,1,1,1,1,1,1,1,1,1,1,1,1,1,1,1,1,1,1,1,1,1,1,1,6),
(2,2),(0.,0.005,0.01,0.015,0.02,0.025,0.03,0.035,0.04,0.045,0.05,0.055,
0.06,0.065,0.07,0.075,0.08,0.085,0.09,0.095,0.1,0.105,0.11,0.115,0.12,0.125,
0.13,0.135,0.14,0.145,0.15,0.155,0.16,0.165,0.17,0.175,0.18,0.185,0.19,
0.195,0.2,0.205,0.21,0.215,0.22,0.225,0.23,0.235,0.24,0.245,0.25,0.255,
0.26,0.265,0.27,0.275,0.28,0.285,0.29,0.295,0.3,0.305,0.31,0.315,0.32,0.325,
0.33,0.335,0.34,0.345,0.35,0.355,0.36,0.365,0.37,0.375,0.38,0.385,0.39,
0.395,0.4,0.405,0.41,0.415,0.42,0.425,0.43,0.435,0.44,0.445,0.45,0.455,
0.46,0.465,0.47,0.475,0.48,0.485,0.49,0.495,0.5,0.505,0.51,0.515,0.52,0.525,
0.53,0.535,0.54,0.545,0.55,0.555,0.56,0.565,0.57,0.575,0.58,0.585,0.59,
0.595,0.6,0.605,0.61,0.615,0.62,0.625,0.63,0.635,0.64,0.645,0.65,0.655,
0.66,0.665,0.67,0.675,0.68,0.685,0.690000000000001,0.695000000000001,0.700000000000001,
0.705000000000001,0.710000000000001,0.715000000000001,0.720000000000001,
0.725000000000001,0.730000000000001,0.735000000000001,0.740000000000001,
0.745000000000001,0.750000000000001,0.755000000000001,0.760000000000001,
0.765000000000001,0.770000000000001,0.775000000000001,0.780000000000001,
0.785000000000001,0.790000000000001,0.795000000000001,0.800000000000001,
0.805000000000001,0.810000000000001,0.815000000000001,0.820000000000001,
0.825000000000001,0.830000000000001,0.835000000000001,0.840000000000001,
0.845000000000001,0.850000000000001,0.855000000000001,0.860000000000001,
0.865000000000001,0.870000000000001,0.875000000000001,0.880000000000001,
0.885000000000001,0.890000000000001,0.895000000000001,0.900000000000001,
0.905000000000001,0.910000000000001,0.915000000000001,0.920000000000001,
0.925000000000001,0.930000000000001,0.935000000000001,0.940000000000001,
0.945000000000001,0.950000000000001,0.955000000000001,0.960000000000001,
0.965000000000001,0.970000000000001,0.975000000000001,0.980000000000001,
0.985000000000001,0.990000000000001,0.995000000000001,1.),(0.,1.2),
 .UNSPECIFIED.)
GEOMETRIC_REPRESENTATION_ITEM()
RATIONAL_B_SPLINE_SURFACE(((1.,1.),(1.,1.),(1.,1.),(1.,1.),(1.,1.),(1.,
1.),(1.,1.),(1.,1.),(1.,1.),(1.,1.),(1.,1.),(1.,1.),(1.,1.),(1.,1.),(1.,
1.),(1.,1.),(1.,1.),(1.,1.),(1.,1.),(1.,1.),(1.,1.),(1.,1.),(1.,1.),(1.,
1.),(1.,1.),(1.,1.),(1.,1.),(1.,1.),(1.,1.),(1.,1.),(1.,1.),(1.,1.),(1.,
1.),(1.,1.),(1.,1.),(1.,1.),(1.,1.),(1.,1.),(1.,1.),(1.,1.),(1.,1.),(1.,
1.),(1.,1.),(1.,1.),(1.,1.),(1.,1.),(1.,1.),(1.,1.),(1.,1.),(1.,1.),(1.,
1.),(1.,1.),(1.,1.),(1.,1.),(1.,1.),(1.,1.),(1.,1.),(1.,1.),(1.,1.),(1.,
1.),(1.,1.),(1.,1.),(1.,1.),(1.,1.),(1.,1.),(1.,1.),(1.,1.),(1.,1.),(1.,
1.),(1.,1.),(1.,1.),(1.,1.),(1.,1.),(1.,1.),(1.,1.),(1.,1.),(1.,1.),(1.,
1.),(1.,1.),(1.,1.),(1.,1.),(1.,1.),(1.,1.),(1.,1.),(1.,1.),(1.,1.),(1.,
1.),(1.,1.),(1.,1.),(1.,1.),(1.,1.),(1.,1.),(1.,1.),(1.,1.),(1.,1.),(1.,
1.),(1.,1.),(1.,1.),(1.,1.),(1.,1.),(1.,1.),(1.,1.),(1.,1.),(1.,1.),(1.,
1.),(1.,1.),(1.,1.),(1.,1.),(1.,1.),(1.,1.),(1.,1.),(1.,1.),(1.,1.),(1.,
1.),(1.,1.),(1.,1.),(1.,1.),(1.,1.),(1.,1.),(1.,1.),(1.,1.),(1.,1.),(1.,
1.),(1.,1.),(1.,1.),(1.,1.),(1.,1.),(1.,1.),(1.,1.),(1.,1.),(1.,1.),(1.,
1.),(1.,1.),(1.,1.),(1.,1.),(1.,1.),(1.,1.),(1.,1.),(1.,1.),(1.,1.),(1.,
1.),(1.,1.),(1.,1.),(1.,1.),(1.,1.),(1.,1.),(1.,1.),(1.,1.),(1.,1.),(1.,
1.),(1.,1.),(1.,1.),(1.,1.),(1.,1.),(1.,1.),(1.,1.),(1.,1.),(1.,1.),(1.,
1.),(1.,1.),(1.,1.),(1.,1.),(1.,1.),(1.,1.),(1.,1.),(1.,1.),(1.,1.),(1.,
1.),(1.,1.),(1.,1.),(1.,1.),(1.,1.),(1.,1.),(1.,1.),(1.,1.),(1.,1.),(1.,
1.),(1.,1.),(1.,1.),(1.,1.),(1.,1.),(1.,1.),(1.,1.),(1.,1.),(1.,1.),(1.,
1.),(1.,1.),(1.,1.),(1.,1.),(1.,1.),(1.,1.),(1.,1.),(1.,1.),(1.,1.),(1.,
1.),(1.,1.),(1.,1.),(1.,1.),(1.,1.),(1.,1.),(1.,1.),(1.,1.),(1.,1.),(1.,
1.),(1.,1.)))
REPRESENTATION_ITEM('')
SURFACE()
);
#1063=(
BOUNDED_SURFACE()
B_SPLINE_SURFACE(5,1,((#207889,#207890),(#207891,#207892),(#207893,#207894),
(#207895,#207896),(#207897,#207898),(#207899,#207900),(#207901,#207902),
(#207903,#207904),(#207905,#207906),(#207907,#207908),(#207909,#207910),
(#207911,#207912),(#207913,#207914),(#207915,#207916),(#207917,#207918),
(#207919,#207920),(#207921,#207922),(#207923,#207924),(#207925,#207926),
(#207927,#207928),(#207929,#207930),(#207931,#207932),(#207933,#207934),
(#207935,#207936),(#207937,#207938),(#207939,#207940),(#207941,#207942),
(#207943,#207944),(#207945,#207946),(#207947,#207948),(#207949,#207950),
(#207951,#207952),(#207953,#207954),(#207955,#207956),(#207957,#207958),
(#207959,#207960),(#207961,#207962),(#207963,#207964),(#207965,#207966),
(#207967,#207968),(#207969,#207970),(#207971,#207972),(#207973,#207974),
(#207975,#207976),(#207977,#207978),(#207979,#207980),(#207981,#207982),
(#207983,#207984),(#207985,#207986),(#207987,#207988),(#207989,#207990),
(#207991,#207992),(#207993,#207994),(#207995,#207996),(#207997,#207998),
(#207999,#208000),(#208001,#208002),(#208003,#208004),(#208005,#208006),
(#208007,#208008),(#208009,#208010),(#208011,#208012),(#208013,#208014),
(#208015,#208016),(#208017,#208018),(#208019,#208020),(#208021,#208022),
(#208023,#208024),(#208025,#208026),(#208027,#208028),(#208029,#208030),
(#208031,#208032),(#208033,#208034),(#208035,#208036),(#208037,#208038),
(#208039,#208040),(#208041,#208042),(#208043,#208044),(#208045,#208046),
(#208047,#208048),(#208049,#208050),(#208051,#208052),(#208053,#208054),
(#208055,#208056),(#208057,#208058),(#208059,#208060),(#208061,#208062),
(#208063,#208064),(#208065,#208066),(#208067,#208068),(#208069,#208070),
(#208071,#208072),(#208073,#208074),(#208075,#208076),(#208077,#208078),
(#208079,#208080),(#208081,#208082),(#208083,#208084),(#208085,#208086),
(#208087,#208088),(#208089,#208090),(#208091,#208092),(#208093,#208094),
(#208095,#208096),(#208097,#208098),(#208099,#208100),(#208101,#208102),
(#208103,#208104),(#208105,#208106),(#208107,#208108),(#208109,#208110),
(#208111,#208112),(#208113,#208114),(#208115,#208116),(#208117,#208118),
(#208119,#208120),(#208121,#208122),(#208123,#208124),(#208125,#208126),
(#208127,#208128),(#208129,#208130),(#208131,#208132),(#208133,#208134),
(#208135,#208136),(#208137,#208138),(#208139,#208140),(#208141,#208142),
(#208143,#208144),(#208145,#208146),(#208147,#208148),(#208149,#208150),
(#208151,#208152),(#208153,#208154),(#208155,#208156),(#208157,#208158),
(#208159,#208160),(#208161,#208162),(#208163,#208164),(#208165,#208166),
(#208167,#208168),(#208169,#208170),(#208171,#208172),(#208173,#208174),
(#208175,#208176),(#208177,#208178),(#208179,#208180),(#208181,#208182),
(#208183,#208184),(#208185,#208186),(#208187,#208188),(#208189,#208190),
(#208191,#208192),(#208193,#208194),(#208195,#208196),(#208197,#208198),
(#208199,#208200),(#208201,#208202),(#208203,#208204),(#208205,#208206),
(#208207,#208208),(#208209,#208210),(#208211,#208212),(#208213,#208214),
(#208215,#208216),(#208217,#208218),(#208219,#208220),(#208221,#208222),
(#208223,#208224),(#208225,#208226),(#208227,#208228),(#208229,#208230),
(#208231,#208232),(#208233,#208234),(#208235,#208236),(#208237,#208238),
(#208239,#208240),(#208241,#208242),(#208243,#208244),(#208245,#208246),
(#208247,#208248),(#208249,#208250),(#208251,#208252),(#208253,#208254),
(#208255,#208256),(#208257,#208258),(#208259,#208260),(#208261,#208262),
(#208263,#208264),(#208265,#208266),(#208267,#208268),(#208269,#208270),
(#208271,#208272),(#208273,#208274),(#208275,#208276),(#208277,#208278),
(#208279,#208280),(#208281,#208282),(#208283,#208284),(#208285,#208286),
(#208287,#208288),(#208289,#208290),(#208291,#208292),(#208293,#208294),
(#208295,#208296),(#208297,#208298)),.UNSPECIFIED.,.F.,.F.,.F.)
B_SPLINE_SURFACE_WITH_KNOTS((6,1,1,1,1,1,1,1,1,1,1,1,1,1,1,1,1,1,1,1,1,
1,1,1,1,1,1,1,1,1,1,1,1,1,1,1,1,1,1,1,1,1,1,1,1,1,1,1,1,1,1,1,1,1,1,1,1,
1,1,1,1,1,1,1,1,1,1,1,1,1,1,1,1,1,1,1,1,1,1,1,1,1,1,1,1,1,1,1,1,1,1,1,1,
1,1,1,1,1,1,1,1,1,1,1,1,1,1,1,1,1,1,1,1,1,1,1,1,1,1,1,1,1,1,1,1,1,1,1,1,
1,1,1,1,1,1,1,1,1,1,1,1,1,1,1,1,1,1,1,1,1,1,1,1,1,1,1,1,1,1,1,1,1,1,1,1,
1,1,1,1,1,1,1,1,1,1,1,1,1,1,1,1,1,1,1,1,1,1,1,1,1,1,1,1,1,1,1,1,1,1,1,6),
(2,2),(-1.,-0.995000000000001,-0.990000000000001,-0.985000000000001,-0.980000000000001,
-0.975000000000001,-0.970000000000001,-0.965000000000001,-0.960000000000001,
-0.955000000000001,-0.950000000000001,-0.945000000000001,-0.940000000000001,
-0.935000000000001,-0.930000000000001,-0.925000000000001,-0.920000000000001,
-0.915000000000001,-0.910000000000001,-0.905000000000001,-0.900000000000001,
-0.895000000000001,-0.890000000000001,-0.885000000000001,-0.880000000000001,
-0.875000000000001,-0.870000000000001,-0.865000000000001,-0.860000000000001,
-0.855000000000001,-0.850000000000001,-0.845000000000001,-0.840000000000001,
-0.835000000000001,-0.830000000000001,-0.825000000000001,-0.820000000000001,
-0.815000000000001,-0.810000000000001,-0.805000000000001,-0.800000000000001,
-0.795000000000001,-0.790000000000001,-0.785000000000001,-0.780000000000001,
-0.775000000000001,-0.770000000000001,-0.765000000000001,-0.760000000000001,
-0.755000000000001,-0.750000000000001,-0.745000000000001,-0.740000000000001,
-0.735000000000001,-0.730000000000001,-0.725000000000001,-0.720000000000001,
-0.715000000000001,-0.710000000000001,-0.705000000000001,-0.700000000000001,
-0.695000000000001,-0.690000000000001,-0.685,-0.68,-0.675,-0.67,-0.665,
-0.66,-0.655,-0.65,-0.645,-0.64,-0.635,-0.63,-0.625,-0.62,-0.615,-0.61,
-0.605,-0.6,-0.595,-0.59,-0.585,-0.58,-0.575,-0.57,-0.565,-0.56,-0.555,
-0.55,-0.545,-0.54,-0.535,-0.53,-0.525,-0.52,-0.515,-0.51,-0.505,-0.5,-0.495,
-0.49,-0.485,-0.48,-0.475,-0.47,-0.465,-0.46,-0.455,-0.45,-0.445,-0.44,
-0.435,-0.43,-0.425,-0.42,-0.415,-0.41,-0.405,-0.4,-0.395,-0.39,-0.385,
-0.38,-0.375,-0.37,-0.365,-0.36,-0.355,-0.35,-0.345,-0.34,-0.335,-0.33,
-0.325,-0.32,-0.315,-0.31,-0.305,-0.3,-0.295,-0.29,-0.285,-0.28,-0.275,
-0.27,-0.265,-0.26,-0.255,-0.25,-0.245,-0.24,-0.235,-0.23,-0.225,-0.22,
-0.215,-0.21,-0.205,-0.2,-0.195,-0.19,-0.185,-0.18,-0.175,-0.17,-0.165,
-0.16,-0.155,-0.15,-0.145,-0.14,-0.135,-0.13,-0.125,-0.12,-0.115,-0.11,
-0.105,-0.1,-0.095,-0.09,-0.085,-0.08,-0.075,-0.07,-0.065,-0.06,-0.055,
-0.05,-0.045,-0.04,-0.035,-0.03,-0.025,-0.02,-0.015,-0.01,-0.005,0.),(0.,
1.2),.UNSPECIFIED.)
GEOMETRIC_REPRESENTATION_ITEM()
RATIONAL_B_SPLINE_SURFACE(((1.,1.),(1.,1.),(1.,1.),(1.,1.),(1.,1.),(1.,
1.),(1.,1.),(1.,1.),(1.,1.),(1.,1.),(1.,1.),(1.,1.),(1.,1.),(1.,1.),(1.,
1.),(1.,1.),(1.,1.),(1.,1.),(1.,1.),(1.,1.),(1.,1.),(1.,1.),(1.,1.),(1.,
1.),(1.,1.),(1.,1.),(1.,1.),(1.,1.),(1.,1.),(1.,1.),(1.,1.),(1.,1.),(1.,
1.),(1.,1.),(1.,1.),(1.,1.),(1.,1.),(1.,1.),(1.,1.),(1.,1.),(1.,1.),(1.,
1.),(1.,1.),(1.,1.),(1.,1.),(1.,1.),(1.,1.),(1.,1.),(1.,1.),(1.,1.),(1.,
1.),(1.,1.),(1.,1.),(1.,1.),(1.,1.),(1.,1.),(1.,1.),(1.,1.),(1.,1.),(1.,
1.),(1.,1.),(1.,1.),(1.,1.),(1.,1.),(1.,1.),(1.,1.),(1.,1.),(1.,1.),(1.,
1.),(1.,1.),(1.,1.),(1.,1.),(1.,1.),(1.,1.),(1.,1.),(1.,1.),(1.,1.),(1.,
1.),(1.,1.),(1.,1.),(1.,1.),(1.,1.),(1.,1.),(1.,1.),(1.,1.),(1.,1.),(1.,
1.),(1.,1.),(1.,1.),(1.,1.),(1.,1.),(1.,1.),(1.,1.),(1.,1.),(1.,1.),(1.,
1.),(1.,1.),(1.,1.),(1.,1.),(1.,1.),(1.,1.),(1.,1.),(1.,1.),(1.,1.),(1.,
1.),(1.,1.),(1.,1.),(1.,1.),(1.,1.),(1.,1.),(1.,1.),(1.,1.),(1.,1.),(1.,
1.),(1.,1.),(1.,1.),(1.,1.),(1.,1.),(1.,1.),(1.,1.),(1.,1.),(1.,1.),(1.,
1.),(1.,1.),(1.,1.),(1.,1.),(1.,1.),(1.,1.),(1.,1.),(1.,1.),(1.,1.),(1.,
1.),(1.,1.),(1.,1.),(1.,1.),(1.,1.),(1.,1.),(1.,1.),(1.,1.),(1.,1.),(1.,
1.),(1.,1.),(1.,1.),(1.,1.),(1.,1.),(1.,1.),(1.,1.),(1.,1.),(1.,1.),(1.,
1.),(1.,1.),(1.,1.),(1.,1.),(1.,1.),(1.,1.),(1.,1.),(1.,1.),(1.,1.),(1.,
1.),(1.,1.),(1.,1.),(1.,1.),(1.,1.),(1.,1.),(1.,1.),(1.,1.),(1.,1.),(1.,
1.),(1.,1.),(1.,1.),(1.,1.),(1.,1.),(1.,1.),(1.,1.),(1.,1.),(1.,1.),(1.,
1.),(1.,1.),(1.,1.),(1.,1.),(1.,1.),(1.,1.),(1.,1.),(1.,1.),(1.,1.),(1.,
1.),(1.,1.),(1.,1.),(1.,1.),(1.,1.),(1.,1.),(1.,1.),(1.,1.),(1.,1.),(1.,
1.),(1.,1.),(1.,1.),(1.,1.),(1.,1.),(1.,1.),(1.,1.),(1.,1.),(1.,1.),(1.,
1.),(1.,1.)))
REPRESENTATION_ITEM('')
SURFACE()
);
#1064=(
BOUNDED_SURFACE()
B_SPLINE_SURFACE(5,1,((#208506,#208507),(#208508,#208509),(#208510,#208511),
(#208512,#208513),(#208514,#208515),(#208516,#208517),(#208518,#208519),
(#208520,#208521),(#208522,#208523),(#208524,#208525),(#208526,#208527),
(#208528,#208529),(#208530,#208531),(#208532,#208533),(#208534,#208535),
(#208536,#208537),(#208538,#208539),(#208540,#208541),(#208542,#208543),
(#208544,#208545),(#208546,#208547),(#208548,#208549),(#208550,#208551),
(#208552,#208553),(#208554,#208555),(#208556,#208557),(#208558,#208559),
(#208560,#208561),(#208562,#208563),(#208564,#208565),(#208566,#208567),
(#208568,#208569),(#208570,#208571),(#208572,#208573),(#208574,#208575),
(#208576,#208577),(#208578,#208579),(#208580,#208581),(#208582,#208583),
(#208584,#208585),(#208586,#208587),(#208588,#208589),(#208590,#208591),
(#208592,#208593),(#208594,#208595),(#208596,#208597),(#208598,#208599),
(#208600,#208601),(#208602,#208603),(#208604,#208605),(#208606,#208607),
(#208608,#208609),(#208610,#208611),(#208612,#208613),(#208614,#208615),
(#208616,#208617),(#208618,#208619),(#208620,#208621),(#208622,#208623),
(#208624,#208625),(#208626,#208627),(#208628,#208629),(#208630,#208631),
(#208632,#208633),(#208634,#208635),(#208636,#208637),(#208638,#208639),
(#208640,#208641),(#208642,#208643),(#208644,#208645),(#208646,#208647),
(#208648,#208649),(#208650,#208651),(#208652,#208653),(#208654,#208655),
(#208656,#208657),(#208658,#208659),(#208660,#208661),(#208662,#208663),
(#208664,#208665),(#208666,#208667),(#208668,#208669),(#208670,#208671),
(#208672,#208673),(#208674,#208675),(#208676,#208677),(#208678,#208679),
(#208680,#208681),(#208682,#208683),(#208684,#208685),(#208686,#208687),
(#208688,#208689),(#208690,#208691),(#208692,#208693),(#208694,#208695),
(#208696,#208697),(#208698,#208699),(#208700,#208701),(#208702,#208703),
(#208704,#208705),(#208706,#208707),(#208708,#208709),(#208710,#208711),
(#208712,#208713),(#208714,#208715),(#208716,#208717),(#208718,#208719),
(#208720,#208721),(#208722,#208723),(#208724,#208725),(#208726,#208727),
(#208728,#208729),(#208730,#208731),(#208732,#208733),(#208734,#208735),
(#208736,#208737),(#208738,#208739),(#208740,#208741),(#208742,#208743),
(#208744,#208745),(#208746,#208747),(#208748,#208749),(#208750,#208751),
(#208752,#208753),(#208754,#208755),(#208756,#208757),(#208758,#208759),
(#208760,#208761),(#208762,#208763),(#208764,#208765),(#208766,#208767),
(#208768,#208769),(#208770,#208771),(#208772,#208773),(#208774,#208775),
(#208776,#208777),(#208778,#208779),(#208780,#208781),(#208782,#208783),
(#208784,#208785),(#208786,#208787),(#208788,#208789),(#208790,#208791),
(#208792,#208793),(#208794,#208795),(#208796,#208797),(#208798,#208799),
(#208800,#208801),(#208802,#208803),(#208804,#208805),(#208806,#208807),
(#208808,#208809),(#208810,#208811),(#208812,#208813),(#208814,#208815),
(#208816,#208817),(#208818,#208819),(#208820,#208821),(#208822,#208823),
(#208824,#208825),(#208826,#208827),(#208828,#208829),(#208830,#208831),
(#208832,#208833),(#208834,#208835),(#208836,#208837),(#208838,#208839),
(#208840,#208841),(#208842,#208843),(#208844,#208845),(#208846,#208847),
(#208848,#208849),(#208850,#208851),(#208852,#208853),(#208854,#208855),
(#208856,#208857),(#208858,#208859),(#208860,#208861),(#208862,#208863),
(#208864,#208865),(#208866,#208867),(#208868,#208869),(#208870,#208871),
(#208872,#208873),(#208874,#208875),(#208876,#208877),(#208878,#208879),
(#208880,#208881),(#208882,#208883),(#208884,#208885),(#208886,#208887),
(#208888,#208889),(#208890,#208891),(#208892,#208893),(#208894,#208895),
(#208896,#208897),(#208898,#208899),(#208900,#208901),(#208902,#208903),
(#208904,#208905),(#208906,#208907),(#208908,#208909),(#208910,#208911),
(#208912,#208913),(#208914,#208915)),.UNSPECIFIED.,.F.,.F.,.F.)
B_SPLINE_SURFACE_WITH_KNOTS((6,1,1,1,1,1,1,1,1,1,1,1,1,1,1,1,1,1,1,1,1,
1,1,1,1,1,1,1,1,1,1,1,1,1,1,1,1,1,1,1,1,1,1,1,1,1,1,1,1,1,1,1,1,1,1,1,1,
1,1,1,1,1,1,1,1,1,1,1,1,1,1,1,1,1,1,1,1,1,1,1,1,1,1,1,1,1,1,1,1,1,1,1,1,
1,1,1,1,1,1,1,1,1,1,1,1,1,1,1,1,1,1,1,1,1,1,1,1,1,1,1,1,1,1,1,1,1,1,1,1,
1,1,1,1,1,1,1,1,1,1,1,1,1,1,1,1,1,1,1,1,1,1,1,1,1,1,1,1,1,1,1,1,1,1,1,1,
1,1,1,1,1,1,1,1,1,1,1,1,1,1,1,1,1,1,1,1,1,1,1,1,1,1,1,1,1,1,1,1,1,1,1,6),
(2,2),(0.,0.005,0.01,0.015,0.02,0.025,0.03,0.035,0.04,0.045,0.05,0.055,
0.06,0.065,0.07,0.075,0.08,0.085,0.09,0.095,0.1,0.105,0.11,0.115,0.12,0.125,
0.13,0.135,0.14,0.145,0.15,0.155,0.16,0.165,0.17,0.175,0.18,0.185,0.19,
0.195,0.2,0.205,0.21,0.215,0.22,0.225,0.23,0.235,0.24,0.245,0.25,0.255,
0.26,0.265,0.27,0.275,0.28,0.285,0.29,0.295,0.3,0.305,0.31,0.315,0.32,0.325,
0.33,0.335,0.34,0.345,0.35,0.355,0.36,0.365,0.37,0.375,0.38,0.385,0.39,
0.395,0.4,0.405,0.41,0.415,0.42,0.425,0.43,0.435,0.44,0.445,0.45,0.455,
0.46,0.465,0.47,0.475,0.48,0.485,0.49,0.495,0.5,0.505,0.51,0.515,0.52,0.525,
0.53,0.535,0.54,0.545,0.55,0.555,0.56,0.565,0.57,0.575,0.58,0.585,0.59,
0.595,0.6,0.605,0.61,0.615,0.62,0.625,0.63,0.635,0.64,0.645,0.65,0.655,
0.66,0.665,0.67,0.675,0.68,0.685,0.690000000000001,0.695000000000001,0.700000000000001,
0.705000000000001,0.710000000000001,0.715000000000001,0.720000000000001,
0.725000000000001,0.730000000000001,0.735000000000001,0.740000000000001,
0.745000000000001,0.750000000000001,0.755000000000001,0.760000000000001,
0.765000000000001,0.770000000000001,0.775000000000001,0.780000000000001,
0.785000000000001,0.790000000000001,0.795000000000001,0.800000000000001,
0.805000000000001,0.810000000000001,0.815000000000001,0.820000000000001,
0.825000000000001,0.830000000000001,0.835000000000001,0.840000000000001,
0.845000000000001,0.850000000000001,0.855000000000001,0.860000000000001,
0.865000000000001,0.870000000000001,0.875000000000001,0.880000000000001,
0.885000000000001,0.890000000000001,0.895000000000001,0.900000000000001,
0.905000000000001,0.910000000000001,0.915000000000001,0.920000000000001,
0.925000000000001,0.930000000000001,0.935000000000001,0.940000000000001,
0.945000000000001,0.950000000000001,0.955000000000001,0.960000000000001,
0.965000000000001,0.970000000000001,0.975000000000001,0.980000000000001,
0.985000000000001,0.990000000000001,0.995000000000001,1.),(0.,1.2),
 .UNSPECIFIED.)
GEOMETRIC_REPRESENTATION_ITEM()
RATIONAL_B_SPLINE_SURFACE(((1.,1.),(1.,1.),(1.,1.),(1.,1.),(1.,1.),(1.,
1.),(1.,1.),(1.,1.),(1.,1.),(1.,1.),(1.,1.),(1.,1.),(1.,1.),(1.,1.),(1.,
1.),(1.,1.),(1.,1.),(1.,1.),(1.,1.),(1.,1.),(1.,1.),(1.,1.),(1.,1.),(1.,
1.),(1.,1.),(1.,1.),(1.,1.),(1.,1.),(1.,1.),(1.,1.),(1.,1.),(1.,1.),(1.,
1.),(1.,1.),(1.,1.),(1.,1.),(1.,1.),(1.,1.),(1.,1.),(1.,1.),(1.,1.),(1.,
1.),(1.,1.),(1.,1.),(1.,1.),(1.,1.),(1.,1.),(1.,1.),(1.,1.),(1.,1.),(1.,
1.),(1.,1.),(1.,1.),(1.,1.),(1.,1.),(1.,1.),(1.,1.),(1.,1.),(1.,1.),(1.,
1.),(1.,1.),(1.,1.),(1.,1.),(1.,1.),(1.,1.),(1.,1.),(1.,1.),(1.,1.),(1.,
1.),(1.,1.),(1.,1.),(1.,1.),(1.,1.),(1.,1.),(1.,1.),(1.,1.),(1.,1.),(1.,
1.),(1.,1.),(1.,1.),(1.,1.),(1.,1.),(1.,1.),(1.,1.),(1.,1.),(1.,1.),(1.,
1.),(1.,1.),(1.,1.),(1.,1.),(1.,1.),(1.,1.),(1.,1.),(1.,1.),(1.,1.),(1.,
1.),(1.,1.),(1.,1.),(1.,1.),(1.,1.),(1.,1.),(1.,1.),(1.,1.),(1.,1.),(1.,
1.),(1.,1.),(1.,1.),(1.,1.),(1.,1.),(1.,1.),(1.,1.),(1.,1.),(1.,1.),(1.,
1.),(1.,1.),(1.,1.),(1.,1.),(1.,1.),(1.,1.),(1.,1.),(1.,1.),(1.,1.),(1.,
1.),(1.,1.),(1.,1.),(1.,1.),(1.,1.),(1.,1.),(1.,1.),(1.,1.),(1.,1.),(1.,
1.),(1.,1.),(1.,1.),(1.,1.),(1.,1.),(1.,1.),(1.,1.),(1.,1.),(1.,1.),(1.,
1.),(1.,1.),(1.,1.),(1.,1.),(1.,1.),(1.,1.),(1.,1.),(1.,1.),(1.,1.),(1.,
1.),(1.,1.),(1.,1.),(1.,1.),(1.,1.),(1.,1.),(1.,1.),(1.,1.),(1.,1.),(1.,
1.),(1.,1.),(1.,1.),(1.,1.),(1.,1.),(1.,1.),(1.,1.),(1.,1.),(1.,1.),(1.,
1.),(1.,1.),(1.,1.),(1.,1.),(1.,1.),(1.,1.),(1.,1.),(1.,1.),(1.,1.),(1.,
1.),(1.,1.),(1.,1.),(1.,1.),(1.,1.),(1.,1.),(1.,1.),(1.,1.),(1.,1.),(1.,
1.),(1.,1.),(1.,1.),(1.,1.),(1.,1.),(1.,1.),(1.,1.),(1.,1.),(1.,1.),(1.,
1.),(1.,1.),(1.,1.),(1.,1.),(1.,1.),(1.,1.),(1.,1.),(1.,1.),(1.,1.),(1.,
1.),(1.,1.)))
REPRESENTATION_ITEM('')
SURFACE()
);
#1065=(
BOUNDED_SURFACE()
B_SPLINE_SURFACE(5,1,((#209127,#209128),(#209129,#209130),(#209131,#209132),
(#209133,#209134),(#209135,#209136),(#209137,#209138),(#209139,#209140),
(#209141,#209142),(#209143,#209144),(#209145,#209146),(#209147,#209148),
(#209149,#209150),(#209151,#209152),(#209153,#209154),(#209155,#209156),
(#209157,#209158),(#209159,#209160),(#209161,#209162),(#209163,#209164),
(#209165,#209166),(#209167,#209168),(#209169,#209170),(#209171,#209172),
(#209173,#209174),(#209175,#209176),(#209177,#209178),(#209179,#209180),
(#209181,#209182),(#209183,#209184),(#209185,#209186),(#209187,#209188),
(#209189,#209190),(#209191,#209192),(#209193,#209194),(#209195,#209196),
(#209197,#209198),(#209199,#209200),(#209201,#209202),(#209203,#209204),
(#209205,#209206),(#209207,#209208),(#209209,#209210),(#209211,#209212),
(#209213,#209214),(#209215,#209216),(#209217,#209218),(#209219,#209220),
(#209221,#209222),(#209223,#209224),(#209225,#209226),(#209227,#209228),
(#209229,#209230),(#209231,#209232),(#209233,#209234),(#209235,#209236),
(#209237,#209238),(#209239,#209240),(#209241,#209242),(#209243,#209244),
(#209245,#209246),(#209247,#209248),(#209249,#209250),(#209251,#209252),
(#209253,#209254),(#209255,#209256),(#209257,#209258),(#209259,#209260),
(#209261,#209262),(#209263,#209264),(#209265,#209266),(#209267,#209268),
(#209269,#209270),(#209271,#209272),(#209273,#209274),(#209275,#209276),
(#209277,#209278),(#209279,#209280),(#209281,#209282),(#209283,#209284),
(#209285,#209286),(#209287,#209288),(#209289,#209290),(#209291,#209292),
(#209293,#209294),(#209295,#209296),(#209297,#209298),(#209299,#209300),
(#209301,#209302),(#209303,#209304),(#209305,#209306),(#209307,#209308),
(#209309,#209310),(#209311,#209312),(#209313,#209314),(#209315,#209316),
(#209317,#209318),(#209319,#209320),(#209321,#209322),(#209323,#209324),
(#209325,#209326),(#209327,#209328),(#209329,#209330),(#209331,#209332),
(#209333,#209334),(#209335,#209336),(#209337,#209338),(#209339,#209340),
(#209341,#209342),(#209343,#209344),(#209345,#209346),(#209347,#209348),
(#209349,#209350),(#209351,#209352),(#209353,#209354),(#209355,#209356),
(#209357,#209358),(#209359,#209360),(#209361,#209362),(#209363,#209364),
(#209365,#209366),(#209367,#209368),(#209369,#209370),(#209371,#209372),
(#209373,#209374),(#209375,#209376),(#209377,#209378),(#209379,#209380),
(#209381,#209382),(#209383,#209384),(#209385,#209386),(#209387,#209388),
(#209389,#209390),(#209391,#209392),(#209393,#209394),(#209395,#209396),
(#209397,#209398),(#209399,#209400),(#209401,#209402),(#209403,#209404),
(#209405,#209406),(#209407,#209408),(#209409,#209410),(#209411,#209412),
(#209413,#209414),(#209415,#209416),(#209417,#209418),(#209419,#209420),
(#209421,#209422),(#209423,#209424),(#209425,#209426),(#209427,#209428),
(#209429,#209430),(#209431,#209432),(#209433,#209434),(#209435,#209436),
(#209437,#209438),(#209439,#209440),(#209441,#209442),(#209443,#209444),
(#209445,#209446),(#209447,#209448),(#209449,#209450),(#209451,#209452),
(#209453,#209454),(#209455,#209456),(#209457,#209458),(#209459,#209460),
(#209461,#209462),(#209463,#209464),(#209465,#209466),(#209467,#209468),
(#209469,#209470),(#209471,#209472),(#209473,#209474),(#209475,#209476),
(#209477,#209478),(#209479,#209480),(#209481,#209482),(#209483,#209484),
(#209485,#209486),(#209487,#209488),(#209489,#209490),(#209491,#209492),
(#209493,#209494),(#209495,#209496),(#209497,#209498),(#209499,#209500),
(#209501,#209502),(#209503,#209504),(#209505,#209506),(#209507,#209508),
(#209509,#209510),(#209511,#209512),(#209513,#209514),(#209515,#209516),
(#209517,#209518),(#209519,#209520),(#209521,#209522),(#209523,#209524),
(#209525,#209526),(#209527,#209528),(#209529,#209530),(#209531,#209532),
(#209533,#209534),(#209535,#209536)),.UNSPECIFIED.,.F.,.F.,.F.)
B_SPLINE_SURFACE_WITH_KNOTS((6,1,1,1,1,1,1,1,1,1,1,1,1,1,1,1,1,1,1,1,1,
1,1,1,1,1,1,1,1,1,1,1,1,1,1,1,1,1,1,1,1,1,1,1,1,1,1,1,1,1,1,1,1,1,1,1,1,
1,1,1,1,1,1,1,1,1,1,1,1,1,1,1,1,1,1,1,1,1,1,1,1,1,1,1,1,1,1,1,1,1,1,1,1,
1,1,1,1,1,1,1,1,1,1,1,1,1,1,1,1,1,1,1,1,1,1,1,1,1,1,1,1,1,1,1,1,1,1,1,1,
1,1,1,1,1,1,1,1,1,1,1,1,1,1,1,1,1,1,1,1,1,1,1,1,1,1,1,1,1,1,1,1,1,1,1,1,
1,1,1,1,1,1,1,1,1,1,1,1,1,1,1,1,1,1,1,1,1,1,1,1,1,1,1,1,1,1,1,1,1,1,1,6),
(2,2),(-1.,-0.995000000000001,-0.990000000000001,-0.985000000000001,-0.980000000000001,
-0.975000000000001,-0.970000000000001,-0.965000000000001,-0.960000000000001,
-0.955000000000001,-0.950000000000001,-0.945000000000001,-0.940000000000001,
-0.935000000000001,-0.930000000000001,-0.925000000000001,-0.920000000000001,
-0.915000000000001,-0.910000000000001,-0.905000000000001,-0.900000000000001,
-0.895000000000001,-0.890000000000001,-0.885000000000001,-0.880000000000001,
-0.875000000000001,-0.870000000000001,-0.865000000000001,-0.860000000000001,
-0.855000000000001,-0.850000000000001,-0.845000000000001,-0.840000000000001,
-0.835000000000001,-0.830000000000001,-0.825000000000001,-0.820000000000001,
-0.815000000000001,-0.810000000000001,-0.805000000000001,-0.800000000000001,
-0.795000000000001,-0.790000000000001,-0.785000000000001,-0.780000000000001,
-0.775000000000001,-0.770000000000001,-0.765000000000001,-0.760000000000001,
-0.755000000000001,-0.750000000000001,-0.745000000000001,-0.740000000000001,
-0.735000000000001,-0.730000000000001,-0.725000000000001,-0.720000000000001,
-0.715000000000001,-0.710000000000001,-0.705000000000001,-0.700000000000001,
-0.695000000000001,-0.690000000000001,-0.685,-0.68,-0.675,-0.67,-0.665,
-0.66,-0.655,-0.65,-0.645,-0.64,-0.635,-0.63,-0.625,-0.62,-0.615,-0.61,
-0.605,-0.6,-0.595,-0.59,-0.585,-0.58,-0.575,-0.57,-0.565,-0.56,-0.555,
-0.55,-0.545,-0.54,-0.535,-0.53,-0.525,-0.52,-0.515,-0.51,-0.505,-0.5,-0.495,
-0.49,-0.485,-0.48,-0.475,-0.47,-0.465,-0.46,-0.455,-0.45,-0.445,-0.44,
-0.435,-0.43,-0.425,-0.42,-0.415,-0.41,-0.405,-0.4,-0.395,-0.39,-0.385,
-0.38,-0.375,-0.37,-0.365,-0.36,-0.355,-0.35,-0.345,-0.34,-0.335,-0.33,
-0.325,-0.32,-0.315,-0.31,-0.305,-0.3,-0.295,-0.29,-0.285,-0.28,-0.275,
-0.27,-0.265,-0.26,-0.255,-0.25,-0.245,-0.24,-0.235,-0.23,-0.225,-0.22,
-0.215,-0.21,-0.205,-0.2,-0.195,-0.19,-0.185,-0.18,-0.175,-0.17,-0.165,
-0.16,-0.155,-0.15,-0.145,-0.14,-0.135,-0.13,-0.125,-0.12,-0.115,-0.11,
-0.105,-0.1,-0.095,-0.09,-0.085,-0.08,-0.075,-0.07,-0.065,-0.06,-0.055,
-0.05,-0.045,-0.04,-0.035,-0.03,-0.025,-0.02,-0.015,-0.01,-0.005,0.),(0.,
1.2),.UNSPECIFIED.)
GEOMETRIC_REPRESENTATION_ITEM()
RATIONAL_B_SPLINE_SURFACE(((1.,1.),(1.,1.),(1.,1.),(1.,1.),(1.,1.),(1.,
1.),(1.,1.),(1.,1.),(1.,1.),(1.,1.),(1.,1.),(1.,1.),(1.,1.),(1.,1.),(1.,
1.),(1.,1.),(1.,1.),(1.,1.),(1.,1.),(1.,1.),(1.,1.),(1.,1.),(1.,1.),(1.,
1.),(1.,1.),(1.,1.),(1.,1.),(1.,1.),(1.,1.),(1.,1.),(1.,1.),(1.,1.),(1.,
1.),(1.,1.),(1.,1.),(1.,1.),(1.,1.),(1.,1.),(1.,1.),(1.,1.),(1.,1.),(1.,
1.),(1.,1.),(1.,1.),(1.,1.),(1.,1.),(1.,1.),(1.,1.),(1.,1.),(1.,1.),(1.,
1.),(1.,1.),(1.,1.),(1.,1.),(1.,1.),(1.,1.),(1.,1.),(1.,1.),(1.,1.),(1.,
1.),(1.,1.),(1.,1.),(1.,1.),(1.,1.),(1.,1.),(1.,1.),(1.,1.),(1.,1.),(1.,
1.),(1.,1.),(1.,1.),(1.,1.),(1.,1.),(1.,1.),(1.,1.),(1.,1.),(1.,1.),(1.,
1.),(1.,1.),(1.,1.),(1.,1.),(1.,1.),(1.,1.),(1.,1.),(1.,1.),(1.,1.),(1.,
1.),(1.,1.),(1.,1.),(1.,1.),(1.,1.),(1.,1.),(1.,1.),(1.,1.),(1.,1.),(1.,
1.),(1.,1.),(1.,1.),(1.,1.),(1.,1.),(1.,1.),(1.,1.),(1.,1.),(1.,1.),(1.,
1.),(1.,1.),(1.,1.),(1.,1.),(1.,1.),(1.,1.),(1.,1.),(1.,1.),(1.,1.),(1.,
1.),(1.,1.),(1.,1.),(1.,1.),(1.,1.),(1.,1.),(1.,1.),(1.,1.),(1.,1.),(1.,
1.),(1.,1.),(1.,1.),(1.,1.),(1.,1.),(1.,1.),(1.,1.),(1.,1.),(1.,1.),(1.,
1.),(1.,1.),(1.,1.),(1.,1.),(1.,1.),(1.,1.),(1.,1.),(1.,1.),(1.,1.),(1.,
1.),(1.,1.),(1.,1.),(1.,1.),(1.,1.),(1.,1.),(1.,1.),(1.,1.),(1.,1.),(1.,
1.),(1.,1.),(1.,1.),(1.,1.),(1.,1.),(1.,1.),(1.,1.),(1.,1.),(1.,1.),(1.,
1.),(1.,1.),(1.,1.),(1.,1.),(1.,1.),(1.,1.),(1.,1.),(1.,1.),(1.,1.),(1.,
1.),(1.,1.),(1.,1.),(1.,1.),(1.,1.),(1.,1.),(1.,1.),(1.,1.),(1.,1.),(1.,
1.),(1.,1.),(1.,1.),(1.,1.),(1.,1.),(1.,1.),(1.,1.),(1.,1.),(1.,1.),(1.,
1.),(1.,1.),(1.,1.),(1.,1.),(1.,1.),(1.,1.),(1.,1.),(1.,1.),(1.,1.),(1.,
1.),(1.,1.),(1.,1.),(1.,1.),(1.,1.),(1.,1.),(1.,1.),(1.,1.),(1.,1.),(1.,
1.),(1.,1.)))
REPRESENTATION_ITEM('')
SURFACE()
);
#1066=(
BOUNDED_SURFACE()
B_SPLINE_SURFACE(5,1,((#209744,#209745),(#209746,#209747),(#209748,#209749),
(#209750,#209751),(#209752,#209753),(#209754,#209755),(#209756,#209757),
(#209758,#209759),(#209760,#209761),(#209762,#209763),(#209764,#209765),
(#209766,#209767),(#209768,#209769),(#209770,#209771),(#209772,#209773),
(#209774,#209775),(#209776,#209777),(#209778,#209779),(#209780,#209781),
(#209782,#209783),(#209784,#209785),(#209786,#209787),(#209788,#209789),
(#209790,#209791),(#209792,#209793),(#209794,#209795),(#209796,#209797),
(#209798,#209799),(#209800,#209801),(#209802,#209803),(#209804,#209805),
(#209806,#209807),(#209808,#209809),(#209810,#209811),(#209812,#209813),
(#209814,#209815),(#209816,#209817),(#209818,#209819),(#209820,#209821),
(#209822,#209823),(#209824,#209825),(#209826,#209827),(#209828,#209829),
(#209830,#209831),(#209832,#209833),(#209834,#209835),(#209836,#209837),
(#209838,#209839),(#209840,#209841),(#209842,#209843),(#209844,#209845),
(#209846,#209847),(#209848,#209849),(#209850,#209851),(#209852,#209853),
(#209854,#209855),(#209856,#209857),(#209858,#209859),(#209860,#209861),
(#209862,#209863),(#209864,#209865),(#209866,#209867),(#209868,#209869),
(#209870,#209871),(#209872,#209873),(#209874,#209875),(#209876,#209877),
(#209878,#209879),(#209880,#209881),(#209882,#209883),(#209884,#209885),
(#209886,#209887),(#209888,#209889),(#209890,#209891),(#209892,#209893),
(#209894,#209895),(#209896,#209897),(#209898,#209899),(#209900,#209901),
(#209902,#209903),(#209904,#209905),(#209906,#209907),(#209908,#209909),
(#209910,#209911),(#209912,#209913),(#209914,#209915),(#209916,#209917),
(#209918,#209919),(#209920,#209921),(#209922,#209923),(#209924,#209925),
(#209926,#209927),(#209928,#209929),(#209930,#209931),(#209932,#209933),
(#209934,#209935),(#209936,#209937),(#209938,#209939),(#209940,#209941),
(#209942,#209943),(#209944,#209945),(#209946,#209947),(#209948,#209949),
(#209950,#209951),(#209952,#209953),(#209954,#209955),(#209956,#209957),
(#209958,#209959),(#209960,#209961),(#209962,#209963),(#209964,#209965),
(#209966,#209967),(#209968,#209969),(#209970,#209971),(#209972,#209973),
(#209974,#209975),(#209976,#209977),(#209978,#209979),(#209980,#209981),
(#209982,#209983),(#209984,#209985),(#209986,#209987),(#209988,#209989),
(#209990,#209991),(#209992,#209993),(#209994,#209995),(#209996,#209997),
(#209998,#209999),(#210000,#210001),(#210002,#210003),(#210004,#210005),
(#210006,#210007),(#210008,#210009),(#210010,#210011),(#210012,#210013),
(#210014,#210015),(#210016,#210017),(#210018,#210019),(#210020,#210021),
(#210022,#210023),(#210024,#210025),(#210026,#210027),(#210028,#210029),
(#210030,#210031),(#210032,#210033),(#210034,#210035),(#210036,#210037),
(#210038,#210039),(#210040,#210041),(#210042,#210043),(#210044,#210045),
(#210046,#210047),(#210048,#210049),(#210050,#210051),(#210052,#210053),
(#210054,#210055),(#210056,#210057),(#210058,#210059),(#210060,#210061),
(#210062,#210063),(#210064,#210065),(#210066,#210067),(#210068,#210069),
(#210070,#210071),(#210072,#210073),(#210074,#210075),(#210076,#210077),
(#210078,#210079),(#210080,#210081),(#210082,#210083),(#210084,#210085),
(#210086,#210087),(#210088,#210089),(#210090,#210091),(#210092,#210093),
(#210094,#210095),(#210096,#210097),(#210098,#210099),(#210100,#210101),
(#210102,#210103),(#210104,#210105),(#210106,#210107),(#210108,#210109),
(#210110,#210111),(#210112,#210113),(#210114,#210115),(#210116,#210117),
(#210118,#210119),(#210120,#210121),(#210122,#210123),(#210124,#210125),
(#210126,#210127),(#210128,#210129),(#210130,#210131),(#210132,#210133),
(#210134,#210135),(#210136,#210137),(#210138,#210139),(#210140,#210141),
(#210142,#210143),(#210144,#210145),(#210146,#210147),(#210148,#210149),
(#210150,#210151),(#210152,#210153)),.UNSPECIFIED.,.F.,.F.,.F.)
B_SPLINE_SURFACE_WITH_KNOTS((6,1,1,1,1,1,1,1,1,1,1,1,1,1,1,1,1,1,1,1,1,
1,1,1,1,1,1,1,1,1,1,1,1,1,1,1,1,1,1,1,1,1,1,1,1,1,1,1,1,1,1,1,1,1,1,1,1,
1,1,1,1,1,1,1,1,1,1,1,1,1,1,1,1,1,1,1,1,1,1,1,1,1,1,1,1,1,1,1,1,1,1,1,1,
1,1,1,1,1,1,1,1,1,1,1,1,1,1,1,1,1,1,1,1,1,1,1,1,1,1,1,1,1,1,1,1,1,1,1,1,
1,1,1,1,1,1,1,1,1,1,1,1,1,1,1,1,1,1,1,1,1,1,1,1,1,1,1,1,1,1,1,1,1,1,1,1,
1,1,1,1,1,1,1,1,1,1,1,1,1,1,1,1,1,1,1,1,1,1,1,1,1,1,1,1,1,1,1,1,1,1,1,6),
(2,2),(0.,0.005,0.01,0.015,0.02,0.025,0.03,0.035,0.04,0.045,0.05,0.055,
0.06,0.065,0.07,0.075,0.08,0.085,0.09,0.095,0.1,0.105,0.11,0.115,0.12,0.125,
0.13,0.135,0.14,0.145,0.15,0.155,0.16,0.165,0.17,0.175,0.18,0.185,0.19,
0.195,0.2,0.205,0.21,0.215,0.22,0.225,0.23,0.235,0.24,0.245,0.25,0.255,
0.26,0.265,0.27,0.275,0.28,0.285,0.29,0.295,0.3,0.305,0.31,0.315,0.32,0.325,
0.33,0.335,0.34,0.345,0.35,0.355,0.36,0.365,0.37,0.375,0.38,0.385,0.39,
0.395,0.4,0.405,0.41,0.415,0.42,0.425,0.43,0.435,0.44,0.445,0.45,0.455,
0.46,0.465,0.47,0.475,0.48,0.485,0.49,0.495,0.5,0.505,0.51,0.515,0.52,0.525,
0.53,0.535,0.54,0.545,0.55,0.555,0.56,0.565,0.57,0.575,0.58,0.585,0.59,
0.595,0.6,0.605,0.61,0.615,0.62,0.625,0.63,0.635,0.64,0.645,0.65,0.655,
0.66,0.665,0.67,0.675,0.68,0.685,0.690000000000001,0.695000000000001,0.700000000000001,
0.705000000000001,0.710000000000001,0.715000000000001,0.720000000000001,
0.725000000000001,0.730000000000001,0.735000000000001,0.740000000000001,
0.745000000000001,0.750000000000001,0.755000000000001,0.760000000000001,
0.765000000000001,0.770000000000001,0.775000000000001,0.780000000000001,
0.785000000000001,0.790000000000001,0.795000000000001,0.800000000000001,
0.805000000000001,0.810000000000001,0.815000000000001,0.820000000000001,
0.825000000000001,0.830000000000001,0.835000000000001,0.840000000000001,
0.845000000000001,0.850000000000001,0.855000000000001,0.860000000000001,
0.865000000000001,0.870000000000001,0.875000000000001,0.880000000000001,
0.885000000000001,0.890000000000001,0.895000000000001,0.900000000000001,
0.905000000000001,0.910000000000001,0.915000000000001,0.920000000000001,
0.925000000000001,0.930000000000001,0.935000000000001,0.940000000000001,
0.945000000000001,0.950000000000001,0.955000000000001,0.960000000000001,
0.965000000000001,0.970000000000001,0.975000000000001,0.980000000000001,
0.985000000000001,0.990000000000001,0.995000000000001,1.),(0.,1.2),
 .UNSPECIFIED.)
GEOMETRIC_REPRESENTATION_ITEM()
RATIONAL_B_SPLINE_SURFACE(((1.,1.),(1.,1.),(1.,1.),(1.,1.),(1.,1.),(1.,
1.),(1.,1.),(1.,1.),(1.,1.),(1.,1.),(1.,1.),(1.,1.),(1.,1.),(1.,1.),(1.,
1.),(1.,1.),(1.,1.),(1.,1.),(1.,1.),(1.,1.),(1.,1.),(1.,1.),(1.,1.),(1.,
1.),(1.,1.),(1.,1.),(1.,1.),(1.,1.),(1.,1.),(1.,1.),(1.,1.),(1.,1.),(1.,
1.),(1.,1.),(1.,1.),(1.,1.),(1.,1.),(1.,1.),(1.,1.),(1.,1.),(1.,1.),(1.,
1.),(1.,1.),(1.,1.),(1.,1.),(1.,1.),(1.,1.),(1.,1.),(1.,1.),(1.,1.),(1.,
1.),(1.,1.),(1.,1.),(1.,1.),(1.,1.),(1.,1.),(1.,1.),(1.,1.),(1.,1.),(1.,
1.),(1.,1.),(1.,1.),(1.,1.),(1.,1.),(1.,1.),(1.,1.),(1.,1.),(1.,1.),(1.,
1.),(1.,1.),(1.,1.),(1.,1.),(1.,1.),(1.,1.),(1.,1.),(1.,1.),(1.,1.),(1.,
1.),(1.,1.),(1.,1.),(1.,1.),(1.,1.),(1.,1.),(1.,1.),(1.,1.),(1.,1.),(1.,
1.),(1.,1.),(1.,1.),(1.,1.),(1.,1.),(1.,1.),(1.,1.),(1.,1.),(1.,1.),(1.,
1.),(1.,1.),(1.,1.),(1.,1.),(1.,1.),(1.,1.),(1.,1.),(1.,1.),(1.,1.),(1.,
1.),(1.,1.),(1.,1.),(1.,1.),(1.,1.),(1.,1.),(1.,1.),(1.,1.),(1.,1.),(1.,
1.),(1.,1.),(1.,1.),(1.,1.),(1.,1.),(1.,1.),(1.,1.),(1.,1.),(1.,1.),(1.,
1.),(1.,1.),(1.,1.),(1.,1.),(1.,1.),(1.,1.),(1.,1.),(1.,1.),(1.,1.),(1.,
1.),(1.,1.),(1.,1.),(1.,1.),(1.,1.),(1.,1.),(1.,1.),(1.,1.),(1.,1.),(1.,
1.),(1.,1.),(1.,1.),(1.,1.),(1.,1.),(1.,1.),(1.,1.),(1.,1.),(1.,1.),(1.,
1.),(1.,1.),(1.,1.),(1.,1.),(1.,1.),(1.,1.),(1.,1.),(1.,1.),(1.,1.),(1.,
1.),(1.,1.),(1.,1.),(1.,1.),(1.,1.),(1.,1.),(1.,1.),(1.,1.),(1.,1.),(1.,
1.),(1.,1.),(1.,1.),(1.,1.),(1.,1.),(1.,1.),(1.,1.),(1.,1.),(1.,1.),(1.,
1.),(1.,1.),(1.,1.),(1.,1.),(1.,1.),(1.,1.),(1.,1.),(1.,1.),(1.,1.),(1.,
1.),(1.,1.),(1.,1.),(1.,1.),(1.,1.),(1.,1.),(1.,1.),(1.,1.),(1.,1.),(1.,
1.),(1.,1.),(1.,1.),(1.,1.),(1.,1.),(1.,1.),(1.,1.),(1.,1.),(1.,1.),(1.,
1.),(1.,1.)))
REPRESENTATION_ITEM('')
SURFACE()
);
#1067=(
BOUNDED_SURFACE()
B_SPLINE_SURFACE(5,1,((#210365,#210366),(#210367,#210368),(#210369,#210370),
(#210371,#210372),(#210373,#210374),(#210375,#210376),(#210377,#210378),
(#210379,#210380),(#210381,#210382),(#210383,#210384),(#210385,#210386),
(#210387,#210388),(#210389,#210390),(#210391,#210392),(#210393,#210394),
(#210395,#210396),(#210397,#210398),(#210399,#210400),(#210401,#210402),
(#210403,#210404),(#210405,#210406),(#210407,#210408),(#210409,#210410),
(#210411,#210412),(#210413,#210414),(#210415,#210416),(#210417,#210418),
(#210419,#210420),(#210421,#210422),(#210423,#210424),(#210425,#210426),
(#210427,#210428),(#210429,#210430),(#210431,#210432),(#210433,#210434),
(#210435,#210436),(#210437,#210438),(#210439,#210440),(#210441,#210442),
(#210443,#210444),(#210445,#210446),(#210447,#210448),(#210449,#210450),
(#210451,#210452),(#210453,#210454),(#210455,#210456),(#210457,#210458),
(#210459,#210460),(#210461,#210462),(#210463,#210464),(#210465,#210466),
(#210467,#210468),(#210469,#210470),(#210471,#210472),(#210473,#210474),
(#210475,#210476),(#210477,#210478),(#210479,#210480),(#210481,#210482),
(#210483,#210484),(#210485,#210486),(#210487,#210488),(#210489,#210490),
(#210491,#210492),(#210493,#210494),(#210495,#210496),(#210497,#210498),
(#210499,#210500),(#210501,#210502),(#210503,#210504),(#210505,#210506),
(#210507,#210508),(#210509,#210510),(#210511,#210512),(#210513,#210514),
(#210515,#210516),(#210517,#210518),(#210519,#210520),(#210521,#210522),
(#210523,#210524),(#210525,#210526),(#210527,#210528),(#210529,#210530),
(#210531,#210532),(#210533,#210534),(#210535,#210536),(#210537,#210538),
(#210539,#210540),(#210541,#210542),(#210543,#210544),(#210545,#210546),
(#210547,#210548),(#210549,#210550),(#210551,#210552),(#210553,#210554),
(#210555,#210556),(#210557,#210558),(#210559,#210560),(#210561,#210562),
(#210563,#210564),(#210565,#210566),(#210567,#210568),(#210569,#210570),
(#210571,#210572),(#210573,#210574),(#210575,#210576),(#210577,#210578),
(#210579,#210580),(#210581,#210582),(#210583,#210584),(#210585,#210586),
(#210587,#210588),(#210589,#210590),(#210591,#210592),(#210593,#210594),
(#210595,#210596),(#210597,#210598),(#210599,#210600),(#210601,#210602),
(#210603,#210604),(#210605,#210606),(#210607,#210608),(#210609,#210610),
(#210611,#210612),(#210613,#210614),(#210615,#210616),(#210617,#210618),
(#210619,#210620),(#210621,#210622),(#210623,#210624),(#210625,#210626),
(#210627,#210628),(#210629,#210630),(#210631,#210632),(#210633,#210634),
(#210635,#210636),(#210637,#210638),(#210639,#210640),(#210641,#210642),
(#210643,#210644),(#210645,#210646),(#210647,#210648),(#210649,#210650),
(#210651,#210652),(#210653,#210654),(#210655,#210656),(#210657,#210658),
(#210659,#210660),(#210661,#210662),(#210663,#210664),(#210665,#210666),
(#210667,#210668),(#210669,#210670),(#210671,#210672),(#210673,#210674),
(#210675,#210676),(#210677,#210678),(#210679,#210680),(#210681,#210682),
(#210683,#210684),(#210685,#210686),(#210687,#210688),(#210689,#210690),
(#210691,#210692),(#210693,#210694),(#210695,#210696),(#210697,#210698),
(#210699,#210700),(#210701,#210702),(#210703,#210704),(#210705,#210706),
(#210707,#210708),(#210709,#210710),(#210711,#210712),(#210713,#210714),
(#210715,#210716),(#210717,#210718),(#210719,#210720),(#210721,#210722),
(#210723,#210724),(#210725,#210726),(#210727,#210728),(#210729,#210730),
(#210731,#210732),(#210733,#210734),(#210735,#210736),(#210737,#210738),
(#210739,#210740),(#210741,#210742),(#210743,#210744),(#210745,#210746),
(#210747,#210748),(#210749,#210750),(#210751,#210752),(#210753,#210754),
(#210755,#210756),(#210757,#210758),(#210759,#210760),(#210761,#210762),
(#210763,#210764),(#210765,#210766),(#210767,#210768),(#210769,#210770),
(#210771,#210772),(#210773,#210774)),.UNSPECIFIED.,.F.,.F.,.F.)
B_SPLINE_SURFACE_WITH_KNOTS((6,1,1,1,1,1,1,1,1,1,1,1,1,1,1,1,1,1,1,1,1,
1,1,1,1,1,1,1,1,1,1,1,1,1,1,1,1,1,1,1,1,1,1,1,1,1,1,1,1,1,1,1,1,1,1,1,1,
1,1,1,1,1,1,1,1,1,1,1,1,1,1,1,1,1,1,1,1,1,1,1,1,1,1,1,1,1,1,1,1,1,1,1,1,
1,1,1,1,1,1,1,1,1,1,1,1,1,1,1,1,1,1,1,1,1,1,1,1,1,1,1,1,1,1,1,1,1,1,1,1,
1,1,1,1,1,1,1,1,1,1,1,1,1,1,1,1,1,1,1,1,1,1,1,1,1,1,1,1,1,1,1,1,1,1,1,1,
1,1,1,1,1,1,1,1,1,1,1,1,1,1,1,1,1,1,1,1,1,1,1,1,1,1,1,1,1,1,1,1,1,1,1,6),
(2,2),(-1.,-0.995000000000001,-0.990000000000001,-0.985000000000001,-0.980000000000001,
-0.975000000000001,-0.970000000000001,-0.965000000000001,-0.960000000000001,
-0.955000000000001,-0.950000000000001,-0.945000000000001,-0.940000000000001,
-0.935000000000001,-0.930000000000001,-0.925000000000001,-0.920000000000001,
-0.915000000000001,-0.910000000000001,-0.905000000000001,-0.900000000000001,
-0.895000000000001,-0.890000000000001,-0.885000000000001,-0.880000000000001,
-0.875000000000001,-0.870000000000001,-0.865000000000001,-0.860000000000001,
-0.855000000000001,-0.850000000000001,-0.845000000000001,-0.840000000000001,
-0.835000000000001,-0.830000000000001,-0.825000000000001,-0.820000000000001,
-0.815000000000001,-0.810000000000001,-0.805000000000001,-0.800000000000001,
-0.795000000000001,-0.790000000000001,-0.785000000000001,-0.780000000000001,
-0.775000000000001,-0.770000000000001,-0.765000000000001,-0.760000000000001,
-0.755000000000001,-0.750000000000001,-0.745000000000001,-0.740000000000001,
-0.735000000000001,-0.730000000000001,-0.725000000000001,-0.720000000000001,
-0.715000000000001,-0.710000000000001,-0.705000000000001,-0.700000000000001,
-0.695000000000001,-0.690000000000001,-0.685,-0.68,-0.675,-0.67,-0.665,
-0.66,-0.655,-0.65,-0.645,-0.64,-0.635,-0.63,-0.625,-0.62,-0.615,-0.61,
-0.605,-0.6,-0.595,-0.59,-0.585,-0.58,-0.575,-0.57,-0.565,-0.56,-0.555,
-0.55,-0.545,-0.54,-0.535,-0.53,-0.525,-0.52,-0.515,-0.51,-0.505,-0.5,-0.495,
-0.49,-0.485,-0.48,-0.475,-0.47,-0.465,-0.46,-0.455,-0.45,-0.445,-0.44,
-0.435,-0.43,-0.425,-0.42,-0.415,-0.41,-0.405,-0.4,-0.395,-0.39,-0.385,
-0.38,-0.375,-0.37,-0.365,-0.36,-0.355,-0.35,-0.345,-0.34,-0.335,-0.33,
-0.325,-0.32,-0.315,-0.31,-0.305,-0.3,-0.295,-0.29,-0.285,-0.28,-0.275,
-0.27,-0.265,-0.26,-0.255,-0.25,-0.245,-0.24,-0.235,-0.23,-0.225,-0.22,
-0.215,-0.21,-0.205,-0.2,-0.195,-0.19,-0.185,-0.18,-0.175,-0.17,-0.165,
-0.16,-0.155,-0.15,-0.145,-0.14,-0.135,-0.13,-0.125,-0.12,-0.115,-0.11,
-0.105,-0.1,-0.095,-0.09,-0.085,-0.08,-0.075,-0.07,-0.065,-0.06,-0.055,
-0.05,-0.045,-0.04,-0.035,-0.03,-0.025,-0.02,-0.015,-0.01,-0.005,0.),(0.,
1.2),.UNSPECIFIED.)
GEOMETRIC_REPRESENTATION_ITEM()
RATIONAL_B_SPLINE_SURFACE(((1.,1.),(1.,1.),(1.,1.),(1.,1.),(1.,1.),(1.,
1.),(1.,1.),(1.,1.),(1.,1.),(1.,1.),(1.,1.),(1.,1.),(1.,1.),(1.,1.),(1.,
1.),(1.,1.),(1.,1.),(1.,1.),(1.,1.),(1.,1.),(1.,1.),(1.,1.),(1.,1.),(1.,
1.),(1.,1.),(1.,1.),(1.,1.),(1.,1.),(1.,1.),(1.,1.),(1.,1.),(1.,1.),(1.,
1.),(1.,1.),(1.,1.),(1.,1.),(1.,1.),(1.,1.),(1.,1.),(1.,1.),(1.,1.),(1.,
1.),(1.,1.),(1.,1.),(1.,1.),(1.,1.),(1.,1.),(1.,1.),(1.,1.),(1.,1.),(1.,
1.),(1.,1.),(1.,1.),(1.,1.),(1.,1.),(1.,1.),(1.,1.),(1.,1.),(1.,1.),(1.,
1.),(1.,1.),(1.,1.),(1.,1.),(1.,1.),(1.,1.),(1.,1.),(1.,1.),(1.,1.),(1.,
1.),(1.,1.),(1.,1.),(1.,1.),(1.,1.),(1.,1.),(1.,1.),(1.,1.),(1.,1.),(1.,
1.),(1.,1.),(1.,1.),(1.,1.),(1.,1.),(1.,1.),(1.,1.),(1.,1.),(1.,1.),(1.,
1.),(1.,1.),(1.,1.),(1.,1.),(1.,1.),(1.,1.),(1.,1.),(1.,1.),(1.,1.),(1.,
1.),(1.,1.),(1.,1.),(1.,1.),(1.,1.),(1.,1.),(1.,1.),(1.,1.),(1.,1.),(1.,
1.),(1.,1.),(1.,1.),(1.,1.),(1.,1.),(1.,1.),(1.,1.),(1.,1.),(1.,1.),(1.,
1.),(1.,1.),(1.,1.),(1.,1.),(1.,1.),(1.,1.),(1.,1.),(1.,1.),(1.,1.),(1.,
1.),(1.,1.),(1.,1.),(1.,1.),(1.,1.),(1.,1.),(1.,1.),(1.,1.),(1.,1.),(1.,
1.),(1.,1.),(1.,1.),(1.,1.),(1.,1.),(1.,1.),(1.,1.),(1.,1.),(1.,1.),(1.,
1.),(1.,1.),(1.,1.),(1.,1.),(1.,1.),(1.,1.),(1.,1.),(1.,1.),(1.,1.),(1.,
1.),(1.,1.),(1.,1.),(1.,1.),(1.,1.),(1.,1.),(1.,1.),(1.,1.),(1.,1.),(1.,
1.),(1.,1.),(1.,1.),(1.,1.),(1.,1.),(1.,1.),(1.,1.),(1.,1.),(1.,1.),(1.,
1.),(1.,1.),(1.,1.),(1.,1.),(1.,1.),(1.,1.),(1.,1.),(1.,1.),(1.,1.),(1.,
1.),(1.,1.),(1.,1.),(1.,1.),(1.,1.),(1.,1.),(1.,1.),(1.,1.),(1.,1.),(1.,
1.),(1.,1.),(1.,1.),(1.,1.),(1.,1.),(1.,1.),(1.,1.),(1.,1.),(1.,1.),(1.,
1.),(1.,1.),(1.,1.),(1.,1.),(1.,1.),(1.,1.),(1.,1.),(1.,1.),(1.,1.),(1.,
1.),(1.,1.)))
REPRESENTATION_ITEM('')
SURFACE()
);
#1068=(
BOUNDED_SURFACE()
B_SPLINE_SURFACE(5,1,((#210982,#210983),(#210984,#210985),(#210986,#210987),
(#210988,#210989),(#210990,#210991),(#210992,#210993),(#210994,#210995),
(#210996,#210997),(#210998,#210999),(#211000,#211001),(#211002,#211003),
(#211004,#211005),(#211006,#211007),(#211008,#211009),(#211010,#211011),
(#211012,#211013),(#211014,#211015),(#211016,#211017),(#211018,#211019),
(#211020,#211021),(#211022,#211023),(#211024,#211025),(#211026,#211027),
(#211028,#211029),(#211030,#211031),(#211032,#211033),(#211034,#211035),
(#211036,#211037),(#211038,#211039),(#211040,#211041),(#211042,#211043),
(#211044,#211045),(#211046,#211047),(#211048,#211049),(#211050,#211051),
(#211052,#211053),(#211054,#211055),(#211056,#211057),(#211058,#211059),
(#211060,#211061),(#211062,#211063),(#211064,#211065),(#211066,#211067),
(#211068,#211069),(#211070,#211071),(#211072,#211073),(#211074,#211075),
(#211076,#211077),(#211078,#211079),(#211080,#211081),(#211082,#211083),
(#211084,#211085),(#211086,#211087),(#211088,#211089),(#211090,#211091),
(#211092,#211093),(#211094,#211095),(#211096,#211097),(#211098,#211099),
(#211100,#211101),(#211102,#211103),(#211104,#211105),(#211106,#211107),
(#211108,#211109),(#211110,#211111),(#211112,#211113),(#211114,#211115),
(#211116,#211117),(#211118,#211119),(#211120,#211121),(#211122,#211123),
(#211124,#211125),(#211126,#211127),(#211128,#211129),(#211130,#211131),
(#211132,#211133),(#211134,#211135),(#211136,#211137),(#211138,#211139),
(#211140,#211141),(#211142,#211143),(#211144,#211145),(#211146,#211147),
(#211148,#211149),(#211150,#211151),(#211152,#211153),(#211154,#211155),
(#211156,#211157),(#211158,#211159),(#211160,#211161),(#211162,#211163),
(#211164,#211165),(#211166,#211167),(#211168,#211169),(#211170,#211171),
(#211172,#211173),(#211174,#211175),(#211176,#211177),(#211178,#211179),
(#211180,#211181),(#211182,#211183),(#211184,#211185),(#211186,#211187),
(#211188,#211189),(#211190,#211191),(#211192,#211193),(#211194,#211195),
(#211196,#211197),(#211198,#211199),(#211200,#211201),(#211202,#211203),
(#211204,#211205),(#211206,#211207),(#211208,#211209),(#211210,#211211),
(#211212,#211213),(#211214,#211215),(#211216,#211217),(#211218,#211219),
(#211220,#211221),(#211222,#211223),(#211224,#211225),(#211226,#211227),
(#211228,#211229),(#211230,#211231),(#211232,#211233),(#211234,#211235),
(#211236,#211237),(#211238,#211239),(#211240,#211241),(#211242,#211243),
(#211244,#211245),(#211246,#211247),(#211248,#211249),(#211250,#211251),
(#211252,#211253),(#211254,#211255),(#211256,#211257),(#211258,#211259),
(#211260,#211261),(#211262,#211263),(#211264,#211265),(#211266,#211267),
(#211268,#211269),(#211270,#211271),(#211272,#211273),(#211274,#211275),
(#211276,#211277),(#211278,#211279),(#211280,#211281),(#211282,#211283),
(#211284,#211285),(#211286,#211287),(#211288,#211289),(#211290,#211291),
(#211292,#211293),(#211294,#211295),(#211296,#211297),(#211298,#211299),
(#211300,#211301),(#211302,#211303),(#211304,#211305),(#211306,#211307),
(#211308,#211309),(#211310,#211311),(#211312,#211313),(#211314,#211315),
(#211316,#211317),(#211318,#211319),(#211320,#211321),(#211322,#211323),
(#211324,#211325),(#211326,#211327),(#211328,#211329),(#211330,#211331),
(#211332,#211333),(#211334,#211335),(#211336,#211337),(#211338,#211339),
(#211340,#211341),(#211342,#211343),(#211344,#211345),(#211346,#211347),
(#211348,#211349),(#211350,#211351),(#211352,#211353),(#211354,#211355),
(#211356,#211357),(#211358,#211359),(#211360,#211361),(#211362,#211363),
(#211364,#211365),(#211366,#211367),(#211368,#211369),(#211370,#211371),
(#211372,#211373),(#211374,#211375),(#211376,#211377),(#211378,#211379),
(#211380,#211381),(#211382,#211383),(#211384,#211385),(#211386,#211387),
(#211388,#211389),(#211390,#211391)),.UNSPECIFIED.,.F.,.F.,.F.)
B_SPLINE_SURFACE_WITH_KNOTS((6,1,1,1,1,1,1,1,1,1,1,1,1,1,1,1,1,1,1,1,1,
1,1,1,1,1,1,1,1,1,1,1,1,1,1,1,1,1,1,1,1,1,1,1,1,1,1,1,1,1,1,1,1,1,1,1,1,
1,1,1,1,1,1,1,1,1,1,1,1,1,1,1,1,1,1,1,1,1,1,1,1,1,1,1,1,1,1,1,1,1,1,1,1,
1,1,1,1,1,1,1,1,1,1,1,1,1,1,1,1,1,1,1,1,1,1,1,1,1,1,1,1,1,1,1,1,1,1,1,1,
1,1,1,1,1,1,1,1,1,1,1,1,1,1,1,1,1,1,1,1,1,1,1,1,1,1,1,1,1,1,1,1,1,1,1,1,
1,1,1,1,1,1,1,1,1,1,1,1,1,1,1,1,1,1,1,1,1,1,1,1,1,1,1,1,1,1,1,1,1,1,1,6),
(2,2),(0.,0.005,0.01,0.015,0.02,0.025,0.03,0.035,0.04,0.045,0.05,0.055,
0.06,0.065,0.07,0.075,0.08,0.085,0.09,0.095,0.1,0.105,0.11,0.115,0.12,0.125,
0.13,0.135,0.14,0.145,0.15,0.155,0.16,0.165,0.17,0.175,0.18,0.185,0.19,
0.195,0.2,0.205,0.21,0.215,0.22,0.225,0.23,0.235,0.24,0.245,0.25,0.255,
0.26,0.265,0.27,0.275,0.28,0.285,0.29,0.295,0.3,0.305,0.31,0.315,0.32,0.325,
0.33,0.335,0.34,0.345,0.35,0.355,0.36,0.365,0.37,0.375,0.38,0.385,0.39,
0.395,0.4,0.405,0.41,0.415,0.42,0.425,0.43,0.435,0.44,0.445,0.45,0.455,
0.46,0.465,0.47,0.475,0.48,0.485,0.49,0.495,0.5,0.505,0.51,0.515,0.52,0.525,
0.53,0.535,0.54,0.545,0.55,0.555,0.56,0.565,0.57,0.575,0.58,0.585,0.59,
0.595,0.6,0.605,0.61,0.615,0.62,0.625,0.63,0.635,0.64,0.645,0.65,0.655,
0.66,0.665,0.67,0.675,0.68,0.685,0.690000000000001,0.695000000000001,0.700000000000001,
0.705000000000001,0.710000000000001,0.715000000000001,0.720000000000001,
0.725000000000001,0.730000000000001,0.735000000000001,0.740000000000001,
0.745000000000001,0.750000000000001,0.755000000000001,0.760000000000001,
0.765000000000001,0.770000000000001,0.775000000000001,0.780000000000001,
0.785000000000001,0.790000000000001,0.795000000000001,0.800000000000001,
0.805000000000001,0.810000000000001,0.815000000000001,0.820000000000001,
0.825000000000001,0.830000000000001,0.835000000000001,0.840000000000001,
0.845000000000001,0.850000000000001,0.855000000000001,0.860000000000001,
0.865000000000001,0.870000000000001,0.875000000000001,0.880000000000001,
0.885000000000001,0.890000000000001,0.895000000000001,0.900000000000001,
0.905000000000001,0.910000000000001,0.915000000000001,0.920000000000001,
0.925000000000001,0.930000000000001,0.935000000000001,0.940000000000001,
0.945000000000001,0.950000000000001,0.955000000000001,0.960000000000001,
0.965000000000001,0.970000000000001,0.975000000000001,0.980000000000001,
0.985000000000001,0.990000000000001,0.995000000000001,1.),(0.,1.2),
 .UNSPECIFIED.)
GEOMETRIC_REPRESENTATION_ITEM()
RATIONAL_B_SPLINE_SURFACE(((1.,1.),(1.,1.),(1.,1.),(1.,1.),(1.,1.),(1.,
1.),(1.,1.),(1.,1.),(1.,1.),(1.,1.),(1.,1.),(1.,1.),(1.,1.),(1.,1.),(1.,
1.),(1.,1.),(1.,1.),(1.,1.),(1.,1.),(1.,1.),(1.,1.),(1.,1.),(1.,1.),(1.,
1.),(1.,1.),(1.,1.),(1.,1.),(1.,1.),(1.,1.),(1.,1.),(1.,1.),(1.,1.),(1.,
1.),(1.,1.),(1.,1.),(1.,1.),(1.,1.),(1.,1.),(1.,1.),(1.,1.),(1.,1.),(1.,
1.),(1.,1.),(1.,1.),(1.,1.),(1.,1.),(1.,1.),(1.,1.),(1.,1.),(1.,1.),(1.,
1.),(1.,1.),(1.,1.),(1.,1.),(1.,1.),(1.,1.),(1.,1.),(1.,1.),(1.,1.),(1.,
1.),(1.,1.),(1.,1.),(1.,1.),(1.,1.),(1.,1.),(1.,1.),(1.,1.),(1.,1.),(1.,
1.),(1.,1.),(1.,1.),(1.,1.),(1.,1.),(1.,1.),(1.,1.),(1.,1.),(1.,1.),(1.,
1.),(1.,1.),(1.,1.),(1.,1.),(1.,1.),(1.,1.),(1.,1.),(1.,1.),(1.,1.),(1.,
1.),(1.,1.),(1.,1.),(1.,1.),(1.,1.),(1.,1.),(1.,1.),(1.,1.),(1.,1.),(1.,
1.),(1.,1.),(1.,1.),(1.,1.),(1.,1.),(1.,1.),(1.,1.),(1.,1.),(1.,1.),(1.,
1.),(1.,1.),(1.,1.),(1.,1.),(1.,1.),(1.,1.),(1.,1.),(1.,1.),(1.,1.),(1.,
1.),(1.,1.),(1.,1.),(1.,1.),(1.,1.),(1.,1.),(1.,1.),(1.,1.),(1.,1.),(1.,
1.),(1.,1.),(1.,1.),(1.,1.),(1.,1.),(1.,1.),(1.,1.),(1.,1.),(1.,1.),(1.,
1.),(1.,1.),(1.,1.),(1.,1.),(1.,1.),(1.,1.),(1.,1.),(1.,1.),(1.,1.),(1.,
1.),(1.,1.),(1.,1.),(1.,1.),(1.,1.),(1.,1.),(1.,1.),(1.,1.),(1.,1.),(1.,
1.),(1.,1.),(1.,1.),(1.,1.),(1.,1.),(1.,1.),(1.,1.),(1.,1.),(1.,1.),(1.,
1.),(1.,1.),(1.,1.),(1.,1.),(1.,1.),(1.,1.),(1.,1.),(1.,1.),(1.,1.),(1.,
1.),(1.,1.),(1.,1.),(1.,1.),(1.,1.),(1.,1.),(1.,1.),(1.,1.),(1.,1.),(1.,
1.),(1.,1.),(1.,1.),(1.,1.),(1.,1.),(1.,1.),(1.,1.),(1.,1.),(1.,1.),(1.,
1.),(1.,1.),(1.,1.),(1.,1.),(1.,1.),(1.,1.),(1.,1.),(1.,1.),(1.,1.),(1.,
1.),(1.,1.),(1.,1.),(1.,1.),(1.,1.),(1.,1.),(1.,1.),(1.,1.),(1.,1.),(1.,
1.),(1.,1.)))
REPRESENTATION_ITEM('')
SURFACE()
);
#1069=(
BOUNDED_SURFACE()
B_SPLINE_SURFACE(5,1,((#211603,#211604),(#211605,#211606),(#211607,#211608),
(#211609,#211610),(#211611,#211612),(#211613,#211614),(#211615,#211616),
(#211617,#211618),(#211619,#211620),(#211621,#211622),(#211623,#211624),
(#211625,#211626),(#211627,#211628),(#211629,#211630),(#211631,#211632),
(#211633,#211634),(#211635,#211636),(#211637,#211638),(#211639,#211640),
(#211641,#211642),(#211643,#211644),(#211645,#211646),(#211647,#211648),
(#211649,#211650),(#211651,#211652),(#211653,#211654),(#211655,#211656),
(#211657,#211658),(#211659,#211660),(#211661,#211662),(#211663,#211664),
(#211665,#211666),(#211667,#211668),(#211669,#211670),(#211671,#211672),
(#211673,#211674),(#211675,#211676),(#211677,#211678),(#211679,#211680),
(#211681,#211682),(#211683,#211684),(#211685,#211686),(#211687,#211688),
(#211689,#211690),(#211691,#211692),(#211693,#211694),(#211695,#211696),
(#211697,#211698),(#211699,#211700),(#211701,#211702),(#211703,#211704),
(#211705,#211706),(#211707,#211708),(#211709,#211710),(#211711,#211712),
(#211713,#211714),(#211715,#211716),(#211717,#211718),(#211719,#211720),
(#211721,#211722),(#211723,#211724),(#211725,#211726),(#211727,#211728),
(#211729,#211730),(#211731,#211732),(#211733,#211734),(#211735,#211736),
(#211737,#211738),(#211739,#211740),(#211741,#211742),(#211743,#211744),
(#211745,#211746),(#211747,#211748),(#211749,#211750),(#211751,#211752),
(#211753,#211754),(#211755,#211756),(#211757,#211758),(#211759,#211760),
(#211761,#211762),(#211763,#211764),(#211765,#211766),(#211767,#211768),
(#211769,#211770),(#211771,#211772),(#211773,#211774),(#211775,#211776),
(#211777,#211778),(#211779,#211780),(#211781,#211782),(#211783,#211784),
(#211785,#211786),(#211787,#211788),(#211789,#211790),(#211791,#211792),
(#211793,#211794),(#211795,#211796),(#211797,#211798),(#211799,#211800),
(#211801,#211802),(#211803,#211804),(#211805,#211806),(#211807,#211808),
(#211809,#211810),(#211811,#211812),(#211813,#211814),(#211815,#211816),
(#211817,#211818),(#211819,#211820),(#211821,#211822),(#211823,#211824),
(#211825,#211826),(#211827,#211828),(#211829,#211830),(#211831,#211832),
(#211833,#211834),(#211835,#211836),(#211837,#211838),(#211839,#211840),
(#211841,#211842),(#211843,#211844),(#211845,#211846),(#211847,#211848),
(#211849,#211850),(#211851,#211852),(#211853,#211854),(#211855,#211856),
(#211857,#211858),(#211859,#211860),(#211861,#211862),(#211863,#211864),
(#211865,#211866),(#211867,#211868),(#211869,#211870),(#211871,#211872),
(#211873,#211874),(#211875,#211876),(#211877,#211878),(#211879,#211880),
(#211881,#211882),(#211883,#211884),(#211885,#211886),(#211887,#211888),
(#211889,#211890),(#211891,#211892),(#211893,#211894),(#211895,#211896),
(#211897,#211898),(#211899,#211900),(#211901,#211902),(#211903,#211904),
(#211905,#211906),(#211907,#211908),(#211909,#211910),(#211911,#211912),
(#211913,#211914),(#211915,#211916),(#211917,#211918),(#211919,#211920),
(#211921,#211922),(#211923,#211924),(#211925,#211926),(#211927,#211928),
(#211929,#211930),(#211931,#211932),(#211933,#211934),(#211935,#211936),
(#211937,#211938),(#211939,#211940),(#211941,#211942),(#211943,#211944),
(#211945,#211946),(#211947,#211948),(#211949,#211950),(#211951,#211952),
(#211953,#211954),(#211955,#211956),(#211957,#211958),(#211959,#211960),
(#211961,#211962),(#211963,#211964),(#211965,#211966),(#211967,#211968),
(#211969,#211970),(#211971,#211972),(#211973,#211974),(#211975,#211976),
(#211977,#211978),(#211979,#211980),(#211981,#211982),(#211983,#211984),
(#211985,#211986),(#211987,#211988),(#211989,#211990),(#211991,#211992),
(#211993,#211994),(#211995,#211996),(#211997,#211998),(#211999,#212000),
(#212001,#212002),(#212003,#212004),(#212005,#212006),(#212007,#212008),
(#212009,#212010),(#212011,#212012)),.UNSPECIFIED.,.F.,.F.,.F.)
B_SPLINE_SURFACE_WITH_KNOTS((6,1,1,1,1,1,1,1,1,1,1,1,1,1,1,1,1,1,1,1,1,
1,1,1,1,1,1,1,1,1,1,1,1,1,1,1,1,1,1,1,1,1,1,1,1,1,1,1,1,1,1,1,1,1,1,1,1,
1,1,1,1,1,1,1,1,1,1,1,1,1,1,1,1,1,1,1,1,1,1,1,1,1,1,1,1,1,1,1,1,1,1,1,1,
1,1,1,1,1,1,1,1,1,1,1,1,1,1,1,1,1,1,1,1,1,1,1,1,1,1,1,1,1,1,1,1,1,1,1,1,
1,1,1,1,1,1,1,1,1,1,1,1,1,1,1,1,1,1,1,1,1,1,1,1,1,1,1,1,1,1,1,1,1,1,1,1,
1,1,1,1,1,1,1,1,1,1,1,1,1,1,1,1,1,1,1,1,1,1,1,1,1,1,1,1,1,1,1,1,1,1,1,6),
(2,2),(-1.,-0.995000000000001,-0.990000000000001,-0.985000000000001,-0.980000000000001,
-0.975000000000001,-0.970000000000001,-0.965000000000001,-0.960000000000001,
-0.955000000000001,-0.950000000000001,-0.945000000000001,-0.940000000000001,
-0.935000000000001,-0.930000000000001,-0.925000000000001,-0.920000000000001,
-0.915000000000001,-0.910000000000001,-0.905000000000001,-0.900000000000001,
-0.895000000000001,-0.890000000000001,-0.885000000000001,-0.880000000000001,
-0.875000000000001,-0.870000000000001,-0.865000000000001,-0.860000000000001,
-0.855000000000001,-0.850000000000001,-0.845000000000001,-0.840000000000001,
-0.835000000000001,-0.830000000000001,-0.825000000000001,-0.820000000000001,
-0.815000000000001,-0.810000000000001,-0.805000000000001,-0.800000000000001,
-0.795000000000001,-0.790000000000001,-0.785000000000001,-0.780000000000001,
-0.775000000000001,-0.770000000000001,-0.765000000000001,-0.760000000000001,
-0.755000000000001,-0.750000000000001,-0.745000000000001,-0.740000000000001,
-0.735000000000001,-0.730000000000001,-0.725000000000001,-0.720000000000001,
-0.715000000000001,-0.710000000000001,-0.705000000000001,-0.700000000000001,
-0.695000000000001,-0.690000000000001,-0.685,-0.68,-0.675,-0.67,-0.665,
-0.66,-0.655,-0.65,-0.645,-0.64,-0.635,-0.63,-0.625,-0.62,-0.615,-0.61,
-0.605,-0.6,-0.595,-0.59,-0.585,-0.58,-0.575,-0.57,-0.565,-0.56,-0.555,
-0.55,-0.545,-0.54,-0.535,-0.53,-0.525,-0.52,-0.515,-0.51,-0.505,-0.5,-0.495,
-0.49,-0.485,-0.48,-0.475,-0.47,-0.465,-0.46,-0.455,-0.45,-0.445,-0.44,
-0.435,-0.43,-0.425,-0.42,-0.415,-0.41,-0.405,-0.4,-0.395,-0.39,-0.385,
-0.38,-0.375,-0.37,-0.365,-0.36,-0.355,-0.35,-0.345,-0.34,-0.335,-0.33,
-0.325,-0.32,-0.315,-0.31,-0.305,-0.3,-0.295,-0.29,-0.285,-0.28,-0.275,
-0.27,-0.265,-0.26,-0.255,-0.25,-0.245,-0.24,-0.235,-0.23,-0.225,-0.22,
-0.215,-0.21,-0.205,-0.2,-0.195,-0.19,-0.185,-0.18,-0.175,-0.17,-0.165,
-0.16,-0.155,-0.15,-0.145,-0.14,-0.135,-0.13,-0.125,-0.12,-0.115,-0.11,
-0.105,-0.1,-0.095,-0.09,-0.085,-0.08,-0.075,-0.07,-0.065,-0.06,-0.055,
-0.05,-0.045,-0.04,-0.035,-0.03,-0.025,-0.02,-0.015,-0.01,-0.005,0.),(0.,
1.2),.UNSPECIFIED.)
GEOMETRIC_REPRESENTATION_ITEM()
RATIONAL_B_SPLINE_SURFACE(((1.,1.),(1.,1.),(1.,1.),(1.,1.),(1.,1.),(1.,
1.),(1.,1.),(1.,1.),(1.,1.),(1.,1.),(1.,1.),(1.,1.),(1.,1.),(1.,1.),(1.,
1.),(1.,1.),(1.,1.),(1.,1.),(1.,1.),(1.,1.),(1.,1.),(1.,1.),(1.,1.),(1.,
1.),(1.,1.),(1.,1.),(1.,1.),(1.,1.),(1.,1.),(1.,1.),(1.,1.),(1.,1.),(1.,
1.),(1.,1.),(1.,1.),(1.,1.),(1.,1.),(1.,1.),(1.,1.),(1.,1.),(1.,1.),(1.,
1.),(1.,1.),(1.,1.),(1.,1.),(1.,1.),(1.,1.),(1.,1.),(1.,1.),(1.,1.),(1.,
1.),(1.,1.),(1.,1.),(1.,1.),(1.,1.),(1.,1.),(1.,1.),(1.,1.),(1.,1.),(1.,
1.),(1.,1.),(1.,1.),(1.,1.),(1.,1.),(1.,1.),(1.,1.),(1.,1.),(1.,1.),(1.,
1.),(1.,1.),(1.,1.),(1.,1.),(1.,1.),(1.,1.),(1.,1.),(1.,1.),(1.,1.),(1.,
1.),(1.,1.),(1.,1.),(1.,1.),(1.,1.),(1.,1.),(1.,1.),(1.,1.),(1.,1.),(1.,
1.),(1.,1.),(1.,1.),(1.,1.),(1.,1.),(1.,1.),(1.,1.),(1.,1.),(1.,1.),(1.,
1.),(1.,1.),(1.,1.),(1.,1.),(1.,1.),(1.,1.),(1.,1.),(1.,1.),(1.,1.),(1.,
1.),(1.,1.),(1.,1.),(1.,1.),(1.,1.),(1.,1.),(1.,1.),(1.,1.),(1.,1.),(1.,
1.),(1.,1.),(1.,1.),(1.,1.),(1.,1.),(1.,1.),(1.,1.),(1.,1.),(1.,1.),(1.,
1.),(1.,1.),(1.,1.),(1.,1.),(1.,1.),(1.,1.),(1.,1.),(1.,1.),(1.,1.),(1.,
1.),(1.,1.),(1.,1.),(1.,1.),(1.,1.),(1.,1.),(1.,1.),(1.,1.),(1.,1.),(1.,
1.),(1.,1.),(1.,1.),(1.,1.),(1.,1.),(1.,1.),(1.,1.),(1.,1.),(1.,1.),(1.,
1.),(1.,1.),(1.,1.),(1.,1.),(1.,1.),(1.,1.),(1.,1.),(1.,1.),(1.,1.),(1.,
1.),(1.,1.),(1.,1.),(1.,1.),(1.,1.),(1.,1.),(1.,1.),(1.,1.),(1.,1.),(1.,
1.),(1.,1.),(1.,1.),(1.,1.),(1.,1.),(1.,1.),(1.,1.),(1.,1.),(1.,1.),(1.,
1.),(1.,1.),(1.,1.),(1.,1.),(1.,1.),(1.,1.),(1.,1.),(1.,1.),(1.,1.),(1.,
1.),(1.,1.),(1.,1.),(1.,1.),(1.,1.),(1.,1.),(1.,1.),(1.,1.),(1.,1.),(1.,
1.),(1.,1.),(1.,1.),(1.,1.),(1.,1.),(1.,1.),(1.,1.),(1.,1.),(1.,1.),(1.,
1.),(1.,1.)))
REPRESENTATION_ITEM('')
SURFACE()
);
#1070=(
BOUNDED_SURFACE()
B_SPLINE_SURFACE(5,1,((#212220,#212221),(#212222,#212223),(#212224,#212225),
(#212226,#212227),(#212228,#212229),(#212230,#212231),(#212232,#212233),
(#212234,#212235),(#212236,#212237),(#212238,#212239),(#212240,#212241),
(#212242,#212243),(#212244,#212245),(#212246,#212247),(#212248,#212249),
(#212250,#212251),(#212252,#212253),(#212254,#212255),(#212256,#212257),
(#212258,#212259),(#212260,#212261),(#212262,#212263),(#212264,#212265),
(#212266,#212267),(#212268,#212269),(#212270,#212271),(#212272,#212273),
(#212274,#212275),(#212276,#212277),(#212278,#212279),(#212280,#212281),
(#212282,#212283),(#212284,#212285),(#212286,#212287),(#212288,#212289),
(#212290,#212291),(#212292,#212293),(#212294,#212295),(#212296,#212297),
(#212298,#212299),(#212300,#212301),(#212302,#212303),(#212304,#212305),
(#212306,#212307),(#212308,#212309),(#212310,#212311),(#212312,#212313),
(#212314,#212315),(#212316,#212317),(#212318,#212319),(#212320,#212321),
(#212322,#212323),(#212324,#212325),(#212326,#212327),(#212328,#212329),
(#212330,#212331),(#212332,#212333),(#212334,#212335),(#212336,#212337),
(#212338,#212339),(#212340,#212341),(#212342,#212343),(#212344,#212345),
(#212346,#212347),(#212348,#212349),(#212350,#212351),(#212352,#212353),
(#212354,#212355),(#212356,#212357),(#212358,#212359),(#212360,#212361),
(#212362,#212363),(#212364,#212365),(#212366,#212367),(#212368,#212369),
(#212370,#212371),(#212372,#212373),(#212374,#212375),(#212376,#212377),
(#212378,#212379),(#212380,#212381),(#212382,#212383),(#212384,#212385),
(#212386,#212387),(#212388,#212389),(#212390,#212391),(#212392,#212393),
(#212394,#212395),(#212396,#212397),(#212398,#212399),(#212400,#212401),
(#212402,#212403),(#212404,#212405),(#212406,#212407),(#212408,#212409),
(#212410,#212411),(#212412,#212413),(#212414,#212415),(#212416,#212417),
(#212418,#212419),(#212420,#212421),(#212422,#212423),(#212424,#212425),
(#212426,#212427),(#212428,#212429),(#212430,#212431),(#212432,#212433),
(#212434,#212435),(#212436,#212437),(#212438,#212439),(#212440,#212441),
(#212442,#212443),(#212444,#212445),(#212446,#212447),(#212448,#212449),
(#212450,#212451),(#212452,#212453),(#212454,#212455),(#212456,#212457),
(#212458,#212459),(#212460,#212461),(#212462,#212463),(#212464,#212465),
(#212466,#212467),(#212468,#212469),(#212470,#212471),(#212472,#212473),
(#212474,#212475),(#212476,#212477),(#212478,#212479),(#212480,#212481),
(#212482,#212483),(#212484,#212485),(#212486,#212487),(#212488,#212489),
(#212490,#212491),(#212492,#212493),(#212494,#212495),(#212496,#212497),
(#212498,#212499),(#212500,#212501),(#212502,#212503),(#212504,#212505),
(#212506,#212507),(#212508,#212509),(#212510,#212511),(#212512,#212513),
(#212514,#212515),(#212516,#212517),(#212518,#212519),(#212520,#212521),
(#212522,#212523),(#212524,#212525),(#212526,#212527),(#212528,#212529),
(#212530,#212531),(#212532,#212533),(#212534,#212535),(#212536,#212537),
(#212538,#212539),(#212540,#212541),(#212542,#212543),(#212544,#212545),
(#212546,#212547),(#212548,#212549),(#212550,#212551),(#212552,#212553),
(#212554,#212555),(#212556,#212557),(#212558,#212559),(#212560,#212561),
(#212562,#212563),(#212564,#212565),(#212566,#212567),(#212568,#212569),
(#212570,#212571),(#212572,#212573),(#212574,#212575),(#212576,#212577),
(#212578,#212579),(#212580,#212581),(#212582,#212583),(#212584,#212585),
(#212586,#212587),(#212588,#212589),(#212590,#212591),(#212592,#212593),
(#212594,#212595),(#212596,#212597),(#212598,#212599),(#212600,#212601),
(#212602,#212603),(#212604,#212605),(#212606,#212607),(#212608,#212609),
(#212610,#212611),(#212612,#212613),(#212614,#212615),(#212616,#212617),
(#212618,#212619),(#212620,#212621),(#212622,#212623),(#212624,#212625),
(#212626,#212627),(#212628,#212629)),.UNSPECIFIED.,.F.,.F.,.F.)
B_SPLINE_SURFACE_WITH_KNOTS((6,1,1,1,1,1,1,1,1,1,1,1,1,1,1,1,1,1,1,1,1,
1,1,1,1,1,1,1,1,1,1,1,1,1,1,1,1,1,1,1,1,1,1,1,1,1,1,1,1,1,1,1,1,1,1,1,1,
1,1,1,1,1,1,1,1,1,1,1,1,1,1,1,1,1,1,1,1,1,1,1,1,1,1,1,1,1,1,1,1,1,1,1,1,
1,1,1,1,1,1,1,1,1,1,1,1,1,1,1,1,1,1,1,1,1,1,1,1,1,1,1,1,1,1,1,1,1,1,1,1,
1,1,1,1,1,1,1,1,1,1,1,1,1,1,1,1,1,1,1,1,1,1,1,1,1,1,1,1,1,1,1,1,1,1,1,1,
1,1,1,1,1,1,1,1,1,1,1,1,1,1,1,1,1,1,1,1,1,1,1,1,1,1,1,1,1,1,1,1,1,1,1,6),
(2,2),(0.,0.005,0.01,0.015,0.02,0.025,0.03,0.035,0.04,0.045,0.05,0.055,
0.06,0.065,0.07,0.075,0.08,0.085,0.09,0.095,0.1,0.105,0.11,0.115,0.12,0.125,
0.13,0.135,0.14,0.145,0.15,0.155,0.16,0.165,0.17,0.175,0.18,0.185,0.19,
0.195,0.2,0.205,0.21,0.215,0.22,0.225,0.23,0.235,0.24,0.245,0.25,0.255,
0.26,0.265,0.27,0.275,0.28,0.285,0.29,0.295,0.3,0.305,0.31,0.315,0.32,0.325,
0.33,0.335,0.34,0.345,0.35,0.355,0.36,0.365,0.37,0.375,0.38,0.385,0.39,
0.395,0.4,0.405,0.41,0.415,0.42,0.425,0.43,0.435,0.44,0.445,0.45,0.455,
0.46,0.465,0.47,0.475,0.48,0.485,0.49,0.495,0.5,0.505,0.51,0.515,0.52,0.525,
0.53,0.535,0.54,0.545,0.55,0.555,0.56,0.565,0.57,0.575,0.58,0.585,0.59,
0.595,0.6,0.605,0.61,0.615,0.62,0.625,0.63,0.635,0.64,0.645,0.65,0.655,
0.66,0.665,0.67,0.675,0.68,0.685,0.690000000000001,0.695000000000001,0.700000000000001,
0.705000000000001,0.710000000000001,0.715000000000001,0.720000000000001,
0.725000000000001,0.730000000000001,0.735000000000001,0.740000000000001,
0.745000000000001,0.750000000000001,0.755000000000001,0.760000000000001,
0.765000000000001,0.770000000000001,0.775000000000001,0.780000000000001,
0.785000000000001,0.790000000000001,0.795000000000001,0.800000000000001,
0.805000000000001,0.810000000000001,0.815000000000001,0.820000000000001,
0.825000000000001,0.830000000000001,0.835000000000001,0.840000000000001,
0.845000000000001,0.850000000000001,0.855000000000001,0.860000000000001,
0.865000000000001,0.870000000000001,0.875000000000001,0.880000000000001,
0.885000000000001,0.890000000000001,0.895000000000001,0.900000000000001,
0.905000000000001,0.910000000000001,0.915000000000001,0.920000000000001,
0.925000000000001,0.930000000000001,0.935000000000001,0.940000000000001,
0.945000000000001,0.950000000000001,0.955000000000001,0.960000000000001,
0.965000000000001,0.970000000000001,0.975000000000001,0.980000000000001,
0.985000000000001,0.990000000000001,0.995000000000001,1.),(0.,1.2),
 .UNSPECIFIED.)
GEOMETRIC_REPRESENTATION_ITEM()
RATIONAL_B_SPLINE_SURFACE(((1.,1.),(1.,1.),(1.,1.),(1.,1.),(1.,1.),(1.,
1.),(1.,1.),(1.,1.),(1.,1.),(1.,1.),(1.,1.),(1.,1.),(1.,1.),(1.,1.),(1.,
1.),(1.,1.),(1.,1.),(1.,1.),(1.,1.),(1.,1.),(1.,1.),(1.,1.),(1.,1.),(1.,
1.),(1.,1.),(1.,1.),(1.,1.),(1.,1.),(1.,1.),(1.,1.),(1.,1.),(1.,1.),(1.,
1.),(1.,1.),(1.,1.),(1.,1.),(1.,1.),(1.,1.),(1.,1.),(1.,1.),(1.,1.),(1.,
1.),(1.,1.),(1.,1.),(1.,1.),(1.,1.),(1.,1.),(1.,1.),(1.,1.),(1.,1.),(1.,
1.),(1.,1.),(1.,1.),(1.,1.),(1.,1.),(1.,1.),(1.,1.),(1.,1.),(1.,1.),(1.,
1.),(1.,1.),(1.,1.),(1.,1.),(1.,1.),(1.,1.),(1.,1.),(1.,1.),(1.,1.),(1.,
1.),(1.,1.),(1.,1.),(1.,1.),(1.,1.),(1.,1.),(1.,1.),(1.,1.),(1.,1.),(1.,
1.),(1.,1.),(1.,1.),(1.,1.),(1.,1.),(1.,1.),(1.,1.),(1.,1.),(1.,1.),(1.,
1.),(1.,1.),(1.,1.),(1.,1.),(1.,1.),(1.,1.),(1.,1.),(1.,1.),(1.,1.),(1.,
1.),(1.,1.),(1.,1.),(1.,1.),(1.,1.),(1.,1.),(1.,1.),(1.,1.),(1.,1.),(1.,
1.),(1.,1.),(1.,1.),(1.,1.),(1.,1.),(1.,1.),(1.,1.),(1.,1.),(1.,1.),(1.,
1.),(1.,1.),(1.,1.),(1.,1.),(1.,1.),(1.,1.),(1.,1.),(1.,1.),(1.,1.),(1.,
1.),(1.,1.),(1.,1.),(1.,1.),(1.,1.),(1.,1.),(1.,1.),(1.,1.),(1.,1.),(1.,
1.),(1.,1.),(1.,1.),(1.,1.),(1.,1.),(1.,1.),(1.,1.),(1.,1.),(1.,1.),(1.,
1.),(1.,1.),(1.,1.),(1.,1.),(1.,1.),(1.,1.),(1.,1.),(1.,1.),(1.,1.),(1.,
1.),(1.,1.),(1.,1.),(1.,1.),(1.,1.),(1.,1.),(1.,1.),(1.,1.),(1.,1.),(1.,
1.),(1.,1.),(1.,1.),(1.,1.),(1.,1.),(1.,1.),(1.,1.),(1.,1.),(1.,1.),(1.,
1.),(1.,1.),(1.,1.),(1.,1.),(1.,1.),(1.,1.),(1.,1.),(1.,1.),(1.,1.),(1.,
1.),(1.,1.),(1.,1.),(1.,1.),(1.,1.),(1.,1.),(1.,1.),(1.,1.),(1.,1.),(1.,
1.),(1.,1.),(1.,1.),(1.,1.),(1.,1.),(1.,1.),(1.,1.),(1.,1.),(1.,1.),(1.,
1.),(1.,1.),(1.,1.),(1.,1.),(1.,1.),(1.,1.),(1.,1.),(1.,1.),(1.,1.),(1.,
1.),(1.,1.)))
REPRESENTATION_ITEM('')
SURFACE()
);
#1071=(
BOUNDED_SURFACE()
B_SPLINE_SURFACE(5,1,((#212841,#212842),(#212843,#212844),(#212845,#212846),
(#212847,#212848),(#212849,#212850),(#212851,#212852),(#212853,#212854),
(#212855,#212856),(#212857,#212858),(#212859,#212860),(#212861,#212862),
(#212863,#212864),(#212865,#212866),(#212867,#212868),(#212869,#212870),
(#212871,#212872),(#212873,#212874),(#212875,#212876),(#212877,#212878),
(#212879,#212880),(#212881,#212882),(#212883,#212884),(#212885,#212886),
(#212887,#212888),(#212889,#212890),(#212891,#212892),(#212893,#212894),
(#212895,#212896),(#212897,#212898),(#212899,#212900),(#212901,#212902),
(#212903,#212904),(#212905,#212906),(#212907,#212908),(#212909,#212910),
(#212911,#212912),(#212913,#212914),(#212915,#212916),(#212917,#212918),
(#212919,#212920),(#212921,#212922),(#212923,#212924),(#212925,#212926),
(#212927,#212928),(#212929,#212930),(#212931,#212932),(#212933,#212934),
(#212935,#212936),(#212937,#212938),(#212939,#212940),(#212941,#212942),
(#212943,#212944),(#212945,#212946),(#212947,#212948),(#212949,#212950),
(#212951,#212952),(#212953,#212954),(#212955,#212956),(#212957,#212958),
(#212959,#212960),(#212961,#212962),(#212963,#212964),(#212965,#212966),
(#212967,#212968),(#212969,#212970),(#212971,#212972),(#212973,#212974),
(#212975,#212976),(#212977,#212978),(#212979,#212980),(#212981,#212982),
(#212983,#212984),(#212985,#212986),(#212987,#212988),(#212989,#212990),
(#212991,#212992),(#212993,#212994),(#212995,#212996),(#212997,#212998),
(#212999,#213000),(#213001,#213002),(#213003,#213004),(#213005,#213006),
(#213007,#213008),(#213009,#213010),(#213011,#213012),(#213013,#213014),
(#213015,#213016),(#213017,#213018),(#213019,#213020),(#213021,#213022),
(#213023,#213024),(#213025,#213026),(#213027,#213028),(#213029,#213030),
(#213031,#213032),(#213033,#213034),(#213035,#213036),(#213037,#213038),
(#213039,#213040),(#213041,#213042),(#213043,#213044),(#213045,#213046),
(#213047,#213048),(#213049,#213050),(#213051,#213052),(#213053,#213054),
(#213055,#213056),(#213057,#213058),(#213059,#213060),(#213061,#213062),
(#213063,#213064),(#213065,#213066),(#213067,#213068),(#213069,#213070),
(#213071,#213072),(#213073,#213074),(#213075,#213076),(#213077,#213078),
(#213079,#213080),(#213081,#213082),(#213083,#213084),(#213085,#213086),
(#213087,#213088),(#213089,#213090),(#213091,#213092),(#213093,#213094),
(#213095,#213096),(#213097,#213098),(#213099,#213100),(#213101,#213102),
(#213103,#213104),(#213105,#213106),(#213107,#213108),(#213109,#213110),
(#213111,#213112),(#213113,#213114),(#213115,#213116),(#213117,#213118),
(#213119,#213120),(#213121,#213122),(#213123,#213124),(#213125,#213126),
(#213127,#213128),(#213129,#213130),(#213131,#213132),(#213133,#213134),
(#213135,#213136),(#213137,#213138),(#213139,#213140),(#213141,#213142),
(#213143,#213144),(#213145,#213146),(#213147,#213148),(#213149,#213150),
(#213151,#213152),(#213153,#213154),(#213155,#213156),(#213157,#213158),
(#213159,#213160),(#213161,#213162),(#213163,#213164),(#213165,#213166),
(#213167,#213168),(#213169,#213170),(#213171,#213172),(#213173,#213174),
(#213175,#213176),(#213177,#213178),(#213179,#213180),(#213181,#213182),
(#213183,#213184),(#213185,#213186),(#213187,#213188),(#213189,#213190),
(#213191,#213192),(#213193,#213194),(#213195,#213196),(#213197,#213198),
(#213199,#213200),(#213201,#213202),(#213203,#213204),(#213205,#213206),
(#213207,#213208),(#213209,#213210),(#213211,#213212),(#213213,#213214),
(#213215,#213216),(#213217,#213218),(#213219,#213220),(#213221,#213222),
(#213223,#213224),(#213225,#213226),(#213227,#213228),(#213229,#213230),
(#213231,#213232),(#213233,#213234),(#213235,#213236),(#213237,#213238),
(#213239,#213240),(#213241,#213242),(#213243,#213244),(#213245,#213246),
(#213247,#213248),(#213249,#213250)),.UNSPECIFIED.,.F.,.F.,.F.)
B_SPLINE_SURFACE_WITH_KNOTS((6,1,1,1,1,1,1,1,1,1,1,1,1,1,1,1,1,1,1,1,1,
1,1,1,1,1,1,1,1,1,1,1,1,1,1,1,1,1,1,1,1,1,1,1,1,1,1,1,1,1,1,1,1,1,1,1,1,
1,1,1,1,1,1,1,1,1,1,1,1,1,1,1,1,1,1,1,1,1,1,1,1,1,1,1,1,1,1,1,1,1,1,1,1,
1,1,1,1,1,1,1,1,1,1,1,1,1,1,1,1,1,1,1,1,1,1,1,1,1,1,1,1,1,1,1,1,1,1,1,1,
1,1,1,1,1,1,1,1,1,1,1,1,1,1,1,1,1,1,1,1,1,1,1,1,1,1,1,1,1,1,1,1,1,1,1,1,
1,1,1,1,1,1,1,1,1,1,1,1,1,1,1,1,1,1,1,1,1,1,1,1,1,1,1,1,1,1,1,1,1,1,1,6),
(2,2),(-1.,-0.995000000000001,-0.990000000000001,-0.985000000000001,-0.980000000000001,
-0.975000000000001,-0.970000000000001,-0.965000000000001,-0.960000000000001,
-0.955000000000001,-0.950000000000001,-0.945000000000001,-0.940000000000001,
-0.935000000000001,-0.930000000000001,-0.925000000000001,-0.920000000000001,
-0.915000000000001,-0.910000000000001,-0.905000000000001,-0.900000000000001,
-0.895000000000001,-0.890000000000001,-0.885000000000001,-0.880000000000001,
-0.875000000000001,-0.870000000000001,-0.865000000000001,-0.860000000000001,
-0.855000000000001,-0.850000000000001,-0.845000000000001,-0.840000000000001,
-0.835000000000001,-0.830000000000001,-0.825000000000001,-0.820000000000001,
-0.815000000000001,-0.810000000000001,-0.805000000000001,-0.800000000000001,
-0.795000000000001,-0.790000000000001,-0.785000000000001,-0.780000000000001,
-0.775000000000001,-0.770000000000001,-0.765000000000001,-0.760000000000001,
-0.755000000000001,-0.750000000000001,-0.745000000000001,-0.740000000000001,
-0.735000000000001,-0.730000000000001,-0.725000000000001,-0.720000000000001,
-0.715000000000001,-0.710000000000001,-0.705000000000001,-0.700000000000001,
-0.695000000000001,-0.690000000000001,-0.685,-0.68,-0.675,-0.67,-0.665,
-0.66,-0.655,-0.65,-0.645,-0.64,-0.635,-0.63,-0.625,-0.62,-0.615,-0.61,
-0.605,-0.6,-0.595,-0.59,-0.585,-0.58,-0.575,-0.57,-0.565,-0.56,-0.555,
-0.55,-0.545,-0.54,-0.535,-0.53,-0.525,-0.52,-0.515,-0.51,-0.505,-0.5,-0.495,
-0.49,-0.485,-0.48,-0.475,-0.47,-0.465,-0.46,-0.455,-0.45,-0.445,-0.44,
-0.435,-0.43,-0.425,-0.42,-0.415,-0.41,-0.405,-0.4,-0.395,-0.39,-0.385,
-0.38,-0.375,-0.37,-0.365,-0.36,-0.355,-0.35,-0.345,-0.34,-0.335,-0.33,
-0.325,-0.32,-0.315,-0.31,-0.305,-0.3,-0.295,-0.29,-0.285,-0.28,-0.275,
-0.27,-0.265,-0.26,-0.255,-0.25,-0.245,-0.24,-0.235,-0.23,-0.225,-0.22,
-0.215,-0.21,-0.205,-0.2,-0.195,-0.19,-0.185,-0.18,-0.175,-0.17,-0.165,
-0.16,-0.155,-0.15,-0.145,-0.14,-0.135,-0.13,-0.125,-0.12,-0.115,-0.11,
-0.105,-0.1,-0.095,-0.09,-0.085,-0.08,-0.075,-0.07,-0.065,-0.06,-0.055,
-0.05,-0.045,-0.04,-0.035,-0.03,-0.025,-0.02,-0.015,-0.01,-0.005,0.),(0.,
1.2),.UNSPECIFIED.)
GEOMETRIC_REPRESENTATION_ITEM()
RATIONAL_B_SPLINE_SURFACE(((1.,1.),(1.,1.),(1.,1.),(1.,1.),(1.,1.),(1.,
1.),(1.,1.),(1.,1.),(1.,1.),(1.,1.),(1.,1.),(1.,1.),(1.,1.),(1.,1.),(1.,
1.),(1.,1.),(1.,1.),(1.,1.),(1.,1.),(1.,1.),(1.,1.),(1.,1.),(1.,1.),(1.,
1.),(1.,1.),(1.,1.),(1.,1.),(1.,1.),(1.,1.),(1.,1.),(1.,1.),(1.,1.),(1.,
1.),(1.,1.),(1.,1.),(1.,1.),(1.,1.),(1.,1.),(1.,1.),(1.,1.),(1.,1.),(1.,
1.),(1.,1.),(1.,1.),(1.,1.),(1.,1.),(1.,1.),(1.,1.),(1.,1.),(1.,1.),(1.,
1.),(1.,1.),(1.,1.),(1.,1.),(1.,1.),(1.,1.),(1.,1.),(1.,1.),(1.,1.),(1.,
1.),(1.,1.),(1.,1.),(1.,1.),(1.,1.),(1.,1.),(1.,1.),(1.,1.),(1.,1.),(1.,
1.),(1.,1.),(1.,1.),(1.,1.),(1.,1.),(1.,1.),(1.,1.),(1.,1.),(1.,1.),(1.,
1.),(1.,1.),(1.,1.),(1.,1.),(1.,1.),(1.,1.),(1.,1.),(1.,1.),(1.,1.),(1.,
1.),(1.,1.),(1.,1.),(1.,1.),(1.,1.),(1.,1.),(1.,1.),(1.,1.),(1.,1.),(1.,
1.),(1.,1.),(1.,1.),(1.,1.),(1.,1.),(1.,1.),(1.,1.),(1.,1.),(1.,1.),(1.,
1.),(1.,1.),(1.,1.),(1.,1.),(1.,1.),(1.,1.),(1.,1.),(1.,1.),(1.,1.),(1.,
1.),(1.,1.),(1.,1.),(1.,1.),(1.,1.),(1.,1.),(1.,1.),(1.,1.),(1.,1.),(1.,
1.),(1.,1.),(1.,1.),(1.,1.),(1.,1.),(1.,1.),(1.,1.),(1.,1.),(1.,1.),(1.,
1.),(1.,1.),(1.,1.),(1.,1.),(1.,1.),(1.,1.),(1.,1.),(1.,1.),(1.,1.),(1.,
1.),(1.,1.),(1.,1.),(1.,1.),(1.,1.),(1.,1.),(1.,1.),(1.,1.),(1.,1.),(1.,
1.),(1.,1.),(1.,1.),(1.,1.),(1.,1.),(1.,1.),(1.,1.),(1.,1.),(1.,1.),(1.,
1.),(1.,1.),(1.,1.),(1.,1.),(1.,1.),(1.,1.),(1.,1.),(1.,1.),(1.,1.),(1.,
1.),(1.,1.),(1.,1.),(1.,1.),(1.,1.),(1.,1.),(1.,1.),(1.,1.),(1.,1.),(1.,
1.),(1.,1.),(1.,1.),(1.,1.),(1.,1.),(1.,1.),(1.,1.),(1.,1.),(1.,1.),(1.,
1.),(1.,1.),(1.,1.),(1.,1.),(1.,1.),(1.,1.),(1.,1.),(1.,1.),(1.,1.),(1.,
1.),(1.,1.),(1.,1.),(1.,1.),(1.,1.),(1.,1.),(1.,1.),(1.,1.),(1.,1.),(1.,
1.),(1.,1.)))
REPRESENTATION_ITEM('')
SURFACE()
);
#1072=(
BOUNDED_SURFACE()
B_SPLINE_SURFACE(5,1,((#213458,#213459),(#213460,#213461),(#213462,#213463),
(#213464,#213465),(#213466,#213467),(#213468,#213469),(#213470,#213471),
(#213472,#213473),(#213474,#213475),(#213476,#213477),(#213478,#213479),
(#213480,#213481),(#213482,#213483),(#213484,#213485),(#213486,#213487),
(#213488,#213489),(#213490,#213491),(#213492,#213493),(#213494,#213495),
(#213496,#213497),(#213498,#213499),(#213500,#213501),(#213502,#213503),
(#213504,#213505),(#213506,#213507),(#213508,#213509),(#213510,#213511),
(#213512,#213513),(#213514,#213515),(#213516,#213517),(#213518,#213519),
(#213520,#213521),(#213522,#213523),(#213524,#213525),(#213526,#213527),
(#213528,#213529),(#213530,#213531),(#213532,#213533),(#213534,#213535),
(#213536,#213537),(#213538,#213539),(#213540,#213541),(#213542,#213543),
(#213544,#213545),(#213546,#213547),(#213548,#213549),(#213550,#213551),
(#213552,#213553),(#213554,#213555),(#213556,#213557),(#213558,#213559),
(#213560,#213561),(#213562,#213563),(#213564,#213565),(#213566,#213567),
(#213568,#213569),(#213570,#213571),(#213572,#213573),(#213574,#213575),
(#213576,#213577),(#213578,#213579),(#213580,#213581),(#213582,#213583),
(#213584,#213585),(#213586,#213587),(#213588,#213589),(#213590,#213591),
(#213592,#213593),(#213594,#213595),(#213596,#213597),(#213598,#213599),
(#213600,#213601),(#213602,#213603),(#213604,#213605),(#213606,#213607),
(#213608,#213609),(#213610,#213611),(#213612,#213613),(#213614,#213615),
(#213616,#213617),(#213618,#213619),(#213620,#213621),(#213622,#213623),
(#213624,#213625),(#213626,#213627),(#213628,#213629),(#213630,#213631),
(#213632,#213633),(#213634,#213635),(#213636,#213637),(#213638,#213639),
(#213640,#213641),(#213642,#213643),(#213644,#213645),(#213646,#213647),
(#213648,#213649),(#213650,#213651),(#213652,#213653),(#213654,#213655),
(#213656,#213657),(#213658,#213659),(#213660,#213661),(#213662,#213663),
(#213664,#213665),(#213666,#213667),(#213668,#213669),(#213670,#213671),
(#213672,#213673),(#213674,#213675),(#213676,#213677),(#213678,#213679),
(#213680,#213681),(#213682,#213683),(#213684,#213685),(#213686,#213687),
(#213688,#213689),(#213690,#213691),(#213692,#213693),(#213694,#213695),
(#213696,#213697),(#213698,#213699),(#213700,#213701),(#213702,#213703),
(#213704,#213705),(#213706,#213707),(#213708,#213709),(#213710,#213711),
(#213712,#213713),(#213714,#213715),(#213716,#213717),(#213718,#213719),
(#213720,#213721),(#213722,#213723),(#213724,#213725),(#213726,#213727),
(#213728,#213729),(#213730,#213731),(#213732,#213733),(#213734,#213735),
(#213736,#213737),(#213738,#213739),(#213740,#213741),(#213742,#213743),
(#213744,#213745),(#213746,#213747),(#213748,#213749),(#213750,#213751),
(#213752,#213753),(#213754,#213755),(#213756,#213757),(#213758,#213759),
(#213760,#213761),(#213762,#213763),(#213764,#213765),(#213766,#213767),
(#213768,#213769),(#213770,#213771),(#213772,#213773),(#213774,#213775),
(#213776,#213777),(#213778,#213779),(#213780,#213781),(#213782,#213783),
(#213784,#213785),(#213786,#213787),(#213788,#213789),(#213790,#213791),
(#213792,#213793),(#213794,#213795),(#213796,#213797),(#213798,#213799),
(#213800,#213801),(#213802,#213803),(#213804,#213805),(#213806,#213807),
(#213808,#213809),(#213810,#213811),(#213812,#213813),(#213814,#213815),
(#213816,#213817),(#213818,#213819),(#213820,#213821),(#213822,#213823),
(#213824,#213825),(#213826,#213827),(#213828,#213829),(#213830,#213831),
(#213832,#213833),(#213834,#213835),(#213836,#213837),(#213838,#213839),
(#213840,#213841),(#213842,#213843),(#213844,#213845),(#213846,#213847),
(#213848,#213849),(#213850,#213851),(#213852,#213853),(#213854,#213855),
(#213856,#213857),(#213858,#213859),(#213860,#213861),(#213862,#213863),
(#213864,#213865),(#213866,#213867)),.UNSPECIFIED.,.F.,.F.,.F.)
B_SPLINE_SURFACE_WITH_KNOTS((6,1,1,1,1,1,1,1,1,1,1,1,1,1,1,1,1,1,1,1,1,
1,1,1,1,1,1,1,1,1,1,1,1,1,1,1,1,1,1,1,1,1,1,1,1,1,1,1,1,1,1,1,1,1,1,1,1,
1,1,1,1,1,1,1,1,1,1,1,1,1,1,1,1,1,1,1,1,1,1,1,1,1,1,1,1,1,1,1,1,1,1,1,1,
1,1,1,1,1,1,1,1,1,1,1,1,1,1,1,1,1,1,1,1,1,1,1,1,1,1,1,1,1,1,1,1,1,1,1,1,
1,1,1,1,1,1,1,1,1,1,1,1,1,1,1,1,1,1,1,1,1,1,1,1,1,1,1,1,1,1,1,1,1,1,1,1,
1,1,1,1,1,1,1,1,1,1,1,1,1,1,1,1,1,1,1,1,1,1,1,1,1,1,1,1,1,1,1,1,1,1,1,6),
(2,2),(0.,0.005,0.01,0.015,0.02,0.025,0.03,0.035,0.04,0.045,0.05,0.055,
0.06,0.065,0.07,0.075,0.08,0.085,0.09,0.095,0.1,0.105,0.11,0.115,0.12,0.125,
0.13,0.135,0.14,0.145,0.15,0.155,0.16,0.165,0.17,0.175,0.18,0.185,0.19,
0.195,0.2,0.205,0.21,0.215,0.22,0.225,0.23,0.235,0.24,0.245,0.25,0.255,
0.26,0.265,0.27,0.275,0.28,0.285,0.29,0.295,0.3,0.305,0.31,0.315,0.32,0.325,
0.33,0.335,0.34,0.345,0.35,0.355,0.36,0.365,0.37,0.375,0.38,0.385,0.39,
0.395,0.4,0.405,0.41,0.415,0.42,0.425,0.43,0.435,0.44,0.445,0.45,0.455,
0.46,0.465,0.47,0.475,0.48,0.485,0.49,0.495,0.5,0.505,0.51,0.515,0.52,0.525,
0.53,0.535,0.54,0.545,0.55,0.555,0.56,0.565,0.57,0.575,0.58,0.585,0.59,
0.595,0.6,0.605,0.61,0.615,0.62,0.625,0.63,0.635,0.64,0.645,0.65,0.655,
0.66,0.665,0.67,0.675,0.68,0.685,0.690000000000001,0.695000000000001,0.700000000000001,
0.705000000000001,0.710000000000001,0.715000000000001,0.720000000000001,
0.725000000000001,0.730000000000001,0.735000000000001,0.740000000000001,
0.745000000000001,0.750000000000001,0.755000000000001,0.760000000000001,
0.765000000000001,0.770000000000001,0.775000000000001,0.780000000000001,
0.785000000000001,0.790000000000001,0.795000000000001,0.800000000000001,
0.805000000000001,0.810000000000001,0.815000000000001,0.820000000000001,
0.825000000000001,0.830000000000001,0.835000000000001,0.840000000000001,
0.845000000000001,0.850000000000001,0.855000000000001,0.860000000000001,
0.865000000000001,0.870000000000001,0.875000000000001,0.880000000000001,
0.885000000000001,0.890000000000001,0.895000000000001,0.900000000000001,
0.905000000000001,0.910000000000001,0.915000000000001,0.920000000000001,
0.925000000000001,0.930000000000001,0.935000000000001,0.940000000000001,
0.945000000000001,0.950000000000001,0.955000000000001,0.960000000000001,
0.965000000000001,0.970000000000001,0.975000000000001,0.980000000000001,
0.985000000000001,0.990000000000001,0.995000000000001,1.),(0.,1.2),
 .UNSPECIFIED.)
GEOMETRIC_REPRESENTATION_ITEM()
RATIONAL_B_SPLINE_SURFACE(((1.,1.),(1.,1.),(1.,1.),(1.,1.),(1.,1.),(1.,
1.),(1.,1.),(1.,1.),(1.,1.),(1.,1.),(1.,1.),(1.,1.),(1.,1.),(1.,1.),(1.,
1.),(1.,1.),(1.,1.),(1.,1.),(1.,1.),(1.,1.),(1.,1.),(1.,1.),(1.,1.),(1.,
1.),(1.,1.),(1.,1.),(1.,1.),(1.,1.),(1.,1.),(1.,1.),(1.,1.),(1.,1.),(1.,
1.),(1.,1.),(1.,1.),(1.,1.),(1.,1.),(1.,1.),(1.,1.),(1.,1.),(1.,1.),(1.,
1.),(1.,1.),(1.,1.),(1.,1.),(1.,1.),(1.,1.),(1.,1.),(1.,1.),(1.,1.),(1.,
1.),(1.,1.),(1.,1.),(1.,1.),(1.,1.),(1.,1.),(1.,1.),(1.,1.),(1.,1.),(1.,
1.),(1.,1.),(1.,1.),(1.,1.),(1.,1.),(1.,1.),(1.,1.),(1.,1.),(1.,1.),(1.,
1.),(1.,1.),(1.,1.),(1.,1.),(1.,1.),(1.,1.),(1.,1.),(1.,1.),(1.,1.),(1.,
1.),(1.,1.),(1.,1.),(1.,1.),(1.,1.),(1.,1.),(1.,1.),(1.,1.),(1.,1.),(1.,
1.),(1.,1.),(1.,1.),(1.,1.),(1.,1.),(1.,1.),(1.,1.),(1.,1.),(1.,1.),(1.,
1.),(1.,1.),(1.,1.),(1.,1.),(1.,1.),(1.,1.),(1.,1.),(1.,1.),(1.,1.),(1.,
1.),(1.,1.),(1.,1.),(1.,1.),(1.,1.),(1.,1.),(1.,1.),(1.,1.),(1.,1.),(1.,
1.),(1.,1.),(1.,1.),(1.,1.),(1.,1.),(1.,1.),(1.,1.),(1.,1.),(1.,1.),(1.,
1.),(1.,1.),(1.,1.),(1.,1.),(1.,1.),(1.,1.),(1.,1.),(1.,1.),(1.,1.),(1.,
1.),(1.,1.),(1.,1.),(1.,1.),(1.,1.),(1.,1.),(1.,1.),(1.,1.),(1.,1.),(1.,
1.),(1.,1.),(1.,1.),(1.,1.),(1.,1.),(1.,1.),(1.,1.),(1.,1.),(1.,1.),(1.,
1.),(1.,1.),(1.,1.),(1.,1.),(1.,1.),(1.,1.),(1.,1.),(1.,1.),(1.,1.),(1.,
1.),(1.,1.),(1.,1.),(1.,1.),(1.,1.),(1.,1.),(1.,1.),(1.,1.),(1.,1.),(1.,
1.),(1.,1.),(1.,1.),(1.,1.),(1.,1.),(1.,1.),(1.,1.),(1.,1.),(1.,1.),(1.,
1.),(1.,1.),(1.,1.),(1.,1.),(1.,1.),(1.,1.),(1.,1.),(1.,1.),(1.,1.),(1.,
1.),(1.,1.),(1.,1.),(1.,1.),(1.,1.),(1.,1.),(1.,1.),(1.,1.),(1.,1.),(1.,
1.),(1.,1.),(1.,1.),(1.,1.),(1.,1.),(1.,1.),(1.,1.),(1.,1.),(1.,1.),(1.,
1.),(1.,1.)))
REPRESENTATION_ITEM('')
SURFACE()
);
#1073=(
BOUNDED_SURFACE()
B_SPLINE_SURFACE(5,1,((#214558,#214559),(#214560,#214561),(#214562,#214563),
(#214564,#214565),(#214566,#214567),(#214568,#214569),(#214570,#214571),
(#214572,#214573),(#214574,#214575),(#214576,#214577),(#214578,#214579),
(#214580,#214581),(#214582,#214583),(#214584,#214585),(#214586,#214587),
(#214588,#214589),(#214590,#214591),(#214592,#214593),(#214594,#214595),
(#214596,#214597),(#214598,#214599),(#214600,#214601),(#214602,#214603),
(#214604,#214605),(#214606,#214607),(#214608,#214609),(#214610,#214611),
(#214612,#214613),(#214614,#214615),(#214616,#214617),(#214618,#214619),
(#214620,#214621),(#214622,#214623),(#214624,#214625),(#214626,#214627),
(#214628,#214629),(#214630,#214631),(#214632,#214633),(#214634,#214635),
(#214636,#214637),(#214638,#214639),(#214640,#214641),(#214642,#214643),
(#214644,#214645),(#214646,#214647),(#214648,#214649),(#214650,#214651),
(#214652,#214653),(#214654,#214655),(#214656,#214657),(#214658,#214659),
(#214660,#214661),(#214662,#214663),(#214664,#214665),(#214666,#214667),
(#214668,#214669),(#214670,#214671),(#214672,#214673),(#214674,#214675),
(#214676,#214677),(#214678,#214679),(#214680,#214681),(#214682,#214683),
(#214684,#214685),(#214686,#214687),(#214688,#214689),(#214690,#214691),
(#214692,#214693),(#214694,#214695),(#214696,#214697),(#214698,#214699),
(#214700,#214701),(#214702,#214703),(#214704,#214705),(#214706,#214707),
(#214708,#214709),(#214710,#214711),(#214712,#214713),(#214714,#214715),
(#214716,#214717),(#214718,#214719),(#214720,#214721),(#214722,#214723),
(#214724,#214725),(#214726,#214727),(#214728,#214729),(#214730,#214731),
(#214732,#214733),(#214734,#214735),(#214736,#214737),(#214738,#214739),
(#214740,#214741),(#214742,#214743),(#214744,#214745),(#214746,#214747),
(#214748,#214749),(#214750,#214751),(#214752,#214753),(#214754,#214755),
(#214756,#214757),(#214758,#214759),(#214760,#214761),(#214762,#214763),
(#214764,#214765),(#214766,#214767),(#214768,#214769),(#214770,#214771),
(#214772,#214773),(#214774,#214775),(#214776,#214777),(#214778,#214779),
(#214780,#214781),(#214782,#214783),(#214784,#214785),(#214786,#214787),
(#214788,#214789),(#214790,#214791),(#214792,#214793),(#214794,#214795),
(#214796,#214797),(#214798,#214799),(#214800,#214801),(#214802,#214803),
(#214804,#214805),(#214806,#214807),(#214808,#214809),(#214810,#214811),
(#214812,#214813),(#214814,#214815),(#214816,#214817),(#214818,#214819),
(#214820,#214821),(#214822,#214823),(#214824,#214825),(#214826,#214827),
(#214828,#214829),(#214830,#214831),(#214832,#214833),(#214834,#214835),
(#214836,#214837),(#214838,#214839),(#214840,#214841),(#214842,#214843),
(#214844,#214845),(#214846,#214847),(#214848,#214849),(#214850,#214851),
(#214852,#214853),(#214854,#214855),(#214856,#214857),(#214858,#214859),
(#214860,#214861),(#214862,#214863),(#214864,#214865),(#214866,#214867),
(#214868,#214869),(#214870,#214871),(#214872,#214873),(#214874,#214875),
(#214876,#214877),(#214878,#214879),(#214880,#214881),(#214882,#214883),
(#214884,#214885),(#214886,#214887),(#214888,#214889),(#214890,#214891),
(#214892,#214893),(#214894,#214895),(#214896,#214897),(#214898,#214899),
(#214900,#214901),(#214902,#214903),(#214904,#214905),(#214906,#214907),
(#214908,#214909),(#214910,#214911),(#214912,#214913),(#214914,#214915),
(#214916,#214917),(#214918,#214919),(#214920,#214921),(#214922,#214923),
(#214924,#214925),(#214926,#214927),(#214928,#214929),(#214930,#214931),
(#214932,#214933),(#214934,#214935),(#214936,#214937),(#214938,#214939),
(#214940,#214941),(#214942,#214943),(#214944,#214945),(#214946,#214947),
(#214948,#214949),(#214950,#214951),(#214952,#214953),(#214954,#214955),
(#214956,#214957),(#214958,#214959),(#214960,#214961),(#214962,#214963),
(#214964,#214965),(#214966,#214967)),.UNSPECIFIED.,.F.,.F.,.F.)
B_SPLINE_SURFACE_WITH_KNOTS((6,1,1,1,1,1,1,1,1,1,1,1,1,1,1,1,1,1,1,1,1,
1,1,1,1,1,1,1,1,1,1,1,1,1,1,1,1,1,1,1,1,1,1,1,1,1,1,1,1,1,1,1,1,1,1,1,1,
1,1,1,1,1,1,1,1,1,1,1,1,1,1,1,1,1,1,1,1,1,1,1,1,1,1,1,1,1,1,1,1,1,1,1,1,
1,1,1,1,1,1,1,1,1,1,1,1,1,1,1,1,1,1,1,1,1,1,1,1,1,1,1,1,1,1,1,1,1,1,1,1,
1,1,1,1,1,1,1,1,1,1,1,1,1,1,1,1,1,1,1,1,1,1,1,1,1,1,1,1,1,1,1,1,1,1,1,1,
1,1,1,1,1,1,1,1,1,1,1,1,1,1,1,1,1,1,1,1,1,1,1,1,1,1,1,1,1,1,1,1,1,1,1,6),
(2,2),(-1.,-0.995000000000001,-0.990000000000001,-0.985000000000001,-0.980000000000001,
-0.975000000000001,-0.970000000000001,-0.965000000000001,-0.960000000000001,
-0.955000000000001,-0.950000000000001,-0.945000000000001,-0.940000000000001,
-0.935000000000001,-0.930000000000001,-0.925000000000001,-0.920000000000001,
-0.915000000000001,-0.910000000000001,-0.905000000000001,-0.900000000000001,
-0.895000000000001,-0.890000000000001,-0.885000000000001,-0.880000000000001,
-0.875000000000001,-0.870000000000001,-0.865000000000001,-0.860000000000001,
-0.855000000000001,-0.850000000000001,-0.845000000000001,-0.840000000000001,
-0.835000000000001,-0.830000000000001,-0.825000000000001,-0.820000000000001,
-0.815000000000001,-0.810000000000001,-0.805000000000001,-0.800000000000001,
-0.795000000000001,-0.790000000000001,-0.785000000000001,-0.780000000000001,
-0.775000000000001,-0.770000000000001,-0.765000000000001,-0.760000000000001,
-0.755000000000001,-0.750000000000001,-0.745000000000001,-0.740000000000001,
-0.735000000000001,-0.730000000000001,-0.725000000000001,-0.720000000000001,
-0.715000000000001,-0.710000000000001,-0.705000000000001,-0.700000000000001,
-0.695000000000001,-0.690000000000001,-0.685,-0.68,-0.675,-0.67,-0.665,
-0.66,-0.655,-0.65,-0.645,-0.64,-0.635,-0.63,-0.625,-0.62,-0.615,-0.61,
-0.605,-0.6,-0.595,-0.59,-0.585,-0.58,-0.575,-0.57,-0.565,-0.56,-0.555,
-0.55,-0.545,-0.54,-0.535,-0.53,-0.525,-0.52,-0.515,-0.51,-0.505,-0.5,-0.495,
-0.49,-0.485,-0.48,-0.475,-0.47,-0.465,-0.46,-0.455,-0.45,-0.445,-0.44,
-0.435,-0.43,-0.425,-0.42,-0.415,-0.41,-0.405,-0.4,-0.395,-0.39,-0.385,
-0.38,-0.375,-0.37,-0.365,-0.36,-0.355,-0.35,-0.345,-0.34,-0.335,-0.33,
-0.325,-0.32,-0.315,-0.31,-0.305,-0.3,-0.295,-0.29,-0.285,-0.28,-0.275,
-0.27,-0.265,-0.26,-0.255,-0.25,-0.245,-0.24,-0.235,-0.23,-0.225,-0.22,
-0.215,-0.21,-0.205,-0.2,-0.195,-0.19,-0.185,-0.18,-0.175,-0.17,-0.165,
-0.16,-0.155,-0.15,-0.145,-0.14,-0.135,-0.13,-0.125,-0.12,-0.115,-0.11,
-0.105,-0.1,-0.095,-0.09,-0.085,-0.08,-0.075,-0.07,-0.065,-0.06,-0.055,
-0.05,-0.045,-0.04,-0.035,-0.03,-0.025,-0.02,-0.015,-0.01,-0.005,0.),(0.,
1.2),.UNSPECIFIED.)
GEOMETRIC_REPRESENTATION_ITEM()
RATIONAL_B_SPLINE_SURFACE(((1.,1.),(1.,1.),(1.,1.),(1.,1.),(1.,1.),(1.,
1.),(1.,1.),(1.,1.),(1.,1.),(1.,1.),(1.,1.),(1.,1.),(1.,1.),(1.,1.),(1.,
1.),(1.,1.),(1.,1.),(1.,1.),(1.,1.),(1.,1.),(1.,1.),(1.,1.),(1.,1.),(1.,
1.),(1.,1.),(1.,1.),(1.,1.),(1.,1.),(1.,1.),(1.,1.),(1.,1.),(1.,1.),(1.,
1.),(1.,1.),(1.,1.),(1.,1.),(1.,1.),(1.,1.),(1.,1.),(1.,1.),(1.,1.),(1.,
1.),(1.,1.),(1.,1.),(1.,1.),(1.,1.),(1.,1.),(1.,1.),(1.,1.),(1.,1.),(1.,
1.),(1.,1.),(1.,1.),(1.,1.),(1.,1.),(1.,1.),(1.,1.),(1.,1.),(1.,1.),(1.,
1.),(1.,1.),(1.,1.),(1.,1.),(1.,1.),(1.,1.),(1.,1.),(1.,1.),(1.,1.),(1.,
1.),(1.,1.),(1.,1.),(1.,1.),(1.,1.),(1.,1.),(1.,1.),(1.,1.),(1.,1.),(1.,
1.),(1.,1.),(1.,1.),(1.,1.),(1.,1.),(1.,1.),(1.,1.),(1.,1.),(1.,1.),(1.,
1.),(1.,1.),(1.,1.),(1.,1.),(1.,1.),(1.,1.),(1.,1.),(1.,1.),(1.,1.),(1.,
1.),(1.,1.),(1.,1.),(1.,1.),(1.,1.),(1.,1.),(1.,1.),(1.,1.),(1.,1.),(1.,
1.),(1.,1.),(1.,1.),(1.,1.),(1.,1.),(1.,1.),(1.,1.),(1.,1.),(1.,1.),(1.,
1.),(1.,1.),(1.,1.),(1.,1.),(1.,1.),(1.,1.),(1.,1.),(1.,1.),(1.,1.),(1.,
1.),(1.,1.),(1.,1.),(1.,1.),(1.,1.),(1.,1.),(1.,1.),(1.,1.),(1.,1.),(1.,
1.),(1.,1.),(1.,1.),(1.,1.),(1.,1.),(1.,1.),(1.,1.),(1.,1.),(1.,1.),(1.,
1.),(1.,1.),(1.,1.),(1.,1.),(1.,1.),(1.,1.),(1.,1.),(1.,1.),(1.,1.),(1.,
1.),(1.,1.),(1.,1.),(1.,1.),(1.,1.),(1.,1.),(1.,1.),(1.,1.),(1.,1.),(1.,
1.),(1.,1.),(1.,1.),(1.,1.),(1.,1.),(1.,1.),(1.,1.),(1.,1.),(1.,1.),(1.,
1.),(1.,1.),(1.,1.),(1.,1.),(1.,1.),(1.,1.),(1.,1.),(1.,1.),(1.,1.),(1.,
1.),(1.,1.),(1.,1.),(1.,1.),(1.,1.),(1.,1.),(1.,1.),(1.,1.),(1.,1.),(1.,
1.),(1.,1.),(1.,1.),(1.,1.),(1.,1.),(1.,1.),(1.,1.),(1.,1.),(1.,1.),(1.,
1.),(1.,1.),(1.,1.),(1.,1.),(1.,1.),(1.,1.),(1.,1.),(1.,1.),(1.,1.),(1.,
1.),(1.,1.)))
REPRESENTATION_ITEM('')
SURFACE()
);
#1074=(
BOUNDED_SURFACE()
B_SPLINE_SURFACE(5,1,((#214968,#214969),(#214970,#214971),(#214972,#214973),
(#214974,#214975),(#214976,#214977),(#214978,#214979),(#214980,#214981),
(#214982,#214983),(#214984,#214985),(#214986,#214987),(#214988,#214989),
(#214990,#214991),(#214992,#214993),(#214994,#214995),(#214996,#214997),
(#214998,#214999),(#215000,#215001),(#215002,#215003),(#215004,#215005),
(#215006,#215007),(#215008,#215009),(#215010,#215011),(#215012,#215013),
(#215014,#215015),(#215016,#215017),(#215018,#215019),(#215020,#215021),
(#215022,#215023),(#215024,#215025),(#215026,#215027),(#215028,#215029),
(#215030,#215031),(#215032,#215033),(#215034,#215035),(#215036,#215037),
(#215038,#215039),(#215040,#215041),(#215042,#215043),(#215044,#215045),
(#215046,#215047),(#215048,#215049),(#215050,#215051),(#215052,#215053),
(#215054,#215055),(#215056,#215057),(#215058,#215059),(#215060,#215061),
(#215062,#215063),(#215064,#215065),(#215066,#215067),(#215068,#215069),
(#215070,#215071),(#215072,#215073),(#215074,#215075),(#215076,#215077),
(#215078,#215079),(#215080,#215081),(#215082,#215083),(#215084,#215085),
(#215086,#215087),(#215088,#215089),(#215090,#215091),(#215092,#215093),
(#215094,#215095),(#215096,#215097),(#215098,#215099),(#215100,#215101),
(#215102,#215103),(#215104,#215105),(#215106,#215107),(#215108,#215109),
(#215110,#215111),(#215112,#215113),(#215114,#215115),(#215116,#215117),
(#215118,#215119),(#215120,#215121),(#215122,#215123),(#215124,#215125),
(#215126,#215127),(#215128,#215129),(#215130,#215131),(#215132,#215133),
(#215134,#215135),(#215136,#215137),(#215138,#215139),(#215140,#215141),
(#215142,#215143),(#215144,#215145),(#215146,#215147),(#215148,#215149),
(#215150,#215151),(#215152,#215153),(#215154,#215155),(#215156,#215157),
(#215158,#215159),(#215160,#215161),(#215162,#215163),(#215164,#215165),
(#215166,#215167),(#215168,#215169),(#215170,#215171),(#215172,#215173),
(#215174,#215175),(#215176,#215177),(#215178,#215179),(#215180,#215181),
(#215182,#215183),(#215184,#215185),(#215186,#215187),(#215188,#215189),
(#215190,#215191),(#215192,#215193),(#215194,#215195),(#215196,#215197),
(#215198,#215199),(#215200,#215201),(#215202,#215203),(#215204,#215205),
(#215206,#215207),(#215208,#215209),(#215210,#215211),(#215212,#215213),
(#215214,#215215),(#215216,#215217),(#215218,#215219),(#215220,#215221),
(#215222,#215223),(#215224,#215225),(#215226,#215227),(#215228,#215229),
(#215230,#215231),(#215232,#215233),(#215234,#215235),(#215236,#215237),
(#215238,#215239),(#215240,#215241),(#215242,#215243),(#215244,#215245),
(#215246,#215247),(#215248,#215249),(#215250,#215251),(#215252,#215253),
(#215254,#215255),(#215256,#215257),(#215258,#215259),(#215260,#215261),
(#215262,#215263),(#215264,#215265),(#215266,#215267),(#215268,#215269),
(#215270,#215271),(#215272,#215273),(#215274,#215275),(#215276,#215277),
(#215278,#215279),(#215280,#215281),(#215282,#215283),(#215284,#215285),
(#215286,#215287),(#215288,#215289),(#215290,#215291),(#215292,#215293),
(#215294,#215295),(#215296,#215297),(#215298,#215299),(#215300,#215301),
(#215302,#215303),(#215304,#215305),(#215306,#215307),(#215308,#215309),
(#215310,#215311),(#215312,#215313),(#215314,#215315),(#215316,#215317),
(#215318,#215319),(#215320,#215321),(#215322,#215323),(#215324,#215325),
(#215326,#215327),(#215328,#215329),(#215330,#215331),(#215332,#215333),
(#215334,#215335),(#215336,#215337),(#215338,#215339),(#215340,#215341),
(#215342,#215343),(#215344,#215345),(#215346,#215347),(#215348,#215349),
(#215350,#215351),(#215352,#215353),(#215354,#215355),(#215356,#215357),
(#215358,#215359),(#215360,#215361),(#215362,#215363),(#215364,#215365),
(#215366,#215367),(#215368,#215369),(#215370,#215371),(#215372,#215373),
(#215374,#215375),(#215376,#215377)),.UNSPECIFIED.,.F.,.F.,.F.)
B_SPLINE_SURFACE_WITH_KNOTS((6,1,1,1,1,1,1,1,1,1,1,1,1,1,1,1,1,1,1,1,1,
1,1,1,1,1,1,1,1,1,1,1,1,1,1,1,1,1,1,1,1,1,1,1,1,1,1,1,1,1,1,1,1,1,1,1,1,
1,1,1,1,1,1,1,1,1,1,1,1,1,1,1,1,1,1,1,1,1,1,1,1,1,1,1,1,1,1,1,1,1,1,1,1,
1,1,1,1,1,1,1,1,1,1,1,1,1,1,1,1,1,1,1,1,1,1,1,1,1,1,1,1,1,1,1,1,1,1,1,1,
1,1,1,1,1,1,1,1,1,1,1,1,1,1,1,1,1,1,1,1,1,1,1,1,1,1,1,1,1,1,1,1,1,1,1,1,
1,1,1,1,1,1,1,1,1,1,1,1,1,1,1,1,1,1,1,1,1,1,1,1,1,1,1,1,1,1,1,1,1,1,1,6),
(2,2),(0.,0.005,0.01,0.015,0.02,0.025,0.03,0.035,0.04,0.045,0.05,0.055,
0.06,0.065,0.07,0.075,0.08,0.085,0.09,0.095,0.1,0.105,0.11,0.115,0.12,0.125,
0.13,0.135,0.14,0.145,0.15,0.155,0.16,0.165,0.17,0.175,0.18,0.185,0.19,
0.195,0.2,0.205,0.21,0.215,0.22,0.225,0.23,0.235,0.24,0.245,0.25,0.255,
0.26,0.265,0.27,0.275,0.28,0.285,0.29,0.295,0.3,0.305,0.31,0.315,0.32,0.325,
0.33,0.335,0.34,0.345,0.35,0.355,0.36,0.365,0.37,0.375,0.38,0.385,0.39,
0.395,0.4,0.405,0.41,0.415,0.42,0.425,0.43,0.435,0.44,0.445,0.45,0.455,
0.46,0.465,0.47,0.475,0.48,0.485,0.49,0.495,0.5,0.505,0.51,0.515,0.52,0.525,
0.53,0.535,0.54,0.545,0.55,0.555,0.56,0.565,0.57,0.575,0.58,0.585,0.59,
0.595,0.6,0.605,0.61,0.615,0.62,0.625,0.63,0.635,0.64,0.645,0.65,0.655,
0.66,0.665,0.67,0.675,0.68,0.685,0.690000000000001,0.695000000000001,0.700000000000001,
0.705000000000001,0.710000000000001,0.715000000000001,0.720000000000001,
0.725000000000001,0.730000000000001,0.735000000000001,0.740000000000001,
0.745000000000001,0.750000000000001,0.755000000000001,0.760000000000001,
0.765000000000001,0.770000000000001,0.775000000000001,0.780000000000001,
0.785000000000001,0.790000000000001,0.795000000000001,0.800000000000001,
0.805000000000001,0.810000000000001,0.815000000000001,0.820000000000001,
0.825000000000001,0.830000000000001,0.835000000000001,0.840000000000001,
0.845000000000001,0.850000000000001,0.855000000000001,0.860000000000001,
0.865000000000001,0.870000000000001,0.875000000000001,0.880000000000001,
0.885000000000001,0.890000000000001,0.895000000000001,0.900000000000001,
0.905000000000001,0.910000000000001,0.915000000000001,0.920000000000001,
0.925000000000001,0.930000000000001,0.935000000000001,0.940000000000001,
0.945000000000001,0.950000000000001,0.955000000000001,0.960000000000001,
0.965000000000001,0.970000000000001,0.975000000000001,0.980000000000001,
0.985000000000001,0.990000000000001,0.995000000000001,1.),(0.,1.2),
 .UNSPECIFIED.)
GEOMETRIC_REPRESENTATION_ITEM()
RATIONAL_B_SPLINE_SURFACE(((1.,1.),(1.,1.),(1.,1.),(1.,1.),(1.,1.),(1.,
1.),(1.,1.),(1.,1.),(1.,1.),(1.,1.),(1.,1.),(1.,1.),(1.,1.),(1.,1.),(1.,
1.),(1.,1.),(1.,1.),(1.,1.),(1.,1.),(1.,1.),(1.,1.),(1.,1.),(1.,1.),(1.,
1.),(1.,1.),(1.,1.),(1.,1.),(1.,1.),(1.,1.),(1.,1.),(1.,1.),(1.,1.),(1.,
1.),(1.,1.),(1.,1.),(1.,1.),(1.,1.),(1.,1.),(1.,1.),(1.,1.),(1.,1.),(1.,
1.),(1.,1.),(1.,1.),(1.,1.),(1.,1.),(1.,1.),(1.,1.),(1.,1.),(1.,1.),(1.,
1.),(1.,1.),(1.,1.),(1.,1.),(1.,1.),(1.,1.),(1.,1.),(1.,1.),(1.,1.),(1.,
1.),(1.,1.),(1.,1.),(1.,1.),(1.,1.),(1.,1.),(1.,1.),(1.,1.),(1.,1.),(1.,
1.),(1.,1.),(1.,1.),(1.,1.),(1.,1.),(1.,1.),(1.,1.),(1.,1.),(1.,1.),(1.,
1.),(1.,1.),(1.,1.),(1.,1.),(1.,1.),(1.,1.),(1.,1.),(1.,1.),(1.,1.),(1.,
1.),(1.,1.),(1.,1.),(1.,1.),(1.,1.),(1.,1.),(1.,1.),(1.,1.),(1.,1.),(1.,
1.),(1.,1.),(1.,1.),(1.,1.),(1.,1.),(1.,1.),(1.,1.),(1.,1.),(1.,1.),(1.,
1.),(1.,1.),(1.,1.),(1.,1.),(1.,1.),(1.,1.),(1.,1.),(1.,1.),(1.,1.),(1.,
1.),(1.,1.),(1.,1.),(1.,1.),(1.,1.),(1.,1.),(1.,1.),(1.,1.),(1.,1.),(1.,
1.),(1.,1.),(1.,1.),(1.,1.),(1.,1.),(1.,1.),(1.,1.),(1.,1.),(1.,1.),(1.,
1.),(1.,1.),(1.,1.),(1.,1.),(1.,1.),(1.,1.),(1.,1.),(1.,1.),(1.,1.),(1.,
1.),(1.,1.),(1.,1.),(1.,1.),(1.,1.),(1.,1.),(1.,1.),(1.,1.),(1.,1.),(1.,
1.),(1.,1.),(1.,1.),(1.,1.),(1.,1.),(1.,1.),(1.,1.),(1.,1.),(1.,1.),(1.,
1.),(1.,1.),(1.,1.),(1.,1.),(1.,1.),(1.,1.),(1.,1.),(1.,1.),(1.,1.),(1.,
1.),(1.,1.),(1.,1.),(1.,1.),(1.,1.),(1.,1.),(1.,1.),(1.,1.),(1.,1.),(1.,
1.),(1.,1.),(1.,1.),(1.,1.),(1.,1.),(1.,1.),(1.,1.),(1.,1.),(1.,1.),(1.,
1.),(1.,1.),(1.,1.),(1.,1.),(1.,1.),(1.,1.),(1.,1.),(1.,1.),(1.,1.),(1.,
1.),(1.,1.),(1.,1.),(1.,1.),(1.,1.),(1.,1.),(1.,1.),(1.,1.),(1.,1.),(1.,
1.),(1.,1.)))
REPRESENTATION_ITEM('')
SURFACE()
);
#1075=(
BOUNDED_SURFACE()
B_SPLINE_SURFACE(5,1,((#216008,#216009),(#216010,#216011),(#216012,#216013),
(#216014,#216015),(#216016,#216017),(#216018,#216019),(#216020,#216021),
(#216022,#216023),(#216024,#216025),(#216026,#216027),(#216028,#216029),
(#216030,#216031),(#216032,#216033),(#216034,#216035),(#216036,#216037),
(#216038,#216039),(#216040,#216041),(#216042,#216043),(#216044,#216045),
(#216046,#216047),(#216048,#216049),(#216050,#216051),(#216052,#216053),
(#216054,#216055),(#216056,#216057),(#216058,#216059),(#216060,#216061),
(#216062,#216063),(#216064,#216065),(#216066,#216067),(#216068,#216069),
(#216070,#216071),(#216072,#216073),(#216074,#216075),(#216076,#216077),
(#216078,#216079),(#216080,#216081),(#216082,#216083),(#216084,#216085),
(#216086,#216087),(#216088,#216089),(#216090,#216091),(#216092,#216093),
(#216094,#216095),(#216096,#216097),(#216098,#216099),(#216100,#216101),
(#216102,#216103),(#216104,#216105),(#216106,#216107),(#216108,#216109),
(#216110,#216111),(#216112,#216113),(#216114,#216115),(#216116,#216117),
(#216118,#216119),(#216120,#216121),(#216122,#216123),(#216124,#216125),
(#216126,#216127),(#216128,#216129),(#216130,#216131),(#216132,#216133),
(#216134,#216135),(#216136,#216137),(#216138,#216139),(#216140,#216141),
(#216142,#216143),(#216144,#216145),(#216146,#216147),(#216148,#216149),
(#216150,#216151),(#216152,#216153),(#216154,#216155),(#216156,#216157),
(#216158,#216159),(#216160,#216161),(#216162,#216163),(#216164,#216165),
(#216166,#216167),(#216168,#216169),(#216170,#216171),(#216172,#216173),
(#216174,#216175),(#216176,#216177),(#216178,#216179),(#216180,#216181),
(#216182,#216183),(#216184,#216185),(#216186,#216187),(#216188,#216189),
(#216190,#216191),(#216192,#216193),(#216194,#216195),(#216196,#216197),
(#216198,#216199),(#216200,#216201),(#216202,#216203),(#216204,#216205),
(#216206,#216207),(#216208,#216209),(#216210,#216211),(#216212,#216213),
(#216214,#216215),(#216216,#216217),(#216218,#216219),(#216220,#216221),
(#216222,#216223),(#216224,#216225),(#216226,#216227),(#216228,#216229),
(#216230,#216231),(#216232,#216233),(#216234,#216235),(#216236,#216237),
(#216238,#216239),(#216240,#216241),(#216242,#216243),(#216244,#216245),
(#216246,#216247),(#216248,#216249),(#216250,#216251),(#216252,#216253),
(#216254,#216255),(#216256,#216257),(#216258,#216259),(#216260,#216261),
(#216262,#216263),(#216264,#216265),(#216266,#216267),(#216268,#216269),
(#216270,#216271),(#216272,#216273),(#216274,#216275),(#216276,#216277),
(#216278,#216279),(#216280,#216281),(#216282,#216283),(#216284,#216285),
(#216286,#216287),(#216288,#216289),(#216290,#216291),(#216292,#216293),
(#216294,#216295),(#216296,#216297),(#216298,#216299),(#216300,#216301),
(#216302,#216303),(#216304,#216305),(#216306,#216307),(#216308,#216309),
(#216310,#216311),(#216312,#216313),(#216314,#216315),(#216316,#216317),
(#216318,#216319),(#216320,#216321),(#216322,#216323),(#216324,#216325),
(#216326,#216327),(#216328,#216329),(#216330,#216331),(#216332,#216333),
(#216334,#216335),(#216336,#216337),(#216338,#216339),(#216340,#216341),
(#216342,#216343),(#216344,#216345),(#216346,#216347),(#216348,#216349),
(#216350,#216351),(#216352,#216353),(#216354,#216355),(#216356,#216357),
(#216358,#216359),(#216360,#216361),(#216362,#216363),(#216364,#216365),
(#216366,#216367),(#216368,#216369),(#216370,#216371),(#216372,#216373),
(#216374,#216375),(#216376,#216377),(#216378,#216379),(#216380,#216381),
(#216382,#216383),(#216384,#216385),(#216386,#216387),(#216388,#216389),
(#216390,#216391),(#216392,#216393),(#216394,#216395),(#216396,#216397),
(#216398,#216399),(#216400,#216401),(#216402,#216403),(#216404,#216405),
(#216406,#216407),(#216408,#216409),(#216410,#216411),(#216412,#216413),
(#216414,#216415),(#216416,#216417)),.UNSPECIFIED.,.F.,.F.,.F.)
B_SPLINE_SURFACE_WITH_KNOTS((6,1,1,1,1,1,1,1,1,1,1,1,1,1,1,1,1,1,1,1,1,
1,1,1,1,1,1,1,1,1,1,1,1,1,1,1,1,1,1,1,1,1,1,1,1,1,1,1,1,1,1,1,1,1,1,1,1,
1,1,1,1,1,1,1,1,1,1,1,1,1,1,1,1,1,1,1,1,1,1,1,1,1,1,1,1,1,1,1,1,1,1,1,1,
1,1,1,1,1,1,1,1,1,1,1,1,1,1,1,1,1,1,1,1,1,1,1,1,1,1,1,1,1,1,1,1,1,1,1,1,
1,1,1,1,1,1,1,1,1,1,1,1,1,1,1,1,1,1,1,1,1,1,1,1,1,1,1,1,1,1,1,1,1,1,1,1,
1,1,1,1,1,1,1,1,1,1,1,1,1,1,1,1,1,1,1,1,1,1,1,1,1,1,1,1,1,1,1,1,1,1,1,6),
(2,2),(-1.,-0.995000000000001,-0.990000000000001,-0.985000000000001,-0.980000000000001,
-0.975000000000001,-0.970000000000001,-0.965000000000001,-0.960000000000001,
-0.955000000000001,-0.950000000000001,-0.945000000000001,-0.940000000000001,
-0.935000000000001,-0.930000000000001,-0.925000000000001,-0.920000000000001,
-0.915000000000001,-0.910000000000001,-0.905000000000001,-0.900000000000001,
-0.895000000000001,-0.890000000000001,-0.885000000000001,-0.880000000000001,
-0.875000000000001,-0.870000000000001,-0.865000000000001,-0.860000000000001,
-0.855000000000001,-0.850000000000001,-0.845000000000001,-0.840000000000001,
-0.835000000000001,-0.830000000000001,-0.825000000000001,-0.820000000000001,
-0.815000000000001,-0.810000000000001,-0.805000000000001,-0.800000000000001,
-0.795000000000001,-0.790000000000001,-0.785000000000001,-0.780000000000001,
-0.775000000000001,-0.770000000000001,-0.765000000000001,-0.760000000000001,
-0.755000000000001,-0.750000000000001,-0.745000000000001,-0.740000000000001,
-0.735000000000001,-0.730000000000001,-0.725000000000001,-0.720000000000001,
-0.715000000000001,-0.710000000000001,-0.705000000000001,-0.700000000000001,
-0.695000000000001,-0.690000000000001,-0.685,-0.68,-0.675,-0.67,-0.665,
-0.66,-0.655,-0.65,-0.645,-0.64,-0.635,-0.63,-0.625,-0.62,-0.615,-0.61,
-0.605,-0.6,-0.595,-0.59,-0.585,-0.58,-0.575,-0.57,-0.565,-0.56,-0.555,
-0.55,-0.545,-0.54,-0.535,-0.53,-0.525,-0.52,-0.515,-0.51,-0.505,-0.5,-0.495,
-0.49,-0.485,-0.48,-0.475,-0.47,-0.465,-0.46,-0.455,-0.45,-0.445,-0.44,
-0.435,-0.43,-0.425,-0.42,-0.415,-0.41,-0.405,-0.4,-0.395,-0.39,-0.385,
-0.38,-0.375,-0.37,-0.365,-0.36,-0.355,-0.35,-0.345,-0.34,-0.335,-0.33,
-0.325,-0.32,-0.315,-0.31,-0.305,-0.3,-0.295,-0.29,-0.285,-0.28,-0.275,
-0.27,-0.265,-0.26,-0.255,-0.25,-0.245,-0.24,-0.235,-0.23,-0.225,-0.22,
-0.215,-0.21,-0.205,-0.2,-0.195,-0.19,-0.185,-0.18,-0.175,-0.17,-0.165,
-0.16,-0.155,-0.15,-0.145,-0.14,-0.135,-0.13,-0.125,-0.12,-0.115,-0.11,
-0.105,-0.1,-0.095,-0.09,-0.085,-0.08,-0.075,-0.07,-0.065,-0.06,-0.055,
-0.05,-0.045,-0.04,-0.035,-0.03,-0.025,-0.02,-0.015,-0.01,-0.005,0.),(0.,
1.2),.UNSPECIFIED.)
GEOMETRIC_REPRESENTATION_ITEM()
RATIONAL_B_SPLINE_SURFACE(((1.,1.),(1.,1.),(1.,1.),(1.,1.),(1.,1.),(1.,
1.),(1.,1.),(1.,1.),(1.,1.),(1.,1.),(1.,1.),(1.,1.),(1.,1.),(1.,1.),(1.,
1.),(1.,1.),(1.,1.),(1.,1.),(1.,1.),(1.,1.),(1.,1.),(1.,1.),(1.,1.),(1.,
1.),(1.,1.),(1.,1.),(1.,1.),(1.,1.),(1.,1.),(1.,1.),(1.,1.),(1.,1.),(1.,
1.),(1.,1.),(1.,1.),(1.,1.),(1.,1.),(1.,1.),(1.,1.),(1.,1.),(1.,1.),(1.,
1.),(1.,1.),(1.,1.),(1.,1.),(1.,1.),(1.,1.),(1.,1.),(1.,1.),(1.,1.),(1.,
1.),(1.,1.),(1.,1.),(1.,1.),(1.,1.),(1.,1.),(1.,1.),(1.,1.),(1.,1.),(1.,
1.),(1.,1.),(1.,1.),(1.,1.),(1.,1.),(1.,1.),(1.,1.),(1.,1.),(1.,1.),(1.,
1.),(1.,1.),(1.,1.),(1.,1.),(1.,1.),(1.,1.),(1.,1.),(1.,1.),(1.,1.),(1.,
1.),(1.,1.),(1.,1.),(1.,1.),(1.,1.),(1.,1.),(1.,1.),(1.,1.),(1.,1.),(1.,
1.),(1.,1.),(1.,1.),(1.,1.),(1.,1.),(1.,1.),(1.,1.),(1.,1.),(1.,1.),(1.,
1.),(1.,1.),(1.,1.),(1.,1.),(1.,1.),(1.,1.),(1.,1.),(1.,1.),(1.,1.),(1.,
1.),(1.,1.),(1.,1.),(1.,1.),(1.,1.),(1.,1.),(1.,1.),(1.,1.),(1.,1.),(1.,
1.),(1.,1.),(1.,1.),(1.,1.),(1.,1.),(1.,1.),(1.,1.),(1.,1.),(1.,1.),(1.,
1.),(1.,1.),(1.,1.),(1.,1.),(1.,1.),(1.,1.),(1.,1.),(1.,1.),(1.,1.),(1.,
1.),(1.,1.),(1.,1.),(1.,1.),(1.,1.),(1.,1.),(1.,1.),(1.,1.),(1.,1.),(1.,
1.),(1.,1.),(1.,1.),(1.,1.),(1.,1.),(1.,1.),(1.,1.),(1.,1.),(1.,1.),(1.,
1.),(1.,1.),(1.,1.),(1.,1.),(1.,1.),(1.,1.),(1.,1.),(1.,1.),(1.,1.),(1.,
1.),(1.,1.),(1.,1.),(1.,1.),(1.,1.),(1.,1.),(1.,1.),(1.,1.),(1.,1.),(1.,
1.),(1.,1.),(1.,1.),(1.,1.),(1.,1.),(1.,1.),(1.,1.),(1.,1.),(1.,1.),(1.,
1.),(1.,1.),(1.,1.),(1.,1.),(1.,1.),(1.,1.),(1.,1.),(1.,1.),(1.,1.),(1.,
1.),(1.,1.),(1.,1.),(1.,1.),(1.,1.),(1.,1.),(1.,1.),(1.,1.),(1.,1.),(1.,
1.),(1.,1.),(1.,1.),(1.,1.),(1.,1.),(1.,1.),(1.,1.),(1.,1.),(1.,1.),(1.,
1.),(1.,1.)))
REPRESENTATION_ITEM('')
SURFACE()
);
#1076=(
BOUNDED_SURFACE()
B_SPLINE_SURFACE(5,1,((#216831,#216832),(#216833,#216834),(#216835,#216836),
(#216837,#216838),(#216839,#216840),(#216841,#216842),(#216843,#216844),
(#216845,#216846),(#216847,#216848),(#216849,#216850),(#216851,#216852),
(#216853,#216854),(#216855,#216856),(#216857,#216858),(#216859,#216860),
(#216861,#216862),(#216863,#216864),(#216865,#216866),(#216867,#216868),
(#216869,#216870),(#216871,#216872),(#216873,#216874),(#216875,#216876),
(#216877,#216878),(#216879,#216880),(#216881,#216882),(#216883,#216884),
(#216885,#216886),(#216887,#216888),(#216889,#216890),(#216891,#216892),
(#216893,#216894),(#216895,#216896),(#216897,#216898),(#216899,#216900),
(#216901,#216902),(#216903,#216904),(#216905,#216906),(#216907,#216908),
(#216909,#216910),(#216911,#216912),(#216913,#216914),(#216915,#216916),
(#216917,#216918),(#216919,#216920),(#216921,#216922),(#216923,#216924),
(#216925,#216926),(#216927,#216928),(#216929,#216930),(#216931,#216932),
(#216933,#216934),(#216935,#216936),(#216937,#216938),(#216939,#216940),
(#216941,#216942),(#216943,#216944),(#216945,#216946),(#216947,#216948),
(#216949,#216950),(#216951,#216952),(#216953,#216954),(#216955,#216956),
(#216957,#216958),(#216959,#216960),(#216961,#216962),(#216963,#216964),
(#216965,#216966),(#216967,#216968),(#216969,#216970),(#216971,#216972),
(#216973,#216974),(#216975,#216976),(#216977,#216978),(#216979,#216980),
(#216981,#216982),(#216983,#216984),(#216985,#216986),(#216987,#216988),
(#216989,#216990),(#216991,#216992),(#216993,#216994),(#216995,#216996),
(#216997,#216998),(#216999,#217000),(#217001,#217002),(#217003,#217004),
(#217005,#217006),(#217007,#217008),(#217009,#217010),(#217011,#217012),
(#217013,#217014),(#217015,#217016),(#217017,#217018),(#217019,#217020),
(#217021,#217022),(#217023,#217024),(#217025,#217026),(#217027,#217028),
(#217029,#217030),(#217031,#217032),(#217033,#217034),(#217035,#217036),
(#217037,#217038),(#217039,#217040),(#217041,#217042),(#217043,#217044),
(#217045,#217046),(#217047,#217048),(#217049,#217050),(#217051,#217052),
(#217053,#217054),(#217055,#217056),(#217057,#217058),(#217059,#217060),
(#217061,#217062),(#217063,#217064),(#217065,#217066),(#217067,#217068),
(#217069,#217070),(#217071,#217072),(#217073,#217074),(#217075,#217076),
(#217077,#217078),(#217079,#217080),(#217081,#217082),(#217083,#217084),
(#217085,#217086),(#217087,#217088),(#217089,#217090),(#217091,#217092),
(#217093,#217094),(#217095,#217096),(#217097,#217098),(#217099,#217100),
(#217101,#217102),(#217103,#217104),(#217105,#217106),(#217107,#217108),
(#217109,#217110),(#217111,#217112),(#217113,#217114),(#217115,#217116),
(#217117,#217118),(#217119,#217120),(#217121,#217122),(#217123,#217124),
(#217125,#217126),(#217127,#217128),(#217129,#217130),(#217131,#217132),
(#217133,#217134),(#217135,#217136),(#217137,#217138),(#217139,#217140),
(#217141,#217142),(#217143,#217144),(#217145,#217146),(#217147,#217148),
(#217149,#217150),(#217151,#217152),(#217153,#217154),(#217155,#217156),
(#217157,#217158),(#217159,#217160),(#217161,#217162),(#217163,#217164),
(#217165,#217166),(#217167,#217168),(#217169,#217170),(#217171,#217172),
(#217173,#217174),(#217175,#217176),(#217177,#217178),(#217179,#217180),
(#217181,#217182),(#217183,#217184),(#217185,#217186),(#217187,#217188),
(#217189,#217190),(#217191,#217192),(#217193,#217194),(#217195,#217196),
(#217197,#217198),(#217199,#217200),(#217201,#217202),(#217203,#217204),
(#217205,#217206),(#217207,#217208),(#217209,#217210),(#217211,#217212),
(#217213,#217214),(#217215,#217216),(#217217,#217218),(#217219,#217220),
(#217221,#217222),(#217223,#217224),(#217225,#217226),(#217227,#217228),
(#217229,#217230),(#217231,#217232),(#217233,#217234),(#217235,#217236),
(#217237,#217238),(#217239,#217240)),.UNSPECIFIED.,.F.,.F.,.F.)
B_SPLINE_SURFACE_WITH_KNOTS((6,1,1,1,1,1,1,1,1,1,1,1,1,1,1,1,1,1,1,1,1,
1,1,1,1,1,1,1,1,1,1,1,1,1,1,1,1,1,1,1,1,1,1,1,1,1,1,1,1,1,1,1,1,1,1,1,1,
1,1,1,1,1,1,1,1,1,1,1,1,1,1,1,1,1,1,1,1,1,1,1,1,1,1,1,1,1,1,1,1,1,1,1,1,
1,1,1,1,1,1,1,1,1,1,1,1,1,1,1,1,1,1,1,1,1,1,1,1,1,1,1,1,1,1,1,1,1,1,1,1,
1,1,1,1,1,1,1,1,1,1,1,1,1,1,1,1,1,1,1,1,1,1,1,1,1,1,1,1,1,1,1,1,1,1,1,1,
1,1,1,1,1,1,1,1,1,1,1,1,1,1,1,1,1,1,1,1,1,1,1,1,1,1,1,1,1,1,1,1,1,1,1,6),
(2,2),(0.,0.005,0.01,0.015,0.02,0.025,0.03,0.035,0.04,0.045,0.05,0.055,
0.06,0.065,0.07,0.075,0.08,0.085,0.09,0.095,0.1,0.105,0.11,0.115,0.12,0.125,
0.13,0.135,0.14,0.145,0.15,0.155,0.16,0.165,0.17,0.175,0.18,0.185,0.19,
0.195,0.2,0.205,0.21,0.215,0.22,0.225,0.23,0.235,0.24,0.245,0.25,0.255,
0.26,0.265,0.27,0.275,0.28,0.285,0.29,0.295,0.3,0.305,0.31,0.315,0.32,0.325,
0.33,0.335,0.34,0.345,0.35,0.355,0.36,0.365,0.37,0.375,0.38,0.385,0.39,
0.395,0.4,0.405,0.41,0.415,0.42,0.425,0.43,0.435,0.44,0.445,0.45,0.455,
0.46,0.465,0.47,0.475,0.48,0.485,0.49,0.495,0.5,0.505,0.51,0.515,0.52,0.525,
0.53,0.535,0.54,0.545,0.55,0.555,0.56,0.565,0.57,0.575,0.58,0.585,0.59,
0.595,0.6,0.605,0.61,0.615,0.62,0.625,0.63,0.635,0.64,0.645,0.65,0.655,
0.66,0.665,0.67,0.675,0.68,0.685,0.690000000000001,0.695000000000001,0.700000000000001,
0.705000000000001,0.710000000000001,0.715000000000001,0.720000000000001,
0.725000000000001,0.730000000000001,0.735000000000001,0.740000000000001,
0.745000000000001,0.750000000000001,0.755000000000001,0.760000000000001,
0.765000000000001,0.770000000000001,0.775000000000001,0.780000000000001,
0.785000000000001,0.790000000000001,0.795000000000001,0.800000000000001,
0.805000000000001,0.810000000000001,0.815000000000001,0.820000000000001,
0.825000000000001,0.830000000000001,0.835000000000001,0.840000000000001,
0.845000000000001,0.850000000000001,0.855000000000001,0.860000000000001,
0.865000000000001,0.870000000000001,0.875000000000001,0.880000000000001,
0.885000000000001,0.890000000000001,0.895000000000001,0.900000000000001,
0.905000000000001,0.910000000000001,0.915000000000001,0.920000000000001,
0.925000000000001,0.930000000000001,0.935000000000001,0.940000000000001,
0.945000000000001,0.950000000000001,0.955000000000001,0.960000000000001,
0.965000000000001,0.970000000000001,0.975000000000001,0.980000000000001,
0.985000000000001,0.990000000000001,0.995000000000001,1.),(0.,1.2),
 .UNSPECIFIED.)
GEOMETRIC_REPRESENTATION_ITEM()
RATIONAL_B_SPLINE_SURFACE(((1.,1.),(1.,1.),(1.,1.),(1.,1.),(1.,1.),(1.,
1.),(1.,1.),(1.,1.),(1.,1.),(1.,1.),(1.,1.),(1.,1.),(1.,1.),(1.,1.),(1.,
1.),(1.,1.),(1.,1.),(1.,1.),(1.,1.),(1.,1.),(1.,1.),(1.,1.),(1.,1.),(1.,
1.),(1.,1.),(1.,1.),(1.,1.),(1.,1.),(1.,1.),(1.,1.),(1.,1.),(1.,1.),(1.,
1.),(1.,1.),(1.,1.),(1.,1.),(1.,1.),(1.,1.),(1.,1.),(1.,1.),(1.,1.),(1.,
1.),(1.,1.),(1.,1.),(1.,1.),(1.,1.),(1.,1.),(1.,1.),(1.,1.),(1.,1.),(1.,
1.),(1.,1.),(1.,1.),(1.,1.),(1.,1.),(1.,1.),(1.,1.),(1.,1.),(1.,1.),(1.,
1.),(1.,1.),(1.,1.),(1.,1.),(1.,1.),(1.,1.),(1.,1.),(1.,1.),(1.,1.),(1.,
1.),(1.,1.),(1.,1.),(1.,1.),(1.,1.),(1.,1.),(1.,1.),(1.,1.),(1.,1.),(1.,
1.),(1.,1.),(1.,1.),(1.,1.),(1.,1.),(1.,1.),(1.,1.),(1.,1.),(1.,1.),(1.,
1.),(1.,1.),(1.,1.),(1.,1.),(1.,1.),(1.,1.),(1.,1.),(1.,1.),(1.,1.),(1.,
1.),(1.,1.),(1.,1.),(1.,1.),(1.,1.),(1.,1.),(1.,1.),(1.,1.),(1.,1.),(1.,
1.),(1.,1.),(1.,1.),(1.,1.),(1.,1.),(1.,1.),(1.,1.),(1.,1.),(1.,1.),(1.,
1.),(1.,1.),(1.,1.),(1.,1.),(1.,1.),(1.,1.),(1.,1.),(1.,1.),(1.,1.),(1.,
1.),(1.,1.),(1.,1.),(1.,1.),(1.,1.),(1.,1.),(1.,1.),(1.,1.),(1.,1.),(1.,
1.),(1.,1.),(1.,1.),(1.,1.),(1.,1.),(1.,1.),(1.,1.),(1.,1.),(1.,1.),(1.,
1.),(1.,1.),(1.,1.),(1.,1.),(1.,1.),(1.,1.),(1.,1.),(1.,1.),(1.,1.),(1.,
1.),(1.,1.),(1.,1.),(1.,1.),(1.,1.),(1.,1.),(1.,1.),(1.,1.),(1.,1.),(1.,
1.),(1.,1.),(1.,1.),(1.,1.),(1.,1.),(1.,1.),(1.,1.),(1.,1.),(1.,1.),(1.,
1.),(1.,1.),(1.,1.),(1.,1.),(1.,1.),(1.,1.),(1.,1.),(1.,1.),(1.,1.),(1.,
1.),(1.,1.),(1.,1.),(1.,1.),(1.,1.),(1.,1.),(1.,1.),(1.,1.),(1.,1.),(1.,
1.),(1.,1.),(1.,1.),(1.,1.),(1.,1.),(1.,1.),(1.,1.),(1.,1.),(1.,1.),(1.,
1.),(1.,1.),(1.,1.),(1.,1.),(1.,1.),(1.,1.),(1.,1.),(1.,1.),(1.,1.),(1.,
1.),(1.,1.)))
REPRESENTATION_ITEM('')
SURFACE()
);
#1077=(
BOUNDED_SURFACE()
B_SPLINE_SURFACE(5,1,((#217660,#217661),(#217662,#217663),(#217664,#217665),
(#217666,#217667),(#217668,#217669),(#217670,#217671),(#217672,#217673),
(#217674,#217675),(#217676,#217677),(#217678,#217679),(#217680,#217681),
(#217682,#217683),(#217684,#217685),(#217686,#217687),(#217688,#217689),
(#217690,#217691),(#217692,#217693),(#217694,#217695),(#217696,#217697),
(#217698,#217699),(#217700,#217701),(#217702,#217703),(#217704,#217705),
(#217706,#217707),(#217708,#217709),(#217710,#217711),(#217712,#217713),
(#217714,#217715),(#217716,#217717),(#217718,#217719),(#217720,#217721),
(#217722,#217723),(#217724,#217725),(#217726,#217727),(#217728,#217729),
(#217730,#217731),(#217732,#217733),(#217734,#217735),(#217736,#217737),
(#217738,#217739),(#217740,#217741),(#217742,#217743),(#217744,#217745),
(#217746,#217747),(#217748,#217749),(#217750,#217751),(#217752,#217753),
(#217754,#217755),(#217756,#217757),(#217758,#217759),(#217760,#217761),
(#217762,#217763),(#217764,#217765),(#217766,#217767),(#217768,#217769),
(#217770,#217771),(#217772,#217773),(#217774,#217775),(#217776,#217777),
(#217778,#217779),(#217780,#217781),(#217782,#217783),(#217784,#217785),
(#217786,#217787),(#217788,#217789),(#217790,#217791),(#217792,#217793),
(#217794,#217795),(#217796,#217797),(#217798,#217799),(#217800,#217801),
(#217802,#217803),(#217804,#217805),(#217806,#217807),(#217808,#217809),
(#217810,#217811),(#217812,#217813),(#217814,#217815),(#217816,#217817),
(#217818,#217819),(#217820,#217821),(#217822,#217823),(#217824,#217825),
(#217826,#217827),(#217828,#217829),(#217830,#217831),(#217832,#217833),
(#217834,#217835),(#217836,#217837),(#217838,#217839),(#217840,#217841),
(#217842,#217843),(#217844,#217845),(#217846,#217847),(#217848,#217849),
(#217850,#217851),(#217852,#217853),(#217854,#217855),(#217856,#217857),
(#217858,#217859),(#217860,#217861),(#217862,#217863),(#217864,#217865),
(#217866,#217867),(#217868,#217869),(#217870,#217871),(#217872,#217873),
(#217874,#217875),(#217876,#217877),(#217878,#217879),(#217880,#217881),
(#217882,#217883),(#217884,#217885),(#217886,#217887),(#217888,#217889),
(#217890,#217891),(#217892,#217893),(#217894,#217895),(#217896,#217897),
(#217898,#217899),(#217900,#217901),(#217902,#217903),(#217904,#217905),
(#217906,#217907),(#217908,#217909),(#217910,#217911),(#217912,#217913),
(#217914,#217915),(#217916,#217917),(#217918,#217919),(#217920,#217921),
(#217922,#217923),(#217924,#217925),(#217926,#217927),(#217928,#217929),
(#217930,#217931),(#217932,#217933),(#217934,#217935),(#217936,#217937),
(#217938,#217939),(#217940,#217941),(#217942,#217943),(#217944,#217945),
(#217946,#217947),(#217948,#217949),(#217950,#217951),(#217952,#217953),
(#217954,#217955),(#217956,#217957),(#217958,#217959),(#217960,#217961),
(#217962,#217963),(#217964,#217965),(#217966,#217967),(#217968,#217969),
(#217970,#217971),(#217972,#217973),(#217974,#217975),(#217976,#217977),
(#217978,#217979),(#217980,#217981),(#217982,#217983),(#217984,#217985),
(#217986,#217987),(#217988,#217989),(#217990,#217991),(#217992,#217993),
(#217994,#217995),(#217996,#217997),(#217998,#217999),(#218000,#218001),
(#218002,#218003),(#218004,#218005),(#218006,#218007),(#218008,#218009),
(#218010,#218011),(#218012,#218013),(#218014,#218015),(#218016,#218017),
(#218018,#218019),(#218020,#218021),(#218022,#218023),(#218024,#218025),
(#218026,#218027),(#218028,#218029),(#218030,#218031),(#218032,#218033),
(#218034,#218035),(#218036,#218037),(#218038,#218039),(#218040,#218041),
(#218042,#218043),(#218044,#218045),(#218046,#218047),(#218048,#218049),
(#218050,#218051),(#218052,#218053),(#218054,#218055),(#218056,#218057),
(#218058,#218059),(#218060,#218061),(#218062,#218063),(#218064,#218065),
(#218066,#218067),(#218068,#218069)),.UNSPECIFIED.,.F.,.F.,.F.)
B_SPLINE_SURFACE_WITH_KNOTS((6,1,1,1,1,1,1,1,1,1,1,1,1,1,1,1,1,1,1,1,1,
1,1,1,1,1,1,1,1,1,1,1,1,1,1,1,1,1,1,1,1,1,1,1,1,1,1,1,1,1,1,1,1,1,1,1,1,
1,1,1,1,1,1,1,1,1,1,1,1,1,1,1,1,1,1,1,1,1,1,1,1,1,1,1,1,1,1,1,1,1,1,1,1,
1,1,1,1,1,1,1,1,1,1,1,1,1,1,1,1,1,1,1,1,1,1,1,1,1,1,1,1,1,1,1,1,1,1,1,1,
1,1,1,1,1,1,1,1,1,1,1,1,1,1,1,1,1,1,1,1,1,1,1,1,1,1,1,1,1,1,1,1,1,1,1,1,
1,1,1,1,1,1,1,1,1,1,1,1,1,1,1,1,1,1,1,1,1,1,1,1,1,1,1,1,1,1,1,1,1,1,1,6),
(2,2),(-1.,-0.995000000000001,-0.990000000000001,-0.985000000000001,-0.980000000000001,
-0.975000000000001,-0.970000000000001,-0.965000000000001,-0.960000000000001,
-0.955000000000001,-0.950000000000001,-0.945000000000001,-0.940000000000001,
-0.935000000000001,-0.930000000000001,-0.925000000000001,-0.920000000000001,
-0.915000000000001,-0.910000000000001,-0.905000000000001,-0.900000000000001,
-0.895000000000001,-0.890000000000001,-0.885000000000001,-0.880000000000001,
-0.875000000000001,-0.870000000000001,-0.865000000000001,-0.860000000000001,
-0.855000000000001,-0.850000000000001,-0.845000000000001,-0.840000000000001,
-0.835000000000001,-0.830000000000001,-0.825000000000001,-0.820000000000001,
-0.815000000000001,-0.810000000000001,-0.805000000000001,-0.800000000000001,
-0.795000000000001,-0.790000000000001,-0.785000000000001,-0.780000000000001,
-0.775000000000001,-0.770000000000001,-0.765000000000001,-0.760000000000001,
-0.755000000000001,-0.750000000000001,-0.745000000000001,-0.740000000000001,
-0.735000000000001,-0.730000000000001,-0.725000000000001,-0.720000000000001,
-0.715000000000001,-0.710000000000001,-0.705000000000001,-0.700000000000001,
-0.695000000000001,-0.690000000000001,-0.685,-0.68,-0.675,-0.67,-0.665,
-0.66,-0.655,-0.65,-0.645,-0.64,-0.635,-0.63,-0.625,-0.62,-0.615,-0.61,
-0.605,-0.6,-0.595,-0.59,-0.585,-0.58,-0.575,-0.57,-0.565,-0.56,-0.555,
-0.55,-0.545,-0.54,-0.535,-0.53,-0.525,-0.52,-0.515,-0.51,-0.505,-0.5,-0.495,
-0.49,-0.485,-0.48,-0.475,-0.47,-0.465,-0.46,-0.455,-0.45,-0.445,-0.44,
-0.435,-0.43,-0.425,-0.42,-0.415,-0.41,-0.405,-0.4,-0.395,-0.39,-0.385,
-0.38,-0.375,-0.37,-0.365,-0.36,-0.355,-0.35,-0.345,-0.34,-0.335,-0.33,
-0.325,-0.32,-0.315,-0.31,-0.305,-0.3,-0.295,-0.29,-0.285,-0.28,-0.275,
-0.27,-0.265,-0.26,-0.255,-0.25,-0.245,-0.24,-0.235,-0.23,-0.225,-0.22,
-0.215,-0.21,-0.205,-0.2,-0.195,-0.19,-0.185,-0.18,-0.175,-0.17,-0.165,
-0.16,-0.155,-0.15,-0.145,-0.14,-0.135,-0.13,-0.125,-0.12,-0.115,-0.11,
-0.105,-0.1,-0.095,-0.09,-0.085,-0.08,-0.075,-0.07,-0.065,-0.06,-0.055,
-0.05,-0.045,-0.04,-0.035,-0.03,-0.025,-0.02,-0.015,-0.01,-0.005,0.),(0.,
1.2),.UNSPECIFIED.)
GEOMETRIC_REPRESENTATION_ITEM()
RATIONAL_B_SPLINE_SURFACE(((1.,1.),(1.,1.),(1.,1.),(1.,1.),(1.,1.),(1.,
1.),(1.,1.),(1.,1.),(1.,1.),(1.,1.),(1.,1.),(1.,1.),(1.,1.),(1.,1.),(1.,
1.),(1.,1.),(1.,1.),(1.,1.),(1.,1.),(1.,1.),(1.,1.),(1.,1.),(1.,1.),(1.,
1.),(1.,1.),(1.,1.),(1.,1.),(1.,1.),(1.,1.),(1.,1.),(1.,1.),(1.,1.),(1.,
1.),(1.,1.),(1.,1.),(1.,1.),(1.,1.),(1.,1.),(1.,1.),(1.,1.),(1.,1.),(1.,
1.),(1.,1.),(1.,1.),(1.,1.),(1.,1.),(1.,1.),(1.,1.),(1.,1.),(1.,1.),(1.,
1.),(1.,1.),(1.,1.),(1.,1.),(1.,1.),(1.,1.),(1.,1.),(1.,1.),(1.,1.),(1.,
1.),(1.,1.),(1.,1.),(1.,1.),(1.,1.),(1.,1.),(1.,1.),(1.,1.),(1.,1.),(1.,
1.),(1.,1.),(1.,1.),(1.,1.),(1.,1.),(1.,1.),(1.,1.),(1.,1.),(1.,1.),(1.,
1.),(1.,1.),(1.,1.),(1.,1.),(1.,1.),(1.,1.),(1.,1.),(1.,1.),(1.,1.),(1.,
1.),(1.,1.),(1.,1.),(1.,1.),(1.,1.),(1.,1.),(1.,1.),(1.,1.),(1.,1.),(1.,
1.),(1.,1.),(1.,1.),(1.,1.),(1.,1.),(1.,1.),(1.,1.),(1.,1.),(1.,1.),(1.,
1.),(1.,1.),(1.,1.),(1.,1.),(1.,1.),(1.,1.),(1.,1.),(1.,1.),(1.,1.),(1.,
1.),(1.,1.),(1.,1.),(1.,1.),(1.,1.),(1.,1.),(1.,1.),(1.,1.),(1.,1.),(1.,
1.),(1.,1.),(1.,1.),(1.,1.),(1.,1.),(1.,1.),(1.,1.),(1.,1.),(1.,1.),(1.,
1.),(1.,1.),(1.,1.),(1.,1.),(1.,1.),(1.,1.),(1.,1.),(1.,1.),(1.,1.),(1.,
1.),(1.,1.),(1.,1.),(1.,1.),(1.,1.),(1.,1.),(1.,1.),(1.,1.),(1.,1.),(1.,
1.),(1.,1.),(1.,1.),(1.,1.),(1.,1.),(1.,1.),(1.,1.),(1.,1.),(1.,1.),(1.,
1.),(1.,1.),(1.,1.),(1.,1.),(1.,1.),(1.,1.),(1.,1.),(1.,1.),(1.,1.),(1.,
1.),(1.,1.),(1.,1.),(1.,1.),(1.,1.),(1.,1.),(1.,1.),(1.,1.),(1.,1.),(1.,
1.),(1.,1.),(1.,1.),(1.,1.),(1.,1.),(1.,1.),(1.,1.),(1.,1.),(1.,1.),(1.,
1.),(1.,1.),(1.,1.),(1.,1.),(1.,1.),(1.,1.),(1.,1.),(1.,1.),(1.,1.),(1.,
1.),(1.,1.),(1.,1.),(1.,1.),(1.,1.),(1.,1.),(1.,1.),(1.,1.),(1.,1.),(1.,
1.),(1.,1.)))
REPRESENTATION_ITEM('')
SURFACE()
);
#1078=(
BOUNDED_SURFACE()
B_SPLINE_SURFACE(5,1,((#218483,#218484),(#218485,#218486),(#218487,#218488),
(#218489,#218490),(#218491,#218492),(#218493,#218494),(#218495,#218496),
(#218497,#218498),(#218499,#218500),(#218501,#218502),(#218503,#218504),
(#218505,#218506),(#218507,#218508),(#218509,#218510),(#218511,#218512),
(#218513,#218514),(#218515,#218516),(#218517,#218518),(#218519,#218520),
(#218521,#218522),(#218523,#218524),(#218525,#218526),(#218527,#218528),
(#218529,#218530),(#218531,#218532),(#218533,#218534),(#218535,#218536),
(#218537,#218538),(#218539,#218540),(#218541,#218542),(#218543,#218544),
(#218545,#218546),(#218547,#218548),(#218549,#218550),(#218551,#218552),
(#218553,#218554),(#218555,#218556),(#218557,#218558),(#218559,#218560),
(#218561,#218562),(#218563,#218564),(#218565,#218566),(#218567,#218568),
(#218569,#218570),(#218571,#218572),(#218573,#218574),(#218575,#218576),
(#218577,#218578),(#218579,#218580),(#218581,#218582),(#218583,#218584),
(#218585,#218586),(#218587,#218588),(#218589,#218590),(#218591,#218592),
(#218593,#218594),(#218595,#218596),(#218597,#218598),(#218599,#218600),
(#218601,#218602),(#218603,#218604),(#218605,#218606),(#218607,#218608),
(#218609,#218610),(#218611,#218612),(#218613,#218614),(#218615,#218616),
(#218617,#218618),(#218619,#218620),(#218621,#218622),(#218623,#218624),
(#218625,#218626),(#218627,#218628),(#218629,#218630),(#218631,#218632),
(#218633,#218634),(#218635,#218636),(#218637,#218638),(#218639,#218640),
(#218641,#218642),(#218643,#218644),(#218645,#218646),(#218647,#218648),
(#218649,#218650),(#218651,#218652),(#218653,#218654),(#218655,#218656),
(#218657,#218658),(#218659,#218660),(#218661,#218662),(#218663,#218664),
(#218665,#218666),(#218667,#218668),(#218669,#218670),(#218671,#218672),
(#218673,#218674),(#218675,#218676),(#218677,#218678),(#218679,#218680),
(#218681,#218682),(#218683,#218684),(#218685,#218686),(#218687,#218688),
(#218689,#218690),(#218691,#218692),(#218693,#218694),(#218695,#218696),
(#218697,#218698),(#218699,#218700),(#218701,#218702),(#218703,#218704),
(#218705,#218706),(#218707,#218708),(#218709,#218710),(#218711,#218712),
(#218713,#218714),(#218715,#218716),(#218717,#218718),(#218719,#218720),
(#218721,#218722),(#218723,#218724),(#218725,#218726),(#218727,#218728),
(#218729,#218730),(#218731,#218732),(#218733,#218734),(#218735,#218736),
(#218737,#218738),(#218739,#218740),(#218741,#218742),(#218743,#218744),
(#218745,#218746),(#218747,#218748),(#218749,#218750),(#218751,#218752),
(#218753,#218754),(#218755,#218756),(#218757,#218758),(#218759,#218760),
(#218761,#218762),(#218763,#218764),(#218765,#218766),(#218767,#218768),
(#218769,#218770),(#218771,#218772),(#218773,#218774),(#218775,#218776),
(#218777,#218778),(#218779,#218780),(#218781,#218782),(#218783,#218784),
(#218785,#218786),(#218787,#218788),(#218789,#218790),(#218791,#218792),
(#218793,#218794),(#218795,#218796),(#218797,#218798),(#218799,#218800),
(#218801,#218802),(#218803,#218804),(#218805,#218806),(#218807,#218808),
(#218809,#218810),(#218811,#218812),(#218813,#218814),(#218815,#218816),
(#218817,#218818),(#218819,#218820),(#218821,#218822),(#218823,#218824),
(#218825,#218826),(#218827,#218828),(#218829,#218830),(#218831,#218832),
(#218833,#218834),(#218835,#218836),(#218837,#218838),(#218839,#218840),
(#218841,#218842),(#218843,#218844),(#218845,#218846),(#218847,#218848),
(#218849,#218850),(#218851,#218852),(#218853,#218854),(#218855,#218856),
(#218857,#218858),(#218859,#218860),(#218861,#218862),(#218863,#218864),
(#218865,#218866),(#218867,#218868),(#218869,#218870),(#218871,#218872),
(#218873,#218874),(#218875,#218876),(#218877,#218878),(#218879,#218880),
(#218881,#218882),(#218883,#218884),(#218885,#218886),(#218887,#218888),
(#218889,#218890),(#218891,#218892)),.UNSPECIFIED.,.F.,.F.,.F.)
B_SPLINE_SURFACE_WITH_KNOTS((6,1,1,1,1,1,1,1,1,1,1,1,1,1,1,1,1,1,1,1,1,
1,1,1,1,1,1,1,1,1,1,1,1,1,1,1,1,1,1,1,1,1,1,1,1,1,1,1,1,1,1,1,1,1,1,1,1,
1,1,1,1,1,1,1,1,1,1,1,1,1,1,1,1,1,1,1,1,1,1,1,1,1,1,1,1,1,1,1,1,1,1,1,1,
1,1,1,1,1,1,1,1,1,1,1,1,1,1,1,1,1,1,1,1,1,1,1,1,1,1,1,1,1,1,1,1,1,1,1,1,
1,1,1,1,1,1,1,1,1,1,1,1,1,1,1,1,1,1,1,1,1,1,1,1,1,1,1,1,1,1,1,1,1,1,1,1,
1,1,1,1,1,1,1,1,1,1,1,1,1,1,1,1,1,1,1,1,1,1,1,1,1,1,1,1,1,1,1,1,1,1,1,6),
(2,2),(0.,0.005,0.01,0.015,0.02,0.025,0.03,0.035,0.04,0.045,0.05,0.055,
0.06,0.065,0.07,0.075,0.08,0.085,0.09,0.095,0.1,0.105,0.11,0.115,0.12,0.125,
0.13,0.135,0.14,0.145,0.15,0.155,0.16,0.165,0.17,0.175,0.18,0.185,0.19,
0.195,0.2,0.205,0.21,0.215,0.22,0.225,0.23,0.235,0.24,0.245,0.25,0.255,
0.26,0.265,0.27,0.275,0.28,0.285,0.29,0.295,0.3,0.305,0.31,0.315,0.32,0.325,
0.33,0.335,0.34,0.345,0.35,0.355,0.36,0.365,0.37,0.375,0.38,0.385,0.39,
0.395,0.4,0.405,0.41,0.415,0.42,0.425,0.43,0.435,0.44,0.445,0.45,0.455,
0.46,0.465,0.47,0.475,0.48,0.485,0.49,0.495,0.5,0.505,0.51,0.515,0.52,0.525,
0.53,0.535,0.54,0.545,0.55,0.555,0.56,0.565,0.57,0.575,0.58,0.585,0.59,
0.595,0.6,0.605,0.61,0.615,0.62,0.625,0.63,0.635,0.64,0.645,0.65,0.655,
0.66,0.665,0.67,0.675,0.68,0.685,0.690000000000001,0.695000000000001,0.700000000000001,
0.705000000000001,0.710000000000001,0.715000000000001,0.720000000000001,
0.725000000000001,0.730000000000001,0.735000000000001,0.740000000000001,
0.745000000000001,0.750000000000001,0.755000000000001,0.760000000000001,
0.765000000000001,0.770000000000001,0.775000000000001,0.780000000000001,
0.785000000000001,0.790000000000001,0.795000000000001,0.800000000000001,
0.805000000000001,0.810000000000001,0.815000000000001,0.820000000000001,
0.825000000000001,0.830000000000001,0.835000000000001,0.840000000000001,
0.845000000000001,0.850000000000001,0.855000000000001,0.860000000000001,
0.865000000000001,0.870000000000001,0.875000000000001,0.880000000000001,
0.885000000000001,0.890000000000001,0.895000000000001,0.900000000000001,
0.905000000000001,0.910000000000001,0.915000000000001,0.920000000000001,
0.925000000000001,0.930000000000001,0.935000000000001,0.940000000000001,
0.945000000000001,0.950000000000001,0.955000000000001,0.960000000000001,
0.965000000000001,0.970000000000001,0.975000000000001,0.980000000000001,
0.985000000000001,0.990000000000001,0.995000000000001,1.),(0.,1.2),
 .UNSPECIFIED.)
GEOMETRIC_REPRESENTATION_ITEM()
RATIONAL_B_SPLINE_SURFACE(((1.,1.),(1.,1.),(1.,1.),(1.,1.),(1.,1.),(1.,
1.),(1.,1.),(1.,1.),(1.,1.),(1.,1.),(1.,1.),(1.,1.),(1.,1.),(1.,1.),(1.,
1.),(1.,1.),(1.,1.),(1.,1.),(1.,1.),(1.,1.),(1.,1.),(1.,1.),(1.,1.),(1.,
1.),(1.,1.),(1.,1.),(1.,1.),(1.,1.),(1.,1.),(1.,1.),(1.,1.),(1.,1.),(1.,
1.),(1.,1.),(1.,1.),(1.,1.),(1.,1.),(1.,1.),(1.,1.),(1.,1.),(1.,1.),(1.,
1.),(1.,1.),(1.,1.),(1.,1.),(1.,1.),(1.,1.),(1.,1.),(1.,1.),(1.,1.),(1.,
1.),(1.,1.),(1.,1.),(1.,1.),(1.,1.),(1.,1.),(1.,1.),(1.,1.),(1.,1.),(1.,
1.),(1.,1.),(1.,1.),(1.,1.),(1.,1.),(1.,1.),(1.,1.),(1.,1.),(1.,1.),(1.,
1.),(1.,1.),(1.,1.),(1.,1.),(1.,1.),(1.,1.),(1.,1.),(1.,1.),(1.,1.),(1.,
1.),(1.,1.),(1.,1.),(1.,1.),(1.,1.),(1.,1.),(1.,1.),(1.,1.),(1.,1.),(1.,
1.),(1.,1.),(1.,1.),(1.,1.),(1.,1.),(1.,1.),(1.,1.),(1.,1.),(1.,1.),(1.,
1.),(1.,1.),(1.,1.),(1.,1.),(1.,1.),(1.,1.),(1.,1.),(1.,1.),(1.,1.),(1.,
1.),(1.,1.),(1.,1.),(1.,1.),(1.,1.),(1.,1.),(1.,1.),(1.,1.),(1.,1.),(1.,
1.),(1.,1.),(1.,1.),(1.,1.),(1.,1.),(1.,1.),(1.,1.),(1.,1.),(1.,1.),(1.,
1.),(1.,1.),(1.,1.),(1.,1.),(1.,1.),(1.,1.),(1.,1.),(1.,1.),(1.,1.),(1.,
1.),(1.,1.),(1.,1.),(1.,1.),(1.,1.),(1.,1.),(1.,1.),(1.,1.),(1.,1.),(1.,
1.),(1.,1.),(1.,1.),(1.,1.),(1.,1.),(1.,1.),(1.,1.),(1.,1.),(1.,1.),(1.,
1.),(1.,1.),(1.,1.),(1.,1.),(1.,1.),(1.,1.),(1.,1.),(1.,1.),(1.,1.),(1.,
1.),(1.,1.),(1.,1.),(1.,1.),(1.,1.),(1.,1.),(1.,1.),(1.,1.),(1.,1.),(1.,
1.),(1.,1.),(1.,1.),(1.,1.),(1.,1.),(1.,1.),(1.,1.),(1.,1.),(1.,1.),(1.,
1.),(1.,1.),(1.,1.),(1.,1.),(1.,1.),(1.,1.),(1.,1.),(1.,1.),(1.,1.),(1.,
1.),(1.,1.),(1.,1.),(1.,1.),(1.,1.),(1.,1.),(1.,1.),(1.,1.),(1.,1.),(1.,
1.),(1.,1.),(1.,1.),(1.,1.),(1.,1.),(1.,1.),(1.,1.),(1.,1.),(1.,1.),(1.,
1.),(1.,1.)))
REPRESENTATION_ITEM('')
SURFACE()
);
#1079=(
BOUNDED_SURFACE()
B_SPLINE_SURFACE(5,1,((#219312,#219313),(#219314,#219315),(#219316,#219317),
(#219318,#219319),(#219320,#219321),(#219322,#219323),(#219324,#219325),
(#219326,#219327),(#219328,#219329),(#219330,#219331),(#219332,#219333),
(#219334,#219335),(#219336,#219337),(#219338,#219339),(#219340,#219341),
(#219342,#219343),(#219344,#219345),(#219346,#219347),(#219348,#219349),
(#219350,#219351),(#219352,#219353),(#219354,#219355),(#219356,#219357),
(#219358,#219359),(#219360,#219361),(#219362,#219363),(#219364,#219365),
(#219366,#219367),(#219368,#219369),(#219370,#219371),(#219372,#219373),
(#219374,#219375),(#219376,#219377),(#219378,#219379),(#219380,#219381),
(#219382,#219383),(#219384,#219385),(#219386,#219387),(#219388,#219389),
(#219390,#219391),(#219392,#219393),(#219394,#219395),(#219396,#219397),
(#219398,#219399),(#219400,#219401),(#219402,#219403),(#219404,#219405),
(#219406,#219407),(#219408,#219409),(#219410,#219411),(#219412,#219413),
(#219414,#219415),(#219416,#219417),(#219418,#219419),(#219420,#219421),
(#219422,#219423),(#219424,#219425),(#219426,#219427),(#219428,#219429),
(#219430,#219431),(#219432,#219433),(#219434,#219435),(#219436,#219437),
(#219438,#219439),(#219440,#219441),(#219442,#219443),(#219444,#219445),
(#219446,#219447),(#219448,#219449),(#219450,#219451),(#219452,#219453),
(#219454,#219455),(#219456,#219457),(#219458,#219459),(#219460,#219461),
(#219462,#219463),(#219464,#219465),(#219466,#219467),(#219468,#219469),
(#219470,#219471),(#219472,#219473),(#219474,#219475),(#219476,#219477),
(#219478,#219479),(#219480,#219481),(#219482,#219483),(#219484,#219485),
(#219486,#219487),(#219488,#219489),(#219490,#219491),(#219492,#219493),
(#219494,#219495),(#219496,#219497),(#219498,#219499),(#219500,#219501),
(#219502,#219503),(#219504,#219505),(#219506,#219507),(#219508,#219509),
(#219510,#219511),(#219512,#219513),(#219514,#219515),(#219516,#219517),
(#219518,#219519),(#219520,#219521),(#219522,#219523),(#219524,#219525),
(#219526,#219527),(#219528,#219529),(#219530,#219531),(#219532,#219533),
(#219534,#219535),(#219536,#219537),(#219538,#219539),(#219540,#219541),
(#219542,#219543),(#219544,#219545),(#219546,#219547),(#219548,#219549),
(#219550,#219551),(#219552,#219553),(#219554,#219555),(#219556,#219557),
(#219558,#219559),(#219560,#219561),(#219562,#219563),(#219564,#219565),
(#219566,#219567),(#219568,#219569),(#219570,#219571),(#219572,#219573),
(#219574,#219575),(#219576,#219577),(#219578,#219579),(#219580,#219581),
(#219582,#219583),(#219584,#219585),(#219586,#219587),(#219588,#219589),
(#219590,#219591),(#219592,#219593),(#219594,#219595),(#219596,#219597),
(#219598,#219599),(#219600,#219601),(#219602,#219603),(#219604,#219605),
(#219606,#219607),(#219608,#219609),(#219610,#219611),(#219612,#219613),
(#219614,#219615),(#219616,#219617),(#219618,#219619),(#219620,#219621),
(#219622,#219623),(#219624,#219625),(#219626,#219627),(#219628,#219629),
(#219630,#219631),(#219632,#219633),(#219634,#219635),(#219636,#219637),
(#219638,#219639),(#219640,#219641),(#219642,#219643),(#219644,#219645),
(#219646,#219647),(#219648,#219649),(#219650,#219651),(#219652,#219653),
(#219654,#219655),(#219656,#219657),(#219658,#219659),(#219660,#219661),
(#219662,#219663),(#219664,#219665),(#219666,#219667),(#219668,#219669),
(#219670,#219671),(#219672,#219673),(#219674,#219675),(#219676,#219677),
(#219678,#219679),(#219680,#219681),(#219682,#219683),(#219684,#219685),
(#219686,#219687),(#219688,#219689),(#219690,#219691),(#219692,#219693),
(#219694,#219695),(#219696,#219697),(#219698,#219699),(#219700,#219701),
(#219702,#219703),(#219704,#219705),(#219706,#219707),(#219708,#219709),
(#219710,#219711),(#219712,#219713),(#219714,#219715),(#219716,#219717),
(#219718,#219719),(#219720,#219721)),.UNSPECIFIED.,.F.,.F.,.F.)
B_SPLINE_SURFACE_WITH_KNOTS((6,1,1,1,1,1,1,1,1,1,1,1,1,1,1,1,1,1,1,1,1,
1,1,1,1,1,1,1,1,1,1,1,1,1,1,1,1,1,1,1,1,1,1,1,1,1,1,1,1,1,1,1,1,1,1,1,1,
1,1,1,1,1,1,1,1,1,1,1,1,1,1,1,1,1,1,1,1,1,1,1,1,1,1,1,1,1,1,1,1,1,1,1,1,
1,1,1,1,1,1,1,1,1,1,1,1,1,1,1,1,1,1,1,1,1,1,1,1,1,1,1,1,1,1,1,1,1,1,1,1,
1,1,1,1,1,1,1,1,1,1,1,1,1,1,1,1,1,1,1,1,1,1,1,1,1,1,1,1,1,1,1,1,1,1,1,1,
1,1,1,1,1,1,1,1,1,1,1,1,1,1,1,1,1,1,1,1,1,1,1,1,1,1,1,1,1,1,1,1,1,1,1,6),
(2,2),(-1.,-0.995000000000001,-0.990000000000001,-0.985000000000001,-0.980000000000001,
-0.975000000000001,-0.970000000000001,-0.965000000000001,-0.960000000000001,
-0.955000000000001,-0.950000000000001,-0.945000000000001,-0.940000000000001,
-0.935000000000001,-0.930000000000001,-0.925000000000001,-0.920000000000001,
-0.915000000000001,-0.910000000000001,-0.905000000000001,-0.900000000000001,
-0.895000000000001,-0.890000000000001,-0.885000000000001,-0.880000000000001,
-0.875000000000001,-0.870000000000001,-0.865000000000001,-0.860000000000001,
-0.855000000000001,-0.850000000000001,-0.845000000000001,-0.840000000000001,
-0.835000000000001,-0.830000000000001,-0.825000000000001,-0.820000000000001,
-0.815000000000001,-0.810000000000001,-0.805000000000001,-0.800000000000001,
-0.795000000000001,-0.790000000000001,-0.785000000000001,-0.780000000000001,
-0.775000000000001,-0.770000000000001,-0.765000000000001,-0.760000000000001,
-0.755000000000001,-0.750000000000001,-0.745000000000001,-0.740000000000001,
-0.735000000000001,-0.730000000000001,-0.725000000000001,-0.720000000000001,
-0.715000000000001,-0.710000000000001,-0.705000000000001,-0.700000000000001,
-0.695000000000001,-0.690000000000001,-0.685,-0.68,-0.675,-0.67,-0.665,
-0.66,-0.655,-0.65,-0.645,-0.64,-0.635,-0.63,-0.625,-0.62,-0.615,-0.61,
-0.605,-0.6,-0.595,-0.59,-0.585,-0.58,-0.575,-0.57,-0.565,-0.56,-0.555,
-0.55,-0.545,-0.54,-0.535,-0.53,-0.525,-0.52,-0.515,-0.51,-0.505,-0.5,-0.495,
-0.49,-0.485,-0.48,-0.475,-0.47,-0.465,-0.46,-0.455,-0.45,-0.445,-0.44,
-0.435,-0.43,-0.425,-0.42,-0.415,-0.41,-0.405,-0.4,-0.395,-0.39,-0.385,
-0.38,-0.375,-0.37,-0.365,-0.36,-0.355,-0.35,-0.345,-0.34,-0.335,-0.33,
-0.325,-0.32,-0.315,-0.31,-0.305,-0.3,-0.295,-0.29,-0.285,-0.28,-0.275,
-0.27,-0.265,-0.26,-0.255,-0.25,-0.245,-0.24,-0.235,-0.23,-0.225,-0.22,
-0.215,-0.21,-0.205,-0.2,-0.195,-0.19,-0.185,-0.18,-0.175,-0.17,-0.165,
-0.16,-0.155,-0.15,-0.145,-0.14,-0.135,-0.13,-0.125,-0.12,-0.115,-0.11,
-0.105,-0.1,-0.095,-0.09,-0.085,-0.08,-0.075,-0.07,-0.065,-0.06,-0.055,
-0.05,-0.045,-0.04,-0.035,-0.03,-0.025,-0.02,-0.015,-0.01,-0.005,0.),(0.,
1.2),.UNSPECIFIED.)
GEOMETRIC_REPRESENTATION_ITEM()
RATIONAL_B_SPLINE_SURFACE(((1.,1.),(1.,1.),(1.,1.),(1.,1.),(1.,1.),(1.,
1.),(1.,1.),(1.,1.),(1.,1.),(1.,1.),(1.,1.),(1.,1.),(1.,1.),(1.,1.),(1.,
1.),(1.,1.),(1.,1.),(1.,1.),(1.,1.),(1.,1.),(1.,1.),(1.,1.),(1.,1.),(1.,
1.),(1.,1.),(1.,1.),(1.,1.),(1.,1.),(1.,1.),(1.,1.),(1.,1.),(1.,1.),(1.,
1.),(1.,1.),(1.,1.),(1.,1.),(1.,1.),(1.,1.),(1.,1.),(1.,1.),(1.,1.),(1.,
1.),(1.,1.),(1.,1.),(1.,1.),(1.,1.),(1.,1.),(1.,1.),(1.,1.),(1.,1.),(1.,
1.),(1.,1.),(1.,1.),(1.,1.),(1.,1.),(1.,1.),(1.,1.),(1.,1.),(1.,1.),(1.,
1.),(1.,1.),(1.,1.),(1.,1.),(1.,1.),(1.,1.),(1.,1.),(1.,1.),(1.,1.),(1.,
1.),(1.,1.),(1.,1.),(1.,1.),(1.,1.),(1.,1.),(1.,1.),(1.,1.),(1.,1.),(1.,
1.),(1.,1.),(1.,1.),(1.,1.),(1.,1.),(1.,1.),(1.,1.),(1.,1.),(1.,1.),(1.,
1.),(1.,1.),(1.,1.),(1.,1.),(1.,1.),(1.,1.),(1.,1.),(1.,1.),(1.,1.),(1.,
1.),(1.,1.),(1.,1.),(1.,1.),(1.,1.),(1.,1.),(1.,1.),(1.,1.),(1.,1.),(1.,
1.),(1.,1.),(1.,1.),(1.,1.),(1.,1.),(1.,1.),(1.,1.),(1.,1.),(1.,1.),(1.,
1.),(1.,1.),(1.,1.),(1.,1.),(1.,1.),(1.,1.),(1.,1.),(1.,1.),(1.,1.),(1.,
1.),(1.,1.),(1.,1.),(1.,1.),(1.,1.),(1.,1.),(1.,1.),(1.,1.),(1.,1.),(1.,
1.),(1.,1.),(1.,1.),(1.,1.),(1.,1.),(1.,1.),(1.,1.),(1.,1.),(1.,1.),(1.,
1.),(1.,1.),(1.,1.),(1.,1.),(1.,1.),(1.,1.),(1.,1.),(1.,1.),(1.,1.),(1.,
1.),(1.,1.),(1.,1.),(1.,1.),(1.,1.),(1.,1.),(1.,1.),(1.,1.),(1.,1.),(1.,
1.),(1.,1.),(1.,1.),(1.,1.),(1.,1.),(1.,1.),(1.,1.),(1.,1.),(1.,1.),(1.,
1.),(1.,1.),(1.,1.),(1.,1.),(1.,1.),(1.,1.),(1.,1.),(1.,1.),(1.,1.),(1.,
1.),(1.,1.),(1.,1.),(1.,1.),(1.,1.),(1.,1.),(1.,1.),(1.,1.),(1.,1.),(1.,
1.),(1.,1.),(1.,1.),(1.,1.),(1.,1.),(1.,1.),(1.,1.),(1.,1.),(1.,1.),(1.,
1.),(1.,1.),(1.,1.),(1.,1.),(1.,1.),(1.,1.),(1.,1.),(1.,1.),(1.,1.),(1.,
1.),(1.,1.)))
REPRESENTATION_ITEM('')
SURFACE()
);
#1080=(
BOUNDED_SURFACE()
B_SPLINE_SURFACE(5,1,((#220135,#220136),(#220137,#220138),(#220139,#220140),
(#220141,#220142),(#220143,#220144),(#220145,#220146),(#220147,#220148),
(#220149,#220150),(#220151,#220152),(#220153,#220154),(#220155,#220156),
(#220157,#220158),(#220159,#220160),(#220161,#220162),(#220163,#220164),
(#220165,#220166),(#220167,#220168),(#220169,#220170),(#220171,#220172),
(#220173,#220174),(#220175,#220176),(#220177,#220178),(#220179,#220180),
(#220181,#220182),(#220183,#220184),(#220185,#220186),(#220187,#220188),
(#220189,#220190),(#220191,#220192),(#220193,#220194),(#220195,#220196),
(#220197,#220198),(#220199,#220200),(#220201,#220202),(#220203,#220204),
(#220205,#220206),(#220207,#220208),(#220209,#220210),(#220211,#220212),
(#220213,#220214),(#220215,#220216),(#220217,#220218),(#220219,#220220),
(#220221,#220222),(#220223,#220224),(#220225,#220226),(#220227,#220228),
(#220229,#220230),(#220231,#220232),(#220233,#220234),(#220235,#220236),
(#220237,#220238),(#220239,#220240),(#220241,#220242),(#220243,#220244),
(#220245,#220246),(#220247,#220248),(#220249,#220250),(#220251,#220252),
(#220253,#220254),(#220255,#220256),(#220257,#220258),(#220259,#220260),
(#220261,#220262),(#220263,#220264),(#220265,#220266),(#220267,#220268),
(#220269,#220270),(#220271,#220272),(#220273,#220274),(#220275,#220276),
(#220277,#220278),(#220279,#220280),(#220281,#220282),(#220283,#220284),
(#220285,#220286),(#220287,#220288),(#220289,#220290),(#220291,#220292),
(#220293,#220294),(#220295,#220296),(#220297,#220298),(#220299,#220300),
(#220301,#220302),(#220303,#220304),(#220305,#220306),(#220307,#220308),
(#220309,#220310),(#220311,#220312),(#220313,#220314),(#220315,#220316),
(#220317,#220318),(#220319,#220320),(#220321,#220322),(#220323,#220324),
(#220325,#220326),(#220327,#220328),(#220329,#220330),(#220331,#220332),
(#220333,#220334),(#220335,#220336),(#220337,#220338),(#220339,#220340),
(#220341,#220342),(#220343,#220344),(#220345,#220346),(#220347,#220348),
(#220349,#220350),(#220351,#220352),(#220353,#220354),(#220355,#220356),
(#220357,#220358),(#220359,#220360),(#220361,#220362),(#220363,#220364),
(#220365,#220366),(#220367,#220368),(#220369,#220370),(#220371,#220372),
(#220373,#220374),(#220375,#220376),(#220377,#220378),(#220379,#220380),
(#220381,#220382),(#220383,#220384),(#220385,#220386),(#220387,#220388),
(#220389,#220390),(#220391,#220392),(#220393,#220394),(#220395,#220396),
(#220397,#220398),(#220399,#220400),(#220401,#220402),(#220403,#220404),
(#220405,#220406),(#220407,#220408),(#220409,#220410),(#220411,#220412),
(#220413,#220414),(#220415,#220416),(#220417,#220418),(#220419,#220420),
(#220421,#220422),(#220423,#220424),(#220425,#220426),(#220427,#220428),
(#220429,#220430),(#220431,#220432),(#220433,#220434),(#220435,#220436),
(#220437,#220438),(#220439,#220440),(#220441,#220442),(#220443,#220444),
(#220445,#220446),(#220447,#220448),(#220449,#220450),(#220451,#220452),
(#220453,#220454),(#220455,#220456),(#220457,#220458),(#220459,#220460),
(#220461,#220462),(#220463,#220464),(#220465,#220466),(#220467,#220468),
(#220469,#220470),(#220471,#220472),(#220473,#220474),(#220475,#220476),
(#220477,#220478),(#220479,#220480),(#220481,#220482),(#220483,#220484),
(#220485,#220486),(#220487,#220488),(#220489,#220490),(#220491,#220492),
(#220493,#220494),(#220495,#220496),(#220497,#220498),(#220499,#220500),
(#220501,#220502),(#220503,#220504),(#220505,#220506),(#220507,#220508),
(#220509,#220510),(#220511,#220512),(#220513,#220514),(#220515,#220516),
(#220517,#220518),(#220519,#220520),(#220521,#220522),(#220523,#220524),
(#220525,#220526),(#220527,#220528),(#220529,#220530),(#220531,#220532),
(#220533,#220534),(#220535,#220536),(#220537,#220538),(#220539,#220540),
(#220541,#220542),(#220543,#220544)),.UNSPECIFIED.,.F.,.F.,.F.)
B_SPLINE_SURFACE_WITH_KNOTS((6,1,1,1,1,1,1,1,1,1,1,1,1,1,1,1,1,1,1,1,1,
1,1,1,1,1,1,1,1,1,1,1,1,1,1,1,1,1,1,1,1,1,1,1,1,1,1,1,1,1,1,1,1,1,1,1,1,
1,1,1,1,1,1,1,1,1,1,1,1,1,1,1,1,1,1,1,1,1,1,1,1,1,1,1,1,1,1,1,1,1,1,1,1,
1,1,1,1,1,1,1,1,1,1,1,1,1,1,1,1,1,1,1,1,1,1,1,1,1,1,1,1,1,1,1,1,1,1,1,1,
1,1,1,1,1,1,1,1,1,1,1,1,1,1,1,1,1,1,1,1,1,1,1,1,1,1,1,1,1,1,1,1,1,1,1,1,
1,1,1,1,1,1,1,1,1,1,1,1,1,1,1,1,1,1,1,1,1,1,1,1,1,1,1,1,1,1,1,1,1,1,1,6),
(2,2),(0.,0.005,0.01,0.015,0.02,0.025,0.03,0.035,0.04,0.045,0.05,0.055,
0.06,0.065,0.07,0.075,0.08,0.085,0.09,0.095,0.1,0.105,0.11,0.115,0.12,0.125,
0.13,0.135,0.14,0.145,0.15,0.155,0.16,0.165,0.17,0.175,0.18,0.185,0.19,
0.195,0.2,0.205,0.21,0.215,0.22,0.225,0.23,0.235,0.24,0.245,0.25,0.255,
0.26,0.265,0.27,0.275,0.28,0.285,0.29,0.295,0.3,0.305,0.31,0.315,0.32,0.325,
0.33,0.335,0.34,0.345,0.35,0.355,0.36,0.365,0.37,0.375,0.38,0.385,0.39,
0.395,0.4,0.405,0.41,0.415,0.42,0.425,0.43,0.435,0.44,0.445,0.45,0.455,
0.46,0.465,0.47,0.475,0.48,0.485,0.49,0.495,0.5,0.505,0.51,0.515,0.52,0.525,
0.53,0.535,0.54,0.545,0.55,0.555,0.56,0.565,0.57,0.575,0.58,0.585,0.59,
0.595,0.6,0.605,0.61,0.615,0.62,0.625,0.63,0.635,0.64,0.645,0.65,0.655,
0.66,0.665,0.67,0.675,0.68,0.685,0.690000000000001,0.695000000000001,0.700000000000001,
0.705000000000001,0.710000000000001,0.715000000000001,0.720000000000001,
0.725000000000001,0.730000000000001,0.735000000000001,0.740000000000001,
0.745000000000001,0.750000000000001,0.755000000000001,0.760000000000001,
0.765000000000001,0.770000000000001,0.775000000000001,0.780000000000001,
0.785000000000001,0.790000000000001,0.795000000000001,0.800000000000001,
0.805000000000001,0.810000000000001,0.815000000000001,0.820000000000001,
0.825000000000001,0.830000000000001,0.835000000000001,0.840000000000001,
0.845000000000001,0.850000000000001,0.855000000000001,0.860000000000001,
0.865000000000001,0.870000000000001,0.875000000000001,0.880000000000001,
0.885000000000001,0.890000000000001,0.895000000000001,0.900000000000001,
0.905000000000001,0.910000000000001,0.915000000000001,0.920000000000001,
0.925000000000001,0.930000000000001,0.935000000000001,0.940000000000001,
0.945000000000001,0.950000000000001,0.955000000000001,0.960000000000001,
0.965000000000001,0.970000000000001,0.975000000000001,0.980000000000001,
0.985000000000001,0.990000000000001,0.995000000000001,1.),(0.,1.2),
 .UNSPECIFIED.)
GEOMETRIC_REPRESENTATION_ITEM()
RATIONAL_B_SPLINE_SURFACE(((1.,1.),(1.,1.),(1.,1.),(1.,1.),(1.,1.),(1.,
1.),(1.,1.),(1.,1.),(1.,1.),(1.,1.),(1.,1.),(1.,1.),(1.,1.),(1.,1.),(1.,
1.),(1.,1.),(1.,1.),(1.,1.),(1.,1.),(1.,1.),(1.,1.),(1.,1.),(1.,1.),(1.,
1.),(1.,1.),(1.,1.),(1.,1.),(1.,1.),(1.,1.),(1.,1.),(1.,1.),(1.,1.),(1.,
1.),(1.,1.),(1.,1.),(1.,1.),(1.,1.),(1.,1.),(1.,1.),(1.,1.),(1.,1.),(1.,
1.),(1.,1.),(1.,1.),(1.,1.),(1.,1.),(1.,1.),(1.,1.),(1.,1.),(1.,1.),(1.,
1.),(1.,1.),(1.,1.),(1.,1.),(1.,1.),(1.,1.),(1.,1.),(1.,1.),(1.,1.),(1.,
1.),(1.,1.),(1.,1.),(1.,1.),(1.,1.),(1.,1.),(1.,1.),(1.,1.),(1.,1.),(1.,
1.),(1.,1.),(1.,1.),(1.,1.),(1.,1.),(1.,1.),(1.,1.),(1.,1.),(1.,1.),(1.,
1.),(1.,1.),(1.,1.),(1.,1.),(1.,1.),(1.,1.),(1.,1.),(1.,1.),(1.,1.),(1.,
1.),(1.,1.),(1.,1.),(1.,1.),(1.,1.),(1.,1.),(1.,1.),(1.,1.),(1.,1.),(1.,
1.),(1.,1.),(1.,1.),(1.,1.),(1.,1.),(1.,1.),(1.,1.),(1.,1.),(1.,1.),(1.,
1.),(1.,1.),(1.,1.),(1.,1.),(1.,1.),(1.,1.),(1.,1.),(1.,1.),(1.,1.),(1.,
1.),(1.,1.),(1.,1.),(1.,1.),(1.,1.),(1.,1.),(1.,1.),(1.,1.),(1.,1.),(1.,
1.),(1.,1.),(1.,1.),(1.,1.),(1.,1.),(1.,1.),(1.,1.),(1.,1.),(1.,1.),(1.,
1.),(1.,1.),(1.,1.),(1.,1.),(1.,1.),(1.,1.),(1.,1.),(1.,1.),(1.,1.),(1.,
1.),(1.,1.),(1.,1.),(1.,1.),(1.,1.),(1.,1.),(1.,1.),(1.,1.),(1.,1.),(1.,
1.),(1.,1.),(1.,1.),(1.,1.),(1.,1.),(1.,1.),(1.,1.),(1.,1.),(1.,1.),(1.,
1.),(1.,1.),(1.,1.),(1.,1.),(1.,1.),(1.,1.),(1.,1.),(1.,1.),(1.,1.),(1.,
1.),(1.,1.),(1.,1.),(1.,1.),(1.,1.),(1.,1.),(1.,1.),(1.,1.),(1.,1.),(1.,
1.),(1.,1.),(1.,1.),(1.,1.),(1.,1.),(1.,1.),(1.,1.),(1.,1.),(1.,1.),(1.,
1.),(1.,1.),(1.,1.),(1.,1.),(1.,1.),(1.,1.),(1.,1.),(1.,1.),(1.,1.),(1.,
1.),(1.,1.),(1.,1.),(1.,1.),(1.,1.),(1.,1.),(1.,1.),(1.,1.),(1.,1.),(1.,
1.),(1.,1.)))
REPRESENTATION_ITEM('')
SURFACE()
);
#1081=(
BOUNDED_SURFACE()
B_SPLINE_SURFACE(5,1,((#220964,#220965),(#220966,#220967),(#220968,#220969),
(#220970,#220971),(#220972,#220973),(#220974,#220975),(#220976,#220977),
(#220978,#220979),(#220980,#220981),(#220982,#220983),(#220984,#220985),
(#220986,#220987),(#220988,#220989),(#220990,#220991),(#220992,#220993),
(#220994,#220995),(#220996,#220997),(#220998,#220999),(#221000,#221001),
(#221002,#221003),(#221004,#221005),(#221006,#221007),(#221008,#221009),
(#221010,#221011),(#221012,#221013),(#221014,#221015),(#221016,#221017),
(#221018,#221019),(#221020,#221021),(#221022,#221023),(#221024,#221025),
(#221026,#221027),(#221028,#221029),(#221030,#221031),(#221032,#221033),
(#221034,#221035),(#221036,#221037),(#221038,#221039),(#221040,#221041),
(#221042,#221043),(#221044,#221045),(#221046,#221047),(#221048,#221049),
(#221050,#221051),(#221052,#221053),(#221054,#221055),(#221056,#221057),
(#221058,#221059),(#221060,#221061),(#221062,#221063),(#221064,#221065),
(#221066,#221067),(#221068,#221069),(#221070,#221071),(#221072,#221073),
(#221074,#221075),(#221076,#221077),(#221078,#221079),(#221080,#221081),
(#221082,#221083),(#221084,#221085),(#221086,#221087),(#221088,#221089),
(#221090,#221091),(#221092,#221093),(#221094,#221095),(#221096,#221097),
(#221098,#221099),(#221100,#221101),(#221102,#221103),(#221104,#221105),
(#221106,#221107),(#221108,#221109),(#221110,#221111),(#221112,#221113),
(#221114,#221115),(#221116,#221117),(#221118,#221119),(#221120,#221121),
(#221122,#221123),(#221124,#221125),(#221126,#221127),(#221128,#221129),
(#221130,#221131),(#221132,#221133),(#221134,#221135),(#221136,#221137),
(#221138,#221139),(#221140,#221141),(#221142,#221143),(#221144,#221145),
(#221146,#221147),(#221148,#221149),(#221150,#221151),(#221152,#221153),
(#221154,#221155),(#221156,#221157),(#221158,#221159),(#221160,#221161),
(#221162,#221163),(#221164,#221165),(#221166,#221167),(#221168,#221169),
(#221170,#221171),(#221172,#221173),(#221174,#221175),(#221176,#221177),
(#221178,#221179),(#221180,#221181),(#221182,#221183),(#221184,#221185),
(#221186,#221187),(#221188,#221189),(#221190,#221191),(#221192,#221193),
(#221194,#221195),(#221196,#221197),(#221198,#221199),(#221200,#221201),
(#221202,#221203),(#221204,#221205),(#221206,#221207),(#221208,#221209),
(#221210,#221211),(#221212,#221213),(#221214,#221215),(#221216,#221217),
(#221218,#221219),(#221220,#221221),(#221222,#221223),(#221224,#221225),
(#221226,#221227),(#221228,#221229),(#221230,#221231),(#221232,#221233),
(#221234,#221235),(#221236,#221237),(#221238,#221239),(#221240,#221241),
(#221242,#221243),(#221244,#221245),(#221246,#221247),(#221248,#221249),
(#221250,#221251),(#221252,#221253),(#221254,#221255),(#221256,#221257),
(#221258,#221259),(#221260,#221261),(#221262,#221263),(#221264,#221265),
(#221266,#221267),(#221268,#221269),(#221270,#221271),(#221272,#221273),
(#221274,#221275),(#221276,#221277),(#221278,#221279),(#221280,#221281),
(#221282,#221283),(#221284,#221285),(#221286,#221287),(#221288,#221289),
(#221290,#221291),(#221292,#221293),(#221294,#221295),(#221296,#221297),
(#221298,#221299),(#221300,#221301),(#221302,#221303),(#221304,#221305),
(#221306,#221307),(#221308,#221309),(#221310,#221311),(#221312,#221313),
(#221314,#221315),(#221316,#221317),(#221318,#221319),(#221320,#221321),
(#221322,#221323),(#221324,#221325),(#221326,#221327),(#221328,#221329),
(#221330,#221331),(#221332,#221333),(#221334,#221335),(#221336,#221337),
(#221338,#221339),(#221340,#221341),(#221342,#221343),(#221344,#221345),
(#221346,#221347),(#221348,#221349),(#221350,#221351),(#221352,#221353),
(#221354,#221355),(#221356,#221357),(#221358,#221359),(#221360,#221361),
(#221362,#221363),(#221364,#221365),(#221366,#221367),(#221368,#221369),
(#221370,#221371),(#221372,#221373)),.UNSPECIFIED.,.F.,.F.,.F.)
B_SPLINE_SURFACE_WITH_KNOTS((6,1,1,1,1,1,1,1,1,1,1,1,1,1,1,1,1,1,1,1,1,
1,1,1,1,1,1,1,1,1,1,1,1,1,1,1,1,1,1,1,1,1,1,1,1,1,1,1,1,1,1,1,1,1,1,1,1,
1,1,1,1,1,1,1,1,1,1,1,1,1,1,1,1,1,1,1,1,1,1,1,1,1,1,1,1,1,1,1,1,1,1,1,1,
1,1,1,1,1,1,1,1,1,1,1,1,1,1,1,1,1,1,1,1,1,1,1,1,1,1,1,1,1,1,1,1,1,1,1,1,
1,1,1,1,1,1,1,1,1,1,1,1,1,1,1,1,1,1,1,1,1,1,1,1,1,1,1,1,1,1,1,1,1,1,1,1,
1,1,1,1,1,1,1,1,1,1,1,1,1,1,1,1,1,1,1,1,1,1,1,1,1,1,1,1,1,1,1,1,1,1,1,6),
(2,2),(-1.,-0.995000000000001,-0.990000000000001,-0.985000000000001,-0.980000000000001,
-0.975000000000001,-0.970000000000001,-0.965000000000001,-0.960000000000001,
-0.955000000000001,-0.950000000000001,-0.945000000000001,-0.940000000000001,
-0.935000000000001,-0.930000000000001,-0.925000000000001,-0.920000000000001,
-0.915000000000001,-0.910000000000001,-0.905000000000001,-0.900000000000001,
-0.895000000000001,-0.890000000000001,-0.885000000000001,-0.880000000000001,
-0.875000000000001,-0.870000000000001,-0.865000000000001,-0.860000000000001,
-0.855000000000001,-0.850000000000001,-0.845000000000001,-0.840000000000001,
-0.835000000000001,-0.830000000000001,-0.825000000000001,-0.820000000000001,
-0.815000000000001,-0.810000000000001,-0.805000000000001,-0.800000000000001,
-0.795000000000001,-0.790000000000001,-0.785000000000001,-0.780000000000001,
-0.775000000000001,-0.770000000000001,-0.765000000000001,-0.760000000000001,
-0.755000000000001,-0.750000000000001,-0.745000000000001,-0.740000000000001,
-0.735000000000001,-0.730000000000001,-0.725000000000001,-0.720000000000001,
-0.715000000000001,-0.710000000000001,-0.705000000000001,-0.700000000000001,
-0.695000000000001,-0.690000000000001,-0.685,-0.68,-0.675,-0.67,-0.665,
-0.66,-0.655,-0.65,-0.645,-0.64,-0.635,-0.63,-0.625,-0.62,-0.615,-0.61,
-0.605,-0.6,-0.595,-0.59,-0.585,-0.58,-0.575,-0.57,-0.565,-0.56,-0.555,
-0.55,-0.545,-0.54,-0.535,-0.53,-0.525,-0.52,-0.515,-0.51,-0.505,-0.5,-0.495,
-0.49,-0.485,-0.48,-0.475,-0.47,-0.465,-0.46,-0.455,-0.45,-0.445,-0.44,
-0.435,-0.43,-0.425,-0.42,-0.415,-0.41,-0.405,-0.4,-0.395,-0.39,-0.385,
-0.38,-0.375,-0.37,-0.365,-0.36,-0.355,-0.35,-0.345,-0.34,-0.335,-0.33,
-0.325,-0.32,-0.315,-0.31,-0.305,-0.3,-0.295,-0.29,-0.285,-0.28,-0.275,
-0.27,-0.265,-0.26,-0.255,-0.25,-0.245,-0.24,-0.235,-0.23,-0.225,-0.22,
-0.215,-0.21,-0.205,-0.2,-0.195,-0.19,-0.185,-0.18,-0.175,-0.17,-0.165,
-0.16,-0.155,-0.15,-0.145,-0.14,-0.135,-0.13,-0.125,-0.12,-0.115,-0.11,
-0.105,-0.1,-0.095,-0.09,-0.085,-0.08,-0.075,-0.07,-0.065,-0.06,-0.055,
-0.05,-0.045,-0.04,-0.035,-0.03,-0.025,-0.02,-0.015,-0.01,-0.005,0.),(0.,
1.2),.UNSPECIFIED.)
GEOMETRIC_REPRESENTATION_ITEM()
RATIONAL_B_SPLINE_SURFACE(((1.,1.),(1.,1.),(1.,1.),(1.,1.),(1.,1.),(1.,
1.),(1.,1.),(1.,1.),(1.,1.),(1.,1.),(1.,1.),(1.,1.),(1.,1.),(1.,1.),(1.,
1.),(1.,1.),(1.,1.),(1.,1.),(1.,1.),(1.,1.),(1.,1.),(1.,1.),(1.,1.),(1.,
1.),(1.,1.),(1.,1.),(1.,1.),(1.,1.),(1.,1.),(1.,1.),(1.,1.),(1.,1.),(1.,
1.),(1.,1.),(1.,1.),(1.,1.),(1.,1.),(1.,1.),(1.,1.),(1.,1.),(1.,1.),(1.,
1.),(1.,1.),(1.,1.),(1.,1.),(1.,1.),(1.,1.),(1.,1.),(1.,1.),(1.,1.),(1.,
1.),(1.,1.),(1.,1.),(1.,1.),(1.,1.),(1.,1.),(1.,1.),(1.,1.),(1.,1.),(1.,
1.),(1.,1.),(1.,1.),(1.,1.),(1.,1.),(1.,1.),(1.,1.),(1.,1.),(1.,1.),(1.,
1.),(1.,1.),(1.,1.),(1.,1.),(1.,1.),(1.,1.),(1.,1.),(1.,1.),(1.,1.),(1.,
1.),(1.,1.),(1.,1.),(1.,1.),(1.,1.),(1.,1.),(1.,1.),(1.,1.),(1.,1.),(1.,
1.),(1.,1.),(1.,1.),(1.,1.),(1.,1.),(1.,1.),(1.,1.),(1.,1.),(1.,1.),(1.,
1.),(1.,1.),(1.,1.),(1.,1.),(1.,1.),(1.,1.),(1.,1.),(1.,1.),(1.,1.),(1.,
1.),(1.,1.),(1.,1.),(1.,1.),(1.,1.),(1.,1.),(1.,1.),(1.,1.),(1.,1.),(1.,
1.),(1.,1.),(1.,1.),(1.,1.),(1.,1.),(1.,1.),(1.,1.),(1.,1.),(1.,1.),(1.,
1.),(1.,1.),(1.,1.),(1.,1.),(1.,1.),(1.,1.),(1.,1.),(1.,1.),(1.,1.),(1.,
1.),(1.,1.),(1.,1.),(1.,1.),(1.,1.),(1.,1.),(1.,1.),(1.,1.),(1.,1.),(1.,
1.),(1.,1.),(1.,1.),(1.,1.),(1.,1.),(1.,1.),(1.,1.),(1.,1.),(1.,1.),(1.,
1.),(1.,1.),(1.,1.),(1.,1.),(1.,1.),(1.,1.),(1.,1.),(1.,1.),(1.,1.),(1.,
1.),(1.,1.),(1.,1.),(1.,1.),(1.,1.),(1.,1.),(1.,1.),(1.,1.),(1.,1.),(1.,
1.),(1.,1.),(1.,1.),(1.,1.),(1.,1.),(1.,1.),(1.,1.),(1.,1.),(1.,1.),(1.,
1.),(1.,1.),(1.,1.),(1.,1.),(1.,1.),(1.,1.),(1.,1.),(1.,1.),(1.,1.),(1.,
1.),(1.,1.),(1.,1.),(1.,1.),(1.,1.),(1.,1.),(1.,1.),(1.,1.),(1.,1.),(1.,
1.),(1.,1.),(1.,1.),(1.,1.),(1.,1.),(1.,1.),(1.,1.),(1.,1.),(1.,1.),(1.,
1.),(1.,1.)))
REPRESENTATION_ITEM('')
SURFACE()
);
#1082=(
BOUNDED_SURFACE()
B_SPLINE_SURFACE(5,1,((#221787,#221788),(#221789,#221790),(#221791,#221792),
(#221793,#221794),(#221795,#221796),(#221797,#221798),(#221799,#221800),
(#221801,#221802),(#221803,#221804),(#221805,#221806),(#221807,#221808),
(#221809,#221810),(#221811,#221812),(#221813,#221814),(#221815,#221816),
(#221817,#221818),(#221819,#221820),(#221821,#221822),(#221823,#221824),
(#221825,#221826),(#221827,#221828),(#221829,#221830),(#221831,#221832),
(#221833,#221834),(#221835,#221836),(#221837,#221838),(#221839,#221840),
(#221841,#221842),(#221843,#221844),(#221845,#221846),(#221847,#221848),
(#221849,#221850),(#221851,#221852),(#221853,#221854),(#221855,#221856),
(#221857,#221858),(#221859,#221860),(#221861,#221862),(#221863,#221864),
(#221865,#221866),(#221867,#221868),(#221869,#221870),(#221871,#221872),
(#221873,#221874),(#221875,#221876),(#221877,#221878),(#221879,#221880),
(#221881,#221882),(#221883,#221884),(#221885,#221886),(#221887,#221888),
(#221889,#221890),(#221891,#221892),(#221893,#221894),(#221895,#221896),
(#221897,#221898),(#221899,#221900),(#221901,#221902),(#221903,#221904),
(#221905,#221906),(#221907,#221908),(#221909,#221910),(#221911,#221912),
(#221913,#221914),(#221915,#221916),(#221917,#221918),(#221919,#221920),
(#221921,#221922),(#221923,#221924),(#221925,#221926),(#221927,#221928),
(#221929,#221930),(#221931,#221932),(#221933,#221934),(#221935,#221936),
(#221937,#221938),(#221939,#221940),(#221941,#221942),(#221943,#221944),
(#221945,#221946),(#221947,#221948),(#221949,#221950),(#221951,#221952),
(#221953,#221954),(#221955,#221956),(#221957,#221958),(#221959,#221960),
(#221961,#221962),(#221963,#221964),(#221965,#221966),(#221967,#221968),
(#221969,#221970),(#221971,#221972),(#221973,#221974),(#221975,#221976),
(#221977,#221978),(#221979,#221980),(#221981,#221982),(#221983,#221984),
(#221985,#221986),(#221987,#221988),(#221989,#221990),(#221991,#221992),
(#221993,#221994),(#221995,#221996),(#221997,#221998),(#221999,#222000),
(#222001,#222002),(#222003,#222004),(#222005,#222006),(#222007,#222008),
(#222009,#222010),(#222011,#222012),(#222013,#222014),(#222015,#222016),
(#222017,#222018),(#222019,#222020),(#222021,#222022),(#222023,#222024),
(#222025,#222026),(#222027,#222028),(#222029,#222030),(#222031,#222032),
(#222033,#222034),(#222035,#222036),(#222037,#222038),(#222039,#222040),
(#222041,#222042),(#222043,#222044),(#222045,#222046),(#222047,#222048),
(#222049,#222050),(#222051,#222052),(#222053,#222054),(#222055,#222056),
(#222057,#222058),(#222059,#222060),(#222061,#222062),(#222063,#222064),
(#222065,#222066),(#222067,#222068),(#222069,#222070),(#222071,#222072),
(#222073,#222074),(#222075,#222076),(#222077,#222078),(#222079,#222080),
(#222081,#222082),(#222083,#222084),(#222085,#222086),(#222087,#222088),
(#222089,#222090),(#222091,#222092),(#222093,#222094),(#222095,#222096),
(#222097,#222098),(#222099,#222100),(#222101,#222102),(#222103,#222104),
(#222105,#222106),(#222107,#222108),(#222109,#222110),(#222111,#222112),
(#222113,#222114),(#222115,#222116),(#222117,#222118),(#222119,#222120),
(#222121,#222122),(#222123,#222124),(#222125,#222126),(#222127,#222128),
(#222129,#222130),(#222131,#222132),(#222133,#222134),(#222135,#222136),
(#222137,#222138),(#222139,#222140),(#222141,#222142),(#222143,#222144),
(#222145,#222146),(#222147,#222148),(#222149,#222150),(#222151,#222152),
(#222153,#222154),(#222155,#222156),(#222157,#222158),(#222159,#222160),
(#222161,#222162),(#222163,#222164),(#222165,#222166),(#222167,#222168),
(#222169,#222170),(#222171,#222172),(#222173,#222174),(#222175,#222176),
(#222177,#222178),(#222179,#222180),(#222181,#222182),(#222183,#222184),
(#222185,#222186),(#222187,#222188),(#222189,#222190),(#222191,#222192),
(#222193,#222194),(#222195,#222196)),.UNSPECIFIED.,.F.,.F.,.F.)
B_SPLINE_SURFACE_WITH_KNOTS((6,1,1,1,1,1,1,1,1,1,1,1,1,1,1,1,1,1,1,1,1,
1,1,1,1,1,1,1,1,1,1,1,1,1,1,1,1,1,1,1,1,1,1,1,1,1,1,1,1,1,1,1,1,1,1,1,1,
1,1,1,1,1,1,1,1,1,1,1,1,1,1,1,1,1,1,1,1,1,1,1,1,1,1,1,1,1,1,1,1,1,1,1,1,
1,1,1,1,1,1,1,1,1,1,1,1,1,1,1,1,1,1,1,1,1,1,1,1,1,1,1,1,1,1,1,1,1,1,1,1,
1,1,1,1,1,1,1,1,1,1,1,1,1,1,1,1,1,1,1,1,1,1,1,1,1,1,1,1,1,1,1,1,1,1,1,1,
1,1,1,1,1,1,1,1,1,1,1,1,1,1,1,1,1,1,1,1,1,1,1,1,1,1,1,1,1,1,1,1,1,1,1,6),
(2,2),(0.,0.005,0.01,0.015,0.02,0.025,0.03,0.035,0.04,0.045,0.05,0.055,
0.06,0.065,0.07,0.075,0.08,0.085,0.09,0.095,0.1,0.105,0.11,0.115,0.12,0.125,
0.13,0.135,0.14,0.145,0.15,0.155,0.16,0.165,0.17,0.175,0.18,0.185,0.19,
0.195,0.2,0.205,0.21,0.215,0.22,0.225,0.23,0.235,0.24,0.245,0.25,0.255,
0.26,0.265,0.27,0.275,0.28,0.285,0.29,0.295,0.3,0.305,0.31,0.315,0.32,0.325,
0.33,0.335,0.34,0.345,0.35,0.355,0.36,0.365,0.37,0.375,0.38,0.385,0.39,
0.395,0.4,0.405,0.41,0.415,0.42,0.425,0.43,0.435,0.44,0.445,0.45,0.455,
0.46,0.465,0.47,0.475,0.48,0.485,0.49,0.495,0.5,0.505,0.51,0.515,0.52,0.525,
0.53,0.535,0.54,0.545,0.55,0.555,0.56,0.565,0.57,0.575,0.58,0.585,0.59,
0.595,0.6,0.605,0.61,0.615,0.62,0.625,0.63,0.635,0.64,0.645,0.65,0.655,
0.66,0.665,0.67,0.675,0.68,0.685,0.690000000000001,0.695000000000001,0.700000000000001,
0.705000000000001,0.710000000000001,0.715000000000001,0.720000000000001,
0.725000000000001,0.730000000000001,0.735000000000001,0.740000000000001,
0.745000000000001,0.750000000000001,0.755000000000001,0.760000000000001,
0.765000000000001,0.770000000000001,0.775000000000001,0.780000000000001,
0.785000000000001,0.790000000000001,0.795000000000001,0.800000000000001,
0.805000000000001,0.810000000000001,0.815000000000001,0.820000000000001,
0.825000000000001,0.830000000000001,0.835000000000001,0.840000000000001,
0.845000000000001,0.850000000000001,0.855000000000001,0.860000000000001,
0.865000000000001,0.870000000000001,0.875000000000001,0.880000000000001,
0.885000000000001,0.890000000000001,0.895000000000001,0.900000000000001,
0.905000000000001,0.910000000000001,0.915000000000001,0.920000000000001,
0.925000000000001,0.930000000000001,0.935000000000001,0.940000000000001,
0.945000000000001,0.950000000000001,0.955000000000001,0.960000000000001,
0.965000000000001,0.970000000000001,0.975000000000001,0.980000000000001,
0.985000000000001,0.990000000000001,0.995000000000001,1.),(0.,1.2),
 .UNSPECIFIED.)
GEOMETRIC_REPRESENTATION_ITEM()
RATIONAL_B_SPLINE_SURFACE(((1.,1.),(1.,1.),(1.,1.),(1.,1.),(1.,1.),(1.,
1.),(1.,1.),(1.,1.),(1.,1.),(1.,1.),(1.,1.),(1.,1.),(1.,1.),(1.,1.),(1.,
1.),(1.,1.),(1.,1.),(1.,1.),(1.,1.),(1.,1.),(1.,1.),(1.,1.),(1.,1.),(1.,
1.),(1.,1.),(1.,1.),(1.,1.),(1.,1.),(1.,1.),(1.,1.),(1.,1.),(1.,1.),(1.,
1.),(1.,1.),(1.,1.),(1.,1.),(1.,1.),(1.,1.),(1.,1.),(1.,1.),(1.,1.),(1.,
1.),(1.,1.),(1.,1.),(1.,1.),(1.,1.),(1.,1.),(1.,1.),(1.,1.),(1.,1.),(1.,
1.),(1.,1.),(1.,1.),(1.,1.),(1.,1.),(1.,1.),(1.,1.),(1.,1.),(1.,1.),(1.,
1.),(1.,1.),(1.,1.),(1.,1.),(1.,1.),(1.,1.),(1.,1.),(1.,1.),(1.,1.),(1.,
1.),(1.,1.),(1.,1.),(1.,1.),(1.,1.),(1.,1.),(1.,1.),(1.,1.),(1.,1.),(1.,
1.),(1.,1.),(1.,1.),(1.,1.),(1.,1.),(1.,1.),(1.,1.),(1.,1.),(1.,1.),(1.,
1.),(1.,1.),(1.,1.),(1.,1.),(1.,1.),(1.,1.),(1.,1.),(1.,1.),(1.,1.),(1.,
1.),(1.,1.),(1.,1.),(1.,1.),(1.,1.),(1.,1.),(1.,1.),(1.,1.),(1.,1.),(1.,
1.),(1.,1.),(1.,1.),(1.,1.),(1.,1.),(1.,1.),(1.,1.),(1.,1.),(1.,1.),(1.,
1.),(1.,1.),(1.,1.),(1.,1.),(1.,1.),(1.,1.),(1.,1.),(1.,1.),(1.,1.),(1.,
1.),(1.,1.),(1.,1.),(1.,1.),(1.,1.),(1.,1.),(1.,1.),(1.,1.),(1.,1.),(1.,
1.),(1.,1.),(1.,1.),(1.,1.),(1.,1.),(1.,1.),(1.,1.),(1.,1.),(1.,1.),(1.,
1.),(1.,1.),(1.,1.),(1.,1.),(1.,1.),(1.,1.),(1.,1.),(1.,1.),(1.,1.),(1.,
1.),(1.,1.),(1.,1.),(1.,1.),(1.,1.),(1.,1.),(1.,1.),(1.,1.),(1.,1.),(1.,
1.),(1.,1.),(1.,1.),(1.,1.),(1.,1.),(1.,1.),(1.,1.),(1.,1.),(1.,1.),(1.,
1.),(1.,1.),(1.,1.),(1.,1.),(1.,1.),(1.,1.),(1.,1.),(1.,1.),(1.,1.),(1.,
1.),(1.,1.),(1.,1.),(1.,1.),(1.,1.),(1.,1.),(1.,1.),(1.,1.),(1.,1.),(1.,
1.),(1.,1.),(1.,1.),(1.,1.),(1.,1.),(1.,1.),(1.,1.),(1.,1.),(1.,1.),(1.,
1.),(1.,1.),(1.,1.),(1.,1.),(1.,1.),(1.,1.),(1.,1.),(1.,1.),(1.,1.),(1.,
1.),(1.,1.)))
REPRESENTATION_ITEM('')
SURFACE()
);
#1083=(
BOUNDED_SURFACE()
B_SPLINE_SURFACE(5,1,((#222616,#222617),(#222618,#222619),(#222620,#222621),
(#222622,#222623),(#222624,#222625),(#222626,#222627),(#222628,#222629),
(#222630,#222631),(#222632,#222633),(#222634,#222635),(#222636,#222637),
(#222638,#222639),(#222640,#222641),(#222642,#222643),(#222644,#222645),
(#222646,#222647),(#222648,#222649),(#222650,#222651),(#222652,#222653),
(#222654,#222655),(#222656,#222657),(#222658,#222659),(#222660,#222661),
(#222662,#222663),(#222664,#222665),(#222666,#222667),(#222668,#222669),
(#222670,#222671),(#222672,#222673),(#222674,#222675),(#222676,#222677),
(#222678,#222679),(#222680,#222681),(#222682,#222683),(#222684,#222685),
(#222686,#222687),(#222688,#222689),(#222690,#222691),(#222692,#222693),
(#222694,#222695),(#222696,#222697),(#222698,#222699),(#222700,#222701),
(#222702,#222703),(#222704,#222705),(#222706,#222707),(#222708,#222709),
(#222710,#222711),(#222712,#222713),(#222714,#222715),(#222716,#222717),
(#222718,#222719),(#222720,#222721),(#222722,#222723),(#222724,#222725),
(#222726,#222727),(#222728,#222729),(#222730,#222731),(#222732,#222733),
(#222734,#222735),(#222736,#222737),(#222738,#222739),(#222740,#222741),
(#222742,#222743),(#222744,#222745),(#222746,#222747),(#222748,#222749),
(#222750,#222751),(#222752,#222753),(#222754,#222755),(#222756,#222757),
(#222758,#222759),(#222760,#222761),(#222762,#222763),(#222764,#222765),
(#222766,#222767),(#222768,#222769),(#222770,#222771),(#222772,#222773),
(#222774,#222775),(#222776,#222777),(#222778,#222779),(#222780,#222781),
(#222782,#222783),(#222784,#222785),(#222786,#222787),(#222788,#222789),
(#222790,#222791),(#222792,#222793),(#222794,#222795),(#222796,#222797),
(#222798,#222799),(#222800,#222801),(#222802,#222803),(#222804,#222805),
(#222806,#222807),(#222808,#222809),(#222810,#222811),(#222812,#222813),
(#222814,#222815),(#222816,#222817),(#222818,#222819),(#222820,#222821),
(#222822,#222823),(#222824,#222825),(#222826,#222827),(#222828,#222829),
(#222830,#222831),(#222832,#222833),(#222834,#222835),(#222836,#222837),
(#222838,#222839),(#222840,#222841),(#222842,#222843),(#222844,#222845),
(#222846,#222847),(#222848,#222849),(#222850,#222851),(#222852,#222853),
(#222854,#222855),(#222856,#222857),(#222858,#222859),(#222860,#222861),
(#222862,#222863),(#222864,#222865),(#222866,#222867),(#222868,#222869),
(#222870,#222871),(#222872,#222873),(#222874,#222875),(#222876,#222877),
(#222878,#222879),(#222880,#222881),(#222882,#222883),(#222884,#222885),
(#222886,#222887),(#222888,#222889),(#222890,#222891),(#222892,#222893),
(#222894,#222895),(#222896,#222897),(#222898,#222899),(#222900,#222901),
(#222902,#222903),(#222904,#222905),(#222906,#222907),(#222908,#222909),
(#222910,#222911),(#222912,#222913),(#222914,#222915),(#222916,#222917),
(#222918,#222919),(#222920,#222921),(#222922,#222923),(#222924,#222925),
(#222926,#222927),(#222928,#222929),(#222930,#222931),(#222932,#222933),
(#222934,#222935),(#222936,#222937),(#222938,#222939),(#222940,#222941),
(#222942,#222943),(#222944,#222945),(#222946,#222947),(#222948,#222949),
(#222950,#222951),(#222952,#222953),(#222954,#222955),(#222956,#222957),
(#222958,#222959),(#222960,#222961),(#222962,#222963),(#222964,#222965),
(#222966,#222967),(#222968,#222969),(#222970,#222971),(#222972,#222973),
(#222974,#222975),(#222976,#222977),(#222978,#222979),(#222980,#222981),
(#222982,#222983),(#222984,#222985),(#222986,#222987),(#222988,#222989),
(#222990,#222991),(#222992,#222993),(#222994,#222995),(#222996,#222997),
(#222998,#222999),(#223000,#223001),(#223002,#223003),(#223004,#223005),
(#223006,#223007),(#223008,#223009),(#223010,#223011),(#223012,#223013),
(#223014,#223015),(#223016,#223017),(#223018,#223019),(#223020,#223021),
(#223022,#223023),(#223024,#223025)),.UNSPECIFIED.,.F.,.F.,.F.)
B_SPLINE_SURFACE_WITH_KNOTS((6,1,1,1,1,1,1,1,1,1,1,1,1,1,1,1,1,1,1,1,1,
1,1,1,1,1,1,1,1,1,1,1,1,1,1,1,1,1,1,1,1,1,1,1,1,1,1,1,1,1,1,1,1,1,1,1,1,
1,1,1,1,1,1,1,1,1,1,1,1,1,1,1,1,1,1,1,1,1,1,1,1,1,1,1,1,1,1,1,1,1,1,1,1,
1,1,1,1,1,1,1,1,1,1,1,1,1,1,1,1,1,1,1,1,1,1,1,1,1,1,1,1,1,1,1,1,1,1,1,1,
1,1,1,1,1,1,1,1,1,1,1,1,1,1,1,1,1,1,1,1,1,1,1,1,1,1,1,1,1,1,1,1,1,1,1,1,
1,1,1,1,1,1,1,1,1,1,1,1,1,1,1,1,1,1,1,1,1,1,1,1,1,1,1,1,1,1,1,1,1,1,1,6),
(2,2),(-1.,-0.995000000000001,-0.990000000000001,-0.985000000000001,-0.980000000000001,
-0.975000000000001,-0.970000000000001,-0.965000000000001,-0.960000000000001,
-0.955000000000001,-0.950000000000001,-0.945000000000001,-0.940000000000001,
-0.935000000000001,-0.930000000000001,-0.925000000000001,-0.920000000000001,
-0.915000000000001,-0.910000000000001,-0.905000000000001,-0.900000000000001,
-0.895000000000001,-0.890000000000001,-0.885000000000001,-0.880000000000001,
-0.875000000000001,-0.870000000000001,-0.865000000000001,-0.860000000000001,
-0.855000000000001,-0.850000000000001,-0.845000000000001,-0.840000000000001,
-0.835000000000001,-0.830000000000001,-0.825000000000001,-0.820000000000001,
-0.815000000000001,-0.810000000000001,-0.805000000000001,-0.800000000000001,
-0.795000000000001,-0.790000000000001,-0.785000000000001,-0.780000000000001,
-0.775000000000001,-0.770000000000001,-0.765000000000001,-0.760000000000001,
-0.755000000000001,-0.750000000000001,-0.745000000000001,-0.740000000000001,
-0.735000000000001,-0.730000000000001,-0.725000000000001,-0.720000000000001,
-0.715000000000001,-0.710000000000001,-0.705000000000001,-0.700000000000001,
-0.695000000000001,-0.690000000000001,-0.685,-0.68,-0.675,-0.67,-0.665,
-0.66,-0.655,-0.65,-0.645,-0.64,-0.635,-0.63,-0.625,-0.62,-0.615,-0.61,
-0.605,-0.6,-0.595,-0.59,-0.585,-0.58,-0.575,-0.57,-0.565,-0.56,-0.555,
-0.55,-0.545,-0.54,-0.535,-0.53,-0.525,-0.52,-0.515,-0.51,-0.505,-0.5,-0.495,
-0.49,-0.485,-0.48,-0.475,-0.47,-0.465,-0.46,-0.455,-0.45,-0.445,-0.44,
-0.435,-0.43,-0.425,-0.42,-0.415,-0.41,-0.405,-0.4,-0.395,-0.39,-0.385,
-0.38,-0.375,-0.37,-0.365,-0.36,-0.355,-0.35,-0.345,-0.34,-0.335,-0.33,
-0.325,-0.32,-0.315,-0.31,-0.305,-0.3,-0.295,-0.29,-0.285,-0.28,-0.275,
-0.27,-0.265,-0.26,-0.255,-0.25,-0.245,-0.24,-0.235,-0.23,-0.225,-0.22,
-0.215,-0.21,-0.205,-0.2,-0.195,-0.19,-0.185,-0.18,-0.175,-0.17,-0.165,
-0.16,-0.155,-0.15,-0.145,-0.14,-0.135,-0.13,-0.125,-0.12,-0.115,-0.11,
-0.105,-0.1,-0.095,-0.09,-0.085,-0.08,-0.075,-0.07,-0.065,-0.06,-0.055,
-0.05,-0.045,-0.04,-0.035,-0.03,-0.025,-0.02,-0.015,-0.01,-0.005,0.),(0.,
1.2),.UNSPECIFIED.)
GEOMETRIC_REPRESENTATION_ITEM()
RATIONAL_B_SPLINE_SURFACE(((1.,1.),(1.,1.),(1.,1.),(1.,1.),(1.,1.),(1.,
1.),(1.,1.),(1.,1.),(1.,1.),(1.,1.),(1.,1.),(1.,1.),(1.,1.),(1.,1.),(1.,
1.),(1.,1.),(1.,1.),(1.,1.),(1.,1.),(1.,1.),(1.,1.),(1.,1.),(1.,1.),(1.,
1.),(1.,1.),(1.,1.),(1.,1.),(1.,1.),(1.,1.),(1.,1.),(1.,1.),(1.,1.),(1.,
1.),(1.,1.),(1.,1.),(1.,1.),(1.,1.),(1.,1.),(1.,1.),(1.,1.),(1.,1.),(1.,
1.),(1.,1.),(1.,1.),(1.,1.),(1.,1.),(1.,1.),(1.,1.),(1.,1.),(1.,1.),(1.,
1.),(1.,1.),(1.,1.),(1.,1.),(1.,1.),(1.,1.),(1.,1.),(1.,1.),(1.,1.),(1.,
1.),(1.,1.),(1.,1.),(1.,1.),(1.,1.),(1.,1.),(1.,1.),(1.,1.),(1.,1.),(1.,
1.),(1.,1.),(1.,1.),(1.,1.),(1.,1.),(1.,1.),(1.,1.),(1.,1.),(1.,1.),(1.,
1.),(1.,1.),(1.,1.),(1.,1.),(1.,1.),(1.,1.),(1.,1.),(1.,1.),(1.,1.),(1.,
1.),(1.,1.),(1.,1.),(1.,1.),(1.,1.),(1.,1.),(1.,1.),(1.,1.),(1.,1.),(1.,
1.),(1.,1.),(1.,1.),(1.,1.),(1.,1.),(1.,1.),(1.,1.),(1.,1.),(1.,1.),(1.,
1.),(1.,1.),(1.,1.),(1.,1.),(1.,1.),(1.,1.),(1.,1.),(1.,1.),(1.,1.),(1.,
1.),(1.,1.),(1.,1.),(1.,1.),(1.,1.),(1.,1.),(1.,1.),(1.,1.),(1.,1.),(1.,
1.),(1.,1.),(1.,1.),(1.,1.),(1.,1.),(1.,1.),(1.,1.),(1.,1.),(1.,1.),(1.,
1.),(1.,1.),(1.,1.),(1.,1.),(1.,1.),(1.,1.),(1.,1.),(1.,1.),(1.,1.),(1.,
1.),(1.,1.),(1.,1.),(1.,1.),(1.,1.),(1.,1.),(1.,1.),(1.,1.),(1.,1.),(1.,
1.),(1.,1.),(1.,1.),(1.,1.),(1.,1.),(1.,1.),(1.,1.),(1.,1.),(1.,1.),(1.,
1.),(1.,1.),(1.,1.),(1.,1.),(1.,1.),(1.,1.),(1.,1.),(1.,1.),(1.,1.),(1.,
1.),(1.,1.),(1.,1.),(1.,1.),(1.,1.),(1.,1.),(1.,1.),(1.,1.),(1.,1.),(1.,
1.),(1.,1.),(1.,1.),(1.,1.),(1.,1.),(1.,1.),(1.,1.),(1.,1.),(1.,1.),(1.,
1.),(1.,1.),(1.,1.),(1.,1.),(1.,1.),(1.,1.),(1.,1.),(1.,1.),(1.,1.),(1.,
1.),(1.,1.),(1.,1.),(1.,1.),(1.,1.),(1.,1.),(1.,1.),(1.,1.),(1.,1.),(1.,
1.),(1.,1.)))
REPRESENTATION_ITEM('')
SURFACE()
);
#1084=(
BOUNDED_SURFACE()
B_SPLINE_SURFACE(5,1,((#223439,#223440),(#223441,#223442),(#223443,#223444),
(#223445,#223446),(#223447,#223448),(#223449,#223450),(#223451,#223452),
(#223453,#223454),(#223455,#223456),(#223457,#223458),(#223459,#223460),
(#223461,#223462),(#223463,#223464),(#223465,#223466),(#223467,#223468),
(#223469,#223470),(#223471,#223472),(#223473,#223474),(#223475,#223476),
(#223477,#223478),(#223479,#223480),(#223481,#223482),(#223483,#223484),
(#223485,#223486),(#223487,#223488),(#223489,#223490),(#223491,#223492),
(#223493,#223494),(#223495,#223496),(#223497,#223498),(#223499,#223500),
(#223501,#223502),(#223503,#223504),(#223505,#223506),(#223507,#223508),
(#223509,#223510),(#223511,#223512),(#223513,#223514),(#223515,#223516),
(#223517,#223518),(#223519,#223520),(#223521,#223522),(#223523,#223524),
(#223525,#223526),(#223527,#223528),(#223529,#223530),(#223531,#223532),
(#223533,#223534),(#223535,#223536),(#223537,#223538),(#223539,#223540),
(#223541,#223542),(#223543,#223544),(#223545,#223546),(#223547,#223548),
(#223549,#223550),(#223551,#223552),(#223553,#223554),(#223555,#223556),
(#223557,#223558),(#223559,#223560),(#223561,#223562),(#223563,#223564),
(#223565,#223566),(#223567,#223568),(#223569,#223570),(#223571,#223572),
(#223573,#223574),(#223575,#223576),(#223577,#223578),(#223579,#223580),
(#223581,#223582),(#223583,#223584),(#223585,#223586),(#223587,#223588),
(#223589,#223590),(#223591,#223592),(#223593,#223594),(#223595,#223596),
(#223597,#223598),(#223599,#223600),(#223601,#223602),(#223603,#223604),
(#223605,#223606),(#223607,#223608),(#223609,#223610),(#223611,#223612),
(#223613,#223614),(#223615,#223616),(#223617,#223618),(#223619,#223620),
(#223621,#223622),(#223623,#223624),(#223625,#223626),(#223627,#223628),
(#223629,#223630),(#223631,#223632),(#223633,#223634),(#223635,#223636),
(#223637,#223638),(#223639,#223640),(#223641,#223642),(#223643,#223644),
(#223645,#223646),(#223647,#223648),(#223649,#223650),(#223651,#223652),
(#223653,#223654),(#223655,#223656),(#223657,#223658),(#223659,#223660),
(#223661,#223662),(#223663,#223664),(#223665,#223666),(#223667,#223668),
(#223669,#223670),(#223671,#223672),(#223673,#223674),(#223675,#223676),
(#223677,#223678),(#223679,#223680),(#223681,#223682),(#223683,#223684),
(#223685,#223686),(#223687,#223688),(#223689,#223690),(#223691,#223692),
(#223693,#223694),(#223695,#223696),(#223697,#223698),(#223699,#223700),
(#223701,#223702),(#223703,#223704),(#223705,#223706),(#223707,#223708),
(#223709,#223710),(#223711,#223712),(#223713,#223714),(#223715,#223716),
(#223717,#223718),(#223719,#223720),(#223721,#223722),(#223723,#223724),
(#223725,#223726),(#223727,#223728),(#223729,#223730),(#223731,#223732),
(#223733,#223734),(#223735,#223736),(#223737,#223738),(#223739,#223740),
(#223741,#223742),(#223743,#223744),(#223745,#223746),(#223747,#223748),
(#223749,#223750),(#223751,#223752),(#223753,#223754),(#223755,#223756),
(#223757,#223758),(#223759,#223760),(#223761,#223762),(#223763,#223764),
(#223765,#223766),(#223767,#223768),(#223769,#223770),(#223771,#223772),
(#223773,#223774),(#223775,#223776),(#223777,#223778),(#223779,#223780),
(#223781,#223782),(#223783,#223784),(#223785,#223786),(#223787,#223788),
(#223789,#223790),(#223791,#223792),(#223793,#223794),(#223795,#223796),
(#223797,#223798),(#223799,#223800),(#223801,#223802),(#223803,#223804),
(#223805,#223806),(#223807,#223808),(#223809,#223810),(#223811,#223812),
(#223813,#223814),(#223815,#223816),(#223817,#223818),(#223819,#223820),
(#223821,#223822),(#223823,#223824),(#223825,#223826),(#223827,#223828),
(#223829,#223830),(#223831,#223832),(#223833,#223834),(#223835,#223836),
(#223837,#223838),(#223839,#223840),(#223841,#223842),(#223843,#223844),
(#223845,#223846),(#223847,#223848)),.UNSPECIFIED.,.F.,.F.,.F.)
B_SPLINE_SURFACE_WITH_KNOTS((6,1,1,1,1,1,1,1,1,1,1,1,1,1,1,1,1,1,1,1,1,
1,1,1,1,1,1,1,1,1,1,1,1,1,1,1,1,1,1,1,1,1,1,1,1,1,1,1,1,1,1,1,1,1,1,1,1,
1,1,1,1,1,1,1,1,1,1,1,1,1,1,1,1,1,1,1,1,1,1,1,1,1,1,1,1,1,1,1,1,1,1,1,1,
1,1,1,1,1,1,1,1,1,1,1,1,1,1,1,1,1,1,1,1,1,1,1,1,1,1,1,1,1,1,1,1,1,1,1,1,
1,1,1,1,1,1,1,1,1,1,1,1,1,1,1,1,1,1,1,1,1,1,1,1,1,1,1,1,1,1,1,1,1,1,1,1,
1,1,1,1,1,1,1,1,1,1,1,1,1,1,1,1,1,1,1,1,1,1,1,1,1,1,1,1,1,1,1,1,1,1,1,6),
(2,2),(0.,0.005,0.01,0.015,0.02,0.025,0.03,0.035,0.04,0.045,0.05,0.055,
0.06,0.065,0.07,0.075,0.08,0.085,0.09,0.095,0.1,0.105,0.11,0.115,0.12,0.125,
0.13,0.135,0.14,0.145,0.15,0.155,0.16,0.165,0.17,0.175,0.18,0.185,0.19,
0.195,0.2,0.205,0.21,0.215,0.22,0.225,0.23,0.235,0.24,0.245,0.25,0.255,
0.26,0.265,0.27,0.275,0.28,0.285,0.29,0.295,0.3,0.305,0.31,0.315,0.32,0.325,
0.33,0.335,0.34,0.345,0.35,0.355,0.36,0.365,0.37,0.375,0.38,0.385,0.39,
0.395,0.4,0.405,0.41,0.415,0.42,0.425,0.43,0.435,0.44,0.445,0.45,0.455,
0.46,0.465,0.47,0.475,0.48,0.485,0.49,0.495,0.5,0.505,0.51,0.515,0.52,0.525,
0.53,0.535,0.54,0.545,0.55,0.555,0.56,0.565,0.57,0.575,0.58,0.585,0.59,
0.595,0.6,0.605,0.61,0.615,0.62,0.625,0.63,0.635,0.64,0.645,0.65,0.655,
0.66,0.665,0.67,0.675,0.68,0.685,0.690000000000001,0.695000000000001,0.700000000000001,
0.705000000000001,0.710000000000001,0.715000000000001,0.720000000000001,
0.725000000000001,0.730000000000001,0.735000000000001,0.740000000000001,
0.745000000000001,0.750000000000001,0.755000000000001,0.760000000000001,
0.765000000000001,0.770000000000001,0.775000000000001,0.780000000000001,
0.785000000000001,0.790000000000001,0.795000000000001,0.800000000000001,
0.805000000000001,0.810000000000001,0.815000000000001,0.820000000000001,
0.825000000000001,0.830000000000001,0.835000000000001,0.840000000000001,
0.845000000000001,0.850000000000001,0.855000000000001,0.860000000000001,
0.865000000000001,0.870000000000001,0.875000000000001,0.880000000000001,
0.885000000000001,0.890000000000001,0.895000000000001,0.900000000000001,
0.905000000000001,0.910000000000001,0.915000000000001,0.920000000000001,
0.925000000000001,0.930000000000001,0.935000000000001,0.940000000000001,
0.945000000000001,0.950000000000001,0.955000000000001,0.960000000000001,
0.965000000000001,0.970000000000001,0.975000000000001,0.980000000000001,
0.985000000000001,0.990000000000001,0.995000000000001,1.),(0.,1.2),
 .UNSPECIFIED.)
GEOMETRIC_REPRESENTATION_ITEM()
RATIONAL_B_SPLINE_SURFACE(((1.,1.),(1.,1.),(1.,1.),(1.,1.),(1.,1.),(1.,
1.),(1.,1.),(1.,1.),(1.,1.),(1.,1.),(1.,1.),(1.,1.),(1.,1.),(1.,1.),(1.,
1.),(1.,1.),(1.,1.),(1.,1.),(1.,1.),(1.,1.),(1.,1.),(1.,1.),(1.,1.),(1.,
1.),(1.,1.),(1.,1.),(1.,1.),(1.,1.),(1.,1.),(1.,1.),(1.,1.),(1.,1.),(1.,
1.),(1.,1.),(1.,1.),(1.,1.),(1.,1.),(1.,1.),(1.,1.),(1.,1.),(1.,1.),(1.,
1.),(1.,1.),(1.,1.),(1.,1.),(1.,1.),(1.,1.),(1.,1.),(1.,1.),(1.,1.),(1.,
1.),(1.,1.),(1.,1.),(1.,1.),(1.,1.),(1.,1.),(1.,1.),(1.,1.),(1.,1.),(1.,
1.),(1.,1.),(1.,1.),(1.,1.),(1.,1.),(1.,1.),(1.,1.),(1.,1.),(1.,1.),(1.,
1.),(1.,1.),(1.,1.),(1.,1.),(1.,1.),(1.,1.),(1.,1.),(1.,1.),(1.,1.),(1.,
1.),(1.,1.),(1.,1.),(1.,1.),(1.,1.),(1.,1.),(1.,1.),(1.,1.),(1.,1.),(1.,
1.),(1.,1.),(1.,1.),(1.,1.),(1.,1.),(1.,1.),(1.,1.),(1.,1.),(1.,1.),(1.,
1.),(1.,1.),(1.,1.),(1.,1.),(1.,1.),(1.,1.),(1.,1.),(1.,1.),(1.,1.),(1.,
1.),(1.,1.),(1.,1.),(1.,1.),(1.,1.),(1.,1.),(1.,1.),(1.,1.),(1.,1.),(1.,
1.),(1.,1.),(1.,1.),(1.,1.),(1.,1.),(1.,1.),(1.,1.),(1.,1.),(1.,1.),(1.,
1.),(1.,1.),(1.,1.),(1.,1.),(1.,1.),(1.,1.),(1.,1.),(1.,1.),(1.,1.),(1.,
1.),(1.,1.),(1.,1.),(1.,1.),(1.,1.),(1.,1.),(1.,1.),(1.,1.),(1.,1.),(1.,
1.),(1.,1.),(1.,1.),(1.,1.),(1.,1.),(1.,1.),(1.,1.),(1.,1.),(1.,1.),(1.,
1.),(1.,1.),(1.,1.),(1.,1.),(1.,1.),(1.,1.),(1.,1.),(1.,1.),(1.,1.),(1.,
1.),(1.,1.),(1.,1.),(1.,1.),(1.,1.),(1.,1.),(1.,1.),(1.,1.),(1.,1.),(1.,
1.),(1.,1.),(1.,1.),(1.,1.),(1.,1.),(1.,1.),(1.,1.),(1.,1.),(1.,1.),(1.,
1.),(1.,1.),(1.,1.),(1.,1.),(1.,1.),(1.,1.),(1.,1.),(1.,1.),(1.,1.),(1.,
1.),(1.,1.),(1.,1.),(1.,1.),(1.,1.),(1.,1.),(1.,1.),(1.,1.),(1.,1.),(1.,
1.),(1.,1.),(1.,1.),(1.,1.),(1.,1.),(1.,1.),(1.,1.),(1.,1.),(1.,1.),(1.,
1.),(1.,1.)))
REPRESENTATION_ITEM('')
SURFACE()
);
#1085=(
BOUNDED_SURFACE()
B_SPLINE_SURFACE(5,1,((#224268,#224269),(#224270,#224271),(#224272,#224273),
(#224274,#224275),(#224276,#224277),(#224278,#224279),(#224280,#224281),
(#224282,#224283),(#224284,#224285),(#224286,#224287),(#224288,#224289),
(#224290,#224291),(#224292,#224293),(#224294,#224295),(#224296,#224297),
(#224298,#224299),(#224300,#224301),(#224302,#224303),(#224304,#224305),
(#224306,#224307),(#224308,#224309),(#224310,#224311),(#224312,#224313),
(#224314,#224315),(#224316,#224317),(#224318,#224319),(#224320,#224321),
(#224322,#224323),(#224324,#224325),(#224326,#224327),(#224328,#224329),
(#224330,#224331),(#224332,#224333),(#224334,#224335),(#224336,#224337),
(#224338,#224339),(#224340,#224341),(#224342,#224343),(#224344,#224345),
(#224346,#224347),(#224348,#224349),(#224350,#224351),(#224352,#224353),
(#224354,#224355),(#224356,#224357),(#224358,#224359),(#224360,#224361),
(#224362,#224363),(#224364,#224365),(#224366,#224367),(#224368,#224369),
(#224370,#224371),(#224372,#224373),(#224374,#224375),(#224376,#224377),
(#224378,#224379),(#224380,#224381),(#224382,#224383),(#224384,#224385),
(#224386,#224387),(#224388,#224389),(#224390,#224391),(#224392,#224393),
(#224394,#224395),(#224396,#224397),(#224398,#224399),(#224400,#224401),
(#224402,#224403),(#224404,#224405),(#224406,#224407),(#224408,#224409),
(#224410,#224411),(#224412,#224413),(#224414,#224415),(#224416,#224417),
(#224418,#224419),(#224420,#224421),(#224422,#224423),(#224424,#224425),
(#224426,#224427),(#224428,#224429),(#224430,#224431),(#224432,#224433),
(#224434,#224435),(#224436,#224437),(#224438,#224439),(#224440,#224441),
(#224442,#224443),(#224444,#224445),(#224446,#224447),(#224448,#224449),
(#224450,#224451),(#224452,#224453),(#224454,#224455),(#224456,#224457),
(#224458,#224459),(#224460,#224461),(#224462,#224463),(#224464,#224465),
(#224466,#224467),(#224468,#224469),(#224470,#224471),(#224472,#224473),
(#224474,#224475),(#224476,#224477),(#224478,#224479),(#224480,#224481),
(#224482,#224483),(#224484,#224485),(#224486,#224487),(#224488,#224489),
(#224490,#224491),(#224492,#224493),(#224494,#224495),(#224496,#224497),
(#224498,#224499),(#224500,#224501),(#224502,#224503),(#224504,#224505),
(#224506,#224507),(#224508,#224509),(#224510,#224511),(#224512,#224513),
(#224514,#224515),(#224516,#224517),(#224518,#224519),(#224520,#224521),
(#224522,#224523),(#224524,#224525),(#224526,#224527),(#224528,#224529),
(#224530,#224531),(#224532,#224533),(#224534,#224535),(#224536,#224537),
(#224538,#224539),(#224540,#224541),(#224542,#224543),(#224544,#224545),
(#224546,#224547),(#224548,#224549),(#224550,#224551),(#224552,#224553),
(#224554,#224555),(#224556,#224557),(#224558,#224559),(#224560,#224561),
(#224562,#224563),(#224564,#224565),(#224566,#224567),(#224568,#224569),
(#224570,#224571),(#224572,#224573),(#224574,#224575),(#224576,#224577),
(#224578,#224579),(#224580,#224581),(#224582,#224583),(#224584,#224585),
(#224586,#224587),(#224588,#224589),(#224590,#224591),(#224592,#224593),
(#224594,#224595),(#224596,#224597),(#224598,#224599),(#224600,#224601),
(#224602,#224603),(#224604,#224605),(#224606,#224607),(#224608,#224609),
(#224610,#224611),(#224612,#224613),(#224614,#224615),(#224616,#224617),
(#224618,#224619),(#224620,#224621),(#224622,#224623),(#224624,#224625),
(#224626,#224627),(#224628,#224629),(#224630,#224631),(#224632,#224633),
(#224634,#224635),(#224636,#224637),(#224638,#224639),(#224640,#224641),
(#224642,#224643),(#224644,#224645),(#224646,#224647),(#224648,#224649),
(#224650,#224651),(#224652,#224653),(#224654,#224655),(#224656,#224657),
(#224658,#224659),(#224660,#224661),(#224662,#224663),(#224664,#224665),
(#224666,#224667),(#224668,#224669),(#224670,#224671),(#224672,#224673),
(#224674,#224675),(#224676,#224677)),.UNSPECIFIED.,.F.,.F.,.F.)
B_SPLINE_SURFACE_WITH_KNOTS((6,1,1,1,1,1,1,1,1,1,1,1,1,1,1,1,1,1,1,1,1,
1,1,1,1,1,1,1,1,1,1,1,1,1,1,1,1,1,1,1,1,1,1,1,1,1,1,1,1,1,1,1,1,1,1,1,1,
1,1,1,1,1,1,1,1,1,1,1,1,1,1,1,1,1,1,1,1,1,1,1,1,1,1,1,1,1,1,1,1,1,1,1,1,
1,1,1,1,1,1,1,1,1,1,1,1,1,1,1,1,1,1,1,1,1,1,1,1,1,1,1,1,1,1,1,1,1,1,1,1,
1,1,1,1,1,1,1,1,1,1,1,1,1,1,1,1,1,1,1,1,1,1,1,1,1,1,1,1,1,1,1,1,1,1,1,1,
1,1,1,1,1,1,1,1,1,1,1,1,1,1,1,1,1,1,1,1,1,1,1,1,1,1,1,1,1,1,1,1,1,1,1,6),
(2,2),(-1.,-0.995000000000001,-0.990000000000001,-0.985000000000001,-0.980000000000001,
-0.975000000000001,-0.970000000000001,-0.965000000000001,-0.960000000000001,
-0.955000000000001,-0.950000000000001,-0.945000000000001,-0.940000000000001,
-0.935000000000001,-0.930000000000001,-0.925000000000001,-0.920000000000001,
-0.915000000000001,-0.910000000000001,-0.905000000000001,-0.900000000000001,
-0.895000000000001,-0.890000000000001,-0.885000000000001,-0.880000000000001,
-0.875000000000001,-0.870000000000001,-0.865000000000001,-0.860000000000001,
-0.855000000000001,-0.850000000000001,-0.845000000000001,-0.840000000000001,
-0.835000000000001,-0.830000000000001,-0.825000000000001,-0.820000000000001,
-0.815000000000001,-0.810000000000001,-0.805000000000001,-0.800000000000001,
-0.795000000000001,-0.790000000000001,-0.785000000000001,-0.780000000000001,
-0.775000000000001,-0.770000000000001,-0.765000000000001,-0.760000000000001,
-0.755000000000001,-0.750000000000001,-0.745000000000001,-0.740000000000001,
-0.735000000000001,-0.730000000000001,-0.725000000000001,-0.720000000000001,
-0.715000000000001,-0.710000000000001,-0.705000000000001,-0.700000000000001,
-0.695000000000001,-0.690000000000001,-0.685,-0.68,-0.675,-0.67,-0.665,
-0.66,-0.655,-0.65,-0.645,-0.64,-0.635,-0.63,-0.625,-0.62,-0.615,-0.61,
-0.605,-0.6,-0.595,-0.59,-0.585,-0.58,-0.575,-0.57,-0.565,-0.56,-0.555,
-0.55,-0.545,-0.54,-0.535,-0.53,-0.525,-0.52,-0.515,-0.51,-0.505,-0.5,-0.495,
-0.49,-0.485,-0.48,-0.475,-0.47,-0.465,-0.46,-0.455,-0.45,-0.445,-0.44,
-0.435,-0.43,-0.425,-0.42,-0.415,-0.41,-0.405,-0.4,-0.395,-0.39,-0.385,
-0.38,-0.375,-0.37,-0.365,-0.36,-0.355,-0.35,-0.345,-0.34,-0.335,-0.33,
-0.325,-0.32,-0.315,-0.31,-0.305,-0.3,-0.295,-0.29,-0.285,-0.28,-0.275,
-0.27,-0.265,-0.26,-0.255,-0.25,-0.245,-0.24,-0.235,-0.23,-0.225,-0.22,
-0.215,-0.21,-0.205,-0.2,-0.195,-0.19,-0.185,-0.18,-0.175,-0.17,-0.165,
-0.16,-0.155,-0.15,-0.145,-0.14,-0.135,-0.13,-0.125,-0.12,-0.115,-0.11,
-0.105,-0.1,-0.095,-0.09,-0.085,-0.08,-0.075,-0.07,-0.065,-0.06,-0.055,
-0.05,-0.045,-0.04,-0.035,-0.03,-0.025,-0.02,-0.015,-0.01,-0.005,0.),(0.,
1.2),.UNSPECIFIED.)
GEOMETRIC_REPRESENTATION_ITEM()
RATIONAL_B_SPLINE_SURFACE(((1.,1.),(1.,1.),(1.,1.),(1.,1.),(1.,1.),(1.,
1.),(1.,1.),(1.,1.),(1.,1.),(1.,1.),(1.,1.),(1.,1.),(1.,1.),(1.,1.),(1.,
1.),(1.,1.),(1.,1.),(1.,1.),(1.,1.),(1.,1.),(1.,1.),(1.,1.),(1.,1.),(1.,
1.),(1.,1.),(1.,1.),(1.,1.),(1.,1.),(1.,1.),(1.,1.),(1.,1.),(1.,1.),(1.,
1.),(1.,1.),(1.,1.),(1.,1.),(1.,1.),(1.,1.),(1.,1.),(1.,1.),(1.,1.),(1.,
1.),(1.,1.),(1.,1.),(1.,1.),(1.,1.),(1.,1.),(1.,1.),(1.,1.),(1.,1.),(1.,
1.),(1.,1.),(1.,1.),(1.,1.),(1.,1.),(1.,1.),(1.,1.),(1.,1.),(1.,1.),(1.,
1.),(1.,1.),(1.,1.),(1.,1.),(1.,1.),(1.,1.),(1.,1.),(1.,1.),(1.,1.),(1.,
1.),(1.,1.),(1.,1.),(1.,1.),(1.,1.),(1.,1.),(1.,1.),(1.,1.),(1.,1.),(1.,
1.),(1.,1.),(1.,1.),(1.,1.),(1.,1.),(1.,1.),(1.,1.),(1.,1.),(1.,1.),(1.,
1.),(1.,1.),(1.,1.),(1.,1.),(1.,1.),(1.,1.),(1.,1.),(1.,1.),(1.,1.),(1.,
1.),(1.,1.),(1.,1.),(1.,1.),(1.,1.),(1.,1.),(1.,1.),(1.,1.),(1.,1.),(1.,
1.),(1.,1.),(1.,1.),(1.,1.),(1.,1.),(1.,1.),(1.,1.),(1.,1.),(1.,1.),(1.,
1.),(1.,1.),(1.,1.),(1.,1.),(1.,1.),(1.,1.),(1.,1.),(1.,1.),(1.,1.),(1.,
1.),(1.,1.),(1.,1.),(1.,1.),(1.,1.),(1.,1.),(1.,1.),(1.,1.),(1.,1.),(1.,
1.),(1.,1.),(1.,1.),(1.,1.),(1.,1.),(1.,1.),(1.,1.),(1.,1.),(1.,1.),(1.,
1.),(1.,1.),(1.,1.),(1.,1.),(1.,1.),(1.,1.),(1.,1.),(1.,1.),(1.,1.),(1.,
1.),(1.,1.),(1.,1.),(1.,1.),(1.,1.),(1.,1.),(1.,1.),(1.,1.),(1.,1.),(1.,
1.),(1.,1.),(1.,1.),(1.,1.),(1.,1.),(1.,1.),(1.,1.),(1.,1.),(1.,1.),(1.,
1.),(1.,1.),(1.,1.),(1.,1.),(1.,1.),(1.,1.),(1.,1.),(1.,1.),(1.,1.),(1.,
1.),(1.,1.),(1.,1.),(1.,1.),(1.,1.),(1.,1.),(1.,1.),(1.,1.),(1.,1.),(1.,
1.),(1.,1.),(1.,1.),(1.,1.),(1.,1.),(1.,1.),(1.,1.),(1.,1.),(1.,1.),(1.,
1.),(1.,1.),(1.,1.),(1.,1.),(1.,1.),(1.,1.),(1.,1.),(1.,1.),(1.,1.),(1.,
1.),(1.,1.)))
REPRESENTATION_ITEM('')
SURFACE()
);
#1086=(
BOUNDED_SURFACE()
B_SPLINE_SURFACE(5,1,((#225091,#225092),(#225093,#225094),(#225095,#225096),
(#225097,#225098),(#225099,#225100),(#225101,#225102),(#225103,#225104),
(#225105,#225106),(#225107,#225108),(#225109,#225110),(#225111,#225112),
(#225113,#225114),(#225115,#225116),(#225117,#225118),(#225119,#225120),
(#225121,#225122),(#225123,#225124),(#225125,#225126),(#225127,#225128),
(#225129,#225130),(#225131,#225132),(#225133,#225134),(#225135,#225136),
(#225137,#225138),(#225139,#225140),(#225141,#225142),(#225143,#225144),
(#225145,#225146),(#225147,#225148),(#225149,#225150),(#225151,#225152),
(#225153,#225154),(#225155,#225156),(#225157,#225158),(#225159,#225160),
(#225161,#225162),(#225163,#225164),(#225165,#225166),(#225167,#225168),
(#225169,#225170),(#225171,#225172),(#225173,#225174),(#225175,#225176),
(#225177,#225178),(#225179,#225180),(#225181,#225182),(#225183,#225184),
(#225185,#225186),(#225187,#225188),(#225189,#225190),(#225191,#225192),
(#225193,#225194),(#225195,#225196),(#225197,#225198),(#225199,#225200),
(#225201,#225202),(#225203,#225204),(#225205,#225206),(#225207,#225208),
(#225209,#225210),(#225211,#225212),(#225213,#225214),(#225215,#225216),
(#225217,#225218),(#225219,#225220),(#225221,#225222),(#225223,#225224),
(#225225,#225226),(#225227,#225228),(#225229,#225230),(#225231,#225232),
(#225233,#225234),(#225235,#225236),(#225237,#225238),(#225239,#225240),
(#225241,#225242),(#225243,#225244),(#225245,#225246),(#225247,#225248),
(#225249,#225250),(#225251,#225252),(#225253,#225254),(#225255,#225256),
(#225257,#225258),(#225259,#225260),(#225261,#225262),(#225263,#225264),
(#225265,#225266),(#225267,#225268),(#225269,#225270),(#225271,#225272),
(#225273,#225274),(#225275,#225276),(#225277,#225278),(#225279,#225280),
(#225281,#225282),(#225283,#225284),(#225285,#225286),(#225287,#225288),
(#225289,#225290),(#225291,#225292),(#225293,#225294),(#225295,#225296),
(#225297,#225298),(#225299,#225300),(#225301,#225302),(#225303,#225304),
(#225305,#225306),(#225307,#225308),(#225309,#225310),(#225311,#225312),
(#225313,#225314),(#225315,#225316),(#225317,#225318),(#225319,#225320),
(#225321,#225322),(#225323,#225324),(#225325,#225326),(#225327,#225328),
(#225329,#225330),(#225331,#225332),(#225333,#225334),(#225335,#225336),
(#225337,#225338),(#225339,#225340),(#225341,#225342),(#225343,#225344),
(#225345,#225346),(#225347,#225348),(#225349,#225350),(#225351,#225352),
(#225353,#225354),(#225355,#225356),(#225357,#225358),(#225359,#225360),
(#225361,#225362),(#225363,#225364),(#225365,#225366),(#225367,#225368),
(#225369,#225370),(#225371,#225372),(#225373,#225374),(#225375,#225376),
(#225377,#225378),(#225379,#225380),(#225381,#225382),(#225383,#225384),
(#225385,#225386),(#225387,#225388),(#225389,#225390),(#225391,#225392),
(#225393,#225394),(#225395,#225396),(#225397,#225398),(#225399,#225400),
(#225401,#225402),(#225403,#225404),(#225405,#225406),(#225407,#225408),
(#225409,#225410),(#225411,#225412),(#225413,#225414),(#225415,#225416),
(#225417,#225418),(#225419,#225420),(#225421,#225422),(#225423,#225424),
(#225425,#225426),(#225427,#225428),(#225429,#225430),(#225431,#225432),
(#225433,#225434),(#225435,#225436),(#225437,#225438),(#225439,#225440),
(#225441,#225442),(#225443,#225444),(#225445,#225446),(#225447,#225448),
(#225449,#225450),(#225451,#225452),(#225453,#225454),(#225455,#225456),
(#225457,#225458),(#225459,#225460),(#225461,#225462),(#225463,#225464),
(#225465,#225466),(#225467,#225468),(#225469,#225470),(#225471,#225472),
(#225473,#225474),(#225475,#225476),(#225477,#225478),(#225479,#225480),
(#225481,#225482),(#225483,#225484),(#225485,#225486),(#225487,#225488),
(#225489,#225490),(#225491,#225492),(#225493,#225494),(#225495,#225496),
(#225497,#225498),(#225499,#225500)),.UNSPECIFIED.,.F.,.F.,.F.)
B_SPLINE_SURFACE_WITH_KNOTS((6,1,1,1,1,1,1,1,1,1,1,1,1,1,1,1,1,1,1,1,1,
1,1,1,1,1,1,1,1,1,1,1,1,1,1,1,1,1,1,1,1,1,1,1,1,1,1,1,1,1,1,1,1,1,1,1,1,
1,1,1,1,1,1,1,1,1,1,1,1,1,1,1,1,1,1,1,1,1,1,1,1,1,1,1,1,1,1,1,1,1,1,1,1,
1,1,1,1,1,1,1,1,1,1,1,1,1,1,1,1,1,1,1,1,1,1,1,1,1,1,1,1,1,1,1,1,1,1,1,1,
1,1,1,1,1,1,1,1,1,1,1,1,1,1,1,1,1,1,1,1,1,1,1,1,1,1,1,1,1,1,1,1,1,1,1,1,
1,1,1,1,1,1,1,1,1,1,1,1,1,1,1,1,1,1,1,1,1,1,1,1,1,1,1,1,1,1,1,1,1,1,1,6),
(2,2),(0.,0.005,0.01,0.015,0.02,0.025,0.03,0.035,0.04,0.045,0.05,0.055,
0.06,0.065,0.07,0.075,0.08,0.085,0.09,0.095,0.1,0.105,0.11,0.115,0.12,0.125,
0.13,0.135,0.14,0.145,0.15,0.155,0.16,0.165,0.17,0.175,0.18,0.185,0.19,
0.195,0.2,0.205,0.21,0.215,0.22,0.225,0.23,0.235,0.24,0.245,0.25,0.255,
0.26,0.265,0.27,0.275,0.28,0.285,0.29,0.295,0.3,0.305,0.31,0.315,0.32,0.325,
0.33,0.335,0.34,0.345,0.35,0.355,0.36,0.365,0.37,0.375,0.38,0.385,0.39,
0.395,0.4,0.405,0.41,0.415,0.42,0.425,0.43,0.435,0.44,0.445,0.45,0.455,
0.46,0.465,0.47,0.475,0.48,0.485,0.49,0.495,0.5,0.505,0.51,0.515,0.52,0.525,
0.53,0.535,0.54,0.545,0.55,0.555,0.56,0.565,0.57,0.575,0.58,0.585,0.59,
0.595,0.6,0.605,0.61,0.615,0.62,0.625,0.63,0.635,0.64,0.645,0.65,0.655,
0.66,0.665,0.67,0.675,0.68,0.685,0.690000000000001,0.695000000000001,0.700000000000001,
0.705000000000001,0.710000000000001,0.715000000000001,0.720000000000001,
0.725000000000001,0.730000000000001,0.735000000000001,0.740000000000001,
0.745000000000001,0.750000000000001,0.755000000000001,0.760000000000001,
0.765000000000001,0.770000000000001,0.775000000000001,0.780000000000001,
0.785000000000001,0.790000000000001,0.795000000000001,0.800000000000001,
0.805000000000001,0.810000000000001,0.815000000000001,0.820000000000001,
0.825000000000001,0.830000000000001,0.835000000000001,0.840000000000001,
0.845000000000001,0.850000000000001,0.855000000000001,0.860000000000001,
0.865000000000001,0.870000000000001,0.875000000000001,0.880000000000001,
0.885000000000001,0.890000000000001,0.895000000000001,0.900000000000001,
0.905000000000001,0.910000000000001,0.915000000000001,0.920000000000001,
0.925000000000001,0.930000000000001,0.935000000000001,0.940000000000001,
0.945000000000001,0.950000000000001,0.955000000000001,0.960000000000001,
0.965000000000001,0.970000000000001,0.975000000000001,0.980000000000001,
0.985000000000001,0.990000000000001,0.995000000000001,1.),(0.,1.2),
 .UNSPECIFIED.)
GEOMETRIC_REPRESENTATION_ITEM()
RATIONAL_B_SPLINE_SURFACE(((1.,1.),(1.,1.),(1.,1.),(1.,1.),(1.,1.),(1.,
1.),(1.,1.),(1.,1.),(1.,1.),(1.,1.),(1.,1.),(1.,1.),(1.,1.),(1.,1.),(1.,
1.),(1.,1.),(1.,1.),(1.,1.),(1.,1.),(1.,1.),(1.,1.),(1.,1.),(1.,1.),(1.,
1.),(1.,1.),(1.,1.),(1.,1.),(1.,1.),(1.,1.),(1.,1.),(1.,1.),(1.,1.),(1.,
1.),(1.,1.),(1.,1.),(1.,1.),(1.,1.),(1.,1.),(1.,1.),(1.,1.),(1.,1.),(1.,
1.),(1.,1.),(1.,1.),(1.,1.),(1.,1.),(1.,1.),(1.,1.),(1.,1.),(1.,1.),(1.,
1.),(1.,1.),(1.,1.),(1.,1.),(1.,1.),(1.,1.),(1.,1.),(1.,1.),(1.,1.),(1.,
1.),(1.,1.),(1.,1.),(1.,1.),(1.,1.),(1.,1.),(1.,1.),(1.,1.),(1.,1.),(1.,
1.),(1.,1.),(1.,1.),(1.,1.),(1.,1.),(1.,1.),(1.,1.),(1.,1.),(1.,1.),(1.,
1.),(1.,1.),(1.,1.),(1.,1.),(1.,1.),(1.,1.),(1.,1.),(1.,1.),(1.,1.),(1.,
1.),(1.,1.),(1.,1.),(1.,1.),(1.,1.),(1.,1.),(1.,1.),(1.,1.),(1.,1.),(1.,
1.),(1.,1.),(1.,1.),(1.,1.),(1.,1.),(1.,1.),(1.,1.),(1.,1.),(1.,1.),(1.,
1.),(1.,1.),(1.,1.),(1.,1.),(1.,1.),(1.,1.),(1.,1.),(1.,1.),(1.,1.),(1.,
1.),(1.,1.),(1.,1.),(1.,1.),(1.,1.),(1.,1.),(1.,1.),(1.,1.),(1.,1.),(1.,
1.),(1.,1.),(1.,1.),(1.,1.),(1.,1.),(1.,1.),(1.,1.),(1.,1.),(1.,1.),(1.,
1.),(1.,1.),(1.,1.),(1.,1.),(1.,1.),(1.,1.),(1.,1.),(1.,1.),(1.,1.),(1.,
1.),(1.,1.),(1.,1.),(1.,1.),(1.,1.),(1.,1.),(1.,1.),(1.,1.),(1.,1.),(1.,
1.),(1.,1.),(1.,1.),(1.,1.),(1.,1.),(1.,1.),(1.,1.),(1.,1.),(1.,1.),(1.,
1.),(1.,1.),(1.,1.),(1.,1.),(1.,1.),(1.,1.),(1.,1.),(1.,1.),(1.,1.),(1.,
1.),(1.,1.),(1.,1.),(1.,1.),(1.,1.),(1.,1.),(1.,1.),(1.,1.),(1.,1.),(1.,
1.),(1.,1.),(1.,1.),(1.,1.),(1.,1.),(1.,1.),(1.,1.),(1.,1.),(1.,1.),(1.,
1.),(1.,1.),(1.,1.),(1.,1.),(1.,1.),(1.,1.),(1.,1.),(1.,1.),(1.,1.),(1.,
1.),(1.,1.),(1.,1.),(1.,1.),(1.,1.),(1.,1.),(1.,1.),(1.,1.),(1.,1.),(1.,
1.),(1.,1.)))
REPRESENTATION_ITEM('')
SURFACE()
);
#1087=(
BOUNDED_SURFACE()
B_SPLINE_SURFACE(5,1,((#225920,#225921),(#225922,#225923),(#225924,#225925),
(#225926,#225927),(#225928,#225929),(#225930,#225931),(#225932,#225933),
(#225934,#225935),(#225936,#225937),(#225938,#225939),(#225940,#225941),
(#225942,#225943),(#225944,#225945),(#225946,#225947),(#225948,#225949),
(#225950,#225951),(#225952,#225953),(#225954,#225955),(#225956,#225957),
(#225958,#225959),(#225960,#225961),(#225962,#225963),(#225964,#225965),
(#225966,#225967),(#225968,#225969),(#225970,#225971),(#225972,#225973),
(#225974,#225975),(#225976,#225977),(#225978,#225979),(#225980,#225981),
(#225982,#225983),(#225984,#225985),(#225986,#225987),(#225988,#225989),
(#225990,#225991),(#225992,#225993),(#225994,#225995),(#225996,#225997),
(#225998,#225999),(#226000,#226001),(#226002,#226003),(#226004,#226005),
(#226006,#226007),(#226008,#226009),(#226010,#226011),(#226012,#226013),
(#226014,#226015),(#226016,#226017),(#226018,#226019),(#226020,#226021),
(#226022,#226023),(#226024,#226025),(#226026,#226027),(#226028,#226029),
(#226030,#226031),(#226032,#226033),(#226034,#226035),(#226036,#226037),
(#226038,#226039),(#226040,#226041),(#226042,#226043),(#226044,#226045),
(#226046,#226047),(#226048,#226049),(#226050,#226051),(#226052,#226053),
(#226054,#226055),(#226056,#226057),(#226058,#226059),(#226060,#226061),
(#226062,#226063),(#226064,#226065),(#226066,#226067),(#226068,#226069),
(#226070,#226071),(#226072,#226073),(#226074,#226075),(#226076,#226077),
(#226078,#226079),(#226080,#226081),(#226082,#226083),(#226084,#226085),
(#226086,#226087),(#226088,#226089),(#226090,#226091),(#226092,#226093),
(#226094,#226095),(#226096,#226097),(#226098,#226099),(#226100,#226101),
(#226102,#226103),(#226104,#226105),(#226106,#226107),(#226108,#226109),
(#226110,#226111),(#226112,#226113),(#226114,#226115),(#226116,#226117),
(#226118,#226119),(#226120,#226121),(#226122,#226123),(#226124,#226125),
(#226126,#226127),(#226128,#226129),(#226130,#226131),(#226132,#226133),
(#226134,#226135),(#226136,#226137),(#226138,#226139),(#226140,#226141),
(#226142,#226143),(#226144,#226145),(#226146,#226147),(#226148,#226149),
(#226150,#226151),(#226152,#226153),(#226154,#226155),(#226156,#226157),
(#226158,#226159),(#226160,#226161),(#226162,#226163),(#226164,#226165),
(#226166,#226167),(#226168,#226169),(#226170,#226171),(#226172,#226173),
(#226174,#226175),(#226176,#226177),(#226178,#226179),(#226180,#226181),
(#226182,#226183),(#226184,#226185),(#226186,#226187),(#226188,#226189),
(#226190,#226191),(#226192,#226193),(#226194,#226195),(#226196,#226197),
(#226198,#226199),(#226200,#226201),(#226202,#226203),(#226204,#226205),
(#226206,#226207),(#226208,#226209),(#226210,#226211),(#226212,#226213),
(#226214,#226215),(#226216,#226217),(#226218,#226219),(#226220,#226221),
(#226222,#226223),(#226224,#226225),(#226226,#226227),(#226228,#226229),
(#226230,#226231),(#226232,#226233),(#226234,#226235),(#226236,#226237),
(#226238,#226239),(#226240,#226241),(#226242,#226243),(#226244,#226245),
(#226246,#226247),(#226248,#226249),(#226250,#226251),(#226252,#226253),
(#226254,#226255),(#226256,#226257),(#226258,#226259),(#226260,#226261),
(#226262,#226263),(#226264,#226265),(#226266,#226267),(#226268,#226269),
(#226270,#226271),(#226272,#226273),(#226274,#226275),(#226276,#226277),
(#226278,#226279),(#226280,#226281),(#226282,#226283),(#226284,#226285),
(#226286,#226287),(#226288,#226289),(#226290,#226291),(#226292,#226293),
(#226294,#226295),(#226296,#226297),(#226298,#226299),(#226300,#226301),
(#226302,#226303),(#226304,#226305),(#226306,#226307),(#226308,#226309),
(#226310,#226311),(#226312,#226313),(#226314,#226315),(#226316,#226317),
(#226318,#226319),(#226320,#226321),(#226322,#226323),(#226324,#226325),
(#226326,#226327),(#226328,#226329)),.UNSPECIFIED.,.F.,.F.,.F.)
B_SPLINE_SURFACE_WITH_KNOTS((6,1,1,1,1,1,1,1,1,1,1,1,1,1,1,1,1,1,1,1,1,
1,1,1,1,1,1,1,1,1,1,1,1,1,1,1,1,1,1,1,1,1,1,1,1,1,1,1,1,1,1,1,1,1,1,1,1,
1,1,1,1,1,1,1,1,1,1,1,1,1,1,1,1,1,1,1,1,1,1,1,1,1,1,1,1,1,1,1,1,1,1,1,1,
1,1,1,1,1,1,1,1,1,1,1,1,1,1,1,1,1,1,1,1,1,1,1,1,1,1,1,1,1,1,1,1,1,1,1,1,
1,1,1,1,1,1,1,1,1,1,1,1,1,1,1,1,1,1,1,1,1,1,1,1,1,1,1,1,1,1,1,1,1,1,1,1,
1,1,1,1,1,1,1,1,1,1,1,1,1,1,1,1,1,1,1,1,1,1,1,1,1,1,1,1,1,1,1,1,1,1,1,6),
(2,2),(-1.,-0.995000000000001,-0.990000000000001,-0.985000000000001,-0.980000000000001,
-0.975000000000001,-0.970000000000001,-0.965000000000001,-0.960000000000001,
-0.955000000000001,-0.950000000000001,-0.945000000000001,-0.940000000000001,
-0.935000000000001,-0.930000000000001,-0.925000000000001,-0.920000000000001,
-0.915000000000001,-0.910000000000001,-0.905000000000001,-0.900000000000001,
-0.895000000000001,-0.890000000000001,-0.885000000000001,-0.880000000000001,
-0.875000000000001,-0.870000000000001,-0.865000000000001,-0.860000000000001,
-0.855000000000001,-0.850000000000001,-0.845000000000001,-0.840000000000001,
-0.835000000000001,-0.830000000000001,-0.825000000000001,-0.820000000000001,
-0.815000000000001,-0.810000000000001,-0.805000000000001,-0.800000000000001,
-0.795000000000001,-0.790000000000001,-0.785000000000001,-0.780000000000001,
-0.775000000000001,-0.770000000000001,-0.765000000000001,-0.760000000000001,
-0.755000000000001,-0.750000000000001,-0.745000000000001,-0.740000000000001,
-0.735000000000001,-0.730000000000001,-0.725000000000001,-0.720000000000001,
-0.715000000000001,-0.710000000000001,-0.705000000000001,-0.700000000000001,
-0.695000000000001,-0.690000000000001,-0.685,-0.68,-0.675,-0.67,-0.665,
-0.66,-0.655,-0.65,-0.645,-0.64,-0.635,-0.63,-0.625,-0.62,-0.615,-0.61,
-0.605,-0.6,-0.595,-0.59,-0.585,-0.58,-0.575,-0.57,-0.565,-0.56,-0.555,
-0.55,-0.545,-0.54,-0.535,-0.53,-0.525,-0.52,-0.515,-0.51,-0.505,-0.5,-0.495,
-0.49,-0.485,-0.48,-0.475,-0.47,-0.465,-0.46,-0.455,-0.45,-0.445,-0.44,
-0.435,-0.43,-0.425,-0.42,-0.415,-0.41,-0.405,-0.4,-0.395,-0.39,-0.385,
-0.38,-0.375,-0.37,-0.365,-0.36,-0.355,-0.35,-0.345,-0.34,-0.335,-0.33,
-0.325,-0.32,-0.315,-0.31,-0.305,-0.3,-0.295,-0.29,-0.285,-0.28,-0.275,
-0.27,-0.265,-0.26,-0.255,-0.25,-0.245,-0.24,-0.235,-0.23,-0.225,-0.22,
-0.215,-0.21,-0.205,-0.2,-0.195,-0.19,-0.185,-0.18,-0.175,-0.17,-0.165,
-0.16,-0.155,-0.15,-0.145,-0.14,-0.135,-0.13,-0.125,-0.12,-0.115,-0.11,
-0.105,-0.1,-0.095,-0.09,-0.085,-0.08,-0.075,-0.07,-0.065,-0.06,-0.055,
-0.05,-0.045,-0.04,-0.035,-0.03,-0.025,-0.02,-0.015,-0.01,-0.005,0.),(0.,
1.2),.UNSPECIFIED.)
GEOMETRIC_REPRESENTATION_ITEM()
RATIONAL_B_SPLINE_SURFACE(((1.,1.),(1.,1.),(1.,1.),(1.,1.),(1.,1.),(1.,
1.),(1.,1.),(1.,1.),(1.,1.),(1.,1.),(1.,1.),(1.,1.),(1.,1.),(1.,1.),(1.,
1.),(1.,1.),(1.,1.),(1.,1.),(1.,1.),(1.,1.),(1.,1.),(1.,1.),(1.,1.),(1.,
1.),(1.,1.),(1.,1.),(1.,1.),(1.,1.),(1.,1.),(1.,1.),(1.,1.),(1.,1.),(1.,
1.),(1.,1.),(1.,1.),(1.,1.),(1.,1.),(1.,1.),(1.,1.),(1.,1.),(1.,1.),(1.,
1.),(1.,1.),(1.,1.),(1.,1.),(1.,1.),(1.,1.),(1.,1.),(1.,1.),(1.,1.),(1.,
1.),(1.,1.),(1.,1.),(1.,1.),(1.,1.),(1.,1.),(1.,1.),(1.,1.),(1.,1.),(1.,
1.),(1.,1.),(1.,1.),(1.,1.),(1.,1.),(1.,1.),(1.,1.),(1.,1.),(1.,1.),(1.,
1.),(1.,1.),(1.,1.),(1.,1.),(1.,1.),(1.,1.),(1.,1.),(1.,1.),(1.,1.),(1.,
1.),(1.,1.),(1.,1.),(1.,1.),(1.,1.),(1.,1.),(1.,1.),(1.,1.),(1.,1.),(1.,
1.),(1.,1.),(1.,1.),(1.,1.),(1.,1.),(1.,1.),(1.,1.),(1.,1.),(1.,1.),(1.,
1.),(1.,1.),(1.,1.),(1.,1.),(1.,1.),(1.,1.),(1.,1.),(1.,1.),(1.,1.),(1.,
1.),(1.,1.),(1.,1.),(1.,1.),(1.,1.),(1.,1.),(1.,1.),(1.,1.),(1.,1.),(1.,
1.),(1.,1.),(1.,1.),(1.,1.),(1.,1.),(1.,1.),(1.,1.),(1.,1.),(1.,1.),(1.,
1.),(1.,1.),(1.,1.),(1.,1.),(1.,1.),(1.,1.),(1.,1.),(1.,1.),(1.,1.),(1.,
1.),(1.,1.),(1.,1.),(1.,1.),(1.,1.),(1.,1.),(1.,1.),(1.,1.),(1.,1.),(1.,
1.),(1.,1.),(1.,1.),(1.,1.),(1.,1.),(1.,1.),(1.,1.),(1.,1.),(1.,1.),(1.,
1.),(1.,1.),(1.,1.),(1.,1.),(1.,1.),(1.,1.),(1.,1.),(1.,1.),(1.,1.),(1.,
1.),(1.,1.),(1.,1.),(1.,1.),(1.,1.),(1.,1.),(1.,1.),(1.,1.),(1.,1.),(1.,
1.),(1.,1.),(1.,1.),(1.,1.),(1.,1.),(1.,1.),(1.,1.),(1.,1.),(1.,1.),(1.,
1.),(1.,1.),(1.,1.),(1.,1.),(1.,1.),(1.,1.),(1.,1.),(1.,1.),(1.,1.),(1.,
1.),(1.,1.),(1.,1.),(1.,1.),(1.,1.),(1.,1.),(1.,1.),(1.,1.),(1.,1.),(1.,
1.),(1.,1.),(1.,1.),(1.,1.),(1.,1.),(1.,1.),(1.,1.),(1.,1.),(1.,1.),(1.,
1.),(1.,1.)))
REPRESENTATION_ITEM('')
SURFACE()
);
#1088=(
BOUNDED_SURFACE()
B_SPLINE_SURFACE(5,1,((#226743,#226744),(#226745,#226746),(#226747,#226748),
(#226749,#226750),(#226751,#226752),(#226753,#226754),(#226755,#226756),
(#226757,#226758),(#226759,#226760),(#226761,#226762),(#226763,#226764),
(#226765,#226766),(#226767,#226768),(#226769,#226770),(#226771,#226772),
(#226773,#226774),(#226775,#226776),(#226777,#226778),(#226779,#226780),
(#226781,#226782),(#226783,#226784),(#226785,#226786),(#226787,#226788),
(#226789,#226790),(#226791,#226792),(#226793,#226794),(#226795,#226796),
(#226797,#226798),(#226799,#226800),(#226801,#226802),(#226803,#226804),
(#226805,#226806),(#226807,#226808),(#226809,#226810),(#226811,#226812),
(#226813,#226814),(#226815,#226816),(#226817,#226818),(#226819,#226820),
(#226821,#226822),(#226823,#226824),(#226825,#226826),(#226827,#226828),
(#226829,#226830),(#226831,#226832),(#226833,#226834),(#226835,#226836),
(#226837,#226838),(#226839,#226840),(#226841,#226842),(#226843,#226844),
(#226845,#226846),(#226847,#226848),(#226849,#226850),(#226851,#226852),
(#226853,#226854),(#226855,#226856),(#226857,#226858),(#226859,#226860),
(#226861,#226862),(#226863,#226864),(#226865,#226866),(#226867,#226868),
(#226869,#226870),(#226871,#226872),(#226873,#226874),(#226875,#226876),
(#226877,#226878),(#226879,#226880),(#226881,#226882),(#226883,#226884),
(#226885,#226886),(#226887,#226888),(#226889,#226890),(#226891,#226892),
(#226893,#226894),(#226895,#226896),(#226897,#226898),(#226899,#226900),
(#226901,#226902),(#226903,#226904),(#226905,#226906),(#226907,#226908),
(#226909,#226910),(#226911,#226912),(#226913,#226914),(#226915,#226916),
(#226917,#226918),(#226919,#226920),(#226921,#226922),(#226923,#226924),
(#226925,#226926),(#226927,#226928),(#226929,#226930),(#226931,#226932),
(#226933,#226934),(#226935,#226936),(#226937,#226938),(#226939,#226940),
(#226941,#226942),(#226943,#226944),(#226945,#226946),(#226947,#226948),
(#226949,#226950),(#226951,#226952),(#226953,#226954),(#226955,#226956),
(#226957,#226958),(#226959,#226960),(#226961,#226962),(#226963,#226964),
(#226965,#226966),(#226967,#226968),(#226969,#226970),(#226971,#226972),
(#226973,#226974),(#226975,#226976),(#226977,#226978),(#226979,#226980),
(#226981,#226982),(#226983,#226984),(#226985,#226986),(#226987,#226988),
(#226989,#226990),(#226991,#226992),(#226993,#226994),(#226995,#226996),
(#226997,#226998),(#226999,#227000),(#227001,#227002),(#227003,#227004),
(#227005,#227006),(#227007,#227008),(#227009,#227010),(#227011,#227012),
(#227013,#227014),(#227015,#227016),(#227017,#227018),(#227019,#227020),
(#227021,#227022),(#227023,#227024),(#227025,#227026),(#227027,#227028),
(#227029,#227030),(#227031,#227032),(#227033,#227034),(#227035,#227036),
(#227037,#227038),(#227039,#227040),(#227041,#227042),(#227043,#227044),
(#227045,#227046),(#227047,#227048),(#227049,#227050),(#227051,#227052),
(#227053,#227054),(#227055,#227056),(#227057,#227058),(#227059,#227060),
(#227061,#227062),(#227063,#227064),(#227065,#227066),(#227067,#227068),
(#227069,#227070),(#227071,#227072),(#227073,#227074),(#227075,#227076),
(#227077,#227078),(#227079,#227080),(#227081,#227082),(#227083,#227084),
(#227085,#227086),(#227087,#227088),(#227089,#227090),(#227091,#227092),
(#227093,#227094),(#227095,#227096),(#227097,#227098),(#227099,#227100),
(#227101,#227102),(#227103,#227104),(#227105,#227106),(#227107,#227108),
(#227109,#227110),(#227111,#227112),(#227113,#227114),(#227115,#227116),
(#227117,#227118),(#227119,#227120),(#227121,#227122),(#227123,#227124),
(#227125,#227126),(#227127,#227128),(#227129,#227130),(#227131,#227132),
(#227133,#227134),(#227135,#227136),(#227137,#227138),(#227139,#227140),
(#227141,#227142),(#227143,#227144),(#227145,#227146),(#227147,#227148),
(#227149,#227150),(#227151,#227152)),.UNSPECIFIED.,.F.,.F.,.F.)
B_SPLINE_SURFACE_WITH_KNOTS((6,1,1,1,1,1,1,1,1,1,1,1,1,1,1,1,1,1,1,1,1,
1,1,1,1,1,1,1,1,1,1,1,1,1,1,1,1,1,1,1,1,1,1,1,1,1,1,1,1,1,1,1,1,1,1,1,1,
1,1,1,1,1,1,1,1,1,1,1,1,1,1,1,1,1,1,1,1,1,1,1,1,1,1,1,1,1,1,1,1,1,1,1,1,
1,1,1,1,1,1,1,1,1,1,1,1,1,1,1,1,1,1,1,1,1,1,1,1,1,1,1,1,1,1,1,1,1,1,1,1,
1,1,1,1,1,1,1,1,1,1,1,1,1,1,1,1,1,1,1,1,1,1,1,1,1,1,1,1,1,1,1,1,1,1,1,1,
1,1,1,1,1,1,1,1,1,1,1,1,1,1,1,1,1,1,1,1,1,1,1,1,1,1,1,1,1,1,1,1,1,1,1,6),
(2,2),(0.,0.005,0.01,0.015,0.02,0.025,0.03,0.035,0.04,0.045,0.05,0.055,
0.06,0.065,0.07,0.075,0.08,0.085,0.09,0.095,0.1,0.105,0.11,0.115,0.12,0.125,
0.13,0.135,0.14,0.145,0.15,0.155,0.16,0.165,0.17,0.175,0.18,0.185,0.19,
0.195,0.2,0.205,0.21,0.215,0.22,0.225,0.23,0.235,0.24,0.245,0.25,0.255,
0.26,0.265,0.27,0.275,0.28,0.285,0.29,0.295,0.3,0.305,0.31,0.315,0.32,0.325,
0.33,0.335,0.34,0.345,0.35,0.355,0.36,0.365,0.37,0.375,0.38,0.385,0.39,
0.395,0.4,0.405,0.41,0.415,0.42,0.425,0.43,0.435,0.44,0.445,0.45,0.455,
0.46,0.465,0.47,0.475,0.48,0.485,0.49,0.495,0.5,0.505,0.51,0.515,0.52,0.525,
0.53,0.535,0.54,0.545,0.55,0.555,0.56,0.565,0.57,0.575,0.58,0.585,0.59,
0.595,0.6,0.605,0.61,0.615,0.62,0.625,0.63,0.635,0.64,0.645,0.65,0.655,
0.66,0.665,0.67,0.675,0.68,0.685,0.690000000000001,0.695000000000001,0.700000000000001,
0.705000000000001,0.710000000000001,0.715000000000001,0.720000000000001,
0.725000000000001,0.730000000000001,0.735000000000001,0.740000000000001,
0.745000000000001,0.750000000000001,0.755000000000001,0.760000000000001,
0.765000000000001,0.770000000000001,0.775000000000001,0.780000000000001,
0.785000000000001,0.790000000000001,0.795000000000001,0.800000000000001,
0.805000000000001,0.810000000000001,0.815000000000001,0.820000000000001,
0.825000000000001,0.830000000000001,0.835000000000001,0.840000000000001,
0.845000000000001,0.850000000000001,0.855000000000001,0.860000000000001,
0.865000000000001,0.870000000000001,0.875000000000001,0.880000000000001,
0.885000000000001,0.890000000000001,0.895000000000001,0.900000000000001,
0.905000000000001,0.910000000000001,0.915000000000001,0.920000000000001,
0.925000000000001,0.930000000000001,0.935000000000001,0.940000000000001,
0.945000000000001,0.950000000000001,0.955000000000001,0.960000000000001,
0.965000000000001,0.970000000000001,0.975000000000001,0.980000000000001,
0.985000000000001,0.990000000000001,0.995000000000001,1.),(0.,1.2),
 .UNSPECIFIED.)
GEOMETRIC_REPRESENTATION_ITEM()
RATIONAL_B_SPLINE_SURFACE(((1.,1.),(1.,1.),(1.,1.),(1.,1.),(1.,1.),(1.,
1.),(1.,1.),(1.,1.),(1.,1.),(1.,1.),(1.,1.),(1.,1.),(1.,1.),(1.,1.),(1.,
1.),(1.,1.),(1.,1.),(1.,1.),(1.,1.),(1.,1.),(1.,1.),(1.,1.),(1.,1.),(1.,
1.),(1.,1.),(1.,1.),(1.,1.),(1.,1.),(1.,1.),(1.,1.),(1.,1.),(1.,1.),(1.,
1.),(1.,1.),(1.,1.),(1.,1.),(1.,1.),(1.,1.),(1.,1.),(1.,1.),(1.,1.),(1.,
1.),(1.,1.),(1.,1.),(1.,1.),(1.,1.),(1.,1.),(1.,1.),(1.,1.),(1.,1.),(1.,
1.),(1.,1.),(1.,1.),(1.,1.),(1.,1.),(1.,1.),(1.,1.),(1.,1.),(1.,1.),(1.,
1.),(1.,1.),(1.,1.),(1.,1.),(1.,1.),(1.,1.),(1.,1.),(1.,1.),(1.,1.),(1.,
1.),(1.,1.),(1.,1.),(1.,1.),(1.,1.),(1.,1.),(1.,1.),(1.,1.),(1.,1.),(1.,
1.),(1.,1.),(1.,1.),(1.,1.),(1.,1.),(1.,1.),(1.,1.),(1.,1.),(1.,1.),(1.,
1.),(1.,1.),(1.,1.),(1.,1.),(1.,1.),(1.,1.),(1.,1.),(1.,1.),(1.,1.),(1.,
1.),(1.,1.),(1.,1.),(1.,1.),(1.,1.),(1.,1.),(1.,1.),(1.,1.),(1.,1.),(1.,
1.),(1.,1.),(1.,1.),(1.,1.),(1.,1.),(1.,1.),(1.,1.),(1.,1.),(1.,1.),(1.,
1.),(1.,1.),(1.,1.),(1.,1.),(1.,1.),(1.,1.),(1.,1.),(1.,1.),(1.,1.),(1.,
1.),(1.,1.),(1.,1.),(1.,1.),(1.,1.),(1.,1.),(1.,1.),(1.,1.),(1.,1.),(1.,
1.),(1.,1.),(1.,1.),(1.,1.),(1.,1.),(1.,1.),(1.,1.),(1.,1.),(1.,1.),(1.,
1.),(1.,1.),(1.,1.),(1.,1.),(1.,1.),(1.,1.),(1.,1.),(1.,1.),(1.,1.),(1.,
1.),(1.,1.),(1.,1.),(1.,1.),(1.,1.),(1.,1.),(1.,1.),(1.,1.),(1.,1.),(1.,
1.),(1.,1.),(1.,1.),(1.,1.),(1.,1.),(1.,1.),(1.,1.),(1.,1.),(1.,1.),(1.,
1.),(1.,1.),(1.,1.),(1.,1.),(1.,1.),(1.,1.),(1.,1.),(1.,1.),(1.,1.),(1.,
1.),(1.,1.),(1.,1.),(1.,1.),(1.,1.),(1.,1.),(1.,1.),(1.,1.),(1.,1.),(1.,
1.),(1.,1.),(1.,1.),(1.,1.),(1.,1.),(1.,1.),(1.,1.),(1.,1.),(1.,1.),(1.,
1.),(1.,1.),(1.,1.),(1.,1.),(1.,1.),(1.,1.),(1.,1.),(1.,1.),(1.,1.),(1.,
1.),(1.,1.)))
REPRESENTATION_ITEM('')
SURFACE()
);
#1089=(
BOUNDED_SURFACE()
B_SPLINE_SURFACE(5,1,((#227572,#227573),(#227574,#227575),(#227576,#227577),
(#227578,#227579),(#227580,#227581),(#227582,#227583),(#227584,#227585),
(#227586,#227587),(#227588,#227589),(#227590,#227591),(#227592,#227593),
(#227594,#227595),(#227596,#227597),(#227598,#227599),(#227600,#227601),
(#227602,#227603),(#227604,#227605),(#227606,#227607),(#227608,#227609),
(#227610,#227611),(#227612,#227613),(#227614,#227615),(#227616,#227617),
(#227618,#227619),(#227620,#227621),(#227622,#227623),(#227624,#227625),
(#227626,#227627),(#227628,#227629),(#227630,#227631),(#227632,#227633),
(#227634,#227635),(#227636,#227637),(#227638,#227639),(#227640,#227641),
(#227642,#227643),(#227644,#227645),(#227646,#227647),(#227648,#227649),
(#227650,#227651),(#227652,#227653),(#227654,#227655),(#227656,#227657),
(#227658,#227659),(#227660,#227661),(#227662,#227663),(#227664,#227665),
(#227666,#227667),(#227668,#227669),(#227670,#227671),(#227672,#227673),
(#227674,#227675),(#227676,#227677),(#227678,#227679),(#227680,#227681),
(#227682,#227683),(#227684,#227685),(#227686,#227687),(#227688,#227689),
(#227690,#227691),(#227692,#227693),(#227694,#227695),(#227696,#227697),
(#227698,#227699),(#227700,#227701),(#227702,#227703),(#227704,#227705),
(#227706,#227707),(#227708,#227709),(#227710,#227711),(#227712,#227713),
(#227714,#227715),(#227716,#227717),(#227718,#227719),(#227720,#227721),
(#227722,#227723),(#227724,#227725),(#227726,#227727),(#227728,#227729),
(#227730,#227731),(#227732,#227733),(#227734,#227735),(#227736,#227737),
(#227738,#227739),(#227740,#227741),(#227742,#227743),(#227744,#227745),
(#227746,#227747),(#227748,#227749),(#227750,#227751),(#227752,#227753),
(#227754,#227755),(#227756,#227757),(#227758,#227759),(#227760,#227761),
(#227762,#227763),(#227764,#227765),(#227766,#227767),(#227768,#227769),
(#227770,#227771),(#227772,#227773),(#227774,#227775),(#227776,#227777),
(#227778,#227779),(#227780,#227781),(#227782,#227783),(#227784,#227785),
(#227786,#227787),(#227788,#227789),(#227790,#227791),(#227792,#227793),
(#227794,#227795),(#227796,#227797),(#227798,#227799),(#227800,#227801),
(#227802,#227803),(#227804,#227805),(#227806,#227807),(#227808,#227809),
(#227810,#227811),(#227812,#227813),(#227814,#227815),(#227816,#227817),
(#227818,#227819),(#227820,#227821),(#227822,#227823),(#227824,#227825),
(#227826,#227827),(#227828,#227829),(#227830,#227831),(#227832,#227833),
(#227834,#227835),(#227836,#227837),(#227838,#227839),(#227840,#227841),
(#227842,#227843),(#227844,#227845),(#227846,#227847),(#227848,#227849),
(#227850,#227851),(#227852,#227853),(#227854,#227855),(#227856,#227857),
(#227858,#227859),(#227860,#227861),(#227862,#227863),(#227864,#227865),
(#227866,#227867),(#227868,#227869),(#227870,#227871),(#227872,#227873),
(#227874,#227875),(#227876,#227877),(#227878,#227879),(#227880,#227881),
(#227882,#227883),(#227884,#227885),(#227886,#227887),(#227888,#227889),
(#227890,#227891),(#227892,#227893),(#227894,#227895),(#227896,#227897),
(#227898,#227899),(#227900,#227901),(#227902,#227903),(#227904,#227905),
(#227906,#227907),(#227908,#227909),(#227910,#227911),(#227912,#227913),
(#227914,#227915),(#227916,#227917),(#227918,#227919),(#227920,#227921),
(#227922,#227923),(#227924,#227925),(#227926,#227927),(#227928,#227929),
(#227930,#227931),(#227932,#227933),(#227934,#227935),(#227936,#227937),
(#227938,#227939),(#227940,#227941),(#227942,#227943),(#227944,#227945),
(#227946,#227947),(#227948,#227949),(#227950,#227951),(#227952,#227953),
(#227954,#227955),(#227956,#227957),(#227958,#227959),(#227960,#227961),
(#227962,#227963),(#227964,#227965),(#227966,#227967),(#227968,#227969),
(#227970,#227971),(#227972,#227973),(#227974,#227975),(#227976,#227977),
(#227978,#227979),(#227980,#227981)),.UNSPECIFIED.,.F.,.F.,.F.)
B_SPLINE_SURFACE_WITH_KNOTS((6,1,1,1,1,1,1,1,1,1,1,1,1,1,1,1,1,1,1,1,1,
1,1,1,1,1,1,1,1,1,1,1,1,1,1,1,1,1,1,1,1,1,1,1,1,1,1,1,1,1,1,1,1,1,1,1,1,
1,1,1,1,1,1,1,1,1,1,1,1,1,1,1,1,1,1,1,1,1,1,1,1,1,1,1,1,1,1,1,1,1,1,1,1,
1,1,1,1,1,1,1,1,1,1,1,1,1,1,1,1,1,1,1,1,1,1,1,1,1,1,1,1,1,1,1,1,1,1,1,1,
1,1,1,1,1,1,1,1,1,1,1,1,1,1,1,1,1,1,1,1,1,1,1,1,1,1,1,1,1,1,1,1,1,1,1,1,
1,1,1,1,1,1,1,1,1,1,1,1,1,1,1,1,1,1,1,1,1,1,1,1,1,1,1,1,1,1,1,1,1,1,1,6),
(2,2),(-1.,-0.995000000000001,-0.990000000000001,-0.985000000000001,-0.980000000000001,
-0.975000000000001,-0.970000000000001,-0.965000000000001,-0.960000000000001,
-0.955000000000001,-0.950000000000001,-0.945000000000001,-0.940000000000001,
-0.935000000000001,-0.930000000000001,-0.925000000000001,-0.920000000000001,
-0.915000000000001,-0.910000000000001,-0.905000000000001,-0.900000000000001,
-0.895000000000001,-0.890000000000001,-0.885000000000001,-0.880000000000001,
-0.875000000000001,-0.870000000000001,-0.865000000000001,-0.860000000000001,
-0.855000000000001,-0.850000000000001,-0.845000000000001,-0.840000000000001,
-0.835000000000001,-0.830000000000001,-0.825000000000001,-0.820000000000001,
-0.815000000000001,-0.810000000000001,-0.805000000000001,-0.800000000000001,
-0.795000000000001,-0.790000000000001,-0.785000000000001,-0.780000000000001,
-0.775000000000001,-0.770000000000001,-0.765000000000001,-0.760000000000001,
-0.755000000000001,-0.750000000000001,-0.745000000000001,-0.740000000000001,
-0.735000000000001,-0.730000000000001,-0.725000000000001,-0.720000000000001,
-0.715000000000001,-0.710000000000001,-0.705000000000001,-0.700000000000001,
-0.695000000000001,-0.690000000000001,-0.685,-0.68,-0.675,-0.67,-0.665,
-0.66,-0.655,-0.65,-0.645,-0.64,-0.635,-0.63,-0.625,-0.62,-0.615,-0.61,
-0.605,-0.6,-0.595,-0.59,-0.585,-0.58,-0.575,-0.57,-0.565,-0.56,-0.555,
-0.55,-0.545,-0.54,-0.535,-0.53,-0.525,-0.52,-0.515,-0.51,-0.505,-0.5,-0.495,
-0.49,-0.485,-0.48,-0.475,-0.47,-0.465,-0.46,-0.455,-0.45,-0.445,-0.44,
-0.435,-0.43,-0.425,-0.42,-0.415,-0.41,-0.405,-0.4,-0.395,-0.39,-0.385,
-0.38,-0.375,-0.37,-0.365,-0.36,-0.355,-0.35,-0.345,-0.34,-0.335,-0.33,
-0.325,-0.32,-0.315,-0.31,-0.305,-0.3,-0.295,-0.29,-0.285,-0.28,-0.275,
-0.27,-0.265,-0.26,-0.255,-0.25,-0.245,-0.24,-0.235,-0.23,-0.225,-0.22,
-0.215,-0.21,-0.205,-0.2,-0.195,-0.19,-0.185,-0.18,-0.175,-0.17,-0.165,
-0.16,-0.155,-0.15,-0.145,-0.14,-0.135,-0.13,-0.125,-0.12,-0.115,-0.11,
-0.105,-0.1,-0.095,-0.09,-0.085,-0.08,-0.075,-0.07,-0.065,-0.06,-0.055,
-0.05,-0.045,-0.04,-0.035,-0.03,-0.025,-0.02,-0.015,-0.01,-0.005,0.),(0.,
1.2),.UNSPECIFIED.)
GEOMETRIC_REPRESENTATION_ITEM()
RATIONAL_B_SPLINE_SURFACE(((1.,1.),(1.,1.),(1.,1.),(1.,1.),(1.,1.),(1.,
1.),(1.,1.),(1.,1.),(1.,1.),(1.,1.),(1.,1.),(1.,1.),(1.,1.),(1.,1.),(1.,
1.),(1.,1.),(1.,1.),(1.,1.),(1.,1.),(1.,1.),(1.,1.),(1.,1.),(1.,1.),(1.,
1.),(1.,1.),(1.,1.),(1.,1.),(1.,1.),(1.,1.),(1.,1.),(1.,1.),(1.,1.),(1.,
1.),(1.,1.),(1.,1.),(1.,1.),(1.,1.),(1.,1.),(1.,1.),(1.,1.),(1.,1.),(1.,
1.),(1.,1.),(1.,1.),(1.,1.),(1.,1.),(1.,1.),(1.,1.),(1.,1.),(1.,1.),(1.,
1.),(1.,1.),(1.,1.),(1.,1.),(1.,1.),(1.,1.),(1.,1.),(1.,1.),(1.,1.),(1.,
1.),(1.,1.),(1.,1.),(1.,1.),(1.,1.),(1.,1.),(1.,1.),(1.,1.),(1.,1.),(1.,
1.),(1.,1.),(1.,1.),(1.,1.),(1.,1.),(1.,1.),(1.,1.),(1.,1.),(1.,1.),(1.,
1.),(1.,1.),(1.,1.),(1.,1.),(1.,1.),(1.,1.),(1.,1.),(1.,1.),(1.,1.),(1.,
1.),(1.,1.),(1.,1.),(1.,1.),(1.,1.),(1.,1.),(1.,1.),(1.,1.),(1.,1.),(1.,
1.),(1.,1.),(1.,1.),(1.,1.),(1.,1.),(1.,1.),(1.,1.),(1.,1.),(1.,1.),(1.,
1.),(1.,1.),(1.,1.),(1.,1.),(1.,1.),(1.,1.),(1.,1.),(1.,1.),(1.,1.),(1.,
1.),(1.,1.),(1.,1.),(1.,1.),(1.,1.),(1.,1.),(1.,1.),(1.,1.),(1.,1.),(1.,
1.),(1.,1.),(1.,1.),(1.,1.),(1.,1.),(1.,1.),(1.,1.),(1.,1.),(1.,1.),(1.,
1.),(1.,1.),(1.,1.),(1.,1.),(1.,1.),(1.,1.),(1.,1.),(1.,1.),(1.,1.),(1.,
1.),(1.,1.),(1.,1.),(1.,1.),(1.,1.),(1.,1.),(1.,1.),(1.,1.),(1.,1.),(1.,
1.),(1.,1.),(1.,1.),(1.,1.),(1.,1.),(1.,1.),(1.,1.),(1.,1.),(1.,1.),(1.,
1.),(1.,1.),(1.,1.),(1.,1.),(1.,1.),(1.,1.),(1.,1.),(1.,1.),(1.,1.),(1.,
1.),(1.,1.),(1.,1.),(1.,1.),(1.,1.),(1.,1.),(1.,1.),(1.,1.),(1.,1.),(1.,
1.),(1.,1.),(1.,1.),(1.,1.),(1.,1.),(1.,1.),(1.,1.),(1.,1.),(1.,1.),(1.,
1.),(1.,1.),(1.,1.),(1.,1.),(1.,1.),(1.,1.),(1.,1.),(1.,1.),(1.,1.),(1.,
1.),(1.,1.),(1.,1.),(1.,1.),(1.,1.),(1.,1.),(1.,1.),(1.,1.),(1.,1.),(1.,
1.),(1.,1.)))
REPRESENTATION_ITEM('')
SURFACE()
);
#1090=(
BOUNDED_SURFACE()
B_SPLINE_SURFACE(5,1,((#228395,#228396),(#228397,#228398),(#228399,#228400),
(#228401,#228402),(#228403,#228404),(#228405,#228406),(#228407,#228408),
(#228409,#228410),(#228411,#228412),(#228413,#228414),(#228415,#228416),
(#228417,#228418),(#228419,#228420),(#228421,#228422),(#228423,#228424),
(#228425,#228426),(#228427,#228428),(#228429,#228430),(#228431,#228432),
(#228433,#228434),(#228435,#228436),(#228437,#228438),(#228439,#228440),
(#228441,#228442),(#228443,#228444),(#228445,#228446),(#228447,#228448),
(#228449,#228450),(#228451,#228452),(#228453,#228454),(#228455,#228456),
(#228457,#228458),(#228459,#228460),(#228461,#228462),(#228463,#228464),
(#228465,#228466),(#228467,#228468),(#228469,#228470),(#228471,#228472),
(#228473,#228474),(#228475,#228476),(#228477,#228478),(#228479,#228480),
(#228481,#228482),(#228483,#228484),(#228485,#228486),(#228487,#228488),
(#228489,#228490),(#228491,#228492),(#228493,#228494),(#228495,#228496),
(#228497,#228498),(#228499,#228500),(#228501,#228502),(#228503,#228504),
(#228505,#228506),(#228507,#228508),(#228509,#228510),(#228511,#228512),
(#228513,#228514),(#228515,#228516),(#228517,#228518),(#228519,#228520),
(#228521,#228522),(#228523,#228524),(#228525,#228526),(#228527,#228528),
(#228529,#228530),(#228531,#228532),(#228533,#228534),(#228535,#228536),
(#228537,#228538),(#228539,#228540),(#228541,#228542),(#228543,#228544),
(#228545,#228546),(#228547,#228548),(#228549,#228550),(#228551,#228552),
(#228553,#228554),(#228555,#228556),(#228557,#228558),(#228559,#228560),
(#228561,#228562),(#228563,#228564),(#228565,#228566),(#228567,#228568),
(#228569,#228570),(#228571,#228572),(#228573,#228574),(#228575,#228576),
(#228577,#228578),(#228579,#228580),(#228581,#228582),(#228583,#228584),
(#228585,#228586),(#228587,#228588),(#228589,#228590),(#228591,#228592),
(#228593,#228594),(#228595,#228596),(#228597,#228598),(#228599,#228600),
(#228601,#228602),(#228603,#228604),(#228605,#228606),(#228607,#228608),
(#228609,#228610),(#228611,#228612),(#228613,#228614),(#228615,#228616),
(#228617,#228618),(#228619,#228620),(#228621,#228622),(#228623,#228624),
(#228625,#228626),(#228627,#228628),(#228629,#228630),(#228631,#228632),
(#228633,#228634),(#228635,#228636),(#228637,#228638),(#228639,#228640),
(#228641,#228642),(#228643,#228644),(#228645,#228646),(#228647,#228648),
(#228649,#228650),(#228651,#228652),(#228653,#228654),(#228655,#228656),
(#228657,#228658),(#228659,#228660),(#228661,#228662),(#228663,#228664),
(#228665,#228666),(#228667,#228668),(#228669,#228670),(#228671,#228672),
(#228673,#228674),(#228675,#228676),(#228677,#228678),(#228679,#228680),
(#228681,#228682),(#228683,#228684),(#228685,#228686),(#228687,#228688),
(#228689,#228690),(#228691,#228692),(#228693,#228694),(#228695,#228696),
(#228697,#228698),(#228699,#228700),(#228701,#228702),(#228703,#228704),
(#228705,#228706),(#228707,#228708),(#228709,#228710),(#228711,#228712),
(#228713,#228714),(#228715,#228716),(#228717,#228718),(#228719,#228720),
(#228721,#228722),(#228723,#228724),(#228725,#228726),(#228727,#228728),
(#228729,#228730),(#228731,#228732),(#228733,#228734),(#228735,#228736),
(#228737,#228738),(#228739,#228740),(#228741,#228742),(#228743,#228744),
(#228745,#228746),(#228747,#228748),(#228749,#228750),(#228751,#228752),
(#228753,#228754),(#228755,#228756),(#228757,#228758),(#228759,#228760),
(#228761,#228762),(#228763,#228764),(#228765,#228766),(#228767,#228768),
(#228769,#228770),(#228771,#228772),(#228773,#228774),(#228775,#228776),
(#228777,#228778),(#228779,#228780),(#228781,#228782),(#228783,#228784),
(#228785,#228786),(#228787,#228788),(#228789,#228790),(#228791,#228792),
(#228793,#228794),(#228795,#228796),(#228797,#228798),(#228799,#228800),
(#228801,#228802),(#228803,#228804)),.UNSPECIFIED.,.F.,.F.,.F.)
B_SPLINE_SURFACE_WITH_KNOTS((6,1,1,1,1,1,1,1,1,1,1,1,1,1,1,1,1,1,1,1,1,
1,1,1,1,1,1,1,1,1,1,1,1,1,1,1,1,1,1,1,1,1,1,1,1,1,1,1,1,1,1,1,1,1,1,1,1,
1,1,1,1,1,1,1,1,1,1,1,1,1,1,1,1,1,1,1,1,1,1,1,1,1,1,1,1,1,1,1,1,1,1,1,1,
1,1,1,1,1,1,1,1,1,1,1,1,1,1,1,1,1,1,1,1,1,1,1,1,1,1,1,1,1,1,1,1,1,1,1,1,
1,1,1,1,1,1,1,1,1,1,1,1,1,1,1,1,1,1,1,1,1,1,1,1,1,1,1,1,1,1,1,1,1,1,1,1,
1,1,1,1,1,1,1,1,1,1,1,1,1,1,1,1,1,1,1,1,1,1,1,1,1,1,1,1,1,1,1,1,1,1,1,6),
(2,2),(0.,0.005,0.01,0.015,0.02,0.025,0.03,0.035,0.04,0.045,0.05,0.055,
0.06,0.065,0.07,0.075,0.08,0.085,0.09,0.095,0.1,0.105,0.11,0.115,0.12,0.125,
0.13,0.135,0.14,0.145,0.15,0.155,0.16,0.165,0.17,0.175,0.18,0.185,0.19,
0.195,0.2,0.205,0.21,0.215,0.22,0.225,0.23,0.235,0.24,0.245,0.25,0.255,
0.26,0.265,0.27,0.275,0.28,0.285,0.29,0.295,0.3,0.305,0.31,0.315,0.32,0.325,
0.33,0.335,0.34,0.345,0.35,0.355,0.36,0.365,0.37,0.375,0.38,0.385,0.39,
0.395,0.4,0.405,0.41,0.415,0.42,0.425,0.43,0.435,0.44,0.445,0.45,0.455,
0.46,0.465,0.47,0.475,0.48,0.485,0.49,0.495,0.5,0.505,0.51,0.515,0.52,0.525,
0.53,0.535,0.54,0.545,0.55,0.555,0.56,0.565,0.57,0.575,0.58,0.585,0.59,
0.595,0.6,0.605,0.61,0.615,0.62,0.625,0.63,0.635,0.64,0.645,0.65,0.655,
0.66,0.665,0.67,0.675,0.68,0.685,0.690000000000001,0.695000000000001,0.700000000000001,
0.705000000000001,0.710000000000001,0.715000000000001,0.720000000000001,
0.725000000000001,0.730000000000001,0.735000000000001,0.740000000000001,
0.745000000000001,0.750000000000001,0.755000000000001,0.760000000000001,
0.765000000000001,0.770000000000001,0.775000000000001,0.780000000000001,
0.785000000000001,0.790000000000001,0.795000000000001,0.800000000000001,
0.805000000000001,0.810000000000001,0.815000000000001,0.820000000000001,
0.825000000000001,0.830000000000001,0.835000000000001,0.840000000000001,
0.845000000000001,0.850000000000001,0.855000000000001,0.860000000000001,
0.865000000000001,0.870000000000001,0.875000000000001,0.880000000000001,
0.885000000000001,0.890000000000001,0.895000000000001,0.900000000000001,
0.905000000000001,0.910000000000001,0.915000000000001,0.920000000000001,
0.925000000000001,0.930000000000001,0.935000000000001,0.940000000000001,
0.945000000000001,0.950000000000001,0.955000000000001,0.960000000000001,
0.965000000000001,0.970000000000001,0.975000000000001,0.980000000000001,
0.985000000000001,0.990000000000001,0.995000000000001,1.),(0.,1.2),
 .UNSPECIFIED.)
GEOMETRIC_REPRESENTATION_ITEM()
RATIONAL_B_SPLINE_SURFACE(((1.,1.),(1.,1.),(1.,1.),(1.,1.),(1.,1.),(1.,
1.),(1.,1.),(1.,1.),(1.,1.),(1.,1.),(1.,1.),(1.,1.),(1.,1.),(1.,1.),(1.,
1.),(1.,1.),(1.,1.),(1.,1.),(1.,1.),(1.,1.),(1.,1.),(1.,1.),(1.,1.),(1.,
1.),(1.,1.),(1.,1.),(1.,1.),(1.,1.),(1.,1.),(1.,1.),(1.,1.),(1.,1.),(1.,
1.),(1.,1.),(1.,1.),(1.,1.),(1.,1.),(1.,1.),(1.,1.),(1.,1.),(1.,1.),(1.,
1.),(1.,1.),(1.,1.),(1.,1.),(1.,1.),(1.,1.),(1.,1.),(1.,1.),(1.,1.),(1.,
1.),(1.,1.),(1.,1.),(1.,1.),(1.,1.),(1.,1.),(1.,1.),(1.,1.),(1.,1.),(1.,
1.),(1.,1.),(1.,1.),(1.,1.),(1.,1.),(1.,1.),(1.,1.),(1.,1.),(1.,1.),(1.,
1.),(1.,1.),(1.,1.),(1.,1.),(1.,1.),(1.,1.),(1.,1.),(1.,1.),(1.,1.),(1.,
1.),(1.,1.),(1.,1.),(1.,1.),(1.,1.),(1.,1.),(1.,1.),(1.,1.),(1.,1.),(1.,
1.),(1.,1.),(1.,1.),(1.,1.),(1.,1.),(1.,1.),(1.,1.),(1.,1.),(1.,1.),(1.,
1.),(1.,1.),(1.,1.),(1.,1.),(1.,1.),(1.,1.),(1.,1.),(1.,1.),(1.,1.),(1.,
1.),(1.,1.),(1.,1.),(1.,1.),(1.,1.),(1.,1.),(1.,1.),(1.,1.),(1.,1.),(1.,
1.),(1.,1.),(1.,1.),(1.,1.),(1.,1.),(1.,1.),(1.,1.),(1.,1.),(1.,1.),(1.,
1.),(1.,1.),(1.,1.),(1.,1.),(1.,1.),(1.,1.),(1.,1.),(1.,1.),(1.,1.),(1.,
1.),(1.,1.),(1.,1.),(1.,1.),(1.,1.),(1.,1.),(1.,1.),(1.,1.),(1.,1.),(1.,
1.),(1.,1.),(1.,1.),(1.,1.),(1.,1.),(1.,1.),(1.,1.),(1.,1.),(1.,1.),(1.,
1.),(1.,1.),(1.,1.),(1.,1.),(1.,1.),(1.,1.),(1.,1.),(1.,1.),(1.,1.),(1.,
1.),(1.,1.),(1.,1.),(1.,1.),(1.,1.),(1.,1.),(1.,1.),(1.,1.),(1.,1.),(1.,
1.),(1.,1.),(1.,1.),(1.,1.),(1.,1.),(1.,1.),(1.,1.),(1.,1.),(1.,1.),(1.,
1.),(1.,1.),(1.,1.),(1.,1.),(1.,1.),(1.,1.),(1.,1.),(1.,1.),(1.,1.),(1.,
1.),(1.,1.),(1.,1.),(1.,1.),(1.,1.),(1.,1.),(1.,1.),(1.,1.),(1.,1.),(1.,
1.),(1.,1.),(1.,1.),(1.,1.),(1.,1.),(1.,1.),(1.,1.),(1.,1.),(1.,1.),(1.,
1.),(1.,1.)))
REPRESENTATION_ITEM('')
SURFACE()
);
#1091=(
BOUNDED_SURFACE()
B_SPLINE_SURFACE(5,1,((#229224,#229225),(#229226,#229227),(#229228,#229229),
(#229230,#229231),(#229232,#229233),(#229234,#229235),(#229236,#229237),
(#229238,#229239),(#229240,#229241),(#229242,#229243),(#229244,#229245),
(#229246,#229247),(#229248,#229249),(#229250,#229251),(#229252,#229253),
(#229254,#229255),(#229256,#229257),(#229258,#229259),(#229260,#229261),
(#229262,#229263),(#229264,#229265),(#229266,#229267),(#229268,#229269),
(#229270,#229271),(#229272,#229273),(#229274,#229275),(#229276,#229277),
(#229278,#229279),(#229280,#229281),(#229282,#229283),(#229284,#229285),
(#229286,#229287),(#229288,#229289),(#229290,#229291),(#229292,#229293),
(#229294,#229295),(#229296,#229297),(#229298,#229299),(#229300,#229301),
(#229302,#229303),(#229304,#229305),(#229306,#229307),(#229308,#229309),
(#229310,#229311),(#229312,#229313),(#229314,#229315),(#229316,#229317),
(#229318,#229319),(#229320,#229321),(#229322,#229323),(#229324,#229325),
(#229326,#229327),(#229328,#229329),(#229330,#229331),(#229332,#229333),
(#229334,#229335),(#229336,#229337),(#229338,#229339),(#229340,#229341),
(#229342,#229343),(#229344,#229345),(#229346,#229347),(#229348,#229349),
(#229350,#229351),(#229352,#229353),(#229354,#229355),(#229356,#229357),
(#229358,#229359),(#229360,#229361),(#229362,#229363),(#229364,#229365),
(#229366,#229367),(#229368,#229369),(#229370,#229371),(#229372,#229373),
(#229374,#229375),(#229376,#229377),(#229378,#229379),(#229380,#229381),
(#229382,#229383),(#229384,#229385),(#229386,#229387),(#229388,#229389),
(#229390,#229391),(#229392,#229393),(#229394,#229395),(#229396,#229397),
(#229398,#229399),(#229400,#229401),(#229402,#229403),(#229404,#229405),
(#229406,#229407),(#229408,#229409),(#229410,#229411),(#229412,#229413),
(#229414,#229415),(#229416,#229417),(#229418,#229419),(#229420,#229421),
(#229422,#229423),(#229424,#229425),(#229426,#229427),(#229428,#229429),
(#229430,#229431),(#229432,#229433),(#229434,#229435),(#229436,#229437),
(#229438,#229439),(#229440,#229441),(#229442,#229443),(#229444,#229445),
(#229446,#229447),(#229448,#229449),(#229450,#229451),(#229452,#229453),
(#229454,#229455),(#229456,#229457),(#229458,#229459),(#229460,#229461),
(#229462,#229463),(#229464,#229465),(#229466,#229467),(#229468,#229469),
(#229470,#229471),(#229472,#229473),(#229474,#229475),(#229476,#229477),
(#229478,#229479),(#229480,#229481),(#229482,#229483),(#229484,#229485),
(#229486,#229487),(#229488,#229489),(#229490,#229491),(#229492,#229493),
(#229494,#229495),(#229496,#229497),(#229498,#229499),(#229500,#229501),
(#229502,#229503),(#229504,#229505),(#229506,#229507),(#229508,#229509),
(#229510,#229511),(#229512,#229513),(#229514,#229515),(#229516,#229517),
(#229518,#229519),(#229520,#229521),(#229522,#229523),(#229524,#229525),
(#229526,#229527),(#229528,#229529),(#229530,#229531),(#229532,#229533),
(#229534,#229535),(#229536,#229537),(#229538,#229539),(#229540,#229541),
(#229542,#229543),(#229544,#229545),(#229546,#229547),(#229548,#229549),
(#229550,#229551),(#229552,#229553),(#229554,#229555),(#229556,#229557),
(#229558,#229559),(#229560,#229561),(#229562,#229563),(#229564,#229565),
(#229566,#229567),(#229568,#229569),(#229570,#229571),(#229572,#229573),
(#229574,#229575),(#229576,#229577),(#229578,#229579),(#229580,#229581),
(#229582,#229583),(#229584,#229585),(#229586,#229587),(#229588,#229589),
(#229590,#229591),(#229592,#229593),(#229594,#229595),(#229596,#229597),
(#229598,#229599),(#229600,#229601),(#229602,#229603),(#229604,#229605),
(#229606,#229607),(#229608,#229609),(#229610,#229611),(#229612,#229613),
(#229614,#229615),(#229616,#229617),(#229618,#229619),(#229620,#229621),
(#229622,#229623),(#229624,#229625),(#229626,#229627),(#229628,#229629),
(#229630,#229631),(#229632,#229633)),.UNSPECIFIED.,.F.,.F.,.F.)
B_SPLINE_SURFACE_WITH_KNOTS((6,1,1,1,1,1,1,1,1,1,1,1,1,1,1,1,1,1,1,1,1,
1,1,1,1,1,1,1,1,1,1,1,1,1,1,1,1,1,1,1,1,1,1,1,1,1,1,1,1,1,1,1,1,1,1,1,1,
1,1,1,1,1,1,1,1,1,1,1,1,1,1,1,1,1,1,1,1,1,1,1,1,1,1,1,1,1,1,1,1,1,1,1,1,
1,1,1,1,1,1,1,1,1,1,1,1,1,1,1,1,1,1,1,1,1,1,1,1,1,1,1,1,1,1,1,1,1,1,1,1,
1,1,1,1,1,1,1,1,1,1,1,1,1,1,1,1,1,1,1,1,1,1,1,1,1,1,1,1,1,1,1,1,1,1,1,1,
1,1,1,1,1,1,1,1,1,1,1,1,1,1,1,1,1,1,1,1,1,1,1,1,1,1,1,1,1,1,1,1,1,1,1,6),
(2,2),(-1.,-0.995000000000001,-0.990000000000001,-0.985000000000001,-0.980000000000001,
-0.975000000000001,-0.970000000000001,-0.965000000000001,-0.960000000000001,
-0.955000000000001,-0.950000000000001,-0.945000000000001,-0.940000000000001,
-0.935000000000001,-0.930000000000001,-0.925000000000001,-0.920000000000001,
-0.915000000000001,-0.910000000000001,-0.905000000000001,-0.900000000000001,
-0.895000000000001,-0.890000000000001,-0.885000000000001,-0.880000000000001,
-0.875000000000001,-0.870000000000001,-0.865000000000001,-0.860000000000001,
-0.855000000000001,-0.850000000000001,-0.845000000000001,-0.840000000000001,
-0.835000000000001,-0.830000000000001,-0.825000000000001,-0.820000000000001,
-0.815000000000001,-0.810000000000001,-0.805000000000001,-0.800000000000001,
-0.795000000000001,-0.790000000000001,-0.785000000000001,-0.780000000000001,
-0.775000000000001,-0.770000000000001,-0.765000000000001,-0.760000000000001,
-0.755000000000001,-0.750000000000001,-0.745000000000001,-0.740000000000001,
-0.735000000000001,-0.730000000000001,-0.725000000000001,-0.720000000000001,
-0.715000000000001,-0.710000000000001,-0.705000000000001,-0.700000000000001,
-0.695000000000001,-0.690000000000001,-0.685,-0.68,-0.675,-0.67,-0.665,
-0.66,-0.655,-0.65,-0.645,-0.64,-0.635,-0.63,-0.625,-0.62,-0.615,-0.61,
-0.605,-0.6,-0.595,-0.59,-0.585,-0.58,-0.575,-0.57,-0.565,-0.56,-0.555,
-0.55,-0.545,-0.54,-0.535,-0.53,-0.525,-0.52,-0.515,-0.51,-0.505,-0.5,-0.495,
-0.49,-0.485,-0.48,-0.475,-0.47,-0.465,-0.46,-0.455,-0.45,-0.445,-0.44,
-0.435,-0.43,-0.425,-0.42,-0.415,-0.41,-0.405,-0.4,-0.395,-0.39,-0.385,
-0.38,-0.375,-0.37,-0.365,-0.36,-0.355,-0.35,-0.345,-0.34,-0.335,-0.33,
-0.325,-0.32,-0.315,-0.31,-0.305,-0.3,-0.295,-0.29,-0.285,-0.28,-0.275,
-0.27,-0.265,-0.26,-0.255,-0.25,-0.245,-0.24,-0.235,-0.23,-0.225,-0.22,
-0.215,-0.21,-0.205,-0.2,-0.195,-0.19,-0.185,-0.18,-0.175,-0.17,-0.165,
-0.16,-0.155,-0.15,-0.145,-0.14,-0.135,-0.13,-0.125,-0.12,-0.115,-0.11,
-0.105,-0.1,-0.095,-0.09,-0.085,-0.08,-0.075,-0.07,-0.065,-0.06,-0.055,
-0.05,-0.045,-0.04,-0.035,-0.03,-0.025,-0.02,-0.015,-0.01,-0.005,0.),(0.,
1.2),.UNSPECIFIED.)
GEOMETRIC_REPRESENTATION_ITEM()
RATIONAL_B_SPLINE_SURFACE(((1.,1.),(1.,1.),(1.,1.),(1.,1.),(1.,1.),(1.,
1.),(1.,1.),(1.,1.),(1.,1.),(1.,1.),(1.,1.),(1.,1.),(1.,1.),(1.,1.),(1.,
1.),(1.,1.),(1.,1.),(1.,1.),(1.,1.),(1.,1.),(1.,1.),(1.,1.),(1.,1.),(1.,
1.),(1.,1.),(1.,1.),(1.,1.),(1.,1.),(1.,1.),(1.,1.),(1.,1.),(1.,1.),(1.,
1.),(1.,1.),(1.,1.),(1.,1.),(1.,1.),(1.,1.),(1.,1.),(1.,1.),(1.,1.),(1.,
1.),(1.,1.),(1.,1.),(1.,1.),(1.,1.),(1.,1.),(1.,1.),(1.,1.),(1.,1.),(1.,
1.),(1.,1.),(1.,1.),(1.,1.),(1.,1.),(1.,1.),(1.,1.),(1.,1.),(1.,1.),(1.,
1.),(1.,1.),(1.,1.),(1.,1.),(1.,1.),(1.,1.),(1.,1.),(1.,1.),(1.,1.),(1.,
1.),(1.,1.),(1.,1.),(1.,1.),(1.,1.),(1.,1.),(1.,1.),(1.,1.),(1.,1.),(1.,
1.),(1.,1.),(1.,1.),(1.,1.),(1.,1.),(1.,1.),(1.,1.),(1.,1.),(1.,1.),(1.,
1.),(1.,1.),(1.,1.),(1.,1.),(1.,1.),(1.,1.),(1.,1.),(1.,1.),(1.,1.),(1.,
1.),(1.,1.),(1.,1.),(1.,1.),(1.,1.),(1.,1.),(1.,1.),(1.,1.),(1.,1.),(1.,
1.),(1.,1.),(1.,1.),(1.,1.),(1.,1.),(1.,1.),(1.,1.),(1.,1.),(1.,1.),(1.,
1.),(1.,1.),(1.,1.),(1.,1.),(1.,1.),(1.,1.),(1.,1.),(1.,1.),(1.,1.),(1.,
1.),(1.,1.),(1.,1.),(1.,1.),(1.,1.),(1.,1.),(1.,1.),(1.,1.),(1.,1.),(1.,
1.),(1.,1.),(1.,1.),(1.,1.),(1.,1.),(1.,1.),(1.,1.),(1.,1.),(1.,1.),(1.,
1.),(1.,1.),(1.,1.),(1.,1.),(1.,1.),(1.,1.),(1.,1.),(1.,1.),(1.,1.),(1.,
1.),(1.,1.),(1.,1.),(1.,1.),(1.,1.),(1.,1.),(1.,1.),(1.,1.),(1.,1.),(1.,
1.),(1.,1.),(1.,1.),(1.,1.),(1.,1.),(1.,1.),(1.,1.),(1.,1.),(1.,1.),(1.,
1.),(1.,1.),(1.,1.),(1.,1.),(1.,1.),(1.,1.),(1.,1.),(1.,1.),(1.,1.),(1.,
1.),(1.,1.),(1.,1.),(1.,1.),(1.,1.),(1.,1.),(1.,1.),(1.,1.),(1.,1.),(1.,
1.),(1.,1.),(1.,1.),(1.,1.),(1.,1.),(1.,1.),(1.,1.),(1.,1.),(1.,1.),(1.,
1.),(1.,1.),(1.,1.),(1.,1.),(1.,1.),(1.,1.),(1.,1.),(1.,1.),(1.,1.),(1.,
1.),(1.,1.)))
REPRESENTATION_ITEM('')
SURFACE()
);
#1092=(
BOUNDED_SURFACE()
B_SPLINE_SURFACE(5,1,((#230047,#230048),(#230049,#230050),(#230051,#230052),
(#230053,#230054),(#230055,#230056),(#230057,#230058),(#230059,#230060),
(#230061,#230062),(#230063,#230064),(#230065,#230066),(#230067,#230068),
(#230069,#230070),(#230071,#230072),(#230073,#230074),(#230075,#230076),
(#230077,#230078),(#230079,#230080),(#230081,#230082),(#230083,#230084),
(#230085,#230086),(#230087,#230088),(#230089,#230090),(#230091,#230092),
(#230093,#230094),(#230095,#230096),(#230097,#230098),(#230099,#230100),
(#230101,#230102),(#230103,#230104),(#230105,#230106),(#230107,#230108),
(#230109,#230110),(#230111,#230112),(#230113,#230114),(#230115,#230116),
(#230117,#230118),(#230119,#230120),(#230121,#230122),(#230123,#230124),
(#230125,#230126),(#230127,#230128),(#230129,#230130),(#230131,#230132),
(#230133,#230134),(#230135,#230136),(#230137,#230138),(#230139,#230140),
(#230141,#230142),(#230143,#230144),(#230145,#230146),(#230147,#230148),
(#230149,#230150),(#230151,#230152),(#230153,#230154),(#230155,#230156),
(#230157,#230158),(#230159,#230160),(#230161,#230162),(#230163,#230164),
(#230165,#230166),(#230167,#230168),(#230169,#230170),(#230171,#230172),
(#230173,#230174),(#230175,#230176),(#230177,#230178),(#230179,#230180),
(#230181,#230182),(#230183,#230184),(#230185,#230186),(#230187,#230188),
(#230189,#230190),(#230191,#230192),(#230193,#230194),(#230195,#230196),
(#230197,#230198),(#230199,#230200),(#230201,#230202),(#230203,#230204),
(#230205,#230206),(#230207,#230208),(#230209,#230210),(#230211,#230212),
(#230213,#230214),(#230215,#230216),(#230217,#230218),(#230219,#230220),
(#230221,#230222),(#230223,#230224),(#230225,#230226),(#230227,#230228),
(#230229,#230230),(#230231,#230232),(#230233,#230234),(#230235,#230236),
(#230237,#230238),(#230239,#230240),(#230241,#230242),(#230243,#230244),
(#230245,#230246),(#230247,#230248),(#230249,#230250),(#230251,#230252),
(#230253,#230254),(#230255,#230256),(#230257,#230258),(#230259,#230260),
(#230261,#230262),(#230263,#230264),(#230265,#230266),(#230267,#230268),
(#230269,#230270),(#230271,#230272),(#230273,#230274),(#230275,#230276),
(#230277,#230278),(#230279,#230280),(#230281,#230282),(#230283,#230284),
(#230285,#230286),(#230287,#230288),(#230289,#230290),(#230291,#230292),
(#230293,#230294),(#230295,#230296),(#230297,#230298),(#230299,#230300),
(#230301,#230302),(#230303,#230304),(#230305,#230306),(#230307,#230308),
(#230309,#230310),(#230311,#230312),(#230313,#230314),(#230315,#230316),
(#230317,#230318),(#230319,#230320),(#230321,#230322),(#230323,#230324),
(#230325,#230326),(#230327,#230328),(#230329,#230330),(#230331,#230332),
(#230333,#230334),(#230335,#230336),(#230337,#230338),(#230339,#230340),
(#230341,#230342),(#230343,#230344),(#230345,#230346),(#230347,#230348),
(#230349,#230350),(#230351,#230352),(#230353,#230354),(#230355,#230356),
(#230357,#230358),(#230359,#230360),(#230361,#230362),(#230363,#230364),
(#230365,#230366),(#230367,#230368),(#230369,#230370),(#230371,#230372),
(#230373,#230374),(#230375,#230376),(#230377,#230378),(#230379,#230380),
(#230381,#230382),(#230383,#230384),(#230385,#230386),(#230387,#230388),
(#230389,#230390),(#230391,#230392),(#230393,#230394),(#230395,#230396),
(#230397,#230398),(#230399,#230400),(#230401,#230402),(#230403,#230404),
(#230405,#230406),(#230407,#230408),(#230409,#230410),(#230411,#230412),
(#230413,#230414),(#230415,#230416),(#230417,#230418),(#230419,#230420),
(#230421,#230422),(#230423,#230424),(#230425,#230426),(#230427,#230428),
(#230429,#230430),(#230431,#230432),(#230433,#230434),(#230435,#230436),
(#230437,#230438),(#230439,#230440),(#230441,#230442),(#230443,#230444),
(#230445,#230446),(#230447,#230448),(#230449,#230450),(#230451,#230452),
(#230453,#230454),(#230455,#230456)),.UNSPECIFIED.,.F.,.F.,.F.)
B_SPLINE_SURFACE_WITH_KNOTS((6,1,1,1,1,1,1,1,1,1,1,1,1,1,1,1,1,1,1,1,1,
1,1,1,1,1,1,1,1,1,1,1,1,1,1,1,1,1,1,1,1,1,1,1,1,1,1,1,1,1,1,1,1,1,1,1,1,
1,1,1,1,1,1,1,1,1,1,1,1,1,1,1,1,1,1,1,1,1,1,1,1,1,1,1,1,1,1,1,1,1,1,1,1,
1,1,1,1,1,1,1,1,1,1,1,1,1,1,1,1,1,1,1,1,1,1,1,1,1,1,1,1,1,1,1,1,1,1,1,1,
1,1,1,1,1,1,1,1,1,1,1,1,1,1,1,1,1,1,1,1,1,1,1,1,1,1,1,1,1,1,1,1,1,1,1,1,
1,1,1,1,1,1,1,1,1,1,1,1,1,1,1,1,1,1,1,1,1,1,1,1,1,1,1,1,1,1,1,1,1,1,1,6),
(2,2),(0.,0.005,0.01,0.015,0.02,0.025,0.03,0.035,0.04,0.045,0.05,0.055,
0.06,0.065,0.07,0.075,0.08,0.085,0.09,0.095,0.1,0.105,0.11,0.115,0.12,0.125,
0.13,0.135,0.14,0.145,0.15,0.155,0.16,0.165,0.17,0.175,0.18,0.185,0.19,
0.195,0.2,0.205,0.21,0.215,0.22,0.225,0.23,0.235,0.24,0.245,0.25,0.255,
0.26,0.265,0.27,0.275,0.28,0.285,0.29,0.295,0.3,0.305,0.31,0.315,0.32,0.325,
0.33,0.335,0.34,0.345,0.35,0.355,0.36,0.365,0.37,0.375,0.38,0.385,0.39,
0.395,0.4,0.405,0.41,0.415,0.42,0.425,0.43,0.435,0.44,0.445,0.45,0.455,
0.46,0.465,0.47,0.475,0.48,0.485,0.49,0.495,0.5,0.505,0.51,0.515,0.52,0.525,
0.53,0.535,0.54,0.545,0.55,0.555,0.56,0.565,0.57,0.575,0.58,0.585,0.59,
0.595,0.6,0.605,0.61,0.615,0.62,0.625,0.63,0.635,0.64,0.645,0.65,0.655,
0.66,0.665,0.67,0.675,0.68,0.685,0.690000000000001,0.695000000000001,0.700000000000001,
0.705000000000001,0.710000000000001,0.715000000000001,0.720000000000001,
0.725000000000001,0.730000000000001,0.735000000000001,0.740000000000001,
0.745000000000001,0.750000000000001,0.755000000000001,0.760000000000001,
0.765000000000001,0.770000000000001,0.775000000000001,0.780000000000001,
0.785000000000001,0.790000000000001,0.795000000000001,0.800000000000001,
0.805000000000001,0.810000000000001,0.815000000000001,0.820000000000001,
0.825000000000001,0.830000000000001,0.835000000000001,0.840000000000001,
0.845000000000001,0.850000000000001,0.855000000000001,0.860000000000001,
0.865000000000001,0.870000000000001,0.875000000000001,0.880000000000001,
0.885000000000001,0.890000000000001,0.895000000000001,0.900000000000001,
0.905000000000001,0.910000000000001,0.915000000000001,0.920000000000001,
0.925000000000001,0.930000000000001,0.935000000000001,0.940000000000001,
0.945000000000001,0.950000000000001,0.955000000000001,0.960000000000001,
0.965000000000001,0.970000000000001,0.975000000000001,0.980000000000001,
0.985000000000001,0.990000000000001,0.995000000000001,1.),(0.,1.2),
 .UNSPECIFIED.)
GEOMETRIC_REPRESENTATION_ITEM()
RATIONAL_B_SPLINE_SURFACE(((1.,1.),(1.,1.),(1.,1.),(1.,1.),(1.,1.),(1.,
1.),(1.,1.),(1.,1.),(1.,1.),(1.,1.),(1.,1.),(1.,1.),(1.,1.),(1.,1.),(1.,
1.),(1.,1.),(1.,1.),(1.,1.),(1.,1.),(1.,1.),(1.,1.),(1.,1.),(1.,1.),(1.,
1.),(1.,1.),(1.,1.),(1.,1.),(1.,1.),(1.,1.),(1.,1.),(1.,1.),(1.,1.),(1.,
1.),(1.,1.),(1.,1.),(1.,1.),(1.,1.),(1.,1.),(1.,1.),(1.,1.),(1.,1.),(1.,
1.),(1.,1.),(1.,1.),(1.,1.),(1.,1.),(1.,1.),(1.,1.),(1.,1.),(1.,1.),(1.,
1.),(1.,1.),(1.,1.),(1.,1.),(1.,1.),(1.,1.),(1.,1.),(1.,1.),(1.,1.),(1.,
1.),(1.,1.),(1.,1.),(1.,1.),(1.,1.),(1.,1.),(1.,1.),(1.,1.),(1.,1.),(1.,
1.),(1.,1.),(1.,1.),(1.,1.),(1.,1.),(1.,1.),(1.,1.),(1.,1.),(1.,1.),(1.,
1.),(1.,1.),(1.,1.),(1.,1.),(1.,1.),(1.,1.),(1.,1.),(1.,1.),(1.,1.),(1.,
1.),(1.,1.),(1.,1.),(1.,1.),(1.,1.),(1.,1.),(1.,1.),(1.,1.),(1.,1.),(1.,
1.),(1.,1.),(1.,1.),(1.,1.),(1.,1.),(1.,1.),(1.,1.),(1.,1.),(1.,1.),(1.,
1.),(1.,1.),(1.,1.),(1.,1.),(1.,1.),(1.,1.),(1.,1.),(1.,1.),(1.,1.),(1.,
1.),(1.,1.),(1.,1.),(1.,1.),(1.,1.),(1.,1.),(1.,1.),(1.,1.),(1.,1.),(1.,
1.),(1.,1.),(1.,1.),(1.,1.),(1.,1.),(1.,1.),(1.,1.),(1.,1.),(1.,1.),(1.,
1.),(1.,1.),(1.,1.),(1.,1.),(1.,1.),(1.,1.),(1.,1.),(1.,1.),(1.,1.),(1.,
1.),(1.,1.),(1.,1.),(1.,1.),(1.,1.),(1.,1.),(1.,1.),(1.,1.),(1.,1.),(1.,
1.),(1.,1.),(1.,1.),(1.,1.),(1.,1.),(1.,1.),(1.,1.),(1.,1.),(1.,1.),(1.,
1.),(1.,1.),(1.,1.),(1.,1.),(1.,1.),(1.,1.),(1.,1.),(1.,1.),(1.,1.),(1.,
1.),(1.,1.),(1.,1.),(1.,1.),(1.,1.),(1.,1.),(1.,1.),(1.,1.),(1.,1.),(1.,
1.),(1.,1.),(1.,1.),(1.,1.),(1.,1.),(1.,1.),(1.,1.),(1.,1.),(1.,1.),(1.,
1.),(1.,1.),(1.,1.),(1.,1.),(1.,1.),(1.,1.),(1.,1.),(1.,1.),(1.,1.),(1.,
1.),(1.,1.),(1.,1.),(1.,1.),(1.,1.),(1.,1.),(1.,1.),(1.,1.),(1.,1.),(1.,
1.),(1.,1.)))
REPRESENTATION_ITEM('')
SURFACE()
);
#1093=(
BOUNDED_SURFACE()
B_SPLINE_SURFACE(5,1,((#230876,#230877),(#230878,#230879),(#230880,#230881),
(#230882,#230883),(#230884,#230885),(#230886,#230887),(#230888,#230889),
(#230890,#230891),(#230892,#230893),(#230894,#230895),(#230896,#230897),
(#230898,#230899),(#230900,#230901),(#230902,#230903),(#230904,#230905),
(#230906,#230907),(#230908,#230909),(#230910,#230911),(#230912,#230913),
(#230914,#230915),(#230916,#230917),(#230918,#230919),(#230920,#230921),
(#230922,#230923),(#230924,#230925),(#230926,#230927),(#230928,#230929),
(#230930,#230931),(#230932,#230933),(#230934,#230935),(#230936,#230937),
(#230938,#230939),(#230940,#230941),(#230942,#230943),(#230944,#230945),
(#230946,#230947),(#230948,#230949),(#230950,#230951),(#230952,#230953),
(#230954,#230955),(#230956,#230957),(#230958,#230959),(#230960,#230961),
(#230962,#230963),(#230964,#230965),(#230966,#230967),(#230968,#230969),
(#230970,#230971),(#230972,#230973),(#230974,#230975),(#230976,#230977),
(#230978,#230979),(#230980,#230981),(#230982,#230983),(#230984,#230985),
(#230986,#230987),(#230988,#230989),(#230990,#230991),(#230992,#230993),
(#230994,#230995),(#230996,#230997),(#230998,#230999),(#231000,#231001),
(#231002,#231003),(#231004,#231005),(#231006,#231007),(#231008,#231009),
(#231010,#231011),(#231012,#231013),(#231014,#231015),(#231016,#231017),
(#231018,#231019),(#231020,#231021),(#231022,#231023),(#231024,#231025),
(#231026,#231027),(#231028,#231029),(#231030,#231031),(#231032,#231033),
(#231034,#231035),(#231036,#231037),(#231038,#231039),(#231040,#231041),
(#231042,#231043),(#231044,#231045),(#231046,#231047),(#231048,#231049),
(#231050,#231051),(#231052,#231053),(#231054,#231055),(#231056,#231057),
(#231058,#231059),(#231060,#231061),(#231062,#231063),(#231064,#231065),
(#231066,#231067),(#231068,#231069),(#231070,#231071),(#231072,#231073),
(#231074,#231075),(#231076,#231077),(#231078,#231079),(#231080,#231081),
(#231082,#231083),(#231084,#231085),(#231086,#231087),(#231088,#231089),
(#231090,#231091),(#231092,#231093),(#231094,#231095),(#231096,#231097),
(#231098,#231099),(#231100,#231101),(#231102,#231103),(#231104,#231105),
(#231106,#231107),(#231108,#231109),(#231110,#231111),(#231112,#231113),
(#231114,#231115),(#231116,#231117),(#231118,#231119),(#231120,#231121),
(#231122,#231123),(#231124,#231125),(#231126,#231127),(#231128,#231129),
(#231130,#231131),(#231132,#231133),(#231134,#231135),(#231136,#231137),
(#231138,#231139),(#231140,#231141),(#231142,#231143),(#231144,#231145),
(#231146,#231147),(#231148,#231149),(#231150,#231151),(#231152,#231153),
(#231154,#231155),(#231156,#231157),(#231158,#231159),(#231160,#231161),
(#231162,#231163),(#231164,#231165),(#231166,#231167),(#231168,#231169),
(#231170,#231171),(#231172,#231173),(#231174,#231175),(#231176,#231177),
(#231178,#231179),(#231180,#231181),(#231182,#231183),(#231184,#231185),
(#231186,#231187),(#231188,#231189),(#231190,#231191),(#231192,#231193),
(#231194,#231195),(#231196,#231197),(#231198,#231199),(#231200,#231201),
(#231202,#231203),(#231204,#231205),(#231206,#231207),(#231208,#231209),
(#231210,#231211),(#231212,#231213),(#231214,#231215),(#231216,#231217),
(#231218,#231219),(#231220,#231221),(#231222,#231223),(#231224,#231225),
(#231226,#231227),(#231228,#231229),(#231230,#231231),(#231232,#231233),
(#231234,#231235),(#231236,#231237),(#231238,#231239),(#231240,#231241),
(#231242,#231243),(#231244,#231245),(#231246,#231247),(#231248,#231249),
(#231250,#231251),(#231252,#231253),(#231254,#231255),(#231256,#231257),
(#231258,#231259),(#231260,#231261),(#231262,#231263),(#231264,#231265),
(#231266,#231267),(#231268,#231269),(#231270,#231271),(#231272,#231273),
(#231274,#231275),(#231276,#231277),(#231278,#231279),(#231280,#231281),
(#231282,#231283),(#231284,#231285)),.UNSPECIFIED.,.F.,.F.,.F.)
B_SPLINE_SURFACE_WITH_KNOTS((6,1,1,1,1,1,1,1,1,1,1,1,1,1,1,1,1,1,1,1,1,
1,1,1,1,1,1,1,1,1,1,1,1,1,1,1,1,1,1,1,1,1,1,1,1,1,1,1,1,1,1,1,1,1,1,1,1,
1,1,1,1,1,1,1,1,1,1,1,1,1,1,1,1,1,1,1,1,1,1,1,1,1,1,1,1,1,1,1,1,1,1,1,1,
1,1,1,1,1,1,1,1,1,1,1,1,1,1,1,1,1,1,1,1,1,1,1,1,1,1,1,1,1,1,1,1,1,1,1,1,
1,1,1,1,1,1,1,1,1,1,1,1,1,1,1,1,1,1,1,1,1,1,1,1,1,1,1,1,1,1,1,1,1,1,1,1,
1,1,1,1,1,1,1,1,1,1,1,1,1,1,1,1,1,1,1,1,1,1,1,1,1,1,1,1,1,1,1,1,1,1,1,6),
(2,2),(-1.,-0.995000000000001,-0.990000000000001,-0.985000000000001,-0.980000000000001,
-0.975000000000001,-0.970000000000001,-0.965000000000001,-0.960000000000001,
-0.955000000000001,-0.950000000000001,-0.945000000000001,-0.940000000000001,
-0.935000000000001,-0.930000000000001,-0.925000000000001,-0.920000000000001,
-0.915000000000001,-0.910000000000001,-0.905000000000001,-0.900000000000001,
-0.895000000000001,-0.890000000000001,-0.885000000000001,-0.880000000000001,
-0.875000000000001,-0.870000000000001,-0.865000000000001,-0.860000000000001,
-0.855000000000001,-0.850000000000001,-0.845000000000001,-0.840000000000001,
-0.835000000000001,-0.830000000000001,-0.825000000000001,-0.820000000000001,
-0.815000000000001,-0.810000000000001,-0.805000000000001,-0.800000000000001,
-0.795000000000001,-0.790000000000001,-0.785000000000001,-0.780000000000001,
-0.775000000000001,-0.770000000000001,-0.765000000000001,-0.760000000000001,
-0.755000000000001,-0.750000000000001,-0.745000000000001,-0.740000000000001,
-0.735000000000001,-0.730000000000001,-0.725000000000001,-0.720000000000001,
-0.715000000000001,-0.710000000000001,-0.705000000000001,-0.700000000000001,
-0.695000000000001,-0.690000000000001,-0.685,-0.68,-0.675,-0.67,-0.665,
-0.66,-0.655,-0.65,-0.645,-0.64,-0.635,-0.63,-0.625,-0.62,-0.615,-0.61,
-0.605,-0.6,-0.595,-0.59,-0.585,-0.58,-0.575,-0.57,-0.565,-0.56,-0.555,
-0.55,-0.545,-0.54,-0.535,-0.53,-0.525,-0.52,-0.515,-0.51,-0.505,-0.5,-0.495,
-0.49,-0.485,-0.48,-0.475,-0.47,-0.465,-0.46,-0.455,-0.45,-0.445,-0.44,
-0.435,-0.43,-0.425,-0.42,-0.415,-0.41,-0.405,-0.4,-0.395,-0.39,-0.385,
-0.38,-0.375,-0.37,-0.365,-0.36,-0.355,-0.35,-0.345,-0.34,-0.335,-0.33,
-0.325,-0.32,-0.315,-0.31,-0.305,-0.3,-0.295,-0.29,-0.285,-0.28,-0.275,
-0.27,-0.265,-0.26,-0.255,-0.25,-0.245,-0.24,-0.235,-0.23,-0.225,-0.22,
-0.215,-0.21,-0.205,-0.2,-0.195,-0.19,-0.185,-0.18,-0.175,-0.17,-0.165,
-0.16,-0.155,-0.15,-0.145,-0.14,-0.135,-0.13,-0.125,-0.12,-0.115,-0.11,
-0.105,-0.1,-0.095,-0.09,-0.085,-0.08,-0.075,-0.07,-0.065,-0.06,-0.055,
-0.05,-0.045,-0.04,-0.035,-0.03,-0.025,-0.02,-0.015,-0.01,-0.005,0.),(0.,
1.2),.UNSPECIFIED.)
GEOMETRIC_REPRESENTATION_ITEM()
RATIONAL_B_SPLINE_SURFACE(((1.,1.),(1.,1.),(1.,1.),(1.,1.),(1.,1.),(1.,
1.),(1.,1.),(1.,1.),(1.,1.),(1.,1.),(1.,1.),(1.,1.),(1.,1.),(1.,1.),(1.,
1.),(1.,1.),(1.,1.),(1.,1.),(1.,1.),(1.,1.),(1.,1.),(1.,1.),(1.,1.),(1.,
1.),(1.,1.),(1.,1.),(1.,1.),(1.,1.),(1.,1.),(1.,1.),(1.,1.),(1.,1.),(1.,
1.),(1.,1.),(1.,1.),(1.,1.),(1.,1.),(1.,1.),(1.,1.),(1.,1.),(1.,1.),(1.,
1.),(1.,1.),(1.,1.),(1.,1.),(1.,1.),(1.,1.),(1.,1.),(1.,1.),(1.,1.),(1.,
1.),(1.,1.),(1.,1.),(1.,1.),(1.,1.),(1.,1.),(1.,1.),(1.,1.),(1.,1.),(1.,
1.),(1.,1.),(1.,1.),(1.,1.),(1.,1.),(1.,1.),(1.,1.),(1.,1.),(1.,1.),(1.,
1.),(1.,1.),(1.,1.),(1.,1.),(1.,1.),(1.,1.),(1.,1.),(1.,1.),(1.,1.),(1.,
1.),(1.,1.),(1.,1.),(1.,1.),(1.,1.),(1.,1.),(1.,1.),(1.,1.),(1.,1.),(1.,
1.),(1.,1.),(1.,1.),(1.,1.),(1.,1.),(1.,1.),(1.,1.),(1.,1.),(1.,1.),(1.,
1.),(1.,1.),(1.,1.),(1.,1.),(1.,1.),(1.,1.),(1.,1.),(1.,1.),(1.,1.),(1.,
1.),(1.,1.),(1.,1.),(1.,1.),(1.,1.),(1.,1.),(1.,1.),(1.,1.),(1.,1.),(1.,
1.),(1.,1.),(1.,1.),(1.,1.),(1.,1.),(1.,1.),(1.,1.),(1.,1.),(1.,1.),(1.,
1.),(1.,1.),(1.,1.),(1.,1.),(1.,1.),(1.,1.),(1.,1.),(1.,1.),(1.,1.),(1.,
1.),(1.,1.),(1.,1.),(1.,1.),(1.,1.),(1.,1.),(1.,1.),(1.,1.),(1.,1.),(1.,
1.),(1.,1.),(1.,1.),(1.,1.),(1.,1.),(1.,1.),(1.,1.),(1.,1.),(1.,1.),(1.,
1.),(1.,1.),(1.,1.),(1.,1.),(1.,1.),(1.,1.),(1.,1.),(1.,1.),(1.,1.),(1.,
1.),(1.,1.),(1.,1.),(1.,1.),(1.,1.),(1.,1.),(1.,1.),(1.,1.),(1.,1.),(1.,
1.),(1.,1.),(1.,1.),(1.,1.),(1.,1.),(1.,1.),(1.,1.),(1.,1.),(1.,1.),(1.,
1.),(1.,1.),(1.,1.),(1.,1.),(1.,1.),(1.,1.),(1.,1.),(1.,1.),(1.,1.),(1.,
1.),(1.,1.),(1.,1.),(1.,1.),(1.,1.),(1.,1.),(1.,1.),(1.,1.),(1.,1.),(1.,
1.),(1.,1.),(1.,1.),(1.,1.),(1.,1.),(1.,1.),(1.,1.),(1.,1.),(1.,1.),(1.,
1.),(1.,1.)))
REPRESENTATION_ITEM('')
SURFACE()
);
#1094=(
BOUNDED_SURFACE()
B_SPLINE_SURFACE(5,1,((#231699,#231700),(#231701,#231702),(#231703,#231704),
(#231705,#231706),(#231707,#231708),(#231709,#231710),(#231711,#231712),
(#231713,#231714),(#231715,#231716),(#231717,#231718),(#231719,#231720),
(#231721,#231722),(#231723,#231724),(#231725,#231726),(#231727,#231728),
(#231729,#231730),(#231731,#231732),(#231733,#231734),(#231735,#231736),
(#231737,#231738),(#231739,#231740),(#231741,#231742),(#231743,#231744),
(#231745,#231746),(#231747,#231748),(#231749,#231750),(#231751,#231752),
(#231753,#231754),(#231755,#231756),(#231757,#231758),(#231759,#231760),
(#231761,#231762),(#231763,#231764),(#231765,#231766),(#231767,#231768),
(#231769,#231770),(#231771,#231772),(#231773,#231774),(#231775,#231776),
(#231777,#231778),(#231779,#231780),(#231781,#231782),(#231783,#231784),
(#231785,#231786),(#231787,#231788),(#231789,#231790),(#231791,#231792),
(#231793,#231794),(#231795,#231796),(#231797,#231798),(#231799,#231800),
(#231801,#231802),(#231803,#231804),(#231805,#231806),(#231807,#231808),
(#231809,#231810),(#231811,#231812),(#231813,#231814),(#231815,#231816),
(#231817,#231818),(#231819,#231820),(#231821,#231822),(#231823,#231824),
(#231825,#231826),(#231827,#231828),(#231829,#231830),(#231831,#231832),
(#231833,#231834),(#231835,#231836),(#231837,#231838),(#231839,#231840),
(#231841,#231842),(#231843,#231844),(#231845,#231846),(#231847,#231848),
(#231849,#231850),(#231851,#231852),(#231853,#231854),(#231855,#231856),
(#231857,#231858),(#231859,#231860),(#231861,#231862),(#231863,#231864),
(#231865,#231866),(#231867,#231868),(#231869,#231870),(#231871,#231872),
(#231873,#231874),(#231875,#231876),(#231877,#231878),(#231879,#231880),
(#231881,#231882),(#231883,#231884),(#231885,#231886),(#231887,#231888),
(#231889,#231890),(#231891,#231892),(#231893,#231894),(#231895,#231896),
(#231897,#231898),(#231899,#231900),(#231901,#231902),(#231903,#231904),
(#231905,#231906),(#231907,#231908),(#231909,#231910),(#231911,#231912),
(#231913,#231914),(#231915,#231916),(#231917,#231918),(#231919,#231920),
(#231921,#231922),(#231923,#231924),(#231925,#231926),(#231927,#231928),
(#231929,#231930),(#231931,#231932),(#231933,#231934),(#231935,#231936),
(#231937,#231938),(#231939,#231940),(#231941,#231942),(#231943,#231944),
(#231945,#231946),(#231947,#231948),(#231949,#231950),(#231951,#231952),
(#231953,#231954),(#231955,#231956),(#231957,#231958),(#231959,#231960),
(#231961,#231962),(#231963,#231964),(#231965,#231966),(#231967,#231968),
(#231969,#231970),(#231971,#231972),(#231973,#231974),(#231975,#231976),
(#231977,#231978),(#231979,#231980),(#231981,#231982),(#231983,#231984),
(#231985,#231986),(#231987,#231988),(#231989,#231990),(#231991,#231992),
(#231993,#231994),(#231995,#231996),(#231997,#231998),(#231999,#232000),
(#232001,#232002),(#232003,#232004),(#232005,#232006),(#232007,#232008),
(#232009,#232010),(#232011,#232012),(#232013,#232014),(#232015,#232016),
(#232017,#232018),(#232019,#232020),(#232021,#232022),(#232023,#232024),
(#232025,#232026),(#232027,#232028),(#232029,#232030),(#232031,#232032),
(#232033,#232034),(#232035,#232036),(#232037,#232038),(#232039,#232040),
(#232041,#232042),(#232043,#232044),(#232045,#232046),(#232047,#232048),
(#232049,#232050),(#232051,#232052),(#232053,#232054),(#232055,#232056),
(#232057,#232058),(#232059,#232060),(#232061,#232062),(#232063,#232064),
(#232065,#232066),(#232067,#232068),(#232069,#232070),(#232071,#232072),
(#232073,#232074),(#232075,#232076),(#232077,#232078),(#232079,#232080),
(#232081,#232082),(#232083,#232084),(#232085,#232086),(#232087,#232088),
(#232089,#232090),(#232091,#232092),(#232093,#232094),(#232095,#232096),
(#232097,#232098),(#232099,#232100),(#232101,#232102),(#232103,#232104),
(#232105,#232106),(#232107,#232108)),.UNSPECIFIED.,.F.,.F.,.F.)
B_SPLINE_SURFACE_WITH_KNOTS((6,1,1,1,1,1,1,1,1,1,1,1,1,1,1,1,1,1,1,1,1,
1,1,1,1,1,1,1,1,1,1,1,1,1,1,1,1,1,1,1,1,1,1,1,1,1,1,1,1,1,1,1,1,1,1,1,1,
1,1,1,1,1,1,1,1,1,1,1,1,1,1,1,1,1,1,1,1,1,1,1,1,1,1,1,1,1,1,1,1,1,1,1,1,
1,1,1,1,1,1,1,1,1,1,1,1,1,1,1,1,1,1,1,1,1,1,1,1,1,1,1,1,1,1,1,1,1,1,1,1,
1,1,1,1,1,1,1,1,1,1,1,1,1,1,1,1,1,1,1,1,1,1,1,1,1,1,1,1,1,1,1,1,1,1,1,1,
1,1,1,1,1,1,1,1,1,1,1,1,1,1,1,1,1,1,1,1,1,1,1,1,1,1,1,1,1,1,1,1,1,1,1,6),
(2,2),(0.,0.005,0.01,0.015,0.02,0.025,0.03,0.035,0.04,0.045,0.05,0.055,
0.06,0.065,0.07,0.075,0.08,0.085,0.09,0.095,0.1,0.105,0.11,0.115,0.12,0.125,
0.13,0.135,0.14,0.145,0.15,0.155,0.16,0.165,0.17,0.175,0.18,0.185,0.19,
0.195,0.2,0.205,0.21,0.215,0.22,0.225,0.23,0.235,0.24,0.245,0.25,0.255,
0.26,0.265,0.27,0.275,0.28,0.285,0.29,0.295,0.3,0.305,0.31,0.315,0.32,0.325,
0.33,0.335,0.34,0.345,0.35,0.355,0.36,0.365,0.37,0.375,0.38,0.385,0.39,
0.395,0.4,0.405,0.41,0.415,0.42,0.425,0.43,0.435,0.44,0.445,0.45,0.455,
0.46,0.465,0.47,0.475,0.48,0.485,0.49,0.495,0.5,0.505,0.51,0.515,0.52,0.525,
0.53,0.535,0.54,0.545,0.55,0.555,0.56,0.565,0.57,0.575,0.58,0.585,0.59,
0.595,0.6,0.605,0.61,0.615,0.62,0.625,0.63,0.635,0.64,0.645,0.65,0.655,
0.66,0.665,0.67,0.675,0.68,0.685,0.690000000000001,0.695000000000001,0.700000000000001,
0.705000000000001,0.710000000000001,0.715000000000001,0.720000000000001,
0.725000000000001,0.730000000000001,0.735000000000001,0.740000000000001,
0.745000000000001,0.750000000000001,0.755000000000001,0.760000000000001,
0.765000000000001,0.770000000000001,0.775000000000001,0.780000000000001,
0.785000000000001,0.790000000000001,0.795000000000001,0.800000000000001,
0.805000000000001,0.810000000000001,0.815000000000001,0.820000000000001,
0.825000000000001,0.830000000000001,0.835000000000001,0.840000000000001,
0.845000000000001,0.850000000000001,0.855000000000001,0.860000000000001,
0.865000000000001,0.870000000000001,0.875000000000001,0.880000000000001,
0.885000000000001,0.890000000000001,0.895000000000001,0.900000000000001,
0.905000000000001,0.910000000000001,0.915000000000001,0.920000000000001,
0.925000000000001,0.930000000000001,0.935000000000001,0.940000000000001,
0.945000000000001,0.950000000000001,0.955000000000001,0.960000000000001,
0.965000000000001,0.970000000000001,0.975000000000001,0.980000000000001,
0.985000000000001,0.990000000000001,0.995000000000001,1.),(0.,1.2),
 .UNSPECIFIED.)
GEOMETRIC_REPRESENTATION_ITEM()
RATIONAL_B_SPLINE_SURFACE(((1.,1.),(1.,1.),(1.,1.),(1.,1.),(1.,1.),(1.,
1.),(1.,1.),(1.,1.),(1.,1.),(1.,1.),(1.,1.),(1.,1.),(1.,1.),(1.,1.),(1.,
1.),(1.,1.),(1.,1.),(1.,1.),(1.,1.),(1.,1.),(1.,1.),(1.,1.),(1.,1.),(1.,
1.),(1.,1.),(1.,1.),(1.,1.),(1.,1.),(1.,1.),(1.,1.),(1.,1.),(1.,1.),(1.,
1.),(1.,1.),(1.,1.),(1.,1.),(1.,1.),(1.,1.),(1.,1.),(1.,1.),(1.,1.),(1.,
1.),(1.,1.),(1.,1.),(1.,1.),(1.,1.),(1.,1.),(1.,1.),(1.,1.),(1.,1.),(1.,
1.),(1.,1.),(1.,1.),(1.,1.),(1.,1.),(1.,1.),(1.,1.),(1.,1.),(1.,1.),(1.,
1.),(1.,1.),(1.,1.),(1.,1.),(1.,1.),(1.,1.),(1.,1.),(1.,1.),(1.,1.),(1.,
1.),(1.,1.),(1.,1.),(1.,1.),(1.,1.),(1.,1.),(1.,1.),(1.,1.),(1.,1.),(1.,
1.),(1.,1.),(1.,1.),(1.,1.),(1.,1.),(1.,1.),(1.,1.),(1.,1.),(1.,1.),(1.,
1.),(1.,1.),(1.,1.),(1.,1.),(1.,1.),(1.,1.),(1.,1.),(1.,1.),(1.,1.),(1.,
1.),(1.,1.),(1.,1.),(1.,1.),(1.,1.),(1.,1.),(1.,1.),(1.,1.),(1.,1.),(1.,
1.),(1.,1.),(1.,1.),(1.,1.),(1.,1.),(1.,1.),(1.,1.),(1.,1.),(1.,1.),(1.,
1.),(1.,1.),(1.,1.),(1.,1.),(1.,1.),(1.,1.),(1.,1.),(1.,1.),(1.,1.),(1.,
1.),(1.,1.),(1.,1.),(1.,1.),(1.,1.),(1.,1.),(1.,1.),(1.,1.),(1.,1.),(1.,
1.),(1.,1.),(1.,1.),(1.,1.),(1.,1.),(1.,1.),(1.,1.),(1.,1.),(1.,1.),(1.,
1.),(1.,1.),(1.,1.),(1.,1.),(1.,1.),(1.,1.),(1.,1.),(1.,1.),(1.,1.),(1.,
1.),(1.,1.),(1.,1.),(1.,1.),(1.,1.),(1.,1.),(1.,1.),(1.,1.),(1.,1.),(1.,
1.),(1.,1.),(1.,1.),(1.,1.),(1.,1.),(1.,1.),(1.,1.),(1.,1.),(1.,1.),(1.,
1.),(1.,1.),(1.,1.),(1.,1.),(1.,1.),(1.,1.),(1.,1.),(1.,1.),(1.,1.),(1.,
1.),(1.,1.),(1.,1.),(1.,1.),(1.,1.),(1.,1.),(1.,1.),(1.,1.),(1.,1.),(1.,
1.),(1.,1.),(1.,1.),(1.,1.),(1.,1.),(1.,1.),(1.,1.),(1.,1.),(1.,1.),(1.,
1.),(1.,1.),(1.,1.),(1.,1.),(1.,1.),(1.,1.),(1.,1.),(1.,1.),(1.,1.),(1.,
1.),(1.,1.)))
REPRESENTATION_ITEM('')
SURFACE()
);
#1095=(
BOUNDED_SURFACE()
B_SPLINE_SURFACE(5,1,((#232528,#232529),(#232530,#232531),(#232532,#232533),
(#232534,#232535),(#232536,#232537),(#232538,#232539),(#232540,#232541),
(#232542,#232543),(#232544,#232545),(#232546,#232547),(#232548,#232549),
(#232550,#232551),(#232552,#232553),(#232554,#232555),(#232556,#232557),
(#232558,#232559),(#232560,#232561),(#232562,#232563),(#232564,#232565),
(#232566,#232567),(#232568,#232569),(#232570,#232571),(#232572,#232573),
(#232574,#232575),(#232576,#232577),(#232578,#232579),(#232580,#232581),
(#232582,#232583),(#232584,#232585),(#232586,#232587),(#232588,#232589),
(#232590,#232591),(#232592,#232593),(#232594,#232595),(#232596,#232597),
(#232598,#232599),(#232600,#232601),(#232602,#232603),(#232604,#232605),
(#232606,#232607),(#232608,#232609),(#232610,#232611),(#232612,#232613),
(#232614,#232615),(#232616,#232617),(#232618,#232619),(#232620,#232621),
(#232622,#232623),(#232624,#232625),(#232626,#232627),(#232628,#232629),
(#232630,#232631),(#232632,#232633),(#232634,#232635),(#232636,#232637),
(#232638,#232639),(#232640,#232641),(#232642,#232643),(#232644,#232645),
(#232646,#232647),(#232648,#232649),(#232650,#232651),(#232652,#232653),
(#232654,#232655),(#232656,#232657),(#232658,#232659),(#232660,#232661),
(#232662,#232663),(#232664,#232665),(#232666,#232667),(#232668,#232669),
(#232670,#232671),(#232672,#232673),(#232674,#232675),(#232676,#232677),
(#232678,#232679),(#232680,#232681),(#232682,#232683),(#232684,#232685),
(#232686,#232687),(#232688,#232689),(#232690,#232691),(#232692,#232693),
(#232694,#232695),(#232696,#232697),(#232698,#232699),(#232700,#232701),
(#232702,#232703),(#232704,#232705),(#232706,#232707),(#232708,#232709),
(#232710,#232711),(#232712,#232713),(#232714,#232715),(#232716,#232717),
(#232718,#232719),(#232720,#232721),(#232722,#232723),(#232724,#232725),
(#232726,#232727),(#232728,#232729),(#232730,#232731),(#232732,#232733),
(#232734,#232735),(#232736,#232737),(#232738,#232739),(#232740,#232741),
(#232742,#232743),(#232744,#232745),(#232746,#232747),(#232748,#232749),
(#232750,#232751),(#232752,#232753),(#232754,#232755),(#232756,#232757),
(#232758,#232759),(#232760,#232761),(#232762,#232763),(#232764,#232765),
(#232766,#232767),(#232768,#232769),(#232770,#232771),(#232772,#232773),
(#232774,#232775),(#232776,#232777),(#232778,#232779),(#232780,#232781),
(#232782,#232783),(#232784,#232785),(#232786,#232787),(#232788,#232789),
(#232790,#232791),(#232792,#232793),(#232794,#232795),(#232796,#232797),
(#232798,#232799),(#232800,#232801),(#232802,#232803),(#232804,#232805),
(#232806,#232807),(#232808,#232809),(#232810,#232811),(#232812,#232813),
(#232814,#232815),(#232816,#232817),(#232818,#232819),(#232820,#232821),
(#232822,#232823),(#232824,#232825),(#232826,#232827),(#232828,#232829),
(#232830,#232831),(#232832,#232833),(#232834,#232835),(#232836,#232837),
(#232838,#232839),(#232840,#232841),(#232842,#232843),(#232844,#232845),
(#232846,#232847),(#232848,#232849),(#232850,#232851),(#232852,#232853),
(#232854,#232855),(#232856,#232857),(#232858,#232859),(#232860,#232861),
(#232862,#232863),(#232864,#232865),(#232866,#232867),(#232868,#232869),
(#232870,#232871),(#232872,#232873),(#232874,#232875),(#232876,#232877),
(#232878,#232879),(#232880,#232881),(#232882,#232883),(#232884,#232885),
(#232886,#232887),(#232888,#232889),(#232890,#232891),(#232892,#232893),
(#232894,#232895),(#232896,#232897),(#232898,#232899),(#232900,#232901),
(#232902,#232903),(#232904,#232905),(#232906,#232907),(#232908,#232909),
(#232910,#232911),(#232912,#232913),(#232914,#232915),(#232916,#232917),
(#232918,#232919),(#232920,#232921),(#232922,#232923),(#232924,#232925),
(#232926,#232927),(#232928,#232929),(#232930,#232931),(#232932,#232933),
(#232934,#232935),(#232936,#232937)),.UNSPECIFIED.,.F.,.F.,.F.)
B_SPLINE_SURFACE_WITH_KNOTS((6,1,1,1,1,1,1,1,1,1,1,1,1,1,1,1,1,1,1,1,1,
1,1,1,1,1,1,1,1,1,1,1,1,1,1,1,1,1,1,1,1,1,1,1,1,1,1,1,1,1,1,1,1,1,1,1,1,
1,1,1,1,1,1,1,1,1,1,1,1,1,1,1,1,1,1,1,1,1,1,1,1,1,1,1,1,1,1,1,1,1,1,1,1,
1,1,1,1,1,1,1,1,1,1,1,1,1,1,1,1,1,1,1,1,1,1,1,1,1,1,1,1,1,1,1,1,1,1,1,1,
1,1,1,1,1,1,1,1,1,1,1,1,1,1,1,1,1,1,1,1,1,1,1,1,1,1,1,1,1,1,1,1,1,1,1,1,
1,1,1,1,1,1,1,1,1,1,1,1,1,1,1,1,1,1,1,1,1,1,1,1,1,1,1,1,1,1,1,1,1,1,1,6),
(2,2),(-1.,-0.995000000000001,-0.990000000000001,-0.985000000000001,-0.980000000000001,
-0.975000000000001,-0.970000000000001,-0.965000000000001,-0.960000000000001,
-0.955000000000001,-0.950000000000001,-0.945000000000001,-0.940000000000001,
-0.935000000000001,-0.930000000000001,-0.925000000000001,-0.920000000000001,
-0.915000000000001,-0.910000000000001,-0.905000000000001,-0.900000000000001,
-0.895000000000001,-0.890000000000001,-0.885000000000001,-0.880000000000001,
-0.875000000000001,-0.870000000000001,-0.865000000000001,-0.860000000000001,
-0.855000000000001,-0.850000000000001,-0.845000000000001,-0.840000000000001,
-0.835000000000001,-0.830000000000001,-0.825000000000001,-0.820000000000001,
-0.815000000000001,-0.810000000000001,-0.805000000000001,-0.800000000000001,
-0.795000000000001,-0.790000000000001,-0.785000000000001,-0.780000000000001,
-0.775000000000001,-0.770000000000001,-0.765000000000001,-0.760000000000001,
-0.755000000000001,-0.750000000000001,-0.745000000000001,-0.740000000000001,
-0.735000000000001,-0.730000000000001,-0.725000000000001,-0.720000000000001,
-0.715000000000001,-0.710000000000001,-0.705000000000001,-0.700000000000001,
-0.695000000000001,-0.690000000000001,-0.685,-0.68,-0.675,-0.67,-0.665,
-0.66,-0.655,-0.65,-0.645,-0.64,-0.635,-0.63,-0.625,-0.62,-0.615,-0.61,
-0.605,-0.6,-0.595,-0.59,-0.585,-0.58,-0.575,-0.57,-0.565,-0.56,-0.555,
-0.55,-0.545,-0.54,-0.535,-0.53,-0.525,-0.52,-0.515,-0.51,-0.505,-0.5,-0.495,
-0.49,-0.485,-0.48,-0.475,-0.47,-0.465,-0.46,-0.455,-0.45,-0.445,-0.44,
-0.435,-0.43,-0.425,-0.42,-0.415,-0.41,-0.405,-0.4,-0.395,-0.39,-0.385,
-0.38,-0.375,-0.37,-0.365,-0.36,-0.355,-0.35,-0.345,-0.34,-0.335,-0.33,
-0.325,-0.32,-0.315,-0.31,-0.305,-0.3,-0.295,-0.29,-0.285,-0.28,-0.275,
-0.27,-0.265,-0.26,-0.255,-0.25,-0.245,-0.24,-0.235,-0.23,-0.225,-0.22,
-0.215,-0.21,-0.205,-0.2,-0.195,-0.19,-0.185,-0.18,-0.175,-0.17,-0.165,
-0.16,-0.155,-0.15,-0.145,-0.14,-0.135,-0.13,-0.125,-0.12,-0.115,-0.11,
-0.105,-0.1,-0.095,-0.09,-0.085,-0.08,-0.075,-0.07,-0.065,-0.06,-0.055,
-0.05,-0.045,-0.04,-0.035,-0.03,-0.025,-0.02,-0.015,-0.01,-0.005,0.),(0.,
1.2),.UNSPECIFIED.)
GEOMETRIC_REPRESENTATION_ITEM()
RATIONAL_B_SPLINE_SURFACE(((1.,1.),(1.,1.),(1.,1.),(1.,1.),(1.,1.),(1.,
1.),(1.,1.),(1.,1.),(1.,1.),(1.,1.),(1.,1.),(1.,1.),(1.,1.),(1.,1.),(1.,
1.),(1.,1.),(1.,1.),(1.,1.),(1.,1.),(1.,1.),(1.,1.),(1.,1.),(1.,1.),(1.,
1.),(1.,1.),(1.,1.),(1.,1.),(1.,1.),(1.,1.),(1.,1.),(1.,1.),(1.,1.),(1.,
1.),(1.,1.),(1.,1.),(1.,1.),(1.,1.),(1.,1.),(1.,1.),(1.,1.),(1.,1.),(1.,
1.),(1.,1.),(1.,1.),(1.,1.),(1.,1.),(1.,1.),(1.,1.),(1.,1.),(1.,1.),(1.,
1.),(1.,1.),(1.,1.),(1.,1.),(1.,1.),(1.,1.),(1.,1.),(1.,1.),(1.,1.),(1.,
1.),(1.,1.),(1.,1.),(1.,1.),(1.,1.),(1.,1.),(1.,1.),(1.,1.),(1.,1.),(1.,
1.),(1.,1.),(1.,1.),(1.,1.),(1.,1.),(1.,1.),(1.,1.),(1.,1.),(1.,1.),(1.,
1.),(1.,1.),(1.,1.),(1.,1.),(1.,1.),(1.,1.),(1.,1.),(1.,1.),(1.,1.),(1.,
1.),(1.,1.),(1.,1.),(1.,1.),(1.,1.),(1.,1.),(1.,1.),(1.,1.),(1.,1.),(1.,
1.),(1.,1.),(1.,1.),(1.,1.),(1.,1.),(1.,1.),(1.,1.),(1.,1.),(1.,1.),(1.,
1.),(1.,1.),(1.,1.),(1.,1.),(1.,1.),(1.,1.),(1.,1.),(1.,1.),(1.,1.),(1.,
1.),(1.,1.),(1.,1.),(1.,1.),(1.,1.),(1.,1.),(1.,1.),(1.,1.),(1.,1.),(1.,
1.),(1.,1.),(1.,1.),(1.,1.),(1.,1.),(1.,1.),(1.,1.),(1.,1.),(1.,1.),(1.,
1.),(1.,1.),(1.,1.),(1.,1.),(1.,1.),(1.,1.),(1.,1.),(1.,1.),(1.,1.),(1.,
1.),(1.,1.),(1.,1.),(1.,1.),(1.,1.),(1.,1.),(1.,1.),(1.,1.),(1.,1.),(1.,
1.),(1.,1.),(1.,1.),(1.,1.),(1.,1.),(1.,1.),(1.,1.),(1.,1.),(1.,1.),(1.,
1.),(1.,1.),(1.,1.),(1.,1.),(1.,1.),(1.,1.),(1.,1.),(1.,1.),(1.,1.),(1.,
1.),(1.,1.),(1.,1.),(1.,1.),(1.,1.),(1.,1.),(1.,1.),(1.,1.),(1.,1.),(1.,
1.),(1.,1.),(1.,1.),(1.,1.),(1.,1.),(1.,1.),(1.,1.),(1.,1.),(1.,1.),(1.,
1.),(1.,1.),(1.,1.),(1.,1.),(1.,1.),(1.,1.),(1.,1.),(1.,1.),(1.,1.),(1.,
1.),(1.,1.),(1.,1.),(1.,1.),(1.,1.),(1.,1.),(1.,1.),(1.,1.),(1.,1.),(1.,
1.),(1.,1.)))
REPRESENTATION_ITEM('')
SURFACE()
);
#1096=(
BOUNDED_SURFACE()
B_SPLINE_SURFACE(5,1,((#233351,#233352),(#233353,#233354),(#233355,#233356),
(#233357,#233358),(#233359,#233360),(#233361,#233362),(#233363,#233364),
(#233365,#233366),(#233367,#233368),(#233369,#233370),(#233371,#233372),
(#233373,#233374),(#233375,#233376),(#233377,#233378),(#233379,#233380),
(#233381,#233382),(#233383,#233384),(#233385,#233386),(#233387,#233388),
(#233389,#233390),(#233391,#233392),(#233393,#233394),(#233395,#233396),
(#233397,#233398),(#233399,#233400),(#233401,#233402),(#233403,#233404),
(#233405,#233406),(#233407,#233408),(#233409,#233410),(#233411,#233412),
(#233413,#233414),(#233415,#233416),(#233417,#233418),(#233419,#233420),
(#233421,#233422),(#233423,#233424),(#233425,#233426),(#233427,#233428),
(#233429,#233430),(#233431,#233432),(#233433,#233434),(#233435,#233436),
(#233437,#233438),(#233439,#233440),(#233441,#233442),(#233443,#233444),
(#233445,#233446),(#233447,#233448),(#233449,#233450),(#233451,#233452),
(#233453,#233454),(#233455,#233456),(#233457,#233458),(#233459,#233460),
(#233461,#233462),(#233463,#233464),(#233465,#233466),(#233467,#233468),
(#233469,#233470),(#233471,#233472),(#233473,#233474),(#233475,#233476),
(#233477,#233478),(#233479,#233480),(#233481,#233482),(#233483,#233484),
(#233485,#233486),(#233487,#233488),(#233489,#233490),(#233491,#233492),
(#233493,#233494),(#233495,#233496),(#233497,#233498),(#233499,#233500),
(#233501,#233502),(#233503,#233504),(#233505,#233506),(#233507,#233508),
(#233509,#233510),(#233511,#233512),(#233513,#233514),(#233515,#233516),
(#233517,#233518),(#233519,#233520),(#233521,#233522),(#233523,#233524),
(#233525,#233526),(#233527,#233528),(#233529,#233530),(#233531,#233532),
(#233533,#233534),(#233535,#233536),(#233537,#233538),(#233539,#233540),
(#233541,#233542),(#233543,#233544),(#233545,#233546),(#233547,#233548),
(#233549,#233550),(#233551,#233552),(#233553,#233554),(#233555,#233556),
(#233557,#233558),(#233559,#233560),(#233561,#233562),(#233563,#233564),
(#233565,#233566),(#233567,#233568),(#233569,#233570),(#233571,#233572),
(#233573,#233574),(#233575,#233576),(#233577,#233578),(#233579,#233580),
(#233581,#233582),(#233583,#233584),(#233585,#233586),(#233587,#233588),
(#233589,#233590),(#233591,#233592),(#233593,#233594),(#233595,#233596),
(#233597,#233598),(#233599,#233600),(#233601,#233602),(#233603,#233604),
(#233605,#233606),(#233607,#233608),(#233609,#233610),(#233611,#233612),
(#233613,#233614),(#233615,#233616),(#233617,#233618),(#233619,#233620),
(#233621,#233622),(#233623,#233624),(#233625,#233626),(#233627,#233628),
(#233629,#233630),(#233631,#233632),(#233633,#233634),(#233635,#233636),
(#233637,#233638),(#233639,#233640),(#233641,#233642),(#233643,#233644),
(#233645,#233646),(#233647,#233648),(#233649,#233650),(#233651,#233652),
(#233653,#233654),(#233655,#233656),(#233657,#233658),(#233659,#233660),
(#233661,#233662),(#233663,#233664),(#233665,#233666),(#233667,#233668),
(#233669,#233670),(#233671,#233672),(#233673,#233674),(#233675,#233676),
(#233677,#233678),(#233679,#233680),(#233681,#233682),(#233683,#233684),
(#233685,#233686),(#233687,#233688),(#233689,#233690),(#233691,#233692),
(#233693,#233694),(#233695,#233696),(#233697,#233698),(#233699,#233700),
(#233701,#233702),(#233703,#233704),(#233705,#233706),(#233707,#233708),
(#233709,#233710),(#233711,#233712),(#233713,#233714),(#233715,#233716),
(#233717,#233718),(#233719,#233720),(#233721,#233722),(#233723,#233724),
(#233725,#233726),(#233727,#233728),(#233729,#233730),(#233731,#233732),
(#233733,#233734),(#233735,#233736),(#233737,#233738),(#233739,#233740),
(#233741,#233742),(#233743,#233744),(#233745,#233746),(#233747,#233748),
(#233749,#233750),(#233751,#233752),(#233753,#233754),(#233755,#233756),
(#233757,#233758),(#233759,#233760)),.UNSPECIFIED.,.F.,.F.,.F.)
B_SPLINE_SURFACE_WITH_KNOTS((6,1,1,1,1,1,1,1,1,1,1,1,1,1,1,1,1,1,1,1,1,
1,1,1,1,1,1,1,1,1,1,1,1,1,1,1,1,1,1,1,1,1,1,1,1,1,1,1,1,1,1,1,1,1,1,1,1,
1,1,1,1,1,1,1,1,1,1,1,1,1,1,1,1,1,1,1,1,1,1,1,1,1,1,1,1,1,1,1,1,1,1,1,1,
1,1,1,1,1,1,1,1,1,1,1,1,1,1,1,1,1,1,1,1,1,1,1,1,1,1,1,1,1,1,1,1,1,1,1,1,
1,1,1,1,1,1,1,1,1,1,1,1,1,1,1,1,1,1,1,1,1,1,1,1,1,1,1,1,1,1,1,1,1,1,1,1,
1,1,1,1,1,1,1,1,1,1,1,1,1,1,1,1,1,1,1,1,1,1,1,1,1,1,1,1,1,1,1,1,1,1,1,6),
(2,2),(0.,0.005,0.01,0.015,0.02,0.025,0.03,0.035,0.04,0.045,0.05,0.055,
0.06,0.065,0.07,0.075,0.08,0.085,0.09,0.095,0.1,0.105,0.11,0.115,0.12,0.125,
0.13,0.135,0.14,0.145,0.15,0.155,0.16,0.165,0.17,0.175,0.18,0.185,0.19,
0.195,0.2,0.205,0.21,0.215,0.22,0.225,0.23,0.235,0.24,0.245,0.25,0.255,
0.26,0.265,0.27,0.275,0.28,0.285,0.29,0.295,0.3,0.305,0.31,0.315,0.32,0.325,
0.33,0.335,0.34,0.345,0.35,0.355,0.36,0.365,0.37,0.375,0.38,0.385,0.39,
0.395,0.4,0.405,0.41,0.415,0.42,0.425,0.43,0.435,0.44,0.445,0.45,0.455,
0.46,0.465,0.47,0.475,0.48,0.485,0.49,0.495,0.5,0.505,0.51,0.515,0.52,0.525,
0.53,0.535,0.54,0.545,0.55,0.555,0.56,0.565,0.57,0.575,0.58,0.585,0.59,
0.595,0.6,0.605,0.61,0.615,0.62,0.625,0.63,0.635,0.64,0.645,0.65,0.655,
0.66,0.665,0.67,0.675,0.68,0.685,0.690000000000001,0.695000000000001,0.700000000000001,
0.705000000000001,0.710000000000001,0.715000000000001,0.720000000000001,
0.725000000000001,0.730000000000001,0.735000000000001,0.740000000000001,
0.745000000000001,0.750000000000001,0.755000000000001,0.760000000000001,
0.765000000000001,0.770000000000001,0.775000000000001,0.780000000000001,
0.785000000000001,0.790000000000001,0.795000000000001,0.800000000000001,
0.805000000000001,0.810000000000001,0.815000000000001,0.820000000000001,
0.825000000000001,0.830000000000001,0.835000000000001,0.840000000000001,
0.845000000000001,0.850000000000001,0.855000000000001,0.860000000000001,
0.865000000000001,0.870000000000001,0.875000000000001,0.880000000000001,
0.885000000000001,0.890000000000001,0.895000000000001,0.900000000000001,
0.905000000000001,0.910000000000001,0.915000000000001,0.920000000000001,
0.925000000000001,0.930000000000001,0.935000000000001,0.940000000000001,
0.945000000000001,0.950000000000001,0.955000000000001,0.960000000000001,
0.965000000000001,0.970000000000001,0.975000000000001,0.980000000000001,
0.985000000000001,0.990000000000001,0.995000000000001,1.),(0.,1.2),
 .UNSPECIFIED.)
GEOMETRIC_REPRESENTATION_ITEM()
RATIONAL_B_SPLINE_SURFACE(((1.,1.),(1.,1.),(1.,1.),(1.,1.),(1.,1.),(1.,
1.),(1.,1.),(1.,1.),(1.,1.),(1.,1.),(1.,1.),(1.,1.),(1.,1.),(1.,1.),(1.,
1.),(1.,1.),(1.,1.),(1.,1.),(1.,1.),(1.,1.),(1.,1.),(1.,1.),(1.,1.),(1.,
1.),(1.,1.),(1.,1.),(1.,1.),(1.,1.),(1.,1.),(1.,1.),(1.,1.),(1.,1.),(1.,
1.),(1.,1.),(1.,1.),(1.,1.),(1.,1.),(1.,1.),(1.,1.),(1.,1.),(1.,1.),(1.,
1.),(1.,1.),(1.,1.),(1.,1.),(1.,1.),(1.,1.),(1.,1.),(1.,1.),(1.,1.),(1.,
1.),(1.,1.),(1.,1.),(1.,1.),(1.,1.),(1.,1.),(1.,1.),(1.,1.),(1.,1.),(1.,
1.),(1.,1.),(1.,1.),(1.,1.),(1.,1.),(1.,1.),(1.,1.),(1.,1.),(1.,1.),(1.,
1.),(1.,1.),(1.,1.),(1.,1.),(1.,1.),(1.,1.),(1.,1.),(1.,1.),(1.,1.),(1.,
1.),(1.,1.),(1.,1.),(1.,1.),(1.,1.),(1.,1.),(1.,1.),(1.,1.),(1.,1.),(1.,
1.),(1.,1.),(1.,1.),(1.,1.),(1.,1.),(1.,1.),(1.,1.),(1.,1.),(1.,1.),(1.,
1.),(1.,1.),(1.,1.),(1.,1.),(1.,1.),(1.,1.),(1.,1.),(1.,1.),(1.,1.),(1.,
1.),(1.,1.),(1.,1.),(1.,1.),(1.,1.),(1.,1.),(1.,1.),(1.,1.),(1.,1.),(1.,
1.),(1.,1.),(1.,1.),(1.,1.),(1.,1.),(1.,1.),(1.,1.),(1.,1.),(1.,1.),(1.,
1.),(1.,1.),(1.,1.),(1.,1.),(1.,1.),(1.,1.),(1.,1.),(1.,1.),(1.,1.),(1.,
1.),(1.,1.),(1.,1.),(1.,1.),(1.,1.),(1.,1.),(1.,1.),(1.,1.),(1.,1.),(1.,
1.),(1.,1.),(1.,1.),(1.,1.),(1.,1.),(1.,1.),(1.,1.),(1.,1.),(1.,1.),(1.,
1.),(1.,1.),(1.,1.),(1.,1.),(1.,1.),(1.,1.),(1.,1.),(1.,1.),(1.,1.),(1.,
1.),(1.,1.),(1.,1.),(1.,1.),(1.,1.),(1.,1.),(1.,1.),(1.,1.),(1.,1.),(1.,
1.),(1.,1.),(1.,1.),(1.,1.),(1.,1.),(1.,1.),(1.,1.),(1.,1.),(1.,1.),(1.,
1.),(1.,1.),(1.,1.),(1.,1.),(1.,1.),(1.,1.),(1.,1.),(1.,1.),(1.,1.),(1.,
1.),(1.,1.),(1.,1.),(1.,1.),(1.,1.),(1.,1.),(1.,1.),(1.,1.),(1.,1.),(1.,
1.),(1.,1.),(1.,1.),(1.,1.),(1.,1.),(1.,1.),(1.,1.),(1.,1.),(1.,1.),(1.,
1.),(1.,1.)))
REPRESENTATION_ITEM('')
SURFACE()
);
#1097=(
BOUNDED_SURFACE()
B_SPLINE_SURFACE(5,1,((#234180,#234181),(#234182,#234183),(#234184,#234185),
(#234186,#234187),(#234188,#234189),(#234190,#234191),(#234192,#234193),
(#234194,#234195),(#234196,#234197),(#234198,#234199),(#234200,#234201),
(#234202,#234203),(#234204,#234205),(#234206,#234207),(#234208,#234209),
(#234210,#234211),(#234212,#234213),(#234214,#234215),(#234216,#234217),
(#234218,#234219),(#234220,#234221),(#234222,#234223),(#234224,#234225),
(#234226,#234227),(#234228,#234229),(#234230,#234231),(#234232,#234233),
(#234234,#234235),(#234236,#234237),(#234238,#234239),(#234240,#234241),
(#234242,#234243),(#234244,#234245),(#234246,#234247),(#234248,#234249),
(#234250,#234251),(#234252,#234253),(#234254,#234255),(#234256,#234257),
(#234258,#234259),(#234260,#234261),(#234262,#234263),(#234264,#234265),
(#234266,#234267),(#234268,#234269),(#234270,#234271),(#234272,#234273),
(#234274,#234275),(#234276,#234277),(#234278,#234279),(#234280,#234281),
(#234282,#234283),(#234284,#234285),(#234286,#234287),(#234288,#234289),
(#234290,#234291),(#234292,#234293),(#234294,#234295),(#234296,#234297),
(#234298,#234299),(#234300,#234301),(#234302,#234303),(#234304,#234305),
(#234306,#234307),(#234308,#234309),(#234310,#234311),(#234312,#234313),
(#234314,#234315),(#234316,#234317),(#234318,#234319),(#234320,#234321),
(#234322,#234323),(#234324,#234325),(#234326,#234327),(#234328,#234329),
(#234330,#234331),(#234332,#234333),(#234334,#234335),(#234336,#234337),
(#234338,#234339),(#234340,#234341),(#234342,#234343),(#234344,#234345),
(#234346,#234347),(#234348,#234349),(#234350,#234351),(#234352,#234353),
(#234354,#234355),(#234356,#234357),(#234358,#234359),(#234360,#234361),
(#234362,#234363),(#234364,#234365),(#234366,#234367),(#234368,#234369),
(#234370,#234371),(#234372,#234373),(#234374,#234375),(#234376,#234377),
(#234378,#234379),(#234380,#234381),(#234382,#234383),(#234384,#234385),
(#234386,#234387),(#234388,#234389),(#234390,#234391),(#234392,#234393),
(#234394,#234395),(#234396,#234397),(#234398,#234399),(#234400,#234401),
(#234402,#234403),(#234404,#234405),(#234406,#234407),(#234408,#234409),
(#234410,#234411),(#234412,#234413),(#234414,#234415),(#234416,#234417),
(#234418,#234419),(#234420,#234421),(#234422,#234423),(#234424,#234425),
(#234426,#234427),(#234428,#234429),(#234430,#234431),(#234432,#234433),
(#234434,#234435),(#234436,#234437),(#234438,#234439),(#234440,#234441),
(#234442,#234443),(#234444,#234445),(#234446,#234447),(#234448,#234449),
(#234450,#234451),(#234452,#234453),(#234454,#234455),(#234456,#234457),
(#234458,#234459),(#234460,#234461),(#234462,#234463),(#234464,#234465),
(#234466,#234467),(#234468,#234469),(#234470,#234471),(#234472,#234473),
(#234474,#234475),(#234476,#234477),(#234478,#234479),(#234480,#234481),
(#234482,#234483),(#234484,#234485),(#234486,#234487),(#234488,#234489),
(#234490,#234491),(#234492,#234493),(#234494,#234495),(#234496,#234497),
(#234498,#234499),(#234500,#234501),(#234502,#234503),(#234504,#234505),
(#234506,#234507),(#234508,#234509),(#234510,#234511),(#234512,#234513),
(#234514,#234515),(#234516,#234517),(#234518,#234519),(#234520,#234521),
(#234522,#234523),(#234524,#234525),(#234526,#234527),(#234528,#234529),
(#234530,#234531),(#234532,#234533),(#234534,#234535),(#234536,#234537),
(#234538,#234539),(#234540,#234541),(#234542,#234543),(#234544,#234545),
(#234546,#234547),(#234548,#234549),(#234550,#234551),(#234552,#234553),
(#234554,#234555),(#234556,#234557),(#234558,#234559),(#234560,#234561),
(#234562,#234563),(#234564,#234565),(#234566,#234567),(#234568,#234569),
(#234570,#234571),(#234572,#234573),(#234574,#234575),(#234576,#234577),
(#234578,#234579),(#234580,#234581),(#234582,#234583),(#234584,#234585),
(#234586,#234587),(#234588,#234589)),.UNSPECIFIED.,.F.,.F.,.F.)
B_SPLINE_SURFACE_WITH_KNOTS((6,1,1,1,1,1,1,1,1,1,1,1,1,1,1,1,1,1,1,1,1,
1,1,1,1,1,1,1,1,1,1,1,1,1,1,1,1,1,1,1,1,1,1,1,1,1,1,1,1,1,1,1,1,1,1,1,1,
1,1,1,1,1,1,1,1,1,1,1,1,1,1,1,1,1,1,1,1,1,1,1,1,1,1,1,1,1,1,1,1,1,1,1,1,
1,1,1,1,1,1,1,1,1,1,1,1,1,1,1,1,1,1,1,1,1,1,1,1,1,1,1,1,1,1,1,1,1,1,1,1,
1,1,1,1,1,1,1,1,1,1,1,1,1,1,1,1,1,1,1,1,1,1,1,1,1,1,1,1,1,1,1,1,1,1,1,1,
1,1,1,1,1,1,1,1,1,1,1,1,1,1,1,1,1,1,1,1,1,1,1,1,1,1,1,1,1,1,1,1,1,1,1,6),
(2,2),(-1.,-0.995000000000001,-0.990000000000001,-0.985000000000001,-0.980000000000001,
-0.975000000000001,-0.970000000000001,-0.965000000000001,-0.960000000000001,
-0.955000000000001,-0.950000000000001,-0.945000000000001,-0.940000000000001,
-0.935000000000001,-0.930000000000001,-0.925000000000001,-0.920000000000001,
-0.915000000000001,-0.910000000000001,-0.905000000000001,-0.900000000000001,
-0.895000000000001,-0.890000000000001,-0.885000000000001,-0.880000000000001,
-0.875000000000001,-0.870000000000001,-0.865000000000001,-0.860000000000001,
-0.855000000000001,-0.850000000000001,-0.845000000000001,-0.840000000000001,
-0.835000000000001,-0.830000000000001,-0.825000000000001,-0.820000000000001,
-0.815000000000001,-0.810000000000001,-0.805000000000001,-0.800000000000001,
-0.795000000000001,-0.790000000000001,-0.785000000000001,-0.780000000000001,
-0.775000000000001,-0.770000000000001,-0.765000000000001,-0.760000000000001,
-0.755000000000001,-0.750000000000001,-0.745000000000001,-0.740000000000001,
-0.735000000000001,-0.730000000000001,-0.725000000000001,-0.720000000000001,
-0.715000000000001,-0.710000000000001,-0.705000000000001,-0.700000000000001,
-0.695000000000001,-0.690000000000001,-0.685,-0.68,-0.675,-0.67,-0.665,
-0.66,-0.655,-0.65,-0.645,-0.64,-0.635,-0.63,-0.625,-0.62,-0.615,-0.61,
-0.605,-0.6,-0.595,-0.59,-0.585,-0.58,-0.575,-0.57,-0.565,-0.56,-0.555,
-0.55,-0.545,-0.54,-0.535,-0.53,-0.525,-0.52,-0.515,-0.51,-0.505,-0.5,-0.495,
-0.49,-0.485,-0.48,-0.475,-0.47,-0.465,-0.46,-0.455,-0.45,-0.445,-0.44,
-0.435,-0.43,-0.425,-0.42,-0.415,-0.41,-0.405,-0.4,-0.395,-0.39,-0.385,
-0.38,-0.375,-0.37,-0.365,-0.36,-0.355,-0.35,-0.345,-0.34,-0.335,-0.33,
-0.325,-0.32,-0.315,-0.31,-0.305,-0.3,-0.295,-0.29,-0.285,-0.28,-0.275,
-0.27,-0.265,-0.26,-0.255,-0.25,-0.245,-0.24,-0.235,-0.23,-0.225,-0.22,
-0.215,-0.21,-0.205,-0.2,-0.195,-0.19,-0.185,-0.18,-0.175,-0.17,-0.165,
-0.16,-0.155,-0.15,-0.145,-0.14,-0.135,-0.13,-0.125,-0.12,-0.115,-0.11,
-0.105,-0.1,-0.095,-0.09,-0.085,-0.08,-0.075,-0.07,-0.065,-0.06,-0.055,
-0.05,-0.045,-0.04,-0.035,-0.03,-0.025,-0.02,-0.015,-0.01,-0.005,0.),(0.,
1.2),.UNSPECIFIED.)
GEOMETRIC_REPRESENTATION_ITEM()
RATIONAL_B_SPLINE_SURFACE(((1.,1.),(1.,1.),(1.,1.),(1.,1.),(1.,1.),(1.,
1.),(1.,1.),(1.,1.),(1.,1.),(1.,1.),(1.,1.),(1.,1.),(1.,1.),(1.,1.),(1.,
1.),(1.,1.),(1.,1.),(1.,1.),(1.,1.),(1.,1.),(1.,1.),(1.,1.),(1.,1.),(1.,
1.),(1.,1.),(1.,1.),(1.,1.),(1.,1.),(1.,1.),(1.,1.),(1.,1.),(1.,1.),(1.,
1.),(1.,1.),(1.,1.),(1.,1.),(1.,1.),(1.,1.),(1.,1.),(1.,1.),(1.,1.),(1.,
1.),(1.,1.),(1.,1.),(1.,1.),(1.,1.),(1.,1.),(1.,1.),(1.,1.),(1.,1.),(1.,
1.),(1.,1.),(1.,1.),(1.,1.),(1.,1.),(1.,1.),(1.,1.),(1.,1.),(1.,1.),(1.,
1.),(1.,1.),(1.,1.),(1.,1.),(1.,1.),(1.,1.),(1.,1.),(1.,1.),(1.,1.),(1.,
1.),(1.,1.),(1.,1.),(1.,1.),(1.,1.),(1.,1.),(1.,1.),(1.,1.),(1.,1.),(1.,
1.),(1.,1.),(1.,1.),(1.,1.),(1.,1.),(1.,1.),(1.,1.),(1.,1.),(1.,1.),(1.,
1.),(1.,1.),(1.,1.),(1.,1.),(1.,1.),(1.,1.),(1.,1.),(1.,1.),(1.,1.),(1.,
1.),(1.,1.),(1.,1.),(1.,1.),(1.,1.),(1.,1.),(1.,1.),(1.,1.),(1.,1.),(1.,
1.),(1.,1.),(1.,1.),(1.,1.),(1.,1.),(1.,1.),(1.,1.),(1.,1.),(1.,1.),(1.,
1.),(1.,1.),(1.,1.),(1.,1.),(1.,1.),(1.,1.),(1.,1.),(1.,1.),(1.,1.),(1.,
1.),(1.,1.),(1.,1.),(1.,1.),(1.,1.),(1.,1.),(1.,1.),(1.,1.),(1.,1.),(1.,
1.),(1.,1.),(1.,1.),(1.,1.),(1.,1.),(1.,1.),(1.,1.),(1.,1.),(1.,1.),(1.,
1.),(1.,1.),(1.,1.),(1.,1.),(1.,1.),(1.,1.),(1.,1.),(1.,1.),(1.,1.),(1.,
1.),(1.,1.),(1.,1.),(1.,1.),(1.,1.),(1.,1.),(1.,1.),(1.,1.),(1.,1.),(1.,
1.),(1.,1.),(1.,1.),(1.,1.),(1.,1.),(1.,1.),(1.,1.),(1.,1.),(1.,1.),(1.,
1.),(1.,1.),(1.,1.),(1.,1.),(1.,1.),(1.,1.),(1.,1.),(1.,1.),(1.,1.),(1.,
1.),(1.,1.),(1.,1.),(1.,1.),(1.,1.),(1.,1.),(1.,1.),(1.,1.),(1.,1.),(1.,
1.),(1.,1.),(1.,1.),(1.,1.),(1.,1.),(1.,1.),(1.,1.),(1.,1.),(1.,1.),(1.,
1.),(1.,1.),(1.,1.),(1.,1.),(1.,1.),(1.,1.),(1.,1.),(1.,1.),(1.,1.),(1.,
1.),(1.,1.)))
REPRESENTATION_ITEM('')
SURFACE()
);
#1098=(
BOUNDED_SURFACE()
B_SPLINE_SURFACE(5,1,((#235003,#235004),(#235005,#235006),(#235007,#235008),
(#235009,#235010),(#235011,#235012),(#235013,#235014),(#235015,#235016),
(#235017,#235018),(#235019,#235020),(#235021,#235022),(#235023,#235024),
(#235025,#235026),(#235027,#235028),(#235029,#235030),(#235031,#235032),
(#235033,#235034),(#235035,#235036),(#235037,#235038),(#235039,#235040),
(#235041,#235042),(#235043,#235044),(#235045,#235046),(#235047,#235048),
(#235049,#235050),(#235051,#235052),(#235053,#235054),(#235055,#235056),
(#235057,#235058),(#235059,#235060),(#235061,#235062),(#235063,#235064),
(#235065,#235066),(#235067,#235068),(#235069,#235070),(#235071,#235072),
(#235073,#235074),(#235075,#235076),(#235077,#235078),(#235079,#235080),
(#235081,#235082),(#235083,#235084),(#235085,#235086),(#235087,#235088),
(#235089,#235090),(#235091,#235092),(#235093,#235094),(#235095,#235096),
(#235097,#235098),(#235099,#235100),(#235101,#235102),(#235103,#235104),
(#235105,#235106),(#235107,#235108),(#235109,#235110),(#235111,#235112),
(#235113,#235114),(#235115,#235116),(#235117,#235118),(#235119,#235120),
(#235121,#235122),(#235123,#235124),(#235125,#235126),(#235127,#235128),
(#235129,#235130),(#235131,#235132),(#235133,#235134),(#235135,#235136),
(#235137,#235138),(#235139,#235140),(#235141,#235142),(#235143,#235144),
(#235145,#235146),(#235147,#235148),(#235149,#235150),(#235151,#235152),
(#235153,#235154),(#235155,#235156),(#235157,#235158),(#235159,#235160),
(#235161,#235162),(#235163,#235164),(#235165,#235166),(#235167,#235168),
(#235169,#235170),(#235171,#235172),(#235173,#235174),(#235175,#235176),
(#235177,#235178),(#235179,#235180),(#235181,#235182),(#235183,#235184),
(#235185,#235186),(#235187,#235188),(#235189,#235190),(#235191,#235192),
(#235193,#235194),(#235195,#235196),(#235197,#235198),(#235199,#235200),
(#235201,#235202),(#235203,#235204),(#235205,#235206),(#235207,#235208),
(#235209,#235210),(#235211,#235212),(#235213,#235214),(#235215,#235216),
(#235217,#235218),(#235219,#235220),(#235221,#235222),(#235223,#235224),
(#235225,#235226),(#235227,#235228),(#235229,#235230),(#235231,#235232),
(#235233,#235234),(#235235,#235236),(#235237,#235238),(#235239,#235240),
(#235241,#235242),(#235243,#235244),(#235245,#235246),(#235247,#235248),
(#235249,#235250),(#235251,#235252),(#235253,#235254),(#235255,#235256),
(#235257,#235258),(#235259,#235260),(#235261,#235262),(#235263,#235264),
(#235265,#235266),(#235267,#235268),(#235269,#235270),(#235271,#235272),
(#235273,#235274),(#235275,#235276),(#235277,#235278),(#235279,#235280),
(#235281,#235282),(#235283,#235284),(#235285,#235286),(#235287,#235288),
(#235289,#235290),(#235291,#235292),(#235293,#235294),(#235295,#235296),
(#235297,#235298),(#235299,#235300),(#235301,#235302),(#235303,#235304),
(#235305,#235306),(#235307,#235308),(#235309,#235310),(#235311,#235312),
(#235313,#235314),(#235315,#235316),(#235317,#235318),(#235319,#235320),
(#235321,#235322),(#235323,#235324),(#235325,#235326),(#235327,#235328),
(#235329,#235330),(#235331,#235332),(#235333,#235334),(#235335,#235336),
(#235337,#235338),(#235339,#235340),(#235341,#235342),(#235343,#235344),
(#235345,#235346),(#235347,#235348),(#235349,#235350),(#235351,#235352),
(#235353,#235354),(#235355,#235356),(#235357,#235358),(#235359,#235360),
(#235361,#235362),(#235363,#235364),(#235365,#235366),(#235367,#235368),
(#235369,#235370),(#235371,#235372),(#235373,#235374),(#235375,#235376),
(#235377,#235378),(#235379,#235380),(#235381,#235382),(#235383,#235384),
(#235385,#235386),(#235387,#235388),(#235389,#235390),(#235391,#235392),
(#235393,#235394),(#235395,#235396),(#235397,#235398),(#235399,#235400),
(#235401,#235402),(#235403,#235404),(#235405,#235406),(#235407,#235408),
(#235409,#235410),(#235411,#235412)),.UNSPECIFIED.,.F.,.F.,.F.)
B_SPLINE_SURFACE_WITH_KNOTS((6,1,1,1,1,1,1,1,1,1,1,1,1,1,1,1,1,1,1,1,1,
1,1,1,1,1,1,1,1,1,1,1,1,1,1,1,1,1,1,1,1,1,1,1,1,1,1,1,1,1,1,1,1,1,1,1,1,
1,1,1,1,1,1,1,1,1,1,1,1,1,1,1,1,1,1,1,1,1,1,1,1,1,1,1,1,1,1,1,1,1,1,1,1,
1,1,1,1,1,1,1,1,1,1,1,1,1,1,1,1,1,1,1,1,1,1,1,1,1,1,1,1,1,1,1,1,1,1,1,1,
1,1,1,1,1,1,1,1,1,1,1,1,1,1,1,1,1,1,1,1,1,1,1,1,1,1,1,1,1,1,1,1,1,1,1,1,
1,1,1,1,1,1,1,1,1,1,1,1,1,1,1,1,1,1,1,1,1,1,1,1,1,1,1,1,1,1,1,1,1,1,1,6),
(2,2),(0.,0.005,0.01,0.015,0.02,0.025,0.03,0.035,0.04,0.045,0.05,0.055,
0.06,0.065,0.07,0.075,0.08,0.085,0.09,0.095,0.1,0.105,0.11,0.115,0.12,0.125,
0.13,0.135,0.14,0.145,0.15,0.155,0.16,0.165,0.17,0.175,0.18,0.185,0.19,
0.195,0.2,0.205,0.21,0.215,0.22,0.225,0.23,0.235,0.24,0.245,0.25,0.255,
0.26,0.265,0.27,0.275,0.28,0.285,0.29,0.295,0.3,0.305,0.31,0.315,0.32,0.325,
0.33,0.335,0.34,0.345,0.35,0.355,0.36,0.365,0.37,0.375,0.38,0.385,0.39,
0.395,0.4,0.405,0.41,0.415,0.42,0.425,0.43,0.435,0.44,0.445,0.45,0.455,
0.46,0.465,0.47,0.475,0.48,0.485,0.49,0.495,0.5,0.505,0.51,0.515,0.52,0.525,
0.53,0.535,0.54,0.545,0.55,0.555,0.56,0.565,0.57,0.575,0.58,0.585,0.59,
0.595,0.6,0.605,0.61,0.615,0.62,0.625,0.63,0.635,0.64,0.645,0.65,0.655,
0.66,0.665,0.67,0.675,0.68,0.685,0.690000000000001,0.695000000000001,0.700000000000001,
0.705000000000001,0.710000000000001,0.715000000000001,0.720000000000001,
0.725000000000001,0.730000000000001,0.735000000000001,0.740000000000001,
0.745000000000001,0.750000000000001,0.755000000000001,0.760000000000001,
0.765000000000001,0.770000000000001,0.775000000000001,0.780000000000001,
0.785000000000001,0.790000000000001,0.795000000000001,0.800000000000001,
0.805000000000001,0.810000000000001,0.815000000000001,0.820000000000001,
0.825000000000001,0.830000000000001,0.835000000000001,0.840000000000001,
0.845000000000001,0.850000000000001,0.855000000000001,0.860000000000001,
0.865000000000001,0.870000000000001,0.875000000000001,0.880000000000001,
0.885000000000001,0.890000000000001,0.895000000000001,0.900000000000001,
0.905000000000001,0.910000000000001,0.915000000000001,0.920000000000001,
0.925000000000001,0.930000000000001,0.935000000000001,0.940000000000001,
0.945000000000001,0.950000000000001,0.955000000000001,0.960000000000001,
0.965000000000001,0.970000000000001,0.975000000000001,0.980000000000001,
0.985000000000001,0.990000000000001,0.995000000000001,1.),(0.,1.2),
 .UNSPECIFIED.)
GEOMETRIC_REPRESENTATION_ITEM()
RATIONAL_B_SPLINE_SURFACE(((1.,1.),(1.,1.),(1.,1.),(1.,1.),(1.,1.),(1.,
1.),(1.,1.),(1.,1.),(1.,1.),(1.,1.),(1.,1.),(1.,1.),(1.,1.),(1.,1.),(1.,
1.),(1.,1.),(1.,1.),(1.,1.),(1.,1.),(1.,1.),(1.,1.),(1.,1.),(1.,1.),(1.,
1.),(1.,1.),(1.,1.),(1.,1.),(1.,1.),(1.,1.),(1.,1.),(1.,1.),(1.,1.),(1.,
1.),(1.,1.),(1.,1.),(1.,1.),(1.,1.),(1.,1.),(1.,1.),(1.,1.),(1.,1.),(1.,
1.),(1.,1.),(1.,1.),(1.,1.),(1.,1.),(1.,1.),(1.,1.),(1.,1.),(1.,1.),(1.,
1.),(1.,1.),(1.,1.),(1.,1.),(1.,1.),(1.,1.),(1.,1.),(1.,1.),(1.,1.),(1.,
1.),(1.,1.),(1.,1.),(1.,1.),(1.,1.),(1.,1.),(1.,1.),(1.,1.),(1.,1.),(1.,
1.),(1.,1.),(1.,1.),(1.,1.),(1.,1.),(1.,1.),(1.,1.),(1.,1.),(1.,1.),(1.,
1.),(1.,1.),(1.,1.),(1.,1.),(1.,1.),(1.,1.),(1.,1.),(1.,1.),(1.,1.),(1.,
1.),(1.,1.),(1.,1.),(1.,1.),(1.,1.),(1.,1.),(1.,1.),(1.,1.),(1.,1.),(1.,
1.),(1.,1.),(1.,1.),(1.,1.),(1.,1.),(1.,1.),(1.,1.),(1.,1.),(1.,1.),(1.,
1.),(1.,1.),(1.,1.),(1.,1.),(1.,1.),(1.,1.),(1.,1.),(1.,1.),(1.,1.),(1.,
1.),(1.,1.),(1.,1.),(1.,1.),(1.,1.),(1.,1.),(1.,1.),(1.,1.),(1.,1.),(1.,
1.),(1.,1.),(1.,1.),(1.,1.),(1.,1.),(1.,1.),(1.,1.),(1.,1.),(1.,1.),(1.,
1.),(1.,1.),(1.,1.),(1.,1.),(1.,1.),(1.,1.),(1.,1.),(1.,1.),(1.,1.),(1.,
1.),(1.,1.),(1.,1.),(1.,1.),(1.,1.),(1.,1.),(1.,1.),(1.,1.),(1.,1.),(1.,
1.),(1.,1.),(1.,1.),(1.,1.),(1.,1.),(1.,1.),(1.,1.),(1.,1.),(1.,1.),(1.,
1.),(1.,1.),(1.,1.),(1.,1.),(1.,1.),(1.,1.),(1.,1.),(1.,1.),(1.,1.),(1.,
1.),(1.,1.),(1.,1.),(1.,1.),(1.,1.),(1.,1.),(1.,1.),(1.,1.),(1.,1.),(1.,
1.),(1.,1.),(1.,1.),(1.,1.),(1.,1.),(1.,1.),(1.,1.),(1.,1.),(1.,1.),(1.,
1.),(1.,1.),(1.,1.),(1.,1.),(1.,1.),(1.,1.),(1.,1.),(1.,1.),(1.,1.),(1.,
1.),(1.,1.),(1.,1.),(1.,1.),(1.,1.),(1.,1.),(1.,1.),(1.,1.),(1.,1.),(1.,
1.),(1.,1.)))
REPRESENTATION_ITEM('')
SURFACE()
);
#1099=(
BOUNDED_SURFACE()
B_SPLINE_SURFACE(5,1,((#235832,#235833),(#235834,#235835),(#235836,#235837),
(#235838,#235839),(#235840,#235841),(#235842,#235843),(#235844,#235845),
(#235846,#235847),(#235848,#235849),(#235850,#235851),(#235852,#235853),
(#235854,#235855),(#235856,#235857),(#235858,#235859),(#235860,#235861),
(#235862,#235863),(#235864,#235865),(#235866,#235867),(#235868,#235869),
(#235870,#235871),(#235872,#235873),(#235874,#235875),(#235876,#235877),
(#235878,#235879),(#235880,#235881),(#235882,#235883),(#235884,#235885),
(#235886,#235887),(#235888,#235889),(#235890,#235891),(#235892,#235893),
(#235894,#235895),(#235896,#235897),(#235898,#235899),(#235900,#235901),
(#235902,#235903),(#235904,#235905),(#235906,#235907),(#235908,#235909),
(#235910,#235911),(#235912,#235913),(#235914,#235915),(#235916,#235917),
(#235918,#235919),(#235920,#235921),(#235922,#235923),(#235924,#235925),
(#235926,#235927),(#235928,#235929),(#235930,#235931),(#235932,#235933),
(#235934,#235935),(#235936,#235937),(#235938,#235939),(#235940,#235941),
(#235942,#235943),(#235944,#235945),(#235946,#235947),(#235948,#235949),
(#235950,#235951),(#235952,#235953),(#235954,#235955),(#235956,#235957),
(#235958,#235959),(#235960,#235961),(#235962,#235963),(#235964,#235965),
(#235966,#235967),(#235968,#235969),(#235970,#235971),(#235972,#235973),
(#235974,#235975),(#235976,#235977),(#235978,#235979),(#235980,#235981),
(#235982,#235983),(#235984,#235985),(#235986,#235987),(#235988,#235989),
(#235990,#235991),(#235992,#235993),(#235994,#235995),(#235996,#235997),
(#235998,#235999),(#236000,#236001),(#236002,#236003),(#236004,#236005),
(#236006,#236007),(#236008,#236009),(#236010,#236011),(#236012,#236013),
(#236014,#236015),(#236016,#236017),(#236018,#236019),(#236020,#236021),
(#236022,#236023),(#236024,#236025),(#236026,#236027),(#236028,#236029),
(#236030,#236031),(#236032,#236033),(#236034,#236035),(#236036,#236037),
(#236038,#236039),(#236040,#236041),(#236042,#236043),(#236044,#236045),
(#236046,#236047),(#236048,#236049),(#236050,#236051),(#236052,#236053),
(#236054,#236055),(#236056,#236057),(#236058,#236059),(#236060,#236061),
(#236062,#236063),(#236064,#236065),(#236066,#236067),(#236068,#236069),
(#236070,#236071),(#236072,#236073),(#236074,#236075),(#236076,#236077),
(#236078,#236079),(#236080,#236081),(#236082,#236083),(#236084,#236085),
(#236086,#236087),(#236088,#236089),(#236090,#236091),(#236092,#236093),
(#236094,#236095),(#236096,#236097),(#236098,#236099),(#236100,#236101),
(#236102,#236103),(#236104,#236105),(#236106,#236107),(#236108,#236109),
(#236110,#236111),(#236112,#236113),(#236114,#236115),(#236116,#236117),
(#236118,#236119),(#236120,#236121),(#236122,#236123),(#236124,#236125),
(#236126,#236127),(#236128,#236129),(#236130,#236131),(#236132,#236133),
(#236134,#236135),(#236136,#236137),(#236138,#236139),(#236140,#236141),
(#236142,#236143),(#236144,#236145),(#236146,#236147),(#236148,#236149),
(#236150,#236151),(#236152,#236153),(#236154,#236155),(#236156,#236157),
(#236158,#236159),(#236160,#236161),(#236162,#236163),(#236164,#236165),
(#236166,#236167),(#236168,#236169),(#236170,#236171),(#236172,#236173),
(#236174,#236175),(#236176,#236177),(#236178,#236179),(#236180,#236181),
(#236182,#236183),(#236184,#236185),(#236186,#236187),(#236188,#236189),
(#236190,#236191),(#236192,#236193),(#236194,#236195),(#236196,#236197),
(#236198,#236199),(#236200,#236201),(#236202,#236203),(#236204,#236205),
(#236206,#236207),(#236208,#236209),(#236210,#236211),(#236212,#236213),
(#236214,#236215),(#236216,#236217),(#236218,#236219),(#236220,#236221),
(#236222,#236223),(#236224,#236225),(#236226,#236227),(#236228,#236229),
(#236230,#236231),(#236232,#236233),(#236234,#236235),(#236236,#236237),
(#236238,#236239),(#236240,#236241)),.UNSPECIFIED.,.F.,.F.,.F.)
B_SPLINE_SURFACE_WITH_KNOTS((6,1,1,1,1,1,1,1,1,1,1,1,1,1,1,1,1,1,1,1,1,
1,1,1,1,1,1,1,1,1,1,1,1,1,1,1,1,1,1,1,1,1,1,1,1,1,1,1,1,1,1,1,1,1,1,1,1,
1,1,1,1,1,1,1,1,1,1,1,1,1,1,1,1,1,1,1,1,1,1,1,1,1,1,1,1,1,1,1,1,1,1,1,1,
1,1,1,1,1,1,1,1,1,1,1,1,1,1,1,1,1,1,1,1,1,1,1,1,1,1,1,1,1,1,1,1,1,1,1,1,
1,1,1,1,1,1,1,1,1,1,1,1,1,1,1,1,1,1,1,1,1,1,1,1,1,1,1,1,1,1,1,1,1,1,1,1,
1,1,1,1,1,1,1,1,1,1,1,1,1,1,1,1,1,1,1,1,1,1,1,1,1,1,1,1,1,1,1,1,1,1,1,6),
(2,2),(-1.,-0.995000000000001,-0.990000000000001,-0.985000000000001,-0.980000000000001,
-0.975000000000001,-0.970000000000001,-0.965000000000001,-0.960000000000001,
-0.955000000000001,-0.950000000000001,-0.945000000000001,-0.940000000000001,
-0.935000000000001,-0.930000000000001,-0.925000000000001,-0.920000000000001,
-0.915000000000001,-0.910000000000001,-0.905000000000001,-0.900000000000001,
-0.895000000000001,-0.890000000000001,-0.885000000000001,-0.880000000000001,
-0.875000000000001,-0.870000000000001,-0.865000000000001,-0.860000000000001,
-0.855000000000001,-0.850000000000001,-0.845000000000001,-0.840000000000001,
-0.835000000000001,-0.830000000000001,-0.825000000000001,-0.820000000000001,
-0.815000000000001,-0.810000000000001,-0.805000000000001,-0.800000000000001,
-0.795000000000001,-0.790000000000001,-0.785000000000001,-0.780000000000001,
-0.775000000000001,-0.770000000000001,-0.765000000000001,-0.760000000000001,
-0.755000000000001,-0.750000000000001,-0.745000000000001,-0.740000000000001,
-0.735000000000001,-0.730000000000001,-0.725000000000001,-0.720000000000001,
-0.715000000000001,-0.710000000000001,-0.705000000000001,-0.700000000000001,
-0.695000000000001,-0.690000000000001,-0.685,-0.68,-0.675,-0.67,-0.665,
-0.66,-0.655,-0.65,-0.645,-0.64,-0.635,-0.63,-0.625,-0.62,-0.615,-0.61,
-0.605,-0.6,-0.595,-0.59,-0.585,-0.58,-0.575,-0.57,-0.565,-0.56,-0.555,
-0.55,-0.545,-0.54,-0.535,-0.53,-0.525,-0.52,-0.515,-0.51,-0.505,-0.5,-0.495,
-0.49,-0.485,-0.48,-0.475,-0.47,-0.465,-0.46,-0.455,-0.45,-0.445,-0.44,
-0.435,-0.43,-0.425,-0.42,-0.415,-0.41,-0.405,-0.4,-0.395,-0.39,-0.385,
-0.38,-0.375,-0.37,-0.365,-0.36,-0.355,-0.35,-0.345,-0.34,-0.335,-0.33,
-0.325,-0.32,-0.315,-0.31,-0.305,-0.3,-0.295,-0.29,-0.285,-0.28,-0.275,
-0.27,-0.265,-0.26,-0.255,-0.25,-0.245,-0.24,-0.235,-0.23,-0.225,-0.22,
-0.215,-0.21,-0.205,-0.2,-0.195,-0.19,-0.185,-0.18,-0.175,-0.17,-0.165,
-0.16,-0.155,-0.15,-0.145,-0.14,-0.135,-0.13,-0.125,-0.12,-0.115,-0.11,
-0.105,-0.1,-0.095,-0.09,-0.085,-0.08,-0.075,-0.07,-0.065,-0.06,-0.055,
-0.05,-0.045,-0.04,-0.035,-0.03,-0.025,-0.02,-0.015,-0.01,-0.005,0.),(0.,
1.2),.UNSPECIFIED.)
GEOMETRIC_REPRESENTATION_ITEM()
RATIONAL_B_SPLINE_SURFACE(((1.,1.),(1.,1.),(1.,1.),(1.,1.),(1.,1.),(1.,
1.),(1.,1.),(1.,1.),(1.,1.),(1.,1.),(1.,1.),(1.,1.),(1.,1.),(1.,1.),(1.,
1.),(1.,1.),(1.,1.),(1.,1.),(1.,1.),(1.,1.),(1.,1.),(1.,1.),(1.,1.),(1.,
1.),(1.,1.),(1.,1.),(1.,1.),(1.,1.),(1.,1.),(1.,1.),(1.,1.),(1.,1.),(1.,
1.),(1.,1.),(1.,1.),(1.,1.),(1.,1.),(1.,1.),(1.,1.),(1.,1.),(1.,1.),(1.,
1.),(1.,1.),(1.,1.),(1.,1.),(1.,1.),(1.,1.),(1.,1.),(1.,1.),(1.,1.),(1.,
1.),(1.,1.),(1.,1.),(1.,1.),(1.,1.),(1.,1.),(1.,1.),(1.,1.),(1.,1.),(1.,
1.),(1.,1.),(1.,1.),(1.,1.),(1.,1.),(1.,1.),(1.,1.),(1.,1.),(1.,1.),(1.,
1.),(1.,1.),(1.,1.),(1.,1.),(1.,1.),(1.,1.),(1.,1.),(1.,1.),(1.,1.),(1.,
1.),(1.,1.),(1.,1.),(1.,1.),(1.,1.),(1.,1.),(1.,1.),(1.,1.),(1.,1.),(1.,
1.),(1.,1.),(1.,1.),(1.,1.),(1.,1.),(1.,1.),(1.,1.),(1.,1.),(1.,1.),(1.,
1.),(1.,1.),(1.,1.),(1.,1.),(1.,1.),(1.,1.),(1.,1.),(1.,1.),(1.,1.),(1.,
1.),(1.,1.),(1.,1.),(1.,1.),(1.,1.),(1.,1.),(1.,1.),(1.,1.),(1.,1.),(1.,
1.),(1.,1.),(1.,1.),(1.,1.),(1.,1.),(1.,1.),(1.,1.),(1.,1.),(1.,1.),(1.,
1.),(1.,1.),(1.,1.),(1.,1.),(1.,1.),(1.,1.),(1.,1.),(1.,1.),(1.,1.),(1.,
1.),(1.,1.),(1.,1.),(1.,1.),(1.,1.),(1.,1.),(1.,1.),(1.,1.),(1.,1.),(1.,
1.),(1.,1.),(1.,1.),(1.,1.),(1.,1.),(1.,1.),(1.,1.),(1.,1.),(1.,1.),(1.,
1.),(1.,1.),(1.,1.),(1.,1.),(1.,1.),(1.,1.),(1.,1.),(1.,1.),(1.,1.),(1.,
1.),(1.,1.),(1.,1.),(1.,1.),(1.,1.),(1.,1.),(1.,1.),(1.,1.),(1.,1.),(1.,
1.),(1.,1.),(1.,1.),(1.,1.),(1.,1.),(1.,1.),(1.,1.),(1.,1.),(1.,1.),(1.,
1.),(1.,1.),(1.,1.),(1.,1.),(1.,1.),(1.,1.),(1.,1.),(1.,1.),(1.,1.),(1.,
1.),(1.,1.),(1.,1.),(1.,1.),(1.,1.),(1.,1.),(1.,1.),(1.,1.),(1.,1.),(1.,
1.),(1.,1.),(1.,1.),(1.,1.),(1.,1.),(1.,1.),(1.,1.),(1.,1.),(1.,1.),(1.,
1.),(1.,1.)))
REPRESENTATION_ITEM('')
SURFACE()
);
#1100=(
BOUNDED_SURFACE()
B_SPLINE_SURFACE(5,1,((#236655,#236656),(#236657,#236658),(#236659,#236660),
(#236661,#236662),(#236663,#236664),(#236665,#236666),(#236667,#236668),
(#236669,#236670),(#236671,#236672),(#236673,#236674),(#236675,#236676),
(#236677,#236678),(#236679,#236680),(#236681,#236682),(#236683,#236684),
(#236685,#236686),(#236687,#236688),(#236689,#236690),(#236691,#236692),
(#236693,#236694),(#236695,#236696),(#236697,#236698),(#236699,#236700),
(#236701,#236702),(#236703,#236704),(#236705,#236706),(#236707,#236708),
(#236709,#236710),(#236711,#236712),(#236713,#236714),(#236715,#236716),
(#236717,#236718),(#236719,#236720),(#236721,#236722),(#236723,#236724),
(#236725,#236726),(#236727,#236728),(#236729,#236730),(#236731,#236732),
(#236733,#236734),(#236735,#236736),(#236737,#236738),(#236739,#236740),
(#236741,#236742),(#236743,#236744),(#236745,#236746),(#236747,#236748),
(#236749,#236750),(#236751,#236752),(#236753,#236754),(#236755,#236756),
(#236757,#236758),(#236759,#236760),(#236761,#236762),(#236763,#236764),
(#236765,#236766),(#236767,#236768),(#236769,#236770),(#236771,#236772),
(#236773,#236774),(#236775,#236776),(#236777,#236778),(#236779,#236780),
(#236781,#236782),(#236783,#236784),(#236785,#236786),(#236787,#236788),
(#236789,#236790),(#236791,#236792),(#236793,#236794),(#236795,#236796),
(#236797,#236798),(#236799,#236800),(#236801,#236802),(#236803,#236804),
(#236805,#236806),(#236807,#236808),(#236809,#236810),(#236811,#236812),
(#236813,#236814),(#236815,#236816),(#236817,#236818),(#236819,#236820),
(#236821,#236822),(#236823,#236824),(#236825,#236826),(#236827,#236828),
(#236829,#236830),(#236831,#236832),(#236833,#236834),(#236835,#236836),
(#236837,#236838),(#236839,#236840),(#236841,#236842),(#236843,#236844),
(#236845,#236846),(#236847,#236848),(#236849,#236850),(#236851,#236852),
(#236853,#236854),(#236855,#236856),(#236857,#236858),(#236859,#236860),
(#236861,#236862),(#236863,#236864),(#236865,#236866),(#236867,#236868),
(#236869,#236870),(#236871,#236872),(#236873,#236874),(#236875,#236876),
(#236877,#236878),(#236879,#236880),(#236881,#236882),(#236883,#236884),
(#236885,#236886),(#236887,#236888),(#236889,#236890),(#236891,#236892),
(#236893,#236894),(#236895,#236896),(#236897,#236898),(#236899,#236900),
(#236901,#236902),(#236903,#236904),(#236905,#236906),(#236907,#236908),
(#236909,#236910),(#236911,#236912),(#236913,#236914),(#236915,#236916),
(#236917,#236918),(#236919,#236920),(#236921,#236922),(#236923,#236924),
(#236925,#236926),(#236927,#236928),(#236929,#236930),(#236931,#236932),
(#236933,#236934),(#236935,#236936),(#236937,#236938),(#236939,#236940),
(#236941,#236942),(#236943,#236944),(#236945,#236946),(#236947,#236948),
(#236949,#236950),(#236951,#236952),(#236953,#236954),(#236955,#236956),
(#236957,#236958),(#236959,#236960),(#236961,#236962),(#236963,#236964),
(#236965,#236966),(#236967,#236968),(#236969,#236970),(#236971,#236972),
(#236973,#236974),(#236975,#236976),(#236977,#236978),(#236979,#236980),
(#236981,#236982),(#236983,#236984),(#236985,#236986),(#236987,#236988),
(#236989,#236990),(#236991,#236992),(#236993,#236994),(#236995,#236996),
(#236997,#236998),(#236999,#237000),(#237001,#237002),(#237003,#237004),
(#237005,#237006),(#237007,#237008),(#237009,#237010),(#237011,#237012),
(#237013,#237014),(#237015,#237016),(#237017,#237018),(#237019,#237020),
(#237021,#237022),(#237023,#237024),(#237025,#237026),(#237027,#237028),
(#237029,#237030),(#237031,#237032),(#237033,#237034),(#237035,#237036),
(#237037,#237038),(#237039,#237040),(#237041,#237042),(#237043,#237044),
(#237045,#237046),(#237047,#237048),(#237049,#237050),(#237051,#237052),
(#237053,#237054),(#237055,#237056),(#237057,#237058),(#237059,#237060),
(#237061,#237062),(#237063,#237064)),.UNSPECIFIED.,.F.,.F.,.F.)
B_SPLINE_SURFACE_WITH_KNOTS((6,1,1,1,1,1,1,1,1,1,1,1,1,1,1,1,1,1,1,1,1,
1,1,1,1,1,1,1,1,1,1,1,1,1,1,1,1,1,1,1,1,1,1,1,1,1,1,1,1,1,1,1,1,1,1,1,1,
1,1,1,1,1,1,1,1,1,1,1,1,1,1,1,1,1,1,1,1,1,1,1,1,1,1,1,1,1,1,1,1,1,1,1,1,
1,1,1,1,1,1,1,1,1,1,1,1,1,1,1,1,1,1,1,1,1,1,1,1,1,1,1,1,1,1,1,1,1,1,1,1,
1,1,1,1,1,1,1,1,1,1,1,1,1,1,1,1,1,1,1,1,1,1,1,1,1,1,1,1,1,1,1,1,1,1,1,1,
1,1,1,1,1,1,1,1,1,1,1,1,1,1,1,1,1,1,1,1,1,1,1,1,1,1,1,1,1,1,1,1,1,1,1,6),
(2,2),(0.,0.005,0.01,0.015,0.02,0.025,0.03,0.035,0.04,0.045,0.05,0.055,
0.06,0.065,0.07,0.075,0.08,0.085,0.09,0.095,0.1,0.105,0.11,0.115,0.12,0.125,
0.13,0.135,0.14,0.145,0.15,0.155,0.16,0.165,0.17,0.175,0.18,0.185,0.19,
0.195,0.2,0.205,0.21,0.215,0.22,0.225,0.23,0.235,0.24,0.245,0.25,0.255,
0.26,0.265,0.27,0.275,0.28,0.285,0.29,0.295,0.3,0.305,0.31,0.315,0.32,0.325,
0.33,0.335,0.34,0.345,0.35,0.355,0.36,0.365,0.37,0.375,0.38,0.385,0.39,
0.395,0.4,0.405,0.41,0.415,0.42,0.425,0.43,0.435,0.44,0.445,0.45,0.455,
0.46,0.465,0.47,0.475,0.48,0.485,0.49,0.495,0.5,0.505,0.51,0.515,0.52,0.525,
0.53,0.535,0.54,0.545,0.55,0.555,0.56,0.565,0.57,0.575,0.58,0.585,0.59,
0.595,0.6,0.605,0.61,0.615,0.62,0.625,0.63,0.635,0.64,0.645,0.65,0.655,
0.66,0.665,0.67,0.675,0.68,0.685,0.690000000000001,0.695000000000001,0.700000000000001,
0.705000000000001,0.710000000000001,0.715000000000001,0.720000000000001,
0.725000000000001,0.730000000000001,0.735000000000001,0.740000000000001,
0.745000000000001,0.750000000000001,0.755000000000001,0.760000000000001,
0.765000000000001,0.770000000000001,0.775000000000001,0.780000000000001,
0.785000000000001,0.790000000000001,0.795000000000001,0.800000000000001,
0.805000000000001,0.810000000000001,0.815000000000001,0.820000000000001,
0.825000000000001,0.830000000000001,0.835000000000001,0.840000000000001,
0.845000000000001,0.850000000000001,0.855000000000001,0.860000000000001,
0.865000000000001,0.870000000000001,0.875000000000001,0.880000000000001,
0.885000000000001,0.890000000000001,0.895000000000001,0.900000000000001,
0.905000000000001,0.910000000000001,0.915000000000001,0.920000000000001,
0.925000000000001,0.930000000000001,0.935000000000001,0.940000000000001,
0.945000000000001,0.950000000000001,0.955000000000001,0.960000000000001,
0.965000000000001,0.970000000000001,0.975000000000001,0.980000000000001,
0.985000000000001,0.990000000000001,0.995000000000001,1.),(0.,1.2),
 .UNSPECIFIED.)
GEOMETRIC_REPRESENTATION_ITEM()
RATIONAL_B_SPLINE_SURFACE(((1.,1.),(1.,1.),(1.,1.),(1.,1.),(1.,1.),(1.,
1.),(1.,1.),(1.,1.),(1.,1.),(1.,1.),(1.,1.),(1.,1.),(1.,1.),(1.,1.),(1.,
1.),(1.,1.),(1.,1.),(1.,1.),(1.,1.),(1.,1.),(1.,1.),(1.,1.),(1.,1.),(1.,
1.),(1.,1.),(1.,1.),(1.,1.),(1.,1.),(1.,1.),(1.,1.),(1.,1.),(1.,1.),(1.,
1.),(1.,1.),(1.,1.),(1.,1.),(1.,1.),(1.,1.),(1.,1.),(1.,1.),(1.,1.),(1.,
1.),(1.,1.),(1.,1.),(1.,1.),(1.,1.),(1.,1.),(1.,1.),(1.,1.),(1.,1.),(1.,
1.),(1.,1.),(1.,1.),(1.,1.),(1.,1.),(1.,1.),(1.,1.),(1.,1.),(1.,1.),(1.,
1.),(1.,1.),(1.,1.),(1.,1.),(1.,1.),(1.,1.),(1.,1.),(1.,1.),(1.,1.),(1.,
1.),(1.,1.),(1.,1.),(1.,1.),(1.,1.),(1.,1.),(1.,1.),(1.,1.),(1.,1.),(1.,
1.),(1.,1.),(1.,1.),(1.,1.),(1.,1.),(1.,1.),(1.,1.),(1.,1.),(1.,1.),(1.,
1.),(1.,1.),(1.,1.),(1.,1.),(1.,1.),(1.,1.),(1.,1.),(1.,1.),(1.,1.),(1.,
1.),(1.,1.),(1.,1.),(1.,1.),(1.,1.),(1.,1.),(1.,1.),(1.,1.),(1.,1.),(1.,
1.),(1.,1.),(1.,1.),(1.,1.),(1.,1.),(1.,1.),(1.,1.),(1.,1.),(1.,1.),(1.,
1.),(1.,1.),(1.,1.),(1.,1.),(1.,1.),(1.,1.),(1.,1.),(1.,1.),(1.,1.),(1.,
1.),(1.,1.),(1.,1.),(1.,1.),(1.,1.),(1.,1.),(1.,1.),(1.,1.),(1.,1.),(1.,
1.),(1.,1.),(1.,1.),(1.,1.),(1.,1.),(1.,1.),(1.,1.),(1.,1.),(1.,1.),(1.,
1.),(1.,1.),(1.,1.),(1.,1.),(1.,1.),(1.,1.),(1.,1.),(1.,1.),(1.,1.),(1.,
1.),(1.,1.),(1.,1.),(1.,1.),(1.,1.),(1.,1.),(1.,1.),(1.,1.),(1.,1.),(1.,
1.),(1.,1.),(1.,1.),(1.,1.),(1.,1.),(1.,1.),(1.,1.),(1.,1.),(1.,1.),(1.,
1.),(1.,1.),(1.,1.),(1.,1.),(1.,1.),(1.,1.),(1.,1.),(1.,1.),(1.,1.),(1.,
1.),(1.,1.),(1.,1.),(1.,1.),(1.,1.),(1.,1.),(1.,1.),(1.,1.),(1.,1.),(1.,
1.),(1.,1.),(1.,1.),(1.,1.),(1.,1.),(1.,1.),(1.,1.),(1.,1.),(1.,1.),(1.,
1.),(1.,1.),(1.,1.),(1.,1.),(1.,1.),(1.,1.),(1.,1.),(1.,1.),(1.,1.),(1.,
1.),(1.,1.)))
REPRESENTATION_ITEM('')
SURFACE()
);
#1101=(
BOUNDED_SURFACE()
B_SPLINE_SURFACE(5,1,((#237484,#237485),(#237486,#237487),(#237488,#237489),
(#237490,#237491),(#237492,#237493),(#237494,#237495),(#237496,#237497),
(#237498,#237499),(#237500,#237501),(#237502,#237503),(#237504,#237505),
(#237506,#237507),(#237508,#237509),(#237510,#237511),(#237512,#237513),
(#237514,#237515),(#237516,#237517),(#237518,#237519),(#237520,#237521),
(#237522,#237523),(#237524,#237525),(#237526,#237527),(#237528,#237529),
(#237530,#237531),(#237532,#237533),(#237534,#237535),(#237536,#237537),
(#237538,#237539),(#237540,#237541),(#237542,#237543),(#237544,#237545),
(#237546,#237547),(#237548,#237549),(#237550,#237551),(#237552,#237553),
(#237554,#237555),(#237556,#237557),(#237558,#237559),(#237560,#237561),
(#237562,#237563),(#237564,#237565),(#237566,#237567),(#237568,#237569),
(#237570,#237571),(#237572,#237573),(#237574,#237575),(#237576,#237577),
(#237578,#237579),(#237580,#237581),(#237582,#237583),(#237584,#237585),
(#237586,#237587),(#237588,#237589),(#237590,#237591),(#237592,#237593),
(#237594,#237595),(#237596,#237597),(#237598,#237599),(#237600,#237601),
(#237602,#237603),(#237604,#237605),(#237606,#237607),(#237608,#237609),
(#237610,#237611),(#237612,#237613),(#237614,#237615),(#237616,#237617),
(#237618,#237619),(#237620,#237621),(#237622,#237623),(#237624,#237625),
(#237626,#237627),(#237628,#237629),(#237630,#237631),(#237632,#237633),
(#237634,#237635),(#237636,#237637),(#237638,#237639),(#237640,#237641),
(#237642,#237643),(#237644,#237645),(#237646,#237647),(#237648,#237649),
(#237650,#237651),(#237652,#237653),(#237654,#237655),(#237656,#237657),
(#237658,#237659),(#237660,#237661),(#237662,#237663),(#237664,#237665),
(#237666,#237667),(#237668,#237669),(#237670,#237671),(#237672,#237673),
(#237674,#237675),(#237676,#237677),(#237678,#237679),(#237680,#237681),
(#237682,#237683),(#237684,#237685),(#237686,#237687),(#237688,#237689),
(#237690,#237691),(#237692,#237693),(#237694,#237695),(#237696,#237697),
(#237698,#237699),(#237700,#237701),(#237702,#237703),(#237704,#237705),
(#237706,#237707),(#237708,#237709),(#237710,#237711),(#237712,#237713),
(#237714,#237715),(#237716,#237717),(#237718,#237719),(#237720,#237721),
(#237722,#237723),(#237724,#237725),(#237726,#237727),(#237728,#237729),
(#237730,#237731),(#237732,#237733),(#237734,#237735),(#237736,#237737),
(#237738,#237739),(#237740,#237741),(#237742,#237743),(#237744,#237745),
(#237746,#237747),(#237748,#237749),(#237750,#237751),(#237752,#237753),
(#237754,#237755),(#237756,#237757),(#237758,#237759),(#237760,#237761),
(#237762,#237763),(#237764,#237765),(#237766,#237767),(#237768,#237769),
(#237770,#237771),(#237772,#237773),(#237774,#237775),(#237776,#237777),
(#237778,#237779),(#237780,#237781),(#237782,#237783),(#237784,#237785),
(#237786,#237787),(#237788,#237789),(#237790,#237791),(#237792,#237793),
(#237794,#237795),(#237796,#237797),(#237798,#237799),(#237800,#237801),
(#237802,#237803),(#237804,#237805),(#237806,#237807),(#237808,#237809),
(#237810,#237811),(#237812,#237813),(#237814,#237815),(#237816,#237817),
(#237818,#237819),(#237820,#237821),(#237822,#237823),(#237824,#237825),
(#237826,#237827),(#237828,#237829),(#237830,#237831),(#237832,#237833),
(#237834,#237835),(#237836,#237837),(#237838,#237839),(#237840,#237841),
(#237842,#237843),(#237844,#237845),(#237846,#237847),(#237848,#237849),
(#237850,#237851),(#237852,#237853),(#237854,#237855),(#237856,#237857),
(#237858,#237859),(#237860,#237861),(#237862,#237863),(#237864,#237865),
(#237866,#237867),(#237868,#237869),(#237870,#237871),(#237872,#237873),
(#237874,#237875),(#237876,#237877),(#237878,#237879),(#237880,#237881),
(#237882,#237883),(#237884,#237885),(#237886,#237887),(#237888,#237889),
(#237890,#237891),(#237892,#237893)),.UNSPECIFIED.,.F.,.F.,.F.)
B_SPLINE_SURFACE_WITH_KNOTS((6,1,1,1,1,1,1,1,1,1,1,1,1,1,1,1,1,1,1,1,1,
1,1,1,1,1,1,1,1,1,1,1,1,1,1,1,1,1,1,1,1,1,1,1,1,1,1,1,1,1,1,1,1,1,1,1,1,
1,1,1,1,1,1,1,1,1,1,1,1,1,1,1,1,1,1,1,1,1,1,1,1,1,1,1,1,1,1,1,1,1,1,1,1,
1,1,1,1,1,1,1,1,1,1,1,1,1,1,1,1,1,1,1,1,1,1,1,1,1,1,1,1,1,1,1,1,1,1,1,1,
1,1,1,1,1,1,1,1,1,1,1,1,1,1,1,1,1,1,1,1,1,1,1,1,1,1,1,1,1,1,1,1,1,1,1,1,
1,1,1,1,1,1,1,1,1,1,1,1,1,1,1,1,1,1,1,1,1,1,1,1,1,1,1,1,1,1,1,1,1,1,1,6),
(2,2),(-1.,-0.995000000000001,-0.990000000000001,-0.985000000000001,-0.980000000000001,
-0.975000000000001,-0.970000000000001,-0.965000000000001,-0.960000000000001,
-0.955000000000001,-0.950000000000001,-0.945000000000001,-0.940000000000001,
-0.935000000000001,-0.930000000000001,-0.925000000000001,-0.920000000000001,
-0.915000000000001,-0.910000000000001,-0.905000000000001,-0.900000000000001,
-0.895000000000001,-0.890000000000001,-0.885000000000001,-0.880000000000001,
-0.875000000000001,-0.870000000000001,-0.865000000000001,-0.860000000000001,
-0.855000000000001,-0.850000000000001,-0.845000000000001,-0.840000000000001,
-0.835000000000001,-0.830000000000001,-0.825000000000001,-0.820000000000001,
-0.815000000000001,-0.810000000000001,-0.805000000000001,-0.800000000000001,
-0.795000000000001,-0.790000000000001,-0.785000000000001,-0.780000000000001,
-0.775000000000001,-0.770000000000001,-0.765000000000001,-0.760000000000001,
-0.755000000000001,-0.750000000000001,-0.745000000000001,-0.740000000000001,
-0.735000000000001,-0.730000000000001,-0.725000000000001,-0.720000000000001,
-0.715000000000001,-0.710000000000001,-0.705000000000001,-0.700000000000001,
-0.695000000000001,-0.690000000000001,-0.685,-0.68,-0.675,-0.67,-0.665,
-0.66,-0.655,-0.65,-0.645,-0.64,-0.635,-0.63,-0.625,-0.62,-0.615,-0.61,
-0.605,-0.6,-0.595,-0.59,-0.585,-0.58,-0.575,-0.57,-0.565,-0.56,-0.555,
-0.55,-0.545,-0.54,-0.535,-0.53,-0.525,-0.52,-0.515,-0.51,-0.505,-0.5,-0.495,
-0.49,-0.485,-0.48,-0.475,-0.47,-0.465,-0.46,-0.455,-0.45,-0.445,-0.44,
-0.435,-0.43,-0.425,-0.42,-0.415,-0.41,-0.405,-0.4,-0.395,-0.39,-0.385,
-0.38,-0.375,-0.37,-0.365,-0.36,-0.355,-0.35,-0.345,-0.34,-0.335,-0.33,
-0.325,-0.32,-0.315,-0.31,-0.305,-0.3,-0.295,-0.29,-0.285,-0.28,-0.275,
-0.27,-0.265,-0.26,-0.255,-0.25,-0.245,-0.24,-0.235,-0.23,-0.225,-0.22,
-0.215,-0.21,-0.205,-0.2,-0.195,-0.19,-0.185,-0.18,-0.175,-0.17,-0.165,
-0.16,-0.155,-0.15,-0.145,-0.14,-0.135,-0.13,-0.125,-0.12,-0.115,-0.11,
-0.105,-0.1,-0.095,-0.09,-0.085,-0.08,-0.075,-0.07,-0.065,-0.06,-0.055,
-0.05,-0.045,-0.04,-0.035,-0.03,-0.025,-0.02,-0.015,-0.01,-0.005,0.),(0.,
1.2),.UNSPECIFIED.)
GEOMETRIC_REPRESENTATION_ITEM()
RATIONAL_B_SPLINE_SURFACE(((1.,1.),(1.,1.),(1.,1.),(1.,1.),(1.,1.),(1.,
1.),(1.,1.),(1.,1.),(1.,1.),(1.,1.),(1.,1.),(1.,1.),(1.,1.),(1.,1.),(1.,
1.),(1.,1.),(1.,1.),(1.,1.),(1.,1.),(1.,1.),(1.,1.),(1.,1.),(1.,1.),(1.,
1.),(1.,1.),(1.,1.),(1.,1.),(1.,1.),(1.,1.),(1.,1.),(1.,1.),(1.,1.),(1.,
1.),(1.,1.),(1.,1.),(1.,1.),(1.,1.),(1.,1.),(1.,1.),(1.,1.),(1.,1.),(1.,
1.),(1.,1.),(1.,1.),(1.,1.),(1.,1.),(1.,1.),(1.,1.),(1.,1.),(1.,1.),(1.,
1.),(1.,1.),(1.,1.),(1.,1.),(1.,1.),(1.,1.),(1.,1.),(1.,1.),(1.,1.),(1.,
1.),(1.,1.),(1.,1.),(1.,1.),(1.,1.),(1.,1.),(1.,1.),(1.,1.),(1.,1.),(1.,
1.),(1.,1.),(1.,1.),(1.,1.),(1.,1.),(1.,1.),(1.,1.),(1.,1.),(1.,1.),(1.,
1.),(1.,1.),(1.,1.),(1.,1.),(1.,1.),(1.,1.),(1.,1.),(1.,1.),(1.,1.),(1.,
1.),(1.,1.),(1.,1.),(1.,1.),(1.,1.),(1.,1.),(1.,1.),(1.,1.),(1.,1.),(1.,
1.),(1.,1.),(1.,1.),(1.,1.),(1.,1.),(1.,1.),(1.,1.),(1.,1.),(1.,1.),(1.,
1.),(1.,1.),(1.,1.),(1.,1.),(1.,1.),(1.,1.),(1.,1.),(1.,1.),(1.,1.),(1.,
1.),(1.,1.),(1.,1.),(1.,1.),(1.,1.),(1.,1.),(1.,1.),(1.,1.),(1.,1.),(1.,
1.),(1.,1.),(1.,1.),(1.,1.),(1.,1.),(1.,1.),(1.,1.),(1.,1.),(1.,1.),(1.,
1.),(1.,1.),(1.,1.),(1.,1.),(1.,1.),(1.,1.),(1.,1.),(1.,1.),(1.,1.),(1.,
1.),(1.,1.),(1.,1.),(1.,1.),(1.,1.),(1.,1.),(1.,1.),(1.,1.),(1.,1.),(1.,
1.),(1.,1.),(1.,1.),(1.,1.),(1.,1.),(1.,1.),(1.,1.),(1.,1.),(1.,1.),(1.,
1.),(1.,1.),(1.,1.),(1.,1.),(1.,1.),(1.,1.),(1.,1.),(1.,1.),(1.,1.),(1.,
1.),(1.,1.),(1.,1.),(1.,1.),(1.,1.),(1.,1.),(1.,1.),(1.,1.),(1.,1.),(1.,
1.),(1.,1.),(1.,1.),(1.,1.),(1.,1.),(1.,1.),(1.,1.),(1.,1.),(1.,1.),(1.,
1.),(1.,1.),(1.,1.),(1.,1.),(1.,1.),(1.,1.),(1.,1.),(1.,1.),(1.,1.),(1.,
1.),(1.,1.),(1.,1.),(1.,1.),(1.,1.),(1.,1.),(1.,1.),(1.,1.),(1.,1.),(1.,
1.),(1.,1.)))
REPRESENTATION_ITEM('')
SURFACE()
);
#1102=(
BOUNDED_SURFACE()
B_SPLINE_SURFACE(5,1,((#238307,#238308),(#238309,#238310),(#238311,#238312),
(#238313,#238314),(#238315,#238316),(#238317,#238318),(#238319,#238320),
(#238321,#238322),(#238323,#238324),(#238325,#238326),(#238327,#238328),
(#238329,#238330),(#238331,#238332),(#238333,#238334),(#238335,#238336),
(#238337,#238338),(#238339,#238340),(#238341,#238342),(#238343,#238344),
(#238345,#238346),(#238347,#238348),(#238349,#238350),(#238351,#238352),
(#238353,#238354),(#238355,#238356),(#238357,#238358),(#238359,#238360),
(#238361,#238362),(#238363,#238364),(#238365,#238366),(#238367,#238368),
(#238369,#238370),(#238371,#238372),(#238373,#238374),(#238375,#238376),
(#238377,#238378),(#238379,#238380),(#238381,#238382),(#238383,#238384),
(#238385,#238386),(#238387,#238388),(#238389,#238390),(#238391,#238392),
(#238393,#238394),(#238395,#238396),(#238397,#238398),(#238399,#238400),
(#238401,#238402),(#238403,#238404),(#238405,#238406),(#238407,#238408),
(#238409,#238410),(#238411,#238412),(#238413,#238414),(#238415,#238416),
(#238417,#238418),(#238419,#238420),(#238421,#238422),(#238423,#238424),
(#238425,#238426),(#238427,#238428),(#238429,#238430),(#238431,#238432),
(#238433,#238434),(#238435,#238436),(#238437,#238438),(#238439,#238440),
(#238441,#238442),(#238443,#238444),(#238445,#238446),(#238447,#238448),
(#238449,#238450),(#238451,#238452),(#238453,#238454),(#238455,#238456),
(#238457,#238458),(#238459,#238460),(#238461,#238462),(#238463,#238464),
(#238465,#238466),(#238467,#238468),(#238469,#238470),(#238471,#238472),
(#238473,#238474),(#238475,#238476),(#238477,#238478),(#238479,#238480),
(#238481,#238482),(#238483,#238484),(#238485,#238486),(#238487,#238488),
(#238489,#238490),(#238491,#238492),(#238493,#238494),(#238495,#238496),
(#238497,#238498),(#238499,#238500),(#238501,#238502),(#238503,#238504),
(#238505,#238506),(#238507,#238508),(#238509,#238510),(#238511,#238512),
(#238513,#238514),(#238515,#238516),(#238517,#238518),(#238519,#238520),
(#238521,#238522),(#238523,#238524),(#238525,#238526),(#238527,#238528),
(#238529,#238530),(#238531,#238532),(#238533,#238534),(#238535,#238536),
(#238537,#238538),(#238539,#238540),(#238541,#238542),(#238543,#238544),
(#238545,#238546),(#238547,#238548),(#238549,#238550),(#238551,#238552),
(#238553,#238554),(#238555,#238556),(#238557,#238558),(#238559,#238560),
(#238561,#238562),(#238563,#238564),(#238565,#238566),(#238567,#238568),
(#238569,#238570),(#238571,#238572),(#238573,#238574),(#238575,#238576),
(#238577,#238578),(#238579,#238580),(#238581,#238582),(#238583,#238584),
(#238585,#238586),(#238587,#238588),(#238589,#238590),(#238591,#238592),
(#238593,#238594),(#238595,#238596),(#238597,#238598),(#238599,#238600),
(#238601,#238602),(#238603,#238604),(#238605,#238606),(#238607,#238608),
(#238609,#238610),(#238611,#238612),(#238613,#238614),(#238615,#238616),
(#238617,#238618),(#238619,#238620),(#238621,#238622),(#238623,#238624),
(#238625,#238626),(#238627,#238628),(#238629,#238630),(#238631,#238632),
(#238633,#238634),(#238635,#238636),(#238637,#238638),(#238639,#238640),
(#238641,#238642),(#238643,#238644),(#238645,#238646),(#238647,#238648),
(#238649,#238650),(#238651,#238652),(#238653,#238654),(#238655,#238656),
(#238657,#238658),(#238659,#238660),(#238661,#238662),(#238663,#238664),
(#238665,#238666),(#238667,#238668),(#238669,#238670),(#238671,#238672),
(#238673,#238674),(#238675,#238676),(#238677,#238678),(#238679,#238680),
(#238681,#238682),(#238683,#238684),(#238685,#238686),(#238687,#238688),
(#238689,#238690),(#238691,#238692),(#238693,#238694),(#238695,#238696),
(#238697,#238698),(#238699,#238700),(#238701,#238702),(#238703,#238704),
(#238705,#238706),(#238707,#238708),(#238709,#238710),(#238711,#238712),
(#238713,#238714),(#238715,#238716)),.UNSPECIFIED.,.F.,.F.,.F.)
B_SPLINE_SURFACE_WITH_KNOTS((6,1,1,1,1,1,1,1,1,1,1,1,1,1,1,1,1,1,1,1,1,
1,1,1,1,1,1,1,1,1,1,1,1,1,1,1,1,1,1,1,1,1,1,1,1,1,1,1,1,1,1,1,1,1,1,1,1,
1,1,1,1,1,1,1,1,1,1,1,1,1,1,1,1,1,1,1,1,1,1,1,1,1,1,1,1,1,1,1,1,1,1,1,1,
1,1,1,1,1,1,1,1,1,1,1,1,1,1,1,1,1,1,1,1,1,1,1,1,1,1,1,1,1,1,1,1,1,1,1,1,
1,1,1,1,1,1,1,1,1,1,1,1,1,1,1,1,1,1,1,1,1,1,1,1,1,1,1,1,1,1,1,1,1,1,1,1,
1,1,1,1,1,1,1,1,1,1,1,1,1,1,1,1,1,1,1,1,1,1,1,1,1,1,1,1,1,1,1,1,1,1,1,6),
(2,2),(0.,0.005,0.01,0.015,0.02,0.025,0.03,0.035,0.04,0.045,0.05,0.055,
0.06,0.065,0.07,0.075,0.08,0.085,0.09,0.095,0.1,0.105,0.11,0.115,0.12,0.125,
0.13,0.135,0.14,0.145,0.15,0.155,0.16,0.165,0.17,0.175,0.18,0.185,0.19,
0.195,0.2,0.205,0.21,0.215,0.22,0.225,0.23,0.235,0.24,0.245,0.25,0.255,
0.26,0.265,0.27,0.275,0.28,0.285,0.29,0.295,0.3,0.305,0.31,0.315,0.32,0.325,
0.33,0.335,0.34,0.345,0.35,0.355,0.36,0.365,0.37,0.375,0.38,0.385,0.39,
0.395,0.4,0.405,0.41,0.415,0.42,0.425,0.43,0.435,0.44,0.445,0.45,0.455,
0.46,0.465,0.47,0.475,0.48,0.485,0.49,0.495,0.5,0.505,0.51,0.515,0.52,0.525,
0.53,0.535,0.54,0.545,0.55,0.555,0.56,0.565,0.57,0.575,0.58,0.585,0.59,
0.595,0.6,0.605,0.61,0.615,0.62,0.625,0.63,0.635,0.64,0.645,0.65,0.655,
0.66,0.665,0.67,0.675,0.68,0.685,0.690000000000001,0.695000000000001,0.700000000000001,
0.705000000000001,0.710000000000001,0.715000000000001,0.720000000000001,
0.725000000000001,0.730000000000001,0.735000000000001,0.740000000000001,
0.745000000000001,0.750000000000001,0.755000000000001,0.760000000000001,
0.765000000000001,0.770000000000001,0.775000000000001,0.780000000000001,
0.785000000000001,0.790000000000001,0.795000000000001,0.800000000000001,
0.805000000000001,0.810000000000001,0.815000000000001,0.820000000000001,
0.825000000000001,0.830000000000001,0.835000000000001,0.840000000000001,
0.845000000000001,0.850000000000001,0.855000000000001,0.860000000000001,
0.865000000000001,0.870000000000001,0.875000000000001,0.880000000000001,
0.885000000000001,0.890000000000001,0.895000000000001,0.900000000000001,
0.905000000000001,0.910000000000001,0.915000000000001,0.920000000000001,
0.925000000000001,0.930000000000001,0.935000000000001,0.940000000000001,
0.945000000000001,0.950000000000001,0.955000000000001,0.960000000000001,
0.965000000000001,0.970000000000001,0.975000000000001,0.980000000000001,
0.985000000000001,0.990000000000001,0.995000000000001,1.),(0.,1.2),
 .UNSPECIFIED.)
GEOMETRIC_REPRESENTATION_ITEM()
RATIONAL_B_SPLINE_SURFACE(((1.,1.),(1.,1.),(1.,1.),(1.,1.),(1.,1.),(1.,
1.),(1.,1.),(1.,1.),(1.,1.),(1.,1.),(1.,1.),(1.,1.),(1.,1.),(1.,1.),(1.,
1.),(1.,1.),(1.,1.),(1.,1.),(1.,1.),(1.,1.),(1.,1.),(1.,1.),(1.,1.),(1.,
1.),(1.,1.),(1.,1.),(1.,1.),(1.,1.),(1.,1.),(1.,1.),(1.,1.),(1.,1.),(1.,
1.),(1.,1.),(1.,1.),(1.,1.),(1.,1.),(1.,1.),(1.,1.),(1.,1.),(1.,1.),(1.,
1.),(1.,1.),(1.,1.),(1.,1.),(1.,1.),(1.,1.),(1.,1.),(1.,1.),(1.,1.),(1.,
1.),(1.,1.),(1.,1.),(1.,1.),(1.,1.),(1.,1.),(1.,1.),(1.,1.),(1.,1.),(1.,
1.),(1.,1.),(1.,1.),(1.,1.),(1.,1.),(1.,1.),(1.,1.),(1.,1.),(1.,1.),(1.,
1.),(1.,1.),(1.,1.),(1.,1.),(1.,1.),(1.,1.),(1.,1.),(1.,1.),(1.,1.),(1.,
1.),(1.,1.),(1.,1.),(1.,1.),(1.,1.),(1.,1.),(1.,1.),(1.,1.),(1.,1.),(1.,
1.),(1.,1.),(1.,1.),(1.,1.),(1.,1.),(1.,1.),(1.,1.),(1.,1.),(1.,1.),(1.,
1.),(1.,1.),(1.,1.),(1.,1.),(1.,1.),(1.,1.),(1.,1.),(1.,1.),(1.,1.),(1.,
1.),(1.,1.),(1.,1.),(1.,1.),(1.,1.),(1.,1.),(1.,1.),(1.,1.),(1.,1.),(1.,
1.),(1.,1.),(1.,1.),(1.,1.),(1.,1.),(1.,1.),(1.,1.),(1.,1.),(1.,1.),(1.,
1.),(1.,1.),(1.,1.),(1.,1.),(1.,1.),(1.,1.),(1.,1.),(1.,1.),(1.,1.),(1.,
1.),(1.,1.),(1.,1.),(1.,1.),(1.,1.),(1.,1.),(1.,1.),(1.,1.),(1.,1.),(1.,
1.),(1.,1.),(1.,1.),(1.,1.),(1.,1.),(1.,1.),(1.,1.),(1.,1.),(1.,1.),(1.,
1.),(1.,1.),(1.,1.),(1.,1.),(1.,1.),(1.,1.),(1.,1.),(1.,1.),(1.,1.),(1.,
1.),(1.,1.),(1.,1.),(1.,1.),(1.,1.),(1.,1.),(1.,1.),(1.,1.),(1.,1.),(1.,
1.),(1.,1.),(1.,1.),(1.,1.),(1.,1.),(1.,1.),(1.,1.),(1.,1.),(1.,1.),(1.,
1.),(1.,1.),(1.,1.),(1.,1.),(1.,1.),(1.,1.),(1.,1.),(1.,1.),(1.,1.),(1.,
1.),(1.,1.),(1.,1.),(1.,1.),(1.,1.),(1.,1.),(1.,1.),(1.,1.),(1.,1.),(1.,
1.),(1.,1.),(1.,1.),(1.,1.),(1.,1.),(1.,1.),(1.,1.),(1.,1.),(1.,1.),(1.,
1.),(1.,1.)))
REPRESENTATION_ITEM('')
SURFACE()
);
#1103=(
BOUNDED_SURFACE()
B_SPLINE_SURFACE(5,1,((#239136,#239137),(#239138,#239139),(#239140,#239141),
(#239142,#239143),(#239144,#239145),(#239146,#239147),(#239148,#239149),
(#239150,#239151),(#239152,#239153),(#239154,#239155),(#239156,#239157),
(#239158,#239159),(#239160,#239161),(#239162,#239163),(#239164,#239165),
(#239166,#239167),(#239168,#239169),(#239170,#239171),(#239172,#239173),
(#239174,#239175),(#239176,#239177),(#239178,#239179),(#239180,#239181),
(#239182,#239183),(#239184,#239185),(#239186,#239187),(#239188,#239189),
(#239190,#239191),(#239192,#239193),(#239194,#239195),(#239196,#239197),
(#239198,#239199),(#239200,#239201),(#239202,#239203),(#239204,#239205),
(#239206,#239207),(#239208,#239209),(#239210,#239211),(#239212,#239213),
(#239214,#239215),(#239216,#239217),(#239218,#239219),(#239220,#239221),
(#239222,#239223),(#239224,#239225),(#239226,#239227),(#239228,#239229),
(#239230,#239231),(#239232,#239233),(#239234,#239235),(#239236,#239237),
(#239238,#239239),(#239240,#239241),(#239242,#239243),(#239244,#239245),
(#239246,#239247),(#239248,#239249),(#239250,#239251),(#239252,#239253),
(#239254,#239255),(#239256,#239257),(#239258,#239259),(#239260,#239261),
(#239262,#239263),(#239264,#239265),(#239266,#239267),(#239268,#239269),
(#239270,#239271),(#239272,#239273),(#239274,#239275),(#239276,#239277),
(#239278,#239279),(#239280,#239281),(#239282,#239283),(#239284,#239285),
(#239286,#239287),(#239288,#239289),(#239290,#239291),(#239292,#239293),
(#239294,#239295),(#239296,#239297),(#239298,#239299),(#239300,#239301),
(#239302,#239303),(#239304,#239305),(#239306,#239307),(#239308,#239309),
(#239310,#239311),(#239312,#239313),(#239314,#239315),(#239316,#239317),
(#239318,#239319),(#239320,#239321),(#239322,#239323),(#239324,#239325),
(#239326,#239327),(#239328,#239329),(#239330,#239331),(#239332,#239333),
(#239334,#239335),(#239336,#239337),(#239338,#239339),(#239340,#239341),
(#239342,#239343),(#239344,#239345),(#239346,#239347),(#239348,#239349),
(#239350,#239351),(#239352,#239353),(#239354,#239355),(#239356,#239357),
(#239358,#239359),(#239360,#239361),(#239362,#239363),(#239364,#239365),
(#239366,#239367),(#239368,#239369),(#239370,#239371),(#239372,#239373),
(#239374,#239375),(#239376,#239377),(#239378,#239379),(#239380,#239381),
(#239382,#239383),(#239384,#239385),(#239386,#239387),(#239388,#239389),
(#239390,#239391),(#239392,#239393),(#239394,#239395),(#239396,#239397),
(#239398,#239399),(#239400,#239401),(#239402,#239403),(#239404,#239405),
(#239406,#239407),(#239408,#239409),(#239410,#239411),(#239412,#239413),
(#239414,#239415),(#239416,#239417),(#239418,#239419),(#239420,#239421),
(#239422,#239423),(#239424,#239425),(#239426,#239427),(#239428,#239429),
(#239430,#239431),(#239432,#239433),(#239434,#239435),(#239436,#239437),
(#239438,#239439),(#239440,#239441),(#239442,#239443),(#239444,#239445),
(#239446,#239447),(#239448,#239449),(#239450,#239451),(#239452,#239453),
(#239454,#239455),(#239456,#239457),(#239458,#239459),(#239460,#239461),
(#239462,#239463),(#239464,#239465),(#239466,#239467),(#239468,#239469),
(#239470,#239471),(#239472,#239473),(#239474,#239475),(#239476,#239477),
(#239478,#239479),(#239480,#239481),(#239482,#239483),(#239484,#239485),
(#239486,#239487),(#239488,#239489),(#239490,#239491),(#239492,#239493),
(#239494,#239495),(#239496,#239497),(#239498,#239499),(#239500,#239501),
(#239502,#239503),(#239504,#239505),(#239506,#239507),(#239508,#239509),
(#239510,#239511),(#239512,#239513),(#239514,#239515),(#239516,#239517),
(#239518,#239519),(#239520,#239521),(#239522,#239523),(#239524,#239525),
(#239526,#239527),(#239528,#239529),(#239530,#239531),(#239532,#239533),
(#239534,#239535),(#239536,#239537),(#239538,#239539),(#239540,#239541),
(#239542,#239543),(#239544,#239545)),.UNSPECIFIED.,.F.,.F.,.F.)
B_SPLINE_SURFACE_WITH_KNOTS((6,1,1,1,1,1,1,1,1,1,1,1,1,1,1,1,1,1,1,1,1,
1,1,1,1,1,1,1,1,1,1,1,1,1,1,1,1,1,1,1,1,1,1,1,1,1,1,1,1,1,1,1,1,1,1,1,1,
1,1,1,1,1,1,1,1,1,1,1,1,1,1,1,1,1,1,1,1,1,1,1,1,1,1,1,1,1,1,1,1,1,1,1,1,
1,1,1,1,1,1,1,1,1,1,1,1,1,1,1,1,1,1,1,1,1,1,1,1,1,1,1,1,1,1,1,1,1,1,1,1,
1,1,1,1,1,1,1,1,1,1,1,1,1,1,1,1,1,1,1,1,1,1,1,1,1,1,1,1,1,1,1,1,1,1,1,1,
1,1,1,1,1,1,1,1,1,1,1,1,1,1,1,1,1,1,1,1,1,1,1,1,1,1,1,1,1,1,1,1,1,1,1,6),
(2,2),(-1.,-0.995000000000001,-0.990000000000001,-0.985000000000001,-0.980000000000001,
-0.975000000000001,-0.970000000000001,-0.965000000000001,-0.960000000000001,
-0.955000000000001,-0.950000000000001,-0.945000000000001,-0.940000000000001,
-0.935000000000001,-0.930000000000001,-0.925000000000001,-0.920000000000001,
-0.915000000000001,-0.910000000000001,-0.905000000000001,-0.900000000000001,
-0.895000000000001,-0.890000000000001,-0.885000000000001,-0.880000000000001,
-0.875000000000001,-0.870000000000001,-0.865000000000001,-0.860000000000001,
-0.855000000000001,-0.850000000000001,-0.845000000000001,-0.840000000000001,
-0.835000000000001,-0.830000000000001,-0.825000000000001,-0.820000000000001,
-0.815000000000001,-0.810000000000001,-0.805000000000001,-0.800000000000001,
-0.795000000000001,-0.790000000000001,-0.785000000000001,-0.780000000000001,
-0.775000000000001,-0.770000000000001,-0.765000000000001,-0.760000000000001,
-0.755000000000001,-0.750000000000001,-0.745000000000001,-0.740000000000001,
-0.735000000000001,-0.730000000000001,-0.725000000000001,-0.720000000000001,
-0.715000000000001,-0.710000000000001,-0.705000000000001,-0.700000000000001,
-0.695000000000001,-0.690000000000001,-0.685,-0.68,-0.675,-0.67,-0.665,
-0.66,-0.655,-0.65,-0.645,-0.64,-0.635,-0.63,-0.625,-0.62,-0.615,-0.61,
-0.605,-0.6,-0.595,-0.59,-0.585,-0.58,-0.575,-0.57,-0.565,-0.56,-0.555,
-0.55,-0.545,-0.54,-0.535,-0.53,-0.525,-0.52,-0.515,-0.51,-0.505,-0.5,-0.495,
-0.49,-0.485,-0.48,-0.475,-0.47,-0.465,-0.46,-0.455,-0.45,-0.445,-0.44,
-0.435,-0.43,-0.425,-0.42,-0.415,-0.41,-0.405,-0.4,-0.395,-0.39,-0.385,
-0.38,-0.375,-0.37,-0.365,-0.36,-0.355,-0.35,-0.345,-0.34,-0.335,-0.33,
-0.325,-0.32,-0.315,-0.31,-0.305,-0.3,-0.295,-0.29,-0.285,-0.28,-0.275,
-0.27,-0.265,-0.26,-0.255,-0.25,-0.245,-0.24,-0.235,-0.23,-0.225,-0.22,
-0.215,-0.21,-0.205,-0.2,-0.195,-0.19,-0.185,-0.18,-0.175,-0.17,-0.165,
-0.16,-0.155,-0.15,-0.145,-0.14,-0.135,-0.13,-0.125,-0.12,-0.115,-0.11,
-0.105,-0.1,-0.095,-0.09,-0.085,-0.08,-0.075,-0.07,-0.065,-0.06,-0.055,
-0.05,-0.045,-0.04,-0.035,-0.03,-0.025,-0.02,-0.015,-0.01,-0.005,0.),(0.,
1.2),.UNSPECIFIED.)
GEOMETRIC_REPRESENTATION_ITEM()
RATIONAL_B_SPLINE_SURFACE(((1.,1.),(1.,1.),(1.,1.),(1.,1.),(1.,1.),(1.,
1.),(1.,1.),(1.,1.),(1.,1.),(1.,1.),(1.,1.),(1.,1.),(1.,1.),(1.,1.),(1.,
1.),(1.,1.),(1.,1.),(1.,1.),(1.,1.),(1.,1.),(1.,1.),(1.,1.),(1.,1.),(1.,
1.),(1.,1.),(1.,1.),(1.,1.),(1.,1.),(1.,1.),(1.,1.),(1.,1.),(1.,1.),(1.,
1.),(1.,1.),(1.,1.),(1.,1.),(1.,1.),(1.,1.),(1.,1.),(1.,1.),(1.,1.),(1.,
1.),(1.,1.),(1.,1.),(1.,1.),(1.,1.),(1.,1.),(1.,1.),(1.,1.),(1.,1.),(1.,
1.),(1.,1.),(1.,1.),(1.,1.),(1.,1.),(1.,1.),(1.,1.),(1.,1.),(1.,1.),(1.,
1.),(1.,1.),(1.,1.),(1.,1.),(1.,1.),(1.,1.),(1.,1.),(1.,1.),(1.,1.),(1.,
1.),(1.,1.),(1.,1.),(1.,1.),(1.,1.),(1.,1.),(1.,1.),(1.,1.),(1.,1.),(1.,
1.),(1.,1.),(1.,1.),(1.,1.),(1.,1.),(1.,1.),(1.,1.),(1.,1.),(1.,1.),(1.,
1.),(1.,1.),(1.,1.),(1.,1.),(1.,1.),(1.,1.),(1.,1.),(1.,1.),(1.,1.),(1.,
1.),(1.,1.),(1.,1.),(1.,1.),(1.,1.),(1.,1.),(1.,1.),(1.,1.),(1.,1.),(1.,
1.),(1.,1.),(1.,1.),(1.,1.),(1.,1.),(1.,1.),(1.,1.),(1.,1.),(1.,1.),(1.,
1.),(1.,1.),(1.,1.),(1.,1.),(1.,1.),(1.,1.),(1.,1.),(1.,1.),(1.,1.),(1.,
1.),(1.,1.),(1.,1.),(1.,1.),(1.,1.),(1.,1.),(1.,1.),(1.,1.),(1.,1.),(1.,
1.),(1.,1.),(1.,1.),(1.,1.),(1.,1.),(1.,1.),(1.,1.),(1.,1.),(1.,1.),(1.,
1.),(1.,1.),(1.,1.),(1.,1.),(1.,1.),(1.,1.),(1.,1.),(1.,1.),(1.,1.),(1.,
1.),(1.,1.),(1.,1.),(1.,1.),(1.,1.),(1.,1.),(1.,1.),(1.,1.),(1.,1.),(1.,
1.),(1.,1.),(1.,1.),(1.,1.),(1.,1.),(1.,1.),(1.,1.),(1.,1.),(1.,1.),(1.,
1.),(1.,1.),(1.,1.),(1.,1.),(1.,1.),(1.,1.),(1.,1.),(1.,1.),(1.,1.),(1.,
1.),(1.,1.),(1.,1.),(1.,1.),(1.,1.),(1.,1.),(1.,1.),(1.,1.),(1.,1.),(1.,
1.),(1.,1.),(1.,1.),(1.,1.),(1.,1.),(1.,1.),(1.,1.),(1.,1.),(1.,1.),(1.,
1.),(1.,1.),(1.,1.),(1.,1.),(1.,1.),(1.,1.),(1.,1.),(1.,1.),(1.,1.),(1.,
1.),(1.,1.)))
REPRESENTATION_ITEM('')
SURFACE()
);
#1104=(
BOUNDED_SURFACE()
B_SPLINE_SURFACE(5,1,((#239959,#239960),(#239961,#239962),(#239963,#239964),
(#239965,#239966),(#239967,#239968),(#239969,#239970),(#239971,#239972),
(#239973,#239974),(#239975,#239976),(#239977,#239978),(#239979,#239980),
(#239981,#239982),(#239983,#239984),(#239985,#239986),(#239987,#239988),
(#239989,#239990),(#239991,#239992),(#239993,#239994),(#239995,#239996),
(#239997,#239998),(#239999,#240000),(#240001,#240002),(#240003,#240004),
(#240005,#240006),(#240007,#240008),(#240009,#240010),(#240011,#240012),
(#240013,#240014),(#240015,#240016),(#240017,#240018),(#240019,#240020),
(#240021,#240022),(#240023,#240024),(#240025,#240026),(#240027,#240028),
(#240029,#240030),(#240031,#240032),(#240033,#240034),(#240035,#240036),
(#240037,#240038),(#240039,#240040),(#240041,#240042),(#240043,#240044),
(#240045,#240046),(#240047,#240048),(#240049,#240050),(#240051,#240052),
(#240053,#240054),(#240055,#240056),(#240057,#240058),(#240059,#240060),
(#240061,#240062),(#240063,#240064),(#240065,#240066),(#240067,#240068),
(#240069,#240070),(#240071,#240072),(#240073,#240074),(#240075,#240076),
(#240077,#240078),(#240079,#240080),(#240081,#240082),(#240083,#240084),
(#240085,#240086),(#240087,#240088),(#240089,#240090),(#240091,#240092),
(#240093,#240094),(#240095,#240096),(#240097,#240098),(#240099,#240100),
(#240101,#240102),(#240103,#240104),(#240105,#240106),(#240107,#240108),
(#240109,#240110),(#240111,#240112),(#240113,#240114),(#240115,#240116),
(#240117,#240118),(#240119,#240120),(#240121,#240122),(#240123,#240124),
(#240125,#240126),(#240127,#240128),(#240129,#240130),(#240131,#240132),
(#240133,#240134),(#240135,#240136),(#240137,#240138),(#240139,#240140),
(#240141,#240142),(#240143,#240144),(#240145,#240146),(#240147,#240148),
(#240149,#240150),(#240151,#240152),(#240153,#240154),(#240155,#240156),
(#240157,#240158),(#240159,#240160),(#240161,#240162),(#240163,#240164),
(#240165,#240166),(#240167,#240168),(#240169,#240170),(#240171,#240172),
(#240173,#240174),(#240175,#240176),(#240177,#240178),(#240179,#240180),
(#240181,#240182),(#240183,#240184),(#240185,#240186),(#240187,#240188),
(#240189,#240190),(#240191,#240192),(#240193,#240194),(#240195,#240196),
(#240197,#240198),(#240199,#240200),(#240201,#240202),(#240203,#240204),
(#240205,#240206),(#240207,#240208),(#240209,#240210),(#240211,#240212),
(#240213,#240214),(#240215,#240216),(#240217,#240218),(#240219,#240220),
(#240221,#240222),(#240223,#240224),(#240225,#240226),(#240227,#240228),
(#240229,#240230),(#240231,#240232),(#240233,#240234),(#240235,#240236),
(#240237,#240238),(#240239,#240240),(#240241,#240242),(#240243,#240244),
(#240245,#240246),(#240247,#240248),(#240249,#240250),(#240251,#240252),
(#240253,#240254),(#240255,#240256),(#240257,#240258),(#240259,#240260),
(#240261,#240262),(#240263,#240264),(#240265,#240266),(#240267,#240268),
(#240269,#240270),(#240271,#240272),(#240273,#240274),(#240275,#240276),
(#240277,#240278),(#240279,#240280),(#240281,#240282),(#240283,#240284),
(#240285,#240286),(#240287,#240288),(#240289,#240290),(#240291,#240292),
(#240293,#240294),(#240295,#240296),(#240297,#240298),(#240299,#240300),
(#240301,#240302),(#240303,#240304),(#240305,#240306),(#240307,#240308),
(#240309,#240310),(#240311,#240312),(#240313,#240314),(#240315,#240316),
(#240317,#240318),(#240319,#240320),(#240321,#240322),(#240323,#240324),
(#240325,#240326),(#240327,#240328),(#240329,#240330),(#240331,#240332),
(#240333,#240334),(#240335,#240336),(#240337,#240338),(#240339,#240340),
(#240341,#240342),(#240343,#240344),(#240345,#240346),(#240347,#240348),
(#240349,#240350),(#240351,#240352),(#240353,#240354),(#240355,#240356),
(#240357,#240358),(#240359,#240360),(#240361,#240362),(#240363,#240364),
(#240365,#240366),(#240367,#240368)),.UNSPECIFIED.,.F.,.F.,.F.)
B_SPLINE_SURFACE_WITH_KNOTS((6,1,1,1,1,1,1,1,1,1,1,1,1,1,1,1,1,1,1,1,1,
1,1,1,1,1,1,1,1,1,1,1,1,1,1,1,1,1,1,1,1,1,1,1,1,1,1,1,1,1,1,1,1,1,1,1,1,
1,1,1,1,1,1,1,1,1,1,1,1,1,1,1,1,1,1,1,1,1,1,1,1,1,1,1,1,1,1,1,1,1,1,1,1,
1,1,1,1,1,1,1,1,1,1,1,1,1,1,1,1,1,1,1,1,1,1,1,1,1,1,1,1,1,1,1,1,1,1,1,1,
1,1,1,1,1,1,1,1,1,1,1,1,1,1,1,1,1,1,1,1,1,1,1,1,1,1,1,1,1,1,1,1,1,1,1,1,
1,1,1,1,1,1,1,1,1,1,1,1,1,1,1,1,1,1,1,1,1,1,1,1,1,1,1,1,1,1,1,1,1,1,1,6),
(2,2),(0.,0.005,0.01,0.015,0.02,0.025,0.03,0.035,0.04,0.045,0.05,0.055,
0.06,0.065,0.07,0.075,0.08,0.085,0.09,0.095,0.1,0.105,0.11,0.115,0.12,0.125,
0.13,0.135,0.14,0.145,0.15,0.155,0.16,0.165,0.17,0.175,0.18,0.185,0.19,
0.195,0.2,0.205,0.21,0.215,0.22,0.225,0.23,0.235,0.24,0.245,0.25,0.255,
0.26,0.265,0.27,0.275,0.28,0.285,0.29,0.295,0.3,0.305,0.31,0.315,0.32,0.325,
0.33,0.335,0.34,0.345,0.35,0.355,0.36,0.365,0.37,0.375,0.38,0.385,0.39,
0.395,0.4,0.405,0.41,0.415,0.42,0.425,0.43,0.435,0.44,0.445,0.45,0.455,
0.46,0.465,0.47,0.475,0.48,0.485,0.49,0.495,0.5,0.505,0.51,0.515,0.52,0.525,
0.53,0.535,0.54,0.545,0.55,0.555,0.56,0.565,0.57,0.575,0.58,0.585,0.59,
0.595,0.6,0.605,0.61,0.615,0.62,0.625,0.63,0.635,0.64,0.645,0.65,0.655,
0.66,0.665,0.67,0.675,0.68,0.685,0.690000000000001,0.695000000000001,0.700000000000001,
0.705000000000001,0.710000000000001,0.715000000000001,0.720000000000001,
0.725000000000001,0.730000000000001,0.735000000000001,0.740000000000001,
0.745000000000001,0.750000000000001,0.755000000000001,0.760000000000001,
0.765000000000001,0.770000000000001,0.775000000000001,0.780000000000001,
0.785000000000001,0.790000000000001,0.795000000000001,0.800000000000001,
0.805000000000001,0.810000000000001,0.815000000000001,0.820000000000001,
0.825000000000001,0.830000000000001,0.835000000000001,0.840000000000001,
0.845000000000001,0.850000000000001,0.855000000000001,0.860000000000001,
0.865000000000001,0.870000000000001,0.875000000000001,0.880000000000001,
0.885000000000001,0.890000000000001,0.895000000000001,0.900000000000001,
0.905000000000001,0.910000000000001,0.915000000000001,0.920000000000001,
0.925000000000001,0.930000000000001,0.935000000000001,0.940000000000001,
0.945000000000001,0.950000000000001,0.955000000000001,0.960000000000001,
0.965000000000001,0.970000000000001,0.975000000000001,0.980000000000001,
0.985000000000001,0.990000000000001,0.995000000000001,1.),(0.,1.2),
 .UNSPECIFIED.)
GEOMETRIC_REPRESENTATION_ITEM()
RATIONAL_B_SPLINE_SURFACE(((1.,1.),(1.,1.),(1.,1.),(1.,1.),(1.,1.),(1.,
1.),(1.,1.),(1.,1.),(1.,1.),(1.,1.),(1.,1.),(1.,1.),(1.,1.),(1.,1.),(1.,
1.),(1.,1.),(1.,1.),(1.,1.),(1.,1.),(1.,1.),(1.,1.),(1.,1.),(1.,1.),(1.,
1.),(1.,1.),(1.,1.),(1.,1.),(1.,1.),(1.,1.),(1.,1.),(1.,1.),(1.,1.),(1.,
1.),(1.,1.),(1.,1.),(1.,1.),(1.,1.),(1.,1.),(1.,1.),(1.,1.),(1.,1.),(1.,
1.),(1.,1.),(1.,1.),(1.,1.),(1.,1.),(1.,1.),(1.,1.),(1.,1.),(1.,1.),(1.,
1.),(1.,1.),(1.,1.),(1.,1.),(1.,1.),(1.,1.),(1.,1.),(1.,1.),(1.,1.),(1.,
1.),(1.,1.),(1.,1.),(1.,1.),(1.,1.),(1.,1.),(1.,1.),(1.,1.),(1.,1.),(1.,
1.),(1.,1.),(1.,1.),(1.,1.),(1.,1.),(1.,1.),(1.,1.),(1.,1.),(1.,1.),(1.,
1.),(1.,1.),(1.,1.),(1.,1.),(1.,1.),(1.,1.),(1.,1.),(1.,1.),(1.,1.),(1.,
1.),(1.,1.),(1.,1.),(1.,1.),(1.,1.),(1.,1.),(1.,1.),(1.,1.),(1.,1.),(1.,
1.),(1.,1.),(1.,1.),(1.,1.),(1.,1.),(1.,1.),(1.,1.),(1.,1.),(1.,1.),(1.,
1.),(1.,1.),(1.,1.),(1.,1.),(1.,1.),(1.,1.),(1.,1.),(1.,1.),(1.,1.),(1.,
1.),(1.,1.),(1.,1.),(1.,1.),(1.,1.),(1.,1.),(1.,1.),(1.,1.),(1.,1.),(1.,
1.),(1.,1.),(1.,1.),(1.,1.),(1.,1.),(1.,1.),(1.,1.),(1.,1.),(1.,1.),(1.,
1.),(1.,1.),(1.,1.),(1.,1.),(1.,1.),(1.,1.),(1.,1.),(1.,1.),(1.,1.),(1.,
1.),(1.,1.),(1.,1.),(1.,1.),(1.,1.),(1.,1.),(1.,1.),(1.,1.),(1.,1.),(1.,
1.),(1.,1.),(1.,1.),(1.,1.),(1.,1.),(1.,1.),(1.,1.),(1.,1.),(1.,1.),(1.,
1.),(1.,1.),(1.,1.),(1.,1.),(1.,1.),(1.,1.),(1.,1.),(1.,1.),(1.,1.),(1.,
1.),(1.,1.),(1.,1.),(1.,1.),(1.,1.),(1.,1.),(1.,1.),(1.,1.),(1.,1.),(1.,
1.),(1.,1.),(1.,1.),(1.,1.),(1.,1.),(1.,1.),(1.,1.),(1.,1.),(1.,1.),(1.,
1.),(1.,1.),(1.,1.),(1.,1.),(1.,1.),(1.,1.),(1.,1.),(1.,1.),(1.,1.),(1.,
1.),(1.,1.),(1.,1.),(1.,1.),(1.,1.),(1.,1.),(1.,1.),(1.,1.),(1.,1.),(1.,
1.),(1.,1.)))
REPRESENTATION_ITEM('')
SURFACE()
);
#1105=(
BOUNDED_SURFACE()
B_SPLINE_SURFACE(5,1,((#240788,#240789),(#240790,#240791),(#240792,#240793),
(#240794,#240795),(#240796,#240797),(#240798,#240799),(#240800,#240801),
(#240802,#240803),(#240804,#240805),(#240806,#240807),(#240808,#240809),
(#240810,#240811),(#240812,#240813),(#240814,#240815),(#240816,#240817),
(#240818,#240819),(#240820,#240821),(#240822,#240823),(#240824,#240825),
(#240826,#240827),(#240828,#240829),(#240830,#240831),(#240832,#240833),
(#240834,#240835),(#240836,#240837),(#240838,#240839),(#240840,#240841),
(#240842,#240843),(#240844,#240845),(#240846,#240847),(#240848,#240849),
(#240850,#240851),(#240852,#240853),(#240854,#240855),(#240856,#240857),
(#240858,#240859),(#240860,#240861),(#240862,#240863),(#240864,#240865),
(#240866,#240867),(#240868,#240869),(#240870,#240871),(#240872,#240873),
(#240874,#240875),(#240876,#240877),(#240878,#240879),(#240880,#240881),
(#240882,#240883),(#240884,#240885),(#240886,#240887),(#240888,#240889),
(#240890,#240891),(#240892,#240893),(#240894,#240895),(#240896,#240897),
(#240898,#240899),(#240900,#240901),(#240902,#240903),(#240904,#240905),
(#240906,#240907),(#240908,#240909),(#240910,#240911),(#240912,#240913),
(#240914,#240915),(#240916,#240917),(#240918,#240919),(#240920,#240921),
(#240922,#240923),(#240924,#240925),(#240926,#240927),(#240928,#240929),
(#240930,#240931),(#240932,#240933),(#240934,#240935),(#240936,#240937),
(#240938,#240939),(#240940,#240941),(#240942,#240943),(#240944,#240945),
(#240946,#240947),(#240948,#240949),(#240950,#240951),(#240952,#240953),
(#240954,#240955),(#240956,#240957),(#240958,#240959),(#240960,#240961),
(#240962,#240963),(#240964,#240965),(#240966,#240967),(#240968,#240969),
(#240970,#240971),(#240972,#240973),(#240974,#240975),(#240976,#240977),
(#240978,#240979),(#240980,#240981),(#240982,#240983),(#240984,#240985),
(#240986,#240987),(#240988,#240989),(#240990,#240991),(#240992,#240993),
(#240994,#240995),(#240996,#240997),(#240998,#240999),(#241000,#241001),
(#241002,#241003),(#241004,#241005),(#241006,#241007),(#241008,#241009),
(#241010,#241011),(#241012,#241013),(#241014,#241015),(#241016,#241017),
(#241018,#241019),(#241020,#241021),(#241022,#241023),(#241024,#241025),
(#241026,#241027),(#241028,#241029),(#241030,#241031),(#241032,#241033),
(#241034,#241035),(#241036,#241037),(#241038,#241039),(#241040,#241041),
(#241042,#241043),(#241044,#241045),(#241046,#241047),(#241048,#241049),
(#241050,#241051),(#241052,#241053),(#241054,#241055),(#241056,#241057),
(#241058,#241059),(#241060,#241061),(#241062,#241063),(#241064,#241065),
(#241066,#241067),(#241068,#241069),(#241070,#241071),(#241072,#241073),
(#241074,#241075),(#241076,#241077),(#241078,#241079),(#241080,#241081),
(#241082,#241083),(#241084,#241085),(#241086,#241087),(#241088,#241089),
(#241090,#241091),(#241092,#241093),(#241094,#241095),(#241096,#241097),
(#241098,#241099),(#241100,#241101),(#241102,#241103),(#241104,#241105),
(#241106,#241107),(#241108,#241109),(#241110,#241111),(#241112,#241113),
(#241114,#241115),(#241116,#241117),(#241118,#241119),(#241120,#241121),
(#241122,#241123),(#241124,#241125),(#241126,#241127),(#241128,#241129),
(#241130,#241131),(#241132,#241133),(#241134,#241135),(#241136,#241137),
(#241138,#241139),(#241140,#241141),(#241142,#241143),(#241144,#241145),
(#241146,#241147),(#241148,#241149),(#241150,#241151),(#241152,#241153),
(#241154,#241155),(#241156,#241157),(#241158,#241159),(#241160,#241161),
(#241162,#241163),(#241164,#241165),(#241166,#241167),(#241168,#241169),
(#241170,#241171),(#241172,#241173),(#241174,#241175),(#241176,#241177),
(#241178,#241179),(#241180,#241181),(#241182,#241183),(#241184,#241185),
(#241186,#241187),(#241188,#241189),(#241190,#241191),(#241192,#241193),
(#241194,#241195),(#241196,#241197)),.UNSPECIFIED.,.F.,.F.,.F.)
B_SPLINE_SURFACE_WITH_KNOTS((6,1,1,1,1,1,1,1,1,1,1,1,1,1,1,1,1,1,1,1,1,
1,1,1,1,1,1,1,1,1,1,1,1,1,1,1,1,1,1,1,1,1,1,1,1,1,1,1,1,1,1,1,1,1,1,1,1,
1,1,1,1,1,1,1,1,1,1,1,1,1,1,1,1,1,1,1,1,1,1,1,1,1,1,1,1,1,1,1,1,1,1,1,1,
1,1,1,1,1,1,1,1,1,1,1,1,1,1,1,1,1,1,1,1,1,1,1,1,1,1,1,1,1,1,1,1,1,1,1,1,
1,1,1,1,1,1,1,1,1,1,1,1,1,1,1,1,1,1,1,1,1,1,1,1,1,1,1,1,1,1,1,1,1,1,1,1,
1,1,1,1,1,1,1,1,1,1,1,1,1,1,1,1,1,1,1,1,1,1,1,1,1,1,1,1,1,1,1,1,1,1,1,6),
(2,2),(-1.,-0.995000000000001,-0.990000000000001,-0.985000000000001,-0.980000000000001,
-0.975000000000001,-0.970000000000001,-0.965000000000001,-0.960000000000001,
-0.955000000000001,-0.950000000000001,-0.945000000000001,-0.940000000000001,
-0.935000000000001,-0.930000000000001,-0.925000000000001,-0.920000000000001,
-0.915000000000001,-0.910000000000001,-0.905000000000001,-0.900000000000001,
-0.895000000000001,-0.890000000000001,-0.885000000000001,-0.880000000000001,
-0.875000000000001,-0.870000000000001,-0.865000000000001,-0.860000000000001,
-0.855000000000001,-0.850000000000001,-0.845000000000001,-0.840000000000001,
-0.835000000000001,-0.830000000000001,-0.825000000000001,-0.820000000000001,
-0.815000000000001,-0.810000000000001,-0.805000000000001,-0.800000000000001,
-0.795000000000001,-0.790000000000001,-0.785000000000001,-0.780000000000001,
-0.775000000000001,-0.770000000000001,-0.765000000000001,-0.760000000000001,
-0.755000000000001,-0.750000000000001,-0.745000000000001,-0.740000000000001,
-0.735000000000001,-0.730000000000001,-0.725000000000001,-0.720000000000001,
-0.715000000000001,-0.710000000000001,-0.705000000000001,-0.700000000000001,
-0.695000000000001,-0.690000000000001,-0.685,-0.68,-0.675,-0.67,-0.665,
-0.66,-0.655,-0.65,-0.645,-0.64,-0.635,-0.63,-0.625,-0.62,-0.615,-0.61,
-0.605,-0.6,-0.595,-0.59,-0.585,-0.58,-0.575,-0.57,-0.565,-0.56,-0.555,
-0.55,-0.545,-0.54,-0.535,-0.53,-0.525,-0.52,-0.515,-0.51,-0.505,-0.5,-0.495,
-0.49,-0.485,-0.48,-0.475,-0.47,-0.465,-0.46,-0.455,-0.45,-0.445,-0.44,
-0.435,-0.43,-0.425,-0.42,-0.415,-0.41,-0.405,-0.4,-0.395,-0.39,-0.385,
-0.38,-0.375,-0.37,-0.365,-0.36,-0.355,-0.35,-0.345,-0.34,-0.335,-0.33,
-0.325,-0.32,-0.315,-0.31,-0.305,-0.3,-0.295,-0.29,-0.285,-0.28,-0.275,
-0.27,-0.265,-0.26,-0.255,-0.25,-0.245,-0.24,-0.235,-0.23,-0.225,-0.22,
-0.215,-0.21,-0.205,-0.2,-0.195,-0.19,-0.185,-0.18,-0.175,-0.17,-0.165,
-0.16,-0.155,-0.15,-0.145,-0.14,-0.135,-0.13,-0.125,-0.12,-0.115,-0.11,
-0.105,-0.1,-0.095,-0.09,-0.085,-0.08,-0.075,-0.07,-0.065,-0.06,-0.055,
-0.05,-0.045,-0.04,-0.035,-0.03,-0.025,-0.02,-0.015,-0.01,-0.005,0.),(0.,
1.2),.UNSPECIFIED.)
GEOMETRIC_REPRESENTATION_ITEM()
RATIONAL_B_SPLINE_SURFACE(((1.,1.),(1.,1.),(1.,1.),(1.,1.),(1.,1.),(1.,
1.),(1.,1.),(1.,1.),(1.,1.),(1.,1.),(1.,1.),(1.,1.),(1.,1.),(1.,1.),(1.,
1.),(1.,1.),(1.,1.),(1.,1.),(1.,1.),(1.,1.),(1.,1.),(1.,1.),(1.,1.),(1.,
1.),(1.,1.),(1.,1.),(1.,1.),(1.,1.),(1.,1.),(1.,1.),(1.,1.),(1.,1.),(1.,
1.),(1.,1.),(1.,1.),(1.,1.),(1.,1.),(1.,1.),(1.,1.),(1.,1.),(1.,1.),(1.,
1.),(1.,1.),(1.,1.),(1.,1.),(1.,1.),(1.,1.),(1.,1.),(1.,1.),(1.,1.),(1.,
1.),(1.,1.),(1.,1.),(1.,1.),(1.,1.),(1.,1.),(1.,1.),(1.,1.),(1.,1.),(1.,
1.),(1.,1.),(1.,1.),(1.,1.),(1.,1.),(1.,1.),(1.,1.),(1.,1.),(1.,1.),(1.,
1.),(1.,1.),(1.,1.),(1.,1.),(1.,1.),(1.,1.),(1.,1.),(1.,1.),(1.,1.),(1.,
1.),(1.,1.),(1.,1.),(1.,1.),(1.,1.),(1.,1.),(1.,1.),(1.,1.),(1.,1.),(1.,
1.),(1.,1.),(1.,1.),(1.,1.),(1.,1.),(1.,1.),(1.,1.),(1.,1.),(1.,1.),(1.,
1.),(1.,1.),(1.,1.),(1.,1.),(1.,1.),(1.,1.),(1.,1.),(1.,1.),(1.,1.),(1.,
1.),(1.,1.),(1.,1.),(1.,1.),(1.,1.),(1.,1.),(1.,1.),(1.,1.),(1.,1.),(1.,
1.),(1.,1.),(1.,1.),(1.,1.),(1.,1.),(1.,1.),(1.,1.),(1.,1.),(1.,1.),(1.,
1.),(1.,1.),(1.,1.),(1.,1.),(1.,1.),(1.,1.),(1.,1.),(1.,1.),(1.,1.),(1.,
1.),(1.,1.),(1.,1.),(1.,1.),(1.,1.),(1.,1.),(1.,1.),(1.,1.),(1.,1.),(1.,
1.),(1.,1.),(1.,1.),(1.,1.),(1.,1.),(1.,1.),(1.,1.),(1.,1.),(1.,1.),(1.,
1.),(1.,1.),(1.,1.),(1.,1.),(1.,1.),(1.,1.),(1.,1.),(1.,1.),(1.,1.),(1.,
1.),(1.,1.),(1.,1.),(1.,1.),(1.,1.),(1.,1.),(1.,1.),(1.,1.),(1.,1.),(1.,
1.),(1.,1.),(1.,1.),(1.,1.),(1.,1.),(1.,1.),(1.,1.),(1.,1.),(1.,1.),(1.,
1.),(1.,1.),(1.,1.),(1.,1.),(1.,1.),(1.,1.),(1.,1.),(1.,1.),(1.,1.),(1.,
1.),(1.,1.),(1.,1.),(1.,1.),(1.,1.),(1.,1.),(1.,1.),(1.,1.),(1.,1.),(1.,
1.),(1.,1.),(1.,1.),(1.,1.),(1.,1.),(1.,1.),(1.,1.),(1.,1.),(1.,1.),(1.,
1.),(1.,1.)))
REPRESENTATION_ITEM('')
SURFACE()
);
#1106=(
BOUNDED_SURFACE()
B_SPLINE_SURFACE(5,1,((#241611,#241612),(#241613,#241614),(#241615,#241616),
(#241617,#241618),(#241619,#241620),(#241621,#241622),(#241623,#241624),
(#241625,#241626),(#241627,#241628),(#241629,#241630),(#241631,#241632),
(#241633,#241634),(#241635,#241636),(#241637,#241638),(#241639,#241640),
(#241641,#241642),(#241643,#241644),(#241645,#241646),(#241647,#241648),
(#241649,#241650),(#241651,#241652),(#241653,#241654),(#241655,#241656),
(#241657,#241658),(#241659,#241660),(#241661,#241662),(#241663,#241664),
(#241665,#241666),(#241667,#241668),(#241669,#241670),(#241671,#241672),
(#241673,#241674),(#241675,#241676),(#241677,#241678),(#241679,#241680),
(#241681,#241682),(#241683,#241684),(#241685,#241686),(#241687,#241688),
(#241689,#241690),(#241691,#241692),(#241693,#241694),(#241695,#241696),
(#241697,#241698),(#241699,#241700),(#241701,#241702),(#241703,#241704),
(#241705,#241706),(#241707,#241708),(#241709,#241710),(#241711,#241712),
(#241713,#241714),(#241715,#241716),(#241717,#241718),(#241719,#241720),
(#241721,#241722),(#241723,#241724),(#241725,#241726),(#241727,#241728),
(#241729,#241730),(#241731,#241732),(#241733,#241734),(#241735,#241736),
(#241737,#241738),(#241739,#241740),(#241741,#241742),(#241743,#241744),
(#241745,#241746),(#241747,#241748),(#241749,#241750),(#241751,#241752),
(#241753,#241754),(#241755,#241756),(#241757,#241758),(#241759,#241760),
(#241761,#241762),(#241763,#241764),(#241765,#241766),(#241767,#241768),
(#241769,#241770),(#241771,#241772),(#241773,#241774),(#241775,#241776),
(#241777,#241778),(#241779,#241780),(#241781,#241782),(#241783,#241784),
(#241785,#241786),(#241787,#241788),(#241789,#241790),(#241791,#241792),
(#241793,#241794),(#241795,#241796),(#241797,#241798),(#241799,#241800),
(#241801,#241802),(#241803,#241804),(#241805,#241806),(#241807,#241808),
(#241809,#241810),(#241811,#241812),(#241813,#241814),(#241815,#241816),
(#241817,#241818),(#241819,#241820),(#241821,#241822),(#241823,#241824),
(#241825,#241826),(#241827,#241828),(#241829,#241830),(#241831,#241832),
(#241833,#241834),(#241835,#241836),(#241837,#241838),(#241839,#241840),
(#241841,#241842),(#241843,#241844),(#241845,#241846),(#241847,#241848),
(#241849,#241850),(#241851,#241852),(#241853,#241854),(#241855,#241856),
(#241857,#241858),(#241859,#241860),(#241861,#241862),(#241863,#241864),
(#241865,#241866),(#241867,#241868),(#241869,#241870),(#241871,#241872),
(#241873,#241874),(#241875,#241876),(#241877,#241878),(#241879,#241880),
(#241881,#241882),(#241883,#241884),(#241885,#241886),(#241887,#241888),
(#241889,#241890),(#241891,#241892),(#241893,#241894),(#241895,#241896),
(#241897,#241898),(#241899,#241900),(#241901,#241902),(#241903,#241904),
(#241905,#241906),(#241907,#241908),(#241909,#241910),(#241911,#241912),
(#241913,#241914),(#241915,#241916),(#241917,#241918),(#241919,#241920),
(#241921,#241922),(#241923,#241924),(#241925,#241926),(#241927,#241928),
(#241929,#241930),(#241931,#241932),(#241933,#241934),(#241935,#241936),
(#241937,#241938),(#241939,#241940),(#241941,#241942),(#241943,#241944),
(#241945,#241946),(#241947,#241948),(#241949,#241950),(#241951,#241952),
(#241953,#241954),(#241955,#241956),(#241957,#241958),(#241959,#241960),
(#241961,#241962),(#241963,#241964),(#241965,#241966),(#241967,#241968),
(#241969,#241970),(#241971,#241972),(#241973,#241974),(#241975,#241976),
(#241977,#241978),(#241979,#241980),(#241981,#241982),(#241983,#241984),
(#241985,#241986),(#241987,#241988),(#241989,#241990),(#241991,#241992),
(#241993,#241994),(#241995,#241996),(#241997,#241998),(#241999,#242000),
(#242001,#242002),(#242003,#242004),(#242005,#242006),(#242007,#242008),
(#242009,#242010),(#242011,#242012),(#242013,#242014),(#242015,#242016),
(#242017,#242018),(#242019,#242020)),.UNSPECIFIED.,.F.,.F.,.F.)
B_SPLINE_SURFACE_WITH_KNOTS((6,1,1,1,1,1,1,1,1,1,1,1,1,1,1,1,1,1,1,1,1,
1,1,1,1,1,1,1,1,1,1,1,1,1,1,1,1,1,1,1,1,1,1,1,1,1,1,1,1,1,1,1,1,1,1,1,1,
1,1,1,1,1,1,1,1,1,1,1,1,1,1,1,1,1,1,1,1,1,1,1,1,1,1,1,1,1,1,1,1,1,1,1,1,
1,1,1,1,1,1,1,1,1,1,1,1,1,1,1,1,1,1,1,1,1,1,1,1,1,1,1,1,1,1,1,1,1,1,1,1,
1,1,1,1,1,1,1,1,1,1,1,1,1,1,1,1,1,1,1,1,1,1,1,1,1,1,1,1,1,1,1,1,1,1,1,1,
1,1,1,1,1,1,1,1,1,1,1,1,1,1,1,1,1,1,1,1,1,1,1,1,1,1,1,1,1,1,1,1,1,1,1,6),
(2,2),(0.,0.005,0.01,0.015,0.02,0.025,0.03,0.035,0.04,0.045,0.05,0.055,
0.06,0.065,0.07,0.075,0.08,0.085,0.09,0.095,0.1,0.105,0.11,0.115,0.12,0.125,
0.13,0.135,0.14,0.145,0.15,0.155,0.16,0.165,0.17,0.175,0.18,0.185,0.19,
0.195,0.2,0.205,0.21,0.215,0.22,0.225,0.23,0.235,0.24,0.245,0.25,0.255,
0.26,0.265,0.27,0.275,0.28,0.285,0.29,0.295,0.3,0.305,0.31,0.315,0.32,0.325,
0.33,0.335,0.34,0.345,0.35,0.355,0.36,0.365,0.37,0.375,0.38,0.385,0.39,
0.395,0.4,0.405,0.41,0.415,0.42,0.425,0.43,0.435,0.44,0.445,0.45,0.455,
0.46,0.465,0.47,0.475,0.48,0.485,0.49,0.495,0.5,0.505,0.51,0.515,0.52,0.525,
0.53,0.535,0.54,0.545,0.55,0.555,0.56,0.565,0.57,0.575,0.58,0.585,0.59,
0.595,0.6,0.605,0.61,0.615,0.62,0.625,0.63,0.635,0.64,0.645,0.65,0.655,
0.66,0.665,0.67,0.675,0.68,0.685,0.690000000000001,0.695000000000001,0.700000000000001,
0.705000000000001,0.710000000000001,0.715000000000001,0.720000000000001,
0.725000000000001,0.730000000000001,0.735000000000001,0.740000000000001,
0.745000000000001,0.750000000000001,0.755000000000001,0.760000000000001,
0.765000000000001,0.770000000000001,0.775000000000001,0.780000000000001,
0.785000000000001,0.790000000000001,0.795000000000001,0.800000000000001,
0.805000000000001,0.810000000000001,0.815000000000001,0.820000000000001,
0.825000000000001,0.830000000000001,0.835000000000001,0.840000000000001,
0.845000000000001,0.850000000000001,0.855000000000001,0.860000000000001,
0.865000000000001,0.870000000000001,0.875000000000001,0.880000000000001,
0.885000000000001,0.890000000000001,0.895000000000001,0.900000000000001,
0.905000000000001,0.910000000000001,0.915000000000001,0.920000000000001,
0.925000000000001,0.930000000000001,0.935000000000001,0.940000000000001,
0.945000000000001,0.950000000000001,0.955000000000001,0.960000000000001,
0.965000000000001,0.970000000000001,0.975000000000001,0.980000000000001,
0.985000000000001,0.990000000000001,0.995000000000001,1.),(0.,1.2),
 .UNSPECIFIED.)
GEOMETRIC_REPRESENTATION_ITEM()
RATIONAL_B_SPLINE_SURFACE(((1.,1.),(1.,1.),(1.,1.),(1.,1.),(1.,1.),(1.,
1.),(1.,1.),(1.,1.),(1.,1.),(1.,1.),(1.,1.),(1.,1.),(1.,1.),(1.,1.),(1.,
1.),(1.,1.),(1.,1.),(1.,1.),(1.,1.),(1.,1.),(1.,1.),(1.,1.),(1.,1.),(1.,
1.),(1.,1.),(1.,1.),(1.,1.),(1.,1.),(1.,1.),(1.,1.),(1.,1.),(1.,1.),(1.,
1.),(1.,1.),(1.,1.),(1.,1.),(1.,1.),(1.,1.),(1.,1.),(1.,1.),(1.,1.),(1.,
1.),(1.,1.),(1.,1.),(1.,1.),(1.,1.),(1.,1.),(1.,1.),(1.,1.),(1.,1.),(1.,
1.),(1.,1.),(1.,1.),(1.,1.),(1.,1.),(1.,1.),(1.,1.),(1.,1.),(1.,1.),(1.,
1.),(1.,1.),(1.,1.),(1.,1.),(1.,1.),(1.,1.),(1.,1.),(1.,1.),(1.,1.),(1.,
1.),(1.,1.),(1.,1.),(1.,1.),(1.,1.),(1.,1.),(1.,1.),(1.,1.),(1.,1.),(1.,
1.),(1.,1.),(1.,1.),(1.,1.),(1.,1.),(1.,1.),(1.,1.),(1.,1.),(1.,1.),(1.,
1.),(1.,1.),(1.,1.),(1.,1.),(1.,1.),(1.,1.),(1.,1.),(1.,1.),(1.,1.),(1.,
1.),(1.,1.),(1.,1.),(1.,1.),(1.,1.),(1.,1.),(1.,1.),(1.,1.),(1.,1.),(1.,
1.),(1.,1.),(1.,1.),(1.,1.),(1.,1.),(1.,1.),(1.,1.),(1.,1.),(1.,1.),(1.,
1.),(1.,1.),(1.,1.),(1.,1.),(1.,1.),(1.,1.),(1.,1.),(1.,1.),(1.,1.),(1.,
1.),(1.,1.),(1.,1.),(1.,1.),(1.,1.),(1.,1.),(1.,1.),(1.,1.),(1.,1.),(1.,
1.),(1.,1.),(1.,1.),(1.,1.),(1.,1.),(1.,1.),(1.,1.),(1.,1.),(1.,1.),(1.,
1.),(1.,1.),(1.,1.),(1.,1.),(1.,1.),(1.,1.),(1.,1.),(1.,1.),(1.,1.),(1.,
1.),(1.,1.),(1.,1.),(1.,1.),(1.,1.),(1.,1.),(1.,1.),(1.,1.),(1.,1.),(1.,
1.),(1.,1.),(1.,1.),(1.,1.),(1.,1.),(1.,1.),(1.,1.),(1.,1.),(1.,1.),(1.,
1.),(1.,1.),(1.,1.),(1.,1.),(1.,1.),(1.,1.),(1.,1.),(1.,1.),(1.,1.),(1.,
1.),(1.,1.),(1.,1.),(1.,1.),(1.,1.),(1.,1.),(1.,1.),(1.,1.),(1.,1.),(1.,
1.),(1.,1.),(1.,1.),(1.,1.),(1.,1.),(1.,1.),(1.,1.),(1.,1.),(1.,1.),(1.,
1.),(1.,1.),(1.,1.),(1.,1.),(1.,1.),(1.,1.),(1.,1.),(1.,1.),(1.,1.),(1.,
1.),(1.,1.)))
REPRESENTATION_ITEM('')
SURFACE()
);
#1107=(
BOUNDED_SURFACE()
B_SPLINE_SURFACE(5,1,((#242440,#242441),(#242442,#242443),(#242444,#242445),
(#242446,#242447),(#242448,#242449),(#242450,#242451),(#242452,#242453),
(#242454,#242455),(#242456,#242457),(#242458,#242459),(#242460,#242461),
(#242462,#242463),(#242464,#242465),(#242466,#242467),(#242468,#242469),
(#242470,#242471),(#242472,#242473),(#242474,#242475),(#242476,#242477),
(#242478,#242479),(#242480,#242481),(#242482,#242483),(#242484,#242485),
(#242486,#242487),(#242488,#242489),(#242490,#242491),(#242492,#242493),
(#242494,#242495),(#242496,#242497),(#242498,#242499),(#242500,#242501),
(#242502,#242503),(#242504,#242505),(#242506,#242507),(#242508,#242509),
(#242510,#242511),(#242512,#242513),(#242514,#242515),(#242516,#242517),
(#242518,#242519),(#242520,#242521),(#242522,#242523),(#242524,#242525),
(#242526,#242527),(#242528,#242529),(#242530,#242531),(#242532,#242533),
(#242534,#242535),(#242536,#242537),(#242538,#242539),(#242540,#242541),
(#242542,#242543),(#242544,#242545),(#242546,#242547),(#242548,#242549),
(#242550,#242551),(#242552,#242553),(#242554,#242555),(#242556,#242557),
(#242558,#242559),(#242560,#242561),(#242562,#242563),(#242564,#242565),
(#242566,#242567),(#242568,#242569),(#242570,#242571),(#242572,#242573),
(#242574,#242575),(#242576,#242577),(#242578,#242579),(#242580,#242581),
(#242582,#242583),(#242584,#242585),(#242586,#242587),(#242588,#242589),
(#242590,#242591),(#242592,#242593),(#242594,#242595),(#242596,#242597),
(#242598,#242599),(#242600,#242601),(#242602,#242603),(#242604,#242605),
(#242606,#242607),(#242608,#242609),(#242610,#242611),(#242612,#242613),
(#242614,#242615),(#242616,#242617),(#242618,#242619),(#242620,#242621),
(#242622,#242623),(#242624,#242625),(#242626,#242627),(#242628,#242629),
(#242630,#242631),(#242632,#242633),(#242634,#242635),(#242636,#242637),
(#242638,#242639),(#242640,#242641),(#242642,#242643),(#242644,#242645),
(#242646,#242647),(#242648,#242649),(#242650,#242651),(#242652,#242653),
(#242654,#242655),(#242656,#242657),(#242658,#242659),(#242660,#242661),
(#242662,#242663),(#242664,#242665),(#242666,#242667),(#242668,#242669),
(#242670,#242671),(#242672,#242673),(#242674,#242675),(#242676,#242677),
(#242678,#242679),(#242680,#242681),(#242682,#242683),(#242684,#242685),
(#242686,#242687),(#242688,#242689),(#242690,#242691),(#242692,#242693),
(#242694,#242695),(#242696,#242697),(#242698,#242699),(#242700,#242701),
(#242702,#242703),(#242704,#242705),(#242706,#242707),(#242708,#242709),
(#242710,#242711),(#242712,#242713),(#242714,#242715),(#242716,#242717),
(#242718,#242719),(#242720,#242721),(#242722,#242723),(#242724,#242725),
(#242726,#242727),(#242728,#242729),(#242730,#242731),(#242732,#242733),
(#242734,#242735),(#242736,#242737),(#242738,#242739),(#242740,#242741),
(#242742,#242743),(#242744,#242745),(#242746,#242747),(#242748,#242749),
(#242750,#242751),(#242752,#242753),(#242754,#242755),(#242756,#242757),
(#242758,#242759),(#242760,#242761),(#242762,#242763),(#242764,#242765),
(#242766,#242767),(#242768,#242769),(#242770,#242771),(#242772,#242773),
(#242774,#242775),(#242776,#242777),(#242778,#242779),(#242780,#242781),
(#242782,#242783),(#242784,#242785),(#242786,#242787),(#242788,#242789),
(#242790,#242791),(#242792,#242793),(#242794,#242795),(#242796,#242797),
(#242798,#242799),(#242800,#242801),(#242802,#242803),(#242804,#242805),
(#242806,#242807),(#242808,#242809),(#242810,#242811),(#242812,#242813),
(#242814,#242815),(#242816,#242817),(#242818,#242819),(#242820,#242821),
(#242822,#242823),(#242824,#242825),(#242826,#242827),(#242828,#242829),
(#242830,#242831),(#242832,#242833),(#242834,#242835),(#242836,#242837),
(#242838,#242839),(#242840,#242841),(#242842,#242843),(#242844,#242845),
(#242846,#242847),(#242848,#242849)),.UNSPECIFIED.,.F.,.F.,.F.)
B_SPLINE_SURFACE_WITH_KNOTS((6,1,1,1,1,1,1,1,1,1,1,1,1,1,1,1,1,1,1,1,1,
1,1,1,1,1,1,1,1,1,1,1,1,1,1,1,1,1,1,1,1,1,1,1,1,1,1,1,1,1,1,1,1,1,1,1,1,
1,1,1,1,1,1,1,1,1,1,1,1,1,1,1,1,1,1,1,1,1,1,1,1,1,1,1,1,1,1,1,1,1,1,1,1,
1,1,1,1,1,1,1,1,1,1,1,1,1,1,1,1,1,1,1,1,1,1,1,1,1,1,1,1,1,1,1,1,1,1,1,1,
1,1,1,1,1,1,1,1,1,1,1,1,1,1,1,1,1,1,1,1,1,1,1,1,1,1,1,1,1,1,1,1,1,1,1,1,
1,1,1,1,1,1,1,1,1,1,1,1,1,1,1,1,1,1,1,1,1,1,1,1,1,1,1,1,1,1,1,1,1,1,1,6),
(2,2),(-1.,-0.995000000000001,-0.990000000000001,-0.985000000000001,-0.980000000000001,
-0.975000000000001,-0.970000000000001,-0.965000000000001,-0.960000000000001,
-0.955000000000001,-0.950000000000001,-0.945000000000001,-0.940000000000001,
-0.935000000000001,-0.930000000000001,-0.925000000000001,-0.920000000000001,
-0.915000000000001,-0.910000000000001,-0.905000000000001,-0.900000000000001,
-0.895000000000001,-0.890000000000001,-0.885000000000001,-0.880000000000001,
-0.875000000000001,-0.870000000000001,-0.865000000000001,-0.860000000000001,
-0.855000000000001,-0.850000000000001,-0.845000000000001,-0.840000000000001,
-0.835000000000001,-0.830000000000001,-0.825000000000001,-0.820000000000001,
-0.815000000000001,-0.810000000000001,-0.805000000000001,-0.800000000000001,
-0.795000000000001,-0.790000000000001,-0.785000000000001,-0.780000000000001,
-0.775000000000001,-0.770000000000001,-0.765000000000001,-0.760000000000001,
-0.755000000000001,-0.750000000000001,-0.745000000000001,-0.740000000000001,
-0.735000000000001,-0.730000000000001,-0.725000000000001,-0.720000000000001,
-0.715000000000001,-0.710000000000001,-0.705000000000001,-0.700000000000001,
-0.695000000000001,-0.690000000000001,-0.685,-0.68,-0.675,-0.67,-0.665,
-0.66,-0.655,-0.65,-0.645,-0.64,-0.635,-0.63,-0.625,-0.62,-0.615,-0.61,
-0.605,-0.6,-0.595,-0.59,-0.585,-0.58,-0.575,-0.57,-0.565,-0.56,-0.555,
-0.55,-0.545,-0.54,-0.535,-0.53,-0.525,-0.52,-0.515,-0.51,-0.505,-0.5,-0.495,
-0.49,-0.485,-0.48,-0.475,-0.47,-0.465,-0.46,-0.455,-0.45,-0.445,-0.44,
-0.435,-0.43,-0.425,-0.42,-0.415,-0.41,-0.405,-0.4,-0.395,-0.39,-0.385,
-0.38,-0.375,-0.37,-0.365,-0.36,-0.355,-0.35,-0.345,-0.34,-0.335,-0.33,
-0.325,-0.32,-0.315,-0.31,-0.305,-0.3,-0.295,-0.29,-0.285,-0.28,-0.275,
-0.27,-0.265,-0.26,-0.255,-0.25,-0.245,-0.24,-0.235,-0.23,-0.225,-0.22,
-0.215,-0.21,-0.205,-0.2,-0.195,-0.19,-0.185,-0.18,-0.175,-0.17,-0.165,
-0.16,-0.155,-0.15,-0.145,-0.14,-0.135,-0.13,-0.125,-0.12,-0.115,-0.11,
-0.105,-0.1,-0.095,-0.09,-0.085,-0.08,-0.075,-0.07,-0.065,-0.06,-0.055,
-0.05,-0.045,-0.04,-0.035,-0.03,-0.025,-0.02,-0.015,-0.01,-0.005,0.),(0.,
1.2),.UNSPECIFIED.)
GEOMETRIC_REPRESENTATION_ITEM()
RATIONAL_B_SPLINE_SURFACE(((1.,1.),(1.,1.),(1.,1.),(1.,1.),(1.,1.),(1.,
1.),(1.,1.),(1.,1.),(1.,1.),(1.,1.),(1.,1.),(1.,1.),(1.,1.),(1.,1.),(1.,
1.),(1.,1.),(1.,1.),(1.,1.),(1.,1.),(1.,1.),(1.,1.),(1.,1.),(1.,1.),(1.,
1.),(1.,1.),(1.,1.),(1.,1.),(1.,1.),(1.,1.),(1.,1.),(1.,1.),(1.,1.),(1.,
1.),(1.,1.),(1.,1.),(1.,1.),(1.,1.),(1.,1.),(1.,1.),(1.,1.),(1.,1.),(1.,
1.),(1.,1.),(1.,1.),(1.,1.),(1.,1.),(1.,1.),(1.,1.),(1.,1.),(1.,1.),(1.,
1.),(1.,1.),(1.,1.),(1.,1.),(1.,1.),(1.,1.),(1.,1.),(1.,1.),(1.,1.),(1.,
1.),(1.,1.),(1.,1.),(1.,1.),(1.,1.),(1.,1.),(1.,1.),(1.,1.),(1.,1.),(1.,
1.),(1.,1.),(1.,1.),(1.,1.),(1.,1.),(1.,1.),(1.,1.),(1.,1.),(1.,1.),(1.,
1.),(1.,1.),(1.,1.),(1.,1.),(1.,1.),(1.,1.),(1.,1.),(1.,1.),(1.,1.),(1.,
1.),(1.,1.),(1.,1.),(1.,1.),(1.,1.),(1.,1.),(1.,1.),(1.,1.),(1.,1.),(1.,
1.),(1.,1.),(1.,1.),(1.,1.),(1.,1.),(1.,1.),(1.,1.),(1.,1.),(1.,1.),(1.,
1.),(1.,1.),(1.,1.),(1.,1.),(1.,1.),(1.,1.),(1.,1.),(1.,1.),(1.,1.),(1.,
1.),(1.,1.),(1.,1.),(1.,1.),(1.,1.),(1.,1.),(1.,1.),(1.,1.),(1.,1.),(1.,
1.),(1.,1.),(1.,1.),(1.,1.),(1.,1.),(1.,1.),(1.,1.),(1.,1.),(1.,1.),(1.,
1.),(1.,1.),(1.,1.),(1.,1.),(1.,1.),(1.,1.),(1.,1.),(1.,1.),(1.,1.),(1.,
1.),(1.,1.),(1.,1.),(1.,1.),(1.,1.),(1.,1.),(1.,1.),(1.,1.),(1.,1.),(1.,
1.),(1.,1.),(1.,1.),(1.,1.),(1.,1.),(1.,1.),(1.,1.),(1.,1.),(1.,1.),(1.,
1.),(1.,1.),(1.,1.),(1.,1.),(1.,1.),(1.,1.),(1.,1.),(1.,1.),(1.,1.),(1.,
1.),(1.,1.),(1.,1.),(1.,1.),(1.,1.),(1.,1.),(1.,1.),(1.,1.),(1.,1.),(1.,
1.),(1.,1.),(1.,1.),(1.,1.),(1.,1.),(1.,1.),(1.,1.),(1.,1.),(1.,1.),(1.,
1.),(1.,1.),(1.,1.),(1.,1.),(1.,1.),(1.,1.),(1.,1.),(1.,1.),(1.,1.),(1.,
1.),(1.,1.),(1.,1.),(1.,1.),(1.,1.),(1.,1.),(1.,1.),(1.,1.),(1.,1.),(1.,
1.),(1.,1.)))
REPRESENTATION_ITEM('')
SURFACE()
);
#1108=(
BOUNDED_SURFACE()
B_SPLINE_SURFACE(5,1,((#243263,#243264),(#243265,#243266),(#243267,#243268),
(#243269,#243270),(#243271,#243272),(#243273,#243274),(#243275,#243276),
(#243277,#243278),(#243279,#243280),(#243281,#243282),(#243283,#243284),
(#243285,#243286),(#243287,#243288),(#243289,#243290),(#243291,#243292),
(#243293,#243294),(#243295,#243296),(#243297,#243298),(#243299,#243300),
(#243301,#243302),(#243303,#243304),(#243305,#243306),(#243307,#243308),
(#243309,#243310),(#243311,#243312),(#243313,#243314),(#243315,#243316),
(#243317,#243318),(#243319,#243320),(#243321,#243322),(#243323,#243324),
(#243325,#243326),(#243327,#243328),(#243329,#243330),(#243331,#243332),
(#243333,#243334),(#243335,#243336),(#243337,#243338),(#243339,#243340),
(#243341,#243342),(#243343,#243344),(#243345,#243346),(#243347,#243348),
(#243349,#243350),(#243351,#243352),(#243353,#243354),(#243355,#243356),
(#243357,#243358),(#243359,#243360),(#243361,#243362),(#243363,#243364),
(#243365,#243366),(#243367,#243368),(#243369,#243370),(#243371,#243372),
(#243373,#243374),(#243375,#243376),(#243377,#243378),(#243379,#243380),
(#243381,#243382),(#243383,#243384),(#243385,#243386),(#243387,#243388),
(#243389,#243390),(#243391,#243392),(#243393,#243394),(#243395,#243396),
(#243397,#243398),(#243399,#243400),(#243401,#243402),(#243403,#243404),
(#243405,#243406),(#243407,#243408),(#243409,#243410),(#243411,#243412),
(#243413,#243414),(#243415,#243416),(#243417,#243418),(#243419,#243420),
(#243421,#243422),(#243423,#243424),(#243425,#243426),(#243427,#243428),
(#243429,#243430),(#243431,#243432),(#243433,#243434),(#243435,#243436),
(#243437,#243438),(#243439,#243440),(#243441,#243442),(#243443,#243444),
(#243445,#243446),(#243447,#243448),(#243449,#243450),(#243451,#243452),
(#243453,#243454),(#243455,#243456),(#243457,#243458),(#243459,#243460),
(#243461,#243462),(#243463,#243464),(#243465,#243466),(#243467,#243468),
(#243469,#243470),(#243471,#243472),(#243473,#243474),(#243475,#243476),
(#243477,#243478),(#243479,#243480),(#243481,#243482),(#243483,#243484),
(#243485,#243486),(#243487,#243488),(#243489,#243490),(#243491,#243492),
(#243493,#243494),(#243495,#243496),(#243497,#243498),(#243499,#243500),
(#243501,#243502),(#243503,#243504),(#243505,#243506),(#243507,#243508),
(#243509,#243510),(#243511,#243512),(#243513,#243514),(#243515,#243516),
(#243517,#243518),(#243519,#243520),(#243521,#243522),(#243523,#243524),
(#243525,#243526),(#243527,#243528),(#243529,#243530),(#243531,#243532),
(#243533,#243534),(#243535,#243536),(#243537,#243538),(#243539,#243540),
(#243541,#243542),(#243543,#243544),(#243545,#243546),(#243547,#243548),
(#243549,#243550),(#243551,#243552),(#243553,#243554),(#243555,#243556),
(#243557,#243558),(#243559,#243560),(#243561,#243562),(#243563,#243564),
(#243565,#243566),(#243567,#243568),(#243569,#243570),(#243571,#243572),
(#243573,#243574),(#243575,#243576),(#243577,#243578),(#243579,#243580),
(#243581,#243582),(#243583,#243584),(#243585,#243586),(#243587,#243588),
(#243589,#243590),(#243591,#243592),(#243593,#243594),(#243595,#243596),
(#243597,#243598),(#243599,#243600),(#243601,#243602),(#243603,#243604),
(#243605,#243606),(#243607,#243608),(#243609,#243610),(#243611,#243612),
(#243613,#243614),(#243615,#243616),(#243617,#243618),(#243619,#243620),
(#243621,#243622),(#243623,#243624),(#243625,#243626),(#243627,#243628),
(#243629,#243630),(#243631,#243632),(#243633,#243634),(#243635,#243636),
(#243637,#243638),(#243639,#243640),(#243641,#243642),(#243643,#243644),
(#243645,#243646),(#243647,#243648),(#243649,#243650),(#243651,#243652),
(#243653,#243654),(#243655,#243656),(#243657,#243658),(#243659,#243660),
(#243661,#243662),(#243663,#243664),(#243665,#243666),(#243667,#243668),
(#243669,#243670),(#243671,#243672)),.UNSPECIFIED.,.F.,.F.,.F.)
B_SPLINE_SURFACE_WITH_KNOTS((6,1,1,1,1,1,1,1,1,1,1,1,1,1,1,1,1,1,1,1,1,
1,1,1,1,1,1,1,1,1,1,1,1,1,1,1,1,1,1,1,1,1,1,1,1,1,1,1,1,1,1,1,1,1,1,1,1,
1,1,1,1,1,1,1,1,1,1,1,1,1,1,1,1,1,1,1,1,1,1,1,1,1,1,1,1,1,1,1,1,1,1,1,1,
1,1,1,1,1,1,1,1,1,1,1,1,1,1,1,1,1,1,1,1,1,1,1,1,1,1,1,1,1,1,1,1,1,1,1,1,
1,1,1,1,1,1,1,1,1,1,1,1,1,1,1,1,1,1,1,1,1,1,1,1,1,1,1,1,1,1,1,1,1,1,1,1,
1,1,1,1,1,1,1,1,1,1,1,1,1,1,1,1,1,1,1,1,1,1,1,1,1,1,1,1,1,1,1,1,1,1,1,6),
(2,2),(0.,0.005,0.01,0.015,0.02,0.025,0.03,0.035,0.04,0.045,0.05,0.055,
0.06,0.065,0.07,0.075,0.08,0.085,0.09,0.095,0.1,0.105,0.11,0.115,0.12,0.125,
0.13,0.135,0.14,0.145,0.15,0.155,0.16,0.165,0.17,0.175,0.18,0.185,0.19,
0.195,0.2,0.205,0.21,0.215,0.22,0.225,0.23,0.235,0.24,0.245,0.25,0.255,
0.26,0.265,0.27,0.275,0.28,0.285,0.29,0.295,0.3,0.305,0.31,0.315,0.32,0.325,
0.33,0.335,0.34,0.345,0.35,0.355,0.36,0.365,0.37,0.375,0.38,0.385,0.39,
0.395,0.4,0.405,0.41,0.415,0.42,0.425,0.43,0.435,0.44,0.445,0.45,0.455,
0.46,0.465,0.47,0.475,0.48,0.485,0.49,0.495,0.5,0.505,0.51,0.515,0.52,0.525,
0.53,0.535,0.54,0.545,0.55,0.555,0.56,0.565,0.57,0.575,0.58,0.585,0.59,
0.595,0.6,0.605,0.61,0.615,0.62,0.625,0.63,0.635,0.64,0.645,0.65,0.655,
0.66,0.665,0.67,0.675,0.68,0.685,0.690000000000001,0.695000000000001,0.700000000000001,
0.705000000000001,0.710000000000001,0.715000000000001,0.720000000000001,
0.725000000000001,0.730000000000001,0.735000000000001,0.740000000000001,
0.745000000000001,0.750000000000001,0.755000000000001,0.760000000000001,
0.765000000000001,0.770000000000001,0.775000000000001,0.780000000000001,
0.785000000000001,0.790000000000001,0.795000000000001,0.800000000000001,
0.805000000000001,0.810000000000001,0.815000000000001,0.820000000000001,
0.825000000000001,0.830000000000001,0.835000000000001,0.840000000000001,
0.845000000000001,0.850000000000001,0.855000000000001,0.860000000000001,
0.865000000000001,0.870000000000001,0.875000000000001,0.880000000000001,
0.885000000000001,0.890000000000001,0.895000000000001,0.900000000000001,
0.905000000000001,0.910000000000001,0.915000000000001,0.920000000000001,
0.925000000000001,0.930000000000001,0.935000000000001,0.940000000000001,
0.945000000000001,0.950000000000001,0.955000000000001,0.960000000000001,
0.965000000000001,0.970000000000001,0.975000000000001,0.980000000000001,
0.985000000000001,0.990000000000001,0.995000000000001,1.),(0.,1.2),
 .UNSPECIFIED.)
GEOMETRIC_REPRESENTATION_ITEM()
RATIONAL_B_SPLINE_SURFACE(((1.,1.),(1.,1.),(1.,1.),(1.,1.),(1.,1.),(1.,
1.),(1.,1.),(1.,1.),(1.,1.),(1.,1.),(1.,1.),(1.,1.),(1.,1.),(1.,1.),(1.,
1.),(1.,1.),(1.,1.),(1.,1.),(1.,1.),(1.,1.),(1.,1.),(1.,1.),(1.,1.),(1.,
1.),(1.,1.),(1.,1.),(1.,1.),(1.,1.),(1.,1.),(1.,1.),(1.,1.),(1.,1.),(1.,
1.),(1.,1.),(1.,1.),(1.,1.),(1.,1.),(1.,1.),(1.,1.),(1.,1.),(1.,1.),(1.,
1.),(1.,1.),(1.,1.),(1.,1.),(1.,1.),(1.,1.),(1.,1.),(1.,1.),(1.,1.),(1.,
1.),(1.,1.),(1.,1.),(1.,1.),(1.,1.),(1.,1.),(1.,1.),(1.,1.),(1.,1.),(1.,
1.),(1.,1.),(1.,1.),(1.,1.),(1.,1.),(1.,1.),(1.,1.),(1.,1.),(1.,1.),(1.,
1.),(1.,1.),(1.,1.),(1.,1.),(1.,1.),(1.,1.),(1.,1.),(1.,1.),(1.,1.),(1.,
1.),(1.,1.),(1.,1.),(1.,1.),(1.,1.),(1.,1.),(1.,1.),(1.,1.),(1.,1.),(1.,
1.),(1.,1.),(1.,1.),(1.,1.),(1.,1.),(1.,1.),(1.,1.),(1.,1.),(1.,1.),(1.,
1.),(1.,1.),(1.,1.),(1.,1.),(1.,1.),(1.,1.),(1.,1.),(1.,1.),(1.,1.),(1.,
1.),(1.,1.),(1.,1.),(1.,1.),(1.,1.),(1.,1.),(1.,1.),(1.,1.),(1.,1.),(1.,
1.),(1.,1.),(1.,1.),(1.,1.),(1.,1.),(1.,1.),(1.,1.),(1.,1.),(1.,1.),(1.,
1.),(1.,1.),(1.,1.),(1.,1.),(1.,1.),(1.,1.),(1.,1.),(1.,1.),(1.,1.),(1.,
1.),(1.,1.),(1.,1.),(1.,1.),(1.,1.),(1.,1.),(1.,1.),(1.,1.),(1.,1.),(1.,
1.),(1.,1.),(1.,1.),(1.,1.),(1.,1.),(1.,1.),(1.,1.),(1.,1.),(1.,1.),(1.,
1.),(1.,1.),(1.,1.),(1.,1.),(1.,1.),(1.,1.),(1.,1.),(1.,1.),(1.,1.),(1.,
1.),(1.,1.),(1.,1.),(1.,1.),(1.,1.),(1.,1.),(1.,1.),(1.,1.),(1.,1.),(1.,
1.),(1.,1.),(1.,1.),(1.,1.),(1.,1.),(1.,1.),(1.,1.),(1.,1.),(1.,1.),(1.,
1.),(1.,1.),(1.,1.),(1.,1.),(1.,1.),(1.,1.),(1.,1.),(1.,1.),(1.,1.),(1.,
1.),(1.,1.),(1.,1.),(1.,1.),(1.,1.),(1.,1.),(1.,1.),(1.,1.),(1.,1.),(1.,
1.),(1.,1.),(1.,1.),(1.,1.),(1.,1.),(1.,1.),(1.,1.),(1.,1.),(1.,1.),(1.,
1.),(1.,1.)))
REPRESENTATION_ITEM('')
SURFACE()
);
#1109=(
BOUNDED_SURFACE()
B_SPLINE_SURFACE(5,1,((#244092,#244093),(#244094,#244095),(#244096,#244097),
(#244098,#244099),(#244100,#244101),(#244102,#244103),(#244104,#244105),
(#244106,#244107),(#244108,#244109),(#244110,#244111),(#244112,#244113),
(#244114,#244115),(#244116,#244117),(#244118,#244119),(#244120,#244121),
(#244122,#244123),(#244124,#244125),(#244126,#244127),(#244128,#244129),
(#244130,#244131),(#244132,#244133),(#244134,#244135),(#244136,#244137),
(#244138,#244139),(#244140,#244141),(#244142,#244143),(#244144,#244145),
(#244146,#244147),(#244148,#244149),(#244150,#244151),(#244152,#244153),
(#244154,#244155),(#244156,#244157),(#244158,#244159),(#244160,#244161),
(#244162,#244163),(#244164,#244165),(#244166,#244167),(#244168,#244169),
(#244170,#244171),(#244172,#244173),(#244174,#244175),(#244176,#244177),
(#244178,#244179),(#244180,#244181),(#244182,#244183),(#244184,#244185),
(#244186,#244187),(#244188,#244189),(#244190,#244191),(#244192,#244193),
(#244194,#244195),(#244196,#244197),(#244198,#244199),(#244200,#244201),
(#244202,#244203),(#244204,#244205),(#244206,#244207),(#244208,#244209),
(#244210,#244211),(#244212,#244213),(#244214,#244215),(#244216,#244217),
(#244218,#244219),(#244220,#244221),(#244222,#244223),(#244224,#244225),
(#244226,#244227),(#244228,#244229),(#244230,#244231),(#244232,#244233),
(#244234,#244235),(#244236,#244237),(#244238,#244239),(#244240,#244241),
(#244242,#244243),(#244244,#244245),(#244246,#244247),(#244248,#244249),
(#244250,#244251),(#244252,#244253),(#244254,#244255),(#244256,#244257),
(#244258,#244259),(#244260,#244261),(#244262,#244263),(#244264,#244265),
(#244266,#244267),(#244268,#244269),(#244270,#244271),(#244272,#244273),
(#244274,#244275),(#244276,#244277),(#244278,#244279),(#244280,#244281),
(#244282,#244283),(#244284,#244285),(#244286,#244287),(#244288,#244289),
(#244290,#244291),(#244292,#244293),(#244294,#244295),(#244296,#244297),
(#244298,#244299),(#244300,#244301),(#244302,#244303),(#244304,#244305),
(#244306,#244307),(#244308,#244309),(#244310,#244311),(#244312,#244313),
(#244314,#244315),(#244316,#244317),(#244318,#244319),(#244320,#244321),
(#244322,#244323),(#244324,#244325),(#244326,#244327),(#244328,#244329),
(#244330,#244331),(#244332,#244333),(#244334,#244335),(#244336,#244337),
(#244338,#244339),(#244340,#244341),(#244342,#244343),(#244344,#244345),
(#244346,#244347),(#244348,#244349),(#244350,#244351),(#244352,#244353),
(#244354,#244355),(#244356,#244357),(#244358,#244359),(#244360,#244361),
(#244362,#244363),(#244364,#244365),(#244366,#244367),(#244368,#244369),
(#244370,#244371),(#244372,#244373),(#244374,#244375),(#244376,#244377),
(#244378,#244379),(#244380,#244381),(#244382,#244383),(#244384,#244385),
(#244386,#244387),(#244388,#244389),(#244390,#244391),(#244392,#244393),
(#244394,#244395),(#244396,#244397),(#244398,#244399),(#244400,#244401),
(#244402,#244403),(#244404,#244405),(#244406,#244407),(#244408,#244409),
(#244410,#244411),(#244412,#244413),(#244414,#244415),(#244416,#244417),
(#244418,#244419),(#244420,#244421),(#244422,#244423),(#244424,#244425),
(#244426,#244427),(#244428,#244429),(#244430,#244431),(#244432,#244433),
(#244434,#244435),(#244436,#244437),(#244438,#244439),(#244440,#244441),
(#244442,#244443),(#244444,#244445),(#244446,#244447),(#244448,#244449),
(#244450,#244451),(#244452,#244453),(#244454,#244455),(#244456,#244457),
(#244458,#244459),(#244460,#244461),(#244462,#244463),(#244464,#244465),
(#244466,#244467),(#244468,#244469),(#244470,#244471),(#244472,#244473),
(#244474,#244475),(#244476,#244477),(#244478,#244479),(#244480,#244481),
(#244482,#244483),(#244484,#244485),(#244486,#244487),(#244488,#244489),
(#244490,#244491),(#244492,#244493),(#244494,#244495),(#244496,#244497),
(#244498,#244499),(#244500,#244501)),.UNSPECIFIED.,.F.,.F.,.F.)
B_SPLINE_SURFACE_WITH_KNOTS((6,1,1,1,1,1,1,1,1,1,1,1,1,1,1,1,1,1,1,1,1,
1,1,1,1,1,1,1,1,1,1,1,1,1,1,1,1,1,1,1,1,1,1,1,1,1,1,1,1,1,1,1,1,1,1,1,1,
1,1,1,1,1,1,1,1,1,1,1,1,1,1,1,1,1,1,1,1,1,1,1,1,1,1,1,1,1,1,1,1,1,1,1,1,
1,1,1,1,1,1,1,1,1,1,1,1,1,1,1,1,1,1,1,1,1,1,1,1,1,1,1,1,1,1,1,1,1,1,1,1,
1,1,1,1,1,1,1,1,1,1,1,1,1,1,1,1,1,1,1,1,1,1,1,1,1,1,1,1,1,1,1,1,1,1,1,1,
1,1,1,1,1,1,1,1,1,1,1,1,1,1,1,1,1,1,1,1,1,1,1,1,1,1,1,1,1,1,1,1,1,1,1,6),
(2,2),(-1.,-0.995000000000001,-0.990000000000001,-0.985000000000001,-0.980000000000001,
-0.975000000000001,-0.970000000000001,-0.965000000000001,-0.960000000000001,
-0.955000000000001,-0.950000000000001,-0.945000000000001,-0.940000000000001,
-0.935000000000001,-0.930000000000001,-0.925000000000001,-0.920000000000001,
-0.915000000000001,-0.910000000000001,-0.905000000000001,-0.900000000000001,
-0.895000000000001,-0.890000000000001,-0.885000000000001,-0.880000000000001,
-0.875000000000001,-0.870000000000001,-0.865000000000001,-0.860000000000001,
-0.855000000000001,-0.850000000000001,-0.845000000000001,-0.840000000000001,
-0.835000000000001,-0.830000000000001,-0.825000000000001,-0.820000000000001,
-0.815000000000001,-0.810000000000001,-0.805000000000001,-0.800000000000001,
-0.795000000000001,-0.790000000000001,-0.785000000000001,-0.780000000000001,
-0.775000000000001,-0.770000000000001,-0.765000000000001,-0.760000000000001,
-0.755000000000001,-0.750000000000001,-0.745000000000001,-0.740000000000001,
-0.735000000000001,-0.730000000000001,-0.725000000000001,-0.720000000000001,
-0.715000000000001,-0.710000000000001,-0.705000000000001,-0.700000000000001,
-0.695000000000001,-0.690000000000001,-0.685,-0.68,-0.675,-0.67,-0.665,
-0.66,-0.655,-0.65,-0.645,-0.64,-0.635,-0.63,-0.625,-0.62,-0.615,-0.61,
-0.605,-0.6,-0.595,-0.59,-0.585,-0.58,-0.575,-0.57,-0.565,-0.56,-0.555,
-0.55,-0.545,-0.54,-0.535,-0.53,-0.525,-0.52,-0.515,-0.51,-0.505,-0.5,-0.495,
-0.49,-0.485,-0.48,-0.475,-0.47,-0.465,-0.46,-0.455,-0.45,-0.445,-0.44,
-0.435,-0.43,-0.425,-0.42,-0.415,-0.41,-0.405,-0.4,-0.395,-0.39,-0.385,
-0.38,-0.375,-0.37,-0.365,-0.36,-0.355,-0.35,-0.345,-0.34,-0.335,-0.33,
-0.325,-0.32,-0.315,-0.31,-0.305,-0.3,-0.295,-0.29,-0.285,-0.28,-0.275,
-0.27,-0.265,-0.26,-0.255,-0.25,-0.245,-0.24,-0.235,-0.23,-0.225,-0.22,
-0.215,-0.21,-0.205,-0.2,-0.195,-0.19,-0.185,-0.18,-0.175,-0.17,-0.165,
-0.16,-0.155,-0.15,-0.145,-0.14,-0.135,-0.13,-0.125,-0.12,-0.115,-0.11,
-0.105,-0.1,-0.095,-0.09,-0.085,-0.08,-0.075,-0.07,-0.065,-0.06,-0.055,
-0.05,-0.045,-0.04,-0.035,-0.03,-0.025,-0.02,-0.015,-0.01,-0.005,0.),(0.,
1.2),.UNSPECIFIED.)
GEOMETRIC_REPRESENTATION_ITEM()
RATIONAL_B_SPLINE_SURFACE(((1.,1.),(1.,1.),(1.,1.),(1.,1.),(1.,1.),(1.,
1.),(1.,1.),(1.,1.),(1.,1.),(1.,1.),(1.,1.),(1.,1.),(1.,1.),(1.,1.),(1.,
1.),(1.,1.),(1.,1.),(1.,1.),(1.,1.),(1.,1.),(1.,1.),(1.,1.),(1.,1.),(1.,
1.),(1.,1.),(1.,1.),(1.,1.),(1.,1.),(1.,1.),(1.,1.),(1.,1.),(1.,1.),(1.,
1.),(1.,1.),(1.,1.),(1.,1.),(1.,1.),(1.,1.),(1.,1.),(1.,1.),(1.,1.),(1.,
1.),(1.,1.),(1.,1.),(1.,1.),(1.,1.),(1.,1.),(1.,1.),(1.,1.),(1.,1.),(1.,
1.),(1.,1.),(1.,1.),(1.,1.),(1.,1.),(1.,1.),(1.,1.),(1.,1.),(1.,1.),(1.,
1.),(1.,1.),(1.,1.),(1.,1.),(1.,1.),(1.,1.),(1.,1.),(1.,1.),(1.,1.),(1.,
1.),(1.,1.),(1.,1.),(1.,1.),(1.,1.),(1.,1.),(1.,1.),(1.,1.),(1.,1.),(1.,
1.),(1.,1.),(1.,1.),(1.,1.),(1.,1.),(1.,1.),(1.,1.),(1.,1.),(1.,1.),(1.,
1.),(1.,1.),(1.,1.),(1.,1.),(1.,1.),(1.,1.),(1.,1.),(1.,1.),(1.,1.),(1.,
1.),(1.,1.),(1.,1.),(1.,1.),(1.,1.),(1.,1.),(1.,1.),(1.,1.),(1.,1.),(1.,
1.),(1.,1.),(1.,1.),(1.,1.),(1.,1.),(1.,1.),(1.,1.),(1.,1.),(1.,1.),(1.,
1.),(1.,1.),(1.,1.),(1.,1.),(1.,1.),(1.,1.),(1.,1.),(1.,1.),(1.,1.),(1.,
1.),(1.,1.),(1.,1.),(1.,1.),(1.,1.),(1.,1.),(1.,1.),(1.,1.),(1.,1.),(1.,
1.),(1.,1.),(1.,1.),(1.,1.),(1.,1.),(1.,1.),(1.,1.),(1.,1.),(1.,1.),(1.,
1.),(1.,1.),(1.,1.),(1.,1.),(1.,1.),(1.,1.),(1.,1.),(1.,1.),(1.,1.),(1.,
1.),(1.,1.),(1.,1.),(1.,1.),(1.,1.),(1.,1.),(1.,1.),(1.,1.),(1.,1.),(1.,
1.),(1.,1.),(1.,1.),(1.,1.),(1.,1.),(1.,1.),(1.,1.),(1.,1.),(1.,1.),(1.,
1.),(1.,1.),(1.,1.),(1.,1.),(1.,1.),(1.,1.),(1.,1.),(1.,1.),(1.,1.),(1.,
1.),(1.,1.),(1.,1.),(1.,1.),(1.,1.),(1.,1.),(1.,1.),(1.,1.),(1.,1.),(1.,
1.),(1.,1.),(1.,1.),(1.,1.),(1.,1.),(1.,1.),(1.,1.),(1.,1.),(1.,1.),(1.,
1.),(1.,1.),(1.,1.),(1.,1.),(1.,1.),(1.,1.),(1.,1.),(1.,1.),(1.,1.),(1.,
1.),(1.,1.)))
REPRESENTATION_ITEM('')
SURFACE()
);
#1110=(
BOUNDED_SURFACE()
B_SPLINE_SURFACE(5,1,((#244915,#244916),(#244917,#244918),(#244919,#244920),
(#244921,#244922),(#244923,#244924),(#244925,#244926),(#244927,#244928),
(#244929,#244930),(#244931,#244932),(#244933,#244934),(#244935,#244936),
(#244937,#244938),(#244939,#244940),(#244941,#244942),(#244943,#244944),
(#244945,#244946),(#244947,#244948),(#244949,#244950),(#244951,#244952),
(#244953,#244954),(#244955,#244956),(#244957,#244958),(#244959,#244960),
(#244961,#244962),(#244963,#244964),(#244965,#244966),(#244967,#244968),
(#244969,#244970),(#244971,#244972),(#244973,#244974),(#244975,#244976),
(#244977,#244978),(#244979,#244980),(#244981,#244982),(#244983,#244984),
(#244985,#244986),(#244987,#244988),(#244989,#244990),(#244991,#244992),
(#244993,#244994),(#244995,#244996),(#244997,#244998),(#244999,#245000),
(#245001,#245002),(#245003,#245004),(#245005,#245006),(#245007,#245008),
(#245009,#245010),(#245011,#245012),(#245013,#245014),(#245015,#245016),
(#245017,#245018),(#245019,#245020),(#245021,#245022),(#245023,#245024),
(#245025,#245026),(#245027,#245028),(#245029,#245030),(#245031,#245032),
(#245033,#245034),(#245035,#245036),(#245037,#245038),(#245039,#245040),
(#245041,#245042),(#245043,#245044),(#245045,#245046),(#245047,#245048),
(#245049,#245050),(#245051,#245052),(#245053,#245054),(#245055,#245056),
(#245057,#245058),(#245059,#245060),(#245061,#245062),(#245063,#245064),
(#245065,#245066),(#245067,#245068),(#245069,#245070),(#245071,#245072),
(#245073,#245074),(#245075,#245076),(#245077,#245078),(#245079,#245080),
(#245081,#245082),(#245083,#245084),(#245085,#245086),(#245087,#245088),
(#245089,#245090),(#245091,#245092),(#245093,#245094),(#245095,#245096),
(#245097,#245098),(#245099,#245100),(#245101,#245102),(#245103,#245104),
(#245105,#245106),(#245107,#245108),(#245109,#245110),(#245111,#245112),
(#245113,#245114),(#245115,#245116),(#245117,#245118),(#245119,#245120),
(#245121,#245122),(#245123,#245124),(#245125,#245126),(#245127,#245128),
(#245129,#245130),(#245131,#245132),(#245133,#245134),(#245135,#245136),
(#245137,#245138),(#245139,#245140),(#245141,#245142),(#245143,#245144),
(#245145,#245146),(#245147,#245148),(#245149,#245150),(#245151,#245152),
(#245153,#245154),(#245155,#245156),(#245157,#245158),(#245159,#245160),
(#245161,#245162),(#245163,#245164),(#245165,#245166),(#245167,#245168),
(#245169,#245170),(#245171,#245172),(#245173,#245174),(#245175,#245176),
(#245177,#245178),(#245179,#245180),(#245181,#245182),(#245183,#245184),
(#245185,#245186),(#245187,#245188),(#245189,#245190),(#245191,#245192),
(#245193,#245194),(#245195,#245196),(#245197,#245198),(#245199,#245200),
(#245201,#245202),(#245203,#245204),(#245205,#245206),(#245207,#245208),
(#245209,#245210),(#245211,#245212),(#245213,#245214),(#245215,#245216),
(#245217,#245218),(#245219,#245220),(#245221,#245222),(#245223,#245224),
(#245225,#245226),(#245227,#245228),(#245229,#245230),(#245231,#245232),
(#245233,#245234),(#245235,#245236),(#245237,#245238),(#245239,#245240),
(#245241,#245242),(#245243,#245244),(#245245,#245246),(#245247,#245248),
(#245249,#245250),(#245251,#245252),(#245253,#245254),(#245255,#245256),
(#245257,#245258),(#245259,#245260),(#245261,#245262),(#245263,#245264),
(#245265,#245266),(#245267,#245268),(#245269,#245270),(#245271,#245272),
(#245273,#245274),(#245275,#245276),(#245277,#245278),(#245279,#245280),
(#245281,#245282),(#245283,#245284),(#245285,#245286),(#245287,#245288),
(#245289,#245290),(#245291,#245292),(#245293,#245294),(#245295,#245296),
(#245297,#245298),(#245299,#245300),(#245301,#245302),(#245303,#245304),
(#245305,#245306),(#245307,#245308),(#245309,#245310),(#245311,#245312),
(#245313,#245314),(#245315,#245316),(#245317,#245318),(#245319,#245320),
(#245321,#245322),(#245323,#245324)),.UNSPECIFIED.,.F.,.F.,.F.)
B_SPLINE_SURFACE_WITH_KNOTS((6,1,1,1,1,1,1,1,1,1,1,1,1,1,1,1,1,1,1,1,1,
1,1,1,1,1,1,1,1,1,1,1,1,1,1,1,1,1,1,1,1,1,1,1,1,1,1,1,1,1,1,1,1,1,1,1,1,
1,1,1,1,1,1,1,1,1,1,1,1,1,1,1,1,1,1,1,1,1,1,1,1,1,1,1,1,1,1,1,1,1,1,1,1,
1,1,1,1,1,1,1,1,1,1,1,1,1,1,1,1,1,1,1,1,1,1,1,1,1,1,1,1,1,1,1,1,1,1,1,1,
1,1,1,1,1,1,1,1,1,1,1,1,1,1,1,1,1,1,1,1,1,1,1,1,1,1,1,1,1,1,1,1,1,1,1,1,
1,1,1,1,1,1,1,1,1,1,1,1,1,1,1,1,1,1,1,1,1,1,1,1,1,1,1,1,1,1,1,1,1,1,1,6),
(2,2),(0.,0.005,0.01,0.015,0.02,0.025,0.03,0.035,0.04,0.045,0.05,0.055,
0.06,0.065,0.07,0.075,0.08,0.085,0.09,0.095,0.1,0.105,0.11,0.115,0.12,0.125,
0.13,0.135,0.14,0.145,0.15,0.155,0.16,0.165,0.17,0.175,0.18,0.185,0.19,
0.195,0.2,0.205,0.21,0.215,0.22,0.225,0.23,0.235,0.24,0.245,0.25,0.255,
0.26,0.265,0.27,0.275,0.28,0.285,0.29,0.295,0.3,0.305,0.31,0.315,0.32,0.325,
0.33,0.335,0.34,0.345,0.35,0.355,0.36,0.365,0.37,0.375,0.38,0.385,0.39,
0.395,0.4,0.405,0.41,0.415,0.42,0.425,0.43,0.435,0.44,0.445,0.45,0.455,
0.46,0.465,0.47,0.475,0.48,0.485,0.49,0.495,0.5,0.505,0.51,0.515,0.52,0.525,
0.53,0.535,0.54,0.545,0.55,0.555,0.56,0.565,0.57,0.575,0.58,0.585,0.59,
0.595,0.6,0.605,0.61,0.615,0.62,0.625,0.63,0.635,0.64,0.645,0.65,0.655,
0.66,0.665,0.67,0.675,0.68,0.685,0.690000000000001,0.695000000000001,0.700000000000001,
0.705000000000001,0.710000000000001,0.715000000000001,0.720000000000001,
0.725000000000001,0.730000000000001,0.735000000000001,0.740000000000001,
0.745000000000001,0.750000000000001,0.755000000000001,0.760000000000001,
0.765000000000001,0.770000000000001,0.775000000000001,0.780000000000001,
0.785000000000001,0.790000000000001,0.795000000000001,0.800000000000001,
0.805000000000001,0.810000000000001,0.815000000000001,0.820000000000001,
0.825000000000001,0.830000000000001,0.835000000000001,0.840000000000001,
0.845000000000001,0.850000000000001,0.855000000000001,0.860000000000001,
0.865000000000001,0.870000000000001,0.875000000000001,0.880000000000001,
0.885000000000001,0.890000000000001,0.895000000000001,0.900000000000001,
0.905000000000001,0.910000000000001,0.915000000000001,0.920000000000001,
0.925000000000001,0.930000000000001,0.935000000000001,0.940000000000001,
0.945000000000001,0.950000000000001,0.955000000000001,0.960000000000001,
0.965000000000001,0.970000000000001,0.975000000000001,0.980000000000001,
0.985000000000001,0.990000000000001,0.995000000000001,1.),(0.,1.2),
 .UNSPECIFIED.)
GEOMETRIC_REPRESENTATION_ITEM()
RATIONAL_B_SPLINE_SURFACE(((1.,1.),(1.,1.),(1.,1.),(1.,1.),(1.,1.),(1.,
1.),(1.,1.),(1.,1.),(1.,1.),(1.,1.),(1.,1.),(1.,1.),(1.,1.),(1.,1.),(1.,
1.),(1.,1.),(1.,1.),(1.,1.),(1.,1.),(1.,1.),(1.,1.),(1.,1.),(1.,1.),(1.,
1.),(1.,1.),(1.,1.),(1.,1.),(1.,1.),(1.,1.),(1.,1.),(1.,1.),(1.,1.),(1.,
1.),(1.,1.),(1.,1.),(1.,1.),(1.,1.),(1.,1.),(1.,1.),(1.,1.),(1.,1.),(1.,
1.),(1.,1.),(1.,1.),(1.,1.),(1.,1.),(1.,1.),(1.,1.),(1.,1.),(1.,1.),(1.,
1.),(1.,1.),(1.,1.),(1.,1.),(1.,1.),(1.,1.),(1.,1.),(1.,1.),(1.,1.),(1.,
1.),(1.,1.),(1.,1.),(1.,1.),(1.,1.),(1.,1.),(1.,1.),(1.,1.),(1.,1.),(1.,
1.),(1.,1.),(1.,1.),(1.,1.),(1.,1.),(1.,1.),(1.,1.),(1.,1.),(1.,1.),(1.,
1.),(1.,1.),(1.,1.),(1.,1.),(1.,1.),(1.,1.),(1.,1.),(1.,1.),(1.,1.),(1.,
1.),(1.,1.),(1.,1.),(1.,1.),(1.,1.),(1.,1.),(1.,1.),(1.,1.),(1.,1.),(1.,
1.),(1.,1.),(1.,1.),(1.,1.),(1.,1.),(1.,1.),(1.,1.),(1.,1.),(1.,1.),(1.,
1.),(1.,1.),(1.,1.),(1.,1.),(1.,1.),(1.,1.),(1.,1.),(1.,1.),(1.,1.),(1.,
1.),(1.,1.),(1.,1.),(1.,1.),(1.,1.),(1.,1.),(1.,1.),(1.,1.),(1.,1.),(1.,
1.),(1.,1.),(1.,1.),(1.,1.),(1.,1.),(1.,1.),(1.,1.),(1.,1.),(1.,1.),(1.,
1.),(1.,1.),(1.,1.),(1.,1.),(1.,1.),(1.,1.),(1.,1.),(1.,1.),(1.,1.),(1.,
1.),(1.,1.),(1.,1.),(1.,1.),(1.,1.),(1.,1.),(1.,1.),(1.,1.),(1.,1.),(1.,
1.),(1.,1.),(1.,1.),(1.,1.),(1.,1.),(1.,1.),(1.,1.),(1.,1.),(1.,1.),(1.,
1.),(1.,1.),(1.,1.),(1.,1.),(1.,1.),(1.,1.),(1.,1.),(1.,1.),(1.,1.),(1.,
1.),(1.,1.),(1.,1.),(1.,1.),(1.,1.),(1.,1.),(1.,1.),(1.,1.),(1.,1.),(1.,
1.),(1.,1.),(1.,1.),(1.,1.),(1.,1.),(1.,1.),(1.,1.),(1.,1.),(1.,1.),(1.,
1.),(1.,1.),(1.,1.),(1.,1.),(1.,1.),(1.,1.),(1.,1.),(1.,1.),(1.,1.),(1.,
1.),(1.,1.),(1.,1.),(1.,1.),(1.,1.),(1.,1.),(1.,1.),(1.,1.),(1.,1.),(1.,
1.),(1.,1.)))
REPRESENTATION_ITEM('')
SURFACE()
);
#1111=(
BOUNDED_SURFACE()
B_SPLINE_SURFACE(5,1,((#245744,#245745),(#245746,#245747),(#245748,#245749),
(#245750,#245751),(#245752,#245753),(#245754,#245755),(#245756,#245757),
(#245758,#245759),(#245760,#245761),(#245762,#245763),(#245764,#245765),
(#245766,#245767),(#245768,#245769),(#245770,#245771),(#245772,#245773),
(#245774,#245775),(#245776,#245777),(#245778,#245779),(#245780,#245781),
(#245782,#245783),(#245784,#245785),(#245786,#245787),(#245788,#245789),
(#245790,#245791),(#245792,#245793),(#245794,#245795),(#245796,#245797),
(#245798,#245799),(#245800,#245801),(#245802,#245803),(#245804,#245805),
(#245806,#245807),(#245808,#245809),(#245810,#245811),(#245812,#245813),
(#245814,#245815),(#245816,#245817),(#245818,#245819),(#245820,#245821),
(#245822,#245823),(#245824,#245825),(#245826,#245827),(#245828,#245829),
(#245830,#245831),(#245832,#245833),(#245834,#245835),(#245836,#245837),
(#245838,#245839),(#245840,#245841),(#245842,#245843),(#245844,#245845),
(#245846,#245847),(#245848,#245849),(#245850,#245851),(#245852,#245853),
(#245854,#245855),(#245856,#245857),(#245858,#245859),(#245860,#245861),
(#245862,#245863),(#245864,#245865),(#245866,#245867),(#245868,#245869),
(#245870,#245871),(#245872,#245873),(#245874,#245875),(#245876,#245877),
(#245878,#245879),(#245880,#245881),(#245882,#245883),(#245884,#245885),
(#245886,#245887),(#245888,#245889),(#245890,#245891),(#245892,#245893),
(#245894,#245895),(#245896,#245897),(#245898,#245899),(#245900,#245901),
(#245902,#245903),(#245904,#245905),(#245906,#245907),(#245908,#245909),
(#245910,#245911),(#245912,#245913),(#245914,#245915),(#245916,#245917),
(#245918,#245919),(#245920,#245921),(#245922,#245923),(#245924,#245925),
(#245926,#245927),(#245928,#245929),(#245930,#245931),(#245932,#245933),
(#245934,#245935),(#245936,#245937),(#245938,#245939),(#245940,#245941),
(#245942,#245943),(#245944,#245945),(#245946,#245947),(#245948,#245949),
(#245950,#245951),(#245952,#245953),(#245954,#245955),(#245956,#245957),
(#245958,#245959),(#245960,#245961),(#245962,#245963),(#245964,#245965),
(#245966,#245967),(#245968,#245969),(#245970,#245971),(#245972,#245973),
(#245974,#245975),(#245976,#245977),(#245978,#245979),(#245980,#245981),
(#245982,#245983),(#245984,#245985),(#245986,#245987),(#245988,#245989),
(#245990,#245991),(#245992,#245993),(#245994,#245995),(#245996,#245997),
(#245998,#245999),(#246000,#246001),(#246002,#246003),(#246004,#246005),
(#246006,#246007),(#246008,#246009),(#246010,#246011),(#246012,#246013),
(#246014,#246015),(#246016,#246017),(#246018,#246019),(#246020,#246021),
(#246022,#246023),(#246024,#246025),(#246026,#246027),(#246028,#246029),
(#246030,#246031),(#246032,#246033),(#246034,#246035),(#246036,#246037),
(#246038,#246039),(#246040,#246041),(#246042,#246043),(#246044,#246045),
(#246046,#246047),(#246048,#246049),(#246050,#246051),(#246052,#246053),
(#246054,#246055),(#246056,#246057),(#246058,#246059),(#246060,#246061),
(#246062,#246063),(#246064,#246065),(#246066,#246067),(#246068,#246069),
(#246070,#246071),(#246072,#246073),(#246074,#246075),(#246076,#246077),
(#246078,#246079),(#246080,#246081),(#246082,#246083),(#246084,#246085),
(#246086,#246087),(#246088,#246089),(#246090,#246091),(#246092,#246093),
(#246094,#246095),(#246096,#246097),(#246098,#246099),(#246100,#246101),
(#246102,#246103),(#246104,#246105),(#246106,#246107),(#246108,#246109),
(#246110,#246111),(#246112,#246113),(#246114,#246115),(#246116,#246117),
(#246118,#246119),(#246120,#246121),(#246122,#246123),(#246124,#246125),
(#246126,#246127),(#246128,#246129),(#246130,#246131),(#246132,#246133),
(#246134,#246135),(#246136,#246137),(#246138,#246139),(#246140,#246141),
(#246142,#246143),(#246144,#246145),(#246146,#246147),(#246148,#246149),
(#246150,#246151),(#246152,#246153)),.UNSPECIFIED.,.F.,.F.,.F.)
B_SPLINE_SURFACE_WITH_KNOTS((6,1,1,1,1,1,1,1,1,1,1,1,1,1,1,1,1,1,1,1,1,
1,1,1,1,1,1,1,1,1,1,1,1,1,1,1,1,1,1,1,1,1,1,1,1,1,1,1,1,1,1,1,1,1,1,1,1,
1,1,1,1,1,1,1,1,1,1,1,1,1,1,1,1,1,1,1,1,1,1,1,1,1,1,1,1,1,1,1,1,1,1,1,1,
1,1,1,1,1,1,1,1,1,1,1,1,1,1,1,1,1,1,1,1,1,1,1,1,1,1,1,1,1,1,1,1,1,1,1,1,
1,1,1,1,1,1,1,1,1,1,1,1,1,1,1,1,1,1,1,1,1,1,1,1,1,1,1,1,1,1,1,1,1,1,1,1,
1,1,1,1,1,1,1,1,1,1,1,1,1,1,1,1,1,1,1,1,1,1,1,1,1,1,1,1,1,1,1,1,1,1,1,6),
(2,2),(-1.,-0.995000000000001,-0.990000000000001,-0.985000000000001,-0.980000000000001,
-0.975000000000001,-0.970000000000001,-0.965000000000001,-0.960000000000001,
-0.955000000000001,-0.950000000000001,-0.945000000000001,-0.940000000000001,
-0.935000000000001,-0.930000000000001,-0.925000000000001,-0.920000000000001,
-0.915000000000001,-0.910000000000001,-0.905000000000001,-0.900000000000001,
-0.895000000000001,-0.890000000000001,-0.885000000000001,-0.880000000000001,
-0.875000000000001,-0.870000000000001,-0.865000000000001,-0.860000000000001,
-0.855000000000001,-0.850000000000001,-0.845000000000001,-0.840000000000001,
-0.835000000000001,-0.830000000000001,-0.825000000000001,-0.820000000000001,
-0.815000000000001,-0.810000000000001,-0.805000000000001,-0.800000000000001,
-0.795000000000001,-0.790000000000001,-0.785000000000001,-0.780000000000001,
-0.775000000000001,-0.770000000000001,-0.765000000000001,-0.760000000000001,
-0.755000000000001,-0.750000000000001,-0.745000000000001,-0.740000000000001,
-0.735000000000001,-0.730000000000001,-0.725000000000001,-0.720000000000001,
-0.715000000000001,-0.710000000000001,-0.705000000000001,-0.700000000000001,
-0.695000000000001,-0.690000000000001,-0.685,-0.68,-0.675,-0.67,-0.665,
-0.66,-0.655,-0.65,-0.645,-0.64,-0.635,-0.63,-0.625,-0.62,-0.615,-0.61,
-0.605,-0.6,-0.595,-0.59,-0.585,-0.58,-0.575,-0.57,-0.565,-0.56,-0.555,
-0.55,-0.545,-0.54,-0.535,-0.53,-0.525,-0.52,-0.515,-0.51,-0.505,-0.5,-0.495,
-0.49,-0.485,-0.48,-0.475,-0.47,-0.465,-0.46,-0.455,-0.45,-0.445,-0.44,
-0.435,-0.43,-0.425,-0.42,-0.415,-0.41,-0.405,-0.4,-0.395,-0.39,-0.385,
-0.38,-0.375,-0.37,-0.365,-0.36,-0.355,-0.35,-0.345,-0.34,-0.335,-0.33,
-0.325,-0.32,-0.315,-0.31,-0.305,-0.3,-0.295,-0.29,-0.285,-0.28,-0.275,
-0.27,-0.265,-0.26,-0.255,-0.25,-0.245,-0.24,-0.235,-0.23,-0.225,-0.22,
-0.215,-0.21,-0.205,-0.2,-0.195,-0.19,-0.185,-0.18,-0.175,-0.17,-0.165,
-0.16,-0.155,-0.15,-0.145,-0.14,-0.135,-0.13,-0.125,-0.12,-0.115,-0.11,
-0.105,-0.1,-0.095,-0.09,-0.085,-0.08,-0.075,-0.07,-0.065,-0.06,-0.055,
-0.05,-0.045,-0.04,-0.035,-0.03,-0.025,-0.02,-0.015,-0.01,-0.005,0.),(0.,
1.2),.UNSPECIFIED.)
GEOMETRIC_REPRESENTATION_ITEM()
RATIONAL_B_SPLINE_SURFACE(((1.,1.),(1.,1.),(1.,1.),(1.,1.),(1.,1.),(1.,
1.),(1.,1.),(1.,1.),(1.,1.),(1.,1.),(1.,1.),(1.,1.),(1.,1.),(1.,1.),(1.,
1.),(1.,1.),(1.,1.),(1.,1.),(1.,1.),(1.,1.),(1.,1.),(1.,1.),(1.,1.),(1.,
1.),(1.,1.),(1.,1.),(1.,1.),(1.,1.),(1.,1.),(1.,1.),(1.,1.),(1.,1.),(1.,
1.),(1.,1.),(1.,1.),(1.,1.),(1.,1.),(1.,1.),(1.,1.),(1.,1.),(1.,1.),(1.,
1.),(1.,1.),(1.,1.),(1.,1.),(1.,1.),(1.,1.),(1.,1.),(1.,1.),(1.,1.),(1.,
1.),(1.,1.),(1.,1.),(1.,1.),(1.,1.),(1.,1.),(1.,1.),(1.,1.),(1.,1.),(1.,
1.),(1.,1.),(1.,1.),(1.,1.),(1.,1.),(1.,1.),(1.,1.),(1.,1.),(1.,1.),(1.,
1.),(1.,1.),(1.,1.),(1.,1.),(1.,1.),(1.,1.),(1.,1.),(1.,1.),(1.,1.),(1.,
1.),(1.,1.),(1.,1.),(1.,1.),(1.,1.),(1.,1.),(1.,1.),(1.,1.),(1.,1.),(1.,
1.),(1.,1.),(1.,1.),(1.,1.),(1.,1.),(1.,1.),(1.,1.),(1.,1.),(1.,1.),(1.,
1.),(1.,1.),(1.,1.),(1.,1.),(1.,1.),(1.,1.),(1.,1.),(1.,1.),(1.,1.),(1.,
1.),(1.,1.),(1.,1.),(1.,1.),(1.,1.),(1.,1.),(1.,1.),(1.,1.),(1.,1.),(1.,
1.),(1.,1.),(1.,1.),(1.,1.),(1.,1.),(1.,1.),(1.,1.),(1.,1.),(1.,1.),(1.,
1.),(1.,1.),(1.,1.),(1.,1.),(1.,1.),(1.,1.),(1.,1.),(1.,1.),(1.,1.),(1.,
1.),(1.,1.),(1.,1.),(1.,1.),(1.,1.),(1.,1.),(1.,1.),(1.,1.),(1.,1.),(1.,
1.),(1.,1.),(1.,1.),(1.,1.),(1.,1.),(1.,1.),(1.,1.),(1.,1.),(1.,1.),(1.,
1.),(1.,1.),(1.,1.),(1.,1.),(1.,1.),(1.,1.),(1.,1.),(1.,1.),(1.,1.),(1.,
1.),(1.,1.),(1.,1.),(1.,1.),(1.,1.),(1.,1.),(1.,1.),(1.,1.),(1.,1.),(1.,
1.),(1.,1.),(1.,1.),(1.,1.),(1.,1.),(1.,1.),(1.,1.),(1.,1.),(1.,1.),(1.,
1.),(1.,1.),(1.,1.),(1.,1.),(1.,1.),(1.,1.),(1.,1.),(1.,1.),(1.,1.),(1.,
1.),(1.,1.),(1.,1.),(1.,1.),(1.,1.),(1.,1.),(1.,1.),(1.,1.),(1.,1.),(1.,
1.),(1.,1.),(1.,1.),(1.,1.),(1.,1.),(1.,1.),(1.,1.),(1.,1.),(1.,1.),(1.,
1.),(1.,1.)))
REPRESENTATION_ITEM('')
SURFACE()
);
#1112=(
BOUNDED_SURFACE()
B_SPLINE_SURFACE(5,1,((#246567,#246568),(#246569,#246570),(#246571,#246572),
(#246573,#246574),(#246575,#246576),(#246577,#246578),(#246579,#246580),
(#246581,#246582),(#246583,#246584),(#246585,#246586),(#246587,#246588),
(#246589,#246590),(#246591,#246592),(#246593,#246594),(#246595,#246596),
(#246597,#246598),(#246599,#246600),(#246601,#246602),(#246603,#246604),
(#246605,#246606),(#246607,#246608),(#246609,#246610),(#246611,#246612),
(#246613,#246614),(#246615,#246616),(#246617,#246618),(#246619,#246620),
(#246621,#246622),(#246623,#246624),(#246625,#246626),(#246627,#246628),
(#246629,#246630),(#246631,#246632),(#246633,#246634),(#246635,#246636),
(#246637,#246638),(#246639,#246640),(#246641,#246642),(#246643,#246644),
(#246645,#246646),(#246647,#246648),(#246649,#246650),(#246651,#246652),
(#246653,#246654),(#246655,#246656),(#246657,#246658),(#246659,#246660),
(#246661,#246662),(#246663,#246664),(#246665,#246666),(#246667,#246668),
(#246669,#246670),(#246671,#246672),(#246673,#246674),(#246675,#246676),
(#246677,#246678),(#246679,#246680),(#246681,#246682),(#246683,#246684),
(#246685,#246686),(#246687,#246688),(#246689,#246690),(#246691,#246692),
(#246693,#246694),(#246695,#246696),(#246697,#246698),(#246699,#246700),
(#246701,#246702),(#246703,#246704),(#246705,#246706),(#246707,#246708),
(#246709,#246710),(#246711,#246712),(#246713,#246714),(#246715,#246716),
(#246717,#246718),(#246719,#246720),(#246721,#246722),(#246723,#246724),
(#246725,#246726),(#246727,#246728),(#246729,#246730),(#246731,#246732),
(#246733,#246734),(#246735,#246736),(#246737,#246738),(#246739,#246740),
(#246741,#246742),(#246743,#246744),(#246745,#246746),(#246747,#246748),
(#246749,#246750),(#246751,#246752),(#246753,#246754),(#246755,#246756),
(#246757,#246758),(#246759,#246760),(#246761,#246762),(#246763,#246764),
(#246765,#246766),(#246767,#246768),(#246769,#246770),(#246771,#246772),
(#246773,#246774),(#246775,#246776),(#246777,#246778),(#246779,#246780),
(#246781,#246782),(#246783,#246784),(#246785,#246786),(#246787,#246788),
(#246789,#246790),(#246791,#246792),(#246793,#246794),(#246795,#246796),
(#246797,#246798),(#246799,#246800),(#246801,#246802),(#246803,#246804),
(#246805,#246806),(#246807,#246808),(#246809,#246810),(#246811,#246812),
(#246813,#246814),(#246815,#246816),(#246817,#246818),(#246819,#246820),
(#246821,#246822),(#246823,#246824),(#246825,#246826),(#246827,#246828),
(#246829,#246830),(#246831,#246832),(#246833,#246834),(#246835,#246836),
(#246837,#246838),(#246839,#246840),(#246841,#246842),(#246843,#246844),
(#246845,#246846),(#246847,#246848),(#246849,#246850),(#246851,#246852),
(#246853,#246854),(#246855,#246856),(#246857,#246858),(#246859,#246860),
(#246861,#246862),(#246863,#246864),(#246865,#246866),(#246867,#246868),
(#246869,#246870),(#246871,#246872),(#246873,#246874),(#246875,#246876),
(#246877,#246878),(#246879,#246880),(#246881,#246882),(#246883,#246884),
(#246885,#246886),(#246887,#246888),(#246889,#246890),(#246891,#246892),
(#246893,#246894),(#246895,#246896),(#246897,#246898),(#246899,#246900),
(#246901,#246902),(#246903,#246904),(#246905,#246906),(#246907,#246908),
(#246909,#246910),(#246911,#246912),(#246913,#246914),(#246915,#246916),
(#246917,#246918),(#246919,#246920),(#246921,#246922),(#246923,#246924),
(#246925,#246926),(#246927,#246928),(#246929,#246930),(#246931,#246932),
(#246933,#246934),(#246935,#246936),(#246937,#246938),(#246939,#246940),
(#246941,#246942),(#246943,#246944),(#246945,#246946),(#246947,#246948),
(#246949,#246950),(#246951,#246952),(#246953,#246954),(#246955,#246956),
(#246957,#246958),(#246959,#246960),(#246961,#246962),(#246963,#246964),
(#246965,#246966),(#246967,#246968),(#246969,#246970),(#246971,#246972),
(#246973,#246974),(#246975,#246976)),.UNSPECIFIED.,.F.,.F.,.F.)
B_SPLINE_SURFACE_WITH_KNOTS((6,1,1,1,1,1,1,1,1,1,1,1,1,1,1,1,1,1,1,1,1,
1,1,1,1,1,1,1,1,1,1,1,1,1,1,1,1,1,1,1,1,1,1,1,1,1,1,1,1,1,1,1,1,1,1,1,1,
1,1,1,1,1,1,1,1,1,1,1,1,1,1,1,1,1,1,1,1,1,1,1,1,1,1,1,1,1,1,1,1,1,1,1,1,
1,1,1,1,1,1,1,1,1,1,1,1,1,1,1,1,1,1,1,1,1,1,1,1,1,1,1,1,1,1,1,1,1,1,1,1,
1,1,1,1,1,1,1,1,1,1,1,1,1,1,1,1,1,1,1,1,1,1,1,1,1,1,1,1,1,1,1,1,1,1,1,1,
1,1,1,1,1,1,1,1,1,1,1,1,1,1,1,1,1,1,1,1,1,1,1,1,1,1,1,1,1,1,1,1,1,1,1,6),
(2,2),(0.,0.005,0.01,0.015,0.02,0.025,0.03,0.035,0.04,0.045,0.05,0.055,
0.06,0.065,0.07,0.075,0.08,0.085,0.09,0.095,0.1,0.105,0.11,0.115,0.12,0.125,
0.13,0.135,0.14,0.145,0.15,0.155,0.16,0.165,0.17,0.175,0.18,0.185,0.19,
0.195,0.2,0.205,0.21,0.215,0.22,0.225,0.23,0.235,0.24,0.245,0.25,0.255,
0.26,0.265,0.27,0.275,0.28,0.285,0.29,0.295,0.3,0.305,0.31,0.315,0.32,0.325,
0.33,0.335,0.34,0.345,0.35,0.355,0.36,0.365,0.37,0.375,0.38,0.385,0.39,
0.395,0.4,0.405,0.41,0.415,0.42,0.425,0.43,0.435,0.44,0.445,0.45,0.455,
0.46,0.465,0.47,0.475,0.48,0.485,0.49,0.495,0.5,0.505,0.51,0.515,0.52,0.525,
0.53,0.535,0.54,0.545,0.55,0.555,0.56,0.565,0.57,0.575,0.58,0.585,0.59,
0.595,0.6,0.605,0.61,0.615,0.62,0.625,0.63,0.635,0.64,0.645,0.65,0.655,
0.66,0.665,0.67,0.675,0.68,0.685,0.690000000000001,0.695000000000001,0.700000000000001,
0.705000000000001,0.710000000000001,0.715000000000001,0.720000000000001,
0.725000000000001,0.730000000000001,0.735000000000001,0.740000000000001,
0.745000000000001,0.750000000000001,0.755000000000001,0.760000000000001,
0.765000000000001,0.770000000000001,0.775000000000001,0.780000000000001,
0.785000000000001,0.790000000000001,0.795000000000001,0.800000000000001,
0.805000000000001,0.810000000000001,0.815000000000001,0.820000000000001,
0.825000000000001,0.830000000000001,0.835000000000001,0.840000000000001,
0.845000000000001,0.850000000000001,0.855000000000001,0.860000000000001,
0.865000000000001,0.870000000000001,0.875000000000001,0.880000000000001,
0.885000000000001,0.890000000000001,0.895000000000001,0.900000000000001,
0.905000000000001,0.910000000000001,0.915000000000001,0.920000000000001,
0.925000000000001,0.930000000000001,0.935000000000001,0.940000000000001,
0.945000000000001,0.950000000000001,0.955000000000001,0.960000000000001,
0.965000000000001,0.970000000000001,0.975000000000001,0.980000000000001,
0.985000000000001,0.990000000000001,0.995000000000001,1.),(0.,1.2),
 .UNSPECIFIED.)
GEOMETRIC_REPRESENTATION_ITEM()
RATIONAL_B_SPLINE_SURFACE(((1.,1.),(1.,1.),(1.,1.),(1.,1.),(1.,1.),(1.,
1.),(1.,1.),(1.,1.),(1.,1.),(1.,1.),(1.,1.),(1.,1.),(1.,1.),(1.,1.),(1.,
1.),(1.,1.),(1.,1.),(1.,1.),(1.,1.),(1.,1.),(1.,1.),(1.,1.),(1.,1.),(1.,
1.),(1.,1.),(1.,1.),(1.,1.),(1.,1.),(1.,1.),(1.,1.),(1.,1.),(1.,1.),(1.,
1.),(1.,1.),(1.,1.),(1.,1.),(1.,1.),(1.,1.),(1.,1.),(1.,1.),(1.,1.),(1.,
1.),(1.,1.),(1.,1.),(1.,1.),(1.,1.),(1.,1.),(1.,1.),(1.,1.),(1.,1.),(1.,
1.),(1.,1.),(1.,1.),(1.,1.),(1.,1.),(1.,1.),(1.,1.),(1.,1.),(1.,1.),(1.,
1.),(1.,1.),(1.,1.),(1.,1.),(1.,1.),(1.,1.),(1.,1.),(1.,1.),(1.,1.),(1.,
1.),(1.,1.),(1.,1.),(1.,1.),(1.,1.),(1.,1.),(1.,1.),(1.,1.),(1.,1.),(1.,
1.),(1.,1.),(1.,1.),(1.,1.),(1.,1.),(1.,1.),(1.,1.),(1.,1.),(1.,1.),(1.,
1.),(1.,1.),(1.,1.),(1.,1.),(1.,1.),(1.,1.),(1.,1.),(1.,1.),(1.,1.),(1.,
1.),(1.,1.),(1.,1.),(1.,1.),(1.,1.),(1.,1.),(1.,1.),(1.,1.),(1.,1.),(1.,
1.),(1.,1.),(1.,1.),(1.,1.),(1.,1.),(1.,1.),(1.,1.),(1.,1.),(1.,1.),(1.,
1.),(1.,1.),(1.,1.),(1.,1.),(1.,1.),(1.,1.),(1.,1.),(1.,1.),(1.,1.),(1.,
1.),(1.,1.),(1.,1.),(1.,1.),(1.,1.),(1.,1.),(1.,1.),(1.,1.),(1.,1.),(1.,
1.),(1.,1.),(1.,1.),(1.,1.),(1.,1.),(1.,1.),(1.,1.),(1.,1.),(1.,1.),(1.,
1.),(1.,1.),(1.,1.),(1.,1.),(1.,1.),(1.,1.),(1.,1.),(1.,1.),(1.,1.),(1.,
1.),(1.,1.),(1.,1.),(1.,1.),(1.,1.),(1.,1.),(1.,1.),(1.,1.),(1.,1.),(1.,
1.),(1.,1.),(1.,1.),(1.,1.),(1.,1.),(1.,1.),(1.,1.),(1.,1.),(1.,1.),(1.,
1.),(1.,1.),(1.,1.),(1.,1.),(1.,1.),(1.,1.),(1.,1.),(1.,1.),(1.,1.),(1.,
1.),(1.,1.),(1.,1.),(1.,1.),(1.,1.),(1.,1.),(1.,1.),(1.,1.),(1.,1.),(1.,
1.),(1.,1.),(1.,1.),(1.,1.),(1.,1.),(1.,1.),(1.,1.),(1.,1.),(1.,1.),(1.,
1.),(1.,1.),(1.,1.),(1.,1.),(1.,1.),(1.,1.),(1.,1.),(1.,1.),(1.,1.),(1.,
1.),(1.,1.)))
REPRESENTATION_ITEM('')
SURFACE()
);
#1113=(
BOUNDED_SURFACE()
B_SPLINE_SURFACE(5,1,((#247396,#247397),(#247398,#247399),(#247400,#247401),
(#247402,#247403),(#247404,#247405),(#247406,#247407),(#247408,#247409),
(#247410,#247411),(#247412,#247413),(#247414,#247415),(#247416,#247417),
(#247418,#247419),(#247420,#247421),(#247422,#247423),(#247424,#247425),
(#247426,#247427),(#247428,#247429),(#247430,#247431),(#247432,#247433),
(#247434,#247435),(#247436,#247437),(#247438,#247439),(#247440,#247441),
(#247442,#247443),(#247444,#247445),(#247446,#247447),(#247448,#247449),
(#247450,#247451),(#247452,#247453),(#247454,#247455),(#247456,#247457),
(#247458,#247459),(#247460,#247461),(#247462,#247463),(#247464,#247465),
(#247466,#247467),(#247468,#247469),(#247470,#247471),(#247472,#247473),
(#247474,#247475),(#247476,#247477),(#247478,#247479),(#247480,#247481),
(#247482,#247483),(#247484,#247485),(#247486,#247487),(#247488,#247489),
(#247490,#247491),(#247492,#247493),(#247494,#247495),(#247496,#247497),
(#247498,#247499),(#247500,#247501),(#247502,#247503),(#247504,#247505),
(#247506,#247507),(#247508,#247509),(#247510,#247511),(#247512,#247513),
(#247514,#247515),(#247516,#247517),(#247518,#247519),(#247520,#247521),
(#247522,#247523),(#247524,#247525),(#247526,#247527),(#247528,#247529),
(#247530,#247531),(#247532,#247533),(#247534,#247535),(#247536,#247537),
(#247538,#247539),(#247540,#247541),(#247542,#247543),(#247544,#247545),
(#247546,#247547),(#247548,#247549),(#247550,#247551),(#247552,#247553),
(#247554,#247555),(#247556,#247557),(#247558,#247559),(#247560,#247561),
(#247562,#247563),(#247564,#247565),(#247566,#247567),(#247568,#247569),
(#247570,#247571),(#247572,#247573),(#247574,#247575),(#247576,#247577),
(#247578,#247579),(#247580,#247581),(#247582,#247583),(#247584,#247585),
(#247586,#247587),(#247588,#247589),(#247590,#247591),(#247592,#247593),
(#247594,#247595),(#247596,#247597),(#247598,#247599),(#247600,#247601),
(#247602,#247603),(#247604,#247605),(#247606,#247607),(#247608,#247609),
(#247610,#247611),(#247612,#247613),(#247614,#247615),(#247616,#247617),
(#247618,#247619),(#247620,#247621),(#247622,#247623),(#247624,#247625),
(#247626,#247627),(#247628,#247629),(#247630,#247631),(#247632,#247633),
(#247634,#247635),(#247636,#247637),(#247638,#247639),(#247640,#247641),
(#247642,#247643),(#247644,#247645),(#247646,#247647),(#247648,#247649),
(#247650,#247651),(#247652,#247653),(#247654,#247655),(#247656,#247657),
(#247658,#247659),(#247660,#247661),(#247662,#247663),(#247664,#247665),
(#247666,#247667),(#247668,#247669),(#247670,#247671),(#247672,#247673),
(#247674,#247675),(#247676,#247677),(#247678,#247679),(#247680,#247681),
(#247682,#247683),(#247684,#247685),(#247686,#247687),(#247688,#247689),
(#247690,#247691),(#247692,#247693),(#247694,#247695),(#247696,#247697),
(#247698,#247699),(#247700,#247701),(#247702,#247703),(#247704,#247705),
(#247706,#247707),(#247708,#247709),(#247710,#247711),(#247712,#247713),
(#247714,#247715),(#247716,#247717),(#247718,#247719),(#247720,#247721),
(#247722,#247723),(#247724,#247725),(#247726,#247727),(#247728,#247729),
(#247730,#247731),(#247732,#247733),(#247734,#247735),(#247736,#247737),
(#247738,#247739),(#247740,#247741),(#247742,#247743),(#247744,#247745),
(#247746,#247747),(#247748,#247749),(#247750,#247751),(#247752,#247753),
(#247754,#247755),(#247756,#247757),(#247758,#247759),(#247760,#247761),
(#247762,#247763),(#247764,#247765),(#247766,#247767),(#247768,#247769),
(#247770,#247771),(#247772,#247773),(#247774,#247775),(#247776,#247777),
(#247778,#247779),(#247780,#247781),(#247782,#247783),(#247784,#247785),
(#247786,#247787),(#247788,#247789),(#247790,#247791),(#247792,#247793),
(#247794,#247795),(#247796,#247797),(#247798,#247799),(#247800,#247801),
(#247802,#247803),(#247804,#247805)),.UNSPECIFIED.,.F.,.F.,.F.)
B_SPLINE_SURFACE_WITH_KNOTS((6,1,1,1,1,1,1,1,1,1,1,1,1,1,1,1,1,1,1,1,1,
1,1,1,1,1,1,1,1,1,1,1,1,1,1,1,1,1,1,1,1,1,1,1,1,1,1,1,1,1,1,1,1,1,1,1,1,
1,1,1,1,1,1,1,1,1,1,1,1,1,1,1,1,1,1,1,1,1,1,1,1,1,1,1,1,1,1,1,1,1,1,1,1,
1,1,1,1,1,1,1,1,1,1,1,1,1,1,1,1,1,1,1,1,1,1,1,1,1,1,1,1,1,1,1,1,1,1,1,1,
1,1,1,1,1,1,1,1,1,1,1,1,1,1,1,1,1,1,1,1,1,1,1,1,1,1,1,1,1,1,1,1,1,1,1,1,
1,1,1,1,1,1,1,1,1,1,1,1,1,1,1,1,1,1,1,1,1,1,1,1,1,1,1,1,1,1,1,1,1,1,1,6),
(2,2),(-1.,-0.995000000000001,-0.990000000000001,-0.985000000000001,-0.980000000000001,
-0.975000000000001,-0.970000000000001,-0.965000000000001,-0.960000000000001,
-0.955000000000001,-0.950000000000001,-0.945000000000001,-0.940000000000001,
-0.935000000000001,-0.930000000000001,-0.925000000000001,-0.920000000000001,
-0.915000000000001,-0.910000000000001,-0.905000000000001,-0.900000000000001,
-0.895000000000001,-0.890000000000001,-0.885000000000001,-0.880000000000001,
-0.875000000000001,-0.870000000000001,-0.865000000000001,-0.860000000000001,
-0.855000000000001,-0.850000000000001,-0.845000000000001,-0.840000000000001,
-0.835000000000001,-0.830000000000001,-0.825000000000001,-0.820000000000001,
-0.815000000000001,-0.810000000000001,-0.805000000000001,-0.800000000000001,
-0.795000000000001,-0.790000000000001,-0.785000000000001,-0.780000000000001,
-0.775000000000001,-0.770000000000001,-0.765000000000001,-0.760000000000001,
-0.755000000000001,-0.750000000000001,-0.745000000000001,-0.740000000000001,
-0.735000000000001,-0.730000000000001,-0.725000000000001,-0.720000000000001,
-0.715000000000001,-0.710000000000001,-0.705000000000001,-0.700000000000001,
-0.695000000000001,-0.690000000000001,-0.685,-0.68,-0.675,-0.67,-0.665,
-0.66,-0.655,-0.65,-0.645,-0.64,-0.635,-0.63,-0.625,-0.62,-0.615,-0.61,
-0.605,-0.6,-0.595,-0.59,-0.585,-0.58,-0.575,-0.57,-0.565,-0.56,-0.555,
-0.55,-0.545,-0.54,-0.535,-0.53,-0.525,-0.52,-0.515,-0.51,-0.505,-0.5,-0.495,
-0.49,-0.485,-0.48,-0.475,-0.47,-0.465,-0.46,-0.455,-0.45,-0.445,-0.44,
-0.435,-0.43,-0.425,-0.42,-0.415,-0.41,-0.405,-0.4,-0.395,-0.39,-0.385,
-0.38,-0.375,-0.37,-0.365,-0.36,-0.355,-0.35,-0.345,-0.34,-0.335,-0.33,
-0.325,-0.32,-0.315,-0.31,-0.305,-0.3,-0.295,-0.29,-0.285,-0.28,-0.275,
-0.27,-0.265,-0.26,-0.255,-0.25,-0.245,-0.24,-0.235,-0.23,-0.225,-0.22,
-0.215,-0.21,-0.205,-0.2,-0.195,-0.19,-0.185,-0.18,-0.175,-0.17,-0.165,
-0.16,-0.155,-0.15,-0.145,-0.14,-0.135,-0.13,-0.125,-0.12,-0.115,-0.11,
-0.105,-0.1,-0.095,-0.09,-0.085,-0.08,-0.075,-0.07,-0.065,-0.06,-0.055,
-0.05,-0.045,-0.04,-0.035,-0.03,-0.025,-0.02,-0.015,-0.01,-0.005,0.),(0.,
1.2),.UNSPECIFIED.)
GEOMETRIC_REPRESENTATION_ITEM()
RATIONAL_B_SPLINE_SURFACE(((1.,1.),(1.,1.),(1.,1.),(1.,1.),(1.,1.),(1.,
1.),(1.,1.),(1.,1.),(1.,1.),(1.,1.),(1.,1.),(1.,1.),(1.,1.),(1.,1.),(1.,
1.),(1.,1.),(1.,1.),(1.,1.),(1.,1.),(1.,1.),(1.,1.),(1.,1.),(1.,1.),(1.,
1.),(1.,1.),(1.,1.),(1.,1.),(1.,1.),(1.,1.),(1.,1.),(1.,1.),(1.,1.),(1.,
1.),(1.,1.),(1.,1.),(1.,1.),(1.,1.),(1.,1.),(1.,1.),(1.,1.),(1.,1.),(1.,
1.),(1.,1.),(1.,1.),(1.,1.),(1.,1.),(1.,1.),(1.,1.),(1.,1.),(1.,1.),(1.,
1.),(1.,1.),(1.,1.),(1.,1.),(1.,1.),(1.,1.),(1.,1.),(1.,1.),(1.,1.),(1.,
1.),(1.,1.),(1.,1.),(1.,1.),(1.,1.),(1.,1.),(1.,1.),(1.,1.),(1.,1.),(1.,
1.),(1.,1.),(1.,1.),(1.,1.),(1.,1.),(1.,1.),(1.,1.),(1.,1.),(1.,1.),(1.,
1.),(1.,1.),(1.,1.),(1.,1.),(1.,1.),(1.,1.),(1.,1.),(1.,1.),(1.,1.),(1.,
1.),(1.,1.),(1.,1.),(1.,1.),(1.,1.),(1.,1.),(1.,1.),(1.,1.),(1.,1.),(1.,
1.),(1.,1.),(1.,1.),(1.,1.),(1.,1.),(1.,1.),(1.,1.),(1.,1.),(1.,1.),(1.,
1.),(1.,1.),(1.,1.),(1.,1.),(1.,1.),(1.,1.),(1.,1.),(1.,1.),(1.,1.),(1.,
1.),(1.,1.),(1.,1.),(1.,1.),(1.,1.),(1.,1.),(1.,1.),(1.,1.),(1.,1.),(1.,
1.),(1.,1.),(1.,1.),(1.,1.),(1.,1.),(1.,1.),(1.,1.),(1.,1.),(1.,1.),(1.,
1.),(1.,1.),(1.,1.),(1.,1.),(1.,1.),(1.,1.),(1.,1.),(1.,1.),(1.,1.),(1.,
1.),(1.,1.),(1.,1.),(1.,1.),(1.,1.),(1.,1.),(1.,1.),(1.,1.),(1.,1.),(1.,
1.),(1.,1.),(1.,1.),(1.,1.),(1.,1.),(1.,1.),(1.,1.),(1.,1.),(1.,1.),(1.,
1.),(1.,1.),(1.,1.),(1.,1.),(1.,1.),(1.,1.),(1.,1.),(1.,1.),(1.,1.),(1.,
1.),(1.,1.),(1.,1.),(1.,1.),(1.,1.),(1.,1.),(1.,1.),(1.,1.),(1.,1.),(1.,
1.),(1.,1.),(1.,1.),(1.,1.),(1.,1.),(1.,1.),(1.,1.),(1.,1.),(1.,1.),(1.,
1.),(1.,1.),(1.,1.),(1.,1.),(1.,1.),(1.,1.),(1.,1.),(1.,1.),(1.,1.),(1.,
1.),(1.,1.),(1.,1.),(1.,1.),(1.,1.),(1.,1.),(1.,1.),(1.,1.),(1.,1.),(1.,
1.),(1.,1.)))
REPRESENTATION_ITEM('')
SURFACE()
);
#1114=(
BOUNDED_SURFACE()
B_SPLINE_SURFACE(5,1,((#248219,#248220),(#248221,#248222),(#248223,#248224),
(#248225,#248226),(#248227,#248228),(#248229,#248230),(#248231,#248232),
(#248233,#248234),(#248235,#248236),(#248237,#248238),(#248239,#248240),
(#248241,#248242),(#248243,#248244),(#248245,#248246),(#248247,#248248),
(#248249,#248250),(#248251,#248252),(#248253,#248254),(#248255,#248256),
(#248257,#248258),(#248259,#248260),(#248261,#248262),(#248263,#248264),
(#248265,#248266),(#248267,#248268),(#248269,#248270),(#248271,#248272),
(#248273,#248274),(#248275,#248276),(#248277,#248278),(#248279,#248280),
(#248281,#248282),(#248283,#248284),(#248285,#248286),(#248287,#248288),
(#248289,#248290),(#248291,#248292),(#248293,#248294),(#248295,#248296),
(#248297,#248298),(#248299,#248300),(#248301,#248302),(#248303,#248304),
(#248305,#248306),(#248307,#248308),(#248309,#248310),(#248311,#248312),
(#248313,#248314),(#248315,#248316),(#248317,#248318),(#248319,#248320),
(#248321,#248322),(#248323,#248324),(#248325,#248326),(#248327,#248328),
(#248329,#248330),(#248331,#248332),(#248333,#248334),(#248335,#248336),
(#248337,#248338),(#248339,#248340),(#248341,#248342),(#248343,#248344),
(#248345,#248346),(#248347,#248348),(#248349,#248350),(#248351,#248352),
(#248353,#248354),(#248355,#248356),(#248357,#248358),(#248359,#248360),
(#248361,#248362),(#248363,#248364),(#248365,#248366),(#248367,#248368),
(#248369,#248370),(#248371,#248372),(#248373,#248374),(#248375,#248376),
(#248377,#248378),(#248379,#248380),(#248381,#248382),(#248383,#248384),
(#248385,#248386),(#248387,#248388),(#248389,#248390),(#248391,#248392),
(#248393,#248394),(#248395,#248396),(#248397,#248398),(#248399,#248400),
(#248401,#248402),(#248403,#248404),(#248405,#248406),(#248407,#248408),
(#248409,#248410),(#248411,#248412),(#248413,#248414),(#248415,#248416),
(#248417,#248418),(#248419,#248420),(#248421,#248422),(#248423,#248424),
(#248425,#248426),(#248427,#248428),(#248429,#248430),(#248431,#248432),
(#248433,#248434),(#248435,#248436),(#248437,#248438),(#248439,#248440),
(#248441,#248442),(#248443,#248444),(#248445,#248446),(#248447,#248448),
(#248449,#248450),(#248451,#248452),(#248453,#248454),(#248455,#248456),
(#248457,#248458),(#248459,#248460),(#248461,#248462),(#248463,#248464),
(#248465,#248466),(#248467,#248468),(#248469,#248470),(#248471,#248472),
(#248473,#248474),(#248475,#248476),(#248477,#248478),(#248479,#248480),
(#248481,#248482),(#248483,#248484),(#248485,#248486),(#248487,#248488),
(#248489,#248490),(#248491,#248492),(#248493,#248494),(#248495,#248496),
(#248497,#248498),(#248499,#248500),(#248501,#248502),(#248503,#248504),
(#248505,#248506),(#248507,#248508),(#248509,#248510),(#248511,#248512),
(#248513,#248514),(#248515,#248516),(#248517,#248518),(#248519,#248520),
(#248521,#248522),(#248523,#248524),(#248525,#248526),(#248527,#248528),
(#248529,#248530),(#248531,#248532),(#248533,#248534),(#248535,#248536),
(#248537,#248538),(#248539,#248540),(#248541,#248542),(#248543,#248544),
(#248545,#248546),(#248547,#248548),(#248549,#248550),(#248551,#248552),
(#248553,#248554),(#248555,#248556),(#248557,#248558),(#248559,#248560),
(#248561,#248562),(#248563,#248564),(#248565,#248566),(#248567,#248568),
(#248569,#248570),(#248571,#248572),(#248573,#248574),(#248575,#248576),
(#248577,#248578),(#248579,#248580),(#248581,#248582),(#248583,#248584),
(#248585,#248586),(#248587,#248588),(#248589,#248590),(#248591,#248592),
(#248593,#248594),(#248595,#248596),(#248597,#248598),(#248599,#248600),
(#248601,#248602),(#248603,#248604),(#248605,#248606),(#248607,#248608),
(#248609,#248610),(#248611,#248612),(#248613,#248614),(#248615,#248616),
(#248617,#248618),(#248619,#248620),(#248621,#248622),(#248623,#248624),
(#248625,#248626),(#248627,#248628)),.UNSPECIFIED.,.F.,.F.,.F.)
B_SPLINE_SURFACE_WITH_KNOTS((6,1,1,1,1,1,1,1,1,1,1,1,1,1,1,1,1,1,1,1,1,
1,1,1,1,1,1,1,1,1,1,1,1,1,1,1,1,1,1,1,1,1,1,1,1,1,1,1,1,1,1,1,1,1,1,1,1,
1,1,1,1,1,1,1,1,1,1,1,1,1,1,1,1,1,1,1,1,1,1,1,1,1,1,1,1,1,1,1,1,1,1,1,1,
1,1,1,1,1,1,1,1,1,1,1,1,1,1,1,1,1,1,1,1,1,1,1,1,1,1,1,1,1,1,1,1,1,1,1,1,
1,1,1,1,1,1,1,1,1,1,1,1,1,1,1,1,1,1,1,1,1,1,1,1,1,1,1,1,1,1,1,1,1,1,1,1,
1,1,1,1,1,1,1,1,1,1,1,1,1,1,1,1,1,1,1,1,1,1,1,1,1,1,1,1,1,1,1,1,1,1,1,6),
(2,2),(0.,0.005,0.01,0.015,0.02,0.025,0.03,0.035,0.04,0.045,0.05,0.055,
0.06,0.065,0.07,0.075,0.08,0.085,0.09,0.095,0.1,0.105,0.11,0.115,0.12,0.125,
0.13,0.135,0.14,0.145,0.15,0.155,0.16,0.165,0.17,0.175,0.18,0.185,0.19,
0.195,0.2,0.205,0.21,0.215,0.22,0.225,0.23,0.235,0.24,0.245,0.25,0.255,
0.26,0.265,0.27,0.275,0.28,0.285,0.29,0.295,0.3,0.305,0.31,0.315,0.32,0.325,
0.33,0.335,0.34,0.345,0.35,0.355,0.36,0.365,0.37,0.375,0.38,0.385,0.39,
0.395,0.4,0.405,0.41,0.415,0.42,0.425,0.43,0.435,0.44,0.445,0.45,0.455,
0.46,0.465,0.47,0.475,0.48,0.485,0.49,0.495,0.5,0.505,0.51,0.515,0.52,0.525,
0.53,0.535,0.54,0.545,0.55,0.555,0.56,0.565,0.57,0.575,0.58,0.585,0.59,
0.595,0.6,0.605,0.61,0.615,0.62,0.625,0.63,0.635,0.64,0.645,0.65,0.655,
0.66,0.665,0.67,0.675,0.68,0.685,0.690000000000001,0.695000000000001,0.700000000000001,
0.705000000000001,0.710000000000001,0.715000000000001,0.720000000000001,
0.725000000000001,0.730000000000001,0.735000000000001,0.740000000000001,
0.745000000000001,0.750000000000001,0.755000000000001,0.760000000000001,
0.765000000000001,0.770000000000001,0.775000000000001,0.780000000000001,
0.785000000000001,0.790000000000001,0.795000000000001,0.800000000000001,
0.805000000000001,0.810000000000001,0.815000000000001,0.820000000000001,
0.825000000000001,0.830000000000001,0.835000000000001,0.840000000000001,
0.845000000000001,0.850000000000001,0.855000000000001,0.860000000000001,
0.865000000000001,0.870000000000001,0.875000000000001,0.880000000000001,
0.885000000000001,0.890000000000001,0.895000000000001,0.900000000000001,
0.905000000000001,0.910000000000001,0.915000000000001,0.920000000000001,
0.925000000000001,0.930000000000001,0.935000000000001,0.940000000000001,
0.945000000000001,0.950000000000001,0.955000000000001,0.960000000000001,
0.965000000000001,0.970000000000001,0.975000000000001,0.980000000000001,
0.985000000000001,0.990000000000001,0.995000000000001,1.),(0.,1.2),
 .UNSPECIFIED.)
GEOMETRIC_REPRESENTATION_ITEM()
RATIONAL_B_SPLINE_SURFACE(((1.,1.),(1.,1.),(1.,1.),(1.,1.),(1.,1.),(1.,
1.),(1.,1.),(1.,1.),(1.,1.),(1.,1.),(1.,1.),(1.,1.),(1.,1.),(1.,1.),(1.,
1.),(1.,1.),(1.,1.),(1.,1.),(1.,1.),(1.,1.),(1.,1.),(1.,1.),(1.,1.),(1.,
1.),(1.,1.),(1.,1.),(1.,1.),(1.,1.),(1.,1.),(1.,1.),(1.,1.),(1.,1.),(1.,
1.),(1.,1.),(1.,1.),(1.,1.),(1.,1.),(1.,1.),(1.,1.),(1.,1.),(1.,1.),(1.,
1.),(1.,1.),(1.,1.),(1.,1.),(1.,1.),(1.,1.),(1.,1.),(1.,1.),(1.,1.),(1.,
1.),(1.,1.),(1.,1.),(1.,1.),(1.,1.),(1.,1.),(1.,1.),(1.,1.),(1.,1.),(1.,
1.),(1.,1.),(1.,1.),(1.,1.),(1.,1.),(1.,1.),(1.,1.),(1.,1.),(1.,1.),(1.,
1.),(1.,1.),(1.,1.),(1.,1.),(1.,1.),(1.,1.),(1.,1.),(1.,1.),(1.,1.),(1.,
1.),(1.,1.),(1.,1.),(1.,1.),(1.,1.),(1.,1.),(1.,1.),(1.,1.),(1.,1.),(1.,
1.),(1.,1.),(1.,1.),(1.,1.),(1.,1.),(1.,1.),(1.,1.),(1.,1.),(1.,1.),(1.,
1.),(1.,1.),(1.,1.),(1.,1.),(1.,1.),(1.,1.),(1.,1.),(1.,1.),(1.,1.),(1.,
1.),(1.,1.),(1.,1.),(1.,1.),(1.,1.),(1.,1.),(1.,1.),(1.,1.),(1.,1.),(1.,
1.),(1.,1.),(1.,1.),(1.,1.),(1.,1.),(1.,1.),(1.,1.),(1.,1.),(1.,1.),(1.,
1.),(1.,1.),(1.,1.),(1.,1.),(1.,1.),(1.,1.),(1.,1.),(1.,1.),(1.,1.),(1.,
1.),(1.,1.),(1.,1.),(1.,1.),(1.,1.),(1.,1.),(1.,1.),(1.,1.),(1.,1.),(1.,
1.),(1.,1.),(1.,1.),(1.,1.),(1.,1.),(1.,1.),(1.,1.),(1.,1.),(1.,1.),(1.,
1.),(1.,1.),(1.,1.),(1.,1.),(1.,1.),(1.,1.),(1.,1.),(1.,1.),(1.,1.),(1.,
1.),(1.,1.),(1.,1.),(1.,1.),(1.,1.),(1.,1.),(1.,1.),(1.,1.),(1.,1.),(1.,
1.),(1.,1.),(1.,1.),(1.,1.),(1.,1.),(1.,1.),(1.,1.),(1.,1.),(1.,1.),(1.,
1.),(1.,1.),(1.,1.),(1.,1.),(1.,1.),(1.,1.),(1.,1.),(1.,1.),(1.,1.),(1.,
1.),(1.,1.),(1.,1.),(1.,1.),(1.,1.),(1.,1.),(1.,1.),(1.,1.),(1.,1.),(1.,
1.),(1.,1.),(1.,1.),(1.,1.),(1.,1.),(1.,1.),(1.,1.),(1.,1.),(1.,1.),(1.,
1.),(1.,1.)))
REPRESENTATION_ITEM('')
SURFACE()
);
#1115=(
BOUNDED_SURFACE()
B_SPLINE_SURFACE(5,1,((#249048,#249049),(#249050,#249051),(#249052,#249053),
(#249054,#249055),(#249056,#249057),(#249058,#249059),(#249060,#249061),
(#249062,#249063),(#249064,#249065),(#249066,#249067),(#249068,#249069),
(#249070,#249071),(#249072,#249073),(#249074,#249075),(#249076,#249077),
(#249078,#249079),(#249080,#249081),(#249082,#249083),(#249084,#249085),
(#249086,#249087),(#249088,#249089),(#249090,#249091),(#249092,#249093),
(#249094,#249095),(#249096,#249097),(#249098,#249099),(#249100,#249101),
(#249102,#249103),(#249104,#249105),(#249106,#249107),(#249108,#249109),
(#249110,#249111),(#249112,#249113),(#249114,#249115),(#249116,#249117),
(#249118,#249119),(#249120,#249121),(#249122,#249123),(#249124,#249125),
(#249126,#249127),(#249128,#249129),(#249130,#249131),(#249132,#249133),
(#249134,#249135),(#249136,#249137),(#249138,#249139),(#249140,#249141),
(#249142,#249143),(#249144,#249145),(#249146,#249147),(#249148,#249149),
(#249150,#249151),(#249152,#249153),(#249154,#249155),(#249156,#249157),
(#249158,#249159),(#249160,#249161),(#249162,#249163),(#249164,#249165),
(#249166,#249167),(#249168,#249169),(#249170,#249171),(#249172,#249173),
(#249174,#249175),(#249176,#249177),(#249178,#249179),(#249180,#249181),
(#249182,#249183),(#249184,#249185),(#249186,#249187),(#249188,#249189),
(#249190,#249191),(#249192,#249193),(#249194,#249195),(#249196,#249197),
(#249198,#249199),(#249200,#249201),(#249202,#249203),(#249204,#249205),
(#249206,#249207),(#249208,#249209),(#249210,#249211),(#249212,#249213),
(#249214,#249215),(#249216,#249217),(#249218,#249219),(#249220,#249221),
(#249222,#249223),(#249224,#249225),(#249226,#249227),(#249228,#249229),
(#249230,#249231),(#249232,#249233),(#249234,#249235),(#249236,#249237),
(#249238,#249239),(#249240,#249241),(#249242,#249243),(#249244,#249245),
(#249246,#249247),(#249248,#249249),(#249250,#249251),(#249252,#249253),
(#249254,#249255),(#249256,#249257),(#249258,#249259),(#249260,#249261),
(#249262,#249263),(#249264,#249265),(#249266,#249267),(#249268,#249269),
(#249270,#249271),(#249272,#249273),(#249274,#249275),(#249276,#249277),
(#249278,#249279),(#249280,#249281),(#249282,#249283),(#249284,#249285),
(#249286,#249287),(#249288,#249289),(#249290,#249291),(#249292,#249293),
(#249294,#249295),(#249296,#249297),(#249298,#249299),(#249300,#249301),
(#249302,#249303),(#249304,#249305),(#249306,#249307),(#249308,#249309),
(#249310,#249311),(#249312,#249313),(#249314,#249315),(#249316,#249317),
(#249318,#249319),(#249320,#249321),(#249322,#249323),(#249324,#249325),
(#249326,#249327),(#249328,#249329),(#249330,#249331),(#249332,#249333),
(#249334,#249335),(#249336,#249337),(#249338,#249339),(#249340,#249341),
(#249342,#249343),(#249344,#249345),(#249346,#249347),(#249348,#249349),
(#249350,#249351),(#249352,#249353),(#249354,#249355),(#249356,#249357),
(#249358,#249359),(#249360,#249361),(#249362,#249363),(#249364,#249365),
(#249366,#249367),(#249368,#249369),(#249370,#249371),(#249372,#249373),
(#249374,#249375),(#249376,#249377),(#249378,#249379),(#249380,#249381),
(#249382,#249383),(#249384,#249385),(#249386,#249387),(#249388,#249389),
(#249390,#249391),(#249392,#249393),(#249394,#249395),(#249396,#249397),
(#249398,#249399),(#249400,#249401),(#249402,#249403),(#249404,#249405),
(#249406,#249407),(#249408,#249409),(#249410,#249411),(#249412,#249413),
(#249414,#249415),(#249416,#249417),(#249418,#249419),(#249420,#249421),
(#249422,#249423),(#249424,#249425),(#249426,#249427),(#249428,#249429),
(#249430,#249431),(#249432,#249433),(#249434,#249435),(#249436,#249437),
(#249438,#249439),(#249440,#249441),(#249442,#249443),(#249444,#249445),
(#249446,#249447),(#249448,#249449),(#249450,#249451),(#249452,#249453),
(#249454,#249455),(#249456,#249457)),.UNSPECIFIED.,.F.,.F.,.F.)
B_SPLINE_SURFACE_WITH_KNOTS((6,1,1,1,1,1,1,1,1,1,1,1,1,1,1,1,1,1,1,1,1,
1,1,1,1,1,1,1,1,1,1,1,1,1,1,1,1,1,1,1,1,1,1,1,1,1,1,1,1,1,1,1,1,1,1,1,1,
1,1,1,1,1,1,1,1,1,1,1,1,1,1,1,1,1,1,1,1,1,1,1,1,1,1,1,1,1,1,1,1,1,1,1,1,
1,1,1,1,1,1,1,1,1,1,1,1,1,1,1,1,1,1,1,1,1,1,1,1,1,1,1,1,1,1,1,1,1,1,1,1,
1,1,1,1,1,1,1,1,1,1,1,1,1,1,1,1,1,1,1,1,1,1,1,1,1,1,1,1,1,1,1,1,1,1,1,1,
1,1,1,1,1,1,1,1,1,1,1,1,1,1,1,1,1,1,1,1,1,1,1,1,1,1,1,1,1,1,1,1,1,1,1,6),
(2,2),(-1.,-0.995000000000001,-0.990000000000001,-0.985000000000001,-0.980000000000001,
-0.975000000000001,-0.970000000000001,-0.965000000000001,-0.960000000000001,
-0.955000000000001,-0.950000000000001,-0.945000000000001,-0.940000000000001,
-0.935000000000001,-0.930000000000001,-0.925000000000001,-0.920000000000001,
-0.915000000000001,-0.910000000000001,-0.905000000000001,-0.900000000000001,
-0.895000000000001,-0.890000000000001,-0.885000000000001,-0.880000000000001,
-0.875000000000001,-0.870000000000001,-0.865000000000001,-0.860000000000001,
-0.855000000000001,-0.850000000000001,-0.845000000000001,-0.840000000000001,
-0.835000000000001,-0.830000000000001,-0.825000000000001,-0.820000000000001,
-0.815000000000001,-0.810000000000001,-0.805000000000001,-0.800000000000001,
-0.795000000000001,-0.790000000000001,-0.785000000000001,-0.780000000000001,
-0.775000000000001,-0.770000000000001,-0.765000000000001,-0.760000000000001,
-0.755000000000001,-0.750000000000001,-0.745000000000001,-0.740000000000001,
-0.735000000000001,-0.730000000000001,-0.725000000000001,-0.720000000000001,
-0.715000000000001,-0.710000000000001,-0.705000000000001,-0.700000000000001,
-0.695000000000001,-0.690000000000001,-0.685,-0.68,-0.675,-0.67,-0.665,
-0.66,-0.655,-0.65,-0.645,-0.64,-0.635,-0.63,-0.625,-0.62,-0.615,-0.61,
-0.605,-0.6,-0.595,-0.59,-0.585,-0.58,-0.575,-0.57,-0.565,-0.56,-0.555,
-0.55,-0.545,-0.54,-0.535,-0.53,-0.525,-0.52,-0.515,-0.51,-0.505,-0.5,-0.495,
-0.49,-0.485,-0.48,-0.475,-0.47,-0.465,-0.46,-0.455,-0.45,-0.445,-0.44,
-0.435,-0.43,-0.425,-0.42,-0.415,-0.41,-0.405,-0.4,-0.395,-0.39,-0.385,
-0.38,-0.375,-0.37,-0.365,-0.36,-0.355,-0.35,-0.345,-0.34,-0.335,-0.33,
-0.325,-0.32,-0.315,-0.31,-0.305,-0.3,-0.295,-0.29,-0.285,-0.28,-0.275,
-0.27,-0.265,-0.26,-0.255,-0.25,-0.245,-0.24,-0.235,-0.23,-0.225,-0.22,
-0.215,-0.21,-0.205,-0.2,-0.195,-0.19,-0.185,-0.18,-0.175,-0.17,-0.165,
-0.16,-0.155,-0.15,-0.145,-0.14,-0.135,-0.13,-0.125,-0.12,-0.115,-0.11,
-0.105,-0.1,-0.095,-0.09,-0.085,-0.08,-0.075,-0.07,-0.065,-0.06,-0.055,
-0.05,-0.045,-0.04,-0.035,-0.03,-0.025,-0.02,-0.015,-0.01,-0.005,0.),(0.,
1.2),.UNSPECIFIED.)
GEOMETRIC_REPRESENTATION_ITEM()
RATIONAL_B_SPLINE_SURFACE(((1.,1.),(1.,1.),(1.,1.),(1.,1.),(1.,1.),(1.,
1.),(1.,1.),(1.,1.),(1.,1.),(1.,1.),(1.,1.),(1.,1.),(1.,1.),(1.,1.),(1.,
1.),(1.,1.),(1.,1.),(1.,1.),(1.,1.),(1.,1.),(1.,1.),(1.,1.),(1.,1.),(1.,
1.),(1.,1.),(1.,1.),(1.,1.),(1.,1.),(1.,1.),(1.,1.),(1.,1.),(1.,1.),(1.,
1.),(1.,1.),(1.,1.),(1.,1.),(1.,1.),(1.,1.),(1.,1.),(1.,1.),(1.,1.),(1.,
1.),(1.,1.),(1.,1.),(1.,1.),(1.,1.),(1.,1.),(1.,1.),(1.,1.),(1.,1.),(1.,
1.),(1.,1.),(1.,1.),(1.,1.),(1.,1.),(1.,1.),(1.,1.),(1.,1.),(1.,1.),(1.,
1.),(1.,1.),(1.,1.),(1.,1.),(1.,1.),(1.,1.),(1.,1.),(1.,1.),(1.,1.),(1.,
1.),(1.,1.),(1.,1.),(1.,1.),(1.,1.),(1.,1.),(1.,1.),(1.,1.),(1.,1.),(1.,
1.),(1.,1.),(1.,1.),(1.,1.),(1.,1.),(1.,1.),(1.,1.),(1.,1.),(1.,1.),(1.,
1.),(1.,1.),(1.,1.),(1.,1.),(1.,1.),(1.,1.),(1.,1.),(1.,1.),(1.,1.),(1.,
1.),(1.,1.),(1.,1.),(1.,1.),(1.,1.),(1.,1.),(1.,1.),(1.,1.),(1.,1.),(1.,
1.),(1.,1.),(1.,1.),(1.,1.),(1.,1.),(1.,1.),(1.,1.),(1.,1.),(1.,1.),(1.,
1.),(1.,1.),(1.,1.),(1.,1.),(1.,1.),(1.,1.),(1.,1.),(1.,1.),(1.,1.),(1.,
1.),(1.,1.),(1.,1.),(1.,1.),(1.,1.),(1.,1.),(1.,1.),(1.,1.),(1.,1.),(1.,
1.),(1.,1.),(1.,1.),(1.,1.),(1.,1.),(1.,1.),(1.,1.),(1.,1.),(1.,1.),(1.,
1.),(1.,1.),(1.,1.),(1.,1.),(1.,1.),(1.,1.),(1.,1.),(1.,1.),(1.,1.),(1.,
1.),(1.,1.),(1.,1.),(1.,1.),(1.,1.),(1.,1.),(1.,1.),(1.,1.),(1.,1.),(1.,
1.),(1.,1.),(1.,1.),(1.,1.),(1.,1.),(1.,1.),(1.,1.),(1.,1.),(1.,1.),(1.,
1.),(1.,1.),(1.,1.),(1.,1.),(1.,1.),(1.,1.),(1.,1.),(1.,1.),(1.,1.),(1.,
1.),(1.,1.),(1.,1.),(1.,1.),(1.,1.),(1.,1.),(1.,1.),(1.,1.),(1.,1.),(1.,
1.),(1.,1.),(1.,1.),(1.,1.),(1.,1.),(1.,1.),(1.,1.),(1.,1.),(1.,1.),(1.,
1.),(1.,1.),(1.,1.),(1.,1.),(1.,1.),(1.,1.),(1.,1.),(1.,1.),(1.,1.),(1.,
1.),(1.,1.)))
REPRESENTATION_ITEM('')
SURFACE()
);
#1116=(
BOUNDED_SURFACE()
B_SPLINE_SURFACE(5,1,((#249871,#249872),(#249873,#249874),(#249875,#249876),
(#249877,#249878),(#249879,#249880),(#249881,#249882),(#249883,#249884),
(#249885,#249886),(#249887,#249888),(#249889,#249890),(#249891,#249892),
(#249893,#249894),(#249895,#249896),(#249897,#249898),(#249899,#249900),
(#249901,#249902),(#249903,#249904),(#249905,#249906),(#249907,#249908),
(#249909,#249910),(#249911,#249912),(#249913,#249914),(#249915,#249916),
(#249917,#249918),(#249919,#249920),(#249921,#249922),(#249923,#249924),
(#249925,#249926),(#249927,#249928),(#249929,#249930),(#249931,#249932),
(#249933,#249934),(#249935,#249936),(#249937,#249938),(#249939,#249940),
(#249941,#249942),(#249943,#249944),(#249945,#249946),(#249947,#249948),
(#249949,#249950),(#249951,#249952),(#249953,#249954),(#249955,#249956),
(#249957,#249958),(#249959,#249960),(#249961,#249962),(#249963,#249964),
(#249965,#249966),(#249967,#249968),(#249969,#249970),(#249971,#249972),
(#249973,#249974),(#249975,#249976),(#249977,#249978),(#249979,#249980),
(#249981,#249982),(#249983,#249984),(#249985,#249986),(#249987,#249988),
(#249989,#249990),(#249991,#249992),(#249993,#249994),(#249995,#249996),
(#249997,#249998),(#249999,#250000),(#250001,#250002),(#250003,#250004),
(#250005,#250006),(#250007,#250008),(#250009,#250010),(#250011,#250012),
(#250013,#250014),(#250015,#250016),(#250017,#250018),(#250019,#250020),
(#250021,#250022),(#250023,#250024),(#250025,#250026),(#250027,#250028),
(#250029,#250030),(#250031,#250032),(#250033,#250034),(#250035,#250036),
(#250037,#250038),(#250039,#250040),(#250041,#250042),(#250043,#250044),
(#250045,#250046),(#250047,#250048),(#250049,#250050),(#250051,#250052),
(#250053,#250054),(#250055,#250056),(#250057,#250058),(#250059,#250060),
(#250061,#250062),(#250063,#250064),(#250065,#250066),(#250067,#250068),
(#250069,#250070),(#250071,#250072),(#250073,#250074),(#250075,#250076),
(#250077,#250078),(#250079,#250080),(#250081,#250082),(#250083,#250084),
(#250085,#250086),(#250087,#250088),(#250089,#250090),(#250091,#250092),
(#250093,#250094),(#250095,#250096),(#250097,#250098),(#250099,#250100),
(#250101,#250102),(#250103,#250104),(#250105,#250106),(#250107,#250108),
(#250109,#250110),(#250111,#250112),(#250113,#250114),(#250115,#250116),
(#250117,#250118),(#250119,#250120),(#250121,#250122),(#250123,#250124),
(#250125,#250126),(#250127,#250128),(#250129,#250130),(#250131,#250132),
(#250133,#250134),(#250135,#250136),(#250137,#250138),(#250139,#250140),
(#250141,#250142),(#250143,#250144),(#250145,#250146),(#250147,#250148),
(#250149,#250150),(#250151,#250152),(#250153,#250154),(#250155,#250156),
(#250157,#250158),(#250159,#250160),(#250161,#250162),(#250163,#250164),
(#250165,#250166),(#250167,#250168),(#250169,#250170),(#250171,#250172),
(#250173,#250174),(#250175,#250176),(#250177,#250178),(#250179,#250180),
(#250181,#250182),(#250183,#250184),(#250185,#250186),(#250187,#250188),
(#250189,#250190),(#250191,#250192),(#250193,#250194),(#250195,#250196),
(#250197,#250198),(#250199,#250200),(#250201,#250202),(#250203,#250204),
(#250205,#250206),(#250207,#250208),(#250209,#250210),(#250211,#250212),
(#250213,#250214),(#250215,#250216),(#250217,#250218),(#250219,#250220),
(#250221,#250222),(#250223,#250224),(#250225,#250226),(#250227,#250228),
(#250229,#250230),(#250231,#250232),(#250233,#250234),(#250235,#250236),
(#250237,#250238),(#250239,#250240),(#250241,#250242),(#250243,#250244),
(#250245,#250246),(#250247,#250248),(#250249,#250250),(#250251,#250252),
(#250253,#250254),(#250255,#250256),(#250257,#250258),(#250259,#250260),
(#250261,#250262),(#250263,#250264),(#250265,#250266),(#250267,#250268),
(#250269,#250270),(#250271,#250272),(#250273,#250274),(#250275,#250276),
(#250277,#250278),(#250279,#250280)),.UNSPECIFIED.,.F.,.F.,.F.)
B_SPLINE_SURFACE_WITH_KNOTS((6,1,1,1,1,1,1,1,1,1,1,1,1,1,1,1,1,1,1,1,1,
1,1,1,1,1,1,1,1,1,1,1,1,1,1,1,1,1,1,1,1,1,1,1,1,1,1,1,1,1,1,1,1,1,1,1,1,
1,1,1,1,1,1,1,1,1,1,1,1,1,1,1,1,1,1,1,1,1,1,1,1,1,1,1,1,1,1,1,1,1,1,1,1,
1,1,1,1,1,1,1,1,1,1,1,1,1,1,1,1,1,1,1,1,1,1,1,1,1,1,1,1,1,1,1,1,1,1,1,1,
1,1,1,1,1,1,1,1,1,1,1,1,1,1,1,1,1,1,1,1,1,1,1,1,1,1,1,1,1,1,1,1,1,1,1,1,
1,1,1,1,1,1,1,1,1,1,1,1,1,1,1,1,1,1,1,1,1,1,1,1,1,1,1,1,1,1,1,1,1,1,1,6),
(2,2),(0.,0.005,0.01,0.015,0.02,0.025,0.03,0.035,0.04,0.045,0.05,0.055,
0.06,0.065,0.07,0.075,0.08,0.085,0.09,0.095,0.1,0.105,0.11,0.115,0.12,0.125,
0.13,0.135,0.14,0.145,0.15,0.155,0.16,0.165,0.17,0.175,0.18,0.185,0.19,
0.195,0.2,0.205,0.21,0.215,0.22,0.225,0.23,0.235,0.24,0.245,0.25,0.255,
0.26,0.265,0.27,0.275,0.28,0.285,0.29,0.295,0.3,0.305,0.31,0.315,0.32,0.325,
0.33,0.335,0.34,0.345,0.35,0.355,0.36,0.365,0.37,0.375,0.38,0.385,0.39,
0.395,0.4,0.405,0.41,0.415,0.42,0.425,0.43,0.435,0.44,0.445,0.45,0.455,
0.46,0.465,0.47,0.475,0.48,0.485,0.49,0.495,0.5,0.505,0.51,0.515,0.52,0.525,
0.53,0.535,0.54,0.545,0.55,0.555,0.56,0.565,0.57,0.575,0.58,0.585,0.59,
0.595,0.6,0.605,0.61,0.615,0.62,0.625,0.63,0.635,0.64,0.645,0.65,0.655,
0.66,0.665,0.67,0.675,0.68,0.685,0.690000000000001,0.695000000000001,0.700000000000001,
0.705000000000001,0.710000000000001,0.715000000000001,0.720000000000001,
0.725000000000001,0.730000000000001,0.735000000000001,0.740000000000001,
0.745000000000001,0.750000000000001,0.755000000000001,0.760000000000001,
0.765000000000001,0.770000000000001,0.775000000000001,0.780000000000001,
0.785000000000001,0.790000000000001,0.795000000000001,0.800000000000001,
0.805000000000001,0.810000000000001,0.815000000000001,0.820000000000001,
0.825000000000001,0.830000000000001,0.835000000000001,0.840000000000001,
0.845000000000001,0.850000000000001,0.855000000000001,0.860000000000001,
0.865000000000001,0.870000000000001,0.875000000000001,0.880000000000001,
0.885000000000001,0.890000000000001,0.895000000000001,0.900000000000001,
0.905000000000001,0.910000000000001,0.915000000000001,0.920000000000001,
0.925000000000001,0.930000000000001,0.935000000000001,0.940000000000001,
0.945000000000001,0.950000000000001,0.955000000000001,0.960000000000001,
0.965000000000001,0.970000000000001,0.975000000000001,0.980000000000001,
0.985000000000001,0.990000000000001,0.995000000000001,1.),(0.,1.2),
 .UNSPECIFIED.)
GEOMETRIC_REPRESENTATION_ITEM()
RATIONAL_B_SPLINE_SURFACE(((1.,1.),(1.,1.),(1.,1.),(1.,1.),(1.,1.),(1.,
1.),(1.,1.),(1.,1.),(1.,1.),(1.,1.),(1.,1.),(1.,1.),(1.,1.),(1.,1.),(1.,
1.),(1.,1.),(1.,1.),(1.,1.),(1.,1.),(1.,1.),(1.,1.),(1.,1.),(1.,1.),(1.,
1.),(1.,1.),(1.,1.),(1.,1.),(1.,1.),(1.,1.),(1.,1.),(1.,1.),(1.,1.),(1.,
1.),(1.,1.),(1.,1.),(1.,1.),(1.,1.),(1.,1.),(1.,1.),(1.,1.),(1.,1.),(1.,
1.),(1.,1.),(1.,1.),(1.,1.),(1.,1.),(1.,1.),(1.,1.),(1.,1.),(1.,1.),(1.,
1.),(1.,1.),(1.,1.),(1.,1.),(1.,1.),(1.,1.),(1.,1.),(1.,1.),(1.,1.),(1.,
1.),(1.,1.),(1.,1.),(1.,1.),(1.,1.),(1.,1.),(1.,1.),(1.,1.),(1.,1.),(1.,
1.),(1.,1.),(1.,1.),(1.,1.),(1.,1.),(1.,1.),(1.,1.),(1.,1.),(1.,1.),(1.,
1.),(1.,1.),(1.,1.),(1.,1.),(1.,1.),(1.,1.),(1.,1.),(1.,1.),(1.,1.),(1.,
1.),(1.,1.),(1.,1.),(1.,1.),(1.,1.),(1.,1.),(1.,1.),(1.,1.),(1.,1.),(1.,
1.),(1.,1.),(1.,1.),(1.,1.),(1.,1.),(1.,1.),(1.,1.),(1.,1.),(1.,1.),(1.,
1.),(1.,1.),(1.,1.),(1.,1.),(1.,1.),(1.,1.),(1.,1.),(1.,1.),(1.,1.),(1.,
1.),(1.,1.),(1.,1.),(1.,1.),(1.,1.),(1.,1.),(1.,1.),(1.,1.),(1.,1.),(1.,
1.),(1.,1.),(1.,1.),(1.,1.),(1.,1.),(1.,1.),(1.,1.),(1.,1.),(1.,1.),(1.,
1.),(1.,1.),(1.,1.),(1.,1.),(1.,1.),(1.,1.),(1.,1.),(1.,1.),(1.,1.),(1.,
1.),(1.,1.),(1.,1.),(1.,1.),(1.,1.),(1.,1.),(1.,1.),(1.,1.),(1.,1.),(1.,
1.),(1.,1.),(1.,1.),(1.,1.),(1.,1.),(1.,1.),(1.,1.),(1.,1.),(1.,1.),(1.,
1.),(1.,1.),(1.,1.),(1.,1.),(1.,1.),(1.,1.),(1.,1.),(1.,1.),(1.,1.),(1.,
1.),(1.,1.),(1.,1.),(1.,1.),(1.,1.),(1.,1.),(1.,1.),(1.,1.),(1.,1.),(1.,
1.),(1.,1.),(1.,1.),(1.,1.),(1.,1.),(1.,1.),(1.,1.),(1.,1.),(1.,1.),(1.,
1.),(1.,1.),(1.,1.),(1.,1.),(1.,1.),(1.,1.),(1.,1.),(1.,1.),(1.,1.),(1.,
1.),(1.,1.),(1.,1.),(1.,1.),(1.,1.),(1.,1.),(1.,1.),(1.,1.),(1.,1.),(1.,
1.),(1.,1.)))
REPRESENTATION_ITEM('')
SURFACE()
);
#1117=(
BOUNDED_SURFACE()
B_SPLINE_SURFACE(5,1,((#250700,#250701),(#250702,#250703),(#250704,#250705),
(#250706,#250707),(#250708,#250709),(#250710,#250711),(#250712,#250713),
(#250714,#250715),(#250716,#250717),(#250718,#250719),(#250720,#250721),
(#250722,#250723),(#250724,#250725),(#250726,#250727),(#250728,#250729),
(#250730,#250731),(#250732,#250733),(#250734,#250735),(#250736,#250737),
(#250738,#250739),(#250740,#250741),(#250742,#250743),(#250744,#250745),
(#250746,#250747),(#250748,#250749),(#250750,#250751),(#250752,#250753),
(#250754,#250755),(#250756,#250757),(#250758,#250759),(#250760,#250761),
(#250762,#250763),(#250764,#250765),(#250766,#250767),(#250768,#250769),
(#250770,#250771),(#250772,#250773),(#250774,#250775),(#250776,#250777),
(#250778,#250779),(#250780,#250781),(#250782,#250783),(#250784,#250785),
(#250786,#250787),(#250788,#250789),(#250790,#250791),(#250792,#250793),
(#250794,#250795),(#250796,#250797),(#250798,#250799),(#250800,#250801),
(#250802,#250803),(#250804,#250805),(#250806,#250807),(#250808,#250809),
(#250810,#250811),(#250812,#250813),(#250814,#250815),(#250816,#250817),
(#250818,#250819),(#250820,#250821),(#250822,#250823),(#250824,#250825),
(#250826,#250827),(#250828,#250829),(#250830,#250831),(#250832,#250833),
(#250834,#250835),(#250836,#250837),(#250838,#250839),(#250840,#250841),
(#250842,#250843),(#250844,#250845),(#250846,#250847),(#250848,#250849),
(#250850,#250851),(#250852,#250853),(#250854,#250855),(#250856,#250857),
(#250858,#250859),(#250860,#250861),(#250862,#250863),(#250864,#250865),
(#250866,#250867),(#250868,#250869),(#250870,#250871),(#250872,#250873),
(#250874,#250875),(#250876,#250877),(#250878,#250879),(#250880,#250881),
(#250882,#250883),(#250884,#250885),(#250886,#250887),(#250888,#250889),
(#250890,#250891),(#250892,#250893),(#250894,#250895),(#250896,#250897),
(#250898,#250899),(#250900,#250901),(#250902,#250903),(#250904,#250905),
(#250906,#250907),(#250908,#250909),(#250910,#250911),(#250912,#250913),
(#250914,#250915),(#250916,#250917),(#250918,#250919),(#250920,#250921),
(#250922,#250923),(#250924,#250925),(#250926,#250927),(#250928,#250929),
(#250930,#250931),(#250932,#250933),(#250934,#250935),(#250936,#250937),
(#250938,#250939),(#250940,#250941),(#250942,#250943),(#250944,#250945),
(#250946,#250947),(#250948,#250949),(#250950,#250951),(#250952,#250953),
(#250954,#250955),(#250956,#250957),(#250958,#250959),(#250960,#250961),
(#250962,#250963),(#250964,#250965),(#250966,#250967),(#250968,#250969),
(#250970,#250971),(#250972,#250973),(#250974,#250975),(#250976,#250977),
(#250978,#250979),(#250980,#250981),(#250982,#250983),(#250984,#250985),
(#250986,#250987),(#250988,#250989),(#250990,#250991),(#250992,#250993),
(#250994,#250995),(#250996,#250997),(#250998,#250999),(#251000,#251001),
(#251002,#251003),(#251004,#251005),(#251006,#251007),(#251008,#251009),
(#251010,#251011),(#251012,#251013),(#251014,#251015),(#251016,#251017),
(#251018,#251019),(#251020,#251021),(#251022,#251023),(#251024,#251025),
(#251026,#251027),(#251028,#251029),(#251030,#251031),(#251032,#251033),
(#251034,#251035),(#251036,#251037),(#251038,#251039),(#251040,#251041),
(#251042,#251043),(#251044,#251045),(#251046,#251047),(#251048,#251049),
(#251050,#251051),(#251052,#251053),(#251054,#251055),(#251056,#251057),
(#251058,#251059),(#251060,#251061),(#251062,#251063),(#251064,#251065),
(#251066,#251067),(#251068,#251069),(#251070,#251071),(#251072,#251073),
(#251074,#251075),(#251076,#251077),(#251078,#251079),(#251080,#251081),
(#251082,#251083),(#251084,#251085),(#251086,#251087),(#251088,#251089),
(#251090,#251091),(#251092,#251093),(#251094,#251095),(#251096,#251097),
(#251098,#251099),(#251100,#251101),(#251102,#251103),(#251104,#251105),
(#251106,#251107),(#251108,#251109)),.UNSPECIFIED.,.F.,.F.,.F.)
B_SPLINE_SURFACE_WITH_KNOTS((6,1,1,1,1,1,1,1,1,1,1,1,1,1,1,1,1,1,1,1,1,
1,1,1,1,1,1,1,1,1,1,1,1,1,1,1,1,1,1,1,1,1,1,1,1,1,1,1,1,1,1,1,1,1,1,1,1,
1,1,1,1,1,1,1,1,1,1,1,1,1,1,1,1,1,1,1,1,1,1,1,1,1,1,1,1,1,1,1,1,1,1,1,1,
1,1,1,1,1,1,1,1,1,1,1,1,1,1,1,1,1,1,1,1,1,1,1,1,1,1,1,1,1,1,1,1,1,1,1,1,
1,1,1,1,1,1,1,1,1,1,1,1,1,1,1,1,1,1,1,1,1,1,1,1,1,1,1,1,1,1,1,1,1,1,1,1,
1,1,1,1,1,1,1,1,1,1,1,1,1,1,1,1,1,1,1,1,1,1,1,1,1,1,1,1,1,1,1,1,1,1,1,6),
(2,2),(-1.,-0.995000000000001,-0.990000000000001,-0.985000000000001,-0.980000000000001,
-0.975000000000001,-0.970000000000001,-0.965000000000001,-0.960000000000001,
-0.955000000000001,-0.950000000000001,-0.945000000000001,-0.940000000000001,
-0.935000000000001,-0.930000000000001,-0.925000000000001,-0.920000000000001,
-0.915000000000001,-0.910000000000001,-0.905000000000001,-0.900000000000001,
-0.895000000000001,-0.890000000000001,-0.885000000000001,-0.880000000000001,
-0.875000000000001,-0.870000000000001,-0.865000000000001,-0.860000000000001,
-0.855000000000001,-0.850000000000001,-0.845000000000001,-0.840000000000001,
-0.835000000000001,-0.830000000000001,-0.825000000000001,-0.820000000000001,
-0.815000000000001,-0.810000000000001,-0.805000000000001,-0.800000000000001,
-0.795000000000001,-0.790000000000001,-0.785000000000001,-0.780000000000001,
-0.775000000000001,-0.770000000000001,-0.765000000000001,-0.760000000000001,
-0.755000000000001,-0.750000000000001,-0.745000000000001,-0.740000000000001,
-0.735000000000001,-0.730000000000001,-0.725000000000001,-0.720000000000001,
-0.715000000000001,-0.710000000000001,-0.705000000000001,-0.700000000000001,
-0.695000000000001,-0.690000000000001,-0.685,-0.68,-0.675,-0.67,-0.665,
-0.66,-0.655,-0.65,-0.645,-0.64,-0.635,-0.63,-0.625,-0.62,-0.615,-0.61,
-0.605,-0.6,-0.595,-0.59,-0.585,-0.58,-0.575,-0.57,-0.565,-0.56,-0.555,
-0.55,-0.545,-0.54,-0.535,-0.53,-0.525,-0.52,-0.515,-0.51,-0.505,-0.5,-0.495,
-0.49,-0.485,-0.48,-0.475,-0.47,-0.465,-0.46,-0.455,-0.45,-0.445,-0.44,
-0.435,-0.43,-0.425,-0.42,-0.415,-0.41,-0.405,-0.4,-0.395,-0.39,-0.385,
-0.38,-0.375,-0.37,-0.365,-0.36,-0.355,-0.35,-0.345,-0.34,-0.335,-0.33,
-0.325,-0.32,-0.315,-0.31,-0.305,-0.3,-0.295,-0.29,-0.285,-0.28,-0.275,
-0.27,-0.265,-0.26,-0.255,-0.25,-0.245,-0.24,-0.235,-0.23,-0.225,-0.22,
-0.215,-0.21,-0.205,-0.2,-0.195,-0.19,-0.185,-0.18,-0.175,-0.17,-0.165,
-0.16,-0.155,-0.15,-0.145,-0.14,-0.135,-0.13,-0.125,-0.12,-0.115,-0.11,
-0.105,-0.1,-0.095,-0.09,-0.085,-0.08,-0.075,-0.07,-0.065,-0.06,-0.055,
-0.05,-0.045,-0.04,-0.035,-0.03,-0.025,-0.02,-0.015,-0.01,-0.005,0.),(0.,
1.2),.UNSPECIFIED.)
GEOMETRIC_REPRESENTATION_ITEM()
RATIONAL_B_SPLINE_SURFACE(((1.,1.),(1.,1.),(1.,1.),(1.,1.),(1.,1.),(1.,
1.),(1.,1.),(1.,1.),(1.,1.),(1.,1.),(1.,1.),(1.,1.),(1.,1.),(1.,1.),(1.,
1.),(1.,1.),(1.,1.),(1.,1.),(1.,1.),(1.,1.),(1.,1.),(1.,1.),(1.,1.),(1.,
1.),(1.,1.),(1.,1.),(1.,1.),(1.,1.),(1.,1.),(1.,1.),(1.,1.),(1.,1.),(1.,
1.),(1.,1.),(1.,1.),(1.,1.),(1.,1.),(1.,1.),(1.,1.),(1.,1.),(1.,1.),(1.,
1.),(1.,1.),(1.,1.),(1.,1.),(1.,1.),(1.,1.),(1.,1.),(1.,1.),(1.,1.),(1.,
1.),(1.,1.),(1.,1.),(1.,1.),(1.,1.),(1.,1.),(1.,1.),(1.,1.),(1.,1.),(1.,
1.),(1.,1.),(1.,1.),(1.,1.),(1.,1.),(1.,1.),(1.,1.),(1.,1.),(1.,1.),(1.,
1.),(1.,1.),(1.,1.),(1.,1.),(1.,1.),(1.,1.),(1.,1.),(1.,1.),(1.,1.),(1.,
1.),(1.,1.),(1.,1.),(1.,1.),(1.,1.),(1.,1.),(1.,1.),(1.,1.),(1.,1.),(1.,
1.),(1.,1.),(1.,1.),(1.,1.),(1.,1.),(1.,1.),(1.,1.),(1.,1.),(1.,1.),(1.,
1.),(1.,1.),(1.,1.),(1.,1.),(1.,1.),(1.,1.),(1.,1.),(1.,1.),(1.,1.),(1.,
1.),(1.,1.),(1.,1.),(1.,1.),(1.,1.),(1.,1.),(1.,1.),(1.,1.),(1.,1.),(1.,
1.),(1.,1.),(1.,1.),(1.,1.),(1.,1.),(1.,1.),(1.,1.),(1.,1.),(1.,1.),(1.,
1.),(1.,1.),(1.,1.),(1.,1.),(1.,1.),(1.,1.),(1.,1.),(1.,1.),(1.,1.),(1.,
1.),(1.,1.),(1.,1.),(1.,1.),(1.,1.),(1.,1.),(1.,1.),(1.,1.),(1.,1.),(1.,
1.),(1.,1.),(1.,1.),(1.,1.),(1.,1.),(1.,1.),(1.,1.),(1.,1.),(1.,1.),(1.,
1.),(1.,1.),(1.,1.),(1.,1.),(1.,1.),(1.,1.),(1.,1.),(1.,1.),(1.,1.),(1.,
1.),(1.,1.),(1.,1.),(1.,1.),(1.,1.),(1.,1.),(1.,1.),(1.,1.),(1.,1.),(1.,
1.),(1.,1.),(1.,1.),(1.,1.),(1.,1.),(1.,1.),(1.,1.),(1.,1.),(1.,1.),(1.,
1.),(1.,1.),(1.,1.),(1.,1.),(1.,1.),(1.,1.),(1.,1.),(1.,1.),(1.,1.),(1.,
1.),(1.,1.),(1.,1.),(1.,1.),(1.,1.),(1.,1.),(1.,1.),(1.,1.),(1.,1.),(1.,
1.),(1.,1.),(1.,1.),(1.,1.),(1.,1.),(1.,1.),(1.,1.),(1.,1.),(1.,1.),(1.,
1.),(1.,1.)))
REPRESENTATION_ITEM('')
SURFACE()
);
#1118=(
BOUNDED_SURFACE()
B_SPLINE_SURFACE(5,1,((#251523,#251524),(#251525,#251526),(#251527,#251528),
(#251529,#251530),(#251531,#251532),(#251533,#251534),(#251535,#251536),
(#251537,#251538),(#251539,#251540),(#251541,#251542),(#251543,#251544),
(#251545,#251546),(#251547,#251548),(#251549,#251550),(#251551,#251552),
(#251553,#251554),(#251555,#251556),(#251557,#251558),(#251559,#251560),
(#251561,#251562),(#251563,#251564),(#251565,#251566),(#251567,#251568),
(#251569,#251570),(#251571,#251572),(#251573,#251574),(#251575,#251576),
(#251577,#251578),(#251579,#251580),(#251581,#251582),(#251583,#251584),
(#251585,#251586),(#251587,#251588),(#251589,#251590),(#251591,#251592),
(#251593,#251594),(#251595,#251596),(#251597,#251598),(#251599,#251600),
(#251601,#251602),(#251603,#251604),(#251605,#251606),(#251607,#251608),
(#251609,#251610),(#251611,#251612),(#251613,#251614),(#251615,#251616),
(#251617,#251618),(#251619,#251620),(#251621,#251622),(#251623,#251624),
(#251625,#251626),(#251627,#251628),(#251629,#251630),(#251631,#251632),
(#251633,#251634),(#251635,#251636),(#251637,#251638),(#251639,#251640),
(#251641,#251642),(#251643,#251644),(#251645,#251646),(#251647,#251648),
(#251649,#251650),(#251651,#251652),(#251653,#251654),(#251655,#251656),
(#251657,#251658),(#251659,#251660),(#251661,#251662),(#251663,#251664),
(#251665,#251666),(#251667,#251668),(#251669,#251670),(#251671,#251672),
(#251673,#251674),(#251675,#251676),(#251677,#251678),(#251679,#251680),
(#251681,#251682),(#251683,#251684),(#251685,#251686),(#251687,#251688),
(#251689,#251690),(#251691,#251692),(#251693,#251694),(#251695,#251696),
(#251697,#251698),(#251699,#251700),(#251701,#251702),(#251703,#251704),
(#251705,#251706),(#251707,#251708),(#251709,#251710),(#251711,#251712),
(#251713,#251714),(#251715,#251716),(#251717,#251718),(#251719,#251720),
(#251721,#251722),(#251723,#251724),(#251725,#251726),(#251727,#251728),
(#251729,#251730),(#251731,#251732),(#251733,#251734),(#251735,#251736),
(#251737,#251738),(#251739,#251740),(#251741,#251742),(#251743,#251744),
(#251745,#251746),(#251747,#251748),(#251749,#251750),(#251751,#251752),
(#251753,#251754),(#251755,#251756),(#251757,#251758),(#251759,#251760),
(#251761,#251762),(#251763,#251764),(#251765,#251766),(#251767,#251768),
(#251769,#251770),(#251771,#251772),(#251773,#251774),(#251775,#251776),
(#251777,#251778),(#251779,#251780),(#251781,#251782),(#251783,#251784),
(#251785,#251786),(#251787,#251788),(#251789,#251790),(#251791,#251792),
(#251793,#251794),(#251795,#251796),(#251797,#251798),(#251799,#251800),
(#251801,#251802),(#251803,#251804),(#251805,#251806),(#251807,#251808),
(#251809,#251810),(#251811,#251812),(#251813,#251814),(#251815,#251816),
(#251817,#251818),(#251819,#251820),(#251821,#251822),(#251823,#251824),
(#251825,#251826),(#251827,#251828),(#251829,#251830),(#251831,#251832),
(#251833,#251834),(#251835,#251836),(#251837,#251838),(#251839,#251840),
(#251841,#251842),(#251843,#251844),(#251845,#251846),(#251847,#251848),
(#251849,#251850),(#251851,#251852),(#251853,#251854),(#251855,#251856),
(#251857,#251858),(#251859,#251860),(#251861,#251862),(#251863,#251864),
(#251865,#251866),(#251867,#251868),(#251869,#251870),(#251871,#251872),
(#251873,#251874),(#251875,#251876),(#251877,#251878),(#251879,#251880),
(#251881,#251882),(#251883,#251884),(#251885,#251886),(#251887,#251888),
(#251889,#251890),(#251891,#251892),(#251893,#251894),(#251895,#251896),
(#251897,#251898),(#251899,#251900),(#251901,#251902),(#251903,#251904),
(#251905,#251906),(#251907,#251908),(#251909,#251910),(#251911,#251912),
(#251913,#251914),(#251915,#251916),(#251917,#251918),(#251919,#251920),
(#251921,#251922),(#251923,#251924),(#251925,#251926),(#251927,#251928),
(#251929,#251930),(#251931,#251932)),.UNSPECIFIED.,.F.,.F.,.F.)
B_SPLINE_SURFACE_WITH_KNOTS((6,1,1,1,1,1,1,1,1,1,1,1,1,1,1,1,1,1,1,1,1,
1,1,1,1,1,1,1,1,1,1,1,1,1,1,1,1,1,1,1,1,1,1,1,1,1,1,1,1,1,1,1,1,1,1,1,1,
1,1,1,1,1,1,1,1,1,1,1,1,1,1,1,1,1,1,1,1,1,1,1,1,1,1,1,1,1,1,1,1,1,1,1,1,
1,1,1,1,1,1,1,1,1,1,1,1,1,1,1,1,1,1,1,1,1,1,1,1,1,1,1,1,1,1,1,1,1,1,1,1,
1,1,1,1,1,1,1,1,1,1,1,1,1,1,1,1,1,1,1,1,1,1,1,1,1,1,1,1,1,1,1,1,1,1,1,1,
1,1,1,1,1,1,1,1,1,1,1,1,1,1,1,1,1,1,1,1,1,1,1,1,1,1,1,1,1,1,1,1,1,1,1,6),
(2,2),(0.,0.005,0.01,0.015,0.02,0.025,0.03,0.035,0.04,0.045,0.05,0.055,
0.06,0.065,0.07,0.075,0.08,0.085,0.09,0.095,0.1,0.105,0.11,0.115,0.12,0.125,
0.13,0.135,0.14,0.145,0.15,0.155,0.16,0.165,0.17,0.175,0.18,0.185,0.19,
0.195,0.2,0.205,0.21,0.215,0.22,0.225,0.23,0.235,0.24,0.245,0.25,0.255,
0.26,0.265,0.27,0.275,0.28,0.285,0.29,0.295,0.3,0.305,0.31,0.315,0.32,0.325,
0.33,0.335,0.34,0.345,0.35,0.355,0.36,0.365,0.37,0.375,0.38,0.385,0.39,
0.395,0.4,0.405,0.41,0.415,0.42,0.425,0.43,0.435,0.44,0.445,0.45,0.455,
0.46,0.465,0.47,0.475,0.48,0.485,0.49,0.495,0.5,0.505,0.51,0.515,0.52,0.525,
0.53,0.535,0.54,0.545,0.55,0.555,0.56,0.565,0.57,0.575,0.58,0.585,0.59,
0.595,0.6,0.605,0.61,0.615,0.62,0.625,0.63,0.635,0.64,0.645,0.65,0.655,
0.66,0.665,0.67,0.675,0.68,0.685,0.690000000000001,0.695000000000001,0.700000000000001,
0.705000000000001,0.710000000000001,0.715000000000001,0.720000000000001,
0.725000000000001,0.730000000000001,0.735000000000001,0.740000000000001,
0.745000000000001,0.750000000000001,0.755000000000001,0.760000000000001,
0.765000000000001,0.770000000000001,0.775000000000001,0.780000000000001,
0.785000000000001,0.790000000000001,0.795000000000001,0.800000000000001,
0.805000000000001,0.810000000000001,0.815000000000001,0.820000000000001,
0.825000000000001,0.830000000000001,0.835000000000001,0.840000000000001,
0.845000000000001,0.850000000000001,0.855000000000001,0.860000000000001,
0.865000000000001,0.870000000000001,0.875000000000001,0.880000000000001,
0.885000000000001,0.890000000000001,0.895000000000001,0.900000000000001,
0.905000000000001,0.910000000000001,0.915000000000001,0.920000000000001,
0.925000000000001,0.930000000000001,0.935000000000001,0.940000000000001,
0.945000000000001,0.950000000000001,0.955000000000001,0.960000000000001,
0.965000000000001,0.970000000000001,0.975000000000001,0.980000000000001,
0.985000000000001,0.990000000000001,0.995000000000001,1.),(0.,1.2),
 .UNSPECIFIED.)
GEOMETRIC_REPRESENTATION_ITEM()
RATIONAL_B_SPLINE_SURFACE(((1.,1.),(1.,1.),(1.,1.),(1.,1.),(1.,1.),(1.,
1.),(1.,1.),(1.,1.),(1.,1.),(1.,1.),(1.,1.),(1.,1.),(1.,1.),(1.,1.),(1.,
1.),(1.,1.),(1.,1.),(1.,1.),(1.,1.),(1.,1.),(1.,1.),(1.,1.),(1.,1.),(1.,
1.),(1.,1.),(1.,1.),(1.,1.),(1.,1.),(1.,1.),(1.,1.),(1.,1.),(1.,1.),(1.,
1.),(1.,1.),(1.,1.),(1.,1.),(1.,1.),(1.,1.),(1.,1.),(1.,1.),(1.,1.),(1.,
1.),(1.,1.),(1.,1.),(1.,1.),(1.,1.),(1.,1.),(1.,1.),(1.,1.),(1.,1.),(1.,
1.),(1.,1.),(1.,1.),(1.,1.),(1.,1.),(1.,1.),(1.,1.),(1.,1.),(1.,1.),(1.,
1.),(1.,1.),(1.,1.),(1.,1.),(1.,1.),(1.,1.),(1.,1.),(1.,1.),(1.,1.),(1.,
1.),(1.,1.),(1.,1.),(1.,1.),(1.,1.),(1.,1.),(1.,1.),(1.,1.),(1.,1.),(1.,
1.),(1.,1.),(1.,1.),(1.,1.),(1.,1.),(1.,1.),(1.,1.),(1.,1.),(1.,1.),(1.,
1.),(1.,1.),(1.,1.),(1.,1.),(1.,1.),(1.,1.),(1.,1.),(1.,1.),(1.,1.),(1.,
1.),(1.,1.),(1.,1.),(1.,1.),(1.,1.),(1.,1.),(1.,1.),(1.,1.),(1.,1.),(1.,
1.),(1.,1.),(1.,1.),(1.,1.),(1.,1.),(1.,1.),(1.,1.),(1.,1.),(1.,1.),(1.,
1.),(1.,1.),(1.,1.),(1.,1.),(1.,1.),(1.,1.),(1.,1.),(1.,1.),(1.,1.),(1.,
1.),(1.,1.),(1.,1.),(1.,1.),(1.,1.),(1.,1.),(1.,1.),(1.,1.),(1.,1.),(1.,
1.),(1.,1.),(1.,1.),(1.,1.),(1.,1.),(1.,1.),(1.,1.),(1.,1.),(1.,1.),(1.,
1.),(1.,1.),(1.,1.),(1.,1.),(1.,1.),(1.,1.),(1.,1.),(1.,1.),(1.,1.),(1.,
1.),(1.,1.),(1.,1.),(1.,1.),(1.,1.),(1.,1.),(1.,1.),(1.,1.),(1.,1.),(1.,
1.),(1.,1.),(1.,1.),(1.,1.),(1.,1.),(1.,1.),(1.,1.),(1.,1.),(1.,1.),(1.,
1.),(1.,1.),(1.,1.),(1.,1.),(1.,1.),(1.,1.),(1.,1.),(1.,1.),(1.,1.),(1.,
1.),(1.,1.),(1.,1.),(1.,1.),(1.,1.),(1.,1.),(1.,1.),(1.,1.),(1.,1.),(1.,
1.),(1.,1.),(1.,1.),(1.,1.),(1.,1.),(1.,1.),(1.,1.),(1.,1.),(1.,1.),(1.,
1.),(1.,1.),(1.,1.),(1.,1.),(1.,1.),(1.,1.),(1.,1.),(1.,1.),(1.,1.),(1.,
1.),(1.,1.)))
REPRESENTATION_ITEM('')
SURFACE()
);
#1119=(
BOUNDED_SURFACE()
B_SPLINE_SURFACE(5,1,((#252352,#252353),(#252354,#252355),(#252356,#252357),
(#252358,#252359),(#252360,#252361),(#252362,#252363),(#252364,#252365),
(#252366,#252367),(#252368,#252369),(#252370,#252371),(#252372,#252373),
(#252374,#252375),(#252376,#252377),(#252378,#252379),(#252380,#252381),
(#252382,#252383),(#252384,#252385),(#252386,#252387),(#252388,#252389),
(#252390,#252391),(#252392,#252393),(#252394,#252395),(#252396,#252397),
(#252398,#252399),(#252400,#252401),(#252402,#252403),(#252404,#252405),
(#252406,#252407),(#252408,#252409),(#252410,#252411),(#252412,#252413),
(#252414,#252415),(#252416,#252417),(#252418,#252419),(#252420,#252421),
(#252422,#252423),(#252424,#252425),(#252426,#252427),(#252428,#252429),
(#252430,#252431),(#252432,#252433),(#252434,#252435),(#252436,#252437),
(#252438,#252439),(#252440,#252441),(#252442,#252443),(#252444,#252445),
(#252446,#252447),(#252448,#252449),(#252450,#252451),(#252452,#252453),
(#252454,#252455),(#252456,#252457),(#252458,#252459),(#252460,#252461),
(#252462,#252463),(#252464,#252465),(#252466,#252467),(#252468,#252469),
(#252470,#252471),(#252472,#252473),(#252474,#252475),(#252476,#252477),
(#252478,#252479),(#252480,#252481),(#252482,#252483),(#252484,#252485),
(#252486,#252487),(#252488,#252489),(#252490,#252491),(#252492,#252493),
(#252494,#252495),(#252496,#252497),(#252498,#252499),(#252500,#252501),
(#252502,#252503),(#252504,#252505),(#252506,#252507),(#252508,#252509),
(#252510,#252511),(#252512,#252513),(#252514,#252515),(#252516,#252517),
(#252518,#252519),(#252520,#252521),(#252522,#252523),(#252524,#252525),
(#252526,#252527),(#252528,#252529),(#252530,#252531),(#252532,#252533),
(#252534,#252535),(#252536,#252537),(#252538,#252539),(#252540,#252541),
(#252542,#252543),(#252544,#252545),(#252546,#252547),(#252548,#252549),
(#252550,#252551),(#252552,#252553),(#252554,#252555),(#252556,#252557),
(#252558,#252559),(#252560,#252561),(#252562,#252563),(#252564,#252565),
(#252566,#252567),(#252568,#252569),(#252570,#252571),(#252572,#252573),
(#252574,#252575),(#252576,#252577),(#252578,#252579),(#252580,#252581),
(#252582,#252583),(#252584,#252585),(#252586,#252587),(#252588,#252589),
(#252590,#252591),(#252592,#252593),(#252594,#252595),(#252596,#252597),
(#252598,#252599),(#252600,#252601),(#252602,#252603),(#252604,#252605),
(#252606,#252607),(#252608,#252609),(#252610,#252611),(#252612,#252613),
(#252614,#252615),(#252616,#252617),(#252618,#252619),(#252620,#252621),
(#252622,#252623),(#252624,#252625),(#252626,#252627),(#252628,#252629),
(#252630,#252631),(#252632,#252633),(#252634,#252635),(#252636,#252637),
(#252638,#252639),(#252640,#252641),(#252642,#252643),(#252644,#252645),
(#252646,#252647),(#252648,#252649),(#252650,#252651),(#252652,#252653),
(#252654,#252655),(#252656,#252657),(#252658,#252659),(#252660,#252661),
(#252662,#252663),(#252664,#252665),(#252666,#252667),(#252668,#252669),
(#252670,#252671),(#252672,#252673),(#252674,#252675),(#252676,#252677),
(#252678,#252679),(#252680,#252681),(#252682,#252683),(#252684,#252685),
(#252686,#252687),(#252688,#252689),(#252690,#252691),(#252692,#252693),
(#252694,#252695),(#252696,#252697),(#252698,#252699),(#252700,#252701),
(#252702,#252703),(#252704,#252705),(#252706,#252707),(#252708,#252709),
(#252710,#252711),(#252712,#252713),(#252714,#252715),(#252716,#252717),
(#252718,#252719),(#252720,#252721),(#252722,#252723),(#252724,#252725),
(#252726,#252727),(#252728,#252729),(#252730,#252731),(#252732,#252733),
(#252734,#252735),(#252736,#252737),(#252738,#252739),(#252740,#252741),
(#252742,#252743),(#252744,#252745),(#252746,#252747),(#252748,#252749),
(#252750,#252751),(#252752,#252753),(#252754,#252755),(#252756,#252757),
(#252758,#252759),(#252760,#252761)),.UNSPECIFIED.,.F.,.F.,.F.)
B_SPLINE_SURFACE_WITH_KNOTS((6,1,1,1,1,1,1,1,1,1,1,1,1,1,1,1,1,1,1,1,1,
1,1,1,1,1,1,1,1,1,1,1,1,1,1,1,1,1,1,1,1,1,1,1,1,1,1,1,1,1,1,1,1,1,1,1,1,
1,1,1,1,1,1,1,1,1,1,1,1,1,1,1,1,1,1,1,1,1,1,1,1,1,1,1,1,1,1,1,1,1,1,1,1,
1,1,1,1,1,1,1,1,1,1,1,1,1,1,1,1,1,1,1,1,1,1,1,1,1,1,1,1,1,1,1,1,1,1,1,1,
1,1,1,1,1,1,1,1,1,1,1,1,1,1,1,1,1,1,1,1,1,1,1,1,1,1,1,1,1,1,1,1,1,1,1,1,
1,1,1,1,1,1,1,1,1,1,1,1,1,1,1,1,1,1,1,1,1,1,1,1,1,1,1,1,1,1,1,1,1,1,1,6),
(2,2),(-1.,-0.995000000000001,-0.990000000000001,-0.985000000000001,-0.980000000000001,
-0.975000000000001,-0.970000000000001,-0.965000000000001,-0.960000000000001,
-0.955000000000001,-0.950000000000001,-0.945000000000001,-0.940000000000001,
-0.935000000000001,-0.930000000000001,-0.925000000000001,-0.920000000000001,
-0.915000000000001,-0.910000000000001,-0.905000000000001,-0.900000000000001,
-0.895000000000001,-0.890000000000001,-0.885000000000001,-0.880000000000001,
-0.875000000000001,-0.870000000000001,-0.865000000000001,-0.860000000000001,
-0.855000000000001,-0.850000000000001,-0.845000000000001,-0.840000000000001,
-0.835000000000001,-0.830000000000001,-0.825000000000001,-0.820000000000001,
-0.815000000000001,-0.810000000000001,-0.805000000000001,-0.800000000000001,
-0.795000000000001,-0.790000000000001,-0.785000000000001,-0.780000000000001,
-0.775000000000001,-0.770000000000001,-0.765000000000001,-0.760000000000001,
-0.755000000000001,-0.750000000000001,-0.745000000000001,-0.740000000000001,
-0.735000000000001,-0.730000000000001,-0.725000000000001,-0.720000000000001,
-0.715000000000001,-0.710000000000001,-0.705000000000001,-0.700000000000001,
-0.695000000000001,-0.690000000000001,-0.685,-0.68,-0.675,-0.67,-0.665,
-0.66,-0.655,-0.65,-0.645,-0.64,-0.635,-0.63,-0.625,-0.62,-0.615,-0.61,
-0.605,-0.6,-0.595,-0.59,-0.585,-0.58,-0.575,-0.57,-0.565,-0.56,-0.555,
-0.55,-0.545,-0.54,-0.535,-0.53,-0.525,-0.52,-0.515,-0.51,-0.505,-0.5,-0.495,
-0.49,-0.485,-0.48,-0.475,-0.47,-0.465,-0.46,-0.455,-0.45,-0.445,-0.44,
-0.435,-0.43,-0.425,-0.42,-0.415,-0.41,-0.405,-0.4,-0.395,-0.39,-0.385,
-0.38,-0.375,-0.37,-0.365,-0.36,-0.355,-0.35,-0.345,-0.34,-0.335,-0.33,
-0.325,-0.32,-0.315,-0.31,-0.305,-0.3,-0.295,-0.29,-0.285,-0.28,-0.275,
-0.27,-0.265,-0.26,-0.255,-0.25,-0.245,-0.24,-0.235,-0.23,-0.225,-0.22,
-0.215,-0.21,-0.205,-0.2,-0.195,-0.19,-0.185,-0.18,-0.175,-0.17,-0.165,
-0.16,-0.155,-0.15,-0.145,-0.14,-0.135,-0.13,-0.125,-0.12,-0.115,-0.11,
-0.105,-0.1,-0.095,-0.09,-0.085,-0.08,-0.075,-0.07,-0.065,-0.06,-0.055,
-0.05,-0.045,-0.04,-0.035,-0.03,-0.025,-0.02,-0.015,-0.01,-0.005,0.),(0.,
1.2),.UNSPECIFIED.)
GEOMETRIC_REPRESENTATION_ITEM()
RATIONAL_B_SPLINE_SURFACE(((1.,1.),(1.,1.),(1.,1.),(1.,1.),(1.,1.),(1.,
1.),(1.,1.),(1.,1.),(1.,1.),(1.,1.),(1.,1.),(1.,1.),(1.,1.),(1.,1.),(1.,
1.),(1.,1.),(1.,1.),(1.,1.),(1.,1.),(1.,1.),(1.,1.),(1.,1.),(1.,1.),(1.,
1.),(1.,1.),(1.,1.),(1.,1.),(1.,1.),(1.,1.),(1.,1.),(1.,1.),(1.,1.),(1.,
1.),(1.,1.),(1.,1.),(1.,1.),(1.,1.),(1.,1.),(1.,1.),(1.,1.),(1.,1.),(1.,
1.),(1.,1.),(1.,1.),(1.,1.),(1.,1.),(1.,1.),(1.,1.),(1.,1.),(1.,1.),(1.,
1.),(1.,1.),(1.,1.),(1.,1.),(1.,1.),(1.,1.),(1.,1.),(1.,1.),(1.,1.),(1.,
1.),(1.,1.),(1.,1.),(1.,1.),(1.,1.),(1.,1.),(1.,1.),(1.,1.),(1.,1.),(1.,
1.),(1.,1.),(1.,1.),(1.,1.),(1.,1.),(1.,1.),(1.,1.),(1.,1.),(1.,1.),(1.,
1.),(1.,1.),(1.,1.),(1.,1.),(1.,1.),(1.,1.),(1.,1.),(1.,1.),(1.,1.),(1.,
1.),(1.,1.),(1.,1.),(1.,1.),(1.,1.),(1.,1.),(1.,1.),(1.,1.),(1.,1.),(1.,
1.),(1.,1.),(1.,1.),(1.,1.),(1.,1.),(1.,1.),(1.,1.),(1.,1.),(1.,1.),(1.,
1.),(1.,1.),(1.,1.),(1.,1.),(1.,1.),(1.,1.),(1.,1.),(1.,1.),(1.,1.),(1.,
1.),(1.,1.),(1.,1.),(1.,1.),(1.,1.),(1.,1.),(1.,1.),(1.,1.),(1.,1.),(1.,
1.),(1.,1.),(1.,1.),(1.,1.),(1.,1.),(1.,1.),(1.,1.),(1.,1.),(1.,1.),(1.,
1.),(1.,1.),(1.,1.),(1.,1.),(1.,1.),(1.,1.),(1.,1.),(1.,1.),(1.,1.),(1.,
1.),(1.,1.),(1.,1.),(1.,1.),(1.,1.),(1.,1.),(1.,1.),(1.,1.),(1.,1.),(1.,
1.),(1.,1.),(1.,1.),(1.,1.),(1.,1.),(1.,1.),(1.,1.),(1.,1.),(1.,1.),(1.,
1.),(1.,1.),(1.,1.),(1.,1.),(1.,1.),(1.,1.),(1.,1.),(1.,1.),(1.,1.),(1.,
1.),(1.,1.),(1.,1.),(1.,1.),(1.,1.),(1.,1.),(1.,1.),(1.,1.),(1.,1.),(1.,
1.),(1.,1.),(1.,1.),(1.,1.),(1.,1.),(1.,1.),(1.,1.),(1.,1.),(1.,1.),(1.,
1.),(1.,1.),(1.,1.),(1.,1.),(1.,1.),(1.,1.),(1.,1.),(1.,1.),(1.,1.),(1.,
1.),(1.,1.),(1.,1.),(1.,1.),(1.,1.),(1.,1.),(1.,1.),(1.,1.),(1.,1.),(1.,
1.),(1.,1.)))
REPRESENTATION_ITEM('')
SURFACE()
);
#1120=(
BOUNDED_SURFACE()
B_SPLINE_SURFACE(5,1,((#253175,#253176),(#253177,#253178),(#253179,#253180),
(#253181,#253182),(#253183,#253184),(#253185,#253186),(#253187,#253188),
(#253189,#253190),(#253191,#253192),(#253193,#253194),(#253195,#253196),
(#253197,#253198),(#253199,#253200),(#253201,#253202),(#253203,#253204),
(#253205,#253206),(#253207,#253208),(#253209,#253210),(#253211,#253212),
(#253213,#253214),(#253215,#253216),(#253217,#253218),(#253219,#253220),
(#253221,#253222),(#253223,#253224),(#253225,#253226),(#253227,#253228),
(#253229,#253230),(#253231,#253232),(#253233,#253234),(#253235,#253236),
(#253237,#253238),(#253239,#253240),(#253241,#253242),(#253243,#253244),
(#253245,#253246),(#253247,#253248),(#253249,#253250),(#253251,#253252),
(#253253,#253254),(#253255,#253256),(#253257,#253258),(#253259,#253260),
(#253261,#253262),(#253263,#253264),(#253265,#253266),(#253267,#253268),
(#253269,#253270),(#253271,#253272),(#253273,#253274),(#253275,#253276),
(#253277,#253278),(#253279,#253280),(#253281,#253282),(#253283,#253284),
(#253285,#253286),(#253287,#253288),(#253289,#253290),(#253291,#253292),
(#253293,#253294),(#253295,#253296),(#253297,#253298),(#253299,#253300),
(#253301,#253302),(#253303,#253304),(#253305,#253306),(#253307,#253308),
(#253309,#253310),(#253311,#253312),(#253313,#253314),(#253315,#253316),
(#253317,#253318),(#253319,#253320),(#253321,#253322),(#253323,#253324),
(#253325,#253326),(#253327,#253328),(#253329,#253330),(#253331,#253332),
(#253333,#253334),(#253335,#253336),(#253337,#253338),(#253339,#253340),
(#253341,#253342),(#253343,#253344),(#253345,#253346),(#253347,#253348),
(#253349,#253350),(#253351,#253352),(#253353,#253354),(#253355,#253356),
(#253357,#253358),(#253359,#253360),(#253361,#253362),(#253363,#253364),
(#253365,#253366),(#253367,#253368),(#253369,#253370),(#253371,#253372),
(#253373,#253374),(#253375,#253376),(#253377,#253378),(#253379,#253380),
(#253381,#253382),(#253383,#253384),(#253385,#253386),(#253387,#253388),
(#253389,#253390),(#253391,#253392),(#253393,#253394),(#253395,#253396),
(#253397,#253398),(#253399,#253400),(#253401,#253402),(#253403,#253404),
(#253405,#253406),(#253407,#253408),(#253409,#253410),(#253411,#253412),
(#253413,#253414),(#253415,#253416),(#253417,#253418),(#253419,#253420),
(#253421,#253422),(#253423,#253424),(#253425,#253426),(#253427,#253428),
(#253429,#253430),(#253431,#253432),(#253433,#253434),(#253435,#253436),
(#253437,#253438),(#253439,#253440),(#253441,#253442),(#253443,#253444),
(#253445,#253446),(#253447,#253448),(#253449,#253450),(#253451,#253452),
(#253453,#253454),(#253455,#253456),(#253457,#253458),(#253459,#253460),
(#253461,#253462),(#253463,#253464),(#253465,#253466),(#253467,#253468),
(#253469,#253470),(#253471,#253472),(#253473,#253474),(#253475,#253476),
(#253477,#253478),(#253479,#253480),(#253481,#253482),(#253483,#253484),
(#253485,#253486),(#253487,#253488),(#253489,#253490),(#253491,#253492),
(#253493,#253494),(#253495,#253496),(#253497,#253498),(#253499,#253500),
(#253501,#253502),(#253503,#253504),(#253505,#253506),(#253507,#253508),
(#253509,#253510),(#253511,#253512),(#253513,#253514),(#253515,#253516),
(#253517,#253518),(#253519,#253520),(#253521,#253522),(#253523,#253524),
(#253525,#253526),(#253527,#253528),(#253529,#253530),(#253531,#253532),
(#253533,#253534),(#253535,#253536),(#253537,#253538),(#253539,#253540),
(#253541,#253542),(#253543,#253544),(#253545,#253546),(#253547,#253548),
(#253549,#253550),(#253551,#253552),(#253553,#253554),(#253555,#253556),
(#253557,#253558),(#253559,#253560),(#253561,#253562),(#253563,#253564),
(#253565,#253566),(#253567,#253568),(#253569,#253570),(#253571,#253572),
(#253573,#253574),(#253575,#253576),(#253577,#253578),(#253579,#253580),
(#253581,#253582),(#253583,#253584)),.UNSPECIFIED.,.F.,.F.,.F.)
B_SPLINE_SURFACE_WITH_KNOTS((6,1,1,1,1,1,1,1,1,1,1,1,1,1,1,1,1,1,1,1,1,
1,1,1,1,1,1,1,1,1,1,1,1,1,1,1,1,1,1,1,1,1,1,1,1,1,1,1,1,1,1,1,1,1,1,1,1,
1,1,1,1,1,1,1,1,1,1,1,1,1,1,1,1,1,1,1,1,1,1,1,1,1,1,1,1,1,1,1,1,1,1,1,1,
1,1,1,1,1,1,1,1,1,1,1,1,1,1,1,1,1,1,1,1,1,1,1,1,1,1,1,1,1,1,1,1,1,1,1,1,
1,1,1,1,1,1,1,1,1,1,1,1,1,1,1,1,1,1,1,1,1,1,1,1,1,1,1,1,1,1,1,1,1,1,1,1,
1,1,1,1,1,1,1,1,1,1,1,1,1,1,1,1,1,1,1,1,1,1,1,1,1,1,1,1,1,1,1,1,1,1,1,6),
(2,2),(0.,0.005,0.01,0.015,0.02,0.025,0.03,0.035,0.04,0.045,0.05,0.055,
0.06,0.065,0.07,0.075,0.08,0.085,0.09,0.095,0.1,0.105,0.11,0.115,0.12,0.125,
0.13,0.135,0.14,0.145,0.15,0.155,0.16,0.165,0.17,0.175,0.18,0.185,0.19,
0.195,0.2,0.205,0.21,0.215,0.22,0.225,0.23,0.235,0.24,0.245,0.25,0.255,
0.26,0.265,0.27,0.275,0.28,0.285,0.29,0.295,0.3,0.305,0.31,0.315,0.32,0.325,
0.33,0.335,0.34,0.345,0.35,0.355,0.36,0.365,0.37,0.375,0.38,0.385,0.39,
0.395,0.4,0.405,0.41,0.415,0.42,0.425,0.43,0.435,0.44,0.445,0.45,0.455,
0.46,0.465,0.47,0.475,0.48,0.485,0.49,0.495,0.5,0.505,0.51,0.515,0.52,0.525,
0.53,0.535,0.54,0.545,0.55,0.555,0.56,0.565,0.57,0.575,0.58,0.585,0.59,
0.595,0.6,0.605,0.61,0.615,0.62,0.625,0.63,0.635,0.64,0.645,0.65,0.655,
0.66,0.665,0.67,0.675,0.68,0.685,0.690000000000001,0.695000000000001,0.700000000000001,
0.705000000000001,0.710000000000001,0.715000000000001,0.720000000000001,
0.725000000000001,0.730000000000001,0.735000000000001,0.740000000000001,
0.745000000000001,0.750000000000001,0.755000000000001,0.760000000000001,
0.765000000000001,0.770000000000001,0.775000000000001,0.780000000000001,
0.785000000000001,0.790000000000001,0.795000000000001,0.800000000000001,
0.805000000000001,0.810000000000001,0.815000000000001,0.820000000000001,
0.825000000000001,0.830000000000001,0.835000000000001,0.840000000000001,
0.845000000000001,0.850000000000001,0.855000000000001,0.860000000000001,
0.865000000000001,0.870000000000001,0.875000000000001,0.880000000000001,
0.885000000000001,0.890000000000001,0.895000000000001,0.900000000000001,
0.905000000000001,0.910000000000001,0.915000000000001,0.920000000000001,
0.925000000000001,0.930000000000001,0.935000000000001,0.940000000000001,
0.945000000000001,0.950000000000001,0.955000000000001,0.960000000000001,
0.965000000000001,0.970000000000001,0.975000000000001,0.980000000000001,
0.985000000000001,0.990000000000001,0.995000000000001,1.),(0.,1.2),
 .UNSPECIFIED.)
GEOMETRIC_REPRESENTATION_ITEM()
RATIONAL_B_SPLINE_SURFACE(((1.,1.),(1.,1.),(1.,1.),(1.,1.),(1.,1.),(1.,
1.),(1.,1.),(1.,1.),(1.,1.),(1.,1.),(1.,1.),(1.,1.),(1.,1.),(1.,1.),(1.,
1.),(1.,1.),(1.,1.),(1.,1.),(1.,1.),(1.,1.),(1.,1.),(1.,1.),(1.,1.),(1.,
1.),(1.,1.),(1.,1.),(1.,1.),(1.,1.),(1.,1.),(1.,1.),(1.,1.),(1.,1.),(1.,
1.),(1.,1.),(1.,1.),(1.,1.),(1.,1.),(1.,1.),(1.,1.),(1.,1.),(1.,1.),(1.,
1.),(1.,1.),(1.,1.),(1.,1.),(1.,1.),(1.,1.),(1.,1.),(1.,1.),(1.,1.),(1.,
1.),(1.,1.),(1.,1.),(1.,1.),(1.,1.),(1.,1.),(1.,1.),(1.,1.),(1.,1.),(1.,
1.),(1.,1.),(1.,1.),(1.,1.),(1.,1.),(1.,1.),(1.,1.),(1.,1.),(1.,1.),(1.,
1.),(1.,1.),(1.,1.),(1.,1.),(1.,1.),(1.,1.),(1.,1.),(1.,1.),(1.,1.),(1.,
1.),(1.,1.),(1.,1.),(1.,1.),(1.,1.),(1.,1.),(1.,1.),(1.,1.),(1.,1.),(1.,
1.),(1.,1.),(1.,1.),(1.,1.),(1.,1.),(1.,1.),(1.,1.),(1.,1.),(1.,1.),(1.,
1.),(1.,1.),(1.,1.),(1.,1.),(1.,1.),(1.,1.),(1.,1.),(1.,1.),(1.,1.),(1.,
1.),(1.,1.),(1.,1.),(1.,1.),(1.,1.),(1.,1.),(1.,1.),(1.,1.),(1.,1.),(1.,
1.),(1.,1.),(1.,1.),(1.,1.),(1.,1.),(1.,1.),(1.,1.),(1.,1.),(1.,1.),(1.,
1.),(1.,1.),(1.,1.),(1.,1.),(1.,1.),(1.,1.),(1.,1.),(1.,1.),(1.,1.),(1.,
1.),(1.,1.),(1.,1.),(1.,1.),(1.,1.),(1.,1.),(1.,1.),(1.,1.),(1.,1.),(1.,
1.),(1.,1.),(1.,1.),(1.,1.),(1.,1.),(1.,1.),(1.,1.),(1.,1.),(1.,1.),(1.,
1.),(1.,1.),(1.,1.),(1.,1.),(1.,1.),(1.,1.),(1.,1.),(1.,1.),(1.,1.),(1.,
1.),(1.,1.),(1.,1.),(1.,1.),(1.,1.),(1.,1.),(1.,1.),(1.,1.),(1.,1.),(1.,
1.),(1.,1.),(1.,1.),(1.,1.),(1.,1.),(1.,1.),(1.,1.),(1.,1.),(1.,1.),(1.,
1.),(1.,1.),(1.,1.),(1.,1.),(1.,1.),(1.,1.),(1.,1.),(1.,1.),(1.,1.),(1.,
1.),(1.,1.),(1.,1.),(1.,1.),(1.,1.),(1.,1.),(1.,1.),(1.,1.),(1.,1.),(1.,
1.),(1.,1.),(1.,1.),(1.,1.),(1.,1.),(1.,1.),(1.,1.),(1.,1.),(1.,1.),(1.,
1.),(1.,1.)))
REPRESENTATION_ITEM('')
SURFACE()
);
#1121=(
BOUNDED_SURFACE()
B_SPLINE_SURFACE(5,1,((#254933,#254934),(#254935,#254936),(#254937,#254938),
(#254939,#254940),(#254941,#254942),(#254943,#254944),(#254945,#254946),
(#254947,#254948),(#254949,#254950),(#254951,#254952),(#254953,#254954),
(#254955,#254956),(#254957,#254958),(#254959,#254960),(#254961,#254962),
(#254963,#254964),(#254965,#254966),(#254967,#254968),(#254969,#254970),
(#254971,#254972),(#254973,#254974),(#254975,#254976),(#254977,#254978),
(#254979,#254980),(#254981,#254982),(#254983,#254984),(#254985,#254986),
(#254987,#254988),(#254989,#254990),(#254991,#254992),(#254993,#254994),
(#254995,#254996),(#254997,#254998),(#254999,#255000),(#255001,#255002),
(#255003,#255004),(#255005,#255006),(#255007,#255008),(#255009,#255010),
(#255011,#255012),(#255013,#255014),(#255015,#255016),(#255017,#255018),
(#255019,#255020),(#255021,#255022),(#255023,#255024),(#255025,#255026),
(#255027,#255028),(#255029,#255030),(#255031,#255032),(#255033,#255034),
(#255035,#255036),(#255037,#255038),(#255039,#255040),(#255041,#255042),
(#255043,#255044),(#255045,#255046),(#255047,#255048),(#255049,#255050),
(#255051,#255052),(#255053,#255054),(#255055,#255056),(#255057,#255058),
(#255059,#255060),(#255061,#255062),(#255063,#255064),(#255065,#255066),
(#255067,#255068),(#255069,#255070),(#255071,#255072),(#255073,#255074),
(#255075,#255076),(#255077,#255078),(#255079,#255080),(#255081,#255082),
(#255083,#255084),(#255085,#255086),(#255087,#255088),(#255089,#255090),
(#255091,#255092),(#255093,#255094),(#255095,#255096),(#255097,#255098),
(#255099,#255100),(#255101,#255102),(#255103,#255104),(#255105,#255106),
(#255107,#255108),(#255109,#255110),(#255111,#255112),(#255113,#255114),
(#255115,#255116),(#255117,#255118),(#255119,#255120),(#255121,#255122),
(#255123,#255124),(#255125,#255126),(#255127,#255128),(#255129,#255130),
(#255131,#255132),(#255133,#255134),(#255135,#255136),(#255137,#255138),
(#255139,#255140),(#255141,#255142),(#255143,#255144),(#255145,#255146),
(#255147,#255148),(#255149,#255150),(#255151,#255152),(#255153,#255154),
(#255155,#255156),(#255157,#255158),(#255159,#255160),(#255161,#255162),
(#255163,#255164),(#255165,#255166),(#255167,#255168),(#255169,#255170),
(#255171,#255172),(#255173,#255174),(#255175,#255176),(#255177,#255178),
(#255179,#255180),(#255181,#255182),(#255183,#255184),(#255185,#255186),
(#255187,#255188),(#255189,#255190),(#255191,#255192),(#255193,#255194),
(#255195,#255196),(#255197,#255198),(#255199,#255200),(#255201,#255202),
(#255203,#255204),(#255205,#255206),(#255207,#255208),(#255209,#255210),
(#255211,#255212),(#255213,#255214),(#255215,#255216),(#255217,#255218),
(#255219,#255220),(#255221,#255222),(#255223,#255224),(#255225,#255226),
(#255227,#255228),(#255229,#255230),(#255231,#255232),(#255233,#255234),
(#255235,#255236),(#255237,#255238),(#255239,#255240),(#255241,#255242),
(#255243,#255244),(#255245,#255246),(#255247,#255248),(#255249,#255250),
(#255251,#255252),(#255253,#255254),(#255255,#255256),(#255257,#255258),
(#255259,#255260),(#255261,#255262),(#255263,#255264),(#255265,#255266),
(#255267,#255268),(#255269,#255270),(#255271,#255272),(#255273,#255274),
(#255275,#255276),(#255277,#255278),(#255279,#255280),(#255281,#255282),
(#255283,#255284),(#255285,#255286),(#255287,#255288),(#255289,#255290),
(#255291,#255292),(#255293,#255294),(#255295,#255296),(#255297,#255298),
(#255299,#255300),(#255301,#255302),(#255303,#255304),(#255305,#255306),
(#255307,#255308),(#255309,#255310),(#255311,#255312),(#255313,#255314),
(#255315,#255316),(#255317,#255318),(#255319,#255320),(#255321,#255322),
(#255323,#255324),(#255325,#255326),(#255327,#255328),(#255329,#255330),
(#255331,#255332),(#255333,#255334),(#255335,#255336),(#255337,#255338),
(#255339,#255340),(#255341,#255342)),.UNSPECIFIED.,.F.,.F.,.F.)
B_SPLINE_SURFACE_WITH_KNOTS((6,1,1,1,1,1,1,1,1,1,1,1,1,1,1,1,1,1,1,1,1,
1,1,1,1,1,1,1,1,1,1,1,1,1,1,1,1,1,1,1,1,1,1,1,1,1,1,1,1,1,1,1,1,1,1,1,1,
1,1,1,1,1,1,1,1,1,1,1,1,1,1,1,1,1,1,1,1,1,1,1,1,1,1,1,1,1,1,1,1,1,1,1,1,
1,1,1,1,1,1,1,1,1,1,1,1,1,1,1,1,1,1,1,1,1,1,1,1,1,1,1,1,1,1,1,1,1,1,1,1,
1,1,1,1,1,1,1,1,1,1,1,1,1,1,1,1,1,1,1,1,1,1,1,1,1,1,1,1,1,1,1,1,1,1,1,1,
1,1,1,1,1,1,1,1,1,1,1,1,1,1,1,1,1,1,1,1,1,1,1,1,1,1,1,1,1,1,1,1,1,1,1,6),
(2,2),(-1.,-0.995000000000001,-0.990000000000001,-0.985000000000001,-0.980000000000001,
-0.975000000000001,-0.970000000000001,-0.965000000000001,-0.960000000000001,
-0.955000000000001,-0.950000000000001,-0.945000000000001,-0.940000000000001,
-0.935000000000001,-0.930000000000001,-0.925000000000001,-0.920000000000001,
-0.915000000000001,-0.910000000000001,-0.905000000000001,-0.900000000000001,
-0.895000000000001,-0.890000000000001,-0.885000000000001,-0.880000000000001,
-0.875000000000001,-0.870000000000001,-0.865000000000001,-0.860000000000001,
-0.855000000000001,-0.850000000000001,-0.845000000000001,-0.840000000000001,
-0.835000000000001,-0.830000000000001,-0.825000000000001,-0.820000000000001,
-0.815000000000001,-0.810000000000001,-0.805000000000001,-0.800000000000001,
-0.795000000000001,-0.790000000000001,-0.785000000000001,-0.780000000000001,
-0.775000000000001,-0.770000000000001,-0.765000000000001,-0.760000000000001,
-0.755000000000001,-0.750000000000001,-0.745000000000001,-0.740000000000001,
-0.735000000000001,-0.730000000000001,-0.725000000000001,-0.720000000000001,
-0.715000000000001,-0.710000000000001,-0.705000000000001,-0.700000000000001,
-0.695000000000001,-0.690000000000001,-0.685,-0.68,-0.675,-0.67,-0.665,
-0.66,-0.655,-0.65,-0.645,-0.64,-0.635,-0.63,-0.625,-0.62,-0.615,-0.61,
-0.605,-0.6,-0.595,-0.59,-0.585,-0.58,-0.575,-0.57,-0.565,-0.56,-0.555,
-0.55,-0.545,-0.54,-0.535,-0.53,-0.525,-0.52,-0.515,-0.51,-0.505,-0.5,-0.495,
-0.49,-0.485,-0.48,-0.475,-0.47,-0.465,-0.46,-0.455,-0.45,-0.445,-0.44,
-0.435,-0.43,-0.425,-0.42,-0.415,-0.41,-0.405,-0.4,-0.395,-0.39,-0.385,
-0.38,-0.375,-0.37,-0.365,-0.36,-0.355,-0.35,-0.345,-0.34,-0.335,-0.33,
-0.325,-0.32,-0.315,-0.31,-0.305,-0.3,-0.295,-0.29,-0.285,-0.28,-0.275,
-0.27,-0.265,-0.26,-0.255,-0.25,-0.245,-0.24,-0.235,-0.23,-0.225,-0.22,
-0.215,-0.21,-0.205,-0.2,-0.195,-0.19,-0.185,-0.18,-0.175,-0.17,-0.165,
-0.16,-0.155,-0.15,-0.145,-0.14,-0.135,-0.13,-0.125,-0.12,-0.115,-0.11,
-0.105,-0.1,-0.095,-0.09,-0.085,-0.08,-0.075,-0.07,-0.065,-0.06,-0.055,
-0.05,-0.045,-0.04,-0.035,-0.03,-0.025,-0.02,-0.015,-0.01,-0.005,0.),(0.,
1.2),.UNSPECIFIED.)
GEOMETRIC_REPRESENTATION_ITEM()
RATIONAL_B_SPLINE_SURFACE(((1.,1.),(1.,1.),(1.,1.),(1.,1.),(1.,1.),(1.,
1.),(1.,1.),(1.,1.),(1.,1.),(1.,1.),(1.,1.),(1.,1.),(1.,1.),(1.,1.),(1.,
1.),(1.,1.),(1.,1.),(1.,1.),(1.,1.),(1.,1.),(1.,1.),(1.,1.),(1.,1.),(1.,
1.),(1.,1.),(1.,1.),(1.,1.),(1.,1.),(1.,1.),(1.,1.),(1.,1.),(1.,1.),(1.,
1.),(1.,1.),(1.,1.),(1.,1.),(1.,1.),(1.,1.),(1.,1.),(1.,1.),(1.,1.),(1.,
1.),(1.,1.),(1.,1.),(1.,1.),(1.,1.),(1.,1.),(1.,1.),(1.,1.),(1.,1.),(1.,
1.),(1.,1.),(1.,1.),(1.,1.),(1.,1.),(1.,1.),(1.,1.),(1.,1.),(1.,1.),(1.,
1.),(1.,1.),(1.,1.),(1.,1.),(1.,1.),(1.,1.),(1.,1.),(1.,1.),(1.,1.),(1.,
1.),(1.,1.),(1.,1.),(1.,1.),(1.,1.),(1.,1.),(1.,1.),(1.,1.),(1.,1.),(1.,
1.),(1.,1.),(1.,1.),(1.,1.),(1.,1.),(1.,1.),(1.,1.),(1.,1.),(1.,1.),(1.,
1.),(1.,1.),(1.,1.),(1.,1.),(1.,1.),(1.,1.),(1.,1.),(1.,1.),(1.,1.),(1.,
1.),(1.,1.),(1.,1.),(1.,1.),(1.,1.),(1.,1.),(1.,1.),(1.,1.),(1.,1.),(1.,
1.),(1.,1.),(1.,1.),(1.,1.),(1.,1.),(1.,1.),(1.,1.),(1.,1.),(1.,1.),(1.,
1.),(1.,1.),(1.,1.),(1.,1.),(1.,1.),(1.,1.),(1.,1.),(1.,1.),(1.,1.),(1.,
1.),(1.,1.),(1.,1.),(1.,1.),(1.,1.),(1.,1.),(1.,1.),(1.,1.),(1.,1.),(1.,
1.),(1.,1.),(1.,1.),(1.,1.),(1.,1.),(1.,1.),(1.,1.),(1.,1.),(1.,1.),(1.,
1.),(1.,1.),(1.,1.),(1.,1.),(1.,1.),(1.,1.),(1.,1.),(1.,1.),(1.,1.),(1.,
1.),(1.,1.),(1.,1.),(1.,1.),(1.,1.),(1.,1.),(1.,1.),(1.,1.),(1.,1.),(1.,
1.),(1.,1.),(1.,1.),(1.,1.),(1.,1.),(1.,1.),(1.,1.),(1.,1.),(1.,1.),(1.,
1.),(1.,1.),(1.,1.),(1.,1.),(1.,1.),(1.,1.),(1.,1.),(1.,1.),(1.,1.),(1.,
1.),(1.,1.),(1.,1.),(1.,1.),(1.,1.),(1.,1.),(1.,1.),(1.,1.),(1.,1.),(1.,
1.),(1.,1.),(1.,1.),(1.,1.),(1.,1.),(1.,1.),(1.,1.),(1.,1.),(1.,1.),(1.,
1.),(1.,1.),(1.,1.),(1.,1.),(1.,1.),(1.,1.),(1.,1.),(1.,1.),(1.,1.),(1.,
1.),(1.,1.)))
REPRESENTATION_ITEM('')
SURFACE()
);
#1122=(
BOUNDED_SURFACE()
B_SPLINE_SURFACE(5,1,((#255343,#255344),(#255345,#255346),(#255347,#255348),
(#255349,#255350),(#255351,#255352),(#255353,#255354),(#255355,#255356),
(#255357,#255358),(#255359,#255360),(#255361,#255362),(#255363,#255364),
(#255365,#255366),(#255367,#255368),(#255369,#255370),(#255371,#255372),
(#255373,#255374),(#255375,#255376),(#255377,#255378),(#255379,#255380),
(#255381,#255382),(#255383,#255384),(#255385,#255386),(#255387,#255388),
(#255389,#255390),(#255391,#255392),(#255393,#255394),(#255395,#255396),
(#255397,#255398),(#255399,#255400),(#255401,#255402),(#255403,#255404),
(#255405,#255406),(#255407,#255408),(#255409,#255410),(#255411,#255412),
(#255413,#255414),(#255415,#255416),(#255417,#255418),(#255419,#255420),
(#255421,#255422),(#255423,#255424),(#255425,#255426),(#255427,#255428),
(#255429,#255430),(#255431,#255432),(#255433,#255434),(#255435,#255436),
(#255437,#255438),(#255439,#255440),(#255441,#255442),(#255443,#255444),
(#255445,#255446),(#255447,#255448),(#255449,#255450),(#255451,#255452),
(#255453,#255454),(#255455,#255456),(#255457,#255458),(#255459,#255460),
(#255461,#255462),(#255463,#255464),(#255465,#255466),(#255467,#255468),
(#255469,#255470),(#255471,#255472),(#255473,#255474),(#255475,#255476),
(#255477,#255478),(#255479,#255480),(#255481,#255482),(#255483,#255484),
(#255485,#255486),(#255487,#255488),(#255489,#255490),(#255491,#255492),
(#255493,#255494),(#255495,#255496),(#255497,#255498),(#255499,#255500),
(#255501,#255502),(#255503,#255504),(#255505,#255506),(#255507,#255508),
(#255509,#255510),(#255511,#255512),(#255513,#255514),(#255515,#255516),
(#255517,#255518),(#255519,#255520),(#255521,#255522),(#255523,#255524),
(#255525,#255526),(#255527,#255528),(#255529,#255530),(#255531,#255532),
(#255533,#255534),(#255535,#255536),(#255537,#255538),(#255539,#255540),
(#255541,#255542),(#255543,#255544),(#255545,#255546),(#255547,#255548),
(#255549,#255550),(#255551,#255552),(#255553,#255554),(#255555,#255556),
(#255557,#255558),(#255559,#255560),(#255561,#255562),(#255563,#255564),
(#255565,#255566),(#255567,#255568),(#255569,#255570),(#255571,#255572),
(#255573,#255574),(#255575,#255576),(#255577,#255578),(#255579,#255580),
(#255581,#255582),(#255583,#255584),(#255585,#255586),(#255587,#255588),
(#255589,#255590),(#255591,#255592),(#255593,#255594),(#255595,#255596),
(#255597,#255598),(#255599,#255600),(#255601,#255602),(#255603,#255604),
(#255605,#255606),(#255607,#255608),(#255609,#255610),(#255611,#255612),
(#255613,#255614),(#255615,#255616),(#255617,#255618),(#255619,#255620),
(#255621,#255622),(#255623,#255624),(#255625,#255626),(#255627,#255628),
(#255629,#255630),(#255631,#255632),(#255633,#255634),(#255635,#255636),
(#255637,#255638),(#255639,#255640),(#255641,#255642),(#255643,#255644),
(#255645,#255646),(#255647,#255648),(#255649,#255650),(#255651,#255652),
(#255653,#255654),(#255655,#255656),(#255657,#255658),(#255659,#255660),
(#255661,#255662),(#255663,#255664),(#255665,#255666),(#255667,#255668),
(#255669,#255670),(#255671,#255672),(#255673,#255674),(#255675,#255676),
(#255677,#255678),(#255679,#255680),(#255681,#255682),(#255683,#255684),
(#255685,#255686),(#255687,#255688),(#255689,#255690),(#255691,#255692),
(#255693,#255694),(#255695,#255696),(#255697,#255698),(#255699,#255700),
(#255701,#255702),(#255703,#255704),(#255705,#255706),(#255707,#255708),
(#255709,#255710),(#255711,#255712),(#255713,#255714),(#255715,#255716),
(#255717,#255718),(#255719,#255720),(#255721,#255722),(#255723,#255724),
(#255725,#255726),(#255727,#255728),(#255729,#255730),(#255731,#255732),
(#255733,#255734),(#255735,#255736),(#255737,#255738),(#255739,#255740),
(#255741,#255742),(#255743,#255744),(#255745,#255746),(#255747,#255748),
(#255749,#255750),(#255751,#255752)),.UNSPECIFIED.,.F.,.F.,.F.)
B_SPLINE_SURFACE_WITH_KNOTS((6,1,1,1,1,1,1,1,1,1,1,1,1,1,1,1,1,1,1,1,1,
1,1,1,1,1,1,1,1,1,1,1,1,1,1,1,1,1,1,1,1,1,1,1,1,1,1,1,1,1,1,1,1,1,1,1,1,
1,1,1,1,1,1,1,1,1,1,1,1,1,1,1,1,1,1,1,1,1,1,1,1,1,1,1,1,1,1,1,1,1,1,1,1,
1,1,1,1,1,1,1,1,1,1,1,1,1,1,1,1,1,1,1,1,1,1,1,1,1,1,1,1,1,1,1,1,1,1,1,1,
1,1,1,1,1,1,1,1,1,1,1,1,1,1,1,1,1,1,1,1,1,1,1,1,1,1,1,1,1,1,1,1,1,1,1,1,
1,1,1,1,1,1,1,1,1,1,1,1,1,1,1,1,1,1,1,1,1,1,1,1,1,1,1,1,1,1,1,1,1,1,1,6),
(2,2),(0.,0.005,0.01,0.015,0.02,0.025,0.03,0.035,0.04,0.045,0.05,0.055,
0.06,0.065,0.07,0.075,0.08,0.085,0.09,0.095,0.1,0.105,0.11,0.115,0.12,0.125,
0.13,0.135,0.14,0.145,0.15,0.155,0.16,0.165,0.17,0.175,0.18,0.185,0.19,
0.195,0.2,0.205,0.21,0.215,0.22,0.225,0.23,0.235,0.24,0.245,0.25,0.255,
0.26,0.265,0.27,0.275,0.28,0.285,0.29,0.295,0.3,0.305,0.31,0.315,0.32,0.325,
0.33,0.335,0.34,0.345,0.35,0.355,0.36,0.365,0.37,0.375,0.38,0.385,0.39,
0.395,0.4,0.405,0.41,0.415,0.42,0.425,0.43,0.435,0.44,0.445,0.45,0.455,
0.46,0.465,0.47,0.475,0.48,0.485,0.49,0.495,0.5,0.505,0.51,0.515,0.52,0.525,
0.53,0.535,0.54,0.545,0.55,0.555,0.56,0.565,0.57,0.575,0.58,0.585,0.59,
0.595,0.6,0.605,0.61,0.615,0.62,0.625,0.63,0.635,0.64,0.645,0.65,0.655,
0.66,0.665,0.67,0.675,0.68,0.685,0.690000000000001,0.695000000000001,0.700000000000001,
0.705000000000001,0.710000000000001,0.715000000000001,0.720000000000001,
0.725000000000001,0.730000000000001,0.735000000000001,0.740000000000001,
0.745000000000001,0.750000000000001,0.755000000000001,0.760000000000001,
0.765000000000001,0.770000000000001,0.775000000000001,0.780000000000001,
0.785000000000001,0.790000000000001,0.795000000000001,0.800000000000001,
0.805000000000001,0.810000000000001,0.815000000000001,0.820000000000001,
0.825000000000001,0.830000000000001,0.835000000000001,0.840000000000001,
0.845000000000001,0.850000000000001,0.855000000000001,0.860000000000001,
0.865000000000001,0.870000000000001,0.875000000000001,0.880000000000001,
0.885000000000001,0.890000000000001,0.895000000000001,0.900000000000001,
0.905000000000001,0.910000000000001,0.915000000000001,0.920000000000001,
0.925000000000001,0.930000000000001,0.935000000000001,0.940000000000001,
0.945000000000001,0.950000000000001,0.955000000000001,0.960000000000001,
0.965000000000001,0.970000000000001,0.975000000000001,0.980000000000001,
0.985000000000001,0.990000000000001,0.995000000000001,1.),(0.,1.2),
 .UNSPECIFIED.)
GEOMETRIC_REPRESENTATION_ITEM()
RATIONAL_B_SPLINE_SURFACE(((1.,1.),(1.,1.),(1.,1.),(1.,1.),(1.,1.),(1.,
1.),(1.,1.),(1.,1.),(1.,1.),(1.,1.),(1.,1.),(1.,1.),(1.,1.),(1.,1.),(1.,
1.),(1.,1.),(1.,1.),(1.,1.),(1.,1.),(1.,1.),(1.,1.),(1.,1.),(1.,1.),(1.,
1.),(1.,1.),(1.,1.),(1.,1.),(1.,1.),(1.,1.),(1.,1.),(1.,1.),(1.,1.),(1.,
1.),(1.,1.),(1.,1.),(1.,1.),(1.,1.),(1.,1.),(1.,1.),(1.,1.),(1.,1.),(1.,
1.),(1.,1.),(1.,1.),(1.,1.),(1.,1.),(1.,1.),(1.,1.),(1.,1.),(1.,1.),(1.,
1.),(1.,1.),(1.,1.),(1.,1.),(1.,1.),(1.,1.),(1.,1.),(1.,1.),(1.,1.),(1.,
1.),(1.,1.),(1.,1.),(1.,1.),(1.,1.),(1.,1.),(1.,1.),(1.,1.),(1.,1.),(1.,
1.),(1.,1.),(1.,1.),(1.,1.),(1.,1.),(1.,1.),(1.,1.),(1.,1.),(1.,1.),(1.,
1.),(1.,1.),(1.,1.),(1.,1.),(1.,1.),(1.,1.),(1.,1.),(1.,1.),(1.,1.),(1.,
1.),(1.,1.),(1.,1.),(1.,1.),(1.,1.),(1.,1.),(1.,1.),(1.,1.),(1.,1.),(1.,
1.),(1.,1.),(1.,1.),(1.,1.),(1.,1.),(1.,1.),(1.,1.),(1.,1.),(1.,1.),(1.,
1.),(1.,1.),(1.,1.),(1.,1.),(1.,1.),(1.,1.),(1.,1.),(1.,1.),(1.,1.),(1.,
1.),(1.,1.),(1.,1.),(1.,1.),(1.,1.),(1.,1.),(1.,1.),(1.,1.),(1.,1.),(1.,
1.),(1.,1.),(1.,1.),(1.,1.),(1.,1.),(1.,1.),(1.,1.),(1.,1.),(1.,1.),(1.,
1.),(1.,1.),(1.,1.),(1.,1.),(1.,1.),(1.,1.),(1.,1.),(1.,1.),(1.,1.),(1.,
1.),(1.,1.),(1.,1.),(1.,1.),(1.,1.),(1.,1.),(1.,1.),(1.,1.),(1.,1.),(1.,
1.),(1.,1.),(1.,1.),(1.,1.),(1.,1.),(1.,1.),(1.,1.),(1.,1.),(1.,1.),(1.,
1.),(1.,1.),(1.,1.),(1.,1.),(1.,1.),(1.,1.),(1.,1.),(1.,1.),(1.,1.),(1.,
1.),(1.,1.),(1.,1.),(1.,1.),(1.,1.),(1.,1.),(1.,1.),(1.,1.),(1.,1.),(1.,
1.),(1.,1.),(1.,1.),(1.,1.),(1.,1.),(1.,1.),(1.,1.),(1.,1.),(1.,1.),(1.,
1.),(1.,1.),(1.,1.),(1.,1.),(1.,1.),(1.,1.),(1.,1.),(1.,1.),(1.,1.),(1.,
1.),(1.,1.),(1.,1.),(1.,1.),(1.,1.),(1.,1.),(1.,1.),(1.,1.),(1.,1.),(1.,
1.),(1.,1.)))
REPRESENTATION_ITEM('')
SURFACE()
);
#1123=SHAPE_REPRESENTATION_RELATIONSHIP('SRR','None',#259370,#1143);
#1124=SHAPE_REPRESENTATION_RELATIONSHIP('SRR','None',#259371,#1144);
#1125=SHAPE_REPRESENTATION_RELATIONSHIP('SRR','None',#259372,#1145);
#1126=SHAPE_REPRESENTATION_RELATIONSHIP('SRR','None',#259373,#1146);
#1127=SHAPE_REPRESENTATION_RELATIONSHIP('SRR','None',#259374,#1147);
#1128=SHAPE_REPRESENTATION_RELATIONSHIP('SRR','None',#259375,#1148);
#1129=SHAPE_REPRESENTATION_RELATIONSHIP('SRR','None',#259376,#1149);
#1130=SHAPE_REPRESENTATION_RELATIONSHIP('SRR','None',#259377,#1150);
#1131=SHAPE_REPRESENTATION_RELATIONSHIP('SRR','None',#259378,#1151);
#1132=SHAPE_REPRESENTATION_RELATIONSHIP('SRR','None',#259379,#1152);
#1133=SHAPE_REPRESENTATION_RELATIONSHIP('SRR','None',#259380,#1153);
#1134=SHAPE_REPRESENTATION_RELATIONSHIP('SRR','None',#259381,#1154);
#1135=SHAPE_REPRESENTATION_RELATIONSHIP('SRR','None',#259382,#1155);
#1136=SHAPE_REPRESENTATION_RELATIONSHIP('SRR','None',#259383,#1156);
#1137=SHAPE_REPRESENTATION_RELATIONSHIP('SRR','None',#259384,#1157);
#1138=SHAPE_REPRESENTATION_RELATIONSHIP('SRR','None',#259385,#1158);
#1139=SHAPE_REPRESENTATION_RELATIONSHIP('SRR','None',#259386,#1159);
#1140=SHAPE_REPRESENTATION_RELATIONSHIP('SRR','None',#259387,#1160);
#1141=SHAPE_REPRESENTATION_RELATIONSHIP('SRR','None',#259388,#1161);
#1142=SHAPE_REPRESENTATION_RELATIONSHIP('SRR','None',#259389,#1162);
#1143=ADVANCED_BREP_SHAPE_REPRESENTATION('',(#1183),#259204);
#1144=ADVANCED_BREP_SHAPE_REPRESENTATION('',(#1184),#259205);
#1145=ADVANCED_BREP_SHAPE_REPRESENTATION('',(#1185),#259206);
#1146=ADVANCED_BREP_SHAPE_REPRESENTATION('',(#1186),#259207);
#1147=ADVANCED_BREP_SHAPE_REPRESENTATION('',(#1187),#259208);
#1148=ADVANCED_BREP_SHAPE_REPRESENTATION('',(#1188),#259209);
#1149=ADVANCED_BREP_SHAPE_REPRESENTATION('',(#1189),#259210);
#1150=ADVANCED_BREP_SHAPE_REPRESENTATION('',(#1190),#259211);
#1151=ADVANCED_BREP_SHAPE_REPRESENTATION('',(#1191),#259212);
#1152=ADVANCED_BREP_SHAPE_REPRESENTATION('',(#1192),#259213);
#1153=ADVANCED_BREP_SHAPE_REPRESENTATION('',(#1193),#259214);
#1154=ADVANCED_BREP_SHAPE_REPRESENTATION('',(#1194),#259215);
#1155=ADVANCED_BREP_SHAPE_REPRESENTATION('',(#1195),#259216);
#1156=ADVANCED_BREP_SHAPE_REPRESENTATION('',(#1196),#259217);
#1157=ADVANCED_BREP_SHAPE_REPRESENTATION('',(#1197),#259218);
#1158=ADVANCED_BREP_SHAPE_REPRESENTATION('',(#1198),#259219);
#1159=ADVANCED_BREP_SHAPE_REPRESENTATION('',(#1199),#259220);
#1160=ADVANCED_BREP_SHAPE_REPRESENTATION('',(#1200),#259221);
#1161=ADVANCED_BREP_SHAPE_REPRESENTATION('',(#1201),#259222);
#1162=ADVANCED_BREP_SHAPE_REPRESENTATION('',(#1202),#259223);
#1163=STYLED_ITEM('',(#259479),#1183);
#1164=STYLED_ITEM('',(#259480),#1184);
#1165=STYLED_ITEM('',(#259481),#1185);
#1166=STYLED_ITEM('',(#259482),#1186);
#1167=STYLED_ITEM('',(#259483),#1187);
#1168=STYLED_ITEM('',(#259484),#1188);
#1169=STYLED_ITEM('',(#259484),#1189);
#1170=STYLED_ITEM('',(#259485),#1190);
#1171=STYLED_ITEM('',(#259486),#1191);
#1172=STYLED_ITEM('',(#259487),#1192);
#1173=STYLED_ITEM('',(#259485),#1193);
#1174=STYLED_ITEM('',(#259488),#1194);
#1175=STYLED_ITEM('',(#259489),#1195);
#1176=STYLED_ITEM('',(#259490),#1196);
#1177=STYLED_ITEM('',(#259485),#1197);
#1178=STYLED_ITEM('',(#259485),#1198);
#1179=STYLED_ITEM('',(#259489),#1199);
#1180=STYLED_ITEM('',(#259489),#1200);
#1181=STYLED_ITEM('',(#259491),#1201);
#1182=STYLED_ITEM('',(#259492),#1202);
#1183=MANIFOLD_SOLID_BREP('Body1',#25150);
#1184=MANIFOLD_SOLID_BREP('Body1',#25151);
#1185=MANIFOLD_SOLID_BREP('Body1',#25152);
#1186=MANIFOLD_SOLID_BREP('Body1',#25153);
#1187=MANIFOLD_SOLID_BREP('Gear blank',#25154);
#1188=MANIFOLD_SOLID_BREP('Gear blank',#25155);
#1189=MANIFOLD_SOLID_BREP('Gear blank',#25156);
#1190=MANIFOLD_SOLID_BREP('Body1',#25157);
#1191=MANIFOLD_SOLID_BREP('Body1',#25158);
#1192=MANIFOLD_SOLID_BREP('Body1',#25159);
#1193=MANIFOLD_SOLID_BREP('Body1',#25160);
#1194=MANIFOLD_SOLID_BREP('Body1',#25161);
#1195=MANIFOLD_SOLID_BREP('Body1',#25162);
#1196=MANIFOLD_SOLID_BREP('Body1',#25163);
#1197=MANIFOLD_SOLID_BREP('Body1',#25164);
#1198=MANIFOLD_SOLID_BREP('Body1',#25165);
#1199=MANIFOLD_SOLID_BREP('Body1',#25166);
#1200=MANIFOLD_SOLID_BREP('Body1',#25167);
#1201=MANIFOLD_SOLID_BREP('Body1',#25168);
#1202=MANIFOLD_SOLID_BREP('Socket head cap screw M6x20',#25169);
#1203=FACE_BOUND('',#3350,.T.);
#1204=FACE_BOUND('',#3352,.T.);
#1205=FACE_BOUND('',#3353,.T.);
#1206=FACE_BOUND('',#3354,.T.);
#1207=FACE_BOUND('',#3355,.T.);
#1208=FACE_BOUND('',#3356,.T.);
#1209=FACE_BOUND('',#3357,.T.);
#1210=FACE_BOUND('',#3358,.T.);
#1211=FACE_BOUND('',#3359,.T.);
#1212=FACE_BOUND('',#3360,.T.);
#1213=FACE_BOUND('',#3362,.T.);
#1214=FACE_BOUND('',#3363,.T.);
#1215=FACE_BOUND('',#3364,.T.);
#1216=FACE_BOUND('',#3365,.T.);
#1217=FACE_BOUND('',#3366,.T.);
#1218=FACE_BOUND('',#3367,.T.);
#1219=FACE_BOUND('',#3368,.T.);
#1220=FACE_BOUND('',#3369,.T.);
#1221=FACE_BOUND('',#3370,.T.);
#1222=FACE_BOUND('',#3372,.T.);
#1223=FACE_BOUND('',#3373,.T.);
#1224=FACE_BOUND('',#3374,.T.);
#1225=FACE_BOUND('',#3375,.T.);
#1226=FACE_BOUND('',#3376,.T.);
#1227=FACE_BOUND('',#3377,.T.);
#1228=FACE_BOUND('',#3378,.T.);
#1229=FACE_BOUND('',#3379,.T.);
#1230=FACE_BOUND('',#3380,.T.);
#1231=FACE_BOUND('',#3382,.T.);
#1232=FACE_BOUND('',#3383,.T.);
#1233=FACE_BOUND('',#3384,.T.);
#1234=FACE_BOUND('',#3385,.T.);
#1235=FACE_BOUND('',#3386,.T.);
#1236=FACE_BOUND('',#3390,.T.);
#1237=FACE_BOUND('',#3392,.T.);
#1238=FACE_BOUND('',#3393,.T.);
#1239=FACE_BOUND('',#3394,.T.);
#1240=FACE_BOUND('',#3395,.T.);
#1241=FACE_BOUND('',#3396,.T.);
#1242=FACE_BOUND('',#3407,.T.);
#1243=FACE_BOUND('',#3408,.T.);
#1244=FACE_BOUND('',#3409,.T.);
#1245=FACE_BOUND('',#3411,.T.);
#1246=FACE_BOUND('',#3413,.T.);
#1247=FACE_BOUND('',#3425,.T.);
#1248=FACE_BOUND('',#3426,.T.);
#1249=FACE_BOUND('',#3427,.T.);
#1250=FACE_BOUND('',#3428,.T.);
#1251=FACE_BOUND('',#3429,.T.);
#1252=FACE_BOUND('',#3430,.T.);
#1253=FACE_BOUND('',#3431,.T.);
#1254=FACE_BOUND('',#3432,.T.);
#1255=FACE_BOUND('',#3433,.T.);
#1256=FACE_BOUND('',#3435,.T.);
#1257=FACE_BOUND('',#3436,.T.);
#1258=FACE_BOUND('',#3437,.T.);
#1259=FACE_BOUND('',#3438,.T.);
#1260=FACE_BOUND('',#3439,.T.);
#1261=FACE_BOUND('',#3440,.T.);
#1262=FACE_BOUND('',#3441,.T.);
#1263=FACE_BOUND('',#3442,.T.);
#1264=FACE_BOUND('',#3443,.T.);
#1265=FACE_BOUND('',#3451,.T.);
#1266=FACE_BOUND('',#3453,.T.);
#1267=FACE_BOUND('',#3457,.T.);
#1268=FACE_BOUND('',#3459,.T.);
#1269=FACE_BOUND('',#3462,.T.);
#1270=FACE_BOUND('',#3464,.T.);
#1271=FACE_BOUND('',#3468,.T.);
#1272=FACE_BOUND('',#3470,.T.);
#1273=FACE_BOUND('',#3474,.T.);
#1274=FACE_BOUND('',#3480,.T.);
#1275=FACE_BOUND('',#3482,.T.);
#1276=FACE_BOUND('',#3923,.T.);
#1277=FACE_BOUND('',#3926,.T.);
#1278=FACE_BOUND('',#3927,.T.);
#1279=FACE_BOUND('',#3928,.T.);
#1280=FACE_BOUND('',#3930,.T.);
#1281=FACE_BOUND('',#3936,.T.);
#1282=FACE_BOUND('',#4099,.T.);
#1283=FACE_BOUND('',#4293,.T.);
#1284=FACE_BOUND('',#4295,.T.);
#1285=FACE_BOUND('',#4331,.T.);
#1286=FACE_BOUND('',#4333,.T.);
#1287=FACE_BOUND('',#4341,.T.);
#1288=FACE_BOUND('',#4343,.T.);
#1289=FACE_BOUND('',#4347,.T.);
#1290=FACE_BOUND('',#4349,.T.);
#1291=FACE_BOUND('',#4355,.T.);
#1292=FACE_BOUND('',#4357,.T.);
#1293=FACE_BOUND('',#4361,.T.);
#1294=FACE_BOUND('',#4364,.T.);
#1295=FACE_BOUND('',#4366,.T.);
#1296=FACE_BOUND('',#4372,.T.);
#1297=FACE_BOUND('',#4376,.T.);
#1298=FACE_BOUND('',#4377,.T.);
#1299=FACE_BOUND('',#4378,.T.);
#1300=FACE_BOUND('',#4379,.T.);
#1301=FACE_BOUND('',#4381,.T.);
#1302=FACE_BOUND('',#4382,.T.);
#1303=FACE_BOUND('',#4383,.T.);
#1304=FACE_BOUND('',#4384,.T.);
#1305=FACE_BOUND('',#4394,.T.);
#1306=FACE_BOUND('',#4396,.T.);
#1307=FACE_BOUND('',#4399,.T.);
#1308=FACE_BOUND('',#4401,.T.);
#1309=FACE_BOUND('',#4404,.T.);
#1310=FACE_BOUND('',#4418,.T.);
#1311=FACE_BOUND('',#4420,.T.);
#1312=FACE_BOUND('',#4424,.T.);
#1313=FACE_BOUND('',#4426,.T.);
#1314=FACE_BOUND('',#4430,.T.);
#1315=FACE_BOUND('',#4432,.T.);
#1316=FACE_BOUND('',#4500,.T.);
#1317=FACE_BOUND('',#4503,.T.);
#1318=B_SPLINE_SURFACE_WITH_KNOTS('',3,3,((#42197,#42198,#42199,#42200,
#42201,#42202,#42203,#42204,#42205,#42206,#42207,#42208,#42209,#42210,#42211,
#42212,#42213,#42214,#42215,#42216,#42217,#42218,#42219,#42220,#42221,#42222,
#42223,#42224,#42225,#42226,#42227,#42228,#42229,#42230,#42231,#42232,#42233,
#42234,#42235,#42236,#42237,#42238,#42239,#42240,#42241,#42242,#42243,#42244,
#42245,#42246,#42247,#42248,#42249,#42250,#42251,#42252,#42253,#42254,#42255,
#42256,#42257,#42258,#42259,#42260,#42261,#42262,#42263,#42264,#42265,#42266,
#42267,#42268,#42269,#42270,#42271,#42272,#42273,#42274,#42275,#42276,#42277,
#42278,#42279,#42280,#42281,#42282,#42283,#42284,#42285,#42286,#42287,#42288,
#42289,#42290,#42291,#42292,#42293,#42294,#42295,#42296),(#42297,#42298,
#42299,#42300,#42301,#42302,#42303,#42304,#42305,#42306,#42307,#42308,#42309,
#42310,#42311,#42312,#42313,#42314,#42315,#42316,#42317,#42318,#42319,#42320,
#42321,#42322,#42323,#42324,#42325,#42326,#42327,#42328,#42329,#42330,#42331,
#42332,#42333,#42334,#42335,#42336,#42337,#42338,#42339,#42340,#42341,#42342,
#42343,#42344,#42345,#42346,#42347,#42348,#42349,#42350,#42351,#42352,#42353,
#42354,#42355,#42356,#42357,#42358,#42359,#42360,#42361,#42362,#42363,#42364,
#42365,#42366,#42367,#42368,#42369,#42370,#42371,#42372,#42373,#42374,#42375,
#42376,#42377,#42378,#42379,#42380,#42381,#42382,#42383,#42384,#42385,#42386,
#42387,#42388,#42389,#42390,#42391,#42392,#42393,#42394,#42395,#42396),
(#42397,#42398,#42399,#42400,#42401,#42402,#42403,#42404,#42405,#42406,
#42407,#42408,#42409,#42410,#42411,#42412,#42413,#42414,#42415,#42416,#42417,
#42418,#42419,#42420,#42421,#42422,#42423,#42424,#42425,#42426,#42427,#42428,
#42429,#42430,#42431,#42432,#42433,#42434,#42435,#42436,#42437,#42438,#42439,
#42440,#42441,#42442,#42443,#42444,#42445,#42446,#42447,#42448,#42449,#42450,
#42451,#42452,#42453,#42454,#42455,#42456,#42457,#42458,#42459,#42460,#42461,
#42462,#42463,#42464,#42465,#42466,#42467,#42468,#42469,#42470,#42471,#42472,
#42473,#42474,#42475,#42476,#42477,#42478,#42479,#42480,#42481,#42482,#42483,
#42484,#42485,#42486,#42487,#42488,#42489,#42490,#42491,#42492,#42493,#42494,
#42495,#42496),(#42497,#42498,#42499,#42500,#42501,#42502,#42503,#42504,
#42505,#42506,#42507,#42508,#42509,#42510,#42511,#42512,#42513,#42514,#42515,
#42516,#42517,#42518,#42519,#42520,#42521,#42522,#42523,#42524,#42525,#42526,
#42527,#42528,#42529,#42530,#42531,#42532,#42533,#42534,#42535,#42536,#42537,
#42538,#42539,#42540,#42541,#42542,#42543,#42544,#42545,#42546,#42547,#42548,
#42549,#42550,#42551,#42552,#42553,#42554,#42555,#42556,#42557,#42558,#42559,
#42560,#42561,#42562,#42563,#42564,#42565,#42566,#42567,#42568,#42569,#42570,
#42571,#42572,#42573,#42574,#42575,#42576,#42577,#42578,#42579,#42580,#42581,
#42582,#42583,#42584,#42585,#42586,#42587,#42588,#42589,#42590,#42591,#42592,
#42593,#42594,#42595,#42596)),.UNSPECIFIED.,.F.,.F.,.F.,(4,4),(4,1,1,1,
1,1,1,1,1,1,1,1,1,1,1,1,1,1,1,1,1,1,1,1,1,1,1,1,1,1,1,1,1,1,1,1,1,1,1,1,
1,1,1,1,1,1,1,1,1,1,1,1,1,1,1,1,1,1,1,1,1,1,1,1,1,1,1,1,1,1,1,1,1,1,1,1,
1,1,1,1,1,1,1,1,1,1,1,1,1,1,1,1,1,1,1,1,1,4),(0.,0.064201349933887),(11.8589888623077,
12.8514087025213,13.843828542735,14.8362483829486,15.8286682231622,16.8210880633759,
17.8135079035895,18.8059277438031,19.7983475840168,20.7907674242304,21.783187264444,
22.7756071046577,23.7680269448713,24.7604467850849,25.7528666252985,26.7452864655122,
27.7377063057258,28.7301261459394,29.7225459861531,30.7149658263667,31.7073856665803,
32.699805506794,33.6922253470076,34.6846451872212,35.6770650274349,36.6694848676485,
37.6619047078621,38.6543245480758,39.6467443882894,40.639164228503,41.6315840687166,
42.6240039089303,43.6164237491439,44.6088435893575,45.6012634295712,46.5936832697848,
47.5861031099984,48.5785229502121,49.5709427904257,50.5633626306393,51.555782470853,
52.5482023110666,53.5406221512802,54.5330419914939,55.5254618317075,56.5178816719211,
57.5103015121348,58.5027213523484,59.495141192562,60.4875610327756,61.4799808729893,
62.4724007132029,63.4648205534165,64.4572403936302,65.4496602338438,66.4420800740574,
67.4344999142711,68.4269197544847,69.4193395946983,70.411759434912,71.4041792751256,
72.3965991153392,73.3890189555529,74.3814387957665,75.3738586359801,76.3662784761938,
77.3586983164074,78.351118156621,79.3435379968347,80.3359578370483,81.3283776772619,
82.3207975174756,83.3132173576892,84.3056371979028,85.2980570381164,86.2904768783301,
87.2828967185437,88.2753165587573,89.267736398971,90.2601562391846,91.2525760793982,
92.2449959196119,93.2374157598255,94.2298356000391,95.2222554402528,96.2146752804664,
97.20709512068,98.1995149608937,99.1919348011073,100.184354641321,101.176774481535,
102.169194321748,103.161614161962,104.154034002175,105.146453842389,106.138873682603,
107.131293522816,108.12371336303),.UNSPECIFIED.);
#1319=B_SPLINE_SURFACE_WITH_KNOTS('',3,3,((#42716,#42717,#42718,#42719,
#42720,#42721,#42722,#42723,#42724,#42725,#42726,#42727,#42728,#42729,#42730,
#42731,#42732,#42733,#42734,#42735,#42736,#42737,#42738,#42739,#42740,#42741,
#42742,#42743,#42744,#42745,#42746,#42747,#42748,#42749,#42750,#42751,#42752,
#42753,#42754,#42755,#42756,#42757,#42758,#42759,#42760,#42761,#42762,#42763,
#42764,#42765,#42766,#42767,#42768,#42769,#42770,#42771,#42772,#42773,#42774,
#42775,#42776,#42777,#42778,#42779,#42780,#42781,#42782,#42783,#42784,#42785,
#42786,#42787,#42788,#42789,#42790,#42791,#42792,#42793,#42794,#42795,#42796,
#42797,#42798,#42799,#42800,#42801,#42802,#42803,#42804,#42805,#42806,#42807,
#42808,#42809,#42810,#42811,#42812,#42813,#42814,#42815),(#42816,#42817,
#42818,#42819,#42820,#42821,#42822,#42823,#42824,#42825,#42826,#42827,#42828,
#42829,#42830,#42831,#42832,#42833,#42834,#42835,#42836,#42837,#42838,#42839,
#42840,#42841,#42842,#42843,#42844,#42845,#42846,#42847,#42848,#42849,#42850,
#42851,#42852,#42853,#42854,#42855,#42856,#42857,#42858,#42859,#42860,#42861,
#42862,#42863,#42864,#42865,#42866,#42867,#42868,#42869,#42870,#42871,#42872,
#42873,#42874,#42875,#42876,#42877,#42878,#42879,#42880,#42881,#42882,#42883,
#42884,#42885,#42886,#42887,#42888,#42889,#42890,#42891,#42892,#42893,#42894,
#42895,#42896,#42897,#42898,#42899,#42900,#42901,#42902,#42903,#42904,#42905,
#42906,#42907,#42908,#42909,#42910,#42911,#42912,#42913,#42914,#42915),
(#42916,#42917,#42918,#42919,#42920,#42921,#42922,#42923,#42924,#42925,
#42926,#42927,#42928,#42929,#42930,#42931,#42932,#42933,#42934,#42935,#42936,
#42937,#42938,#42939,#42940,#42941,#42942,#42943,#42944,#42945,#42946,#42947,
#42948,#42949,#42950,#42951,#42952,#42953,#42954,#42955,#42956,#42957,#42958,
#42959,#42960,#42961,#42962,#42963,#42964,#42965,#42966,#42967,#42968,#42969,
#42970,#42971,#42972,#42973,#42974,#42975,#42976,#42977,#42978,#42979,#42980,
#42981,#42982,#42983,#42984,#42985,#42986,#42987,#42988,#42989,#42990,#42991,
#42992,#42993,#42994,#42995,#42996,#42997,#42998,#42999,#43000,#43001,#43002,
#43003,#43004,#43005,#43006,#43007,#43008,#43009,#43010,#43011,#43012,#43013,
#43014,#43015),(#43016,#43017,#43018,#43019,#43020,#43021,#43022,#43023,
#43024,#43025,#43026,#43027,#43028,#43029,#43030,#43031,#43032,#43033,#43034,
#43035,#43036,#43037,#43038,#43039,#43040,#43041,#43042,#43043,#43044,#43045,
#43046,#43047,#43048,#43049,#43050,#43051,#43052,#43053,#43054,#43055,#43056,
#43057,#43058,#43059,#43060,#43061,#43062,#43063,#43064,#43065,#43066,#43067,
#43068,#43069,#43070,#43071,#43072,#43073,#43074,#43075,#43076,#43077,#43078,
#43079,#43080,#43081,#43082,#43083,#43084,#43085,#43086,#43087,#43088,#43089,
#43090,#43091,#43092,#43093,#43094,#43095,#43096,#43097,#43098,#43099,#43100,
#43101,#43102,#43103,#43104,#43105,#43106,#43107,#43108,#43109,#43110,#43111,
#43112,#43113,#43114,#43115)),.UNSPECIFIED.,.F.,.F.,.F.,(4,4),(4,1,1,1,
1,1,1,1,1,1,1,1,1,1,1,1,1,1,1,1,1,1,1,1,1,1,1,1,1,1,1,1,1,1,1,1,1,1,1,1,
1,1,1,1,1,1,1,1,1,1,1,1,1,1,1,1,1,1,1,1,1,1,1,1,1,1,1,1,1,1,1,1,1,1,1,1,
1,1,1,1,1,1,1,1,1,1,1,1,1,1,1,1,1,1,1,1,1,4),(0.,0.064201349933887),(14.3984001269718,
15.3908199671854,16.3832398073991,17.3756596476127,18.3680794878263,19.36049932804,
20.3529191682536,21.3453390084672,22.3377588486809,23.3301786888945,24.3225985291081,
25.3150183693218,26.3074382095354,27.299858049749,28.2922778899627,29.2846977301763,
30.2771175703899,31.2695374106036,32.2619572508172,33.2543770910308,34.2467969312444,
35.2392167714581,36.2316366116717,37.2240564518853,38.216476292099,39.2088961323126,
40.2013159725262,41.1937358127399,42.1861556529535,43.1785754931671,44.1709953333808,
45.1634151735944,46.155835013808,47.1482548540217,48.1406746942353,49.1330945344489,
50.1255143746626,51.1179342148762,52.1103540550898,53.1027738953035,54.0951937355171,
55.0876135757307,56.0800334159443,57.072453256158,58.0648730963716,59.0572929365852,
60.0497127767989,61.0421326170125,62.0345524572261,63.0269722974398,64.0193921376534,
65.011811977867,66.0042318180807,66.9966516582943,67.9890714985079,68.9814913387216,
69.9739111789352,70.9663310191488,71.9587508593625,72.9511706995761,73.9435905397897,
74.9360103800034,75.928430220217,76.9208500604306,77.9132699006443,78.9056897408579,
79.8981095810715,80.8905294212852,81.8829492614988,82.8753691017124,83.867788941926,
84.8602087821397,85.8526286223533,86.8450484625669,87.8374683027806,88.8298881429942,
89.8223079832078,90.8147278234215,91.8071476636351,92.7995675038487,93.7919873440624,
94.784407184276,95.7768270244896,96.7692468647032,97.7616667049169,98.7540865451305,
99.7465063853441,100.738926225558,101.731346065771,102.723765905985,103.716185746199,
104.708605586412,105.701025426626,106.69344526684,107.685865107053,108.678284947267,
109.67070478748,110.663124627694),.UNSPECIFIED.);
#1320=B_SPLINE_SURFACE_WITH_KNOTS('',3,3,((#43444,#43445,#43446,#43447,
#43448,#43449,#43450,#43451,#43452,#43453,#43454,#43455,#43456,#43457,#43458,
#43459,#43460,#43461,#43462,#43463,#43464,#43465,#43466,#43467,#43468,#43469,
#43470,#43471,#43472,#43473,#43474,#43475,#43476,#43477,#43478,#43479,#43480,
#43481,#43482,#43483,#43484,#43485,#43486,#43487,#43488,#43489,#43490,#43491,
#43492,#43493,#43494,#43495,#43496,#43497,#43498,#43499,#43500,#43501,#43502,
#43503,#43504,#43505,#43506,#43507,#43508,#43509,#43510,#43511,#43512,#43513,
#43514,#43515,#43516,#43517,#43518,#43519,#43520,#43521,#43522,#43523,#43524,
#43525,#43526,#43527,#43528,#43529,#43530,#43531,#43532,#43533,#43534,#43535,
#43536,#43537,#43538,#43539,#43540,#43541,#43542,#43543),(#43544,#43545,
#43546,#43547,#43548,#43549,#43550,#43551,#43552,#43553,#43554,#43555,#43556,
#43557,#43558,#43559,#43560,#43561,#43562,#43563,#43564,#43565,#43566,#43567,
#43568,#43569,#43570,#43571,#43572,#43573,#43574,#43575,#43576,#43577,#43578,
#43579,#43580,#43581,#43582,#43583,#43584,#43585,#43586,#43587,#43588,#43589,
#43590,#43591,#43592,#43593,#43594,#43595,#43596,#43597,#43598,#43599,#43600,
#43601,#43602,#43603,#43604,#43605,#43606,#43607,#43608,#43609,#43610,#43611,
#43612,#43613,#43614,#43615,#43616,#43617,#43618,#43619,#43620,#43621,#43622,
#43623,#43624,#43625,#43626,#43627,#43628,#43629,#43630,#43631,#43632,#43633,
#43634,#43635,#43636,#43637,#43638,#43639,#43640,#43641,#43642,#43643),
(#43644,#43645,#43646,#43647,#43648,#43649,#43650,#43651,#43652,#43653,
#43654,#43655,#43656,#43657,#43658,#43659,#43660,#43661,#43662,#43663,#43664,
#43665,#43666,#43667,#43668,#43669,#43670,#43671,#43672,#43673,#43674,#43675,
#43676,#43677,#43678,#43679,#43680,#43681,#43682,#43683,#43684,#43685,#43686,
#43687,#43688,#43689,#43690,#43691,#43692,#43693,#43694,#43695,#43696,#43697,
#43698,#43699,#43700,#43701,#43702,#43703,#43704,#43705,#43706,#43707,#43708,
#43709,#43710,#43711,#43712,#43713,#43714,#43715,#43716,#43717,#43718,#43719,
#43720,#43721,#43722,#43723,#43724,#43725,#43726,#43727,#43728,#43729,#43730,
#43731,#43732,#43733,#43734,#43735,#43736,#43737,#43738,#43739,#43740,#43741,
#43742,#43743),(#43744,#43745,#43746,#43747,#43748,#43749,#43750,#43751,
#43752,#43753,#43754,#43755,#43756,#43757,#43758,#43759,#43760,#43761,#43762,
#43763,#43764,#43765,#43766,#43767,#43768,#43769,#43770,#43771,#43772,#43773,
#43774,#43775,#43776,#43777,#43778,#43779,#43780,#43781,#43782,#43783,#43784,
#43785,#43786,#43787,#43788,#43789,#43790,#43791,#43792,#43793,#43794,#43795,
#43796,#43797,#43798,#43799,#43800,#43801,#43802,#43803,#43804,#43805,#43806,
#43807,#43808,#43809,#43810,#43811,#43812,#43813,#43814,#43815,#43816,#43817,
#43818,#43819,#43820,#43821,#43822,#43823,#43824,#43825,#43826,#43827,#43828,
#43829,#43830,#43831,#43832,#43833,#43834,#43835,#43836,#43837,#43838,#43839,
#43840,#43841,#43842,#43843)),.UNSPECIFIED.,.F.,.F.,.F.,(4,4),(4,1,1,1,
1,1,1,1,1,1,1,1,1,1,1,1,1,1,1,1,1,1,1,1,1,1,1,1,1,1,1,1,1,1,1,1,1,1,1,1,
1,1,1,1,1,1,1,1,1,1,1,1,1,1,1,1,1,1,1,1,1,1,1,1,1,1,1,1,1,1,1,1,1,1,1,1,
1,1,1,1,1,1,1,1,1,1,1,1,1,1,1,1,1,1,1,1,1,4),(0.,0.064201349933887),(11.8589888623077,
12.8514087025213,13.843828542735,14.8362483829486,15.8286682231622,16.8210880633759,
17.8135079035895,18.8059277438031,19.7983475840168,20.7907674242304,21.783187264444,
22.7756071046577,23.7680269448713,24.7604467850849,25.7528666252986,26.7452864655122,
27.7377063057259,28.7301261459395,29.7225459861531,30.7149658263668,31.7073856665804,
32.699805506794,33.6922253470076,34.6846451872213,35.6770650274349,36.6694848676485,
37.6619047078622,38.6543245480758,39.6467443882895,40.6391642285031,41.6315840687167,
42.6240039089304,43.616423749144,44.6088435893576,45.6012634295713,46.5936832697849,
47.5861031099985,48.5785229502122,49.5709427904258,50.5633626306394,51.5557824708531,
52.5482023110667,53.5406221512803,54.533041991494,55.5254618317076,56.5178816719212,
57.5103015121349,58.5027213523485,59.4951411925621,60.4875610327758,61.4799808729894,
62.472400713203,63.4648205534167,64.4572403936303,65.4496602338439,66.4420800740576,
67.4344999142712,68.4269197544848,69.4193395946985,70.4117594349121,71.4041792751257,
72.3965991153394,73.389018955553,74.3814387957666,75.3738586359803,76.3662784761939,
77.3586983164075,78.3511181566212,79.3435379968348,80.3359578370484,81.3283776772621,
82.3207975174757,83.3132173576894,84.305637197903,85.2980570381166,86.2904768783303,
87.2828967185439,88.2753165587575,89.2677363989712,90.2601562391848,91.2525760793984,
92.2449959196121,93.2374157598257,94.2298356000393,95.222255440253,96.2146752804666,
97.2070951206802,98.1995149608939,99.1919348011075,100.184354641321,101.176774481535,
102.169194321748,103.161614161962,104.154034002176,105.146453842389,106.138873682603,
107.131293522817,108.12371336303),.UNSPECIFIED.);
#1321=B_SPLINE_SURFACE_WITH_KNOTS('',3,3,((#43963,#43964,#43965,#43966,
#43967,#43968,#43969,#43970,#43971,#43972,#43973,#43974,#43975,#43976,#43977,
#43978,#43979,#43980,#43981,#43982,#43983,#43984,#43985,#43986,#43987,#43988,
#43989,#43990,#43991,#43992,#43993,#43994,#43995,#43996,#43997,#43998,#43999,
#44000,#44001,#44002,#44003,#44004,#44005,#44006,#44007,#44008,#44009,#44010,
#44011,#44012,#44013,#44014,#44015,#44016,#44017,#44018,#44019,#44020,#44021,
#44022,#44023,#44024,#44025,#44026,#44027,#44028,#44029,#44030,#44031,#44032,
#44033,#44034,#44035,#44036,#44037,#44038,#44039,#44040,#44041,#44042,#44043,
#44044,#44045,#44046,#44047,#44048,#44049,#44050,#44051,#44052,#44053,#44054,
#44055,#44056,#44057,#44058,#44059,#44060,#44061,#44062),(#44063,#44064,
#44065,#44066,#44067,#44068,#44069,#44070,#44071,#44072,#44073,#44074,#44075,
#44076,#44077,#44078,#44079,#44080,#44081,#44082,#44083,#44084,#44085,#44086,
#44087,#44088,#44089,#44090,#44091,#44092,#44093,#44094,#44095,#44096,#44097,
#44098,#44099,#44100,#44101,#44102,#44103,#44104,#44105,#44106,#44107,#44108,
#44109,#44110,#44111,#44112,#44113,#44114,#44115,#44116,#44117,#44118,#44119,
#44120,#44121,#44122,#44123,#44124,#44125,#44126,#44127,#44128,#44129,#44130,
#44131,#44132,#44133,#44134,#44135,#44136,#44137,#44138,#44139,#44140,#44141,
#44142,#44143,#44144,#44145,#44146,#44147,#44148,#44149,#44150,#44151,#44152,
#44153,#44154,#44155,#44156,#44157,#44158,#44159,#44160,#44161,#44162),
(#44163,#44164,#44165,#44166,#44167,#44168,#44169,#44170,#44171,#44172,
#44173,#44174,#44175,#44176,#44177,#44178,#44179,#44180,#44181,#44182,#44183,
#44184,#44185,#44186,#44187,#44188,#44189,#44190,#44191,#44192,#44193,#44194,
#44195,#44196,#44197,#44198,#44199,#44200,#44201,#44202,#44203,#44204,#44205,
#44206,#44207,#44208,#44209,#44210,#44211,#44212,#44213,#44214,#44215,#44216,
#44217,#44218,#44219,#44220,#44221,#44222,#44223,#44224,#44225,#44226,#44227,
#44228,#44229,#44230,#44231,#44232,#44233,#44234,#44235,#44236,#44237,#44238,
#44239,#44240,#44241,#44242,#44243,#44244,#44245,#44246,#44247,#44248,#44249,
#44250,#44251,#44252,#44253,#44254,#44255,#44256,#44257,#44258,#44259,#44260,
#44261,#44262),(#44263,#44264,#44265,#44266,#44267,#44268,#44269,#44270,
#44271,#44272,#44273,#44274,#44275,#44276,#44277,#44278,#44279,#44280,#44281,
#44282,#44283,#44284,#44285,#44286,#44287,#44288,#44289,#44290,#44291,#44292,
#44293,#44294,#44295,#44296,#44297,#44298,#44299,#44300,#44301,#44302,#44303,
#44304,#44305,#44306,#44307,#44308,#44309,#44310,#44311,#44312,#44313,#44314,
#44315,#44316,#44317,#44318,#44319,#44320,#44321,#44322,#44323,#44324,#44325,
#44326,#44327,#44328,#44329,#44330,#44331,#44332,#44333,#44334,#44335,#44336,
#44337,#44338,#44339,#44340,#44341,#44342,#44343,#44344,#44345,#44346,#44347,
#44348,#44349,#44350,#44351,#44352,#44353,#44354,#44355,#44356,#44357,#44358,
#44359,#44360,#44361,#44362)),.UNSPECIFIED.,.F.,.F.,.F.,(4,4),(4,1,1,1,
1,1,1,1,1,1,1,1,1,1,1,1,1,1,1,1,1,1,1,1,1,1,1,1,1,1,1,1,1,1,1,1,1,1,1,1,
1,1,1,1,1,1,1,1,1,1,1,1,1,1,1,1,1,1,1,1,1,1,1,1,1,1,1,1,1,1,1,1,1,1,1,1,
1,1,1,1,1,1,1,1,1,1,1,1,1,1,1,1,1,1,1,1,1,4),(0.,0.064201349933887),(14.3984001269718,
15.3908199671854,16.3832398073991,17.3756596476127,18.3680794878263,19.36049932804,
20.3529191682536,21.3453390084673,22.3377588486809,23.3301786888945,24.3225985291082,
25.3150183693218,26.3074382095354,27.2998580497491,28.2922778899627,29.2846977301763,
30.27711757039,31.2695374106036,32.2619572508172,33.2543770910309,34.2467969312445,
35.2392167714581,36.2316366116718,37.2240564518854,38.216476292099,39.2088961323127,
40.2013159725263,41.1937358127399,42.1861556529536,43.1785754931672,44.1709953333808,
45.1634151735945,46.1558350138081,47.1482548540217,48.1406746942354,49.133094534449,
50.1255143746626,51.1179342148763,52.1103540550899,53.1027738953035,54.0951937355172,
55.0876135757308,56.0800334159444,57.0724532561581,58.0648730963717,59.0572929365853,
60.049712776799,61.0421326170126,62.0345524572262,63.0269722974399,64.0193921376535,
65.0118119778672,66.0042318180808,66.9966516582944,67.9890714985081,68.9814913387217,
69.9739111789353,70.966331019149,71.9587508593626,72.9511706995762,73.9435905397899,
74.9360103800035,75.9284302202171,76.9208500604308,77.9132699006444,78.905689740858,
79.8981095810717,80.8905294212853,81.8829492614989,82.8753691017126,83.8677889419262,
84.8602087821398,85.8526286223535,86.8450484625671,87.8374683027807,88.8298881429944,
89.822307983208,90.8147278234216,91.8071476636353,92.7995675038489,93.7919873440625,
94.7844071842762,95.7768270244898,96.7692468647034,97.7616667049171,98.7540865451307,
99.7465063853443,100.738926225558,101.731346065772,102.723765905985,103.716185746199,
104.708605586413,105.701025426626,106.69344526684,107.685865107053,108.678284947267,
109.670704787481,110.663124627694),.UNSPECIFIED.);
#1322=B_SPLINE_SURFACE_WITH_KNOTS('',3,3,((#44691,#44692,#44693,#44694,
#44695,#44696,#44697,#44698,#44699,#44700,#44701,#44702,#44703,#44704,#44705,
#44706,#44707,#44708,#44709,#44710,#44711,#44712,#44713,#44714,#44715,#44716,
#44717,#44718,#44719,#44720,#44721,#44722,#44723,#44724,#44725,#44726,#44727,
#44728,#44729,#44730,#44731,#44732,#44733,#44734,#44735,#44736,#44737,#44738,
#44739,#44740,#44741,#44742,#44743,#44744,#44745,#44746,#44747,#44748,#44749,
#44750,#44751,#44752,#44753,#44754,#44755,#44756,#44757,#44758,#44759,#44760,
#44761,#44762,#44763,#44764,#44765,#44766,#44767,#44768,#44769,#44770,#44771,
#44772,#44773,#44774,#44775,#44776,#44777,#44778,#44779,#44780,#44781,#44782,
#44783,#44784,#44785,#44786,#44787,#44788,#44789,#44790),(#44791,#44792,
#44793,#44794,#44795,#44796,#44797,#44798,#44799,#44800,#44801,#44802,#44803,
#44804,#44805,#44806,#44807,#44808,#44809,#44810,#44811,#44812,#44813,#44814,
#44815,#44816,#44817,#44818,#44819,#44820,#44821,#44822,#44823,#44824,#44825,
#44826,#44827,#44828,#44829,#44830,#44831,#44832,#44833,#44834,#44835,#44836,
#44837,#44838,#44839,#44840,#44841,#44842,#44843,#44844,#44845,#44846,#44847,
#44848,#44849,#44850,#44851,#44852,#44853,#44854,#44855,#44856,#44857,#44858,
#44859,#44860,#44861,#44862,#44863,#44864,#44865,#44866,#44867,#44868,#44869,
#44870,#44871,#44872,#44873,#44874,#44875,#44876,#44877,#44878,#44879,#44880,
#44881,#44882,#44883,#44884,#44885,#44886,#44887,#44888,#44889,#44890),
(#44891,#44892,#44893,#44894,#44895,#44896,#44897,#44898,#44899,#44900,
#44901,#44902,#44903,#44904,#44905,#44906,#44907,#44908,#44909,#44910,#44911,
#44912,#44913,#44914,#44915,#44916,#44917,#44918,#44919,#44920,#44921,#44922,
#44923,#44924,#44925,#44926,#44927,#44928,#44929,#44930,#44931,#44932,#44933,
#44934,#44935,#44936,#44937,#44938,#44939,#44940,#44941,#44942,#44943,#44944,
#44945,#44946,#44947,#44948,#44949,#44950,#44951,#44952,#44953,#44954,#44955,
#44956,#44957,#44958,#44959,#44960,#44961,#44962,#44963,#44964,#44965,#44966,
#44967,#44968,#44969,#44970,#44971,#44972,#44973,#44974,#44975,#44976,#44977,
#44978,#44979,#44980,#44981,#44982,#44983,#44984,#44985,#44986,#44987,#44988,
#44989,#44990),(#44991,#44992,#44993,#44994,#44995,#44996,#44997,#44998,
#44999,#45000,#45001,#45002,#45003,#45004,#45005,#45006,#45007,#45008,#45009,
#45010,#45011,#45012,#45013,#45014,#45015,#45016,#45017,#45018,#45019,#45020,
#45021,#45022,#45023,#45024,#45025,#45026,#45027,#45028,#45029,#45030,#45031,
#45032,#45033,#45034,#45035,#45036,#45037,#45038,#45039,#45040,#45041,#45042,
#45043,#45044,#45045,#45046,#45047,#45048,#45049,#45050,#45051,#45052,#45053,
#45054,#45055,#45056,#45057,#45058,#45059,#45060,#45061,#45062,#45063,#45064,
#45065,#45066,#45067,#45068,#45069,#45070,#45071,#45072,#45073,#45074,#45075,
#45076,#45077,#45078,#45079,#45080,#45081,#45082,#45083,#45084,#45085,#45086,
#45087,#45088,#45089,#45090)),.UNSPECIFIED.,.F.,.F.,.F.,(4,4),(4,1,1,1,
1,1,1,1,1,1,1,1,1,1,1,1,1,1,1,1,1,1,1,1,1,1,1,1,1,1,1,1,1,1,1,1,1,1,1,1,
1,1,1,1,1,1,1,1,1,1,1,1,1,1,1,1,1,1,1,1,1,1,1,1,1,1,1,1,1,1,1,1,1,1,1,1,
1,1,1,1,1,1,1,1,1,1,1,1,1,1,1,1,1,1,1,1,1,4),(0.,0.064201349933887),(11.8589888623078,
12.8514087025215,13.8438285427351,14.8362483829487,15.8286682231624,16.821088063376,
17.8135079035896,18.8059277438032,19.7983475840169,20.7907674242305,21.7831872644441,
22.7756071046578,23.7680269448714,24.760446785085,25.7528666252987,26.7452864655123,
27.7377063057259,28.7301261459396,29.7225459861532,30.7149658263668,31.7073856665805,
32.6998055067941,33.6922253470077,34.6846451872214,35.677065027435,36.6694848676486,
37.6619047078623,38.6543245480759,39.6467443882895,40.6391642285032,41.6315840687168,
42.6240039089304,43.6164237491441,44.6088435893577,45.6012634295713,46.593683269785,
47.5861031099986,48.5785229502122,49.5709427904259,50.5633626306395,51.5557824708531,
52.5482023110668,53.5406221512804,54.533041991494,55.5254618317077,56.5178816719213,
57.5103015121349,58.5027213523486,59.4951411925622,60.4875610327758,61.4799808729895,
62.4724007132031,63.4648205534167,64.4572403936303,65.449660233844,66.4420800740576,
67.4344999142712,68.4269197544849,69.4193395946985,70.4117594349121,71.4041792751258,
72.3965991153394,73.389018955553,74.3814387957667,75.3738586359803,76.3662784761939,
77.3586983164076,78.3511181566212,79.3435379968348,80.3359578370485,81.3283776772621,
82.3207975174757,83.3132173576894,84.305637197903,85.2980570381166,86.2904768783303,
87.2828967185439,88.2753165587575,89.2677363989712,90.2601562391848,91.2525760793984,
92.2449959196121,93.2374157598257,94.2298356000393,95.222255440253,96.2146752804666,
97.2070951206802,98.1995149608939,99.1919348011075,100.184354641321,101.176774481535,
102.169194321748,103.161614161962,104.154034002176,105.146453842389,106.138873682603,
107.131293522817,108.12371336303),.UNSPECIFIED.);
#1323=B_SPLINE_SURFACE_WITH_KNOTS('',3,3,((#45210,#45211,#45212,#45213,
#45214,#45215,#45216,#45217,#45218,#45219,#45220,#45221,#45222,#45223,#45224,
#45225,#45226,#45227,#45228,#45229,#45230,#45231,#45232,#45233,#45234,#45235,
#45236,#45237,#45238,#45239,#45240,#45241,#45242,#45243,#45244,#45245,#45246,
#45247,#45248,#45249,#45250,#45251,#45252,#45253,#45254,#45255,#45256,#45257,
#45258,#45259,#45260,#45261,#45262,#45263,#45264,#45265,#45266,#45267,#45268,
#45269,#45270,#45271,#45272,#45273,#45274,#45275,#45276,#45277,#45278,#45279,
#45280,#45281,#45282,#45283,#45284,#45285,#45286,#45287,#45288,#45289,#45290,
#45291,#45292,#45293,#45294,#45295,#45296,#45297,#45298,#45299,#45300,#45301,
#45302,#45303,#45304,#45305,#45306,#45307,#45308,#45309),(#45310,#45311,
#45312,#45313,#45314,#45315,#45316,#45317,#45318,#45319,#45320,#45321,#45322,
#45323,#45324,#45325,#45326,#45327,#45328,#45329,#45330,#45331,#45332,#45333,
#45334,#45335,#45336,#45337,#45338,#45339,#45340,#45341,#45342,#45343,#45344,
#45345,#45346,#45347,#45348,#45349,#45350,#45351,#45352,#45353,#45354,#45355,
#45356,#45357,#45358,#45359,#45360,#45361,#45362,#45363,#45364,#45365,#45366,
#45367,#45368,#45369,#45370,#45371,#45372,#45373,#45374,#45375,#45376,#45377,
#45378,#45379,#45380,#45381,#45382,#45383,#45384,#45385,#45386,#45387,#45388,
#45389,#45390,#45391,#45392,#45393,#45394,#45395,#45396,#45397,#45398,#45399,
#45400,#45401,#45402,#45403,#45404,#45405,#45406,#45407,#45408,#45409),
(#45410,#45411,#45412,#45413,#45414,#45415,#45416,#45417,#45418,#45419,
#45420,#45421,#45422,#45423,#45424,#45425,#45426,#45427,#45428,#45429,#45430,
#45431,#45432,#45433,#45434,#45435,#45436,#45437,#45438,#45439,#45440,#45441,
#45442,#45443,#45444,#45445,#45446,#45447,#45448,#45449,#45450,#45451,#45452,
#45453,#45454,#45455,#45456,#45457,#45458,#45459,#45460,#45461,#45462,#45463,
#45464,#45465,#45466,#45467,#45468,#45469,#45470,#45471,#45472,#45473,#45474,
#45475,#45476,#45477,#45478,#45479,#45480,#45481,#45482,#45483,#45484,#45485,
#45486,#45487,#45488,#45489,#45490,#45491,#45492,#45493,#45494,#45495,#45496,
#45497,#45498,#45499,#45500,#45501,#45502,#45503,#45504,#45505,#45506,#45507,
#45508,#45509),(#45510,#45511,#45512,#45513,#45514,#45515,#45516,#45517,
#45518,#45519,#45520,#45521,#45522,#45523,#45524,#45525,#45526,#45527,#45528,
#45529,#45530,#45531,#45532,#45533,#45534,#45535,#45536,#45537,#45538,#45539,
#45540,#45541,#45542,#45543,#45544,#45545,#45546,#45547,#45548,#45549,#45550,
#45551,#45552,#45553,#45554,#45555,#45556,#45557,#45558,#45559,#45560,#45561,
#45562,#45563,#45564,#45565,#45566,#45567,#45568,#45569,#45570,#45571,#45572,
#45573,#45574,#45575,#45576,#45577,#45578,#45579,#45580,#45581,#45582,#45583,
#45584,#45585,#45586,#45587,#45588,#45589,#45590,#45591,#45592,#45593,#45594,
#45595,#45596,#45597,#45598,#45599,#45600,#45601,#45602,#45603,#45604,#45605,
#45606,#45607,#45608,#45609)),.UNSPECIFIED.,.F.,.F.,.F.,(4,4),(4,1,1,1,
1,1,1,1,1,1,1,1,1,1,1,1,1,1,1,1,1,1,1,1,1,1,1,1,1,1,1,1,1,1,1,1,1,1,1,1,
1,1,1,1,1,1,1,1,1,1,1,1,1,1,1,1,1,1,1,1,1,1,1,1,1,1,1,1,1,1,1,1,1,1,1,1,
1,1,1,1,1,1,1,1,1,1,1,1,1,1,1,1,1,1,1,1,1,4),(0.,0.064201349933887),(14.3984001269719,
15.3908199671856,16.3832398073992,17.3756596476128,18.3680794878265,19.3604993280401,
20.3529191682537,21.3453390084674,22.337758848681,23.3301786888946,24.3225985291083,
25.3150183693219,26.3074382095355,27.2998580497492,28.2922778899628,29.2846977301764,
30.2771175703901,31.2695374106037,32.2619572508173,33.2543770910309,34.2467969312446,
35.2392167714582,36.2316366116718,37.2240564518855,38.2164762920991,39.2088961323127,
40.2013159725264,41.19373581274,42.1861556529536,43.1785754931673,44.1709953333809,
45.1634151735945,46.1558350138082,47.1482548540218,48.1406746942354,49.1330945344491,
50.1255143746627,51.1179342148763,52.11035405509,53.1027738953036,54.0951937355172,
55.0876135757309,56.0800334159445,57.0724532561581,58.0648730963718,59.0572929365854,
60.049712776799,61.0421326170127,62.0345524572263,63.0269722974399,64.0193921376536,
65.0118119778672,66.0042318180808,66.9966516582945,67.9890714985081,68.9814913387217,
69.9739111789354,70.966331019149,71.9587508593626,72.9511706995763,73.9435905397899,
74.9360103800035,75.9284302202172,76.9208500604308,77.9132699006444,78.9056897408581,
79.8981095810717,80.8905294212853,81.882949261499,82.8753691017126,83.8677889419262,
84.8602087821399,85.8526286223535,86.8450484625671,87.8374683027808,88.8298881429944,
89.822307983208,90.8147278234217,91.8071476636353,92.7995675038489,93.7919873440626,
94.7844071842762,95.7768270244898,96.7692468647035,97.7616667049171,98.7540865451307,
99.7465063853444,100.738926225558,101.731346065772,102.723765905985,103.716185746199,
104.708605586413,105.701025426626,106.69344526684,107.685865107053,108.678284947267,
109.670704787481,110.663124627694),.UNSPECIFIED.);
#1324=B_SPLINE_SURFACE_WITH_KNOTS('',3,3,((#45938,#45939,#45940,#45941,
#45942,#45943,#45944,#45945,#45946,#45947,#45948,#45949,#45950,#45951,#45952,
#45953,#45954,#45955,#45956,#45957,#45958,#45959,#45960,#45961,#45962,#45963,
#45964,#45965,#45966,#45967,#45968,#45969,#45970,#45971,#45972,#45973,#45974,
#45975,#45976,#45977,#45978,#45979,#45980,#45981,#45982,#45983,#45984,#45985,
#45986,#45987,#45988,#45989,#45990,#45991,#45992,#45993,#45994,#45995,#45996,
#45997,#45998,#45999,#46000,#46001,#46002,#46003,#46004,#46005,#46006,#46007,
#46008,#46009,#46010,#46011,#46012,#46013,#46014,#46015,#46016,#46017,#46018,
#46019,#46020,#46021,#46022,#46023,#46024,#46025,#46026,#46027,#46028,#46029,
#46030,#46031,#46032,#46033,#46034,#46035,#46036,#46037),(#46038,#46039,
#46040,#46041,#46042,#46043,#46044,#46045,#46046,#46047,#46048,#46049,#46050,
#46051,#46052,#46053,#46054,#46055,#46056,#46057,#46058,#46059,#46060,#46061,
#46062,#46063,#46064,#46065,#46066,#46067,#46068,#46069,#46070,#46071,#46072,
#46073,#46074,#46075,#46076,#46077,#46078,#46079,#46080,#46081,#46082,#46083,
#46084,#46085,#46086,#46087,#46088,#46089,#46090,#46091,#46092,#46093,#46094,
#46095,#46096,#46097,#46098,#46099,#46100,#46101,#46102,#46103,#46104,#46105,
#46106,#46107,#46108,#46109,#46110,#46111,#46112,#46113,#46114,#46115,#46116,
#46117,#46118,#46119,#46120,#46121,#46122,#46123,#46124,#46125,#46126,#46127,
#46128,#46129,#46130,#46131,#46132,#46133,#46134,#46135,#46136,#46137),
(#46138,#46139,#46140,#46141,#46142,#46143,#46144,#46145,#46146,#46147,
#46148,#46149,#46150,#46151,#46152,#46153,#46154,#46155,#46156,#46157,#46158,
#46159,#46160,#46161,#46162,#46163,#46164,#46165,#46166,#46167,#46168,#46169,
#46170,#46171,#46172,#46173,#46174,#46175,#46176,#46177,#46178,#46179,#46180,
#46181,#46182,#46183,#46184,#46185,#46186,#46187,#46188,#46189,#46190,#46191,
#46192,#46193,#46194,#46195,#46196,#46197,#46198,#46199,#46200,#46201,#46202,
#46203,#46204,#46205,#46206,#46207,#46208,#46209,#46210,#46211,#46212,#46213,
#46214,#46215,#46216,#46217,#46218,#46219,#46220,#46221,#46222,#46223,#46224,
#46225,#46226,#46227,#46228,#46229,#46230,#46231,#46232,#46233,#46234,#46235,
#46236,#46237),(#46238,#46239,#46240,#46241,#46242,#46243,#46244,#46245,
#46246,#46247,#46248,#46249,#46250,#46251,#46252,#46253,#46254,#46255,#46256,
#46257,#46258,#46259,#46260,#46261,#46262,#46263,#46264,#46265,#46266,#46267,
#46268,#46269,#46270,#46271,#46272,#46273,#46274,#46275,#46276,#46277,#46278,
#46279,#46280,#46281,#46282,#46283,#46284,#46285,#46286,#46287,#46288,#46289,
#46290,#46291,#46292,#46293,#46294,#46295,#46296,#46297,#46298,#46299,#46300,
#46301,#46302,#46303,#46304,#46305,#46306,#46307,#46308,#46309,#46310,#46311,
#46312,#46313,#46314,#46315,#46316,#46317,#46318,#46319,#46320,#46321,#46322,
#46323,#46324,#46325,#46326,#46327,#46328,#46329,#46330,#46331,#46332,#46333,
#46334,#46335,#46336,#46337)),.UNSPECIFIED.,.F.,.F.,.F.,(4,4),(4,1,1,1,
1,1,1,1,1,1,1,1,1,1,1,1,1,1,1,1,1,1,1,1,1,1,1,1,1,1,1,1,1,1,1,1,1,1,1,1,
1,1,1,1,1,1,1,1,1,1,1,1,1,1,1,1,1,1,1,1,1,1,1,1,1,1,1,1,1,1,1,1,1,1,1,1,
1,1,1,1,1,1,1,1,1,1,1,1,1,1,1,1,1,1,1,1,1,4),(0.,0.064201349933887),(11.8589888623077,
12.8514087025213,13.843828542735,14.8362483829486,15.8286682231622,16.8210880633759,
17.8135079035895,18.8059277438031,19.7983475840168,20.7907674242304,21.783187264444,
22.7756071046577,23.7680269448713,24.7604467850849,25.7528666252986,26.7452864655122,
27.7377063057258,28.7301261459395,29.7225459861531,30.7149658263667,31.7073856665804,
32.699805506794,33.6922253470076,34.6846451872213,35.6770650274349,36.6694848676485,
37.6619047078622,38.6543245480758,39.6467443882894,40.6391642285031,41.6315840687167,
42.6240039089303,43.616423749144,44.6088435893576,45.6012634295713,46.5936832697849,
47.5861031099985,48.5785229502122,49.5709427904258,50.5633626306394,51.5557824708531,
52.5482023110667,53.5406221512803,54.533041991494,55.5254618317076,56.5178816719212,
57.5103015121349,58.5027213523485,59.4951411925621,60.4875610327758,61.4799808729894,
62.472400713203,63.4648205534167,64.4572403936303,65.4496602338439,66.4420800740576,
67.4344999142712,68.4269197544848,69.4193395946985,70.4117594349121,71.4041792751257,
72.3965991153394,73.389018955553,74.3814387957666,75.3738586359803,76.3662784761939,
77.3586983164075,78.3511181566212,79.3435379968348,80.3359578370484,81.3283776772621,
82.3207975174757,83.3132173576893,84.305637197903,85.2980570381166,86.2904768783302,
87.2828967185439,88.2753165587575,89.2677363989711,90.2601562391848,91.2525760793984,
92.2449959196121,93.2374157598257,94.2298356000393,95.222255440253,96.2146752804666,
97.2070951206802,98.1995149608939,99.1919348011075,100.184354641321,101.176774481535,
102.169194321748,103.161614161962,104.154034002176,105.146453842389,106.138873682603,
107.131293522817,108.12371336303),.UNSPECIFIED.);
#1325=B_SPLINE_SURFACE_WITH_KNOTS('',3,3,((#46457,#46458,#46459,#46460,
#46461,#46462,#46463,#46464,#46465,#46466,#46467,#46468,#46469,#46470,#46471,
#46472,#46473,#46474,#46475,#46476,#46477,#46478,#46479,#46480,#46481,#46482,
#46483,#46484,#46485,#46486,#46487,#46488,#46489,#46490,#46491,#46492,#46493,
#46494,#46495,#46496,#46497,#46498,#46499,#46500,#46501,#46502,#46503,#46504,
#46505,#46506,#46507,#46508,#46509,#46510,#46511,#46512,#46513,#46514,#46515,
#46516,#46517,#46518,#46519,#46520,#46521,#46522,#46523,#46524,#46525,#46526,
#46527,#46528,#46529,#46530,#46531,#46532,#46533,#46534,#46535,#46536,#46537,
#46538,#46539,#46540,#46541,#46542,#46543,#46544,#46545,#46546,#46547,#46548,
#46549,#46550,#46551,#46552,#46553,#46554,#46555,#46556),(#46557,#46558,
#46559,#46560,#46561,#46562,#46563,#46564,#46565,#46566,#46567,#46568,#46569,
#46570,#46571,#46572,#46573,#46574,#46575,#46576,#46577,#46578,#46579,#46580,
#46581,#46582,#46583,#46584,#46585,#46586,#46587,#46588,#46589,#46590,#46591,
#46592,#46593,#46594,#46595,#46596,#46597,#46598,#46599,#46600,#46601,#46602,
#46603,#46604,#46605,#46606,#46607,#46608,#46609,#46610,#46611,#46612,#46613,
#46614,#46615,#46616,#46617,#46618,#46619,#46620,#46621,#46622,#46623,#46624,
#46625,#46626,#46627,#46628,#46629,#46630,#46631,#46632,#46633,#46634,#46635,
#46636,#46637,#46638,#46639,#46640,#46641,#46642,#46643,#46644,#46645,#46646,
#46647,#46648,#46649,#46650,#46651,#46652,#46653,#46654,#46655,#46656),
(#46657,#46658,#46659,#46660,#46661,#46662,#46663,#46664,#46665,#46666,
#46667,#46668,#46669,#46670,#46671,#46672,#46673,#46674,#46675,#46676,#46677,
#46678,#46679,#46680,#46681,#46682,#46683,#46684,#46685,#46686,#46687,#46688,
#46689,#46690,#46691,#46692,#46693,#46694,#46695,#46696,#46697,#46698,#46699,
#46700,#46701,#46702,#46703,#46704,#46705,#46706,#46707,#46708,#46709,#46710,
#46711,#46712,#46713,#46714,#46715,#46716,#46717,#46718,#46719,#46720,#46721,
#46722,#46723,#46724,#46725,#46726,#46727,#46728,#46729,#46730,#46731,#46732,
#46733,#46734,#46735,#46736,#46737,#46738,#46739,#46740,#46741,#46742,#46743,
#46744,#46745,#46746,#46747,#46748,#46749,#46750,#46751,#46752,#46753,#46754,
#46755,#46756),(#46757,#46758,#46759,#46760,#46761,#46762,#46763,#46764,
#46765,#46766,#46767,#46768,#46769,#46770,#46771,#46772,#46773,#46774,#46775,
#46776,#46777,#46778,#46779,#46780,#46781,#46782,#46783,#46784,#46785,#46786,
#46787,#46788,#46789,#46790,#46791,#46792,#46793,#46794,#46795,#46796,#46797,
#46798,#46799,#46800,#46801,#46802,#46803,#46804,#46805,#46806,#46807,#46808,
#46809,#46810,#46811,#46812,#46813,#46814,#46815,#46816,#46817,#46818,#46819,
#46820,#46821,#46822,#46823,#46824,#46825,#46826,#46827,#46828,#46829,#46830,
#46831,#46832,#46833,#46834,#46835,#46836,#46837,#46838,#46839,#46840,#46841,
#46842,#46843,#46844,#46845,#46846,#46847,#46848,#46849,#46850,#46851,#46852,
#46853,#46854,#46855,#46856)),.UNSPECIFIED.,.F.,.F.,.F.,(4,4),(4,1,1,1,
1,1,1,1,1,1,1,1,1,1,1,1,1,1,1,1,1,1,1,1,1,1,1,1,1,1,1,1,1,1,1,1,1,1,1,1,
1,1,1,1,1,1,1,1,1,1,1,1,1,1,1,1,1,1,1,1,1,1,1,1,1,1,1,1,1,1,1,1,1,1,1,1,
1,1,1,1,1,1,1,1,1,1,1,1,1,1,1,1,1,1,1,1,1,4),(0.,0.064201349933887),(14.3984001269718,
15.3908199671854,16.3832398073991,17.3756596476127,18.3680794878263,19.36049932804,
20.3529191682536,21.3453390084673,22.3377588486809,23.3301786888945,24.3225985291082,
25.3150183693218,26.3074382095354,27.2998580497491,28.2922778899627,29.2846977301763,
30.27711757039,31.2695374106036,32.2619572508172,33.2543770910309,34.2467969312445,
35.2392167714581,36.2316366116718,37.2240564518854,38.216476292099,39.2088961323127,
40.2013159725263,41.1937358127399,42.1861556529536,43.1785754931672,44.1709953333808,
45.1634151735945,46.1558350138081,47.1482548540217,48.1406746942354,49.133094534449,
50.1255143746626,51.1179342148763,52.1103540550899,53.1027738953035,54.0951937355172,
55.0876135757308,56.0800334159444,57.0724532561581,58.0648730963717,59.0572929365853,
60.049712776799,61.0421326170126,62.0345524572262,63.0269722974399,64.0193921376535,
65.0118119778672,66.0042318180808,66.9966516582944,67.9890714985081,68.9814913387217,
69.9739111789353,70.966331019149,71.9587508593626,72.9511706995762,73.9435905397899,
74.9360103800035,75.9284302202171,76.9208500604308,77.9132699006444,78.905689740858,
79.8981095810717,80.8905294212853,81.8829492614989,82.8753691017126,83.8677889419262,
84.8602087821398,85.8526286223535,86.8450484625671,87.8374683027807,88.8298881429944,
89.822307983208,90.8147278234216,91.8071476636353,92.7995675038489,93.7919873440625,
94.7844071842762,95.7768270244898,96.7692468647034,97.7616667049171,98.7540865451307,
99.7465063853443,100.738926225558,101.731346065772,102.723765905985,103.716185746199,
104.708605586413,105.701025426626,106.69344526684,107.685865107053,108.678284947267,
109.670704787481,110.663124627694),.UNSPECIFIED.);
#1326=B_SPLINE_SURFACE_WITH_KNOTS('',3,3,((#47185,#47186,#47187,#47188,
#47189,#47190,#47191,#47192,#47193,#47194,#47195,#47196,#47197,#47198,#47199,
#47200,#47201,#47202,#47203,#47204,#47205,#47206,#47207,#47208,#47209,#47210,
#47211,#47212,#47213,#47214,#47215,#47216,#47217,#47218,#47219,#47220,#47221,
#47222,#47223,#47224,#47225,#47226,#47227,#47228,#47229,#47230,#47231,#47232,
#47233,#47234,#47235,#47236,#47237,#47238,#47239,#47240,#47241,#47242,#47243,
#47244,#47245,#47246,#47247,#47248,#47249,#47250,#47251,#47252,#47253,#47254,
#47255,#47256,#47257,#47258,#47259,#47260,#47261,#47262,#47263,#47264,#47265,
#47266,#47267,#47268,#47269,#47270,#47271,#47272,#47273,#47274,#47275,#47276,
#47277,#47278,#47279,#47280,#47281,#47282,#47283,#47284),(#47285,#47286,
#47287,#47288,#47289,#47290,#47291,#47292,#47293,#47294,#47295,#47296,#47297,
#47298,#47299,#47300,#47301,#47302,#47303,#47304,#47305,#47306,#47307,#47308,
#47309,#47310,#47311,#47312,#47313,#47314,#47315,#47316,#47317,#47318,#47319,
#47320,#47321,#47322,#47323,#47324,#47325,#47326,#47327,#47328,#47329,#47330,
#47331,#47332,#47333,#47334,#47335,#47336,#47337,#47338,#47339,#47340,#47341,
#47342,#47343,#47344,#47345,#47346,#47347,#47348,#47349,#47350,#47351,#47352,
#47353,#47354,#47355,#47356,#47357,#47358,#47359,#47360,#47361,#47362,#47363,
#47364,#47365,#47366,#47367,#47368,#47369,#47370,#47371,#47372,#47373,#47374,
#47375,#47376,#47377,#47378,#47379,#47380,#47381,#47382,#47383,#47384),
(#47385,#47386,#47387,#47388,#47389,#47390,#47391,#47392,#47393,#47394,
#47395,#47396,#47397,#47398,#47399,#47400,#47401,#47402,#47403,#47404,#47405,
#47406,#47407,#47408,#47409,#47410,#47411,#47412,#47413,#47414,#47415,#47416,
#47417,#47418,#47419,#47420,#47421,#47422,#47423,#47424,#47425,#47426,#47427,
#47428,#47429,#47430,#47431,#47432,#47433,#47434,#47435,#47436,#47437,#47438,
#47439,#47440,#47441,#47442,#47443,#47444,#47445,#47446,#47447,#47448,#47449,
#47450,#47451,#47452,#47453,#47454,#47455,#47456,#47457,#47458,#47459,#47460,
#47461,#47462,#47463,#47464,#47465,#47466,#47467,#47468,#47469,#47470,#47471,
#47472,#47473,#47474,#47475,#47476,#47477,#47478,#47479,#47480,#47481,#47482,
#47483,#47484),(#47485,#47486,#47487,#47488,#47489,#47490,#47491,#47492,
#47493,#47494,#47495,#47496,#47497,#47498,#47499,#47500,#47501,#47502,#47503,
#47504,#47505,#47506,#47507,#47508,#47509,#47510,#47511,#47512,#47513,#47514,
#47515,#47516,#47517,#47518,#47519,#47520,#47521,#47522,#47523,#47524,#47525,
#47526,#47527,#47528,#47529,#47530,#47531,#47532,#47533,#47534,#47535,#47536,
#47537,#47538,#47539,#47540,#47541,#47542,#47543,#47544,#47545,#47546,#47547,
#47548,#47549,#47550,#47551,#47552,#47553,#47554,#47555,#47556,#47557,#47558,
#47559,#47560,#47561,#47562,#47563,#47564,#47565,#47566,#47567,#47568,#47569,
#47570,#47571,#47572,#47573,#47574,#47575,#47576,#47577,#47578,#47579,#47580,
#47581,#47582,#47583,#47584)),.UNSPECIFIED.,.F.,.F.,.F.,(4,4),(4,1,1,1,
1,1,1,1,1,1,1,1,1,1,1,1,1,1,1,1,1,1,1,1,1,1,1,1,1,1,1,1,1,1,1,1,1,1,1,1,
1,1,1,1,1,1,1,1,1,1,1,1,1,1,1,1,1,1,1,1,1,1,1,1,1,1,1,1,1,1,1,1,1,1,1,1,
1,1,1,1,1,1,1,1,1,1,1,1,1,1,1,1,1,1,1,1,1,4),(0.,0.064201349933887),(11.8589888623078,
12.8514087025215,13.8438285427351,14.8362483829487,15.8286682231624,16.821088063376,
17.8135079035896,18.8059277438032,19.7983475840169,20.7907674242305,21.7831872644441,
22.7756071046578,23.7680269448714,24.760446785085,25.7528666252987,26.7452864655123,
27.7377063057259,28.7301261459396,29.7225459861532,30.7149658263668,31.7073856665805,
32.6998055067941,33.6922253470077,34.6846451872214,35.677065027435,36.6694848676486,
37.6619047078623,38.6543245480759,39.6467443882895,40.6391642285032,41.6315840687168,
42.6240039089304,43.6164237491441,44.6088435893577,45.6012634295713,46.593683269785,
47.5861031099986,48.5785229502122,49.5709427904259,50.5633626306395,51.5557824708531,
52.5482023110668,53.5406221512804,54.533041991494,55.5254618317077,56.5178816719213,
57.5103015121349,58.5027213523486,59.4951411925622,60.4875610327758,61.4799808729895,
62.4724007132031,63.4648205534167,64.4572403936303,65.449660233844,66.4420800740576,
67.4344999142712,68.4269197544849,69.4193395946985,70.4117594349121,71.4041792751258,
72.3965991153394,73.389018955553,74.3814387957667,75.3738586359803,76.3662784761939,
77.3586983164076,78.3511181566212,79.3435379968348,80.3359578370485,81.3283776772621,
82.3207975174757,83.3132173576894,84.305637197903,85.2980570381166,86.2904768783303,
87.2828967185439,88.2753165587575,89.2677363989712,90.2601562391848,91.2525760793984,
92.2449959196121,93.2374157598257,94.2298356000393,95.222255440253,96.2146752804666,
97.2070951206802,98.1995149608939,99.1919348011075,100.184354641321,101.176774481535,
102.169194321748,103.161614161962,104.154034002176,105.146453842389,106.138873682603,
107.131293522817,108.12371336303),.UNSPECIFIED.);
#1327=B_SPLINE_SURFACE_WITH_KNOTS('',3,3,((#47704,#47705,#47706,#47707,
#47708,#47709,#47710,#47711,#47712,#47713,#47714,#47715,#47716,#47717,#47718,
#47719,#47720,#47721,#47722,#47723,#47724,#47725,#47726,#47727,#47728,#47729,
#47730,#47731,#47732,#47733,#47734,#47735,#47736,#47737,#47738,#47739,#47740,
#47741,#47742,#47743,#47744,#47745,#47746,#47747,#47748,#47749,#47750,#47751,
#47752,#47753,#47754,#47755,#47756,#47757,#47758,#47759,#47760,#47761,#47762,
#47763,#47764,#47765,#47766,#47767,#47768,#47769,#47770,#47771,#47772,#47773,
#47774,#47775,#47776,#47777,#47778,#47779,#47780,#47781,#47782,#47783,#47784,
#47785,#47786,#47787,#47788,#47789,#47790,#47791,#47792,#47793,#47794,#47795,
#47796,#47797,#47798,#47799,#47800,#47801,#47802,#47803),(#47804,#47805,
#47806,#47807,#47808,#47809,#47810,#47811,#47812,#47813,#47814,#47815,#47816,
#47817,#47818,#47819,#47820,#47821,#47822,#47823,#47824,#47825,#47826,#47827,
#47828,#47829,#47830,#47831,#47832,#47833,#47834,#47835,#47836,#47837,#47838,
#47839,#47840,#47841,#47842,#47843,#47844,#47845,#47846,#47847,#47848,#47849,
#47850,#47851,#47852,#47853,#47854,#47855,#47856,#47857,#47858,#47859,#47860,
#47861,#47862,#47863,#47864,#47865,#47866,#47867,#47868,#47869,#47870,#47871,
#47872,#47873,#47874,#47875,#47876,#47877,#47878,#47879,#47880,#47881,#47882,
#47883,#47884,#47885,#47886,#47887,#47888,#47889,#47890,#47891,#47892,#47893,
#47894,#47895,#47896,#47897,#47898,#47899,#47900,#47901,#47902,#47903),
(#47904,#47905,#47906,#47907,#47908,#47909,#47910,#47911,#47912,#47913,
#47914,#47915,#47916,#47917,#47918,#47919,#47920,#47921,#47922,#47923,#47924,
#47925,#47926,#47927,#47928,#47929,#47930,#47931,#47932,#47933,#47934,#47935,
#47936,#47937,#47938,#47939,#47940,#47941,#47942,#47943,#47944,#47945,#47946,
#47947,#47948,#47949,#47950,#47951,#47952,#47953,#47954,#47955,#47956,#47957,
#47958,#47959,#47960,#47961,#47962,#47963,#47964,#47965,#47966,#47967,#47968,
#47969,#47970,#47971,#47972,#47973,#47974,#47975,#47976,#47977,#47978,#47979,
#47980,#47981,#47982,#47983,#47984,#47985,#47986,#47987,#47988,#47989,#47990,
#47991,#47992,#47993,#47994,#47995,#47996,#47997,#47998,#47999,#48000,#48001,
#48002,#48003),(#48004,#48005,#48006,#48007,#48008,#48009,#48010,#48011,
#48012,#48013,#48014,#48015,#48016,#48017,#48018,#48019,#48020,#48021,#48022,
#48023,#48024,#48025,#48026,#48027,#48028,#48029,#48030,#48031,#48032,#48033,
#48034,#48035,#48036,#48037,#48038,#48039,#48040,#48041,#48042,#48043,#48044,
#48045,#48046,#48047,#48048,#48049,#48050,#48051,#48052,#48053,#48054,#48055,
#48056,#48057,#48058,#48059,#48060,#48061,#48062,#48063,#48064,#48065,#48066,
#48067,#48068,#48069,#48070,#48071,#48072,#48073,#48074,#48075,#48076,#48077,
#48078,#48079,#48080,#48081,#48082,#48083,#48084,#48085,#48086,#48087,#48088,
#48089,#48090,#48091,#48092,#48093,#48094,#48095,#48096,#48097,#48098,#48099,
#48100,#48101,#48102,#48103)),.UNSPECIFIED.,.F.,.F.,.F.,(4,4),(4,1,1,1,
1,1,1,1,1,1,1,1,1,1,1,1,1,1,1,1,1,1,1,1,1,1,1,1,1,1,1,1,1,1,1,1,1,1,1,1,
1,1,1,1,1,1,1,1,1,1,1,1,1,1,1,1,1,1,1,1,1,1,1,1,1,1,1,1,1,1,1,1,1,1,1,1,
1,1,1,1,1,1,1,1,1,1,1,1,1,1,1,1,1,1,1,1,1,4),(0.,0.064201349933887),(14.3984001269719,
15.3908199671856,16.3832398073992,17.3756596476128,18.3680794878265,19.3604993280401,
20.3529191682537,21.3453390084674,22.337758848681,23.3301786888946,24.3225985291083,
25.3150183693219,26.3074382095355,27.2998580497492,28.2922778899628,29.2846977301764,
30.2771175703901,31.2695374106037,32.2619572508173,33.2543770910309,34.2467969312446,
35.2392167714582,36.2316366116718,37.2240564518855,38.2164762920991,39.2088961323127,
40.2013159725264,41.19373581274,42.1861556529536,43.1785754931673,44.1709953333809,
45.1634151735945,46.1558350138082,47.1482548540218,48.1406746942354,49.1330945344491,
50.1255143746627,51.1179342148763,52.11035405509,53.1027738953036,54.0951937355172,
55.0876135757309,56.0800334159445,57.0724532561581,58.0648730963718,59.0572929365854,
60.049712776799,61.0421326170127,62.0345524572263,63.0269722974399,64.0193921376536,
65.0118119778672,66.0042318180808,66.9966516582945,67.9890714985081,68.9814913387217,
69.9739111789354,70.966331019149,71.9587508593626,72.9511706995763,73.9435905397899,
74.9360103800035,75.9284302202172,76.9208500604308,77.9132699006444,78.9056897408581,
79.8981095810717,80.8905294212853,81.882949261499,82.8753691017126,83.8677889419262,
84.8602087821399,85.8526286223535,86.8450484625671,87.8374683027808,88.8298881429944,
89.822307983208,90.8147278234217,91.8071476636353,92.7995675038489,93.7919873440626,
94.7844071842762,95.7768270244898,96.7692468647035,97.7616667049171,98.7540865451307,
99.7465063853444,100.738926225558,101.731346065772,102.723765905985,103.716185746199,
104.708605586413,105.701025426626,106.69344526684,107.685865107053,108.678284947267,
109.670704787481,110.663124627694),.UNSPECIFIED.);
#1328=B_SPLINE_SURFACE_WITH_KNOTS('',3,3,((#48432,#48433,#48434,#48435,
#48436,#48437,#48438,#48439,#48440,#48441,#48442,#48443,#48444,#48445,#48446,
#48447,#48448,#48449,#48450,#48451,#48452,#48453,#48454,#48455,#48456,#48457,
#48458,#48459,#48460,#48461,#48462,#48463,#48464,#48465,#48466,#48467,#48468,
#48469,#48470,#48471,#48472,#48473,#48474,#48475,#48476,#48477,#48478,#48479,
#48480,#48481,#48482,#48483,#48484,#48485,#48486,#48487,#48488,#48489,#48490,
#48491,#48492,#48493,#48494,#48495,#48496,#48497,#48498,#48499,#48500,#48501,
#48502,#48503,#48504,#48505,#48506,#48507,#48508,#48509,#48510,#48511,#48512,
#48513,#48514,#48515,#48516,#48517,#48518,#48519,#48520,#48521,#48522,#48523,
#48524,#48525,#48526,#48527,#48528,#48529,#48530,#48531),(#48532,#48533,
#48534,#48535,#48536,#48537,#48538,#48539,#48540,#48541,#48542,#48543,#48544,
#48545,#48546,#48547,#48548,#48549,#48550,#48551,#48552,#48553,#48554,#48555,
#48556,#48557,#48558,#48559,#48560,#48561,#48562,#48563,#48564,#48565,#48566,
#48567,#48568,#48569,#48570,#48571,#48572,#48573,#48574,#48575,#48576,#48577,
#48578,#48579,#48580,#48581,#48582,#48583,#48584,#48585,#48586,#48587,#48588,
#48589,#48590,#48591,#48592,#48593,#48594,#48595,#48596,#48597,#48598,#48599,
#48600,#48601,#48602,#48603,#48604,#48605,#48606,#48607,#48608,#48609,#48610,
#48611,#48612,#48613,#48614,#48615,#48616,#48617,#48618,#48619,#48620,#48621,
#48622,#48623,#48624,#48625,#48626,#48627,#48628,#48629,#48630,#48631),
(#48632,#48633,#48634,#48635,#48636,#48637,#48638,#48639,#48640,#48641,
#48642,#48643,#48644,#48645,#48646,#48647,#48648,#48649,#48650,#48651,#48652,
#48653,#48654,#48655,#48656,#48657,#48658,#48659,#48660,#48661,#48662,#48663,
#48664,#48665,#48666,#48667,#48668,#48669,#48670,#48671,#48672,#48673,#48674,
#48675,#48676,#48677,#48678,#48679,#48680,#48681,#48682,#48683,#48684,#48685,
#48686,#48687,#48688,#48689,#48690,#48691,#48692,#48693,#48694,#48695,#48696,
#48697,#48698,#48699,#48700,#48701,#48702,#48703,#48704,#48705,#48706,#48707,
#48708,#48709,#48710,#48711,#48712,#48713,#48714,#48715,#48716,#48717,#48718,
#48719,#48720,#48721,#48722,#48723,#48724,#48725,#48726,#48727,#48728,#48729,
#48730,#48731),(#48732,#48733,#48734,#48735,#48736,#48737,#48738,#48739,
#48740,#48741,#48742,#48743,#48744,#48745,#48746,#48747,#48748,#48749,#48750,
#48751,#48752,#48753,#48754,#48755,#48756,#48757,#48758,#48759,#48760,#48761,
#48762,#48763,#48764,#48765,#48766,#48767,#48768,#48769,#48770,#48771,#48772,
#48773,#48774,#48775,#48776,#48777,#48778,#48779,#48780,#48781,#48782,#48783,
#48784,#48785,#48786,#48787,#48788,#48789,#48790,#48791,#48792,#48793,#48794,
#48795,#48796,#48797,#48798,#48799,#48800,#48801,#48802,#48803,#48804,#48805,
#48806,#48807,#48808,#48809,#48810,#48811,#48812,#48813,#48814,#48815,#48816,
#48817,#48818,#48819,#48820,#48821,#48822,#48823,#48824,#48825,#48826,#48827,
#48828,#48829,#48830,#48831)),.UNSPECIFIED.,.F.,.F.,.F.,(4,4),(4,1,1,1,
1,1,1,1,1,1,1,1,1,1,1,1,1,1,1,1,1,1,1,1,1,1,1,1,1,1,1,1,1,1,1,1,1,1,1,1,
1,1,1,1,1,1,1,1,1,1,1,1,1,1,1,1,1,1,1,1,1,1,1,1,1,1,1,1,1,1,1,1,1,1,1,1,
1,1,1,1,1,1,1,1,1,1,1,1,1,1,1,1,1,1,1,1,1,4),(0.,0.064201349933887),(11.8589888623077,
12.8514087025213,13.843828542735,14.8362483829486,15.8286682231622,16.8210880633759,
17.8135079035895,18.8059277438031,19.7983475840168,20.7907674242304,21.783187264444,
22.7756071046577,23.7680269448713,24.7604467850849,25.7528666252986,26.7452864655122,
27.7377063057258,28.7301261459395,29.7225459861531,30.7149658263668,31.7073856665804,
32.699805506794,33.6922253470076,34.6846451872213,35.6770650274349,36.6694848676485,
37.6619047078622,38.6543245480758,39.6467443882895,40.6391642285031,41.6315840687167,
42.6240039089304,43.616423749144,44.6088435893576,45.6012634295713,46.5936832697849,
47.5861031099985,48.5785229502122,49.5709427904258,50.5633626306394,51.5557824708531,
52.5482023110667,53.5406221512803,54.533041991494,55.5254618317076,56.5178816719212,
57.5103015121349,58.5027213523485,59.4951411925621,60.4875610327758,61.4799808729894,
62.472400713203,63.4648205534167,64.4572403936303,65.4496602338439,66.4420800740576,
67.4344999142712,68.4269197544848,69.4193395946985,70.4117594349121,71.4041792751257,
72.3965991153394,73.389018955553,74.3814387957666,75.3738586359803,76.3662784761939,
77.3586983164075,78.3511181566212,79.3435379968348,80.3359578370484,81.3283776772621,
82.3207975174757,83.3132173576894,84.305637197903,85.2980570381166,86.2904768783303,
87.2828967185439,88.2753165587575,89.2677363989712,90.2601562391848,91.2525760793984,
92.2449959196121,93.2374157598257,94.2298356000393,95.222255440253,96.2146752804666,
97.2070951206802,98.1995149608939,99.1919348011075,100.184354641321,101.176774481535,
102.169194321748,103.161614161962,104.154034002176,105.146453842389,106.138873682603,
107.131293522817,108.12371336303),.UNSPECIFIED.);
#1329=B_SPLINE_SURFACE_WITH_KNOTS('',3,3,((#48951,#48952,#48953,#48954,
#48955,#48956,#48957,#48958,#48959,#48960,#48961,#48962,#48963,#48964,#48965,
#48966,#48967,#48968,#48969,#48970,#48971,#48972,#48973,#48974,#48975,#48976,
#48977,#48978,#48979,#48980,#48981,#48982,#48983,#48984,#48985,#48986,#48987,
#48988,#48989,#48990,#48991,#48992,#48993,#48994,#48995,#48996,#48997,#48998,
#48999,#49000,#49001,#49002,#49003,#49004,#49005,#49006,#49007,#49008,#49009,
#49010,#49011,#49012,#49013,#49014,#49015,#49016,#49017,#49018,#49019,#49020,
#49021,#49022,#49023,#49024,#49025,#49026,#49027,#49028,#49029,#49030,#49031,
#49032,#49033,#49034,#49035,#49036,#49037,#49038,#49039,#49040,#49041,#49042,
#49043,#49044,#49045,#49046,#49047,#49048,#49049,#49050),(#49051,#49052,
#49053,#49054,#49055,#49056,#49057,#49058,#49059,#49060,#49061,#49062,#49063,
#49064,#49065,#49066,#49067,#49068,#49069,#49070,#49071,#49072,#49073,#49074,
#49075,#49076,#49077,#49078,#49079,#49080,#49081,#49082,#49083,#49084,#49085,
#49086,#49087,#49088,#49089,#49090,#49091,#49092,#49093,#49094,#49095,#49096,
#49097,#49098,#49099,#49100,#49101,#49102,#49103,#49104,#49105,#49106,#49107,
#49108,#49109,#49110,#49111,#49112,#49113,#49114,#49115,#49116,#49117,#49118,
#49119,#49120,#49121,#49122,#49123,#49124,#49125,#49126,#49127,#49128,#49129,
#49130,#49131,#49132,#49133,#49134,#49135,#49136,#49137,#49138,#49139,#49140,
#49141,#49142,#49143,#49144,#49145,#49146,#49147,#49148,#49149,#49150),
(#49151,#49152,#49153,#49154,#49155,#49156,#49157,#49158,#49159,#49160,
#49161,#49162,#49163,#49164,#49165,#49166,#49167,#49168,#49169,#49170,#49171,
#49172,#49173,#49174,#49175,#49176,#49177,#49178,#49179,#49180,#49181,#49182,
#49183,#49184,#49185,#49186,#49187,#49188,#49189,#49190,#49191,#49192,#49193,
#49194,#49195,#49196,#49197,#49198,#49199,#49200,#49201,#49202,#49203,#49204,
#49205,#49206,#49207,#49208,#49209,#49210,#49211,#49212,#49213,#49214,#49215,
#49216,#49217,#49218,#49219,#49220,#49221,#49222,#49223,#49224,#49225,#49226,
#49227,#49228,#49229,#49230,#49231,#49232,#49233,#49234,#49235,#49236,#49237,
#49238,#49239,#49240,#49241,#49242,#49243,#49244,#49245,#49246,#49247,#49248,
#49249,#49250),(#49251,#49252,#49253,#49254,#49255,#49256,#49257,#49258,
#49259,#49260,#49261,#49262,#49263,#49264,#49265,#49266,#49267,#49268,#49269,
#49270,#49271,#49272,#49273,#49274,#49275,#49276,#49277,#49278,#49279,#49280,
#49281,#49282,#49283,#49284,#49285,#49286,#49287,#49288,#49289,#49290,#49291,
#49292,#49293,#49294,#49295,#49296,#49297,#49298,#49299,#49300,#49301,#49302,
#49303,#49304,#49305,#49306,#49307,#49308,#49309,#49310,#49311,#49312,#49313,
#49314,#49315,#49316,#49317,#49318,#49319,#49320,#49321,#49322,#49323,#49324,
#49325,#49326,#49327,#49328,#49329,#49330,#49331,#49332,#49333,#49334,#49335,
#49336,#49337,#49338,#49339,#49340,#49341,#49342,#49343,#49344,#49345,#49346,
#49347,#49348,#49349,#49350)),.UNSPECIFIED.,.F.,.F.,.F.,(4,4),(4,1,1,1,
1,1,1,1,1,1,1,1,1,1,1,1,1,1,1,1,1,1,1,1,1,1,1,1,1,1,1,1,1,1,1,1,1,1,1,1,
1,1,1,1,1,1,1,1,1,1,1,1,1,1,1,1,1,1,1,1,1,1,1,1,1,1,1,1,1,1,1,1,1,1,1,1,
1,1,1,1,1,1,1,1,1,1,1,1,1,1,1,1,1,1,1,1,1,4),(0.,0.064201349933887),(14.3984001269718,
15.3908199671854,16.3832398073991,17.3756596476127,18.3680794878263,19.36049932804,
20.3529191682536,21.3453390084673,22.3377588486809,23.3301786888945,24.3225985291082,
25.3150183693218,26.3074382095354,27.2998580497491,28.2922778899627,29.2846977301763,
30.27711757039,31.2695374106036,32.2619572508172,33.2543770910309,34.2467969312445,
35.2392167714581,36.2316366116718,37.2240564518854,38.216476292099,39.2088961323127,
40.2013159725263,41.1937358127399,42.1861556529536,43.1785754931672,44.1709953333808,
45.1634151735945,46.1558350138081,47.1482548540217,48.1406746942354,49.133094534449,
50.1255143746626,51.1179342148763,52.1103540550899,53.1027738953035,54.0951937355172,
55.0876135757308,56.0800334159444,57.0724532561581,58.0648730963717,59.0572929365853,
60.049712776799,61.0421326170126,62.0345524572262,63.0269722974399,64.0193921376535,
65.0118119778672,66.0042318180808,66.9966516582944,67.9890714985081,68.9814913387217,
69.9739111789353,70.966331019149,71.9587508593626,72.9511706995762,73.9435905397899,
74.9360103800035,75.9284302202171,76.9208500604308,77.9132699006444,78.905689740858,
79.8981095810717,80.8905294212853,81.8829492614989,82.8753691017126,83.8677889419262,
84.8602087821398,85.8526286223535,86.8450484625671,87.8374683027807,88.8298881429944,
89.822307983208,90.8147278234216,91.8071476636353,92.7995675038489,93.7919873440625,
94.7844071842762,95.7768270244898,96.7692468647034,97.7616667049171,98.7540865451307,
99.7465063853443,100.738926225558,101.731346065772,102.723765905985,103.716185746199,
104.708605586413,105.701025426626,106.69344526684,107.685865107053,108.678284947267,
109.670704787481,110.663124627694),.UNSPECIFIED.);
#1330=B_SPLINE_SURFACE_WITH_KNOTS('',3,3,((#49679,#49680,#49681,#49682,
#49683,#49684,#49685,#49686,#49687,#49688,#49689,#49690,#49691,#49692,#49693,
#49694,#49695,#49696,#49697,#49698,#49699,#49700,#49701,#49702,#49703,#49704,
#49705,#49706,#49707,#49708,#49709,#49710,#49711,#49712,#49713,#49714,#49715,
#49716,#49717,#49718,#49719,#49720,#49721,#49722,#49723,#49724,#49725,#49726,
#49727,#49728,#49729,#49730,#49731,#49732,#49733,#49734,#49735,#49736,#49737,
#49738,#49739,#49740,#49741,#49742,#49743,#49744,#49745,#49746,#49747,#49748,
#49749,#49750,#49751,#49752,#49753,#49754,#49755,#49756,#49757,#49758,#49759,
#49760,#49761,#49762,#49763,#49764,#49765,#49766,#49767,#49768,#49769,#49770,
#49771,#49772,#49773,#49774,#49775,#49776,#49777,#49778),(#49779,#49780,
#49781,#49782,#49783,#49784,#49785,#49786,#49787,#49788,#49789,#49790,#49791,
#49792,#49793,#49794,#49795,#49796,#49797,#49798,#49799,#49800,#49801,#49802,
#49803,#49804,#49805,#49806,#49807,#49808,#49809,#49810,#49811,#49812,#49813,
#49814,#49815,#49816,#49817,#49818,#49819,#49820,#49821,#49822,#49823,#49824,
#49825,#49826,#49827,#49828,#49829,#49830,#49831,#49832,#49833,#49834,#49835,
#49836,#49837,#49838,#49839,#49840,#49841,#49842,#49843,#49844,#49845,#49846,
#49847,#49848,#49849,#49850,#49851,#49852,#49853,#49854,#49855,#49856,#49857,
#49858,#49859,#49860,#49861,#49862,#49863,#49864,#49865,#49866,#49867,#49868,
#49869,#49870,#49871,#49872,#49873,#49874,#49875,#49876,#49877,#49878),
(#49879,#49880,#49881,#49882,#49883,#49884,#49885,#49886,#49887,#49888,
#49889,#49890,#49891,#49892,#49893,#49894,#49895,#49896,#49897,#49898,#49899,
#49900,#49901,#49902,#49903,#49904,#49905,#49906,#49907,#49908,#49909,#49910,
#49911,#49912,#49913,#49914,#49915,#49916,#49917,#49918,#49919,#49920,#49921,
#49922,#49923,#49924,#49925,#49926,#49927,#49928,#49929,#49930,#49931,#49932,
#49933,#49934,#49935,#49936,#49937,#49938,#49939,#49940,#49941,#49942,#49943,
#49944,#49945,#49946,#49947,#49948,#49949,#49950,#49951,#49952,#49953,#49954,
#49955,#49956,#49957,#49958,#49959,#49960,#49961,#49962,#49963,#49964,#49965,
#49966,#49967,#49968,#49969,#49970,#49971,#49972,#49973,#49974,#49975,#49976,
#49977,#49978),(#49979,#49980,#49981,#49982,#49983,#49984,#49985,#49986,
#49987,#49988,#49989,#49990,#49991,#49992,#49993,#49994,#49995,#49996,#49997,
#49998,#49999,#50000,#50001,#50002,#50003,#50004,#50005,#50006,#50007,#50008,
#50009,#50010,#50011,#50012,#50013,#50014,#50015,#50016,#50017,#50018,#50019,
#50020,#50021,#50022,#50023,#50024,#50025,#50026,#50027,#50028,#50029,#50030,
#50031,#50032,#50033,#50034,#50035,#50036,#50037,#50038,#50039,#50040,#50041,
#50042,#50043,#50044,#50045,#50046,#50047,#50048,#50049,#50050,#50051,#50052,
#50053,#50054,#50055,#50056,#50057,#50058,#50059,#50060,#50061,#50062,#50063,
#50064,#50065,#50066,#50067,#50068,#50069,#50070,#50071,#50072,#50073,#50074,
#50075,#50076,#50077,#50078)),.UNSPECIFIED.,.F.,.F.,.F.,(4,4),(4,1,1,1,
1,1,1,1,1,1,1,1,1,1,1,1,1,1,1,1,1,1,1,1,1,1,1,1,1,1,1,1,1,1,1,1,1,1,1,1,
1,1,1,1,1,1,1,1,1,1,1,1,1,1,1,1,1,1,1,1,1,1,1,1,1,1,1,1,1,1,1,1,1,1,1,1,
1,1,1,1,1,1,1,1,1,1,1,1,1,1,1,1,1,1,1,1,1,4),(0.,0.064201349933887),(11.8589888623078,
12.8514087025215,13.8438285427351,14.8362483829487,15.8286682231624,16.821088063376,
17.8135079035896,18.8059277438032,19.7983475840169,20.7907674242305,21.7831872644441,
22.7756071046578,23.7680269448714,24.760446785085,25.7528666252987,26.7452864655123,
27.7377063057259,28.7301261459396,29.7225459861532,30.7149658263668,31.7073856665805,
32.6998055067941,33.6922253470077,34.6846451872214,35.677065027435,36.6694848676486,
37.6619047078623,38.6543245480759,39.6467443882895,40.6391642285032,41.6315840687168,
42.6240039089304,43.6164237491441,44.6088435893577,45.6012634295713,46.593683269785,
47.5861031099986,48.5785229502122,49.5709427904259,50.5633626306395,51.5557824708531,
52.5482023110668,53.5406221512804,54.533041991494,55.5254618317077,56.5178816719213,
57.5103015121349,58.5027213523486,59.4951411925622,60.4875610327758,61.4799808729895,
62.4724007132031,63.4648205534167,64.4572403936303,65.449660233844,66.4420800740576,
67.4344999142712,68.4269197544849,69.4193395946985,70.4117594349121,71.4041792751258,
72.3965991153394,73.389018955553,74.3814387957667,75.3738586359803,76.3662784761939,
77.3586983164076,78.3511181566212,79.3435379968348,80.3359578370485,81.3283776772621,
82.3207975174757,83.3132173576894,84.305637197903,85.2980570381166,86.2904768783303,
87.2828967185439,88.2753165587575,89.2677363989712,90.2601562391848,91.2525760793984,
92.2449959196121,93.2374157598257,94.2298356000393,95.222255440253,96.2146752804666,
97.2070951206802,98.1995149608939,99.1919348011075,100.184354641321,101.176774481535,
102.169194321748,103.161614161962,104.154034002176,105.146453842389,106.138873682603,
107.131293522817,108.12371336303),.UNSPECIFIED.);
#1331=B_SPLINE_SURFACE_WITH_KNOTS('',3,3,((#50198,#50199,#50200,#50201,
#50202,#50203,#50204,#50205,#50206,#50207,#50208,#50209,#50210,#50211,#50212,
#50213,#50214,#50215,#50216,#50217,#50218,#50219,#50220,#50221,#50222,#50223,
#50224,#50225,#50226,#50227,#50228,#50229,#50230,#50231,#50232,#50233,#50234,
#50235,#50236,#50237,#50238,#50239,#50240,#50241,#50242,#50243,#50244,#50245,
#50246,#50247,#50248,#50249,#50250,#50251,#50252,#50253,#50254,#50255,#50256,
#50257,#50258,#50259,#50260,#50261,#50262,#50263,#50264,#50265,#50266,#50267,
#50268,#50269,#50270,#50271,#50272,#50273,#50274,#50275,#50276,#50277,#50278,
#50279,#50280,#50281,#50282,#50283,#50284,#50285,#50286,#50287,#50288,#50289,
#50290,#50291,#50292,#50293,#50294,#50295,#50296,#50297),(#50298,#50299,
#50300,#50301,#50302,#50303,#50304,#50305,#50306,#50307,#50308,#50309,#50310,
#50311,#50312,#50313,#50314,#50315,#50316,#50317,#50318,#50319,#50320,#50321,
#50322,#50323,#50324,#50325,#50326,#50327,#50328,#50329,#50330,#50331,#50332,
#50333,#50334,#50335,#50336,#50337,#50338,#50339,#50340,#50341,#50342,#50343,
#50344,#50345,#50346,#50347,#50348,#50349,#50350,#50351,#50352,#50353,#50354,
#50355,#50356,#50357,#50358,#50359,#50360,#50361,#50362,#50363,#50364,#50365,
#50366,#50367,#50368,#50369,#50370,#50371,#50372,#50373,#50374,#50375,#50376,
#50377,#50378,#50379,#50380,#50381,#50382,#50383,#50384,#50385,#50386,#50387,
#50388,#50389,#50390,#50391,#50392,#50393,#50394,#50395,#50396,#50397),
(#50398,#50399,#50400,#50401,#50402,#50403,#50404,#50405,#50406,#50407,
#50408,#50409,#50410,#50411,#50412,#50413,#50414,#50415,#50416,#50417,#50418,
#50419,#50420,#50421,#50422,#50423,#50424,#50425,#50426,#50427,#50428,#50429,
#50430,#50431,#50432,#50433,#50434,#50435,#50436,#50437,#50438,#50439,#50440,
#50441,#50442,#50443,#50444,#50445,#50446,#50447,#50448,#50449,#50450,#50451,
#50452,#50453,#50454,#50455,#50456,#50457,#50458,#50459,#50460,#50461,#50462,
#50463,#50464,#50465,#50466,#50467,#50468,#50469,#50470,#50471,#50472,#50473,
#50474,#50475,#50476,#50477,#50478,#50479,#50480,#50481,#50482,#50483,#50484,
#50485,#50486,#50487,#50488,#50489,#50490,#50491,#50492,#50493,#50494,#50495,
#50496,#50497),(#50498,#50499,#50500,#50501,#50502,#50503,#50504,#50505,
#50506,#50507,#50508,#50509,#50510,#50511,#50512,#50513,#50514,#50515,#50516,
#50517,#50518,#50519,#50520,#50521,#50522,#50523,#50524,#50525,#50526,#50527,
#50528,#50529,#50530,#50531,#50532,#50533,#50534,#50535,#50536,#50537,#50538,
#50539,#50540,#50541,#50542,#50543,#50544,#50545,#50546,#50547,#50548,#50549,
#50550,#50551,#50552,#50553,#50554,#50555,#50556,#50557,#50558,#50559,#50560,
#50561,#50562,#50563,#50564,#50565,#50566,#50567,#50568,#50569,#50570,#50571,
#50572,#50573,#50574,#50575,#50576,#50577,#50578,#50579,#50580,#50581,#50582,
#50583,#50584,#50585,#50586,#50587,#50588,#50589,#50590,#50591,#50592,#50593,
#50594,#50595,#50596,#50597)),.UNSPECIFIED.,.F.,.F.,.F.,(4,4),(4,1,1,1,
1,1,1,1,1,1,1,1,1,1,1,1,1,1,1,1,1,1,1,1,1,1,1,1,1,1,1,1,1,1,1,1,1,1,1,1,
1,1,1,1,1,1,1,1,1,1,1,1,1,1,1,1,1,1,1,1,1,1,1,1,1,1,1,1,1,1,1,1,1,1,1,1,
1,1,1,1,1,1,1,1,1,1,1,1,1,1,1,1,1,1,1,1,1,4),(0.,0.064201349933887),(14.3984001269719,
15.3908199671856,16.3832398073992,17.3756596476128,18.3680794878265,19.3604993280401,
20.3529191682537,21.3453390084674,22.337758848681,23.3301786888946,24.3225985291083,
25.3150183693219,26.3074382095355,27.2998580497492,28.2922778899628,29.2846977301764,
30.2771175703901,31.2695374106037,32.2619572508173,33.2543770910309,34.2467969312446,
35.2392167714582,36.2316366116718,37.2240564518855,38.2164762920991,39.2088961323127,
40.2013159725264,41.19373581274,42.1861556529536,43.1785754931673,44.1709953333809,
45.1634151735945,46.1558350138082,47.1482548540218,48.1406746942354,49.1330945344491,
50.1255143746627,51.1179342148763,52.11035405509,53.1027738953036,54.0951937355172,
55.0876135757309,56.0800334159445,57.0724532561581,58.0648730963718,59.0572929365854,
60.049712776799,61.0421326170127,62.0345524572263,63.0269722974399,64.0193921376536,
65.0118119778672,66.0042318180808,66.9966516582945,67.9890714985081,68.9814913387217,
69.9739111789354,70.966331019149,71.9587508593626,72.9511706995763,73.9435905397899,
74.9360103800035,75.9284302202172,76.9208500604308,77.9132699006444,78.9056897408581,
79.8981095810717,80.8905294212853,81.882949261499,82.8753691017126,83.8677889419262,
84.8602087821399,85.8526286223535,86.8450484625671,87.8374683027808,88.8298881429944,
89.822307983208,90.8147278234217,91.8071476636353,92.7995675038489,93.7919873440626,
94.7844071842762,95.7768270244898,96.7692468647035,97.7616667049171,98.7540865451307,
99.7465063853444,100.738926225558,101.731346065772,102.723765905985,103.716185746199,
104.708605586413,105.701025426626,106.69344526684,107.685865107053,108.678284947267,
109.670704787481,110.663124627694),.UNSPECIFIED.);
#1332=B_SPLINE_SURFACE_WITH_KNOTS('',3,3,((#50926,#50927,#50928,#50929,
#50930,#50931,#50932,#50933,#50934,#50935,#50936,#50937,#50938,#50939,#50940,
#50941,#50942,#50943,#50944,#50945,#50946,#50947,#50948,#50949,#50950,#50951,
#50952,#50953,#50954,#50955,#50956,#50957,#50958,#50959,#50960,#50961,#50962,
#50963,#50964,#50965,#50966,#50967,#50968,#50969,#50970,#50971,#50972,#50973,
#50974,#50975,#50976,#50977,#50978,#50979,#50980,#50981,#50982,#50983,#50984,
#50985,#50986,#50987,#50988,#50989,#50990,#50991,#50992,#50993,#50994,#50995,
#50996,#50997,#50998,#50999,#51000,#51001,#51002,#51003,#51004,#51005,#51006,
#51007,#51008,#51009,#51010,#51011,#51012,#51013,#51014,#51015,#51016,#51017,
#51018,#51019,#51020,#51021,#51022,#51023,#51024,#51025),(#51026,#51027,
#51028,#51029,#51030,#51031,#51032,#51033,#51034,#51035,#51036,#51037,#51038,
#51039,#51040,#51041,#51042,#51043,#51044,#51045,#51046,#51047,#51048,#51049,
#51050,#51051,#51052,#51053,#51054,#51055,#51056,#51057,#51058,#51059,#51060,
#51061,#51062,#51063,#51064,#51065,#51066,#51067,#51068,#51069,#51070,#51071,
#51072,#51073,#51074,#51075,#51076,#51077,#51078,#51079,#51080,#51081,#51082,
#51083,#51084,#51085,#51086,#51087,#51088,#51089,#51090,#51091,#51092,#51093,
#51094,#51095,#51096,#51097,#51098,#51099,#51100,#51101,#51102,#51103,#51104,
#51105,#51106,#51107,#51108,#51109,#51110,#51111,#51112,#51113,#51114,#51115,
#51116,#51117,#51118,#51119,#51120,#51121,#51122,#51123,#51124,#51125),
(#51126,#51127,#51128,#51129,#51130,#51131,#51132,#51133,#51134,#51135,
#51136,#51137,#51138,#51139,#51140,#51141,#51142,#51143,#51144,#51145,#51146,
#51147,#51148,#51149,#51150,#51151,#51152,#51153,#51154,#51155,#51156,#51157,
#51158,#51159,#51160,#51161,#51162,#51163,#51164,#51165,#51166,#51167,#51168,
#51169,#51170,#51171,#51172,#51173,#51174,#51175,#51176,#51177,#51178,#51179,
#51180,#51181,#51182,#51183,#51184,#51185,#51186,#51187,#51188,#51189,#51190,
#51191,#51192,#51193,#51194,#51195,#51196,#51197,#51198,#51199,#51200,#51201,
#51202,#51203,#51204,#51205,#51206,#51207,#51208,#51209,#51210,#51211,#51212,
#51213,#51214,#51215,#51216,#51217,#51218,#51219,#51220,#51221,#51222,#51223,
#51224,#51225),(#51226,#51227,#51228,#51229,#51230,#51231,#51232,#51233,
#51234,#51235,#51236,#51237,#51238,#51239,#51240,#51241,#51242,#51243,#51244,
#51245,#51246,#51247,#51248,#51249,#51250,#51251,#51252,#51253,#51254,#51255,
#51256,#51257,#51258,#51259,#51260,#51261,#51262,#51263,#51264,#51265,#51266,
#51267,#51268,#51269,#51270,#51271,#51272,#51273,#51274,#51275,#51276,#51277,
#51278,#51279,#51280,#51281,#51282,#51283,#51284,#51285,#51286,#51287,#51288,
#51289,#51290,#51291,#51292,#51293,#51294,#51295,#51296,#51297,#51298,#51299,
#51300,#51301,#51302,#51303,#51304,#51305,#51306,#51307,#51308,#51309,#51310,
#51311,#51312,#51313,#51314,#51315,#51316,#51317,#51318,#51319,#51320,#51321,
#51322,#51323,#51324,#51325)),.UNSPECIFIED.,.F.,.F.,.F.,(4,4),(4,1,1,1,
1,1,1,1,1,1,1,1,1,1,1,1,1,1,1,1,1,1,1,1,1,1,1,1,1,1,1,1,1,1,1,1,1,1,1,1,
1,1,1,1,1,1,1,1,1,1,1,1,1,1,1,1,1,1,1,1,1,1,1,1,1,1,1,1,1,1,1,1,1,1,1,1,
1,1,1,1,1,1,1,1,1,1,1,1,1,1,1,1,1,1,1,1,1,4),(0.,0.064201349933887),(11.8589888623078,
12.8514087025215,13.8438285427351,14.8362483829487,15.8286682231624,16.821088063376,
17.8135079035896,18.8059277438032,19.7983475840169,20.7907674242305,21.7831872644441,
22.7756071046578,23.7680269448714,24.760446785085,25.7528666252987,26.7452864655123,
27.7377063057259,28.7301261459396,29.7225459861532,30.7149658263668,31.7073856665805,
32.6998055067941,33.6922253470077,34.6846451872214,35.677065027435,36.6694848676486,
37.6619047078623,38.6543245480759,39.6467443882895,40.6391642285032,41.6315840687168,
42.6240039089304,43.6164237491441,44.6088435893577,45.6012634295713,46.593683269785,
47.5861031099986,48.5785229502122,49.5709427904259,50.5633626306395,51.5557824708531,
52.5482023110668,53.5406221512804,54.533041991494,55.5254618317077,56.5178816719213,
57.5103015121349,58.5027213523486,59.4951411925622,60.4875610327758,61.4799808729895,
62.4724007132031,63.4648205534167,64.4572403936303,65.449660233844,66.4420800740576,
67.4344999142712,68.4269197544849,69.4193395946985,70.4117594349121,71.4041792751258,
72.3965991153394,73.389018955553,74.3814387957667,75.3738586359803,76.3662784761939,
77.3586983164076,78.3511181566212,79.3435379968348,80.3359578370485,81.3283776772621,
82.3207975174757,83.3132173576894,84.305637197903,85.2980570381166,86.2904768783303,
87.2828967185439,88.2753165587575,89.2677363989712,90.2601562391848,91.2525760793984,
92.2449959196121,93.2374157598257,94.2298356000393,95.222255440253,96.2146752804666,
97.2070951206802,98.1995149608939,99.1919348011075,100.184354641321,101.176774481535,
102.169194321748,103.161614161962,104.154034002176,105.146453842389,106.138873682603,
107.131293522817,108.12371336303),.UNSPECIFIED.);
#1333=B_SPLINE_SURFACE_WITH_KNOTS('',3,3,((#51445,#51446,#51447,#51448,
#51449,#51450,#51451,#51452,#51453,#51454,#51455,#51456,#51457,#51458,#51459,
#51460,#51461,#51462,#51463,#51464,#51465,#51466,#51467,#51468,#51469,#51470,
#51471,#51472,#51473,#51474,#51475,#51476,#51477,#51478,#51479,#51480,#51481,
#51482,#51483,#51484,#51485,#51486,#51487,#51488,#51489,#51490,#51491,#51492,
#51493,#51494,#51495,#51496,#51497,#51498,#51499,#51500,#51501,#51502,#51503,
#51504,#51505,#51506,#51507,#51508,#51509,#51510,#51511,#51512,#51513,#51514,
#51515,#51516,#51517,#51518,#51519,#51520,#51521,#51522,#51523,#51524,#51525,
#51526,#51527,#51528,#51529,#51530,#51531,#51532,#51533,#51534,#51535,#51536,
#51537,#51538,#51539,#51540,#51541,#51542,#51543,#51544),(#51545,#51546,
#51547,#51548,#51549,#51550,#51551,#51552,#51553,#51554,#51555,#51556,#51557,
#51558,#51559,#51560,#51561,#51562,#51563,#51564,#51565,#51566,#51567,#51568,
#51569,#51570,#51571,#51572,#51573,#51574,#51575,#51576,#51577,#51578,#51579,
#51580,#51581,#51582,#51583,#51584,#51585,#51586,#51587,#51588,#51589,#51590,
#51591,#51592,#51593,#51594,#51595,#51596,#51597,#51598,#51599,#51600,#51601,
#51602,#51603,#51604,#51605,#51606,#51607,#51608,#51609,#51610,#51611,#51612,
#51613,#51614,#51615,#51616,#51617,#51618,#51619,#51620,#51621,#51622,#51623,
#51624,#51625,#51626,#51627,#51628,#51629,#51630,#51631,#51632,#51633,#51634,
#51635,#51636,#51637,#51638,#51639,#51640,#51641,#51642,#51643,#51644),
(#51645,#51646,#51647,#51648,#51649,#51650,#51651,#51652,#51653,#51654,
#51655,#51656,#51657,#51658,#51659,#51660,#51661,#51662,#51663,#51664,#51665,
#51666,#51667,#51668,#51669,#51670,#51671,#51672,#51673,#51674,#51675,#51676,
#51677,#51678,#51679,#51680,#51681,#51682,#51683,#51684,#51685,#51686,#51687,
#51688,#51689,#51690,#51691,#51692,#51693,#51694,#51695,#51696,#51697,#51698,
#51699,#51700,#51701,#51702,#51703,#51704,#51705,#51706,#51707,#51708,#51709,
#51710,#51711,#51712,#51713,#51714,#51715,#51716,#51717,#51718,#51719,#51720,
#51721,#51722,#51723,#51724,#51725,#51726,#51727,#51728,#51729,#51730,#51731,
#51732,#51733,#51734,#51735,#51736,#51737,#51738,#51739,#51740,#51741,#51742,
#51743,#51744),(#51745,#51746,#51747,#51748,#51749,#51750,#51751,#51752,
#51753,#51754,#51755,#51756,#51757,#51758,#51759,#51760,#51761,#51762,#51763,
#51764,#51765,#51766,#51767,#51768,#51769,#51770,#51771,#51772,#51773,#51774,
#51775,#51776,#51777,#51778,#51779,#51780,#51781,#51782,#51783,#51784,#51785,
#51786,#51787,#51788,#51789,#51790,#51791,#51792,#51793,#51794,#51795,#51796,
#51797,#51798,#51799,#51800,#51801,#51802,#51803,#51804,#51805,#51806,#51807,
#51808,#51809,#51810,#51811,#51812,#51813,#51814,#51815,#51816,#51817,#51818,
#51819,#51820,#51821,#51822,#51823,#51824,#51825,#51826,#51827,#51828,#51829,
#51830,#51831,#51832,#51833,#51834,#51835,#51836,#51837,#51838,#51839,#51840,
#51841,#51842,#51843,#51844)),.UNSPECIFIED.,.F.,.F.,.F.,(4,4),(4,1,1,1,
1,1,1,1,1,1,1,1,1,1,1,1,1,1,1,1,1,1,1,1,1,1,1,1,1,1,1,1,1,1,1,1,1,1,1,1,
1,1,1,1,1,1,1,1,1,1,1,1,1,1,1,1,1,1,1,1,1,1,1,1,1,1,1,1,1,1,1,1,1,1,1,1,
1,1,1,1,1,1,1,1,1,1,1,1,1,1,1,1,1,1,1,1,1,4),(0.,0.064201349933887),(14.3984001269719,
15.3908199671856,16.3832398073992,17.3756596476128,18.3680794878265,19.3604993280401,
20.3529191682537,21.3453390084674,22.337758848681,23.3301786888946,24.3225985291083,
25.3150183693219,26.3074382095355,27.2998580497492,28.2922778899628,29.2846977301764,
30.2771175703901,31.2695374106037,32.2619572508173,33.2543770910309,34.2467969312446,
35.2392167714582,36.2316366116718,37.2240564518855,38.2164762920991,39.2088961323127,
40.2013159725264,41.19373581274,42.1861556529536,43.1785754931673,44.1709953333809,
45.1634151735945,46.1558350138082,47.1482548540218,48.1406746942354,49.1330945344491,
50.1255143746627,51.1179342148763,52.11035405509,53.1027738953036,54.0951937355172,
55.0876135757309,56.0800334159445,57.0724532561581,58.0648730963718,59.0572929365854,
60.049712776799,61.0421326170127,62.0345524572263,63.0269722974399,64.0193921376536,
65.0118119778672,66.0042318180808,66.9966516582945,67.9890714985081,68.9814913387217,
69.9739111789354,70.966331019149,71.9587508593626,72.9511706995763,73.9435905397899,
74.9360103800035,75.9284302202172,76.9208500604308,77.9132699006444,78.9056897408581,
79.8981095810717,80.8905294212853,81.882949261499,82.8753691017126,83.8677889419262,
84.8602087821399,85.8526286223535,86.8450484625671,87.8374683027808,88.8298881429944,
89.822307983208,90.8147278234217,91.8071476636353,92.7995675038489,93.7919873440626,
94.7844071842762,95.7768270244898,96.7692468647035,97.7616667049171,98.7540865451307,
99.7465063853444,100.738926225558,101.731346065772,102.723765905985,103.716185746199,
104.708605586413,105.701025426626,106.69344526684,107.685865107053,108.678284947267,
109.670704787481,110.663124627694),.UNSPECIFIED.);
#1334=B_SPLINE_SURFACE_WITH_KNOTS('',3,3,((#52576,#52577,#52578,#52579),
(#52580,#52581,#52582,#52583),(#52584,#52585,#52586,#52587),(#52588,#52589,
#52590,#52591),(#52592,#52593,#52594,#52595)),.UNSPECIFIED.,.F.,.F.,.F.,
(4,1,4),(4,4),(0.,0.571428571428571,1.),(-2.77555756156289E-17,1.2),
 .UNSPECIFIED.);
#1335=B_SPLINE_SURFACE_WITH_KNOTS('',3,3,((#53423,#53424,#53425,#53426),
(#53427,#53428,#53429,#53430),(#53431,#53432,#53433,#53434),(#53435,#53436,
#53437,#53438),(#53439,#53440,#53441,#53442)),.UNSPECIFIED.,.F.,.F.,.F.,
(4,1,4),(4,4),(0.,0.571428571428571,1.),(0.,1.2),.UNSPECIFIED.);
#1336=B_SPLINE_SURFACE_WITH_KNOTS('',3,3,((#53472,#53473,#53474,#53475),
(#53476,#53477,#53478,#53479),(#53480,#53481,#53482,#53483),(#53484,#53485,
#53486,#53487),(#53488,#53489,#53490,#53491)),.UNSPECIFIED.,.F.,.F.,.F.,
(4,1,4),(4,4),(0.,0.571428571428571,1.),(9.71445146547012E-17,1.2),
 .UNSPECIFIED.);
#1337=B_SPLINE_SURFACE_WITH_KNOTS('',3,3,((#54319,#54320,#54321,#54322),
(#54323,#54324,#54325,#54326),(#54327,#54328,#54329,#54330),(#54331,#54332,
#54333,#54334),(#54335,#54336,#54337,#54338)),.UNSPECIFIED.,.F.,.F.,.F.,
(4,1,4),(4,4),(0.,0.571428571428571,1.),(-6.97125684381022E-36,1.2),
 .UNSPECIFIED.);
#1338=B_SPLINE_SURFACE_WITH_KNOTS('',3,3,((#54368,#54369,#54370,#54371),
(#54372,#54373,#54374,#54375),(#54376,#54377,#54378,#54379),(#54380,#54381,
#54382,#54383),(#54384,#54385,#54386,#54387)),.UNSPECIFIED.,.F.,.F.,.F.,
(4,1,4),(4,4),(0.,0.571428571428571,1.),(4.06042677328019E-17,1.2),
 .UNSPECIFIED.);
#1339=B_SPLINE_SURFACE_WITH_KNOTS('',3,3,((#55215,#55216,#55217,#55218),
(#55219,#55220,#55221,#55222),(#55223,#55224,#55225,#55226),(#55227,#55228,
#55229,#55230),(#55231,#55232,#55233,#55234)),.UNSPECIFIED.,.F.,.F.,.F.,
(4,1,4),(4,4),(0.,0.571428571428571,1.),(-8.32667268468868E-17,1.2),
 .UNSPECIFIED.);
#1340=B_SPLINE_SURFACE_WITH_KNOTS('',3,3,((#55264,#55265,#55266,#55267),
(#55268,#55269,#55270,#55271),(#55272,#55273,#55274,#55275),(#55276,#55277,
#55278,#55279),(#55280,#55281,#55282,#55283)),.UNSPECIFIED.,.F.,.F.,.F.,
(4,1,4),(4,4),(0.,0.571428571428571,1.),(9.71445146547012E-17,1.2),
 .UNSPECIFIED.);
#1341=B_SPLINE_SURFACE_WITH_KNOTS('',3,3,((#56111,#56112,#56113,#56114),
(#56115,#56116,#56117,#56118),(#56119,#56120,#56121,#56122),(#56123,#56124,
#56125,#56126),(#56127,#56128,#56129,#56130)),.UNSPECIFIED.,.F.,.F.,.F.,
(4,1,4),(4,4),(0.,0.571428571428571,1.),(2.77555756156289E-17,1.2),
 .UNSPECIFIED.);
#1342=B_SPLINE_SURFACE_WITH_KNOTS('',3,3,((#56160,#56161,#56162,#56163),
(#56164,#56165,#56166,#56167),(#56168,#56169,#56170,#56171),(#56172,#56173,
#56174,#56175),(#56176,#56177,#56178,#56179)),.UNSPECIFIED.,.F.,.F.,.F.,
(4,1,4),(4,4),(0.,0.571428571428571,1.),(1.66533453693773E-16,1.2),
 .UNSPECIFIED.);
#1343=B_SPLINE_SURFACE_WITH_KNOTS('',3,3,((#57007,#57008,#57009,#57010),
(#57011,#57012,#57013,#57014),(#57015,#57016,#57017,#57018),(#57019,#57020,
#57021,#57022),(#57023,#57024,#57025,#57026)),.UNSPECIFIED.,.F.,.F.,.F.,
(4,1,4),(4,4),(0.,0.571428571428571,1.),(-4.16333634234434E-17,1.2),
 .UNSPECIFIED.);
#1344=B_SPLINE_SURFACE_WITH_KNOTS('',3,3,((#57056,#57057,#57058,#57059),
(#57060,#57061,#57062,#57063),(#57064,#57065,#57066,#57067),(#57068,#57069,
#57070,#57071),(#57072,#57073,#57074,#57075)),.UNSPECIFIED.,.F.,.F.,.F.,
(4,1,4),(4,4),(0.,0.571428571428571,1.),(1.38777878078145E-16,1.2),
 .UNSPECIFIED.);
#1345=B_SPLINE_SURFACE_WITH_KNOTS('',3,3,((#57903,#57904,#57905,#57906),
(#57907,#57908,#57909,#57910),(#57911,#57912,#57913,#57914),(#57915,#57916,
#57917,#57918),(#57919,#57920,#57921,#57922)),.UNSPECIFIED.,.F.,.F.,.F.,
(4,1,4),(4,4),(0.,0.571428571428571,1.),(-8.43563892506861E-17,1.2),
 .UNSPECIFIED.);
#1346=B_SPLINE_SURFACE_WITH_KNOTS('',3,3,((#57952,#57953,#57954,#57955),
(#57956,#57957,#57958,#57959),(#57960,#57961,#57962,#57963),(#57964,#57965,
#57966,#57967),(#57968,#57969,#57970,#57971)),.UNSPECIFIED.,.F.,.F.,.F.,
(4,1,4),(4,4),(0.,0.571428571428571,1.),(1.66533453693773E-16,1.2),
 .UNSPECIFIED.);
#1347=B_SPLINE_SURFACE_WITH_KNOTS('',3,3,((#58799,#58800,#58801,#58802),
(#58803,#58804,#58805,#58806),(#58807,#58808,#58809,#58810),(#58811,#58812,
#58813,#58814),(#58815,#58816,#58817,#58818)),.UNSPECIFIED.,.F.,.F.,.F.,
(4,1,4),(4,4),(0.,0.571428571428571,1.),(2.77555756156289E-17,1.2),
 .UNSPECIFIED.);
#1348=B_SPLINE_SURFACE_WITH_KNOTS('',3,3,((#58848,#58849,#58850,#58851),
(#58852,#58853,#58854,#58855),(#58856,#58857,#58858,#58859),(#58860,#58861,
#58862,#58863),(#58864,#58865,#58866,#58867)),.UNSPECIFIED.,.F.,.F.,.F.,
(4,1,4),(4,4),(0.,0.571428571428571,1.),(-8.32667268468868E-17,1.2),
 .UNSPECIFIED.);
#1349=B_SPLINE_SURFACE_WITH_KNOTS('',3,3,((#59695,#59696,#59697,#59698),
(#59699,#59700,#59701,#59702),(#59703,#59704,#59705,#59706),(#59707,#59708,
#59709,#59710),(#59711,#59712,#59713,#59714)),.UNSPECIFIED.,.F.,.F.,.F.,
(4,1,4),(4,4),(0.,0.571428571428571,1.),(5.55111512312578E-17,1.2),
 .UNSPECIFIED.);
#1350=B_SPLINE_SURFACE_WITH_KNOTS('',3,3,((#59744,#59745,#59746,#59747),
(#59748,#59749,#59750,#59751),(#59752,#59753,#59754,#59755),(#59756,#59757,
#59758,#59759),(#59760,#59761,#59762,#59763)),.UNSPECIFIED.,.F.,.F.,.F.,
(4,1,4),(4,4),(0.,0.571428571428571,1.),(1.66533453693773E-16,1.2),
 .UNSPECIFIED.);
#1351=B_SPLINE_SURFACE_WITH_KNOTS('',3,3,((#60591,#60592,#60593,#60594),
(#60595,#60596,#60597,#60598),(#60599,#60600,#60601,#60602),(#60603,#60604,
#60605,#60606),(#60607,#60608,#60609,#60610)),.UNSPECIFIED.,.F.,.F.,.F.,
(4,1,4),(4,4),(0.,0.571428571428571,1.),(-8.9628248557339E-17,1.2),
 .UNSPECIFIED.);
#1352=B_SPLINE_SURFACE_WITH_KNOTS('',3,3,((#60640,#60641,#60642,#60643),
(#60644,#60645,#60646,#60647),(#60648,#60649,#60650,#60651),(#60652,#60653,
#60654,#60655),(#60656,#60657,#60658,#60659)),.UNSPECIFIED.,.F.,.F.,.F.,
(4,1,4),(4,4),(0.,0.571428571428571,1.),(8.0522471671843E-17,1.2),
 .UNSPECIFIED.);
#1353=B_SPLINE_SURFACE_WITH_KNOTS('',3,3,((#61487,#61488,#61489,#61490),
(#61491,#61492,#61493,#61494),(#61495,#61496,#61497,#61498),(#61499,#61500,
#61501,#61502),(#61503,#61504,#61505,#61506)),.UNSPECIFIED.,.F.,.F.,.F.,
(4,1,4),(4,4),(0.,0.571428571428571,1.),(-7.52391395153922E-36,1.2),
 .UNSPECIFIED.);
#1354=B_SPLINE_SURFACE_WITH_KNOTS('',3,3,((#61536,#61537,#61538,#61539),
(#61540,#61541,#61542,#61543),(#61544,#61545,#61546,#61547),(#61548,#61549,
#61550,#61551),(#61552,#61553,#61554,#61555)),.UNSPECIFIED.,.F.,.F.,.F.,
(4,1,4),(4,4),(0.,0.571428571428571,1.),(9.71445146547012E-17,1.2),
 .UNSPECIFIED.);
#1355=B_SPLINE_SURFACE_WITH_KNOTS('',3,3,((#62383,#62384,#62385,#62386),
(#62387,#62388,#62389,#62390),(#62391,#62392,#62393,#62394),(#62395,#62396,
#62397,#62398),(#62399,#62400,#62401,#62402)),.UNSPECIFIED.,.F.,.F.,.F.,
(4,1,4),(4,4),(0.,0.571428571428571,1.),(2.77555756156289E-17,1.2),
 .UNSPECIFIED.);
#1356=B_SPLINE_SURFACE_WITH_KNOTS('',3,3,((#62432,#62433,#62434,#62435),
(#62436,#62437,#62438,#62439),(#62440,#62441,#62442,#62443),(#62444,#62445,
#62446,#62447),(#62448,#62449,#62450,#62451)),.UNSPECIFIED.,.F.,.F.,.F.,
(4,1,4),(4,4),(0.,0.571428571428571,1.),(6.66446838640284E-17,1.2),
 .UNSPECIFIED.);
#1357=B_SPLINE_SURFACE_WITH_KNOTS('',3,3,((#63279,#63280,#63281,#63282),
(#63283,#63284,#63285,#63286),(#63287,#63288,#63289,#63290),(#63291,#63292,
#63293,#63294),(#63295,#63296,#63297,#63298)),.UNSPECIFIED.,.F.,.F.,.F.,
(4,1,4),(4,4),(0.,0.571428571428571,1.),(-4.16333634234434E-17,1.2),
 .UNSPECIFIED.);
#1358=B_SPLINE_SURFACE_WITH_KNOTS('',3,3,((#63328,#63329,#63330,#63331),
(#63332,#63333,#63334,#63335),(#63336,#63337,#63338,#63339),(#63340,#63341,
#63342,#63343),(#63344,#63345,#63346,#63347)),.UNSPECIFIED.,.F.,.F.,.F.,
(4,1,4),(4,4),(0.,0.571428571428571,1.),(0.,1.2),.UNSPECIFIED.);
#1359=B_SPLINE_SURFACE_WITH_KNOTS('',3,3,((#64175,#64176,#64177,#64178),
(#64179,#64180,#64181,#64182),(#64183,#64184,#64185,#64186),(#64187,#64188,
#64189,#64190),(#64191,#64192,#64193,#64194)),.UNSPECIFIED.,.F.,.F.,.F.,
(4,1,4),(4,4),(0.,0.571428571428571,1.),(2.77555756156289E-17,1.2),
 .UNSPECIFIED.);
#1360=B_SPLINE_SURFACE_WITH_KNOTS('',3,3,((#64224,#64225,#64226,#64227),
(#64228,#64229,#64230,#64231),(#64232,#64233,#64234,#64235),(#64236,#64237,
#64238,#64239),(#64240,#64241,#64242,#64243)),.UNSPECIFIED.,.F.,.F.,.F.,
(4,1,4),(4,4),(0.,0.571428571428571,1.),(9.71445146547012E-17,1.2),
 .UNSPECIFIED.);
#1361=B_SPLINE_SURFACE_WITH_KNOTS('',3,3,((#65071,#65072,#65073,#65074),
(#65075,#65076,#65077,#65078),(#65079,#65080,#65081,#65082),(#65083,#65084,
#65085,#65086),(#65087,#65088,#65089,#65090)),.UNSPECIFIED.,.F.,.F.,.F.,
(4,1,4),(4,4),(0.,0.571428571428571,1.),(-1.11022302462516E-16,1.2),
 .UNSPECIFIED.);
#1362=B_SPLINE_SURFACE_WITH_KNOTS('',3,3,((#65120,#65121,#65122,#65123),
(#65124,#65125,#65126,#65127),(#65128,#65129,#65130,#65131),(#65132,#65133,
#65134,#65135),(#65136,#65137,#65138,#65139)),.UNSPECIFIED.,.F.,.F.,.F.,
(4,1,4),(4,4),(0.,0.571428571428571,1.),(6.66446838640285E-17,1.2),
 .UNSPECIFIED.);
#1363=B_SPLINE_SURFACE_WITH_KNOTS('',3,3,((#65967,#65968,#65969,#65970),
(#65971,#65972,#65973,#65974),(#65975,#65976,#65977,#65978),(#65979,#65980,
#65981,#65982),(#65983,#65984,#65985,#65986)),.UNSPECIFIED.,.F.,.F.,.F.,
(4,1,4),(4,4),(0.,0.571428571428571,1.),(2.77555756156289E-17,1.2),
 .UNSPECIFIED.);
#1364=B_SPLINE_SURFACE_WITH_KNOTS('',3,3,((#66016,#66017,#66018,#66019),
(#66020,#66021,#66022,#66023),(#66024,#66025,#66026,#66027),(#66028,#66029,
#66030,#66031),(#66032,#66033,#66034,#66035)),.UNSPECIFIED.,.F.,.F.,.F.,
(4,1,4),(4,4),(0.,0.571428571428571,1.),(6.93889390390723E-17,1.2),
 .UNSPECIFIED.);
#1365=B_SPLINE_SURFACE_WITH_KNOTS('',3,3,((#66863,#66864,#66865,#66866),
(#66867,#66868,#66869,#66870),(#66871,#66872,#66873,#66874),(#66875,#66876,
#66877,#66878),(#66879,#66880,#66881,#66882)),.UNSPECIFIED.,.F.,.F.,.F.,
(4,1,4),(4,4),(0.,0.571428571428571,1.),(0.,1.2),.UNSPECIFIED.);
#1366=B_SPLINE_SURFACE_WITH_KNOTS('',3,3,((#66912,#66913,#66914,#66915),
(#66916,#66917,#66918,#66919),(#66920,#66921,#66922,#66923),(#66924,#66925,
#66926,#66927),(#66928,#66929,#66930,#66931)),.UNSPECIFIED.,.F.,.F.,.F.,
(4,1,4),(4,4),(0.,0.571428571428571,1.),(8.32667268468867E-17,1.2),
 .UNSPECIFIED.);
#1367=B_SPLINE_SURFACE_WITH_KNOTS('',3,3,((#67759,#67760,#67761,#67762),
(#67763,#67764,#67765,#67766),(#67767,#67768,#67769,#67770),(#67771,#67772,
#67773,#67774),(#67775,#67776,#67777,#67778)),.UNSPECIFIED.,.F.,.F.,.F.,
(4,1,4),(4,4),(0.,0.571428571428571,1.),(-5.55111512312578E-17,1.2),
 .UNSPECIFIED.);
#1368=B_SPLINE_SURFACE_WITH_KNOTS('',3,3,((#67808,#67809,#67810,#67811),
(#67812,#67813,#67814,#67815),(#67816,#67817,#67818,#67819),(#67820,#67821,
#67822,#67823),(#67824,#67825,#67826,#67827)),.UNSPECIFIED.,.F.,.F.,.F.,
(4,1,4),(4,4),(0.,0.571428571428571,1.),(0.,1.2),.UNSPECIFIED.);
#1369=B_SPLINE_SURFACE_WITH_KNOTS('',3,3,((#68655,#68656,#68657,#68658),
(#68659,#68660,#68661,#68662),(#68663,#68664,#68665,#68666),(#68667,#68668,
#68669,#68670),(#68671,#68672,#68673,#68674)),.UNSPECIFIED.,.F.,.F.,.F.,
(4,1,4),(4,4),(0.,0.571428571428571,1.),(-8.32667268468868E-17,1.2),
 .UNSPECIFIED.);
#1370=B_SPLINE_SURFACE_WITH_KNOTS('',3,3,((#68704,#68705,#68706,#68707),
(#68708,#68709,#68710,#68711),(#68712,#68713,#68714,#68715),(#68716,#68717,
#68718,#68719),(#68720,#68721,#68722,#68723)),.UNSPECIFIED.,.F.,.F.,.F.,
(4,1,4),(4,4),(0.,0.571428571428571,1.),(9.71445146547012E-17,1.2),
 .UNSPECIFIED.);
#1371=B_SPLINE_SURFACE_WITH_KNOTS('',3,3,((#69551,#69552,#69553,#69554),
(#69555,#69556,#69557,#69558),(#69559,#69560,#69561,#69562),(#69563,#69564,
#69565,#69566),(#69567,#69568,#69569,#69570)),.UNSPECIFIED.,.F.,.F.,.F.,
(4,1,4),(4,4),(0.,0.571428571428571,1.),(-2.74425517504386E-18,1.2),
 .UNSPECIFIED.);
#1372=B_SPLINE_SURFACE_WITH_KNOTS('',3,3,((#69600,#69601,#69602,#69603),
(#69604,#69605,#69606,#69607),(#69608,#69609,#69610,#69611),(#69612,#69613,
#69614,#69615),(#69616,#69617,#69618,#69619)),.UNSPECIFIED.,.F.,.F.,.F.,
(4,1,4),(4,4),(0.,0.571428571428571,1.),(8.0522471671843E-17,1.2),
 .UNSPECIFIED.);
#1373=B_SPLINE_SURFACE_WITH_KNOTS('',3,3,((#70447,#70448,#70449,#70450),
(#70451,#70452,#70453,#70454),(#70455,#70456,#70457,#70458),(#70459,#70460,
#70461,#70462),(#70463,#70464,#70465,#70466)),.UNSPECIFIED.,.F.,.F.,.F.,
(4,1,4),(4,4),(0.,0.571428571428571,1.),(-1.38777878078145E-16,1.2),
 .UNSPECIFIED.);
#1374=B_SPLINE_SURFACE_WITH_KNOTS('',3,3,((#70496,#70497,#70498,#70499),
(#70500,#70501,#70502,#70503),(#70504,#70505,#70506,#70507),(#70508,#70509,
#70510,#70511),(#70512,#70513,#70514,#70515)),.UNSPECIFIED.,.F.,.F.,.F.,
(4,1,4),(4,4),(0.,0.571428571428571,1.),(8.32667268468867E-17,1.2),
 .UNSPECIFIED.);
#1375=B_SPLINE_SURFACE_WITH_KNOTS('',3,3,((#71343,#71344,#71345,#71346),
(#71347,#71348,#71349,#71350),(#71351,#71352,#71353,#71354),(#71355,#71356,
#71357,#71358),(#71359,#71360,#71361,#71362)),.UNSPECIFIED.,.F.,.F.,.F.,
(4,1,4),(4,4),(0.,0.571428571428571,1.),(0.,1.2),.UNSPECIFIED.);
#1376=B_SPLINE_SURFACE_WITH_KNOTS('',3,3,((#71392,#71393,#71394,#71395),
(#71396,#71397,#71398,#71399),(#71400,#71401,#71402,#71403),(#71404,#71405,
#71406,#71407),(#71408,#71409,#71410,#71411)),.UNSPECIFIED.,.F.,.F.,.F.,
(4,1,4),(4,4),(0.,0.571428571428571,1.),(1.66533453693773E-16,1.2),
 .UNSPECIFIED.);
#1377=B_SPLINE_SURFACE_WITH_KNOTS('',3,3,((#72239,#72240,#72241,#72242),
(#72243,#72244,#72245,#72246),(#72247,#72248,#72249,#72250),(#72251,#72252,
#72253,#72254),(#72255,#72256,#72257,#72258)),.UNSPECIFIED.,.F.,.F.,.F.,
(4,1,4),(4,4),(0.,0.571428571428571,1.),(-1.38777878078145E-16,1.2),
 .UNSPECIFIED.);
#1378=B_SPLINE_SURFACE_WITH_KNOTS('',3,3,((#72288,#72289,#72290,#72291),
(#72292,#72293,#72294,#72295),(#72296,#72297,#72298,#72299),(#72300,#72301,
#72302,#72303),(#72304,#72305,#72306,#72307)),.UNSPECIFIED.,.F.,.F.,.F.,
(4,1,4),(4,4),(0.,0.571428571428571,1.),(-2.08166817117217E-17,1.2),
 .UNSPECIFIED.);
#1379=B_SPLINE_SURFACE_WITH_KNOTS('',3,3,((#73135,#73136,#73137,#73138),
(#73139,#73140,#73141,#73142),(#73143,#73144,#73145,#73146),(#73147,#73148,
#73149,#73150),(#73151,#73152,#73153,#73154)),.UNSPECIFIED.,.F.,.F.,.F.,
(4,1,4),(4,4),(0.,0.571428571428571,1.),(-8.32667268468868E-17,1.2),
 .UNSPECIFIED.);
#1380=B_SPLINE_SURFACE_WITH_KNOTS('',3,3,((#73184,#73185,#73186,#73187),
(#73188,#73189,#73190,#73191),(#73192,#73193,#73194,#73195),(#73196,#73197,
#73198,#73199),(#73200,#73201,#73202,#73203)),.UNSPECIFIED.,.F.,.F.,.F.,
(4,1,4),(4,4),(0.,0.571428571428571,1.),(1.38777878078145E-16,1.2),
 .UNSPECIFIED.);
#1381=B_SPLINE_SURFACE_WITH_KNOTS('',3,3,((#74031,#74032,#74033,#74034),
(#74035,#74036,#74037,#74038),(#74039,#74040,#74041,#74042),(#74043,#74044,
#74045,#74046),(#74047,#74048,#74049,#74050)),.UNSPECIFIED.,.F.,.F.,.F.,
(4,1,4),(4,4),(0.,0.571428571428571,1.),(-8.43563892506861E-17,1.2),
 .UNSPECIFIED.);
#1382=B_SPLINE_SURFACE_WITH_KNOTS('',3,3,((#74080,#74081,#74082,#74083),
(#74084,#74085,#74086,#74087),(#74088,#74089,#74090,#74091),(#74092,#74093,
#74094,#74095),(#74096,#74097,#74098,#74099)),.UNSPECIFIED.,.F.,.F.,.F.,
(4,1,4),(4,4),(0.,0.571428571428571,1.),(9.71445146547012E-17,1.2),
 .UNSPECIFIED.);
#1383=B_SPLINE_SURFACE_WITH_KNOTS('',3,3,((#74927,#74928,#74929,#74930),
(#74931,#74932,#74933,#74934),(#74935,#74936,#74937,#74938),(#74939,#74940,
#74941,#74942),(#74943,#74944,#74945,#74946)),.UNSPECIFIED.,.F.,.F.,.F.,
(4,1,4),(4,4),(0.,0.571428571428571,1.),(0.,1.2),.UNSPECIFIED.);
#1384=B_SPLINE_SURFACE_WITH_KNOTS('',3,3,((#74976,#74977,#74978,#74979),
(#74980,#74981,#74982,#74983),(#74984,#74985,#74986,#74987),(#74988,#74989,
#74990,#74991),(#74992,#74993,#74994,#74995)),.UNSPECIFIED.,.F.,.F.,.F.,
(4,1,4),(4,4),(0.,0.571428571428571,1.),(9.71445146547012E-17,1.2),
 .UNSPECIFIED.);
#1385=B_SPLINE_SURFACE_WITH_KNOTS('',3,3,((#75823,#75824,#75825,#75826),
(#75827,#75828,#75829,#75830),(#75831,#75832,#75833,#75834),(#75835,#75836,
#75837,#75838),(#75839,#75840,#75841,#75842)),.UNSPECIFIED.,.F.,.F.,.F.,
(4,1,4),(4,4),(0.,0.571428571428571,1.),(-1.49437708898837E-16,1.2),
 .UNSPECIFIED.);
#1386=B_SPLINE_SURFACE_WITH_KNOTS('',3,3,((#75872,#75873,#75874,#75875),
(#75876,#75877,#75878,#75879),(#75880,#75881,#75882,#75883),(#75884,#75885,
#75886,#75887),(#75888,#75889,#75890,#75891)),.UNSPECIFIED.,.F.,.F.,.F.,
(4,1,4),(4,4),(0.,0.571428571428571,1.),(9.71445146547012E-17,1.2),
 .UNSPECIFIED.);
#1387=B_SPLINE_SURFACE_WITH_KNOTS('',3,3,((#76719,#76720,#76721,#76722),
(#76723,#76724,#76725,#76726),(#76727,#76728,#76729,#76730),(#76731,#76732,
#76733,#76734),(#76735,#76736,#76737,#76738)),.UNSPECIFIED.,.F.,.F.,.F.,
(4,1,4),(4,4),(0.,0.571428571428571,1.),(0.,1.2),.UNSPECIFIED.);
#1388=B_SPLINE_SURFACE_WITH_KNOTS('',3,3,((#76768,#76769,#76770,#76771),
(#76772,#76773,#76774,#76775),(#76776,#76777,#76778,#76779),(#76780,#76781,
#76782,#76783),(#76784,#76785,#76786,#76787)),.UNSPECIFIED.,.F.,.F.,.F.,
(4,1,4),(4,4),(0.,0.571428571428571,1.),(1.66533453693773E-16,1.2),
 .UNSPECIFIED.);
#1389=B_SPLINE_SURFACE_WITH_KNOTS('',3,3,((#77615,#77616,#77617,#77618),
(#77619,#77620,#77621,#77622),(#77623,#77624,#77625,#77626),(#77627,#77628,
#77629,#77630),(#77631,#77632,#77633,#77634)),.UNSPECIFIED.,.F.,.F.,.F.,
(4,1,4),(4,4),(0.,0.571428571428571,1.),(-1.47525527564366E-17,1.2),
 .UNSPECIFIED.);
#1390=B_SPLINE_SURFACE_WITH_KNOTS('',3,3,((#77664,#77665,#77666,#77667),
(#77668,#77669,#77670,#77671),(#77672,#77673,#77674,#77675),(#77676,#77677,
#77678,#77679),(#77680,#77681,#77682,#77683)),.UNSPECIFIED.,.F.,.F.,.F.,
(4,1,4),(4,4),(0.,0.571428571428571,1.),(-8.32667268468867E-17,1.2),
 .UNSPECIFIED.);
#1391=B_SPLINE_SURFACE_WITH_KNOTS('',3,3,((#78511,#78512,#78513,#78514),
(#78515,#78516,#78517,#78518),(#78519,#78520,#78521,#78522),(#78523,#78524,
#78525,#78526),(#78527,#78528,#78529,#78530)),.UNSPECIFIED.,.F.,.F.,.F.,
(4,1,4),(4,4),(0.,0.571428571428571,1.),(2.77555756156289E-17,1.2),
 .UNSPECIFIED.);
#1392=B_SPLINE_SURFACE_WITH_KNOTS('',3,3,((#78560,#78561,#78562,#78563),
(#78564,#78565,#78566,#78567),(#78568,#78569,#78570,#78571),(#78572,#78573,
#78574,#78575),(#78576,#78577,#78578,#78579)),.UNSPECIFIED.,.F.,.F.,.F.,
(4,1,4),(4,4),(0.,0.571428571428571,1.),(9.44002594796574E-17,1.2),
 .UNSPECIFIED.);
#1393=B_SPLINE_SURFACE_WITH_KNOTS('',3,3,((#79407,#79408,#79409,#79410),
(#79411,#79412,#79413,#79414),(#79415,#79416,#79417,#79418),(#79419,#79420,
#79421,#79422),(#79423,#79424,#79425,#79426)),.UNSPECIFIED.,.F.,.F.,.F.,
(4,1,4),(4,4),(0.,0.571428571428571,1.),(0.,1.2),.UNSPECIFIED.);
#1394=B_SPLINE_SURFACE_WITH_KNOTS('',3,3,((#79456,#79457,#79458,#79459),
(#79460,#79461,#79462,#79463),(#79464,#79465,#79466,#79467),(#79468,#79469,
#79470,#79471),(#79472,#79473,#79474,#79475)),.UNSPECIFIED.,.F.,.F.,.F.,
(4,1,4),(4,4),(0.,0.571428571428571,1.),(1.66533453693773E-16,1.2),
 .UNSPECIFIED.);
#1395=B_SPLINE_SURFACE_WITH_KNOTS('',3,3,((#80303,#80304,#80305,#80306),
(#80307,#80308,#80309,#80310),(#80311,#80312,#80313,#80314),(#80315,#80316,
#80317,#80318),(#80319,#80320,#80321,#80322)),.UNSPECIFIED.,.F.,.F.,.F.,
(4,1,4),(4,4),(0.,0.571428571428571,1.),(-1.8224407144634E-16,1.2),
 .UNSPECIFIED.);
#1396=B_SPLINE_SURFACE_WITH_KNOTS('',3,3,((#80352,#80353,#80354,#80355),
(#80356,#80357,#80358,#80359),(#80360,#80361,#80362,#80363),(#80364,#80365,
#80366,#80367),(#80368,#80369,#80370,#80371)),.UNSPECIFIED.,.F.,.F.,.F.,
(4,1,4),(4,4),(0.,0.571428571428571,1.),(-1.8809784878858E-36,1.2),
 .UNSPECIFIED.);
#1397=B_SPLINE_SURFACE_WITH_KNOTS('',3,3,((#81199,#81200,#81201,#81202),
(#81203,#81204,#81205,#81206),(#81207,#81208,#81209,#81210),(#81211,#81212,
#81213,#81214),(#81215,#81216,#81217,#81218)),.UNSPECIFIED.,.F.,.F.,.F.,
(4,1,4),(4,4),(0.,0.571428571428571,1.),(-5.55111512312578E-17,1.2),
 .UNSPECIFIED.);
#1398=B_SPLINE_SURFACE_WITH_KNOTS('',3,3,((#81248,#81249,#81250,#81251),
(#81252,#81253,#81254,#81255),(#81256,#81257,#81258,#81259),(#81260,#81261,
#81262,#81263),(#81264,#81265,#81266,#81267)),.UNSPECIFIED.,.F.,.F.,.F.,
(4,1,4),(4,4),(0.,0.571428571428571,1.),(9.71445146547012E-17,1.2),
 .UNSPECIFIED.);
#1399=B_SPLINE_SURFACE_WITH_KNOTS('',3,3,((#82095,#82096,#82097,#82098),
(#82099,#82100,#82101,#82102),(#82103,#82104,#82105,#82106),(#82107,#82108,
#82109,#82110),(#82111,#82112,#82113,#82114)),.UNSPECIFIED.,.F.,.F.,.F.,
(4,1,4),(4,4),(0.,0.571428571428571,1.),(-8.32667268468867E-17,1.2),
 .UNSPECIFIED.);
#1400=B_SPLINE_SURFACE_WITH_KNOTS('',3,3,((#82144,#82145,#82146,#82147),
(#82148,#82149,#82150,#82151),(#82152,#82153,#82154,#82155),(#82156,#82157,
#82158,#82159),(#82160,#82161,#82162,#82163)),.UNSPECIFIED.,.F.,.F.,.F.,
(4,1,4),(4,4),(0.,0.571428571428571,1.),(0.,1.2),.UNSPECIFIED.);
#1401=B_SPLINE_SURFACE_WITH_KNOTS('',3,3,((#82991,#82992,#82993,#82994),
(#82995,#82996,#82997,#82998),(#82999,#83000,#83001,#83002),(#83003,#83004,
#83005,#83006),(#83007,#83008,#83009,#83010)),.UNSPECIFIED.,.F.,.F.,.F.,
(4,1,4),(4,4),(0.,0.571428571428571,1.),(0.,1.2),.UNSPECIFIED.);
#1402=B_SPLINE_SURFACE_WITH_KNOTS('',3,3,((#83040,#83041,#83042,#83043),
(#83044,#83045,#83046,#83047),(#83048,#83049,#83050,#83051),(#83052,#83053,
#83054,#83055),(#83056,#83057,#83058,#83059)),.UNSPECIFIED.,.F.,.F.,.F.,
(4,1,4),(4,4),(0.,0.571428571428571,1.),(9.71445146547012E-17,1.2),
 .UNSPECIFIED.);
#1403=B_SPLINE_SURFACE_WITH_KNOTS('',3,3,((#83887,#83888,#83889,#83890),
(#83891,#83892,#83893,#83894),(#83895,#83896,#83897,#83898),(#83899,#83900,
#83901,#83902),(#83903,#83904,#83905,#83906)),.UNSPECIFIED.,.F.,.F.,.F.,
(4,1,4),(4,4),(0.,0.571428571428571,1.),(-2.77555756156289E-17,1.2),
 .UNSPECIFIED.);
#1404=B_SPLINE_SURFACE_WITH_KNOTS('',3,3,((#83936,#83937,#83938,#83939),
(#83940,#83941,#83942,#83943),(#83944,#83945,#83946,#83947),(#83948,#83949,
#83950,#83951),(#83952,#83953,#83954,#83955)),.UNSPECIFIED.,.F.,.F.,.F.,
(4,1,4),(4,4),(0.,0.571428571428571,1.),(9.71445146547012E-17,1.2),
 .UNSPECIFIED.);
#1405=B_SPLINE_SURFACE_WITH_KNOTS('',3,3,((#84783,#84784,#84785,#84786),
(#84787,#84788,#84789,#84790),(#84791,#84792,#84793,#84794),(#84795,#84796,
#84797,#84798),(#84799,#84800,#84801,#84802)),.UNSPECIFIED.,.F.,.F.,.F.,
(4,1,4),(4,4),(0.,0.571428571428571,1.),(-9.71445146547012E-17,1.2),
 .UNSPECIFIED.);
#1406=B_SPLINE_SURFACE_WITH_KNOTS('',3,3,((#84832,#84833,#84834,#84835),
(#84836,#84837,#84838,#84839),(#84840,#84841,#84842,#84843),(#84844,#84845,
#84846,#84847),(#84848,#84849,#84850,#84851)),.UNSPECIFIED.,.F.,.F.,.F.,
(4,1,4),(4,4),(0.,0.571428571428571,1.),(3.88891082483996E-17,1.2),
 .UNSPECIFIED.);
#1407=B_SPLINE_SURFACE_WITH_KNOTS('',3,3,((#85679,#85680,#85681,#85682),
(#85683,#85684,#85685,#85686),(#85687,#85688,#85689,#85690),(#85691,#85692,
#85693,#85694),(#85695,#85696,#85697,#85698)),.UNSPECIFIED.,.F.,.F.,.F.,
(4,1,4),(4,4),(0.,0.571428571428571,1.),(-1.11022302462516E-16,1.2),
 .UNSPECIFIED.);
#1408=B_SPLINE_SURFACE_WITH_KNOTS('',3,3,((#85728,#85729,#85730,#85731),
(#85732,#85733,#85734,#85735),(#85736,#85737,#85738,#85739),(#85740,#85741,
#85742,#85743),(#85744,#85745,#85746,#85747)),.UNSPECIFIED.,.F.,.F.,.F.,
(4,1,4),(4,4),(0.,0.571428571428571,1.),(3.88891082483996E-17,1.2),
 .UNSPECIFIED.);
#1409=B_SPLINE_SURFACE_WITH_KNOTS('',3,3,((#86575,#86576,#86577,#86578),
(#86579,#86580,#86581,#86582),(#86583,#86584,#86585,#86586),(#86587,#86588,
#86589,#86590),(#86591,#86592,#86593,#86594)),.UNSPECIFIED.,.F.,.F.,.F.,
(4,1,4),(4,4),(0.,0.571428571428571,1.),(-1.8809784878848E-36,1.2),
 .UNSPECIFIED.);
#1410=B_SPLINE_SURFACE_WITH_KNOTS('',3,3,((#86624,#86625,#86626,#86627),
(#86628,#86629,#86630,#86631),(#86632,#86633,#86634,#86635),(#86636,#86637,
#86638,#86639),(#86640,#86641,#86642,#86643)),.UNSPECIFIED.,.F.,.F.,.F.,
(4,1,4),(4,4),(0.,0.571428571428571,1.),(-1.11022302462516E-16,1.2),
 .UNSPECIFIED.);
#1411=B_SPLINE_SURFACE_WITH_KNOTS('',3,3,((#87471,#87472,#87473,#87474),
(#87475,#87476,#87477,#87478),(#87479,#87480,#87481,#87482),(#87483,#87484,
#87485,#87486),(#87487,#87488,#87489,#87490)),.UNSPECIFIED.,.F.,.F.,.F.,
(4,1,4),(4,4),(0.,0.571428571428571,1.),(-8.32667268468867E-17,1.2),
 .UNSPECIFIED.);
#1412=B_SPLINE_SURFACE_WITH_KNOTS('',3,3,((#87520,#87521,#87522,#87523),
(#87524,#87525,#87526,#87527),(#87528,#87529,#87530,#87531),(#87532,#87533,
#87534,#87535),(#87536,#87537,#87538,#87539)),.UNSPECIFIED.,.F.,.F.,.F.,
(4,1,4),(4,4),(0.,0.571428571428571,1.),(9.71445146547012E-17,1.2),
 .UNSPECIFIED.);
#1413=B_SPLINE_SURFACE_WITH_KNOTS('',3,3,((#88367,#88368,#88369,#88370),
(#88371,#88372,#88373,#88374),(#88375,#88376,#88377,#88378),(#88379,#88380,
#88381,#88382),(#88383,#88384,#88385,#88386)),.UNSPECIFIED.,.F.,.F.,.F.,
(4,1,4),(4,4),(0.,0.571428571428571,1.),(2.77555756156289E-17,1.2),
 .UNSPECIFIED.);
#1414=B_SPLINE_SURFACE_WITH_KNOTS('',3,3,((#88416,#88417,#88418,#88419),
(#88420,#88421,#88422,#88423),(#88424,#88425,#88426,#88427),(#88428,#88429,
#88430,#88431),(#88432,#88433,#88434,#88435)),.UNSPECIFIED.,.F.,.F.,.F.,
(4,1,4),(4,4),(0.,0.571428571428571,1.),(-1.38777878078145E-16,1.2),
 .UNSPECIFIED.);
#1415=B_SPLINE_SURFACE_WITH_KNOTS('',3,3,((#89263,#89264,#89265,#89266),
(#89267,#89268,#89269,#89270),(#89271,#89272,#89273,#89274),(#89275,#89276,
#89277,#89278),(#89279,#89280,#89281,#89282)),.UNSPECIFIED.,.F.,.F.,.F.,
(4,1,4),(4,4),(0.,0.571428571428571,1.),(2.77555756156289E-17,1.2),
 .UNSPECIFIED.);
#1416=B_SPLINE_SURFACE_WITH_KNOTS('',3,3,((#89312,#89313,#89314,#89315),
(#89316,#89317,#89318,#89319),(#89320,#89321,#89322,#89323),(#89324,#89325,
#89326,#89327),(#89328,#89329,#89330,#89331)),.UNSPECIFIED.,.F.,.F.,.F.,
(4,1,4),(4,4),(0.,0.571428571428571,1.),(9.71445146547012E-17,1.2),
 .UNSPECIFIED.);
#1417=B_SPLINE_SURFACE_WITH_KNOTS('',3,3,((#90159,#90160,#90161,#90162),
(#90163,#90164,#90165,#90166),(#90167,#90168,#90169,#90170),(#90171,#90172,
#90173,#90174),(#90175,#90176,#90177,#90178)),.UNSPECIFIED.,.F.,.F.,.F.,
(4,1,4),(4,4),(0.,0.571428571428571,1.),(-7.5239139515392E-36,1.2),
 .UNSPECIFIED.);
#1418=B_SPLINE_SURFACE_WITH_KNOTS('',3,3,((#90208,#90209,#90210,#90211),
(#90212,#90213,#90214,#90215),(#90216,#90217,#90218,#90219),(#90220,#90221,
#90222,#90223),(#90224,#90225,#90226,#90227)),.UNSPECIFIED.,.F.,.F.,.F.,
(4,1,4),(4,4),(0.,0.571428571428571,1.),(8.05224716718429E-17,1.2),
 .UNSPECIFIED.);
#1419=B_SPLINE_SURFACE_WITH_KNOTS('',3,3,((#91055,#91056,#91057,#91058),
(#91059,#91060,#91061,#91062),(#91063,#91064,#91065,#91066),(#91067,#91068,
#91069,#91070),(#91071,#91072,#91073,#91074)),.UNSPECIFIED.,.F.,.F.,.F.,
(4,1,4),(4,4),(0.,0.571428571428571,1.),(0.,1.2),.UNSPECIFIED.);
#1420=B_SPLINE_SURFACE_WITH_KNOTS('',3,3,((#91104,#91105,#91106,#91107),
(#91108,#91109,#91110,#91111),(#91112,#91113,#91114,#91115),(#91116,#91117,
#91118,#91119),(#91120,#91121,#91122,#91123)),.UNSPECIFIED.,.F.,.F.,.F.,
(4,1,4),(4,4),(0.,0.571428571428571,1.),(9.71445146547012E-17,1.2),
 .UNSPECIFIED.);
#1421=B_SPLINE_SURFACE_WITH_KNOTS('',3,3,((#91951,#91952,#91953,#91954),
(#91955,#91956,#91957,#91958),(#91959,#91960,#91961,#91962),(#91963,#91964,
#91965,#91966),(#91967,#91968,#91969,#91970)),.UNSPECIFIED.,.F.,.F.,.F.,
(4,1,4),(4,4),(0.,0.571428571428571,1.),(-1.49437708898837E-16,1.2),
 .UNSPECIFIED.);
#1422=B_SPLINE_SURFACE_WITH_KNOTS('',3,3,((#92000,#92001,#92002,#92003),
(#92004,#92005,#92006,#92007),(#92008,#92009,#92010,#92011),(#92012,#92013,
#92014,#92015),(#92016,#92017,#92018,#92019)),.UNSPECIFIED.,.F.,.F.,.F.,
(4,1,4),(4,4),(0.,0.571428571428571,1.),(5.55111512312578E-17,1.2),
 .UNSPECIFIED.);
#1423=B_SPLINE_SURFACE_WITH_KNOTS('',3,3,((#92847,#92848,#92849,#92850),
(#92851,#92852,#92853,#92854),(#92855,#92856,#92857,#92858),(#92859,#92860,
#92861,#92862),(#92863,#92864,#92865,#92866)),.UNSPECIFIED.,.F.,.F.,.F.,
(4,1,4),(4,4),(0.,0.571428571428571,1.),(-8.32667268468867E-17,1.2),
 .UNSPECIFIED.);
#1424=B_SPLINE_SURFACE_WITH_KNOTS('',3,3,((#92896,#92897,#92898,#92899),
(#92900,#92901,#92902,#92903),(#92904,#92905,#92906,#92907),(#92908,#92909,
#92910,#92911),(#92912,#92913,#92914,#92915)),.UNSPECIFIED.,.F.,.F.,.F.,
(4,1,4),(4,4),(0.,0.571428571428571,1.),(9.71445146547012E-17,1.2),
 .UNSPECIFIED.);
#1425=B_SPLINE_SURFACE_WITH_KNOTS('',3,3,((#93743,#93744,#93745,#93746),
(#93747,#93748,#93749,#93750),(#93751,#93752,#93753,#93754),(#93755,#93756,
#93757,#93758),(#93759,#93760,#93761,#93762)),.UNSPECIFIED.,.F.,.F.,.F.,
(4,1,4),(4,4),(0.,0.571428571428571,1.),(-8.32667268468868E-17,1.2),
 .UNSPECIFIED.);
#1426=B_SPLINE_SURFACE_WITH_KNOTS('',3,3,((#93792,#93793,#93794,#93795),
(#93796,#93797,#93798,#93799),(#93800,#93801,#93802,#93803),(#93804,#93805,
#93806,#93807),(#93808,#93809,#93810,#93811)),.UNSPECIFIED.,.F.,.F.,.F.,
(4,1,4),(4,4),(0.,0.571428571428571,1.),(-8.32667268468867E-17,1.2),
 .UNSPECIFIED.);
#1427=B_SPLINE_SURFACE_WITH_KNOTS('',3,3,((#94639,#94640,#94641,#94642),
(#94643,#94644,#94645,#94646),(#94647,#94648,#94649,#94650),(#94651,#94652,
#94653,#94654),(#94655,#94656,#94657,#94658)),.UNSPECIFIED.,.F.,.F.,.F.,
(4,1,4),(4,4),(0.,0.571428571428571,1.),(2.77555756156289E-17,1.2),
 .UNSPECIFIED.);
#1428=B_SPLINE_SURFACE_WITH_KNOTS('',3,3,((#94688,#94689,#94690,#94691),
(#94692,#94693,#94694,#94695),(#94696,#94697,#94698,#94699),(#94700,#94701,
#94702,#94703),(#94704,#94705,#94706,#94707)),.UNSPECIFIED.,.F.,.F.,.F.,
(4,1,4),(4,4),(0.,0.571428571428571,1.),(8.32667268468867E-17,1.2),
 .UNSPECIFIED.);
#1429=B_SPLINE_SURFACE_WITH_KNOTS('',3,3,((#95535,#95536,#95537,#95538),
(#95539,#95540,#95541,#95542),(#95543,#95544,#95545,#95546),(#95547,#95548,
#95549,#95550),(#95551,#95552,#95553,#95554)),.UNSPECIFIED.,.F.,.F.,.F.,
(4,1,4),(4,4),(0.,0.571428571428571,1.),(2.77555756156289E-17,1.2),
 .UNSPECIFIED.);
#1430=B_SPLINE_SURFACE_WITH_KNOTS('',3,3,((#95584,#95585,#95586,#95587),
(#95588,#95589,#95590,#95591),(#95592,#95593,#95594,#95595),(#95596,#95597,
#95598,#95599),(#95600,#95601,#95602,#95603)),.UNSPECIFIED.,.F.,.F.,.F.,
(4,1,4),(4,4),(0.,0.571428571428571,1.),(5.55111512312578E-17,1.2),
 .UNSPECIFIED.);
#1431=B_SPLINE_SURFACE_WITH_KNOTS('',3,3,((#96431,#96432,#96433,#96434),
(#96435,#96436,#96437,#96438),(#96439,#96440,#96441,#96442),(#96443,#96444,
#96445,#96446),(#96447,#96448,#96449,#96450)),.UNSPECIFIED.,.F.,.F.,.F.,
(4,1,4),(4,4),(0.,0.571428571428571,1.),(-1.38777878078145E-16,1.2),
 .UNSPECIFIED.);
#1432=B_SPLINE_SURFACE_WITH_KNOTS('',3,3,((#96480,#96481,#96482,#96483),
(#96484,#96485,#96486,#96487),(#96488,#96489,#96490,#96491),(#96492,#96493,
#96494,#96495),(#96496,#96497,#96498,#96499)),.UNSPECIFIED.,.F.,.F.,.F.,
(4,1,4),(4,4),(0.,0.571428571428571,1.),(2.77555756156289E-17,1.2),
 .UNSPECIFIED.);
#1433=B_SPLINE_SURFACE_WITH_KNOTS('',3,3,((#97327,#97328,#97329,#97330),
(#97331,#97332,#97333,#97334),(#97335,#97336,#97337,#97338),(#97339,#97340,
#97341,#97342),(#97343,#97344,#97345,#97346)),.UNSPECIFIED.,.F.,.F.,.F.,
(4,1,4),(4,4),(0.,0.571428571428571,1.),(0.,1.2),.UNSPECIFIED.);
#1434=B_SPLINE_SURFACE_WITH_KNOTS('',3,3,((#97376,#97377,#97378,#97379),
(#97380,#97381,#97382,#97383),(#97384,#97385,#97386,#97387),(#97388,#97389,
#97390,#97391),(#97392,#97393,#97394,#97395)),.UNSPECIFIED.,.F.,.F.,.F.,
(4,1,4),(4,4),(0.,0.571428571428571,1.),(1.66533453693773E-16,1.2),
 .UNSPECIFIED.);
#1435=B_SPLINE_SURFACE_WITH_KNOTS('',3,3,((#98223,#98224,#98225,#98226),
(#98227,#98228,#98229,#98230),(#98231,#98232,#98233,#98234),(#98235,#98236,
#98237,#98238),(#98239,#98240,#98241,#98242)),.UNSPECIFIED.,.F.,.F.,.F.,
(4,1,4),(4,4),(0.,0.571428571428571,1.),(-8.32667268468867E-17,1.2),
 .UNSPECIFIED.);
#1436=B_SPLINE_SURFACE_WITH_KNOTS('',3,3,((#98272,#98273,#98274,#98275),
(#98276,#98277,#98278,#98279),(#98280,#98281,#98282,#98283),(#98284,#98285,
#98286,#98287),(#98288,#98289,#98290,#98291)),.UNSPECIFIED.,.F.,.F.,.F.,
(4,1,4),(4,4),(0.,0.571428571428571,1.),(9.71445146547012E-17,1.2),
 .UNSPECIFIED.);
#1437=B_SPLINE_SURFACE_WITH_KNOTS('',3,3,((#99119,#99120,#99121,#99122),
(#99123,#99124,#99125,#99126),(#99127,#99128,#99129,#99130),(#99131,#99132,
#99133,#99134),(#99135,#99136,#99137,#99138)),.UNSPECIFIED.,.F.,.F.,.F.,
(4,1,4),(4,4),(0.,0.571428571428571,1.),(-2.03133674691991E-35,1.2),
 .UNSPECIFIED.);
#1438=B_SPLINE_SURFACE_WITH_KNOTS('',3,3,((#99168,#99169,#99170,#99171),
(#99172,#99173,#99174,#99175),(#99176,#99177,#99178,#99179),(#99180,#99181,
#99182,#99183),(#99184,#99185,#99186,#99187)),.UNSPECIFIED.,.F.,.F.,.F.,
(4,1,4),(4,4),(0.,0.571428571428571,1.),(-1.83155496676632E-16,1.2),
 .UNSPECIFIED.);
#1439=B_SPLINE_SURFACE_WITH_KNOTS('',3,3,((#100015,#100016,#100017,#100018),
(#100019,#100020,#100021,#100022),(#100023,#100024,#100025,#100026),(#100027,
#100028,#100029,#100030),(#100031,#100032,#100033,#100034)),
 .UNSPECIFIED.,.F.,.F.,.F.,(4,1,4),(4,4),(0.,0.571428571428571,1.),(-1.38777878078145E-16,
1.2),.UNSPECIFIED.);
#1440=B_SPLINE_SURFACE_WITH_KNOTS('',3,3,((#100064,#100065,#100066,#100067),
(#100068,#100069,#100070,#100071),(#100072,#100073,#100074,#100075),(#100076,
#100077,#100078,#100079),(#100080,#100081,#100082,#100083)),
 .UNSPECIFIED.,.F.,.F.,.F.,(4,1,4),(4,4),(0.,0.571428571428571,1.),(1.66533453693773E-16,
1.2),.UNSPECIFIED.);
#1441=B_SPLINE_SURFACE_WITH_KNOTS('',3,3,((#100911,#100912,#100913,#100914),
(#100915,#100916,#100917,#100918),(#100919,#100920,#100921,#100922),(#100923,
#100924,#100925,#100926),(#100927,#100928,#100929,#100930)),
 .UNSPECIFIED.,.F.,.F.,.F.,(4,1,4),(4,4),(0.,0.571428571428571,1.),(0.,
1.2),.UNSPECIFIED.);
#1442=B_SPLINE_SURFACE_WITH_KNOTS('',3,3,((#100960,#100961,#100962,#100963),
(#100964,#100965,#100966,#100967),(#100968,#100969,#100970,#100971),(#100972,
#100973,#100974,#100975),(#100976,#100977,#100978,#100979)),
 .UNSPECIFIED.,.F.,.F.,.F.,(4,1,4),(4,4),(0.,0.571428571428571,1.),(-1.38777878078145E-16,
1.2),.UNSPECIFIED.);
#1443=B_SPLINE_SURFACE_WITH_KNOTS('',3,3,((#101807,#101808,#101809,#101810),
(#101811,#101812,#101813,#101814),(#101815,#101816,#101817,#101818),(#101819,
#101820,#101821,#101822),(#101823,#101824,#101825,#101826)),
 .UNSPECIFIED.,.F.,.F.,.F.,(4,1,4),(4,4),(0.,0.571428571428571,1.),(-1.88097848788491E-36,
1.2),.UNSPECIFIED.);
#1444=B_SPLINE_SURFACE_WITH_KNOTS('',3,3,((#101856,#101857,#101858,#101859),
(#101860,#101861,#101862,#101863),(#101864,#101865,#101866,#101867),(#101868,
#101869,#101870,#101871),(#101872,#101873,#101874,#101875)),
 .UNSPECIFIED.,.F.,.F.,.F.,(4,1,4),(4,4),(0.,0.571428571428571,1.),(2.77555756156289E-17,
1.2),.UNSPECIFIED.);
#1445=B_SPLINE_SURFACE_WITH_KNOTS('',3,3,((#102703,#102704,#102705,#102706),
(#102707,#102708,#102709,#102710),(#102711,#102712,#102713,#102714),(#102715,
#102716,#102717,#102718),(#102719,#102720,#102721,#102722)),
 .UNSPECIFIED.,.F.,.F.,.F.,(4,1,4),(4,4),(0.,0.571428571428571,1.),(-1.38777878078145E-16,
1.2),.UNSPECIFIED.);
#1446=B_SPLINE_SURFACE_WITH_KNOTS('',3,3,((#102752,#102753,#102754,#102755),
(#102756,#102757,#102758,#102759),(#102760,#102761,#102762,#102763),(#102764,
#102765,#102766,#102767),(#102768,#102769,#102770,#102771)),
 .UNSPECIFIED.,.F.,.F.,.F.,(4,1,4),(4,4),(0.,0.571428571428571,1.),(0.,
1.2),.UNSPECIFIED.);
#1447=B_SPLINE_SURFACE_WITH_KNOTS('',3,3,((#103599,#103600,#103601,#103602),
(#103603,#103604,#103605,#103606),(#103607,#103608,#103609,#103610),(#103611,
#103612,#103613,#103614),(#103615,#103616,#103617,#103618)),
 .UNSPECIFIED.,.F.,.F.,.F.,(4,1,4),(4,4),(0.,0.571428571428571,1.),(0.,
1.2),.UNSPECIFIED.);
#1448=B_SPLINE_SURFACE_WITH_KNOTS('',3,3,((#103648,#103649,#103650,#103651),
(#103652,#103653,#103654,#103655),(#103656,#103657,#103658,#103659),(#103660,
#103661,#103662,#103663),(#103664,#103665,#103666,#103667)),
 .UNSPECIFIED.,.F.,.F.,.F.,(4,1,4),(4,4),(0.,0.571428571428571,1.),(9.71445146547012E-17,
1.2),.UNSPECIFIED.);
#1449=B_SPLINE_SURFACE_WITH_KNOTS('',3,3,((#104495,#104496,#104497,#104498),
(#104499,#104500,#104501,#104502),(#104503,#104504,#104505,#104506),(#104507,
#104508,#104509,#104510),(#104511,#104512,#104513,#104514)),
 .UNSPECIFIED.,.F.,.F.,.F.,(4,1,4),(4,4),(0.,0.571428571428571,1.),(-5.55111512312578E-17,
1.2),.UNSPECIFIED.);
#1450=B_SPLINE_SURFACE_WITH_KNOTS('',3,3,((#104544,#104545,#104546,#104547),
(#104548,#104549,#104550,#104551),(#104552,#104553,#104554,#104555),(#104556,
#104557,#104558,#104559),(#104560,#104561,#104562,#104563)),
 .UNSPECIFIED.,.F.,.F.,.F.,(4,1,4),(4,4),(0.,0.571428571428571,1.),(9.71445146547012E-17,
1.2),.UNSPECIFIED.);
#1451=B_SPLINE_SURFACE_WITH_KNOTS('',3,3,((#105391,#105392,#105393,#105394),
(#105395,#105396,#105397,#105398),(#105399,#105400,#105401,#105402),(#105403,
#105404,#105405,#105406),(#105407,#105408,#105409,#105410)),
 .UNSPECIFIED.,.F.,.F.,.F.,(4,1,4),(4,4),(0.,0.571428571428571,1.),(-1.41402172924014E-16,
1.2),.UNSPECIFIED.);
#1452=B_SPLINE_SURFACE_WITH_KNOTS('',3,3,((#105440,#105441,#105442,#105443),
(#105444,#105445,#105446,#105447),(#105448,#105449,#105450,#105451),(#105452,
#105453,#105454,#105455),(#105456,#105457,#105458,#105459)),
 .UNSPECIFIED.,.F.,.F.,.F.,(4,1,4),(4,4),(0.,0.571428571428571,1.),(0.,
1.2),.UNSPECIFIED.);
#1453=B_SPLINE_SURFACE_WITH_KNOTS('',3,3,((#106287,#106288,#106289,#106290),
(#106291,#106292,#106293,#106294),(#106295,#106296,#106297,#106298),(#106299,
#106300,#106301,#106302),(#106303,#106304,#106305,#106306)),
 .UNSPECIFIED.,.F.,.F.,.F.,(4,1,4),(4,4),(0.,0.571428571428571,1.),(-1.11022302462516E-16,
1.2),.UNSPECIFIED.);
#1454=B_SPLINE_SURFACE_WITH_KNOTS('',3,3,((#106336,#106337,#106338,#106339),
(#106340,#106341,#106342,#106343),(#106344,#106345,#106346,#106347),(#106348,
#106349,#106350,#106351),(#106352,#106353,#106354,#106355)),
 .UNSPECIFIED.,.F.,.F.,.F.,(4,1,4),(4,4),(0.,0.571428571428571,1.),(1.38777878078145E-16,
1.2),.UNSPECIFIED.);
#1455=B_SPLINE_SURFACE_WITH_KNOTS('',3,3,((#107183,#107184,#107185,#107186),
(#107187,#107188,#107189,#107190),(#107191,#107192,#107193,#107194),(#107195,
#107196,#107197,#107198),(#107199,#107200,#107201,#107202)),
 .UNSPECIFIED.,.F.,.F.,.F.,(4,1,4),(4,4),(0.,0.571428571428571,1.),(2.77555756156289E-17,
1.2),.UNSPECIFIED.);
#1456=B_SPLINE_SURFACE_WITH_KNOTS('',3,3,((#107232,#107233,#107234,#107235),
(#107236,#107237,#107238,#107239),(#107240,#107241,#107242,#107243),(#107244,
#107245,#107246,#107247),(#107248,#107249,#107250,#107251)),
 .UNSPECIFIED.,.F.,.F.,.F.,(4,1,4),(4,4),(0.,0.571428571428571,1.),(0.,
1.2),.UNSPECIFIED.);
#1457=B_SPLINE_SURFACE_WITH_KNOTS('',3,3,((#108079,#108080,#108081,#108082),
(#108083,#108084,#108085,#108086),(#108087,#108088,#108089,#108090),(#108091,
#108092,#108093,#108094),(#108095,#108096,#108097,#108098)),
 .UNSPECIFIED.,.F.,.F.,.F.,(4,1,4),(4,4),(0.,0.571428571428571,1.),(2.77555756156289E-17,
1.2),.UNSPECIFIED.);
#1458=B_SPLINE_SURFACE_WITH_KNOTS('',3,3,((#108128,#108129,#108130,#108131),
(#108132,#108133,#108134,#108135),(#108136,#108137,#108138,#108139),(#108140,
#108141,#108142,#108143),(#108144,#108145,#108146,#108147)),
 .UNSPECIFIED.,.F.,.F.,.F.,(4,1,4),(4,4),(0.,0.571428571428571,1.),(5.55111512312578E-17,
1.2),.UNSPECIFIED.);
#1459=B_SPLINE_SURFACE_WITH_KNOTS('',3,3,((#108975,#108976,#108977,#108978),
(#108979,#108980,#108981,#108982),(#108983,#108984,#108985,#108986),(#108987,
#108988,#108989,#108990),(#108991,#108992,#108993,#108994)),
 .UNSPECIFIED.,.F.,.F.,.F.,(4,1,4),(4,4),(0.,0.571428571428571,1.),(-8.32667268468867E-17,
1.2),.UNSPECIFIED.);
#1460=B_SPLINE_SURFACE_WITH_KNOTS('',3,3,((#109024,#109025,#109026,#109027),
(#109028,#109029,#109030,#109031),(#109032,#109033,#109034,#109035),(#109036,
#109037,#109038,#109039),(#109040,#109041,#109042,#109043)),
 .UNSPECIFIED.,.F.,.F.,.F.,(4,1,4),(4,4),(0.,0.571428571428571,1.),(1.66533453693773E-16,
1.2),.UNSPECIFIED.);
#1461=B_SPLINE_SURFACE_WITH_KNOTS('',3,3,((#109871,#109872,#109873,#109874),
(#109875,#109876,#109877,#109878),(#109879,#109880,#109881,#109882),(#109883,
#109884,#109885,#109886),(#109887,#109888,#109889,#109890)),
 .UNSPECIFIED.,.F.,.F.,.F.,(4,1,4),(4,4),(0.,0.571428571428571,1.),(-1.47525527564366E-17,
1.2),.UNSPECIFIED.);
#1462=B_SPLINE_SURFACE_WITH_KNOTS('',3,3,((#109920,#109921,#109922,#109923),
(#109924,#109925,#109926,#109927),(#109928,#109929,#109930,#109931),(#109932,
#109933,#109934,#109935),(#109936,#109937,#109938,#109939)),
 .UNSPECIFIED.,.F.,.F.,.F.,(4,1,4),(4,4),(0.,0.571428571428571,1.),(9.71445146547012E-17,
1.2),.UNSPECIFIED.);
#1463=B_SPLINE_SURFACE_WITH_KNOTS('',3,3,((#110767,#110768,#110769,#110770),
(#110771,#110772,#110773,#110774),(#110775,#110776,#110777,#110778),(#110779,
#110780,#110781,#110782),(#110783,#110784,#110785,#110786)),
 .UNSPECIFIED.,.F.,.F.,.F.,(4,1,4),(4,4),(0.,0.571428571428571,1.),(2.77555756156289E-17,
1.2),.UNSPECIFIED.);
#1464=B_SPLINE_SURFACE_WITH_KNOTS('',3,3,((#110816,#110817,#110818,#110819),
(#110820,#110821,#110822,#110823),(#110824,#110825,#110826,#110827),(#110828,
#110829,#110830,#110831),(#110832,#110833,#110834,#110835)),
 .UNSPECIFIED.,.F.,.F.,.F.,(4,1,4),(4,4),(0.,0.571428571428571,1.),(0.,
1.2),.UNSPECIFIED.);
#1465=B_SPLINE_SURFACE_WITH_KNOTS('',3,3,((#111663,#111664,#111665,#111666),
(#111667,#111668,#111669,#111670),(#111671,#111672,#111673,#111674),(#111675,
#111676,#111677,#111678),(#111679,#111680,#111681,#111682)),
 .UNSPECIFIED.,.F.,.F.,.F.,(4,1,4),(4,4),(0.,0.571428571428571,1.),(-8.32667268468867E-17,
1.2),.UNSPECIFIED.);
#1466=B_SPLINE_SURFACE_WITH_KNOTS('',3,3,((#111712,#111713,#111714,#111715),
(#111716,#111717,#111718,#111719),(#111720,#111721,#111722,#111723),(#111724,
#111725,#111726,#111727),(#111728,#111729,#111730,#111731)),
 .UNSPECIFIED.,.F.,.F.,.F.,(4,1,4),(4,4),(0.,0.571428571428571,1.),(-5.63859161805989E-17,
1.2),.UNSPECIFIED.);
#1467=B_SPLINE_SURFACE_WITH_KNOTS('',3,3,((#112559,#112560,#112561,#112562),
(#112563,#112564,#112565,#112566),(#112567,#112568,#112569,#112570),(#112571,
#112572,#112573,#112574),(#112575,#112576,#112577,#112578)),
 .UNSPECIFIED.,.F.,.F.,.F.,(4,1,4),(4,4),(0.,0.571428571428571,1.),(-3.76195697576961E-36,
1.2),.UNSPECIFIED.);
#1468=B_SPLINE_SURFACE_WITH_KNOTS('',3,3,((#112608,#112609,#112610,#112611),
(#112612,#112613,#112614,#112615),(#112616,#112617,#112618,#112619),(#112620,
#112621,#112622,#112623),(#112624,#112625,#112626,#112627)),
 .UNSPECIFIED.,.F.,.F.,.F.,(4,1,4),(4,4),(0.,0.571428571428571,1.),(2.77555756156289E-17,
1.2),.UNSPECIFIED.);
#1469=B_SPLINE_SURFACE_WITH_KNOTS('',3,3,((#113455,#113456,#113457,#113458),
(#113459,#113460,#113461,#113462),(#113463,#113464,#113465,#113466),(#113467,
#113468,#113469,#113470),(#113471,#113472,#113473,#113474)),
 .UNSPECIFIED.,.F.,.F.,.F.,(4,1,4),(4,4),(0.,0.571428571428571,1.),(0.,
1.2),.UNSPECIFIED.);
#1470=B_SPLINE_SURFACE_WITH_KNOTS('',3,3,((#113504,#113505,#113506,#113507),
(#113508,#113509,#113510,#113511),(#113512,#113513,#113514,#113515),(#113516,
#113517,#113518,#113519),(#113520,#113521,#113522,#113523)),
 .UNSPECIFIED.,.F.,.F.,.F.,(4,1,4),(4,4),(0.,0.571428571428571,1.),(9.71445146547012E-17,
1.2),.UNSPECIFIED.);
#1471=B_SPLINE_SURFACE_WITH_KNOTS('',3,3,((#114351,#114352,#114353,#114354),
(#114355,#114356,#114357,#114358),(#114359,#114360,#114361,#114362),(#114363,
#114364,#114365,#114366),(#114367,#114368,#114369,#114370)),
 .UNSPECIFIED.,.F.,.F.,.F.,(4,1,4),(4,4),(0.,0.571428571428571,1.),(-6.03986977505924E-17,
1.2),.UNSPECIFIED.);
#1472=B_SPLINE_SURFACE_WITH_KNOTS('',3,3,((#114400,#114401,#114402,#114403),
(#114404,#114405,#114406,#114407),(#114408,#114409,#114410,#114411),(#114412,
#114413,#114414,#114415),(#114416,#114417,#114418,#114419)),
 .UNSPECIFIED.,.F.,.F.,.F.,(4,1,4),(4,4),(0.,0.571428571428571,1.),(9.71445146547012E-17,
1.2),.UNSPECIFIED.);
#1473=B_SPLINE_SURFACE_WITH_KNOTS('',3,3,((#115247,#115248,#115249,#115250),
(#115251,#115252,#115253,#115254),(#115255,#115256,#115257,#115258),(#115259,
#115260,#115261,#115262),(#115263,#115264,#115265,#115266)),
 .UNSPECIFIED.,.F.,.F.,.F.,(4,1,4),(4,4),(0.,0.571428571428571,1.),(2.77555756156289E-17,
1.2),.UNSPECIFIED.);
#1474=B_SPLINE_SURFACE_WITH_KNOTS('',3,3,((#115296,#115297,#115298,#115299),
(#115300,#115301,#115302,#115303),(#115304,#115305,#115306,#115307),(#115308,
#115309,#115310,#115311),(#115312,#115313,#115314,#115315)),
 .UNSPECIFIED.,.F.,.F.,.F.,(4,1,4),(4,4),(0.,0.571428571428571,1.),(0.,
1.2),.UNSPECIFIED.);
#1475=B_SPLINE_SURFACE_WITH_KNOTS('',3,3,((#116143,#116144,#116145,#116146),
(#116147,#116148,#116149,#116150),(#116151,#116152,#116153,#116154),(#116155,
#116156,#116157,#116158),(#116159,#116160,#116161,#116162)),
 .UNSPECIFIED.,.F.,.F.,.F.,(4,1,4),(4,4),(0.,0.571428571428571,1.),(-5.55111512312578E-17,
1.2),.UNSPECIFIED.);
#1476=B_SPLINE_SURFACE_WITH_KNOTS('',3,3,((#173282,#173283,#173284,#173285),
(#173286,#173287,#173288,#173289),(#173290,#173291,#173292,#173293),(#173294,
#173295,#173296,#173297),(#173298,#173299,#173300,#173301)),
 .UNSPECIFIED.,.F.,.F.,.F.,(4,1,4),(4,4),(0.,0.571428571428571,1.),(2.13940539033965E-17,
1.2),.UNSPECIFIED.);
#1477=B_SPLINE_SURFACE_WITH_KNOTS('',3,3,((#174126,#174127,#174128,#174129),
(#174130,#174131,#174132,#174133),(#174134,#174135,#174136,#174137),(#174138,
#174139,#174140,#174141),(#174142,#174143,#174144,#174145)),
 .UNSPECIFIED.,.F.,.F.,.F.,(4,1,4),(4,4),(0.,0.571428571428571,1.),(0.,
1.2),.UNSPECIFIED.);
#1478=B_SPLINE_SURFACE_WITH_KNOTS('',3,3,((#257559,#257560,#257561,#257562,
#257563,#257564,#257565,#257566,#257567,#257568,#257569,#257570,#257571,
#257572,#257573,#257574,#257575,#257576,#257577,#257578,#257579,#257580,
#257581,#257582,#257583,#257584,#257585,#257586,#257587,#257588,#257589,
#257590,#257591,#257592,#257593,#257594,#257595,#257596,#257597,#257598,
#257599,#257600,#257601,#257602,#257603,#257604,#257605,#257606,#257607,
#257608,#257609,#257610,#257611,#257612,#257613,#257614,#257615,#257616,
#257617,#257618,#257619,#257620,#257621,#257622,#257623,#257624,#257625,
#257626,#257627,#257628,#257629,#257630,#257631,#257632,#257633,#257634,
#257635,#257636,#257637,#257638,#257639,#257640,#257641,#257642,#257643,
#257644,#257645,#257646,#257647,#257648,#257649,#257650,#257651,#257652,
#257653,#257654,#257655,#257656,#257657,#257658,#257659,#257660,#257661,
#257662,#257663,#257664,#257665,#257666,#257667,#257668,#257669,#257670,
#257671,#257672,#257673,#257674,#257675,#257676,#257677,#257678,#257679,
#257680,#257681,#257682,#257683,#257684,#257685,#257686,#257687,#257688,
#257689),(#257690,#257691,#257692,#257693,#257694,#257695,#257696,#257697,
#257698,#257699,#257700,#257701,#257702,#257703,#257704,#257705,#257706,
#257707,#257708,#257709,#257710,#257711,#257712,#257713,#257714,#257715,
#257716,#257717,#257718,#257719,#257720,#257721,#257722,#257723,#257724,
#257725,#257726,#257727,#257728,#257729,#257730,#257731,#257732,#257733,
#257734,#257735,#257736,#257737,#257738,#257739,#257740,#257741,#257742,
#257743,#257744,#257745,#257746,#257747,#257748,#257749,#257750,#257751,
#257752,#257753,#257754,#257755,#257756,#257757,#257758,#257759,#257760,
#257761,#257762,#257763,#257764,#257765,#257766,#257767,#257768,#257769,
#257770,#257771,#257772,#257773,#257774,#257775,#257776,#257777,#257778,
#257779,#257780,#257781,#257782,#257783,#257784,#257785,#257786,#257787,
#257788,#257789,#257790,#257791,#257792,#257793,#257794,#257795,#257796,
#257797,#257798,#257799,#257800,#257801,#257802,#257803,#257804,#257805,
#257806,#257807,#257808,#257809,#257810,#257811,#257812,#257813,#257814,
#257815,#257816,#257817,#257818,#257819,#257820),(#257821,#257822,#257823,
#257824,#257825,#257826,#257827,#257828,#257829,#257830,#257831,#257832,
#257833,#257834,#257835,#257836,#257837,#257838,#257839,#257840,#257841,
#257842,#257843,#257844,#257845,#257846,#257847,#257848,#257849,#257850,
#257851,#257852,#257853,#257854,#257855,#257856,#257857,#257858,#257859,
#257860,#257861,#257862,#257863,#257864,#257865,#257866,#257867,#257868,
#257869,#257870,#257871,#257872,#257873,#257874,#257875,#257876,#257877,
#257878,#257879,#257880,#257881,#257882,#257883,#257884,#257885,#257886,
#257887,#257888,#257889,#257890,#257891,#257892,#257893,#257894,#257895,
#257896,#257897,#257898,#257899,#257900,#257901,#257902,#257903,#257904,
#257905,#257906,#257907,#257908,#257909,#257910,#257911,#257912,#257913,
#257914,#257915,#257916,#257917,#257918,#257919,#257920,#257921,#257922,
#257923,#257924,#257925,#257926,#257927,#257928,#257929,#257930,#257931,
#257932,#257933,#257934,#257935,#257936,#257937,#257938,#257939,#257940,
#257941,#257942,#257943,#257944,#257945,#257946,#257947,#257948,#257949,
#257950,#257951),(#257952,#257953,#257954,#257955,#257956,#257957,#257958,
#257959,#257960,#257961,#257962,#257963,#257964,#257965,#257966,#257967,
#257968,#257969,#257970,#257971,#257972,#257973,#257974,#257975,#257976,
#257977,#257978,#257979,#257980,#257981,#257982,#257983,#257984,#257985,
#257986,#257987,#257988,#257989,#257990,#257991,#257992,#257993,#257994,
#257995,#257996,#257997,#257998,#257999,#258000,#258001,#258002,#258003,
#258004,#258005,#258006,#258007,#258008,#258009,#258010,#258011,#258012,
#258013,#258014,#258015,#258016,#258017,#258018,#258019,#258020,#258021,
#258022,#258023,#258024,#258025,#258026,#258027,#258028,#258029,#258030,
#258031,#258032,#258033,#258034,#258035,#258036,#258037,#258038,#258039,
#258040,#258041,#258042,#258043,#258044,#258045,#258046,#258047,#258048,
#258049,#258050,#258051,#258052,#258053,#258054,#258055,#258056,#258057,
#258058,#258059,#258060,#258061,#258062,#258063,#258064,#258065,#258066,
#258067,#258068,#258069,#258070,#258071,#258072,#258073,#258074,#258075,
#258076,#258077,#258078,#258079,#258080,#258081,#258082)),.UNSPECIFIED.,
 .F.,.F.,.F.,(4,4),(4,1,1,1,1,1,1,1,1,1,1,1,1,1,1,1,1,1,1,1,1,1,1,1,1,1,
1,1,1,1,1,1,1,1,1,1,1,1,1,1,1,1,1,1,1,1,1,1,1,1,1,1,1,1,1,1,1,1,1,1,1,1,
1,1,1,1,1,1,1,1,1,1,1,1,1,1,1,1,1,1,1,1,1,1,1,1,1,1,1,1,1,1,1,1,1,1,1,1,
1,1,1,1,1,1,1,1,1,1,1,1,1,1,1,1,1,1,1,1,1,1,1,1,1,1,1,1,1,1,4),(0.,0.0658467982010768),
(8.30747755240104,9.30538649238933,10.3032954323776,11.3012043723659,12.2991133123542,
13.2970222523425,14.2949311923308,15.2928401323191,16.2907490723073,17.2886580122956,
18.2865669522839,19.2844758922722,20.2823848322605,21.2802937722488,22.2782027122371,
23.2761116522254,24.2740205922137,25.2719295322019,26.2698384721902,27.2677474121785,
28.2656563521668,29.2635652921551,30.2614742321434,31.2593831721317,32.25729211212,
33.2552010521082,34.2531099920965,35.2510189320848,36.2489278720731,37.2468368120614,
38.2447457520497,39.242654692038,40.2405636320263,41.2384725720146,42.2363815120028,
43.2342904519911,44.2321993919794,45.2301083319677,46.228017271956,47.2259262119443,
48.2238351519326,49.2217440919209,50.2196530319092,51.2175619718974,52.2154709118857,
53.213379851874,54.2112887918623,55.2091977318506,56.2071066718389,57.2050156118272,
58.2029245518155,59.2008334918037,60.198742431792,61.1966513717803,62.1945603117686,
63.1924692517569,64.1903781917452,65.1882871317335,66.1861960717218,67.1841050117101,
68.1820139516983,69.1799228916866,70.1778318316749,71.1757407716632,72.1736497116515,
73.1715586516398,74.1694675916281,75.1673765316164,76.1652854716046,77.1631944115929,
78.1611033515812,79.1590122915695,80.1569212315578,81.1548301715461,82.1527391115344,
83.1506480515227,84.148556991511,85.1464659314993,86.1443748714875,87.1422838114758,
88.1401927514641,89.1381016914524,90.1360106314407,91.133919571429,92.1318285114173,
93.1297374514056,94.1276463913938,95.1255553313821,96.1234642713704,97.1213732113587,
98.119282151347,99.1171910913353,100.115100031324,101.113008971312,102.1109179113,
103.108826851288,104.106735791277,105.104644731265,106.102553671253,107.100462611242,
108.09837155123,109.096280491218,110.094189431206,111.092098371195,112.090007311183,
113.087916251171,114.08582519116,115.083734131148,116.081643071136,117.079552011124,
118.077460951113,119.075369891101,120.073278831089,121.071187771078,122.069096711066,
123.067005651054,124.064914591042,125.062823531031,126.060732471019,127.058641411007,
128.056550350996,129.054459290984,130.052368230972,131.05027717096,132.048186110949,
133.046095050937,134.044003990925,135.041912930914,136.039821870902),
 .UNSPECIFIED.);
#1479=B_SPLINE_SURFACE_WITH_KNOTS('',3,3,((#258309,#258310,#258311,#258312,
#258313,#258314,#258315,#258316,#258317,#258318,#258319,#258320,#258321,
#258322,#258323,#258324,#258325,#258326,#258327,#258328,#258329,#258330,
#258331,#258332,#258333,#258334,#258335,#258336,#258337,#258338,#258339,
#258340,#258341,#258342,#258343,#258344,#258345,#258346,#258347,#258348,
#258349,#258350,#258351,#258352,#258353,#258354,#258355,#258356,#258357,
#258358,#258359,#258360,#258361,#258362,#258363,#258364,#258365,#258366,
#258367,#258368,#258369,#258370,#258371,#258372,#258373,#258374,#258375,
#258376,#258377,#258378,#258379,#258380,#258381,#258382,#258383,#258384,
#258385,#258386,#258387,#258388,#258389,#258390,#258391,#258392,#258393,
#258394,#258395,#258396,#258397,#258398,#258399,#258400,#258401,#258402,
#258403,#258404,#258405,#258406,#258407,#258408,#258409,#258410,#258411,
#258412,#258413,#258414,#258415,#258416,#258417,#258418,#258419,#258420,
#258421,#258422,#258423,#258424,#258425,#258426,#258427,#258428,#258429,
#258430,#258431,#258432,#258433,#258434,#258435,#258436,#258437,#258438,
#258439),(#258440,#258441,#258442,#258443,#258444,#258445,#258446,#258447,
#258448,#258449,#258450,#258451,#258452,#258453,#258454,#258455,#258456,
#258457,#258458,#258459,#258460,#258461,#258462,#258463,#258464,#258465,
#258466,#258467,#258468,#258469,#258470,#258471,#258472,#258473,#258474,
#258475,#258476,#258477,#258478,#258479,#258480,#258481,#258482,#258483,
#258484,#258485,#258486,#258487,#258488,#258489,#258490,#258491,#258492,
#258493,#258494,#258495,#258496,#258497,#258498,#258499,#258500,#258501,
#258502,#258503,#258504,#258505,#258506,#258507,#258508,#258509,#258510,
#258511,#258512,#258513,#258514,#258515,#258516,#258517,#258518,#258519,
#258520,#258521,#258522,#258523,#258524,#258525,#258526,#258527,#258528,
#258529,#258530,#258531,#258532,#258533,#258534,#258535,#258536,#258537,
#258538,#258539,#258540,#258541,#258542,#258543,#258544,#258545,#258546,
#258547,#258548,#258549,#258550,#258551,#258552,#258553,#258554,#258555,
#258556,#258557,#258558,#258559,#258560,#258561,#258562,#258563,#258564,
#258565,#258566,#258567,#258568,#258569,#258570),(#258571,#258572,#258573,
#258574,#258575,#258576,#258577,#258578,#258579,#258580,#258581,#258582,
#258583,#258584,#258585,#258586,#258587,#258588,#258589,#258590,#258591,
#258592,#258593,#258594,#258595,#258596,#258597,#258598,#258599,#258600,
#258601,#258602,#258603,#258604,#258605,#258606,#258607,#258608,#258609,
#258610,#258611,#258612,#258613,#258614,#258615,#258616,#258617,#258618,
#258619,#258620,#258621,#258622,#258623,#258624,#258625,#258626,#258627,
#258628,#258629,#258630,#258631,#258632,#258633,#258634,#258635,#258636,
#258637,#258638,#258639,#258640,#258641,#258642,#258643,#258644,#258645,
#258646,#258647,#258648,#258649,#258650,#258651,#258652,#258653,#258654,
#258655,#258656,#258657,#258658,#258659,#258660,#258661,#258662,#258663,
#258664,#258665,#258666,#258667,#258668,#258669,#258670,#258671,#258672,
#258673,#258674,#258675,#258676,#258677,#258678,#258679,#258680,#258681,
#258682,#258683,#258684,#258685,#258686,#258687,#258688,#258689,#258690,
#258691,#258692,#258693,#258694,#258695,#258696,#258697,#258698,#258699,
#258700,#258701),(#258702,#258703,#258704,#258705,#258706,#258707,#258708,
#258709,#258710,#258711,#258712,#258713,#258714,#258715,#258716,#258717,
#258718,#258719,#258720,#258721,#258722,#258723,#258724,#258725,#258726,
#258727,#258728,#258729,#258730,#258731,#258732,#258733,#258734,#258735,
#258736,#258737,#258738,#258739,#258740,#258741,#258742,#258743,#258744,
#258745,#258746,#258747,#258748,#258749,#258750,#258751,#258752,#258753,
#258754,#258755,#258756,#258757,#258758,#258759,#258760,#258761,#258762,
#258763,#258764,#258765,#258766,#258767,#258768,#258769,#258770,#258771,
#258772,#258773,#258774,#258775,#258776,#258777,#258778,#258779,#258780,
#258781,#258782,#258783,#258784,#258785,#258786,#258787,#258788,#258789,
#258790,#258791,#258792,#258793,#258794,#258795,#258796,#258797,#258798,
#258799,#258800,#258801,#258802,#258803,#258804,#258805,#258806,#258807,
#258808,#258809,#258810,#258811,#258812,#258813,#258814,#258815,#258816,
#258817,#258818,#258819,#258820,#258821,#258822,#258823,#258824,#258825,
#258826,#258827,#258828,#258829,#258830,#258831,#258832)),.UNSPECIFIED.,
 .F.,.F.,.F.,(4,4),(4,1,1,1,1,1,1,1,1,1,1,1,1,1,1,1,1,1,1,1,1,1,1,1,1,1,
1,1,1,1,1,1,1,1,1,1,1,1,1,1,1,1,1,1,1,1,1,1,1,1,1,1,1,1,1,1,1,1,1,1,1,1,
1,1,1,1,1,1,1,1,1,1,1,1,1,1,1,1,1,1,1,1,1,1,1,1,1,1,1,1,1,1,1,1,1,1,1,1,
1,1,1,1,1,1,1,1,1,1,1,1,1,1,1,1,1,1,1,1,1,1,1,1,1,1,1,1,1,1,4),(0.,0.0658467982010768),
(11.6150328478182,12.6129417878065,13.6108507277948,14.6087596677831,15.6066686077714,
16.6045775477597,17.602486487748,18.6003954277363,19.5983043677246,20.5962133077128,
21.5941222477011,22.5920311876894,23.5899401276777,24.587849067666,25.5857580076543,
26.5836669476426,27.5815758876309,28.5794848276191,29.5773937676074,30.5753027075957,
31.573211647584,32.5711205875723,33.5690295275606,34.5669384675489,35.5648474075372,
36.5627563475255,37.5606652875137,38.558574227502,39.5564831674903,40.5543921074786,
41.5523010474669,42.5502099874552,43.5481189274435,44.5460278674318,45.54393680742,
46.5418457474083,47.5397546873966,48.5376636273849,49.5355725673732,50.5334815073615,
51.5313904473498,52.5292993873381,53.5272083273263,54.5251172673146,55.5230262073029,
56.5209351472912,57.5188440872795,58.5167530272678,59.5146619672561,60.5125709072444,
61.5104798472327,62.5083887872209,63.5062977272092,64.5042066671975,65.5021156071858,
66.5000245471741,67.4979334871624,68.4958424271507,69.493751367139,70.4916603071272,
71.4895692471155,72.4874781871038,73.4853871270921,74.4832960670804,75.4812050070687,
76.479113947057,77.4770228870453,78.4749318270335,79.4728407670218,80.4707497070101,
81.4686586469984,82.4665675869867,83.464476526975,84.4623854669633,85.4602944069516,
86.4582033469399,87.4561122869281,88.4540212269164,89.4519301669047,90.449839106893,
91.4477480468813,92.4456569868696,93.4435659268579,94.4414748668462,95.4393838068345,
96.4372927468227,97.435201686811,98.4331106267993,99.4310195667876,100.428928506776,
101.426837446764,102.424746386752,103.422655326741,104.420564266729,105.418473206717,
106.416382146706,107.414291086694,108.412200026682,109.41010896667,110.408017906659,
111.405926846647,112.403835786635,113.401744726624,114.399653666612,115.3975626066,
116.395471546589,117.393380486577,118.391289426565,119.389198366553,120.387107306542,
121.38501624653,122.382925186518,123.380834126507,124.378743066495,125.376652006483,
126.374560946471,127.37246988646,128.370378826448,129.368287766436,130.366196706425,
131.364105646413,132.362014586401,133.359923526389,134.357832466378,135.355741406366,
136.353650346354,137.351559286343,138.349468226331,139.347377166319),
 .UNSPECIFIED.);
#1480=PLANE('',#25693);
#1481=PLANE('',#25696);
#1482=PLANE('',#25699);
#1483=PLANE('',#25702);
#1484=PLANE('',#25705);
#1485=PLANE('',#25708);
#1486=PLANE('',#25711);
#1487=PLANE('',#25714);
#1488=PLANE('',#25717);
#1489=PLANE('',#25718);
#1490=PLANE('',#25719);
#1491=PLANE('',#25720);
#1492=PLANE('',#25721);
#1493=PLANE('',#25722);
#1494=PLANE('',#25723);
#1495=PLANE('',#25724);
#1496=PLANE('',#25740);
#1497=PLANE('',#25748);
#1498=PLANE('',#25749);
#1499=PLANE('',#25755);
#1500=PLANE('',#25756);
#1501=PLANE('',#25760);
#1502=PLANE('',#25763);
#1503=PLANE('',#25766);
#1504=PLANE('',#25769);
#1505=PLANE('',#25776);
#1506=PLANE('',#25777);
#1507=PLANE('',#25809);
#1508=PLANE('',#25810);
#1509=PLANE('',#25812);
#1510=PLANE('',#25813);
#1511=PLANE('',#25815);
#1512=PLANE('',#25816);
#1513=PLANE('',#25817);
#1514=PLANE('',#25822);
#1515=PLANE('',#25824);
#1516=PLANE('',#25831);
#1517=PLANE('',#25833);
#1518=PLANE('',#25837);
#1519=PLANE('',#25840);
#1520=PLANE('',#25846);
#1521=PLANE('',#25849);
#1522=PLANE('',#25855);
#1523=PLANE('',#25859);
#1524=PLANE('',#25862);
#1525=PLANE('',#25863);
#1526=PLANE('',#25867);
#1527=PLANE('',#25870);
#1528=PLANE('',#25873);
#1529=PLANE('',#25876);
#1530=PLANE('',#26306);
#1531=PLANE('',#26313);
#1532=PLANE('',#26315);
#1533=PLANE('',#26316);
#1534=PLANE('',#26317);
#1535=PLANE('',#26321);
#1536=PLANE('',#26420);
#1537=PLANE('',#26427);
#1538=PLANE('',#26434);
#1539=PLANE('',#26441);
#1540=PLANE('',#26448);
#1541=PLANE('',#26455);
#1542=PLANE('',#26462);
#1543=PLANE('',#26469);
#1544=PLANE('',#26476);
#1545=PLANE('',#26483);
#1546=PLANE('',#26490);
#1547=PLANE('',#26497);
#1548=PLANE('',#26504);
#1549=PLANE('',#26511);
#1550=PLANE('',#26518);
#1551=PLANE('',#26525);
#1552=PLANE('',#26532);
#1553=PLANE('',#26539);
#1554=PLANE('',#26546);
#1555=PLANE('',#26553);
#1556=PLANE('',#26560);
#1557=PLANE('',#26567);
#1558=PLANE('',#26574);
#1559=PLANE('',#26579);
#1560=PLANE('',#26580);
#1561=PLANE('',#26581);
#1562=PLANE('',#26582);
#1563=PLANE('',#26583);
#1564=PLANE('',#26584);
#1565=PLANE('',#26585);
#1566=PLANE('',#26586);
#1567=PLANE('',#26587);
#1568=PLANE('',#26588);
#1569=PLANE('',#26589);
#1570=PLANE('',#26590);
#1571=PLANE('',#26591);
#1572=PLANE('',#26592);
#1573=PLANE('',#26593);
#1574=PLANE('',#26594);
#1575=PLANE('',#26595);
#1576=PLANE('',#26596);
#1577=PLANE('',#26597);
#1578=PLANE('',#26598);
#1579=PLANE('',#26599);
#1580=PLANE('',#26600);
#1581=PLANE('',#26601);
#1582=PLANE('',#26602);
#1583=PLANE('',#26654);
#1584=PLANE('',#26657);
#1585=PLANE('',#26663);
#1586=PLANE('',#26673);
#1587=PLANE('',#26683);
#1588=PLANE('',#26693);
#1589=PLANE('',#26703);
#1590=PLANE('',#26713);
#1591=PLANE('',#26723);
#1592=PLANE('',#26733);
#1593=PLANE('',#26743);
#1594=PLANE('',#26753);
#1595=PLANE('',#26763);
#1596=PLANE('',#26773);
#1597=PLANE('',#26783);
#1598=PLANE('',#26793);
#1599=PLANE('',#26803);
#1600=PLANE('',#26813);
#1601=PLANE('',#26823);
#1602=PLANE('',#26833);
#1603=PLANE('',#26843);
#1604=PLANE('',#26853);
#1605=PLANE('',#26863);
#1606=PLANE('',#26873);
#1607=PLANE('',#26883);
#1608=PLANE('',#26890);
#1609=PLANE('',#26891);
#1610=PLANE('',#26892);
#1611=PLANE('',#26893);
#1612=PLANE('',#26894);
#1613=PLANE('',#26895);
#1614=PLANE('',#26896);
#1615=PLANE('',#26897);
#1616=PLANE('',#26898);
#1617=PLANE('',#26899);
#1618=PLANE('',#26900);
#1619=PLANE('',#26901);
#1620=PLANE('',#26902);
#1621=PLANE('',#26903);
#1622=PLANE('',#26904);
#1623=PLANE('',#26905);
#1624=PLANE('',#26906);
#1625=PLANE('',#26907);
#1626=PLANE('',#26908);
#1627=PLANE('',#26909);
#1628=PLANE('',#26910);
#1629=PLANE('',#26911);
#1630=PLANE('',#26912);
#1631=PLANE('',#26913);
#1632=PLANE('',#26942);
#1633=PLANE('',#26995);
#1634=PLANE('',#26998);
#1635=PLANE('',#27008);
#1636=PLANE('',#27009);
#1637=PLANE('',#27011);
#1638=PLANE('',#27012);
#1639=PLANE('',#27014);
#1640=PLANE('',#27015);
#1641=PLANE('',#27016);
#1642=PLANE('',#27021);
#1643=PLANE('',#27023);
#1644=PLANE('',#27030);
#1645=PLANE('',#27032);
#1646=PLANE('',#27045);
#1647=PLANE('',#27048);
#1648=PLANE('',#27055);
#1649=PLANE('',#27056);
#1650=PLANE('',#27059);
#1651=PLANE('',#27065);
#1652=PLANE('',#27068);
#1653=PLANE('',#27074);
#1654=PLANE('',#27075);
#1655=PLANE('',#27077);
#1656=PLANE('',#27078);
#1657=PLANE('',#27079);
#1658=PLANE('',#27080);
#1659=PLANE('',#27081);
#1660=PLANE('',#27082);
#1661=PLANE('',#27090);
#1662=PLANE('',#27091);
#1663=PLANE('',#27096);
#1664=PLANE('',#27098);
#1665=PLANE('',#27102);
#1666=PLANE('',#27107);
#1667=PLANE('',#27109);
#1668=PLANE('',#27111);
#1669=PLANE('',#27112);
#1670=PLANE('',#27113);
#1671=PLANE('',#27120);
#1672=PLANE('',#27128);
#1673=PLANE('',#27129);
#1674=PLANE('',#27137);
#1675=PLANE('',#27138);
#1676=PLANE('',#27146);
#1677=PLANE('',#27147);
#1678=PLANE('',#27149);
#1679=PLANE('',#27150);
#1680=PLANE('',#27151);
#1681=PLANE('',#27158);
#1682=PLANE('',#27160);
#1683=PLANE('',#27161);
#1684=PLANE('',#27162);
#1685=PLANE('',#27169);
#1686=PLANE('',#27174);
#1687=PLANE('',#27175);
#1688=PLANE('',#27223);
#1689=PLANE('',#27224);
#1690=PLANE('',#27225);
#1691=PLANE('',#27226);
#1692=PLANE('',#27227);
#1693=PLANE('',#27228);
#1694=PLANE('',#27229);
#1695=PLANE('',#27230);
#1696=PLANE('',#27234);
#1697=PLANE('',#27235);
#1698=FACE_OUTER_BOUND('',#3044,.T.);
#1699=FACE_OUTER_BOUND('',#3045,.T.);
#1700=FACE_OUTER_BOUND('',#3046,.T.);
#1701=FACE_OUTER_BOUND('',#3047,.T.);
#1702=FACE_OUTER_BOUND('',#3048,.T.);
#1703=FACE_OUTER_BOUND('',#3049,.T.);
#1704=FACE_OUTER_BOUND('',#3050,.T.);
#1705=FACE_OUTER_BOUND('',#3051,.T.);
#1706=FACE_OUTER_BOUND('',#3052,.T.);
#1707=FACE_OUTER_BOUND('',#3053,.T.);
#1708=FACE_OUTER_BOUND('',#3054,.T.);
#1709=FACE_OUTER_BOUND('',#3055,.T.);
#1710=FACE_OUTER_BOUND('',#3056,.T.);
#1711=FACE_OUTER_BOUND('',#3057,.T.);
#1712=FACE_OUTER_BOUND('',#3058,.T.);
#1713=FACE_OUTER_BOUND('',#3059,.T.);
#1714=FACE_OUTER_BOUND('',#3060,.T.);
#1715=FACE_OUTER_BOUND('',#3061,.T.);
#1716=FACE_OUTER_BOUND('',#3062,.T.);
#1717=FACE_OUTER_BOUND('',#3063,.T.);
#1718=FACE_OUTER_BOUND('',#3064,.T.);
#1719=FACE_OUTER_BOUND('',#3065,.T.);
#1720=FACE_OUTER_BOUND('',#3066,.T.);
#1721=FACE_OUTER_BOUND('',#3067,.T.);
#1722=FACE_OUTER_BOUND('',#3068,.T.);
#1723=FACE_OUTER_BOUND('',#3069,.T.);
#1724=FACE_OUTER_BOUND('',#3070,.T.);
#1725=FACE_OUTER_BOUND('',#3071,.T.);
#1726=FACE_OUTER_BOUND('',#3072,.T.);
#1727=FACE_OUTER_BOUND('',#3073,.T.);
#1728=FACE_OUTER_BOUND('',#3074,.T.);
#1729=FACE_OUTER_BOUND('',#3075,.T.);
#1730=FACE_OUTER_BOUND('',#3076,.T.);
#1731=FACE_OUTER_BOUND('',#3077,.T.);
#1732=FACE_OUTER_BOUND('',#3078,.T.);
#1733=FACE_OUTER_BOUND('',#3079,.T.);
#1734=FACE_OUTER_BOUND('',#3080,.T.);
#1735=FACE_OUTER_BOUND('',#3081,.T.);
#1736=FACE_OUTER_BOUND('',#3082,.T.);
#1737=FACE_OUTER_BOUND('',#3083,.T.);
#1738=FACE_OUTER_BOUND('',#3084,.T.);
#1739=FACE_OUTER_BOUND('',#3085,.T.);
#1740=FACE_OUTER_BOUND('',#3086,.T.);
#1741=FACE_OUTER_BOUND('',#3087,.T.);
#1742=FACE_OUTER_BOUND('',#3088,.T.);
#1743=FACE_OUTER_BOUND('',#3089,.T.);
#1744=FACE_OUTER_BOUND('',#3090,.T.);
#1745=FACE_OUTER_BOUND('',#3091,.T.);
#1746=FACE_OUTER_BOUND('',#3092,.T.);
#1747=FACE_OUTER_BOUND('',#3093,.T.);
#1748=FACE_OUTER_BOUND('',#3094,.T.);
#1749=FACE_OUTER_BOUND('',#3095,.T.);
#1750=FACE_OUTER_BOUND('',#3096,.T.);
#1751=FACE_OUTER_BOUND('',#3097,.T.);
#1752=FACE_OUTER_BOUND('',#3098,.T.);
#1753=FACE_OUTER_BOUND('',#3099,.T.);
#1754=FACE_OUTER_BOUND('',#3100,.T.);
#1755=FACE_OUTER_BOUND('',#3101,.T.);
#1756=FACE_OUTER_BOUND('',#3102,.T.);
#1757=FACE_OUTER_BOUND('',#3103,.T.);
#1758=FACE_OUTER_BOUND('',#3104,.T.);
#1759=FACE_OUTER_BOUND('',#3105,.T.);
#1760=FACE_OUTER_BOUND('',#3106,.T.);
#1761=FACE_OUTER_BOUND('',#3107,.T.);
#1762=FACE_OUTER_BOUND('',#3108,.T.);
#1763=FACE_OUTER_BOUND('',#3109,.T.);
#1764=FACE_OUTER_BOUND('',#3110,.T.);
#1765=FACE_OUTER_BOUND('',#3111,.T.);
#1766=FACE_OUTER_BOUND('',#3112,.T.);
#1767=FACE_OUTER_BOUND('',#3113,.T.);
#1768=FACE_OUTER_BOUND('',#3114,.T.);
#1769=FACE_OUTER_BOUND('',#3115,.T.);
#1770=FACE_OUTER_BOUND('',#3116,.T.);
#1771=FACE_OUTER_BOUND('',#3117,.T.);
#1772=FACE_OUTER_BOUND('',#3118,.T.);
#1773=FACE_OUTER_BOUND('',#3119,.T.);
#1774=FACE_OUTER_BOUND('',#3120,.T.);
#1775=FACE_OUTER_BOUND('',#3121,.T.);
#1776=FACE_OUTER_BOUND('',#3122,.T.);
#1777=FACE_OUTER_BOUND('',#3123,.T.);
#1778=FACE_OUTER_BOUND('',#3124,.T.);
#1779=FACE_OUTER_BOUND('',#3125,.T.);
#1780=FACE_OUTER_BOUND('',#3126,.T.);
#1781=FACE_OUTER_BOUND('',#3127,.T.);
#1782=FACE_OUTER_BOUND('',#3128,.T.);
#1783=FACE_OUTER_BOUND('',#3129,.T.);
#1784=FACE_OUTER_BOUND('',#3130,.T.);
#1785=FACE_OUTER_BOUND('',#3131,.T.);
#1786=FACE_OUTER_BOUND('',#3132,.T.);
#1787=FACE_OUTER_BOUND('',#3133,.T.);
#1788=FACE_OUTER_BOUND('',#3134,.T.);
#1789=FACE_OUTER_BOUND('',#3135,.T.);
#1790=FACE_OUTER_BOUND('',#3136,.T.);
#1791=FACE_OUTER_BOUND('',#3137,.T.);
#1792=FACE_OUTER_BOUND('',#3138,.T.);
#1793=FACE_OUTER_BOUND('',#3139,.T.);
#1794=FACE_OUTER_BOUND('',#3140,.T.);
#1795=FACE_OUTER_BOUND('',#3141,.T.);
#1796=FACE_OUTER_BOUND('',#3142,.T.);
#1797=FACE_OUTER_BOUND('',#3143,.T.);
#1798=FACE_OUTER_BOUND('',#3144,.T.);
#1799=FACE_OUTER_BOUND('',#3145,.T.);
#1800=FACE_OUTER_BOUND('',#3146,.T.);
#1801=FACE_OUTER_BOUND('',#3147,.T.);
#1802=FACE_OUTER_BOUND('',#3148,.T.);
#1803=FACE_OUTER_BOUND('',#3149,.T.);
#1804=FACE_OUTER_BOUND('',#3150,.T.);
#1805=FACE_OUTER_BOUND('',#3151,.T.);
#1806=FACE_OUTER_BOUND('',#3152,.T.);
#1807=FACE_OUTER_BOUND('',#3153,.T.);
#1808=FACE_OUTER_BOUND('',#3154,.T.);
#1809=FACE_OUTER_BOUND('',#3155,.T.);
#1810=FACE_OUTER_BOUND('',#3156,.T.);
#1811=FACE_OUTER_BOUND('',#3157,.T.);
#1812=FACE_OUTER_BOUND('',#3158,.T.);
#1813=FACE_OUTER_BOUND('',#3159,.T.);
#1814=FACE_OUTER_BOUND('',#3160,.T.);
#1815=FACE_OUTER_BOUND('',#3161,.T.);
#1816=FACE_OUTER_BOUND('',#3162,.T.);
#1817=FACE_OUTER_BOUND('',#3163,.T.);
#1818=FACE_OUTER_BOUND('',#3164,.T.);
#1819=FACE_OUTER_BOUND('',#3165,.T.);
#1820=FACE_OUTER_BOUND('',#3166,.T.);
#1821=FACE_OUTER_BOUND('',#3167,.T.);
#1822=FACE_OUTER_BOUND('',#3168,.T.);
#1823=FACE_OUTER_BOUND('',#3169,.T.);
#1824=FACE_OUTER_BOUND('',#3170,.T.);
#1825=FACE_OUTER_BOUND('',#3171,.T.);
#1826=FACE_OUTER_BOUND('',#3172,.T.);
#1827=FACE_OUTER_BOUND('',#3173,.T.);
#1828=FACE_OUTER_BOUND('',#3174,.T.);
#1829=FACE_OUTER_BOUND('',#3175,.T.);
#1830=FACE_OUTER_BOUND('',#3176,.T.);
#1831=FACE_OUTER_BOUND('',#3177,.T.);
#1832=FACE_OUTER_BOUND('',#3178,.T.);
#1833=FACE_OUTER_BOUND('',#3179,.T.);
#1834=FACE_OUTER_BOUND('',#3180,.T.);
#1835=FACE_OUTER_BOUND('',#3181,.T.);
#1836=FACE_OUTER_BOUND('',#3182,.T.);
#1837=FACE_OUTER_BOUND('',#3183,.T.);
#1838=FACE_OUTER_BOUND('',#3184,.T.);
#1839=FACE_OUTER_BOUND('',#3185,.T.);
#1840=FACE_OUTER_BOUND('',#3186,.T.);
#1841=FACE_OUTER_BOUND('',#3187,.T.);
#1842=FACE_OUTER_BOUND('',#3188,.T.);
#1843=FACE_OUTER_BOUND('',#3189,.T.);
#1844=FACE_OUTER_BOUND('',#3190,.T.);
#1845=FACE_OUTER_BOUND('',#3191,.T.);
#1846=FACE_OUTER_BOUND('',#3192,.T.);
#1847=FACE_OUTER_BOUND('',#3193,.T.);
#1848=FACE_OUTER_BOUND('',#3194,.T.);
#1849=FACE_OUTER_BOUND('',#3195,.T.);
#1850=FACE_OUTER_BOUND('',#3196,.T.);
#1851=FACE_OUTER_BOUND('',#3197,.T.);
#1852=FACE_OUTER_BOUND('',#3198,.T.);
#1853=FACE_OUTER_BOUND('',#3199,.T.);
#1854=FACE_OUTER_BOUND('',#3200,.T.);
#1855=FACE_OUTER_BOUND('',#3201,.T.);
#1856=FACE_OUTER_BOUND('',#3202,.T.);
#1857=FACE_OUTER_BOUND('',#3203,.T.);
#1858=FACE_OUTER_BOUND('',#3204,.T.);
#1859=FACE_OUTER_BOUND('',#3205,.T.);
#1860=FACE_OUTER_BOUND('',#3206,.T.);
#1861=FACE_OUTER_BOUND('',#3207,.T.);
#1862=FACE_OUTER_BOUND('',#3208,.T.);
#1863=FACE_OUTER_BOUND('',#3209,.T.);
#1864=FACE_OUTER_BOUND('',#3210,.T.);
#1865=FACE_OUTER_BOUND('',#3211,.T.);
#1866=FACE_OUTER_BOUND('',#3212,.T.);
#1867=FACE_OUTER_BOUND('',#3213,.T.);
#1868=FACE_OUTER_BOUND('',#3214,.T.);
#1869=FACE_OUTER_BOUND('',#3215,.T.);
#1870=FACE_OUTER_BOUND('',#3216,.T.);
#1871=FACE_OUTER_BOUND('',#3217,.T.);
#1872=FACE_OUTER_BOUND('',#3218,.T.);
#1873=FACE_OUTER_BOUND('',#3219,.T.);
#1874=FACE_OUTER_BOUND('',#3220,.T.);
#1875=FACE_OUTER_BOUND('',#3221,.T.);
#1876=FACE_OUTER_BOUND('',#3222,.T.);
#1877=FACE_OUTER_BOUND('',#3223,.T.);
#1878=FACE_OUTER_BOUND('',#3224,.T.);
#1879=FACE_OUTER_BOUND('',#3225,.T.);
#1880=FACE_OUTER_BOUND('',#3226,.T.);
#1881=FACE_OUTER_BOUND('',#3227,.T.);
#1882=FACE_OUTER_BOUND('',#3228,.T.);
#1883=FACE_OUTER_BOUND('',#3229,.T.);
#1884=FACE_OUTER_BOUND('',#3230,.T.);
#1885=FACE_OUTER_BOUND('',#3231,.T.);
#1886=FACE_OUTER_BOUND('',#3232,.T.);
#1887=FACE_OUTER_BOUND('',#3233,.T.);
#1888=FACE_OUTER_BOUND('',#3234,.T.);
#1889=FACE_OUTER_BOUND('',#3235,.T.);
#1890=FACE_OUTER_BOUND('',#3236,.T.);
#1891=FACE_OUTER_BOUND('',#3237,.T.);
#1892=FACE_OUTER_BOUND('',#3238,.T.);
#1893=FACE_OUTER_BOUND('',#3239,.T.);
#1894=FACE_OUTER_BOUND('',#3240,.T.);
#1895=FACE_OUTER_BOUND('',#3241,.T.);
#1896=FACE_OUTER_BOUND('',#3242,.T.);
#1897=FACE_OUTER_BOUND('',#3243,.T.);
#1898=FACE_OUTER_BOUND('',#3244,.T.);
#1899=FACE_OUTER_BOUND('',#3245,.T.);
#1900=FACE_OUTER_BOUND('',#3246,.T.);
#1901=FACE_OUTER_BOUND('',#3247,.T.);
#1902=FACE_OUTER_BOUND('',#3248,.T.);
#1903=FACE_OUTER_BOUND('',#3249,.T.);
#1904=FACE_OUTER_BOUND('',#3250,.T.);
#1905=FACE_OUTER_BOUND('',#3251,.T.);
#1906=FACE_OUTER_BOUND('',#3252,.T.);
#1907=FACE_OUTER_BOUND('',#3253,.T.);
#1908=FACE_OUTER_BOUND('',#3254,.T.);
#1909=FACE_OUTER_BOUND('',#3255,.T.);
#1910=FACE_OUTER_BOUND('',#3256,.T.);
#1911=FACE_OUTER_BOUND('',#3257,.T.);
#1912=FACE_OUTER_BOUND('',#3258,.T.);
#1913=FACE_OUTER_BOUND('',#3259,.T.);
#1914=FACE_OUTER_BOUND('',#3260,.T.);
#1915=FACE_OUTER_BOUND('',#3261,.T.);
#1916=FACE_OUTER_BOUND('',#3262,.T.);
#1917=FACE_OUTER_BOUND('',#3263,.T.);
#1918=FACE_OUTER_BOUND('',#3264,.T.);
#1919=FACE_OUTER_BOUND('',#3265,.T.);
#1920=FACE_OUTER_BOUND('',#3266,.T.);
#1921=FACE_OUTER_BOUND('',#3267,.T.);
#1922=FACE_OUTER_BOUND('',#3268,.T.);
#1923=FACE_OUTER_BOUND('',#3269,.T.);
#1924=FACE_OUTER_BOUND('',#3270,.T.);
#1925=FACE_OUTER_BOUND('',#3271,.T.);
#1926=FACE_OUTER_BOUND('',#3272,.T.);
#1927=FACE_OUTER_BOUND('',#3273,.T.);
#1928=FACE_OUTER_BOUND('',#3274,.T.);
#1929=FACE_OUTER_BOUND('',#3275,.T.);
#1930=FACE_OUTER_BOUND('',#3276,.T.);
#1931=FACE_OUTER_BOUND('',#3277,.T.);
#1932=FACE_OUTER_BOUND('',#3278,.T.);
#1933=FACE_OUTER_BOUND('',#3279,.T.);
#1934=FACE_OUTER_BOUND('',#3280,.T.);
#1935=FACE_OUTER_BOUND('',#3281,.T.);
#1936=FACE_OUTER_BOUND('',#3282,.T.);
#1937=FACE_OUTER_BOUND('',#3283,.T.);
#1938=FACE_OUTER_BOUND('',#3284,.T.);
#1939=FACE_OUTER_BOUND('',#3285,.T.);
#1940=FACE_OUTER_BOUND('',#3286,.T.);
#1941=FACE_OUTER_BOUND('',#3287,.T.);
#1942=FACE_OUTER_BOUND('',#3288,.T.);
#1943=FACE_OUTER_BOUND('',#3289,.T.);
#1944=FACE_OUTER_BOUND('',#3290,.T.);
#1945=FACE_OUTER_BOUND('',#3291,.T.);
#1946=FACE_OUTER_BOUND('',#3292,.T.);
#1947=FACE_OUTER_BOUND('',#3293,.T.);
#1948=FACE_OUTER_BOUND('',#3294,.T.);
#1949=FACE_OUTER_BOUND('',#3295,.T.);
#1950=FACE_OUTER_BOUND('',#3296,.T.);
#1951=FACE_OUTER_BOUND('',#3297,.T.);
#1952=FACE_OUTER_BOUND('',#3298,.T.);
#1953=FACE_OUTER_BOUND('',#3299,.T.);
#1954=FACE_OUTER_BOUND('',#3300,.T.);
#1955=FACE_OUTER_BOUND('',#3301,.T.);
#1956=FACE_OUTER_BOUND('',#3302,.T.);
#1957=FACE_OUTER_BOUND('',#3303,.T.);
#1958=FACE_OUTER_BOUND('',#3304,.T.);
#1959=FACE_OUTER_BOUND('',#3305,.T.);
#1960=FACE_OUTER_BOUND('',#3306,.T.);
#1961=FACE_OUTER_BOUND('',#3307,.T.);
#1962=FACE_OUTER_BOUND('',#3308,.T.);
#1963=FACE_OUTER_BOUND('',#3309,.T.);
#1964=FACE_OUTER_BOUND('',#3310,.T.);
#1965=FACE_OUTER_BOUND('',#3311,.T.);
#1966=FACE_OUTER_BOUND('',#3312,.T.);
#1967=FACE_OUTER_BOUND('',#3313,.T.);
#1968=FACE_OUTER_BOUND('',#3314,.T.);
#1969=FACE_OUTER_BOUND('',#3315,.T.);
#1970=FACE_OUTER_BOUND('',#3316,.T.);
#1971=FACE_OUTER_BOUND('',#3317,.T.);
#1972=FACE_OUTER_BOUND('',#3318,.T.);
#1973=FACE_OUTER_BOUND('',#3319,.T.);
#1974=FACE_OUTER_BOUND('',#3320,.T.);
#1975=FACE_OUTER_BOUND('',#3321,.T.);
#1976=FACE_OUTER_BOUND('',#3322,.T.);
#1977=FACE_OUTER_BOUND('',#3323,.T.);
#1978=FACE_OUTER_BOUND('',#3324,.T.);
#1979=FACE_OUTER_BOUND('',#3325,.T.);
#1980=FACE_OUTER_BOUND('',#3326,.T.);
#1981=FACE_OUTER_BOUND('',#3327,.T.);
#1982=FACE_OUTER_BOUND('',#3328,.T.);
#1983=FACE_OUTER_BOUND('',#3329,.T.);
#1984=FACE_OUTER_BOUND('',#3330,.T.);
#1985=FACE_OUTER_BOUND('',#3331,.T.);
#1986=FACE_OUTER_BOUND('',#3332,.T.);
#1987=FACE_OUTER_BOUND('',#3333,.T.);
#1988=FACE_OUTER_BOUND('',#3334,.T.);
#1989=FACE_OUTER_BOUND('',#3335,.T.);
#1990=FACE_OUTER_BOUND('',#3336,.T.);
#1991=FACE_OUTER_BOUND('',#3337,.T.);
#1992=FACE_OUTER_BOUND('',#3338,.T.);
#1993=FACE_OUTER_BOUND('',#3339,.T.);
#1994=FACE_OUTER_BOUND('',#3340,.T.);
#1995=FACE_OUTER_BOUND('',#3341,.T.);
#1996=FACE_OUTER_BOUND('',#3342,.T.);
#1997=FACE_OUTER_BOUND('',#3343,.T.);
#1998=FACE_OUTER_BOUND('',#3344,.T.);
#1999=FACE_OUTER_BOUND('',#3345,.T.);
#2000=FACE_OUTER_BOUND('',#3346,.T.);
#2001=FACE_OUTER_BOUND('',#3347,.T.);
#2002=FACE_OUTER_BOUND('',#3348,.T.);
#2003=FACE_OUTER_BOUND('',#3349,.T.);
#2004=FACE_OUTER_BOUND('',#3351,.T.);
#2005=FACE_OUTER_BOUND('',#3361,.T.);
#2006=FACE_OUTER_BOUND('',#3371,.T.);
#2007=FACE_OUTER_BOUND('',#3381,.T.);
#2008=FACE_OUTER_BOUND('',#3387,.T.);
#2009=FACE_OUTER_BOUND('',#3388,.T.);
#2010=FACE_OUTER_BOUND('',#3389,.T.);
#2011=FACE_OUTER_BOUND('',#3391,.T.);
#2012=FACE_OUTER_BOUND('',#3397,.T.);
#2013=FACE_OUTER_BOUND('',#3398,.T.);
#2014=FACE_OUTER_BOUND('',#3399,.T.);
#2015=FACE_OUTER_BOUND('',#3400,.T.);
#2016=FACE_OUTER_BOUND('',#3401,.T.);
#2017=FACE_OUTER_BOUND('',#3402,.T.);
#2018=FACE_OUTER_BOUND('',#3403,.T.);
#2019=FACE_OUTER_BOUND('',#3404,.T.);
#2020=FACE_OUTER_BOUND('',#3405,.T.);
#2021=FACE_OUTER_BOUND('',#3406,.T.);
#2022=FACE_OUTER_BOUND('',#3410,.T.);
#2023=FACE_OUTER_BOUND('',#3412,.T.);
#2024=FACE_OUTER_BOUND('',#3414,.T.);
#2025=FACE_OUTER_BOUND('',#3415,.T.);
#2026=FACE_OUTER_BOUND('',#3416,.T.);
#2027=FACE_OUTER_BOUND('',#3417,.T.);
#2028=FACE_OUTER_BOUND('',#3418,.T.);
#2029=FACE_OUTER_BOUND('',#3419,.T.);
#2030=FACE_OUTER_BOUND('',#3420,.T.);
#2031=FACE_OUTER_BOUND('',#3421,.T.);
#2032=FACE_OUTER_BOUND('',#3422,.T.);
#2033=FACE_OUTER_BOUND('',#3423,.T.);
#2034=FACE_OUTER_BOUND('',#3424,.T.);
#2035=FACE_OUTER_BOUND('',#3434,.T.);
#2036=FACE_OUTER_BOUND('',#3444,.T.);
#2037=FACE_OUTER_BOUND('',#3445,.T.);
#2038=FACE_OUTER_BOUND('',#3446,.T.);
#2039=FACE_OUTER_BOUND('',#3447,.T.);
#2040=FACE_OUTER_BOUND('',#3448,.T.);
#2041=FACE_OUTER_BOUND('',#3449,.T.);
#2042=FACE_OUTER_BOUND('',#3450,.T.);
#2043=FACE_OUTER_BOUND('',#3452,.T.);
#2044=FACE_OUTER_BOUND('',#3454,.T.);
#2045=FACE_OUTER_BOUND('',#3455,.T.);
#2046=FACE_OUTER_BOUND('',#3456,.T.);
#2047=FACE_OUTER_BOUND('',#3458,.T.);
#2048=FACE_OUTER_BOUND('',#3460,.T.);
#2049=FACE_OUTER_BOUND('',#3461,.T.);
#2050=FACE_OUTER_BOUND('',#3463,.T.);
#2051=FACE_OUTER_BOUND('',#3465,.T.);
#2052=FACE_OUTER_BOUND('',#3466,.T.);
#2053=FACE_OUTER_BOUND('',#3467,.T.);
#2054=FACE_OUTER_BOUND('',#3469,.T.);
#2055=FACE_OUTER_BOUND('',#3471,.T.);
#2056=FACE_OUTER_BOUND('',#3472,.T.);
#2057=FACE_OUTER_BOUND('',#3473,.T.);
#2058=FACE_OUTER_BOUND('',#3475,.T.);
#2059=FACE_OUTER_BOUND('',#3476,.T.);
#2060=FACE_OUTER_BOUND('',#3477,.T.);
#2061=FACE_OUTER_BOUND('',#3478,.T.);
#2062=FACE_OUTER_BOUND('',#3479,.T.);
#2063=FACE_OUTER_BOUND('',#3481,.T.);
#2064=FACE_OUTER_BOUND('',#3483,.T.);
#2065=FACE_OUTER_BOUND('',#3484,.T.);
#2066=FACE_OUTER_BOUND('',#3485,.T.);
#2067=FACE_OUTER_BOUND('',#3486,.T.);
#2068=FACE_OUTER_BOUND('',#3487,.T.);
#2069=FACE_OUTER_BOUND('',#3488,.T.);
#2070=FACE_OUTER_BOUND('',#3489,.T.);
#2071=FACE_OUTER_BOUND('',#3490,.T.);
#2072=FACE_OUTER_BOUND('',#3491,.T.);
#2073=FACE_OUTER_BOUND('',#3492,.T.);
#2074=FACE_OUTER_BOUND('',#3493,.T.);
#2075=FACE_OUTER_BOUND('',#3494,.T.);
#2076=FACE_OUTER_BOUND('',#3495,.T.);
#2077=FACE_OUTER_BOUND('',#3496,.T.);
#2078=FACE_OUTER_BOUND('',#3497,.T.);
#2079=FACE_OUTER_BOUND('',#3498,.T.);
#2080=FACE_OUTER_BOUND('',#3499,.T.);
#2081=FACE_OUTER_BOUND('',#3500,.T.);
#2082=FACE_OUTER_BOUND('',#3501,.T.);
#2083=FACE_OUTER_BOUND('',#3502,.T.);
#2084=FACE_OUTER_BOUND('',#3503,.T.);
#2085=FACE_OUTER_BOUND('',#3504,.T.);
#2086=FACE_OUTER_BOUND('',#3505,.T.);
#2087=FACE_OUTER_BOUND('',#3506,.T.);
#2088=FACE_OUTER_BOUND('',#3507,.T.);
#2089=FACE_OUTER_BOUND('',#3508,.T.);
#2090=FACE_OUTER_BOUND('',#3509,.T.);
#2091=FACE_OUTER_BOUND('',#3510,.T.);
#2092=FACE_OUTER_BOUND('',#3511,.T.);
#2093=FACE_OUTER_BOUND('',#3512,.T.);
#2094=FACE_OUTER_BOUND('',#3513,.T.);
#2095=FACE_OUTER_BOUND('',#3514,.T.);
#2096=FACE_OUTER_BOUND('',#3515,.T.);
#2097=FACE_OUTER_BOUND('',#3516,.T.);
#2098=FACE_OUTER_BOUND('',#3517,.T.);
#2099=FACE_OUTER_BOUND('',#3518,.T.);
#2100=FACE_OUTER_BOUND('',#3519,.T.);
#2101=FACE_OUTER_BOUND('',#3520,.T.);
#2102=FACE_OUTER_BOUND('',#3521,.T.);
#2103=FACE_OUTER_BOUND('',#3522,.T.);
#2104=FACE_OUTER_BOUND('',#3523,.T.);
#2105=FACE_OUTER_BOUND('',#3524,.T.);
#2106=FACE_OUTER_BOUND('',#3525,.T.);
#2107=FACE_OUTER_BOUND('',#3526,.T.);
#2108=FACE_OUTER_BOUND('',#3527,.T.);
#2109=FACE_OUTER_BOUND('',#3528,.T.);
#2110=FACE_OUTER_BOUND('',#3529,.T.);
#2111=FACE_OUTER_BOUND('',#3530,.T.);
#2112=FACE_OUTER_BOUND('',#3531,.T.);
#2113=FACE_OUTER_BOUND('',#3532,.T.);
#2114=FACE_OUTER_BOUND('',#3533,.T.);
#2115=FACE_OUTER_BOUND('',#3534,.T.);
#2116=FACE_OUTER_BOUND('',#3535,.T.);
#2117=FACE_OUTER_BOUND('',#3536,.T.);
#2118=FACE_OUTER_BOUND('',#3537,.T.);
#2119=FACE_OUTER_BOUND('',#3538,.T.);
#2120=FACE_OUTER_BOUND('',#3539,.T.);
#2121=FACE_OUTER_BOUND('',#3540,.T.);
#2122=FACE_OUTER_BOUND('',#3541,.T.);
#2123=FACE_OUTER_BOUND('',#3542,.T.);
#2124=FACE_OUTER_BOUND('',#3543,.T.);
#2125=FACE_OUTER_BOUND('',#3544,.T.);
#2126=FACE_OUTER_BOUND('',#3545,.T.);
#2127=FACE_OUTER_BOUND('',#3546,.T.);
#2128=FACE_OUTER_BOUND('',#3547,.T.);
#2129=FACE_OUTER_BOUND('',#3548,.T.);
#2130=FACE_OUTER_BOUND('',#3549,.T.);
#2131=FACE_OUTER_BOUND('',#3550,.T.);
#2132=FACE_OUTER_BOUND('',#3551,.T.);
#2133=FACE_OUTER_BOUND('',#3552,.T.);
#2134=FACE_OUTER_BOUND('',#3553,.T.);
#2135=FACE_OUTER_BOUND('',#3554,.T.);
#2136=FACE_OUTER_BOUND('',#3555,.T.);
#2137=FACE_OUTER_BOUND('',#3556,.T.);
#2138=FACE_OUTER_BOUND('',#3557,.T.);
#2139=FACE_OUTER_BOUND('',#3558,.T.);
#2140=FACE_OUTER_BOUND('',#3559,.T.);
#2141=FACE_OUTER_BOUND('',#3560,.T.);
#2142=FACE_OUTER_BOUND('',#3561,.T.);
#2143=FACE_OUTER_BOUND('',#3562,.T.);
#2144=FACE_OUTER_BOUND('',#3563,.T.);
#2145=FACE_OUTER_BOUND('',#3564,.T.);
#2146=FACE_OUTER_BOUND('',#3565,.T.);
#2147=FACE_OUTER_BOUND('',#3566,.T.);
#2148=FACE_OUTER_BOUND('',#3567,.T.);
#2149=FACE_OUTER_BOUND('',#3568,.T.);
#2150=FACE_OUTER_BOUND('',#3569,.T.);
#2151=FACE_OUTER_BOUND('',#3570,.T.);
#2152=FACE_OUTER_BOUND('',#3571,.T.);
#2153=FACE_OUTER_BOUND('',#3572,.T.);
#2154=FACE_OUTER_BOUND('',#3573,.T.);
#2155=FACE_OUTER_BOUND('',#3574,.T.);
#2156=FACE_OUTER_BOUND('',#3575,.T.);
#2157=FACE_OUTER_BOUND('',#3576,.T.);
#2158=FACE_OUTER_BOUND('',#3577,.T.);
#2159=FACE_OUTER_BOUND('',#3578,.T.);
#2160=FACE_OUTER_BOUND('',#3579,.T.);
#2161=FACE_OUTER_BOUND('',#3580,.T.);
#2162=FACE_OUTER_BOUND('',#3581,.T.);
#2163=FACE_OUTER_BOUND('',#3582,.T.);
#2164=FACE_OUTER_BOUND('',#3583,.T.);
#2165=FACE_OUTER_BOUND('',#3584,.T.);
#2166=FACE_OUTER_BOUND('',#3585,.T.);
#2167=FACE_OUTER_BOUND('',#3586,.T.);
#2168=FACE_OUTER_BOUND('',#3587,.T.);
#2169=FACE_OUTER_BOUND('',#3588,.T.);
#2170=FACE_OUTER_BOUND('',#3589,.T.);
#2171=FACE_OUTER_BOUND('',#3590,.T.);
#2172=FACE_OUTER_BOUND('',#3591,.T.);
#2173=FACE_OUTER_BOUND('',#3592,.T.);
#2174=FACE_OUTER_BOUND('',#3593,.T.);
#2175=FACE_OUTER_BOUND('',#3594,.T.);
#2176=FACE_OUTER_BOUND('',#3595,.T.);
#2177=FACE_OUTER_BOUND('',#3596,.T.);
#2178=FACE_OUTER_BOUND('',#3597,.T.);
#2179=FACE_OUTER_BOUND('',#3598,.T.);
#2180=FACE_OUTER_BOUND('',#3599,.T.);
#2181=FACE_OUTER_BOUND('',#3600,.T.);
#2182=FACE_OUTER_BOUND('',#3601,.T.);
#2183=FACE_OUTER_BOUND('',#3602,.T.);
#2184=FACE_OUTER_BOUND('',#3603,.T.);
#2185=FACE_OUTER_BOUND('',#3604,.T.);
#2186=FACE_OUTER_BOUND('',#3605,.T.);
#2187=FACE_OUTER_BOUND('',#3606,.T.);
#2188=FACE_OUTER_BOUND('',#3607,.T.);
#2189=FACE_OUTER_BOUND('',#3608,.T.);
#2190=FACE_OUTER_BOUND('',#3609,.T.);
#2191=FACE_OUTER_BOUND('',#3610,.T.);
#2192=FACE_OUTER_BOUND('',#3611,.T.);
#2193=FACE_OUTER_BOUND('',#3612,.T.);
#2194=FACE_OUTER_BOUND('',#3613,.T.);
#2195=FACE_OUTER_BOUND('',#3614,.T.);
#2196=FACE_OUTER_BOUND('',#3615,.T.);
#2197=FACE_OUTER_BOUND('',#3616,.T.);
#2198=FACE_OUTER_BOUND('',#3617,.T.);
#2199=FACE_OUTER_BOUND('',#3618,.T.);
#2200=FACE_OUTER_BOUND('',#3619,.T.);
#2201=FACE_OUTER_BOUND('',#3620,.T.);
#2202=FACE_OUTER_BOUND('',#3621,.T.);
#2203=FACE_OUTER_BOUND('',#3622,.T.);
#2204=FACE_OUTER_BOUND('',#3623,.T.);
#2205=FACE_OUTER_BOUND('',#3624,.T.);
#2206=FACE_OUTER_BOUND('',#3625,.T.);
#2207=FACE_OUTER_BOUND('',#3626,.T.);
#2208=FACE_OUTER_BOUND('',#3627,.T.);
#2209=FACE_OUTER_BOUND('',#3628,.T.);
#2210=FACE_OUTER_BOUND('',#3629,.T.);
#2211=FACE_OUTER_BOUND('',#3630,.T.);
#2212=FACE_OUTER_BOUND('',#3631,.T.);
#2213=FACE_OUTER_BOUND('',#3632,.T.);
#2214=FACE_OUTER_BOUND('',#3633,.T.);
#2215=FACE_OUTER_BOUND('',#3634,.T.);
#2216=FACE_OUTER_BOUND('',#3635,.T.);
#2217=FACE_OUTER_BOUND('',#3636,.T.);
#2218=FACE_OUTER_BOUND('',#3637,.T.);
#2219=FACE_OUTER_BOUND('',#3638,.T.);
#2220=FACE_OUTER_BOUND('',#3639,.T.);
#2221=FACE_OUTER_BOUND('',#3640,.T.);
#2222=FACE_OUTER_BOUND('',#3641,.T.);
#2223=FACE_OUTER_BOUND('',#3642,.T.);
#2224=FACE_OUTER_BOUND('',#3643,.T.);
#2225=FACE_OUTER_BOUND('',#3644,.T.);
#2226=FACE_OUTER_BOUND('',#3645,.T.);
#2227=FACE_OUTER_BOUND('',#3646,.T.);
#2228=FACE_OUTER_BOUND('',#3647,.T.);
#2229=FACE_OUTER_BOUND('',#3648,.T.);
#2230=FACE_OUTER_BOUND('',#3649,.T.);
#2231=FACE_OUTER_BOUND('',#3650,.T.);
#2232=FACE_OUTER_BOUND('',#3651,.T.);
#2233=FACE_OUTER_BOUND('',#3652,.T.);
#2234=FACE_OUTER_BOUND('',#3653,.T.);
#2235=FACE_OUTER_BOUND('',#3654,.T.);
#2236=FACE_OUTER_BOUND('',#3655,.T.);
#2237=FACE_OUTER_BOUND('',#3656,.T.);
#2238=FACE_OUTER_BOUND('',#3657,.T.);
#2239=FACE_OUTER_BOUND('',#3658,.T.);
#2240=FACE_OUTER_BOUND('',#3659,.T.);
#2241=FACE_OUTER_BOUND('',#3660,.T.);
#2242=FACE_OUTER_BOUND('',#3661,.T.);
#2243=FACE_OUTER_BOUND('',#3662,.T.);
#2244=FACE_OUTER_BOUND('',#3663,.T.);
#2245=FACE_OUTER_BOUND('',#3664,.T.);
#2246=FACE_OUTER_BOUND('',#3665,.T.);
#2247=FACE_OUTER_BOUND('',#3666,.T.);
#2248=FACE_OUTER_BOUND('',#3667,.T.);
#2249=FACE_OUTER_BOUND('',#3668,.T.);
#2250=FACE_OUTER_BOUND('',#3669,.T.);
#2251=FACE_OUTER_BOUND('',#3670,.T.);
#2252=FACE_OUTER_BOUND('',#3671,.T.);
#2253=FACE_OUTER_BOUND('',#3672,.T.);
#2254=FACE_OUTER_BOUND('',#3673,.T.);
#2255=FACE_OUTER_BOUND('',#3674,.T.);
#2256=FACE_OUTER_BOUND('',#3675,.T.);
#2257=FACE_OUTER_BOUND('',#3676,.T.);
#2258=FACE_OUTER_BOUND('',#3677,.T.);
#2259=FACE_OUTER_BOUND('',#3678,.T.);
#2260=FACE_OUTER_BOUND('',#3679,.T.);
#2261=FACE_OUTER_BOUND('',#3680,.T.);
#2262=FACE_OUTER_BOUND('',#3681,.T.);
#2263=FACE_OUTER_BOUND('',#3682,.T.);
#2264=FACE_OUTER_BOUND('',#3683,.T.);
#2265=FACE_OUTER_BOUND('',#3684,.T.);
#2266=FACE_OUTER_BOUND('',#3685,.T.);
#2267=FACE_OUTER_BOUND('',#3686,.T.);
#2268=FACE_OUTER_BOUND('',#3687,.T.);
#2269=FACE_OUTER_BOUND('',#3688,.T.);
#2270=FACE_OUTER_BOUND('',#3689,.T.);
#2271=FACE_OUTER_BOUND('',#3690,.T.);
#2272=FACE_OUTER_BOUND('',#3691,.T.);
#2273=FACE_OUTER_BOUND('',#3692,.T.);
#2274=FACE_OUTER_BOUND('',#3693,.T.);
#2275=FACE_OUTER_BOUND('',#3694,.T.);
#2276=FACE_OUTER_BOUND('',#3695,.T.);
#2277=FACE_OUTER_BOUND('',#3696,.T.);
#2278=FACE_OUTER_BOUND('',#3697,.T.);
#2279=FACE_OUTER_BOUND('',#3698,.T.);
#2280=FACE_OUTER_BOUND('',#3699,.T.);
#2281=FACE_OUTER_BOUND('',#3700,.T.);
#2282=FACE_OUTER_BOUND('',#3701,.T.);
#2283=FACE_OUTER_BOUND('',#3702,.T.);
#2284=FACE_OUTER_BOUND('',#3703,.T.);
#2285=FACE_OUTER_BOUND('',#3704,.T.);
#2286=FACE_OUTER_BOUND('',#3705,.T.);
#2287=FACE_OUTER_BOUND('',#3706,.T.);
#2288=FACE_OUTER_BOUND('',#3707,.T.);
#2289=FACE_OUTER_BOUND('',#3708,.T.);
#2290=FACE_OUTER_BOUND('',#3709,.T.);
#2291=FACE_OUTER_BOUND('',#3710,.T.);
#2292=FACE_OUTER_BOUND('',#3711,.T.);
#2293=FACE_OUTER_BOUND('',#3712,.T.);
#2294=FACE_OUTER_BOUND('',#3713,.T.);
#2295=FACE_OUTER_BOUND('',#3714,.T.);
#2296=FACE_OUTER_BOUND('',#3715,.T.);
#2297=FACE_OUTER_BOUND('',#3716,.T.);
#2298=FACE_OUTER_BOUND('',#3717,.T.);
#2299=FACE_OUTER_BOUND('',#3718,.T.);
#2300=FACE_OUTER_BOUND('',#3719,.T.);
#2301=FACE_OUTER_BOUND('',#3720,.T.);
#2302=FACE_OUTER_BOUND('',#3721,.T.);
#2303=FACE_OUTER_BOUND('',#3722,.T.);
#2304=FACE_OUTER_BOUND('',#3723,.T.);
#2305=FACE_OUTER_BOUND('',#3724,.T.);
#2306=FACE_OUTER_BOUND('',#3725,.T.);
#2307=FACE_OUTER_BOUND('',#3726,.T.);
#2308=FACE_OUTER_BOUND('',#3727,.T.);
#2309=FACE_OUTER_BOUND('',#3728,.T.);
#2310=FACE_OUTER_BOUND('',#3729,.T.);
#2311=FACE_OUTER_BOUND('',#3730,.T.);
#2312=FACE_OUTER_BOUND('',#3731,.T.);
#2313=FACE_OUTER_BOUND('',#3732,.T.);
#2314=FACE_OUTER_BOUND('',#3733,.T.);
#2315=FACE_OUTER_BOUND('',#3734,.T.);
#2316=FACE_OUTER_BOUND('',#3735,.T.);
#2317=FACE_OUTER_BOUND('',#3736,.T.);
#2318=FACE_OUTER_BOUND('',#3737,.T.);
#2319=FACE_OUTER_BOUND('',#3738,.T.);
#2320=FACE_OUTER_BOUND('',#3739,.T.);
#2321=FACE_OUTER_BOUND('',#3740,.T.);
#2322=FACE_OUTER_BOUND('',#3741,.T.);
#2323=FACE_OUTER_BOUND('',#3742,.T.);
#2324=FACE_OUTER_BOUND('',#3743,.T.);
#2325=FACE_OUTER_BOUND('',#3744,.T.);
#2326=FACE_OUTER_BOUND('',#3745,.T.);
#2327=FACE_OUTER_BOUND('',#3746,.T.);
#2328=FACE_OUTER_BOUND('',#3747,.T.);
#2329=FACE_OUTER_BOUND('',#3748,.T.);
#2330=FACE_OUTER_BOUND('',#3749,.T.);
#2331=FACE_OUTER_BOUND('',#3750,.T.);
#2332=FACE_OUTER_BOUND('',#3751,.T.);
#2333=FACE_OUTER_BOUND('',#3752,.T.);
#2334=FACE_OUTER_BOUND('',#3753,.T.);
#2335=FACE_OUTER_BOUND('',#3754,.T.);
#2336=FACE_OUTER_BOUND('',#3755,.T.);
#2337=FACE_OUTER_BOUND('',#3756,.T.);
#2338=FACE_OUTER_BOUND('',#3757,.T.);
#2339=FACE_OUTER_BOUND('',#3758,.T.);
#2340=FACE_OUTER_BOUND('',#3759,.T.);
#2341=FACE_OUTER_BOUND('',#3760,.T.);
#2342=FACE_OUTER_BOUND('',#3761,.T.);
#2343=FACE_OUTER_BOUND('',#3762,.T.);
#2344=FACE_OUTER_BOUND('',#3763,.T.);
#2345=FACE_OUTER_BOUND('',#3764,.T.);
#2346=FACE_OUTER_BOUND('',#3765,.T.);
#2347=FACE_OUTER_BOUND('',#3766,.T.);
#2348=FACE_OUTER_BOUND('',#3767,.T.);
#2349=FACE_OUTER_BOUND('',#3768,.T.);
#2350=FACE_OUTER_BOUND('',#3769,.T.);
#2351=FACE_OUTER_BOUND('',#3770,.T.);
#2352=FACE_OUTER_BOUND('',#3771,.T.);
#2353=FACE_OUTER_BOUND('',#3772,.T.);
#2354=FACE_OUTER_BOUND('',#3773,.T.);
#2355=FACE_OUTER_BOUND('',#3774,.T.);
#2356=FACE_OUTER_BOUND('',#3775,.T.);
#2357=FACE_OUTER_BOUND('',#3776,.T.);
#2358=FACE_OUTER_BOUND('',#3777,.T.);
#2359=FACE_OUTER_BOUND('',#3778,.T.);
#2360=FACE_OUTER_BOUND('',#3779,.T.);
#2361=FACE_OUTER_BOUND('',#3780,.T.);
#2362=FACE_OUTER_BOUND('',#3781,.T.);
#2363=FACE_OUTER_BOUND('',#3782,.T.);
#2364=FACE_OUTER_BOUND('',#3783,.T.);
#2365=FACE_OUTER_BOUND('',#3784,.T.);
#2366=FACE_OUTER_BOUND('',#3785,.T.);
#2367=FACE_OUTER_BOUND('',#3786,.T.);
#2368=FACE_OUTER_BOUND('',#3787,.T.);
#2369=FACE_OUTER_BOUND('',#3788,.T.);
#2370=FACE_OUTER_BOUND('',#3789,.T.);
#2371=FACE_OUTER_BOUND('',#3790,.T.);
#2372=FACE_OUTER_BOUND('',#3791,.T.);
#2373=FACE_OUTER_BOUND('',#3792,.T.);
#2374=FACE_OUTER_BOUND('',#3793,.T.);
#2375=FACE_OUTER_BOUND('',#3794,.T.);
#2376=FACE_OUTER_BOUND('',#3795,.T.);
#2377=FACE_OUTER_BOUND('',#3796,.T.);
#2378=FACE_OUTER_BOUND('',#3797,.T.);
#2379=FACE_OUTER_BOUND('',#3798,.T.);
#2380=FACE_OUTER_BOUND('',#3799,.T.);
#2381=FACE_OUTER_BOUND('',#3800,.T.);
#2382=FACE_OUTER_BOUND('',#3801,.T.);
#2383=FACE_OUTER_BOUND('',#3802,.T.);
#2384=FACE_OUTER_BOUND('',#3803,.T.);
#2385=FACE_OUTER_BOUND('',#3804,.T.);
#2386=FACE_OUTER_BOUND('',#3805,.T.);
#2387=FACE_OUTER_BOUND('',#3806,.T.);
#2388=FACE_OUTER_BOUND('',#3807,.T.);
#2389=FACE_OUTER_BOUND('',#3808,.T.);
#2390=FACE_OUTER_BOUND('',#3809,.T.);
#2391=FACE_OUTER_BOUND('',#3810,.T.);
#2392=FACE_OUTER_BOUND('',#3811,.T.);
#2393=FACE_OUTER_BOUND('',#3812,.T.);
#2394=FACE_OUTER_BOUND('',#3813,.T.);
#2395=FACE_OUTER_BOUND('',#3814,.T.);
#2396=FACE_OUTER_BOUND('',#3815,.T.);
#2397=FACE_OUTER_BOUND('',#3816,.T.);
#2398=FACE_OUTER_BOUND('',#3817,.T.);
#2399=FACE_OUTER_BOUND('',#3818,.T.);
#2400=FACE_OUTER_BOUND('',#3819,.T.);
#2401=FACE_OUTER_BOUND('',#3820,.T.);
#2402=FACE_OUTER_BOUND('',#3821,.T.);
#2403=FACE_OUTER_BOUND('',#3822,.T.);
#2404=FACE_OUTER_BOUND('',#3823,.T.);
#2405=FACE_OUTER_BOUND('',#3824,.T.);
#2406=FACE_OUTER_BOUND('',#3825,.T.);
#2407=FACE_OUTER_BOUND('',#3826,.T.);
#2408=FACE_OUTER_BOUND('',#3827,.T.);
#2409=FACE_OUTER_BOUND('',#3828,.T.);
#2410=FACE_OUTER_BOUND('',#3829,.T.);
#2411=FACE_OUTER_BOUND('',#3830,.T.);
#2412=FACE_OUTER_BOUND('',#3831,.T.);
#2413=FACE_OUTER_BOUND('',#3832,.T.);
#2414=FACE_OUTER_BOUND('',#3833,.T.);
#2415=FACE_OUTER_BOUND('',#3834,.T.);
#2416=FACE_OUTER_BOUND('',#3835,.T.);
#2417=FACE_OUTER_BOUND('',#3836,.T.);
#2418=FACE_OUTER_BOUND('',#3837,.T.);
#2419=FACE_OUTER_BOUND('',#3838,.T.);
#2420=FACE_OUTER_BOUND('',#3839,.T.);
#2421=FACE_OUTER_BOUND('',#3840,.T.);
#2422=FACE_OUTER_BOUND('',#3841,.T.);
#2423=FACE_OUTER_BOUND('',#3842,.T.);
#2424=FACE_OUTER_BOUND('',#3843,.T.);
#2425=FACE_OUTER_BOUND('',#3844,.T.);
#2426=FACE_OUTER_BOUND('',#3845,.T.);
#2427=FACE_OUTER_BOUND('',#3846,.T.);
#2428=FACE_OUTER_BOUND('',#3847,.T.);
#2429=FACE_OUTER_BOUND('',#3848,.T.);
#2430=FACE_OUTER_BOUND('',#3849,.T.);
#2431=FACE_OUTER_BOUND('',#3850,.T.);
#2432=FACE_OUTER_BOUND('',#3851,.T.);
#2433=FACE_OUTER_BOUND('',#3852,.T.);
#2434=FACE_OUTER_BOUND('',#3853,.T.);
#2435=FACE_OUTER_BOUND('',#3854,.T.);
#2436=FACE_OUTER_BOUND('',#3855,.T.);
#2437=FACE_OUTER_BOUND('',#3856,.T.);
#2438=FACE_OUTER_BOUND('',#3857,.T.);
#2439=FACE_OUTER_BOUND('',#3858,.T.);
#2440=FACE_OUTER_BOUND('',#3859,.T.);
#2441=FACE_OUTER_BOUND('',#3860,.T.);
#2442=FACE_OUTER_BOUND('',#3861,.T.);
#2443=FACE_OUTER_BOUND('',#3862,.T.);
#2444=FACE_OUTER_BOUND('',#3863,.T.);
#2445=FACE_OUTER_BOUND('',#3864,.T.);
#2446=FACE_OUTER_BOUND('',#3865,.T.);
#2447=FACE_OUTER_BOUND('',#3866,.T.);
#2448=FACE_OUTER_BOUND('',#3867,.T.);
#2449=FACE_OUTER_BOUND('',#3868,.T.);
#2450=FACE_OUTER_BOUND('',#3869,.T.);
#2451=FACE_OUTER_BOUND('',#3870,.T.);
#2452=FACE_OUTER_BOUND('',#3871,.T.);
#2453=FACE_OUTER_BOUND('',#3872,.T.);
#2454=FACE_OUTER_BOUND('',#3873,.T.);
#2455=FACE_OUTER_BOUND('',#3874,.T.);
#2456=FACE_OUTER_BOUND('',#3875,.T.);
#2457=FACE_OUTER_BOUND('',#3876,.T.);
#2458=FACE_OUTER_BOUND('',#3877,.T.);
#2459=FACE_OUTER_BOUND('',#3878,.T.);
#2460=FACE_OUTER_BOUND('',#3879,.T.);
#2461=FACE_OUTER_BOUND('',#3880,.T.);
#2462=FACE_OUTER_BOUND('',#3881,.T.);
#2463=FACE_OUTER_BOUND('',#3882,.T.);
#2464=FACE_OUTER_BOUND('',#3883,.T.);
#2465=FACE_OUTER_BOUND('',#3884,.T.);
#2466=FACE_OUTER_BOUND('',#3885,.T.);
#2467=FACE_OUTER_BOUND('',#3886,.T.);
#2468=FACE_OUTER_BOUND('',#3887,.T.);
#2469=FACE_OUTER_BOUND('',#3888,.T.);
#2470=FACE_OUTER_BOUND('',#3889,.T.);
#2471=FACE_OUTER_BOUND('',#3890,.T.);
#2472=FACE_OUTER_BOUND('',#3891,.T.);
#2473=FACE_OUTER_BOUND('',#3892,.T.);
#2474=FACE_OUTER_BOUND('',#3893,.T.);
#2475=FACE_OUTER_BOUND('',#3894,.T.);
#2476=FACE_OUTER_BOUND('',#3895,.T.);
#2477=FACE_OUTER_BOUND('',#3896,.T.);
#2478=FACE_OUTER_BOUND('',#3897,.T.);
#2479=FACE_OUTER_BOUND('',#3898,.T.);
#2480=FACE_OUTER_BOUND('',#3899,.T.);
#2481=FACE_OUTER_BOUND('',#3900,.T.);
#2482=FACE_OUTER_BOUND('',#3901,.T.);
#2483=FACE_OUTER_BOUND('',#3902,.T.);
#2484=FACE_OUTER_BOUND('',#3903,.T.);
#2485=FACE_OUTER_BOUND('',#3904,.T.);
#2486=FACE_OUTER_BOUND('',#3905,.T.);
#2487=FACE_OUTER_BOUND('',#3906,.T.);
#2488=FACE_OUTER_BOUND('',#3907,.T.);
#2489=FACE_OUTER_BOUND('',#3908,.T.);
#2490=FACE_OUTER_BOUND('',#3909,.T.);
#2491=FACE_OUTER_BOUND('',#3910,.T.);
#2492=FACE_OUTER_BOUND('',#3911,.T.);
#2493=FACE_OUTER_BOUND('',#3912,.T.);
#2494=FACE_OUTER_BOUND('',#3913,.T.);
#2495=FACE_OUTER_BOUND('',#3914,.T.);
#2496=FACE_OUTER_BOUND('',#3915,.T.);
#2497=FACE_OUTER_BOUND('',#3916,.T.);
#2498=FACE_OUTER_BOUND('',#3917,.T.);
#2499=FACE_OUTER_BOUND('',#3918,.T.);
#2500=FACE_OUTER_BOUND('',#3919,.T.);
#2501=FACE_OUTER_BOUND('',#3920,.T.);
#2502=FACE_OUTER_BOUND('',#3921,.T.);
#2503=FACE_OUTER_BOUND('',#3922,.T.);
#2504=FACE_OUTER_BOUND('',#3924,.T.);
#2505=FACE_OUTER_BOUND('',#3925,.T.);
#2506=FACE_OUTER_BOUND('',#3929,.T.);
#2507=FACE_OUTER_BOUND('',#3931,.T.);
#2508=FACE_OUTER_BOUND('',#3932,.T.);
#2509=FACE_OUTER_BOUND('',#3933,.T.);
#2510=FACE_OUTER_BOUND('',#3934,.T.);
#2511=FACE_OUTER_BOUND('',#3935,.T.);
#2512=FACE_OUTER_BOUND('',#3937,.T.);
#2513=FACE_OUTER_BOUND('',#3938,.T.);
#2514=FACE_OUTER_BOUND('',#3939,.T.);
#2515=FACE_OUTER_BOUND('',#3940,.T.);
#2516=FACE_OUTER_BOUND('',#3941,.T.);
#2517=FACE_OUTER_BOUND('',#3942,.T.);
#2518=FACE_OUTER_BOUND('',#3943,.T.);
#2519=FACE_OUTER_BOUND('',#3944,.T.);
#2520=FACE_OUTER_BOUND('',#3945,.T.);
#2521=FACE_OUTER_BOUND('',#3946,.T.);
#2522=FACE_OUTER_BOUND('',#3947,.T.);
#2523=FACE_OUTER_BOUND('',#3948,.T.);
#2524=FACE_OUTER_BOUND('',#3949,.T.);
#2525=FACE_OUTER_BOUND('',#3950,.T.);
#2526=FACE_OUTER_BOUND('',#3951,.T.);
#2527=FACE_OUTER_BOUND('',#3952,.T.);
#2528=FACE_OUTER_BOUND('',#3953,.T.);
#2529=FACE_OUTER_BOUND('',#3954,.T.);
#2530=FACE_OUTER_BOUND('',#3955,.T.);
#2531=FACE_OUTER_BOUND('',#3956,.T.);
#2532=FACE_OUTER_BOUND('',#3957,.T.);
#2533=FACE_OUTER_BOUND('',#3958,.T.);
#2534=FACE_OUTER_BOUND('',#3959,.T.);
#2535=FACE_OUTER_BOUND('',#3960,.T.);
#2536=FACE_OUTER_BOUND('',#3961,.T.);
#2537=FACE_OUTER_BOUND('',#3962,.T.);
#2538=FACE_OUTER_BOUND('',#3963,.T.);
#2539=FACE_OUTER_BOUND('',#3964,.T.);
#2540=FACE_OUTER_BOUND('',#3965,.T.);
#2541=FACE_OUTER_BOUND('',#3966,.T.);
#2542=FACE_OUTER_BOUND('',#3967,.T.);
#2543=FACE_OUTER_BOUND('',#3968,.T.);
#2544=FACE_OUTER_BOUND('',#3969,.T.);
#2545=FACE_OUTER_BOUND('',#3970,.T.);
#2546=FACE_OUTER_BOUND('',#3971,.T.);
#2547=FACE_OUTER_BOUND('',#3972,.T.);
#2548=FACE_OUTER_BOUND('',#3973,.T.);
#2549=FACE_OUTER_BOUND('',#3974,.T.);
#2550=FACE_OUTER_BOUND('',#3975,.T.);
#2551=FACE_OUTER_BOUND('',#3976,.T.);
#2552=FACE_OUTER_BOUND('',#3977,.T.);
#2553=FACE_OUTER_BOUND('',#3978,.T.);
#2554=FACE_OUTER_BOUND('',#3979,.T.);
#2555=FACE_OUTER_BOUND('',#3980,.T.);
#2556=FACE_OUTER_BOUND('',#3981,.T.);
#2557=FACE_OUTER_BOUND('',#3982,.T.);
#2558=FACE_OUTER_BOUND('',#3983,.T.);
#2559=FACE_OUTER_BOUND('',#3984,.T.);
#2560=FACE_OUTER_BOUND('',#3985,.T.);
#2561=FACE_OUTER_BOUND('',#3986,.T.);
#2562=FACE_OUTER_BOUND('',#3987,.T.);
#2563=FACE_OUTER_BOUND('',#3988,.T.);
#2564=FACE_OUTER_BOUND('',#3989,.T.);
#2565=FACE_OUTER_BOUND('',#3990,.T.);
#2566=FACE_OUTER_BOUND('',#3991,.T.);
#2567=FACE_OUTER_BOUND('',#3992,.T.);
#2568=FACE_OUTER_BOUND('',#3993,.T.);
#2569=FACE_OUTER_BOUND('',#3994,.T.);
#2570=FACE_OUTER_BOUND('',#3995,.T.);
#2571=FACE_OUTER_BOUND('',#3996,.T.);
#2572=FACE_OUTER_BOUND('',#3997,.T.);
#2573=FACE_OUTER_BOUND('',#3998,.T.);
#2574=FACE_OUTER_BOUND('',#3999,.T.);
#2575=FACE_OUTER_BOUND('',#4000,.T.);
#2576=FACE_OUTER_BOUND('',#4001,.T.);
#2577=FACE_OUTER_BOUND('',#4002,.T.);
#2578=FACE_OUTER_BOUND('',#4003,.T.);
#2579=FACE_OUTER_BOUND('',#4004,.T.);
#2580=FACE_OUTER_BOUND('',#4005,.T.);
#2581=FACE_OUTER_BOUND('',#4006,.T.);
#2582=FACE_OUTER_BOUND('',#4007,.T.);
#2583=FACE_OUTER_BOUND('',#4008,.T.);
#2584=FACE_OUTER_BOUND('',#4009,.T.);
#2585=FACE_OUTER_BOUND('',#4010,.T.);
#2586=FACE_OUTER_BOUND('',#4011,.T.);
#2587=FACE_OUTER_BOUND('',#4012,.T.);
#2588=FACE_OUTER_BOUND('',#4013,.T.);
#2589=FACE_OUTER_BOUND('',#4014,.T.);
#2590=FACE_OUTER_BOUND('',#4015,.T.);
#2591=FACE_OUTER_BOUND('',#4016,.T.);
#2592=FACE_OUTER_BOUND('',#4017,.T.);
#2593=FACE_OUTER_BOUND('',#4018,.T.);
#2594=FACE_OUTER_BOUND('',#4019,.T.);
#2595=FACE_OUTER_BOUND('',#4020,.T.);
#2596=FACE_OUTER_BOUND('',#4021,.T.);
#2597=FACE_OUTER_BOUND('',#4022,.T.);
#2598=FACE_OUTER_BOUND('',#4023,.T.);
#2599=FACE_OUTER_BOUND('',#4024,.T.);
#2600=FACE_OUTER_BOUND('',#4025,.T.);
#2601=FACE_OUTER_BOUND('',#4026,.T.);
#2602=FACE_OUTER_BOUND('',#4027,.T.);
#2603=FACE_OUTER_BOUND('',#4028,.T.);
#2604=FACE_OUTER_BOUND('',#4029,.T.);
#2605=FACE_OUTER_BOUND('',#4030,.T.);
#2606=FACE_OUTER_BOUND('',#4031,.T.);
#2607=FACE_OUTER_BOUND('',#4032,.T.);
#2608=FACE_OUTER_BOUND('',#4033,.T.);
#2609=FACE_OUTER_BOUND('',#4034,.T.);
#2610=FACE_OUTER_BOUND('',#4035,.T.);
#2611=FACE_OUTER_BOUND('',#4036,.T.);
#2612=FACE_OUTER_BOUND('',#4037,.T.);
#2613=FACE_OUTER_BOUND('',#4038,.T.);
#2614=FACE_OUTER_BOUND('',#4039,.T.);
#2615=FACE_OUTER_BOUND('',#4040,.T.);
#2616=FACE_OUTER_BOUND('',#4041,.T.);
#2617=FACE_OUTER_BOUND('',#4042,.T.);
#2618=FACE_OUTER_BOUND('',#4043,.T.);
#2619=FACE_OUTER_BOUND('',#4044,.T.);
#2620=FACE_OUTER_BOUND('',#4045,.T.);
#2621=FACE_OUTER_BOUND('',#4046,.T.);
#2622=FACE_OUTER_BOUND('',#4047,.T.);
#2623=FACE_OUTER_BOUND('',#4048,.T.);
#2624=FACE_OUTER_BOUND('',#4049,.T.);
#2625=FACE_OUTER_BOUND('',#4050,.T.);
#2626=FACE_OUTER_BOUND('',#4051,.T.);
#2627=FACE_OUTER_BOUND('',#4052,.T.);
#2628=FACE_OUTER_BOUND('',#4053,.T.);
#2629=FACE_OUTER_BOUND('',#4054,.T.);
#2630=FACE_OUTER_BOUND('',#4055,.T.);
#2631=FACE_OUTER_BOUND('',#4056,.T.);
#2632=FACE_OUTER_BOUND('',#4057,.T.);
#2633=FACE_OUTER_BOUND('',#4058,.T.);
#2634=FACE_OUTER_BOUND('',#4059,.T.);
#2635=FACE_OUTER_BOUND('',#4060,.T.);
#2636=FACE_OUTER_BOUND('',#4061,.T.);
#2637=FACE_OUTER_BOUND('',#4062,.T.);
#2638=FACE_OUTER_BOUND('',#4063,.T.);
#2639=FACE_OUTER_BOUND('',#4064,.T.);
#2640=FACE_OUTER_BOUND('',#4065,.T.);
#2641=FACE_OUTER_BOUND('',#4066,.T.);
#2642=FACE_OUTER_BOUND('',#4067,.T.);
#2643=FACE_OUTER_BOUND('',#4068,.T.);
#2644=FACE_OUTER_BOUND('',#4069,.T.);
#2645=FACE_OUTER_BOUND('',#4070,.T.);
#2646=FACE_OUTER_BOUND('',#4071,.T.);
#2647=FACE_OUTER_BOUND('',#4072,.T.);
#2648=FACE_OUTER_BOUND('',#4073,.T.);
#2649=FACE_OUTER_BOUND('',#4074,.T.);
#2650=FACE_OUTER_BOUND('',#4075,.T.);
#2651=FACE_OUTER_BOUND('',#4076,.T.);
#2652=FACE_OUTER_BOUND('',#4077,.T.);
#2653=FACE_OUTER_BOUND('',#4078,.T.);
#2654=FACE_OUTER_BOUND('',#4079,.T.);
#2655=FACE_OUTER_BOUND('',#4080,.T.);
#2656=FACE_OUTER_BOUND('',#4081,.T.);
#2657=FACE_OUTER_BOUND('',#4082,.T.);
#2658=FACE_OUTER_BOUND('',#4083,.T.);
#2659=FACE_OUTER_BOUND('',#4084,.T.);
#2660=FACE_OUTER_BOUND('',#4085,.T.);
#2661=FACE_OUTER_BOUND('',#4086,.T.);
#2662=FACE_OUTER_BOUND('',#4087,.T.);
#2663=FACE_OUTER_BOUND('',#4088,.T.);
#2664=FACE_OUTER_BOUND('',#4089,.T.);
#2665=FACE_OUTER_BOUND('',#4090,.T.);
#2666=FACE_OUTER_BOUND('',#4091,.T.);
#2667=FACE_OUTER_BOUND('',#4092,.T.);
#2668=FACE_OUTER_BOUND('',#4093,.T.);
#2669=FACE_OUTER_BOUND('',#4094,.T.);
#2670=FACE_OUTER_BOUND('',#4095,.T.);
#2671=FACE_OUTER_BOUND('',#4096,.T.);
#2672=FACE_OUTER_BOUND('',#4097,.T.);
#2673=FACE_OUTER_BOUND('',#4098,.T.);
#2674=FACE_OUTER_BOUND('',#4100,.T.);
#2675=FACE_OUTER_BOUND('',#4101,.T.);
#2676=FACE_OUTER_BOUND('',#4102,.T.);
#2677=FACE_OUTER_BOUND('',#4103,.T.);
#2678=FACE_OUTER_BOUND('',#4104,.T.);
#2679=FACE_OUTER_BOUND('',#4105,.T.);
#2680=FACE_OUTER_BOUND('',#4106,.T.);
#2681=FACE_OUTER_BOUND('',#4107,.T.);
#2682=FACE_OUTER_BOUND('',#4108,.T.);
#2683=FACE_OUTER_BOUND('',#4109,.T.);
#2684=FACE_OUTER_BOUND('',#4110,.T.);
#2685=FACE_OUTER_BOUND('',#4111,.T.);
#2686=FACE_OUTER_BOUND('',#4112,.T.);
#2687=FACE_OUTER_BOUND('',#4113,.T.);
#2688=FACE_OUTER_BOUND('',#4114,.T.);
#2689=FACE_OUTER_BOUND('',#4115,.T.);
#2690=FACE_OUTER_BOUND('',#4116,.T.);
#2691=FACE_OUTER_BOUND('',#4117,.T.);
#2692=FACE_OUTER_BOUND('',#4118,.T.);
#2693=FACE_OUTER_BOUND('',#4119,.T.);
#2694=FACE_OUTER_BOUND('',#4120,.T.);
#2695=FACE_OUTER_BOUND('',#4121,.T.);
#2696=FACE_OUTER_BOUND('',#4122,.T.);
#2697=FACE_OUTER_BOUND('',#4123,.T.);
#2698=FACE_OUTER_BOUND('',#4124,.T.);
#2699=FACE_OUTER_BOUND('',#4125,.T.);
#2700=FACE_OUTER_BOUND('',#4126,.T.);
#2701=FACE_OUTER_BOUND('',#4127,.T.);
#2702=FACE_OUTER_BOUND('',#4128,.T.);
#2703=FACE_OUTER_BOUND('',#4129,.T.);
#2704=FACE_OUTER_BOUND('',#4130,.T.);
#2705=FACE_OUTER_BOUND('',#4131,.T.);
#2706=FACE_OUTER_BOUND('',#4132,.T.);
#2707=FACE_OUTER_BOUND('',#4133,.T.);
#2708=FACE_OUTER_BOUND('',#4134,.T.);
#2709=FACE_OUTER_BOUND('',#4135,.T.);
#2710=FACE_OUTER_BOUND('',#4136,.T.);
#2711=FACE_OUTER_BOUND('',#4137,.T.);
#2712=FACE_OUTER_BOUND('',#4138,.T.);
#2713=FACE_OUTER_BOUND('',#4139,.T.);
#2714=FACE_OUTER_BOUND('',#4140,.T.);
#2715=FACE_OUTER_BOUND('',#4141,.T.);
#2716=FACE_OUTER_BOUND('',#4142,.T.);
#2717=FACE_OUTER_BOUND('',#4143,.T.);
#2718=FACE_OUTER_BOUND('',#4144,.T.);
#2719=FACE_OUTER_BOUND('',#4145,.T.);
#2720=FACE_OUTER_BOUND('',#4146,.T.);
#2721=FACE_OUTER_BOUND('',#4147,.T.);
#2722=FACE_OUTER_BOUND('',#4148,.T.);
#2723=FACE_OUTER_BOUND('',#4149,.T.);
#2724=FACE_OUTER_BOUND('',#4150,.T.);
#2725=FACE_OUTER_BOUND('',#4151,.T.);
#2726=FACE_OUTER_BOUND('',#4152,.T.);
#2727=FACE_OUTER_BOUND('',#4153,.T.);
#2728=FACE_OUTER_BOUND('',#4154,.T.);
#2729=FACE_OUTER_BOUND('',#4155,.T.);
#2730=FACE_OUTER_BOUND('',#4156,.T.);
#2731=FACE_OUTER_BOUND('',#4157,.T.);
#2732=FACE_OUTER_BOUND('',#4158,.T.);
#2733=FACE_OUTER_BOUND('',#4159,.T.);
#2734=FACE_OUTER_BOUND('',#4160,.T.);
#2735=FACE_OUTER_BOUND('',#4161,.T.);
#2736=FACE_OUTER_BOUND('',#4162,.T.);
#2737=FACE_OUTER_BOUND('',#4163,.T.);
#2738=FACE_OUTER_BOUND('',#4164,.T.);
#2739=FACE_OUTER_BOUND('',#4165,.T.);
#2740=FACE_OUTER_BOUND('',#4166,.T.);
#2741=FACE_OUTER_BOUND('',#4167,.T.);
#2742=FACE_OUTER_BOUND('',#4168,.T.);
#2743=FACE_OUTER_BOUND('',#4169,.T.);
#2744=FACE_OUTER_BOUND('',#4170,.T.);
#2745=FACE_OUTER_BOUND('',#4171,.T.);
#2746=FACE_OUTER_BOUND('',#4172,.T.);
#2747=FACE_OUTER_BOUND('',#4173,.T.);
#2748=FACE_OUTER_BOUND('',#4174,.T.);
#2749=FACE_OUTER_BOUND('',#4175,.T.);
#2750=FACE_OUTER_BOUND('',#4176,.T.);
#2751=FACE_OUTER_BOUND('',#4177,.T.);
#2752=FACE_OUTER_BOUND('',#4178,.T.);
#2753=FACE_OUTER_BOUND('',#4179,.T.);
#2754=FACE_OUTER_BOUND('',#4180,.T.);
#2755=FACE_OUTER_BOUND('',#4181,.T.);
#2756=FACE_OUTER_BOUND('',#4182,.T.);
#2757=FACE_OUTER_BOUND('',#4183,.T.);
#2758=FACE_OUTER_BOUND('',#4184,.T.);
#2759=FACE_OUTER_BOUND('',#4185,.T.);
#2760=FACE_OUTER_BOUND('',#4186,.T.);
#2761=FACE_OUTER_BOUND('',#4187,.T.);
#2762=FACE_OUTER_BOUND('',#4188,.T.);
#2763=FACE_OUTER_BOUND('',#4189,.T.);
#2764=FACE_OUTER_BOUND('',#4190,.T.);
#2765=FACE_OUTER_BOUND('',#4191,.T.);
#2766=FACE_OUTER_BOUND('',#4192,.T.);
#2767=FACE_OUTER_BOUND('',#4193,.T.);
#2768=FACE_OUTER_BOUND('',#4194,.T.);
#2769=FACE_OUTER_BOUND('',#4195,.T.);
#2770=FACE_OUTER_BOUND('',#4196,.T.);
#2771=FACE_OUTER_BOUND('',#4197,.T.);
#2772=FACE_OUTER_BOUND('',#4198,.T.);
#2773=FACE_OUTER_BOUND('',#4199,.T.);
#2774=FACE_OUTER_BOUND('',#4200,.T.);
#2775=FACE_OUTER_BOUND('',#4201,.T.);
#2776=FACE_OUTER_BOUND('',#4202,.T.);
#2777=FACE_OUTER_BOUND('',#4203,.T.);
#2778=FACE_OUTER_BOUND('',#4204,.T.);
#2779=FACE_OUTER_BOUND('',#4205,.T.);
#2780=FACE_OUTER_BOUND('',#4206,.T.);
#2781=FACE_OUTER_BOUND('',#4207,.T.);
#2782=FACE_OUTER_BOUND('',#4208,.T.);
#2783=FACE_OUTER_BOUND('',#4209,.T.);
#2784=FACE_OUTER_BOUND('',#4210,.T.);
#2785=FACE_OUTER_BOUND('',#4211,.T.);
#2786=FACE_OUTER_BOUND('',#4212,.T.);
#2787=FACE_OUTER_BOUND('',#4213,.T.);
#2788=FACE_OUTER_BOUND('',#4214,.T.);
#2789=FACE_OUTER_BOUND('',#4215,.T.);
#2790=FACE_OUTER_BOUND('',#4216,.T.);
#2791=FACE_OUTER_BOUND('',#4217,.T.);
#2792=FACE_OUTER_BOUND('',#4218,.T.);
#2793=FACE_OUTER_BOUND('',#4219,.T.);
#2794=FACE_OUTER_BOUND('',#4220,.T.);
#2795=FACE_OUTER_BOUND('',#4221,.T.);
#2796=FACE_OUTER_BOUND('',#4222,.T.);
#2797=FACE_OUTER_BOUND('',#4223,.T.);
#2798=FACE_OUTER_BOUND('',#4224,.T.);
#2799=FACE_OUTER_BOUND('',#4225,.T.);
#2800=FACE_OUTER_BOUND('',#4226,.T.);
#2801=FACE_OUTER_BOUND('',#4227,.T.);
#2802=FACE_OUTER_BOUND('',#4228,.T.);
#2803=FACE_OUTER_BOUND('',#4229,.T.);
#2804=FACE_OUTER_BOUND('',#4230,.T.);
#2805=FACE_OUTER_BOUND('',#4231,.T.);
#2806=FACE_OUTER_BOUND('',#4232,.T.);
#2807=FACE_OUTER_BOUND('',#4233,.T.);
#2808=FACE_OUTER_BOUND('',#4234,.T.);
#2809=FACE_OUTER_BOUND('',#4235,.T.);
#2810=FACE_OUTER_BOUND('',#4236,.T.);
#2811=FACE_OUTER_BOUND('',#4237,.T.);
#2812=FACE_OUTER_BOUND('',#4238,.T.);
#2813=FACE_OUTER_BOUND('',#4239,.T.);
#2814=FACE_OUTER_BOUND('',#4240,.T.);
#2815=FACE_OUTER_BOUND('',#4241,.T.);
#2816=FACE_OUTER_BOUND('',#4242,.T.);
#2817=FACE_OUTER_BOUND('',#4243,.T.);
#2818=FACE_OUTER_BOUND('',#4244,.T.);
#2819=FACE_OUTER_BOUND('',#4245,.T.);
#2820=FACE_OUTER_BOUND('',#4246,.T.);
#2821=FACE_OUTER_BOUND('',#4247,.T.);
#2822=FACE_OUTER_BOUND('',#4248,.T.);
#2823=FACE_OUTER_BOUND('',#4249,.T.);
#2824=FACE_OUTER_BOUND('',#4250,.T.);
#2825=FACE_OUTER_BOUND('',#4251,.T.);
#2826=FACE_OUTER_BOUND('',#4252,.T.);
#2827=FACE_OUTER_BOUND('',#4253,.T.);
#2828=FACE_OUTER_BOUND('',#4254,.T.);
#2829=FACE_OUTER_BOUND('',#4255,.T.);
#2830=FACE_OUTER_BOUND('',#4256,.T.);
#2831=FACE_OUTER_BOUND('',#4257,.T.);
#2832=FACE_OUTER_BOUND('',#4258,.T.);
#2833=FACE_OUTER_BOUND('',#4259,.T.);
#2834=FACE_OUTER_BOUND('',#4260,.T.);
#2835=FACE_OUTER_BOUND('',#4261,.T.);
#2836=FACE_OUTER_BOUND('',#4262,.T.);
#2837=FACE_OUTER_BOUND('',#4263,.T.);
#2838=FACE_OUTER_BOUND('',#4264,.T.);
#2839=FACE_OUTER_BOUND('',#4265,.T.);
#2840=FACE_OUTER_BOUND('',#4266,.T.);
#2841=FACE_OUTER_BOUND('',#4267,.T.);
#2842=FACE_OUTER_BOUND('',#4268,.T.);
#2843=FACE_OUTER_BOUND('',#4269,.T.);
#2844=FACE_OUTER_BOUND('',#4270,.T.);
#2845=FACE_OUTER_BOUND('',#4271,.T.);
#2846=FACE_OUTER_BOUND('',#4272,.T.);
#2847=FACE_OUTER_BOUND('',#4273,.T.);
#2848=FACE_OUTER_BOUND('',#4274,.T.);
#2849=FACE_OUTER_BOUND('',#4275,.T.);
#2850=FACE_OUTER_BOUND('',#4276,.T.);
#2851=FACE_OUTER_BOUND('',#4277,.T.);
#2852=FACE_OUTER_BOUND('',#4278,.T.);
#2853=FACE_OUTER_BOUND('',#4279,.T.);
#2854=FACE_OUTER_BOUND('',#4280,.T.);
#2855=FACE_OUTER_BOUND('',#4281,.T.);
#2856=FACE_OUTER_BOUND('',#4282,.T.);
#2857=FACE_OUTER_BOUND('',#4283,.T.);
#2858=FACE_OUTER_BOUND('',#4284,.T.);
#2859=FACE_OUTER_BOUND('',#4285,.T.);
#2860=FACE_OUTER_BOUND('',#4286,.T.);
#2861=FACE_OUTER_BOUND('',#4287,.T.);
#2862=FACE_OUTER_BOUND('',#4288,.T.);
#2863=FACE_OUTER_BOUND('',#4289,.T.);
#2864=FACE_OUTER_BOUND('',#4290,.T.);
#2865=FACE_OUTER_BOUND('',#4291,.T.);
#2866=FACE_OUTER_BOUND('',#4292,.T.);
#2867=FACE_OUTER_BOUND('',#4294,.T.);
#2868=FACE_OUTER_BOUND('',#4296,.T.);
#2869=FACE_OUTER_BOUND('',#4297,.T.);
#2870=FACE_OUTER_BOUND('',#4298,.T.);
#2871=FACE_OUTER_BOUND('',#4299,.T.);
#2872=FACE_OUTER_BOUND('',#4300,.T.);
#2873=FACE_OUTER_BOUND('',#4301,.T.);
#2874=FACE_OUTER_BOUND('',#4302,.T.);
#2875=FACE_OUTER_BOUND('',#4303,.T.);
#2876=FACE_OUTER_BOUND('',#4304,.T.);
#2877=FACE_OUTER_BOUND('',#4305,.T.);
#2878=FACE_OUTER_BOUND('',#4306,.T.);
#2879=FACE_OUTER_BOUND('',#4307,.T.);
#2880=FACE_OUTER_BOUND('',#4308,.T.);
#2881=FACE_OUTER_BOUND('',#4309,.T.);
#2882=FACE_OUTER_BOUND('',#4310,.T.);
#2883=FACE_OUTER_BOUND('',#4311,.T.);
#2884=FACE_OUTER_BOUND('',#4312,.T.);
#2885=FACE_OUTER_BOUND('',#4313,.T.);
#2886=FACE_OUTER_BOUND('',#4314,.T.);
#2887=FACE_OUTER_BOUND('',#4315,.T.);
#2888=FACE_OUTER_BOUND('',#4316,.T.);
#2889=FACE_OUTER_BOUND('',#4317,.T.);
#2890=FACE_OUTER_BOUND('',#4318,.T.);
#2891=FACE_OUTER_BOUND('',#4319,.T.);
#2892=FACE_OUTER_BOUND('',#4320,.T.);
#2893=FACE_OUTER_BOUND('',#4321,.T.);
#2894=FACE_OUTER_BOUND('',#4322,.T.);
#2895=FACE_OUTER_BOUND('',#4323,.T.);
#2896=FACE_OUTER_BOUND('',#4324,.T.);
#2897=FACE_OUTER_BOUND('',#4325,.T.);
#2898=FACE_OUTER_BOUND('',#4326,.T.);
#2899=FACE_OUTER_BOUND('',#4327,.T.);
#2900=FACE_OUTER_BOUND('',#4328,.T.);
#2901=FACE_OUTER_BOUND('',#4329,.T.);
#2902=FACE_OUTER_BOUND('',#4330,.T.);
#2903=FACE_OUTER_BOUND('',#4332,.T.);
#2904=FACE_OUTER_BOUND('',#4334,.T.);
#2905=FACE_OUTER_BOUND('',#4335,.T.);
#2906=FACE_OUTER_BOUND('',#4336,.T.);
#2907=FACE_OUTER_BOUND('',#4337,.T.);
#2908=FACE_OUTER_BOUND('',#4338,.T.);
#2909=FACE_OUTER_BOUND('',#4339,.T.);
#2910=FACE_OUTER_BOUND('',#4340,.T.);
#2911=FACE_OUTER_BOUND('',#4342,.T.);
#2912=FACE_OUTER_BOUND('',#4344,.T.);
#2913=FACE_OUTER_BOUND('',#4345,.T.);
#2914=FACE_OUTER_BOUND('',#4346,.T.);
#2915=FACE_OUTER_BOUND('',#4348,.T.);
#2916=FACE_OUTER_BOUND('',#4350,.T.);
#2917=FACE_OUTER_BOUND('',#4351,.T.);
#2918=FACE_OUTER_BOUND('',#4352,.T.);
#2919=FACE_OUTER_BOUND('',#4353,.T.);
#2920=FACE_OUTER_BOUND('',#4354,.T.);
#2921=FACE_OUTER_BOUND('',#4356,.T.);
#2922=FACE_OUTER_BOUND('',#4358,.T.);
#2923=FACE_OUTER_BOUND('',#4359,.T.);
#2924=FACE_OUTER_BOUND('',#4360,.T.);
#2925=FACE_OUTER_BOUND('',#4362,.T.);
#2926=FACE_OUTER_BOUND('',#4363,.T.);
#2927=FACE_OUTER_BOUND('',#4365,.T.);
#2928=FACE_OUTER_BOUND('',#4367,.T.);
#2929=FACE_OUTER_BOUND('',#4368,.T.);
#2930=FACE_OUTER_BOUND('',#4369,.T.);
#2931=FACE_OUTER_BOUND('',#4370,.T.);
#2932=FACE_OUTER_BOUND('',#4371,.T.);
#2933=FACE_OUTER_BOUND('',#4373,.T.);
#2934=FACE_OUTER_BOUND('',#4374,.T.);
#2935=FACE_OUTER_BOUND('',#4375,.T.);
#2936=FACE_OUTER_BOUND('',#4380,.T.);
#2937=FACE_OUTER_BOUND('',#4385,.T.);
#2938=FACE_OUTER_BOUND('',#4386,.T.);
#2939=FACE_OUTER_BOUND('',#4387,.T.);
#2940=FACE_OUTER_BOUND('',#4388,.T.);
#2941=FACE_OUTER_BOUND('',#4389,.T.);
#2942=FACE_OUTER_BOUND('',#4390,.T.);
#2943=FACE_OUTER_BOUND('',#4391,.T.);
#2944=FACE_OUTER_BOUND('',#4392,.T.);
#2945=FACE_OUTER_BOUND('',#4393,.T.);
#2946=FACE_OUTER_BOUND('',#4395,.T.);
#2947=FACE_OUTER_BOUND('',#4397,.T.);
#2948=FACE_OUTER_BOUND('',#4398,.T.);
#2949=FACE_OUTER_BOUND('',#4400,.T.);
#2950=FACE_OUTER_BOUND('',#4402,.T.);
#2951=FACE_OUTER_BOUND('',#4403,.T.);
#2952=FACE_OUTER_BOUND('',#4405,.T.);
#2953=FACE_OUTER_BOUND('',#4406,.T.);
#2954=FACE_OUTER_BOUND('',#4407,.T.);
#2955=FACE_OUTER_BOUND('',#4408,.T.);
#2956=FACE_OUTER_BOUND('',#4409,.T.);
#2957=FACE_OUTER_BOUND('',#4410,.T.);
#2958=FACE_OUTER_BOUND('',#4411,.T.);
#2959=FACE_OUTER_BOUND('',#4412,.T.);
#2960=FACE_OUTER_BOUND('',#4413,.T.);
#2961=FACE_OUTER_BOUND('',#4414,.T.);
#2962=FACE_OUTER_BOUND('',#4415,.T.);
#2963=FACE_OUTER_BOUND('',#4416,.T.);
#2964=FACE_OUTER_BOUND('',#4417,.T.);
#2965=FACE_OUTER_BOUND('',#4419,.T.);
#2966=FACE_OUTER_BOUND('',#4421,.T.);
#2967=FACE_OUTER_BOUND('',#4422,.T.);
#2968=FACE_OUTER_BOUND('',#4423,.T.);
#2969=FACE_OUTER_BOUND('',#4425,.T.);
#2970=FACE_OUTER_BOUND('',#4427,.T.);
#2971=FACE_OUTER_BOUND('',#4428,.T.);
#2972=FACE_OUTER_BOUND('',#4429,.T.);
#2973=FACE_OUTER_BOUND('',#4431,.T.);
#2974=FACE_OUTER_BOUND('',#4433,.T.);
#2975=FACE_OUTER_BOUND('',#4434,.T.);
#2976=FACE_OUTER_BOUND('',#4435,.T.);
#2977=FACE_OUTER_BOUND('',#4436,.T.);
#2978=FACE_OUTER_BOUND('',#4437,.T.);
#2979=FACE_OUTER_BOUND('',#4438,.T.);
#2980=FACE_OUTER_BOUND('',#4439,.T.);
#2981=FACE_OUTER_BOUND('',#4440,.T.);
#2982=FACE_OUTER_BOUND('',#4441,.T.);
#2983=FACE_OUTER_BOUND('',#4442,.T.);
#2984=FACE_OUTER_BOUND('',#4443,.T.);
#2985=FACE_OUTER_BOUND('',#4444,.T.);
#2986=FACE_OUTER_BOUND('',#4445,.T.);
#2987=FACE_OUTER_BOUND('',#4446,.T.);
#2988=FACE_OUTER_BOUND('',#4447,.T.);
#2989=FACE_OUTER_BOUND('',#4448,.T.);
#2990=FACE_OUTER_BOUND('',#4449,.T.);
#2991=FACE_OUTER_BOUND('',#4450,.T.);
#2992=FACE_OUTER_BOUND('',#4451,.T.);
#2993=FACE_OUTER_BOUND('',#4452,.T.);
#2994=FACE_OUTER_BOUND('',#4453,.T.);
#2995=FACE_OUTER_BOUND('',#4454,.T.);
#2996=FACE_OUTER_BOUND('',#4455,.T.);
#2997=FACE_OUTER_BOUND('',#4456,.T.);
#2998=FACE_OUTER_BOUND('',#4457,.T.);
#2999=FACE_OUTER_BOUND('',#4458,.T.);
#3000=FACE_OUTER_BOUND('',#4459,.T.);
#3001=FACE_OUTER_BOUND('',#4460,.T.);
#3002=FACE_OUTER_BOUND('',#4461,.T.);
#3003=FACE_OUTER_BOUND('',#4462,.T.);
#3004=FACE_OUTER_BOUND('',#4463,.T.);
#3005=FACE_OUTER_BOUND('',#4464,.T.);
#3006=FACE_OUTER_BOUND('',#4465,.T.);
#3007=FACE_OUTER_BOUND('',#4466,.T.);
#3008=FACE_OUTER_BOUND('',#4467,.T.);
#3009=FACE_OUTER_BOUND('',#4468,.T.);
#3010=FACE_OUTER_BOUND('',#4469,.T.);
#3011=FACE_OUTER_BOUND('',#4470,.T.);
#3012=FACE_OUTER_BOUND('',#4471,.T.);
#3013=FACE_OUTER_BOUND('',#4472,.T.);
#3014=FACE_OUTER_BOUND('',#4473,.T.);
#3015=FACE_OUTER_BOUND('',#4474,.T.);
#3016=FACE_OUTER_BOUND('',#4475,.T.);
#3017=FACE_OUTER_BOUND('',#4476,.T.);
#3018=FACE_OUTER_BOUND('',#4477,.T.);
#3019=FACE_OUTER_BOUND('',#4478,.T.);
#3020=FACE_OUTER_BOUND('',#4479,.T.);
#3021=FACE_OUTER_BOUND('',#4480,.T.);
#3022=FACE_OUTER_BOUND('',#4481,.T.);
#3023=FACE_OUTER_BOUND('',#4482,.T.);
#3024=FACE_OUTER_BOUND('',#4483,.T.);
#3025=FACE_OUTER_BOUND('',#4484,.T.);
#3026=FACE_OUTER_BOUND('',#4485,.T.);
#3027=FACE_OUTER_BOUND('',#4486,.T.);
#3028=FACE_OUTER_BOUND('',#4487,.T.);
#3029=FACE_OUTER_BOUND('',#4488,.T.);
#3030=FACE_OUTER_BOUND('',#4489,.T.);
#3031=FACE_OUTER_BOUND('',#4490,.T.);
#3032=FACE_OUTER_BOUND('',#4491,.T.);
#3033=FACE_OUTER_BOUND('',#4492,.T.);
#3034=FACE_OUTER_BOUND('',#4493,.T.);
#3035=FACE_OUTER_BOUND('',#4494,.T.);
#3036=FACE_OUTER_BOUND('',#4495,.T.);
#3037=FACE_OUTER_BOUND('',#4496,.T.);
#3038=FACE_OUTER_BOUND('',#4497,.T.);
#3039=FACE_OUTER_BOUND('',#4498,.T.);
#3040=FACE_OUTER_BOUND('',#4499,.T.);
#3041=FACE_OUTER_BOUND('',#4501,.T.);
#3042=FACE_OUTER_BOUND('',#4502,.T.);
#3043=FACE_OUTER_BOUND('',#4504,.T.);
#3044=EDGE_LOOP('',(#15424,#15425,#15426,#15427,#15428,#15429,#15430,#15431));
#3045=EDGE_LOOP('',(#15432,#15433,#15434,#15435));
#3046=EDGE_LOOP('',(#15436,#15437,#15438,#15439));
#3047=EDGE_LOOP('',(#15440,#15441,#15442,#15443));
#3048=EDGE_LOOP('',(#15444,#15445,#15446,#15447));
#3049=EDGE_LOOP('',(#15448,#15449,#15450,#15451));
#3050=EDGE_LOOP('',(#15452,#15453,#15454,#15455));
#3051=EDGE_LOOP('',(#15456,#15457,#15458,#15459));
#3052=EDGE_LOOP('',(#15460,#15461,#15462,#15463));
#3053=EDGE_LOOP('',(#15464,#15465,#15466,#15467));
#3054=EDGE_LOOP('',(#15468,#15469,#15470,#15471));
#3055=EDGE_LOOP('',(#15472,#15473,#15474,#15475));
#3056=EDGE_LOOP('',(#15476,#15477,#15478,#15479));
#3057=EDGE_LOOP('',(#15480,#15481,#15482,#15483));
#3058=EDGE_LOOP('',(#15484,#15485,#15486,#15487));
#3059=EDGE_LOOP('',(#15488,#15489,#15490,#15491));
#3060=EDGE_LOOP('',(#15492,#15493,#15494,#15495));
#3061=EDGE_LOOP('',(#15496,#15497,#15498,#15499));
#3062=EDGE_LOOP('',(#15500,#15501,#15502,#15503));
#3063=EDGE_LOOP('',(#15504,#15505,#15506,#15507));
#3064=EDGE_LOOP('',(#15508,#15509,#15510,#15511));
#3065=EDGE_LOOP('',(#15512,#15513,#15514,#15515));
#3066=EDGE_LOOP('',(#15516,#15517,#15518,#15519));
#3067=EDGE_LOOP('',(#15520,#15521,#15522,#15523));
#3068=EDGE_LOOP('',(#15524,#15525,#15526,#15527));
#3069=EDGE_LOOP('',(#15528,#15529,#15530,#15531));
#3070=EDGE_LOOP('',(#15532,#15533,#15534,#15535));
#3071=EDGE_LOOP('',(#15536,#15537,#15538,#15539));
#3072=EDGE_LOOP('',(#15540,#15541,#15542,#15543));
#3073=EDGE_LOOP('',(#15544,#15545,#15546,#15547));
#3074=EDGE_LOOP('',(#15548,#15549,#15550,#15551,#15552,#15553,#15554,#15555));
#3075=EDGE_LOOP('',(#15556,#15557,#15558,#15559));
#3076=EDGE_LOOP('',(#15560,#15561,#15562,#15563));
#3077=EDGE_LOOP('',(#15564,#15565,#15566,#15567));
#3078=EDGE_LOOP('',(#15568,#15569,#15570,#15571));
#3079=EDGE_LOOP('',(#15572,#15573,#15574,#15575));
#3080=EDGE_LOOP('',(#15576,#15577,#15578,#15579));
#3081=EDGE_LOOP('',(#15580,#15581,#15582,#15583));
#3082=EDGE_LOOP('',(#15584,#15585,#15586,#15587));
#3083=EDGE_LOOP('',(#15588,#15589,#15590,#15591));
#3084=EDGE_LOOP('',(#15592,#15593,#15594,#15595));
#3085=EDGE_LOOP('',(#15596,#15597,#15598,#15599));
#3086=EDGE_LOOP('',(#15600,#15601,#15602,#15603));
#3087=EDGE_LOOP('',(#15604,#15605,#15606,#15607));
#3088=EDGE_LOOP('',(#15608,#15609,#15610,#15611));
#3089=EDGE_LOOP('',(#15612,#15613,#15614,#15615));
#3090=EDGE_LOOP('',(#15616,#15617,#15618,#15619));
#3091=EDGE_LOOP('',(#15620,#15621,#15622,#15623));
#3092=EDGE_LOOP('',(#15624,#15625,#15626,#15627));
#3093=EDGE_LOOP('',(#15628,#15629,#15630,#15631));
#3094=EDGE_LOOP('',(#15632,#15633,#15634,#15635));
#3095=EDGE_LOOP('',(#15636,#15637,#15638,#15639));
#3096=EDGE_LOOP('',(#15640,#15641,#15642,#15643));
#3097=EDGE_LOOP('',(#15644,#15645,#15646,#15647));
#3098=EDGE_LOOP('',(#15648,#15649,#15650,#15651));
#3099=EDGE_LOOP('',(#15652,#15653,#15654,#15655));
#3100=EDGE_LOOP('',(#15656,#15657,#15658,#15659));
#3101=EDGE_LOOP('',(#15660,#15661,#15662,#15663));
#3102=EDGE_LOOP('',(#15664,#15665,#15666,#15667));
#3103=EDGE_LOOP('',(#15668,#15669,#15670,#15671));
#3104=EDGE_LOOP('',(#15672,#15673,#15674,#15675,#15676,#15677,#15678,#15679));
#3105=EDGE_LOOP('',(#15680,#15681,#15682,#15683));
#3106=EDGE_LOOP('',(#15684,#15685,#15686,#15687));
#3107=EDGE_LOOP('',(#15688,#15689,#15690,#15691));
#3108=EDGE_LOOP('',(#15692,#15693,#15694,#15695));
#3109=EDGE_LOOP('',(#15696,#15697,#15698,#15699));
#3110=EDGE_LOOP('',(#15700,#15701,#15702,#15703));
#3111=EDGE_LOOP('',(#15704,#15705,#15706,#15707));
#3112=EDGE_LOOP('',(#15708,#15709,#15710,#15711));
#3113=EDGE_LOOP('',(#15712,#15713,#15714,#15715));
#3114=EDGE_LOOP('',(#15716,#15717,#15718,#15719));
#3115=EDGE_LOOP('',(#15720,#15721,#15722,#15723));
#3116=EDGE_LOOP('',(#15724,#15725,#15726,#15727));
#3117=EDGE_LOOP('',(#15728,#15729,#15730,#15731));
#3118=EDGE_LOOP('',(#15732,#15733,#15734,#15735));
#3119=EDGE_LOOP('',(#15736,#15737,#15738,#15739));
#3120=EDGE_LOOP('',(#15740,#15741,#15742,#15743));
#3121=EDGE_LOOP('',(#15744,#15745,#15746,#15747));
#3122=EDGE_LOOP('',(#15748,#15749,#15750,#15751));
#3123=EDGE_LOOP('',(#15752,#15753,#15754,#15755));
#3124=EDGE_LOOP('',(#15756,#15757,#15758,#15759));
#3125=EDGE_LOOP('',(#15760,#15761,#15762,#15763));
#3126=EDGE_LOOP('',(#15764,#15765,#15766,#15767));
#3127=EDGE_LOOP('',(#15768,#15769,#15770,#15771));
#3128=EDGE_LOOP('',(#15772,#15773,#15774,#15775));
#3129=EDGE_LOOP('',(#15776,#15777,#15778,#15779));
#3130=EDGE_LOOP('',(#15780,#15781,#15782,#15783));
#3131=EDGE_LOOP('',(#15784,#15785,#15786,#15787));
#3132=EDGE_LOOP('',(#15788,#15789,#15790,#15791));
#3133=EDGE_LOOP('',(#15792,#15793,#15794,#15795));
#3134=EDGE_LOOP('',(#15796,#15797,#15798,#15799,#15800,#15801,#15802,#15803));
#3135=EDGE_LOOP('',(#15804,#15805,#15806,#15807));
#3136=EDGE_LOOP('',(#15808,#15809,#15810,#15811));
#3137=EDGE_LOOP('',(#15812,#15813,#15814,#15815));
#3138=EDGE_LOOP('',(#15816,#15817,#15818,#15819));
#3139=EDGE_LOOP('',(#15820,#15821,#15822,#15823));
#3140=EDGE_LOOP('',(#15824,#15825,#15826,#15827));
#3141=EDGE_LOOP('',(#15828,#15829,#15830,#15831));
#3142=EDGE_LOOP('',(#15832,#15833,#15834,#15835));
#3143=EDGE_LOOP('',(#15836,#15837,#15838,#15839));
#3144=EDGE_LOOP('',(#15840,#15841,#15842,#15843));
#3145=EDGE_LOOP('',(#15844,#15845,#15846,#15847));
#3146=EDGE_LOOP('',(#15848,#15849,#15850,#15851));
#3147=EDGE_LOOP('',(#15852,#15853,#15854,#15855));
#3148=EDGE_LOOP('',(#15856,#15857,#15858,#15859));
#3149=EDGE_LOOP('',(#15860,#15861,#15862,#15863));
#3150=EDGE_LOOP('',(#15864,#15865,#15866,#15867));
#3151=EDGE_LOOP('',(#15868,#15869,#15870,#15871));
#3152=EDGE_LOOP('',(#15872,#15873,#15874,#15875));
#3153=EDGE_LOOP('',(#15876,#15877,#15878,#15879));
#3154=EDGE_LOOP('',(#15880,#15881,#15882,#15883));
#3155=EDGE_LOOP('',(#15884,#15885,#15886,#15887));
#3156=EDGE_LOOP('',(#15888,#15889,#15890,#15891));
#3157=EDGE_LOOP('',(#15892,#15893,#15894,#15895));
#3158=EDGE_LOOP('',(#15896,#15897,#15898,#15899));
#3159=EDGE_LOOP('',(#15900,#15901,#15902,#15903));
#3160=EDGE_LOOP('',(#15904,#15905,#15906,#15907));
#3161=EDGE_LOOP('',(#15908,#15909,#15910,#15911));
#3162=EDGE_LOOP('',(#15912,#15913,#15914,#15915));
#3163=EDGE_LOOP('',(#15916,#15917,#15918,#15919));
#3164=EDGE_LOOP('',(#15920,#15921,#15922,#15923,#15924,#15925,#15926,#15927));
#3165=EDGE_LOOP('',(#15928,#15929,#15930,#15931));
#3166=EDGE_LOOP('',(#15932,#15933,#15934,#15935));
#3167=EDGE_LOOP('',(#15936,#15937,#15938,#15939));
#3168=EDGE_LOOP('',(#15940,#15941,#15942,#15943));
#3169=EDGE_LOOP('',(#15944,#15945,#15946,#15947));
#3170=EDGE_LOOP('',(#15948,#15949,#15950,#15951));
#3171=EDGE_LOOP('',(#15952,#15953,#15954,#15955));
#3172=EDGE_LOOP('',(#15956,#15957,#15958,#15959));
#3173=EDGE_LOOP('',(#15960,#15961,#15962,#15963));
#3174=EDGE_LOOP('',(#15964,#15965,#15966,#15967));
#3175=EDGE_LOOP('',(#15968,#15969,#15970,#15971));
#3176=EDGE_LOOP('',(#15972,#15973,#15974,#15975));
#3177=EDGE_LOOP('',(#15976,#15977,#15978,#15979));
#3178=EDGE_LOOP('',(#15980,#15981,#15982,#15983));
#3179=EDGE_LOOP('',(#15984,#15985,#15986,#15987));
#3180=EDGE_LOOP('',(#15988,#15989,#15990,#15991));
#3181=EDGE_LOOP('',(#15992,#15993,#15994,#15995));
#3182=EDGE_LOOP('',(#15996,#15997,#15998,#15999));
#3183=EDGE_LOOP('',(#16000,#16001,#16002,#16003));
#3184=EDGE_LOOP('',(#16004,#16005,#16006,#16007));
#3185=EDGE_LOOP('',(#16008,#16009,#16010,#16011));
#3186=EDGE_LOOP('',(#16012,#16013,#16014,#16015));
#3187=EDGE_LOOP('',(#16016,#16017,#16018,#16019));
#3188=EDGE_LOOP('',(#16020,#16021,#16022,#16023));
#3189=EDGE_LOOP('',(#16024,#16025,#16026,#16027));
#3190=EDGE_LOOP('',(#16028,#16029,#16030,#16031));
#3191=EDGE_LOOP('',(#16032,#16033,#16034,#16035));
#3192=EDGE_LOOP('',(#16036,#16037,#16038,#16039));
#3193=EDGE_LOOP('',(#16040,#16041,#16042,#16043));
#3194=EDGE_LOOP('',(#16044,#16045,#16046,#16047,#16048,#16049,#16050,#16051));
#3195=EDGE_LOOP('',(#16052,#16053,#16054,#16055));
#3196=EDGE_LOOP('',(#16056,#16057,#16058,#16059));
#3197=EDGE_LOOP('',(#16060,#16061,#16062,#16063));
#3198=EDGE_LOOP('',(#16064,#16065,#16066,#16067));
#3199=EDGE_LOOP('',(#16068,#16069,#16070,#16071));
#3200=EDGE_LOOP('',(#16072,#16073,#16074,#16075));
#3201=EDGE_LOOP('',(#16076,#16077,#16078,#16079));
#3202=EDGE_LOOP('',(#16080,#16081,#16082,#16083));
#3203=EDGE_LOOP('',(#16084,#16085,#16086,#16087));
#3204=EDGE_LOOP('',(#16088,#16089,#16090,#16091));
#3205=EDGE_LOOP('',(#16092,#16093,#16094,#16095));
#3206=EDGE_LOOP('',(#16096,#16097,#16098,#16099));
#3207=EDGE_LOOP('',(#16100,#16101,#16102,#16103));
#3208=EDGE_LOOP('',(#16104,#16105,#16106,#16107));
#3209=EDGE_LOOP('',(#16108,#16109,#16110,#16111));
#3210=EDGE_LOOP('',(#16112,#16113,#16114,#16115));
#3211=EDGE_LOOP('',(#16116,#16117,#16118,#16119));
#3212=EDGE_LOOP('',(#16120,#16121,#16122,#16123));
#3213=EDGE_LOOP('',(#16124,#16125,#16126,#16127));
#3214=EDGE_LOOP('',(#16128,#16129,#16130,#16131));
#3215=EDGE_LOOP('',(#16132,#16133,#16134,#16135));
#3216=EDGE_LOOP('',(#16136,#16137,#16138,#16139));
#3217=EDGE_LOOP('',(#16140,#16141,#16142,#16143));
#3218=EDGE_LOOP('',(#16144,#16145,#16146,#16147));
#3219=EDGE_LOOP('',(#16148,#16149,#16150,#16151));
#3220=EDGE_LOOP('',(#16152,#16153,#16154,#16155));
#3221=EDGE_LOOP('',(#16156,#16157,#16158,#16159));
#3222=EDGE_LOOP('',(#16160,#16161,#16162,#16163));
#3223=EDGE_LOOP('',(#16164,#16165,#16166,#16167));
#3224=EDGE_LOOP('',(#16168,#16169,#16170,#16171,#16172,#16173,#16174,#16175));
#3225=EDGE_LOOP('',(#16176,#16177,#16178,#16179));
#3226=EDGE_LOOP('',(#16180,#16181,#16182,#16183));
#3227=EDGE_LOOP('',(#16184,#16185,#16186,#16187));
#3228=EDGE_LOOP('',(#16188,#16189,#16190,#16191));
#3229=EDGE_LOOP('',(#16192,#16193,#16194,#16195));
#3230=EDGE_LOOP('',(#16196,#16197,#16198,#16199));
#3231=EDGE_LOOP('',(#16200,#16201,#16202,#16203));
#3232=EDGE_LOOP('',(#16204,#16205,#16206,#16207));
#3233=EDGE_LOOP('',(#16208,#16209,#16210,#16211));
#3234=EDGE_LOOP('',(#16212,#16213,#16214,#16215));
#3235=EDGE_LOOP('',(#16216,#16217,#16218,#16219));
#3236=EDGE_LOOP('',(#16220,#16221,#16222,#16223));
#3237=EDGE_LOOP('',(#16224,#16225,#16226,#16227));
#3238=EDGE_LOOP('',(#16228,#16229,#16230,#16231));
#3239=EDGE_LOOP('',(#16232,#16233,#16234,#16235));
#3240=EDGE_LOOP('',(#16236,#16237,#16238,#16239));
#3241=EDGE_LOOP('',(#16240,#16241,#16242,#16243));
#3242=EDGE_LOOP('',(#16244,#16245,#16246,#16247));
#3243=EDGE_LOOP('',(#16248,#16249,#16250,#16251));
#3244=EDGE_LOOP('',(#16252,#16253,#16254,#16255));
#3245=EDGE_LOOP('',(#16256,#16257,#16258,#16259));
#3246=EDGE_LOOP('',(#16260,#16261,#16262,#16263));
#3247=EDGE_LOOP('',(#16264,#16265,#16266,#16267));
#3248=EDGE_LOOP('',(#16268,#16269,#16270,#16271));
#3249=EDGE_LOOP('',(#16272,#16273,#16274,#16275));
#3250=EDGE_LOOP('',(#16276,#16277,#16278,#16279));
#3251=EDGE_LOOP('',(#16280,#16281,#16282,#16283));
#3252=EDGE_LOOP('',(#16284,#16285,#16286,#16287));
#3253=EDGE_LOOP('',(#16288,#16289,#16290,#16291));
#3254=EDGE_LOOP('',(#16292,#16293,#16294,#16295,#16296,#16297,#16298,#16299));
#3255=EDGE_LOOP('',(#16300,#16301,#16302,#16303));
#3256=EDGE_LOOP('',(#16304,#16305,#16306,#16307));
#3257=EDGE_LOOP('',(#16308,#16309,#16310,#16311));
#3258=EDGE_LOOP('',(#16312,#16313,#16314,#16315));
#3259=EDGE_LOOP('',(#16316,#16317,#16318,#16319));
#3260=EDGE_LOOP('',(#16320,#16321,#16322,#16323));
#3261=EDGE_LOOP('',(#16324,#16325,#16326,#16327));
#3262=EDGE_LOOP('',(#16328,#16329,#16330,#16331));
#3263=EDGE_LOOP('',(#16332,#16333,#16334,#16335));
#3264=EDGE_LOOP('',(#16336,#16337,#16338,#16339));
#3265=EDGE_LOOP('',(#16340,#16341,#16342,#16343));
#3266=EDGE_LOOP('',(#16344,#16345,#16346,#16347));
#3267=EDGE_LOOP('',(#16348,#16349,#16350,#16351));
#3268=EDGE_LOOP('',(#16352,#16353,#16354,#16355));
#3269=EDGE_LOOP('',(#16356,#16357,#16358,#16359));
#3270=EDGE_LOOP('',(#16360,#16361,#16362,#16363));
#3271=EDGE_LOOP('',(#16364,#16365,#16366,#16367));
#3272=EDGE_LOOP('',(#16368,#16369,#16370,#16371));
#3273=EDGE_LOOP('',(#16372,#16373,#16374,#16375));
#3274=EDGE_LOOP('',(#16376,#16377,#16378,#16379));
#3275=EDGE_LOOP('',(#16380,#16381,#16382,#16383));
#3276=EDGE_LOOP('',(#16384,#16385,#16386,#16387));
#3277=EDGE_LOOP('',(#16388,#16389,#16390,#16391));
#3278=EDGE_LOOP('',(#16392,#16393,#16394,#16395));
#3279=EDGE_LOOP('',(#16396,#16397,#16398,#16399));
#3280=EDGE_LOOP('',(#16400,#16401,#16402,#16403));
#3281=EDGE_LOOP('',(#16404,#16405,#16406,#16407));
#3282=EDGE_LOOP('',(#16408,#16409,#16410,#16411));
#3283=EDGE_LOOP('',(#16412,#16413,#16414,#16415));
#3284=EDGE_LOOP('',(#16416,#16417,#16418,#16419,#16420,#16421));
#3285=EDGE_LOOP('',(#16422,#16423,#16424,#16425,#16426,#16427));
#3286=EDGE_LOOP('',(#16428,#16429,#16430,#16431,#16432,#16433,#16434,#16435));
#3287=EDGE_LOOP('',(#16436,#16437,#16438,#16439,#16440,#16441));
#3288=EDGE_LOOP('',(#16442,#16443,#16444,#16445,#16446,#16447));
#3289=EDGE_LOOP('',(#16448,#16449,#16450,#16451,#16452,#16453));
#3290=EDGE_LOOP('',(#16454,#16455,#16456,#16457,#16458,#16459,#16460,#16461));
#3291=EDGE_LOOP('',(#16462,#16463,#16464,#16465,#16466,#16467));
#3292=EDGE_LOOP('',(#16468,#16469,#16470,#16471,#16472,#16473));
#3293=EDGE_LOOP('',(#16474,#16475,#16476,#16477,#16478,#16479));
#3294=EDGE_LOOP('',(#16480,#16481,#16482,#16483,#16484,#16485,#16486,#16487));
#3295=EDGE_LOOP('',(#16488,#16489,#16490,#16491,#16492,#16493));
#3296=EDGE_LOOP('',(#16494,#16495,#16496,#16497,#16498));
#3297=EDGE_LOOP('',(#16499,#16500,#16501,#16502));
#3298=EDGE_LOOP('',(#16503,#16504,#16505,#16506,#16507,#16508,#16509,#16510,
#16511,#16512,#16513,#16514,#16515,#16516,#16517,#16518,#16519,#16520,#16521,
#16522,#16523,#16524,#16525,#16526,#16527,#16528,#16529,#16530,#16531,#16532,
#16533,#16534,#16535,#16536));
#3299=EDGE_LOOP('',(#16537,#16538,#16539,#16540,#16541,#16542,#16543,#16544,
#16545,#16546,#16547,#16548,#16549,#16550,#16551,#16552,#16553,#16554,#16555,
#16556,#16557,#16558,#16559,#16560,#16561,#16562,#16563,#16564,#16565,#16566,
#16567,#16568,#16569,#16570));
#3300=EDGE_LOOP('',(#16571,#16572,#16573,#16574));
#3301=EDGE_LOOP('',(#16575,#16576,#16577,#16578,#16579));
#3302=EDGE_LOOP('',(#16580,#16581,#16582,#16583));
#3303=EDGE_LOOP('',(#16584,#16585,#16586,#16587,#16588,#16589,#16590,#16591,
#16592,#16593,#16594,#16595,#16596,#16597,#16598,#16599,#16600,#16601,#16602,
#16603,#16604,#16605,#16606,#16607,#16608,#16609,#16610,#16611,#16612,#16613,
#16614,#16615,#16616,#16617));
#3304=EDGE_LOOP('',(#16618,#16619,#16620,#16621,#16622,#16623,#16624,#16625,
#16626,#16627,#16628,#16629,#16630,#16631,#16632,#16633,#16634,#16635,#16636,
#16637,#16638,#16639,#16640,#16641,#16642,#16643,#16644,#16645,#16646,#16647,
#16648,#16649,#16650,#16651));
#3305=EDGE_LOOP('',(#16652,#16653,#16654,#16655));
#3306=EDGE_LOOP('',(#16656,#16657,#16658,#16659,#16660));
#3307=EDGE_LOOP('',(#16661,#16662,#16663,#16664));
#3308=EDGE_LOOP('',(#16665,#16666,#16667,#16668,#16669,#16670,#16671,#16672,
#16673,#16674,#16675,#16676,#16677,#16678,#16679,#16680,#16681,#16682,#16683,
#16684,#16685,#16686,#16687,#16688,#16689,#16690,#16691,#16692,#16693,#16694,
#16695,#16696,#16697,#16698));
#3309=EDGE_LOOP('',(#16699,#16700,#16701,#16702,#16703,#16704,#16705,#16706,
#16707,#16708,#16709,#16710,#16711,#16712,#16713,#16714,#16715,#16716,#16717,
#16718,#16719,#16720,#16721,#16722,#16723,#16724,#16725,#16726,#16727,#16728,
#16729,#16730,#16731,#16732));
#3310=EDGE_LOOP('',(#16733,#16734,#16735,#16736));
#3311=EDGE_LOOP('',(#16737,#16738,#16739,#16740,#16741));
#3312=EDGE_LOOP('',(#16742,#16743,#16744,#16745));
#3313=EDGE_LOOP('',(#16746,#16747,#16748,#16749,#16750,#16751,#16752,#16753,
#16754,#16755,#16756,#16757,#16758,#16759,#16760,#16761,#16762,#16763,#16764,
#16765,#16766,#16767,#16768,#16769,#16770,#16771,#16772,#16773,#16774,#16775,
#16776,#16777,#16778,#16779));
#3314=EDGE_LOOP('',(#16780,#16781,#16782,#16783,#16784,#16785,#16786,#16787,
#16788,#16789,#16790,#16791,#16792,#16793,#16794,#16795,#16796,#16797,#16798,
#16799,#16800,#16801,#16802,#16803,#16804,#16805,#16806,#16807,#16808,#16809,
#16810,#16811,#16812,#16813));
#3315=EDGE_LOOP('',(#16814,#16815,#16816,#16817));
#3316=EDGE_LOOP('',(#16818,#16819,#16820,#16821,#16822));
#3317=EDGE_LOOP('',(#16823,#16824,#16825,#16826));
#3318=EDGE_LOOP('',(#16827,#16828,#16829,#16830,#16831,#16832,#16833,#16834,
#16835,#16836,#16837,#16838,#16839,#16840,#16841,#16842,#16843,#16844,#16845,
#16846,#16847,#16848,#16849,#16850,#16851,#16852,#16853,#16854,#16855,#16856,
#16857,#16858,#16859,#16860));
#3319=EDGE_LOOP('',(#16861,#16862,#16863,#16864,#16865,#16866,#16867,#16868,
#16869,#16870,#16871,#16872,#16873,#16874,#16875,#16876,#16877,#16878,#16879,
#16880,#16881,#16882,#16883,#16884,#16885,#16886,#16887,#16888,#16889,#16890,
#16891,#16892,#16893,#16894));
#3320=EDGE_LOOP('',(#16895,#16896,#16897,#16898));
#3321=EDGE_LOOP('',(#16899,#16900,#16901,#16902,#16903));
#3322=EDGE_LOOP('',(#16904,#16905,#16906,#16907));
#3323=EDGE_LOOP('',(#16908,#16909,#16910,#16911,#16912,#16913,#16914,#16915,
#16916,#16917,#16918,#16919,#16920,#16921,#16922,#16923,#16924,#16925,#16926,
#16927,#16928,#16929,#16930,#16931,#16932,#16933,#16934,#16935,#16936,#16937,
#16938,#16939,#16940,#16941));
#3324=EDGE_LOOP('',(#16942,#16943,#16944,#16945,#16946,#16947,#16948,#16949,
#16950,#16951,#16952,#16953,#16954,#16955,#16956,#16957,#16958,#16959,#16960,
#16961,#16962,#16963,#16964,#16965,#16966,#16967,#16968,#16969,#16970,#16971,
#16972,#16973,#16974,#16975));
#3325=EDGE_LOOP('',(#16976,#16977,#16978,#16979));
#3326=EDGE_LOOP('',(#16980,#16981,#16982,#16983,#16984));
#3327=EDGE_LOOP('',(#16985,#16986,#16987,#16988));
#3328=EDGE_LOOP('',(#16989,#16990,#16991,#16992,#16993,#16994,#16995,#16996,
#16997,#16998,#16999,#17000,#17001,#17002,#17003,#17004,#17005,#17006,#17007,
#17008,#17009,#17010,#17011,#17012,#17013,#17014,#17015,#17016,#17017,#17018,
#17019,#17020,#17021,#17022));
#3329=EDGE_LOOP('',(#17023,#17024,#17025,#17026,#17027,#17028,#17029,#17030,
#17031,#17032,#17033,#17034,#17035,#17036,#17037,#17038,#17039,#17040,#17041,
#17042,#17043,#17044,#17045,#17046,#17047,#17048,#17049,#17050,#17051,#17052,
#17053,#17054,#17055,#17056));
#3330=EDGE_LOOP('',(#17057,#17058,#17059,#17060));
#3331=EDGE_LOOP('',(#17061,#17062,#17063,#17064,#17065));
#3332=EDGE_LOOP('',(#17066,#17067,#17068,#17069));
#3333=EDGE_LOOP('',(#17070,#17071,#17072,#17073,#17074,#17075,#17076,#17077,
#17078,#17079,#17080,#17081,#17082,#17083,#17084,#17085,#17086,#17087,#17088,
#17089,#17090,#17091,#17092,#17093,#17094,#17095,#17096,#17097,#17098,#17099,
#17100,#17101,#17102,#17103));
#3334=EDGE_LOOP('',(#17104,#17105,#17106,#17107,#17108,#17109,#17110,#17111,
#17112,#17113,#17114,#17115,#17116,#17117,#17118,#17119,#17120,#17121,#17122,
#17123,#17124,#17125,#17126,#17127,#17128,#17129,#17130,#17131,#17132,#17133,
#17134,#17135,#17136,#17137));
#3335=EDGE_LOOP('',(#17138,#17139,#17140,#17141));
#3336=EDGE_LOOP('',(#17142));
#3337=EDGE_LOOP('',(#17143));
#3338=EDGE_LOOP('',(#17144));
#3339=EDGE_LOOP('',(#17145));
#3340=EDGE_LOOP('',(#17146));
#3341=EDGE_LOOP('',(#17147));
#3342=EDGE_LOOP('',(#17148));
#3343=EDGE_LOOP('',(#17149));
#3344=EDGE_LOOP('',(#17150,#17151,#17152,#17153));
#3345=EDGE_LOOP('',(#17154,#17155,#17156,#17157));
#3346=EDGE_LOOP('',(#17158,#17159,#17160,#17161));
#3347=EDGE_LOOP('',(#17162,#17163,#17164,#17165));
#3348=EDGE_LOOP('',(#17166,#17167,#17168,#17169));
#3349=EDGE_LOOP('',(#17170));
#3350=EDGE_LOOP('',(#17171));
#3351=EDGE_LOOP('',(#17172,#17173,#17174,#17175,#17176,#17177,#17178,#17179,
#17180,#17181,#17182,#17183,#17184,#17185,#17186,#17187,#17188,#17189,#17190));
#3352=EDGE_LOOP('',(#17191,#17192));
#3353=EDGE_LOOP('',(#17193,#17194));
#3354=EDGE_LOOP('',(#17195));
#3355=EDGE_LOOP('',(#17196,#17197));
#3356=EDGE_LOOP('',(#17198,#17199));
#3357=EDGE_LOOP('',(#17200));
#3358=EDGE_LOOP('',(#17201,#17202));
#3359=EDGE_LOOP('',(#17203,#17204));
#3360=EDGE_LOOP('',(#17205));
#3361=EDGE_LOOP('',(#17206,#17207,#17208,#17209,#17210,#17211,#17212,#17213,
#17214,#17215,#17216,#17217,#17218,#17219,#17220,#17221,#17222,#17223,#17224));
#3362=EDGE_LOOP('',(#17225,#17226));
#3363=EDGE_LOOP('',(#17227,#17228));
#3364=EDGE_LOOP('',(#17229,#17230,#17231));
#3365=EDGE_LOOP('',(#17232,#17233));
#3366=EDGE_LOOP('',(#17234,#17235));
#3367=EDGE_LOOP('',(#17236,#17237,#17238));
#3368=EDGE_LOOP('',(#17239,#17240));
#3369=EDGE_LOOP('',(#17241,#17242));
#3370=EDGE_LOOP('',(#17243,#17244,#17245));
#3371=EDGE_LOOP('',(#17246));
#3372=EDGE_LOOP('',(#17247,#17248,#17249,#17250));
#3373=EDGE_LOOP('',(#17251,#17252,#17253,#17254));
#3374=EDGE_LOOP('',(#17255,#17256,#17257,#17258));
#3375=EDGE_LOOP('',(#17259,#17260,#17261,#17262));
#3376=EDGE_LOOP('',(#17263));
#3377=EDGE_LOOP('',(#17264,#17265,#17266,#17267));
#3378=EDGE_LOOP('',(#17268,#17269,#17270,#17271));
#3379=EDGE_LOOP('',(#17272,#17273,#17274,#17275));
#3380=EDGE_LOOP('',(#17276,#17277,#17278,#17279));
#3381=EDGE_LOOP('',(#17280));
#3382=EDGE_LOOP('',(#17281));
#3383=EDGE_LOOP('',(#17282));
#3384=EDGE_LOOP('',(#17283));
#3385=EDGE_LOOP('',(#17284));
#3386=EDGE_LOOP('',(#17285));
#3387=EDGE_LOOP('',(#17286,#17287,#17288,#17289));
#3388=EDGE_LOOP('',(#17290,#17291,#17292,#17293));
#3389=EDGE_LOOP('',(#17294));
#3390=EDGE_LOOP('',(#17295));
#3391=EDGE_LOOP('',(#17296));
#3392=EDGE_LOOP('',(#17297));
#3393=EDGE_LOOP('',(#17298));
#3394=EDGE_LOOP('',(#17299));
#3395=EDGE_LOOP('',(#17300));
#3396=EDGE_LOOP('',(#17301));
#3397=EDGE_LOOP('',(#17302,#17303,#17304,#17305,#17306));
#3398=EDGE_LOOP('',(#17307));
#3399=EDGE_LOOP('',(#17308,#17309,#17310,#17311,#17312));
#3400=EDGE_LOOP('',(#17313));
#3401=EDGE_LOOP('',(#17314,#17315,#17316,#17317,#17318,#17319));
#3402=EDGE_LOOP('',(#17320));
#3403=EDGE_LOOP('',(#17321,#17322,#17323,#17324,#17325,#17326));
#3404=EDGE_LOOP('',(#17327));
#3405=EDGE_LOOP('',(#17328,#17329,#17330,#17331));
#3406=EDGE_LOOP('',(#17332,#17333,#17334,#17335,#17336,#17337,#17338,#17339,
#17340));
#3407=EDGE_LOOP('',(#17341,#17342));
#3408=EDGE_LOOP('',(#17343,#17344));
#3409=EDGE_LOOP('',(#17345,#17346,#17347));
#3410=EDGE_LOOP('',(#17348));
#3411=EDGE_LOOP('',(#17349));
#3412=EDGE_LOOP('',(#17350));
#3413=EDGE_LOOP('',(#17351));
#3414=EDGE_LOOP('',(#17352,#17353,#17354,#17355));
#3415=EDGE_LOOP('',(#17356,#17357,#17358,#17359));
#3416=EDGE_LOOP('',(#17360,#17361,#17362,#17363));
#3417=EDGE_LOOP('',(#17364,#17365,#17366,#17367));
#3418=EDGE_LOOP('',(#17368,#17369,#17370,#17371));
#3419=EDGE_LOOP('',(#17372,#17373,#17374,#17375));
#3420=EDGE_LOOP('',(#17376,#17377,#17378,#17379));
#3421=EDGE_LOOP('',(#17380,#17381,#17382,#17383));
#3422=EDGE_LOOP('',(#17384,#17385,#17386,#17387));
#3423=EDGE_LOOP('',(#17388,#17389,#17390,#17391));
#3424=EDGE_LOOP('',(#17392));
#3425=EDGE_LOOP('',(#17393));
#3426=EDGE_LOOP('',(#17394));
#3427=EDGE_LOOP('',(#17395));
#3428=EDGE_LOOP('',(#17396));
#3429=EDGE_LOOP('',(#17397));
#3430=EDGE_LOOP('',(#17398));
#3431=EDGE_LOOP('',(#17399));
#3432=EDGE_LOOP('',(#17400));
#3433=EDGE_LOOP('',(#17401));
#3434=EDGE_LOOP('',(#17402));
#3435=EDGE_LOOP('',(#17403));
#3436=EDGE_LOOP('',(#17404));
#3437=EDGE_LOOP('',(#17405));
#3438=EDGE_LOOP('',(#17406));
#3439=EDGE_LOOP('',(#17407));
#3440=EDGE_LOOP('',(#17408));
#3441=EDGE_LOOP('',(#17409));
#3442=EDGE_LOOP('',(#17410));
#3443=EDGE_LOOP('',(#17411));
#3444=EDGE_LOOP('',(#17412,#17413,#17414,#17415));
#3445=EDGE_LOOP('',(#17416,#17417,#17418,#17419));
#3446=EDGE_LOOP('',(#17420,#17421,#17422,#17423));
#3447=EDGE_LOOP('',(#17424,#17425,#17426,#17427));
#3448=EDGE_LOOP('',(#17428,#17429,#17430,#17431));
#3449=EDGE_LOOP('',(#17432,#17433,#17434,#17435));
#3450=EDGE_LOOP('',(#17436));
#3451=EDGE_LOOP('',(#17437));
#3452=EDGE_LOOP('',(#17438));
#3453=EDGE_LOOP('',(#17439));
#3454=EDGE_LOOP('',(#17440,#17441,#17442,#17443));
#3455=EDGE_LOOP('',(#17444,#17445,#17446,#17447));
#3456=EDGE_LOOP('',(#17448));
#3457=EDGE_LOOP('',(#17449));
#3458=EDGE_LOOP('',(#17450));
#3459=EDGE_LOOP('',(#17451));
#3460=EDGE_LOOP('',(#17452,#17453,#17454,#17455));
#3461=EDGE_LOOP('',(#17456));
#3462=EDGE_LOOP('',(#17457));
#3463=EDGE_LOOP('',(#17458));
#3464=EDGE_LOOP('',(#17459));
#3465=EDGE_LOOP('',(#17460,#17461,#17462,#17463));
#3466=EDGE_LOOP('',(#17464,#17465,#17466,#17467));
#3467=EDGE_LOOP('',(#17468));
#3468=EDGE_LOOP('',(#17469));
#3469=EDGE_LOOP('',(#17470));
#3470=EDGE_LOOP('',(#17471));
#3471=EDGE_LOOP('',(#17472,#17473,#17474,#17475));
#3472=EDGE_LOOP('',(#17476,#17477,#17478,#17479));
#3473=EDGE_LOOP('',(#17480,#17481,#17482,#17483));
#3474=EDGE_LOOP('',(#17484,#17485,#17486,#17487));
#3475=EDGE_LOOP('',(#17488));
#3476=EDGE_LOOP('',(#17489,#17490,#17491,#17492));
#3477=EDGE_LOOP('',(#17493));
#3478=EDGE_LOOP('',(#17494,#17495,#17496,#17497));
#3479=EDGE_LOOP('',(#17498));
#3480=EDGE_LOOP('',(#17499));
#3481=EDGE_LOOP('',(#17500));
#3482=EDGE_LOOP('',(#17501));
#3483=EDGE_LOOP('',(#17502,#17503,#17504,#17505,#17506));
#3484=EDGE_LOOP('',(#17507));
#3485=EDGE_LOOP('',(#17508,#17509,#17510,#17511,#17512));
#3486=EDGE_LOOP('',(#17513));
#3487=EDGE_LOOP('',(#17514,#17515,#17516,#17517,#17518,#17519));
#3488=EDGE_LOOP('',(#17520));
#3489=EDGE_LOOP('',(#17521,#17522,#17523,#17524,#17525,#17526));
#3490=EDGE_LOOP('',(#17527));
#3491=EDGE_LOOP('',(#17528,#17529,#17530,#17531));
#3492=EDGE_LOOP('',(#17532,#17533,#17534,#17535));
#3493=EDGE_LOOP('',(#17536,#17537,#17538,#17539));
#3494=EDGE_LOOP('',(#17540,#17541,#17542,#17543));
#3495=EDGE_LOOP('',(#17544,#17545,#17546,#17547));
#3496=EDGE_LOOP('',(#17548,#17549,#17550,#17551));
#3497=EDGE_LOOP('',(#17552,#17553,#17554,#17555));
#3498=EDGE_LOOP('',(#17556,#17557,#17558,#17559));
#3499=EDGE_LOOP('',(#17560,#17561,#17562,#17563));
#3500=EDGE_LOOP('',(#17564,#17565,#17566,#17567));
#3501=EDGE_LOOP('',(#17568,#17569,#17570,#17571));
#3502=EDGE_LOOP('',(#17572,#17573,#17574,#17575));
#3503=EDGE_LOOP('',(#17576,#17577,#17578,#17579));
#3504=EDGE_LOOP('',(#17580,#17581,#17582,#17583));
#3505=EDGE_LOOP('',(#17584,#17585,#17586,#17587));
#3506=EDGE_LOOP('',(#17588,#17589,#17590,#17591));
#3507=EDGE_LOOP('',(#17592,#17593,#17594,#17595));
#3508=EDGE_LOOP('',(#17596,#17597,#17598,#17599));
#3509=EDGE_LOOP('',(#17600,#17601,#17602,#17603));
#3510=EDGE_LOOP('',(#17604,#17605,#17606,#17607));
#3511=EDGE_LOOP('',(#17608,#17609,#17610,#17611));
#3512=EDGE_LOOP('',(#17612,#17613,#17614,#17615));
#3513=EDGE_LOOP('',(#17616,#17617,#17618,#17619));
#3514=EDGE_LOOP('',(#17620,#17621,#17622,#17623));
#3515=EDGE_LOOP('',(#17624,#17625,#17626,#17627));
#3516=EDGE_LOOP('',(#17628,#17629,#17630,#17631));
#3517=EDGE_LOOP('',(#17632,#17633,#17634,#17635));
#3518=EDGE_LOOP('',(#17636,#17637,#17638,#17639));
#3519=EDGE_LOOP('',(#17640,#17641,#17642,#17643));
#3520=EDGE_LOOP('',(#17644,#17645,#17646,#17647));
#3521=EDGE_LOOP('',(#17648,#17649,#17650,#17651));
#3522=EDGE_LOOP('',(#17652,#17653,#17654,#17655));
#3523=EDGE_LOOP('',(#17656,#17657,#17658,#17659));
#3524=EDGE_LOOP('',(#17660,#17661,#17662,#17663));
#3525=EDGE_LOOP('',(#17664,#17665,#17666,#17667));
#3526=EDGE_LOOP('',(#17668,#17669,#17670,#17671));
#3527=EDGE_LOOP('',(#17672,#17673,#17674,#17675));
#3528=EDGE_LOOP('',(#17676,#17677,#17678,#17679));
#3529=EDGE_LOOP('',(#17680,#17681,#17682,#17683));
#3530=EDGE_LOOP('',(#17684,#17685,#17686,#17687));
#3531=EDGE_LOOP('',(#17688,#17689,#17690,#17691));
#3532=EDGE_LOOP('',(#17692,#17693,#17694,#17695));
#3533=EDGE_LOOP('',(#17696,#17697,#17698,#17699));
#3534=EDGE_LOOP('',(#17700,#17701,#17702,#17703));
#3535=EDGE_LOOP('',(#17704,#17705,#17706,#17707));
#3536=EDGE_LOOP('',(#17708,#17709,#17710,#17711));
#3537=EDGE_LOOP('',(#17712,#17713,#17714,#17715));
#3538=EDGE_LOOP('',(#17716,#17717,#17718,#17719));
#3539=EDGE_LOOP('',(#17720,#17721,#17722,#17723));
#3540=EDGE_LOOP('',(#17724,#17725,#17726,#17727));
#3541=EDGE_LOOP('',(#17728,#17729,#17730,#17731));
#3542=EDGE_LOOP('',(#17732,#17733,#17734,#17735));
#3543=EDGE_LOOP('',(#17736,#17737,#17738,#17739));
#3544=EDGE_LOOP('',(#17740,#17741,#17742,#17743));
#3545=EDGE_LOOP('',(#17744,#17745,#17746,#17747));
#3546=EDGE_LOOP('',(#17748,#17749,#17750,#17751));
#3547=EDGE_LOOP('',(#17752,#17753,#17754,#17755));
#3548=EDGE_LOOP('',(#17756,#17757,#17758,#17759));
#3549=EDGE_LOOP('',(#17760,#17761,#17762,#17763));
#3550=EDGE_LOOP('',(#17764,#17765,#17766,#17767));
#3551=EDGE_LOOP('',(#17768,#17769,#17770,#17771));
#3552=EDGE_LOOP('',(#17772,#17773,#17774,#17775));
#3553=EDGE_LOOP('',(#17776,#17777,#17778,#17779));
#3554=EDGE_LOOP('',(#17780,#17781,#17782,#17783));
#3555=EDGE_LOOP('',(#17784,#17785,#17786,#17787));
#3556=EDGE_LOOP('',(#17788,#17789,#17790,#17791));
#3557=EDGE_LOOP('',(#17792,#17793,#17794,#17795));
#3558=EDGE_LOOP('',(#17796,#17797,#17798,#17799));
#3559=EDGE_LOOP('',(#17800,#17801,#17802,#17803));
#3560=EDGE_LOOP('',(#17804,#17805,#17806,#17807));
#3561=EDGE_LOOP('',(#17808,#17809,#17810,#17811));
#3562=EDGE_LOOP('',(#17812,#17813,#17814,#17815));
#3563=EDGE_LOOP('',(#17816,#17817,#17818,#17819));
#3564=EDGE_LOOP('',(#17820,#17821,#17822,#17823));
#3565=EDGE_LOOP('',(#17824,#17825,#17826,#17827));
#3566=EDGE_LOOP('',(#17828,#17829,#17830,#17831));
#3567=EDGE_LOOP('',(#17832,#17833,#17834,#17835));
#3568=EDGE_LOOP('',(#17836,#17837,#17838,#17839));
#3569=EDGE_LOOP('',(#17840,#17841,#17842,#17843));
#3570=EDGE_LOOP('',(#17844,#17845,#17846,#17847));
#3571=EDGE_LOOP('',(#17848,#17849,#17850,#17851));
#3572=EDGE_LOOP('',(#17852,#17853,#17854,#17855));
#3573=EDGE_LOOP('',(#17856,#17857,#17858,#17859));
#3574=EDGE_LOOP('',(#17860,#17861,#17862,#17863));
#3575=EDGE_LOOP('',(#17864,#17865,#17866,#17867));
#3576=EDGE_LOOP('',(#17868,#17869,#17870,#17871));
#3577=EDGE_LOOP('',(#17872,#17873,#17874,#17875));
#3578=EDGE_LOOP('',(#17876,#17877,#17878,#17879));
#3579=EDGE_LOOP('',(#17880,#17881,#17882,#17883));
#3580=EDGE_LOOP('',(#17884,#17885,#17886,#17887));
#3581=EDGE_LOOP('',(#17888,#17889,#17890,#17891));
#3582=EDGE_LOOP('',(#17892,#17893,#17894,#17895));
#3583=EDGE_LOOP('',(#17896,#17897,#17898,#17899));
#3584=EDGE_LOOP('',(#17900,#17901,#17902,#17903));
#3585=EDGE_LOOP('',(#17904,#17905,#17906,#17907));
#3586=EDGE_LOOP('',(#17908,#17909,#17910,#17911));
#3587=EDGE_LOOP('',(#17912,#17913,#17914,#17915));
#3588=EDGE_LOOP('',(#17916,#17917,#17918,#17919));
#3589=EDGE_LOOP('',(#17920,#17921,#17922,#17923));
#3590=EDGE_LOOP('',(#17924,#17925,#17926,#17927));
#3591=EDGE_LOOP('',(#17928,#17929,#17930,#17931));
#3592=EDGE_LOOP('',(#17932,#17933,#17934,#17935));
#3593=EDGE_LOOP('',(#17936,#17937,#17938,#17939));
#3594=EDGE_LOOP('',(#17940,#17941,#17942,#17943));
#3595=EDGE_LOOP('',(#17944,#17945,#17946,#17947));
#3596=EDGE_LOOP('',(#17948,#17949,#17950,#17951));
#3597=EDGE_LOOP('',(#17952,#17953,#17954,#17955));
#3598=EDGE_LOOP('',(#17956,#17957,#17958,#17959));
#3599=EDGE_LOOP('',(#17960,#17961,#17962,#17963));
#3600=EDGE_LOOP('',(#17964,#17965,#17966,#17967));
#3601=EDGE_LOOP('',(#17968,#17969,#17970,#17971));
#3602=EDGE_LOOP('',(#17972,#17973,#17974,#17975));
#3603=EDGE_LOOP('',(#17976,#17977,#17978,#17979));
#3604=EDGE_LOOP('',(#17980,#17981,#17982,#17983));
#3605=EDGE_LOOP('',(#17984,#17985,#17986,#17987));
#3606=EDGE_LOOP('',(#17988,#17989,#17990,#17991));
#3607=EDGE_LOOP('',(#17992,#17993,#17994,#17995));
#3608=EDGE_LOOP('',(#17996,#17997,#17998,#17999));
#3609=EDGE_LOOP('',(#18000,#18001,#18002,#18003));
#3610=EDGE_LOOP('',(#18004,#18005,#18006,#18007));
#3611=EDGE_LOOP('',(#18008,#18009,#18010,#18011));
#3612=EDGE_LOOP('',(#18012,#18013,#18014,#18015));
#3613=EDGE_LOOP('',(#18016,#18017,#18018,#18019));
#3614=EDGE_LOOP('',(#18020,#18021,#18022,#18023));
#3615=EDGE_LOOP('',(#18024,#18025,#18026,#18027));
#3616=EDGE_LOOP('',(#18028,#18029,#18030,#18031));
#3617=EDGE_LOOP('',(#18032,#18033,#18034,#18035));
#3618=EDGE_LOOP('',(#18036,#18037,#18038,#18039));
#3619=EDGE_LOOP('',(#18040,#18041,#18042,#18043));
#3620=EDGE_LOOP('',(#18044,#18045,#18046,#18047));
#3621=EDGE_LOOP('',(#18048,#18049,#18050,#18051));
#3622=EDGE_LOOP('',(#18052,#18053,#18054,#18055));
#3623=EDGE_LOOP('',(#18056,#18057,#18058,#18059));
#3624=EDGE_LOOP('',(#18060,#18061,#18062,#18063));
#3625=EDGE_LOOP('',(#18064,#18065,#18066,#18067));
#3626=EDGE_LOOP('',(#18068,#18069,#18070,#18071));
#3627=EDGE_LOOP('',(#18072,#18073,#18074,#18075));
#3628=EDGE_LOOP('',(#18076,#18077,#18078,#18079));
#3629=EDGE_LOOP('',(#18080,#18081,#18082,#18083));
#3630=EDGE_LOOP('',(#18084,#18085,#18086,#18087));
#3631=EDGE_LOOP('',(#18088,#18089,#18090,#18091));
#3632=EDGE_LOOP('',(#18092,#18093,#18094,#18095));
#3633=EDGE_LOOP('',(#18096,#18097,#18098,#18099));
#3634=EDGE_LOOP('',(#18100,#18101,#18102,#18103));
#3635=EDGE_LOOP('',(#18104,#18105,#18106,#18107));
#3636=EDGE_LOOP('',(#18108,#18109,#18110,#18111));
#3637=EDGE_LOOP('',(#18112,#18113,#18114,#18115));
#3638=EDGE_LOOP('',(#18116,#18117,#18118,#18119));
#3639=EDGE_LOOP('',(#18120,#18121,#18122,#18123));
#3640=EDGE_LOOP('',(#18124,#18125,#18126,#18127));
#3641=EDGE_LOOP('',(#18128,#18129,#18130,#18131));
#3642=EDGE_LOOP('',(#18132,#18133,#18134,#18135));
#3643=EDGE_LOOP('',(#18136,#18137,#18138,#18139));
#3644=EDGE_LOOP('',(#18140,#18141,#18142,#18143));
#3645=EDGE_LOOP('',(#18144,#18145,#18146,#18147));
#3646=EDGE_LOOP('',(#18148,#18149,#18150,#18151));
#3647=EDGE_LOOP('',(#18152,#18153,#18154,#18155));
#3648=EDGE_LOOP('',(#18156,#18157,#18158,#18159));
#3649=EDGE_LOOP('',(#18160,#18161,#18162,#18163));
#3650=EDGE_LOOP('',(#18164,#18165,#18166,#18167));
#3651=EDGE_LOOP('',(#18168,#18169,#18170,#18171));
#3652=EDGE_LOOP('',(#18172,#18173,#18174,#18175));
#3653=EDGE_LOOP('',(#18176,#18177,#18178,#18179));
#3654=EDGE_LOOP('',(#18180,#18181,#18182,#18183));
#3655=EDGE_LOOP('',(#18184,#18185,#18186,#18187));
#3656=EDGE_LOOP('',(#18188,#18189,#18190,#18191));
#3657=EDGE_LOOP('',(#18192,#18193,#18194,#18195));
#3658=EDGE_LOOP('',(#18196,#18197,#18198,#18199));
#3659=EDGE_LOOP('',(#18200,#18201,#18202,#18203));
#3660=EDGE_LOOP('',(#18204,#18205,#18206,#18207));
#3661=EDGE_LOOP('',(#18208,#18209,#18210,#18211));
#3662=EDGE_LOOP('',(#18212,#18213,#18214,#18215));
#3663=EDGE_LOOP('',(#18216,#18217,#18218,#18219));
#3664=EDGE_LOOP('',(#18220,#18221,#18222,#18223));
#3665=EDGE_LOOP('',(#18224,#18225,#18226,#18227));
#3666=EDGE_LOOP('',(#18228,#18229,#18230,#18231));
#3667=EDGE_LOOP('',(#18232,#18233,#18234,#18235));
#3668=EDGE_LOOP('',(#18236,#18237,#18238,#18239));
#3669=EDGE_LOOP('',(#18240,#18241,#18242,#18243));
#3670=EDGE_LOOP('',(#18244,#18245,#18246,#18247));
#3671=EDGE_LOOP('',(#18248,#18249,#18250,#18251));
#3672=EDGE_LOOP('',(#18252,#18253,#18254,#18255));
#3673=EDGE_LOOP('',(#18256,#18257,#18258,#18259));
#3674=EDGE_LOOP('',(#18260,#18261,#18262,#18263));
#3675=EDGE_LOOP('',(#18264,#18265,#18266,#18267));
#3676=EDGE_LOOP('',(#18268,#18269,#18270,#18271));
#3677=EDGE_LOOP('',(#18272,#18273,#18274,#18275));
#3678=EDGE_LOOP('',(#18276,#18277,#18278,#18279));
#3679=EDGE_LOOP('',(#18280,#18281,#18282,#18283));
#3680=EDGE_LOOP('',(#18284,#18285,#18286,#18287));
#3681=EDGE_LOOP('',(#18288,#18289,#18290,#18291));
#3682=EDGE_LOOP('',(#18292,#18293,#18294,#18295));
#3683=EDGE_LOOP('',(#18296,#18297,#18298,#18299));
#3684=EDGE_LOOP('',(#18300,#18301,#18302,#18303));
#3685=EDGE_LOOP('',(#18304,#18305,#18306,#18307));
#3686=EDGE_LOOP('',(#18308,#18309,#18310,#18311));
#3687=EDGE_LOOP('',(#18312,#18313,#18314,#18315));
#3688=EDGE_LOOP('',(#18316,#18317,#18318,#18319));
#3689=EDGE_LOOP('',(#18320,#18321,#18322,#18323));
#3690=EDGE_LOOP('',(#18324,#18325,#18326,#18327));
#3691=EDGE_LOOP('',(#18328,#18329,#18330,#18331));
#3692=EDGE_LOOP('',(#18332,#18333,#18334,#18335));
#3693=EDGE_LOOP('',(#18336,#18337,#18338,#18339));
#3694=EDGE_LOOP('',(#18340,#18341,#18342,#18343));
#3695=EDGE_LOOP('',(#18344,#18345,#18346,#18347));
#3696=EDGE_LOOP('',(#18348,#18349,#18350,#18351));
#3697=EDGE_LOOP('',(#18352,#18353,#18354,#18355));
#3698=EDGE_LOOP('',(#18356,#18357,#18358,#18359));
#3699=EDGE_LOOP('',(#18360,#18361,#18362,#18363));
#3700=EDGE_LOOP('',(#18364,#18365,#18366,#18367));
#3701=EDGE_LOOP('',(#18368,#18369,#18370,#18371));
#3702=EDGE_LOOP('',(#18372,#18373,#18374,#18375));
#3703=EDGE_LOOP('',(#18376,#18377,#18378,#18379));
#3704=EDGE_LOOP('',(#18380,#18381,#18382,#18383));
#3705=EDGE_LOOP('',(#18384,#18385,#18386,#18387));
#3706=EDGE_LOOP('',(#18388,#18389,#18390,#18391));
#3707=EDGE_LOOP('',(#18392,#18393,#18394,#18395));
#3708=EDGE_LOOP('',(#18396,#18397,#18398,#18399));
#3709=EDGE_LOOP('',(#18400,#18401,#18402,#18403));
#3710=EDGE_LOOP('',(#18404,#18405,#18406,#18407));
#3711=EDGE_LOOP('',(#18408,#18409,#18410,#18411));
#3712=EDGE_LOOP('',(#18412,#18413,#18414,#18415));
#3713=EDGE_LOOP('',(#18416,#18417,#18418,#18419));
#3714=EDGE_LOOP('',(#18420,#18421,#18422,#18423));
#3715=EDGE_LOOP('',(#18424,#18425,#18426,#18427));
#3716=EDGE_LOOP('',(#18428,#18429,#18430,#18431));
#3717=EDGE_LOOP('',(#18432,#18433,#18434,#18435));
#3718=EDGE_LOOP('',(#18436,#18437,#18438,#18439));
#3719=EDGE_LOOP('',(#18440,#18441,#18442,#18443));
#3720=EDGE_LOOP('',(#18444,#18445,#18446,#18447));
#3721=EDGE_LOOP('',(#18448,#18449,#18450,#18451));
#3722=EDGE_LOOP('',(#18452,#18453,#18454,#18455));
#3723=EDGE_LOOP('',(#18456,#18457,#18458,#18459));
#3724=EDGE_LOOP('',(#18460,#18461,#18462,#18463));
#3725=EDGE_LOOP('',(#18464,#18465,#18466,#18467));
#3726=EDGE_LOOP('',(#18468,#18469,#18470,#18471));
#3727=EDGE_LOOP('',(#18472,#18473,#18474,#18475));
#3728=EDGE_LOOP('',(#18476,#18477,#18478,#18479));
#3729=EDGE_LOOP('',(#18480,#18481,#18482,#18483));
#3730=EDGE_LOOP('',(#18484,#18485,#18486,#18487));
#3731=EDGE_LOOP('',(#18488,#18489,#18490,#18491));
#3732=EDGE_LOOP('',(#18492,#18493,#18494,#18495));
#3733=EDGE_LOOP('',(#18496,#18497,#18498,#18499));
#3734=EDGE_LOOP('',(#18500,#18501,#18502,#18503));
#3735=EDGE_LOOP('',(#18504,#18505,#18506,#18507));
#3736=EDGE_LOOP('',(#18508,#18509,#18510,#18511));
#3737=EDGE_LOOP('',(#18512,#18513,#18514,#18515));
#3738=EDGE_LOOP('',(#18516,#18517,#18518,#18519));
#3739=EDGE_LOOP('',(#18520,#18521,#18522,#18523));
#3740=EDGE_LOOP('',(#18524,#18525,#18526,#18527));
#3741=EDGE_LOOP('',(#18528,#18529,#18530,#18531));
#3742=EDGE_LOOP('',(#18532,#18533,#18534,#18535));
#3743=EDGE_LOOP('',(#18536,#18537,#18538,#18539));
#3744=EDGE_LOOP('',(#18540,#18541,#18542,#18543));
#3745=EDGE_LOOP('',(#18544,#18545,#18546,#18547));
#3746=EDGE_LOOP('',(#18548,#18549,#18550,#18551));
#3747=EDGE_LOOP('',(#18552,#18553,#18554,#18555));
#3748=EDGE_LOOP('',(#18556,#18557,#18558,#18559));
#3749=EDGE_LOOP('',(#18560,#18561,#18562,#18563));
#3750=EDGE_LOOP('',(#18564,#18565,#18566,#18567));
#3751=EDGE_LOOP('',(#18568,#18569,#18570,#18571));
#3752=EDGE_LOOP('',(#18572,#18573,#18574,#18575));
#3753=EDGE_LOOP('',(#18576,#18577,#18578,#18579));
#3754=EDGE_LOOP('',(#18580,#18581,#18582,#18583));
#3755=EDGE_LOOP('',(#18584,#18585,#18586,#18587));
#3756=EDGE_LOOP('',(#18588,#18589,#18590,#18591));
#3757=EDGE_LOOP('',(#18592,#18593,#18594,#18595));
#3758=EDGE_LOOP('',(#18596,#18597,#18598,#18599));
#3759=EDGE_LOOP('',(#18600,#18601,#18602,#18603));
#3760=EDGE_LOOP('',(#18604,#18605,#18606,#18607));
#3761=EDGE_LOOP('',(#18608,#18609,#18610,#18611));
#3762=EDGE_LOOP('',(#18612,#18613,#18614,#18615));
#3763=EDGE_LOOP('',(#18616,#18617,#18618,#18619));
#3764=EDGE_LOOP('',(#18620,#18621,#18622,#18623));
#3765=EDGE_LOOP('',(#18624,#18625,#18626,#18627));
#3766=EDGE_LOOP('',(#18628,#18629,#18630,#18631));
#3767=EDGE_LOOP('',(#18632,#18633,#18634,#18635));
#3768=EDGE_LOOP('',(#18636,#18637,#18638,#18639));
#3769=EDGE_LOOP('',(#18640,#18641,#18642,#18643));
#3770=EDGE_LOOP('',(#18644,#18645,#18646,#18647));
#3771=EDGE_LOOP('',(#18648,#18649,#18650,#18651));
#3772=EDGE_LOOP('',(#18652,#18653,#18654,#18655));
#3773=EDGE_LOOP('',(#18656,#18657,#18658,#18659));
#3774=EDGE_LOOP('',(#18660,#18661,#18662,#18663));
#3775=EDGE_LOOP('',(#18664,#18665,#18666,#18667));
#3776=EDGE_LOOP('',(#18668,#18669,#18670,#18671));
#3777=EDGE_LOOP('',(#18672,#18673,#18674,#18675));
#3778=EDGE_LOOP('',(#18676,#18677,#18678,#18679));
#3779=EDGE_LOOP('',(#18680,#18681,#18682,#18683));
#3780=EDGE_LOOP('',(#18684,#18685,#18686,#18687));
#3781=EDGE_LOOP('',(#18688,#18689,#18690,#18691));
#3782=EDGE_LOOP('',(#18692,#18693,#18694,#18695));
#3783=EDGE_LOOP('',(#18696,#18697,#18698,#18699));
#3784=EDGE_LOOP('',(#18700,#18701,#18702,#18703));
#3785=EDGE_LOOP('',(#18704,#18705,#18706,#18707));
#3786=EDGE_LOOP('',(#18708,#18709,#18710,#18711));
#3787=EDGE_LOOP('',(#18712,#18713,#18714,#18715));
#3788=EDGE_LOOP('',(#18716,#18717,#18718,#18719));
#3789=EDGE_LOOP('',(#18720,#18721,#18722,#18723));
#3790=EDGE_LOOP('',(#18724,#18725,#18726,#18727));
#3791=EDGE_LOOP('',(#18728,#18729,#18730,#18731));
#3792=EDGE_LOOP('',(#18732,#18733,#18734,#18735));
#3793=EDGE_LOOP('',(#18736,#18737,#18738,#18739));
#3794=EDGE_LOOP('',(#18740,#18741,#18742,#18743));
#3795=EDGE_LOOP('',(#18744,#18745,#18746,#18747));
#3796=EDGE_LOOP('',(#18748,#18749,#18750,#18751));
#3797=EDGE_LOOP('',(#18752,#18753,#18754,#18755));
#3798=EDGE_LOOP('',(#18756,#18757,#18758,#18759));
#3799=EDGE_LOOP('',(#18760,#18761,#18762,#18763));
#3800=EDGE_LOOP('',(#18764,#18765,#18766,#18767));
#3801=EDGE_LOOP('',(#18768,#18769,#18770,#18771));
#3802=EDGE_LOOP('',(#18772,#18773,#18774,#18775));
#3803=EDGE_LOOP('',(#18776,#18777,#18778,#18779));
#3804=EDGE_LOOP('',(#18780,#18781,#18782,#18783));
#3805=EDGE_LOOP('',(#18784,#18785,#18786,#18787));
#3806=EDGE_LOOP('',(#18788,#18789,#18790,#18791));
#3807=EDGE_LOOP('',(#18792,#18793,#18794,#18795));
#3808=EDGE_LOOP('',(#18796,#18797,#18798,#18799));
#3809=EDGE_LOOP('',(#18800,#18801,#18802,#18803));
#3810=EDGE_LOOP('',(#18804,#18805,#18806,#18807));
#3811=EDGE_LOOP('',(#18808,#18809,#18810,#18811));
#3812=EDGE_LOOP('',(#18812,#18813,#18814,#18815));
#3813=EDGE_LOOP('',(#18816,#18817,#18818,#18819));
#3814=EDGE_LOOP('',(#18820,#18821,#18822,#18823));
#3815=EDGE_LOOP('',(#18824,#18825,#18826,#18827));
#3816=EDGE_LOOP('',(#18828,#18829,#18830,#18831));
#3817=EDGE_LOOP('',(#18832,#18833,#18834,#18835));
#3818=EDGE_LOOP('',(#18836,#18837,#18838,#18839));
#3819=EDGE_LOOP('',(#18840,#18841,#18842,#18843));
#3820=EDGE_LOOP('',(#18844,#18845,#18846,#18847));
#3821=EDGE_LOOP('',(#18848,#18849,#18850,#18851));
#3822=EDGE_LOOP('',(#18852,#18853,#18854,#18855));
#3823=EDGE_LOOP('',(#18856,#18857,#18858,#18859));
#3824=EDGE_LOOP('',(#18860,#18861,#18862,#18863));
#3825=EDGE_LOOP('',(#18864,#18865,#18866,#18867));
#3826=EDGE_LOOP('',(#18868,#18869,#18870,#18871));
#3827=EDGE_LOOP('',(#18872,#18873,#18874,#18875));
#3828=EDGE_LOOP('',(#18876,#18877,#18878,#18879));
#3829=EDGE_LOOP('',(#18880,#18881,#18882,#18883));
#3830=EDGE_LOOP('',(#18884,#18885,#18886,#18887));
#3831=EDGE_LOOP('',(#18888,#18889,#18890,#18891));
#3832=EDGE_LOOP('',(#18892,#18893,#18894,#18895));
#3833=EDGE_LOOP('',(#18896,#18897,#18898,#18899));
#3834=EDGE_LOOP('',(#18900,#18901,#18902,#18903));
#3835=EDGE_LOOP('',(#18904,#18905,#18906,#18907));
#3836=EDGE_LOOP('',(#18908,#18909,#18910,#18911));
#3837=EDGE_LOOP('',(#18912,#18913,#18914,#18915));
#3838=EDGE_LOOP('',(#18916,#18917,#18918,#18919));
#3839=EDGE_LOOP('',(#18920,#18921,#18922,#18923));
#3840=EDGE_LOOP('',(#18924,#18925,#18926,#18927));
#3841=EDGE_LOOP('',(#18928,#18929,#18930,#18931));
#3842=EDGE_LOOP('',(#18932,#18933,#18934,#18935));
#3843=EDGE_LOOP('',(#18936,#18937,#18938,#18939));
#3844=EDGE_LOOP('',(#18940,#18941,#18942,#18943));
#3845=EDGE_LOOP('',(#18944,#18945,#18946,#18947));
#3846=EDGE_LOOP('',(#18948,#18949,#18950,#18951));
#3847=EDGE_LOOP('',(#18952,#18953,#18954,#18955));
#3848=EDGE_LOOP('',(#18956,#18957,#18958,#18959));
#3849=EDGE_LOOP('',(#18960,#18961,#18962,#18963));
#3850=EDGE_LOOP('',(#18964,#18965,#18966,#18967));
#3851=EDGE_LOOP('',(#18968,#18969,#18970,#18971));
#3852=EDGE_LOOP('',(#18972,#18973,#18974,#18975));
#3853=EDGE_LOOP('',(#18976,#18977,#18978,#18979));
#3854=EDGE_LOOP('',(#18980,#18981,#18982,#18983));
#3855=EDGE_LOOP('',(#18984,#18985,#18986,#18987));
#3856=EDGE_LOOP('',(#18988,#18989,#18990,#18991));
#3857=EDGE_LOOP('',(#18992,#18993,#18994,#18995));
#3858=EDGE_LOOP('',(#18996,#18997,#18998,#18999));
#3859=EDGE_LOOP('',(#19000,#19001,#19002,#19003));
#3860=EDGE_LOOP('',(#19004,#19005,#19006,#19007));
#3861=EDGE_LOOP('',(#19008,#19009,#19010,#19011));
#3862=EDGE_LOOP('',(#19012,#19013,#19014,#19015));
#3863=EDGE_LOOP('',(#19016,#19017,#19018,#19019));
#3864=EDGE_LOOP('',(#19020,#19021,#19022,#19023));
#3865=EDGE_LOOP('',(#19024,#19025,#19026,#19027));
#3866=EDGE_LOOP('',(#19028,#19029,#19030,#19031));
#3867=EDGE_LOOP('',(#19032,#19033,#19034,#19035));
#3868=EDGE_LOOP('',(#19036,#19037,#19038,#19039));
#3869=EDGE_LOOP('',(#19040,#19041,#19042,#19043));
#3870=EDGE_LOOP('',(#19044,#19045,#19046,#19047));
#3871=EDGE_LOOP('',(#19048,#19049,#19050,#19051));
#3872=EDGE_LOOP('',(#19052,#19053,#19054,#19055));
#3873=EDGE_LOOP('',(#19056,#19057,#19058,#19059));
#3874=EDGE_LOOP('',(#19060,#19061,#19062,#19063));
#3875=EDGE_LOOP('',(#19064,#19065,#19066,#19067));
#3876=EDGE_LOOP('',(#19068,#19069,#19070,#19071));
#3877=EDGE_LOOP('',(#19072,#19073,#19074,#19075));
#3878=EDGE_LOOP('',(#19076,#19077,#19078,#19079));
#3879=EDGE_LOOP('',(#19080,#19081,#19082,#19083));
#3880=EDGE_LOOP('',(#19084,#19085,#19086,#19087));
#3881=EDGE_LOOP('',(#19088,#19089,#19090,#19091));
#3882=EDGE_LOOP('',(#19092,#19093,#19094,#19095));
#3883=EDGE_LOOP('',(#19096,#19097,#19098,#19099));
#3884=EDGE_LOOP('',(#19100,#19101,#19102,#19103));
#3885=EDGE_LOOP('',(#19104,#19105,#19106,#19107));
#3886=EDGE_LOOP('',(#19108,#19109,#19110,#19111));
#3887=EDGE_LOOP('',(#19112,#19113,#19114,#19115));
#3888=EDGE_LOOP('',(#19116,#19117,#19118,#19119));
#3889=EDGE_LOOP('',(#19120,#19121,#19122,#19123));
#3890=EDGE_LOOP('',(#19124,#19125,#19126,#19127));
#3891=EDGE_LOOP('',(#19128,#19129,#19130,#19131));
#3892=EDGE_LOOP('',(#19132,#19133,#19134,#19135));
#3893=EDGE_LOOP('',(#19136,#19137,#19138,#19139));
#3894=EDGE_LOOP('',(#19140,#19141,#19142,#19143));
#3895=EDGE_LOOP('',(#19144,#19145,#19146,#19147));
#3896=EDGE_LOOP('',(#19148,#19149,#19150,#19151));
#3897=EDGE_LOOP('',(#19152,#19153,#19154,#19155));
#3898=EDGE_LOOP('',(#19156,#19157,#19158,#19159));
#3899=EDGE_LOOP('',(#19160,#19161,#19162,#19163));
#3900=EDGE_LOOP('',(#19164,#19165,#19166,#19167));
#3901=EDGE_LOOP('',(#19168,#19169,#19170,#19171));
#3902=EDGE_LOOP('',(#19172,#19173,#19174,#19175));
#3903=EDGE_LOOP('',(#19176,#19177,#19178,#19179));
#3904=EDGE_LOOP('',(#19180,#19181,#19182,#19183));
#3905=EDGE_LOOP('',(#19184,#19185,#19186,#19187));
#3906=EDGE_LOOP('',(#19188,#19189,#19190,#19191));
#3907=EDGE_LOOP('',(#19192,#19193,#19194,#19195));
#3908=EDGE_LOOP('',(#19196,#19197,#19198,#19199));
#3909=EDGE_LOOP('',(#19200,#19201,#19202,#19203));
#3910=EDGE_LOOP('',(#19204,#19205,#19206,#19207));
#3911=EDGE_LOOP('',(#19208,#19209,#19210,#19211));
#3912=EDGE_LOOP('',(#19212,#19213,#19214,#19215));
#3913=EDGE_LOOP('',(#19216,#19217,#19218,#19219));
#3914=EDGE_LOOP('',(#19220,#19221,#19222,#19223));
#3915=EDGE_LOOP('',(#19224,#19225,#19226,#19227));
#3916=EDGE_LOOP('',(#19228,#19229,#19230,#19231));
#3917=EDGE_LOOP('',(#19232,#19233,#19234,#19235));
#3918=EDGE_LOOP('',(#19236,#19237,#19238,#19239));
#3919=EDGE_LOOP('',(#19240,#19241,#19242,#19243));
#3920=EDGE_LOOP('',(#19244,#19245,#19246,#19247));
#3921=EDGE_LOOP('',(#19248,#19249,#19250,#19251));
#3922=EDGE_LOOP('',(#19252));
#3923=EDGE_LOOP('',(#19253,#19254,#19255,#19256,#19257,#19258,#19259,#19260,
#19261,#19262,#19263,#19264,#19265,#19266,#19267,#19268,#19269,#19270,#19271,
#19272,#19273,#19274,#19275,#19276,#19277,#19278,#19279,#19280,#19281,#19282,
#19283,#19284,#19285,#19286,#19287,#19288,#19289,#19290,#19291,#19292,#19293,
#19294,#19295,#19296,#19297,#19298,#19299,#19300,#19301,#19302,#19303,#19304,
#19305,#19306,#19307,#19308,#19309,#19310,#19311,#19312,#19313,#19314,#19315,
#19316,#19317,#19318,#19319,#19320,#19321,#19322,#19323,#19324,#19325,#19326,
#19327,#19328,#19329,#19330,#19331,#19332,#19333,#19334,#19335,#19336,#19337,
#19338,#19339,#19340,#19341,#19342,#19343,#19344,#19345,#19346,#19347,#19348,
#19349,#19350,#19351,#19352,#19353,#19354,#19355,#19356,#19357,#19358,#19359,
#19360,#19361,#19362,#19363,#19364,#19365,#19366,#19367,#19368,#19369,#19370,
#19371,#19372,#19373,#19374,#19375,#19376,#19377,#19378,#19379,#19380,#19381,
#19382,#19383,#19384,#19385,#19386,#19387,#19388,#19389,#19390,#19391,#19392,
#19393,#19394,#19395,#19396,#19397,#19398,#19399,#19400,#19401,#19402,#19403,
#19404,#19405,#19406,#19407,#19408,#19409,#19410,#19411,#19412,#19413,#19414,
#19415,#19416,#19417,#19418,#19419,#19420,#19421,#19422,#19423,#19424,#19425,
#19426,#19427,#19428,#19429,#19430,#19431,#19432,#19433,#19434,#19435,#19436,
#19437,#19438,#19439,#19440,#19441,#19442,#19443,#19444,#19445,#19446,#19447,
#19448,#19449,#19450,#19451,#19452,#19453,#19454,#19455,#19456,#19457,#19458,
#19459,#19460,#19461,#19462,#19463,#19464,#19465,#19466,#19467,#19468,#19469,
#19470,#19471,#19472,#19473,#19474,#19475,#19476,#19477,#19478,#19479,#19480,
#19481,#19482,#19483,#19484,#19485,#19486,#19487,#19488,#19489,#19490,#19491,
#19492,#19493,#19494,#19495,#19496,#19497,#19498,#19499,#19500,#19501,#19502,
#19503,#19504,#19505,#19506,#19507,#19508,#19509,#19510,#19511,#19512,#19513,
#19514,#19515,#19516,#19517,#19518,#19519,#19520,#19521,#19522,#19523,#19524,
#19525,#19526,#19527,#19528,#19529,#19530,#19531,#19532,#19533,#19534,#19535,
#19536,#19537,#19538,#19539,#19540,#19541,#19542,#19543,#19544,#19545,#19546,
#19547,#19548,#19549,#19550,#19551,#19552,#19553,#19554,#19555,#19556,#19557,
#19558,#19559,#19560,#19561,#19562,#19563,#19564,#19565,#19566,#19567,#19568,
#19569,#19570,#19571,#19572,#19573,#19574,#19575,#19576,#19577,#19578,#19579,
#19580,#19581,#19582,#19583,#19584,#19585,#19586,#19587,#19588,#19589,#19590,
#19591,#19592,#19593,#19594,#19595,#19596,#19597,#19598,#19599,#19600,#19601,
#19602,#19603,#19604,#19605,#19606,#19607,#19608,#19609,#19610,#19611,#19612,
#19613,#19614,#19615,#19616,#19617,#19618,#19619,#19620,#19621,#19622,#19623,
#19624,#19625,#19626,#19627,#19628,#19629,#19630,#19631,#19632,#19633,#19634,
#19635,#19636,#19637,#19638,#19639,#19640,#19641,#19642,#19643,#19644,#19645,
#19646,#19647,#19648,#19649,#19650,#19651,#19652,#19653,#19654,#19655,#19656,
#19657,#19658,#19659,#19660,#19661,#19662,#19663,#19664,#19665,#19666,#19667,
#19668,#19669,#19670,#19671,#19672,#19673,#19674,#19675,#19676,#19677,#19678,
#19679,#19680,#19681,#19682,#19683,#19684));
#3924=EDGE_LOOP('',(#19685,#19686,#19687,#19688));
#3925=EDGE_LOOP('',(#19689,#19690,#19691,#19692,#19693,#19694,#19695,#19696,
#19697));
#3926=EDGE_LOOP('',(#19698,#19699));
#3927=EDGE_LOOP('',(#19700,#19701));
#3928=EDGE_LOOP('',(#19702,#19703,#19704));
#3929=EDGE_LOOP('',(#19705));
#3930=EDGE_LOOP('',(#19706,#19707,#19708,#19709,#19710,#19711,#19712,#19713,
#19714,#19715,#19716,#19717,#19718,#19719,#19720,#19721,#19722,#19723,#19724,
#19725,#19726,#19727,#19728,#19729,#19730,#19731,#19732,#19733,#19734,#19735,
#19736,#19737,#19738,#19739,#19740,#19741,#19742,#19743,#19744,#19745,#19746,
#19747,#19748,#19749,#19750,#19751,#19752,#19753,#19754,#19755,#19756,#19757,
#19758,#19759,#19760,#19761,#19762,#19763,#19764,#19765,#19766,#19767,#19768,
#19769,#19770,#19771,#19772,#19773,#19774,#19775,#19776,#19777,#19778,#19779,
#19780,#19781,#19782,#19783,#19784,#19785,#19786,#19787,#19788,#19789,#19790,
#19791,#19792,#19793,#19794,#19795,#19796,#19797,#19798,#19799,#19800,#19801,
#19802,#19803,#19804,#19805,#19806,#19807,#19808,#19809,#19810,#19811,#19812,
#19813,#19814,#19815,#19816,#19817,#19818,#19819,#19820,#19821,#19822,#19823,
#19824,#19825,#19826,#19827,#19828,#19829,#19830,#19831,#19832,#19833,#19834,
#19835,#19836,#19837,#19838,#19839,#19840,#19841,#19842,#19843,#19844,#19845,
#19846,#19847,#19848,#19849,#19850,#19851,#19852,#19853,#19854,#19855,#19856,
#19857,#19858,#19859,#19860,#19861,#19862,#19863,#19864,#19865,#19866,#19867,
#19868,#19869,#19870,#19871,#19872,#19873,#19874,#19875,#19876,#19877,#19878,
#19879,#19880,#19881,#19882,#19883,#19884,#19885,#19886,#19887,#19888,#19889,
#19890,#19891,#19892,#19893,#19894,#19895,#19896,#19897,#19898,#19899,#19900,
#19901,#19902,#19903,#19904,#19905,#19906,#19907,#19908,#19909,#19910,#19911,
#19912,#19913,#19914,#19915,#19916,#19917,#19918,#19919,#19920,#19921,#19922,
#19923,#19924,#19925,#19926,#19927,#19928,#19929,#19930,#19931,#19932,#19933,
#19934,#19935,#19936,#19937,#19938,#19939,#19940,#19941,#19942,#19943,#19944,
#19945,#19946,#19947,#19948,#19949,#19950,#19951,#19952,#19953,#19954,#19955,
#19956,#19957,#19958,#19959,#19960,#19961,#19962,#19963,#19964,#19965,#19966,
#19967,#19968,#19969,#19970,#19971,#19972,#19973,#19974,#19975,#19976,#19977,
#19978,#19979,#19980,#19981,#19982,#19983,#19984,#19985,#19986,#19987,#19988,
#19989,#19990,#19991,#19992,#19993,#19994,#19995,#19996,#19997,#19998,#19999,
#20000,#20001,#20002,#20003,#20004,#20005,#20006,#20007,#20008,#20009,#20010,
#20011,#20012,#20013,#20014,#20015,#20016,#20017,#20018,#20019,#20020,#20021,
#20022,#20023,#20024,#20025,#20026,#20027,#20028,#20029,#20030,#20031,#20032,
#20033,#20034,#20035,#20036,#20037,#20038,#20039,#20040,#20041,#20042,#20043,
#20044,#20045,#20046,#20047,#20048,#20049,#20050,#20051,#20052,#20053,#20054,
#20055,#20056,#20057,#20058,#20059,#20060,#20061,#20062,#20063,#20064,#20065,
#20066,#20067,#20068,#20069,#20070,#20071,#20072,#20073,#20074,#20075,#20076,
#20077,#20078,#20079,#20080,#20081,#20082,#20083,#20084,#20085,#20086,#20087,
#20088,#20089,#20090,#20091,#20092,#20093,#20094,#20095,#20096,#20097,#20098,
#20099,#20100,#20101,#20102,#20103,#20104,#20105,#20106,#20107,#20108,#20109,
#20110,#20111,#20112,#20113,#20114,#20115,#20116,#20117,#20118,#20119,#20120,
#20121,#20122,#20123,#20124,#20125,#20126,#20127,#20128,#20129,#20130,#20131,
#20132,#20133,#20134,#20135,#20136,#20137));
#3931=EDGE_LOOP('',(#20138,#20139,#20140,#20141));
#3932=EDGE_LOOP('',(#20142,#20143,#20144,#20145));
#3933=EDGE_LOOP('',(#20146,#20147,#20148,#20149));
#3934=EDGE_LOOP('',(#20150,#20151,#20152,#20153));
#3935=EDGE_LOOP('',(#20154,#20155,#20156,#20157,#20158,#20159,#20160,#20161,
#20162,#20163,#20164,#20165,#20166,#20167,#20168,#20169,#20170,#20171,#20172,
#20173,#20174,#20175,#20176,#20177,#20178,#20179,#20180,#20181,#20182,#20183,
#20184,#20185,#20186,#20187,#20188,#20189,#20190,#20191,#20192,#20193,#20194,
#20195,#20196,#20197,#20198,#20199,#20200,#20201,#20202,#20203,#20204,#20205,
#20206,#20207,#20208,#20209,#20210,#20211,#20212,#20213,#20214,#20215,#20216,
#20217,#20218,#20219,#20220,#20221,#20222,#20223,#20224,#20225,#20226,#20227,
#20228,#20229,#20230,#20231,#20232,#20233,#20234,#20235,#20236,#20237,#20238,
#20239,#20240,#20241,#20242,#20243,#20244,#20245,#20246,#20247,#20248,#20249,
#20250,#20251,#20252,#20253,#20254,#20255,#20256,#20257,#20258,#20259,#20260,
#20261,#20262,#20263,#20264,#20265,#20266,#20267,#20268,#20269,#20270,#20271,
#20272,#20273,#20274,#20275,#20276,#20277,#20278,#20279,#20280,#20281,#20282,
#20283,#20284,#20285,#20286,#20287,#20288,#20289,#20290,#20291,#20292,#20293,
#20294,#20295,#20296,#20297,#20298,#20299,#20300,#20301,#20302,#20303,#20304,
#20305,#20306,#20307,#20308,#20309,#20310,#20311,#20312,#20313,#20314,#20315,
#20316,#20317,#20318,#20319,#20320,#20321,#20322,#20323,#20324,#20325,#20326,
#20327,#20328,#20329,#20330,#20331,#20332,#20333,#20334,#20335,#20336,#20337,
#20338,#20339,#20340,#20341,#20342,#20343,#20344,#20345));
#3936=EDGE_LOOP('',(#20346,#20347,#20348,#20349));
#3937=EDGE_LOOP('',(#20350,#20351,#20352,#20353));
#3938=EDGE_LOOP('',(#20354,#20355,#20356,#20357));
#3939=EDGE_LOOP('',(#20358,#20359,#20360,#20361));
#3940=EDGE_LOOP('',(#20362,#20363,#20364,#20365));
#3941=EDGE_LOOP('',(#20366,#20367,#20368,#20369));
#3942=EDGE_LOOP('',(#20370,#20371,#20372,#20373));
#3943=EDGE_LOOP('',(#20374,#20375,#20376,#20377));
#3944=EDGE_LOOP('',(#20378,#20379,#20380,#20381));
#3945=EDGE_LOOP('',(#20382,#20383,#20384,#20385));
#3946=EDGE_LOOP('',(#20386,#20387,#20388,#20389));
#3947=EDGE_LOOP('',(#20390,#20391,#20392,#20393));
#3948=EDGE_LOOP('',(#20394,#20395,#20396,#20397));
#3949=EDGE_LOOP('',(#20398,#20399,#20400,#20401));
#3950=EDGE_LOOP('',(#20402,#20403,#20404,#20405));
#3951=EDGE_LOOP('',(#20406,#20407,#20408,#20409));
#3952=EDGE_LOOP('',(#20410,#20411,#20412,#20413));
#3953=EDGE_LOOP('',(#20414,#20415,#20416,#20417));
#3954=EDGE_LOOP('',(#20418,#20419,#20420,#20421));
#3955=EDGE_LOOP('',(#20422,#20423,#20424,#20425));
#3956=EDGE_LOOP('',(#20426,#20427,#20428,#20429));
#3957=EDGE_LOOP('',(#20430,#20431,#20432,#20433));
#3958=EDGE_LOOP('',(#20434,#20435,#20436,#20437));
#3959=EDGE_LOOP('',(#20438,#20439,#20440,#20441));
#3960=EDGE_LOOP('',(#20442,#20443,#20444,#20445));
#3961=EDGE_LOOP('',(#20446,#20447,#20448,#20449));
#3962=EDGE_LOOP('',(#20450,#20451,#20452,#20453));
#3963=EDGE_LOOP('',(#20454,#20455,#20456,#20457));
#3964=EDGE_LOOP('',(#20458,#20459,#20460,#20461));
#3965=EDGE_LOOP('',(#20462,#20463,#20464,#20465));
#3966=EDGE_LOOP('',(#20466,#20467,#20468,#20469));
#3967=EDGE_LOOP('',(#20470,#20471,#20472,#20473));
#3968=EDGE_LOOP('',(#20474,#20475,#20476,#20477));
#3969=EDGE_LOOP('',(#20478,#20479,#20480,#20481));
#3970=EDGE_LOOP('',(#20482,#20483,#20484,#20485));
#3971=EDGE_LOOP('',(#20486,#20487,#20488,#20489));
#3972=EDGE_LOOP('',(#20490,#20491,#20492,#20493));
#3973=EDGE_LOOP('',(#20494,#20495,#20496,#20497));
#3974=EDGE_LOOP('',(#20498,#20499,#20500,#20501));
#3975=EDGE_LOOP('',(#20502,#20503,#20504,#20505));
#3976=EDGE_LOOP('',(#20506,#20507,#20508,#20509));
#3977=EDGE_LOOP('',(#20510,#20511,#20512,#20513));
#3978=EDGE_LOOP('',(#20514,#20515,#20516,#20517));
#3979=EDGE_LOOP('',(#20518,#20519,#20520,#20521));
#3980=EDGE_LOOP('',(#20522,#20523,#20524,#20525));
#3981=EDGE_LOOP('',(#20526,#20527,#20528,#20529));
#3982=EDGE_LOOP('',(#20530,#20531,#20532,#20533));
#3983=EDGE_LOOP('',(#20534,#20535,#20536,#20537));
#3984=EDGE_LOOP('',(#20538,#20539,#20540,#20541));
#3985=EDGE_LOOP('',(#20542,#20543,#20544,#20545));
#3986=EDGE_LOOP('',(#20546,#20547,#20548,#20549));
#3987=EDGE_LOOP('',(#20550,#20551,#20552,#20553));
#3988=EDGE_LOOP('',(#20554,#20555,#20556,#20557));
#3989=EDGE_LOOP('',(#20558,#20559,#20560,#20561));
#3990=EDGE_LOOP('',(#20562,#20563,#20564,#20565));
#3991=EDGE_LOOP('',(#20566,#20567,#20568,#20569));
#3992=EDGE_LOOP('',(#20570,#20571,#20572,#20573));
#3993=EDGE_LOOP('',(#20574,#20575,#20576,#20577));
#3994=EDGE_LOOP('',(#20578,#20579,#20580,#20581));
#3995=EDGE_LOOP('',(#20582,#20583,#20584,#20585));
#3996=EDGE_LOOP('',(#20586,#20587,#20588,#20589));
#3997=EDGE_LOOP('',(#20590,#20591,#20592,#20593));
#3998=EDGE_LOOP('',(#20594,#20595,#20596,#20597));
#3999=EDGE_LOOP('',(#20598,#20599,#20600,#20601));
#4000=EDGE_LOOP('',(#20602,#20603,#20604,#20605));
#4001=EDGE_LOOP('',(#20606,#20607,#20608,#20609));
#4002=EDGE_LOOP('',(#20610,#20611,#20612,#20613));
#4003=EDGE_LOOP('',(#20614,#20615,#20616,#20617));
#4004=EDGE_LOOP('',(#20618,#20619,#20620,#20621));
#4005=EDGE_LOOP('',(#20622,#20623,#20624,#20625));
#4006=EDGE_LOOP('',(#20626,#20627,#20628,#20629));
#4007=EDGE_LOOP('',(#20630,#20631,#20632,#20633));
#4008=EDGE_LOOP('',(#20634,#20635,#20636,#20637));
#4009=EDGE_LOOP('',(#20638,#20639,#20640,#20641));
#4010=EDGE_LOOP('',(#20642,#20643,#20644,#20645));
#4011=EDGE_LOOP('',(#20646,#20647,#20648,#20649));
#4012=EDGE_LOOP('',(#20650,#20651,#20652,#20653));
#4013=EDGE_LOOP('',(#20654,#20655,#20656,#20657));
#4014=EDGE_LOOP('',(#20658,#20659,#20660,#20661));
#4015=EDGE_LOOP('',(#20662,#20663,#20664,#20665));
#4016=EDGE_LOOP('',(#20666,#20667,#20668,#20669));
#4017=EDGE_LOOP('',(#20670,#20671,#20672,#20673));
#4018=EDGE_LOOP('',(#20674,#20675,#20676,#20677));
#4019=EDGE_LOOP('',(#20678,#20679,#20680,#20681));
#4020=EDGE_LOOP('',(#20682,#20683,#20684,#20685));
#4021=EDGE_LOOP('',(#20686,#20687,#20688,#20689));
#4022=EDGE_LOOP('',(#20690,#20691,#20692,#20693));
#4023=EDGE_LOOP('',(#20694,#20695,#20696,#20697));
#4024=EDGE_LOOP('',(#20698,#20699,#20700,#20701));
#4025=EDGE_LOOP('',(#20702,#20703,#20704,#20705));
#4026=EDGE_LOOP('',(#20706,#20707,#20708,#20709));
#4027=EDGE_LOOP('',(#20710,#20711,#20712,#20713));
#4028=EDGE_LOOP('',(#20714,#20715,#20716,#20717));
#4029=EDGE_LOOP('',(#20718,#20719,#20720,#20721));
#4030=EDGE_LOOP('',(#20722,#20723,#20724,#20725));
#4031=EDGE_LOOP('',(#20726,#20727,#20728,#20729));
#4032=EDGE_LOOP('',(#20730,#20731,#20732,#20733));
#4033=EDGE_LOOP('',(#20734,#20735,#20736,#20737));
#4034=EDGE_LOOP('',(#20738,#20739,#20740,#20741));
#4035=EDGE_LOOP('',(#20742,#20743,#20744,#20745));
#4036=EDGE_LOOP('',(#20746,#20747,#20748,#20749));
#4037=EDGE_LOOP('',(#20750,#20751,#20752,#20753));
#4038=EDGE_LOOP('',(#20754,#20755,#20756,#20757));
#4039=EDGE_LOOP('',(#20758,#20759,#20760,#20761));
#4040=EDGE_LOOP('',(#20762,#20763,#20764,#20765));
#4041=EDGE_LOOP('',(#20766,#20767,#20768,#20769));
#4042=EDGE_LOOP('',(#20770,#20771,#20772,#20773));
#4043=EDGE_LOOP('',(#20774,#20775,#20776,#20777));
#4044=EDGE_LOOP('',(#20778,#20779,#20780,#20781));
#4045=EDGE_LOOP('',(#20782,#20783,#20784,#20785));
#4046=EDGE_LOOP('',(#20786,#20787,#20788,#20789));
#4047=EDGE_LOOP('',(#20790,#20791,#20792,#20793));
#4048=EDGE_LOOP('',(#20794,#20795,#20796,#20797));
#4049=EDGE_LOOP('',(#20798,#20799,#20800,#20801));
#4050=EDGE_LOOP('',(#20802,#20803,#20804,#20805));
#4051=EDGE_LOOP('',(#20806,#20807,#20808,#20809));
#4052=EDGE_LOOP('',(#20810,#20811,#20812,#20813));
#4053=EDGE_LOOP('',(#20814,#20815,#20816,#20817));
#4054=EDGE_LOOP('',(#20818,#20819,#20820,#20821));
#4055=EDGE_LOOP('',(#20822,#20823,#20824,#20825));
#4056=EDGE_LOOP('',(#20826,#20827,#20828,#20829));
#4057=EDGE_LOOP('',(#20830,#20831,#20832,#20833));
#4058=EDGE_LOOP('',(#20834,#20835,#20836,#20837));
#4059=EDGE_LOOP('',(#20838,#20839,#20840,#20841));
#4060=EDGE_LOOP('',(#20842,#20843,#20844,#20845));
#4061=EDGE_LOOP('',(#20846,#20847,#20848,#20849));
#4062=EDGE_LOOP('',(#20850,#20851,#20852,#20853));
#4063=EDGE_LOOP('',(#20854,#20855,#20856,#20857));
#4064=EDGE_LOOP('',(#20858,#20859,#20860,#20861));
#4065=EDGE_LOOP('',(#20862,#20863,#20864,#20865));
#4066=EDGE_LOOP('',(#20866,#20867,#20868,#20869));
#4067=EDGE_LOOP('',(#20870,#20871,#20872,#20873));
#4068=EDGE_LOOP('',(#20874,#20875,#20876,#20877));
#4069=EDGE_LOOP('',(#20878,#20879,#20880,#20881));
#4070=EDGE_LOOP('',(#20882,#20883,#20884,#20885));
#4071=EDGE_LOOP('',(#20886,#20887,#20888,#20889));
#4072=EDGE_LOOP('',(#20890,#20891,#20892,#20893));
#4073=EDGE_LOOP('',(#20894,#20895,#20896,#20897));
#4074=EDGE_LOOP('',(#20898,#20899,#20900,#20901));
#4075=EDGE_LOOP('',(#20902,#20903,#20904,#20905));
#4076=EDGE_LOOP('',(#20906,#20907,#20908,#20909));
#4077=EDGE_LOOP('',(#20910,#20911,#20912,#20913));
#4078=EDGE_LOOP('',(#20914,#20915,#20916,#20917));
#4079=EDGE_LOOP('',(#20918,#20919,#20920,#20921));
#4080=EDGE_LOOP('',(#20922,#20923,#20924,#20925));
#4081=EDGE_LOOP('',(#20926,#20927,#20928,#20929));
#4082=EDGE_LOOP('',(#20930,#20931,#20932,#20933));
#4083=EDGE_LOOP('',(#20934,#20935,#20936,#20937));
#4084=EDGE_LOOP('',(#20938,#20939,#20940,#20941));
#4085=EDGE_LOOP('',(#20942,#20943,#20944,#20945));
#4086=EDGE_LOOP('',(#20946,#20947,#20948,#20949));
#4087=EDGE_LOOP('',(#20950,#20951,#20952,#20953));
#4088=EDGE_LOOP('',(#20954,#20955,#20956,#20957));
#4089=EDGE_LOOP('',(#20958,#20959,#20960,#20961));
#4090=EDGE_LOOP('',(#20962,#20963,#20964,#20965));
#4091=EDGE_LOOP('',(#20966,#20967,#20968,#20969));
#4092=EDGE_LOOP('',(#20970,#20971,#20972,#20973));
#4093=EDGE_LOOP('',(#20974,#20975,#20976,#20977));
#4094=EDGE_LOOP('',(#20978,#20979,#20980,#20981));
#4095=EDGE_LOOP('',(#20982,#20983,#20984,#20985));
#4096=EDGE_LOOP('',(#20986,#20987,#20988,#20989));
#4097=EDGE_LOOP('',(#20990,#20991,#20992,#20993));
#4098=EDGE_LOOP('',(#20994,#20995,#20996,#20997,#20998,#20999,#21000,#21001,
#21002,#21003,#21004,#21005,#21006,#21007,#21008,#21009,#21010,#21011,#21012,
#21013,#21014,#21015,#21016,#21017,#21018,#21019,#21020,#21021,#21022,#21023,
#21024,#21025,#21026,#21027,#21028,#21029,#21030,#21031,#21032,#21033,#21034,
#21035,#21036,#21037,#21038,#21039,#21040,#21041,#21042,#21043,#21044,#21045,
#21046,#21047,#21048,#21049,#21050,#21051,#21052,#21053,#21054,#21055,#21056,
#21057,#21058,#21059,#21060,#21061,#21062,#21063,#21064,#21065,#21066,#21067,
#21068,#21069,#21070,#21071,#21072,#21073,#21074,#21075,#21076,#21077,#21078,
#21079,#21080,#21081,#21082,#21083,#21084,#21085,#21086,#21087,#21088,#21089,
#21090,#21091,#21092,#21093,#21094,#21095,#21096,#21097,#21098,#21099,#21100,
#21101,#21102,#21103,#21104,#21105,#21106,#21107,#21108,#21109,#21110,#21111,
#21112,#21113,#21114,#21115,#21116,#21117,#21118,#21119,#21120,#21121,#21122,
#21123,#21124,#21125,#21126,#21127,#21128,#21129,#21130,#21131,#21132,#21133,
#21134,#21135,#21136,#21137,#21138,#21139,#21140,#21141,#21142,#21143,#21144,
#21145,#21146,#21147,#21148,#21149,#21150,#21151,#21152,#21153,#21154,#21155,
#21156,#21157,#21158,#21159,#21160,#21161,#21162,#21163,#21164,#21165,#21166,
#21167,#21168,#21169,#21170,#21171,#21172,#21173,#21174,#21175,#21176,#21177,
#21178,#21179,#21180,#21181,#21182,#21183,#21184,#21185));
#4099=EDGE_LOOP('',(#21186,#21187,#21188,#21189));
#4100=EDGE_LOOP('',(#21190,#21191,#21192,#21193));
#4101=EDGE_LOOP('',(#21194,#21195,#21196,#21197));
#4102=EDGE_LOOP('',(#21198,#21199,#21200,#21201));
#4103=EDGE_LOOP('',(#21202,#21203,#21204,#21205));
#4104=EDGE_LOOP('',(#21206,#21207,#21208,#21209));
#4105=EDGE_LOOP('',(#21210,#21211,#21212,#21213));
#4106=EDGE_LOOP('',(#21214,#21215,#21216,#21217));
#4107=EDGE_LOOP('',(#21218,#21219,#21220,#21221));
#4108=EDGE_LOOP('',(#21222,#21223,#21224,#21225));
#4109=EDGE_LOOP('',(#21226,#21227,#21228,#21229));
#4110=EDGE_LOOP('',(#21230,#21231,#21232,#21233));
#4111=EDGE_LOOP('',(#21234,#21235,#21236,#21237));
#4112=EDGE_LOOP('',(#21238,#21239,#21240,#21241));
#4113=EDGE_LOOP('',(#21242,#21243,#21244,#21245));
#4114=EDGE_LOOP('',(#21246,#21247,#21248,#21249));
#4115=EDGE_LOOP('',(#21250,#21251,#21252,#21253));
#4116=EDGE_LOOP('',(#21254,#21255,#21256,#21257));
#4117=EDGE_LOOP('',(#21258,#21259,#21260,#21261));
#4118=EDGE_LOOP('',(#21262,#21263,#21264,#21265));
#4119=EDGE_LOOP('',(#21266,#21267,#21268,#21269));
#4120=EDGE_LOOP('',(#21270,#21271,#21272,#21273));
#4121=EDGE_LOOP('',(#21274,#21275,#21276,#21277));
#4122=EDGE_LOOP('',(#21278,#21279,#21280,#21281));
#4123=EDGE_LOOP('',(#21282,#21283,#21284,#21285));
#4124=EDGE_LOOP('',(#21286,#21287,#21288,#21289));
#4125=EDGE_LOOP('',(#21290,#21291,#21292,#21293));
#4126=EDGE_LOOP('',(#21294,#21295,#21296,#21297));
#4127=EDGE_LOOP('',(#21298,#21299,#21300,#21301));
#4128=EDGE_LOOP('',(#21302,#21303,#21304,#21305));
#4129=EDGE_LOOP('',(#21306,#21307,#21308,#21309));
#4130=EDGE_LOOP('',(#21310,#21311,#21312,#21313));
#4131=EDGE_LOOP('',(#21314,#21315,#21316,#21317));
#4132=EDGE_LOOP('',(#21318,#21319,#21320,#21321));
#4133=EDGE_LOOP('',(#21322,#21323,#21324,#21325));
#4134=EDGE_LOOP('',(#21326,#21327,#21328,#21329));
#4135=EDGE_LOOP('',(#21330,#21331,#21332,#21333));
#4136=EDGE_LOOP('',(#21334,#21335,#21336,#21337));
#4137=EDGE_LOOP('',(#21338,#21339,#21340,#21341));
#4138=EDGE_LOOP('',(#21342,#21343,#21344,#21345));
#4139=EDGE_LOOP('',(#21346,#21347,#21348,#21349));
#4140=EDGE_LOOP('',(#21350,#21351,#21352,#21353));
#4141=EDGE_LOOP('',(#21354,#21355,#21356,#21357));
#4142=EDGE_LOOP('',(#21358,#21359,#21360,#21361));
#4143=EDGE_LOOP('',(#21362,#21363,#21364,#21365));
#4144=EDGE_LOOP('',(#21366,#21367,#21368,#21369));
#4145=EDGE_LOOP('',(#21370,#21371,#21372,#21373));
#4146=EDGE_LOOP('',(#21374,#21375,#21376,#21377));
#4147=EDGE_LOOP('',(#21378,#21379,#21380,#21381));
#4148=EDGE_LOOP('',(#21382,#21383,#21384,#21385));
#4149=EDGE_LOOP('',(#21386,#21387,#21388,#21389));
#4150=EDGE_LOOP('',(#21390,#21391,#21392,#21393));
#4151=EDGE_LOOP('',(#21394,#21395,#21396,#21397));
#4152=EDGE_LOOP('',(#21398,#21399,#21400,#21401));
#4153=EDGE_LOOP('',(#21402,#21403,#21404,#21405));
#4154=EDGE_LOOP('',(#21406,#21407,#21408,#21409));
#4155=EDGE_LOOP('',(#21410,#21411,#21412,#21413));
#4156=EDGE_LOOP('',(#21414,#21415,#21416,#21417));
#4157=EDGE_LOOP('',(#21418,#21419,#21420,#21421));
#4158=EDGE_LOOP('',(#21422,#21423,#21424,#21425));
#4159=EDGE_LOOP('',(#21426,#21427,#21428,#21429));
#4160=EDGE_LOOP('',(#21430,#21431,#21432,#21433));
#4161=EDGE_LOOP('',(#21434,#21435,#21436,#21437));
#4162=EDGE_LOOP('',(#21438,#21439,#21440,#21441));
#4163=EDGE_LOOP('',(#21442,#21443,#21444,#21445));
#4164=EDGE_LOOP('',(#21446,#21447,#21448,#21449));
#4165=EDGE_LOOP('',(#21450,#21451,#21452,#21453));
#4166=EDGE_LOOP('',(#21454,#21455,#21456,#21457));
#4167=EDGE_LOOP('',(#21458,#21459,#21460,#21461));
#4168=EDGE_LOOP('',(#21462,#21463,#21464,#21465));
#4169=EDGE_LOOP('',(#21466,#21467,#21468,#21469));
#4170=EDGE_LOOP('',(#21470,#21471,#21472,#21473));
#4171=EDGE_LOOP('',(#21474,#21475,#21476,#21477));
#4172=EDGE_LOOP('',(#21478,#21479,#21480,#21481));
#4173=EDGE_LOOP('',(#21482,#21483,#21484,#21485));
#4174=EDGE_LOOP('',(#21486,#21487,#21488,#21489));
#4175=EDGE_LOOP('',(#21490,#21491,#21492,#21493));
#4176=EDGE_LOOP('',(#21494,#21495,#21496,#21497));
#4177=EDGE_LOOP('',(#21498,#21499,#21500,#21501));
#4178=EDGE_LOOP('',(#21502,#21503,#21504,#21505));
#4179=EDGE_LOOP('',(#21506,#21507,#21508,#21509));
#4180=EDGE_LOOP('',(#21510,#21511,#21512,#21513));
#4181=EDGE_LOOP('',(#21514,#21515,#21516,#21517));
#4182=EDGE_LOOP('',(#21518,#21519,#21520,#21521));
#4183=EDGE_LOOP('',(#21522,#21523,#21524,#21525));
#4184=EDGE_LOOP('',(#21526,#21527,#21528,#21529));
#4185=EDGE_LOOP('',(#21530,#21531,#21532,#21533));
#4186=EDGE_LOOP('',(#21534,#21535,#21536,#21537));
#4187=EDGE_LOOP('',(#21538,#21539,#21540,#21541));
#4188=EDGE_LOOP('',(#21542,#21543,#21544,#21545));
#4189=EDGE_LOOP('',(#21546,#21547,#21548,#21549));
#4190=EDGE_LOOP('',(#21550,#21551,#21552,#21553));
#4191=EDGE_LOOP('',(#21554,#21555,#21556,#21557));
#4192=EDGE_LOOP('',(#21558,#21559,#21560,#21561));
#4193=EDGE_LOOP('',(#21562,#21563,#21564,#21565));
#4194=EDGE_LOOP('',(#21566,#21567,#21568,#21569));
#4195=EDGE_LOOP('',(#21570,#21571,#21572,#21573));
#4196=EDGE_LOOP('',(#21574,#21575,#21576,#21577));
#4197=EDGE_LOOP('',(#21578,#21579,#21580,#21581));
#4198=EDGE_LOOP('',(#21582,#21583,#21584,#21585));
#4199=EDGE_LOOP('',(#21586,#21587,#21588,#21589));
#4200=EDGE_LOOP('',(#21590,#21591,#21592,#21593));
#4201=EDGE_LOOP('',(#21594,#21595,#21596,#21597));
#4202=EDGE_LOOP('',(#21598,#21599,#21600,#21601));
#4203=EDGE_LOOP('',(#21602,#21603,#21604,#21605));
#4204=EDGE_LOOP('',(#21606,#21607,#21608,#21609));
#4205=EDGE_LOOP('',(#21610,#21611,#21612,#21613));
#4206=EDGE_LOOP('',(#21614,#21615,#21616,#21617));
#4207=EDGE_LOOP('',(#21618,#21619,#21620,#21621));
#4208=EDGE_LOOP('',(#21622,#21623,#21624,#21625));
#4209=EDGE_LOOP('',(#21626,#21627,#21628,#21629));
#4210=EDGE_LOOP('',(#21630,#21631,#21632,#21633));
#4211=EDGE_LOOP('',(#21634,#21635,#21636,#21637));
#4212=EDGE_LOOP('',(#21638,#21639,#21640,#21641));
#4213=EDGE_LOOP('',(#21642,#21643,#21644,#21645));
#4214=EDGE_LOOP('',(#21646,#21647,#21648,#21649));
#4215=EDGE_LOOP('',(#21650,#21651,#21652,#21653));
#4216=EDGE_LOOP('',(#21654,#21655,#21656,#21657));
#4217=EDGE_LOOP('',(#21658,#21659,#21660,#21661));
#4218=EDGE_LOOP('',(#21662,#21663,#21664,#21665));
#4219=EDGE_LOOP('',(#21666,#21667,#21668,#21669));
#4220=EDGE_LOOP('',(#21670,#21671,#21672,#21673));
#4221=EDGE_LOOP('',(#21674,#21675,#21676,#21677));
#4222=EDGE_LOOP('',(#21678,#21679,#21680,#21681));
#4223=EDGE_LOOP('',(#21682,#21683,#21684,#21685));
#4224=EDGE_LOOP('',(#21686,#21687,#21688,#21689));
#4225=EDGE_LOOP('',(#21690,#21691,#21692,#21693));
#4226=EDGE_LOOP('',(#21694,#21695,#21696,#21697));
#4227=EDGE_LOOP('',(#21698,#21699,#21700,#21701));
#4228=EDGE_LOOP('',(#21702,#21703,#21704,#21705));
#4229=EDGE_LOOP('',(#21706,#21707,#21708,#21709));
#4230=EDGE_LOOP('',(#21710,#21711,#21712,#21713));
#4231=EDGE_LOOP('',(#21714,#21715,#21716,#21717));
#4232=EDGE_LOOP('',(#21718,#21719,#21720,#21721));
#4233=EDGE_LOOP('',(#21722,#21723,#21724,#21725));
#4234=EDGE_LOOP('',(#21726,#21727,#21728,#21729));
#4235=EDGE_LOOP('',(#21730,#21731,#21732,#21733));
#4236=EDGE_LOOP('',(#21734,#21735,#21736,#21737));
#4237=EDGE_LOOP('',(#21738,#21739,#21740,#21741));
#4238=EDGE_LOOP('',(#21742,#21743,#21744,#21745));
#4239=EDGE_LOOP('',(#21746,#21747,#21748,#21749));
#4240=EDGE_LOOP('',(#21750,#21751,#21752,#21753));
#4241=EDGE_LOOP('',(#21754,#21755,#21756,#21757));
#4242=EDGE_LOOP('',(#21758,#21759,#21760,#21761));
#4243=EDGE_LOOP('',(#21762,#21763,#21764,#21765));
#4244=EDGE_LOOP('',(#21766,#21767,#21768,#21769));
#4245=EDGE_LOOP('',(#21770,#21771,#21772,#21773));
#4246=EDGE_LOOP('',(#21774,#21775,#21776,#21777));
#4247=EDGE_LOOP('',(#21778,#21779,#21780,#21781));
#4248=EDGE_LOOP('',(#21782,#21783,#21784,#21785));
#4249=EDGE_LOOP('',(#21786,#21787,#21788,#21789));
#4250=EDGE_LOOP('',(#21790,#21791,#21792,#21793));
#4251=EDGE_LOOP('',(#21794,#21795,#21796,#21797));
#4252=EDGE_LOOP('',(#21798,#21799,#21800,#21801));
#4253=EDGE_LOOP('',(#21802,#21803,#21804,#21805));
#4254=EDGE_LOOP('',(#21806,#21807,#21808,#21809));
#4255=EDGE_LOOP('',(#21810,#21811,#21812,#21813));
#4256=EDGE_LOOP('',(#21814,#21815,#21816,#21817));
#4257=EDGE_LOOP('',(#21818,#21819,#21820,#21821));
#4258=EDGE_LOOP('',(#21822,#21823,#21824,#21825));
#4259=EDGE_LOOP('',(#21826,#21827,#21828,#21829));
#4260=EDGE_LOOP('',(#21830,#21831,#21832,#21833));
#4261=EDGE_LOOP('',(#21834,#21835,#21836,#21837));
#4262=EDGE_LOOP('',(#21838,#21839,#21840,#21841));
#4263=EDGE_LOOP('',(#21842,#21843,#21844,#21845));
#4264=EDGE_LOOP('',(#21846,#21847,#21848,#21849));
#4265=EDGE_LOOP('',(#21850,#21851,#21852,#21853));
#4266=EDGE_LOOP('',(#21854,#21855,#21856,#21857));
#4267=EDGE_LOOP('',(#21858,#21859,#21860,#21861));
#4268=EDGE_LOOP('',(#21862,#21863,#21864,#21865));
#4269=EDGE_LOOP('',(#21866,#21867,#21868,#21869));
#4270=EDGE_LOOP('',(#21870,#21871,#21872,#21873));
#4271=EDGE_LOOP('',(#21874,#21875,#21876,#21877));
#4272=EDGE_LOOP('',(#21878,#21879,#21880,#21881));
#4273=EDGE_LOOP('',(#21882,#21883,#21884,#21885));
#4274=EDGE_LOOP('',(#21886,#21887,#21888,#21889));
#4275=EDGE_LOOP('',(#21890,#21891,#21892,#21893));
#4276=EDGE_LOOP('',(#21894,#21895,#21896,#21897));
#4277=EDGE_LOOP('',(#21898,#21899,#21900,#21901));
#4278=EDGE_LOOP('',(#21902,#21903,#21904,#21905));
#4279=EDGE_LOOP('',(#21906,#21907,#21908,#21909));
#4280=EDGE_LOOP('',(#21910,#21911,#21912,#21913));
#4281=EDGE_LOOP('',(#21914,#21915,#21916,#21917));
#4282=EDGE_LOOP('',(#21918,#21919,#21920,#21921));
#4283=EDGE_LOOP('',(#21922,#21923,#21924,#21925));
#4284=EDGE_LOOP('',(#21926,#21927,#21928,#21929));
#4285=EDGE_LOOP('',(#21930,#21931,#21932,#21933));
#4286=EDGE_LOOP('',(#21934,#21935,#21936,#21937));
#4287=EDGE_LOOP('',(#21938,#21939,#21940,#21941));
#4288=EDGE_LOOP('',(#21942,#21943,#21944,#21945));
#4289=EDGE_LOOP('',(#21946,#21947,#21948,#21949));
#4290=EDGE_LOOP('',(#21950,#21951,#21952,#21953));
#4291=EDGE_LOOP('',(#21954,#21955,#21956,#21957));
#4292=EDGE_LOOP('',(#21958,#21959,#21960,#21961,#21962,#21963,#21964,#21965,
#21966,#21967,#21968,#21969,#21970,#21971,#21972,#21973,#21974,#21975,#21976,
#21977,#21978,#21979,#21980,#21981,#21982,#21983,#21984,#21985,#21986,#21987,
#21988,#21989,#21990,#21991,#21992,#21993,#21994,#21995,#21996,#21997,#21998,
#21999,#22000,#22001,#22002,#22003,#22004,#22005,#22006,#22007,#22008,#22009,
#22010,#22011,#22012,#22013,#22014,#22015,#22016,#22017,#22018,#22019,#22020,
#22021,#22022,#22023,#22024,#22025,#22026,#22027,#22028,#22029,#22030,#22031,
#22032,#22033,#22034,#22035,#22036,#22037,#22038,#22039,#22040,#22041,#22042,
#22043,#22044,#22045,#22046,#22047,#22048,#22049,#22050,#22051,#22052,#22053,
#22054,#22055,#22056,#22057,#22058,#22059,#22060,#22061,#22062,#22063,#22064,
#22065,#22066,#22067,#22068,#22069,#22070,#22071,#22072,#22073,#22074,#22075,
#22076,#22077,#22078,#22079,#22080,#22081,#22082,#22083,#22084,#22085,#22086,
#22087,#22088,#22089,#22090,#22091,#22092,#22093,#22094,#22095,#22096,#22097,
#22098,#22099,#22100,#22101,#22102,#22103,#22104,#22105,#22106,#22107,#22108,
#22109,#22110,#22111,#22112,#22113,#22114,#22115,#22116,#22117,#22118,#22119,
#22120,#22121,#22122,#22123,#22124,#22125,#22126,#22127,#22128,#22129,#22130,
#22131,#22132,#22133,#22134,#22135,#22136,#22137,#22138,#22139,#22140,#22141,
#22142,#22143,#22144,#22145,#22146,#22147,#22148,#22149));
#4293=EDGE_LOOP('',(#22150));
#4294=EDGE_LOOP('',(#22151,#22152,#22153,#22154,#22155,#22156,#22157,#22158,
#22159,#22160,#22161,#22162,#22163,#22164,#22165,#22166,#22167,#22168,#22169,
#22170,#22171,#22172,#22173,#22174,#22175,#22176,#22177,#22178,#22179,#22180,
#22181,#22182,#22183,#22184,#22185,#22186,#22187,#22188,#22189,#22190,#22191,
#22192,#22193,#22194,#22195,#22196,#22197,#22198,#22199,#22200,#22201,#22202,
#22203,#22204,#22205,#22206,#22207,#22208,#22209,#22210,#22211,#22212,#22213,
#22214,#22215,#22216,#22217,#22218,#22219,#22220,#22221,#22222,#22223,#22224,
#22225,#22226,#22227,#22228,#22229,#22230,#22231,#22232,#22233,#22234,#22235,
#22236,#22237,#22238,#22239,#22240,#22241,#22242,#22243,#22244,#22245,#22246,
#22247,#22248,#22249,#22250,#22251,#22252,#22253,#22254,#22255,#22256,#22257,
#22258,#22259,#22260,#22261,#22262,#22263,#22264,#22265,#22266,#22267,#22268,
#22269,#22270,#22271,#22272,#22273,#22274,#22275,#22276,#22277,#22278,#22279,
#22280,#22281,#22282,#22283,#22284,#22285,#22286,#22287,#22288,#22289,#22290,
#22291,#22292,#22293,#22294,#22295,#22296,#22297,#22298,#22299,#22300,#22301,
#22302,#22303,#22304,#22305,#22306,#22307,#22308,#22309,#22310,#22311,#22312,
#22313,#22314,#22315,#22316,#22317,#22318,#22319,#22320,#22321,#22322,#22323,
#22324,#22325,#22326,#22327,#22328,#22329,#22330,#22331,#22332,#22333,#22334,
#22335,#22336,#22337,#22338,#22339,#22340,#22341,#22342));
#4295=EDGE_LOOP('',(#22343));
#4296=EDGE_LOOP('',(#22344,#22345,#22346,#22347));
#4297=EDGE_LOOP('',(#22348,#22349,#22350,#22351));
#4298=EDGE_LOOP('',(#22352,#22353,#22354,#22355));
#4299=EDGE_LOOP('',(#22356,#22357,#22358,#22359));
#4300=EDGE_LOOP('',(#22360,#22361,#22362,#22363));
#4301=EDGE_LOOP('',(#22364,#22365,#22366,#22367));
#4302=EDGE_LOOP('',(#22368,#22369,#22370,#22371));
#4303=EDGE_LOOP('',(#22372,#22373,#22374,#22375));
#4304=EDGE_LOOP('',(#22376,#22377,#22378,#22379));
#4305=EDGE_LOOP('',(#22380,#22381,#22382,#22383));
#4306=EDGE_LOOP('',(#22384,#22385,#22386,#22387));
#4307=EDGE_LOOP('',(#22388,#22389,#22390,#22391));
#4308=EDGE_LOOP('',(#22392,#22393,#22394,#22395));
#4309=EDGE_LOOP('',(#22396,#22397,#22398,#22399));
#4310=EDGE_LOOP('',(#22400,#22401,#22402,#22403));
#4311=EDGE_LOOP('',(#22404,#22405,#22406,#22407));
#4312=EDGE_LOOP('',(#22408,#22409,#22410,#22411));
#4313=EDGE_LOOP('',(#22412,#22413,#22414,#22415));
#4314=EDGE_LOOP('',(#22416,#22417,#22418,#22419));
#4315=EDGE_LOOP('',(#22420,#22421,#22422,#22423));
#4316=EDGE_LOOP('',(#22424,#22425,#22426,#22427));
#4317=EDGE_LOOP('',(#22428,#22429,#22430,#22431));
#4318=EDGE_LOOP('',(#22432,#22433,#22434,#22435));
#4319=EDGE_LOOP('',(#22436,#22437,#22438,#22439));
#4320=EDGE_LOOP('',(#22440,#22441,#22442,#22443));
#4321=EDGE_LOOP('',(#22444,#22445,#22446,#22447));
#4322=EDGE_LOOP('',(#22448,#22449,#22450,#22451));
#4323=EDGE_LOOP('',(#22452,#22453,#22454,#22455));
#4324=EDGE_LOOP('',(#22456,#22457,#22458,#22459));
#4325=EDGE_LOOP('',(#22460,#22461,#22462,#22463));
#4326=EDGE_LOOP('',(#22464,#22465,#22466,#22467));
#4327=EDGE_LOOP('',(#22468,#22469,#22470,#22471));
#4328=EDGE_LOOP('',(#22472,#22473,#22474,#22475));
#4329=EDGE_LOOP('',(#22476,#22477,#22478,#22479));
#4330=EDGE_LOOP('',(#22480));
#4331=EDGE_LOOP('',(#22481));
#4332=EDGE_LOOP('',(#22482));
#4333=EDGE_LOOP('',(#22483));
#4334=EDGE_LOOP('',(#22484,#22485,#22486,#22487));
#4335=EDGE_LOOP('',(#22488,#22489,#22490,#22491));
#4336=EDGE_LOOP('',(#22492,#22493,#22494,#22495));
#4337=EDGE_LOOP('',(#22496,#22497,#22498,#22499));
#4338=EDGE_LOOP('',(#22500,#22501,#22502,#22503));
#4339=EDGE_LOOP('',(#22504,#22505,#22506,#22507));
#4340=EDGE_LOOP('',(#22508));
#4341=EDGE_LOOP('',(#22509));
#4342=EDGE_LOOP('',(#22510));
#4343=EDGE_LOOP('',(#22511));
#4344=EDGE_LOOP('',(#22512,#22513,#22514,#22515));
#4345=EDGE_LOOP('',(#22516,#22517,#22518,#22519));
#4346=EDGE_LOOP('',(#22520));
#4347=EDGE_LOOP('',(#22521));
#4348=EDGE_LOOP('',(#22522));
#4349=EDGE_LOOP('',(#22523));
#4350=EDGE_LOOP('',(#22524,#22525,#22526,#22527));
#4351=EDGE_LOOP('',(#22528,#22529,#22530,#22531));
#4352=EDGE_LOOP('',(#22532,#22533,#22534,#22535));
#4353=EDGE_LOOP('',(#22536,#22537,#22538,#22539));
#4354=EDGE_LOOP('',(#22540));
#4355=EDGE_LOOP('',(#22541));
#4356=EDGE_LOOP('',(#22542));
#4357=EDGE_LOOP('',(#22543));
#4358=EDGE_LOOP('',(#22544,#22545,#22546,#22547));
#4359=EDGE_LOOP('',(#22548,#22549,#22550,#22551));
#4360=EDGE_LOOP('',(#22552,#22553,#22554,#22555));
#4361=EDGE_LOOP('',(#22556,#22557,#22558,#22559));
#4362=EDGE_LOOP('',(#22560));
#4363=EDGE_LOOP('',(#22561));
#4364=EDGE_LOOP('',(#22562));
#4365=EDGE_LOOP('',(#22563));
#4366=EDGE_LOOP('',(#22564));
#4367=EDGE_LOOP('',(#22565,#22566,#22567,#22568));
#4368=EDGE_LOOP('',(#22569,#22570,#22571,#22572));
#4369=EDGE_LOOP('',(#22573));
#4370=EDGE_LOOP('',(#22574,#22575,#22576,#22577));
#4371=EDGE_LOOP('',(#22578));
#4372=EDGE_LOOP('',(#22579));
#4373=EDGE_LOOP('',(#22580,#22581,#22582,#22583));
#4374=EDGE_LOOP('',(#22584,#22585,#22586,#22587));
#4375=EDGE_LOOP('',(#22588));
#4376=EDGE_LOOP('',(#22589));
#4377=EDGE_LOOP('',(#22590));
#4378=EDGE_LOOP('',(#22591));
#4379=EDGE_LOOP('',(#22592));
#4380=EDGE_LOOP('',(#22593));
#4381=EDGE_LOOP('',(#22594));
#4382=EDGE_LOOP('',(#22595));
#4383=EDGE_LOOP('',(#22596));
#4384=EDGE_LOOP('',(#22597));
#4385=EDGE_LOOP('',(#22598,#22599,#22600,#22601));
#4386=EDGE_LOOP('',(#22602,#22603,#22604,#22605));
#4387=EDGE_LOOP('',(#22606,#22607,#22608,#22609));
#4388=EDGE_LOOP('',(#22610,#22611,#22612,#22613));
#4389=EDGE_LOOP('',(#22614,#22615,#22616,#22617));
#4390=EDGE_LOOP('',(#22618,#22619,#22620,#22621));
#4391=EDGE_LOOP('',(#22622,#22623,#22624,#22625));
#4392=EDGE_LOOP('',(#22626,#22627,#22628,#22629));
#4393=EDGE_LOOP('',(#22630));
#4394=EDGE_LOOP('',(#22631));
#4395=EDGE_LOOP('',(#22632));
#4396=EDGE_LOOP('',(#22633));
#4397=EDGE_LOOP('',(#22634,#22635,#22636,#22637));
#4398=EDGE_LOOP('',(#22638));
#4399=EDGE_LOOP('',(#22639));
#4400=EDGE_LOOP('',(#22640));
#4401=EDGE_LOOP('',(#22641));
#4402=EDGE_LOOP('',(#22642,#22643,#22644,#22645));
#4403=EDGE_LOOP('',(#22646));
#4404=EDGE_LOOP('',(#22647));
#4405=EDGE_LOOP('',(#22648,#22649,#22650,#22651));
#4406=EDGE_LOOP('',(#22652));
#4407=EDGE_LOOP('',(#22653,#22654,#22655,#22656));
#4408=EDGE_LOOP('',(#22657));
#4409=EDGE_LOOP('',(#22658,#22659,#22660,#22661));
#4410=EDGE_LOOP('',(#22662,#22663,#22664,#22665));
#4411=EDGE_LOOP('',(#22666,#22667,#22668,#22669));
#4412=EDGE_LOOP('',(#22670,#22671,#22672,#22673));
#4413=EDGE_LOOP('',(#22674,#22675,#22676,#22677));
#4414=EDGE_LOOP('',(#22678,#22679,#22680,#22681));
#4415=EDGE_LOOP('',(#22682,#22683,#22684,#22685));
#4416=EDGE_LOOP('',(#22686,#22687,#22688,#22689));
#4417=EDGE_LOOP('',(#22690));
#4418=EDGE_LOOP('',(#22691));
#4419=EDGE_LOOP('',(#22692));
#4420=EDGE_LOOP('',(#22693));
#4421=EDGE_LOOP('',(#22694,#22695,#22696,#22697));
#4422=EDGE_LOOP('',(#22698,#22699,#22700,#22701));
#4423=EDGE_LOOP('',(#22702));
#4424=EDGE_LOOP('',(#22703));
#4425=EDGE_LOOP('',(#22704));
#4426=EDGE_LOOP('',(#22705));
#4427=EDGE_LOOP('',(#22706,#22707,#22708,#22709));
#4428=EDGE_LOOP('',(#22710,#22711,#22712,#22713));
#4429=EDGE_LOOP('',(#22714));
#4430=EDGE_LOOP('',(#22715));
#4431=EDGE_LOOP('',(#22716));
#4432=EDGE_LOOP('',(#22717));
#4433=EDGE_LOOP('',(#22718,#22719,#22720,#22721));
#4434=EDGE_LOOP('',(#22722,#22723,#22724,#22725));
#4435=EDGE_LOOP('',(#22726,#22727,#22728,#22729));
#4436=EDGE_LOOP('',(#22730,#22731,#22732,#22733));
#4437=EDGE_LOOP('',(#22734,#22735,#22736,#22737));
#4438=EDGE_LOOP('',(#22738,#22739,#22740,#22741));
#4439=EDGE_LOOP('',(#22742,#22743,#22744,#22745));
#4440=EDGE_LOOP('',(#22746,#22747,#22748,#22749));
#4441=EDGE_LOOP('',(#22750,#22751,#22752,#22753));
#4442=EDGE_LOOP('',(#22754,#22755,#22756,#22757));
#4443=EDGE_LOOP('',(#22758,#22759,#22760,#22761));
#4444=EDGE_LOOP('',(#22762,#22763,#22764,#22765));
#4445=EDGE_LOOP('',(#22766,#22767,#22768,#22769));
#4446=EDGE_LOOP('',(#22770));
#4447=EDGE_LOOP('',(#22771));
#4448=EDGE_LOOP('',(#22772,#22773,#22774,#22775));
#4449=EDGE_LOOP('',(#22776,#22777,#22778,#22779));
#4450=EDGE_LOOP('',(#22780,#22781,#22782,#22783));
#4451=EDGE_LOOP('',(#22784,#22785,#22786,#22787));
#4452=EDGE_LOOP('',(#22788,#22789,#22790,#22791));
#4453=EDGE_LOOP('',(#22792,#22793,#22794,#22795));
#4454=EDGE_LOOP('',(#22796,#22797,#22798,#22799));
#4455=EDGE_LOOP('',(#22800,#22801,#22802,#22803));
#4456=EDGE_LOOP('',(#22804,#22805,#22806,#22807));
#4457=EDGE_LOOP('',(#22808,#22809,#22810,#22811));
#4458=EDGE_LOOP('',(#22812,#22813,#22814,#22815));
#4459=EDGE_LOOP('',(#22816,#22817,#22818,#22819));
#4460=EDGE_LOOP('',(#22820,#22821,#22822,#22823));
#4461=EDGE_LOOP('',(#22824,#22825,#22826,#22827));
#4462=EDGE_LOOP('',(#22828,#22829,#22830,#22831));
#4463=EDGE_LOOP('',(#22832,#22833,#22834,#22835));
#4464=EDGE_LOOP('',(#22836,#22837,#22838,#22839));
#4465=EDGE_LOOP('',(#22840,#22841,#22842,#22843));
#4466=EDGE_LOOP('',(#22844,#22845,#22846,#22847));
#4467=EDGE_LOOP('',(#22848,#22849,#22850,#22851));
#4468=EDGE_LOOP('',(#22852,#22853,#22854,#22855));
#4469=EDGE_LOOP('',(#22856,#22857,#22858,#22859));
#4470=EDGE_LOOP('',(#22860,#22861,#22862,#22863));
#4471=EDGE_LOOP('',(#22864,#22865,#22866,#22867));
#4472=EDGE_LOOP('',(#22868,#22869,#22870,#22871));
#4473=EDGE_LOOP('',(#22872,#22873,#22874,#22875));
#4474=EDGE_LOOP('',(#22876,#22877,#22878,#22879));
#4475=EDGE_LOOP('',(#22880,#22881,#22882,#22883));
#4476=EDGE_LOOP('',(#22884,#22885,#22886,#22887));
#4477=EDGE_LOOP('',(#22888,#22889,#22890,#22891));
#4478=EDGE_LOOP('',(#22892,#22893,#22894,#22895));
#4479=EDGE_LOOP('',(#22896,#22897,#22898,#22899));
#4480=EDGE_LOOP('',(#22900,#22901,#22902,#22903));
#4481=EDGE_LOOP('',(#22904,#22905,#22906,#22907));
#4482=EDGE_LOOP('',(#22908,#22909,#22910,#22911));
#4483=EDGE_LOOP('',(#22912,#22913,#22914,#22915));
#4484=EDGE_LOOP('',(#22916,#22917,#22918,#22919));
#4485=EDGE_LOOP('',(#22920,#22921,#22922,#22923));
#4486=EDGE_LOOP('',(#22924,#22925,#22926,#22927));
#4487=EDGE_LOOP('',(#22928,#22929,#22930,#22931));
#4488=EDGE_LOOP('',(#22932,#22933,#22934,#22935,#22936,#22937,#22938,#22939,
#22940,#22941,#22942,#22943,#22944,#22945,#22946,#22947,#22948,#22949,#22950,
#22951,#22952,#22953,#22954,#22955,#22956,#22957,#22958,#22959,#22960,#22961,
#22962,#22963,#22964,#22965,#22966,#22967,#22968,#22969,#22970,#22971,#22972,
#22973,#22974,#22975));
#4489=EDGE_LOOP('',(#22976,#22977,#22978,#22979));
#4490=EDGE_LOOP('',(#22980,#22981,#22982,#22983,#22984,#22985,#22986,#22987,
#22988,#22989,#22990,#22991,#22992,#22993,#22994,#22995,#22996,#22997,#22998,
#22999,#23000,#23001,#23002,#23003,#23004,#23005,#23006,#23007,#23008,#23009,
#23010,#23011,#23012,#23013,#23014,#23015,#23016,#23017,#23018,#23019,#23020,
#23021,#23022,#23023));
#4491=EDGE_LOOP('',(#23024,#23025,#23026,#23027));
#4492=EDGE_LOOP('',(#23028,#23029,#23030,#23031));
#4493=EDGE_LOOP('',(#23032,#23033,#23034,#23035));
#4494=EDGE_LOOP('',(#23036,#23037,#23038,#23039));
#4495=EDGE_LOOP('',(#23040,#23041,#23042,#23043));
#4496=EDGE_LOOP('',(#23044,#23045,#23046,#23047));
#4497=EDGE_LOOP('',(#23048,#23049,#23050,#23051));
#4498=EDGE_LOOP('',(#23052,#23053,#23054,#23055,#23056,#23057));
#4499=EDGE_LOOP('',(#23058));
#4500=EDGE_LOOP('',(#23059,#23060,#23061,#23062));
#4501=EDGE_LOOP('',(#23063,#23064,#23065,#23066));
#4502=EDGE_LOOP('',(#23067));
#4503=EDGE_LOOP('',(#23068,#23069,#23070,#23071,#23072,#23073));
#4504=EDGE_LOOP('',(#23074,#23075,#23076,#23077));
#4505=CIRCLE('',#25394,2.5175);
#4506=CIRCLE('',#25395,2.5175);
#4507=CIRCLE('',#25396,2.5175);
#4508=CIRCLE('',#25411,2.5175);
#4509=CIRCLE('',#25413,3.07349999999999);
#4510=CIRCLE('',#25428,3.0735);
#4511=CIRCLE('',#25430,2.5175);
#4512=CIRCLE('',#25431,2.5175);
#4513=CIRCLE('',#25432,2.5175);
#4514=CIRCLE('',#25447,2.5175);
#4515=CIRCLE('',#25449,3.07349999999999);
#4516=CIRCLE('',#25464,3.0735);
#4517=CIRCLE('',#25466,2.5175);
#4518=CIRCLE('',#25467,2.5175);
#4519=CIRCLE('',#25468,2.5175);
#4520=CIRCLE('',#25483,2.5175);
#4521=CIRCLE('',#25485,3.0735);
#4522=CIRCLE('',#25500,3.0735);
#4523=CIRCLE('',#25502,2.5175);
#4524=CIRCLE('',#25503,2.5175);
#4525=CIRCLE('',#25504,2.5175);
#4526=CIRCLE('',#25519,2.5175);
#4527=CIRCLE('',#25521,3.07349999999999);
#4528=CIRCLE('',#25536,3.0735);
#4529=CIRCLE('',#25538,2.5175);
#4530=CIRCLE('',#25539,2.5175);
#4531=CIRCLE('',#25540,2.5175);
#4532=CIRCLE('',#25555,2.5175);
#4533=CIRCLE('',#25557,3.0735);
#4534=CIRCLE('',#25572,3.0735);
#4535=CIRCLE('',#25574,2.5175);
#4536=CIRCLE('',#25575,2.5175);
#4537=CIRCLE('',#25576,2.5175);
#4538=CIRCLE('',#25591,2.5175);
#4539=CIRCLE('',#25593,3.07349999999999);
#4540=CIRCLE('',#25608,3.0735);
#4541=CIRCLE('',#25610,2.5175);
#4542=CIRCLE('',#25611,2.5175);
#4543=CIRCLE('',#25612,2.5175);
#4544=CIRCLE('',#25627,2.5175);
#4545=CIRCLE('',#25629,3.0735);
#4546=CIRCLE('',#25644,3.0735);
#4547=CIRCLE('',#25646,2.5175);
#4548=CIRCLE('',#25647,2.5175);
#4549=CIRCLE('',#25648,2.5175);
#4550=CIRCLE('',#25663,2.5175);
#4551=CIRCLE('',#25665,3.0735);
#4552=CIRCLE('',#25680,3.0735);
#4553=CIRCLE('',#25726,5.5);
#4554=CIRCLE('',#25727,5.5);
#4555=CIRCLE('',#25729,5.5);
#4556=CIRCLE('',#25730,5.5);
#4557=CIRCLE('',#25732,5.5);
#4558=CIRCLE('',#25733,5.5);
#4559=CIRCLE('',#25735,5.5);
#4560=CIRCLE('',#25736,5.5);
#4561=CIRCLE('',#25738,18.);
#4562=CIRCLE('',#25739,18.);
#4563=CIRCLE('',#25741,17.);
#4564=CIRCLE('',#25743,90.);
#4565=CIRCLE('',#25744,90.);
#4566=CIRCLE('',#25746,100.);
#4567=CIRCLE('',#25747,100.);
#4568=CIRCLE('',#25750,140.);
#4569=CIRCLE('',#25752,17.);
#4570=CIRCLE('',#25754,140.);
#4571=CIRCLE('',#25759,2.);
#4572=CIRCLE('',#25762,2.);
#4573=CIRCLE('',#25765,2.);
#4574=CIRCLE('',#25768,2.);
#4575=CIRCLE('',#25771,18.);
#4576=CIRCLE('',#25772,18.);
#4577=CIRCLE('',#25774,90.);
#4578=CIRCLE('',#25775,90.);
#4579=CIRCLE('',#25780,3.5);
#4580=CIRCLE('',#25781,3.5);
#4581=CIRCLE('',#25783,3.5);
#4582=CIRCLE('',#25784,3.5);
#4583=CIRCLE('',#25786,3.5);
#4584=CIRCLE('',#25787,3.5);
#4585=CIRCLE('',#25789,3.5);
#4586=CIRCLE('',#25790,3.5);
#4587=CIRCLE('',#25792,3.5);
#4588=CIRCLE('',#25793,3.5);
#4589=CIRCLE('',#25795,3.5);
#4590=CIRCLE('',#25796,3.5);
#4591=CIRCLE('',#25798,3.5);
#4592=CIRCLE('',#25799,3.5);
#4593=CIRCLE('',#25801,3.5);
#4594=CIRCLE('',#25802,3.5);
#4595=CIRCLE('',#25804,18.);
#4596=CIRCLE('',#25805,18.);
#4597=CIRCLE('',#25807,100.);
#4598=CIRCLE('',#25808,100.);
#4599=CIRCLE('',#25814,8.);
#4600=CIRCLE('',#25818,8.);
#4601=CIRCLE('',#25820,7.);
#4602=CIRCLE('',#25821,7.);
#4603=CIRCLE('',#25823,8.);
#4604=CIRCLE('',#25825,8.);
#4605=CIRCLE('',#25827,8.);
#4606=CIRCLE('',#25829,15.);
#4607=CIRCLE('',#25830,15.);
#4608=CIRCLE('',#25832,16.);
#4609=CIRCLE('',#25834,16.);
#4610=CIRCLE('',#25836,16.);
#4611=CIRCLE('',#25838,11.);
#4612=CIRCLE('',#25839,8.);
#4613=CIRCLE('',#25841,11.);
#4614=CIRCLE('',#25842,8.);
#4615=CIRCLE('',#25845,8.);
#4616=CIRCLE('',#25847,20.);
#4617=CIRCLE('',#25848,16.);
#4618=CIRCLE('',#25850,20.);
#4619=CIRCLE('',#25853,16.);
#4620=CIRCLE('',#25857,8.);
#4621=CIRCLE('',#25858,8.);
#4622=CIRCLE('',#25861,16.);
#4623=CIRCLE('',#25866,2.);
#4624=CIRCLE('',#25869,2.);
#4625=CIRCLE('',#25872,2.);
#4626=CIRCLE('',#25875,2.);
#4627=CIRCLE('',#25878,74.4999999996252);
#4628=CIRCLE('',#25879,74.4999999996252);
#4629=CIRCLE('',#25881,74.4999999996252);
#4630=CIRCLE('',#25882,74.4999999996252);
#4631=CIRCLE('',#25884,74.4999999996252);
#4632=CIRCLE('',#25885,74.4999999996252);
#4633=CIRCLE('',#25887,74.4999999996252);
#4634=CIRCLE('',#25888,74.4999999996252);
#4635=CIRCLE('',#25890,74.4999999996252);
#4636=CIRCLE('',#25891,74.4999999996252);
#4637=CIRCLE('',#25893,74.4999999996252);
#4638=CIRCLE('',#25894,74.4999999996252);
#4639=CIRCLE('',#25896,74.4999999996252);
#4640=CIRCLE('',#25897,74.4999999996252);
#4641=CIRCLE('',#25899,74.4999999996252);
#4642=CIRCLE('',#25900,74.4999999996252);
#4643=CIRCLE('',#25902,74.4999999996252);
#4644=CIRCLE('',#25903,74.4999999996252);
#4645=CIRCLE('',#25905,74.4999999996252);
#4646=CIRCLE('',#25906,74.4999999996252);
#4647=CIRCLE('',#25908,74.4999999996252);
#4648=CIRCLE('',#25909,74.4999999996252);
#4649=CIRCLE('',#25911,74.4999999996252);
#4650=CIRCLE('',#25912,74.4999999996252);
#4651=CIRCLE('',#25914,74.4999999996252);
#4652=CIRCLE('',#25915,74.4999999996252);
#4653=CIRCLE('',#25917,74.4999999996252);
#4654=CIRCLE('',#25918,74.4999999996252);
#4655=CIRCLE('',#25920,74.4999999996252);
#4656=CIRCLE('',#25921,74.4999999996252);
#4657=CIRCLE('',#25923,74.4999999996252);
#4658=CIRCLE('',#25924,74.4999999996252);
#4659=CIRCLE('',#25926,74.4999999996252);
#4660=CIRCLE('',#25927,74.4999999996252);
#4661=CIRCLE('',#25929,74.4999999996252);
#4662=CIRCLE('',#25930,74.4999999996252);
#4663=CIRCLE('',#25932,74.4999999996252);
#4664=CIRCLE('',#25933,74.4999999996252);
#4665=CIRCLE('',#25935,74.4999999996252);
#4666=CIRCLE('',#25936,74.4999999996252);
#4667=CIRCLE('',#25938,74.4999999996252);
#4668=CIRCLE('',#25939,74.4999999996252);
#4669=CIRCLE('',#25941,74.4999999996252);
#4670=CIRCLE('',#25942,74.4999999996252);
#4671=CIRCLE('',#25944,74.4999999996252);
#4672=CIRCLE('',#25945,74.4999999996252);
#4673=CIRCLE('',#25947,74.4999999996252);
#4674=CIRCLE('',#25948,74.4999999996252);
#4675=CIRCLE('',#25950,74.4999999996252);
#4676=CIRCLE('',#25951,74.4999999996252);
#4677=CIRCLE('',#25953,74.4999999996252);
#4678=CIRCLE('',#25954,74.4999999996252);
#4679=CIRCLE('',#25956,74.4999999996252);
#4680=CIRCLE('',#25957,74.4999999996252);
#4681=CIRCLE('',#25959,74.4999999996252);
#4682=CIRCLE('',#25960,74.4999999996252);
#4683=CIRCLE('',#25962,74.4999999996252);
#4684=CIRCLE('',#25963,74.4999999996252);
#4685=CIRCLE('',#25965,74.4999999996252);
#4686=CIRCLE('',#25966,74.4999999996252);
#4687=CIRCLE('',#25968,74.4999999996252);
#4688=CIRCLE('',#25969,74.4999999996252);
#4689=CIRCLE('',#25971,74.4999999996252);
#4690=CIRCLE('',#25972,74.4999999996252);
#4691=CIRCLE('',#25974,74.4999999996252);
#4692=CIRCLE('',#25975,74.4999999996252);
#4693=CIRCLE('',#25977,74.4999999996252);
#4694=CIRCLE('',#25978,74.4999999996252);
#4695=CIRCLE('',#25980,74.4999999996252);
#4696=CIRCLE('',#25981,74.4999999996252);
#4697=CIRCLE('',#25983,74.4999999996252);
#4698=CIRCLE('',#25984,74.4999999996252);
#4699=CIRCLE('',#25986,74.4999999996252);
#4700=CIRCLE('',#25987,74.4999999996252);
#4701=CIRCLE('',#25989,74.4999999996252);
#4702=CIRCLE('',#25990,74.4999999996252);
#4703=CIRCLE('',#25992,74.4999999996252);
#4704=CIRCLE('',#25993,74.4999999996252);
#4705=CIRCLE('',#25995,74.4999999996252);
#4706=CIRCLE('',#25996,74.4999999996252);
#4707=CIRCLE('',#25998,74.4999999996252);
#4708=CIRCLE('',#25999,74.4999999996252);
#4709=CIRCLE('',#26001,74.4999999996252);
#4710=CIRCLE('',#26002,74.4999999996252);
#4711=CIRCLE('',#26004,74.4999999996252);
#4712=CIRCLE('',#26005,74.4999999996252);
#4713=CIRCLE('',#26007,74.4999999996252);
#4714=CIRCLE('',#26008,74.4999999996252);
#4715=CIRCLE('',#26010,74.4999999996252);
#4716=CIRCLE('',#26011,74.4999999996252);
#4717=CIRCLE('',#26013,74.4999999996252);
#4718=CIRCLE('',#26014,74.4999999996252);
#4719=CIRCLE('',#26016,74.4999999996252);
#4720=CIRCLE('',#26017,74.4999999996252);
#4721=CIRCLE('',#26019,74.4999999996252);
#4722=CIRCLE('',#26020,74.4999999996252);
#4723=CIRCLE('',#26022,74.4999999996252);
#4724=CIRCLE('',#26023,74.4999999996252);
#4725=CIRCLE('',#26025,74.4999999996252);
#4726=CIRCLE('',#26026,74.4999999996252);
#4727=CIRCLE('',#26028,74.4999999996252);
#4728=CIRCLE('',#26029,74.4999999996252);
#4729=CIRCLE('',#26031,74.4999999996252);
#4730=CIRCLE('',#26032,74.4999999996252);
#4731=CIRCLE('',#26034,74.4999999996252);
#4732=CIRCLE('',#26035,74.4999999996252);
#4733=CIRCLE('',#26037,74.4999999996252);
#4734=CIRCLE('',#26038,74.4999999996252);
#4735=CIRCLE('',#26040,74.4999999996252);
#4736=CIRCLE('',#26041,74.4999999996252);
#4737=CIRCLE('',#26043,74.4999999996252);
#4738=CIRCLE('',#26044,74.4999999996252);
#4739=CIRCLE('',#26046,74.4999999996252);
#4740=CIRCLE('',#26047,74.4999999996252);
#4741=CIRCLE('',#26049,74.4999999996252);
#4742=CIRCLE('',#26050,74.4999999996252);
#4743=CIRCLE('',#26052,74.4999999996252);
#4744=CIRCLE('',#26053,74.4999999996252);
#4745=CIRCLE('',#26055,74.4999999996252);
#4746=CIRCLE('',#26056,74.4999999996252);
#4747=CIRCLE('',#26058,74.4999999996252);
#4748=CIRCLE('',#26059,74.4999999996252);
#4749=CIRCLE('',#26061,74.4999999996252);
#4750=CIRCLE('',#26062,74.4999999996252);
#4751=CIRCLE('',#26064,74.4999999996252);
#4752=CIRCLE('',#26065,74.4999999996252);
#4753=CIRCLE('',#26067,74.4999999996252);
#4754=CIRCLE('',#26068,74.4999999996252);
#4755=CIRCLE('',#26070,74.4999999996252);
#4756=CIRCLE('',#26071,74.4999999996252);
#4757=CIRCLE('',#26073,74.4999999996252);
#4758=CIRCLE('',#26074,74.4999999996252);
#4759=CIRCLE('',#26076,74.4999999996252);
#4760=CIRCLE('',#26077,74.4999999996252);
#4761=CIRCLE('',#26079,74.4999999996252);
#4762=CIRCLE('',#26080,74.4999999996252);
#4763=CIRCLE('',#26082,74.4999999996252);
#4764=CIRCLE('',#26083,74.4999999996252);
#4765=CIRCLE('',#26085,74.4999999996252);
#4766=CIRCLE('',#26086,74.4999999996252);
#4767=CIRCLE('',#26088,74.4999999996252);
#4768=CIRCLE('',#26089,74.4999999996252);
#4769=CIRCLE('',#26091,70.);
#4770=CIRCLE('',#26092,70.);
#4771=CIRCLE('',#26094,70.);
#4772=CIRCLE('',#26095,70.);
#4773=CIRCLE('',#26097,70.);
#4774=CIRCLE('',#26098,70.);
#4775=CIRCLE('',#26100,70.);
#4776=CIRCLE('',#26101,70.);
#4777=CIRCLE('',#26103,70.);
#4778=CIRCLE('',#26104,70.);
#4779=CIRCLE('',#26106,70.);
#4780=CIRCLE('',#26107,70.);
#4781=CIRCLE('',#26109,70.);
#4782=CIRCLE('',#26110,70.);
#4783=CIRCLE('',#26112,70.);
#4784=CIRCLE('',#26113,70.);
#4785=CIRCLE('',#26115,70.);
#4786=CIRCLE('',#26116,70.);
#4787=CIRCLE('',#26118,70.);
#4788=CIRCLE('',#26119,70.);
#4789=CIRCLE('',#26121,70.);
#4790=CIRCLE('',#26122,70.);
#4791=CIRCLE('',#26124,70.);
#4792=CIRCLE('',#26125,70.);
#4793=CIRCLE('',#26127,70.);
#4794=CIRCLE('',#26128,70.);
#4795=CIRCLE('',#26130,70.);
#4796=CIRCLE('',#26131,70.);
#4797=CIRCLE('',#26133,70.);
#4798=CIRCLE('',#26134,70.);
#4799=CIRCLE('',#26136,70.);
#4800=CIRCLE('',#26137,70.);
#4801=CIRCLE('',#26139,70.);
#4802=CIRCLE('',#26140,70.);
#4803=CIRCLE('',#26142,70.);
#4804=CIRCLE('',#26143,70.);
#4805=CIRCLE('',#26145,70.);
#4806=CIRCLE('',#26146,70.);
#4807=CIRCLE('',#26148,70.);
#4808=CIRCLE('',#26149,70.);
#4809=CIRCLE('',#26151,70.);
#4810=CIRCLE('',#26152,70.);
#4811=CIRCLE('',#26154,70.);
#4812=CIRCLE('',#26155,70.);
#4813=CIRCLE('',#26157,70.);
#4814=CIRCLE('',#26158,70.);
#4815=CIRCLE('',#26160,70.);
#4816=CIRCLE('',#26161,70.);
#4817=CIRCLE('',#26163,70.);
#4818=CIRCLE('',#26164,70.);
#4819=CIRCLE('',#26166,70.);
#4820=CIRCLE('',#26167,70.);
#4821=CIRCLE('',#26169,70.);
#4822=CIRCLE('',#26170,70.);
#4823=CIRCLE('',#26172,70.);
#4824=CIRCLE('',#26173,70.);
#4825=CIRCLE('',#26175,70.);
#4826=CIRCLE('',#26176,70.);
#4827=CIRCLE('',#26178,70.);
#4828=CIRCLE('',#26179,70.);
#4829=CIRCLE('',#26181,70.);
#4830=CIRCLE('',#26182,70.);
#4831=CIRCLE('',#26184,70.);
#4832=CIRCLE('',#26185,70.);
#4833=CIRCLE('',#26187,70.);
#4834=CIRCLE('',#26188,70.);
#4835=CIRCLE('',#26190,70.);
#4836=CIRCLE('',#26191,70.);
#4837=CIRCLE('',#26193,70.);
#4838=CIRCLE('',#26194,70.);
#4839=CIRCLE('',#26196,70.);
#4840=CIRCLE('',#26197,70.);
#4841=CIRCLE('',#26199,70.);
#4842=CIRCLE('',#26200,70.);
#4843=CIRCLE('',#26202,70.);
#4844=CIRCLE('',#26203,70.);
#4845=CIRCLE('',#26205,70.);
#4846=CIRCLE('',#26206,70.);
#4847=CIRCLE('',#26208,70.);
#4848=CIRCLE('',#26209,70.);
#4849=CIRCLE('',#26211,70.);
#4850=CIRCLE('',#26212,70.);
#4851=CIRCLE('',#26214,70.);
#4852=CIRCLE('',#26215,70.);
#4853=CIRCLE('',#26217,70.);
#4854=CIRCLE('',#26218,70.);
#4855=CIRCLE('',#26220,70.);
#4856=CIRCLE('',#26221,70.);
#4857=CIRCLE('',#26223,70.);
#4858=CIRCLE('',#26224,70.);
#4859=CIRCLE('',#26226,70.);
#4860=CIRCLE('',#26227,70.);
#4861=CIRCLE('',#26229,70.);
#4862=CIRCLE('',#26230,70.);
#4863=CIRCLE('',#26232,70.);
#4864=CIRCLE('',#26233,70.);
#4865=CIRCLE('',#26235,70.);
#4866=CIRCLE('',#26236,70.);
#4867=CIRCLE('',#26238,70.);
#4868=CIRCLE('',#26239,70.);
#4869=CIRCLE('',#26241,70.);
#4870=CIRCLE('',#26242,70.);
#4871=CIRCLE('',#26244,70.);
#4872=CIRCLE('',#26245,70.);
#4873=CIRCLE('',#26247,70.);
#4874=CIRCLE('',#26248,70.);
#4875=CIRCLE('',#26250,70.);
#4876=CIRCLE('',#26251,70.);
#4877=CIRCLE('',#26253,70.);
#4878=CIRCLE('',#26254,70.);
#4879=CIRCLE('',#26256,70.);
#4880=CIRCLE('',#26257,70.);
#4881=CIRCLE('',#26259,70.);
#4882=CIRCLE('',#26260,70.);
#4883=CIRCLE('',#26262,70.);
#4884=CIRCLE('',#26263,70.);
#4885=CIRCLE('',#26265,70.);
#4886=CIRCLE('',#26266,70.);
#4887=CIRCLE('',#26268,70.);
#4888=CIRCLE('',#26269,70.);
#4889=CIRCLE('',#26271,70.);
#4890=CIRCLE('',#26272,70.);
#4891=CIRCLE('',#26274,70.);
#4892=CIRCLE('',#26275,70.);
#4893=CIRCLE('',#26277,70.);
#4894=CIRCLE('',#26278,70.);
#4895=CIRCLE('',#26280,70.);
#4896=CIRCLE('',#26281,70.);
#4897=CIRCLE('',#26283,70.);
#4898=CIRCLE('',#26284,70.);
#4899=CIRCLE('',#26286,70.);
#4900=CIRCLE('',#26287,70.);
#4901=CIRCLE('',#26289,70.);
#4902=CIRCLE('',#26290,70.);
#4903=CIRCLE('',#26292,70.);
#4904=CIRCLE('',#26293,70.);
#4905=CIRCLE('',#26295,70.);
#4906=CIRCLE('',#26296,70.);
#4907=CIRCLE('',#26298,70.);
#4908=CIRCLE('',#26299,70.);
#4909=CIRCLE('',#26301,70.);
#4910=CIRCLE('',#26302,70.);
#4911=CIRCLE('',#26304,74.4999999996252);
#4912=CIRCLE('',#26305,74.4999999996252);
#4913=CIRCLE('',#26307,90.);
#4914=CIRCLE('',#26308,70.);
#4915=CIRCLE('',#26310,70.);
#4916=CIRCLE('',#26312,90.);
#4917=CIRCLE('',#26319,8.);
#4918=CIRCLE('',#26320,8.);
#4919=CIRCLE('',#26322,26.);
#4920=CIRCLE('',#26323,0.5);
#4921=CIRCLE('',#26324,21.4999999999992);
#4922=CIRCLE('',#26325,0.5);
#4923=CIRCLE('',#26326,26.);
#4924=CIRCLE('',#26327,0.5);
#4925=CIRCLE('',#26328,21.4999999999992);
#4926=CIRCLE('',#26329,0.5);
#4927=CIRCLE('',#26330,26.);
#4928=CIRCLE('',#26331,0.5);
#4929=CIRCLE('',#26332,21.4999999999992);
#4930=CIRCLE('',#26333,0.5);
#4931=CIRCLE('',#26334,26.);
#4932=CIRCLE('',#26335,0.5);
#4933=CIRCLE('',#26336,21.4999999999992);
#4934=CIRCLE('',#26337,0.5);
#4935=CIRCLE('',#26338,26.);
#4936=CIRCLE('',#26339,0.5);
#4937=CIRCLE('',#26340,21.4999999999992);
#4938=CIRCLE('',#26341,0.5);
#4939=CIRCLE('',#26342,26.);
#4940=CIRCLE('',#26343,0.5);
#4941=CIRCLE('',#26344,21.4999999999992);
#4942=CIRCLE('',#26345,0.5);
#4943=CIRCLE('',#26346,26.);
#4944=CIRCLE('',#26347,0.5);
#4945=CIRCLE('',#26348,21.4999999999992);
#4946=CIRCLE('',#26349,0.5);
#4947=CIRCLE('',#26350,26.);
#4948=CIRCLE('',#26351,0.5);
#4949=CIRCLE('',#26352,21.4999999999992);
#4950=CIRCLE('',#26353,0.5);
#4951=CIRCLE('',#26354,26.);
#4952=CIRCLE('',#26355,0.5);
#4953=CIRCLE('',#26356,21.4999999999992);
#4954=CIRCLE('',#26357,0.5);
#4955=CIRCLE('',#26358,26.);
#4956=CIRCLE('',#26359,0.5);
#4957=CIRCLE('',#26360,21.4999999999992);
#4958=CIRCLE('',#26361,0.5);
#4959=CIRCLE('',#26362,26.);
#4960=CIRCLE('',#26363,0.5);
#4961=CIRCLE('',#26364,21.4999999999992);
#4962=CIRCLE('',#26365,0.5);
#4963=CIRCLE('',#26366,26.);
#4964=CIRCLE('',#26367,0.5);
#4965=CIRCLE('',#26368,21.4999999999992);
#4966=CIRCLE('',#26369,0.5);
#4967=CIRCLE('',#26370,26.);
#4968=CIRCLE('',#26371,0.5);
#4969=CIRCLE('',#26372,21.4999999999992);
#4970=CIRCLE('',#26373,0.5);
#4971=CIRCLE('',#26374,26.);
#4972=CIRCLE('',#26375,0.5);
#4973=CIRCLE('',#26376,21.4999999999992);
#4974=CIRCLE('',#26377,0.5);
#4975=CIRCLE('',#26378,26.);
#4976=CIRCLE('',#26379,0.5);
#4977=CIRCLE('',#26380,21.4999999999992);
#4978=CIRCLE('',#26381,0.5);
#4979=CIRCLE('',#26382,26.);
#4980=CIRCLE('',#26383,0.5);
#4981=CIRCLE('',#26384,21.4999999999992);
#4982=CIRCLE('',#26385,0.5);
#4983=CIRCLE('',#26386,26.);
#4984=CIRCLE('',#26387,0.5);
#4985=CIRCLE('',#26388,21.4999999999992);
#4986=CIRCLE('',#26389,0.5);
#4987=CIRCLE('',#26390,26.);
#4988=CIRCLE('',#26391,0.5);
#4989=CIRCLE('',#26392,21.4999999999992);
#4990=CIRCLE('',#26393,0.5);
#4991=CIRCLE('',#26394,26.);
#4992=CIRCLE('',#26395,0.5);
#4993=CIRCLE('',#26396,21.4999999999992);
#4994=CIRCLE('',#26397,0.5);
#4995=CIRCLE('',#26398,26.);
#4996=CIRCLE('',#26399,0.5);
#4997=CIRCLE('',#26400,21.4999999999992);
#4998=CIRCLE('',#26401,0.5);
#4999=CIRCLE('',#26402,26.);
#5000=CIRCLE('',#26403,0.5);
#5001=CIRCLE('',#26404,21.4999999999992);
#5002=CIRCLE('',#26405,0.5);
#5003=CIRCLE('',#26406,26.);
#5004=CIRCLE('',#26407,0.5);
#5005=CIRCLE('',#26408,21.4999999999992);
#5006=CIRCLE('',#26409,0.5);
#5007=CIRCLE('',#26410,26.);
#5008=CIRCLE('',#26411,0.5);
#5009=CIRCLE('',#26412,21.4999999999992);
#5010=CIRCLE('',#26413,0.5);
#5011=CIRCLE('',#26414,26.);
#5012=CIRCLE('',#26415,0.5);
#5013=CIRCLE('',#26416,21.4999999999992);
#5014=CIRCLE('',#26417,0.5);
#5015=CIRCLE('',#26419,0.5);
#5016=CIRCLE('',#26422,0.5);
#5017=CIRCLE('',#26424,21.4999999999992);
#5018=CIRCLE('',#26426,0.5);
#5019=CIRCLE('',#26429,0.5);
#5020=CIRCLE('',#26431,21.4999999999992);
#5021=CIRCLE('',#26433,0.5);
#5022=CIRCLE('',#26436,0.5);
#5023=CIRCLE('',#26438,21.4999999999992);
#5024=CIRCLE('',#26440,0.5);
#5025=CIRCLE('',#26443,0.5);
#5026=CIRCLE('',#26445,21.4999999999992);
#5027=CIRCLE('',#26447,0.5);
#5028=CIRCLE('',#26450,0.5);
#5029=CIRCLE('',#26452,21.4999999999992);
#5030=CIRCLE('',#26454,0.5);
#5031=CIRCLE('',#26457,0.5);
#5032=CIRCLE('',#26459,21.4999999999992);
#5033=CIRCLE('',#26461,0.5);
#5034=CIRCLE('',#26464,0.5);
#5035=CIRCLE('',#26466,21.4999999999992);
#5036=CIRCLE('',#26468,0.5);
#5037=CIRCLE('',#26471,0.5);
#5038=CIRCLE('',#26473,21.4999999999992);
#5039=CIRCLE('',#26475,0.5);
#5040=CIRCLE('',#26478,0.5);
#5041=CIRCLE('',#26480,21.4999999999992);
#5042=CIRCLE('',#26482,0.5);
#5043=CIRCLE('',#26485,0.5);
#5044=CIRCLE('',#26487,21.4999999999992);
#5045=CIRCLE('',#26489,0.5);
#5046=CIRCLE('',#26492,0.5);
#5047=CIRCLE('',#26494,21.4999999999992);
#5048=CIRCLE('',#26496,0.5);
#5049=CIRCLE('',#26499,0.5);
#5050=CIRCLE('',#26501,21.4999999999992);
#5051=CIRCLE('',#26503,0.5);
#5052=CIRCLE('',#26506,0.5);
#5053=CIRCLE('',#26508,21.4999999999992);
#5054=CIRCLE('',#26510,0.5);
#5055=CIRCLE('',#26513,0.5);
#5056=CIRCLE('',#26515,21.4999999999992);
#5057=CIRCLE('',#26517,0.5);
#5058=CIRCLE('',#26520,0.5);
#5059=CIRCLE('',#26522,21.4999999999992);
#5060=CIRCLE('',#26524,0.5);
#5061=CIRCLE('',#26527,0.5);
#5062=CIRCLE('',#26529,21.4999999999992);
#5063=CIRCLE('',#26531,0.5);
#5064=CIRCLE('',#26534,0.5);
#5065=CIRCLE('',#26536,21.4999999999992);
#5066=CIRCLE('',#26538,0.5);
#5067=CIRCLE('',#26541,0.5);
#5068=CIRCLE('',#26543,21.4999999999992);
#5069=CIRCLE('',#26545,0.5);
#5070=CIRCLE('',#26548,0.5);
#5071=CIRCLE('',#26550,21.4999999999992);
#5072=CIRCLE('',#26552,0.5);
#5073=CIRCLE('',#26555,0.5);
#5074=CIRCLE('',#26557,21.4999999999992);
#5075=CIRCLE('',#26559,0.5);
#5076=CIRCLE('',#26562,0.5);
#5077=CIRCLE('',#26564,21.4999999999992);
#5078=CIRCLE('',#26566,0.5);
#5079=CIRCLE('',#26569,0.5);
#5080=CIRCLE('',#26571,21.4999999999992);
#5081=CIRCLE('',#26573,0.5);
#5082=CIRCLE('',#26576,0.5);
#5083=CIRCLE('',#26578,21.4999999999992);
#5084=CIRCLE('',#26603,26.);
#5085=CIRCLE('',#26604,26.);
#5086=CIRCLE('',#26605,26.);
#5087=CIRCLE('',#26606,26.);
#5088=CIRCLE('',#26607,26.);
#5089=CIRCLE('',#26608,26.);
#5090=CIRCLE('',#26609,26.);
#5091=CIRCLE('',#26610,26.);
#5092=CIRCLE('',#26611,26.);
#5093=CIRCLE('',#26612,26.);
#5094=CIRCLE('',#26613,26.);
#5095=CIRCLE('',#26614,26.);
#5096=CIRCLE('',#26615,26.);
#5097=CIRCLE('',#26616,26.);
#5098=CIRCLE('',#26617,26.);
#5099=CIRCLE('',#26618,26.);
#5100=CIRCLE('',#26619,26.);
#5101=CIRCLE('',#26620,26.);
#5102=CIRCLE('',#26621,26.);
#5103=CIRCLE('',#26622,26.);
#5104=CIRCLE('',#26623,26.);
#5105=CIRCLE('',#26624,26.);
#5106=CIRCLE('',#26625,26.);
#5107=CIRCLE('',#26626,0.5);
#5108=CIRCLE('',#26627,21.4999999999992);
#5109=CIRCLE('',#26628,0.5);
#5110=CIRCLE('',#26629,26.);
#5111=CIRCLE('',#26661,0.5);
#5112=CIRCLE('',#26662,0.5);
#5113=CIRCLE('',#26665,0.5);
#5114=CIRCLE('',#26666,0.5);
#5115=CIRCLE('',#26668,21.4999999999992);
#5116=CIRCLE('',#26669,21.4999999999992);
#5117=CIRCLE('',#26671,0.5);
#5118=CIRCLE('',#26672,0.5);
#5119=CIRCLE('',#26675,0.5);
#5120=CIRCLE('',#26676,0.5);
#5121=CIRCLE('',#26678,21.4999999999992);
#5122=CIRCLE('',#26679,21.4999999999992);
#5123=CIRCLE('',#26681,0.5);
#5124=CIRCLE('',#26682,0.5);
#5125=CIRCLE('',#26685,0.5);
#5126=CIRCLE('',#26686,0.5);
#5127=CIRCLE('',#26688,21.4999999999992);
#5128=CIRCLE('',#26689,21.4999999999992);
#5129=CIRCLE('',#26691,0.5);
#5130=CIRCLE('',#26692,0.5);
#5131=CIRCLE('',#26695,0.5);
#5132=CIRCLE('',#26696,0.5);
#5133=CIRCLE('',#26698,21.4999999999992);
#5134=CIRCLE('',#26699,21.4999999999992);
#5135=CIRCLE('',#26701,0.5);
#5136=CIRCLE('',#26702,0.5);
#5137=CIRCLE('',#26705,0.5);
#5138=CIRCLE('',#26706,0.5);
#5139=CIRCLE('',#26708,21.4999999999992);
#5140=CIRCLE('',#26709,21.4999999999992);
#5141=CIRCLE('',#26711,0.5);
#5142=CIRCLE('',#26712,0.5);
#5143=CIRCLE('',#26715,0.5);
#5144=CIRCLE('',#26716,0.5);
#5145=CIRCLE('',#26718,21.4999999999992);
#5146=CIRCLE('',#26719,21.4999999999992);
#5147=CIRCLE('',#26721,0.5);
#5148=CIRCLE('',#26722,0.5);
#5149=CIRCLE('',#26725,0.5);
#5150=CIRCLE('',#26726,0.5);
#5151=CIRCLE('',#26728,21.4999999999992);
#5152=CIRCLE('',#26729,21.4999999999992);
#5153=CIRCLE('',#26731,0.5);
#5154=CIRCLE('',#26732,0.5);
#5155=CIRCLE('',#26735,0.5);
#5156=CIRCLE('',#26736,0.5);
#5157=CIRCLE('',#26738,21.4999999999992);
#5158=CIRCLE('',#26739,21.4999999999992);
#5159=CIRCLE('',#26741,0.5);
#5160=CIRCLE('',#26742,0.5);
#5161=CIRCLE('',#26745,0.5);
#5162=CIRCLE('',#26746,0.5);
#5163=CIRCLE('',#26748,21.4999999999992);
#5164=CIRCLE('',#26749,21.4999999999992);
#5165=CIRCLE('',#26751,0.5);
#5166=CIRCLE('',#26752,0.5);
#5167=CIRCLE('',#26755,0.5);
#5168=CIRCLE('',#26756,0.5);
#5169=CIRCLE('',#26758,21.4999999999992);
#5170=CIRCLE('',#26759,21.4999999999992);
#5171=CIRCLE('',#26761,0.5);
#5172=CIRCLE('',#26762,0.5);
#5173=CIRCLE('',#26765,0.5);
#5174=CIRCLE('',#26766,0.5);
#5175=CIRCLE('',#26768,21.4999999999992);
#5176=CIRCLE('',#26769,21.4999999999992);
#5177=CIRCLE('',#26771,0.5);
#5178=CIRCLE('',#26772,0.5);
#5179=CIRCLE('',#26775,0.5);
#5180=CIRCLE('',#26776,0.5);
#5181=CIRCLE('',#26778,21.4999999999992);
#5182=CIRCLE('',#26779,21.4999999999992);
#5183=CIRCLE('',#26781,0.5);
#5184=CIRCLE('',#26782,0.5);
#5185=CIRCLE('',#26785,0.5);
#5186=CIRCLE('',#26786,0.5);
#5187=CIRCLE('',#26788,21.4999999999992);
#5188=CIRCLE('',#26789,21.4999999999992);
#5189=CIRCLE('',#26791,0.5);
#5190=CIRCLE('',#26792,0.5);
#5191=CIRCLE('',#26795,0.5);
#5192=CIRCLE('',#26796,0.5);
#5193=CIRCLE('',#26798,21.4999999999992);
#5194=CIRCLE('',#26799,21.4999999999992);
#5195=CIRCLE('',#26801,0.5);
#5196=CIRCLE('',#26802,0.5);
#5197=CIRCLE('',#26805,0.5);
#5198=CIRCLE('',#26806,0.5);
#5199=CIRCLE('',#26808,21.4999999999992);
#5200=CIRCLE('',#26809,21.4999999999992);
#5201=CIRCLE('',#26811,0.5);
#5202=CIRCLE('',#26812,0.5);
#5203=CIRCLE('',#26815,0.5);
#5204=CIRCLE('',#26816,0.5);
#5205=CIRCLE('',#26818,21.4999999999992);
#5206=CIRCLE('',#26819,21.4999999999992);
#5207=CIRCLE('',#26821,0.5);
#5208=CIRCLE('',#26822,0.5);
#5209=CIRCLE('',#26825,0.5);
#5210=CIRCLE('',#26826,0.5);
#5211=CIRCLE('',#26828,21.4999999999992);
#5212=CIRCLE('',#26829,21.4999999999992);
#5213=CIRCLE('',#26831,0.5);
#5214=CIRCLE('',#26832,0.5);
#5215=CIRCLE('',#26835,0.5);
#5216=CIRCLE('',#26836,0.5);
#5217=CIRCLE('',#26838,21.4999999999992);
#5218=CIRCLE('',#26839,21.4999999999992);
#5219=CIRCLE('',#26841,0.5);
#5220=CIRCLE('',#26842,0.5);
#5221=CIRCLE('',#26845,0.5);
#5222=CIRCLE('',#26846,0.5);
#5223=CIRCLE('',#26848,21.4999999999992);
#5224=CIRCLE('',#26849,21.4999999999992);
#5225=CIRCLE('',#26851,0.5);
#5226=CIRCLE('',#26852,0.5);
#5227=CIRCLE('',#26855,0.5);
#5228=CIRCLE('',#26856,0.5);
#5229=CIRCLE('',#26858,21.4999999999992);
#5230=CIRCLE('',#26859,21.4999999999992);
#5231=CIRCLE('',#26861,0.5);
#5232=CIRCLE('',#26862,0.5);
#5233=CIRCLE('',#26865,0.5);
#5234=CIRCLE('',#26866,0.5);
#5235=CIRCLE('',#26868,21.4999999999992);
#5236=CIRCLE('',#26869,21.4999999999992);
#5237=CIRCLE('',#26871,0.5);
#5238=CIRCLE('',#26872,0.5);
#5239=CIRCLE('',#26875,0.5);
#5240=CIRCLE('',#26876,0.5);
#5241=CIRCLE('',#26878,21.4999999999992);
#5242=CIRCLE('',#26879,21.4999999999992);
#5243=CIRCLE('',#26881,0.5);
#5244=CIRCLE('',#26882,0.5);
#5245=CIRCLE('',#26885,0.5);
#5246=CIRCLE('',#26886,0.5);
#5247=CIRCLE('',#26888,21.4999999999992);
#5248=CIRCLE('',#26889,21.4999999999992);
#5249=CIRCLE('',#26914,26.);
#5250=CIRCLE('',#26915,26.);
#5251=CIRCLE('',#26916,26.);
#5252=CIRCLE('',#26917,26.);
#5253=CIRCLE('',#26918,26.);
#5254=CIRCLE('',#26919,26.);
#5255=CIRCLE('',#26920,26.);
#5256=CIRCLE('',#26921,26.);
#5257=CIRCLE('',#26922,26.);
#5258=CIRCLE('',#26923,26.);
#5259=CIRCLE('',#26924,26.);
#5260=CIRCLE('',#26925,26.);
#5261=CIRCLE('',#26926,26.);
#5262=CIRCLE('',#26927,26.);
#5263=CIRCLE('',#26928,26.);
#5264=CIRCLE('',#26929,26.);
#5265=CIRCLE('',#26930,26.);
#5266=CIRCLE('',#26931,26.);
#5267=CIRCLE('',#26932,26.);
#5268=CIRCLE('',#26933,26.);
#5269=CIRCLE('',#26934,26.);
#5270=CIRCLE('',#26935,26.);
#5271=CIRCLE('',#26936,26.);
#5272=CIRCLE('',#26937,0.5);
#5273=CIRCLE('',#26938,21.4999999999992);
#5274=CIRCLE('',#26939,0.5);
#5275=CIRCLE('',#26940,26.);
#5276=CIRCLE('',#26941,7.);
#5277=CIRCLE('',#26943,26.);
#5278=CIRCLE('',#26944,0.5);
#5279=CIRCLE('',#26945,21.4999999999992);
#5280=CIRCLE('',#26946,0.5);
#5281=CIRCLE('',#26947,26.);
#5282=CIRCLE('',#26948,26.);
#5283=CIRCLE('',#26949,26.);
#5284=CIRCLE('',#26950,26.);
#5285=CIRCLE('',#26951,26.);
#5286=CIRCLE('',#26952,26.);
#5287=CIRCLE('',#26953,26.);
#5288=CIRCLE('',#26954,26.);
#5289=CIRCLE('',#26955,26.);
#5290=CIRCLE('',#26956,26.);
#5291=CIRCLE('',#26957,26.);
#5292=CIRCLE('',#26958,26.);
#5293=CIRCLE('',#26959,26.);
#5294=CIRCLE('',#26960,26.);
#5295=CIRCLE('',#26961,26.);
#5296=CIRCLE('',#26962,26.);
#5297=CIRCLE('',#26963,26.);
#5298=CIRCLE('',#26964,26.);
#5299=CIRCLE('',#26965,26.);
#5300=CIRCLE('',#26966,26.);
#5301=CIRCLE('',#26967,26.);
#5302=CIRCLE('',#26968,26.);
#5303=CIRCLE('',#26969,26.);
#5304=CIRCLE('',#26970,7.);
#5305=CIRCLE('',#27003,16.);
#5306=CIRCLE('',#27004,16.);
#5307=CIRCLE('',#27006,18.);
#5308=CIRCLE('',#27007,18.);
#5309=CIRCLE('',#27013,8.);
#5310=CIRCLE('',#27017,8.);
#5311=CIRCLE('',#27019,7.);
#5312=CIRCLE('',#27020,7.);
#5313=CIRCLE('',#27022,8.);
#5314=CIRCLE('',#27024,8.);
#5315=CIRCLE('',#27026,8.);
#5316=CIRCLE('',#27028,15.);
#5317=CIRCLE('',#27029,15.);
#5318=CIRCLE('',#27031,16.);
#5319=CIRCLE('',#27033,16.);
#5320=CIRCLE('',#27035,16.);
#5321=CIRCLE('',#27037,5.);
#5322=CIRCLE('',#27038,5.);
#5323=CIRCLE('',#27040,5.);
#5324=CIRCLE('',#27041,5.);
#5325=CIRCLE('',#27043,5.);
#5326=CIRCLE('',#27044,5.);
#5327=CIRCLE('',#27046,11.);
#5328=CIRCLE('',#27047,8.);
#5329=CIRCLE('',#27049,11.);
#5330=CIRCLE('',#27050,8.);
#5331=CIRCLE('',#27053,8.);
#5332=CIRCLE('',#27057,20.);
#5333=CIRCLE('',#27058,16.);
#5334=CIRCLE('',#27060,20.);
#5335=CIRCLE('',#27061,16.);
#5336=CIRCLE('',#27064,16.);
#5337=CIRCLE('',#27066,12.);
#5338=CIRCLE('',#27070,12.);
#5339=CIRCLE('',#27072,70.);
#5340=CIRCLE('',#27073,70.);
#5341=CIRCLE('',#27085,5.);
#5342=CIRCLE('',#27086,5.);
#5343=CIRCLE('',#27088,7.);
#5344=CIRCLE('',#27089,7.);
#5345=CIRCLE('',#27094,4.);
#5346=CIRCLE('',#27095,4.);
#5347=CIRCLE('',#27097,5.);
#5348=CIRCLE('',#27099,5.);
#5349=CIRCLE('',#27101,5.);
#5350=CIRCLE('',#27103,8.);
#5351=CIRCLE('',#27104,5.);
#5352=CIRCLE('',#27106,8.);
#5353=CIRCLE('',#27114,8.);
#5354=CIRCLE('',#27115,4.);
#5355=CIRCLE('',#27117,4.);
#5356=CIRCLE('',#27119,8.);
#5357=CIRCLE('',#27123,5.);
#5358=CIRCLE('',#27124,5.);
#5359=CIRCLE('',#27126,10.);
#5360=CIRCLE('',#27127,10.);
#5361=CIRCLE('',#27132,8.);
#5362=CIRCLE('',#27133,8.);
#5363=CIRCLE('',#27135,11.);
#5364=CIRCLE('',#27136,11.);
#5365=CIRCLE('',#27141,16.);
#5366=CIRCLE('',#27142,16.);
#5367=CIRCLE('',#27144,20.);
#5368=CIRCLE('',#27145,20.);
#5369=CIRCLE('',#27152,11.);
#5370=CIRCLE('',#27153,7.);
#5371=CIRCLE('',#27155,7.);
#5372=CIRCLE('',#27157,11.);
#5373=CIRCLE('',#27163,20.);
#5374=CIRCLE('',#27164,15.);
#5375=CIRCLE('',#27166,15.);
#5376=CIRCLE('',#27168,20.);
#5377=CIRCLE('',#27172,2.);
#5378=CIRCLE('',#27173,2.);
#5379=CIRCLE('',#27178,2.942);
#5380=CIRCLE('',#27199,2.37175);
#5381=CIRCLE('',#27220,2.37175);
#5382=CIRCLE('',#27222,2.942);
#5383=CIRCLE('',#27231,5.);
#5384=CIRCLE('',#27233,5.);
#5385=B_SPLINE_CURVE_WITH_KNOTS('',3,(#32412,#32413,#32414,#32415),
 .UNSPECIFIED.,.F.,.F.,(4,4),(95.5573427486707,96.2647245007224),
 .UNSPECIFIED.);
#5386=B_SPLINE_CURVE_WITH_KNOTS('',3,(#32423,#32424,#32425,#32426,#32427,
#32428,#32429,#32430,#32431,#32432),.UNSPECIFIED.,.F.,.F.,(4,3,3,4),(-94.2477796076938,
-93.2874649800815,-92.2950451398679,-91.8135687061554),.UNSPECIFIED.);
#5387=B_SPLINE_CURVE_WITH_KNOTS('',3,(#32437,#32438,#32439,#32440,#32441,
#32442,#32443,#32444,#32445,#32446,#32447,#32448,#32449,#32450,#32451,#32452,
#32453,#32454,#32455,#32456,#32457,#32458,#32459,#32460,#32461),
 .UNSPECIFIED.,.F.,.F.,(4,3,3,3,3,3,3,3,4),(89.2741574414911,89.317785619227,
90.3102054594406,91.3026252996542,92.2950451398679,93.2874649800815,94.2798848202951,
95.2723046605088,95.5573427486707),.UNSPECIFIED.);
#5388=B_SPLINE_CURVE_WITH_KNOTS('',3,(#32462,#32463,#32464,#32465,#32466,
#32467,#32468,#32469,#32470,#32471,#32472,#32473,#32474,#32475,#32476,#32477,
#32478,#32479,#32480,#32481,#32482,#32483),.UNSPECIFIED.,.F.,.F.,(4,3,3,
3,3,3,3,4),(-91.8135687061554,-91.3026252996542,-90.3102054594406,-89.317785619227,
-88.3253657790133,-87.3329459387997,-86.3405260985861,-85.5303833989757),
 .UNSPECIFIED.);
#5389=B_SPLINE_CURVE_WITH_KNOTS('',3,(#32488,#32489,#32490,#32491,#32492,
#32493,#32494,#32495,#32496,#32497,#32498,#32499,#32500,#32501,#32502,#32503,
#32504,#32505,#32506,#32507,#32508,#32509),.UNSPECIFIED.,.F.,.F.,(4,3,3,
3,3,3,3,4),(82.9909721343116,83.3632665779452,84.3556864181588,85.3481062583724,
86.3405260985861,87.3329459387997,88.3253657790133,89.2741574414911),
 .UNSPECIFIED.);
#5390=B_SPLINE_CURVE_WITH_KNOTS('',3,(#32510,#32511,#32512,#32513,#32514,
#32515,#32516,#32517,#32518,#32519,#32520,#32521,#32522,#32523,#32524,#32525,
#32526,#32527,#32528,#32529,#32530,#32531,#32532,#32533,#32534),
 .UNSPECIFIED.,.F.,.F.,(4,3,3,3,3,3,3,3,4),(-85.5303833989757,-85.3481062583724,
-84.3556864181588,-83.3632665779452,-82.3708467377315,-81.3784268975179,
-80.3860070573043,-79.3935872170906,-79.2471980917961),.UNSPECIFIED.);
#5391=B_SPLINE_CURVE_WITH_KNOTS('',3,(#32539,#32540,#32541,#32542,#32543,
#32544,#32545,#32546,#32547,#32548,#32549,#32550,#32551,#32552,#32553,#32554,
#32555,#32556,#32557,#32558,#32559,#32560),.UNSPECIFIED.,.F.,.F.,(4,3,3,
3,3,3,3,4),(76.7077868271319,77.4087475366634,78.401167376877,79.3935872170906,
80.3860070573043,81.3784268975179,82.3708467377315,82.9909721343116),
 .UNSPECIFIED.);
#5392=B_SPLINE_CURVE_WITH_KNOTS('',3,(#32561,#32562,#32563,#32564,#32565,
#32566,#32567,#32568,#32569,#32570,#32571,#32572,#32573,#32574,#32575,#32576,
#32577,#32578,#32579,#32580,#32581,#32582),.UNSPECIFIED.,.F.,.F.,(4,3,3,
3,3,3,3,4),(-79.2471980917961,-78.401167376877,-77.4087475366633,-76.4163276964497,
-75.4239078562361,-74.4314880160224,-73.4390681758088,-72.9640127846165),
 .UNSPECIFIED.);
#5393=B_SPLINE_CURVE_WITH_KNOTS('',3,(#32587,#32588,#32589,#32590,#32591,
#32592,#32593,#32594,#32595,#32596,#32597,#32598,#32599,#32600,#32601,#32602,
#32603,#32604,#32605,#32606,#32607,#32608,#32609,#32610,#32611),
 .UNSPECIFIED.,.F.,.F.,(4,3,3,3,3,3,3,3,4),(70.4246015199523,70.4618086551679,
71.4542284953816,72.4466483355952,73.4390681758088,74.4314880160225,75.4239078562361,
76.4163276964497,76.7077868271319),.UNSPECIFIED.);
#5394=B_SPLINE_CURVE_WITH_KNOTS('',3,(#32612,#32613,#32614,#32615,#32616,
#32617,#32618,#32619,#32620,#32621,#32622,#32623,#32624,#32625,#32626,#32627,
#32628,#32629,#32630,#32631,#32632,#32633),.UNSPECIFIED.,.F.,.F.,(4,3,3,
3,3,3,3,4),(-72.9640127846165,-72.4466483355952,-71.4542284953815,-70.4618086551679,
-69.4693888149543,-68.4769689747406,-67.484549134527,-66.680827477437),
 .UNSPECIFIED.);
#5395=B_SPLINE_CURVE_WITH_KNOTS('',3,(#32638,#32639,#32640,#32641,#32642,
#32643,#32644,#32645,#32646,#32647,#32648,#32649,#32650,#32651,#32652,#32653,
#32654,#32655,#32656,#32657,#32658,#32659),.UNSPECIFIED.,.F.,.F.,(4,3,3,
3,3,3,3,4),(64.1414162127728,64.5072896138861,65.4997094540998,66.4921292943134,
67.484549134527,68.4769689747407,69.4693888149543,70.4246015199523),
 .UNSPECIFIED.);
#5396=B_SPLINE_CURVE_WITH_KNOTS('',3,(#32660,#32661,#32662,#32663,#32664,
#32665,#32666,#32667,#32668,#32669,#32670,#32671,#32672,#32673,#32674,#32675,
#32676,#32677,#32678,#32679,#32680,#32681,#32682,#32683,#32684),
 .UNSPECIFIED.,.F.,.F.,(4,3,3,3,3,3,3,3,4),(-66.680827477437,-66.4921292943134,
-65.4997094540998,-64.5072896138861,-63.5148697736725,-62.5224499334589,
-61.5300300932452,-60.5376102530316,-60.3976421702573),.UNSPECIFIED.);
#5397=B_SPLINE_CURVE_WITH_KNOTS('',3,(#32689,#32690,#32691,#32692,#32693,
#32694,#32695,#32696,#32697,#32698,#32699,#32700,#32701,#32702,#32703,#32704,
#32705,#32706,#32707,#32708,#32709,#32710),.UNSPECIFIED.,.F.,.F.,(4,3,3,
3,3,3,3,4),(57.8582309055932,58.5527705726043,59.545190412818,60.5376102530316,
61.5300300932452,62.5224499334589,63.5148697736725,64.1414162127728),
 .UNSPECIFIED.);
#5398=B_SPLINE_CURVE_WITH_KNOTS('',3,(#32711,#32712,#32713,#32714,#32715,
#32716,#32717,#32718,#32719,#32720,#32721,#32722,#32723,#32724,#32725,#32726,
#32727,#32728,#32729,#32730,#32731,#32732),.UNSPECIFIED.,.F.,.F.,(4,3,3,
3,3,3,3,4),(-60.3976421702573,-59.545190412818,-58.5527705726043,-57.5603507323907,
-56.5679308921771,-55.5755110519634,-54.5830912117498,-54.1144568630777),
 .UNSPECIFIED.);
#5399=B_SPLINE_CURVE_WITH_KNOTS('',3,(#32737,#32738,#32739,#32740,#32741,
#32742,#32743,#32744,#32745,#32746,#32747,#32748,#32749,#32750,#32751,#32752,
#32753,#32754,#32755,#32756,#32757,#32758,#32759,#32760,#32761),
 .UNSPECIFIED.,.F.,.F.,(4,3,3,3,3,3,3,3,4),(51.5750455984135,51.6058316911089,
52.5982515313225,53.5906713715362,54.5830912117498,55.5755110519634,56.5679308921771,
57.5603507323907,57.8582309055932),.UNSPECIFIED.);
#5400=B_SPLINE_CURVE_WITH_KNOTS('',3,(#32762,#32763,#32764,#32765,#32766,
#32767,#32768,#32769,#32770,#32771,#32772,#32773,#32774,#32775,#32776,#32777,
#32778,#32779,#32780,#32781,#32782,#32783),.UNSPECIFIED.,.F.,.F.,(4,3,3,
3,3,3,3,4),(-54.1144568630777,-53.5906713715362,-52.5982515313225,-51.6058316911089,
-50.6134118508953,-49.6209920106816,-48.628572170468,-47.8312715558982),
 .UNSPECIFIED.);
#5401=B_SPLINE_CURVE_WITH_KNOTS('',3,(#32788,#32789,#32790,#32791,#32792,
#32793,#32794,#32795,#32796,#32797,#32798,#32799,#32800,#32801,#32802,#32803,
#32804,#32805,#32806,#32807,#32808,#32809),.UNSPECIFIED.,.F.,.F.,(4,3,3,
3,3,3,3,4),(45.291860291234,45.6513126498271,46.6437324900407,47.6361523302544,
48.628572170468,49.6209920106816,50.6134118508953,51.5750455984135),
 .UNSPECIFIED.);
#5402=B_SPLINE_CURVE_WITH_KNOTS('',3,(#32810,#32811,#32812,#32813,#32814,
#32815,#32816,#32817,#32818,#32819,#32820,#32821,#32822,#32823,#32824,#32825,
#32826,#32827,#32828,#32829,#32830,#32831,#32832,#32833,#32834),
 .UNSPECIFIED.,.F.,.F.,(4,3,3,3,3,3,3,3,4),(-47.8312715558982,-47.6361523302544,
-46.6437324900407,-45.6513126498271,-44.6588928096135,-43.6664729693998,
-42.6740531291862,-41.6816332889726,-41.5480862487186),.UNSPECIFIED.);
#5403=B_SPLINE_CURVE_WITH_KNOTS('',3,(#32839,#32840,#32841,#32842,#32843,
#32844,#32845,#32846,#32847,#32848,#32849,#32850,#32851,#32852,#32853,#32854,
#32855,#32856,#32857,#32858,#32859,#32860),.UNSPECIFIED.,.F.,.F.,(4,3,3,
3,3,3,3,4),(39.0086749840544,39.6967936085453,40.6892134487589,41.6816332889726,
42.6740531291862,43.6664729693998,44.6588928096135,45.291860291234),
 .UNSPECIFIED.);
#5404=B_SPLINE_CURVE_WITH_KNOTS('',3,(#32861,#32862,#32863,#32864,#32865,
#32866,#32867,#32868,#32869,#32870,#32871,#32872,#32873,#32874,#32875,#32876,
#32877,#32878,#32879,#32880,#32881,#32882),.UNSPECIFIED.,.F.,.F.,(4,3,3,
3,3,3,3,4),(-41.5480862487186,-40.6892134487589,-39.6967936085453,-38.7043737683317,
-37.711953928118,-36.7195340879044,-35.7271142476908,-35.2649009415389),
 .UNSPECIFIED.);
#5405=B_SPLINE_CURVE_WITH_KNOTS('',3,(#32887,#32888,#32889,#32890,#32891,
#32892,#32893,#32894,#32895,#32896,#32897,#32898,#32899,#32900,#32901,#32902,
#32903,#32904,#32905,#32906,#32907,#32908,#32909,#32910,#32911),
 .UNSPECIFIED.,.F.,.F.,(4,3,3,3,3,3,3,3,4),(32.7254896768748,32.7498547270499,
33.7422745672635,34.7346944074771,35.7271142476908,36.7195340879044,37.711953928118,
38.7043737683317,39.0086749840544),.UNSPECIFIED.);
#5406=B_SPLINE_CURVE_WITH_KNOTS('',3,(#32912,#32913,#32914,#32915,#32916,
#32917,#32918,#32919,#32920,#32921,#32922,#32923,#32924,#32925,#32926,#32927,
#32928,#32929,#32930,#32931,#32932,#32933),.UNSPECIFIED.,.F.,.F.,(4,3,3,
3,3,3,3,4),(-35.2649009415389,-34.7346944074771,-33.7422745672635,-32.7498547270499,
-31.7574348868362,-30.7650150466226,-29.772595206409,-28.9817156343594),
 .UNSPECIFIED.);
#5407=B_SPLINE_CURVE_WITH_KNOTS('',3,(#32938,#32939,#32940,#32941,#32942,
#32943,#32944,#32945,#32946,#32947,#32948,#32949,#32950,#32951,#32952,#32953,
#32954,#32955,#32956,#32957,#32958,#32959),.UNSPECIFIED.,.F.,.F.,(4,3,3,
3,3,3,3,4),(26.4423043696952,26.7953356857681,27.7877555259817,28.7801753661954,
29.772595206409,30.7650150466226,31.7574348868363,32.7254896768748),
 .UNSPECIFIED.);
#5408=B_SPLINE_CURVE_WITH_KNOTS('',3,(#32960,#32961,#32962,#32963,#32964,
#32965,#32966,#32967,#32968,#32969,#32970,#32971,#32972,#32973,#32974,#32975,
#32976,#32977,#32978,#32979,#32980,#32981,#32982,#32983,#32984),
 .UNSPECIFIED.,.F.,.F.,(4,3,3,3,3,3,3,3,4),(-28.9817156343594,-28.7801753661953,
-27.7877555259817,-26.7953356857681,-25.8029158455544,-24.8104960053408,
-23.8180761651272,-22.8256563249135,-22.6985303271798),.UNSPECIFIED.);
#5409=B_SPLINE_CURVE_WITH_KNOTS('',3,(#32989,#32990,#32991,#32992,#32993,
#32994,#32995,#32996,#32997,#32998,#32999,#33000,#33001,#33002,#33003,#33004,
#33005,#33006,#33007,#33008,#33009,#33010),.UNSPECIFIED.,.F.,.F.,(4,3,3,
3,3,3,3,4),(20.1591190625156,20.8408166444863,21.8332364846999,22.8256563249136,
23.8180761651272,24.8104960053408,25.8029158455545,26.4423043696952),
 .UNSPECIFIED.);
#5410=B_SPLINE_CURVE_WITH_KNOTS('',3,(#33011,#33012,#33013,#33014,#33015,
#33016,#33017,#33018,#33019,#33020,#33021,#33022,#33023,#33024,#33025,#33026,
#33027,#33028,#33029,#33030,#33031,#33032),.UNSPECIFIED.,.F.,.F.,(4,3,3,
3,3,3,3,4),(-22.6985303271798,-21.8332364846999,-20.8408166444863,-19.8483968042727,
-18.855976964059,-17.8635571238454,-16.8711372836318,-16.4153450200002),
 .UNSPECIFIED.);
#5411=B_SPLINE_CURVE_WITH_KNOTS('',3,(#33037,#33038,#33039,#33040,#33041,
#33042,#33043,#33044,#33045,#33046,#33047,#33048,#33049,#33050,#33051,#33052,
#33053,#33054,#33055,#33056,#33057,#33058,#33059,#33060,#33061),
 .UNSPECIFIED.,.F.,.F.,(4,3,3,3,3,3,3,3,4),(13.875933755336,13.8938777629909,
14.8862976032045,15.8787174434181,16.8711372836318,17.8635571238454,18.855976964059,
19.8483968042727,20.1591190625156),.UNSPECIFIED.);
#5412=B_SPLINE_CURVE_WITH_KNOTS('',3,(#33062,#33063,#33064,#33065,#33066,
#33067,#33068,#33069,#33070,#33071,#33072,#33073,#33074,#33075,#33076,#33077,
#33078,#33079,#33080,#33081,#33082,#33083),.UNSPECIFIED.,.F.,.F.,(4,3,3,
3,3,3,3,4),(-16.4153450200002,-15.8787174434181,-14.8862976032045,-13.8938777629909,
-12.9014579227772,-11.9090380825636,-10.91661824235,-10.1321597128207),
 .UNSPECIFIED.);
#5413=B_SPLINE_CURVE_WITH_KNOTS('',3,(#33089,#33090,#33091,#33092,#33093,
#33094,#33095,#33096,#33097,#33098,#33099,#33100,#33101),.UNSPECIFIED.,
 .F.,.F.,(4,3,3,3,4),(-3.848974405641,-2.9772595206409,-1.98483968042726,
-0.992419840213632,0.),.UNSPECIFIED.);
#5414=B_SPLINE_CURVE_WITH_KNOTS('',3,(#33104,#33105,#33106,#33107,#33108,
#33109,#33110,#33111,#33112,#33113,#33114,#33115,#33116,#33117,#33118,#33119,
#33120,#33121,#33122),.UNSPECIFIED.,.F.,.F.,(4,3,3,3,3,3,4),(2.01694489302852,
2.9772595206409,3.96967936085453,4.96209920106817,5.9545190412818,6.94693888149543,
7.59274844815647),.UNSPECIFIED.);
#5415=B_SPLINE_CURVE_WITH_KNOTS('',3,(#33128,#33129,#33130,#33131,#33132,
#33133,#33134,#33135),.UNSPECIFIED.,.F.,.F.,(4,1,1,1,1,4),(103.672557568463,
104.154034002176,105.146453842389,106.138873682603,107.131293522817,108.12371336303),
 .UNSPECIFIED.);
#5416=B_SPLINE_CURVE_WITH_KNOTS('',3,(#33138,#33139,#33140,#33141,#33142,
#33143,#33144,#33145,#33146),.UNSPECIFIED.,.F.,.F.,(4,1,1,1,1,1,4),(103.672557568463,
103.716185746199,104.708605586413,105.701025426626,106.69344526684,107.685865107053,
108.646179734666),.UNSPECIFIED.);
#5417=B_SPLINE_CURVE_WITH_KNOTS('',3,(#33151,#33152,#33153,#33154,#33155,
#33156,#33157,#33158,#33159,#33160),.UNSPECIFIED.,.F.,.F.,(4,1,1,1,1,1,
1,4),(97.3893722612835,98.1995149608939,99.1919348011075,100.184354641321,
101.176774481535,102.169194321748,103.161614161962,103.672557568463),
 .UNSPECIFIED.);
#5418=B_SPLINE_CURVE_WITH_KNOTS('',3,(#33161,#33162,#33163,#33164,#33165,
#33166,#33167,#33168,#33169,#33170),.UNSPECIFIED.,.F.,.F.,(4,1,1,1,1,1,
1,4),(97.3893722612835,97.7616667049171,98.7540865451307,99.7465063853444,
100.738926225558,101.731346065772,102.723765905985,103.672557568463),
 .UNSPECIFIED.);
#5419=B_SPLINE_CURVE_WITH_KNOTS('',3,(#33175,#33176,#33177,#33178,#33179,
#33180,#33181,#33182,#33183,#33184,#33185),.UNSPECIFIED.,.F.,.F.,(4,1,1,
1,1,1,1,1,4),(91.106186954104,91.2525760793984,92.2449959196121,93.2374157598257,
94.2298356000393,95.222255440253,96.2146752804666,97.2070951206802,97.3893722612835),
 .UNSPECIFIED.);
#5420=B_SPLINE_CURVE_WITH_KNOTS('',3,(#33186,#33187,#33188,#33189,#33190,
#33191,#33192,#33193,#33194,#33195),.UNSPECIFIED.,.F.,.F.,(4,1,1,1,1,1,
1,4),(91.106186954104,91.8071476636353,92.7995675038489,93.7919873440626,
94.7844071842762,95.7768270244898,96.7692468647035,97.3893722612835),
 .UNSPECIFIED.);
#5421=B_SPLINE_CURVE_WITH_KNOTS('',3,(#33200,#33201,#33202,#33203,#33204,
#33205,#33206,#33207,#33208,#33209),.UNSPECIFIED.,.F.,.F.,(4,1,1,1,1,1,
1,4),(84.8230016469244,85.2980570381166,86.2904768783303,87.2828967185439,
88.2753165587575,89.2677363989712,90.2601562391848,91.106186954104),
 .UNSPECIFIED.);
#5422=B_SPLINE_CURVE_WITH_KNOTS('',3,(#33210,#33211,#33212,#33213,#33214,
#33215,#33216,#33217,#33218,#33219,#33220),.UNSPECIFIED.,.F.,.F.,(4,1,1,
1,1,1,1,1,4),(84.8230016469244,84.8602087821399,85.8526286223535,86.8450484625671,
87.8374683027808,88.8298881429944,89.822307983208,90.8147278234217,91.106186954104),
 .UNSPECIFIED.);
#5423=B_SPLINE_CURVE_WITH_KNOTS('',3,(#33225,#33226,#33227,#33228,#33229,
#33230,#33231,#33232,#33233,#33234),.UNSPECIFIED.,.F.,.F.,(4,1,1,1,1,1,
1,4),(78.5398163397448,79.3435379968348,80.3359578370485,81.3283776772621,
82.3207975174757,83.3132173576894,84.305637197903,84.8230016469244),
 .UNSPECIFIED.);
#5424=B_SPLINE_CURVE_WITH_KNOTS('',3,(#33235,#33236,#33237,#33238,#33239,
#33240,#33241,#33242,#33243,#33244),.UNSPECIFIED.,.F.,.F.,(4,1,1,1,1,1,
1,4),(78.5398163397448,78.9056897408581,79.8981095810717,80.8905294212853,
81.882949261499,82.8753691017126,83.8677889419262,84.8230016469244),
 .UNSPECIFIED.);
#5425=B_SPLINE_CURVE_WITH_KNOTS('',3,(#33249,#33250,#33251,#33252,#33253,
#33254,#33255,#33256,#33257,#33258,#33259),.UNSPECIFIED.,.F.,.F.,(4,1,1,
1,1,1,1,1,4),(72.2566310325653,72.3965991153394,73.389018955553,74.3814387957667,
75.3738586359803,76.3662784761939,77.3586983164076,78.3511181566212,78.5398163397448),
 .UNSPECIFIED.);
#5426=B_SPLINE_CURVE_WITH_KNOTS('',3,(#33260,#33261,#33262,#33263,#33264,
#33265,#33266,#33267,#33268,#33269),.UNSPECIFIED.,.F.,.F.,(4,1,1,1,1,1,
1,4),(72.2566310325651,72.9511706995763,73.9435905397899,74.9360103800035,
75.9284302202172,76.9208500604308,77.9132699006444,78.5398163397448),
 .UNSPECIFIED.);
#5427=B_SPLINE_CURVE_WITH_KNOTS('',3,(#33274,#33275,#33276,#33277,#33278,
#33279,#33280,#33281,#33282,#33283),.UNSPECIFIED.,.F.,.F.,(4,1,1,1,1,1,
1,4),(65.9734457253856,66.4420800740576,67.4344999142712,68.4269197544849,
69.4193395946985,70.4117594349121,71.4041792751258,72.2566310325653),
 .UNSPECIFIED.);
#5428=B_SPLINE_CURVE_WITH_KNOTS('',3,(#33284,#33285,#33286,#33287,#33288,
#33289,#33290,#33291,#33292,#33293,#33294),.UNSPECIFIED.,.F.,.F.,(4,1,1,
1,1,1,1,1,4),(65.9734457253856,66.0042318180808,66.9966516582945,67.9890714985081,
68.9814913387217,69.9739111789354,70.966331019149,71.9587508593626,72.2566310325651),
 .UNSPECIFIED.);
#5429=B_SPLINE_CURVE_WITH_KNOTS('',3,(#33299,#33300,#33301,#33302,#33303,
#33304,#33305,#33306,#33307,#33308),.UNSPECIFIED.,.F.,.F.,(4,1,1,1,1,1,
1,4),(59.690260418206,60.4875610327758,61.4799808729895,62.4724007132031,
63.4648205534167,64.4572403936303,65.449660233844,65.9734457253856),
 .UNSPECIFIED.);
#5430=B_SPLINE_CURVE_WITH_KNOTS('',3,(#33309,#33310,#33311,#33312,#33313,
#33314,#33315,#33316,#33317,#33318),.UNSPECIFIED.,.F.,.F.,(4,1,1,1,1,1,
1,4),(59.690260418206,60.049712776799,61.0421326170127,62.0345524572263,
63.0269722974399,64.0193921376536,65.0118119778672,65.9734457253856),
 .UNSPECIFIED.);
#5431=B_SPLINE_CURVE_WITH_KNOTS('',3,(#33323,#33324,#33325,#33326,#33327,
#33328,#33329,#33330,#33331,#33332,#33333),.UNSPECIFIED.,.F.,.F.,(4,1,1,
1,1,1,1,1,4),(53.4070751110265,53.5406221512804,54.533041991494,55.5254618317077,
56.5178816719213,57.5103015121349,58.5027213523486,59.4951411925622,59.690260418206),
 .UNSPECIFIED.);
#5432=B_SPLINE_CURVE_WITH_KNOTS('',3,(#33334,#33335,#33336,#33337,#33338,
#33339,#33340,#33341,#33342,#33343),.UNSPECIFIED.,.F.,.F.,(4,1,1,1,1,1,
1,4),(53.4070751110265,54.0951937355172,55.0876135757309,56.0800334159445,
57.0724532561581,58.0648730963718,59.0572929365854,59.690260418206),
 .UNSPECIFIED.);
#5433=B_SPLINE_CURVE_WITH_KNOTS('',3,(#33348,#33349,#33350,#33351,#33352,
#33353,#33354,#33355,#33356,#33357),.UNSPECIFIED.,.F.,.F.,(4,1,1,1,1,1,
1,4),(47.1238898038468,47.5861031099986,48.5785229502122,49.5709427904259,
50.5633626306395,51.5557824708531,52.5482023110668,53.4070751110265),
 .UNSPECIFIED.);
#5434=B_SPLINE_CURVE_WITH_KNOTS('',3,(#33358,#33359,#33360,#33361,#33362,
#33363,#33364,#33365,#33366,#33367,#33368),.UNSPECIFIED.,.F.,.F.,(4,1,1,
1,1,1,1,1,4),(47.1238898038468,47.1482548540218,48.1406746942354,49.1330945344491,
50.1255143746627,51.1179342148763,52.11035405509,53.1027738953036,53.4070751110265),
 .UNSPECIFIED.);
#5435=B_SPLINE_CURVE_WITH_KNOTS('',3,(#33373,#33374,#33375,#33376,#33377,
#33378,#33379,#33380,#33381,#33382),.UNSPECIFIED.,.F.,.F.,(4,1,1,1,1,1,
1,4),(40.8407044966672,41.6315840687168,42.6240039089304,43.6164237491441,
44.6088435893577,45.6012634295713,46.593683269785,47.1238898038468),
 .UNSPECIFIED.);
#5436=B_SPLINE_CURVE_WITH_KNOTS('',3,(#33383,#33384,#33385,#33386,#33387,
#33388,#33389,#33390,#33391,#33392),.UNSPECIFIED.,.F.,.F.,(4,1,1,1,1,1,
1,4),(40.8407044966672,41.19373581274,42.1861556529536,43.1785754931673,
44.1709953333809,45.1634151735945,46.1558350138082,47.1238898038468),
 .UNSPECIFIED.);
#5437=B_SPLINE_CURVE_WITH_KNOTS('',3,(#33397,#33398,#33399,#33400,#33401,
#33402,#33403,#33404,#33405,#33406,#33407),.UNSPECIFIED.,.F.,.F.,(4,1,1,
1,1,1,1,1,4),(34.5575191894877,34.6846451872214,35.677065027435,36.6694848676486,
37.6619047078623,38.6543245480759,39.6467443882895,40.6391642285032,40.8407044966672),
 .UNSPECIFIED.);
#5438=B_SPLINE_CURVE_WITH_KNOTS('',3,(#33408,#33409,#33410,#33411,#33412,
#33413,#33414,#33415,#33416,#33417),.UNSPECIFIED.,.F.,.F.,(4,1,1,1,1,1,
1,4),(34.5575191894877,35.2392167714582,36.2316366116718,37.2240564518855,
38.2164762920991,39.2088961323127,40.2013159725264,40.8407044966672),
 .UNSPECIFIED.);
#5439=B_SPLINE_CURVE_WITH_KNOTS('',3,(#33422,#33423,#33424,#33425,#33426,
#33427,#33428,#33429,#33430,#33431),.UNSPECIFIED.,.F.,.F.,(4,1,1,1,1,1,
1,4),(28.2743338823081,28.7301261459396,29.7225459861532,30.7149658263668,
31.7073856665805,32.6998055067941,33.6922253470077,34.5575191894877),
 .UNSPECIFIED.);
#5440=B_SPLINE_CURVE_WITH_KNOTS('',3,(#33432,#33433,#33434,#33435,#33436,
#33437,#33438,#33439,#33440,#33441,#33442),.UNSPECIFIED.,.F.,.F.,(4,1,1,
1,1,1,1,1,4),(28.2743338823081,28.2922778899628,29.2846977301764,30.2771175703901,
31.2695374106037,32.2619572508173,33.2543770910309,34.2467969312446,34.5575191894877),
 .UNSPECIFIED.);
#5441=B_SPLINE_CURVE_WITH_KNOTS('',3,(#33447,#33448,#33449,#33450,#33451,
#33452,#33453,#33454,#33455,#33456),.UNSPECIFIED.,.F.,.F.,(4,1,1,1,1,1,
1,4),(21.9911485751285,22.7756071046578,23.7680269448714,24.760446785085,
25.7528666252987,26.7452864655123,27.7377063057259,28.2743338823081),
 .UNSPECIFIED.);
#5442=B_SPLINE_CURVE_WITH_KNOTS('',3,(#33457,#33458,#33459,#33460,#33461,
#33462,#33463,#33464,#33465,#33466),.UNSPECIFIED.,.F.,.F.,(4,1,1,1,1,1,
1,4),(21.9911485751284,22.337758848681,23.3301786888946,24.3225985291083,
25.3150183693219,26.3074382095355,27.2998580497492,28.2743338823081),
 .UNSPECIFIED.);
#5443=B_SPLINE_CURVE_WITH_KNOTS('',3,(#33472,#33473,#33474,#33475,#33476),
 .UNSPECIFIED.,.F.,.F.,(4,1,4),(14.3984001269719,15.3908199671856,15.7079632679489),
 .UNSPECIFIED.);
#5444=B_SPLINE_CURVE_WITH_KNOTS('',3,(#33479,#33480,#33481,#33482,#33483),
 .UNSPECIFIED.,.F.,.F.,(4,1,4),(13.8759337553364,14.8362483829487,15.7079632679489),
 .UNSPECIFIED.);
#5445=B_SPLINE_CURVE_WITH_KNOTS('',3,(#33489,#33490,#33491,#33492),
 .UNSPECIFIED.,.F.,.F.,(4,4),(95.5573427486707,96.2647245007224),
 .UNSPECIFIED.);
#5446=B_SPLINE_CURVE_WITH_KNOTS('',3,(#33500,#33501,#33502,#33503,#33504,
#33505,#33506,#33507,#33508,#33509),.UNSPECIFIED.,.F.,.F.,(4,3,3,4),(-94.2477796076938,
-93.2874649800815,-92.2950451398678,-91.8135687061554),.UNSPECIFIED.);
#5447=B_SPLINE_CURVE_WITH_KNOTS('',3,(#33514,#33515,#33516,#33517,#33518,
#33519,#33520,#33521,#33522,#33523,#33524,#33525,#33526,#33527,#33528,#33529,
#33530,#33531,#33532,#33533,#33534,#33535,#33536,#33537,#33538),
 .UNSPECIFIED.,.F.,.F.,(4,3,3,3,3,3,3,3,4),(89.2741574414911,89.317785619227,
90.3102054594406,91.3026252996542,92.2950451398679,93.2874649800815,94.2798848202951,
95.2723046605088,95.5573427486707),.UNSPECIFIED.);
#5448=B_SPLINE_CURVE_WITH_KNOTS('',3,(#33539,#33540,#33541,#33542,#33543,
#33544,#33545,#33546,#33547,#33548,#33549,#33550,#33551,#33552,#33553,#33554,
#33555,#33556,#33557,#33558,#33559,#33560),.UNSPECIFIED.,.F.,.F.,(4,3,3,
3,3,3,3,4),(-91.8135687061554,-91.3026252996542,-90.3102054594406,-89.3177856192269,
-88.3253657790133,-87.3329459387997,-86.3405260985861,-85.5303833989757),
 .UNSPECIFIED.);
#5449=B_SPLINE_CURVE_WITH_KNOTS('',3,(#33565,#33566,#33567,#33568,#33569,
#33570,#33571,#33572,#33573,#33574,#33575,#33576,#33577,#33578,#33579,#33580,
#33581,#33582,#33583,#33584,#33585,#33586),.UNSPECIFIED.,.F.,.F.,(4,3,3,
3,3,3,3,4),(82.9909721343116,83.3632665779452,84.3556864181588,85.3481062583724,
86.3405260985861,87.3329459387997,88.3253657790133,89.2741574414911),
 .UNSPECIFIED.);
#5450=B_SPLINE_CURVE_WITH_KNOTS('',3,(#33587,#33588,#33589,#33590,#33591,
#33592,#33593,#33594,#33595,#33596,#33597,#33598,#33599,#33600,#33601,#33602,
#33603,#33604,#33605,#33606,#33607,#33608,#33609,#33610,#33611),
 .UNSPECIFIED.,.F.,.F.,(4,3,3,3,3,3,3,3,4),(-85.5303833989757,-85.3481062583724,
-84.3556864181588,-83.3632665779452,-82.3708467377315,-81.3784268975179,
-80.3860070573042,-79.3935872170906,-79.2471980917961),.UNSPECIFIED.);
#5451=B_SPLINE_CURVE_WITH_KNOTS('',3,(#33616,#33617,#33618,#33619,#33620,
#33621,#33622,#33623,#33624,#33625,#33626,#33627,#33628,#33629,#33630,#33631,
#33632,#33633,#33634,#33635,#33636,#33637),.UNSPECIFIED.,.F.,.F.,(4,3,3,
3,3,3,3,4),(76.7077868271319,77.4087475366634,78.401167376877,79.3935872170907,
80.3860070573043,81.3784268975179,82.3708467377316,82.9909721343116),
 .UNSPECIFIED.);
#5452=B_SPLINE_CURVE_WITH_KNOTS('',3,(#33638,#33639,#33640,#33641,#33642,
#33643,#33644,#33645,#33646,#33647,#33648,#33649,#33650,#33651,#33652,#33653,
#33654,#33655,#33656,#33657,#33658,#33659),.UNSPECIFIED.,.F.,.F.,(4,3,3,
3,3,3,3,4),(-79.2471980917961,-78.401167376877,-77.4087475366634,-76.4163276964497,
-75.4239078562361,-74.4314880160224,-73.4390681758088,-72.9640127846165),
 .UNSPECIFIED.);
#5453=B_SPLINE_CURVE_WITH_KNOTS('',3,(#33664,#33665,#33666,#33667,#33668,
#33669,#33670,#33671,#33672,#33673,#33674,#33675,#33676,#33677,#33678,#33679,
#33680,#33681,#33682,#33683,#33684,#33685,#33686,#33687,#33688),
 .UNSPECIFIED.,.F.,.F.,(4,3,3,3,3,3,3,3,4),(70.4246015199523,70.4618086551679,
71.4542284953816,72.4466483355952,73.4390681758088,74.4314880160225,75.4239078562361,
76.4163276964497,76.7077868271319),.UNSPECIFIED.);
#5454=B_SPLINE_CURVE_WITH_KNOTS('',3,(#33689,#33690,#33691,#33692,#33693,
#33694,#33695,#33696,#33697,#33698,#33699,#33700,#33701,#33702,#33703,#33704,
#33705,#33706,#33707,#33708,#33709,#33710),.UNSPECIFIED.,.F.,.F.,(4,3,3,
3,3,3,3,4),(-72.9640127846165,-72.4466483355952,-71.4542284953815,-70.4618086551679,
-69.4693888149543,-68.4769689747406,-67.484549134527,-66.680827477437),
 .UNSPECIFIED.);
#5455=B_SPLINE_CURVE_WITH_KNOTS('',3,(#33715,#33716,#33717,#33718,#33719,
#33720,#33721,#33722,#33723,#33724,#33725,#33726,#33727,#33728,#33729,#33730,
#33731,#33732,#33733,#33734,#33735,#33736),.UNSPECIFIED.,.F.,.F.,(4,3,3,
3,3,3,3,4),(64.1414162127728,64.5072896138861,65.4997094540998,66.4921292943134,
67.484549134527,68.4769689747407,69.4693888149543,70.4246015199523),
 .UNSPECIFIED.);
#5456=B_SPLINE_CURVE_WITH_KNOTS('',3,(#33737,#33738,#33739,#33740,#33741,
#33742,#33743,#33744,#33745,#33746,#33747,#33748,#33749,#33750,#33751,#33752,
#33753,#33754,#33755,#33756,#33757,#33758,#33759,#33760,#33761),
 .UNSPECIFIED.,.F.,.F.,(4,3,3,3,3,3,3,3,4),(-66.680827477437,-66.4921292943134,
-65.4997094540998,-64.5072896138861,-63.5148697736725,-62.5224499334589,
-61.5300300932452,-60.5376102530316,-60.3976421702573),.UNSPECIFIED.);
#5457=B_SPLINE_CURVE_WITH_KNOTS('',3,(#33766,#33767,#33768,#33769,#33770,
#33771,#33772,#33773,#33774,#33775,#33776,#33777,#33778,#33779,#33780,#33781,
#33782,#33783,#33784,#33785,#33786,#33787),.UNSPECIFIED.,.F.,.F.,(4,3,3,
3,3,3,3,4),(57.8582309055932,58.5527705726044,59.545190412818,60.5376102530316,
61.5300300932453,62.5224499334589,63.5148697736725,64.1414162127728),
 .UNSPECIFIED.);
#5458=B_SPLINE_CURVE_WITH_KNOTS('',3,(#33788,#33789,#33790,#33791,#33792,
#33793,#33794,#33795,#33796,#33797,#33798,#33799,#33800,#33801,#33802,#33803,
#33804,#33805,#33806,#33807,#33808,#33809),.UNSPECIFIED.,.F.,.F.,(4,3,3,
3,3,3,3,4),(-60.3976421702573,-59.545190412818,-58.5527705726043,-57.5603507323907,
-56.5679308921771,-55.5755110519634,-54.5830912117498,-54.1144568630777),
 .UNSPECIFIED.);
#5459=B_SPLINE_CURVE_WITH_KNOTS('',3,(#33814,#33815,#33816,#33817,#33818,
#33819,#33820,#33821,#33822,#33823,#33824,#33825,#33826,#33827,#33828,#33829,
#33830,#33831,#33832,#33833,#33834,#33835,#33836,#33837,#33838),
 .UNSPECIFIED.,.F.,.F.,(4,3,3,3,3,3,3,3,4),(51.5750455984135,51.6058316911089,
52.5982515313226,53.5906713715362,54.5830912117498,55.5755110519634,56.5679308921771,
57.5603507323907,57.8582309055932),.UNSPECIFIED.);
#5460=B_SPLINE_CURVE_WITH_KNOTS('',3,(#33839,#33840,#33841,#33842,#33843,
#33844,#33845,#33846,#33847,#33848,#33849,#33850,#33851,#33852,#33853,#33854,
#33855,#33856,#33857,#33858,#33859,#33860),.UNSPECIFIED.,.F.,.F.,(4,3,3,
3,3,3,3,4),(-54.1144568630777,-53.5906713715362,-52.5982515313225,-51.6058316911089,
-50.6134118508953,-49.6209920106816,-48.628572170468,-47.8312715558982),
 .UNSPECIFIED.);
#5461=B_SPLINE_CURVE_WITH_KNOTS('',3,(#33865,#33866,#33867,#33868,#33869,
#33870,#33871,#33872,#33873,#33874,#33875,#33876,#33877,#33878,#33879,#33880,
#33881,#33882,#33883,#33884,#33885,#33886),.UNSPECIFIED.,.F.,.F.,(4,3,3,
3,3,3,3,4),(45.291860291234,45.6513126498271,46.6437324900408,47.6361523302544,
48.628572170468,49.6209920106817,50.6134118508953,51.5750455984135),
 .UNSPECIFIED.);
#5462=B_SPLINE_CURVE_WITH_KNOTS('',3,(#33887,#33888,#33889,#33890,#33891,
#33892,#33893,#33894,#33895,#33896,#33897,#33898,#33899,#33900,#33901,#33902,
#33903,#33904,#33905,#33906,#33907,#33908,#33909,#33910,#33911),
 .UNSPECIFIED.,.F.,.F.,(4,3,3,3,3,3,3,3,4),(-47.8312715558982,-47.6361523302544,
-46.6437324900407,-45.6513126498271,-44.6588928096135,-43.6664729693998,
-42.6740531291862,-41.6816332889726,-41.5480862487186),.UNSPECIFIED.);
#5463=B_SPLINE_CURVE_WITH_KNOTS('',3,(#33916,#33917,#33918,#33919,#33920,
#33921,#33922,#33923,#33924,#33925,#33926,#33927,#33928,#33929,#33930,#33931,
#33932,#33933,#33934,#33935,#33936,#33937),.UNSPECIFIED.,.F.,.F.,(4,3,3,
3,3,3,3,4),(39.0086749840544,39.6967936085453,40.6892134487589,41.6816332889726,
42.6740531291862,43.6664729693998,44.6588928096135,45.291860291234),
 .UNSPECIFIED.);
#5464=B_SPLINE_CURVE_WITH_KNOTS('',3,(#33938,#33939,#33940,#33941,#33942,
#33943,#33944,#33945,#33946,#33947,#33948,#33949,#33950,#33951,#33952,#33953,
#33954,#33955,#33956,#33957,#33958,#33959),.UNSPECIFIED.,.F.,.F.,(4,3,3,
3,3,3,3,4),(-41.5480862487186,-40.6892134487589,-39.6967936085453,-38.7043737683317,
-37.711953928118,-36.7195340879044,-35.7271142476908,-35.2649009415389),
 .UNSPECIFIED.);
#5465=B_SPLINE_CURVE_WITH_KNOTS('',3,(#33964,#33965,#33966,#33967,#33968,
#33969,#33970,#33971,#33972,#33973,#33974,#33975,#33976,#33977,#33978,#33979,
#33980,#33981,#33982,#33983,#33984,#33985,#33986,#33987,#33988),
 .UNSPECIFIED.,.F.,.F.,(4,3,3,3,3,3,3,3,4),(32.7254896768748,32.7498547270499,
33.7422745672635,34.7346944074771,35.7271142476908,36.7195340879044,37.711953928118,
38.7043737683317,39.0086749840544),.UNSPECIFIED.);
#5466=B_SPLINE_CURVE_WITH_KNOTS('',3,(#33989,#33990,#33991,#33992,#33993,
#33994,#33995,#33996,#33997,#33998,#33999,#34000,#34001,#34002,#34003,#34004,
#34005,#34006,#34007,#34008,#34009,#34010),.UNSPECIFIED.,.F.,.F.,(4,3,3,
3,3,3,3,4),(-35.2649009415389,-34.7346944074771,-33.7422745672635,-32.7498547270499,
-31.7574348868362,-30.7650150466226,-29.772595206409,-28.9817156343594),
 .UNSPECIFIED.);
#5467=B_SPLINE_CURVE_WITH_KNOTS('',3,(#34015,#34016,#34017,#34018,#34019,
#34020,#34021,#34022,#34023,#34024,#34025,#34026,#34027,#34028,#34029,#34030,
#34031,#34032,#34033,#34034,#34035,#34036),.UNSPECIFIED.,.F.,.F.,(4,3,3,
3,3,3,3,4),(26.4423043696952,26.7953356857681,27.7877555259817,28.7801753661954,
29.772595206409,30.7650150466226,31.7574348868363,32.7254896768748),
 .UNSPECIFIED.);
#5468=B_SPLINE_CURVE_WITH_KNOTS('',3,(#34037,#34038,#34039,#34040,#34041,
#34042,#34043,#34044,#34045,#34046,#34047,#34048,#34049,#34050,#34051,#34052,
#34053,#34054,#34055,#34056,#34057,#34058,#34059,#34060,#34061),
 .UNSPECIFIED.,.F.,.F.,(4,3,3,3,3,3,3,3,4),(-28.9817156343594,-28.7801753661953,
-27.7877555259817,-26.7953356857681,-25.8029158455544,-24.8104960053408,
-23.8180761651272,-22.8256563249135,-22.6985303271798),.UNSPECIFIED.);
#5469=B_SPLINE_CURVE_WITH_KNOTS('',3,(#34066,#34067,#34068,#34069,#34070,
#34071,#34072,#34073,#34074,#34075,#34076,#34077,#34078,#34079,#34080,#34081,
#34082,#34083,#34084,#34085,#34086,#34087),.UNSPECIFIED.,.F.,.F.,(4,3,3,
3,3,3,3,4),(20.1591190625156,20.8408166444863,21.8332364846999,22.8256563249136,
23.8180761651272,24.8104960053408,25.8029158455545,26.4423043696952),
 .UNSPECIFIED.);
#5470=B_SPLINE_CURVE_WITH_KNOTS('',3,(#34088,#34089,#34090,#34091,#34092,
#34093,#34094,#34095,#34096,#34097,#34098,#34099,#34100,#34101,#34102,#34103,
#34104,#34105,#34106,#34107,#34108,#34109),.UNSPECIFIED.,.F.,.F.,(4,3,3,
3,3,3,3,4),(-22.6985303271798,-21.8332364846999,-20.8408166444863,-19.8483968042727,
-18.855976964059,-17.8635571238454,-16.8711372836318,-16.4153450200002),
 .UNSPECIFIED.);
#5471=B_SPLINE_CURVE_WITH_KNOTS('',3,(#34114,#34115,#34116,#34117,#34118,
#34119,#34120,#34121,#34122,#34123,#34124,#34125,#34126,#34127,#34128,#34129,
#34130,#34131,#34132,#34133,#34134,#34135,#34136,#34137,#34138),
 .UNSPECIFIED.,.F.,.F.,(4,3,3,3,3,3,3,3,4),(13.875933755336,13.8938777629909,
14.8862976032045,15.8787174434181,16.8711372836318,17.8635571238454,18.855976964059,
19.8483968042727,20.1591190625156),.UNSPECIFIED.);
#5472=B_SPLINE_CURVE_WITH_KNOTS('',3,(#34139,#34140,#34141,#34142,#34143,
#34144,#34145,#34146,#34147,#34148,#34149,#34150,#34151,#34152,#34153,#34154,
#34155,#34156,#34157,#34158,#34159,#34160),.UNSPECIFIED.,.F.,.F.,(4,3,3,
3,3,3,3,4),(-16.4153450200002,-15.8787174434181,-14.8862976032045,-13.8938777629909,
-12.9014579227772,-11.9090380825636,-10.91661824235,-10.1321597128207),
 .UNSPECIFIED.);
#5473=B_SPLINE_CURVE_WITH_KNOTS('',3,(#34166,#34167,#34168,#34169,#34170,
#34171,#34172,#34173,#34174,#34175,#34176,#34177,#34178),.UNSPECIFIED.,
 .F.,.F.,(4,3,3,3,4),(-3.848974405641,-2.9772595206409,-1.98483968042726,
-0.99241984021363,0.),.UNSPECIFIED.);
#5474=B_SPLINE_CURVE_WITH_KNOTS('',3,(#34181,#34182,#34183,#34184,#34185,
#34186,#34187,#34188,#34189,#34190,#34191,#34192,#34193,#34194,#34195,#34196,
#34197,#34198,#34199),.UNSPECIFIED.,.F.,.F.,(4,3,3,3,3,3,4),(2.01694489302852,
2.9772595206409,3.96967936085454,4.96209920106817,5.9545190412818,6.94693888149544,
7.59274844815647),.UNSPECIFIED.);
#5475=B_SPLINE_CURVE_WITH_KNOTS('',3,(#34205,#34206,#34207,#34208,#34209,
#34210,#34211,#34212),.UNSPECIFIED.,.F.,.F.,(4,1,1,1,1,4),(103.672557568463,
104.154034002176,105.146453842389,106.138873682603,107.131293522817,108.12371336303),
 .UNSPECIFIED.);
#5476=B_SPLINE_CURVE_WITH_KNOTS('',3,(#34215,#34216,#34217,#34218,#34219,
#34220,#34221,#34222,#34223),.UNSPECIFIED.,.F.,.F.,(4,1,1,1,1,1,4),(103.672557568463,
103.716185746199,104.708605586413,105.701025426626,106.69344526684,107.685865107053,
108.646179734666),.UNSPECIFIED.);
#5477=B_SPLINE_CURVE_WITH_KNOTS('',3,(#34228,#34229,#34230,#34231,#34232,
#34233,#34234,#34235,#34236,#34237),.UNSPECIFIED.,.F.,.F.,(4,1,1,1,1,1,
1,4),(97.3893722612835,98.1995149608939,99.1919348011075,100.184354641321,
101.176774481535,102.169194321748,103.161614161962,103.672557568463),
 .UNSPECIFIED.);
#5478=B_SPLINE_CURVE_WITH_KNOTS('',3,(#34238,#34239,#34240,#34241,#34242,
#34243,#34244,#34245,#34246,#34247),.UNSPECIFIED.,.F.,.F.,(4,1,1,1,1,1,
1,4),(97.3893722612835,97.7616667049171,98.7540865451307,99.7465063853444,
100.738926225558,101.731346065772,102.723765905985,103.672557568463),
 .UNSPECIFIED.);
#5479=B_SPLINE_CURVE_WITH_KNOTS('',3,(#34252,#34253,#34254,#34255,#34256,
#34257,#34258,#34259,#34260,#34261,#34262),.UNSPECIFIED.,.F.,.F.,(4,1,1,
1,1,1,1,1,4),(91.106186954104,91.2525760793984,92.2449959196121,93.2374157598257,
94.2298356000393,95.222255440253,96.2146752804666,97.2070951206802,97.3893722612835),
 .UNSPECIFIED.);
#5480=B_SPLINE_CURVE_WITH_KNOTS('',3,(#34263,#34264,#34265,#34266,#34267,
#34268,#34269,#34270,#34271,#34272),.UNSPECIFIED.,.F.,.F.,(4,1,1,1,1,1,
1,4),(91.106186954104,91.8071476636353,92.7995675038489,93.7919873440626,
94.7844071842762,95.7768270244898,96.7692468647035,97.3893722612835),
 .UNSPECIFIED.);
#5481=B_SPLINE_CURVE_WITH_KNOTS('',3,(#34277,#34278,#34279,#34280,#34281,
#34282,#34283,#34284,#34285,#34286),.UNSPECIFIED.,.F.,.F.,(4,1,1,1,1,1,
1,4),(84.8230016469244,85.2980570381166,86.2904768783303,87.2828967185439,
88.2753165587575,89.2677363989712,90.2601562391848,91.106186954104),
 .UNSPECIFIED.);
#5482=B_SPLINE_CURVE_WITH_KNOTS('',3,(#34287,#34288,#34289,#34290,#34291,
#34292,#34293,#34294,#34295,#34296,#34297),.UNSPECIFIED.,.F.,.F.,(4,1,1,
1,1,1,1,1,4),(84.8230016469244,84.8602087821399,85.8526286223535,86.8450484625671,
87.8374683027808,88.8298881429944,89.822307983208,90.8147278234217,91.106186954104),
 .UNSPECIFIED.);
#5483=B_SPLINE_CURVE_WITH_KNOTS('',3,(#34302,#34303,#34304,#34305,#34306,
#34307,#34308,#34309,#34310,#34311),.UNSPECIFIED.,.F.,.F.,(4,1,1,1,1,1,
1,4),(78.5398163397448,79.3435379968348,80.3359578370485,81.3283776772621,
82.3207975174757,83.3132173576894,84.305637197903,84.8230016469244),
 .UNSPECIFIED.);
#5484=B_SPLINE_CURVE_WITH_KNOTS('',3,(#34312,#34313,#34314,#34315,#34316,
#34317,#34318,#34319,#34320,#34321),.UNSPECIFIED.,.F.,.F.,(4,1,1,1,1,1,
1,4),(78.5398163397448,78.9056897408581,79.8981095810717,80.8905294212853,
81.882949261499,82.8753691017126,83.8677889419262,84.8230016469244),
 .UNSPECIFIED.);
#5485=B_SPLINE_CURVE_WITH_KNOTS('',3,(#34326,#34327,#34328,#34329,#34330,
#34331,#34332,#34333,#34334,#34335,#34336),.UNSPECIFIED.,.F.,.F.,(4,1,1,
1,1,1,1,1,4),(72.2566310325653,72.3965991153394,73.389018955553,74.3814387957667,
75.3738586359803,76.3662784761939,77.3586983164076,78.3511181566212,78.5398163397448),
 .UNSPECIFIED.);
#5486=B_SPLINE_CURVE_WITH_KNOTS('',3,(#34337,#34338,#34339,#34340,#34341,
#34342,#34343,#34344,#34345,#34346),.UNSPECIFIED.,.F.,.F.,(4,1,1,1,1,1,
1,4),(72.2566310325651,72.9511706995763,73.9435905397899,74.9360103800035,
75.9284302202172,76.9208500604308,77.9132699006444,78.5398163397448),
 .UNSPECIFIED.);
#5487=B_SPLINE_CURVE_WITH_KNOTS('',3,(#34351,#34352,#34353,#34354,#34355,
#34356,#34357,#34358,#34359,#34360),.UNSPECIFIED.,.F.,.F.,(4,1,1,1,1,1,
1,4),(65.9734457253856,66.4420800740576,67.4344999142712,68.4269197544849,
69.4193395946985,70.4117594349121,71.4041792751258,72.2566310325653),
 .UNSPECIFIED.);
#5488=B_SPLINE_CURVE_WITH_KNOTS('',3,(#34361,#34362,#34363,#34364,#34365,
#34366,#34367,#34368,#34369,#34370,#34371),.UNSPECIFIED.,.F.,.F.,(4,1,1,
1,1,1,1,1,4),(65.9734457253856,66.0042318180808,66.9966516582945,67.9890714985081,
68.9814913387217,69.9739111789354,70.966331019149,71.9587508593626,72.2566310325651),
 .UNSPECIFIED.);
#5489=B_SPLINE_CURVE_WITH_KNOTS('',3,(#34376,#34377,#34378,#34379,#34380,
#34381,#34382,#34383,#34384,#34385),.UNSPECIFIED.,.F.,.F.,(4,1,1,1,1,1,
1,4),(59.690260418206,60.4875610327758,61.4799808729895,62.4724007132031,
63.4648205534167,64.4572403936303,65.449660233844,65.9734457253856),
 .UNSPECIFIED.);
#5490=B_SPLINE_CURVE_WITH_KNOTS('',3,(#34386,#34387,#34388,#34389,#34390,
#34391,#34392,#34393,#34394,#34395),.UNSPECIFIED.,.F.,.F.,(4,1,1,1,1,1,
1,4),(59.690260418206,60.049712776799,61.0421326170127,62.0345524572263,
63.0269722974399,64.0193921376536,65.0118119778672,65.9734457253856),
 .UNSPECIFIED.);
#5491=B_SPLINE_CURVE_WITH_KNOTS('',3,(#34400,#34401,#34402,#34403,#34404,
#34405,#34406,#34407,#34408,#34409,#34410),.UNSPECIFIED.,.F.,.F.,(4,1,1,
1,1,1,1,1,4),(53.4070751110265,53.5406221512804,54.533041991494,55.5254618317077,
56.5178816719213,57.5103015121349,58.5027213523486,59.4951411925622,59.690260418206),
 .UNSPECIFIED.);
#5492=B_SPLINE_CURVE_WITH_KNOTS('',3,(#34411,#34412,#34413,#34414,#34415,
#34416,#34417,#34418,#34419,#34420),.UNSPECIFIED.,.F.,.F.,(4,1,1,1,1,1,
1,4),(53.4070751110265,54.0951937355172,55.0876135757309,56.0800334159445,
57.0724532561581,58.0648730963718,59.0572929365854,59.690260418206),
 .UNSPECIFIED.);
#5493=B_SPLINE_CURVE_WITH_KNOTS('',3,(#34425,#34426,#34427,#34428,#34429,
#34430,#34431,#34432,#34433,#34434),.UNSPECIFIED.,.F.,.F.,(4,1,1,1,1,1,
1,4),(47.1238898038468,47.5861031099986,48.5785229502122,49.5709427904259,
50.5633626306395,51.5557824708531,52.5482023110668,53.4070751110265),
 .UNSPECIFIED.);
#5494=B_SPLINE_CURVE_WITH_KNOTS('',3,(#34435,#34436,#34437,#34438,#34439,
#34440,#34441,#34442,#34443,#34444,#34445),.UNSPECIFIED.,.F.,.F.,(4,1,1,
1,1,1,1,1,4),(47.1238898038468,47.1482548540218,48.1406746942354,49.1330945344491,
50.1255143746627,51.1179342148763,52.11035405509,53.1027738953036,53.4070751110265),
 .UNSPECIFIED.);
#5495=B_SPLINE_CURVE_WITH_KNOTS('',3,(#34450,#34451,#34452,#34453,#34454,
#34455,#34456,#34457,#34458,#34459),.UNSPECIFIED.,.F.,.F.,(4,1,1,1,1,1,
1,4),(40.8407044966672,41.6315840687168,42.6240039089304,43.6164237491441,
44.6088435893577,45.6012634295713,46.593683269785,47.1238898038468),
 .UNSPECIFIED.);
#5496=B_SPLINE_CURVE_WITH_KNOTS('',3,(#34460,#34461,#34462,#34463,#34464,
#34465,#34466,#34467,#34468,#34469),.UNSPECIFIED.,.F.,.F.,(4,1,1,1,1,1,
1,4),(40.8407044966672,41.19373581274,42.1861556529536,43.1785754931673,
44.1709953333809,45.1634151735945,46.1558350138082,47.1238898038468),
 .UNSPECIFIED.);
#5497=B_SPLINE_CURVE_WITH_KNOTS('',3,(#34474,#34475,#34476,#34477,#34478,
#34479,#34480,#34481,#34482,#34483,#34484),.UNSPECIFIED.,.F.,.F.,(4,1,1,
1,1,1,1,1,4),(34.5575191894877,34.6846451872214,35.677065027435,36.6694848676486,
37.6619047078623,38.6543245480759,39.6467443882895,40.6391642285032,40.8407044966672),
 .UNSPECIFIED.);
#5498=B_SPLINE_CURVE_WITH_KNOTS('',3,(#34485,#34486,#34487,#34488,#34489,
#34490,#34491,#34492,#34493,#34494),.UNSPECIFIED.,.F.,.F.,(4,1,1,1,1,1,
1,4),(34.5575191894877,35.2392167714582,36.2316366116718,37.2240564518855,
38.2164762920991,39.2088961323127,40.2013159725264,40.8407044966672),
 .UNSPECIFIED.);
#5499=B_SPLINE_CURVE_WITH_KNOTS('',3,(#34499,#34500,#34501,#34502,#34503,
#34504,#34505,#34506,#34507,#34508),.UNSPECIFIED.,.F.,.F.,(4,1,1,1,1,1,
1,4),(28.2743338823081,28.7301261459396,29.7225459861532,30.7149658263668,
31.7073856665805,32.6998055067941,33.6922253470077,34.5575191894877),
 .UNSPECIFIED.);
#5500=B_SPLINE_CURVE_WITH_KNOTS('',3,(#34509,#34510,#34511,#34512,#34513,
#34514,#34515,#34516,#34517,#34518,#34519),.UNSPECIFIED.,.F.,.F.,(4,1,1,
1,1,1,1,1,4),(28.2743338823081,28.2922778899628,29.2846977301764,30.2771175703901,
31.2695374106037,32.2619572508173,33.2543770910309,34.2467969312446,34.5575191894877),
 .UNSPECIFIED.);
#5501=B_SPLINE_CURVE_WITH_KNOTS('',3,(#34524,#34525,#34526,#34527,#34528,
#34529,#34530,#34531,#34532,#34533),.UNSPECIFIED.,.F.,.F.,(4,1,1,1,1,1,
1,4),(21.9911485751285,22.7756071046578,23.7680269448714,24.760446785085,
25.7528666252987,26.7452864655123,27.7377063057259,28.2743338823081),
 .UNSPECIFIED.);
#5502=B_SPLINE_CURVE_WITH_KNOTS('',3,(#34534,#34535,#34536,#34537,#34538,
#34539,#34540,#34541,#34542,#34543),.UNSPECIFIED.,.F.,.F.,(4,1,1,1,1,1,
1,4),(21.9911485751284,22.337758848681,23.3301786888946,24.3225985291083,
25.3150183693219,26.3074382095355,27.2998580497492,28.2743338823081),
 .UNSPECIFIED.);
#5503=B_SPLINE_CURVE_WITH_KNOTS('',3,(#34549,#34550,#34551,#34552,#34553),
 .UNSPECIFIED.,.F.,.F.,(4,1,4),(14.3984001269719,15.3908199671856,15.7079632679489),
 .UNSPECIFIED.);
#5504=B_SPLINE_CURVE_WITH_KNOTS('',3,(#34556,#34557,#34558,#34559,#34560),
 .UNSPECIFIED.,.F.,.F.,(4,1,4),(13.8759337553364,14.8362483829487,15.7079632679489),
 .UNSPECIFIED.);
#5505=B_SPLINE_CURVE_WITH_KNOTS('',3,(#34566,#34567,#34568,#34569),
 .UNSPECIFIED.,.F.,.F.,(4,4),(95.5573427486708,96.2647245007226),
 .UNSPECIFIED.);
#5506=B_SPLINE_CURVE_WITH_KNOTS('',3,(#34577,#34578,#34579,#34580,#34581,
#34582,#34583,#34584,#34585,#34586),.UNSPECIFIED.,.F.,.F.,(4,3,3,4),(-94.2477796076939,
-93.2874649800816,-92.295045139868,-91.8135687061555),.UNSPECIFIED.);
#5507=B_SPLINE_CURVE_WITH_KNOTS('',3,(#34591,#34592,#34593,#34594,#34595,
#34596,#34597,#34598,#34599,#34600,#34601,#34602,#34603,#34604,#34605,#34606,
#34607,#34608,#34609,#34610,#34611,#34612,#34613,#34614,#34615),
 .UNSPECIFIED.,.F.,.F.,(4,3,3,3,3,3,3,3,4),(89.2741574414912,89.3177856192271,
90.3102054594407,91.3026252996544,92.295045139868,93.2874649800816,94.2798848202952,
95.2723046605089,95.5573427486708),.UNSPECIFIED.);
#5508=B_SPLINE_CURVE_WITH_KNOTS('',3,(#34616,#34617,#34618,#34619,#34620,
#34621,#34622,#34623,#34624,#34625,#34626,#34627,#34628,#34629,#34630,#34631,
#34632,#34633,#34634,#34635,#34636,#34637),.UNSPECIFIED.,.F.,.F.,(4,3,3,
3,3,3,3,4),(-91.8135687061555,-91.3026252996543,-90.3102054594407,-89.3177856192271,
-88.3253657790134,-87.3329459387998,-86.3405260985862,-85.5303833989758),
 .UNSPECIFIED.);
#5509=B_SPLINE_CURVE_WITH_KNOTS('',3,(#34642,#34643,#34644,#34645,#34646,
#34647,#34648,#34649,#34650,#34651,#34652,#34653,#34654,#34655,#34656,#34657,
#34658,#34659,#34660,#34661,#34662,#34663),.UNSPECIFIED.,.F.,.F.,(4,3,3,
3,3,3,3,4),(82.9909721343117,83.3632665779453,84.3556864181589,85.3481062583725,
86.3405260985862,87.3329459387998,88.3253657790134,89.2741574414912),
 .UNSPECIFIED.);
#5510=B_SPLINE_CURVE_WITH_KNOTS('',3,(#34664,#34665,#34666,#34667,#34668,
#34669,#34670,#34671,#34672,#34673,#34674,#34675,#34676,#34677,#34678,#34679,
#34680,#34681,#34682,#34683,#34684,#34685,#34686,#34687,#34688),
 .UNSPECIFIED.,.F.,.F.,(4,3,3,3,3,3,3,3,4),(-85.5303833989758,-85.3481062583725,
-84.3556864181589,-83.3632665779453,-82.3708467377316,-81.378426897518,
-80.3860070573044,-79.3935872170907,-79.2471980917962),.UNSPECIFIED.);
#5511=B_SPLINE_CURVE_WITH_KNOTS('',3,(#34693,#34694,#34695,#34696,#34697,
#34698,#34699,#34700,#34701,#34702,#34703,#34704,#34705,#34706,#34707,#34708,
#34709,#34710,#34711,#34712,#34713,#34714),.UNSPECIFIED.,.F.,.F.,(4,3,3,
3,3,3,3,4),(76.707786827132,77.4087475366635,78.4011673768771,79.3935872170907,
80.3860070573044,81.378426897518,82.3708467377316,82.9909721343117),
 .UNSPECIFIED.);
#5512=B_SPLINE_CURVE_WITH_KNOTS('',3,(#34715,#34716,#34717,#34718,#34719,
#34720,#34721,#34722,#34723,#34724,#34725,#34726,#34727,#34728,#34729,#34730,
#34731,#34732,#34733,#34734,#34735,#34736),.UNSPECIFIED.,.F.,.F.,(4,3,3,
3,3,3,3,4),(-79.2471980917962,-78.4011673768771,-77.4087475366635,-76.4163276964498,
-75.4239078562362,-74.4314880160225,-73.4390681758089,-72.9640127846167),
 .UNSPECIFIED.);
#5513=B_SPLINE_CURVE_WITH_KNOTS('',3,(#34741,#34742,#34743,#34744,#34745,
#34746,#34747,#34748,#34749,#34750,#34751,#34752,#34753,#34754,#34755,#34756,
#34757,#34758,#34759,#34760,#34761,#34762,#34763,#34764,#34765),
 .UNSPECIFIED.,.F.,.F.,(4,3,3,3,3,3,3,3,4),(70.4246015199524,70.461808655168,
71.4542284953817,72.4466483355953,73.4390681758089,74.4314880160226,75.4239078562362,
76.4163276964498,76.707786827132),.UNSPECIFIED.);
#5514=B_SPLINE_CURVE_WITH_KNOTS('',3,(#34766,#34767,#34768,#34769,#34770,
#34771,#34772,#34773,#34774,#34775,#34776,#34777,#34778,#34779,#34780,#34781,
#34782,#34783,#34784,#34785,#34786,#34787),.UNSPECIFIED.,.F.,.F.,(4,3,3,
3,3,3,3,4),(-72.9640127846167,-72.4466483355953,-71.4542284953816,-70.461808655168,
-69.4693888149544,-68.4769689747407,-67.4845491345271,-66.6808274774371),
 .UNSPECIFIED.);
#5515=B_SPLINE_CURVE_WITH_KNOTS('',3,(#34792,#34793,#34794,#34795,#34796,
#34797,#34798,#34799,#34800,#34801,#34802,#34803,#34804,#34805,#34806,#34807,
#34808,#34809,#34810,#34811,#34812,#34813),.UNSPECIFIED.,.F.,.F.,(4,3,3,
3,3,3,3,4),(64.1414162127729,64.5072896138862,65.4997094540998,66.4921292943135,
67.4845491345271,68.4769689747407,69.4693888149544,70.4246015199524),
 .UNSPECIFIED.);
#5516=B_SPLINE_CURVE_WITH_KNOTS('',3,(#34814,#34815,#34816,#34817,#34818,
#34819,#34820,#34821,#34822,#34823,#34824,#34825,#34826,#34827,#34828,#34829,
#34830,#34831,#34832,#34833,#34834,#34835,#34836,#34837,#34838),
 .UNSPECIFIED.,.F.,.F.,(4,3,3,3,3,3,3,3,4),(-66.6808274774371,-66.4921292943135,
-65.4997094540998,-64.5072896138862,-63.5148697736726,-62.5224499334589,
-61.5300300932453,-60.5376102530317,-60.3976421702574),.UNSPECIFIED.);
#5517=B_SPLINE_CURVE_WITH_KNOTS('',3,(#34843,#34844,#34845,#34846,#34847,
#34848,#34849,#34850,#34851,#34852,#34853,#34854,#34855,#34856,#34857,#34858,
#34859,#34860,#34861,#34862,#34863,#34864),.UNSPECIFIED.,.F.,.F.,(4,3,3,
3,3,3,3,4),(57.8582309055933,58.5527705726044,59.545190412818,60.5376102530317,
61.5300300932453,62.5224499334589,63.5148697736726,64.1414162127729),
 .UNSPECIFIED.);
#5518=B_SPLINE_CURVE_WITH_KNOTS('',3,(#34865,#34866,#34867,#34868,#34869,
#34870,#34871,#34872,#34873,#34874,#34875,#34876,#34877,#34878,#34879,#34880,
#34881,#34882,#34883,#34884,#34885,#34886),.UNSPECIFIED.,.F.,.F.,(4,3,3,
3,3,3,3,4),(-60.3976421702574,-59.545190412818,-58.5527705726044,-57.5603507323908,
-56.5679308921771,-55.5755110519635,-54.5830912117499,-54.1144568630778),
 .UNSPECIFIED.);
#5519=B_SPLINE_CURVE_WITH_KNOTS('',3,(#34891,#34892,#34893,#34894,#34895,
#34896,#34897,#34898,#34899,#34900,#34901,#34902,#34903,#34904,#34905,#34906,
#34907,#34908,#34909,#34910,#34911,#34912,#34913,#34914,#34915),
 .UNSPECIFIED.,.F.,.F.,(4,3,3,3,3,3,3,3,4),(51.5750455984136,51.605831691109,
52.5982515313226,53.5906713715362,54.5830912117499,55.5755110519635,56.5679308921771,
57.5603507323908,57.8582309055933),.UNSPECIFIED.);
#5520=B_SPLINE_CURVE_WITH_KNOTS('',3,(#34916,#34917,#34918,#34919,#34920,
#34921,#34922,#34923,#34924,#34925,#34926,#34927,#34928,#34929,#34930,#34931,
#34932,#34933,#34934,#34935,#34936,#34937),.UNSPECIFIED.,.F.,.F.,(4,3,3,
3,3,3,3,4),(-54.1144568630778,-53.5906713715362,-52.5982515313226,-51.605831691109,
-50.6134118508953,-49.6209920106817,-48.6285721704681,-47.8312715558983),
 .UNSPECIFIED.);
#5521=B_SPLINE_CURVE_WITH_KNOTS('',3,(#34942,#34943,#34944,#34945,#34946,
#34947,#34948,#34949,#34950,#34951,#34952,#34953,#34954,#34955,#34956,#34957,
#34958,#34959,#34960,#34961,#34962,#34963),.UNSPECIFIED.,.F.,.F.,(4,3,3,
3,3,3,3,4),(45.2918602912341,45.6513126498272,46.6437324900408,47.6361523302544,
48.6285721704681,49.6209920106817,50.6134118508953,51.5750455984136),
 .UNSPECIFIED.);
#5522=B_SPLINE_CURVE_WITH_KNOTS('',3,(#34964,#34965,#34966,#34967,#34968,
#34969,#34970,#34971,#34972,#34973,#34974,#34975,#34976,#34977,#34978,#34979,
#34980,#34981,#34982,#34983,#34984,#34985,#34986,#34987,#34988),
 .UNSPECIFIED.,.F.,.F.,(4,3,3,3,3,3,3,3,4),(-47.8312715558983,-47.6361523302544,
-46.6437324900408,-45.6513126498272,-44.6588928096135,-43.6664729693999,
-42.6740531291863,-41.6816332889726,-41.5480862487187),.UNSPECIFIED.);
#5523=B_SPLINE_CURVE_WITH_KNOTS('',3,(#34993,#34994,#34995,#34996,#34997,
#34998,#34999,#35000,#35001,#35002,#35003,#35004,#35005,#35006,#35007,#35008,
#35009,#35010,#35011,#35012,#35013,#35014),.UNSPECIFIED.,.F.,.F.,(4,3,3,
3,3,3,3,4),(39.0086749840545,39.6967936085454,40.689213448759,41.6816332889726,
42.6740531291863,43.6664729693999,44.6588928096135,45.2918602912341),
 .UNSPECIFIED.);
#5524=B_SPLINE_CURVE_WITH_KNOTS('',3,(#35015,#35016,#35017,#35018,#35019,
#35020,#35021,#35022,#35023,#35024,#35025,#35026,#35027,#35028,#35029,#35030,
#35031,#35032,#35033,#35034,#35035,#35036),.UNSPECIFIED.,.F.,.F.,(4,3,3,
3,3,3,3,4),(-41.5480862487187,-40.689213448759,-39.6967936085454,-38.7043737683317,
-37.7119539281181,-36.7195340879044,-35.7271142476908,-35.264900941539),
 .UNSPECIFIED.);
#5525=B_SPLINE_CURVE_WITH_KNOTS('',3,(#35041,#35042,#35043,#35044,#35045,
#35046,#35047,#35048,#35049,#35050,#35051,#35052,#35053,#35054,#35055,#35056,
#35057,#35058,#35059,#35060,#35061,#35062,#35063,#35064,#35065),
 .UNSPECIFIED.,.F.,.F.,(4,3,3,3,3,3,3,3,4),(32.725489676875,32.7498547270499,
33.7422745672636,34.7346944074772,35.7271142476908,36.7195340879045,37.7119539281181,
38.7043737683317,39.0086749840545),.UNSPECIFIED.);
#5526=B_SPLINE_CURVE_WITH_KNOTS('',3,(#35066,#35067,#35068,#35069,#35070,
#35071,#35072,#35073,#35074,#35075,#35076,#35077,#35078,#35079,#35080,#35081,
#35082,#35083,#35084,#35085,#35086,#35087),.UNSPECIFIED.,.F.,.F.,(4,3,3,
3,3,3,3,4),(-35.264900941539,-34.7346944074772,-33.7422745672636,-32.7498547270499,
-31.7574348868363,-30.7650150466227,-29.772595206409,-28.9817156343595),
 .UNSPECIFIED.);
#5527=B_SPLINE_CURVE_WITH_KNOTS('',3,(#35092,#35093,#35094,#35095,#35096,
#35097,#35098,#35099,#35100,#35101,#35102,#35103,#35104,#35105,#35106,#35107,
#35108,#35109,#35110,#35111,#35112,#35113),.UNSPECIFIED.,.F.,.F.,(4,3,3,
3,3,3,3,4),(26.4423043696953,26.7953356857681,27.7877555259818,28.7801753661954,
29.772595206409,30.7650150466227,31.7574348868363,32.725489676875),
 .UNSPECIFIED.);
#5528=B_SPLINE_CURVE_WITH_KNOTS('',3,(#35114,#35115,#35116,#35117,#35118,
#35119,#35120,#35121,#35122,#35123,#35124,#35125,#35126,#35127,#35128,#35129,
#35130,#35131,#35132,#35133,#35134,#35135,#35136,#35137,#35138),
 .UNSPECIFIED.,.F.,.F.,(4,3,3,3,3,3,3,3,4),(-28.9817156343595,-28.7801753661954,
-27.7877555259818,-26.7953356857681,-25.8029158455545,-24.8104960053408,
-23.8180761651272,-22.8256563249136,-22.6985303271799),.UNSPECIFIED.);
#5529=B_SPLINE_CURVE_WITH_KNOTS('',3,(#35143,#35144,#35145,#35146,#35147,
#35148,#35149,#35150,#35151,#35152,#35153,#35154,#35155,#35156,#35157,#35158,
#35159,#35160,#35161,#35162,#35163,#35164),.UNSPECIFIED.,.F.,.F.,(4,3,3,
3,3,3,3,4),(20.1591190625157,20.8408166444863,21.8332364846999,22.8256563249136,
23.8180761651272,24.8104960053408,25.8029158455545,26.4423043696953),
 .UNSPECIFIED.);
#5530=B_SPLINE_CURVE_WITH_KNOTS('',3,(#35165,#35166,#35167,#35168,#35169,
#35170,#35171,#35172,#35173,#35174,#35175,#35176,#35177,#35178,#35179,#35180,
#35181,#35182,#35183,#35184,#35185,#35186),.UNSPECIFIED.,.F.,.F.,(4,3,3,
3,3,3,3,4),(-22.6985303271799,-21.8332364846999,-20.8408166444863,-19.8483968042727,
-18.855976964059,-17.8635571238454,-16.8711372836318,-16.4153450200004),
 .UNSPECIFIED.);
#5531=B_SPLINE_CURVE_WITH_KNOTS('',3,(#35191,#35192,#35193,#35194,#35195,
#35196,#35197,#35198,#35199,#35200,#35201,#35202,#35203,#35204,#35205,#35206,
#35207,#35208,#35209,#35210,#35211,#35212,#35213,#35214,#35215),
 .UNSPECIFIED.,.F.,.F.,(4,3,3,3,3,3,3,3,4),(13.8759337553361,13.8938777629909,
14.8862976032045,15.8787174434181,16.8711372836318,17.8635571238454,18.855976964059,
19.8483968042727,20.1591190625157),.UNSPECIFIED.);
#5532=B_SPLINE_CURVE_WITH_KNOTS('',3,(#35216,#35217,#35218,#35219,#35220,
#35221,#35222,#35223,#35224,#35225,#35226,#35227,#35228,#35229,#35230,#35231,
#35232,#35233,#35234,#35235,#35236,#35237),.UNSPECIFIED.,.F.,.F.,(4,3,3,
3,3,3,3,4),(-16.4153450200004,-15.8787174434181,-14.8862976032045,-13.8938777629909,
-12.9014579227772,-11.9090380825636,-10.91661824235,-10.1321597128207),
 .UNSPECIFIED.);
#5533=B_SPLINE_CURVE_WITH_KNOTS('',3,(#35243,#35244,#35245,#35246,#35247,
#35248,#35249,#35250,#35251,#35252,#35253,#35254,#35255),.UNSPECIFIED.,
 .F.,.F.,(4,3,3,3,4),(-3.84897440564112,-2.9772595206409,-1.98483968042727,
-0.992419840213633,0.),.UNSPECIFIED.);
#5534=B_SPLINE_CURVE_WITH_KNOTS('',3,(#35258,#35259,#35260,#35261,#35262,
#35263,#35264,#35265,#35266,#35267,#35268,#35269,#35270,#35271,#35272,#35273,
#35274,#35275,#35276),.UNSPECIFIED.,.F.,.F.,(4,3,3,3,3,3,4),(2.01694489302852,
2.97725952064091,3.96967936085454,4.96209920106817,5.95451904128181,6.94693888149544,
7.59274844815659),.UNSPECIFIED.);
#5535=B_SPLINE_CURVE_WITH_KNOTS('',3,(#35282,#35283,#35284,#35285,#35286,
#35287,#35288,#35289),.UNSPECIFIED.,.F.,.F.,(4,1,1,1,1,4),(103.672557568463,
104.154034002176,105.146453842389,106.138873682603,107.131293522817,108.12371336303),
 .UNSPECIFIED.);
#5536=B_SPLINE_CURVE_WITH_KNOTS('',3,(#35292,#35293,#35294,#35295,#35296,
#35297,#35298,#35299,#35300),.UNSPECIFIED.,.F.,.F.,(4,1,1,1,1,1,4),(103.672557568463,
103.716185746199,104.708605586413,105.701025426626,106.69344526684,107.685865107053,
108.646179734666),.UNSPECIFIED.);
#5537=B_SPLINE_CURVE_WITH_KNOTS('',3,(#35305,#35306,#35307,#35308,#35309,
#35310,#35311,#35312,#35313,#35314),.UNSPECIFIED.,.F.,.F.,(4,1,1,1,1,1,
1,4),(97.3893722612835,98.1995149608939,99.1919348011075,100.184354641321,
101.176774481535,102.169194321748,103.161614161962,103.672557568463),
 .UNSPECIFIED.);
#5538=B_SPLINE_CURVE_WITH_KNOTS('',3,(#35315,#35316,#35317,#35318,#35319,
#35320,#35321,#35322,#35323,#35324),.UNSPECIFIED.,.F.,.F.,(4,1,1,1,1,1,
1,4),(97.3893722612835,97.7616667049171,98.7540865451307,99.7465063853443,
100.738926225558,101.731346065772,102.723765905985,103.672557568463),
 .UNSPECIFIED.);
#5539=B_SPLINE_CURVE_WITH_KNOTS('',3,(#35329,#35330,#35331,#35332,#35333,
#35334,#35335,#35336,#35337,#35338,#35339),.UNSPECIFIED.,.F.,.F.,(4,1,1,
1,1,1,1,1,4),(91.106186954104,91.2525760793984,92.2449959196121,93.2374157598257,
94.2298356000393,95.222255440253,96.2146752804666,97.2070951206802,97.3893722612835),
 .UNSPECIFIED.);
#5540=B_SPLINE_CURVE_WITH_KNOTS('',3,(#35340,#35341,#35342,#35343,#35344,
#35345,#35346,#35347,#35348,#35349),.UNSPECIFIED.,.F.,.F.,(4,1,1,1,1,1,
1,4),(91.106186954104,91.8071476636353,92.7995675038489,93.7919873440625,
94.7844071842762,95.7768270244898,96.7692468647034,97.3893722612835),
 .UNSPECIFIED.);
#5541=B_SPLINE_CURVE_WITH_KNOTS('',3,(#35354,#35355,#35356,#35357,#35358,
#35359,#35360,#35361,#35362,#35363),.UNSPECIFIED.,.F.,.F.,(4,1,1,1,1,1,
1,4),(84.8230016469244,85.2980570381166,86.2904768783303,87.2828967185439,
88.2753165587575,89.2677363989712,90.2601562391848,91.106186954104),
 .UNSPECIFIED.);
#5542=B_SPLINE_CURVE_WITH_KNOTS('',3,(#35364,#35365,#35366,#35367,#35368,
#35369,#35370,#35371,#35372,#35373,#35374),.UNSPECIFIED.,.F.,.F.,(4,1,1,
1,1,1,1,1,4),(84.8230016469244,84.8602087821398,85.8526286223535,86.8450484625671,
87.8374683027807,88.8298881429944,89.822307983208,90.8147278234216,91.106186954104),
 .UNSPECIFIED.);
#5543=B_SPLINE_CURVE_WITH_KNOTS('',3,(#35379,#35380,#35381,#35382,#35383,
#35384,#35385,#35386,#35387,#35388),.UNSPECIFIED.,.F.,.F.,(4,1,1,1,1,1,
1,4),(78.5398163397448,79.3435379968348,80.3359578370484,81.3283776772621,
82.3207975174757,83.3132173576894,84.305637197903,84.8230016469244),
 .UNSPECIFIED.);
#5544=B_SPLINE_CURVE_WITH_KNOTS('',3,(#35389,#35390,#35391,#35392,#35393,
#35394,#35395,#35396,#35397,#35398),.UNSPECIFIED.,.F.,.F.,(4,1,1,1,1,1,
1,4),(78.5398163397448,78.905689740858,79.8981095810717,80.8905294212853,
81.8829492614989,82.8753691017126,83.8677889419262,84.8230016469244),
 .UNSPECIFIED.);
#5545=B_SPLINE_CURVE_WITH_KNOTS('',3,(#35403,#35404,#35405,#35406,#35407,
#35408,#35409,#35410,#35411,#35412,#35413),.UNSPECIFIED.,.F.,.F.,(4,1,1,
1,1,1,1,1,4),(72.2566310325653,72.3965991153394,73.389018955553,74.3814387957666,
75.3738586359803,76.3662784761939,77.3586983164075,78.3511181566212,78.5398163397448),
 .UNSPECIFIED.);
#5546=B_SPLINE_CURVE_WITH_KNOTS('',3,(#35414,#35415,#35416,#35417,#35418,
#35419,#35420,#35421,#35422,#35423),.UNSPECIFIED.,.F.,.F.,(4,1,1,1,1,1,
1,4),(72.2566310325651,72.9511706995762,73.9435905397899,74.9360103800035,
75.9284302202171,76.9208500604308,77.9132699006444,78.5398163397448),
 .UNSPECIFIED.);
#5547=B_SPLINE_CURVE_WITH_KNOTS('',3,(#35428,#35429,#35430,#35431,#35432,
#35433,#35434,#35435,#35436,#35437),.UNSPECIFIED.,.F.,.F.,(4,1,1,1,1,1,
1,4),(65.9734457253856,66.4420800740576,67.4344999142712,68.4269197544848,
69.4193395946985,70.4117594349121,71.4041792751257,72.2566310325653),
 .UNSPECIFIED.);
#5548=B_SPLINE_CURVE_WITH_KNOTS('',3,(#35438,#35439,#35440,#35441,#35442,
#35443,#35444,#35445,#35446,#35447,#35448),.UNSPECIFIED.,.F.,.F.,(4,1,1,
1,1,1,1,1,4),(65.9734457253856,66.0042318180808,66.9966516582944,67.9890714985081,
68.9814913387217,69.9739111789353,70.966331019149,71.9587508593626,72.2566310325651),
 .UNSPECIFIED.);
#5549=B_SPLINE_CURVE_WITH_KNOTS('',3,(#35453,#35454,#35455,#35456,#35457,
#35458,#35459,#35460,#35461,#35462),.UNSPECIFIED.,.F.,.F.,(4,1,1,1,1,1,
1,4),(59.690260418206,60.4875610327758,61.4799808729894,62.472400713203,
63.4648205534167,64.4572403936303,65.4496602338439,65.9734457253856),
 .UNSPECIFIED.);
#5550=B_SPLINE_CURVE_WITH_KNOTS('',3,(#35463,#35464,#35465,#35466,#35467,
#35468,#35469,#35470,#35471,#35472),.UNSPECIFIED.,.F.,.F.,(4,1,1,1,1,1,
1,4),(59.690260418206,60.049712776799,61.0421326170126,62.0345524572262,
63.0269722974399,64.0193921376535,65.0118119778672,65.9734457253856),
 .UNSPECIFIED.);
#5551=B_SPLINE_CURVE_WITH_KNOTS('',3,(#35477,#35478,#35479,#35480,#35481,
#35482,#35483,#35484,#35485,#35486,#35487),.UNSPECIFIED.,.F.,.F.,(4,1,1,
1,1,1,1,1,4),(53.4070751110265,53.5406221512803,54.533041991494,55.5254618317076,
56.5178816719212,57.5103015121349,58.5027213523485,59.4951411925621,59.690260418206),
 .UNSPECIFIED.);
#5552=B_SPLINE_CURVE_WITH_KNOTS('',3,(#35488,#35489,#35490,#35491,#35492,
#35493,#35494,#35495,#35496,#35497),.UNSPECIFIED.,.F.,.F.,(4,1,1,1,1,1,
1,4),(53.4070751110265,54.0951937355172,55.0876135757308,56.0800334159444,
57.0724532561581,58.0648730963717,59.0572929365853,59.690260418206),
 .UNSPECIFIED.);
#5553=B_SPLINE_CURVE_WITH_KNOTS('',3,(#35502,#35503,#35504,#35505,#35506,
#35507,#35508,#35509,#35510,#35511),.UNSPECIFIED.,.F.,.F.,(4,1,1,1,1,1,
1,4),(47.1238898038468,47.5861031099985,48.5785229502122,49.5709427904258,
50.5633626306394,51.5557824708531,52.5482023110667,53.4070751110265),
 .UNSPECIFIED.);
#5554=B_SPLINE_CURVE_WITH_KNOTS('',3,(#35512,#35513,#35514,#35515,#35516,
#35517,#35518,#35519,#35520,#35521,#35522),.UNSPECIFIED.,.F.,.F.,(4,1,1,
1,1,1,1,1,4),(47.1238898038468,47.1482548540217,48.1406746942354,49.133094534449,
50.1255143746626,51.1179342148763,52.1103540550899,53.1027738953035,53.4070751110265),
 .UNSPECIFIED.);
#5555=B_SPLINE_CURVE_WITH_KNOTS('',3,(#35527,#35528,#35529,#35530,#35531,
#35532,#35533,#35534,#35535,#35536),.UNSPECIFIED.,.F.,.F.,(4,1,1,1,1,1,
1,4),(40.8407044966672,41.6315840687167,42.6240039089304,43.616423749144,
44.6088435893576,45.6012634295713,46.5936832697849,47.1238898038468),
 .UNSPECIFIED.);
#5556=B_SPLINE_CURVE_WITH_KNOTS('',3,(#35537,#35538,#35539,#35540,#35541,
#35542,#35543,#35544,#35545,#35546),.UNSPECIFIED.,.F.,.F.,(4,1,1,1,1,1,
1,4),(40.8407044966672,41.1937358127399,42.1861556529536,43.1785754931672,
44.1709953333808,45.1634151735945,46.1558350138081,47.1238898038468),
 .UNSPECIFIED.);
#5557=B_SPLINE_CURVE_WITH_KNOTS('',3,(#35551,#35552,#35553,#35554,#35555,
#35556,#35557,#35558,#35559,#35560,#35561),.UNSPECIFIED.,.F.,.F.,(4,1,1,
1,1,1,1,1,4),(34.5575191894877,34.6846451872213,35.6770650274349,36.6694848676485,
37.6619047078622,38.6543245480758,39.6467443882895,40.6391642285031,40.8407044966672),
 .UNSPECIFIED.);
#5558=B_SPLINE_CURVE_WITH_KNOTS('',3,(#35562,#35563,#35564,#35565,#35566,
#35567,#35568,#35569,#35570,#35571),.UNSPECIFIED.,.F.,.F.,(4,1,1,1,1,1,
1,4),(34.5575191894877,35.2392167714581,36.2316366116718,37.2240564518854,
38.216476292099,39.2088961323127,40.2013159725263,40.8407044966672),
 .UNSPECIFIED.);
#5559=B_SPLINE_CURVE_WITH_KNOTS('',3,(#35576,#35577,#35578,#35579,#35580,
#35581,#35582,#35583,#35584,#35585),.UNSPECIFIED.,.F.,.F.,(4,1,1,1,1,1,
1,4),(28.2743338823081,28.7301261459395,29.7225459861531,30.7149658263668,
31.7073856665804,32.699805506794,33.6922253470076,34.5575191894877),
 .UNSPECIFIED.);
#5560=B_SPLINE_CURVE_WITH_KNOTS('',3,(#35586,#35587,#35588,#35589,#35590,
#35591,#35592,#35593,#35594,#35595,#35596),.UNSPECIFIED.,.F.,.F.,(4,1,1,
1,1,1,1,1,4),(28.2743338823081,28.2922778899627,29.2846977301763,30.27711757039,
31.2695374106036,32.2619572508172,33.2543770910309,34.2467969312445,34.5575191894877),
 .UNSPECIFIED.);
#5561=B_SPLINE_CURVE_WITH_KNOTS('',3,(#35601,#35602,#35603,#35604,#35605,
#35606,#35607,#35608,#35609,#35610),.UNSPECIFIED.,.F.,.F.,(4,1,1,1,1,1,
1,4),(21.9911485751285,22.7756071046577,23.7680269448713,24.7604467850849,
25.7528666252986,26.7452864655122,27.7377063057258,28.2743338823081),
 .UNSPECIFIED.);
#5562=B_SPLINE_CURVE_WITH_KNOTS('',3,(#35611,#35612,#35613,#35614,#35615,
#35616,#35617,#35618,#35619,#35620),.UNSPECIFIED.,.F.,.F.,(4,1,1,1,1,1,
1,4),(21.9911485751284,22.3377588486809,23.3301786888945,24.3225985291082,
25.3150183693218,26.3074382095354,27.2998580497491,28.2743338823081),
 .UNSPECIFIED.);
#5563=B_SPLINE_CURVE_WITH_KNOTS('',3,(#35626,#35627,#35628,#35629,#35630),
 .UNSPECIFIED.,.F.,.F.,(4,1,4),(14.3984001269718,15.3908199671854,15.7079632679489),
 .UNSPECIFIED.);
#5564=B_SPLINE_CURVE_WITH_KNOTS('',3,(#35633,#35634,#35635,#35636,#35637),
 .UNSPECIFIED.,.F.,.F.,(4,1,4),(13.8759337553363,14.8362483829486,15.7079632679489),
 .UNSPECIFIED.);
#5565=B_SPLINE_CURVE_WITH_KNOTS('',3,(#35643,#35644,#35645,#35646),
 .UNSPECIFIED.,.F.,.F.,(4,4),(95.5573427486707,96.2647245007224),
 .UNSPECIFIED.);
#5566=B_SPLINE_CURVE_WITH_KNOTS('',3,(#35654,#35655,#35656,#35657,#35658,
#35659,#35660,#35661,#35662,#35663),.UNSPECIFIED.,.F.,.F.,(4,3,3,4),(-94.2477796076938,
-93.2874649800815,-92.2950451398679,-91.8135687061554),.UNSPECIFIED.);
#5567=B_SPLINE_CURVE_WITH_KNOTS('',3,(#35668,#35669,#35670,#35671,#35672,
#35673,#35674,#35675,#35676,#35677,#35678,#35679,#35680,#35681,#35682,#35683,
#35684,#35685,#35686,#35687,#35688,#35689,#35690,#35691,#35692),
 .UNSPECIFIED.,.F.,.F.,(4,3,3,3,3,3,3,3,4),(89.2741574414911,89.317785619227,
90.3102054594406,91.3026252996542,92.2950451398679,93.2874649800815,94.2798848202951,
95.2723046605088,95.5573427486707),.UNSPECIFIED.);
#5568=B_SPLINE_CURVE_WITH_KNOTS('',3,(#35693,#35694,#35695,#35696,#35697,
#35698,#35699,#35700,#35701,#35702,#35703,#35704,#35705,#35706,#35707,#35708,
#35709,#35710,#35711,#35712,#35713,#35714),.UNSPECIFIED.,.F.,.F.,(4,3,3,
3,3,3,3,4),(-91.8135687061554,-91.3026252996542,-90.3102054594406,-89.317785619227,
-88.3253657790133,-87.3329459387997,-86.3405260985861,-85.5303833989757),
 .UNSPECIFIED.);
#5569=B_SPLINE_CURVE_WITH_KNOTS('',3,(#35719,#35720,#35721,#35722,#35723,
#35724,#35725,#35726,#35727,#35728,#35729,#35730,#35731,#35732,#35733,#35734,
#35735,#35736,#35737,#35738,#35739,#35740),.UNSPECIFIED.,.F.,.F.,(4,3,3,
3,3,3,3,4),(82.9909721343116,83.3632665779452,84.3556864181588,85.3481062583724,
86.3405260985861,87.3329459387997,88.3253657790133,89.2741574414911),
 .UNSPECIFIED.);
#5570=B_SPLINE_CURVE_WITH_KNOTS('',3,(#35741,#35742,#35743,#35744,#35745,
#35746,#35747,#35748,#35749,#35750,#35751,#35752,#35753,#35754,#35755,#35756,
#35757,#35758,#35759,#35760,#35761,#35762,#35763,#35764,#35765),
 .UNSPECIFIED.,.F.,.F.,(4,3,3,3,3,3,3,3,4),(-85.5303833989757,-85.3481062583724,
-84.3556864181588,-83.3632665779452,-82.3708467377315,-81.3784268975179,
-80.3860070573043,-79.3935872170906,-79.2471980917961),.UNSPECIFIED.);
#5571=B_SPLINE_CURVE_WITH_KNOTS('',3,(#35770,#35771,#35772,#35773,#35774,
#35775,#35776,#35777,#35778,#35779,#35780,#35781,#35782,#35783,#35784,#35785,
#35786,#35787,#35788,#35789,#35790,#35791),.UNSPECIFIED.,.F.,.F.,(4,3,3,
3,3,3,3,4),(76.7077868271319,77.4087475366634,78.401167376877,79.3935872170906,
80.3860070573043,81.3784268975179,82.3708467377315,82.9909721343116),
 .UNSPECIFIED.);
#5572=B_SPLINE_CURVE_WITH_KNOTS('',3,(#35792,#35793,#35794,#35795,#35796,
#35797,#35798,#35799,#35800,#35801,#35802,#35803,#35804,#35805,#35806,#35807,
#35808,#35809,#35810,#35811,#35812,#35813),.UNSPECIFIED.,.F.,.F.,(4,3,3,
3,3,3,3,4),(-79.2471980917961,-78.401167376877,-77.4087475366633,-76.4163276964497,
-75.4239078562361,-74.4314880160224,-73.4390681758088,-72.9640127846165),
 .UNSPECIFIED.);
#5573=B_SPLINE_CURVE_WITH_KNOTS('',3,(#35818,#35819,#35820,#35821,#35822,
#35823,#35824,#35825,#35826,#35827,#35828,#35829,#35830,#35831,#35832,#35833,
#35834,#35835,#35836,#35837,#35838,#35839,#35840,#35841,#35842),
 .UNSPECIFIED.,.F.,.F.,(4,3,3,3,3,3,3,3,4),(70.4246015199523,70.4618086551679,
71.4542284953816,72.4466483355952,73.4390681758088,74.4314880160225,75.4239078562361,
76.4163276964497,76.7077868271319),.UNSPECIFIED.);
#5574=B_SPLINE_CURVE_WITH_KNOTS('',3,(#35843,#35844,#35845,#35846,#35847,
#35848,#35849,#35850,#35851,#35852,#35853,#35854,#35855,#35856,#35857,#35858,
#35859,#35860,#35861,#35862,#35863,#35864),.UNSPECIFIED.,.F.,.F.,(4,3,3,
3,3,3,3,4),(-72.9640127846165,-72.4466483355952,-71.4542284953815,-70.4618086551679,
-69.4693888149543,-68.4769689747406,-67.484549134527,-66.680827477437),
 .UNSPECIFIED.);
#5575=B_SPLINE_CURVE_WITH_KNOTS('',3,(#35869,#35870,#35871,#35872,#35873,
#35874,#35875,#35876,#35877,#35878,#35879,#35880,#35881,#35882,#35883,#35884,
#35885,#35886,#35887,#35888,#35889,#35890),.UNSPECIFIED.,.F.,.F.,(4,3,3,
3,3,3,3,4),(64.1414162127728,64.5072896138861,65.4997094540998,66.4921292943134,
67.484549134527,68.4769689747407,69.4693888149543,70.4246015199523),
 .UNSPECIFIED.);
#5576=B_SPLINE_CURVE_WITH_KNOTS('',3,(#35891,#35892,#35893,#35894,#35895,
#35896,#35897,#35898,#35899,#35900,#35901,#35902,#35903,#35904,#35905,#35906,
#35907,#35908,#35909,#35910,#35911,#35912,#35913,#35914,#35915),
 .UNSPECIFIED.,.F.,.F.,(4,3,3,3,3,3,3,3,4),(-66.680827477437,-66.4921292943134,
-65.4997094540998,-64.5072896138861,-63.5148697736725,-62.5224499334589,
-61.5300300932452,-60.5376102530316,-60.3976421702573),.UNSPECIFIED.);
#5577=B_SPLINE_CURVE_WITH_KNOTS('',3,(#35920,#35921,#35922,#35923,#35924,
#35925,#35926,#35927,#35928,#35929,#35930,#35931,#35932,#35933,#35934,#35935,
#35936,#35937,#35938,#35939,#35940,#35941),.UNSPECIFIED.,.F.,.F.,(4,3,3,
3,3,3,3,4),(57.8582309055932,58.5527705726043,59.545190412818,60.5376102530316,
61.5300300932452,62.5224499334589,63.5148697736725,64.1414162127728),
 .UNSPECIFIED.);
#5578=B_SPLINE_CURVE_WITH_KNOTS('',3,(#35942,#35943,#35944,#35945,#35946,
#35947,#35948,#35949,#35950,#35951,#35952,#35953,#35954,#35955,#35956,#35957,
#35958,#35959,#35960,#35961,#35962,#35963),.UNSPECIFIED.,.F.,.F.,(4,3,3,
3,3,3,3,4),(-60.3976421702573,-59.545190412818,-58.5527705726043,-57.5603507323907,
-56.5679308921771,-55.5755110519634,-54.5830912117498,-54.1144568630777),
 .UNSPECIFIED.);
#5579=B_SPLINE_CURVE_WITH_KNOTS('',3,(#35968,#35969,#35970,#35971,#35972,
#35973,#35974,#35975,#35976,#35977,#35978,#35979,#35980,#35981,#35982,#35983,
#35984,#35985,#35986,#35987,#35988,#35989,#35990,#35991,#35992),
 .UNSPECIFIED.,.F.,.F.,(4,3,3,3,3,3,3,3,4),(51.5750455984135,51.6058316911089,
52.5982515313225,53.5906713715362,54.5830912117498,55.5755110519634,56.5679308921771,
57.5603507323907,57.8582309055932),.UNSPECIFIED.);
#5580=B_SPLINE_CURVE_WITH_KNOTS('',3,(#35993,#35994,#35995,#35996,#35997,
#35998,#35999,#36000,#36001,#36002,#36003,#36004,#36005,#36006,#36007,#36008,
#36009,#36010,#36011,#36012,#36013,#36014),.UNSPECIFIED.,.F.,.F.,(4,3,3,
3,3,3,3,4),(-54.1144568630777,-53.5906713715362,-52.5982515313225,-51.6058316911089,
-50.6134118508953,-49.6209920106816,-48.628572170468,-47.8312715558982),
 .UNSPECIFIED.);
#5581=B_SPLINE_CURVE_WITH_KNOTS('',3,(#36019,#36020,#36021,#36022,#36023,
#36024,#36025,#36026,#36027,#36028,#36029,#36030,#36031,#36032,#36033,#36034,
#36035,#36036,#36037,#36038,#36039,#36040),.UNSPECIFIED.,.F.,.F.,(4,3,3,
3,3,3,3,4),(45.291860291234,45.6513126498271,46.6437324900408,47.6361523302544,
48.628572170468,49.6209920106816,50.6134118508953,51.5750455984135),
 .UNSPECIFIED.);
#5582=B_SPLINE_CURVE_WITH_KNOTS('',3,(#36041,#36042,#36043,#36044,#36045,
#36046,#36047,#36048,#36049,#36050,#36051,#36052,#36053,#36054,#36055,#36056,
#36057,#36058,#36059,#36060,#36061,#36062,#36063,#36064,#36065),
 .UNSPECIFIED.,.F.,.F.,(4,3,3,3,3,3,3,3,4),(-47.8312715558982,-47.6361523302544,
-46.6437324900407,-45.6513126498271,-44.6588928096135,-43.6664729693998,
-42.6740531291862,-41.6816332889726,-41.5480862487186),.UNSPECIFIED.);
#5583=B_SPLINE_CURVE_WITH_KNOTS('',3,(#36070,#36071,#36072,#36073,#36074,
#36075,#36076,#36077,#36078,#36079,#36080,#36081,#36082,#36083,#36084,#36085,
#36086,#36087,#36088,#36089,#36090,#36091),.UNSPECIFIED.,.F.,.F.,(4,3,3,
3,3,3,3,4),(39.0086749840544,39.6967936085453,40.6892134487589,41.6816332889726,
42.6740531291862,43.6664729693998,44.6588928096135,45.291860291234),
 .UNSPECIFIED.);
#5584=B_SPLINE_CURVE_WITH_KNOTS('',3,(#36092,#36093,#36094,#36095,#36096,
#36097,#36098,#36099,#36100,#36101,#36102,#36103,#36104,#36105,#36106,#36107,
#36108,#36109,#36110,#36111,#36112,#36113),.UNSPECIFIED.,.F.,.F.,(4,3,3,
3,3,3,3,4),(-41.5480862487186,-40.6892134487589,-39.6967936085453,-38.7043737683317,
-37.711953928118,-36.7195340879044,-35.7271142476908,-35.2649009415389),
 .UNSPECIFIED.);
#5585=B_SPLINE_CURVE_WITH_KNOTS('',3,(#36118,#36119,#36120,#36121,#36122,
#36123,#36124,#36125,#36126,#36127,#36128,#36129,#36130,#36131,#36132,#36133,
#36134,#36135,#36136,#36137,#36138,#36139,#36140,#36141,#36142),
 .UNSPECIFIED.,.F.,.F.,(4,3,3,3,3,3,3,3,4),(32.7254896768748,32.7498547270499,
33.7422745672635,34.7346944074771,35.7271142476908,36.7195340879044,37.711953928118,
38.7043737683317,39.0086749840544),.UNSPECIFIED.);
#5586=B_SPLINE_CURVE_WITH_KNOTS('',3,(#36143,#36144,#36145,#36146,#36147,
#36148,#36149,#36150,#36151,#36152,#36153,#36154,#36155,#36156,#36157,#36158,
#36159,#36160,#36161,#36162,#36163,#36164),.UNSPECIFIED.,.F.,.F.,(4,3,3,
3,3,3,3,4),(-35.2649009415389,-34.7346944074771,-33.7422745672635,-32.7498547270499,
-31.7574348868362,-30.7650150466226,-29.772595206409,-28.9817156343594),
 .UNSPECIFIED.);
#5587=B_SPLINE_CURVE_WITH_KNOTS('',3,(#36169,#36170,#36171,#36172,#36173,
#36174,#36175,#36176,#36177,#36178,#36179,#36180,#36181,#36182,#36183,#36184,
#36185,#36186,#36187,#36188,#36189,#36190),.UNSPECIFIED.,.F.,.F.,(4,3,3,
3,3,3,3,4),(26.4423043696952,26.7953356857681,27.7877555259817,28.7801753661954,
29.772595206409,30.7650150466226,31.7574348868363,32.7254896768748),
 .UNSPECIFIED.);
#5588=B_SPLINE_CURVE_WITH_KNOTS('',3,(#36191,#36192,#36193,#36194,#36195,
#36196,#36197,#36198,#36199,#36200,#36201,#36202,#36203,#36204,#36205,#36206,
#36207,#36208,#36209,#36210,#36211,#36212,#36213,#36214,#36215),
 .UNSPECIFIED.,.F.,.F.,(4,3,3,3,3,3,3,3,4),(-28.9817156343594,-28.7801753661953,
-27.7877555259817,-26.7953356857681,-25.8029158455544,-24.8104960053408,
-23.8180761651272,-22.8256563249135,-22.6985303271798),.UNSPECIFIED.);
#5589=B_SPLINE_CURVE_WITH_KNOTS('',3,(#36220,#36221,#36222,#36223,#36224,
#36225,#36226,#36227,#36228,#36229,#36230,#36231,#36232,#36233,#36234,#36235,
#36236,#36237,#36238,#36239,#36240,#36241),.UNSPECIFIED.,.F.,.F.,(4,3,3,
3,3,3,3,4),(20.1591190625156,20.8408166444863,21.8332364846999,22.8256563249136,
23.8180761651272,24.8104960053408,25.8029158455545,26.4423043696952),
 .UNSPECIFIED.);
#5590=B_SPLINE_CURVE_WITH_KNOTS('',3,(#36242,#36243,#36244,#36245,#36246,
#36247,#36248,#36249,#36250,#36251,#36252,#36253,#36254,#36255,#36256,#36257,
#36258,#36259,#36260,#36261,#36262,#36263),.UNSPECIFIED.,.F.,.F.,(4,3,3,
3,3,3,3,4),(-22.6985303271798,-21.8332364846999,-20.8408166444863,-19.8483968042727,
-18.855976964059,-17.8635571238454,-16.8711372836318,-16.4153450200002),
 .UNSPECIFIED.);
#5591=B_SPLINE_CURVE_WITH_KNOTS('',3,(#36268,#36269,#36270,#36271,#36272,
#36273,#36274,#36275,#36276,#36277,#36278,#36279,#36280,#36281,#36282,#36283,
#36284,#36285,#36286,#36287,#36288,#36289,#36290,#36291,#36292),
 .UNSPECIFIED.,.F.,.F.,(4,3,3,3,3,3,3,3,4),(13.875933755336,13.8938777629909,
14.8862976032045,15.8787174434181,16.8711372836318,17.8635571238454,18.855976964059,
19.8483968042727,20.1591190625156),.UNSPECIFIED.);
#5592=B_SPLINE_CURVE_WITH_KNOTS('',3,(#36293,#36294,#36295,#36296,#36297,
#36298,#36299,#36300,#36301,#36302,#36303,#36304,#36305,#36306,#36307,#36308,
#36309,#36310,#36311,#36312,#36313,#36314),.UNSPECIFIED.,.F.,.F.,(4,3,3,
3,3,3,3,4),(-16.4153450200002,-15.8787174434181,-14.8862976032045,-13.8938777629909,
-12.9014579227772,-11.9090380825636,-10.91661824235,-10.1321597128207),
 .UNSPECIFIED.);
#5593=B_SPLINE_CURVE_WITH_KNOTS('',3,(#36320,#36321,#36322,#36323,#36324,
#36325,#36326,#36327,#36328,#36329,#36330,#36331,#36332),.UNSPECIFIED.,
 .F.,.F.,(4,3,3,3,4),(-3.848974405641,-2.9772595206409,-1.98483968042726,
-0.992419840213632,0.),.UNSPECIFIED.);
#5594=B_SPLINE_CURVE_WITH_KNOTS('',3,(#36335,#36336,#36337,#36338,#36339,
#36340,#36341,#36342,#36343,#36344,#36345,#36346,#36347,#36348,#36349,#36350,
#36351,#36352,#36353),.UNSPECIFIED.,.F.,.F.,(4,3,3,3,3,3,4),(2.01694489302852,
2.9772595206409,3.96967936085453,4.96209920106817,5.9545190412818,6.94693888149543,
7.59274844815647),.UNSPECIFIED.);
#5595=B_SPLINE_CURVE_WITH_KNOTS('',3,(#36359,#36360,#36361,#36362,#36363,
#36364,#36365,#36366),.UNSPECIFIED.,.F.,.F.,(4,1,1,1,1,4),(103.672557568463,
104.154034002176,105.146453842389,106.138873682603,107.131293522817,108.12371336303),
 .UNSPECIFIED.);
#5596=B_SPLINE_CURVE_WITH_KNOTS('',3,(#36369,#36370,#36371,#36372,#36373,
#36374,#36375,#36376,#36377),.UNSPECIFIED.,.F.,.F.,(4,1,1,1,1,1,4),(103.672557568463,
103.716185746199,104.708605586413,105.701025426626,106.69344526684,107.685865107053,
108.646179734666),.UNSPECIFIED.);
#5597=B_SPLINE_CURVE_WITH_KNOTS('',3,(#36382,#36383,#36384,#36385,#36386,
#36387,#36388,#36389,#36390,#36391),.UNSPECIFIED.,.F.,.F.,(4,1,1,1,1,1,
1,4),(97.3893722612835,98.1995149608939,99.1919348011075,100.184354641321,
101.176774481535,102.169194321748,103.161614161962,103.672557568463),
 .UNSPECIFIED.);
#5598=B_SPLINE_CURVE_WITH_KNOTS('',3,(#36392,#36393,#36394,#36395,#36396,
#36397,#36398,#36399,#36400,#36401),.UNSPECIFIED.,.F.,.F.,(4,1,1,1,1,1,
1,4),(97.3893722612835,97.7616667049171,98.7540865451307,99.7465063853444,
100.738926225558,101.731346065772,102.723765905985,103.672557568463),
 .UNSPECIFIED.);
#5599=B_SPLINE_CURVE_WITH_KNOTS('',3,(#36406,#36407,#36408,#36409,#36410,
#36411,#36412,#36413,#36414,#36415,#36416),.UNSPECIFIED.,.F.,.F.,(4,1,1,
1,1,1,1,1,4),(91.106186954104,91.2525760793984,92.2449959196121,93.2374157598257,
94.2298356000393,95.222255440253,96.2146752804666,97.2070951206802,97.3893722612835),
 .UNSPECIFIED.);
#5600=B_SPLINE_CURVE_WITH_KNOTS('',3,(#36417,#36418,#36419,#36420,#36421,
#36422,#36423,#36424,#36425,#36426),.UNSPECIFIED.,.F.,.F.,(4,1,1,1,1,1,
1,4),(91.106186954104,91.8071476636353,92.7995675038489,93.7919873440626,
94.7844071842762,95.7768270244898,96.7692468647035,97.3893722612835),
 .UNSPECIFIED.);
#5601=B_SPLINE_CURVE_WITH_KNOTS('',3,(#36431,#36432,#36433,#36434,#36435,
#36436,#36437,#36438,#36439,#36440),.UNSPECIFIED.,.F.,.F.,(4,1,1,1,1,1,
1,4),(84.8230016469244,85.2980570381166,86.2904768783303,87.2828967185439,
88.2753165587575,89.2677363989712,90.2601562391848,91.106186954104),
 .UNSPECIFIED.);
#5602=B_SPLINE_CURVE_WITH_KNOTS('',3,(#36441,#36442,#36443,#36444,#36445,
#36446,#36447,#36448,#36449,#36450,#36451),.UNSPECIFIED.,.F.,.F.,(4,1,1,
1,1,1,1,1,4),(84.8230016469244,84.8602087821399,85.8526286223535,86.8450484625671,
87.8374683027808,88.8298881429944,89.822307983208,90.8147278234217,91.106186954104),
 .UNSPECIFIED.);
#5603=B_SPLINE_CURVE_WITH_KNOTS('',3,(#36456,#36457,#36458,#36459,#36460,
#36461,#36462,#36463,#36464,#36465),.UNSPECIFIED.,.F.,.F.,(4,1,1,1,1,1,
1,4),(78.5398163397448,79.3435379968348,80.3359578370485,81.3283776772621,
82.3207975174757,83.3132173576894,84.305637197903,84.8230016469244),
 .UNSPECIFIED.);
#5604=B_SPLINE_CURVE_WITH_KNOTS('',3,(#36466,#36467,#36468,#36469,#36470,
#36471,#36472,#36473,#36474,#36475),.UNSPECIFIED.,.F.,.F.,(4,1,1,1,1,1,
1,4),(78.5398163397448,78.9056897408581,79.8981095810717,80.8905294212853,
81.882949261499,82.8753691017126,83.8677889419262,84.8230016469244),
 .UNSPECIFIED.);
#5605=B_SPLINE_CURVE_WITH_KNOTS('',3,(#36480,#36481,#36482,#36483,#36484,
#36485,#36486,#36487,#36488,#36489,#36490),.UNSPECIFIED.,.F.,.F.,(4,1,1,
1,1,1,1,1,4),(72.2566310325653,72.3965991153394,73.389018955553,74.3814387957667,
75.3738586359803,76.3662784761939,77.3586983164076,78.3511181566212,78.5398163397448),
 .UNSPECIFIED.);
#5606=B_SPLINE_CURVE_WITH_KNOTS('',3,(#36491,#36492,#36493,#36494,#36495,
#36496,#36497,#36498,#36499,#36500),.UNSPECIFIED.,.F.,.F.,(4,1,1,1,1,1,
1,4),(72.2566310325651,72.9511706995763,73.9435905397899,74.9360103800035,
75.9284302202172,76.9208500604308,77.9132699006444,78.5398163397448),
 .UNSPECIFIED.);
#5607=B_SPLINE_CURVE_WITH_KNOTS('',3,(#36505,#36506,#36507,#36508,#36509,
#36510,#36511,#36512,#36513,#36514),.UNSPECIFIED.,.F.,.F.,(4,1,1,1,1,1,
1,4),(65.9734457253856,66.4420800740576,67.4344999142712,68.4269197544849,
69.4193395946985,70.4117594349121,71.4041792751258,72.2566310325653),
 .UNSPECIFIED.);
#5608=B_SPLINE_CURVE_WITH_KNOTS('',3,(#36515,#36516,#36517,#36518,#36519,
#36520,#36521,#36522,#36523,#36524,#36525),.UNSPECIFIED.,.F.,.F.,(4,1,1,
1,1,1,1,1,4),(65.9734457253856,66.0042318180808,66.9966516582945,67.9890714985081,
68.9814913387217,69.9739111789354,70.966331019149,71.9587508593626,72.2566310325651),
 .UNSPECIFIED.);
#5609=B_SPLINE_CURVE_WITH_KNOTS('',3,(#36530,#36531,#36532,#36533,#36534,
#36535,#36536,#36537,#36538,#36539),.UNSPECIFIED.,.F.,.F.,(4,1,1,1,1,1,
1,4),(59.690260418206,60.4875610327758,61.4799808729895,62.4724007132031,
63.4648205534167,64.4572403936303,65.449660233844,65.9734457253856),
 .UNSPECIFIED.);
#5610=B_SPLINE_CURVE_WITH_KNOTS('',3,(#36540,#36541,#36542,#36543,#36544,
#36545,#36546,#36547,#36548,#36549),.UNSPECIFIED.,.F.,.F.,(4,1,1,1,1,1,
1,4),(59.690260418206,60.049712776799,61.0421326170127,62.0345524572263,
63.0269722974399,64.0193921376536,65.0118119778672,65.9734457253856),
 .UNSPECIFIED.);
#5611=B_SPLINE_CURVE_WITH_KNOTS('',3,(#36554,#36555,#36556,#36557,#36558,
#36559,#36560,#36561,#36562,#36563,#36564),.UNSPECIFIED.,.F.,.F.,(4,1,1,
1,1,1,1,1,4),(53.4070751110265,53.5406221512804,54.533041991494,55.5254618317077,
56.5178816719213,57.5103015121349,58.5027213523486,59.4951411925622,59.690260418206),
 .UNSPECIFIED.);
#5612=B_SPLINE_CURVE_WITH_KNOTS('',3,(#36565,#36566,#36567,#36568,#36569,
#36570,#36571,#36572,#36573,#36574),.UNSPECIFIED.,.F.,.F.,(4,1,1,1,1,1,
1,4),(53.4070751110265,54.0951937355172,55.0876135757309,56.0800334159445,
57.0724532561581,58.0648730963718,59.0572929365854,59.690260418206),
 .UNSPECIFIED.);
#5613=B_SPLINE_CURVE_WITH_KNOTS('',3,(#36579,#36580,#36581,#36582,#36583,
#36584,#36585,#36586,#36587,#36588),.UNSPECIFIED.,.F.,.F.,(4,1,1,1,1,1,
1,4),(47.1238898038468,47.5861031099986,48.5785229502122,49.5709427904259,
50.5633626306395,51.5557824708531,52.5482023110668,53.4070751110265),
 .UNSPECIFIED.);
#5614=B_SPLINE_CURVE_WITH_KNOTS('',3,(#36589,#36590,#36591,#36592,#36593,
#36594,#36595,#36596,#36597,#36598,#36599),.UNSPECIFIED.,.F.,.F.,(4,1,1,
1,1,1,1,1,4),(47.1238898038468,47.1482548540218,48.1406746942354,49.1330945344491,
50.1255143746627,51.1179342148763,52.11035405509,53.1027738953036,53.4070751110265),
 .UNSPECIFIED.);
#5615=B_SPLINE_CURVE_WITH_KNOTS('',3,(#36604,#36605,#36606,#36607,#36608,
#36609,#36610,#36611,#36612,#36613),.UNSPECIFIED.,.F.,.F.,(4,1,1,1,1,1,
1,4),(40.8407044966672,41.6315840687168,42.6240039089304,43.6164237491441,
44.6088435893577,45.6012634295713,46.593683269785,47.1238898038468),
 .UNSPECIFIED.);
#5616=B_SPLINE_CURVE_WITH_KNOTS('',3,(#36614,#36615,#36616,#36617,#36618,
#36619,#36620,#36621,#36622,#36623),.UNSPECIFIED.,.F.,.F.,(4,1,1,1,1,1,
1,4),(40.8407044966672,41.19373581274,42.1861556529536,43.1785754931673,
44.1709953333809,45.1634151735945,46.1558350138082,47.1238898038468),
 .UNSPECIFIED.);
#5617=B_SPLINE_CURVE_WITH_KNOTS('',3,(#36628,#36629,#36630,#36631,#36632,
#36633,#36634,#36635,#36636,#36637,#36638),.UNSPECIFIED.,.F.,.F.,(4,1,1,
1,1,1,1,1,4),(34.5575191894877,34.6846451872214,35.677065027435,36.6694848676486,
37.6619047078623,38.6543245480759,39.6467443882895,40.6391642285032,40.8407044966672),
 .UNSPECIFIED.);
#5618=B_SPLINE_CURVE_WITH_KNOTS('',3,(#36639,#36640,#36641,#36642,#36643,
#36644,#36645,#36646,#36647,#36648),.UNSPECIFIED.,.F.,.F.,(4,1,1,1,1,1,
1,4),(34.5575191894877,35.2392167714582,36.2316366116718,37.2240564518855,
38.2164762920991,39.2088961323127,40.2013159725264,40.8407044966672),
 .UNSPECIFIED.);
#5619=B_SPLINE_CURVE_WITH_KNOTS('',3,(#36653,#36654,#36655,#36656,#36657,
#36658,#36659,#36660,#36661,#36662),.UNSPECIFIED.,.F.,.F.,(4,1,1,1,1,1,
1,4),(28.2743338823081,28.7301261459396,29.7225459861532,30.7149658263668,
31.7073856665805,32.6998055067941,33.6922253470077,34.5575191894877),
 .UNSPECIFIED.);
#5620=B_SPLINE_CURVE_WITH_KNOTS('',3,(#36663,#36664,#36665,#36666,#36667,
#36668,#36669,#36670,#36671,#36672,#36673),.UNSPECIFIED.,.F.,.F.,(4,1,1,
1,1,1,1,1,4),(28.2743338823081,28.2922778899628,29.2846977301764,30.2771175703901,
31.2695374106037,32.2619572508173,33.2543770910309,34.2467969312446,34.5575191894877),
 .UNSPECIFIED.);
#5621=B_SPLINE_CURVE_WITH_KNOTS('',3,(#36678,#36679,#36680,#36681,#36682,
#36683,#36684,#36685,#36686,#36687),.UNSPECIFIED.,.F.,.F.,(4,1,1,1,1,1,
1,4),(21.9911485751285,22.7756071046578,23.7680269448714,24.760446785085,
25.7528666252987,26.7452864655123,27.7377063057259,28.2743338823081),
 .UNSPECIFIED.);
#5622=B_SPLINE_CURVE_WITH_KNOTS('',3,(#36688,#36689,#36690,#36691,#36692,
#36693,#36694,#36695,#36696,#36697),.UNSPECIFIED.,.F.,.F.,(4,1,1,1,1,1,
1,4),(21.9911485751284,22.337758848681,23.3301786888946,24.3225985291083,
25.3150183693219,26.3074382095355,27.2998580497492,28.2743338823081),
 .UNSPECIFIED.);
#5623=B_SPLINE_CURVE_WITH_KNOTS('',3,(#36703,#36704,#36705,#36706,#36707),
 .UNSPECIFIED.,.F.,.F.,(4,1,4),(14.3984001269719,15.3908199671856,15.7079632679489),
 .UNSPECIFIED.);
#5624=B_SPLINE_CURVE_WITH_KNOTS('',3,(#36710,#36711,#36712,#36713,#36714),
 .UNSPECIFIED.,.F.,.F.,(4,1,4),(13.8759337553364,14.8362483829487,15.7079632679489),
 .UNSPECIFIED.);
#5625=B_SPLINE_CURVE_WITH_KNOTS('',3,(#36720,#36721,#36722,#36723),
 .UNSPECIFIED.,.F.,.F.,(4,4),(95.5573427486708,96.2647245007224),
 .UNSPECIFIED.);
#5626=B_SPLINE_CURVE_WITH_KNOTS('',3,(#36731,#36732,#36733,#36734,#36735,
#36736,#36737,#36738,#36739,#36740),.UNSPECIFIED.,.F.,.F.,(4,3,3,4),(-94.2477796076939,
-93.2874649800816,-92.295045139868,-91.8135687061555),.UNSPECIFIED.);
#5627=B_SPLINE_CURVE_WITH_KNOTS('',3,(#36745,#36746,#36747,#36748,#36749,
#36750,#36751,#36752,#36753,#36754,#36755,#36756,#36757,#36758,#36759,#36760,
#36761,#36762,#36763,#36764,#36765,#36766,#36767,#36768,#36769),
 .UNSPECIFIED.,.F.,.F.,(4,3,3,3,3,3,3,3,4),(89.2741574414912,89.3177856192271,
90.3102054594407,91.3026252996544,92.295045139868,93.2874649800816,94.2798848202953,
95.2723046605089,95.5573427486708),.UNSPECIFIED.);
#5628=B_SPLINE_CURVE_WITH_KNOTS('',3,(#36770,#36771,#36772,#36773,#36774,
#36775,#36776,#36777,#36778,#36779,#36780,#36781,#36782,#36783,#36784,#36785,
#36786,#36787,#36788,#36789,#36790,#36791),.UNSPECIFIED.,.F.,.F.,(4,3,3,
3,3,3,3,4),(-91.8135687061555,-91.3026252996543,-90.3102054594407,-89.3177856192271,
-88.3253657790134,-87.3329459387998,-86.3405260985862,-85.5303833989759),
 .UNSPECIFIED.);
#5629=B_SPLINE_CURVE_WITH_KNOTS('',3,(#36796,#36797,#36798,#36799,#36800,
#36801,#36802,#36803,#36804,#36805,#36806,#36807,#36808,#36809,#36810,#36811,
#36812,#36813,#36814,#36815,#36816,#36817),.UNSPECIFIED.,.F.,.F.,(4,3,3,
3,3,3,3,4),(82.9909721343117,83.3632665779453,84.3556864181589,85.3481062583725,
86.3405260985862,87.3329459387998,88.3253657790134,89.2741574414912),
 .UNSPECIFIED.);
#5630=B_SPLINE_CURVE_WITH_KNOTS('',3,(#36818,#36819,#36820,#36821,#36822,
#36823,#36824,#36825,#36826,#36827,#36828,#36829,#36830,#36831,#36832,#36833,
#36834,#36835,#36836,#36837,#36838,#36839,#36840,#36841,#36842),
 .UNSPECIFIED.,.F.,.F.,(4,3,3,3,3,3,3,3,4),(-85.5303833989759,-85.3481062583725,
-84.3556864181589,-83.3632665779453,-82.3708467377316,-81.378426897518,
-80.3860070573044,-79.3935872170907,-79.2471980917963),.UNSPECIFIED.);
#5631=B_SPLINE_CURVE_WITH_KNOTS('',3,(#36847,#36848,#36849,#36850,#36851,
#36852,#36853,#36854,#36855,#36856,#36857,#36858,#36859,#36860,#36861,#36862,
#36863,#36864,#36865,#36866,#36867,#36868),.UNSPECIFIED.,.F.,.F.,(4,3,3,
3,3,3,3,4),(76.7077868271321,77.4087475366635,78.4011673768771,79.3935872170907,
80.3860070573044,81.378426897518,82.3708467377316,82.9909721343117),
 .UNSPECIFIED.);
#5632=B_SPLINE_CURVE_WITH_KNOTS('',3,(#36869,#36870,#36871,#36872,#36873,
#36874,#36875,#36876,#36877,#36878,#36879,#36880,#36881,#36882,#36883,#36884,
#36885,#36886,#36887,#36888,#36889,#36890),.UNSPECIFIED.,.F.,.F.,(4,3,3,
3,3,3,3,4),(-79.2471980917963,-78.4011673768771,-77.4087475366634,-76.4163276964498,
-75.4239078562362,-74.4314880160225,-73.4390681758089,-72.9640127846167),
 .UNSPECIFIED.);
#5633=B_SPLINE_CURVE_WITH_KNOTS('',3,(#36895,#36896,#36897,#36898,#36899,
#36900,#36901,#36902,#36903,#36904,#36905,#36906,#36907,#36908,#36909,#36910,
#36911,#36912,#36913,#36914,#36915,#36916,#36917,#36918,#36919),
 .UNSPECIFIED.,.F.,.F.,(4,3,3,3,3,3,3,3,4),(70.4246015199524,70.461808655168,
71.4542284953817,72.4466483355953,73.4390681758089,74.4314880160226,75.4239078562362,
76.4163276964498,76.7077868271321),.UNSPECIFIED.);
#5634=B_SPLINE_CURVE_WITH_KNOTS('',3,(#36920,#36921,#36922,#36923,#36924,
#36925,#36926,#36927,#36928,#36929,#36930,#36931,#36932,#36933,#36934,#36935,
#36936,#36937,#36938,#36939,#36940,#36941),.UNSPECIFIED.,.F.,.F.,(4,3,3,
3,3,3,3,4),(-72.9640127846167,-72.4466483355953,-71.4542284953816,-70.461808655168,
-69.4693888149544,-68.4769689747407,-67.4845491345271,-66.6808274774371),
 .UNSPECIFIED.);
#5635=B_SPLINE_CURVE_WITH_KNOTS('',3,(#36946,#36947,#36948,#36949,#36950,
#36951,#36952,#36953,#36954,#36955,#36956,#36957,#36958,#36959,#36960,#36961,
#36962,#36963,#36964,#36965,#36966,#36967),.UNSPECIFIED.,.F.,.F.,(4,3,3,
3,3,3,3,4),(64.1414162127729,64.5072896138862,65.4997094540998,66.4921292943135,
67.4845491345271,68.4769689747407,69.4693888149544,70.4246015199524),
 .UNSPECIFIED.);
#5636=B_SPLINE_CURVE_WITH_KNOTS('',3,(#36968,#36969,#36970,#36971,#36972,
#36973,#36974,#36975,#36976,#36977,#36978,#36979,#36980,#36981,#36982,#36983,
#36984,#36985,#36986,#36987,#36988,#36989,#36990,#36991,#36992),
 .UNSPECIFIED.,.F.,.F.,(4,3,3,3,3,3,3,3,4),(-66.6808274774371,-66.4921292943135,
-65.4997094540998,-64.5072896138862,-63.5148697736726,-62.5224499334589,
-61.5300300932453,-60.5376102530317,-60.3976421702575),.UNSPECIFIED.);
#5637=B_SPLINE_CURVE_WITH_KNOTS('',3,(#36997,#36998,#36999,#37000,#37001,
#37002,#37003,#37004,#37005,#37006,#37007,#37008,#37009,#37010,#37011,#37012,
#37013,#37014,#37015,#37016,#37017,#37018),.UNSPECIFIED.,.F.,.F.,(4,3,3,
3,3,3,3,4),(57.8582309055933,58.5527705726044,59.545190412818,60.5376102530317,
61.5300300932453,62.5224499334589,63.5148697736726,64.1414162127729),
 .UNSPECIFIED.);
#5638=B_SPLINE_CURVE_WITH_KNOTS('',3,(#37019,#37020,#37021,#37022,#37023,
#37024,#37025,#37026,#37027,#37028,#37029,#37030,#37031,#37032,#37033,#37034,
#37035,#37036,#37037,#37038,#37039,#37040),.UNSPECIFIED.,.F.,.F.,(4,3,3,
3,3,3,3,4),(-60.3976421702575,-59.545190412818,-58.5527705726044,-57.5603507323908,
-56.5679308921771,-55.5755110519635,-54.5830912117499,-54.1144568630778),
 .UNSPECIFIED.);
#5639=B_SPLINE_CURVE_WITH_KNOTS('',3,(#37045,#37046,#37047,#37048,#37049,
#37050,#37051,#37052,#37053,#37054,#37055,#37056,#37057,#37058,#37059,#37060,
#37061,#37062,#37063,#37064,#37065,#37066,#37067,#37068,#37069),
 .UNSPECIFIED.,.F.,.F.,(4,3,3,3,3,3,3,3,4),(51.5750455984138,51.605831691109,
52.5982515313226,53.5906713715362,54.5830912117499,55.5755110519635,56.5679308921771,
57.5603507323908,57.8582309055933),.UNSPECIFIED.);
#5640=B_SPLINE_CURVE_WITH_KNOTS('',3,(#37070,#37071,#37072,#37073,#37074,
#37075,#37076,#37077,#37078,#37079,#37080,#37081,#37082,#37083,#37084,#37085,
#37086,#37087,#37088,#37089,#37090,#37091),.UNSPECIFIED.,.F.,.F.,(4,3,3,
3,3,3,3,4),(-54.1144568630778,-53.5906713715362,-52.5982515313226,-51.605831691109,
-50.6134118508953,-49.6209920106817,-48.6285721704681,-47.8312715558983),
 .UNSPECIFIED.);
#5641=B_SPLINE_CURVE_WITH_KNOTS('',3,(#37096,#37097,#37098,#37099,#37100,
#37101,#37102,#37103,#37104,#37105,#37106,#37107,#37108,#37109,#37110,#37111,
#37112,#37113,#37114,#37115,#37116,#37117),.UNSPECIFIED.,.F.,.F.,(4,3,3,
3,3,3,3,4),(45.2918602912341,45.6513126498272,46.6437324900408,47.6361523302544,
48.6285721704681,49.6209920106817,50.6134118508953,51.5750455984138),
 .UNSPECIFIED.);
#5642=B_SPLINE_CURVE_WITH_KNOTS('',3,(#37118,#37119,#37120,#37121,#37122,
#37123,#37124,#37125,#37126,#37127,#37128,#37129,#37130,#37131,#37132,#37133,
#37134,#37135,#37136,#37137,#37138,#37139,#37140,#37141,#37142),
 .UNSPECIFIED.,.F.,.F.,(4,3,3,3,3,3,3,3,4),(-47.8312715558983,-47.6361523302544,
-46.6437324900408,-45.6513126498272,-44.6588928096135,-43.6664729693999,
-42.6740531291863,-41.6816332889726,-41.5480862487187),.UNSPECIFIED.);
#5643=B_SPLINE_CURVE_WITH_KNOTS('',3,(#37147,#37148,#37149,#37150,#37151,
#37152,#37153,#37154,#37155,#37156,#37157,#37158,#37159,#37160,#37161,#37162,
#37163,#37164,#37165,#37166,#37167,#37168),.UNSPECIFIED.,.F.,.F.,(4,3,3,
3,3,3,3,4),(39.0086749840545,39.6967936085454,40.689213448759,41.6816332889726,
42.6740531291863,43.6664729693999,44.6588928096135,45.2918602912341),
 .UNSPECIFIED.);
#5644=B_SPLINE_CURVE_WITH_KNOTS('',3,(#37169,#37170,#37171,#37172,#37173,
#37174,#37175,#37176,#37177,#37178,#37179,#37180,#37181,#37182,#37183,#37184,
#37185,#37186,#37187,#37188,#37189,#37190),.UNSPECIFIED.,.F.,.F.,(4,3,3,
3,3,3,3,4),(-41.5480862487187,-40.689213448759,-39.6967936085454,-38.7043737683317,
-37.7119539281181,-36.7195340879045,-35.7271142476908,-35.2649009415392),
 .UNSPECIFIED.);
#5645=B_SPLINE_CURVE_WITH_KNOTS('',3,(#37195,#37196,#37197,#37198,#37199,
#37200,#37201,#37202,#37203,#37204,#37205,#37206,#37207,#37208,#37209,#37210,
#37211,#37212,#37213,#37214,#37215,#37216,#37217,#37218,#37219),
 .UNSPECIFIED.,.F.,.F.,(4,3,3,3,3,3,3,3,4),(32.725489676875,32.7498547270499,
33.7422745672636,34.7346944074772,35.7271142476908,36.7195340879045,37.7119539281181,
38.7043737683317,39.0086749840545),.UNSPECIFIED.);
#5646=B_SPLINE_CURVE_WITH_KNOTS('',3,(#37220,#37221,#37222,#37223,#37224,
#37225,#37226,#37227,#37228,#37229,#37230,#37231,#37232,#37233,#37234,#37235,
#37236,#37237,#37238,#37239,#37240,#37241),.UNSPECIFIED.,.F.,.F.,(4,3,3,
3,3,3,3,4),(-35.2649009415392,-34.7346944074772,-33.7422745672636,-32.7498547270499,
-31.7574348868363,-30.7650150466226,-29.772595206409,-28.9817156343596),
 .UNSPECIFIED.);
#5647=B_SPLINE_CURVE_WITH_KNOTS('',3,(#37246,#37247,#37248,#37249,#37250,
#37251,#37252,#37253,#37254,#37255,#37256,#37257,#37258,#37259,#37260,#37261,
#37262,#37263,#37264,#37265,#37266,#37267),.UNSPECIFIED.,.F.,.F.,(4,3,3,
3,3,3,3,4),(26.4423043696954,26.7953356857681,27.7877555259818,28.7801753661954,
29.772595206409,30.7650150466227,31.7574348868363,32.725489676875),
 .UNSPECIFIED.);
#5648=B_SPLINE_CURVE_WITH_KNOTS('',3,(#37268,#37269,#37270,#37271,#37272,
#37273,#37274,#37275,#37276,#37277,#37278,#37279,#37280,#37281,#37282,#37283,
#37284,#37285,#37286,#37287,#37288,#37289,#37290,#37291,#37292),
 .UNSPECIFIED.,.F.,.F.,(4,3,3,3,3,3,3,3,4),(-28.9817156343596,-28.7801753661954,
-27.7877555259817,-26.7953356857681,-25.8029158455545,-24.8104960053408,
-23.8180761651272,-22.8256563249136,-22.6985303271799),.UNSPECIFIED.);
#5649=B_SPLINE_CURVE_WITH_KNOTS('',3,(#37297,#37298,#37299,#37300,#37301,
#37302,#37303,#37304,#37305,#37306,#37307,#37308,#37309,#37310,#37311,#37312,
#37313,#37314,#37315,#37316,#37317,#37318),.UNSPECIFIED.,.F.,.F.,(4,3,3,
3,3,3,3,4),(20.1591190625157,20.8408166444863,21.8332364846999,22.8256563249136,
23.8180761651272,24.8104960053409,25.8029158455545,26.4423043696954),
 .UNSPECIFIED.);
#5650=B_SPLINE_CURVE_WITH_KNOTS('',3,(#37319,#37320,#37321,#37322,#37323,
#37324,#37325,#37326,#37327,#37328,#37329,#37330,#37331,#37332,#37333,#37334,
#37335,#37336,#37337,#37338,#37339,#37340),.UNSPECIFIED.,.F.,.F.,(4,3,3,
3,3,3,3,4),(-22.6985303271799,-21.8332364846999,-20.8408166444863,-19.8483968042727,
-18.855976964059,-17.8635571238454,-16.8711372836318,-16.4153450200004),
 .UNSPECIFIED.);
#5651=B_SPLINE_CURVE_WITH_KNOTS('',3,(#37345,#37346,#37347,#37348,#37349,
#37350,#37351,#37352,#37353,#37354,#37355,#37356,#37357,#37358,#37359,#37360,
#37361,#37362,#37363,#37364,#37365,#37366,#37367,#37368,#37369),
 .UNSPECIFIED.,.F.,.F.,(4,3,3,3,3,3,3,3,4),(13.8759337553361,13.8938777629909,
14.8862976032045,15.8787174434181,16.8711372836318,17.8635571238454,18.855976964059,
19.8483968042727,20.1591190625157),.UNSPECIFIED.);
#5652=B_SPLINE_CURVE_WITH_KNOTS('',3,(#37370,#37371,#37372,#37373,#37374,
#37375,#37376,#37377,#37378,#37379,#37380,#37381,#37382,#37383,#37384,#37385,
#37386,#37387,#37388,#37389,#37390,#37391),.UNSPECIFIED.,.F.,.F.,(4,3,3,
3,3,3,3,4),(-16.4153450200004,-15.8787174434181,-14.8862976032045,-13.8938777629909,
-12.9014579227772,-11.9090380825636,-10.91661824235,-10.1321597128208),
 .UNSPECIFIED.);
#5653=B_SPLINE_CURVE_WITH_KNOTS('',3,(#37397,#37398,#37399,#37400,#37401,
#37402,#37403,#37404,#37405,#37406,#37407,#37408,#37409),.UNSPECIFIED.,
 .F.,.F.,(4,3,3,3,4),(-3.84897440564123,-2.9772595206409,-1.98483968042727,
-0.99241984021363,0.),.UNSPECIFIED.);
#5654=B_SPLINE_CURVE_WITH_KNOTS('',3,(#37412,#37413,#37414,#37415,#37416,
#37417,#37418,#37419,#37420,#37421,#37422,#37423,#37424,#37425,#37426,#37427,
#37428,#37429,#37430),.UNSPECIFIED.,.F.,.F.,(4,3,3,3,3,3,4),(2.01694489302852,
2.9772595206409,3.96967936085453,4.96209920106817,5.9545190412818,6.94693888149544,
7.59274844815659),.UNSPECIFIED.);
#5655=B_SPLINE_CURVE_WITH_KNOTS('',3,(#37436,#37437,#37438,#37439,#37440,
#37441,#37442,#37443),.UNSPECIFIED.,.F.,.F.,(4,1,1,1,1,4),(103.672557568463,
104.154034002176,105.146453842389,106.138873682603,107.131293522817,108.12371336303),
 .UNSPECIFIED.);
#5656=B_SPLINE_CURVE_WITH_KNOTS('',3,(#37446,#37447,#37448,#37449,#37450,
#37451,#37452,#37453,#37454),.UNSPECIFIED.,.F.,.F.,(4,1,1,1,1,1,4),(103.672557568463,
103.716185746199,104.708605586413,105.701025426626,106.69344526684,107.685865107053,
108.646179734666),.UNSPECIFIED.);
#5657=B_SPLINE_CURVE_WITH_KNOTS('',3,(#37459,#37460,#37461,#37462,#37463,
#37464,#37465,#37466,#37467,#37468),.UNSPECIFIED.,.F.,.F.,(4,1,1,1,1,1,
1,4),(97.3893722612835,98.1995149608939,99.1919348011075,100.184354641321,
101.176774481535,102.169194321748,103.161614161962,103.672557568463),
 .UNSPECIFIED.);
#5658=B_SPLINE_CURVE_WITH_KNOTS('',3,(#37469,#37470,#37471,#37472,#37473,
#37474,#37475,#37476,#37477,#37478),.UNSPECIFIED.,.F.,.F.,(4,1,1,1,1,1,
1,4),(97.3893722612835,97.7616667049171,98.7540865451307,99.7465063853443,
100.738926225558,101.731346065772,102.723765905985,103.672557568463),
 .UNSPECIFIED.);
#5659=B_SPLINE_CURVE_WITH_KNOTS('',3,(#37483,#37484,#37485,#37486,#37487,
#37488,#37489,#37490,#37491,#37492,#37493),.UNSPECIFIED.,.F.,.F.,(4,1,1,
1,1,1,1,1,4),(91.106186954104,91.2525760793984,92.2449959196121,93.2374157598257,
94.2298356000393,95.222255440253,96.2146752804666,97.2070951206802,97.3893722612835),
 .UNSPECIFIED.);
#5660=B_SPLINE_CURVE_WITH_KNOTS('',3,(#37494,#37495,#37496,#37497,#37498,
#37499,#37500,#37501,#37502,#37503),.UNSPECIFIED.,.F.,.F.,(4,1,1,1,1,1,
1,4),(91.106186954104,91.8071476636353,92.7995675038489,93.7919873440625,
94.7844071842762,95.7768270244898,96.7692468647034,97.3893722612835),
 .UNSPECIFIED.);
#5661=B_SPLINE_CURVE_WITH_KNOTS('',3,(#37508,#37509,#37510,#37511,#37512,
#37513,#37514,#37515,#37516,#37517),.UNSPECIFIED.,.F.,.F.,(4,1,1,1,1,1,
1,4),(84.8230016469244,85.2980570381166,86.2904768783302,87.2828967185439,
88.2753165587575,89.2677363989711,90.2601562391848,91.106186954104),
 .UNSPECIFIED.);
#5662=B_SPLINE_CURVE_WITH_KNOTS('',3,(#37518,#37519,#37520,#37521,#37522,
#37523,#37524,#37525,#37526,#37527,#37528),.UNSPECIFIED.,.F.,.F.,(4,1,1,
1,1,1,1,1,4),(84.8230016469244,84.8602087821398,85.8526286223535,86.8450484625671,
87.8374683027807,88.8298881429944,89.822307983208,90.8147278234216,91.106186954104),
 .UNSPECIFIED.);
#5663=B_SPLINE_CURVE_WITH_KNOTS('',3,(#37533,#37534,#37535,#37536,#37537,
#37538,#37539,#37540,#37541,#37542),.UNSPECIFIED.,.F.,.F.,(4,1,1,1,1,1,
1,4),(78.5398163397448,79.3435379968348,80.3359578370484,81.3283776772621,
82.3207975174757,83.3132173576893,84.305637197903,84.8230016469244),
 .UNSPECIFIED.);
#5664=B_SPLINE_CURVE_WITH_KNOTS('',3,(#37543,#37544,#37545,#37546,#37547,
#37548,#37549,#37550,#37551,#37552),.UNSPECIFIED.,.F.,.F.,(4,1,1,1,1,1,
1,4),(78.5398163397448,78.905689740858,79.8981095810717,80.8905294212853,
81.8829492614989,82.8753691017126,83.8677889419262,84.8230016469244),
 .UNSPECIFIED.);
#5665=B_SPLINE_CURVE_WITH_KNOTS('',3,(#37557,#37558,#37559,#37560,#37561,
#37562,#37563,#37564,#37565,#37566,#37567),.UNSPECIFIED.,.F.,.F.,(4,1,1,
1,1,1,1,1,4),(72.2566310325653,72.3965991153394,73.389018955553,74.3814387957666,
75.3738586359803,76.3662784761939,77.3586983164075,78.3511181566212,78.5398163397448),
 .UNSPECIFIED.);
#5666=B_SPLINE_CURVE_WITH_KNOTS('',3,(#37568,#37569,#37570,#37571,#37572,
#37573,#37574,#37575,#37576,#37577),.UNSPECIFIED.,.F.,.F.,(4,1,1,1,1,1,
1,4),(72.2566310325651,72.9511706995762,73.9435905397899,74.9360103800035,
75.9284302202171,76.9208500604308,77.9132699006444,78.5398163397448),
 .UNSPECIFIED.);
#5667=B_SPLINE_CURVE_WITH_KNOTS('',3,(#37582,#37583,#37584,#37585,#37586,
#37587,#37588,#37589,#37590,#37591),.UNSPECIFIED.,.F.,.F.,(4,1,1,1,1,1,
1,4),(65.9734457253856,66.4420800740576,67.4344999142712,68.4269197544848,
69.4193395946985,70.4117594349121,71.4041792751257,72.2566310325653),
 .UNSPECIFIED.);
#5668=B_SPLINE_CURVE_WITH_KNOTS('',3,(#37592,#37593,#37594,#37595,#37596,
#37597,#37598,#37599,#37600,#37601,#37602),.UNSPECIFIED.,.F.,.F.,(4,1,1,
1,1,1,1,1,4),(65.9734457253856,66.0042318180808,66.9966516582944,67.9890714985081,
68.9814913387217,69.9739111789353,70.966331019149,71.9587508593626,72.2566310325651),
 .UNSPECIFIED.);
#5669=B_SPLINE_CURVE_WITH_KNOTS('',3,(#37607,#37608,#37609,#37610,#37611,
#37612,#37613,#37614,#37615,#37616),.UNSPECIFIED.,.F.,.F.,(4,1,1,1,1,1,
1,4),(59.690260418206,60.4875610327758,61.4799808729894,62.472400713203,
63.4648205534167,64.4572403936303,65.4496602338439,65.9734457253856),
 .UNSPECIFIED.);
#5670=B_SPLINE_CURVE_WITH_KNOTS('',3,(#37617,#37618,#37619,#37620,#37621,
#37622,#37623,#37624,#37625,#37626),.UNSPECIFIED.,.F.,.F.,(4,1,1,1,1,1,
1,4),(59.690260418206,60.049712776799,61.0421326170126,62.0345524572262,
63.0269722974399,64.0193921376535,65.0118119778672,65.9734457253856),
 .UNSPECIFIED.);
#5671=B_SPLINE_CURVE_WITH_KNOTS('',3,(#37631,#37632,#37633,#37634,#37635,
#37636,#37637,#37638,#37639,#37640,#37641),.UNSPECIFIED.,.F.,.F.,(4,1,1,
1,1,1,1,1,4),(53.4070751110265,53.5406221512803,54.533041991494,55.5254618317076,
56.5178816719212,57.5103015121349,58.5027213523485,59.4951411925621,59.690260418206),
 .UNSPECIFIED.);
#5672=B_SPLINE_CURVE_WITH_KNOTS('',3,(#37642,#37643,#37644,#37645,#37646,
#37647,#37648,#37649,#37650,#37651),.UNSPECIFIED.,.F.,.F.,(4,1,1,1,1,1,
1,4),(53.4070751110265,54.0951937355172,55.0876135757308,56.0800334159444,
57.0724532561581,58.0648730963717,59.0572929365853,59.690260418206),
 .UNSPECIFIED.);
#5673=B_SPLINE_CURVE_WITH_KNOTS('',3,(#37656,#37657,#37658,#37659,#37660,
#37661,#37662,#37663,#37664,#37665),.UNSPECIFIED.,.F.,.F.,(4,1,1,1,1,1,
1,4),(47.1238898038468,47.5861031099985,48.5785229502122,49.5709427904258,
50.5633626306394,51.5557824708531,52.5482023110667,53.4070751110265),
 .UNSPECIFIED.);
#5674=B_SPLINE_CURVE_WITH_KNOTS('',3,(#37666,#37667,#37668,#37669,#37670,
#37671,#37672,#37673,#37674,#37675,#37676),.UNSPECIFIED.,.F.,.F.,(4,1,1,
1,1,1,1,1,4),(47.1238898038468,47.1482548540217,48.1406746942354,49.133094534449,
50.1255143746626,51.1179342148763,52.1103540550899,53.1027738953035,53.4070751110265),
 .UNSPECIFIED.);
#5675=B_SPLINE_CURVE_WITH_KNOTS('',3,(#37681,#37682,#37683,#37684,#37685,
#37686,#37687,#37688,#37689,#37690),.UNSPECIFIED.,.F.,.F.,(4,1,1,1,1,1,
1,4),(40.8407044966672,41.6315840687167,42.6240039089303,43.616423749144,
44.6088435893576,45.6012634295713,46.5936832697849,47.1238898038468),
 .UNSPECIFIED.);
#5676=B_SPLINE_CURVE_WITH_KNOTS('',3,(#37691,#37692,#37693,#37694,#37695,
#37696,#37697,#37698,#37699,#37700),.UNSPECIFIED.,.F.,.F.,(4,1,1,1,1,1,
1,4),(40.8407044966672,41.1937358127399,42.1861556529536,43.1785754931672,
44.1709953333808,45.1634151735945,46.1558350138081,47.1238898038468),
 .UNSPECIFIED.);
#5677=B_SPLINE_CURVE_WITH_KNOTS('',3,(#37705,#37706,#37707,#37708,#37709,
#37710,#37711,#37712,#37713,#37714,#37715),.UNSPECIFIED.,.F.,.F.,(4,1,1,
1,1,1,1,1,4),(34.5575191894877,34.6846451872213,35.6770650274349,36.6694848676485,
37.6619047078622,38.6543245480758,39.6467443882894,40.6391642285031,40.8407044966672),
 .UNSPECIFIED.);
#5678=B_SPLINE_CURVE_WITH_KNOTS('',3,(#37716,#37717,#37718,#37719,#37720,
#37721,#37722,#37723,#37724,#37725),.UNSPECIFIED.,.F.,.F.,(4,1,1,1,1,1,
1,4),(34.5575191894877,35.2392167714581,36.2316366116718,37.2240564518854,
38.216476292099,39.2088961323127,40.2013159725263,40.8407044966672),
 .UNSPECIFIED.);
#5679=B_SPLINE_CURVE_WITH_KNOTS('',3,(#37730,#37731,#37732,#37733,#37734,
#37735,#37736,#37737,#37738,#37739),.UNSPECIFIED.,.F.,.F.,(4,1,1,1,1,1,
1,4),(28.2743338823081,28.7301261459395,29.7225459861531,30.7149658263667,
31.7073856665804,32.699805506794,33.6922253470076,34.5575191894877),
 .UNSPECIFIED.);
#5680=B_SPLINE_CURVE_WITH_KNOTS('',3,(#37740,#37741,#37742,#37743,#37744,
#37745,#37746,#37747,#37748,#37749,#37750),.UNSPECIFIED.,.F.,.F.,(4,1,1,
1,1,1,1,1,4),(28.2743338823081,28.2922778899627,29.2846977301763,30.27711757039,
31.2695374106036,32.2619572508172,33.2543770910309,34.2467969312445,34.5575191894877),
 .UNSPECIFIED.);
#5681=B_SPLINE_CURVE_WITH_KNOTS('',3,(#37755,#37756,#37757,#37758,#37759,
#37760,#37761,#37762,#37763,#37764),.UNSPECIFIED.,.F.,.F.,(4,1,1,1,1,1,
1,4),(21.9911485751285,22.7756071046577,23.7680269448713,24.7604467850849,
25.7528666252986,26.7452864655122,27.7377063057258,28.2743338823081),
 .UNSPECIFIED.);
#5682=B_SPLINE_CURVE_WITH_KNOTS('',3,(#37765,#37766,#37767,#37768,#37769,
#37770,#37771,#37772,#37773,#37774),.UNSPECIFIED.,.F.,.F.,(4,1,1,1,1,1,
1,4),(21.9911485751284,22.3377588486809,23.3301786888945,24.3225985291082,
25.3150183693218,26.3074382095354,27.2998580497491,28.2743338823081),
 .UNSPECIFIED.);
#5683=B_SPLINE_CURVE_WITH_KNOTS('',3,(#37780,#37781,#37782,#37783,#37784),
 .UNSPECIFIED.,.F.,.F.,(4,1,4),(14.3984001269718,15.3908199671854,15.7079632679489),
 .UNSPECIFIED.);
#5684=B_SPLINE_CURVE_WITH_KNOTS('',3,(#37787,#37788,#37789,#37790,#37791),
 .UNSPECIFIED.,.F.,.F.,(4,1,4),(13.8759337553363,14.8362483829486,15.7079632679488),
 .UNSPECIFIED.);
#5685=B_SPLINE_CURVE_WITH_KNOTS('',3,(#37797,#37798,#37799,#37800),
 .UNSPECIFIED.,.F.,.F.,(4,4),(95.5573427486707,96.2647245007224),
 .UNSPECIFIED.);
#5686=B_SPLINE_CURVE_WITH_KNOTS('',3,(#37808,#37809,#37810,#37811,#37812,
#37813,#37814,#37815,#37816,#37817),.UNSPECIFIED.,.F.,.F.,(4,3,3,4),(-94.2477796076938,
-93.2874649800815,-92.2950451398679,-91.8135687061554),.UNSPECIFIED.);
#5687=B_SPLINE_CURVE_WITH_KNOTS('',3,(#37822,#37823,#37824,#37825,#37826,
#37827,#37828,#37829,#37830,#37831,#37832,#37833,#37834,#37835,#37836,#37837,
#37838,#37839,#37840,#37841,#37842,#37843,#37844,#37845,#37846),
 .UNSPECIFIED.,.F.,.F.,(4,3,3,3,3,3,3,3,4),(89.2741574414911,89.317785619227,
90.3102054594406,91.3026252996542,92.2950451398679,93.2874649800815,94.2798848202951,
95.2723046605088,95.5573427486707),.UNSPECIFIED.);
#5688=B_SPLINE_CURVE_WITH_KNOTS('',3,(#37847,#37848,#37849,#37850,#37851,
#37852,#37853,#37854,#37855,#37856,#37857,#37858,#37859,#37860,#37861,#37862,
#37863,#37864,#37865,#37866,#37867,#37868),.UNSPECIFIED.,.F.,.F.,(4,3,3,
3,3,3,3,4),(-91.8135687061554,-91.3026252996542,-90.3102054594406,-89.317785619227,
-88.3253657790133,-87.3329459387997,-86.3405260985861,-85.5303833989757),
 .UNSPECIFIED.);
#5689=B_SPLINE_CURVE_WITH_KNOTS('',3,(#37873,#37874,#37875,#37876,#37877,
#37878,#37879,#37880,#37881,#37882,#37883,#37884,#37885,#37886,#37887,#37888,
#37889,#37890,#37891,#37892,#37893,#37894),.UNSPECIFIED.,.F.,.F.,(4,3,3,
3,3,3,3,4),(82.9909721343116,83.3632665779452,84.3556864181588,85.3481062583724,
86.3405260985861,87.3329459387997,88.3253657790133,89.2741574414911),
 .UNSPECIFIED.);
#5690=B_SPLINE_CURVE_WITH_KNOTS('',3,(#37895,#37896,#37897,#37898,#37899,
#37900,#37901,#37902,#37903,#37904,#37905,#37906,#37907,#37908,#37909,#37910,
#37911,#37912,#37913,#37914,#37915,#37916,#37917,#37918,#37919),
 .UNSPECIFIED.,.F.,.F.,(4,3,3,3,3,3,3,3,4),(-85.5303833989757,-85.3481062583724,
-84.3556864181588,-83.3632665779452,-82.3708467377315,-81.3784268975179,
-80.3860070573043,-79.3935872170906,-79.2471980917961),.UNSPECIFIED.);
#5691=B_SPLINE_CURVE_WITH_KNOTS('',3,(#37924,#37925,#37926,#37927,#37928,
#37929,#37930,#37931,#37932,#37933,#37934,#37935,#37936,#37937,#37938,#37939,
#37940,#37941,#37942,#37943,#37944,#37945),.UNSPECIFIED.,.F.,.F.,(4,3,3,
3,3,3,3,4),(76.7077868271319,77.4087475366634,78.401167376877,79.3935872170906,
80.3860070573043,81.3784268975179,82.3708467377315,82.9909721343116),
 .UNSPECIFIED.);
#5692=B_SPLINE_CURVE_WITH_KNOTS('',3,(#37946,#37947,#37948,#37949,#37950,
#37951,#37952,#37953,#37954,#37955,#37956,#37957,#37958,#37959,#37960,#37961,
#37962,#37963,#37964,#37965,#37966,#37967),.UNSPECIFIED.,.F.,.F.,(4,3,3,
3,3,3,3,4),(-79.2471980917961,-78.401167376877,-77.4087475366633,-76.4163276964497,
-75.4239078562361,-74.4314880160224,-73.4390681758088,-72.9640127846165),
 .UNSPECIFIED.);
#5693=B_SPLINE_CURVE_WITH_KNOTS('',3,(#37972,#37973,#37974,#37975,#37976,
#37977,#37978,#37979,#37980,#37981,#37982,#37983,#37984,#37985,#37986,#37987,
#37988,#37989,#37990,#37991,#37992,#37993,#37994,#37995,#37996),
 .UNSPECIFIED.,.F.,.F.,(4,3,3,3,3,3,3,3,4),(70.4246015199523,70.4618086551679,
71.4542284953816,72.4466483355952,73.4390681758088,74.4314880160225,75.4239078562361,
76.4163276964497,76.7077868271319),.UNSPECIFIED.);
#5694=B_SPLINE_CURVE_WITH_KNOTS('',3,(#37997,#37998,#37999,#38000,#38001,
#38002,#38003,#38004,#38005,#38006,#38007,#38008,#38009,#38010,#38011,#38012,
#38013,#38014,#38015,#38016,#38017,#38018),.UNSPECIFIED.,.F.,.F.,(4,3,3,
3,3,3,3,4),(-72.9640127846165,-72.4466483355952,-71.4542284953815,-70.4618086551679,
-69.4693888149543,-68.4769689747406,-67.484549134527,-66.680827477437),
 .UNSPECIFIED.);
#5695=B_SPLINE_CURVE_WITH_KNOTS('',3,(#38023,#38024,#38025,#38026,#38027,
#38028,#38029,#38030,#38031,#38032,#38033,#38034,#38035,#38036,#38037,#38038,
#38039,#38040,#38041,#38042,#38043,#38044),.UNSPECIFIED.,.F.,.F.,(4,3,3,
3,3,3,3,4),(64.1414162127728,64.5072896138861,65.4997094540998,66.4921292943134,
67.484549134527,68.4769689747407,69.4693888149543,70.4246015199523),
 .UNSPECIFIED.);
#5696=B_SPLINE_CURVE_WITH_KNOTS('',3,(#38045,#38046,#38047,#38048,#38049,
#38050,#38051,#38052,#38053,#38054,#38055,#38056,#38057,#38058,#38059,#38060,
#38061,#38062,#38063,#38064,#38065,#38066,#38067,#38068,#38069),
 .UNSPECIFIED.,.F.,.F.,(4,3,3,3,3,3,3,3,4),(-66.680827477437,-66.4921292943134,
-65.4997094540998,-64.5072896138861,-63.5148697736725,-62.5224499334589,
-61.5300300932452,-60.5376102530316,-60.3976421702573),.UNSPECIFIED.);
#5697=B_SPLINE_CURVE_WITH_KNOTS('',3,(#38074,#38075,#38076,#38077,#38078,
#38079,#38080,#38081,#38082,#38083,#38084,#38085,#38086,#38087,#38088,#38089,
#38090,#38091,#38092,#38093,#38094,#38095),.UNSPECIFIED.,.F.,.F.,(4,3,3,
3,3,3,3,4),(57.8582309055932,58.5527705726043,59.545190412818,60.5376102530316,
61.5300300932452,62.5224499334589,63.5148697736725,64.1414162127728),
 .UNSPECIFIED.);
#5698=B_SPLINE_CURVE_WITH_KNOTS('',3,(#38096,#38097,#38098,#38099,#38100,
#38101,#38102,#38103,#38104,#38105,#38106,#38107,#38108,#38109,#38110,#38111,
#38112,#38113,#38114,#38115,#38116,#38117),.UNSPECIFIED.,.F.,.F.,(4,3,3,
3,3,3,3,4),(-60.3976421702573,-59.545190412818,-58.5527705726043,-57.5603507323907,
-56.5679308921771,-55.5755110519634,-54.5830912117498,-54.1144568630777),
 .UNSPECIFIED.);
#5699=B_SPLINE_CURVE_WITH_KNOTS('',3,(#38122,#38123,#38124,#38125,#38126,
#38127,#38128,#38129,#38130,#38131,#38132,#38133,#38134,#38135,#38136,#38137,
#38138,#38139,#38140,#38141,#38142,#38143,#38144,#38145,#38146),
 .UNSPECIFIED.,.F.,.F.,(4,3,3,3,3,3,3,3,4),(51.5750455984135,51.6058316911089,
52.5982515313225,53.5906713715362,54.5830912117498,55.5755110519634,56.5679308921771,
57.5603507323907,57.8582309055932),.UNSPECIFIED.);
#5700=B_SPLINE_CURVE_WITH_KNOTS('',3,(#38147,#38148,#38149,#38150,#38151,
#38152,#38153,#38154,#38155,#38156,#38157,#38158,#38159,#38160,#38161,#38162,
#38163,#38164,#38165,#38166,#38167,#38168),.UNSPECIFIED.,.F.,.F.,(4,3,3,
3,3,3,3,4),(-54.1144568630777,-53.5906713715362,-52.5982515313225,-51.6058316911089,
-50.6134118508953,-49.6209920106816,-48.628572170468,-47.8312715558982),
 .UNSPECIFIED.);
#5701=B_SPLINE_CURVE_WITH_KNOTS('',3,(#38173,#38174,#38175,#38176,#38177,
#38178,#38179,#38180,#38181,#38182,#38183,#38184,#38185,#38186,#38187,#38188,
#38189,#38190,#38191,#38192,#38193,#38194),.UNSPECIFIED.,.F.,.F.,(4,3,3,
3,3,3,3,4),(45.291860291234,45.6513126498271,46.6437324900407,47.6361523302544,
48.628572170468,49.6209920106816,50.6134118508953,51.5750455984135),
 .UNSPECIFIED.);
#5702=B_SPLINE_CURVE_WITH_KNOTS('',3,(#38195,#38196,#38197,#38198,#38199,
#38200,#38201,#38202,#38203,#38204,#38205,#38206,#38207,#38208,#38209,#38210,
#38211,#38212,#38213,#38214,#38215,#38216,#38217,#38218,#38219),
 .UNSPECIFIED.,.F.,.F.,(4,3,3,3,3,3,3,3,4),(-47.8312715558982,-47.6361523302544,
-46.6437324900407,-45.6513126498271,-44.6588928096135,-43.6664729693998,
-42.6740531291862,-41.6816332889726,-41.5480862487186),.UNSPECIFIED.);
#5703=B_SPLINE_CURVE_WITH_KNOTS('',3,(#38224,#38225,#38226,#38227,#38228,
#38229,#38230,#38231,#38232,#38233,#38234,#38235,#38236,#38237,#38238,#38239,
#38240,#38241,#38242,#38243,#38244,#38245),.UNSPECIFIED.,.F.,.F.,(4,3,3,
3,3,3,3,4),(39.0086749840544,39.6967936085453,40.6892134487589,41.6816332889726,
42.6740531291862,43.6664729693998,44.6588928096135,45.291860291234),
 .UNSPECIFIED.);
#5704=B_SPLINE_CURVE_WITH_KNOTS('',3,(#38246,#38247,#38248,#38249,#38250,
#38251,#38252,#38253,#38254,#38255,#38256,#38257,#38258,#38259,#38260,#38261,
#38262,#38263,#38264,#38265,#38266,#38267),.UNSPECIFIED.,.F.,.F.,(4,3,3,
3,3,3,3,4),(-41.5480862487186,-40.6892134487589,-39.6967936085453,-38.7043737683317,
-37.711953928118,-36.7195340879044,-35.7271142476908,-35.2649009415389),
 .UNSPECIFIED.);
#5705=B_SPLINE_CURVE_WITH_KNOTS('',3,(#38272,#38273,#38274,#38275,#38276,
#38277,#38278,#38279,#38280,#38281,#38282,#38283,#38284,#38285,#38286,#38287,
#38288,#38289,#38290,#38291,#38292,#38293,#38294,#38295,#38296),
 .UNSPECIFIED.,.F.,.F.,(4,3,3,3,3,3,3,3,4),(32.7254896768748,32.7498547270499,
33.7422745672635,34.7346944074771,35.7271142476908,36.7195340879044,37.711953928118,
38.7043737683317,39.0086749840544),.UNSPECIFIED.);
#5706=B_SPLINE_CURVE_WITH_KNOTS('',3,(#38297,#38298,#38299,#38300,#38301,
#38302,#38303,#38304,#38305,#38306,#38307,#38308,#38309,#38310,#38311,#38312,
#38313,#38314,#38315,#38316,#38317,#38318),.UNSPECIFIED.,.F.,.F.,(4,3,3,
3,3,3,3,4),(-35.2649009415389,-34.7346944074771,-33.7422745672635,-32.7498547270499,
-31.7574348868362,-30.7650150466226,-29.772595206409,-28.9817156343594),
 .UNSPECIFIED.);
#5707=B_SPLINE_CURVE_WITH_KNOTS('',3,(#38323,#38324,#38325,#38326,#38327,
#38328,#38329,#38330,#38331,#38332,#38333,#38334,#38335,#38336,#38337,#38338,
#38339,#38340,#38341,#38342,#38343,#38344),.UNSPECIFIED.,.F.,.F.,(4,3,3,
3,3,3,3,4),(26.4423043696952,26.7953356857681,27.7877555259817,28.7801753661954,
29.772595206409,30.7650150466226,31.7574348868363,32.7254896768748),
 .UNSPECIFIED.);
#5708=B_SPLINE_CURVE_WITH_KNOTS('',3,(#38345,#38346,#38347,#38348,#38349,
#38350,#38351,#38352,#38353,#38354,#38355,#38356,#38357,#38358,#38359,#38360,
#38361,#38362,#38363,#38364,#38365,#38366,#38367,#38368,#38369),
 .UNSPECIFIED.,.F.,.F.,(4,3,3,3,3,3,3,3,4),(-28.9817156343594,-28.7801753661953,
-27.7877555259817,-26.7953356857681,-25.8029158455544,-24.8104960053408,
-23.8180761651272,-22.8256563249135,-22.6985303271798),.UNSPECIFIED.);
#5709=B_SPLINE_CURVE_WITH_KNOTS('',3,(#38374,#38375,#38376,#38377,#38378,
#38379,#38380,#38381,#38382,#38383,#38384,#38385,#38386,#38387,#38388,#38389,
#38390,#38391,#38392,#38393,#38394,#38395),.UNSPECIFIED.,.F.,.F.,(4,3,3,
3,3,3,3,4),(20.1591190625156,20.8408166444863,21.8332364846999,22.8256563249136,
23.8180761651272,24.8104960053408,25.8029158455545,26.4423043696952),
 .UNSPECIFIED.);
#5710=B_SPLINE_CURVE_WITH_KNOTS('',3,(#38396,#38397,#38398,#38399,#38400,
#38401,#38402,#38403,#38404,#38405,#38406,#38407,#38408,#38409,#38410,#38411,
#38412,#38413,#38414,#38415,#38416,#38417),.UNSPECIFIED.,.F.,.F.,(4,3,3,
3,3,3,3,4),(-22.6985303271798,-21.8332364846999,-20.8408166444863,-19.8483968042727,
-18.855976964059,-17.8635571238454,-16.8711372836318,-16.4153450200002),
 .UNSPECIFIED.);
#5711=B_SPLINE_CURVE_WITH_KNOTS('',3,(#38422,#38423,#38424,#38425,#38426,
#38427,#38428,#38429,#38430,#38431,#38432,#38433,#38434,#38435,#38436,#38437,
#38438,#38439,#38440,#38441,#38442,#38443,#38444,#38445,#38446),
 .UNSPECIFIED.,.F.,.F.,(4,3,3,3,3,3,3,3,4),(13.875933755336,13.8938777629909,
14.8862976032045,15.8787174434181,16.8711372836318,17.8635571238454,18.855976964059,
19.8483968042727,20.1591190625156),.UNSPECIFIED.);
#5712=B_SPLINE_CURVE_WITH_KNOTS('',3,(#38447,#38448,#38449,#38450,#38451,
#38452,#38453,#38454,#38455,#38456,#38457,#38458,#38459,#38460,#38461,#38462,
#38463,#38464,#38465,#38466,#38467,#38468),.UNSPECIFIED.,.F.,.F.,(4,3,3,
3,3,3,3,4),(-16.4153450200002,-15.8787174434181,-14.8862976032045,-13.8938777629909,
-12.9014579227772,-11.9090380825636,-10.91661824235,-10.1321597128207),
 .UNSPECIFIED.);
#5713=B_SPLINE_CURVE_WITH_KNOTS('',3,(#38474,#38475,#38476,#38477,#38478,
#38479,#38480,#38481,#38482,#38483,#38484,#38485,#38486),.UNSPECIFIED.,
 .F.,.F.,(4,3,3,3,4),(-3.848974405641,-2.9772595206409,-1.98483968042726,
-0.992419840213632,0.),.UNSPECIFIED.);
#5714=B_SPLINE_CURVE_WITH_KNOTS('',3,(#38489,#38490,#38491,#38492,#38493,
#38494,#38495,#38496,#38497,#38498,#38499,#38500,#38501,#38502,#38503,#38504,
#38505,#38506,#38507),.UNSPECIFIED.,.F.,.F.,(4,3,3,3,3,3,4),(2.01694489302852,
2.9772595206409,3.96967936085453,4.96209920106817,5.9545190412818,6.94693888149543,
7.59274844815647),.UNSPECIFIED.);
#5715=B_SPLINE_CURVE_WITH_KNOTS('',3,(#38513,#38514,#38515,#38516,#38517,
#38518,#38519,#38520),.UNSPECIFIED.,.F.,.F.,(4,1,1,1,1,4),(103.672557568463,
104.154034002176,105.146453842389,106.138873682603,107.131293522817,108.12371336303),
 .UNSPECIFIED.);
#5716=B_SPLINE_CURVE_WITH_KNOTS('',3,(#38523,#38524,#38525,#38526,#38527,
#38528,#38529,#38530,#38531),.UNSPECIFIED.,.F.,.F.,(4,1,1,1,1,1,4),(103.672557568463,
103.716185746199,104.708605586413,105.701025426626,106.69344526684,107.685865107053,
108.646179734666),.UNSPECIFIED.);
#5717=B_SPLINE_CURVE_WITH_KNOTS('',3,(#38536,#38537,#38538,#38539,#38540,
#38541,#38542,#38543,#38544,#38545),.UNSPECIFIED.,.F.,.F.,(4,1,1,1,1,1,
1,4),(97.3893722612835,98.1995149608939,99.1919348011075,100.184354641321,
101.176774481535,102.169194321748,103.161614161962,103.672557568463),
 .UNSPECIFIED.);
#5718=B_SPLINE_CURVE_WITH_KNOTS('',3,(#38546,#38547,#38548,#38549,#38550,
#38551,#38552,#38553,#38554,#38555),.UNSPECIFIED.,.F.,.F.,(4,1,1,1,1,1,
1,4),(97.3893722612835,97.7616667049171,98.7540865451307,99.7465063853444,
100.738926225558,101.731346065772,102.723765905985,103.672557568463),
 .UNSPECIFIED.);
#5719=B_SPLINE_CURVE_WITH_KNOTS('',3,(#38560,#38561,#38562,#38563,#38564,
#38565,#38566,#38567,#38568,#38569,#38570),.UNSPECIFIED.,.F.,.F.,(4,1,1,
1,1,1,1,1,4),(91.106186954104,91.2525760793984,92.2449959196121,93.2374157598257,
94.2298356000393,95.222255440253,96.2146752804666,97.2070951206802,97.3893722612835),
 .UNSPECIFIED.);
#5720=B_SPLINE_CURVE_WITH_KNOTS('',3,(#38571,#38572,#38573,#38574,#38575,
#38576,#38577,#38578,#38579,#38580),.UNSPECIFIED.,.F.,.F.,(4,1,1,1,1,1,
1,4),(91.106186954104,91.8071476636353,92.7995675038489,93.7919873440626,
94.7844071842762,95.7768270244898,96.7692468647035,97.3893722612835),
 .UNSPECIFIED.);
#5721=B_SPLINE_CURVE_WITH_KNOTS('',3,(#38585,#38586,#38587,#38588,#38589,
#38590,#38591,#38592,#38593,#38594),.UNSPECIFIED.,.F.,.F.,(4,1,1,1,1,1,
1,4),(84.8230016469244,85.2980570381166,86.2904768783303,87.2828967185439,
88.2753165587575,89.2677363989712,90.2601562391848,91.106186954104),
 .UNSPECIFIED.);
#5722=B_SPLINE_CURVE_WITH_KNOTS('',3,(#38595,#38596,#38597,#38598,#38599,
#38600,#38601,#38602,#38603,#38604,#38605),.UNSPECIFIED.,.F.,.F.,(4,1,1,
1,1,1,1,1,4),(84.8230016469244,84.8602087821399,85.8526286223535,86.8450484625671,
87.8374683027808,88.8298881429944,89.822307983208,90.8147278234217,91.106186954104),
 .UNSPECIFIED.);
#5723=B_SPLINE_CURVE_WITH_KNOTS('',3,(#38610,#38611,#38612,#38613,#38614,
#38615,#38616,#38617,#38618,#38619),.UNSPECIFIED.,.F.,.F.,(4,1,1,1,1,1,
1,4),(78.5398163397448,79.3435379968348,80.3359578370485,81.3283776772621,
82.3207975174757,83.3132173576894,84.305637197903,84.8230016469244),
 .UNSPECIFIED.);
#5724=B_SPLINE_CURVE_WITH_KNOTS('',3,(#38620,#38621,#38622,#38623,#38624,
#38625,#38626,#38627,#38628,#38629),.UNSPECIFIED.,.F.,.F.,(4,1,1,1,1,1,
1,4),(78.5398163397448,78.9056897408581,79.8981095810717,80.8905294212853,
81.882949261499,82.8753691017126,83.8677889419262,84.8230016469244),
 .UNSPECIFIED.);
#5725=B_SPLINE_CURVE_WITH_KNOTS('',3,(#38634,#38635,#38636,#38637,#38638,
#38639,#38640,#38641,#38642,#38643,#38644),.UNSPECIFIED.,.F.,.F.,(4,1,1,
1,1,1,1,1,4),(72.2566310325653,72.3965991153394,73.389018955553,74.3814387957667,
75.3738586359803,76.3662784761939,77.3586983164076,78.3511181566212,78.5398163397448),
 .UNSPECIFIED.);
#5726=B_SPLINE_CURVE_WITH_KNOTS('',3,(#38645,#38646,#38647,#38648,#38649,
#38650,#38651,#38652,#38653,#38654),.UNSPECIFIED.,.F.,.F.,(4,1,1,1,1,1,
1,4),(72.2566310325651,72.9511706995763,73.9435905397899,74.9360103800035,
75.9284302202172,76.9208500604308,77.9132699006444,78.5398163397448),
 .UNSPECIFIED.);
#5727=B_SPLINE_CURVE_WITH_KNOTS('',3,(#38659,#38660,#38661,#38662,#38663,
#38664,#38665,#38666,#38667,#38668),.UNSPECIFIED.,.F.,.F.,(4,1,1,1,1,1,
1,4),(65.9734457253856,66.4420800740576,67.4344999142712,68.4269197544849,
69.4193395946985,70.4117594349121,71.4041792751258,72.2566310325653),
 .UNSPECIFIED.);
#5728=B_SPLINE_CURVE_WITH_KNOTS('',3,(#38669,#38670,#38671,#38672,#38673,
#38674,#38675,#38676,#38677,#38678,#38679),.UNSPECIFIED.,.F.,.F.,(4,1,1,
1,1,1,1,1,4),(65.9734457253856,66.0042318180808,66.9966516582945,67.9890714985081,
68.9814913387217,69.9739111789354,70.966331019149,71.9587508593626,72.2566310325651),
 .UNSPECIFIED.);
#5729=B_SPLINE_CURVE_WITH_KNOTS('',3,(#38684,#38685,#38686,#38687,#38688,
#38689,#38690,#38691,#38692,#38693),.UNSPECIFIED.,.F.,.F.,(4,1,1,1,1,1,
1,4),(59.690260418206,60.4875610327758,61.4799808729895,62.4724007132031,
63.4648205534167,64.4572403936303,65.449660233844,65.9734457253856),
 .UNSPECIFIED.);
#5730=B_SPLINE_CURVE_WITH_KNOTS('',3,(#38694,#38695,#38696,#38697,#38698,
#38699,#38700,#38701,#38702,#38703),.UNSPECIFIED.,.F.,.F.,(4,1,1,1,1,1,
1,4),(59.690260418206,60.049712776799,61.0421326170127,62.0345524572263,
63.0269722974399,64.0193921376536,65.0118119778672,65.9734457253856),
 .UNSPECIFIED.);
#5731=B_SPLINE_CURVE_WITH_KNOTS('',3,(#38708,#38709,#38710,#38711,#38712,
#38713,#38714,#38715,#38716,#38717,#38718),.UNSPECIFIED.,.F.,.F.,(4,1,1,
1,1,1,1,1,4),(53.4070751110265,53.5406221512804,54.533041991494,55.5254618317077,
56.5178816719213,57.5103015121349,58.5027213523486,59.4951411925622,59.690260418206),
 .UNSPECIFIED.);
#5732=B_SPLINE_CURVE_WITH_KNOTS('',3,(#38719,#38720,#38721,#38722,#38723,
#38724,#38725,#38726,#38727,#38728),.UNSPECIFIED.,.F.,.F.,(4,1,1,1,1,1,
1,4),(53.4070751110265,54.0951937355172,55.0876135757309,56.0800334159445,
57.0724532561581,58.0648730963718,59.0572929365854,59.690260418206),
 .UNSPECIFIED.);
#5733=B_SPLINE_CURVE_WITH_KNOTS('',3,(#38733,#38734,#38735,#38736,#38737,
#38738,#38739,#38740,#38741,#38742),.UNSPECIFIED.,.F.,.F.,(4,1,1,1,1,1,
1,4),(47.1238898038468,47.5861031099986,48.5785229502122,49.5709427904259,
50.5633626306395,51.5557824708531,52.5482023110668,53.4070751110265),
 .UNSPECIFIED.);
#5734=B_SPLINE_CURVE_WITH_KNOTS('',3,(#38743,#38744,#38745,#38746,#38747,
#38748,#38749,#38750,#38751,#38752,#38753),.UNSPECIFIED.,.F.,.F.,(4,1,1,
1,1,1,1,1,4),(47.1238898038468,47.1482548540218,48.1406746942354,49.1330945344491,
50.1255143746627,51.1179342148763,52.11035405509,53.1027738953036,53.4070751110265),
 .UNSPECIFIED.);
#5735=B_SPLINE_CURVE_WITH_KNOTS('',3,(#38758,#38759,#38760,#38761,#38762,
#38763,#38764,#38765,#38766,#38767),.UNSPECIFIED.,.F.,.F.,(4,1,1,1,1,1,
1,4),(40.8407044966672,41.6315840687168,42.6240039089304,43.6164237491441,
44.6088435893577,45.6012634295713,46.593683269785,47.1238898038468),
 .UNSPECIFIED.);
#5736=B_SPLINE_CURVE_WITH_KNOTS('',3,(#38768,#38769,#38770,#38771,#38772,
#38773,#38774,#38775,#38776,#38777),.UNSPECIFIED.,.F.,.F.,(4,1,1,1,1,1,
1,4),(40.8407044966672,41.19373581274,42.1861556529536,43.1785754931673,
44.1709953333809,45.1634151735945,46.1558350138082,47.1238898038468),
 .UNSPECIFIED.);
#5737=B_SPLINE_CURVE_WITH_KNOTS('',3,(#38782,#38783,#38784,#38785,#38786,
#38787,#38788,#38789,#38790,#38791,#38792),.UNSPECIFIED.,.F.,.F.,(4,1,1,
1,1,1,1,1,4),(34.5575191894877,34.6846451872214,35.677065027435,36.6694848676486,
37.6619047078623,38.6543245480759,39.6467443882895,40.6391642285032,40.8407044966672),
 .UNSPECIFIED.);
#5738=B_SPLINE_CURVE_WITH_KNOTS('',3,(#38793,#38794,#38795,#38796,#38797,
#38798,#38799,#38800,#38801,#38802),.UNSPECIFIED.,.F.,.F.,(4,1,1,1,1,1,
1,4),(34.5575191894877,35.2392167714582,36.2316366116718,37.2240564518855,
38.2164762920991,39.2088961323127,40.2013159725264,40.8407044966672),
 .UNSPECIFIED.);
#5739=B_SPLINE_CURVE_WITH_KNOTS('',3,(#38807,#38808,#38809,#38810,#38811,
#38812,#38813,#38814,#38815,#38816),.UNSPECIFIED.,.F.,.F.,(4,1,1,1,1,1,
1,4),(28.2743338823081,28.7301261459396,29.7225459861532,30.7149658263668,
31.7073856665805,32.6998055067941,33.6922253470077,34.5575191894877),
 .UNSPECIFIED.);
#5740=B_SPLINE_CURVE_WITH_KNOTS('',3,(#38817,#38818,#38819,#38820,#38821,
#38822,#38823,#38824,#38825,#38826,#38827),.UNSPECIFIED.,.F.,.F.,(4,1,1,
1,1,1,1,1,4),(28.2743338823081,28.2922778899628,29.2846977301764,30.2771175703901,
31.2695374106037,32.2619572508173,33.2543770910309,34.2467969312446,34.5575191894877),
 .UNSPECIFIED.);
#5741=B_SPLINE_CURVE_WITH_KNOTS('',3,(#38832,#38833,#38834,#38835,#38836,
#38837,#38838,#38839,#38840,#38841),.UNSPECIFIED.,.F.,.F.,(4,1,1,1,1,1,
1,4),(21.9911485751285,22.7756071046578,23.7680269448714,24.760446785085,
25.7528666252987,26.7452864655123,27.7377063057259,28.2743338823081),
 .UNSPECIFIED.);
#5742=B_SPLINE_CURVE_WITH_KNOTS('',3,(#38842,#38843,#38844,#38845,#38846,
#38847,#38848,#38849,#38850,#38851),.UNSPECIFIED.,.F.,.F.,(4,1,1,1,1,1,
1,4),(21.9911485751284,22.337758848681,23.3301786888946,24.3225985291083,
25.3150183693219,26.3074382095355,27.2998580497492,28.2743338823081),
 .UNSPECIFIED.);
#5743=B_SPLINE_CURVE_WITH_KNOTS('',3,(#38857,#38858,#38859,#38860,#38861),
 .UNSPECIFIED.,.F.,.F.,(4,1,4),(14.3984001269719,15.3908199671856,15.7079632679489),
 .UNSPECIFIED.);
#5744=B_SPLINE_CURVE_WITH_KNOTS('',3,(#38864,#38865,#38866,#38867,#38868),
 .UNSPECIFIED.,.F.,.F.,(4,1,4),(13.8759337553364,14.8362483829487,15.7079632679489),
 .UNSPECIFIED.);
#5745=B_SPLINE_CURVE_WITH_KNOTS('',3,(#38874,#38875,#38876,#38877),
 .UNSPECIFIED.,.F.,.F.,(4,4),(95.5573427486708,96.2647245007226),
 .UNSPECIFIED.);
#5746=B_SPLINE_CURVE_WITH_KNOTS('',3,(#38885,#38886,#38887,#38888,#38889,
#38890,#38891,#38892,#38893,#38894),.UNSPECIFIED.,.F.,.F.,(4,3,3,4),(-94.2477796076939,
-93.2874649800816,-92.295045139868,-91.8135687061555),.UNSPECIFIED.);
#5747=B_SPLINE_CURVE_WITH_KNOTS('',3,(#38899,#38900,#38901,#38902,#38903,
#38904,#38905,#38906,#38907,#38908,#38909,#38910,#38911,#38912,#38913,#38914,
#38915,#38916,#38917,#38918,#38919,#38920,#38921,#38922,#38923),
 .UNSPECIFIED.,.F.,.F.,(4,3,3,3,3,3,3,3,4),(89.2741574414912,89.3177856192271,
90.3102054594407,91.3026252996543,92.295045139868,93.2874649800816,94.2798848202952,
95.2723046605089,95.5573427486708),.UNSPECIFIED.);
#5748=B_SPLINE_CURVE_WITH_KNOTS('',3,(#38924,#38925,#38926,#38927,#38928,
#38929,#38930,#38931,#38932,#38933,#38934,#38935,#38936,#38937,#38938,#38939,
#38940,#38941,#38942,#38943,#38944,#38945),.UNSPECIFIED.,.F.,.F.,(4,3,3,
3,3,3,3,4),(-91.8135687061555,-91.3026252996543,-90.3102054594407,-89.3177856192271,
-88.3253657790134,-87.3329459387998,-86.3405260985862,-85.5303833989759),
 .UNSPECIFIED.);
#5749=B_SPLINE_CURVE_WITH_KNOTS('',3,(#38950,#38951,#38952,#38953,#38954,
#38955,#38956,#38957,#38958,#38959,#38960,#38961,#38962,#38963,#38964,#38965,
#38966,#38967,#38968,#38969,#38970,#38971),.UNSPECIFIED.,.F.,.F.,(4,3,3,
3,3,3,3,4),(82.9909721343117,83.3632665779453,84.3556864181589,85.3481062583725,
86.3405260985862,87.3329459387998,88.3253657790134,89.2741574414912),
 .UNSPECIFIED.);
#5750=B_SPLINE_CURVE_WITH_KNOTS('',3,(#38972,#38973,#38974,#38975,#38976,
#38977,#38978,#38979,#38980,#38981,#38982,#38983,#38984,#38985,#38986,#38987,
#38988,#38989,#38990,#38991,#38992,#38993,#38994,#38995,#38996),
 .UNSPECIFIED.,.F.,.F.,(4,3,3,3,3,3,3,3,4),(-85.5303833989759,-85.3481062583725,
-84.3556864181589,-83.3632665779453,-82.3708467377316,-81.378426897518,
-80.3860070573044,-79.3935872170907,-79.2471980917962),.UNSPECIFIED.);
#5751=B_SPLINE_CURVE_WITH_KNOTS('',3,(#39001,#39002,#39003,#39004,#39005,
#39006,#39007,#39008,#39009,#39010,#39011,#39012,#39013,#39014,#39015,#39016,
#39017,#39018,#39019,#39020,#39021,#39022),.UNSPECIFIED.,.F.,.F.,(4,3,3,
3,3,3,3,4),(76.707786827132,77.4087475366635,78.4011673768771,79.3935872170907,
80.3860070573044,81.378426897518,82.3708467377316,82.9909721343117),
 .UNSPECIFIED.);
#5752=B_SPLINE_CURVE_WITH_KNOTS('',3,(#39023,#39024,#39025,#39026,#39027,
#39028,#39029,#39030,#39031,#39032,#39033,#39034,#39035,#39036,#39037,#39038,
#39039,#39040,#39041,#39042,#39043,#39044),.UNSPECIFIED.,.F.,.F.,(4,3,3,
3,3,3,3,4),(-79.2471980917962,-78.4011673768771,-77.4087475366635,-76.4163276964498,
-75.4239078562362,-74.4314880160225,-73.4390681758089,-72.9640127846167),
 .UNSPECIFIED.);
#5753=B_SPLINE_CURVE_WITH_KNOTS('',3,(#39049,#39050,#39051,#39052,#39053,
#39054,#39055,#39056,#39057,#39058,#39059,#39060,#39061,#39062,#39063,#39064,
#39065,#39066,#39067,#39068,#39069,#39070,#39071,#39072,#39073),
 .UNSPECIFIED.,.F.,.F.,(4,3,3,3,3,3,3,3,4),(70.4246015199524,70.461808655168,
71.4542284953816,72.4466483355953,73.4390681758089,74.4314880160225,75.4239078562362,
76.4163276964498,76.707786827132),.UNSPECIFIED.);
#5754=B_SPLINE_CURVE_WITH_KNOTS('',3,(#39074,#39075,#39076,#39077,#39078,
#39079,#39080,#39081,#39082,#39083,#39084,#39085,#39086,#39087,#39088,#39089,
#39090,#39091,#39092,#39093,#39094,#39095),.UNSPECIFIED.,.F.,.F.,(4,3,3,
3,3,3,3,4),(-72.9640127846167,-72.4466483355953,-71.4542284953816,-70.461808655168,
-69.4693888149544,-68.4769689747407,-67.4845491345271,-66.6808274774371),
 .UNSPECIFIED.);
#5755=B_SPLINE_CURVE_WITH_KNOTS('',3,(#39100,#39101,#39102,#39103,#39104,
#39105,#39106,#39107,#39108,#39109,#39110,#39111,#39112,#39113,#39114,#39115,
#39116,#39117,#39118,#39119,#39120,#39121),.UNSPECIFIED.,.F.,.F.,(4,3,3,
3,3,3,3,4),(64.1414162127729,64.5072896138862,65.4997094540998,66.4921292943135,
67.4845491345271,68.4769689747407,69.4693888149544,70.4246015199524),
 .UNSPECIFIED.);
#5756=B_SPLINE_CURVE_WITH_KNOTS('',3,(#39122,#39123,#39124,#39125,#39126,
#39127,#39128,#39129,#39130,#39131,#39132,#39133,#39134,#39135,#39136,#39137,
#39138,#39139,#39140,#39141,#39142,#39143,#39144,#39145,#39146),
 .UNSPECIFIED.,.F.,.F.,(4,3,3,3,3,3,3,3,4),(-66.6808274774371,-66.4921292943135,
-65.4997094540998,-64.5072896138862,-63.5148697736726,-62.5224499334589,
-61.5300300932453,-60.5376102530317,-60.3976421702575),.UNSPECIFIED.);
#5757=B_SPLINE_CURVE_WITH_KNOTS('',3,(#39151,#39152,#39153,#39154,#39155,
#39156,#39157,#39158,#39159,#39160,#39161,#39162,#39163,#39164,#39165,#39166,
#39167,#39168,#39169,#39170,#39171,#39172),.UNSPECIFIED.,.F.,.F.,(4,3,3,
3,3,3,3,4),(57.8582309055933,58.5527705726044,59.545190412818,60.5376102530317,
61.5300300932453,62.5224499334589,63.5148697736726,64.1414162127729),
 .UNSPECIFIED.);
#5758=B_SPLINE_CURVE_WITH_KNOTS('',3,(#39173,#39174,#39175,#39176,#39177,
#39178,#39179,#39180,#39181,#39182,#39183,#39184,#39185,#39186,#39187,#39188,
#39189,#39190,#39191,#39192,#39193,#39194),.UNSPECIFIED.,.F.,.F.,(4,3,3,
3,3,3,3,4),(-60.3976421702575,-59.545190412818,-58.5527705726044,-57.5603507323908,
-56.5679308921771,-55.5755110519635,-54.5830912117499,-54.1144568630778),
 .UNSPECIFIED.);
#5759=B_SPLINE_CURVE_WITH_KNOTS('',3,(#39199,#39200,#39201,#39202,#39203,
#39204,#39205,#39206,#39207,#39208,#39209,#39210,#39211,#39212,#39213,#39214,
#39215,#39216,#39217,#39218,#39219,#39220,#39221,#39222,#39223),
 .UNSPECIFIED.,.F.,.F.,(4,3,3,3,3,3,3,3,4),(51.5750455984136,51.605831691109,
52.5982515313226,53.5906713715362,54.5830912117499,55.5755110519635,56.5679308921771,
57.5603507323908,57.8582309055933),.UNSPECIFIED.);
#5760=B_SPLINE_CURVE_WITH_KNOTS('',3,(#39224,#39225,#39226,#39227,#39228,
#39229,#39230,#39231,#39232,#39233,#39234,#39235,#39236,#39237,#39238,#39239,
#39240,#39241,#39242,#39243,#39244,#39245),.UNSPECIFIED.,.F.,.F.,(4,3,3,
3,3,3,3,4),(-54.1144568630778,-53.5906713715362,-52.5982515313226,-51.605831691109,
-50.6134118508953,-49.6209920106817,-48.6285721704681,-47.8312715558983),
 .UNSPECIFIED.);
#5761=B_SPLINE_CURVE_WITH_KNOTS('',3,(#39250,#39251,#39252,#39253,#39254,
#39255,#39256,#39257,#39258,#39259,#39260,#39261,#39262,#39263,#39264,#39265,
#39266,#39267,#39268,#39269,#39270,#39271),.UNSPECIFIED.,.F.,.F.,(4,3,3,
3,3,3,3,4),(45.2918602912341,45.6513126498272,46.6437324900408,47.6361523302544,
48.6285721704681,49.6209920106817,50.6134118508953,51.5750455984136),
 .UNSPECIFIED.);
#5762=B_SPLINE_CURVE_WITH_KNOTS('',3,(#39272,#39273,#39274,#39275,#39276,
#39277,#39278,#39279,#39280,#39281,#39282,#39283,#39284,#39285,#39286,#39287,
#39288,#39289,#39290,#39291,#39292,#39293,#39294,#39295,#39296),
 .UNSPECIFIED.,.F.,.F.,(4,3,3,3,3,3,3,3,4),(-47.8312715558983,-47.6361523302544,
-46.6437324900408,-45.6513126498271,-44.6588928096135,-43.6664729693999,
-42.6740531291862,-41.6816332889726,-41.5480862487187),.UNSPECIFIED.);
#5763=B_SPLINE_CURVE_WITH_KNOTS('',3,(#39301,#39302,#39303,#39304,#39305,
#39306,#39307,#39308,#39309,#39310,#39311,#39312,#39313,#39314,#39315,#39316,
#39317,#39318,#39319,#39320,#39321,#39322),.UNSPECIFIED.,.F.,.F.,(4,3,3,
3,3,3,3,4),(39.0086749840545,39.6967936085454,40.689213448759,41.6816332889726,
42.6740531291863,43.6664729693999,44.6588928096135,45.2918602912341),
 .UNSPECIFIED.);
#5764=B_SPLINE_CURVE_WITH_KNOTS('',3,(#39323,#39324,#39325,#39326,#39327,
#39328,#39329,#39330,#39331,#39332,#39333,#39334,#39335,#39336,#39337,#39338,
#39339,#39340,#39341,#39342,#39343,#39344),.UNSPECIFIED.,.F.,.F.,(4,3,3,
3,3,3,3,4),(-41.5480862487187,-40.689213448759,-39.6967936085453,-38.7043737683317,
-37.7119539281181,-36.7195340879044,-35.7271142476908,-35.2649009415392),
 .UNSPECIFIED.);
#5765=B_SPLINE_CURVE_WITH_KNOTS('',3,(#39349,#39350,#39351,#39352,#39353,
#39354,#39355,#39356,#39357,#39358,#39359,#39360,#39361,#39362,#39363,#39364,
#39365,#39366,#39367,#39368,#39369,#39370,#39371,#39372,#39373),
 .UNSPECIFIED.,.F.,.F.,(4,3,3,3,3,3,3,3,4),(32.725489676875,32.7498547270499,
33.7422745672636,34.7346944074772,35.7271142476908,36.7195340879045,37.7119539281181,
38.7043737683317,39.0086749840545),.UNSPECIFIED.);
#5766=B_SPLINE_CURVE_WITH_KNOTS('',3,(#39374,#39375,#39376,#39377,#39378,
#39379,#39380,#39381,#39382,#39383,#39384,#39385,#39386,#39387,#39388,#39389,
#39390,#39391,#39392,#39393,#39394,#39395),.UNSPECIFIED.,.F.,.F.,(4,3,3,
3,3,3,3,4),(-35.2649009415392,-34.7346944074772,-33.7422745672636,-32.7498547270499,
-31.7574348868363,-30.7650150466226,-29.772595206409,-28.9817156343595),
 .UNSPECIFIED.);
#5767=B_SPLINE_CURVE_WITH_KNOTS('',3,(#39400,#39401,#39402,#39403,#39404,
#39405,#39406,#39407,#39408,#39409,#39410,#39411,#39412,#39413,#39414,#39415,
#39416,#39417,#39418,#39419,#39420,#39421),.UNSPECIFIED.,.F.,.F.,(4,3,3,
3,3,3,3,4),(26.4423043696953,26.7953356857681,27.7877555259818,28.7801753661954,
29.772595206409,30.7650150466227,31.7574348868363,32.725489676875),
 .UNSPECIFIED.);
#5768=B_SPLINE_CURVE_WITH_KNOTS('',3,(#39422,#39423,#39424,#39425,#39426,
#39427,#39428,#39429,#39430,#39431,#39432,#39433,#39434,#39435,#39436,#39437,
#39438,#39439,#39440,#39441,#39442,#39443,#39444,#39445,#39446),
 .UNSPECIFIED.,.F.,.F.,(4,3,3,3,3,3,3,3,4),(-28.9817156343595,-28.7801753661954,
-27.7877555259817,-26.7953356857681,-25.8029158455545,-24.8104960053408,
-23.8180761651272,-22.8256563249136,-22.6985303271799),.UNSPECIFIED.);
#5769=B_SPLINE_CURVE_WITH_KNOTS('',3,(#39451,#39452,#39453,#39454,#39455,
#39456,#39457,#39458,#39459,#39460,#39461,#39462,#39463,#39464,#39465,#39466,
#39467,#39468,#39469,#39470,#39471,#39472),.UNSPECIFIED.,.F.,.F.,(4,3,3,
3,3,3,3,4),(20.1591190625157,20.8408166444863,21.8332364847,22.8256563249136,
23.8180761651272,24.8104960053409,25.8029158455545,26.4423043696953),
 .UNSPECIFIED.);
#5770=B_SPLINE_CURVE_WITH_KNOTS('',3,(#39473,#39474,#39475,#39476,#39477,
#39478,#39479,#39480,#39481,#39482,#39483,#39484,#39485,#39486,#39487,#39488,
#39489,#39490,#39491,#39492,#39493,#39494),.UNSPECIFIED.,.F.,.F.,(4,3,3,
3,3,3,3,4),(-22.6985303271799,-21.8332364846999,-20.8408166444863,-19.8483968042727,
-18.855976964059,-17.8635571238454,-16.8711372836318,-16.4153450200004),
 .UNSPECIFIED.);
#5771=B_SPLINE_CURVE_WITH_KNOTS('',3,(#39499,#39500,#39501,#39502,#39503,
#39504,#39505,#39506,#39507,#39508,#39509,#39510,#39511,#39512,#39513,#39514,
#39515,#39516,#39517,#39518,#39519,#39520,#39521,#39522,#39523),
 .UNSPECIFIED.,.F.,.F.,(4,3,3,3,3,3,3,3,4),(13.8759337553361,13.8938777629909,
14.8862976032045,15.8787174434181,16.8711372836318,17.8635571238454,18.8559769640591,
19.8483968042727,20.1591190625157),.UNSPECIFIED.);
#5772=B_SPLINE_CURVE_WITH_KNOTS('',3,(#39524,#39525,#39526,#39527,#39528,
#39529,#39530,#39531,#39532,#39533,#39534,#39535,#39536,#39537,#39538,#39539,
#39540,#39541,#39542,#39543,#39544,#39545),.UNSPECIFIED.,.F.,.F.,(4,3,3,
3,3,3,3,4),(-16.4153450200004,-15.8787174434181,-14.8862976032045,-13.8938777629909,
-12.9014579227772,-11.9090380825636,-10.91661824235,-10.1321597128208),
 .UNSPECIFIED.);
#5773=B_SPLINE_CURVE_WITH_KNOTS('',3,(#39551,#39552,#39553,#39554,#39555,
#39556,#39557,#39558,#39559,#39560,#39561,#39562,#39563),.UNSPECIFIED.,
 .F.,.F.,(4,3,3,3,4),(-3.84897440564123,-2.9772595206409,-1.98483968042727,
-0.992419840213635,0.),.UNSPECIFIED.);
#5774=B_SPLINE_CURVE_WITH_KNOTS('',3,(#39566,#39567,#39568,#39569,#39570,
#39571,#39572,#39573,#39574,#39575,#39576,#39577,#39578,#39579,#39580,#39581,
#39582,#39583,#39584),.UNSPECIFIED.,.F.,.F.,(4,3,3,3,3,3,4),(2.01694489302852,
2.9772595206409,3.96967936085453,4.96209920106817,5.9545190412818,6.94693888149544,
7.59274844815659),.UNSPECIFIED.);
#5775=B_SPLINE_CURVE_WITH_KNOTS('',3,(#39590,#39591,#39592,#39593,#39594,
#39595,#39596,#39597),.UNSPECIFIED.,.F.,.F.,(4,1,1,1,1,4),(103.672557568463,
104.154034002176,105.146453842389,106.138873682603,107.131293522817,108.12371336303),
 .UNSPECIFIED.);
#5776=B_SPLINE_CURVE_WITH_KNOTS('',3,(#39600,#39601,#39602,#39603,#39604,
#39605,#39606,#39607,#39608),.UNSPECIFIED.,.F.,.F.,(4,1,1,1,1,1,4),(103.672557568463,
103.716185746199,104.708605586413,105.701025426626,106.69344526684,107.685865107053,
108.646179734666),.UNSPECIFIED.);
#5777=B_SPLINE_CURVE_WITH_KNOTS('',3,(#39613,#39614,#39615,#39616,#39617,
#39618,#39619,#39620,#39621,#39622),.UNSPECIFIED.,.F.,.F.,(4,1,1,1,1,1,
1,4),(97.3893722612835,98.1995149608939,99.1919348011075,100.184354641321,
101.176774481535,102.169194321748,103.161614161962,103.672557568463),
 .UNSPECIFIED.);
#5778=B_SPLINE_CURVE_WITH_KNOTS('',3,(#39623,#39624,#39625,#39626,#39627,
#39628,#39629,#39630,#39631,#39632),.UNSPECIFIED.,.F.,.F.,(4,1,1,1,1,1,
1,4),(97.3893722612835,97.7616667049171,98.7540865451307,99.7465063853443,
100.738926225558,101.731346065772,102.723765905985,103.672557568463),
 .UNSPECIFIED.);
#5779=B_SPLINE_CURVE_WITH_KNOTS('',3,(#39637,#39638,#39639,#39640,#39641,
#39642,#39643,#39644,#39645,#39646,#39647),.UNSPECIFIED.,.F.,.F.,(4,1,1,
1,1,1,1,1,4),(91.106186954104,91.2525760793984,92.2449959196121,93.2374157598257,
94.2298356000393,95.222255440253,96.2146752804666,97.2070951206802,97.3893722612835),
 .UNSPECIFIED.);
#5780=B_SPLINE_CURVE_WITH_KNOTS('',3,(#39648,#39649,#39650,#39651,#39652,
#39653,#39654,#39655,#39656,#39657),.UNSPECIFIED.,.F.,.F.,(4,1,1,1,1,1,
1,4),(91.106186954104,91.8071476636353,92.7995675038489,93.7919873440625,
94.7844071842762,95.7768270244898,96.7692468647034,97.3893722612835),
 .UNSPECIFIED.);
#5781=B_SPLINE_CURVE_WITH_KNOTS('',3,(#39662,#39663,#39664,#39665,#39666,
#39667,#39668,#39669,#39670,#39671),.UNSPECIFIED.,.F.,.F.,(4,1,1,1,1,1,
1,4),(84.8230016469244,85.2980570381166,86.2904768783303,87.2828967185439,
88.2753165587575,89.2677363989712,90.2601562391848,91.106186954104),
 .UNSPECIFIED.);
#5782=B_SPLINE_CURVE_WITH_KNOTS('',3,(#39672,#39673,#39674,#39675,#39676,
#39677,#39678,#39679,#39680,#39681,#39682),.UNSPECIFIED.,.F.,.F.,(4,1,1,
1,1,1,1,1,4),(84.8230016469244,84.8602087821398,85.8526286223535,86.8450484625671,
87.8374683027807,88.8298881429944,89.822307983208,90.8147278234216,91.106186954104),
 .UNSPECIFIED.);
#5783=B_SPLINE_CURVE_WITH_KNOTS('',3,(#39687,#39688,#39689,#39690,#39691,
#39692,#39693,#39694,#39695,#39696),.UNSPECIFIED.,.F.,.F.,(4,1,1,1,1,1,
1,4),(78.5398163397448,79.3435379968348,80.3359578370484,81.3283776772621,
82.3207975174757,83.3132173576894,84.305637197903,84.8230016469244),
 .UNSPECIFIED.);
#5784=B_SPLINE_CURVE_WITH_KNOTS('',3,(#39697,#39698,#39699,#39700,#39701,
#39702,#39703,#39704,#39705,#39706),.UNSPECIFIED.,.F.,.F.,(4,1,1,1,1,1,
1,4),(78.5398163397448,78.905689740858,79.8981095810717,80.8905294212853,
81.8829492614989,82.8753691017126,83.8677889419262,84.8230016469244),
 .UNSPECIFIED.);
#5785=B_SPLINE_CURVE_WITH_KNOTS('',3,(#39711,#39712,#39713,#39714,#39715,
#39716,#39717,#39718,#39719,#39720,#39721),.UNSPECIFIED.,.F.,.F.,(4,1,1,
1,1,1,1,1,4),(72.2566310325651,72.3965991153394,73.389018955553,74.3814387957666,
75.3738586359803,76.3662784761939,77.3586983164075,78.3511181566212,78.5398163397448),
 .UNSPECIFIED.);
#5786=B_SPLINE_CURVE_WITH_KNOTS('',3,(#39722,#39723,#39724,#39725,#39726,
#39727,#39728,#39729,#39730,#39731),.UNSPECIFIED.,.F.,.F.,(4,1,1,1,1,1,
1,4),(72.2566310325651,72.9511706995762,73.9435905397899,74.9360103800035,
75.9284302202171,76.9208500604308,77.9132699006444,78.5398163397448),
 .UNSPECIFIED.);
#5787=B_SPLINE_CURVE_WITH_KNOTS('',3,(#39736,#39737,#39738,#39739,#39740,
#39741,#39742,#39743,#39744,#39745),.UNSPECIFIED.,.F.,.F.,(4,1,1,1,1,1,
1,4),(65.9734457253856,66.4420800740576,67.4344999142712,68.4269197544848,
69.4193395946985,70.4117594349121,71.4041792751257,72.2566310325651),
 .UNSPECIFIED.);
#5788=B_SPLINE_CURVE_WITH_KNOTS('',3,(#39746,#39747,#39748,#39749,#39750,
#39751,#39752,#39753,#39754,#39755,#39756),.UNSPECIFIED.,.F.,.F.,(4,1,1,
1,1,1,1,1,4),(65.9734457253856,66.0042318180808,66.9966516582944,67.9890714985081,
68.9814913387217,69.9739111789353,70.966331019149,71.9587508593626,72.2566310325651),
 .UNSPECIFIED.);
#5789=B_SPLINE_CURVE_WITH_KNOTS('',3,(#39761,#39762,#39763,#39764,#39765,
#39766,#39767,#39768,#39769,#39770),.UNSPECIFIED.,.F.,.F.,(4,1,1,1,1,1,
1,4),(59.690260418206,60.4875610327758,61.4799808729894,62.472400713203,
63.4648205534167,64.4572403936303,65.4496602338439,65.9734457253856),
 .UNSPECIFIED.);
#5790=B_SPLINE_CURVE_WITH_KNOTS('',3,(#39771,#39772,#39773,#39774,#39775,
#39776,#39777,#39778,#39779,#39780),.UNSPECIFIED.,.F.,.F.,(4,1,1,1,1,1,
1,4),(59.690260418206,60.049712776799,61.0421326170126,62.0345524572262,
63.0269722974399,64.0193921376535,65.0118119778672,65.9734457253856),
 .UNSPECIFIED.);
#5791=B_SPLINE_CURVE_WITH_KNOTS('',3,(#39785,#39786,#39787,#39788,#39789,
#39790,#39791,#39792,#39793,#39794,#39795),.UNSPECIFIED.,.F.,.F.,(4,1,1,
1,1,1,1,1,4),(53.4070751110265,53.5406221512803,54.533041991494,55.5254618317076,
56.5178816719212,57.5103015121349,58.5027213523485,59.4951411925621,59.690260418206),
 .UNSPECIFIED.);
#5792=B_SPLINE_CURVE_WITH_KNOTS('',3,(#39796,#39797,#39798,#39799,#39800,
#39801,#39802,#39803,#39804,#39805),.UNSPECIFIED.,.F.,.F.,(4,1,1,1,1,1,
1,4),(53.4070751110265,54.0951937355172,55.0876135757308,56.0800334159444,
57.0724532561581,58.0648730963717,59.0572929365853,59.690260418206),
 .UNSPECIFIED.);
#5793=B_SPLINE_CURVE_WITH_KNOTS('',3,(#39810,#39811,#39812,#39813,#39814,
#39815,#39816,#39817,#39818,#39819),.UNSPECIFIED.,.F.,.F.,(4,1,1,1,1,1,
1,4),(47.1238898038468,47.5861031099985,48.5785229502122,49.5709427904258,
50.5633626306394,51.5557824708531,52.5482023110667,53.4070751110265),
 .UNSPECIFIED.);
#5794=B_SPLINE_CURVE_WITH_KNOTS('',3,(#39820,#39821,#39822,#39823,#39824,
#39825,#39826,#39827,#39828,#39829,#39830),.UNSPECIFIED.,.F.,.F.,(4,1,1,
1,1,1,1,1,4),(47.1238898038468,47.1482548540217,48.1406746942354,49.133094534449,
50.1255143746626,51.1179342148763,52.1103540550899,53.1027738953035,53.4070751110265),
 .UNSPECIFIED.);
#5795=B_SPLINE_CURVE_WITH_KNOTS('',3,(#39835,#39836,#39837,#39838,#39839,
#39840,#39841,#39842,#39843,#39844),.UNSPECIFIED.,.F.,.F.,(4,1,1,1,1,1,
1,4),(40.8407044966672,41.6315840687167,42.6240039089304,43.616423749144,
44.6088435893576,45.6012634295713,46.5936832697849,47.1238898038468),
 .UNSPECIFIED.);
#5796=B_SPLINE_CURVE_WITH_KNOTS('',3,(#39845,#39846,#39847,#39848,#39849,
#39850,#39851,#39852,#39853,#39854),.UNSPECIFIED.,.F.,.F.,(4,1,1,1,1,1,
1,4),(40.8407044966672,41.1937358127399,42.1861556529536,43.1785754931672,
44.1709953333808,45.1634151735945,46.1558350138081,47.1238898038468),
 .UNSPECIFIED.);
#5797=B_SPLINE_CURVE_WITH_KNOTS('',3,(#39859,#39860,#39861,#39862,#39863,
#39864,#39865,#39866,#39867,#39868,#39869),.UNSPECIFIED.,.F.,.F.,(4,1,1,
1,1,1,1,1,4),(34.5575191894877,34.6846451872213,35.6770650274349,36.6694848676485,
37.6619047078622,38.6543245480758,39.6467443882895,40.6391642285031,40.8407044966672),
 .UNSPECIFIED.);
#5798=B_SPLINE_CURVE_WITH_KNOTS('',3,(#39870,#39871,#39872,#39873,#39874,
#39875,#39876,#39877,#39878,#39879),.UNSPECIFIED.,.F.,.F.,(4,1,1,1,1,1,
1,4),(34.5575191894877,35.2392167714581,36.2316366116718,37.2240564518854,
38.216476292099,39.2088961323127,40.2013159725263,40.8407044966672),
 .UNSPECIFIED.);
#5799=B_SPLINE_CURVE_WITH_KNOTS('',3,(#39884,#39885,#39886,#39887,#39888,
#39889,#39890,#39891,#39892,#39893),.UNSPECIFIED.,.F.,.F.,(4,1,1,1,1,1,
1,4),(28.2743338823081,28.7301261459395,29.7225459861531,30.7149658263668,
31.7073856665804,32.699805506794,33.6922253470076,34.5575191894877),
 .UNSPECIFIED.);
#5800=B_SPLINE_CURVE_WITH_KNOTS('',3,(#39894,#39895,#39896,#39897,#39898,
#39899,#39900,#39901,#39902,#39903,#39904),.UNSPECIFIED.,.F.,.F.,(4,1,1,
1,1,1,1,1,4),(28.2743338823081,28.2922778899627,29.2846977301763,30.27711757039,
31.2695374106036,32.2619572508172,33.2543770910309,34.2467969312445,34.5575191894877),
 .UNSPECIFIED.);
#5801=B_SPLINE_CURVE_WITH_KNOTS('',3,(#39909,#39910,#39911,#39912,#39913,
#39914,#39915,#39916,#39917,#39918),.UNSPECIFIED.,.F.,.F.,(4,1,1,1,1,1,
1,4),(21.9911485751284,22.7756071046577,23.7680269448713,24.7604467850849,
25.7528666252986,26.7452864655122,27.7377063057259,28.2743338823081),
 .UNSPECIFIED.);
#5802=B_SPLINE_CURVE_WITH_KNOTS('',3,(#39919,#39920,#39921,#39922,#39923,
#39924,#39925,#39926,#39927,#39928),.UNSPECIFIED.,.F.,.F.,(4,1,1,1,1,1,
1,4),(21.9911485751284,22.3377588486809,23.3301786888945,24.3225985291082,
25.3150183693218,26.3074382095354,27.2998580497491,28.2743338823081),
 .UNSPECIFIED.);
#5803=B_SPLINE_CURVE_WITH_KNOTS('',3,(#39934,#39935,#39936,#39937,#39938),
 .UNSPECIFIED.,.F.,.F.,(4,1,4),(14.3984001269718,15.3908199671854,15.7079632679489),
 .UNSPECIFIED.);
#5804=B_SPLINE_CURVE_WITH_KNOTS('',3,(#39941,#39942,#39943,#39944,#39945),
 .UNSPECIFIED.,.F.,.F.,(4,1,4),(13.8759337553363,14.8362483829486,15.7079632679489),
 .UNSPECIFIED.);
#5805=B_SPLINE_CURVE_WITH_KNOTS('',3,(#39951,#39952,#39953,#39954),
 .UNSPECIFIED.,.F.,.F.,(4,4),(95.5573427486708,96.2647245007222),
 .UNSPECIFIED.);
#5806=B_SPLINE_CURVE_WITH_KNOTS('',3,(#39962,#39963,#39964,#39965,#39966,
#39967,#39968,#39969,#39970,#39971),.UNSPECIFIED.,.F.,.F.,(4,3,3,4),(-94.2477796076937,
-93.2874649800814,-92.2950451398677,-91.8135687061555),.UNSPECIFIED.);
#5807=B_SPLINE_CURVE_WITH_KNOTS('',3,(#39976,#39977,#39978,#39979,#39980,
#39981,#39982,#39983,#39984,#39985,#39986,#39987,#39988,#39989,#39990,#39991,
#39992,#39993,#39994,#39995,#39996,#39997,#39998,#39999,#40000),
 .UNSPECIFIED.,.F.,.F.,(4,3,3,3,3,3,3,3,4),(89.2741574414912,89.3177856192269,
90.3102054594405,91.3026252996541,92.2950451398678,93.2874649800814,94.279884820295,
95.2723046605086,95.5573427486708),.UNSPECIFIED.);
#5808=B_SPLINE_CURVE_WITH_KNOTS('',3,(#40001,#40002,#40003,#40004,#40005,
#40006,#40007,#40008,#40009,#40010,#40011,#40012,#40013,#40014,#40015,#40016,
#40017,#40018,#40019,#40020,#40021,#40022),.UNSPECIFIED.,.F.,.F.,(4,3,3,
3,3,3,3,4),(-91.8135687061555,-91.3026252996541,-90.3102054594405,-89.3177856192268,
-88.3253657790132,-87.3329459387996,-86.340526098586,-85.5303833989758),
 .UNSPECIFIED.);
#5809=B_SPLINE_CURVE_WITH_KNOTS('',3,(#40027,#40028,#40029,#40030,#40031,
#40032,#40033,#40034,#40035,#40036,#40037,#40038,#40039,#40040,#40041,#40042,
#40043,#40044,#40045,#40046,#40047,#40048),.UNSPECIFIED.,.F.,.F.,(4,3,3,
3,3,3,3,4),(82.9909721343117,83.3632665779451,84.3556864181587,85.3481062583723,
86.340526098586,87.3329459387996,88.3253657790132,89.2741574414912),
 .UNSPECIFIED.);
#5810=B_SPLINE_CURVE_WITH_KNOTS('',3,(#40049,#40050,#40051,#40052,#40053,
#40054,#40055,#40056,#40057,#40058,#40059,#40060,#40061,#40062,#40063,#40064,
#40065,#40066,#40067,#40068,#40069,#40070,#40071,#40072,#40073),
 .UNSPECIFIED.,.F.,.F.,(4,3,3,3,3,3,3,3,4),(-85.5303833989758,-85.3481062583723,
-84.3556864181587,-83.3632665779451,-82.3708467377314,-81.3784268975178,
-80.3860070573042,-79.3935872170905,-79.2471980917962),.UNSPECIFIED.);
#5811=B_SPLINE_CURVE_WITH_KNOTS('',3,(#40078,#40079,#40080,#40081,#40082,
#40083,#40084,#40085,#40086,#40087,#40088,#40089,#40090,#40091,#40092,#40093,
#40094,#40095,#40096,#40097,#40098,#40099),.UNSPECIFIED.,.F.,.F.,(4,3,3,
3,3,3,3,4),(76.707786827132,77.4087475366633,78.4011673768769,79.3935872170906,
80.3860070573042,81.3784268975178,82.3708467377314,82.9909721343117),
 .UNSPECIFIED.);
#5812=B_SPLINE_CURVE_WITH_KNOTS('',3,(#40100,#40101,#40102,#40103,#40104,
#40105,#40106,#40107,#40108,#40109,#40110,#40111,#40112,#40113,#40114,#40115,
#40116,#40117,#40118,#40119,#40120,#40121),.UNSPECIFIED.,.F.,.F.,(4,3,3,
3,3,3,3,4),(-79.2471980917962,-78.4011673768769,-77.4087475366633,-76.4163276964496,
-75.423907856236,-74.4314880160224,-73.4390681758087,-72.9640127846167),
 .UNSPECIFIED.);
#5813=B_SPLINE_CURVE_WITH_KNOTS('',3,(#40126,#40127,#40128,#40129,#40130,
#40131,#40132,#40133,#40134,#40135,#40136,#40137,#40138,#40139,#40140,#40141,
#40142,#40143,#40144,#40145,#40146,#40147,#40148,#40149,#40150),
 .UNSPECIFIED.,.F.,.F.,(4,3,3,3,3,3,3,3,4),(70.4246015199524,70.4618086551678,
71.4542284953815,72.4466483355951,73.4390681758087,74.4314880160224,75.423907856236,
76.4163276964497,76.707786827132),.UNSPECIFIED.);
#5814=B_SPLINE_CURVE_WITH_KNOTS('',3,(#40151,#40152,#40153,#40154,#40155,
#40156,#40157,#40158,#40159,#40160,#40161,#40162,#40163,#40164,#40165,#40166,
#40167,#40168,#40169,#40170,#40171,#40172),.UNSPECIFIED.,.F.,.F.,(4,3,3,
3,3,3,3,4),(-72.9640127846167,-72.4466483355951,-71.4542284953815,-70.4618086551678,
-69.4693888149542,-68.4769689747406,-67.4845491345269,-66.6808274774371),
 .UNSPECIFIED.);
#5815=B_SPLINE_CURVE_WITH_KNOTS('',3,(#40177,#40178,#40179,#40180,#40181,
#40182,#40183,#40184,#40185,#40186,#40187,#40188,#40189,#40190,#40191,#40192,
#40193,#40194,#40195,#40196,#40197,#40198),.UNSPECIFIED.,.F.,.F.,(4,3,3,
3,3,3,3,4),(64.1414162127729,64.5072896138861,65.4997094540997,66.4921292943133,
67.4845491345269,68.4769689747406,69.4693888149542,70.4246015199524),
 .UNSPECIFIED.);
#5816=B_SPLINE_CURVE_WITH_KNOTS('',3,(#40199,#40200,#40201,#40202,#40203,
#40204,#40205,#40206,#40207,#40208,#40209,#40210,#40211,#40212,#40213,#40214,
#40215,#40216,#40217,#40218,#40219,#40220,#40221,#40222,#40223),
 .UNSPECIFIED.,.F.,.F.,(4,3,3,3,3,3,3,3,4),(-66.6808274774371,-66.4921292943133,
-65.4997094540997,-64.507289613886,-63.5148697736724,-62.5224499334588,
-61.5300300932452,-60.5376102530315,-60.3976421702574),.UNSPECIFIED.);
#5817=B_SPLINE_CURVE_WITH_KNOTS('',3,(#40228,#40229,#40230,#40231,#40232,
#40233,#40234,#40235,#40236,#40237,#40238,#40239,#40240,#40241,#40242,#40243,
#40244,#40245,#40246,#40247,#40248,#40249),.UNSPECIFIED.,.F.,.F.,(4,3,3,
3,3,3,3,4),(57.8582309055933,58.5527705726043,59.5451904128179,60.5376102530315,
61.5300300932452,62.5224499334588,63.5148697736725,64.1414162127729),
 .UNSPECIFIED.);
#5818=B_SPLINE_CURVE_WITH_KNOTS('',3,(#40250,#40251,#40252,#40253,#40254,
#40255,#40256,#40257,#40258,#40259,#40260,#40261,#40262,#40263,#40264,#40265,
#40266,#40267,#40268,#40269,#40270,#40271),.UNSPECIFIED.,.F.,.F.,(4,3,3,
3,3,3,3,4),(-60.3976421702574,-59.5451904128179,-58.5527705726043,-57.5603507323906,
-56.567930892177,-55.5755110519634,-54.5830912117497,-54.1144568630778),
 .UNSPECIFIED.);
#5819=B_SPLINE_CURVE_WITH_KNOTS('',3,(#40276,#40277,#40278,#40279,#40280,
#40281,#40282,#40283,#40284,#40285,#40286,#40287,#40288,#40289,#40290,#40291,
#40292,#40293,#40294,#40295,#40296,#40297,#40298,#40299,#40300),
 .UNSPECIFIED.,.F.,.F.,(4,3,3,3,3,3,3,3,4),(51.5750455984136,51.6058316911088,
52.5982515313225,53.5906713715361,54.5830912117497,55.5755110519634,56.567930892177,
57.5603507323906,57.8582309055933),.UNSPECIFIED.);
#5820=B_SPLINE_CURVE_WITH_KNOTS('',3,(#40301,#40302,#40303,#40304,#40305,
#40306,#40307,#40308,#40309,#40310,#40311,#40312,#40313,#40314,#40315,#40316,
#40317,#40318,#40319,#40320,#40321,#40322),.UNSPECIFIED.,.F.,.F.,(4,3,3,
3,3,3,3,4),(-54.1144568630778,-53.5906713715361,-52.5982515313225,-51.6058316911088,
-50.6134118508952,-49.6209920106816,-48.6285721704679,-47.8312715558983),
 .UNSPECIFIED.);
#5821=B_SPLINE_CURVE_WITH_KNOTS('',3,(#40327,#40328,#40329,#40330,#40331,
#40332,#40333,#40334,#40335,#40336,#40337,#40338,#40339,#40340,#40341,#40342,
#40343,#40344,#40345,#40346,#40347,#40348),.UNSPECIFIED.,.F.,.F.,(4,3,3,
3,3,3,3,4),(45.2918602912341,45.6513126498271,46.6437324900407,47.6361523302543,
48.628572170468,49.6209920106816,50.6134118508952,51.5750455984136),
 .UNSPECIFIED.);
#5822=B_SPLINE_CURVE_WITH_KNOTS('',3,(#40349,#40350,#40351,#40352,#40353,
#40354,#40355,#40356,#40357,#40358,#40359,#40360,#40361,#40362,#40363,#40364,
#40365,#40366,#40367,#40368,#40369,#40370,#40371,#40372,#40373),
 .UNSPECIFIED.,.F.,.F.,(4,3,3,3,3,3,3,3,4),(-47.8312715558983,-47.6361523302543,
-46.6437324900407,-45.651312649827,-44.6588928096134,-43.6664729693998,
-42.6740531291861,-41.6816332889725,-41.5480862487187),.UNSPECIFIED.);
#5823=B_SPLINE_CURVE_WITH_KNOTS('',3,(#40378,#40379,#40380,#40381,#40382,
#40383,#40384,#40385,#40386,#40387,#40388,#40389,#40390,#40391,#40392,#40393,
#40394,#40395,#40396,#40397,#40398,#40399),.UNSPECIFIED.,.F.,.F.,(4,3,3,
3,3,3,3,4),(39.0086749840545,39.6967936085453,40.6892134487589,41.6816332889725,
42.6740531291862,43.6664729693998,44.6588928096134,45.2918602912341),
 .UNSPECIFIED.);
#5824=B_SPLINE_CURVE_WITH_KNOTS('',3,(#40400,#40401,#40402,#40403,#40404,
#40405,#40406,#40407,#40408,#40409,#40410,#40411,#40412,#40413,#40414,#40415,
#40416,#40417,#40418,#40419,#40420,#40421),.UNSPECIFIED.,.F.,.F.,(4,3,3,
3,3,3,3,4),(-41.5480862487187,-40.6892134487589,-39.6967936085453,-38.7043737683316,
-37.711953928118,-36.7195340879044,-35.7271142476907,-35.264900941539),
 .UNSPECIFIED.);
#5825=B_SPLINE_CURVE_WITH_KNOTS('',3,(#40426,#40427,#40428,#40429,#40430,
#40431,#40432,#40433,#40434,#40435,#40436,#40437,#40438,#40439,#40440,#40441,
#40442,#40443,#40444,#40445,#40446,#40447,#40448,#40449,#40450),
 .UNSPECIFIED.,.F.,.F.,(4,3,3,3,3,3,3,3,4),(32.725489676875,32.7498547270498,
33.7422745672635,34.7346944074771,35.7271142476907,36.7195340879044,37.711953928118,
38.7043737683316,39.0086749840545),.UNSPECIFIED.);
#5826=B_SPLINE_CURVE_WITH_KNOTS('',3,(#40451,#40452,#40453,#40454,#40455,
#40456,#40457,#40458,#40459,#40460,#40461,#40462,#40463,#40464,#40465,#40466,
#40467,#40468,#40469,#40470,#40471,#40472),.UNSPECIFIED.,.F.,.F.,(4,3,3,
3,3,3,3,4),(-35.264900941539,-34.7346944074771,-33.7422745672635,-32.7498547270498,
-31.7574348868362,-30.7650150466226,-29.7725952064089,-28.9817156343595),
 .UNSPECIFIED.);
#5827=B_SPLINE_CURVE_WITH_KNOTS('',3,(#40477,#40478,#40479,#40480,#40481,
#40482,#40483,#40484,#40485,#40486,#40487,#40488,#40489,#40490,#40491,#40492,
#40493,#40494,#40495,#40496,#40497,#40498),.UNSPECIFIED.,.F.,.F.,(4,3,3,
3,3,3,3,4),(26.4423043696953,26.7953356857681,27.7877555259817,28.7801753661953,
29.772595206409,30.7650150466226,31.7574348868362,32.725489676875),
 .UNSPECIFIED.);
#5828=B_SPLINE_CURVE_WITH_KNOTS('',3,(#40499,#40500,#40501,#40502,#40503,
#40504,#40505,#40506,#40507,#40508,#40509,#40510,#40511,#40512,#40513,#40514,
#40515,#40516,#40517,#40518,#40519,#40520,#40521,#40522,#40523),
 .UNSPECIFIED.,.F.,.F.,(4,3,3,3,3,3,3,3,4),(-28.9817156343595,-28.7801753661953,
-27.7877555259817,-26.7953356857681,-25.8029158455544,-24.8104960053408,
-23.8180761651271,-22.8256563249135,-22.6985303271799),.UNSPECIFIED.);
#5829=B_SPLINE_CURVE_WITH_KNOTS('',3,(#40528,#40529,#40530,#40531,#40532,
#40533,#40534,#40535,#40536,#40537,#40538,#40539,#40540,#40541,#40542,#40543,
#40544,#40545,#40546,#40547,#40548,#40549),.UNSPECIFIED.,.F.,.F.,(4,3,3,
3,3,3,3,4),(20.1591190625157,20.8408166444863,21.8332364846999,22.8256563249135,
23.8180761651272,24.8104960053408,25.8029158455544,26.4423043696953),
 .UNSPECIFIED.);
#5830=B_SPLINE_CURVE_WITH_KNOTS('',3,(#40550,#40551,#40552,#40553,#40554,
#40555,#40556,#40557,#40558,#40559,#40560,#40561,#40562,#40563,#40564,#40565,
#40566,#40567,#40568,#40569,#40570,#40571),.UNSPECIFIED.,.F.,.F.,(4,3,3,
3,3,3,3,4),(-22.6985303271799,-21.8332364846999,-20.8408166444862,-19.8483968042726,
-18.855976964059,-17.8635571238454,-16.8711372836317,-16.4153450200004),
 .UNSPECIFIED.);
#5831=B_SPLINE_CURVE_WITH_KNOTS('',3,(#40576,#40577,#40578,#40579,#40580,
#40581,#40582,#40583,#40584,#40585,#40586,#40587,#40588,#40589,#40590,#40591,
#40592,#40593,#40594,#40595,#40596,#40597,#40598,#40599,#40600),
 .UNSPECIFIED.,.F.,.F.,(4,3,3,3,3,3,3,3,4),(13.8759337553361,13.8938777629908,
14.8862976032045,15.8787174434181,16.8711372836317,17.8635571238454,18.855976964059,
19.8483968042726,20.1591190625157),.UNSPECIFIED.);
#5832=B_SPLINE_CURVE_WITH_KNOTS('',3,(#40601,#40602,#40603,#40604,#40605,
#40606,#40607,#40608,#40609,#40610,#40611,#40612,#40613,#40614,#40615,#40616,
#40617,#40618,#40619,#40620,#40621,#40622),.UNSPECIFIED.,.F.,.F.,(4,3,3,
3,3,3,3,4),(-16.4153450200004,-15.8787174434181,-14.8862976032045,-13.8938777629908,
-12.9014579227772,-11.9090380825636,-10.9166182423499,-10.1321597128208),
 .UNSPECIFIED.);
#5833=B_SPLINE_CURVE_WITH_KNOTS('',3,(#40628,#40629,#40630,#40631,#40632,
#40633,#40634,#40635,#40636,#40637,#40638,#40639,#40640),.UNSPECIFIED.,
 .F.,.F.,(4,3,3,3,4),(-3.84897440564112,-2.97725952064089,-1.98483968042726,
-0.992419840213629,0.),.UNSPECIFIED.);
#5834=B_SPLINE_CURVE_WITH_KNOTS('',3,(#40643,#40644,#40645,#40646,#40647,
#40648,#40649,#40650,#40651,#40652,#40653,#40654,#40655,#40656,#40657,#40658,
#40659,#40660,#40661),.UNSPECIFIED.,.F.,.F.,(4,3,3,3,3,3,4),(2.01694489302852,
2.9772595206409,3.96967936085453,4.96209920106816,5.95451904128179,6.94693888149542,
7.59274844815659),.UNSPECIFIED.);
#5835=B_SPLINE_CURVE_WITH_KNOTS('',3,(#40667,#40668,#40669,#40670,#40671,
#40672,#40673,#40674),.UNSPECIFIED.,.F.,.F.,(4,1,1,1,1,4),(103.672557568463,
104.154034002175,105.146453842389,106.138873682603,107.131293522816,108.12371336303),
 .UNSPECIFIED.);
#5836=B_SPLINE_CURVE_WITH_KNOTS('',3,(#40677,#40678,#40679,#40680,#40681,
#40682,#40683,#40684,#40685),.UNSPECIFIED.,.F.,.F.,(4,1,1,1,1,1,4),(103.672557568463,
103.716185746199,104.708605586412,105.701025426626,106.69344526684,107.685865107053,
108.646179734666),.UNSPECIFIED.);
#5837=B_SPLINE_CURVE_WITH_KNOTS('',3,(#40690,#40691,#40692,#40693,#40694,
#40695,#40696,#40697,#40698,#40699),.UNSPECIFIED.,.F.,.F.,(4,1,1,1,1,1,
1,4),(97.3893722612835,98.1995149608937,99.1919348011073,100.184354641321,
101.176774481535,102.169194321748,103.161614161962,103.672557568463),
 .UNSPECIFIED.);
#5838=B_SPLINE_CURVE_WITH_KNOTS('',3,(#40700,#40701,#40702,#40703,#40704,
#40705,#40706,#40707,#40708,#40709),.UNSPECIFIED.,.F.,.F.,(4,1,1,1,1,1,
1,4),(97.3893722612835,97.7616667049169,98.7540865451305,99.7465063853441,
100.738926225558,101.731346065771,102.723765905985,103.672557568463),
 .UNSPECIFIED.);
#5839=B_SPLINE_CURVE_WITH_KNOTS('',3,(#40714,#40715,#40716,#40717,#40718,
#40719,#40720,#40721,#40722,#40723,#40724),.UNSPECIFIED.,.F.,.F.,(4,1,1,
1,1,1,1,1,4),(91.106186954104,91.2525760793982,92.2449959196119,93.2374157598255,
94.2298356000391,95.2222554402528,96.2146752804664,97.20709512068,97.3893722612835),
 .UNSPECIFIED.);
#5840=B_SPLINE_CURVE_WITH_KNOTS('',3,(#40725,#40726,#40727,#40728,#40729,
#40730,#40731,#40732,#40733,#40734),.UNSPECIFIED.,.F.,.F.,(4,1,1,1,1,1,
1,4),(91.106186954104,91.8071476636351,92.7995675038487,93.7919873440624,
94.784407184276,95.7768270244896,96.7692468647032,97.3893722612835),
 .UNSPECIFIED.);
#5841=B_SPLINE_CURVE_WITH_KNOTS('',3,(#40739,#40740,#40741,#40742,#40743,
#40744,#40745,#40746,#40747,#40748),.UNSPECIFIED.,.F.,.F.,(4,1,1,1,1,1,
1,4),(84.8230016469244,85.2980570381164,86.2904768783301,87.2828967185437,
88.2753165587573,89.267736398971,90.2601562391846,91.106186954104),
 .UNSPECIFIED.);
#5842=B_SPLINE_CURVE_WITH_KNOTS('',3,(#40749,#40750,#40751,#40752,#40753,
#40754,#40755,#40756,#40757,#40758,#40759),.UNSPECIFIED.,.F.,.F.,(4,1,1,
1,1,1,1,1,4),(84.8230016469244,84.8602087821397,85.8526286223533,86.8450484625669,
87.8374683027806,88.8298881429942,89.8223079832078,90.8147278234215,91.106186954104),
 .UNSPECIFIED.);
#5843=B_SPLINE_CURVE_WITH_KNOTS('',3,(#40764,#40765,#40766,#40767,#40768,
#40769,#40770,#40771,#40772,#40773),.UNSPECIFIED.,.F.,.F.,(4,1,1,1,1,1,
1,4),(78.5398163397448,79.3435379968347,80.3359578370483,81.3283776772619,
82.3207975174756,83.3132173576892,84.3056371979028,84.8230016469244),
 .UNSPECIFIED.);
#5844=B_SPLINE_CURVE_WITH_KNOTS('',3,(#40774,#40775,#40776,#40777,#40778,
#40779,#40780,#40781,#40782,#40783),.UNSPECIFIED.,.F.,.F.,(4,1,1,1,1,1,
1,4),(78.5398163397448,78.9056897408579,79.8981095810715,80.8905294212852,
81.8829492614988,82.8753691017124,83.867788941926,84.8230016469244),
 .UNSPECIFIED.);
#5845=B_SPLINE_CURVE_WITH_KNOTS('',3,(#40788,#40789,#40790,#40791,#40792,
#40793,#40794,#40795,#40796,#40797,#40798),.UNSPECIFIED.,.F.,.F.,(4,1,1,
1,1,1,1,1,4),(72.2566310325653,72.3965991153392,73.3890189555529,74.3814387957665,
75.3738586359801,76.3662784761938,77.3586983164074,78.351118156621,78.5398163397448),
 .UNSPECIFIED.);
#5846=B_SPLINE_CURVE_WITH_KNOTS('',3,(#40799,#40800,#40801,#40802,#40803,
#40804,#40805,#40806,#40807,#40808),.UNSPECIFIED.,.F.,.F.,(4,1,1,1,1,1,
1,4),(72.2566310325651,72.9511706995761,73.9435905397897,74.9360103800034,
75.928430220217,76.9208500604306,77.9132699006443,78.5398163397448),
 .UNSPECIFIED.);
#5847=B_SPLINE_CURVE_WITH_KNOTS('',3,(#40813,#40814,#40815,#40816,#40817,
#40818,#40819,#40820,#40821,#40822),.UNSPECIFIED.,.F.,.F.,(4,1,1,1,1,1,
1,4),(65.9734457253856,66.4420800740574,67.4344999142711,68.4269197544847,
69.4193395946983,70.411759434912,71.4041792751256,72.2566310325653),
 .UNSPECIFIED.);
#5848=B_SPLINE_CURVE_WITH_KNOTS('',3,(#40823,#40824,#40825,#40826,#40827,
#40828,#40829,#40830,#40831,#40832,#40833),.UNSPECIFIED.,.F.,.F.,(4,1,1,
1,1,1,1,1,4),(65.9734457253856,66.0042318180807,66.9966516582943,67.9890714985079,
68.9814913387216,69.9739111789352,70.9663310191488,71.9587508593625,72.2566310325651),
 .UNSPECIFIED.);
#5849=B_SPLINE_CURVE_WITH_KNOTS('',3,(#40838,#40839,#40840,#40841,#40842,
#40843,#40844,#40845,#40846,#40847),.UNSPECIFIED.,.F.,.F.,(4,1,1,1,1,1,
1,4),(59.690260418206,60.4875610327756,61.4799808729893,62.4724007132029,
63.4648205534165,64.4572403936302,65.4496602338438,65.9734457253856),
 .UNSPECIFIED.);
#5850=B_SPLINE_CURVE_WITH_KNOTS('',3,(#40848,#40849,#40850,#40851,#40852,
#40853,#40854,#40855,#40856,#40857),.UNSPECIFIED.,.F.,.F.,(4,1,1,1,1,1,
1,4),(59.690260418206,60.0497127767989,61.0421326170125,62.0345524572261,
63.0269722974398,64.0193921376534,65.011811977867,65.9734457253856),
 .UNSPECIFIED.);
#5851=B_SPLINE_CURVE_WITH_KNOTS('',3,(#40862,#40863,#40864,#40865,#40866,
#40867,#40868,#40869,#40870,#40871,#40872),.UNSPECIFIED.,.F.,.F.,(4,1,1,
1,1,1,1,1,4),(53.4070751110265,53.5406221512802,54.5330419914939,55.5254618317075,
56.5178816719211,57.5103015121348,58.5027213523484,59.495141192562,59.690260418206),
 .UNSPECIFIED.);
#5852=B_SPLINE_CURVE_WITH_KNOTS('',3,(#40873,#40874,#40875,#40876,#40877,
#40878,#40879,#40880,#40881,#40882),.UNSPECIFIED.,.F.,.F.,(4,1,1,1,1,1,
1,4),(53.4070751110265,54.0951937355171,55.0876135757307,56.0800334159443,
57.072453256158,58.0648730963716,59.0572929365852,59.690260418206),
 .UNSPECIFIED.);
#5853=B_SPLINE_CURVE_WITH_KNOTS('',3,(#40887,#40888,#40889,#40890,#40891,
#40892,#40893,#40894,#40895,#40896),.UNSPECIFIED.,.F.,.F.,(4,1,1,1,1,1,
1,4),(47.1238898038468,47.5861031099984,48.5785229502121,49.5709427904257,
50.5633626306393,51.555782470853,52.5482023110666,53.4070751110265),
 .UNSPECIFIED.);
#5854=B_SPLINE_CURVE_WITH_KNOTS('',3,(#40897,#40898,#40899,#40900,#40901,
#40902,#40903,#40904,#40905,#40906,#40907),.UNSPECIFIED.,.F.,.F.,(4,1,1,
1,1,1,1,1,4),(47.1238898038468,47.1482548540217,48.1406746942353,49.1330945344489,
50.1255143746626,51.1179342148762,52.1103540550898,53.1027738953035,53.4070751110265),
 .UNSPECIFIED.);
#5855=B_SPLINE_CURVE_WITH_KNOTS('',3,(#40912,#40913,#40914,#40915,#40916,
#40917,#40918,#40919,#40920,#40921),.UNSPECIFIED.,.F.,.F.,(4,1,1,1,1,1,
1,4),(40.8407044966672,41.6315840687166,42.6240039089303,43.6164237491439,
44.6088435893575,45.6012634295712,46.5936832697848,47.1238898038468),
 .UNSPECIFIED.);
#5856=B_SPLINE_CURVE_WITH_KNOTS('',3,(#40922,#40923,#40924,#40925,#40926,
#40927,#40928,#40929,#40930,#40931),.UNSPECIFIED.,.F.,.F.,(4,1,1,1,1,1,
1,4),(40.8407044966672,41.1937358127399,42.1861556529535,43.1785754931671,
44.1709953333808,45.1634151735944,46.155835013808,47.1238898038468),
 .UNSPECIFIED.);
#5857=B_SPLINE_CURVE_WITH_KNOTS('',3,(#40936,#40937,#40938,#40939,#40940,
#40941,#40942,#40943,#40944,#40945,#40946),.UNSPECIFIED.,.F.,.F.,(4,1,1,
1,1,1,1,1,4),(34.5575191894877,34.6846451872212,35.6770650274349,36.6694848676485,
37.6619047078621,38.6543245480758,39.6467443882894,40.639164228503,40.8407044966672),
 .UNSPECIFIED.);
#5858=B_SPLINE_CURVE_WITH_KNOTS('',3,(#40947,#40948,#40949,#40950,#40951,
#40952,#40953,#40954,#40955,#40956),.UNSPECIFIED.,.F.,.F.,(4,1,1,1,1,1,
1,4),(34.5575191894877,35.2392167714581,36.2316366116717,37.2240564518853,
38.216476292099,39.2088961323126,40.2013159725262,40.8407044966672),
 .UNSPECIFIED.);
#5859=B_SPLINE_CURVE_WITH_KNOTS('',3,(#40961,#40962,#40963,#40964,#40965,
#40966,#40967,#40968,#40969,#40970),.UNSPECIFIED.,.F.,.F.,(4,1,1,1,1,1,
1,4),(28.2743338823081,28.7301261459394,29.7225459861531,30.7149658263667,
31.7073856665803,32.699805506794,33.6922253470076,34.5575191894877),
 .UNSPECIFIED.);
#5860=B_SPLINE_CURVE_WITH_KNOTS('',3,(#40971,#40972,#40973,#40974,#40975,
#40976,#40977,#40978,#40979,#40980,#40981),.UNSPECIFIED.,.F.,.F.,(4,1,1,
1,1,1,1,1,4),(28.2743338823081,28.2922778899627,29.2846977301763,30.2771175703899,
31.2695374106036,32.2619572508172,33.2543770910308,34.2467969312444,34.5575191894877),
 .UNSPECIFIED.);
#5861=B_SPLINE_CURVE_WITH_KNOTS('',3,(#40986,#40987,#40988,#40989,#40990,
#40991,#40992,#40993,#40994,#40995),.UNSPECIFIED.,.F.,.F.,(4,1,1,1,1,1,
1,4),(21.9911485751285,22.7756071046577,23.7680269448713,24.7604467850849,
25.7528666252985,26.7452864655122,27.7377063057258,28.2743338823081),
 .UNSPECIFIED.);
#5862=B_SPLINE_CURVE_WITH_KNOTS('',3,(#40996,#40997,#40998,#40999,#41000,
#41001,#41002,#41003,#41004,#41005),.UNSPECIFIED.,.F.,.F.,(4,1,1,1,1,1,
1,4),(21.9911485751284,22.3377588486809,23.3301786888945,24.3225985291081,
25.3150183693218,26.3074382095354,27.299858049749,28.2743338823081),
 .UNSPECIFIED.);
#5863=B_SPLINE_CURVE_WITH_KNOTS('',3,(#41011,#41012,#41013,#41014,#41015),
 .UNSPECIFIED.,.F.,.F.,(4,1,4),(14.3984001269718,15.3908199671854,15.7079632679489),
 .UNSPECIFIED.);
#5864=B_SPLINE_CURVE_WITH_KNOTS('',3,(#41018,#41019,#41020,#41021,#41022),
 .UNSPECIFIED.,.F.,.F.,(4,1,4),(13.8759337553363,14.8362483829486,15.7079632679489),
 .UNSPECIFIED.);
#5865=B_SPLINE_CURVE_WITH_KNOTS('',3,(#41026,#41027,#41028,#41029,#41030,
#41031,#41032,#41033,#41034,#41035,#41036,#41037,#41038,#41039,#41040,#41041,
#41042,#41043),.UNSPECIFIED.,.F.,.F.,(4,2,2,2,2,2,2,2,4),(0.301357973509756,
0.376697466683881,0.452036959858006,0.527376453438759,0.602715947019511,
0.678055440600264,0.753394934181017,0.828734427355142,0.904073920529267),
 .UNSPECIFIED.);
#5866=B_SPLINE_CURVE_WITH_KNOTS('',3,(#41047,#41048,#41049,#41050,#41051,
#41052,#41053,#41054,#41055,#41056,#41057,#41058,#41059,#41060,#41061,#41062,
#41063,#41064,#41065,#41066,#41067,#41068,#41069,#41070,#41071,#41072),
 .UNSPECIFIED.,.F.,.F.,(4,2,2,2,2,2,2,2,2,2,2,2,4),(0.,0.0753399990358931,
0.150679998071786,0.226019996487856,0.301359994903926,0.376699993319996,
0.452039991736066,0.527379990771959,0.602719989807852,0.678059988843745,
0.753399987879638,0.828739986295708,0.904079984711778),.UNSPECIFIED.);
#5867=B_SPLINE_CURVE_WITH_KNOTS('',3,(#41073,#41074,#41075,#41076,#41077,
#41078,#41079,#41080,#41081,#41082),.UNSPECIFIED.,.F.,.F.,(4,2,2,2,4),(0.904079984711778,
0.979419983127848,1.05475998154392,1.13009998057981,1.2054399796157),
 .UNSPECIFIED.);
#5868=B_SPLINE_CURVE_WITH_KNOTS('',3,(#41083,#41084,#41085,#41086,#41087,
#41088,#41089,#41090,#41091,#41092,#41093,#41094,#41095,#41096,#41097,#41098,
#41099,#41100,#41101),.UNSPECIFIED.,.F.,.F.,(4,2,2,2,3,2,2,2,4),(0.904073920529267,
0.979413413703392,1.05475290687752,1.13009240045827,1.20543189403902,1.28077138761978,
1.35611088120053,1.43145037437465,1.50678986754878),.UNSPECIFIED.);
#5869=B_SPLINE_CURVE_WITH_KNOTS('',3,(#41105,#41106,#41107,#41108,#41109,
#41110,#41111,#41112,#41113,#41114,#41115,#41116,#41117,#41118,#41119,#41120,
#41121,#41122),.UNSPECIFIED.,.F.,.F.,(4,2,2,2,2,2,2,2,4),(0.301357973509756,
0.376697466683881,0.452036959858006,0.527376453438759,0.602715947019511,
0.678055440600264,0.753394934181017,0.828734427355142,0.904073920529267),
 .UNSPECIFIED.);
#5870=B_SPLINE_CURVE_WITH_KNOTS('',3,(#41123,#41124,#41125,#41126,#41127,
#41128,#41129,#41130,#41131,#41132,#41133,#41134,#41135,#41136,#41137,#41138,
#41139,#41140,#41141),.UNSPECIFIED.,.F.,.F.,(4,2,2,2,3,2,2,2,4),(0.904073920529267,
0.979413413703392,1.05475290687752,1.13009240045827,1.20543189403902,1.28077138761978,
1.35611088120053,1.43145037437465,1.50678986754878),.UNSPECIFIED.);
#5871=B_SPLINE_CURVE_WITH_KNOTS('',3,(#41145,#41146,#41147,#41148,#41149,
#41150,#41151,#41152,#41153,#41154),.UNSPECIFIED.,.F.,.F.,(4,2,2,2,4),(0.,
0.0753399990358931,0.150679998071786,0.226019996487856,0.301359994903926),
 .UNSPECIFIED.);
#5872=B_SPLINE_CURVE_WITH_KNOTS('',3,(#41155,#41156,#41157,#41158,#41159,
#41160,#41161,#41162,#41163,#41164,#41165,#41166,#41167,#41168,#41169,#41170,
#41171,#41172,#41173,#41174,#41175,#41176,#41177,#41178,#41179,#41180),
 .UNSPECIFIED.,.F.,.F.,(4,2,2,2,2,2,2,2,2,2,2,2,4),(0.301359994903926,0.376699993319996,
0.452039991736066,0.527379990771959,0.602719989807852,0.678059988843745,
0.753399987879638,0.828739986295708,0.904079984711778,0.979419983127848,
1.05475998154392,1.13009998057981,1.2054399796157),.UNSPECIFIED.);
#5873=B_SPLINE_CURVE_WITH_KNOTS('',3,(#41184,#41185,#41186,#41187,#41188,
#41189,#41190,#41191,#41192,#41193,#41194,#41195,#41196,#41197,#41198,#41199,
#41200,#41201),.UNSPECIFIED.,.F.,.F.,(4,2,2,2,2,2,2,2,4),(0.301357973509756,
0.376697466683881,0.452036959858006,0.527376453438759,0.602715947019511,
0.678055440600264,0.753394934181017,0.828734427355142,0.904073920529267),
 .UNSPECIFIED.);
#5874=B_SPLINE_CURVE_WITH_KNOTS('',3,(#41203,#41204,#41205,#41206,#41207,
#41208,#41209,#41210,#41211,#41212),.UNSPECIFIED.,.F.,.F.,(4,2,2,2,4),(1.20543189403902,
1.28077138761978,1.35611088120053,1.43145037437465,1.50678986754878),
 .UNSPECIFIED.);
#5875=B_SPLINE_CURVE_WITH_KNOTS('',3,(#41216,#41217,#41218,#41219,#41220,
#41221,#41222,#41223,#41224,#41225),.UNSPECIFIED.,.F.,.F.,(4,2,2,2,4),(0.904079984711778,
0.979419983127848,1.05475998154392,1.13009998057981,1.2054399796157),
 .UNSPECIFIED.);
#5876=B_SPLINE_CURVE_WITH_KNOTS('',3,(#41227,#41228,#41229,#41230,#41231,
#41232,#41233,#41234,#41235,#41236,#41237,#41238,#41239,#41240,#41241,#41242,
#41243,#41244),.UNSPECIFIED.,.F.,.F.,(4,2,2,2,2,2,2,2,4),(0.301359994903926,
0.376699993319996,0.452039991736066,0.527379990771959,0.602719989807852,
0.678059988843745,0.753399987879638,0.828739986295708,0.904079984711778),
 .UNSPECIFIED.);
#5877=B_SPLINE_CURVE_WITH_KNOTS('',3,(#41245,#41246,#41247,#41248,#41249,
#41250,#41251,#41252,#41253,#41254),.UNSPECIFIED.,.F.,.F.,(4,2,2,2,4),(0.,
0.0753399990358931,0.150679998071786,0.226019996487856,0.301359994903926),
 .UNSPECIFIED.);
#5878=B_SPLINE_CURVE_WITH_KNOTS('',3,(#41255,#41256,#41257,#41258,#41259,
#41260,#41261,#41262,#41263,#41264),.UNSPECIFIED.,.F.,.F.,(4,2,2,2,4),(0.904073920529267,
0.979413413703392,1.05475290687752,1.13009240045827,1.20543189403902),
 .UNSPECIFIED.);
#5879=B_SPLINE_CURVE_WITH_KNOTS('',3,(#41268,#41269,#41270,#41271,#41272,
#41273,#41274,#41275,#41276,#41277,#41278,#41279,#41280,#41281,#41282,#41283,
#41284,#41285),.UNSPECIFIED.,.F.,.F.,(4,2,2,2,2,2,2,2,4),(0.301357973509756,
0.376697466683881,0.452036959858006,0.527376453438759,0.602715947019511,
0.678055440600264,0.753394934181017,0.828734427355142,0.904073920529267),
 .UNSPECIFIED.);
#5880=B_SPLINE_CURVE_WITH_KNOTS('',3,(#41287,#41288,#41289,#41290,#41291,
#41292,#41293,#41294,#41295,#41296),.UNSPECIFIED.,.F.,.F.,(4,2,2,2,4),(1.20543189403902,
1.28077138761978,1.35611088120053,1.43145037437465,1.50678986754878),
 .UNSPECIFIED.);
#5881=B_SPLINE_CURVE_WITH_KNOTS('',3,(#41299,#41300,#41301,#41302,#41303,
#41304,#41305,#41306,#41307,#41308,#41309,#41310,#41311,#41312,#41313,#41314,
#41315,#41316,#41317,#41318,#41319,#41320,#41321,#41322,#41323,#41324,#41325,
#41326,#41327,#41328,#41329,#41330,#41331,#41332),.UNSPECIFIED.,.T.,.F.,
(4,2,2,2,2,2,2,2,2,2,2,2,2,2,2,2,4),(0.,0.0753399990358931,0.150679998071786,
0.226019996487856,0.301359994903926,0.376699993319996,0.452039991736066,
0.527379990771959,0.602719989807852,0.678059988843745,0.753399987879638,
0.828739986295708,0.904079984711778,0.979419983127848,1.05475998154392,
1.13009998057981,1.2054399796157),.UNSPECIFIED.);
#5882=B_SPLINE_CURVE_WITH_KNOTS('',3,(#41333,#41334,#41335,#41336,#41337,
#41338,#41339,#41340,#41341,#41342),.UNSPECIFIED.,.F.,.F.,(4,2,2,2,4),(0.904073920529267,
0.979413413703392,1.05475290687752,1.13009240045827,1.20543189403902),
 .UNSPECIFIED.);
#5883=B_SPLINE_CURVE_WITH_KNOTS('',3,(#41346,#41347,#41348,#41349,#41350,
#41351,#41352,#41353,#41354,#41355,#41356,#41357,#41358,#41359,#41360,#41361,
#41362,#41363),.UNSPECIFIED.,.F.,.F.,(4,2,2,2,2,2,2,2,4),(0.301357973509756,
0.376697466683881,0.452036959858007,0.52737645343876,0.602715947019512,
0.678055440600265,0.753394934181018,0.828734427355143,0.904073920529268),
 .UNSPECIFIED.);
#5884=B_SPLINE_CURVE_WITH_KNOTS('',3,(#41367,#41368,#41369,#41370,#41371,
#41372,#41373,#41374,#41375,#41376,#41377,#41378,#41379,#41380,#41381,#41382,
#41383,#41384,#41385,#41386,#41387,#41388,#41389,#41390,#41391,#41392),
 .UNSPECIFIED.,.F.,.F.,(4,2,2,2,2,2,2,2,2,2,2,2,4),(0.,0.0753399990358932,
0.150679998071786,0.226019996487856,0.301359994903927,0.376699993319997,
0.452039991736067,0.52737999077196,0.602719989807853,0.678059988843746,
0.753399987879639,0.828739986295709,0.90407998471178),.UNSPECIFIED.);
#5885=B_SPLINE_CURVE_WITH_KNOTS('',3,(#41393,#41394,#41395,#41396,#41397,
#41398,#41399,#41400,#41401,#41402),.UNSPECIFIED.,.F.,.F.,(4,2,2,2,4),(0.90407998471178,
0.97941998312785,1.05475998154392,1.13009998057981,1.20543997961571),
 .UNSPECIFIED.);
#5886=B_SPLINE_CURVE_WITH_KNOTS('',3,(#41403,#41404,#41405,#41406,#41407,
#41408,#41409,#41410,#41411,#41412,#41413,#41414,#41415,#41416,#41417,#41418,
#41419,#41420,#41421),.UNSPECIFIED.,.F.,.F.,(4,2,2,2,3,2,2,2,4),(0.904073920529268,
0.979413413703393,1.05475290687752,1.13009240045827,1.20543189403902,1.28077138761978,
1.35611088120053,1.43145037437465,1.50678986754878),.UNSPECIFIED.);
#5887=B_SPLINE_CURVE_WITH_KNOTS('',3,(#41425,#41426,#41427,#41428,#41429,
#41430,#41431,#41432,#41433,#41434,#41435,#41436,#41437,#41438,#41439,#41440,
#41441,#41442),.UNSPECIFIED.,.F.,.F.,(4,2,2,2,2,2,2,2,4),(0.301357973509756,
0.376697466683882,0.452036959858007,0.52737645343876,0.602715947019512,
0.678055440600265,0.753394934181018,0.828734427355143,0.904073920529268),
 .UNSPECIFIED.);
#5888=B_SPLINE_CURVE_WITH_KNOTS('',3,(#41443,#41444,#41445,#41446,#41447,
#41448,#41449,#41450,#41451,#41452,#41453,#41454,#41455,#41456,#41457,#41458,
#41459,#41460,#41461),.UNSPECIFIED.,.F.,.F.,(4,2,2,2,3,2,2,2,4),(0.904073920529268,
0.979413413703394,1.05475290687752,1.13009240045827,1.20543189403902,1.28077138761978,
1.35611088120053,1.43145037437466,1.50678986754878),.UNSPECIFIED.);
#5889=B_SPLINE_CURVE_WITH_KNOTS('',3,(#41465,#41466,#41467,#41468,#41469,
#41470,#41471,#41472,#41473,#41474),.UNSPECIFIED.,.F.,.F.,(4,2,2,2,4),(0.,
0.0753399990358932,0.150679998071786,0.226019996487856,0.301359994903927),
 .UNSPECIFIED.);
#5890=B_SPLINE_CURVE_WITH_KNOTS('',3,(#41475,#41476,#41477,#41478,#41479,
#41480,#41481,#41482,#41483,#41484,#41485,#41486,#41487,#41488,#41489,#41490,
#41491,#41492,#41493,#41494,#41495,#41496,#41497,#41498,#41499,#41500),
 .UNSPECIFIED.,.F.,.F.,(4,2,2,2,2,2,2,2,2,2,2,2,4),(0.301359994903927,0.376699993319997,
0.452039991736067,0.52737999077196,0.602719989807853,0.678059988843746,
0.75339998787964,0.82873998629571,0.90407998471178,0.97941998312785,1.05475998154392,
1.13009998057981,1.20543997961571),.UNSPECIFIED.);
#5891=B_SPLINE_CURVE_WITH_KNOTS('',3,(#41504,#41505,#41506,#41507,#41508,
#41509,#41510,#41511,#41512,#41513,#41514,#41515,#41516,#41517,#41518,#41519,
#41520,#41521),.UNSPECIFIED.,.F.,.F.,(4,2,2,2,2,2,2,2,4),(0.301357973509756,
0.376697466683882,0.452036959858007,0.52737645343876,0.602715947019512,
0.678055440600265,0.753394934181018,0.828734427355143,0.904073920529268),
 .UNSPECIFIED.);
#5892=B_SPLINE_CURVE_WITH_KNOTS('',3,(#41523,#41524,#41525,#41526,#41527,
#41528,#41529,#41530,#41531,#41532),.UNSPECIFIED.,.F.,.F.,(4,2,2,2,4),(1.20543189403902,
1.28077138761978,1.35611088120053,1.43145037437466,1.50678986754878),
 .UNSPECIFIED.);
#5893=B_SPLINE_CURVE_WITH_KNOTS('',3,(#41536,#41537,#41538,#41539,#41540,
#41541,#41542,#41543,#41544,#41545),.UNSPECIFIED.,.F.,.F.,(4,2,2,2,4),(0.90407998471178,
0.97941998312785,1.05475998154392,1.13009998057981,1.20543997961571),
 .UNSPECIFIED.);
#5894=B_SPLINE_CURVE_WITH_KNOTS('',3,(#41547,#41548,#41549,#41550,#41551,
#41552,#41553,#41554,#41555,#41556,#41557,#41558,#41559,#41560,#41561,#41562,
#41563,#41564),.UNSPECIFIED.,.F.,.F.,(4,2,2,2,2,2,2,2,4),(0.301359994903927,
0.376699993319997,0.452039991736067,0.52737999077196,0.602719989807853,
0.678059988843746,0.753399987879639,0.828739986295709,0.90407998471178),
 .UNSPECIFIED.);
#5895=B_SPLINE_CURVE_WITH_KNOTS('',3,(#41565,#41566,#41567,#41568,#41569,
#41570,#41571,#41572,#41573,#41574),.UNSPECIFIED.,.F.,.F.,(4,2,2,2,4),(0.,
0.0753399990358932,0.150679998071786,0.226019996487856,0.301359994903927),
 .UNSPECIFIED.);
#5896=B_SPLINE_CURVE_WITH_KNOTS('',3,(#41575,#41576,#41577,#41578,#41579,
#41580,#41581,#41582,#41583,#41584),.UNSPECIFIED.,.F.,.F.,(4,2,2,2,4),(0.904073920529268,
0.979413413703393,1.05475290687752,1.13009240045827,1.20543189403902),
 .UNSPECIFIED.);
#5897=B_SPLINE_CURVE_WITH_KNOTS('',3,(#41588,#41589,#41590,#41591,#41592,
#41593,#41594,#41595,#41596,#41597,#41598,#41599,#41600,#41601,#41602,#41603,
#41604,#41605),.UNSPECIFIED.,.F.,.F.,(4,2,2,2,2,2,2,2,4),(0.301357973509756,
0.376697466683882,0.452036959858007,0.52737645343876,0.602715947019512,
0.678055440600265,0.753394934181018,0.828734427355143,0.904073920529268),
 .UNSPECIFIED.);
#5898=B_SPLINE_CURVE_WITH_KNOTS('',3,(#41607,#41608,#41609,#41610,#41611,
#41612,#41613,#41614,#41615,#41616),.UNSPECIFIED.,.F.,.F.,(4,2,2,2,4),(1.20543189403902,
1.28077138761978,1.35611088120053,1.43145037437466,1.50678986754878),
 .UNSPECIFIED.);
#5899=B_SPLINE_CURVE_WITH_KNOTS('',3,(#41619,#41620,#41621,#41622,#41623,
#41624,#41625,#41626,#41627,#41628,#41629,#41630,#41631,#41632,#41633,#41634,
#41635,#41636,#41637,#41638,#41639,#41640,#41641,#41642,#41643,#41644,#41645,
#41646,#41647,#41648,#41649,#41650,#41651,#41652),.UNSPECIFIED.,.T.,.F.,
(4,2,2,2,2,2,2,2,2,2,2,2,2,2,2,2,4),(0.,0.0753399990358932,0.150679998071786,
0.226019996487856,0.301359994903927,0.376699993319997,0.452039991736067,
0.52737999077196,0.602719989807853,0.678059988843746,0.753399987879639,
0.828739986295709,0.90407998471178,0.97941998312785,1.05475998154392,1.13009998057981,
1.20543997961571),.UNSPECIFIED.);
#5900=B_SPLINE_CURVE_WITH_KNOTS('',3,(#41653,#41654,#41655,#41656,#41657,
#41658,#41659,#41660,#41661,#41662),.UNSPECIFIED.,.F.,.F.,(4,2,2,2,4),(0.904073920529268,
0.979413413703393,1.05475290687752,1.13009240045827,1.20543189403902),
 .UNSPECIFIED.);
#5901=B_SPLINE_CURVE_WITH_KNOTS('',3,(#41666,#41667,#41668,#41669,#41670,
#41671,#41672,#41673,#41674,#41675,#41676,#41677,#41678,#41679,#41680,#41681,
#41682,#41683),.UNSPECIFIED.,.F.,.F.,(4,2,2,2,2,2,2,2,4),(0.301357973509755,
0.37669746668388,0.452036959858005,0.527376453438758,0.602715947019511,
0.678055440600264,0.753394934181017,0.828734427355142,0.904073920529267),
 .UNSPECIFIED.);
#5902=B_SPLINE_CURVE_WITH_KNOTS('',3,(#41687,#41688,#41689,#41690,#41691,
#41692,#41693,#41694,#41695,#41696,#41697,#41698,#41699,#41700,#41701,#41702,
#41703,#41704,#41705,#41706,#41707,#41708,#41709,#41710,#41711,#41712),
 .UNSPECIFIED.,.F.,.F.,(4,2,2,2,2,2,2,2,2,2,2,2,4),(0.,0.0753399990358932,
0.150679998071786,0.226019996487857,0.301359994903927,0.376699993319997,
0.452039991736067,0.52737999077196,0.602719989807853,0.678059988843747,
0.75339998787964,0.828739986295709,0.904079984711779),.UNSPECIFIED.);
#5903=B_SPLINE_CURVE_WITH_KNOTS('',3,(#41713,#41714,#41715,#41716,#41717,
#41718,#41719,#41720,#41721,#41722),.UNSPECIFIED.,.F.,.F.,(4,2,2,2,4),(0.904079984711779,
0.979419983127849,1.05475998154392,1.13009998057981,1.20543997961571),
 .UNSPECIFIED.);
#5904=B_SPLINE_CURVE_WITH_KNOTS('',3,(#41723,#41724,#41725,#41726,#41727,
#41728,#41729,#41730,#41731,#41732,#41733,#41734,#41735,#41736,#41737,#41738,
#41739,#41740,#41741),.UNSPECIFIED.,.F.,.F.,(4,2,2,2,3,2,2,2,4),(0.904073920529267,
0.979413413703393,1.05475290687752,1.13009240045827,1.20543189403902,1.28077138761978,
1.35611088120053,1.43145037437465,1.50678986754878),.UNSPECIFIED.);
#5905=B_SPLINE_CURVE_WITH_KNOTS('',3,(#41745,#41746,#41747,#41748,#41749,
#41750,#41751,#41752,#41753,#41754,#41755,#41756,#41757,#41758,#41759,#41760,
#41761,#41762),.UNSPECIFIED.,.F.,.F.,(4,2,2,2,2,2,2,2,4),(0.301357973509756,
0.37669746668388,0.452036959858006,0.527376453438758,0.602715947019511,
0.678055440600264,0.753394934181016,0.828734427355142,0.904073920529267),
 .UNSPECIFIED.);
#5906=B_SPLINE_CURVE_WITH_KNOTS('',3,(#41763,#41764,#41765,#41766,#41767,
#41768,#41769,#41770,#41771,#41772,#41773,#41774,#41775,#41776,#41777,#41778,
#41779,#41780,#41781),.UNSPECIFIED.,.F.,.F.,(4,2,2,2,3,2,2,2,4),(0.904073920529267,
0.979413413703393,1.05475290687752,1.13009240045827,1.20543189403902,1.28077138761978,
1.35611088120053,1.43145037437465,1.50678986754878),.UNSPECIFIED.);
#5907=B_SPLINE_CURVE_WITH_KNOTS('',3,(#41785,#41786,#41787,#41788,#41789,
#41790,#41791,#41792,#41793,#41794),.UNSPECIFIED.,.F.,.F.,(4,2,2,2,4),(0.,
0.0753399990358931,0.150679998071786,0.226019996487856,0.301359994903927),
 .UNSPECIFIED.);
#5908=B_SPLINE_CURVE_WITH_KNOTS('',3,(#41795,#41796,#41797,#41798,#41799,
#41800,#41801,#41802,#41803,#41804,#41805,#41806,#41807,#41808,#41809,#41810,
#41811,#41812,#41813,#41814,#41815,#41816,#41817,#41818,#41819,#41820),
 .UNSPECIFIED.,.F.,.F.,(4,2,2,2,2,2,2,2,2,2,2,2,4),(0.301359994903927,0.376699993319997,
0.452039991736067,0.52737999077196,0.602719989807853,0.678059988843746,
0.75339998787964,0.828739986295709,0.904079984711779,0.979419983127849,
1.05475998154392,1.13009998057981,1.2054399796157),.UNSPECIFIED.);
#5909=B_SPLINE_CURVE_WITH_KNOTS('',3,(#41824,#41825,#41826,#41827,#41828,
#41829,#41830,#41831,#41832,#41833,#41834,#41835,#41836,#41837,#41838,#41839,
#41840,#41841),.UNSPECIFIED.,.F.,.F.,(4,2,2,2,2,2,2,2,4),(0.301357973509755,
0.37669746668388,0.452036959858005,0.527376453438758,0.602715947019511,
0.678055440600264,0.753394934181016,0.828734427355142,0.904073920529267),
 .UNSPECIFIED.);
#5910=B_SPLINE_CURVE_WITH_KNOTS('',3,(#41843,#41844,#41845,#41846,#41847,
#41848,#41849,#41850,#41851,#41852),.UNSPECIFIED.,.F.,.F.,(4,2,2,2,4),(1.20543189403902,
1.28077138761978,1.35611088120053,1.43145037437465,1.50678986754878),
 .UNSPECIFIED.);
#5911=B_SPLINE_CURVE_WITH_KNOTS('',3,(#41856,#41857,#41858,#41859,#41860,
#41861,#41862,#41863,#41864,#41865),.UNSPECIFIED.,.F.,.F.,(4,2,2,2,4),(0.904079984711779,
0.979419983127849,1.05475998154392,1.13009998057981,1.2054399796157),
 .UNSPECIFIED.);
#5912=B_SPLINE_CURVE_WITH_KNOTS('',3,(#41867,#41868,#41869,#41870,#41871,
#41872,#41873,#41874,#41875,#41876,#41877,#41878,#41879,#41880,#41881,#41882,
#41883,#41884),.UNSPECIFIED.,.F.,.F.,(4,2,2,2,2,2,2,2,4),(0.301359994903927,
0.376699993319997,0.452039991736067,0.52737999077196,0.602719989807853,
0.678059988843746,0.75339998787964,0.828739986295709,0.904079984711779),
 .UNSPECIFIED.);
#5913=B_SPLINE_CURVE_WITH_KNOTS('',3,(#41885,#41886,#41887,#41888,#41889,
#41890,#41891,#41892,#41893,#41894),.UNSPECIFIED.,.F.,.F.,(4,2,2,2,4),(0.,
0.0753399990358931,0.150679998071786,0.226019996487856,0.301359994903927),
 .UNSPECIFIED.);
#5914=B_SPLINE_CURVE_WITH_KNOTS('',3,(#41895,#41896,#41897,#41898,#41899,
#41900,#41901,#41902,#41903,#41904),.UNSPECIFIED.,.F.,.F.,(4,2,2,2,4),(0.904073920529267,
0.979413413703393,1.05475290687752,1.13009240045827,1.20543189403902),
 .UNSPECIFIED.);
#5915=B_SPLINE_CURVE_WITH_KNOTS('',3,(#41908,#41909,#41910,#41911,#41912,
#41913,#41914,#41915,#41916,#41917,#41918,#41919,#41920,#41921,#41922,#41923,
#41924,#41925),.UNSPECIFIED.,.F.,.F.,(4,2,2,2,2,2,2,2,4),(0.301357973509755,
0.37669746668388,0.452036959858005,0.527376453438758,0.602715947019511,
0.678055440600264,0.753394934181016,0.828734427355142,0.904073920529267),
 .UNSPECIFIED.);
#5916=B_SPLINE_CURVE_WITH_KNOTS('',3,(#41927,#41928,#41929,#41930,#41931,
#41932,#41933,#41934,#41935,#41936),.UNSPECIFIED.,.F.,.F.,(4,2,2,2,4),(1.20543189403902,
1.28077138761978,1.35611088120053,1.43145037437465,1.50678986754878),
 .UNSPECIFIED.);
#5917=B_SPLINE_CURVE_WITH_KNOTS('',3,(#41939,#41940,#41941,#41942,#41943,
#41944,#41945,#41946,#41947,#41948,#41949,#41950,#41951,#41952,#41953,#41954,
#41955,#41956,#41957,#41958,#41959,#41960,#41961,#41962,#41963,#41964,#41965,
#41966,#41967,#41968,#41969,#41970,#41971,#41972),.UNSPECIFIED.,.T.,.F.,
(4,2,2,2,2,2,2,2,2,2,2,2,2,2,2,2,4),(0.,0.0753399990358931,0.150679998071786,
0.226019996487856,0.301359994903927,0.376699993319997,0.452039991736067,
0.52737999077196,0.602719989807853,0.678059988843746,0.75339998787964,0.828739986295709,
0.904079984711779,0.979419983127849,1.05475998154392,1.13009998057981,1.2054399796157),
 .UNSPECIFIED.);
#5918=B_SPLINE_CURVE_WITH_KNOTS('',3,(#41973,#41974,#41975,#41976,#41977,
#41978,#41979,#41980,#41981,#41982),.UNSPECIFIED.,.F.,.F.,(4,2,2,2,4),(0.904073920529267,
0.979413413703393,1.05475290687752,1.13009240045827,1.20543189403902),
 .UNSPECIFIED.);
#5919=B_SPLINE_CURVE_WITH_KNOTS('',3,(#41984,#41985,#41986,#41987,#41988,
#41989,#41990,#41991,#41992,#41993,#41994,#41995,#41996,#41997,#41998,#41999,
#42000,#42001,#42002,#42003,#42004,#42005,#42006,#42007,#42008,#42009,#42010,
#42011,#42012,#42013,#42014,#42015,#42016,#42017,#42018,#42019,#42020,#42021,
#42022,#42023,#42024,#42025,#42026,#42027,#42028,#42029,#42030,#42031,#42032,
#42033,#42034,#42035,#42036,#42037,#42038,#42039,#42040,#42041,#42042,#42043,
#42044,#42045,#42046,#42047,#42048,#42049,#42050,#42051,#42052,#42053,#42054,
#42055,#42056,#42057,#42058,#42059,#42060,#42061,#42062,#42063,#42064,#42065,
#42066,#42067,#42068,#42069,#42070,#42071,#42072,#42073,#42074,#42075,#42076,
#42077,#42078,#42079,#42080),.UNSPECIFIED.,.F.,.F.,(4,3,3,3,3,3,3,3,3,3,
3,3,3,3,3,3,3,3,3,3,3,3,3,3,3,3,3,3,3,3,3,3,4),(-0.569248610399337,-0.543574665913807,
-0.51727245328848,-0.510408802663154,-0.504800523775832,-0.47773970928715,
-0.455902642111078,-0.447185941747197,-0.442501781607008,-0.414772156692359,
-0.386610546537412,-0.358667936434586,-0.344761745295583,-0.340663182606779,
-0.336259776461384,-0.307329116975324,-0.303043171878573,-0.27522662276973,
-0.246781267954678,-0.236972518199776,-0.232129158585461,-0.228298533654497,
-0.199315149767015,-0.169756960554979,-0.139958455388845,-0.123701275093121,
-0.118725825268248,-0.114410875368034,-0.0838707291780127,-0.053291589117924,
-0.0233203534222033,-0.00990101302305402,0.),.UNSPECIFIED.);
#5920=B_SPLINE_CURVE_WITH_KNOTS('',3,(#42081,#42082,#42083,#42084,#42085,
#42086,#42087,#42088,#42089,#42090,#42091,#42092,#42093,#42094,#42095,#42096,
#42097,#42098,#42099,#42100,#42101,#42102,#42103,#42104,#42105,#42106,#42107,
#42108,#42109,#42110,#42111,#42112,#42113,#42114,#42115,#42116,#42117,#42118,
#42119,#42120,#42121,#42122,#42123,#42124,#42125,#42126,#42127,#42128,#42129,
#42130,#42131,#42132,#42133,#42134,#42135,#42136,#42137,#42138,#42139,#42140,
#42141,#42142,#42143,#42144,#42145,#42146,#42147,#42148,#42149,#42150,#42151,
#42152,#42153,#42154,#42155,#42156,#42157,#42158,#42159,#42160,#42161,#42162,
#42163,#42164,#42165,#42166,#42167,#42168,#42169,#42170,#42171,#42172,#42173,
#42174),.UNSPECIFIED.,.F.,.F.,(4,3,3,3,3,3,3,3,3,3,3,3,3,3,3,3,3,3,3,3,
3,3,3,3,3,3,3,3,3,3,3,4),(-0.56684730604813,-0.536665862167618,-0.506059953422707,
-0.497416406503416,-0.490479621633712,-0.460332810122765,-0.437094434682836,
-0.424724933789942,-0.420483367383437,-0.391058514880852,-0.361900337811473,
-0.333575724283842,-0.318788244863715,-0.31312587650193,-0.30869595256902,
-0.280705563216954,-0.274425806603334,-0.245949103512894,-0.216224273057835,
-0.204597316409418,-0.200878698435462,-0.17304519623036,-0.145277260413139,
-0.117980535703011,-0.104251776224188,-0.100006100346348,-0.0958284117611523,
-0.0691557510127404,-0.0429305470424711,-0.0175053685333362,-0.00815045987242433,
0.),.UNSPECIFIED.);
#5921=B_SPLINE_CURVE_WITH_KNOTS('',3,(#42176,#42177,#42178,#42179,#42180,
#42181,#42182,#42183,#42184,#42185,#42186),.UNSPECIFIED.,.F.,.F.,(4,1,1,
1,1,1,1,1,4),(15.7079632679489,15.8286682231622,16.8210880633759,17.8135079035895,
18.8059277438031,19.7983475840168,20.7907674242304,21.783187264444,21.9911485751285),
 .UNSPECIFIED.);
#5922=B_SPLINE_CURVE_WITH_KNOTS('',3,(#42187,#42188,#42189,#42190,#42191,
#42192,#42193,#42194,#42195,#42196),.UNSPECIFIED.,.F.,.F.,(4,1,1,1,1,1,
1,4),(15.7079632679489,16.3832398073991,17.3756596476127,18.3680794878263,
19.36049932804,20.3529191682536,21.3453390084672,21.9911485751284),
 .UNSPECIFIED.);
#5923=B_SPLINE_CURVE_WITH_KNOTS('',3,(#42597,#42598,#42599,#42600,#42601,
#42602,#42603,#42604,#42605,#42606,#42607,#42608,#42609,#42610,#42611,#42612,
#42613,#42614,#42615,#42616,#42617,#42618,#42619,#42620,#42621,#42622,#42623,
#42624,#42625,#42626,#42627,#42628,#42629,#42630,#42631,#42632,#42633,#42634,
#42635,#42636,#42637,#42638,#42639,#42640,#42641,#42642,#42643,#42644,#42645,
#42646,#42647,#42648,#42649,#42650,#42651,#42652,#42653,#42654,#42655,#42656,
#42657,#42658,#42659,#42660,#42661,#42662,#42663,#42664,#42665,#42666,#42667,
#42668,#42669,#42670,#42671,#42672,#42673,#42674,#42675,#42676,#42677,#42678,
#42679,#42680,#42681,#42682,#42683,#42684,#42685,#42686,#42687,#42688,#42689,
#42690),.UNSPECIFIED.,.F.,.F.,(4,3,3,3,3,3,3,3,3,3,3,3,3,3,3,3,3,3,3,3,
3,3,3,3,3,3,3,3,3,3,3,4),(0.,0.0253630259498556,0.0513976226489003,0.0781462280587279,
0.0899194383258336,0.0966315939993256,0.102678021611066,0.129978487836714,
0.157730214206848,0.184644277137016,0.19593207222776,0.203012844728639,
0.207156655375447,0.236271560651484,0.265386465927521,0.293279271834908,
0.302554877553506,0.311292566193412,0.315704524166816,0.343817419217604,
0.372959123929891,0.402412672778624,0.4133424655252,0.422898831534667,0.428117874468216,
0.458184918270041,0.482885311859882,0.492048607646526,0.498170307491992,
0.528680781133954,0.556986492629404,0.566847306048082),.UNSPECIFIED.);
#5924=B_SPLINE_CURVE_WITH_KNOTS('',3,(#42691,#42692,#42693,#42694,#42695,
#42696,#42697,#42698,#42699,#42700,#42701,#42702,#42703,#42704,#42705,#42706,
#42707,#42708,#42709,#42710,#42711,#42712,#42713,#42714,#42715),
 .UNSPECIFIED.,.F.,.F.,(4,3,3,3,3,3,3,3,4),(-10.1321597128208,-9.92419840213631,
-8.93177856192268,-7.93935872170905,-6.94693888149542,-5.95451904128179,
-4.96209920106816,-3.96967936085453,-3.84897440564112),.UNSPECIFIED.);
#5925=B_SPLINE_CURVE_WITH_KNOTS('',3,(#43116,#43117,#43118,#43119,#43120,
#43121,#43122,#43123,#43124,#43125,#43126,#43127,#43128,#43129,#43130,#43131,
#43132,#43133,#43134,#43135,#43136,#43137),.UNSPECIFIED.,.F.,.F.,(4,3,3,
3,3,3,3,4),(7.59274844815659,7.93935872170906,8.93177856192269,9.92419840213632,
10.9166182423499,11.9090380825636,12.9014579227772,13.8759337553361),
 .UNSPECIFIED.);
#5926=B_SPLINE_CURVE_WITH_KNOTS('',3,(#43138,#43139,#43140,#43141,#43142,
#43143,#43144,#43145,#43146,#43147,#43148,#43149,#43150,#43151,#43152,#43153,
#43154,#43155,#43156,#43157,#43158,#43159,#43160,#43161,#43162,#43163,#43164,
#43165,#43166,#43167,#43168,#43169,#43170,#43171,#43172,#43173,#43174,#43175,
#43176,#43177,#43178,#43179,#43180,#43181,#43182,#43183,#43184,#43185,#43186,
#43187,#43188,#43189,#43190,#43191,#43192,#43193,#43194,#43195,#43196,#43197,
#43198,#43199,#43200,#43201,#43202,#43203,#43204,#43205,#43206,#43207,#43208,
#43209,#43210,#43211,#43212,#43213,#43214,#43215,#43216,#43217,#43218,#43219,
#43220,#43221,#43222,#43223,#43224,#43225,#43226,#43227,#43228),
 .UNSPECIFIED.,.F.,.F.,(4,3,3,3,3,3,3,3,3,3,3,3,3,3,3,3,3,3,3,3,3,3,3,3,
3,3,3,3,3,3,4),(0.,0.0297240839684256,0.0601072325498447,0.0893395071893512,
0.114917747498919,0.120626859687113,0.150385989363053,0.179981400050151,
0.208477407454087,0.22042950374967,0.228738548914548,0.234134417006902,
0.264049923336399,0.291955958271147,0.293965429665896,0.322911496990148,
0.339206044994607,0.343413985005071,0.37150622848317,0.399645181299159,
0.427381812169266,0.437705393072651,0.444698500366259,0.448877446518554,
0.476925760110501,0.497961995304462,0.506030983450329,0.511791121632976,
0.537728941220283,0.561070700886344,0.569248610399446),.UNSPECIFIED.);
#5927=B_SPLINE_CURVE_WITH_KNOTS('',3,(#43231,#43232,#43233,#43234,#43235,
#43236,#43237,#43238,#43239,#43240,#43241,#43242,#43243,#43244,#43245,#43246,
#43247,#43248,#43249,#43250,#43251,#43252,#43253,#43254,#43255,#43256,#43257,
#43258,#43259,#43260,#43261,#43262,#43263,#43264,#43265,#43266,#43267,#43268,
#43269,#43270,#43271,#43272,#43273,#43274,#43275,#43276,#43277,#43278,#43279,
#43280,#43281,#43282,#43283,#43284,#43285,#43286,#43287,#43288,#43289,#43290,
#43291,#43292,#43293,#43294,#43295,#43296,#43297,#43298,#43299,#43300,#43301,
#43302,#43303,#43304,#43305,#43306,#43307,#43308,#43309,#43310,#43311,#43312,
#43313,#43314,#43315,#43316,#43317,#43318,#43319,#43320,#43321,#43322,#43323,
#43324,#43325,#43326,#43327),.UNSPECIFIED.,.F.,.F.,(4,3,3,3,3,3,3,3,3,3,
3,3,3,3,3,3,3,3,3,3,3,3,3,3,3,3,3,3,3,3,3,3,4),(-0.569248610399399,-0.543574645887706,
-0.517272416441957,-0.510408710919313,-0.50480052039467,-0.477739691816766,
-0.455902626824495,-0.447185798618006,-0.442501671257752,-0.414772030968201,
-0.386610421128685,-0.358667819158644,-0.344761657338633,-0.340663036091181,
-0.336259738054214,-0.307329079232925,-0.3030431718786,-0.27522663544686,
-0.246781288661493,-0.236972581300584,-0.232129263502791,-0.228298636689681,
-0.199315265324891,-0.169757082759818,-0.139958578416395,-0.123701382742228,
-0.11872612058217,-0.114411165373038,-0.0838710232821164,-0.0532918814757283,
-0.023320643283923,-0.00990101302305864,0.),.UNSPECIFIED.);
#5928=B_SPLINE_CURVE_WITH_KNOTS('',3,(#43328,#43329,#43330,#43331,#43332,
#43333,#43334,#43335,#43336,#43337,#43338,#43339,#43340,#43341,#43342,#43343,
#43344,#43345,#43346,#43347,#43348,#43349,#43350,#43351,#43352,#43353,#43354,
#43355,#43356,#43357,#43358,#43359,#43360,#43361,#43362,#43363,#43364,#43365,
#43366,#43367,#43368,#43369,#43370,#43371,#43372,#43373,#43374,#43375,#43376,
#43377,#43378,#43379,#43380,#43381,#43382,#43383,#43384,#43385,#43386,#43387,
#43388,#43389,#43390,#43391,#43392,#43393,#43394,#43395,#43396,#43397,#43398,
#43399,#43400,#43401,#43402,#43403,#43404,#43405,#43406,#43407,#43408,#43409,
#43410,#43411,#43412,#43413,#43414,#43415,#43416,#43417,#43418,#43419,#43420,
#43421),.UNSPECIFIED.,.F.,.F.,(4,3,3,3,3,3,3,3,3,3,3,3,3,3,3,3,3,3,3,3,
3,3,3,3,3,3,3,3,3,3,3,4),(-0.566847306047971,-0.53666587364779,-0.506059968026337,
-0.497416424417392,-0.490479625055067,-0.460332813265244,-0.437094437432501,
-0.424724940231172,-0.420483374246613,-0.391058520491087,-0.361900342019141,
-0.333575724639118,-0.318788245130165,-0.313125879786658,-0.308695953827476,
-0.280705559915183,-0.274425806603304,-0.245949103194913,-0.216224272779601,
-0.204597317066248,-0.200878698444207,-0.173045197056922,-0.145277260918581,
-0.117980532340416,-0.104251773281916,-0.100006089570323,-0.095828408862559,
-0.0691557456961475,-0.0429305361237256,-0.0175053478877417,-0.0081504598724134,
0.),.UNSPECIFIED.);
#5929=B_SPLINE_CURVE_WITH_KNOTS('',3,(#43423,#43424,#43425,#43426,#43427,
#43428,#43429,#43430,#43431,#43432,#43433),.UNSPECIFIED.,.F.,.F.,(4,1,1,
1,1,1,1,1,4),(15.7079632679489,15.8286682231622,16.8210880633759,17.8135079035895,
18.8059277438031,19.7983475840168,20.7907674242304,21.783187264444,21.9911485751284),
 .UNSPECIFIED.);
#5930=B_SPLINE_CURVE_WITH_KNOTS('',3,(#43434,#43435,#43436,#43437,#43438,
#43439,#43440,#43441,#43442,#43443),.UNSPECIFIED.,.F.,.F.,(4,1,1,1,1,1,
1,4),(15.7079632679489,16.3832398073991,17.3756596476127,18.3680794878263,
19.36049932804,20.3529191682536,21.3453390084673,21.9911485751284),
 .UNSPECIFIED.);
#5931=B_SPLINE_CURVE_WITH_KNOTS('',3,(#43844,#43845,#43846,#43847,#43848,
#43849,#43850,#43851,#43852,#43853,#43854,#43855,#43856,#43857,#43858,#43859,
#43860,#43861,#43862,#43863,#43864,#43865,#43866,#43867,#43868,#43869,#43870,
#43871,#43872,#43873,#43874,#43875,#43876,#43877,#43878,#43879,#43880,#43881,
#43882,#43883,#43884,#43885,#43886,#43887,#43888,#43889,#43890,#43891,#43892,
#43893,#43894,#43895,#43896,#43897,#43898,#43899,#43900,#43901,#43902,#43903,
#43904,#43905,#43906,#43907,#43908,#43909,#43910,#43911,#43912,#43913,#43914,
#43915,#43916,#43917,#43918,#43919,#43920,#43921,#43922,#43923,#43924,#43925,
#43926,#43927,#43928,#43929,#43930,#43931,#43932,#43933,#43934,#43935,#43936,
#43937),.UNSPECIFIED.,.F.,.F.,(4,3,3,3,3,3,3,3,3,3,3,3,3,3,3,3,3,3,3,3,
3,3,3,3,3,3,3,3,3,3,3,4),(0.,0.0253630076180288,0.0513975877046809,0.0781461974825396,
0.0899194311896693,0.0966315930649138,0.102678021603326,0.129978474904837,
0.157730194774643,0.18464426256287,0.195932069023516,0.203012843388201,
0.20715665261236,0.236271559269955,0.26538646592755,0.293279280417395,0.302554895181128,
0.311292641824619,0.315704538622333,0.343817446040152,0.372959156505691,
0.402412706796253,0.413342529374516,0.4228990774176,0.428117895612503,0.458184942155295,
0.482885329773834,0.492048651182197,0.498170303933628,0.528680777336123,
0.556986492629451,0.566847306048124),.UNSPECIFIED.);
#5932=B_SPLINE_CURVE_WITH_KNOTS('',3,(#43938,#43939,#43940,#43941,#43942,
#43943,#43944,#43945,#43946,#43947,#43948,#43949,#43950,#43951,#43952,#43953,
#43954,#43955,#43956,#43957,#43958,#43959,#43960,#43961,#43962),
 .UNSPECIFIED.,.F.,.F.,(4,3,3,3,3,3,3,3,4),(-10.1321597128208,-9.92419840213634,
-8.93177856192271,-7.93935872170907,-6.94693888149544,-5.9545190412818,
-4.96209920106817,-3.96967936085453,-3.84897440564123),.UNSPECIFIED.);
#5933=B_SPLINE_CURVE_WITH_KNOTS('',3,(#44363,#44364,#44365,#44366,#44367,
#44368,#44369,#44370,#44371,#44372,#44373,#44374,#44375,#44376,#44377,#44378,
#44379,#44380,#44381,#44382,#44383,#44384),.UNSPECIFIED.,.F.,.F.,(4,3,3,
3,3,3,3,4),(7.59274844815659,7.93935872170907,8.9317785619227,9.92419840213634,
10.91661824235,11.9090380825636,12.9014579227772,13.8759337553361),
 .UNSPECIFIED.);
#5934=B_SPLINE_CURVE_WITH_KNOTS('',3,(#44385,#44386,#44387,#44388,#44389,
#44390,#44391,#44392,#44393,#44394,#44395,#44396,#44397,#44398,#44399,#44400,
#44401,#44402,#44403,#44404,#44405,#44406,#44407,#44408,#44409,#44410,#44411,
#44412,#44413,#44414,#44415,#44416,#44417,#44418,#44419,#44420,#44421,#44422,
#44423,#44424,#44425,#44426,#44427,#44428,#44429,#44430,#44431,#44432,#44433,
#44434,#44435,#44436,#44437,#44438,#44439,#44440,#44441,#44442,#44443,#44444,
#44445,#44446,#44447,#44448,#44449,#44450,#44451,#44452,#44453,#44454,#44455,
#44456,#44457,#44458,#44459,#44460,#44461,#44462,#44463,#44464,#44465,#44466,
#44467,#44468,#44469,#44470,#44471,#44472,#44473,#44474,#44475),
 .UNSPECIFIED.,.F.,.F.,(4,3,3,3,3,3,3,3,3,3,3,3,3,3,3,3,3,3,3,3,3,3,3,3,
3,3,3,3,3,3,4),(0.,0.0297241015280599,0.0601072589092367,0.089339530253816,
0.114917767680323,0.120626861021768,0.150385991078755,0.179981397219412,
0.208477405331027,0.220429498709529,0.228738535617177,0.234134414459521,
0.264049922062696,0.291955952722432,0.293965429665871,0.322911497915157,
0.339206043082875,0.343413983241414,0.371506227313122,0.399645180488026,
0.427381808130137,0.437705383100523,0.444698406356017,0.448877348536544,
0.476925686623981,0.497961940189559,0.506030881403263,0.51179113945871,
0.537728950453386,0.561070700886291,0.569248610399393),.UNSPECIFIED.);
#5935=B_SPLINE_CURVE_WITH_KNOTS('',3,(#44478,#44479,#44480,#44481,#44482,
#44483,#44484,#44485,#44486,#44487,#44488,#44489,#44490,#44491,#44492,#44493,
#44494,#44495,#44496,#44497,#44498,#44499,#44500,#44501,#44502,#44503,#44504,
#44505,#44506,#44507,#44508,#44509,#44510,#44511,#44512,#44513,#44514,#44515,
#44516,#44517,#44518,#44519,#44520,#44521,#44522,#44523,#44524,#44525,#44526,
#44527,#44528,#44529,#44530,#44531,#44532,#44533,#44534,#44535,#44536,#44537,
#44538,#44539,#44540,#44541,#44542,#44543,#44544,#44545,#44546,#44547,#44548,
#44549,#44550,#44551,#44552,#44553,#44554,#44555,#44556,#44557,#44558,#44559,
#44560,#44561,#44562,#44563,#44564,#44565,#44566,#44567,#44568,#44569,#44570,
#44571,#44572,#44573,#44574),.UNSPECIFIED.,.F.,.F.,(4,3,3,3,3,3,3,3,3,3,
3,3,3,3,3,3,3,3,3,3,3,3,3,3,3,3,3,3,3,3,3,3,4),(-0.569248610399393,-0.543574674480804,
-0.517272469051126,-0.510408841912501,-0.504800525129289,-0.477739716670525,
-0.455902648571535,-0.447186002233845,-0.442501828177038,-0.414772209830522,
-0.386610599542292,-0.358667985965373,-0.344761782443679,-0.340663244529424,
-0.336259792696339,-0.30732913293683,-0.303043171878598,-0.275226617339747,
-0.246781259091957,-0.236972491194407,-0.232129113765856,-0.228298489515272,
-0.199315100266808,-0.169756908209147,-0.139958402689496,-0.123701228981192,
-0.118725698812402,-0.114410751166567,-0.0838706032234413,-0.0532914639090378,
-0.0233202292854336,-0.00990101302306306,0.),.UNSPECIFIED.);
#5936=B_SPLINE_CURVE_WITH_KNOTS('',3,(#44575,#44576,#44577,#44578,#44579,
#44580,#44581,#44582,#44583,#44584,#44585,#44586,#44587,#44588,#44589,#44590,
#44591,#44592,#44593,#44594,#44595,#44596,#44597,#44598,#44599,#44600,#44601,
#44602,#44603,#44604,#44605,#44606,#44607,#44608,#44609,#44610,#44611,#44612,
#44613,#44614,#44615,#44616,#44617,#44618,#44619,#44620,#44621,#44622,#44623,
#44624,#44625,#44626,#44627,#44628,#44629,#44630,#44631,#44632,#44633,#44634,
#44635,#44636,#44637,#44638,#44639,#44640,#44641,#44642,#44643,#44644,#44645,
#44646,#44647,#44648,#44649,#44650,#44651,#44652,#44653,#44654,#44655,#44656,
#44657,#44658,#44659,#44660,#44661,#44662,#44663,#44664,#44665,#44666,#44667,
#44668),.UNSPECIFIED.,.F.,.F.,(4,3,3,3,3,3,3,3,3,3,3,3,3,3,3,3,3,3,3,3,
3,3,3,3,3,3,3,3,3,3,3,4),(-0.566847306048015,-0.536665868221327,-0.506059961122649,
-0.497416415953207,-0.490479623350436,-0.460332811693897,-0.437094436057574,
-0.424724937050165,-0.42048337099133,-0.391058517828774,-0.361900340022409,
-0.333575724459701,-0.318788244995605,-0.313125878209896,-0.308695953223835,
-0.280705561460601,-0.274425806603314,-0.245949103343717,-0.216224272909805,
-0.204597316755682,-0.20087869834534,-0.173045196570911,-0.145277260583828,
-0.117980533828581,-0.10425177458406,-0.100006094404146,-0.0958284101891435,
-0.0691557481657235,-0.0429305412409989,-0.0175053576029524,-0.00815045987241369,
0.),.UNSPECIFIED.);
#5937=B_SPLINE_CURVE_WITH_KNOTS('',3,(#44670,#44671,#44672,#44673,#44674,
#44675,#44676,#44677,#44678,#44679,#44680),.UNSPECIFIED.,.F.,.F.,(4,1,1,
1,1,1,1,1,4),(15.7079632679489,15.8286682231624,16.821088063376,17.8135079035896,
18.8059277438032,19.7983475840169,20.7907674242305,21.7831872644441,21.9911485751285),
 .UNSPECIFIED.);
#5938=B_SPLINE_CURVE_WITH_KNOTS('',3,(#44681,#44682,#44683,#44684,#44685,
#44686,#44687,#44688,#44689,#44690),.UNSPECIFIED.,.F.,.F.,(4,1,1,1,1,1,
1,4),(15.7079632679489,16.3832398073992,17.3756596476128,18.3680794878265,
19.3604993280401,20.3529191682537,21.3453390084674,21.9911485751284),
 .UNSPECIFIED.);
#5939=B_SPLINE_CURVE_WITH_KNOTS('',3,(#45091,#45092,#45093,#45094,#45095,
#45096,#45097,#45098,#45099,#45100,#45101,#45102,#45103,#45104,#45105,#45106,
#45107,#45108,#45109,#45110,#45111,#45112,#45113,#45114,#45115,#45116,#45117,
#45118,#45119,#45120,#45121,#45122,#45123,#45124,#45125,#45126,#45127,#45128,
#45129,#45130,#45131,#45132,#45133,#45134,#45135,#45136,#45137,#45138,#45139,
#45140,#45141,#45142,#45143,#45144,#45145,#45146,#45147,#45148,#45149,#45150,
#45151,#45152,#45153,#45154,#45155,#45156,#45157,#45158,#45159,#45160,#45161,
#45162,#45163,#45164,#45165,#45166,#45167,#45168,#45169,#45170,#45171,#45172,
#45173,#45174,#45175,#45176,#45177,#45178,#45179,#45180,#45181,#45182,#45183,
#45184),.UNSPECIFIED.,.F.,.F.,(4,3,3,3,3,3,3,3,3,3,3,3,3,3,3,3,3,3,3,3,
3,3,3,3,3,3,3,3,3,3,3,4),(0.,0.0253630162810394,0.0513976042172585,0.078146211931042,
0.0899194345617105,0.0966315935064485,0.102678021607179,0.129978481016302,
0.157730203957742,0.184644269450188,0.195932070537851,0.203012844021181,
0.207156653941548,0.236271559934537,0.265386465927526,0.293279276361684,
0.302554886851352,0.31129260608518,0.315704531791299,0.343817433364416,
0.372959141111239,0.402412690720333,0.41334249920042,0.422898961216315,
0.428117885617758,0.458184930864427,0.482885321305682,0.492048630602995,
0.498170305601047,0.528680779114337,0.556986492629444,0.566847306048072),
 .UNSPECIFIED.);
#5940=B_SPLINE_CURVE_WITH_KNOTS('',3,(#45185,#45186,#45187,#45188,#45189,
#45190,#45191,#45192,#45193,#45194,#45195,#45196,#45197,#45198,#45199,#45200,
#45201,#45202,#45203,#45204,#45205,#45206,#45207,#45208,#45209),
 .UNSPECIFIED.,.F.,.F.,(4,3,3,3,3,3,3,3,4),(-10.1321597128207,-9.92419840213633,
-8.93177856192269,-7.93935872170906,-6.94693888149543,-5.9545190412818,
-4.96209920106816,-3.96967936085453,-3.848974405641),.UNSPECIFIED.);
#5941=B_SPLINE_CURVE_WITH_KNOTS('',3,(#45610,#45611,#45612,#45613,#45614,
#45615,#45616,#45617,#45618,#45619,#45620,#45621,#45622,#45623,#45624,#45625,
#45626,#45627,#45628,#45629,#45630,#45631),.UNSPECIFIED.,.F.,.F.,(4,3,3,
3,3,3,3,4),(7.59274844815647,7.93935872170906,8.93177856192269,9.92419840213633,
10.91661824235,11.9090380825636,12.9014579227772,13.875933755336),
 .UNSPECIFIED.);
#5942=B_SPLINE_CURVE_WITH_KNOTS('',3,(#45632,#45633,#45634,#45635,#45636,
#45637,#45638,#45639,#45640,#45641,#45642,#45643,#45644,#45645,#45646,#45647,
#45648,#45649,#45650,#45651,#45652,#45653,#45654,#45655,#45656,#45657,#45658,
#45659,#45660,#45661,#45662,#45663,#45664,#45665,#45666,#45667,#45668,#45669,
#45670,#45671,#45672,#45673,#45674,#45675,#45676,#45677,#45678,#45679,#45680,
#45681,#45682,#45683,#45684,#45685,#45686,#45687,#45688,#45689,#45690,#45691,
#45692,#45693,#45694,#45695,#45696,#45697,#45698,#45699,#45700,#45701,#45702,
#45703,#45704,#45705,#45706,#45707,#45708,#45709,#45710,#45711,#45712,#45713,
#45714,#45715,#45716,#45717,#45718,#45719,#45720,#45721,#45722),
 .UNSPECIFIED.,.F.,.F.,(4,3,3,3,3,3,3,3,3,3,3,3,3,3,3,3,3,3,3,3,3,3,3,3,
3,3,3,3,3,3,4),(0.,0.0297240764494745,0.0601072212620576,0.0893394973125421,
0.114917738856716,0.120626859131278,0.150385988643545,0.179981401276396,
0.20847740837378,0.220429505923984,0.228738554654763,0.234134418137665,
0.264049923901799,0.291955960666471,0.293965429665934,0.322911496593631,
0.339206045811635,0.343413985730059,0.371506228953445,0.399645181615295,
0.427381813866647,0.437705397278763,0.44469853997657,0.448877487839921,
0.47692579110155,0.497962018547772,0.506031026512302,0.511791114109563,
0.537728937371717,0.561070700886438,0.569248610399523),.UNSPECIFIED.);
#5943=B_SPLINE_CURVE_WITH_KNOTS('',3,(#45725,#45726,#45727,#45728,#45729,
#45730,#45731,#45732,#45733,#45734,#45735,#45736,#45737,#45738,#45739,#45740,
#45741,#45742,#45743,#45744,#45745,#45746,#45747,#45748,#45749,#45750,#45751,
#45752,#45753,#45754,#45755,#45756,#45757,#45758,#45759,#45760,#45761,#45762,
#45763,#45764,#45765,#45766,#45767,#45768,#45769,#45770,#45771,#45772,#45773,
#45774,#45775,#45776,#45777,#45778,#45779,#45780,#45781,#45782,#45783,#45784,
#45785,#45786,#45787,#45788,#45789,#45790,#45791,#45792,#45793,#45794,#45795,
#45796,#45797,#45798,#45799,#45800,#45801,#45802,#45803,#45804,#45805,#45806,
#45807,#45808,#45809,#45810,#45811,#45812,#45813,#45814,#45815,#45816,#45817,
#45818,#45819,#45820,#45821),.UNSPECIFIED.,.F.,.F.,(4,3,3,3,3,3,3,3,3,3,
3,3,3,3,3,3,3,3,3,3,3,3,3,3,3,3,3,3,3,3,3,3,4),(-0.569248610399377,-0.54357467448165,
-0.517272469053758,-0.510408841918492,-0.50480052502851,-0.477739716567738,
-0.455902648481596,-0.447186001443042,-0.44250182771911,-0.414772209355928,
-0.386610599068325,-0.358667985497239,-0.34476178209258,-0.340663244000883,
-0.336259792559757,-0.30732913279944,-0.303043171878604,-0.2752266173411,
-0.246781259100878,-0.236972491217739,-0.232129113745793,-0.228298489561011,
-0.199315100312039,-0.169756908254245,-0.139958402733899,-0.123701229020045,
-0.118725698872309,-0.114410751243681,-0.083870603296885,-0.0532914639826537,
-0.0233202293554824,-0.00990101302306316,0.),.UNSPECIFIED.);
#5944=B_SPLINE_CURVE_WITH_KNOTS('',3,(#45822,#45823,#45824,#45825,#45826,
#45827,#45828,#45829,#45830,#45831,#45832,#45833,#45834,#45835,#45836,#45837,
#45838,#45839,#45840,#45841,#45842,#45843,#45844,#45845,#45846,#45847,#45848,
#45849,#45850,#45851,#45852,#45853,#45854,#45855,#45856,#45857,#45858,#45859,
#45860,#45861,#45862,#45863,#45864,#45865,#45866,#45867,#45868,#45869,#45870,
#45871,#45872,#45873,#45874,#45875,#45876,#45877,#45878,#45879,#45880,#45881,
#45882,#45883,#45884,#45885,#45886,#45887,#45888,#45889,#45890,#45891,#45892,
#45893,#45894,#45895,#45896,#45897,#45898,#45899,#45900,#45901,#45902,#45903,
#45904,#45905,#45906,#45907,#45908,#45909,#45910,#45911,#45912,#45913,#45914,
#45915),.UNSPECIFIED.,.F.,.F.,(4,3,3,3,3,3,3,3,3,3,3,3,3,3,3,3,3,3,3,3,
3,3,3,3,3,3,3,3,3,3,3,4),(-0.566847306047991,-0.53666586821921,-0.506059961126055,
-0.497416415953077,-0.49047962338091,-0.460332811721525,-0.43709443608175,
-0.424724937095777,-0.420483370923851,-0.391058517764092,-0.3619003399739,
-0.333575724413931,-0.318788244961279,-0.31312587811604,-0.308695953184524,
-0.280705561426923,-0.274425806603322,-0.245949103340888,-0.216224272907329,
-0.204597316758108,-0.200878698422677,-0.17304519665064,-0.145277260663322,
-0.117980533917273,-0.104251774661665,-0.100006094574606,-0.0958284102179013,
-0.0691557481942624,-0.0429305412697575,-0.0175053576280775,-0.00815045987241409,
0.),.UNSPECIFIED.);
#5945=B_SPLINE_CURVE_WITH_KNOTS('',3,(#45917,#45918,#45919,#45920,#45921,
#45922,#45923,#45924,#45925,#45926,#45927),.UNSPECIFIED.,.F.,.F.,(4,1,1,
1,1,1,1,1,4),(15.7079632679488,15.8286682231622,16.8210880633759,17.8135079035895,
18.8059277438031,19.7983475840168,20.7907674242304,21.783187264444,21.9911485751285),
 .UNSPECIFIED.);
#5946=B_SPLINE_CURVE_WITH_KNOTS('',3,(#45928,#45929,#45930,#45931,#45932,
#45933,#45934,#45935,#45936,#45937),.UNSPECIFIED.,.F.,.F.,(4,1,1,1,1,1,
1,4),(15.7079632679489,16.3832398073991,17.3756596476127,18.3680794878263,
19.36049932804,20.3529191682536,21.3453390084673,21.9911485751284),
 .UNSPECIFIED.);
#5947=B_SPLINE_CURVE_WITH_KNOTS('',3,(#46338,#46339,#46340,#46341,#46342,
#46343,#46344,#46345,#46346,#46347,#46348,#46349,#46350,#46351,#46352,#46353,
#46354,#46355,#46356,#46357,#46358,#46359,#46360,#46361,#46362,#46363,#46364,
#46365,#46366,#46367,#46368,#46369,#46370,#46371,#46372,#46373,#46374,#46375,
#46376,#46377,#46378,#46379,#46380,#46381,#46382,#46383,#46384,#46385,#46386,
#46387,#46388,#46389,#46390,#46391,#46392,#46393,#46394,#46395,#46396,#46397,
#46398,#46399,#46400,#46401,#46402,#46403,#46404,#46405,#46406,#46407,#46408,
#46409,#46410,#46411,#46412,#46413,#46414,#46415,#46416,#46417,#46418,#46419,
#46420,#46421,#46422,#46423,#46424,#46425,#46426,#46427,#46428,#46429,#46430,
#46431),.UNSPECIFIED.,.F.,.F.,(4,3,3,3,3,3,3,3,3,3,3,3,3,3,3,3,3,3,3,3,
3,3,3,3,3,3,3,3,3,3,3,4),(0.,0.0253630162801341,0.051397604216831,0.0781462119306684,
0.0899194345617906,0.0966315935064221,0.102678021611154,0.129978481020733,
0.157730203962062,0.184644269453429,0.195932070538785,0.20301284402031,
0.207156653926934,0.236271559927232,0.26538646592753,0.293279276361627,
0.302554886851072,0.311292606084599,0.315704531791214,0.343817433364128,
0.372959141111098,0.402412690720469,0.413342499200516,0.422898961216301,
0.428117885617808,0.458184930864438,0.482885321305687,0.49204863060229,
0.498170305654284,0.528680779169399,0.556986492629434,0.566847306048108),
 .UNSPECIFIED.);
#5948=B_SPLINE_CURVE_WITH_KNOTS('',3,(#46432,#46433,#46434,#46435,#46436,
#46437,#46438,#46439,#46440,#46441,#46442,#46443,#46444,#46445,#46446,#46447,
#46448,#46449,#46450,#46451,#46452,#46453,#46454,#46455,#46456),
 .UNSPECIFIED.,.F.,.F.,(4,3,3,3,3,3,3,3,4),(-10.1321597128208,-9.92419840213633,
-8.9317785619227,-7.93935872170907,-6.94693888149544,-5.9545190412818,-4.96209920106817,
-3.96967936085453,-3.84897440564123),.UNSPECIFIED.);
#5949=B_SPLINE_CURVE_WITH_KNOTS('',3,(#46857,#46858,#46859,#46860,#46861,
#46862,#46863,#46864,#46865,#46866,#46867,#46868,#46869,#46870,#46871,#46872,
#46873,#46874,#46875,#46876,#46877,#46878),.UNSPECIFIED.,.F.,.F.,(4,3,3,
3,3,3,3,4),(7.59274844815659,7.93935872170907,8.9317785619227,9.92419840213634,
10.91661824235,11.9090380825636,12.9014579227772,13.8759337553361),
 .UNSPECIFIED.);
#5950=B_SPLINE_CURVE_WITH_KNOTS('',3,(#46879,#46880,#46881,#46882,#46883,
#46884,#46885,#46886,#46887,#46888,#46889,#46890,#46891,#46892,#46893,#46894,
#46895,#46896,#46897,#46898,#46899,#46900,#46901,#46902,#46903,#46904,#46905,
#46906,#46907,#46908,#46909,#46910,#46911,#46912,#46913,#46914,#46915,#46916,
#46917,#46918,#46919,#46920,#46921,#46922,#46923,#46924,#46925,#46926,#46927,
#46928,#46929,#46930,#46931,#46932,#46933,#46934,#46935,#46936,#46937,#46938,
#46939,#46940,#46941,#46942,#46943,#46944,#46945,#46946,#46947,#46948,#46949,
#46950,#46951,#46952,#46953,#46954,#46955,#46956,#46957,#46958,#46959,#46960,
#46961,#46962,#46963,#46964,#46965,#46966,#46967,#46968,#46969),
 .UNSPECIFIED.,.F.,.F.,(4,3,3,3,3,3,3,3,3,3,3,3,3,3,3,3,3,3,3,3,3,3,3,3,
3,3,3,3,3,3,4),(0.,0.029724076449364,0.0601072212623451,0.0893394973127924,
0.114917738856934,0.120626859134211,0.150385988646724,0.179981401279999,
0.20847740837648,0.220429505928215,0.228738554666963,0.234134418130225,
0.264049923898074,0.291955960662473,0.293965429665923,0.322911496595274,
0.339206045815667,0.34341398573459,0.371506228958071,0.399645181620042,
0.427381813870245,0.43770539728599,0.444698540053498,0.448877487941438,
0.476925791177684,0.497962018604869,0.506031026616555,0.511791114086853,
0.537728937350807,0.561070700886424,0.569248610399524),.UNSPECIFIED.);
#5951=B_SPLINE_CURVE_WITH_KNOTS('',3,(#46972,#46973,#46974,#46975,#46976,
#46977,#46978,#46979,#46980,#46981,#46982,#46983,#46984,#46985,#46986,#46987,
#46988,#46989,#46990,#46991,#46992,#46993,#46994,#46995,#46996,#46997,#46998,
#46999,#47000,#47001,#47002,#47003,#47004,#47005,#47006,#47007,#47008,#47009,
#47010,#47011,#47012,#47013,#47014,#47015,#47016,#47017,#47018,#47019,#47020,
#47021,#47022,#47023,#47024,#47025,#47026,#47027,#47028,#47029,#47030,#47031,
#47032,#47033,#47034,#47035,#47036,#47037,#47038,#47039,#47040,#47041,#47042,
#47043,#47044,#47045,#47046,#47047,#47048,#47049,#47050,#47051,#47052,#47053,
#47054,#47055,#47056,#47057,#47058,#47059,#47060,#47061,#47062,#47063,#47064,
#47065,#47066,#47067,#47068),.UNSPECIFIED.,.F.,.F.,(4,3,3,3,3,3,3,3,3,3,
3,3,3,3,3,3,3,3,3,3,3,3,3,3,3,3,3,3,3,3,3,3,4),(-0.569248610399425,-0.543574656378576,
-0.517272435738008,-0.510408758966565,-0.504800522056745,-0.477739700856869,
-0.45590263473459,-0.447185872707102,-0.44250172837546,-0.414772096122201,
-0.386610486117207,-0.358667879895409,-0.344761702891216,-0.340663112078979,
-0.336259757977141,-0.307329098806346,-0.303043171878636,-0.275226628804691,
-0.246781277807599,-0.236972548226137,-0.232129208542884,-0.228298582742164,
-0.199315204818196,-0.169757018770865,-0.13995851399337,-0.123701326372081,
-0.118725966008134,-0.114411013541681,-0.0838708693004695,-0.0532917284052035,
-0.0233204915173235,-0.0099010130230586,0.),.UNSPECIFIED.);
#5952=B_SPLINE_CURVE_WITH_KNOTS('',3,(#47069,#47070,#47071,#47072,#47073,
#47074,#47075,#47076,#47077,#47078,#47079,#47080,#47081,#47082,#47083,#47084,
#47085,#47086,#47087,#47088,#47089,#47090,#47091,#47092,#47093,#47094,#47095,
#47096,#47097,#47098,#47099,#47100,#47101,#47102,#47103,#47104,#47105,#47106,
#47107,#47108,#47109,#47110,#47111,#47112,#47113,#47114,#47115,#47116,#47117,
#47118,#47119,#47120,#47121,#47122,#47123,#47124,#47125,#47126,#47127,#47128,
#47129,#47130,#47131,#47132,#47133,#47134,#47135,#47136,#47137,#47138,#47139,
#47140,#47141,#47142,#47143,#47144,#47145,#47146,#47147,#47148,#47149,#47150,
#47151,#47152,#47153,#47154,#47155,#47156,#47157,#47158,#47159,#47160,#47161,
#47162),.UNSPECIFIED.,.F.,.F.,(4,3,3,3,3,3,3,3,3,3,3,3,3,3,3,3,3,3,3,3,
3,3,3,3,3,3,3,3,3,3,3,4),(-0.566847306048015,-0.536665878440076,-0.50605997412493,
-0.497416431897616,-0.490479626448282,-0.460332814543148,-0.437094438550669,
-0.424724942866698,-0.420483377128068,-0.391058522848951,-0.361900343787542,
-0.333575724793978,-0.318788245246312,-0.313125881168901,-0.308695954326937,
-0.280705558504757,-0.274425806603314,-0.245949103059473,-0.21622427266109,
-0.204597317336048,-0.200878698329781,-0.173045197282773,-0.145277261013689,
-0.117980530827865,-0.104251771958434,-0.100006084890927,-0.0958284076234192,
-0.0691557434471268,-0.042930531532881,-0.017505339237663,-0.00815045987241369,
0.),.UNSPECIFIED.);
#5953=B_SPLINE_CURVE_WITH_KNOTS('',3,(#47164,#47165,#47166,#47167,#47168,
#47169,#47170,#47171,#47172,#47173,#47174),.UNSPECIFIED.,.F.,.F.,(4,1,1,
1,1,1,1,1,4),(15.7079632679489,15.8286682231624,16.821088063376,17.8135079035896,
18.8059277438032,19.7983475840169,20.7907674242305,21.7831872644441,21.9911485751285),
 .UNSPECIFIED.);
#5954=B_SPLINE_CURVE_WITH_KNOTS('',3,(#47175,#47176,#47177,#47178,#47179,
#47180,#47181,#47182,#47183,#47184),.UNSPECIFIED.,.F.,.F.,(4,1,1,1,1,1,
1,4),(15.7079632679489,16.3832398073992,17.3756596476128,18.3680794878265,
19.3604993280401,20.3529191682537,21.3453390084674,21.9911485751284),
 .UNSPECIFIED.);
#5955=B_SPLINE_CURVE_WITH_KNOTS('',3,(#47585,#47586,#47587,#47588,#47589,
#47590,#47591,#47592,#47593,#47594,#47595,#47596,#47597,#47598,#47599,#47600,
#47601,#47602,#47603,#47604,#47605,#47606,#47607,#47608,#47609,#47610,#47611,
#47612,#47613,#47614,#47615,#47616,#47617,#47618,#47619,#47620,#47621,#47622,
#47623,#47624,#47625,#47626,#47627,#47628,#47629,#47630,#47631,#47632,#47633,
#47634,#47635,#47636,#47637,#47638,#47639,#47640,#47641,#47642,#47643,#47644,
#47645,#47646,#47647,#47648,#47649,#47650,#47651,#47652,#47653,#47654,#47655,
#47656,#47657,#47658,#47659,#47660,#47661,#47662,#47663,#47664,#47665,#47666,
#47667,#47668,#47669,#47670,#47671,#47672,#47673,#47674,#47675,#47676,#47677,
#47678),.UNSPECIFIED.,.F.,.F.,(4,3,3,3,3,3,3,3,3,3,3,3,3,3,3,3,3,3,3,3,
3,3,3,3,3,3,3,3,3,3,3,4),(0.,0.0253629999646348,0.0513975731150082,0.078146184716573,
0.0899194282101026,0.0966315926743291,0.102678021610072,0.129978469516054,
0.157730186671017,0.184644256485144,0.195932067687582,0.203012842825234,
0.207156651488905,0.236271558708216,0.265386465927526,0.293279283999271,
0.30255490253839,0.311292673391874,0.315704544656251,0.34381745723653,0.372959170103633,
0.402412720995891,0.413342556026173,0.422899180057392,0.428117904444282,
0.458184952131496,0.482885337255983,0.492048669366015,0.498170302461157,
0.528680775761109,0.556986492629444,0.566847306048072),.UNSPECIFIED.);
#5956=B_SPLINE_CURVE_WITH_KNOTS('',3,(#47679,#47680,#47681,#47682,#47683,
#47684,#47685,#47686,#47687,#47688,#47689,#47690,#47691,#47692,#47693,#47694,
#47695,#47696,#47697,#47698,#47699,#47700,#47701,#47702,#47703),
 .UNSPECIFIED.,.F.,.F.,(4,3,3,3,3,3,3,3,4),(-10.1321597128207,-9.92419840213633,
-8.93177856192269,-7.93935872170906,-6.94693888149543,-5.9545190412818,
-4.96209920106816,-3.96967936085453,-3.848974405641),.UNSPECIFIED.);
#5957=B_SPLINE_CURVE_WITH_KNOTS('',3,(#48104,#48105,#48106,#48107,#48108,
#48109,#48110,#48111,#48112,#48113,#48114,#48115,#48116,#48117,#48118,#48119,
#48120,#48121,#48122,#48123,#48124,#48125),.UNSPECIFIED.,.F.,.F.,(4,3,3,
3,3,3,3,4),(7.59274844815647,7.93935872170906,8.93177856192269,9.92419840213633,
10.91661824235,11.9090380825636,12.9014579227772,13.875933755336),
 .UNSPECIFIED.);
#5958=B_SPLINE_CURVE_WITH_KNOTS('',3,(#48126,#48127,#48128,#48129,#48130,
#48131,#48132,#48133,#48134,#48135,#48136,#48137,#48138,#48139,#48140,#48141,
#48142,#48143,#48144,#48145,#48146,#48147,#48148,#48149,#48150,#48151,#48152,
#48153,#48154,#48155,#48156,#48157,#48158,#48159,#48160,#48161,#48162,#48163,
#48164,#48165,#48166,#48167,#48168,#48169,#48170,#48171,#48172,#48173,#48174,
#48175,#48176,#48177,#48178,#48179,#48180,#48181,#48182,#48183,#48184,#48185,
#48186,#48187,#48188,#48189,#48190,#48191,#48192,#48193,#48194,#48195,#48196,
#48197,#48198,#48199,#48200,#48201,#48202,#48203,#48204,#48205,#48206,#48207,
#48208,#48209,#48210,#48211,#48212,#48213,#48214,#48215,#48216),
 .UNSPECIFIED.,.F.,.F.,(4,3,3,3,3,3,3,3,3,3,3,3,3,3,3,3,3,3,3,3,3,3,3,3,
3,3,3,3,3,3,4),(0.,0.0297240923307022,0.0601072451031547,0.0893395181734978,
0.114917757110048,0.120626860335535,0.150385990192878,0.179981398714595,
0.208477406452421,0.220429501364369,0.228738542625386,0.234134415814125,
0.264049922740012,0.29195595563805,0.293965429665899,0.32291149743097,0.339206044085149,
0.343413984151255,0.371506227912012,0.399645180899159,0.427381810232926,
0.437705388298364,0.444698455347404,0.448877399571227,0.476925724900021,
0.497961968896616,0.506030934564902,0.51179113018769,0.537728945681625,
0.561070700886401,0.569248610399486),.UNSPECIFIED.);
#5959=B_SPLINE_CURVE_WITH_KNOTS('',3,(#48219,#48220,#48221,#48222,#48223,
#48224,#48225,#48226,#48227,#48228,#48229,#48230,#48231,#48232,#48233,#48234,
#48235,#48236,#48237,#48238,#48239,#48240,#48241,#48242,#48243,#48244,#48245,
#48246,#48247,#48248,#48249,#48250,#48251,#48252,#48253,#48254,#48255,#48256,
#48257,#48258,#48259,#48260,#48261,#48262,#48263,#48264,#48265,#48266,#48267,
#48268,#48269,#48270,#48271,#48272,#48273,#48274,#48275,#48276,#48277,#48278,
#48279,#48280,#48281,#48282,#48283,#48284,#48285,#48286,#48287,#48288,#48289,
#48290,#48291,#48292,#48293,#48294,#48295,#48296,#48297,#48298,#48299,#48300,
#48301,#48302,#48303,#48304,#48305,#48306,#48307,#48308,#48309,#48310,#48311,
#48312,#48313,#48314,#48315),.UNSPECIFIED.,.F.,.F.,(4,3,3,3,3,3,3,3,3,3,
3,3,3,3,3,3,3,3,3,3,3,3,3,3,3,3,3,3,3,3,3,3,4),(-0.569248610399326,-0.543574656371614,
-0.517272435735161,-0.510408758961596,-0.504800521992165,-0.477739700790141,
-0.455902634676197,-0.447185872187875,-0.442501727990217,-0.414772095728046,
-0.386610485723793,-0.358667879508254,-0.344761702600837,-0.340663111536621,
-0.336259757837447,-0.30732909867532,-0.303043171878586,-0.275226628803054,
-0.246781277807813,-0.236972548227735,-0.232129208596512,-0.22829858282377,
-0.199315204899583,-0.169757018852598,-0.139958514082241,-0.123701326449843,
-0.11872596618965,-0.114411013673191,-0.0838708694366423,-0.0532917285417125,
-0.0233204916530961,-0.0099010130230633,0.),.UNSPECIFIED.);
#5960=B_SPLINE_CURVE_WITH_KNOTS('',3,(#48316,#48317,#48318,#48319,#48320,
#48321,#48322,#48323,#48324,#48325,#48326,#48327,#48328,#48329,#48330,#48331,
#48332,#48333,#48334,#48335,#48336,#48337,#48338,#48339,#48340,#48341,#48342,
#48343,#48344,#48345,#48346,#48347,#48348,#48349,#48350,#48351,#48352,#48353,
#48354,#48355,#48356,#48357,#48358,#48359,#48360,#48361,#48362,#48363,#48364,
#48365,#48366,#48367,#48368,#48369,#48370,#48371,#48372,#48373,#48374,#48375,
#48376,#48377,#48378,#48379,#48380,#48381,#48382,#48383,#48384,#48385,#48386,
#48387,#48388,#48389,#48390,#48391,#48392,#48393,#48394,#48395,#48396,#48397,
#48398,#48399,#48400,#48401,#48402,#48403,#48404,#48405,#48406,#48407,#48408,
#48409),.UNSPECIFIED.,.F.,.F.,(4,3,3,3,3,3,3,3,3,3,3,3,3,3,3,3,3,3,3,3,
3,3,3,3,3,3,3,3,3,3,3,4),(-0.566847306048114,-0.536665878440344,-0.506059974122399,
-0.497416431894722,-0.490479626354958,-0.460332814450562,-0.437094438469659,
-0.424724942717478,-0.420483376948718,-0.391058522671577,-0.361900343654519,
-0.333575724664248,-0.318788245149022,-0.313125880904265,-0.308695954272495,
-0.280705558454138,-0.274425806603343,-0.245949103055171,-0.216224272657327,
-0.204597317339409,-0.200878698484612,-0.173045197439613,-0.145277261167582,
-0.117980530976068,-0.104251772088112,-0.100006085217883,-0.0958284076765524,
-0.0691557434985927,-0.0429305315826143,-0.0175053392821834,-0.00815045987241368,
0.),.UNSPECIFIED.);
#5961=B_SPLINE_CURVE_WITH_KNOTS('',3,(#48411,#48412,#48413,#48414,#48415,
#48416,#48417,#48418,#48419,#48420,#48421),.UNSPECIFIED.,.F.,.F.,(4,1,1,
1,1,1,1,1,4),(15.7079632679489,15.8286682231622,16.8210880633759,17.8135079035895,
18.8059277438031,19.7983475840168,20.7907674242304,21.783187264444,21.9911485751285),
 .UNSPECIFIED.);
#5962=B_SPLINE_CURVE_WITH_KNOTS('',3,(#48422,#48423,#48424,#48425,#48426,
#48427,#48428,#48429,#48430,#48431),.UNSPECIFIED.,.F.,.F.,(4,1,1,1,1,1,
1,4),(15.7079632679489,16.3832398073991,17.3756596476127,18.3680794878263,
19.36049932804,20.3529191682536,21.3453390084673,21.9911485751284),
 .UNSPECIFIED.);
#5963=B_SPLINE_CURVE_WITH_KNOTS('',3,(#48832,#48833,#48834,#48835,#48836,
#48837,#48838,#48839,#48840,#48841,#48842,#48843,#48844,#48845,#48846,#48847,
#48848,#48849,#48850,#48851,#48852,#48853,#48854,#48855,#48856,#48857,#48858,
#48859,#48860,#48861,#48862,#48863,#48864,#48865,#48866,#48867,#48868,#48869,
#48870,#48871,#48872,#48873,#48874,#48875,#48876,#48877,#48878,#48879,#48880,
#48881,#48882,#48883,#48884,#48885,#48886,#48887,#48888,#48889,#48890,#48891,
#48892,#48893,#48894,#48895,#48896,#48897,#48898,#48899,#48900,#48901,#48902,
#48903,#48904,#48905,#48906,#48907,#48908,#48909,#48910,#48911,#48912,#48913,
#48914,#48915,#48916,#48917,#48918,#48919,#48920,#48921,#48922,#48923,#48924,
#48925),.UNSPECIFIED.,.F.,.F.,(4,3,3,3,3,3,3,3,3,3,3,3,3,3,3,3,3,3,3,3,
3,3,3,3,3,3,3,3,3,3,3,4),(0.,0.0253629999638193,0.0513975731141745,0.0781461847158463,
0.0899194282101058,0.0966315926746491,0.102678021599935,0.129978469505849,
0.157730186661174,0.184644256477768,0.19593206768551,0.203012842827579,
0.207156651488323,0.236271558707936,0.265386465927549,0.293279283999287,
0.302554902538345,0.311292673391422,0.315704544656186,0.343817457237586,
0.372959170104838,0.402412720997358,0.413342556028948,0.422899180067306,
0.428117904445187,0.45818495213231,0.482885337256607,0.492048669366648,
0.498170302461362,0.528680775763151,0.5569864926295,0.566847306048176),
 .UNSPECIFIED.);
#5964=B_SPLINE_CURVE_WITH_KNOTS('',3,(#48926,#48927,#48928,#48929,#48930,
#48931,#48932,#48933,#48934,#48935,#48936,#48937,#48938,#48939,#48940,#48941,
#48942,#48943,#48944,#48945,#48946,#48947,#48948,#48949,#48950),
 .UNSPECIFIED.,.F.,.F.,(4,3,3,3,3,3,3,3,4),(-10.1321597128207,-9.92419840213634,
-8.93177856192271,-7.93935872170907,-6.94693888149544,-5.9545190412818,
-4.96209920106817,-3.96967936085453,-3.84897440564112),.UNSPECIFIED.);
#5965=B_SPLINE_CURVE_WITH_KNOTS('',3,(#49351,#49352,#49353,#49354,#49355,
#49356,#49357,#49358,#49359,#49360,#49361,#49362,#49363,#49364,#49365,#49366,
#49367,#49368,#49369,#49370,#49371,#49372),.UNSPECIFIED.,.F.,.F.,(4,3,3,
3,3,3,3,4),(7.59274844815659,7.93935872170907,8.93177856192271,9.92419840213634,
10.91661824235,11.9090380825636,12.9014579227772,13.8759337553361),
 .UNSPECIFIED.);
#5966=B_SPLINE_CURVE_WITH_KNOTS('',3,(#49373,#49374,#49375,#49376,#49377,
#49378,#49379,#49380,#49381,#49382,#49383,#49384,#49385,#49386,#49387,#49388,
#49389,#49390,#49391,#49392,#49393,#49394,#49395,#49396,#49397,#49398,#49399,
#49400,#49401,#49402,#49403,#49404,#49405,#49406,#49407,#49408,#49409,#49410,
#49411,#49412,#49413,#49414,#49415,#49416,#49417,#49418,#49419,#49420,#49421,
#49422,#49423,#49424,#49425,#49426,#49427,#49428,#49429,#49430,#49431,#49432,
#49433,#49434,#49435,#49436,#49437,#49438,#49439,#49440,#49441,#49442,#49443,
#49444,#49445,#49446,#49447,#49448,#49449,#49450,#49451,#49452,#49453,#49454,
#49455,#49456,#49457,#49458,#49459,#49460,#49461,#49462,#49463),
 .UNSPECIFIED.,.F.,.F.,(4,3,3,3,3,3,3,3,3,3,3,3,3,3,3,3,3,3,3,3,3,3,3,3,
3,3,3,3,3,3,4),(0.,0.0297240923312089,0.0601072451030124,0.0893395181733674,
0.114917757109928,0.120626860329316,0.15038599018687,0.179981398708653,
0.208477406447952,0.220429501357406,0.228738542605281,0.234134415810311,
0.264049922738082,0.291955955636873,0.293965429665852,0.322911497430439,
0.33920604408414,0.343413984146313,0.371506227907014,0.399645180894377,
0.427381810227985,0.437705388288875,0.444698455295926,0.448877399529997,
0.476925724869063,0.497961968873363,0.506030934526871,0.511791130158556,
0.537728945654397,0.561070700886262,0.56924861039936),.UNSPECIFIED.);
#5967=B_SPLINE_CURVE_WITH_KNOTS('',3,(#49466,#49467,#49468,#49469,#49470,
#49471,#49472,#49473,#49474,#49475,#49476,#49477,#49478,#49479,#49480,#49481,
#49482,#49483,#49484,#49485,#49486,#49487,#49488,#49489,#49490,#49491,#49492,
#49493,#49494,#49495,#49496,#49497,#49498,#49499,#49500,#49501,#49502,#49503,
#49504,#49505,#49506,#49507,#49508,#49509,#49510,#49511,#49512,#49513,#49514,
#49515,#49516,#49517,#49518,#49519,#49520,#49521,#49522,#49523,#49524,#49525,
#49526,#49527,#49528,#49529,#49530,#49531,#49532,#49533,#49534,#49535,#49536,
#49537,#49538,#49539,#49540,#49541,#49542,#49543,#49544,#49545,#49546,#49547,
#49548,#49549,#49550,#49551,#49552,#49553,#49554,#49555,#49556,#49557,#49558,
#49559,#49560,#49561,#49562),.UNSPECIFIED.,.F.,.F.,(4,3,3,3,3,3,3,3,3,3,
3,3,3,3,3,3,3,3,3,3,3,3,3,3,3,3,3,3,3,3,3,3,4),(-0.569248610399423,-0.543574645891778,
-0.51727241644857,-0.510408710942387,-0.504800520393797,-0.477739691817378,
-0.455902626825033,-0.44718579861244,-0.442501671168929,-0.414772030874631,
-0.386610421034913,-0.358667819068152,-0.344761657270767,-0.34066303604345,
-0.336259738041431,-0.307329079225934,-0.303043171878612,-0.275226635447314,
-0.246781288655212,-0.236972581282364,-0.232129263600874,-0.22829863691149,
-0.199315265549529,-0.169757082987585,-0.139958578646832,-0.123701382943861,
-0.118726121129318,-0.11441116589234,-0.0838710238026174,-0.0532918819919743,
-0.0233206437919336,-0.00990101302306326,0.),.UNSPECIFIED.);
#5968=B_SPLINE_CURVE_WITH_KNOTS('',3,(#49563,#49564,#49565,#49566,#49567,
#49568,#49569,#49570,#49571,#49572,#49573,#49574,#49575,#49576,#49577,#49578,
#49579,#49580,#49581,#49582,#49583,#49584,#49585,#49586,#49587,#49588,#49589,
#49590,#49591,#49592,#49593,#49594,#49595,#49596,#49597,#49598,#49599,#49600,
#49601,#49602,#49603,#49604,#49605,#49606,#49607,#49608,#49609,#49610,#49611,
#49612,#49613,#49614,#49615,#49616,#49617,#49618,#49619,#49620,#49621,#49622,
#49623,#49624,#49625,#49626,#49627,#49628,#49629,#49630,#49631,#49632,#49633,
#49634,#49635,#49636,#49637,#49638,#49639,#49640,#49641,#49642,#49643,#49644,
#49645,#49646,#49647,#49648,#49649,#49650,#49651,#49652,#49653,#49654,#49655,
#49656),.UNSPECIFIED.,.F.,.F.,(4,3,3,3,3,3,3,3,3,3,3,3,3,3,3,3,3,3,3,3,
3,3,3,3,3,3,3,3,3,3,3,4),(-0.566847306048056,-0.536665873647055,-0.506059968025301,
-0.497416424413022,-0.490479625005237,-0.460332813217141,-0.437094437390416,
-0.424724940155325,-0.420483374200065,-0.391058520446558,-0.361900341985754,
-0.333575724604661,-0.318788245104331,-0.31312587971415,-0.308695953790866,
-0.280705559878078,-0.274425806603343,-0.245949103196031,-0.21622427278058,
-0.204597317060357,-0.200878698417494,-0.173045197029915,-0.145277260891852,
-0.117980532310966,-0.104251773256148,-0.100006089486155,-0.0958284088489193,
-0.0691557456817196,-0.0429305361063101,-0.0175053478708221,-0.00815045987242113,
0.),.UNSPECIFIED.);
#5969=B_SPLINE_CURVE_WITH_KNOTS('',3,(#49658,#49659,#49660,#49661,#49662,
#49663,#49664,#49665,#49666,#49667,#49668),.UNSPECIFIED.,.F.,.F.,(4,1,1,
1,1,1,1,1,4),(15.7079632679489,15.8286682231624,16.821088063376,17.8135079035896,
18.8059277438032,19.7983475840169,20.7907674242305,21.7831872644441,21.9911485751285),
 .UNSPECIFIED.);
#5970=B_SPLINE_CURVE_WITH_KNOTS('',3,(#49669,#49670,#49671,#49672,#49673,
#49674,#49675,#49676,#49677,#49678),.UNSPECIFIED.,.F.,.F.,(4,1,1,1,1,1,
1,4),(15.7079632679489,16.3832398073992,17.3756596476128,18.3680794878265,
19.3604993280401,20.3529191682537,21.3453390084674,21.9911485751284),
 .UNSPECIFIED.);
#5971=B_SPLINE_CURVE_WITH_KNOTS('',3,(#50079,#50080,#50081,#50082,#50083,
#50084,#50085,#50086,#50087,#50088,#50089,#50090,#50091,#50092,#50093,#50094,
#50095,#50096,#50097,#50098,#50099,#50100,#50101,#50102,#50103,#50104,#50105,
#50106,#50107,#50108,#50109,#50110,#50111,#50112,#50113,#50114,#50115,#50116,
#50117,#50118,#50119,#50120,#50121,#50122,#50123,#50124,#50125,#50126,#50127,
#50128,#50129,#50130,#50131,#50132,#50133,#50134,#50135,#50136,#50137,#50138,
#50139,#50140,#50141,#50142,#50143,#50144,#50145,#50146,#50147,#50148,#50149,
#50150,#50151,#50152,#50153,#50154,#50155,#50156,#50157,#50158,#50159,#50160,
#50161,#50162,#50163,#50164,#50165,#50166,#50167,#50168,#50169,#50170,#50171,
#50172),.UNSPECIFIED.,.F.,.F.,(4,3,3,3,3,3,3,3,3,3,3,3,3,3,3,3,3,3,3,3,
3,3,3,3,3,3,3,3,3,3,3,4),(0.,0.0253630076183808,0.0513975877048671,0.0781461974827044,
0.0899194311895631,0.0966315930648587,0.102678021607527,0.129978474909251,
0.157730194778542,0.184644262565798,0.195932069024234,0.203012843385935,
0.20715665262694,0.236271559277253,0.265386465927566,0.293279280416962,
0.302554895180608,0.311292641822859,0.31570453862194,0.343817446039294,
0.372959156504723,0.402412706795326,0.413342529372535,0.422899077410131,
0.428117895611974,0.458184942153285,0.482885329772337,0.492048651178443,
0.498170303955202,0.528680777355495,0.556986492629494,0.56684730604812),
 .UNSPECIFIED.);
#5972=B_SPLINE_CURVE_WITH_KNOTS('',3,(#50173,#50174,#50175,#50176,#50177,
#50178,#50179,#50180,#50181,#50182,#50183,#50184,#50185,#50186,#50187,#50188,
#50189,#50190,#50191,#50192,#50193,#50194,#50195,#50196,#50197),
 .UNSPECIFIED.,.F.,.F.,(4,3,3,3,3,3,3,3,4),(-10.1321597128207,-9.92419840213632,
-8.93177856192269,-7.93935872170906,-6.94693888149543,-5.95451904128179,
-4.96209920106816,-3.96967936085453,-3.848974405641),.UNSPECIFIED.);
#5973=B_SPLINE_CURVE_WITH_KNOTS('',3,(#50598,#50599,#50600,#50601,#50602,
#50603,#50604,#50605,#50606,#50607,#50608,#50609,#50610,#50611,#50612,#50613,
#50614,#50615,#50616,#50617,#50618,#50619),.UNSPECIFIED.,.F.,.F.,(4,3,3,
3,3,3,3,4),(7.59274844815647,7.93935872170907,8.9317785619227,9.92419840213634,
10.91661824235,11.9090380825636,12.9014579227772,13.875933755336),
 .UNSPECIFIED.);
#5974=B_SPLINE_CURVE_WITH_KNOTS('',3,(#50620,#50621,#50622,#50623,#50624,
#50625,#50626,#50627,#50628,#50629,#50630,#50631,#50632,#50633,#50634,#50635,
#50636,#50637,#50638,#50639,#50640,#50641,#50642,#50643,#50644,#50645,#50646,
#50647,#50648,#50649,#50650,#50651,#50652,#50653,#50654,#50655,#50656,#50657,
#50658,#50659,#50660,#50661,#50662,#50663,#50664,#50665,#50666,#50667,#50668,
#50669,#50670,#50671,#50672,#50673,#50674,#50675,#50676,#50677,#50678,#50679,
#50680,#50681,#50682,#50683,#50684,#50685,#50686,#50687,#50688,#50689,#50690,
#50691,#50692,#50693,#50694,#50695,#50696,#50697,#50698,#50699,#50700,#50701,
#50702,#50703,#50704,#50705,#50706,#50707,#50708,#50709,#50710),
 .UNSPECIFIED.,.F.,.F.,(4,3,3,3,3,3,3,3,3,3,3,3,3,3,3,3,3,3,3,3,3,3,3,3,
3,3,3,3,3,3,4),(0.,0.0297241015279183,0.0601072589089457,0.0893395302535658,
0.114917767680108,0.120626861018893,0.150385991075238,0.179981397216016,
0.208477405328489,0.220429498705637,0.228738535605999,0.234134414463615,
0.264049922064761,0.291955952723935,0.293965429665907,0.322911497914105,
0.339206043080533,0.343413983249963,0.371506227321681,0.39964518049671,
0.427381808138431,0.437705383117277,0.444698406530902,0.44887734867021,
0.476925686724255,0.497961940264788,0.506030881533375,0.511791139434088,
0.537728950428119,0.561070700886389,0.569248610399474),.UNSPECIFIED.);
#5975=B_SPLINE_CURVE_WITH_KNOTS('',3,(#50713,#50714,#50715,#50716,#50717,
#50718,#50719,#50720,#50721,#50722,#50723,#50724,#50725,#50726,#50727,#50728,
#50729,#50730,#50731,#50732,#50733,#50734,#50735,#50736,#50737,#50738,#50739,
#50740,#50741,#50742,#50743,#50744,#50745,#50746,#50747,#50748,#50749,#50750,
#50751,#50752,#50753,#50754,#50755,#50756,#50757,#50758,#50759,#50760,#50761,
#50762,#50763,#50764,#50765,#50766,#50767,#50768,#50769,#50770,#50771,#50772,
#50773,#50774,#50775,#50776,#50777,#50778,#50779,#50780,#50781,#50782,#50783,
#50784,#50785,#50786,#50787,#50788,#50789,#50790,#50791,#50792,#50793,#50794,
#50795,#50796,#50797,#50798,#50799,#50800,#50801,#50802,#50803,#50804,#50805,
#50806,#50807,#50808,#50809),.UNSPECIFIED.,.F.,.F.,(4,3,3,3,3,3,3,3,3,3,
3,3,3,3,3,3,3,3,3,3,3,3,3,3,3,3,3,3,3,3,3,3,4),(-0.569248610399393,-0.5435746659104,
-0.517272453279993,-0.510408802643641,-0.504800523617045,-0.477739709125334,
-0.455902641969492,-0.447185940467556,-0.442501780583286,-0.414772155649295,
-0.386610545496204,-0.358667935404984,-0.344761744523387,-0.340663181383466,
-0.33625977614692,-0.307329116668616,-0.303043171878598,-0.275226622766843,
-0.2467812679575,-0.236972518209036,-0.232129158610577,-0.22829853363839,
-0.199315149750587,-0.169756960537854,-0.1399584553707,-0.123701275077245,
-0.118725825220484,-0.114410875346345,-0.0838707291517932,-0.05329158908994,
-0.0233203533939032,-0.00990101302306306,0.),.UNSPECIFIED.);
#5976=B_SPLINE_CURVE_WITH_KNOTS('',3,(#50810,#50811,#50812,#50813,#50814,
#50815,#50816,#50817,#50818,#50819,#50820,#50821,#50822,#50823,#50824,#50825,
#50826,#50827,#50828,#50829,#50830,#50831,#50832,#50833,#50834,#50835,#50836,
#50837,#50838,#50839,#50840,#50841,#50842,#50843,#50844,#50845,#50846,#50847,
#50848,#50849,#50850,#50851,#50852,#50853,#50854,#50855,#50856,#50857,#50858,
#50859,#50860,#50861,#50862,#50863,#50864,#50865,#50866,#50867,#50868,#50869,
#50870,#50871,#50872,#50873,#50874,#50875,#50876,#50877,#50878,#50879,#50880,
#50881,#50882,#50883,#50884,#50885,#50886,#50887,#50888,#50889,#50890,#50891,
#50892,#50893,#50894,#50895,#50896,#50897,#50898,#50899,#50900,#50901,#50902,
#50903),.UNSPECIFIED.,.F.,.F.,(4,3,3,3,3,3,3,3,3,3,3,3,3,3,3,3,3,3,3,3,
3,3,3,3,3,3,3,3,3,3,3,4),(-0.566847306048015,-0.536665862165872,-0.506059953424534,
-0.497416406509601,-0.49047962159474,-0.460332810086325,-0.437094434650949,
-0.424724933731654,-0.420483367445324,-0.391058514938839,-0.361900337854958,
-0.333575724322276,-0.318788244892536,-0.313125876579605,-0.308695952531969,
-0.280705563178002,-0.274425806603314,-0.245949103512341,-0.21622427305735,
-0.204597316412413,-0.200878698510381,-0.173045196304837,-0.145277260484532,
-0.117980535767822,-0.104251776280896,-0.100006100365259,-0.0958284117637648,
-0.0691557510171672,-0.0429305470482147,-0.0175053685433162,-0.00815045987241369,
0.),.UNSPECIFIED.);
#5977=B_SPLINE_CURVE_WITH_KNOTS('',3,(#50905,#50906,#50907,#50908,#50909,
#50910,#50911,#50912,#50913,#50914,#50915),.UNSPECIFIED.,.F.,.F.,(4,1,1,
1,1,1,1,1,4),(15.7079632679489,15.8286682231624,16.821088063376,17.8135079035896,
18.8059277438032,19.7983475840169,20.7907674242305,21.7831872644441,21.9911485751285),
 .UNSPECIFIED.);
#5978=B_SPLINE_CURVE_WITH_KNOTS('',3,(#50916,#50917,#50918,#50919,#50920,
#50921,#50922,#50923,#50924,#50925),.UNSPECIFIED.,.F.,.F.,(4,1,1,1,1,1,
1,4),(15.7079632679489,16.3832398073992,17.3756596476128,18.3680794878265,
19.3604993280401,20.3529191682537,21.3453390084674,21.9911485751284),
 .UNSPECIFIED.);
#5979=B_SPLINE_CURVE_WITH_KNOTS('',3,(#51326,#51327,#51328,#51329,#51330,
#51331,#51332,#51333,#51334,#51335,#51336,#51337,#51338,#51339,#51340,#51341,
#51342,#51343,#51344,#51345,#51346,#51347,#51348,#51349,#51350,#51351,#51352,
#51353,#51354,#51355,#51356,#51357,#51358,#51359,#51360,#51361,#51362,#51363,
#51364,#51365,#51366,#51367,#51368,#51369,#51370,#51371,#51372,#51373,#51374,
#51375,#51376,#51377,#51378,#51379,#51380,#51381,#51382,#51383,#51384,#51385,
#51386,#51387,#51388,#51389,#51390,#51391,#51392,#51393,#51394,#51395,#51396,
#51397,#51398,#51399,#51400,#51401,#51402,#51403,#51404,#51405,#51406,#51407,
#51408,#51409,#51410,#51411,#51412,#51413,#51414,#51415,#51416,#51417,#51418,
#51419),.UNSPECIFIED.,.F.,.F.,(4,3,3,3,3,3,3,3,3,3,3,3,3,3,3,3,3,3,3,3,
3,3,3,3,3,3,3,3,3,3,3,4),(0.,0.025363025950112,0.0513976226497874,0.0781462280595047,
0.0899194383261542,0.0966315939995796,0.10267802161317,0.129978487838588,
0.157730214208604,0.184644277138334,0.195932072228315,0.20301284472711,
0.207156655403901,0.236271560665714,0.265386465927526,0.293279271834944,
0.302554877553594,0.311292566193282,0.315704524166865,0.343817419216937,
0.372959123929272,0.402412672778162,0.413342465523867,0.422898831529328,
0.428117874467775,0.458184918270669,0.482885311860363,0.492048607647558,
0.498170307466128,0.528680781105472,0.556986492629444,0.566847306048072),
 .UNSPECIFIED.);
#5980=B_SPLINE_CURVE_WITH_KNOTS('',3,(#51420,#51421,#51422,#51423,#51424,
#51425,#51426,#51427,#51428,#51429,#51430,#51431,#51432,#51433,#51434,#51435,
#51436,#51437,#51438,#51439,#51440,#51441,#51442,#51443,#51444),
 .UNSPECIFIED.,.F.,.F.,(4,3,3,3,3,3,3,3,4),(-10.1321597128207,-9.92419840213633,
-8.93177856192269,-7.93935872170906,-6.94693888149543,-5.9545190412818,
-4.96209920106816,-3.96967936085453,-3.848974405641),.UNSPECIFIED.);
#5981=B_SPLINE_CURVE_WITH_KNOTS('',3,(#51845,#51846,#51847,#51848,#51849,
#51850,#51851,#51852,#51853,#51854,#51855,#51856,#51857,#51858,#51859,#51860,
#51861,#51862,#51863,#51864,#51865,#51866),.UNSPECIFIED.,.F.,.F.,(4,3,3,
3,3,3,3,4),(7.59274844815647,7.93935872170906,8.93177856192269,9.92419840213633,
10.91661824235,11.9090380825636,12.9014579227772,13.875933755336),
 .UNSPECIFIED.);
#5982=B_SPLINE_CURVE_WITH_KNOTS('',3,(#51867,#51868,#51869,#51870,#51871,
#51872,#51873,#51874,#51875,#51876,#51877,#51878,#51879,#51880,#51881,#51882,
#51883,#51884,#51885,#51886,#51887,#51888,#51889,#51890,#51891,#51892,#51893,
#51894,#51895,#51896,#51897,#51898,#51899,#51900,#51901,#51902,#51903,#51904,
#51905,#51906,#51907,#51908,#51909,#51910,#51911,#51912,#51913,#51914,#51915,
#51916,#51917,#51918,#51919,#51920,#51921,#51922,#51923,#51924,#51925,#51926,
#51927,#51928,#51929,#51930,#51931,#51932,#51933,#51934,#51935,#51936,#51937,
#51938,#51939,#51940,#51941,#51942,#51943,#51944,#51945,#51946,#51947,#51948,
#51949,#51950,#51951,#51952,#51953,#51954,#51955,#51956,#51957),
 .UNSPECIFIED.,.F.,.F.,(4,3,3,3,3,3,3,3,3,3,3,3,3,3,3,3,3,3,3,3,3,3,3,3,
3,3,3,3,3,3,4),(0.,0.0297240839681494,0.0601072325488629,0.0893395071884968,
0.114917747498176,0.120626859693154,0.150385989369229,0.179981400055904,
0.208477407458411,0.220429503756483,0.228738548934207,0.234134417028589,
0.264049923347261,0.291955958282,0.293965429665934,0.322911496989362,0.339206044992874,
0.343413984993647,0.371506228471583,0.399645181287735,0.42738181215757,
0.437705393049684,0.444698500099991,0.448877446256884,0.476925759914272,
0.497961995157314,0.506030983187008,0.511791121700786,0.537728941286451,
0.561070700886438,0.569248610399523),.UNSPECIFIED.);
#5983=B_SPLINE_CURVE_WITH_KNOTS('',3,(#52036,#52037,#52038,#52039,#52040,
#52041,#52042,#52043,#52044,#52045,#52046,#52047,#52048,#52049,#52050,#52051,
#52052,#52053),.UNSPECIFIED.,.F.,.F.,(4,2,2,2,2,2,2,2,4),(0.301359994903926,
0.376699993319996,0.452039991736066,0.527379990771959,0.602719989807853,
0.678059988843746,0.753399987879639,0.828739986295709,0.904079984711779),
 .UNSPECIFIED.);
#5984=B_SPLINE_CURVE_WITH_KNOTS('',3,(#52057,#52058,#52059,#52060,#52061,
#52062,#52063,#52064,#52065,#52066,#52067,#52068,#52069,#52070,#52071,#52072,
#52073,#52074,#52075),.UNSPECIFIED.,.F.,.F.,(4,2,2,2,3,2,2,2,4),(0.904079984711779,
0.979419983127849,1.05475998154392,1.13009998057981,1.20543997961571,1.2807799786516,
1.35611997768749,1.43145997610356,1.50679997451963),.UNSPECIFIED.);
#5985=B_SPLINE_CURVE_WITH_KNOTS('',3,(#52080,#52081,#52082,#52083,#52084,
#52085,#52086,#52087,#52088,#52089,#52090,#52091,#52092,#52093,#52094,#52095,
#52096,#52097),.UNSPECIFIED.,.F.,.F.,(4,2,2,2,2,2,2,2,4),(0.301359994903926,
0.376699993319996,0.452039991736066,0.527379990771959,0.602719989807853,
0.678059988843746,0.753399987879639,0.828739986295709,0.904079984711779),
 .UNSPECIFIED.);
#5986=B_SPLINE_CURVE_WITH_KNOTS('',3,(#52098,#52099,#52100,#52101,#52102,
#52103,#52104,#52105,#52106,#52107,#52108,#52109,#52110,#52111,#52112,#52113,
#52114,#52115,#52116),.UNSPECIFIED.,.F.,.F.,(4,2,2,2,3,2,2,2,4),(0.904079984711779,
0.979419983127849,1.05475998154392,1.13009998057981,1.20543997961571,1.2807799786516,
1.35611997768749,1.43145997610356,1.50679997451963),.UNSPECIFIED.);
#5987=B_SPLINE_CURVE_WITH_KNOTS('',3,(#52124,#52125,#52126,#52127,#52128,
#52129,#52130,#52131,#52132,#52133,#52134,#52135,#52136,#52137,#52138,#52139,
#52140,#52141),.UNSPECIFIED.,.F.,.F.,(4,2,2,2,2,2,2,2,4),(0.301359994903926,
0.376699993319996,0.452039991736066,0.527379990771959,0.602719989807853,
0.678059988843746,0.753399987879639,0.828739986295709,0.904079984711779),
 .UNSPECIFIED.);
#5988=B_SPLINE_CURVE_WITH_KNOTS('',3,(#52143,#52144,#52145,#52146,#52147,
#52148,#52149,#52150,#52151,#52152),.UNSPECIFIED.,.F.,.F.,(4,2,2,2,4),(1.20543997961571,
1.2807799786516,1.35611997768749,1.43145997610356,1.50679997451963),
 .UNSPECIFIED.);
#5989=B_SPLINE_CURVE_WITH_KNOTS('',3,(#52156,#52157,#52158,#52159,#52160,
#52161,#52162,#52163,#52164,#52165),.UNSPECIFIED.,.F.,.F.,(4,2,2,2,4),(0.904079984711779,
0.979419983127849,1.05475998154392,1.13009998057981,1.20543997961571),
 .UNSPECIFIED.);
#5990=B_SPLINE_CURVE_WITH_KNOTS('',3,(#52170,#52171,#52172,#52173,#52174,
#52175,#52176,#52177,#52178,#52179,#52180,#52181,#52182,#52183,#52184,#52185,
#52186,#52187),.UNSPECIFIED.,.F.,.F.,(4,2,2,2,2,2,2,2,4),(0.301359994903926,
0.376699993319996,0.452039991736066,0.527379990771959,0.602719989807853,
0.678059988843746,0.753399987879639,0.828739986295709,0.904079984711779),
 .UNSPECIFIED.);
#5991=B_SPLINE_CURVE_WITH_KNOTS('',3,(#52189,#52190,#52191,#52192,#52193,
#52194,#52195,#52196,#52197,#52198),.UNSPECIFIED.,.F.,.F.,(4,2,2,2,4),(1.20543997961571,
1.2807799786516,1.35611997768749,1.43145997610356,1.50679997451963),
 .UNSPECIFIED.);
#5992=B_SPLINE_CURVE_WITH_KNOTS('',3,(#52202,#52203,#52204,#52205,#52206,
#52207,#52208,#52209,#52210,#52211),.UNSPECIFIED.,.F.,.F.,(4,2,2,2,4),(0.904079984711779,
0.979419983127849,1.05475998154392,1.13009998057981,1.20543997961571),
 .UNSPECIFIED.);
#5993=B_SPLINE_CURVE_WITH_KNOTS('',3,(#52399,#52400,#52401,#52402,#52403,
#52404,#52405,#52406,#52407,#52408,#52409,#52410,#52411,#52412,#52413,#52414,
#52415,#52416),.UNSPECIFIED.,.F.,.F.,(4,2,2,2,2,2,2,2,4),(0.301359994903926,
0.376699993319996,0.452039991736066,0.527379990771959,0.602719989807853,
0.678059988843746,0.753399987879639,0.828739986295709,0.904079984711779),
 .UNSPECIFIED.);
#5994=B_SPLINE_CURVE_WITH_KNOTS('',3,(#52420,#52421,#52422,#52423,#52424,
#52425,#52426,#52427,#52428,#52429,#52430,#52431,#52432,#52433,#52434,#52435,
#52436,#52437,#52438),.UNSPECIFIED.,.F.,.F.,(4,2,2,2,3,2,2,2,4),(0.904079984711779,
0.979419983127849,1.05475998154392,1.13009998057981,1.20543997961571,1.2807799786516,
1.35611997768749,1.43145997610356,1.50679997451963),.UNSPECIFIED.);
#5995=B_SPLINE_CURVE_WITH_KNOTS('',3,(#52443,#52444,#52445,#52446,#52447,
#52448,#52449,#52450,#52451,#52452,#52453,#52454,#52455,#52456,#52457,#52458,
#52459,#52460),.UNSPECIFIED.,.F.,.F.,(4,2,2,2,2,2,2,2,4),(0.301359994903926,
0.376699993319996,0.452039991736066,0.527379990771959,0.602719989807853,
0.678059988843746,0.753399987879639,0.828739986295709,0.904079984711779),
 .UNSPECIFIED.);
#5996=B_SPLINE_CURVE_WITH_KNOTS('',3,(#52461,#52462,#52463,#52464,#52465,
#52466,#52467,#52468,#52469,#52470,#52471,#52472,#52473,#52474,#52475,#52476,
#52477,#52478,#52479),.UNSPECIFIED.,.F.,.F.,(4,2,2,2,3,2,2,2,4),(0.904079984711779,
0.979419983127849,1.05475998154392,1.13009998057981,1.20543997961571,1.2807799786516,
1.35611997768749,1.43145997610356,1.50679997451963),.UNSPECIFIED.);
#5997=B_SPLINE_CURVE_WITH_KNOTS('',3,(#52487,#52488,#52489,#52490,#52491,
#52492,#52493,#52494,#52495,#52496,#52497,#52498,#52499,#52500,#52501,#52502,
#52503,#52504),.UNSPECIFIED.,.F.,.F.,(4,2,2,2,2,2,2,2,4),(0.301359994903926,
0.376699993319996,0.452039991736066,0.527379990771959,0.602719989807853,
0.678059988843746,0.753399987879639,0.828739986295709,0.904079984711779),
 .UNSPECIFIED.);
#5998=B_SPLINE_CURVE_WITH_KNOTS('',3,(#52506,#52507,#52508,#52509,#52510,
#52511,#52512,#52513,#52514,#52515),.UNSPECIFIED.,.F.,.F.,(4,2,2,2,4),(1.20543997961571,
1.2807799786516,1.35611997768749,1.43145997610356,1.50679997451963),
 .UNSPECIFIED.);
#5999=B_SPLINE_CURVE_WITH_KNOTS('',3,(#52519,#52520,#52521,#52522,#52523,
#52524,#52525,#52526,#52527,#52528),.UNSPECIFIED.,.F.,.F.,(4,2,2,2,4),(0.904079984711779,
0.979419983127849,1.05475998154392,1.13009998057981,1.20543997961571),
 .UNSPECIFIED.);
#6000=B_SPLINE_CURVE_WITH_KNOTS('',3,(#52533,#52534,#52535,#52536,#52537,
#52538,#52539,#52540,#52541,#52542,#52543,#52544,#52545,#52546,#52547,#52548,
#52549,#52550),.UNSPECIFIED.,.F.,.F.,(4,2,2,2,2,2,2,2,4),(0.301359994903926,
0.376699993319996,0.452039991736066,0.527379990771959,0.602719989807853,
0.678059988843746,0.753399987879639,0.828739986295709,0.904079984711779),
 .UNSPECIFIED.);
#6001=B_SPLINE_CURVE_WITH_KNOTS('',3,(#52552,#52553,#52554,#52555,#52556,
#52557,#52558,#52559,#52560,#52561),.UNSPECIFIED.,.F.,.F.,(4,2,2,2,4),(1.20543997961571,
1.2807799786516,1.35611997768749,1.43145997610356,1.50679997451963),
 .UNSPECIFIED.);
#6002=B_SPLINE_CURVE_WITH_KNOTS('',3,(#52565,#52566,#52567,#52568,#52569,
#52570,#52571,#52572,#52573,#52574),.UNSPECIFIED.,.F.,.F.,(4,2,2,2,4),(0.904079984711779,
0.979419983127849,1.05475998154392,1.13009998057981,1.20543997961571),
 .UNSPECIFIED.);
#6003=B_SPLINE_CURVE_WITH_KNOTS('',3,(#52598,#52599,#52600,#52601,#52602,
#52603,#52604),.UNSPECIFIED.,.F.,.F.,(4,3,4),(0.,0.0330660780484128,0.0578656365847224),
 .UNSPECIFIED.);
#6004=B_SPLINE_CURVE_WITH_KNOTS('',3,(#52606,#52607,#52608,#52609),
 .UNSPECIFIED.,.F.,.F.,(4,4),(-2.77555756156289E-17,1.2),.UNSPECIFIED.);
#6005=B_SPLINE_CURVE_WITH_KNOTS('',3,(#52611,#52612,#52613,#52614,#52615,
#52616,#52617),.UNSPECIFIED.,.F.,.F.,(4,3,4),(0.,0.0247995585363078,0.0578656365847182),
 .UNSPECIFIED.);
#6006=B_SPLINE_CURVE_WITH_KNOTS('',3,(#52618,#52619,#52620,#52621),
 .UNSPECIFIED.,.F.,.F.,(4,4),(-1.2,2.77555756156289E-17),.UNSPECIFIED.);
#6007=B_SPLINE_CURVE_WITH_KNOTS('',3,(#53445,#53446,#53447,#53448,#53449,
#53450,#53451),.UNSPECIFIED.,.F.,.F.,(4,3,4),(0.,0.033066078045883,0.0578656365802953),
 .UNSPECIFIED.);
#6008=B_SPLINE_CURVE_WITH_KNOTS('',3,(#53453,#53454,#53455,#53456),
 .UNSPECIFIED.,.F.,.F.,(4,4),(0.,1.2),.UNSPECIFIED.);
#6009=B_SPLINE_CURVE_WITH_KNOTS('',3,(#53458,#53459,#53460,#53461,#53462,
#53463,#53464),.UNSPECIFIED.,.F.,.F.,(4,3,4),(0.,0.0247995585344089,0.0578656365802874),
 .UNSPECIFIED.);
#6010=B_SPLINE_CURVE_WITH_KNOTS('',3,(#53465,#53466,#53467,#53468),
 .UNSPECIFIED.,.F.,.F.,(4,4),(-1.2,0.),.UNSPECIFIED.);
#6011=B_SPLINE_CURVE_WITH_KNOTS('',3,(#53494,#53495,#53496,#53497,#53498,
#53499,#53500),.UNSPECIFIED.,.F.,.F.,(4,3,4),(0.,0.033066078048414,0.0578656365847245),
 .UNSPECIFIED.);
#6012=B_SPLINE_CURVE_WITH_KNOTS('',3,(#53502,#53503,#53504,#53505),
 .UNSPECIFIED.,.F.,.F.,(4,4),(9.71445146547012E-17,1.2),.UNSPECIFIED.);
#6013=B_SPLINE_CURVE_WITH_KNOTS('',3,(#53507,#53508,#53509,#53510,#53511,
#53512,#53513),.UNSPECIFIED.,.F.,.F.,(4,3,4),(0.,0.02479955853631,0.0578656365847234),
 .UNSPECIFIED.);
#6014=B_SPLINE_CURVE_WITH_KNOTS('',3,(#53514,#53515,#53516,#53517),
 .UNSPECIFIED.,.F.,.F.,(4,4),(-1.2,-9.71445146547012E-17),.UNSPECIFIED.);
#6015=B_SPLINE_CURVE_WITH_KNOTS('',3,(#54341,#54342,#54343,#54344,#54345,
#54346,#54347),.UNSPECIFIED.,.F.,.F.,(4,3,4),(0.,0.033066078045845,0.0578656365802287),
 .UNSPECIFIED.);
#6016=B_SPLINE_CURVE_WITH_KNOTS('',3,(#54349,#54350,#54351,#54352),
 .UNSPECIFIED.,.F.,.F.,(4,4),(-6.97125684381022E-36,1.2),.UNSPECIFIED.);
#6017=B_SPLINE_CURVE_WITH_KNOTS('',3,(#54354,#54355,#54356,#54357,#54358,
#54359,#54360),.UNSPECIFIED.,.F.,.F.,(4,3,4),(0.,0.0247995585343863,0.0578656365802347),
 .UNSPECIFIED.);
#6018=B_SPLINE_CURVE_WITH_KNOTS('',3,(#54361,#54362,#54363,#54364),
 .UNSPECIFIED.,.F.,.F.,(4,4),(-1.2,6.97125684381022E-36),.UNSPECIFIED.);
#6019=B_SPLINE_CURVE_WITH_KNOTS('',3,(#54390,#54391,#54392,#54393,#54394,
#54395,#54396),.UNSPECIFIED.,.F.,.F.,(4,3,4),(0.,0.0330660780483976,0.0578656365846959),
 .UNSPECIFIED.);
#6020=B_SPLINE_CURVE_WITH_KNOTS('',3,(#54398,#54399,#54400,#54401),
 .UNSPECIFIED.,.F.,.F.,(4,4),(4.06042677328019E-17,1.2),.UNSPECIFIED.);
#6021=B_SPLINE_CURVE_WITH_KNOTS('',3,(#54403,#54404,#54405,#54406,#54407,
#54408,#54409),.UNSPECIFIED.,.F.,.F.,(4,3,4),(0.,0.0247995585363066,0.0578656365847153),
 .UNSPECIFIED.);
#6022=B_SPLINE_CURVE_WITH_KNOTS('',3,(#54410,#54411,#54412,#54413),
 .UNSPECIFIED.,.F.,.F.,(4,4),(-1.2,-4.06042677328019E-17),.UNSPECIFIED.);
#6023=B_SPLINE_CURVE_WITH_KNOTS('',3,(#55237,#55238,#55239,#55240,#55241,
#55242,#55243),.UNSPECIFIED.,.F.,.F.,(4,3,4),(0.,0.0330660780458488,0.0578656365802353),
 .UNSPECIFIED.);
#6024=B_SPLINE_CURVE_WITH_KNOTS('',3,(#55245,#55246,#55247,#55248),
 .UNSPECIFIED.,.F.,.F.,(4,4),(-8.32667268468868E-17,1.2),.UNSPECIFIED.);
#6025=B_SPLINE_CURVE_WITH_KNOTS('',3,(#55250,#55251,#55252,#55253,#55254,
#55255,#55256),.UNSPECIFIED.,.F.,.F.,(4,3,4),(0.,0.0247995585343919,0.0578656365802478),
 .UNSPECIFIED.);
#6026=B_SPLINE_CURVE_WITH_KNOTS('',3,(#55257,#55258,#55259,#55260),
 .UNSPECIFIED.,.F.,.F.,(4,4),(-1.2,8.32667268468868E-17),.UNSPECIFIED.);
#6027=B_SPLINE_CURVE_WITH_KNOTS('',3,(#55286,#55287,#55288,#55289,#55290,
#55291,#55292),.UNSPECIFIED.,.F.,.F.,(4,3,4),(0.,0.0330660780484025,0.0578656365847044),
 .UNSPECIFIED.);
#6028=B_SPLINE_CURVE_WITH_KNOTS('',3,(#55294,#55295,#55296,#55297),
 .UNSPECIFIED.,.F.,.F.,(4,4),(9.71445146547012E-17,1.2),.UNSPECIFIED.);
#6029=B_SPLINE_CURVE_WITH_KNOTS('',3,(#55299,#55300,#55301,#55302,#55303,
#55304,#55305),.UNSPECIFIED.,.F.,.F.,(4,3,4),(0.,0.024799558536305,0.0578656365847116),
 .UNSPECIFIED.);
#6030=B_SPLINE_CURVE_WITH_KNOTS('',3,(#55306,#55307,#55308,#55309),
 .UNSPECIFIED.,.F.,.F.,(4,4),(-1.2,-9.71445146547012E-17),.UNSPECIFIED.);
#6031=B_SPLINE_CURVE_WITH_KNOTS('',3,(#56133,#56134,#56135,#56136,#56137,
#56138,#56139),.UNSPECIFIED.,.F.,.F.,(4,3,4),(0.,0.0330660780458838,0.0578656365802966),
 .UNSPECIFIED.);
#6032=B_SPLINE_CURVE_WITH_KNOTS('',3,(#56141,#56142,#56143,#56144),
 .UNSPECIFIED.,.F.,.F.,(4,4),(2.77555756156289E-17,1.2),.UNSPECIFIED.);
#6033=B_SPLINE_CURVE_WITH_KNOTS('',3,(#56146,#56147,#56148,#56149,#56150,
#56151,#56152),.UNSPECIFIED.,.F.,.F.,(4,3,4),(0.,0.024799558534413,0.0578656365802969),
 .UNSPECIFIED.);
#6034=B_SPLINE_CURVE_WITH_KNOTS('',3,(#56153,#56154,#56155,#56156),
 .UNSPECIFIED.,.F.,.F.,(4,4),(-1.2,-2.77555756156289E-17),.UNSPECIFIED.);
#6035=B_SPLINE_CURVE_WITH_KNOTS('',3,(#56182,#56183,#56184,#56185,#56186,
#56187,#56188),.UNSPECIFIED.,.F.,.F.,(4,3,4),(0.,0.0330660780484225,0.0578656365847394),
 .UNSPECIFIED.);
#6036=B_SPLINE_CURVE_WITH_KNOTS('',3,(#56190,#56191,#56192,#56193),
 .UNSPECIFIED.,.F.,.F.,(4,4),(1.66533453693773E-16,1.2),.UNSPECIFIED.);
#6037=B_SPLINE_CURVE_WITH_KNOTS('',3,(#56195,#56196,#56197,#56198,#56199,
#56200,#56201),.UNSPECIFIED.,.F.,.F.,(4,3,4),(0.,0.0247995585363181,0.0578656365847422),
 .UNSPECIFIED.);
#6038=B_SPLINE_CURVE_WITH_KNOTS('',3,(#56202,#56203,#56204,#56205),
 .UNSPECIFIED.,.F.,.F.,(4,4),(-1.2,-1.66533453693773E-16),.UNSPECIFIED.);
#6039=B_SPLINE_CURVE_WITH_KNOTS('',3,(#57029,#57030,#57031,#57032,#57033,
#57034,#57035),.UNSPECIFIED.,.F.,.F.,(4,3,4),(0.,0.0330660780459141,0.0578656365803497),
 .UNSPECIFIED.);
#6040=B_SPLINE_CURVE_WITH_KNOTS('',3,(#57037,#57038,#57039,#57040),
 .UNSPECIFIED.,.F.,.F.,(4,4),(-4.16333634234434E-17,1.2),.UNSPECIFIED.);
#6041=B_SPLINE_CURVE_WITH_KNOTS('',3,(#57042,#57043,#57044,#57045,#57046,
#57047,#57048),.UNSPECIFIED.,.F.,.F.,(4,3,4),(0.,0.0247995585344146,0.0578656365803007),
 .UNSPECIFIED.);
#6042=B_SPLINE_CURVE_WITH_KNOTS('',3,(#57049,#57050,#57051,#57052),
 .UNSPECIFIED.,.F.,.F.,(4,4),(-1.2,4.16333634234434E-17),.UNSPECIFIED.);
#6043=B_SPLINE_CURVE_WITH_KNOTS('',3,(#57078,#57079,#57080,#57081,#57082,
#57083,#57084),.UNSPECIFIED.,.F.,.F.,(4,3,4),(0.,0.0330660780484257,0.057865636584745),
 .UNSPECIFIED.);
#6044=B_SPLINE_CURVE_WITH_KNOTS('',3,(#57086,#57087,#57088,#57089),
 .UNSPECIFIED.,.F.,.F.,(4,4),(1.38777878078145E-16,1.2),.UNSPECIFIED.);
#6045=B_SPLINE_CURVE_WITH_KNOTS('',3,(#57091,#57092,#57093,#57094,#57095,
#57096,#57097),.UNSPECIFIED.,.F.,.F.,(4,3,4),(0.,0.0247995585363191,0.0578656365847445),
 .UNSPECIFIED.);
#6046=B_SPLINE_CURVE_WITH_KNOTS('',3,(#57098,#57099,#57100,#57101),
 .UNSPECIFIED.,.F.,.F.,(4,4),(-1.2,-1.38777878078145E-16),.UNSPECIFIED.);
#6047=B_SPLINE_CURVE_WITH_KNOTS('',3,(#57925,#57926,#57927,#57928,#57929,
#57930,#57931),.UNSPECIFIED.,.F.,.F.,(4,3,4),(0.,0.0330660780458979,0.0578656365803213),
 .UNSPECIFIED.);
#6048=B_SPLINE_CURVE_WITH_KNOTS('',3,(#57933,#57934,#57935,#57936),
 .UNSPECIFIED.,.F.,.F.,(4,4),(-8.43563892506861E-17,1.2),.UNSPECIFIED.);
#6049=B_SPLINE_CURVE_WITH_KNOTS('',3,(#57938,#57939,#57940,#57941,#57942,
#57943,#57944),.UNSPECIFIED.,.F.,.F.,(4,3,4),(0.,0.0247995585344144,0.0578656365803003),
 .UNSPECIFIED.);
#6050=B_SPLINE_CURVE_WITH_KNOTS('',3,(#57945,#57946,#57947,#57948),
 .UNSPECIFIED.,.F.,.F.,(4,4),(-1.2,8.43563892506861E-17),.UNSPECIFIED.);
#6051=B_SPLINE_CURVE_WITH_KNOTS('',3,(#57974,#57975,#57976,#57977,#57978,
#57979,#57980),.UNSPECIFIED.,.F.,.F.,(4,3,4),(0.,0.0330660780484328,0.0578656365847574),
 .UNSPECIFIED.);
#6052=B_SPLINE_CURVE_WITH_KNOTS('',3,(#57982,#57983,#57984,#57985),
 .UNSPECIFIED.,.F.,.F.,(4,4),(1.66533453693773E-16,1.2),.UNSPECIFIED.);
#6053=B_SPLINE_CURVE_WITH_KNOTS('',3,(#57987,#57988,#57989,#57990,#57991,
#57992,#57993),.UNSPECIFIED.,.F.,.F.,(4,3,4),(0.,0.0247995585363196,0.0578656365847458),
 .UNSPECIFIED.);
#6054=B_SPLINE_CURVE_WITH_KNOTS('',3,(#57994,#57995,#57996,#57997),
 .UNSPECIFIED.,.F.,.F.,(4,4),(-1.2,-1.66533453693773E-16),.UNSPECIFIED.);
#6055=B_SPLINE_CURVE_WITH_KNOTS('',3,(#58821,#58822,#58823,#58824,#58825,
#58826,#58827),.UNSPECIFIED.,.F.,.F.,(4,3,4),(0.,0.0330660780458605,0.0578656365802559),
 .UNSPECIFIED.);
#6056=B_SPLINE_CURVE_WITH_KNOTS('',3,(#58829,#58830,#58831,#58832),
 .UNSPECIFIED.,.F.,.F.,(4,4),(2.77555756156289E-17,1.2),.UNSPECIFIED.);
#6057=B_SPLINE_CURVE_WITH_KNOTS('',3,(#58834,#58835,#58836,#58837,#58838,
#58839,#58840),.UNSPECIFIED.,.F.,.F.,(4,3,4),(0.,0.0247995585344011,0.0578656365802693),
 .UNSPECIFIED.);
#6058=B_SPLINE_CURVE_WITH_KNOTS('',3,(#58841,#58842,#58843,#58844),
 .UNSPECIFIED.,.F.,.F.,(4,4),(-1.2,-2.77555756156289E-17),.UNSPECIFIED.);
#6059=B_SPLINE_CURVE_WITH_KNOTS('',3,(#58870,#58871,#58872,#58873,#58874,
#58875,#58876),.UNSPECIFIED.,.F.,.F.,(4,3,4),(0.,0.0330660780484201,0.0578656365847351),
 .UNSPECIFIED.);
#6060=B_SPLINE_CURVE_WITH_KNOTS('',3,(#58878,#58879,#58880,#58881),
 .UNSPECIFIED.,.F.,.F.,(4,4),(-8.32667268468868E-17,1.2),.UNSPECIFIED.);
#6061=B_SPLINE_CURVE_WITH_KNOTS('',3,(#58883,#58884,#58885,#58886,#58887,
#58888,#58889),.UNSPECIFIED.,.F.,.F.,(4,3,4),(0.,0.0247995585363181,0.0578656365847421),
 .UNSPECIFIED.);
#6062=B_SPLINE_CURVE_WITH_KNOTS('',3,(#58890,#58891,#58892,#58893),
 .UNSPECIFIED.,.F.,.F.,(4,4),(-1.2,8.32667268468868E-17),.UNSPECIFIED.);
#6063=B_SPLINE_CURVE_WITH_KNOTS('',3,(#59717,#59718,#59719,#59720,#59721,
#59722,#59723),.UNSPECIFIED.,.F.,.F.,(4,3,4),(0.,0.0330660780458621,0.0578656365802586),
 .UNSPECIFIED.);
#6064=B_SPLINE_CURVE_WITH_KNOTS('',3,(#59725,#59726,#59727,#59728),
 .UNSPECIFIED.,.F.,.F.,(4,4),(5.55111512312578E-17,1.2),.UNSPECIFIED.);
#6065=B_SPLINE_CURVE_WITH_KNOTS('',3,(#59730,#59731,#59732,#59733,#59734,
#59735,#59736),.UNSPECIFIED.,.F.,.F.,(4,3,4),(0.,0.0247995585343903,0.057865636580244),
 .UNSPECIFIED.);
#6066=B_SPLINE_CURVE_WITH_KNOTS('',3,(#59737,#59738,#59739,#59740),
 .UNSPECIFIED.,.F.,.F.,(4,4),(-1.2,-5.55111512312578E-17),.UNSPECIFIED.);
#6067=B_SPLINE_CURVE_WITH_KNOTS('',3,(#59766,#59767,#59768,#59769,#59770,
#59771,#59772),.UNSPECIFIED.,.F.,.F.,(4,3,4),(0.,0.03306607804842,0.057865636584735),
 .UNSPECIFIED.);
#6068=B_SPLINE_CURVE_WITH_KNOTS('',3,(#59774,#59775,#59776,#59777),
 .UNSPECIFIED.,.F.,.F.,(4,4),(1.66533453693773E-16,1.2),.UNSPECIFIED.);
#6069=B_SPLINE_CURVE_WITH_KNOTS('',3,(#59779,#59780,#59781,#59782,#59783,
#59784,#59785),.UNSPECIFIED.,.F.,.F.,(4,3,4),(0.,0.0247995585363173,0.0578656365847403),
 .UNSPECIFIED.);
#6070=B_SPLINE_CURVE_WITH_KNOTS('',3,(#59786,#59787,#59788,#59789),
 .UNSPECIFIED.,.F.,.F.,(4,4),(-1.2,-1.66533453693773E-16),.UNSPECIFIED.);
#6071=B_SPLINE_CURVE_WITH_KNOTS('',3,(#60613,#60614,#60615,#60616,#60617,
#60618,#60619),.UNSPECIFIED.,.F.,.F.,(4,3,4),(0.,0.0330660780458358,0.0578656365802127),
 .UNSPECIFIED.);
#6072=B_SPLINE_CURVE_WITH_KNOTS('',3,(#60621,#60622,#60623,#60624),
 .UNSPECIFIED.,.F.,.F.,(4,4),(-8.9628248557339E-17,1.2),.UNSPECIFIED.);
#6073=B_SPLINE_CURVE_WITH_KNOTS('',3,(#60626,#60627,#60628,#60629,#60630,
#60631,#60632),.UNSPECIFIED.,.F.,.F.,(4,3,4),(0.,0.0247995585343798,0.0578656365802194),
 .UNSPECIFIED.);
#6074=B_SPLINE_CURVE_WITH_KNOTS('',3,(#60633,#60634,#60635,#60636),
 .UNSPECIFIED.,.F.,.F.,(4,4),(-1.2,8.9628248557339E-17),.UNSPECIFIED.);
#6075=B_SPLINE_CURVE_WITH_KNOTS('',3,(#60662,#60663,#60664,#60665,#60666,
#60667,#60668),.UNSPECIFIED.,.F.,.F.,(4,3,4),(0.,0.0330660780483891,0.057865636584681),
 .UNSPECIFIED.);
#6076=B_SPLINE_CURVE_WITH_KNOTS('',3,(#60670,#60671,#60672,#60673),
 .UNSPECIFIED.,.F.,.F.,(4,4),(8.0522471671843E-17,1.2),.UNSPECIFIED.);
#6077=B_SPLINE_CURVE_WITH_KNOTS('',3,(#60675,#60676,#60677,#60678,#60679,
#60680,#60681),.UNSPECIFIED.,.F.,.F.,(4,3,4),(0.,0.024799558536297,0.0578656365846929),
 .UNSPECIFIED.);
#6078=B_SPLINE_CURVE_WITH_KNOTS('',3,(#60682,#60683,#60684,#60685),
 .UNSPECIFIED.,.F.,.F.,(4,4),(-1.2,-8.0522471671843E-17),.UNSPECIFIED.);
#6079=B_SPLINE_CURVE_WITH_KNOTS('',3,(#61509,#61510,#61511,#61512,#61513,
#61514,#61515),.UNSPECIFIED.,.F.,.F.,(4,3,4),(0.,0.033066078045854,0.0578656365802446),
 .UNSPECIFIED.);
#6080=B_SPLINE_CURVE_WITH_KNOTS('',3,(#61517,#61518,#61519,#61520),
 .UNSPECIFIED.,.F.,.F.,(4,4),(-7.52391395153922E-36,1.2),.UNSPECIFIED.);
#6081=B_SPLINE_CURVE_WITH_KNOTS('',3,(#61522,#61523,#61524,#61525,#61526,
#61527,#61528),.UNSPECIFIED.,.F.,.F.,(4,3,4),(0.,0.0247995585343871,0.0578656365802365),
 .UNSPECIFIED.);
#6082=B_SPLINE_CURVE_WITH_KNOTS('',3,(#61529,#61530,#61531,#61532),
 .UNSPECIFIED.,.F.,.F.,(4,4),(-1.2,7.52391395153922E-36),.UNSPECIFIED.);
#6083=B_SPLINE_CURVE_WITH_KNOTS('',3,(#61558,#61559,#61560,#61561,#61562,
#61563,#61564),.UNSPECIFIED.,.F.,.F.,(4,3,4),(0.,0.0330660780484426,0.0578656365847746),
 .UNSPECIFIED.);
#6084=B_SPLINE_CURVE_WITH_KNOTS('',3,(#61566,#61567,#61568,#61569),
 .UNSPECIFIED.,.F.,.F.,(4,4),(9.71445146547012E-17,1.2),.UNSPECIFIED.);
#6085=B_SPLINE_CURVE_WITH_KNOTS('',3,(#61571,#61572,#61573,#61574,#61575,
#61576,#61577),.UNSPECIFIED.,.F.,.F.,(4,3,4),(0.,0.0247995585363433,0.0578656365848011),
 .UNSPECIFIED.);
#6086=B_SPLINE_CURVE_WITH_KNOTS('',3,(#61578,#61579,#61580,#61581),
 .UNSPECIFIED.,.F.,.F.,(4,4),(-1.2,-9.71445146547012E-17),.UNSPECIFIED.);
#6087=B_SPLINE_CURVE_WITH_KNOTS('',3,(#62405,#62406,#62407,#62408,#62409,
#62410,#62411),.UNSPECIFIED.,.F.,.F.,(4,3,4),(0.,0.0330660780458487,0.0578656365802352),
 .UNSPECIFIED.);
#6088=B_SPLINE_CURVE_WITH_KNOTS('',3,(#62413,#62414,#62415,#62416),
 .UNSPECIFIED.,.F.,.F.,(4,4),(2.77555756156289E-17,1.2),.UNSPECIFIED.);
#6089=B_SPLINE_CURVE_WITH_KNOTS('',3,(#62418,#62419,#62420,#62421,#62422,
#62423,#62424),.UNSPECIFIED.,.F.,.F.,(4,3,4),(0.,0.0247995585343886,0.05786563658024),
 .UNSPECIFIED.);
#6090=B_SPLINE_CURVE_WITH_KNOTS('',3,(#62425,#62426,#62427,#62428),
 .UNSPECIFIED.,.F.,.F.,(4,4),(-1.2,-2.77555756156289E-17),.UNSPECIFIED.);
#6091=B_SPLINE_CURVE_WITH_KNOTS('',3,(#62454,#62455,#62456,#62457,#62458,
#62459,#62460),.UNSPECIFIED.,.F.,.F.,(4,3,4),(0.,0.0330660780484585,0.0578656365848024),
 .UNSPECIFIED.);
#6092=B_SPLINE_CURVE_WITH_KNOTS('',3,(#62462,#62463,#62464,#62465),
 .UNSPECIFIED.,.F.,.F.,(4,4),(6.66446838640284E-17,1.2),.UNSPECIFIED.);
#6093=B_SPLINE_CURVE_WITH_KNOTS('',3,(#62467,#62468,#62469,#62470,#62471,
#62472,#62473),.UNSPECIFIED.,.F.,.F.,(4,3,4),(0.,0.0247995585363314,0.0578656365847732),
 .UNSPECIFIED.);
#6094=B_SPLINE_CURVE_WITH_KNOTS('',3,(#62474,#62475,#62476,#62477),
 .UNSPECIFIED.,.F.,.F.,(4,4),(-1.2,-6.66446838640284E-17),.UNSPECIFIED.);
#6095=B_SPLINE_CURVE_WITH_KNOTS('',3,(#63301,#63302,#63303,#63304,#63305,
#63306,#63307),.UNSPECIFIED.,.F.,.F.,(4,3,4),(0.,0.0330660780458707,0.0578656365802737),
 .UNSPECIFIED.);
#6096=B_SPLINE_CURVE_WITH_KNOTS('',3,(#63309,#63310,#63311,#63312),
 .UNSPECIFIED.,.F.,.F.,(4,4),(-4.16333634234434E-17,1.2),.UNSPECIFIED.);
#6097=B_SPLINE_CURVE_WITH_KNOTS('',3,(#63314,#63315,#63316,#63317,#63318,
#63319,#63320),.UNSPECIFIED.,.F.,.F.,(4,3,4),(0.,0.0247995585344061,0.057865636580281),
 .UNSPECIFIED.);
#6098=B_SPLINE_CURVE_WITH_KNOTS('',3,(#63321,#63322,#63323,#63324),
 .UNSPECIFIED.,.F.,.F.,(4,4),(-1.2,4.16333634234434E-17),.UNSPECIFIED.);
#6099=B_SPLINE_CURVE_WITH_KNOTS('',3,(#63350,#63351,#63352,#63353,#63354,
#63355,#63356),.UNSPECIFIED.,.F.,.F.,(4,3,4),(0.,0.0330660780484377,0.0578656365847659),
 .UNSPECIFIED.);
#6100=B_SPLINE_CURVE_WITH_KNOTS('',3,(#63358,#63359,#63360,#63361),
 .UNSPECIFIED.,.F.,.F.,(4,4),(0.,1.2),.UNSPECIFIED.);
#6101=B_SPLINE_CURVE_WITH_KNOTS('',3,(#63363,#63364,#63365,#63366,#63367,
#63368,#63369),.UNSPECIFIED.,.F.,.F.,(4,3,4),(0.,0.0247995585363214,0.0578656365847499),
 .UNSPECIFIED.);
#6102=B_SPLINE_CURVE_WITH_KNOTS('',3,(#63370,#63371,#63372,#63373),
 .UNSPECIFIED.,.F.,.F.,(4,4),(-1.2,0.),.UNSPECIFIED.);
#6103=B_SPLINE_CURVE_WITH_KNOTS('',3,(#64197,#64198,#64199,#64200,#64201,
#64202,#64203),.UNSPECIFIED.,.F.,.F.,(4,3,4),(0.,0.0330660780458375,0.0578656365802156),
 .UNSPECIFIED.);
#6104=B_SPLINE_CURVE_WITH_KNOTS('',3,(#64205,#64206,#64207,#64208),
 .UNSPECIFIED.,.F.,.F.,(4,4),(2.77555756156289E-17,1.2),.UNSPECIFIED.);
#6105=B_SPLINE_CURVE_WITH_KNOTS('',3,(#64210,#64211,#64212,#64213,#64214,
#64215,#64216),.UNSPECIFIED.,.F.,.F.,(4,3,4),(0.,0.0247995585344089,0.0578656365802873),
 .UNSPECIFIED.);
#6106=B_SPLINE_CURVE_WITH_KNOTS('',3,(#64217,#64218,#64219,#64220),
 .UNSPECIFIED.,.F.,.F.,(4,4),(-1.2,-2.77555756156289E-17),.UNSPECIFIED.);
#6107=B_SPLINE_CURVE_WITH_KNOTS('',3,(#64246,#64247,#64248,#64249,#64250,
#64251,#64252),.UNSPECIFIED.,.F.,.F.,(4,3,4),(0.,0.0330660780484158,0.0578656365847277),
 .UNSPECIFIED.);
#6108=B_SPLINE_CURVE_WITH_KNOTS('',3,(#64254,#64255,#64256,#64257),
 .UNSPECIFIED.,.F.,.F.,(4,4),(9.71445146547012E-17,1.2),.UNSPECIFIED.);
#6109=B_SPLINE_CURVE_WITH_KNOTS('',3,(#64259,#64260,#64261,#64262,#64263,
#64264,#64265),.UNSPECIFIED.,.F.,.F.,(4,3,4),(0.,0.024799558536314,0.0578656365847327),
 .UNSPECIFIED.);
#6110=B_SPLINE_CURVE_WITH_KNOTS('',3,(#64266,#64267,#64268,#64269),
 .UNSPECIFIED.,.F.,.F.,(4,4),(-1.2,-9.71445146547012E-17),.UNSPECIFIED.);
#6111=B_SPLINE_CURVE_WITH_KNOTS('',3,(#65093,#65094,#65095,#65096,#65097,
#65098,#65099),.UNSPECIFIED.,.F.,.F.,(4,3,4),(0.,0.0330660780458398,0.0578656365802196),
 .UNSPECIFIED.);
#6112=B_SPLINE_CURVE_WITH_KNOTS('',3,(#65101,#65102,#65103,#65104),
 .UNSPECIFIED.,.F.,.F.,(4,4),(-1.11022302462516E-16,1.2),.UNSPECIFIED.);
#6113=B_SPLINE_CURVE_WITH_KNOTS('',3,(#65106,#65107,#65108,#65109,#65110,
#65111,#65112),.UNSPECIFIED.,.F.,.F.,(4,3,4),(0.,0.0247995585343881,0.057865636580239),
 .UNSPECIFIED.);
#6114=B_SPLINE_CURVE_WITH_KNOTS('',3,(#65113,#65114,#65115,#65116),
 .UNSPECIFIED.,.F.,.F.,(4,4),(-1.2,1.11022302462516E-16),.UNSPECIFIED.);
#6115=B_SPLINE_CURVE_WITH_KNOTS('',3,(#65142,#65143,#65144,#65145,#65146,
#65147,#65148),.UNSPECIFIED.,.F.,.F.,(4,3,4),(0.,0.0330660780484092,0.0578656365847161),
 .UNSPECIFIED.);
#6116=B_SPLINE_CURVE_WITH_KNOTS('',3,(#65150,#65151,#65152,#65153),
 .UNSPECIFIED.,.F.,.F.,(4,4),(6.66446838640285E-17,1.2),.UNSPECIFIED.);
#6117=B_SPLINE_CURVE_WITH_KNOTS('',3,(#65155,#65156,#65157,#65158,#65159,
#65160,#65161),.UNSPECIFIED.,.F.,.F.,(4,3,4),(0.,0.0247995585363108,0.0578656365847252),
 .UNSPECIFIED.);
#6118=B_SPLINE_CURVE_WITH_KNOTS('',3,(#65162,#65163,#65164,#65165),
 .UNSPECIFIED.,.F.,.F.,(4,4),(-1.2,-6.66446838640285E-17),.UNSPECIFIED.);
#6119=B_SPLINE_CURVE_WITH_KNOTS('',3,(#65989,#65990,#65991,#65992,#65993,
#65994,#65995),.UNSPECIFIED.,.F.,.F.,(4,3,4),(0.,0.0330660780458506,0.0578656365802386),
 .UNSPECIFIED.);
#6120=B_SPLINE_CURVE_WITH_KNOTS('',3,(#65997,#65998,#65999,#66000),
 .UNSPECIFIED.,.F.,.F.,(4,4),(2.77555756156289E-17,1.2),.UNSPECIFIED.);
#6121=B_SPLINE_CURVE_WITH_KNOTS('',3,(#66002,#66003,#66004,#66005,#66006,
#66007,#66008),.UNSPECIFIED.,.F.,.F.,(4,3,4),(0.,0.024799558534388,0.0578656365802388),
 .UNSPECIFIED.);
#6122=B_SPLINE_CURVE_WITH_KNOTS('',3,(#66009,#66010,#66011,#66012),
 .UNSPECIFIED.,.F.,.F.,(4,4),(-1.2,-2.77555756156289E-17),.UNSPECIFIED.);
#6123=B_SPLINE_CURVE_WITH_KNOTS('',3,(#66038,#66039,#66040,#66041,#66042,
#66043,#66044),.UNSPECIFIED.,.F.,.F.,(4,3,4),(0.,0.0330660780484157,0.0578656365847274),
 .UNSPECIFIED.);
#6124=B_SPLINE_CURVE_WITH_KNOTS('',3,(#66046,#66047,#66048,#66049),
 .UNSPECIFIED.,.F.,.F.,(4,4),(6.93889390390723E-17,1.2),.UNSPECIFIED.);
#6125=B_SPLINE_CURVE_WITH_KNOTS('',3,(#66051,#66052,#66053,#66054,#66055,
#66056,#66057),.UNSPECIFIED.,.F.,.F.,(4,3,4),(0.,0.0247995585363113,0.0578656365847263),
 .UNSPECIFIED.);
#6126=B_SPLINE_CURVE_WITH_KNOTS('',3,(#66058,#66059,#66060,#66061),
 .UNSPECIFIED.,.F.,.F.,(4,4),(-1.2,-6.93889390390723E-17),.UNSPECIFIED.);
#6127=B_SPLINE_CURVE_WITH_KNOTS('',3,(#66885,#66886,#66887,#66888,#66889,
#66890,#66891),.UNSPECIFIED.,.F.,.F.,(4,3,4),(0.,0.0330660780458591,0.0578656365802535),
 .UNSPECIFIED.);
#6128=B_SPLINE_CURVE_WITH_KNOTS('',3,(#66893,#66894,#66895,#66896),
 .UNSPECIFIED.,.F.,.F.,(4,4),(0.,1.2),.UNSPECIFIED.);
#6129=B_SPLINE_CURVE_WITH_KNOTS('',3,(#66898,#66899,#66900,#66901,#66902,
#66903,#66904),.UNSPECIFIED.,.F.,.F.,(4,3,4),(0.,0.0247995585343995,0.0578656365802656),
 .UNSPECIFIED.);
#6130=B_SPLINE_CURVE_WITH_KNOTS('',3,(#66905,#66906,#66907,#66908),
 .UNSPECIFIED.,.F.,.F.,(4,4),(-1.2,0.),.UNSPECIFIED.);
#6131=B_SPLINE_CURVE_WITH_KNOTS('',3,(#66934,#66935,#66936,#66937,#66938,
#66939,#66940),.UNSPECIFIED.,.F.,.F.,(4,3,4),(0.,0.0330660780484159,0.0578656365847279),
 .UNSPECIFIED.);
#6132=B_SPLINE_CURVE_WITH_KNOTS('',3,(#66942,#66943,#66944,#66945),
 .UNSPECIFIED.,.F.,.F.,(4,4),(8.32667268468867E-17,1.2),.UNSPECIFIED.);
#6133=B_SPLINE_CURVE_WITH_KNOTS('',3,(#66947,#66948,#66949,#66950,#66951,
#66952,#66953),.UNSPECIFIED.,.F.,.F.,(4,3,4),(0.,0.0247995585363112,0.0578656365847262),
 .UNSPECIFIED.);
#6134=B_SPLINE_CURVE_WITH_KNOTS('',3,(#66954,#66955,#66956,#66957),
 .UNSPECIFIED.,.F.,.F.,(4,4),(-1.2,-8.32667268468867E-17),.UNSPECIFIED.);
#6135=B_SPLINE_CURVE_WITH_KNOTS('',3,(#67781,#67782,#67783,#67784,#67785,
#67786,#67787),.UNSPECIFIED.,.F.,.F.,(4,3,4),(0.,0.0330660780458738,0.0578656365802791),
 .UNSPECIFIED.);
#6136=B_SPLINE_CURVE_WITH_KNOTS('',3,(#67789,#67790,#67791,#67792),
 .UNSPECIFIED.,.F.,.F.,(4,4),(-5.55111512312578E-17,1.2),.UNSPECIFIED.);
#6137=B_SPLINE_CURVE_WITH_KNOTS('',3,(#67794,#67795,#67796,#67797,#67798,
#67799,#67800),.UNSPECIFIED.,.F.,.F.,(4,3,4),(0.,0.0247995585344049,0.0578656365802781),
 .UNSPECIFIED.);
#6138=B_SPLINE_CURVE_WITH_KNOTS('',3,(#67801,#67802,#67803,#67804),
 .UNSPECIFIED.,.F.,.F.,(4,4),(-1.2,5.55111512312578E-17),.UNSPECIFIED.);
#6139=B_SPLINE_CURVE_WITH_KNOTS('',3,(#67830,#67831,#67832,#67833,#67834,
#67835,#67836),.UNSPECIFIED.,.F.,.F.,(4,3,4),(0.,0.0330660780483935,0.0578656365846887),
 .UNSPECIFIED.);
#6140=B_SPLINE_CURVE_WITH_KNOTS('',3,(#67838,#67839,#67840,#67841),
 .UNSPECIFIED.,.F.,.F.,(4,4),(0.,1.2),.UNSPECIFIED.);
#6141=B_SPLINE_CURVE_WITH_KNOTS('',3,(#67843,#67844,#67845,#67846,#67847,
#67848,#67849),.UNSPECIFIED.,.F.,.F.,(4,3,4),(0.,0.0247995585363067,0.0578656365847155),
 .UNSPECIFIED.);
#6142=B_SPLINE_CURVE_WITH_KNOTS('',3,(#67850,#67851,#67852,#67853),
 .UNSPECIFIED.,.F.,.F.,(4,4),(-1.2,0.),.UNSPECIFIED.);
#6143=B_SPLINE_CURVE_WITH_KNOTS('',3,(#68677,#68678,#68679,#68680,#68681,
#68682,#68683),.UNSPECIFIED.,.F.,.F.,(4,3,4),(0.,0.0330660780458547,0.0578656365802457),
 .UNSPECIFIED.);
#6144=B_SPLINE_CURVE_WITH_KNOTS('',3,(#68685,#68686,#68687,#68688),
 .UNSPECIFIED.,.F.,.F.,(4,4),(-8.32667268468868E-17,1.2),.UNSPECIFIED.);
#6145=B_SPLINE_CURVE_WITH_KNOTS('',3,(#68690,#68691,#68692,#68693,#68694,
#68695,#68696),.UNSPECIFIED.,.F.,.F.,(4,3,4),(0.,0.0247995585343948,0.0578656365802546),
 .UNSPECIFIED.);
#6146=B_SPLINE_CURVE_WITH_KNOTS('',3,(#68697,#68698,#68699,#68700),
 .UNSPECIFIED.,.F.,.F.,(4,4),(-1.2,8.32667268468868E-17),.UNSPECIFIED.);
#6147=B_SPLINE_CURVE_WITH_KNOTS('',3,(#68726,#68727,#68728,#68729,#68730,
#68731,#68732),.UNSPECIFIED.,.F.,.F.,(4,3,4),(0.,0.0330660780484166,0.0578656365847291),
 .UNSPECIFIED.);
#6148=B_SPLINE_CURVE_WITH_KNOTS('',3,(#68734,#68735,#68736,#68737),
 .UNSPECIFIED.,.F.,.F.,(4,4),(9.71445146547012E-17,1.2),.UNSPECIFIED.);
#6149=B_SPLINE_CURVE_WITH_KNOTS('',3,(#68739,#68740,#68741,#68742,#68743,
#68744,#68745),.UNSPECIFIED.,.F.,.F.,(4,3,4),(0.,0.0247995585363142,0.0578656365847332),
 .UNSPECIFIED.);
#6150=B_SPLINE_CURVE_WITH_KNOTS('',3,(#68746,#68747,#68748,#68749),
 .UNSPECIFIED.,.F.,.F.,(4,4),(-1.2,-9.71445146547012E-17),.UNSPECIFIED.);
#6151=B_SPLINE_CURVE_WITH_KNOTS('',3,(#69573,#69574,#69575,#69576,#69577,
#69578,#69579),.UNSPECIFIED.,.F.,.F.,(4,3,4),(0.,0.0330660780458543,0.057865636580245),
 .UNSPECIFIED.);
#6152=B_SPLINE_CURVE_WITH_KNOTS('',3,(#69581,#69582,#69583,#69584),
 .UNSPECIFIED.,.F.,.F.,(4,4),(-2.74425517504386E-18,1.2),.UNSPECIFIED.);
#6153=B_SPLINE_CURVE_WITH_KNOTS('',3,(#69586,#69587,#69588,#69589,#69590,
#69591,#69592),.UNSPECIFIED.,.F.,.F.,(4,3,4),(0.,0.0247995585344,0.0578656365802666),
 .UNSPECIFIED.);
#6154=B_SPLINE_CURVE_WITH_KNOTS('',3,(#69593,#69594,#69595,#69596),
 .UNSPECIFIED.,.F.,.F.,(4,4),(-1.2,2.74425517504386E-18),.UNSPECIFIED.);
#6155=B_SPLINE_CURVE_WITH_KNOTS('',3,(#69622,#69623,#69624,#69625,#69626,
#69627,#69628),.UNSPECIFIED.,.F.,.F.,(4,3,4),(0.,0.033066078048411,0.0578656365847193),
 .UNSPECIFIED.);
#6156=B_SPLINE_CURVE_WITH_KNOTS('',3,(#69630,#69631,#69632,#69633),
 .UNSPECIFIED.,.F.,.F.,(4,4),(8.0522471671843E-17,1.2),.UNSPECIFIED.);
#6157=B_SPLINE_CURVE_WITH_KNOTS('',3,(#69635,#69636,#69637,#69638,#69639,
#69640,#69641),.UNSPECIFIED.,.F.,.F.,(4,3,4),(0.,0.0247995585363087,0.0578656365847204),
 .UNSPECIFIED.);
#6158=B_SPLINE_CURVE_WITH_KNOTS('',3,(#69642,#69643,#69644,#69645),
 .UNSPECIFIED.,.F.,.F.,(4,4),(-1.2,-8.0522471671843E-17),.UNSPECIFIED.);
#6159=B_SPLINE_CURVE_WITH_KNOTS('',3,(#70469,#70470,#70471,#70472,#70473,
#70474,#70475),.UNSPECIFIED.,.F.,.F.,(4,3,4),(0.,0.0330660780458236,0.0578656365801913),
 .UNSPECIFIED.);
#6160=B_SPLINE_CURVE_WITH_KNOTS('',3,(#70477,#70478,#70479,#70480),
 .UNSPECIFIED.,.F.,.F.,(4,4),(-1.38777878078145E-16,1.2),.UNSPECIFIED.);
#6161=B_SPLINE_CURVE_WITH_KNOTS('',3,(#70482,#70483,#70484,#70485,#70486,
#70487,#70488),.UNSPECIFIED.,.F.,.F.,(4,3,4),(0.,0.024799558534366,0.0578656365801874),
 .UNSPECIFIED.);
#6162=B_SPLINE_CURVE_WITH_KNOTS('',3,(#70489,#70490,#70491,#70492),
 .UNSPECIFIED.,.F.,.F.,(4,4),(-1.2,1.38777878078145E-16),.UNSPECIFIED.);
#6163=B_SPLINE_CURVE_WITH_KNOTS('',3,(#70518,#70519,#70520,#70521,#70522,
#70523,#70524),.UNSPECIFIED.,.F.,.F.,(4,3,4),(0.,0.0330660780484102,0.0578656365847179),
 .UNSPECIFIED.);
#6164=B_SPLINE_CURVE_WITH_KNOTS('',3,(#70526,#70527,#70528,#70529),
 .UNSPECIFIED.,.F.,.F.,(4,4),(8.32667268468867E-17,1.2),.UNSPECIFIED.);
#6165=B_SPLINE_CURVE_WITH_KNOTS('',3,(#70531,#70532,#70533,#70534,#70535,
#70536,#70537),.UNSPECIFIED.,.F.,.F.,(4,3,4),(0.,0.0247995585363082,0.057865636584719),
 .UNSPECIFIED.);
#6166=B_SPLINE_CURVE_WITH_KNOTS('',3,(#70538,#70539,#70540,#70541),
 .UNSPECIFIED.,.F.,.F.,(4,4),(-1.2,-8.32667268468867E-17),.UNSPECIFIED.);
#6167=B_SPLINE_CURVE_WITH_KNOTS('',3,(#71365,#71366,#71367,#71368,#71369,
#71370,#71371),.UNSPECIFIED.,.F.,.F.,(4,3,4),(0.,0.0330660780458722,0.0578656365802764),
 .UNSPECIFIED.);
#6168=B_SPLINE_CURVE_WITH_KNOTS('',3,(#71373,#71374,#71375,#71376),
 .UNSPECIFIED.,.F.,.F.,(4,4),(0.,1.2),.UNSPECIFIED.);
#6169=B_SPLINE_CURVE_WITH_KNOTS('',3,(#71378,#71379,#71380,#71381,#71382,
#71383,#71384),.UNSPECIFIED.,.F.,.F.,(4,3,4),(0.,0.0247995585344033,0.0578656365802744),
 .UNSPECIFIED.);
#6170=B_SPLINE_CURVE_WITH_KNOTS('',3,(#71385,#71386,#71387,#71388),
 .UNSPECIFIED.,.F.,.F.,(4,4),(-1.2,0.),.UNSPECIFIED.);
#6171=B_SPLINE_CURVE_WITH_KNOTS('',3,(#71414,#71415,#71416,#71417,#71418,
#71419,#71420),.UNSPECIFIED.,.F.,.F.,(4,3,4),(0.,0.0330660780484072,0.0578656365847127),
 .UNSPECIFIED.);
#6172=B_SPLINE_CURVE_WITH_KNOTS('',3,(#71422,#71423,#71424,#71425),
 .UNSPECIFIED.,.F.,.F.,(4,4),(1.66533453693773E-16,1.2),.UNSPECIFIED.);
#6173=B_SPLINE_CURVE_WITH_KNOTS('',3,(#71427,#71428,#71429,#71430,#71431,
#71432,#71433),.UNSPECIFIED.,.F.,.F.,(4,3,4),(0.,0.0247995585363061,0.0578656365847142),
 .UNSPECIFIED.);
#6174=B_SPLINE_CURVE_WITH_KNOTS('',3,(#71434,#71435,#71436,#71437),
 .UNSPECIFIED.,.F.,.F.,(4,4),(-1.2,-1.66533453693773E-16),.UNSPECIFIED.);
#6175=B_SPLINE_CURVE_WITH_KNOTS('',3,(#72261,#72262,#72263,#72264,#72265,
#72266,#72267),.UNSPECIFIED.,.F.,.F.,(4,3,4),(0.,0.033066078045837,0.0578656365802148),
 .UNSPECIFIED.);
#6176=B_SPLINE_CURVE_WITH_KNOTS('',3,(#72269,#72270,#72271,#72272),
 .UNSPECIFIED.,.F.,.F.,(4,4),(-1.38777878078145E-16,1.2),.UNSPECIFIED.);
#6177=B_SPLINE_CURVE_WITH_KNOTS('',3,(#72274,#72275,#72276,#72277,#72278,
#72279,#72280),.UNSPECIFIED.,.F.,.F.,(4,3,4),(0.,0.0247995585343889,0.0578656365802407),
 .UNSPECIFIED.);
#6178=B_SPLINE_CURVE_WITH_KNOTS('',3,(#72281,#72282,#72283,#72284),
 .UNSPECIFIED.,.F.,.F.,(4,4),(-1.2,1.38777878078145E-16),.UNSPECIFIED.);
#6179=B_SPLINE_CURVE_WITH_KNOTS('',3,(#72310,#72311,#72312,#72313,#72314,
#72315,#72316),.UNSPECIFIED.,.F.,.F.,(4,3,4),(0.,0.0330660780484256,0.0578656365847448),
 .UNSPECIFIED.);
#6180=B_SPLINE_CURVE_WITH_KNOTS('',3,(#72318,#72319,#72320,#72321),
 .UNSPECIFIED.,.F.,.F.,(4,4),(-2.08166817117217E-17,1.2),.UNSPECIFIED.);
#6181=B_SPLINE_CURVE_WITH_KNOTS('',3,(#72323,#72324,#72325,#72326,#72327,
#72328,#72329),.UNSPECIFIED.,.F.,.F.,(4,3,4),(0.,0.024799558536321,0.057865636584749),
 .UNSPECIFIED.);
#6182=B_SPLINE_CURVE_WITH_KNOTS('',3,(#72330,#72331,#72332,#72333),
 .UNSPECIFIED.,.F.,.F.,(4,4),(-1.2,2.08166817117217E-17),.UNSPECIFIED.);
#6183=B_SPLINE_CURVE_WITH_KNOTS('',3,(#73157,#73158,#73159,#73160,#73161,
#73162,#73163),.UNSPECIFIED.,.F.,.F.,(4,3,4),(0.,0.0330660780458522,0.0578656365802413),
 .UNSPECIFIED.);
#6184=B_SPLINE_CURVE_WITH_KNOTS('',3,(#73165,#73166,#73167,#73168),
 .UNSPECIFIED.,.F.,.F.,(4,4),(-8.32667268468868E-17,1.2),.UNSPECIFIED.);
#6185=B_SPLINE_CURVE_WITH_KNOTS('',3,(#73170,#73171,#73172,#73173,#73174,
#73175,#73176),.UNSPECIFIED.,.F.,.F.,(4,3,4),(0.,0.0247995585343892,0.0578656365802414),
 .UNSPECIFIED.);
#6186=B_SPLINE_CURVE_WITH_KNOTS('',3,(#73177,#73178,#73179,#73180),
 .UNSPECIFIED.,.F.,.F.,(4,4),(-1.2,8.32667268468868E-17),.UNSPECIFIED.);
#6187=B_SPLINE_CURVE_WITH_KNOTS('',3,(#73206,#73207,#73208,#73209,#73210,
#73211,#73212),.UNSPECIFIED.,.F.,.F.,(4,3,4),(0.,0.0330660780484257,0.057865636584745),
 .UNSPECIFIED.);
#6188=B_SPLINE_CURVE_WITH_KNOTS('',3,(#73214,#73215,#73216,#73217),
 .UNSPECIFIED.,.F.,.F.,(4,4),(1.38777878078145E-16,1.2),.UNSPECIFIED.);
#6189=B_SPLINE_CURVE_WITH_KNOTS('',3,(#73219,#73220,#73221,#73222,#73223,
#73224,#73225),.UNSPECIFIED.,.F.,.F.,(4,3,4),(0.,0.0247995585363191,0.0578656365847445),
 .UNSPECIFIED.);
#6190=B_SPLINE_CURVE_WITH_KNOTS('',3,(#73226,#73227,#73228,#73229),
 .UNSPECIFIED.,.F.,.F.,(4,4),(-1.2,-1.38777878078145E-16),.UNSPECIFIED.);
#6191=B_SPLINE_CURVE_WITH_KNOTS('',3,(#74053,#74054,#74055,#74056,#74057,
#74058,#74059),.UNSPECIFIED.,.F.,.F.,(4,3,4),(0.,0.0330660780458979,0.0578656365803213),
 .UNSPECIFIED.);
#6192=B_SPLINE_CURVE_WITH_KNOTS('',3,(#74061,#74062,#74063,#74064),
 .UNSPECIFIED.,.F.,.F.,(4,4),(-8.43563892506861E-17,1.2),.UNSPECIFIED.);
#6193=B_SPLINE_CURVE_WITH_KNOTS('',3,(#74066,#74067,#74068,#74069,#74070,
#74071,#74072),.UNSPECIFIED.,.F.,.F.,(4,3,4),(0.,0.0247995585344144,0.0578656365803003),
 .UNSPECIFIED.);
#6194=B_SPLINE_CURVE_WITH_KNOTS('',3,(#74073,#74074,#74075,#74076),
 .UNSPECIFIED.,.F.,.F.,(4,4),(-1.2,8.43563892506861E-17),.UNSPECIFIED.);
#6195=B_SPLINE_CURVE_WITH_KNOTS('',3,(#74102,#74103,#74104,#74105,#74106,
#74107,#74108),.UNSPECIFIED.,.F.,.F.,(4,3,4),(0.,0.033066078048418,0.0578656365847316),
 .UNSPECIFIED.);
#6196=B_SPLINE_CURVE_WITH_KNOTS('',3,(#74110,#74111,#74112,#74113),
 .UNSPECIFIED.,.F.,.F.,(4,4),(9.71445146547012E-17,1.2),.UNSPECIFIED.);
#6197=B_SPLINE_CURVE_WITH_KNOTS('',3,(#74115,#74116,#74117,#74118,#74119,
#74120,#74121),.UNSPECIFIED.,.F.,.F.,(4,3,4),(0.,0.0247995585363153,0.0578656365847356),
 .UNSPECIFIED.);
#6198=B_SPLINE_CURVE_WITH_KNOTS('',3,(#74122,#74123,#74124,#74125),
 .UNSPECIFIED.,.F.,.F.,(4,4),(-1.2,-9.71445146547012E-17),.UNSPECIFIED.);
#6199=B_SPLINE_CURVE_WITH_KNOTS('',3,(#74949,#74950,#74951,#74952,#74953,
#74954,#74955),.UNSPECIFIED.,.F.,.F.,(4,3,4),(0.,0.0330660780458051,0.0578656365801589),
 .UNSPECIFIED.);
#6200=B_SPLINE_CURVE_WITH_KNOTS('',3,(#74957,#74958,#74959,#74960),
 .UNSPECIFIED.,.F.,.F.,(4,4),(0.,1.2),.UNSPECIFIED.);
#6201=B_SPLINE_CURVE_WITH_KNOTS('',3,(#74962,#74963,#74964,#74965,#74966,
#74967,#74968),.UNSPECIFIED.,.F.,.F.,(4,3,4),(0.,0.0247995585343412,0.0578656365801295),
 .UNSPECIFIED.);
#6202=B_SPLINE_CURVE_WITH_KNOTS('',3,(#74969,#74970,#74971,#74972),
 .UNSPECIFIED.,.F.,.F.,(4,4),(-1.2,0.),.UNSPECIFIED.);
#6203=B_SPLINE_CURVE_WITH_KNOTS('',3,(#74998,#74999,#75000,#75001,#75002,
#75003,#75004),.UNSPECIFIED.,.F.,.F.,(4,3,4),(0.,0.03306607804841,0.0578656365847175),
 .UNSPECIFIED.);
#6204=B_SPLINE_CURVE_WITH_KNOTS('',3,(#75006,#75007,#75008,#75009),
 .UNSPECIFIED.,.F.,.F.,(4,4),(9.71445146547012E-17,1.2),.UNSPECIFIED.);
#6205=B_SPLINE_CURVE_WITH_KNOTS('',3,(#75011,#75012,#75013,#75014,#75015,
#75016,#75017),.UNSPECIFIED.,.F.,.F.,(4,3,4),(0.,0.0247995585363106,0.0578656365847246),
 .UNSPECIFIED.);
#6206=B_SPLINE_CURVE_WITH_KNOTS('',3,(#75018,#75019,#75020,#75021),
 .UNSPECIFIED.,.F.,.F.,(4,4),(-1.2,-9.71445146547012E-17),.UNSPECIFIED.);
#6207=B_SPLINE_CURVE_WITH_KNOTS('',3,(#75845,#75846,#75847,#75848,#75849,
#75850,#75851),.UNSPECIFIED.,.F.,.F.,(4,3,4),(0.,0.0330660780458883,0.0578656365803045),
 .UNSPECIFIED.);
#6208=B_SPLINE_CURVE_WITH_KNOTS('',3,(#75853,#75854,#75855,#75856),
 .UNSPECIFIED.,.F.,.F.,(4,4),(-1.49437708898837E-16,1.2),.UNSPECIFIED.);
#6209=B_SPLINE_CURVE_WITH_KNOTS('',3,(#75858,#75859,#75860,#75861,#75862,
#75863,#75864),.UNSPECIFIED.,.F.,.F.,(4,3,4),(0.,0.0247995585344198,0.0578656365803129),
 .UNSPECIFIED.);
#6210=B_SPLINE_CURVE_WITH_KNOTS('',3,(#75865,#75866,#75867,#75868),
 .UNSPECIFIED.,.F.,.F.,(4,4),(-1.2,1.49437708898837E-16),.UNSPECIFIED.);
#6211=B_SPLINE_CURVE_WITH_KNOTS('',3,(#75894,#75895,#75896,#75897,#75898,
#75899,#75900),.UNSPECIFIED.,.F.,.F.,(4,3,4),(0.,0.0330660780483754,0.057865636584657),
 .UNSPECIFIED.);
#6212=B_SPLINE_CURVE_WITH_KNOTS('',3,(#75902,#75903,#75904,#75905),
 .UNSPECIFIED.,.F.,.F.,(4,4),(9.71445146547012E-17,1.2),.UNSPECIFIED.);
#6213=B_SPLINE_CURVE_WITH_KNOTS('',3,(#75907,#75908,#75909,#75910,#75911,
#75912,#75913),.UNSPECIFIED.,.F.,.F.,(4,3,4),(0.,0.0247995585362854,0.057865636584666),
 .UNSPECIFIED.);
#6214=B_SPLINE_CURVE_WITH_KNOTS('',3,(#75914,#75915,#75916,#75917),
 .UNSPECIFIED.,.F.,.F.,(4,4),(-1.2,-9.71445146547012E-17),.UNSPECIFIED.);
#6215=B_SPLINE_CURVE_WITH_KNOTS('',3,(#76741,#76742,#76743,#76744,#76745,
#76746,#76747),.UNSPECIFIED.,.F.,.F.,(4,3,4),(0.,0.0330660780458802,0.0578656365802904),
 .UNSPECIFIED.);
#6216=B_SPLINE_CURVE_WITH_KNOTS('',3,(#76749,#76750,#76751,#76752),
 .UNSPECIFIED.,.F.,.F.,(4,4),(0.,1.2),.UNSPECIFIED.);
#6217=B_SPLINE_CURVE_WITH_KNOTS('',3,(#76754,#76755,#76756,#76757,#76758,
#76759,#76760),.UNSPECIFIED.,.F.,.F.,(4,3,4),(0.,0.0247995585344145,0.0578656365803004),
 .UNSPECIFIED.);
#6218=B_SPLINE_CURVE_WITH_KNOTS('',3,(#76761,#76762,#76763,#76764),
 .UNSPECIFIED.,.F.,.F.,(4,4),(-1.2,0.),.UNSPECIFIED.);
#6219=B_SPLINE_CURVE_WITH_KNOTS('',3,(#76790,#76791,#76792,#76793,#76794,
#76795,#76796),.UNSPECIFIED.,.F.,.F.,(4,3,4),(0.,0.033066078048439,0.0578656365847682),
 .UNSPECIFIED.);
#6220=B_SPLINE_CURVE_WITH_KNOTS('',3,(#76798,#76799,#76800,#76801),
 .UNSPECIFIED.,.F.,.F.,(4,4),(1.66533453693773E-16,1.2),.UNSPECIFIED.);
#6221=B_SPLINE_CURVE_WITH_KNOTS('',3,(#76803,#76804,#76805,#76806,#76807,
#76808,#76809),.UNSPECIFIED.,.F.,.F.,(4,3,4),(0.,0.0247995585363292,0.0578656365847682),
 .UNSPECIFIED.);
#6222=B_SPLINE_CURVE_WITH_KNOTS('',3,(#76810,#76811,#76812,#76813),
 .UNSPECIFIED.,.F.,.F.,(4,4),(-1.2,-1.66533453693773E-16),.UNSPECIFIED.);
#6223=B_SPLINE_CURVE_WITH_KNOTS('',3,(#77637,#77638,#77639,#77640,#77641,
#77642,#77643),.UNSPECIFIED.,.F.,.F.,(4,3,4),(0.,0.033066078045871,0.0578656365802742),
 .UNSPECIFIED.);
#6224=B_SPLINE_CURVE_WITH_KNOTS('',3,(#77645,#77646,#77647,#77648),
 .UNSPECIFIED.,.F.,.F.,(4,4),(-1.47525527564366E-17,1.2),.UNSPECIFIED.);
#6225=B_SPLINE_CURVE_WITH_KNOTS('',3,(#77650,#77651,#77652,#77653,#77654,
#77655,#77656),.UNSPECIFIED.,.F.,.F.,(4,3,4),(0.,0.0247995585344122,0.057865636580295),
 .UNSPECIFIED.);
#6226=B_SPLINE_CURVE_WITH_KNOTS('',3,(#77657,#77658,#77659,#77660),
 .UNSPECIFIED.,.F.,.F.,(4,4),(-1.2,1.47525527564366E-17),.UNSPECIFIED.);
#6227=B_SPLINE_CURVE_WITH_KNOTS('',3,(#77686,#77687,#77688,#77689,#77690,
#77691,#77692),.UNSPECIFIED.,.F.,.F.,(4,3,4),(0.,0.0330660780484519,0.0578656365847908),
 .UNSPECIFIED.);
#6228=B_SPLINE_CURVE_WITH_KNOTS('',3,(#77694,#77695,#77696,#77697),
 .UNSPECIFIED.,.F.,.F.,(4,4),(-8.32667268468867E-17,1.2),.UNSPECIFIED.);
#6229=B_SPLINE_CURVE_WITH_KNOTS('',3,(#77699,#77700,#77701,#77702,#77703,
#77704,#77705),.UNSPECIFIED.,.F.,.F.,(4,3,4),(0.,0.0247995585363362,0.0578656365847844),
 .UNSPECIFIED.);
#6230=B_SPLINE_CURVE_WITH_KNOTS('',3,(#77706,#77707,#77708,#77709),
 .UNSPECIFIED.,.F.,.F.,(4,4),(-1.2,8.32667268468867E-17),.UNSPECIFIED.);
#6231=B_SPLINE_CURVE_WITH_KNOTS('',3,(#78533,#78534,#78535,#78536,#78537,
#78538,#78539),.UNSPECIFIED.,.F.,.F.,(4,3,4),(0.,0.0330660780458195,0.0578656365801842),
 .UNSPECIFIED.);
#6232=B_SPLINE_CURVE_WITH_KNOTS('',3,(#78541,#78542,#78543,#78544),
 .UNSPECIFIED.,.F.,.F.,(4,4),(2.77555756156289E-17,1.2),.UNSPECIFIED.);
#6233=B_SPLINE_CURVE_WITH_KNOTS('',3,(#78546,#78547,#78548,#78549,#78550,
#78551,#78552),.UNSPECIFIED.,.F.,.F.,(4,3,4),(0.,0.024799558534367,0.0578656365801897),
 .UNSPECIFIED.);
#6234=B_SPLINE_CURVE_WITH_KNOTS('',3,(#78553,#78554,#78555,#78556),
 .UNSPECIFIED.,.F.,.F.,(4,4),(-1.2,-2.77555756156289E-17),.UNSPECIFIED.);
#6235=B_SPLINE_CURVE_WITH_KNOTS('',3,(#78582,#78583,#78584,#78585,#78586,
#78587,#78588),.UNSPECIFIED.,.F.,.F.,(4,3,4),(0.,0.0330660780484703,0.057865636584823),
 .UNSPECIFIED.);
#6236=B_SPLINE_CURVE_WITH_KNOTS('',3,(#78590,#78591,#78592,#78593),
 .UNSPECIFIED.,.F.,.F.,(4,4),(9.44002594796574E-17,1.2),.UNSPECIFIED.);
#6237=B_SPLINE_CURVE_WITH_KNOTS('',3,(#78595,#78596,#78597,#78598,#78599,
#78600,#78601),.UNSPECIFIED.,.F.,.F.,(4,3,4),(0.,0.0247995585363458,0.0578656365848069),
 .UNSPECIFIED.);
#6238=B_SPLINE_CURVE_WITH_KNOTS('',3,(#78602,#78603,#78604,#78605),
 .UNSPECIFIED.,.F.,.F.,(4,4),(-1.2,-9.44002594796574E-17),.UNSPECIFIED.);
#6239=B_SPLINE_CURVE_WITH_KNOTS('',3,(#79429,#79430,#79431,#79432,#79433,
#79434,#79435),.UNSPECIFIED.,.F.,.F.,(4,3,4),(0.,0.0330660780458513,0.0578656365802398),
 .UNSPECIFIED.);
#6240=B_SPLINE_CURVE_WITH_KNOTS('',3,(#79437,#79438,#79439,#79440),
 .UNSPECIFIED.,.F.,.F.,(4,4),(0.,1.2),.UNSPECIFIED.);
#6241=B_SPLINE_CURVE_WITH_KNOTS('',3,(#79442,#79443,#79444,#79445,#79446,
#79447,#79448),.UNSPECIFIED.,.F.,.F.,(4,3,4),(0.,0.0247995585343902,0.0578656365802439),
 .UNSPECIFIED.);
#6242=B_SPLINE_CURVE_WITH_KNOTS('',3,(#79449,#79450,#79451,#79452),
 .UNSPECIFIED.,.F.,.F.,(4,4),(-1.2,0.),.UNSPECIFIED.);
#6243=B_SPLINE_CURVE_WITH_KNOTS('',3,(#79478,#79479,#79480,#79481,#79482,
#79483,#79484),.UNSPECIFIED.,.F.,.F.,(4,3,4),(0.,0.0330660780484092,0.0578656365847161),
 .UNSPECIFIED.);
#6244=B_SPLINE_CURVE_WITH_KNOTS('',3,(#79486,#79487,#79488,#79489),
 .UNSPECIFIED.,.F.,.F.,(4,4),(1.66533453693773E-16,1.2),.UNSPECIFIED.);
#6245=B_SPLINE_CURVE_WITH_KNOTS('',3,(#79491,#79492,#79493,#79494,#79495,
#79496,#79497),.UNSPECIFIED.,.F.,.F.,(4,3,4),(0.,0.0247995585363076,0.0578656365847178),
 .UNSPECIFIED.);
#6246=B_SPLINE_CURVE_WITH_KNOTS('',3,(#79498,#79499,#79500,#79501),
 .UNSPECIFIED.,.F.,.F.,(4,4),(-1.2,-1.66533453693773E-16),.UNSPECIFIED.);
#6247=B_SPLINE_CURVE_WITH_KNOTS('',3,(#80325,#80326,#80327,#80328,#80329,
#80330,#80331),.UNSPECIFIED.,.F.,.F.,(4,3,4),(0.,0.033066078045864,0.0578656365802619),
 .UNSPECIFIED.);
#6248=B_SPLINE_CURVE_WITH_KNOTS('',3,(#80333,#80334,#80335,#80336),
 .UNSPECIFIED.,.F.,.F.,(4,4),(-1.8224407144634E-16,1.2),.UNSPECIFIED.);
#6249=B_SPLINE_CURVE_WITH_KNOTS('',3,(#80338,#80339,#80340,#80341,#80342,
#80343,#80344),.UNSPECIFIED.,.F.,.F.,(4,3,4),(0.,0.0247995585343939,0.0578656365802525),
 .UNSPECIFIED.);
#6250=B_SPLINE_CURVE_WITH_KNOTS('',3,(#80345,#80346,#80347,#80348),
 .UNSPECIFIED.,.F.,.F.,(4,4),(-1.2,1.8224407144634E-16),.UNSPECIFIED.);
#6251=B_SPLINE_CURVE_WITH_KNOTS('',3,(#80374,#80375,#80376,#80377,#80378,
#80379,#80380),.UNSPECIFIED.,.F.,.F.,(4,3,4),(0.,0.0330660780484494,0.0578656365847864),
 .UNSPECIFIED.);
#6252=B_SPLINE_CURVE_WITH_KNOTS('',3,(#80382,#80383,#80384,#80385),
 .UNSPECIFIED.,.F.,.F.,(4,4),(-1.8809784878858E-36,1.2),.UNSPECIFIED.);
#6253=B_SPLINE_CURVE_WITH_KNOTS('',3,(#80387,#80388,#80389,#80390,#80391,
#80392,#80393),.UNSPECIFIED.,.F.,.F.,(4,3,4),(0.,0.0247995585363297,0.0578656365847694),
 .UNSPECIFIED.);
#6254=B_SPLINE_CURVE_WITH_KNOTS('',3,(#80394,#80395,#80396,#80397),
 .UNSPECIFIED.,.F.,.F.,(4,4),(-1.2,1.8809784878858E-36),.UNSPECIFIED.);
#6255=B_SPLINE_CURVE_WITH_KNOTS('',3,(#81221,#81222,#81223,#81224,#81225,
#81226,#81227),.UNSPECIFIED.,.F.,.F.,(4,3,4),(0.,0.033066078045872,0.0578656365802761),
 .UNSPECIFIED.);
#6256=B_SPLINE_CURVE_WITH_KNOTS('',3,(#81229,#81230,#81231,#81232),
 .UNSPECIFIED.,.F.,.F.,(4,4),(-5.55111512312578E-17,1.2),.UNSPECIFIED.);
#6257=B_SPLINE_CURVE_WITH_KNOTS('',3,(#81234,#81235,#81236,#81237,#81238,
#81239,#81240),.UNSPECIFIED.,.F.,.F.,(4,3,4),(0.,0.0247995585344019,0.0578656365802711),
 .UNSPECIFIED.);
#6258=B_SPLINE_CURVE_WITH_KNOTS('',3,(#81241,#81242,#81243,#81244),
 .UNSPECIFIED.,.F.,.F.,(4,4),(-1.2,5.55111512312578E-17),.UNSPECIFIED.);
#6259=B_SPLINE_CURVE_WITH_KNOTS('',3,(#81270,#81271,#81272,#81273,#81274,
#81275,#81276),.UNSPECIFIED.,.F.,.F.,(4,3,4),(0.,0.0330660780483919,0.0578656365846859),
 .UNSPECIFIED.);
#6260=B_SPLINE_CURVE_WITH_KNOTS('',3,(#81278,#81279,#81280,#81281),
 .UNSPECIFIED.,.F.,.F.,(4,4),(9.71445146547012E-17,1.2),.UNSPECIFIED.);
#6261=B_SPLINE_CURVE_WITH_KNOTS('',3,(#81283,#81284,#81285,#81286,#81287,
#81288,#81289),.UNSPECIFIED.,.F.,.F.,(4,3,4),(0.,0.0247995585363007,0.0578656365847015),
 .UNSPECIFIED.);
#6262=B_SPLINE_CURVE_WITH_KNOTS('',3,(#81290,#81291,#81292,#81293),
 .UNSPECIFIED.,.F.,.F.,(4,4),(-1.2,-9.71445146547012E-17),.UNSPECIFIED.);
#6263=B_SPLINE_CURVE_WITH_KNOTS('',3,(#82117,#82118,#82119,#82120,#82121,
#82122,#82123),.UNSPECIFIED.,.F.,.F.,(4,3,4),(0.,0.03306607804585,0.0578656365802375),
 .UNSPECIFIED.);
#6264=B_SPLINE_CURVE_WITH_KNOTS('',3,(#82125,#82126,#82127,#82128),
 .UNSPECIFIED.,.F.,.F.,(4,4),(-8.32667268468867E-17,1.2),.UNSPECIFIED.);
#6265=B_SPLINE_CURVE_WITH_KNOTS('',3,(#82130,#82131,#82132,#82133,#82134,
#82135,#82136),.UNSPECIFIED.,.F.,.F.,(4,3,4),(0.,0.0247995585343902,0.0578656365802437),
 .UNSPECIFIED.);
#6266=B_SPLINE_CURVE_WITH_KNOTS('',3,(#82137,#82138,#82139,#82140),
 .UNSPECIFIED.,.F.,.F.,(4,4),(-1.2,8.32667268468867E-17),.UNSPECIFIED.);
#6267=B_SPLINE_CURVE_WITH_KNOTS('',3,(#82166,#82167,#82168,#82169,#82170,
#82171,#82172),.UNSPECIFIED.,.F.,.F.,(4,3,4),(0.,0.0330660780483826,0.0578656365846695),
 .UNSPECIFIED.);
#6268=B_SPLINE_CURVE_WITH_KNOTS('',3,(#82174,#82175,#82176,#82177),
 .UNSPECIFIED.,.F.,.F.,(4,4),(0.,1.2),.UNSPECIFIED.);
#6269=B_SPLINE_CURVE_WITH_KNOTS('',3,(#82179,#82180,#82181,#82182,#82183,
#82184,#82185),.UNSPECIFIED.,.F.,.F.,(4,3,4),(0.,0.0247995585362904,0.0578656365846775),
 .UNSPECIFIED.);
#6270=B_SPLINE_CURVE_WITH_KNOTS('',3,(#82186,#82187,#82188,#82189),
 .UNSPECIFIED.,.F.,.F.,(4,4),(-1.2,0.),.UNSPECIFIED.);
#6271=B_SPLINE_CURVE_WITH_KNOTS('',3,(#83013,#83014,#83015,#83016,#83017,
#83018,#83019),.UNSPECIFIED.,.F.,.F.,(4,3,4),(0.,0.0330660780458701,0.0578656365802727),
 .UNSPECIFIED.);
#6272=B_SPLINE_CURVE_WITH_KNOTS('',3,(#83021,#83022,#83023,#83024),
 .UNSPECIFIED.,.F.,.F.,(4,4),(0.,1.2),.UNSPECIFIED.);
#6273=B_SPLINE_CURVE_WITH_KNOTS('',3,(#83026,#83027,#83028,#83029,#83030,
#83031,#83032),.UNSPECIFIED.,.F.,.F.,(4,3,4),(0.,0.0247995585344047,0.0578656365802776),
 .UNSPECIFIED.);
#6274=B_SPLINE_CURVE_WITH_KNOTS('',3,(#83033,#83034,#83035,#83036),
 .UNSPECIFIED.,.F.,.F.,(4,4),(-1.2,0.),.UNSPECIFIED.);
#6275=B_SPLINE_CURVE_WITH_KNOTS('',3,(#83062,#83063,#83064,#83065,#83066,
#83067,#83068),.UNSPECIFIED.,.F.,.F.,(4,3,4),(0.,0.0330660780484355,0.0578656365847621),
 .UNSPECIFIED.);
#6276=B_SPLINE_CURVE_WITH_KNOTS('',3,(#83070,#83071,#83072,#83073),
 .UNSPECIFIED.,.F.,.F.,(4,4),(9.71445146547012E-17,1.2),.UNSPECIFIED.);
#6277=B_SPLINE_CURVE_WITH_KNOTS('',3,(#83075,#83076,#83077,#83078,#83079,
#83080,#83081),.UNSPECIFIED.,.F.,.F.,(4,3,4),(0.,0.0247995585363203,0.0578656365847474),
 .UNSPECIFIED.);
#6278=B_SPLINE_CURVE_WITH_KNOTS('',3,(#83082,#83083,#83084,#83085),
 .UNSPECIFIED.,.F.,.F.,(4,4),(-1.2,-9.71445146547012E-17),.UNSPECIFIED.);
#6279=B_SPLINE_CURVE_WITH_KNOTS('',3,(#83909,#83910,#83911,#83912,#83913,
#83914,#83915),.UNSPECIFIED.,.F.,.F.,(4,3,4),(0.,0.0330660780458469,0.057865636580232),
 .UNSPECIFIED.);
#6280=B_SPLINE_CURVE_WITH_KNOTS('',3,(#83917,#83918,#83919,#83920),
 .UNSPECIFIED.,.F.,.F.,(4,4),(-2.77555756156289E-17,1.2),.UNSPECIFIED.);
#6281=B_SPLINE_CURVE_WITH_KNOTS('',3,(#83922,#83923,#83924,#83925,#83926,
#83927,#83928),.UNSPECIFIED.,.F.,.F.,(4,3,4),(0.,0.0247995585343852,0.0578656365802322),
 .UNSPECIFIED.);
#6282=B_SPLINE_CURVE_WITH_KNOTS('',3,(#83929,#83930,#83931,#83932),
 .UNSPECIFIED.,.F.,.F.,(4,4),(-1.2,2.77555756156289E-17),.UNSPECIFIED.);
#6283=B_SPLINE_CURVE_WITH_KNOTS('',3,(#83958,#83959,#83960,#83961,#83962,
#83963,#83964),.UNSPECIFIED.,.F.,.F.,(4,3,4),(0.,0.0330660780484186,0.0578656365847326),
 .UNSPECIFIED.);
#6284=B_SPLINE_CURVE_WITH_KNOTS('',3,(#83966,#83967,#83968,#83969),
 .UNSPECIFIED.,.F.,.F.,(4,4),(9.71445146547012E-17,1.2),.UNSPECIFIED.);
#6285=B_SPLINE_CURVE_WITH_KNOTS('',3,(#83971,#83972,#83973,#83974,#83975,
#83976,#83977),.UNSPECIFIED.,.F.,.F.,(4,3,4),(0.,0.0247995585363121,0.0578656365847283),
 .UNSPECIFIED.);
#6286=B_SPLINE_CURVE_WITH_KNOTS('',3,(#83978,#83979,#83980,#83981),
 .UNSPECIFIED.,.F.,.F.,(4,4),(-1.2,-9.71445146547012E-17),.UNSPECIFIED.);
#6287=B_SPLINE_CURVE_WITH_KNOTS('',3,(#84805,#84806,#84807,#84808,#84809,
#84810,#84811),.UNSPECIFIED.,.F.,.F.,(4,3,4),(0.,0.0330660780458515,0.05786563658024),
 .UNSPECIFIED.);
#6288=B_SPLINE_CURVE_WITH_KNOTS('',3,(#84813,#84814,#84815,#84816),
 .UNSPECIFIED.,.F.,.F.,(4,4),(-9.71445146547012E-17,1.2),.UNSPECIFIED.);
#6289=B_SPLINE_CURVE_WITH_KNOTS('',3,(#84818,#84819,#84820,#84821,#84822,
#84823,#84824),.UNSPECIFIED.,.F.,.F.,(4,3,4),(0.,0.0247995585343902,0.0578656365802438),
 .UNSPECIFIED.);
#6290=B_SPLINE_CURVE_WITH_KNOTS('',3,(#84825,#84826,#84827,#84828),
 .UNSPECIFIED.,.F.,.F.,(4,4),(-1.2,9.71445146547012E-17),.UNSPECIFIED.);
#6291=B_SPLINE_CURVE_WITH_KNOTS('',3,(#84854,#84855,#84856,#84857,#84858,
#84859,#84860),.UNSPECIFIED.,.F.,.F.,(4,3,4),(0.,0.0330660780484054,0.0578656365847094),
 .UNSPECIFIED.);
#6292=B_SPLINE_CURVE_WITH_KNOTS('',3,(#84862,#84863,#84864,#84865),
 .UNSPECIFIED.,.F.,.F.,(4,4),(3.88891082483996E-17,1.2),.UNSPECIFIED.);
#6293=B_SPLINE_CURVE_WITH_KNOTS('',3,(#84867,#84868,#84869,#84870,#84871,
#84872,#84873),.UNSPECIFIED.,.F.,.F.,(4,3,4),(0.,0.0247995585363042,0.0578656365847097),
 .UNSPECIFIED.);
#6294=B_SPLINE_CURVE_WITH_KNOTS('',3,(#84874,#84875,#84876,#84877),
 .UNSPECIFIED.,.F.,.F.,(4,4),(-1.2,-3.88891082483996E-17),.UNSPECIFIED.);
#6295=B_SPLINE_CURVE_WITH_KNOTS('',3,(#85701,#85702,#85703,#85704,#85705,
#85706,#85707),.UNSPECIFIED.,.F.,.F.,(4,3,4),(0.,0.0330660780458555,0.0578656365802471),
 .UNSPECIFIED.);
#6296=B_SPLINE_CURVE_WITH_KNOTS('',3,(#85709,#85710,#85711,#85712),
 .UNSPECIFIED.,.F.,.F.,(4,4),(-1.11022302462516E-16,1.2),.UNSPECIFIED.);
#6297=B_SPLINE_CURVE_WITH_KNOTS('',3,(#85714,#85715,#85716,#85717,#85718,
#85719,#85720),.UNSPECIFIED.,.F.,.F.,(4,3,4),(0.,0.0247995585343896,0.0578656365802423),
 .UNSPECIFIED.);
#6298=B_SPLINE_CURVE_WITH_KNOTS('',3,(#85721,#85722,#85723,#85724),
 .UNSPECIFIED.,.F.,.F.,(4,4),(-1.2,1.11022302462516E-16),.UNSPECIFIED.);
#6299=B_SPLINE_CURVE_WITH_KNOTS('',3,(#85750,#85751,#85752,#85753,#85754,
#85755,#85756),.UNSPECIFIED.,.F.,.F.,(4,3,4),(0.,0.0330660780484363,0.0578656365847635),
 .UNSPECIFIED.);
#6300=B_SPLINE_CURVE_WITH_KNOTS('',3,(#85758,#85759,#85760,#85761),
 .UNSPECIFIED.,.F.,.F.,(4,4),(3.88891082483996E-17,1.2),.UNSPECIFIED.);
#6301=B_SPLINE_CURVE_WITH_KNOTS('',3,(#85763,#85764,#85765,#85766,#85767,
#85768,#85769),.UNSPECIFIED.,.F.,.F.,(4,3,4),(0.,0.0247995585363172,0.05786563658474),
 .UNSPECIFIED.);
#6302=B_SPLINE_CURVE_WITH_KNOTS('',3,(#85770,#85771,#85772,#85773),
 .UNSPECIFIED.,.F.,.F.,(4,4),(-1.2,-3.88891082483996E-17),.UNSPECIFIED.);
#6303=B_SPLINE_CURVE_WITH_KNOTS('',3,(#86597,#86598,#86599,#86600,#86601,
#86602,#86603),.UNSPECIFIED.,.F.,.F.,(4,3,4),(0.,0.033066078045885,0.0578656365802987),
 .UNSPECIFIED.);
#6304=B_SPLINE_CURVE_WITH_KNOTS('',3,(#86605,#86606,#86607,#86608),
 .UNSPECIFIED.,.F.,.F.,(4,4),(-1.8809784878848E-36,1.2),.UNSPECIFIED.);
#6305=B_SPLINE_CURVE_WITH_KNOTS('',3,(#86610,#86611,#86612,#86613,#86614,
#86615,#86616),.UNSPECIFIED.,.F.,.F.,(4,3,4),(0.,0.0247995585344127,0.0578656365802964),
 .UNSPECIFIED.);
#6306=B_SPLINE_CURVE_WITH_KNOTS('',3,(#86617,#86618,#86619,#86620),
 .UNSPECIFIED.,.F.,.F.,(4,4),(-1.2,1.8809784878848E-36),.UNSPECIFIED.);
#6307=B_SPLINE_CURVE_WITH_KNOTS('',3,(#86646,#86647,#86648,#86649,#86650,
#86651,#86652),.UNSPECIFIED.,.F.,.F.,(4,3,4),(0.,0.0330660780484386,0.0578656365847676),
 .UNSPECIFIED.);
#6308=B_SPLINE_CURVE_WITH_KNOTS('',3,(#86654,#86655,#86656,#86657),
 .UNSPECIFIED.,.F.,.F.,(4,4),(-1.11022302462516E-16,1.2),.UNSPECIFIED.);
#6309=B_SPLINE_CURVE_WITH_KNOTS('',3,(#86659,#86660,#86661,#86662,#86663,
#86664,#86665),.UNSPECIFIED.,.F.,.F.,(4,3,4),(0.,0.024799558536317,0.0578656365847397),
 .UNSPECIFIED.);
#6310=B_SPLINE_CURVE_WITH_KNOTS('',3,(#86666,#86667,#86668,#86669),
 .UNSPECIFIED.,.F.,.F.,(4,4),(-1.2,1.11022302462516E-16),.UNSPECIFIED.);
#6311=B_SPLINE_CURVE_WITH_KNOTS('',3,(#87493,#87494,#87495,#87496,#87497,
#87498,#87499),.UNSPECIFIED.,.F.,.F.,(4,3,4),(0.,0.0330660780458761,0.0578656365802832),
 .UNSPECIFIED.);
#6312=B_SPLINE_CURVE_WITH_KNOTS('',3,(#87501,#87502,#87503,#87504),
 .UNSPECIFIED.,.F.,.F.,(4,4),(-8.32667268468867E-17,1.2),.UNSPECIFIED.);
#6313=B_SPLINE_CURVE_WITH_KNOTS('',3,(#87506,#87507,#87508,#87509,#87510,
#87511,#87512),.UNSPECIFIED.,.F.,.F.,(4,3,4),(0.,0.0247995585344117,0.0578656365802939),
 .UNSPECIFIED.);
#6314=B_SPLINE_CURVE_WITH_KNOTS('',3,(#87513,#87514,#87515,#87516),
 .UNSPECIFIED.,.F.,.F.,(4,4),(-1.2,8.32667268468867E-17),.UNSPECIFIED.);
#6315=B_SPLINE_CURVE_WITH_KNOTS('',3,(#87542,#87543,#87544,#87545,#87546,
#87547,#87548),.UNSPECIFIED.,.F.,.F.,(4,3,4),(0.,0.0330660780484119,0.0578656365847208),
 .UNSPECIFIED.);
#6316=B_SPLINE_CURVE_WITH_KNOTS('',3,(#87550,#87551,#87552,#87553),
 .UNSPECIFIED.,.F.,.F.,(4,4),(9.71445146547012E-17,1.2),.UNSPECIFIED.);
#6317=B_SPLINE_CURVE_WITH_KNOTS('',3,(#87555,#87556,#87557,#87558,#87559,
#87560,#87561),.UNSPECIFIED.,.F.,.F.,(4,3,4),(0.,0.0247995585363125,0.0578656365847292),
 .UNSPECIFIED.);
#6318=B_SPLINE_CURVE_WITH_KNOTS('',3,(#87562,#87563,#87564,#87565),
 .UNSPECIFIED.,.F.,.F.,(4,4),(-1.2,-9.71445146547012E-17),.UNSPECIFIED.);
#6319=B_SPLINE_CURVE_WITH_KNOTS('',3,(#88389,#88390,#88391,#88392,#88393,
#88394,#88395),.UNSPECIFIED.,.F.,.F.,(4,3,4),(0.,0.033066078045965,0.0578656365804388),
 .UNSPECIFIED.);
#6320=B_SPLINE_CURVE_WITH_KNOTS('',3,(#88397,#88398,#88399,#88400),
 .UNSPECIFIED.,.F.,.F.,(4,4),(2.77555756156289E-17,1.2),.UNSPECIFIED.);
#6321=B_SPLINE_CURVE_WITH_KNOTS('',3,(#88402,#88403,#88404,#88405,#88406,
#88407,#88408),.UNSPECIFIED.,.F.,.F.,(4,3,4),(0.,0.024799558534469,0.0578656365804277),
 .UNSPECIFIED.);
#6322=B_SPLINE_CURVE_WITH_KNOTS('',3,(#88409,#88410,#88411,#88412),
 .UNSPECIFIED.,.F.,.F.,(4,4),(-1.2,-2.77555756156289E-17),.UNSPECIFIED.);
#6323=B_SPLINE_CURVE_WITH_KNOTS('',3,(#88438,#88439,#88440,#88441,#88442,
#88443,#88444),.UNSPECIFIED.,.F.,.F.,(4,3,4),(0.,0.0330660780484208,0.0578656365847365),
 .UNSPECIFIED.);
#6324=B_SPLINE_CURVE_WITH_KNOTS('',3,(#88446,#88447,#88448,#88449),
 .UNSPECIFIED.,.F.,.F.,(4,4),(-1.38777878078145E-16,1.2),.UNSPECIFIED.);
#6325=B_SPLINE_CURVE_WITH_KNOTS('',3,(#88451,#88452,#88453,#88454,#88455,
#88456,#88457),.UNSPECIFIED.,.F.,.F.,(4,3,4),(0.,0.0247995585363145,0.0578656365847338),
 .UNSPECIFIED.);
#6326=B_SPLINE_CURVE_WITH_KNOTS('',3,(#88458,#88459,#88460,#88461),
 .UNSPECIFIED.,.F.,.F.,(4,4),(-1.2,1.38777878078145E-16),.UNSPECIFIED.);
#6327=B_SPLINE_CURVE_WITH_KNOTS('',3,(#89285,#89286,#89287,#89288,#89289,
#89290,#89291),.UNSPECIFIED.,.F.,.F.,(4,3,4),(0.,0.0330660780458555,0.0578656365802471),
 .UNSPECIFIED.);
#6328=B_SPLINE_CURVE_WITH_KNOTS('',3,(#89293,#89294,#89295,#89296),
 .UNSPECIFIED.,.F.,.F.,(4,4),(2.77555756156289E-17,1.2),.UNSPECIFIED.);
#6329=B_SPLINE_CURVE_WITH_KNOTS('',3,(#89298,#89299,#89300,#89301,#89302,
#89303,#89304),.UNSPECIFIED.,.F.,.F.,(4,3,4),(0.,0.0247995585343909,0.0578656365802454),
 .UNSPECIFIED.);
#6330=B_SPLINE_CURVE_WITH_KNOTS('',3,(#89305,#89306,#89307,#89308),
 .UNSPECIFIED.,.F.,.F.,(4,4),(-1.2,-2.77555756156289E-17),.UNSPECIFIED.);
#6331=B_SPLINE_CURVE_WITH_KNOTS('',3,(#89334,#89335,#89336,#89337,#89338,
#89339,#89340),.UNSPECIFIED.,.F.,.F.,(4,3,4),(0.,0.0330660780484046,0.0578656365847081),
 .UNSPECIFIED.);
#6332=B_SPLINE_CURVE_WITH_KNOTS('',3,(#89342,#89343,#89344,#89345),
 .UNSPECIFIED.,.F.,.F.,(4,4),(9.71445146547012E-17,1.2),.UNSPECIFIED.);
#6333=B_SPLINE_CURVE_WITH_KNOTS('',3,(#89347,#89348,#89349,#89350,#89351,
#89352,#89353),.UNSPECIFIED.,.F.,.F.,(4,3,4),(0.,0.0247995585363076,0.0578656365847176),
 .UNSPECIFIED.);
#6334=B_SPLINE_CURVE_WITH_KNOTS('',3,(#89354,#89355,#89356,#89357),
 .UNSPECIFIED.,.F.,.F.,(4,4),(-1.2,-9.71445146547012E-17),.UNSPECIFIED.);
#6335=B_SPLINE_CURVE_WITH_KNOTS('',3,(#90181,#90182,#90183,#90184,#90185,
#90186,#90187),.UNSPECIFIED.,.F.,.F.,(4,3,4),(0.,0.0330660780458503,0.057865636580238),
 .UNSPECIFIED.);
#6336=B_SPLINE_CURVE_WITH_KNOTS('',3,(#90189,#90190,#90191,#90192),
 .UNSPECIFIED.,.F.,.F.,(4,4),(-7.5239139515392E-36,1.2),.UNSPECIFIED.);
#6337=B_SPLINE_CURVE_WITH_KNOTS('',3,(#90194,#90195,#90196,#90197,#90198,
#90199,#90200),.UNSPECIFIED.,.F.,.F.,(4,3,4),(0.,0.0247995585343863,0.0578656365802348),
 .UNSPECIFIED.);
#6338=B_SPLINE_CURVE_WITH_KNOTS('',3,(#90201,#90202,#90203,#90204),
 .UNSPECIFIED.,.F.,.F.,(4,4),(-1.2,7.5239139515392E-36),.UNSPECIFIED.);
#6339=B_SPLINE_CURVE_WITH_KNOTS('',3,(#90230,#90231,#90232,#90233,#90234,
#90235,#90236),.UNSPECIFIED.,.F.,.F.,(4,3,4),(0.,0.0330660780483922,0.0578656365846863),
 .UNSPECIFIED.);
#6340=B_SPLINE_CURVE_WITH_KNOTS('',3,(#90238,#90239,#90240,#90241),
 .UNSPECIFIED.,.F.,.F.,(4,4),(8.05224716718429E-17,1.2),.UNSPECIFIED.);
#6341=B_SPLINE_CURVE_WITH_KNOTS('',3,(#90243,#90244,#90245,#90246,#90247,
#90248,#90249),.UNSPECIFIED.,.F.,.F.,(4,3,4),(0.,0.0247995585363117,0.0578656365847273),
 .UNSPECIFIED.);
#6342=B_SPLINE_CURVE_WITH_KNOTS('',3,(#90250,#90251,#90252,#90253),
 .UNSPECIFIED.,.F.,.F.,(4,4),(-1.2,-8.05224716718429E-17),.UNSPECIFIED.);
#6343=B_SPLINE_CURVE_WITH_KNOTS('',3,(#91077,#91078,#91079,#91080,#91081,
#91082,#91083),.UNSPECIFIED.,.F.,.F.,(4,3,4),(0.,0.0330660780458931,0.057865636580313),
 .UNSPECIFIED.);
#6344=B_SPLINE_CURVE_WITH_KNOTS('',3,(#91085,#91086,#91087,#91088),
 .UNSPECIFIED.,.F.,.F.,(4,4),(0.,1.2),.UNSPECIFIED.);
#6345=B_SPLINE_CURVE_WITH_KNOTS('',3,(#91090,#91091,#91092,#91093,#91094,
#91095,#91096),.UNSPECIFIED.,.F.,.F.,(4,3,4),(0.,0.0247995585344171,0.0578656365803065),
 .UNSPECIFIED.);
#6346=B_SPLINE_CURVE_WITH_KNOTS('',3,(#91097,#91098,#91099,#91100),
 .UNSPECIFIED.,.F.,.F.,(4,4),(-1.2,0.),.UNSPECIFIED.);
#6347=B_SPLINE_CURVE_WITH_KNOTS('',3,(#91126,#91127,#91128,#91129,#91130,
#91131,#91132),.UNSPECIFIED.,.F.,.F.,(4,3,4),(0.,0.03306607804841,0.0578656365847175),
 .UNSPECIFIED.);
#6348=B_SPLINE_CURVE_WITH_KNOTS('',3,(#91134,#91135,#91136,#91137),
 .UNSPECIFIED.,.F.,.F.,(4,4),(9.71445146547012E-17,1.2),.UNSPECIFIED.);
#6349=B_SPLINE_CURVE_WITH_KNOTS('',3,(#91139,#91140,#91141,#91142,#91143,
#91144,#91145),.UNSPECIFIED.,.F.,.F.,(4,3,4),(0.,0.0247995585363106,0.0578656365847246),
 .UNSPECIFIED.);
#6350=B_SPLINE_CURVE_WITH_KNOTS('',3,(#91146,#91147,#91148,#91149),
 .UNSPECIFIED.,.F.,.F.,(4,4),(-1.2,-9.71445146547012E-17),.UNSPECIFIED.);
#6351=B_SPLINE_CURVE_WITH_KNOTS('',3,(#91973,#91974,#91975,#91976,#91977,
#91978,#91979),.UNSPECIFIED.,.F.,.F.,(4,3,4),(0.,0.0330660780458883,0.0578656365803045),
 .UNSPECIFIED.);
#6352=B_SPLINE_CURVE_WITH_KNOTS('',3,(#91981,#91982,#91983,#91984),
 .UNSPECIFIED.,.F.,.F.,(4,4),(-1.49437708898837E-16,1.2),.UNSPECIFIED.);
#6353=B_SPLINE_CURVE_WITH_KNOTS('',3,(#91986,#91987,#91988,#91989,#91990,
#91991,#91992),.UNSPECIFIED.,.F.,.F.,(4,3,4),(0.,0.0247995585344198,0.0578656365803129),
 .UNSPECIFIED.);
#6354=B_SPLINE_CURVE_WITH_KNOTS('',3,(#91993,#91994,#91995,#91996),
 .UNSPECIFIED.,.F.,.F.,(4,4),(-1.2,1.49437708898837E-16),.UNSPECIFIED.);
#6355=B_SPLINE_CURVE_WITH_KNOTS('',3,(#92022,#92023,#92024,#92025,#92026,
#92027,#92028),.UNSPECIFIED.,.F.,.F.,(4,3,4),(0.,0.0330660780483646,0.057865636584638),
 .UNSPECIFIED.);
#6356=B_SPLINE_CURVE_WITH_KNOTS('',3,(#92030,#92031,#92032,#92033),
 .UNSPECIFIED.,.F.,.F.,(4,4),(5.55111512312578E-17,1.2),.UNSPECIFIED.);
#6357=B_SPLINE_CURVE_WITH_KNOTS('',3,(#92035,#92036,#92037,#92038,#92039,
#92040,#92041),.UNSPECIFIED.,.F.,.F.,(4,3,4),(0.,0.0247995585362812,0.057865636584656),
 .UNSPECIFIED.);
#6358=B_SPLINE_CURVE_WITH_KNOTS('',3,(#92042,#92043,#92044,#92045),
 .UNSPECIFIED.,.F.,.F.,(4,4),(-1.2,-5.55111512312578E-17),.UNSPECIFIED.);
#6359=B_SPLINE_CURVE_WITH_KNOTS('',3,(#92869,#92870,#92871,#92872,#92873,
#92874,#92875),.UNSPECIFIED.,.F.,.F.,(4,3,4),(0.,0.0330660780458722,0.0578656365802764),
 .UNSPECIFIED.);
#6360=B_SPLINE_CURVE_WITH_KNOTS('',3,(#92877,#92878,#92879,#92880),
 .UNSPECIFIED.,.F.,.F.,(4,4),(-8.32667268468867E-17,1.2),.UNSPECIFIED.);
#6361=B_SPLINE_CURVE_WITH_KNOTS('',3,(#92882,#92883,#92884,#92885,#92886,
#92887,#92888),.UNSPECIFIED.,.F.,.F.,(4,3,4),(0.,0.0247995585344042,0.0578656365802765),
 .UNSPECIFIED.);
#6362=B_SPLINE_CURVE_WITH_KNOTS('',3,(#92889,#92890,#92891,#92892),
 .UNSPECIFIED.,.F.,.F.,(4,4),(-1.2,8.32667268468867E-17),.UNSPECIFIED.);
#6363=B_SPLINE_CURVE_WITH_KNOTS('',3,(#92918,#92919,#92920,#92921,#92922,
#92923,#92924),.UNSPECIFIED.,.F.,.F.,(4,3,4),(0.,0.0330660780483716,0.0578656365846503),
 .UNSPECIFIED.);
#6364=B_SPLINE_CURVE_WITH_KNOTS('',3,(#92926,#92927,#92928,#92929),
 .UNSPECIFIED.,.F.,.F.,(4,4),(9.71445146547012E-17,1.2),.UNSPECIFIED.);
#6365=B_SPLINE_CURVE_WITH_KNOTS('',3,(#92931,#92932,#92933,#92934,#92935,
#92936,#92937),.UNSPECIFIED.,.F.,.F.,(4,3,4),(0.,0.0247995585362986,0.0578656365846968),
 .UNSPECIFIED.);
#6366=B_SPLINE_CURVE_WITH_KNOTS('',3,(#92938,#92939,#92940,#92941),
 .UNSPECIFIED.,.F.,.F.,(4,4),(-1.2,-9.71445146547012E-17),.UNSPECIFIED.);
#6367=B_SPLINE_CURVE_WITH_KNOTS('',3,(#93765,#93766,#93767,#93768,#93769,
#93770,#93771),.UNSPECIFIED.,.F.,.F.,(4,3,4),(0.,0.0330660780458217,0.057865636580188),
 .UNSPECIFIED.);
#6368=B_SPLINE_CURVE_WITH_KNOTS('',3,(#93773,#93774,#93775,#93776),
 .UNSPECIFIED.,.F.,.F.,(4,4),(-8.32667268468868E-17,1.2),.UNSPECIFIED.);
#6369=B_SPLINE_CURVE_WITH_KNOTS('',3,(#93778,#93779,#93780,#93781,#93782,
#93783,#93784),.UNSPECIFIED.,.F.,.F.,(4,3,4),(0.,0.0247995585343724,0.0578656365802022),
 .UNSPECIFIED.);
#6370=B_SPLINE_CURVE_WITH_KNOTS('',3,(#93785,#93786,#93787,#93788),
 .UNSPECIFIED.,.F.,.F.,(4,4),(-1.2,8.32667268468868E-17),.UNSPECIFIED.);
#6371=B_SPLINE_CURVE_WITH_KNOTS('',3,(#93814,#93815,#93816,#93817,#93818,
#93819,#93820),.UNSPECIFIED.,.F.,.F.,(4,3,4),(0.,0.0330660780484519,0.0578656365847908),
 .UNSPECIFIED.);
#6372=B_SPLINE_CURVE_WITH_KNOTS('',3,(#93822,#93823,#93824,#93825),
 .UNSPECIFIED.,.F.,.F.,(4,4),(-8.32667268468867E-17,1.2),.UNSPECIFIED.);
#6373=B_SPLINE_CURVE_WITH_KNOTS('',3,(#93827,#93828,#93829,#93830,#93831,
#93832,#93833),.UNSPECIFIED.,.F.,.F.,(4,3,4),(0.,0.0247995585363362,0.0578656365847844),
 .UNSPECIFIED.);
#6374=B_SPLINE_CURVE_WITH_KNOTS('',3,(#93834,#93835,#93836,#93837),
 .UNSPECIFIED.,.F.,.F.,(4,4),(-1.2,8.32667268468867E-17),.UNSPECIFIED.);
#6375=B_SPLINE_CURVE_WITH_KNOTS('',3,(#94661,#94662,#94663,#94664,#94665,
#94666,#94667),.UNSPECIFIED.,.F.,.F.,(4,3,4),(0.,0.0330660780458195,0.0578656365801842),
 .UNSPECIFIED.);
#6376=B_SPLINE_CURVE_WITH_KNOTS('',3,(#94669,#94670,#94671,#94672),
 .UNSPECIFIED.,.F.,.F.,(4,4),(2.77555756156289E-17,1.2),.UNSPECIFIED.);
#6377=B_SPLINE_CURVE_WITH_KNOTS('',3,(#94674,#94675,#94676,#94677,#94678,
#94679,#94680),.UNSPECIFIED.,.F.,.F.,(4,3,4),(0.,0.024799558534367,0.0578656365801897),
 .UNSPECIFIED.);
#6378=B_SPLINE_CURVE_WITH_KNOTS('',3,(#94681,#94682,#94683,#94684),
 .UNSPECIFIED.,.F.,.F.,(4,4),(-1.2,-2.77555756156289E-17),.UNSPECIFIED.);
#6379=B_SPLINE_CURVE_WITH_KNOTS('',3,(#94710,#94711,#94712,#94713,#94714,
#94715,#94716),.UNSPECIFIED.,.F.,.F.,(4,3,4),(0.,0.0330660780484102,0.0578656365847178),
 .UNSPECIFIED.);
#6380=B_SPLINE_CURVE_WITH_KNOTS('',3,(#94718,#94719,#94720,#94721),
 .UNSPECIFIED.,.F.,.F.,(4,4),(8.32667268468867E-17,1.2),.UNSPECIFIED.);
#6381=B_SPLINE_CURVE_WITH_KNOTS('',3,(#94723,#94724,#94725,#94726,#94727,
#94728,#94729),.UNSPECIFIED.,.F.,.F.,(4,3,4),(0.,0.0247995585363047,0.057865636584711),
 .UNSPECIFIED.);
#6382=B_SPLINE_CURVE_WITH_KNOTS('',3,(#94730,#94731,#94732,#94733),
 .UNSPECIFIED.,.F.,.F.,(4,4),(-1.2,-8.32667268468867E-17),.UNSPECIFIED.);
#6383=B_SPLINE_CURVE_WITH_KNOTS('',3,(#95557,#95558,#95559,#95560,#95561,
#95562,#95563),.UNSPECIFIED.,.F.,.F.,(4,3,4),(0.,0.033066078045887,0.0578656365803023),
 .UNSPECIFIED.);
#6384=B_SPLINE_CURVE_WITH_KNOTS('',3,(#95565,#95566,#95567,#95568),
 .UNSPECIFIED.,.F.,.F.,(4,4),(2.77555756156289E-17,1.2),.UNSPECIFIED.);
#6385=B_SPLINE_CURVE_WITH_KNOTS('',3,(#95570,#95571,#95572,#95573,#95574,
#95575,#95576),.UNSPECIFIED.,.F.,.F.,(4,3,4),(0.,0.0247995585344129,0.0578656365802968),
 .UNSPECIFIED.);
#6386=B_SPLINE_CURVE_WITH_KNOTS('',3,(#95577,#95578,#95579,#95580),
 .UNSPECIFIED.,.F.,.F.,(4,4),(-1.2,-2.77555756156289E-17),.UNSPECIFIED.);
#6387=B_SPLINE_CURVE_WITH_KNOTS('',3,(#95606,#95607,#95608,#95609,#95610,
#95611,#95612),.UNSPECIFIED.,.F.,.F.,(4,3,4),(0.,0.0330660780484079,0.0578656365847137),
 .UNSPECIFIED.);
#6388=B_SPLINE_CURVE_WITH_KNOTS('',3,(#95614,#95615,#95616,#95617),
 .UNSPECIFIED.,.F.,.F.,(4,4),(5.55111512312578E-17,1.2),.UNSPECIFIED.);
#6389=B_SPLINE_CURVE_WITH_KNOTS('',3,(#95619,#95620,#95621,#95622,#95623,
#95624,#95625),.UNSPECIFIED.,.F.,.F.,(4,3,4),(0.,0.0247995585363057,0.0578656365847134),
 .UNSPECIFIED.);
#6390=B_SPLINE_CURVE_WITH_KNOTS('',3,(#95626,#95627,#95628,#95629),
 .UNSPECIFIED.,.F.,.F.,(4,4),(-1.2,-5.55111512312578E-17),.UNSPECIFIED.);
#6391=B_SPLINE_CURVE_WITH_KNOTS('',3,(#96453,#96454,#96455,#96456,#96457,
#96458,#96459),.UNSPECIFIED.,.F.,.F.,(4,3,4),(0.,0.0330660780458631,0.0578656365802604),
 .UNSPECIFIED.);
#6392=B_SPLINE_CURVE_WITH_KNOTS('',3,(#96461,#96462,#96463,#96464),
 .UNSPECIFIED.,.F.,.F.,(4,4),(-1.38777878078145E-16,1.2),.UNSPECIFIED.);
#6393=B_SPLINE_CURVE_WITH_KNOTS('',3,(#96466,#96467,#96468,#96469,#96470,
#96471,#96472),.UNSPECIFIED.,.F.,.F.,(4,3,4),(0.,0.0247995585343987,0.0578656365802637),
 .UNSPECIFIED.);
#6394=B_SPLINE_CURVE_WITH_KNOTS('',3,(#96473,#96474,#96475,#96476),
 .UNSPECIFIED.,.F.,.F.,(4,4),(-1.2,1.38777878078145E-16),.UNSPECIFIED.);
#6395=B_SPLINE_CURVE_WITH_KNOTS('',3,(#96502,#96503,#96504,#96505,#96506,
#96507,#96508),.UNSPECIFIED.,.F.,.F.,(4,3,4),(0.,0.0330660780483721,0.0578656365846511),
 .UNSPECIFIED.);
#6396=B_SPLINE_CURVE_WITH_KNOTS('',3,(#96510,#96511,#96512,#96513),
 .UNSPECIFIED.,.F.,.F.,(4,4),(2.77555756156289E-17,1.2),.UNSPECIFIED.);
#6397=B_SPLINE_CURVE_WITH_KNOTS('',3,(#96515,#96516,#96517,#96518,#96519,
#96520,#96521),.UNSPECIFIED.,.F.,.F.,(4,3,4),(0.,0.0247995585362904,0.0578656365846776),
 .UNSPECIFIED.);
#6398=B_SPLINE_CURVE_WITH_KNOTS('',3,(#96522,#96523,#96524,#96525),
 .UNSPECIFIED.,.F.,.F.,(4,4),(-1.2,-2.77555756156289E-17),.UNSPECIFIED.);
#6399=B_SPLINE_CURVE_WITH_KNOTS('',3,(#97349,#97350,#97351,#97352,#97353,
#97354,#97355),.UNSPECIFIED.,.F.,.F.,(4,3,4),(0.,0.0330660780458673,0.0578656365802679),
 .UNSPECIFIED.);
#6400=B_SPLINE_CURVE_WITH_KNOTS('',3,(#97357,#97358,#97359,#97360),
 .UNSPECIFIED.,.F.,.F.,(4,4),(0.,1.2),.UNSPECIFIED.);
#6401=B_SPLINE_CURVE_WITH_KNOTS('',3,(#97362,#97363,#97364,#97365,#97366,
#97367,#97368),.UNSPECIFIED.,.F.,.F.,(4,3,4),(0.,0.0247995585344041,0.0578656365802761),
 .UNSPECIFIED.);
#6402=B_SPLINE_CURVE_WITH_KNOTS('',3,(#97369,#97370,#97371,#97372),
 .UNSPECIFIED.,.F.,.F.,(4,4),(-1.2,0.),.UNSPECIFIED.);
#6403=B_SPLINE_CURVE_WITH_KNOTS('',3,(#97398,#97399,#97400,#97401,#97402,
#97403,#97404),.UNSPECIFIED.,.F.,.F.,(4,3,4),(0.,0.0330660780484141,0.0578656365847246),
 .UNSPECIFIED.);
#6404=B_SPLINE_CURVE_WITH_KNOTS('',3,(#97406,#97407,#97408,#97409),
 .UNSPECIFIED.,.F.,.F.,(4,4),(1.66533453693773E-16,1.2),.UNSPECIFIED.);
#6405=B_SPLINE_CURVE_WITH_KNOTS('',3,(#97411,#97412,#97413,#97414,#97415,
#97416,#97417),.UNSPECIFIED.,.F.,.F.,(4,3,4),(0.,0.024799558536313,0.0578656365847304),
 .UNSPECIFIED.);
#6406=B_SPLINE_CURVE_WITH_KNOTS('',3,(#97418,#97419,#97420,#97421),
 .UNSPECIFIED.,.F.,.F.,(4,4),(-1.2,-1.66533453693773E-16),.UNSPECIFIED.);
#6407=B_SPLINE_CURVE_WITH_KNOTS('',3,(#98245,#98246,#98247,#98248,#98249,
#98250,#98251),.UNSPECIFIED.,.F.,.F.,(4,3,4),(0.,0.0330660780458716,0.0578656365802753),
 .UNSPECIFIED.);
#6408=B_SPLINE_CURVE_WITH_KNOTS('',3,(#98253,#98254,#98255,#98256),
 .UNSPECIFIED.,.F.,.F.,(4,4),(-8.32667268468867E-17,1.2),.UNSPECIFIED.);
#6409=B_SPLINE_CURVE_WITH_KNOTS('',3,(#98258,#98259,#98260,#98261,#98262,
#98263,#98264),.UNSPECIFIED.,.F.,.F.,(4,3,4),(0.,0.0247995585344033,0.0578656365802743),
 .UNSPECIFIED.);
#6410=B_SPLINE_CURVE_WITH_KNOTS('',3,(#98265,#98266,#98267,#98268),
 .UNSPECIFIED.,.F.,.F.,(4,4),(-1.2,8.32667268468867E-17),.UNSPECIFIED.);
#6411=B_SPLINE_CURVE_WITH_KNOTS('',3,(#98294,#98295,#98296,#98297,#98298,
#98299,#98300),.UNSPECIFIED.,.F.,.F.,(4,3,4),(0.,0.0330660780484192,0.0578656365847337),
 .UNSPECIFIED.);
#6412=B_SPLINE_CURVE_WITH_KNOTS('',3,(#98302,#98303,#98304,#98305),
 .UNSPECIFIED.,.F.,.F.,(4,4),(9.71445146547012E-17,1.2),.UNSPECIFIED.);
#6413=B_SPLINE_CURVE_WITH_KNOTS('',3,(#98307,#98308,#98309,#98310,#98311,
#98312,#98313),.UNSPECIFIED.,.F.,.F.,(4,3,4),(0.,0.0247995585363099,0.0578656365847232),
 .UNSPECIFIED.);
#6414=B_SPLINE_CURVE_WITH_KNOTS('',3,(#98314,#98315,#98316,#98317),
 .UNSPECIFIED.,.F.,.F.,(4,4),(-1.2,-9.71445146547012E-17),.UNSPECIFIED.);
#6415=B_SPLINE_CURVE_WITH_KNOTS('',3,(#99141,#99142,#99143,#99144,#99145,
#99146,#99147),.UNSPECIFIED.,.F.,.F.,(4,3,4),(0.,0.0330660780458584,0.0578656365802523),
 .UNSPECIFIED.);
#6416=B_SPLINE_CURVE_WITH_KNOTS('',3,(#99149,#99150,#99151,#99152),
 .UNSPECIFIED.,.F.,.F.,(4,4),(-2.03133674691991E-35,1.2),.UNSPECIFIED.);
#6417=B_SPLINE_CURVE_WITH_KNOTS('',3,(#99154,#99155,#99156,#99157,#99158,
#99159,#99160),.UNSPECIFIED.,.F.,.F.,(4,3,4),(0.,0.0247995585343932,0.0578656365802508),
 .UNSPECIFIED.);
#6418=B_SPLINE_CURVE_WITH_KNOTS('',3,(#99161,#99162,#99163,#99164),
 .UNSPECIFIED.,.F.,.F.,(4,4),(-1.2,2.03133674691991E-35),.UNSPECIFIED.);
#6419=B_SPLINE_CURVE_WITH_KNOTS('',3,(#99190,#99191,#99192,#99193,#99194,
#99195,#99196),.UNSPECIFIED.,.F.,.F.,(4,3,4),(0.,0.033066078048434,0.0578656365847594),
 .UNSPECIFIED.);
#6420=B_SPLINE_CURVE_WITH_KNOTS('',3,(#99198,#99199,#99200,#99201),
 .UNSPECIFIED.,.F.,.F.,(4,4),(-1.83155496676632E-16,1.2),.UNSPECIFIED.);
#6421=B_SPLINE_CURVE_WITH_KNOTS('',3,(#99203,#99204,#99205,#99206,#99207,
#99208,#99209),.UNSPECIFIED.,.F.,.F.,(4,3,4),(0.,0.0247995585363058,0.0578656365847137),
 .UNSPECIFIED.);
#6422=B_SPLINE_CURVE_WITH_KNOTS('',3,(#99210,#99211,#99212,#99213),
 .UNSPECIFIED.,.F.,.F.,(4,4),(-1.2,1.83155496676632E-16),.UNSPECIFIED.);
#6423=B_SPLINE_CURVE_WITH_KNOTS('',3,(#100037,#100038,#100039,#100040,#100041,
#100042,#100043),.UNSPECIFIED.,.F.,.F.,(4,3,4),(0.,0.0330660780458696,0.0578656365802718),
 .UNSPECIFIED.);
#6424=B_SPLINE_CURVE_WITH_KNOTS('',3,(#100045,#100046,#100047,#100048),
 .UNSPECIFIED.,.F.,.F.,(4,4),(-1.38777878078145E-16,1.2),.UNSPECIFIED.);
#6425=B_SPLINE_CURVE_WITH_KNOTS('',3,(#100050,#100051,#100052,#100053,#100054,
#100055,#100056),.UNSPECIFIED.,.F.,.F.,(4,3,4),(0.,0.0247995585343985,0.0578656365802632),
 .UNSPECIFIED.);
#6426=B_SPLINE_CURVE_WITH_KNOTS('',3,(#100057,#100058,#100059,#100060),
 .UNSPECIFIED.,.F.,.F.,(4,4),(-1.2,1.38777878078145E-16),.UNSPECIFIED.);
#6427=B_SPLINE_CURVE_WITH_KNOTS('',3,(#100086,#100087,#100088,#100089,#100090,
#100091,#100092),.UNSPECIFIED.,.F.,.F.,(4,3,4),(0.,0.0330660780483983,0.0578656365846971),
 .UNSPECIFIED.);
#6428=B_SPLINE_CURVE_WITH_KNOTS('',3,(#100094,#100095,#100096,#100097),
 .UNSPECIFIED.,.F.,.F.,(4,4),(1.66533453693773E-16,1.2),.UNSPECIFIED.);
#6429=B_SPLINE_CURVE_WITH_KNOTS('',3,(#100099,#100100,#100101,#100102,#100103,
#100104,#100105),.UNSPECIFIED.,.F.,.F.,(4,3,4),(0.,0.0247995585362993,0.0578656365846983),
 .UNSPECIFIED.);
#6430=B_SPLINE_CURVE_WITH_KNOTS('',3,(#100106,#100107,#100108,#100109),
 .UNSPECIFIED.,.F.,.F.,(4,4),(-1.2,-1.66533453693773E-16),.UNSPECIFIED.);
#6431=B_SPLINE_CURVE_WITH_KNOTS('',3,(#100933,#100934,#100935,#100936,#100937,
#100938,#100939),.UNSPECIFIED.,.F.,.F.,(4,3,4),(0.,0.0330660780458496,0.0578656365802369),
 .UNSPECIFIED.);
#6432=B_SPLINE_CURVE_WITH_KNOTS('',3,(#100941,#100942,#100943,#100944),
 .UNSPECIFIED.,.F.,.F.,(4,4),(0.,1.2),.UNSPECIFIED.);
#6433=B_SPLINE_CURVE_WITH_KNOTS('',3,(#100946,#100947,#100948,#100949,#100950,
#100951,#100952),.UNSPECIFIED.,.F.,.F.,(4,3,4),(0.,0.0247995585343804,0.0578656365802209),
 .UNSPECIFIED.);
#6434=B_SPLINE_CURVE_WITH_KNOTS('',3,(#100953,#100954,#100955,#100956),
 .UNSPECIFIED.,.F.,.F.,(4,4),(-1.2,0.),.UNSPECIFIED.);
#6435=B_SPLINE_CURVE_WITH_KNOTS('',3,(#100982,#100983,#100984,#100985,#100986,
#100987,#100988),.UNSPECIFIED.,.F.,.F.,(4,3,4),(0.,0.0330660780484024,0.0578656365847041),
 .UNSPECIFIED.);
#6436=B_SPLINE_CURVE_WITH_KNOTS('',3,(#100990,#100991,#100992,#100993),
 .UNSPECIFIED.,.F.,.F.,(4,4),(-1.38777878078145E-16,1.2),.UNSPECIFIED.);
#6437=B_SPLINE_CURVE_WITH_KNOTS('',3,(#100995,#100996,#100997,#100998,#100999,
#101000,#101001),.UNSPECIFIED.,.F.,.F.,(4,3,4),(0.,0.0247995585362999,0.0578656365846998),
 .UNSPECIFIED.);
#6438=B_SPLINE_CURVE_WITH_KNOTS('',3,(#101002,#101003,#101004,#101005),
 .UNSPECIFIED.,.F.,.F.,(4,4),(-1.2,1.38777878078145E-16),.UNSPECIFIED.);
#6439=B_SPLINE_CURVE_WITH_KNOTS('',3,(#101829,#101830,#101831,#101832,#101833,
#101834,#101835),.UNSPECIFIED.,.F.,.F.,(4,3,4),(0.,0.033066078045876,0.057865636580283),
 .UNSPECIFIED.);
#6440=B_SPLINE_CURVE_WITH_KNOTS('',3,(#101837,#101838,#101839,#101840),
 .UNSPECIFIED.,.F.,.F.,(4,4),(-1.88097848788491E-36,1.2),.UNSPECIFIED.);
#6441=B_SPLINE_CURVE_WITH_KNOTS('',3,(#101842,#101843,#101844,#101845,#101846,
#101847,#101848),.UNSPECIFIED.,.F.,.F.,(4,3,4),(0.,0.0247995585344058,0.0578656365802801),
 .UNSPECIFIED.);
#6442=B_SPLINE_CURVE_WITH_KNOTS('',3,(#101849,#101850,#101851,#101852),
 .UNSPECIFIED.,.F.,.F.,(4,4),(-1.2,1.88097848788491E-36),.UNSPECIFIED.);
#6443=B_SPLINE_CURVE_WITH_KNOTS('',3,(#101878,#101879,#101880,#101881,#101882,
#101883,#101884),.UNSPECIFIED.,.F.,.F.,(4,3,4),(0.,0.0330660780484209,0.0578656365847367),
 .UNSPECIFIED.);
#6444=B_SPLINE_CURVE_WITH_KNOTS('',3,(#101886,#101887,#101888,#101889),
 .UNSPECIFIED.,.F.,.F.,(4,4),(2.77555756156289E-17,1.2),.UNSPECIFIED.);
#6445=B_SPLINE_CURVE_WITH_KNOTS('',3,(#101891,#101892,#101893,#101894,#101895,
#101896,#101897),.UNSPECIFIED.,.F.,.F.,(4,3,4),(0.,0.0247995585363132,0.0578656365847308),
 .UNSPECIFIED.);
#6446=B_SPLINE_CURVE_WITH_KNOTS('',3,(#101898,#101899,#101900,#101901),
 .UNSPECIFIED.,.F.,.F.,(4,4),(-1.2,-2.77555756156289E-17),.UNSPECIFIED.);
#6447=B_SPLINE_CURVE_WITH_KNOTS('',3,(#102725,#102726,#102727,#102728,#102729,
#102730,#102731),.UNSPECIFIED.,.F.,.F.,(4,3,4),(0.,0.0330660780458869,0.0578656365803021),
 .UNSPECIFIED.);
#6448=B_SPLINE_CURVE_WITH_KNOTS('',3,(#102733,#102734,#102735,#102736),
 .UNSPECIFIED.,.F.,.F.,(4,4),(-1.38777878078145E-16,1.2),.UNSPECIFIED.);
#6449=B_SPLINE_CURVE_WITH_KNOTS('',3,(#102738,#102739,#102740,#102741,#102742,
#102743,#102744),.UNSPECIFIED.,.F.,.F.,(4,3,4),(0.,0.0247995585344142,0.0578656365802999),
 .UNSPECIFIED.);
#6450=B_SPLINE_CURVE_WITH_KNOTS('',3,(#102745,#102746,#102747,#102748),
 .UNSPECIFIED.,.F.,.F.,(4,4),(-1.2,1.38777878078145E-16),.UNSPECIFIED.);
#6451=B_SPLINE_CURVE_WITH_KNOTS('',3,(#102774,#102775,#102776,#102777,#102778,
#102779,#102780),.UNSPECIFIED.,.F.,.F.,(4,3,4),(0.,0.0330660780484272,0.0578656365847475),
 .UNSPECIFIED.);
#6452=B_SPLINE_CURVE_WITH_KNOTS('',3,(#102782,#102783,#102784,#102785),
 .UNSPECIFIED.,.F.,.F.,(4,4),(0.,1.2),.UNSPECIFIED.);
#6453=B_SPLINE_CURVE_WITH_KNOTS('',3,(#102787,#102788,#102789,#102790,#102791,
#102792,#102793),.UNSPECIFIED.,.F.,.F.,(4,3,4),(0.,0.0247995585363195,0.0578656365847456),
 .UNSPECIFIED.);
#6454=B_SPLINE_CURVE_WITH_KNOTS('',3,(#102794,#102795,#102796,#102797),
 .UNSPECIFIED.,.F.,.F.,(4,4),(-1.2,0.),.UNSPECIFIED.);
#6455=B_SPLINE_CURVE_WITH_KNOTS('',3,(#103621,#103622,#103623,#103624,#103625,
#103626,#103627),.UNSPECIFIED.,.F.,.F.,(4,3,4),(0.,0.0330660780458254,0.0578656365801945),
 .UNSPECIFIED.);
#6456=B_SPLINE_CURVE_WITH_KNOTS('',3,(#103629,#103630,#103631,#103632),
 .UNSPECIFIED.,.F.,.F.,(4,4),(0.,1.2),.UNSPECIFIED.);
#6457=B_SPLINE_CURVE_WITH_KNOTS('',3,(#103634,#103635,#103636,#103637,#103638,
#103639,#103640),.UNSPECIFIED.,.F.,.F.,(4,3,4),(0.,0.0247995585343927,0.0578656365802495),
 .UNSPECIFIED.);
#6458=B_SPLINE_CURVE_WITH_KNOTS('',3,(#103641,#103642,#103643,#103644),
 .UNSPECIFIED.,.F.,.F.,(4,4),(-1.2,0.),.UNSPECIFIED.);
#6459=B_SPLINE_CURVE_WITH_KNOTS('',3,(#103670,#103671,#103672,#103673,#103674,
#103675,#103676),.UNSPECIFIED.,.F.,.F.,(4,3,4),(0.,0.0330660780484286,0.05786563658475),
 .UNSPECIFIED.);
#6460=B_SPLINE_CURVE_WITH_KNOTS('',3,(#103678,#103679,#103680,#103681),
 .UNSPECIFIED.,.F.,.F.,(4,4),(9.71445146547012E-17,1.2),.UNSPECIFIED.);
#6461=B_SPLINE_CURVE_WITH_KNOTS('',3,(#103683,#103684,#103685,#103686,#103687,
#103688,#103689),.UNSPECIFIED.,.F.,.F.,(4,3,4),(0.,0.024799558536323,0.0578656365847537),
 .UNSPECIFIED.);
#6462=B_SPLINE_CURVE_WITH_KNOTS('',3,(#103690,#103691,#103692,#103693),
 .UNSPECIFIED.,.F.,.F.,(4,4),(-1.2,-9.71445146547012E-17),.UNSPECIFIED.);
#6463=B_SPLINE_CURVE_WITH_KNOTS('',3,(#104517,#104518,#104519,#104520,#104521,
#104522,#104523),.UNSPECIFIED.,.F.,.F.,(4,3,4),(0.,0.0330660780458335,0.0578656365802087),
 .UNSPECIFIED.);
#6464=B_SPLINE_CURVE_WITH_KNOTS('',3,(#104525,#104526,#104527,#104528),
 .UNSPECIFIED.,.F.,.F.,(4,4),(-5.55111512312578E-17,1.2),.UNSPECIFIED.);
#6465=B_SPLINE_CURVE_WITH_KNOTS('',3,(#104530,#104531,#104532,#104533,#104534,
#104535,#104536),.UNSPECIFIED.,.F.,.F.,(4,3,4),(0.,0.0247995585343757,0.0578656365802101),
 .UNSPECIFIED.);
#6466=B_SPLINE_CURVE_WITH_KNOTS('',3,(#104537,#104538,#104539,#104540),
 .UNSPECIFIED.,.F.,.F.,(4,4),(-1.2,5.55111512312578E-17),.UNSPECIFIED.);
#6467=B_SPLINE_CURVE_WITH_KNOTS('',3,(#104566,#104567,#104568,#104569,#104570,
#104571,#104572),.UNSPECIFIED.,.F.,.F.,(4,3,4),(0.,0.0330660780484165,0.0578656365847288),
 .UNSPECIFIED.);
#6468=B_SPLINE_CURVE_WITH_KNOTS('',3,(#104574,#104575,#104576,#104577),
 .UNSPECIFIED.,.F.,.F.,(4,4),(9.71445146547012E-17,1.2),.UNSPECIFIED.);
#6469=B_SPLINE_CURVE_WITH_KNOTS('',3,(#104579,#104580,#104581,#104582,#104583,
#104584,#104585),.UNSPECIFIED.,.F.,.F.,(4,3,4),(0.,0.0247995585363161,0.0578656365847375),
 .UNSPECIFIED.);
#6470=B_SPLINE_CURVE_WITH_KNOTS('',3,(#104586,#104587,#104588,#104589),
 .UNSPECIFIED.,.F.,.F.,(4,4),(-1.2,-9.71445146547012E-17),.UNSPECIFIED.);
#6471=B_SPLINE_CURVE_WITH_KNOTS('',3,(#105413,#105414,#105415,#105416,#105417,
#105418,#105419),.UNSPECIFIED.,.F.,.F.,(4,3,4),(0.,0.0330660780458765,0.0578656365802839),
 .UNSPECIFIED.);
#6472=B_SPLINE_CURVE_WITH_KNOTS('',3,(#105421,#105422,#105423,#105424),
 .UNSPECIFIED.,.F.,.F.,(4,4),(-1.41402172924014E-16,1.2),.UNSPECIFIED.);
#6473=B_SPLINE_CURVE_WITH_KNOTS('',3,(#105426,#105427,#105428,#105429,#105430,
#105431,#105432),.UNSPECIFIED.,.F.,.F.,(4,3,4),(0.,0.0247995585344063,0.0578656365802813),
 .UNSPECIFIED.);
#6474=B_SPLINE_CURVE_WITH_KNOTS('',3,(#105433,#105434,#105435,#105436),
 .UNSPECIFIED.,.F.,.F.,(4,4),(-1.2,1.41402172924014E-16),.UNSPECIFIED.);
#6475=B_SPLINE_CURVE_WITH_KNOTS('',3,(#105462,#105463,#105464,#105465,#105466,
#105467,#105468),.UNSPECIFIED.,.F.,.F.,(4,3,4),(0.,0.0330660780484353,0.0578656365847618),
 .UNSPECIFIED.);
#6476=B_SPLINE_CURVE_WITH_KNOTS('',3,(#105470,#105471,#105472,#105473),
 .UNSPECIFIED.,.F.,.F.,(4,4),(0.,1.2),.UNSPECIFIED.);
#6477=B_SPLINE_CURVE_WITH_KNOTS('',3,(#105475,#105476,#105477,#105478,#105479,
#105480,#105481),.UNSPECIFIED.,.F.,.F.,(4,3,4),(0.,0.0247995585363296,0.057865636584769),
 .UNSPECIFIED.);
#6478=B_SPLINE_CURVE_WITH_KNOTS('',3,(#105482,#105483,#105484,#105485),
 .UNSPECIFIED.,.F.,.F.,(4,4),(-1.2,0.),.UNSPECIFIED.);
#6479=B_SPLINE_CURVE_WITH_KNOTS('',3,(#106309,#106310,#106311,#106312,#106313,
#106314,#106315),.UNSPECIFIED.,.F.,.F.,(4,3,4),(0.,0.0330660780458757,0.0578656365802824),
 .UNSPECIFIED.);
#6480=B_SPLINE_CURVE_WITH_KNOTS('',3,(#106317,#106318,#106319,#106320),
 .UNSPECIFIED.,.F.,.F.,(4,4),(-1.11022302462516E-16,1.2),.UNSPECIFIED.);
#6481=B_SPLINE_CURVE_WITH_KNOTS('',3,(#106322,#106323,#106324,#106325,#106326,
#106327,#106328),.UNSPECIFIED.,.F.,.F.,(4,3,4),(0.,0.0247995585344084,0.0578656365802862),
 .UNSPECIFIED.);
#6482=B_SPLINE_CURVE_WITH_KNOTS('',3,(#106329,#106330,#106331,#106332),
 .UNSPECIFIED.,.F.,.F.,(4,4),(-1.2,1.11022302462516E-16),.UNSPECIFIED.);
#6483=B_SPLINE_CURVE_WITH_KNOTS('',3,(#106358,#106359,#106360,#106361,#106362,
#106363,#106364),.UNSPECIFIED.,.F.,.F.,(4,3,4),(0.,0.0330660780484577,0.057865636584801),
 .UNSPECIFIED.);
#6484=B_SPLINE_CURVE_WITH_KNOTS('',3,(#106366,#106367,#106368,#106369),
 .UNSPECIFIED.,.F.,.F.,(4,4),(1.38777878078145E-16,1.2),.UNSPECIFIED.);
#6485=B_SPLINE_CURVE_WITH_KNOTS('',3,(#106371,#106372,#106373,#106374,#106375,
#106376,#106377),.UNSPECIFIED.,.F.,.F.,(4,3,4),(0.,0.0247995585363564,0.0578656365848316),
 .UNSPECIFIED.);
#6486=B_SPLINE_CURVE_WITH_KNOTS('',3,(#106378,#106379,#106380,#106381),
 .UNSPECIFIED.,.F.,.F.,(4,4),(-1.2,-1.38777878078145E-16),.UNSPECIFIED.);
#6487=B_SPLINE_CURVE_WITH_KNOTS('',3,(#107205,#107206,#107207,#107208,#107209,
#107210,#107211),.UNSPECIFIED.,.F.,.F.,(4,3,4),(0.,0.0330660780458936,0.0578656365803137),
 .UNSPECIFIED.);
#6488=B_SPLINE_CURVE_WITH_KNOTS('',3,(#107213,#107214,#107215,#107216),
 .UNSPECIFIED.,.F.,.F.,(4,4),(2.77555756156289E-17,1.2),.UNSPECIFIED.);
#6489=B_SPLINE_CURVE_WITH_KNOTS('',3,(#107218,#107219,#107220,#107221,#107222,
#107223,#107224),.UNSPECIFIED.,.F.,.F.,(4,3,4),(0.,0.0247995585344178,0.0578656365803083),
 .UNSPECIFIED.);
#6490=B_SPLINE_CURVE_WITH_KNOTS('',3,(#107225,#107226,#107227,#107228),
 .UNSPECIFIED.,.F.,.F.,(4,4),(-1.2,-2.77555756156289E-17),.UNSPECIFIED.);
#6491=B_SPLINE_CURVE_WITH_KNOTS('',3,(#107254,#107255,#107256,#107257,#107258,
#107259,#107260),.UNSPECIFIED.,.F.,.F.,(4,3,4),(0.,0.0330660780484244,0.0578656365847427),
 .UNSPECIFIED.);
#6492=B_SPLINE_CURVE_WITH_KNOTS('',3,(#107262,#107263,#107264,#107265),
 .UNSPECIFIED.,.F.,.F.,(4,4),(0.,1.2),.UNSPECIFIED.);
#6493=B_SPLINE_CURVE_WITH_KNOTS('',3,(#107267,#107268,#107269,#107270,#107271,
#107272,#107273),.UNSPECIFIED.,.F.,.F.,(4,3,4),(0.,0.0247995585363162,0.0578656365847378),
 .UNSPECIFIED.);
#6494=B_SPLINE_CURVE_WITH_KNOTS('',3,(#107274,#107275,#107276,#107277),
 .UNSPECIFIED.,.F.,.F.,(4,4),(-1.2,0.),.UNSPECIFIED.);
#6495=B_SPLINE_CURVE_WITH_KNOTS('',3,(#108101,#108102,#108103,#108104,#108105,
#108106,#108107),.UNSPECIFIED.,.F.,.F.,(4,3,4),(0.,0.0330660780458305,0.0578656365802034),
 .UNSPECIFIED.);
#6496=B_SPLINE_CURVE_WITH_KNOTS('',3,(#108109,#108110,#108111,#108112),
 .UNSPECIFIED.,.F.,.F.,(4,4),(2.77555756156289E-17,1.2),.UNSPECIFIED.);
#6497=B_SPLINE_CURVE_WITH_KNOTS('',3,(#108114,#108115,#108116,#108117,#108118,
#108119,#108120),.UNSPECIFIED.,.F.,.F.,(4,3,4),(0.,0.0247995585343651,0.0578656365801852),
 .UNSPECIFIED.);
#6498=B_SPLINE_CURVE_WITH_KNOTS('',3,(#108121,#108122,#108123,#108124),
 .UNSPECIFIED.,.F.,.F.,(4,4),(-1.2,-2.77555756156289E-17),.UNSPECIFIED.);
#6499=B_SPLINE_CURVE_WITH_KNOTS('',3,(#108150,#108151,#108152,#108153,#108154,
#108155,#108156),.UNSPECIFIED.,.F.,.F.,(4,3,4),(0.,0.0330660780483646,0.057865636584638),
 .UNSPECIFIED.);
#6500=B_SPLINE_CURVE_WITH_KNOTS('',3,(#108158,#108159,#108160,#108161),
 .UNSPECIFIED.,.F.,.F.,(4,4),(5.55111512312578E-17,1.2),.UNSPECIFIED.);
#6501=B_SPLINE_CURVE_WITH_KNOTS('',3,(#108163,#108164,#108165,#108166,#108167,
#108168,#108169),.UNSPECIFIED.,.F.,.F.,(4,3,4),(0.,0.0247995585362812,0.057865636584656),
 .UNSPECIFIED.);
#6502=B_SPLINE_CURVE_WITH_KNOTS('',3,(#108170,#108171,#108172,#108173),
 .UNSPECIFIED.,.F.,.F.,(4,4),(-1.2,-5.55111512312578E-17),.UNSPECIFIED.);
#6503=B_SPLINE_CURVE_WITH_KNOTS('',3,(#108997,#108998,#108999,#109000,#109001,
#109002,#109003),.UNSPECIFIED.,.F.,.F.,(4,3,4),(0.,0.0330660780458722,0.0578656365802764),
 .UNSPECIFIED.);
#6504=B_SPLINE_CURVE_WITH_KNOTS('',3,(#109005,#109006,#109007,#109008),
 .UNSPECIFIED.,.F.,.F.,(4,4),(-8.32667268468867E-17,1.2),.UNSPECIFIED.);
#6505=B_SPLINE_CURVE_WITH_KNOTS('',3,(#109010,#109011,#109012,#109013,#109014,
#109015,#109016),.UNSPECIFIED.,.F.,.F.,(4,3,4),(0.,0.0247995585344042,0.0578656365802765),
 .UNSPECIFIED.);
#6506=B_SPLINE_CURVE_WITH_KNOTS('',3,(#109017,#109018,#109019,#109020),
 .UNSPECIFIED.,.F.,.F.,(4,4),(-1.2,8.32667268468867E-17),.UNSPECIFIED.);
#6507=B_SPLINE_CURVE_WITH_KNOTS('',3,(#109046,#109047,#109048,#109049,#109050,
#109051,#109052),.UNSPECIFIED.,.F.,.F.,(4,3,4),(0.,0.033066078048439,0.0578656365847682),
 .UNSPECIFIED.);
#6508=B_SPLINE_CURVE_WITH_KNOTS('',3,(#109054,#109055,#109056,#109057),
 .UNSPECIFIED.,.F.,.F.,(4,4),(1.66533453693773E-16,1.2),.UNSPECIFIED.);
#6509=B_SPLINE_CURVE_WITH_KNOTS('',3,(#109059,#109060,#109061,#109062,#109063,
#109064,#109065),.UNSPECIFIED.,.F.,.F.,(4,3,4),(0.,0.0247995585363292,0.0578656365847682),
 .UNSPECIFIED.);
#6510=B_SPLINE_CURVE_WITH_KNOTS('',3,(#109066,#109067,#109068,#109069),
 .UNSPECIFIED.,.F.,.F.,(4,4),(-1.2,-1.66533453693773E-16),.UNSPECIFIED.);
#6511=B_SPLINE_CURVE_WITH_KNOTS('',3,(#109893,#109894,#109895,#109896,#109897,
#109898,#109899),.UNSPECIFIED.,.F.,.F.,(4,3,4),(0.,0.033066078045871,0.0578656365802742),
 .UNSPECIFIED.);
#6512=B_SPLINE_CURVE_WITH_KNOTS('',3,(#109901,#109902,#109903,#109904),
 .UNSPECIFIED.,.F.,.F.,(4,4),(-1.47525527564366E-17,1.2),.UNSPECIFIED.);
#6513=B_SPLINE_CURVE_WITH_KNOTS('',3,(#109906,#109907,#109908,#109909,#109910,
#109911,#109912),.UNSPECIFIED.,.F.,.F.,(4,3,4),(0.,0.0247995585344122,0.057865636580295),
 .UNSPECIFIED.);
#6514=B_SPLINE_CURVE_WITH_KNOTS('',3,(#109913,#109914,#109915,#109916),
 .UNSPECIFIED.,.F.,.F.,(4,4),(-1.2,1.47525527564366E-17),.UNSPECIFIED.);
#6515=B_SPLINE_CURVE_WITH_KNOTS('',3,(#109942,#109943,#109944,#109945,#109946,
#109947,#109948),.UNSPECIFIED.,.F.,.F.,(4,3,4),(0.,0.0330660780484426,0.0578656365847746),
 .UNSPECIFIED.);
#6516=B_SPLINE_CURVE_WITH_KNOTS('',3,(#109950,#109951,#109952,#109953),
 .UNSPECIFIED.,.F.,.F.,(4,4),(9.71445146547012E-17,1.2),.UNSPECIFIED.);
#6517=B_SPLINE_CURVE_WITH_KNOTS('',3,(#109955,#109956,#109957,#109958,#109959,
#109960,#109961),.UNSPECIFIED.,.F.,.F.,(4,3,4),(0.,0.0247995585363433,0.0578656365848011),
 .UNSPECIFIED.);
#6518=B_SPLINE_CURVE_WITH_KNOTS('',3,(#109962,#109963,#109964,#109965),
 .UNSPECIFIED.,.F.,.F.,(4,4),(-1.2,-9.71445146547012E-17),.UNSPECIFIED.);
#6519=B_SPLINE_CURVE_WITH_KNOTS('',3,(#110789,#110790,#110791,#110792,#110793,
#110794,#110795),.UNSPECIFIED.,.F.,.F.,(4,3,4),(0.,0.0330660780458487,0.0578656365802352),
 .UNSPECIFIED.);
#6520=B_SPLINE_CURVE_WITH_KNOTS('',3,(#110797,#110798,#110799,#110800),
 .UNSPECIFIED.,.F.,.F.,(4,4),(2.77555756156289E-17,1.2),.UNSPECIFIED.);
#6521=B_SPLINE_CURVE_WITH_KNOTS('',3,(#110802,#110803,#110804,#110805,#110806,
#110807,#110808),.UNSPECIFIED.,.F.,.F.,(4,3,4),(0.,0.0247995585343886,0.05786563658024),
 .UNSPECIFIED.);
#6522=B_SPLINE_CURVE_WITH_KNOTS('',3,(#110809,#110810,#110811,#110812),
 .UNSPECIFIED.,.F.,.F.,(4,4),(-1.2,-2.77555756156289E-17),.UNSPECIFIED.);
#6523=B_SPLINE_CURVE_WITH_KNOTS('',3,(#110838,#110839,#110840,#110841,#110842,
#110843,#110844),.UNSPECIFIED.,.F.,.F.,(4,3,4),(0.,0.0330660780484081,0.0578656365847142),
 .UNSPECIFIED.);
#6524=B_SPLINE_CURVE_WITH_KNOTS('',3,(#110846,#110847,#110848,#110849),
 .UNSPECIFIED.,.F.,.F.,(4,4),(0.,1.2),.UNSPECIFIED.);
#6525=B_SPLINE_CURVE_WITH_KNOTS('',3,(#110851,#110852,#110853,#110854,#110855,
#110856,#110857),.UNSPECIFIED.,.F.,.F.,(4,3,4),(0.,0.0247995585363053,0.0578656365847123),
 .UNSPECIFIED.);
#6526=B_SPLINE_CURVE_WITH_KNOTS('',3,(#110858,#110859,#110860,#110861),
 .UNSPECIFIED.,.F.,.F.,(4,4),(-1.2,0.),.UNSPECIFIED.);
#6527=B_SPLINE_CURVE_WITH_KNOTS('',3,(#111685,#111686,#111687,#111688,#111689,
#111690,#111691),.UNSPECIFIED.,.F.,.F.,(4,3,4),(0.,0.0330660780458939,0.0578656365803143),
 .UNSPECIFIED.);
#6528=B_SPLINE_CURVE_WITH_KNOTS('',3,(#111693,#111694,#111695,#111696),
 .UNSPECIFIED.,.F.,.F.,(4,4),(-8.32667268468867E-17,1.2),.UNSPECIFIED.);
#6529=B_SPLINE_CURVE_WITH_KNOTS('',3,(#111698,#111699,#111700,#111701,#111702,
#111703,#111704),.UNSPECIFIED.,.F.,.F.,(4,3,4),(0.,0.0247995585344063,0.0578656365802814),
 .UNSPECIFIED.);
#6530=B_SPLINE_CURVE_WITH_KNOTS('',3,(#111705,#111706,#111707,#111708),
 .UNSPECIFIED.,.F.,.F.,(4,4),(-1.2,8.32667268468867E-17),.UNSPECIFIED.);
#6531=B_SPLINE_CURVE_WITH_KNOTS('',3,(#111734,#111735,#111736,#111737,#111738,
#111739,#111740),.UNSPECIFIED.,.F.,.F.,(4,3,4),(0.,0.0330660780483969,0.0578656365846947),
 .UNSPECIFIED.);
#6532=B_SPLINE_CURVE_WITH_KNOTS('',3,(#111742,#111743,#111744,#111745),
 .UNSPECIFIED.,.F.,.F.,(4,4),(-5.63859161805989E-17,1.2),.UNSPECIFIED.);
#6533=B_SPLINE_CURVE_WITH_KNOTS('',3,(#111747,#111748,#111749,#111750,#111751,
#111752,#111753),.UNSPECIFIED.,.F.,.F.,(4,3,4),(0.,0.0247995585362953,0.0578656365846891),
 .UNSPECIFIED.);
#6534=B_SPLINE_CURVE_WITH_KNOTS('',3,(#111754,#111755,#111756,#111757),
 .UNSPECIFIED.,.F.,.F.,(4,4),(-1.2,5.63859161805989E-17),.UNSPECIFIED.);
#6535=B_SPLINE_CURVE_WITH_KNOTS('',3,(#112581,#112582,#112583,#112584,#112585,
#112586,#112587),.UNSPECIFIED.,.F.,.F.,(4,3,4),(0.,0.0330660780458488,0.0578656365802353),
 .UNSPECIFIED.);
#6536=B_SPLINE_CURVE_WITH_KNOTS('',3,(#112589,#112590,#112591,#112592),
 .UNSPECIFIED.,.F.,.F.,(4,4),(-3.76195697576961E-36,1.2),.UNSPECIFIED.);
#6537=B_SPLINE_CURVE_WITH_KNOTS('',3,(#112594,#112595,#112596,#112597,#112598,
#112599,#112600),.UNSPECIFIED.,.F.,.F.,(4,3,4),(0.,0.0247995585344019,0.0578656365802711),
 .UNSPECIFIED.);
#6538=B_SPLINE_CURVE_WITH_KNOTS('',3,(#112601,#112602,#112603,#112604),
 .UNSPECIFIED.,.F.,.F.,(4,4),(-1.2,3.76195697576961E-36),.UNSPECIFIED.);
#6539=B_SPLINE_CURVE_WITH_KNOTS('',3,(#112630,#112631,#112632,#112633,#112634,
#112635,#112636),.UNSPECIFIED.,.F.,.F.,(4,3,4),(0.,0.0330660780483721,0.0578656365846511),
 .UNSPECIFIED.);
#6540=B_SPLINE_CURVE_WITH_KNOTS('',3,(#112638,#112639,#112640,#112641),
 .UNSPECIFIED.,.F.,.F.,(4,4),(2.77555756156289E-17,1.2),.UNSPECIFIED.);
#6541=B_SPLINE_CURVE_WITH_KNOTS('',3,(#112643,#112644,#112645,#112646,#112647,
#112648,#112649),.UNSPECIFIED.,.F.,.F.,(4,3,4),(0.,0.0247995585362904,0.0578656365846776),
 .UNSPECIFIED.);
#6542=B_SPLINE_CURVE_WITH_KNOTS('',3,(#112650,#112651,#112652,#112653),
 .UNSPECIFIED.,.F.,.F.,(4,4),(-1.2,-2.77555756156289E-17),.UNSPECIFIED.);
#6543=B_SPLINE_CURVE_WITH_KNOTS('',3,(#113477,#113478,#113479,#113480,#113481,
#113482,#113483),.UNSPECIFIED.,.F.,.F.,(4,3,4),(0.,0.0330660780458673,0.0578656365802679),
 .UNSPECIFIED.);
#6544=B_SPLINE_CURVE_WITH_KNOTS('',3,(#113485,#113486,#113487,#113488),
 .UNSPECIFIED.,.F.,.F.,(4,4),(0.,1.2),.UNSPECIFIED.);
#6545=B_SPLINE_CURVE_WITH_KNOTS('',3,(#113490,#113491,#113492,#113493,#113494,
#113495,#113496),.UNSPECIFIED.,.F.,.F.,(4,3,4),(0.,0.0247995585344041,0.0578656365802761),
 .UNSPECIFIED.);
#6546=B_SPLINE_CURVE_WITH_KNOTS('',3,(#113497,#113498,#113499,#113500),
 .UNSPECIFIED.,.F.,.F.,(4,4),(-1.2,0.),.UNSPECIFIED.);
#6547=B_SPLINE_CURVE_WITH_KNOTS('',3,(#113526,#113527,#113528,#113529,#113530,
#113531,#113532),.UNSPECIFIED.,.F.,.F.,(4,3,4),(0.,0.0330660780484096,0.0578656365847167),
 .UNSPECIFIED.);
#6548=B_SPLINE_CURVE_WITH_KNOTS('',3,(#113534,#113535,#113536,#113537),
 .UNSPECIFIED.,.F.,.F.,(4,4),(9.71445146547012E-17,1.2),.UNSPECIFIED.);
#6549=B_SPLINE_CURVE_WITH_KNOTS('',3,(#113539,#113540,#113541,#113542,#113543,
#113544,#113545),.UNSPECIFIED.,.F.,.F.,(4,3,4),(0.,0.0247995585363052,0.0578656365847121),
 .UNSPECIFIED.);
#6550=B_SPLINE_CURVE_WITH_KNOTS('',3,(#113546,#113547,#113548,#113549),
 .UNSPECIFIED.,.F.,.F.,(4,4),(-1.2,-9.71445146547012E-17),.UNSPECIFIED.);
#6551=B_SPLINE_CURVE_WITH_KNOTS('',3,(#114373,#114374,#114375,#114376,#114377,
#114378,#114379),.UNSPECIFIED.,.F.,.F.,(4,3,4),(0.,0.0330660780458525,0.0578656365802419),
 .UNSPECIFIED.);
#6552=B_SPLINE_CURVE_WITH_KNOTS('',3,(#114381,#114382,#114383,#114384),
 .UNSPECIFIED.,.F.,.F.,(4,4),(-6.03986977505924E-17,1.2),.UNSPECIFIED.);
#6553=B_SPLINE_CURVE_WITH_KNOTS('',3,(#114386,#114387,#114388,#114389,#114390,
#114391,#114392),.UNSPECIFIED.,.F.,.F.,(4,3,4),(0.,0.0247995585343901,0.0578656365802435),
 .UNSPECIFIED.);
#6554=B_SPLINE_CURVE_WITH_KNOTS('',3,(#114393,#114394,#114395,#114396),
 .UNSPECIFIED.,.F.,.F.,(4,4),(-1.2,6.03986977505924E-17),.UNSPECIFIED.);
#6555=B_SPLINE_CURVE_WITH_KNOTS('',3,(#114422,#114423,#114424,#114425,#114426,
#114427,#114428),.UNSPECIFIED.,.F.,.F.,(4,3,4),(0.,0.0330660780484176,0.0578656365847307),
 .UNSPECIFIED.);
#6556=B_SPLINE_CURVE_WITH_KNOTS('',3,(#114430,#114431,#114432,#114433),
 .UNSPECIFIED.,.F.,.F.,(4,4),(9.71445146547012E-17,1.2),.UNSPECIFIED.);
#6557=B_SPLINE_CURVE_WITH_KNOTS('',3,(#114435,#114436,#114437,#114438,#114439,
#114440,#114441),.UNSPECIFIED.,.F.,.F.,(4,3,4),(0.,0.0247995585363079,0.0578656365847185),
 .UNSPECIFIED.);
#6558=B_SPLINE_CURVE_WITH_KNOTS('',3,(#114442,#114443,#114444,#114445),
 .UNSPECIFIED.,.F.,.F.,(4,4),(-1.2,-9.71445146547012E-17),.UNSPECIFIED.);
#6559=B_SPLINE_CURVE_WITH_KNOTS('',3,(#115269,#115270,#115271,#115272,#115273,
#115274,#115275),.UNSPECIFIED.,.F.,.F.,(4,3,4),(0.,0.0330660780458678,0.0578656365802686),
 .UNSPECIFIED.);
#6560=B_SPLINE_CURVE_WITH_KNOTS('',3,(#115277,#115278,#115279,#115280),
 .UNSPECIFIED.,.F.,.F.,(4,4),(2.77555756156289E-17,1.2),.UNSPECIFIED.);
#6561=B_SPLINE_CURVE_WITH_KNOTS('',3,(#115282,#115283,#115284,#115285,#115286,
#115287,#115288),.UNSPECIFIED.,.F.,.F.,(4,3,4),(0.,0.0247995585344011,0.0578656365802693),
 .UNSPECIFIED.);
#6562=B_SPLINE_CURVE_WITH_KNOTS('',3,(#115289,#115290,#115291,#115292),
 .UNSPECIFIED.,.F.,.F.,(4,4),(-1.2,-2.77555756156289E-17),.UNSPECIFIED.);
#6563=B_SPLINE_CURVE_WITH_KNOTS('',3,(#115318,#115319,#115320,#115321,#115322,
#115323,#115324),.UNSPECIFIED.,.F.,.F.,(4,3,4),(0.,0.033066078048387,0.0578656365846772),
 .UNSPECIFIED.);
#6564=B_SPLINE_CURVE_WITH_KNOTS('',3,(#115326,#115327,#115328,#115329),
 .UNSPECIFIED.,.F.,.F.,(4,4),(0.,1.2),.UNSPECIFIED.);
#6565=B_SPLINE_CURVE_WITH_KNOTS('',3,(#115331,#115332,#115333,#115334,#115335,
#115336,#115337),.UNSPECIFIED.,.F.,.F.,(4,3,4),(0.,0.024799558536296,0.0578656365846907),
 .UNSPECIFIED.);
#6566=B_SPLINE_CURVE_WITH_KNOTS('',3,(#115338,#115339,#115340,#115341),
 .UNSPECIFIED.,.F.,.F.,(4,4),(-1.2,0.),.UNSPECIFIED.);
#6567=B_SPLINE_CURVE_WITH_KNOTS('',3,(#116165,#116166,#116167,#116168,#116169,
#116170,#116171),.UNSPECIFIED.,.F.,.F.,(4,3,4),(0.,0.0330660780458588,0.0578656365802528),
 .UNSPECIFIED.);
#6568=B_SPLINE_CURVE_WITH_KNOTS('',3,(#116173,#116174,#116175,#116176),
 .UNSPECIFIED.,.F.,.F.,(4,4),(-5.55111512312578E-17,1.2),.UNSPECIFIED.);
#6569=B_SPLINE_CURVE_WITH_KNOTS('',3,(#116178,#116179,#116180,#116181,#116182,
#116183,#116184),.UNSPECIFIED.,.F.,.F.,(4,3,4),(0.,0.0247995585343981,0.0578656365802622),
 .UNSPECIFIED.);
#6570=B_SPLINE_CURVE_WITH_KNOTS('',3,(#116185,#116186,#116187,#116188),
 .UNSPECIFIED.,.F.,.F.,(4,4),(-1.2,5.55111512312578E-17),.UNSPECIFIED.);
#6571=B_SPLINE_CURVE_WITH_KNOTS('',3,(#173304,#173305,#173306,#173307,#173308,
#173309,#173310),.UNSPECIFIED.,.F.,.F.,(4,3,4),(0.,0.0330660780484233,0.0578656365847407),
 .UNSPECIFIED.);
#6572=B_SPLINE_CURVE_WITH_KNOTS('',3,(#173312,#173313,#173314,#173315),
 .UNSPECIFIED.,.F.,.F.,(4,4),(2.13940539033965E-17,1.2),.UNSPECIFIED.);
#6573=B_SPLINE_CURVE_WITH_KNOTS('',3,(#173317,#173318,#173319,#173320,#173321,
#173322,#173323),.UNSPECIFIED.,.F.,.F.,(4,3,4),(0.,0.0247995585363121,0.0578656365847283),
 .UNSPECIFIED.);
#6574=B_SPLINE_CURVE_WITH_KNOTS('',3,(#173324,#173325,#173326,#173327),
 .UNSPECIFIED.,.F.,.F.,(4,4),(-1.2,-2.13940539033965E-17),.UNSPECIFIED.);
#6575=B_SPLINE_CURVE_WITH_KNOTS('',3,(#174148,#174149,#174150,#174151,#174152,
#174153,#174154),.UNSPECIFIED.,.F.,.F.,(4,3,4),(0.,0.0330660780458505,0.0578656365802384),
 .UNSPECIFIED.);
#6576=B_SPLINE_CURVE_WITH_KNOTS('',3,(#174156,#174157,#174158,#174159),
 .UNSPECIFIED.,.F.,.F.,(4,4),(0.,1.2),.UNSPECIFIED.);
#6577=B_SPLINE_CURVE_WITH_KNOTS('',3,(#174161,#174162,#174163,#174164,#174165,
#174166,#174167),.UNSPECIFIED.,.F.,.F.,(4,3,4),(0.,0.024799558534381,0.0578656365802222),
 .UNSPECIFIED.);
#6578=B_SPLINE_CURVE_WITH_KNOTS('',3,(#174168,#174169,#174170,#174171),
 .UNSPECIFIED.,.F.,.F.,(4,4),(-1.2,0.),.UNSPECIFIED.);
#6579=B_SPLINE_CURVE_WITH_KNOTS('',3,(#256114,#256115,#256116,#256117,#256118,
#256119,#256120,#256121,#256122,#256123),.UNSPECIFIED.,.F.,.F.,(4,3,3,4),
(-4.09293042013066,-3.99163575995315,-2.99372681996486,-2.06863817490914),
 .UNSPECIFIED.);
#6580=B_SPLINE_CURVE_WITH_KNOTS('',3,(#256126,#256127,#256128,#256129,#256130,
#256131,#256132),.UNSPECIFIED.,.F.,.F.,(4,3,4),(0.,0.997908939988297,1.11730040836816),
 .UNSPECIFIED.);
#6581=B_SPLINE_CURVE_WITH_KNOTS('',3,(#256137,#256138,#256139,#256140,#256141,
#256142,#256143,#256144,#256145,#256146,#256147,#256148,#256149,#256150,
#256151,#256152,#256153,#256154,#256155,#256156,#256157,#256158),
 .UNSPECIFIED.,.F.,.F.,(4,3,3,3,3,3,3,4),(-10.3761157273102,-9.97908939988288,
-8.9811804598946,-7.9832715199063,-6.98536257991802,-5.98745363992973,-4.98954469994144,
-4.09293042013066),.UNSPECIFIED.);
#6582=B_SPLINE_CURVE_WITH_KNOTS('',3,(#256159,#256160,#256161,#256162,#256163,
#256164,#256165,#256166,#256167,#256168,#256169,#256170,#256171,#256172,
#256173,#256174,#256175,#256176,#256177,#256178,#256179,#256180),
 .UNSPECIFIED.,.F.,.F.,(4,3,3,3,3,3,3,4),(1.11730040836816,1.99581787997659,
2.99372681996487,3.99163575995315,4.98954469994144,5.98745363992972,6.98536257991801,
7.40048571554774),.UNSPECIFIED.);
#6583=B_SPLINE_CURVE_WITH_KNOTS('',3,(#256185,#256186,#256187,#256188,#256189,
#256190,#256191,#256192,#256193,#256194,#256195,#256196,#256197,#256198,
#256199,#256200,#256201,#256202,#256203,#256204,#256205,#256206),
 .UNSPECIFIED.,.F.,.F.,(4,3,3,3,3,3,3,4),(-16.6593010344898,-15.9665430398126,
-14.9686340998243,-13.970725159836,-12.9728162198477,-11.9749072798595,
-10.9769983398712,-10.3761157273102),.UNSPECIFIED.);
#6584=B_SPLINE_CURVE_WITH_KNOTS('',3,(#256207,#256208,#256209,#256210,#256211,
#256212,#256213,#256214,#256215,#256216,#256217,#256218,#256219,#256220,
#256221,#256222,#256223,#256224,#256225,#256226,#256227,#256228),
 .UNSPECIFIED.,.F.,.F.,(4,3,3,3,3,3,3,4),(7.40048571554774,7.9832715199063,
8.98118045989459,9.97908939988288,10.9769983398712,11.9749072798595,12.9728162198478,
13.6836710227273),.UNSPECIFIED.);
#6585=B_SPLINE_CURVE_WITH_KNOTS('',3,(#256233,#256234,#256235,#256236,#256237,
#256238,#256239,#256240,#256241,#256242,#256243,#256244,#256245,#256246,
#256247,#256248,#256249,#256250,#256251,#256252,#256253,#256254),
 .UNSPECIFIED.,.F.,.F.,(4,3,3,3,3,3,3,4),(-22.9424863416694,-21.9539966797423,
-20.956087739754,-19.9581787997658,-18.9602698597775,-17.9623609197892,
-16.9644519798009,-16.6593010344898),.UNSPECIFIED.);
#6586=B_SPLINE_CURVE_WITH_KNOTS('',3,(#256255,#256256,#256257,#256258,#256259,
#256260,#256261,#256262,#256263,#256264,#256265,#256266,#256267,#256268,
#256269,#256270,#256271,#256272,#256273,#256274,#256275,#256276,#256277,
#256278,#256279),.UNSPECIFIED.,.F.,.F.,(4,3,3,3,3,3,3,3,4),(13.6836710227273,
13.970725159836,14.9686340998243,15.9665430398126,16.9644519798009,17.9623609197892,
18.9602698597775,19.9581787997658,19.9668563299069),.UNSPECIFIED.);
#6587=B_SPLINE_CURVE_WITH_KNOTS('',3,(#256284,#256285,#256286,#256287,#256288,
#256289,#256290,#256291,#256292,#256293,#256294,#256295,#256296,#256297,
#256298,#256299,#256300,#256301,#256302,#256303,#256304,#256305,#256306,
#256307,#256308),.UNSPECIFIED.,.F.,.F.,(4,3,3,3,3,3,3,3,4),(-29.225671648849,
-28.9393592596604,-27.9414503196721,-26.9435413796838,-25.9456324396955,
-24.9477234997072,-23.9498145597189,-22.9519056197306,-22.9424863416694),
 .UNSPECIFIED.);
#6588=B_SPLINE_CURVE_WITH_KNOTS('',3,(#256309,#256310,#256311,#256312,#256313,
#256314,#256315,#256316,#256317,#256318,#256319,#256320,#256321,#256322,
#256323,#256324,#256325,#256326,#256327,#256328,#256329,#256330),
 .UNSPECIFIED.,.F.,.F.,(4,3,3,3,3,3,3,4),(19.9668563299069,20.9560877397541,
21.9539966797423,22.9519056197306,23.9498145597189,24.9477234997072,25.9456324396955,
26.2500416370865),.UNSPECIFIED.);
#6589=B_SPLINE_CURVE_WITH_KNOTS('',3,(#256335,#256336,#256337,#256338,#256339,
#256340,#256341,#256342,#256343,#256344,#256345,#256346,#256347,#256348,
#256349,#256350,#256351,#256352,#256353,#256354,#256355,#256356),
 .UNSPECIFIED.,.F.,.F.,(4,3,3,3,3,3,3,4),(-35.5088569560286,-34.9268128995901,
-33.9289039596018,-32.9309950196135,-31.9330860796252,-30.9351771396369,
-29.9372681996486,-29.225671648849),.UNSPECIFIED.);
#6590=B_SPLINE_CURVE_WITH_KNOTS('',3,(#256357,#256358,#256359,#256360,#256361,
#256362,#256363,#256364,#256365,#256366,#256367,#256368,#256369,#256370,
#256371,#256372,#256373,#256374,#256375,#256376,#256377,#256378),
 .UNSPECIFIED.,.F.,.F.,(4,3,3,3,3,3,3,4),(26.2500416370865,26.9435413796838,
27.9414503196721,28.9393592596604,29.9372681996487,30.9351771396369,31.9330860796252,
32.5332269442661),.UNSPECIFIED.);
#6591=B_SPLINE_CURVE_WITH_KNOTS('',3,(#256383,#256384,#256385,#256386,#256387,
#256388,#256389,#256390,#256391,#256392,#256393,#256394,#256395,#256396,
#256397,#256398,#256399,#256400,#256401,#256402,#256403,#256404),
 .UNSPECIFIED.,.F.,.F.,(4,3,3,3,3,3,3,4),(-41.7920422632082,-40.9142665395198,
-39.9163575995315,-38.9184486595432,-37.9205397195549,-36.9226307795667,
-35.9247218395784,-35.5088569560286),.UNSPECIFIED.);
#6592=B_SPLINE_CURVE_WITH_KNOTS('',3,(#256405,#256406,#256407,#256408,#256409,
#256410,#256411,#256412,#256413,#256414,#256415,#256416,#256417,#256418,
#256419,#256420,#256421,#256422,#256423,#256424,#256425,#256426),
 .UNSPECIFIED.,.F.,.F.,(4,3,3,3,3,3,3,4),(32.5332269442661,32.9309950196135,
33.9289039596018,34.9268128995901,35.9247218395784,36.9226307795667,37.9205397195549,
38.8164122514457),.UNSPECIFIED.);
#6593=B_SPLINE_CURVE_WITH_KNOTS('',3,(#256431,#256432,#256433,#256434,#256435,
#256436,#256437,#256438,#256439,#256440,#256441,#256442,#256443,#256444,
#256445,#256446,#256447,#256448,#256449,#256450,#256451,#256452,#256453,
#256454,#256455),.UNSPECIFIED.,.F.,.F.,(4,3,3,3,3,3,3,3,4),(-48.0752275703878,
-47.8996291194378,-46.9017201794495,-45.9038112394613,-44.905902299473,
-43.9079933594847,-42.9100844194964,-41.9121754795081,-41.7920422632082),
 .UNSPECIFIED.);
#6594=B_SPLINE_CURVE_WITH_KNOTS('',3,(#256456,#256457,#256458,#256459,#256460,
#256461,#256462,#256463,#256464,#256465,#256466,#256467,#256468,#256469,
#256470,#256471,#256472,#256473,#256474,#256475,#256476,#256477,#256478,
#256479,#256480),.UNSPECIFIED.,.F.,.F.,(4,3,3,3,3,3,3,3,4),(38.8164122514457,
38.9184486595432,39.9163575995315,40.9142665395198,41.9121754795081,42.9100844194964,
43.9079933594847,44.905902299473,45.0995975586253),.UNSPECIFIED.);
#6595=B_SPLINE_CURVE_WITH_KNOTS('',3,(#256485,#256486,#256487,#256488,#256489,
#256490,#256491,#256492,#256493,#256494,#256495,#256496,#256497,#256498,
#256499,#256500,#256501,#256502,#256503,#256504,#256505,#256506),
 .UNSPECIFIED.,.F.,.F.,(4,3,3,3,3,3,3,4),(-54.3584128775674,-53.8870827593676,
-52.8891738193793,-51.891264879391,-50.8933559394027,-49.8954469994144,
-48.8975380594261,-48.0752275703878),.UNSPECIFIED.);
#6596=B_SPLINE_CURVE_WITH_KNOTS('',3,(#256507,#256508,#256509,#256510,#256511,
#256512,#256513,#256514,#256515,#256516,#256517,#256518,#256519,#256520,
#256521,#256522,#256523,#256524,#256525,#256526,#256527,#256528),
 .UNSPECIFIED.,.F.,.F.,(4,3,3,3,3,3,3,4),(45.0995975586253,45.9038112394613,
46.9017201794496,47.8996291194378,48.8975380594261,49.8954469994144,50.8933559394027,
51.3827828658049),.UNSPECIFIED.);
#6597=B_SPLINE_CURVE_WITH_KNOTS('',3,(#256533,#256534,#256535,#256536,#256537,
#256538,#256539,#256540,#256541,#256542,#256543,#256544,#256545,#256546,
#256547,#256548,#256549,#256550,#256551,#256552,#256553,#256554),
 .UNSPECIFIED.,.F.,.F.,(4,3,3,3,3,3,3,4),(-60.641598184747,-59.8745363992973,
-58.876627459309,-57.8787185193207,-56.8808095793324,-55.8829006393441,
-54.8849916993559,-54.3584128775674),.UNSPECIFIED.);
#6598=B_SPLINE_CURVE_WITH_KNOTS('',3,(#256555,#256556,#256557,#256558,#256559,
#256560,#256561,#256562,#256563,#256564,#256565,#256566,#256567,#256568,
#256569,#256570,#256571,#256572,#256573,#256574,#256575,#256576),
 .UNSPECIFIED.,.F.,.F.,(4,3,3,3,3,3,3,4),(51.3827828658049,51.891264879391,
52.8891738193793,53.8870827593676,54.8849916993559,55.8829006393442,56.8808095793325,
57.6659681729845),.UNSPECIFIED.);
#6599=B_SPLINE_CURVE_WITH_KNOTS('',3,(#256581,#256582,#256583,#256584,#256585,
#256586,#256587,#256588,#256589,#256590,#256591,#256592,#256593,#256594,
#256595,#256596,#256597,#256598,#256599,#256600,#256601,#256602,#256603,
#256604,#256605),.UNSPECIFIED.,.F.,.F.,(4,3,3,3,3,3,3,3,4),(-66.9247834919266,
-66.8598989792153,-65.861990039227,-64.8640810992387,-63.8661721592505,
-62.8682632192622,-61.8703542792739,-60.8724453392856,-60.641598184747),
 .UNSPECIFIED.);
#6600=B_SPLINE_CURVE_WITH_KNOTS('',3,(#256606,#256607,#256608,#256609,#256610,
#256611,#256612,#256613,#256614,#256615,#256616,#256617,#256618,#256619,
#256620,#256621,#256622,#256623,#256624,#256625,#256626,#256627,#256628,
#256629,#256630),.UNSPECIFIED.,.F.,.F.,(4,3,3,3,3,3,3,3,4),(57.6659681729845,
57.8787185193207,58.876627459309,59.8745363992973,60.8724453392856,61.8703542792739,
62.8682632192622,63.8661721592505,63.949153480164),.UNSPECIFIED.);
#6601=B_SPLINE_CURVE_WITH_KNOTS('',3,(#256635,#256636,#256637,#256638,#256639,
#256640,#256641,#256642,#256643,#256644,#256645,#256646,#256647,#256648,
#256649,#256650,#256651,#256652,#256653,#256654,#256655,#256656),
 .UNSPECIFIED.,.F.,.F.,(4,3,3,3,3,3,3,4),(-73.2079687991062,-72.847352619145,
-71.8494436791567,-70.8515347391685,-69.8536257991802,-68.8557168591919,
-67.8578079192036,-66.9247834919266),.UNSPECIFIED.);
#6602=B_SPLINE_CURVE_WITH_KNOTS('',3,(#256657,#256658,#256659,#256660,#256661,
#256662,#256663,#256664,#256665,#256666,#256667,#256668,#256669,#256670,
#256671,#256672,#256673,#256674,#256675,#256676,#256677,#256678),
 .UNSPECIFIED.,.F.,.F.,(4,3,3,3,3,3,3,4),(63.949153480164,64.8640810992388,
65.8619900392271,66.8598989792153,67.8578079192036,68.8557168591919,69.8536257991802,
70.2323387873436),.UNSPECIFIED.);
#6603=B_SPLINE_CURVE_WITH_KNOTS('',3,(#256683,#256684,#256685,#256686,#256687,
#256688,#256689,#256690,#256691,#256692,#256693,#256694,#256695,#256696,
#256697,#256698,#256699,#256700,#256701,#256702,#256703,#256704),
 .UNSPECIFIED.,.F.,.F.,(4,3,3,3,3,3,3,4),(-79.4911541062857,-78.8348062590748,
-77.8368973190865,-76.8389883790982,-75.8410794391099,-74.8431704991216,
-73.8452615591333,-73.2079687991062),.UNSPECIFIED.);
#6604=B_SPLINE_CURVE_WITH_KNOTS('',3,(#256705,#256706,#256707,#256708,#256709,
#256710,#256711,#256712,#256713,#256714,#256715,#256716,#256717,#256718,
#256719,#256720,#256721,#256722,#256723,#256724,#256725,#256726),
 .UNSPECIFIED.,.F.,.F.,(4,3,3,3,3,3,3,4),(70.2323387873436,70.8515347391685,
71.8494436791568,72.8473526191451,73.8452615591333,74.8431704991216,75.8410794391099,
76.5155240945232),.UNSPECIFIED.);
#6605=B_SPLINE_CURVE_WITH_KNOTS('',3,(#256731,#256732,#256733,#256734,#256735,
#256736,#256737,#256738,#256739,#256740,#256741,#256742,#256743,#256744,
#256745,#256746,#256747,#256748,#256749,#256750,#256751,#256752),
 .UNSPECIFIED.,.F.,.F.,(4,3,3,3,3,3,3,4),(-85.7743394134653,-84.8222598990045,
-83.8243509590162,-82.8264420190279,-81.8285330790396,-80.8306241390513,
-79.832715199063,-79.4911541062857),.UNSPECIFIED.);
#6606=B_SPLINE_CURVE_WITH_KNOTS('',3,(#256753,#256754,#256755,#256756,#256757,
#256758,#256759,#256760,#256761,#256762,#256763,#256764,#256765,#256766,
#256767,#256768,#256769,#256770,#256771,#256772,#256773,#256774),
 .UNSPECIFIED.,.F.,.F.,(4,3,3,3,3,3,3,4),(76.5155240945232,76.8389883790982,
77.8368973190865,78.8348062590748,79.8327151990631,80.8306241390514,81.8285330790397,
82.7987094017028),.UNSPECIFIED.);
#6607=B_SPLINE_CURVE_WITH_KNOTS('',3,(#256779,#256780,#256781,#256782,#256783,
#256784,#256785,#256786,#256787,#256788,#256789,#256790,#256791,#256792,
#256793,#256794,#256795,#256796,#256797,#256798,#256799,#256800,#256801,
#256802,#256803),.UNSPECIFIED.,.F.,.F.,(4,3,3,3,3,3,3,3,4),(-92.0575247206449,
-91.8076224789225,-90.8097135389342,-89.8118045989459,-88.8138956589576,
-87.8159867189694,-86.8180777789811,-85.8201688389928,-85.7743394134653),
 .UNSPECIFIED.);
#6608=B_SPLINE_CURVE_WITH_KNOTS('',3,(#256804,#256805,#256806,#256807,#256808,
#256809,#256810,#256811,#256812,#256813,#256814,#256815,#256816,#256817,
#256818,#256819,#256820,#256821,#256822,#256823,#256824,#256825,#256826,
#256827,#256828),.UNSPECIFIED.,.F.,.F.,(4,3,3,3,3,3,3,3,4),(82.7987094017028,
82.8264420190279,83.8243509590162,84.8222598990045,85.8201688389928,86.8180777789811,
87.8159867189694,88.8138956589577,89.0818947088824),.UNSPECIFIED.);
#6609=B_SPLINE_CURVE_WITH_KNOTS('',3,(#256833,#256834,#256835,#256836,#256837,
#256838,#256839,#256840,#256841,#256842,#256843,#256844,#256845,#256846,
#256847,#256848,#256849,#256850,#256851,#256852,#256853,#256854),
 .UNSPECIFIED.,.F.,.F.,(4,3,3,3,3,3,3,4),(-98.3407100278245,-97.7950761188523,
-96.7971671788639,-95.7992582388757,-94.8013492988874,-93.8034403588991,
-92.8055314189108,-92.0575247206449),.UNSPECIFIED.);
#6610=B_SPLINE_CURVE_WITH_KNOTS('',3,(#256855,#256856,#256857,#256858,#256859,
#256860,#256861,#256862,#256863,#256864,#256865,#256866,#256867,#256868,
#256869,#256870,#256871,#256872,#256873,#256874,#256875,#256876),
 .UNSPECIFIED.,.F.,.F.,(4,3,3,3,3,3,3,4),(89.0818947088824,89.811804598946,
90.8097135389343,91.8076224789226,92.8055314189108,93.8034403588991,94.8013492988874,
95.365080016062),.UNSPECIFIED.);
#6611=B_SPLINE_CURVE_WITH_KNOTS('',3,(#256881,#256882,#256883,#256884,#256885,
#256886,#256887,#256888,#256889,#256890,#256891,#256892,#256893,#256894,
#256895,#256896,#256897,#256898,#256899,#256900,#256901,#256902),
 .UNSPECIFIED.,.F.,.F.,(4,3,3,3,3,3,3,4),(-104.623895335004,-103.782529758782,
-102.784620818794,-101.786711878805,-100.788802938817,-99.7908939988288,
-98.7929850588405,-98.3407100278245),.UNSPECIFIED.);
#6612=B_SPLINE_CURVE_WITH_KNOTS('',3,(#256903,#256904,#256905,#256906,#256907,
#256908,#256909,#256910,#256911,#256912,#256913,#256914,#256915,#256916,
#256917,#256918,#256919,#256920,#256921,#256922,#256923,#256924),
 .UNSPECIFIED.,.F.,.F.,(4,3,3,3,3,3,3,4),(95.365080016062,95.7992582388757,
96.797167178864,97.7950761188523,98.7929850588406,99.7908939988288,100.788802938817,
101.648265323242),.UNSPECIFIED.);
#6613=B_SPLINE_CURVE_WITH_KNOTS('',3,(#256929,#256930,#256931,#256932,#256933,
#256934,#256935,#256936,#256937,#256938,#256939,#256940,#256941,#256942,
#256943,#256944,#256945,#256946,#256947,#256948,#256949,#256950,#256951,
#256952,#256953),.UNSPECIFIED.,.F.,.F.,(4,3,3,3,3,3,3,3,4),(-110.907080642184,
-110.7678923387,-109.769983398712,-108.772074458723,-107.774165518735,-106.776256578747,
-105.778347638759,-104.78043869877,-104.623895335004),.UNSPECIFIED.);
#6614=B_SPLINE_CURVE_WITH_KNOTS('',3,(#256954,#256955,#256956,#256957,#256958,
#256959,#256960,#256961,#256962,#256963,#256964,#256965,#256966,#256967,
#256968,#256969,#256970,#256971,#256972,#256973,#256974,#256975,#256976,
#256977,#256978),.UNSPECIFIED.,.F.,.F.,(4,3,3,3,3,3,3,3,4),(101.648265323242,
101.786711878805,102.784620818794,103.782529758782,104.78043869877,105.778347638759,
106.776256578747,107.774165518735,107.931450630421),.UNSPECIFIED.);
#6615=B_SPLINE_CURVE_WITH_KNOTS('',3,(#256983,#256984,#256985,#256986,#256987,
#256988,#256989,#256990,#256991,#256992,#256993,#256994,#256995,#256996,
#256997,#256998,#256999,#257000,#257001,#257002,#257003,#257004),
 .UNSPECIFIED.,.F.,.F.,(4,3,3,3,3,3,3,4),(-117.190265949363,-116.75534597863,
-115.757437038641,-114.759528098653,-113.761619158665,-112.763710218677,
-111.765801278688,-110.907080642184),.UNSPECIFIED.);
#6616=B_SPLINE_CURVE_WITH_KNOTS('',3,(#257005,#257006,#257007,#257008,#257009,
#257010,#257011,#257012,#257013,#257014,#257015,#257016,#257017,#257018,
#257019,#257020,#257021,#257022,#257023,#257024,#257025,#257026),
 .UNSPECIFIED.,.F.,.F.,(4,3,3,3,3,3,3,4),(107.931450630421,108.772074458723,
109.769983398712,110.7678923387,111.765801278688,112.763710218677,113.761619158665,
114.214635937601),.UNSPECIFIED.);
#6617=B_SPLINE_CURVE_WITH_KNOTS('',3,(#257031,#257032,#257033,#257034,#257035,
#257036,#257037,#257038,#257039,#257040,#257041,#257042,#257043,#257044,
#257045,#257046,#257047,#257048,#257049,#257050,#257051,#257052),
 .UNSPECIFIED.,.F.,.F.,(4,3,3,3,3,3,3,4),(-123.473451256543,-122.742799618559,
-121.744890678571,-120.746981738583,-119.749072798595,-118.751163858606,
-117.753254918618,-117.190265949363),.UNSPECIFIED.);
#6618=B_SPLINE_CURVE_WITH_KNOTS('',3,(#257053,#257054,#257055,#257056,#257057,
#257058,#257059,#257060,#257061,#257062,#257063,#257064,#257065,#257066,
#257067,#257068,#257069,#257070,#257071,#257072,#257073,#257074),
 .UNSPECIFIED.,.F.,.F.,(4,3,3,3,3,3,3,4),(114.214635937601,114.759528098653,
115.757437038641,116.75534597863,117.753254918618,118.751163858606,119.749072798595,
120.49782124478),.UNSPECIFIED.);
#6619=B_SPLINE_CURVE_WITH_KNOTS('',3,(#257080,#257081,#257082,#257083,#257084,
#257085),.UNSPECIFIED.,.F.,.F.,(4,1,1,4),(135.088484104361,135.355741406366,
136.353650346354,137.27873899141),.UNSPECIFIED.);
#6620=B_SPLINE_CURVE_WITH_KNOTS('',3,(#257088,#257089,#257090,#257091),
 .UNSPECIFIED.,.F.,.F.,(4,4),(135.088484104361,136.039821870902),
 .UNSPECIFIED.);
#6621=B_SPLINE_CURVE_WITH_KNOTS('',3,(#257096,#257097,#257098,#257099,#257100,
#257101,#257102,#257103,#257104,#257105),.UNSPECIFIED.,.F.,.F.,(4,1,1,1,
1,1,1,4),(128.805298797182,129.368287766436,130.366196706425,131.364105646413,
132.362014586401,133.359923526389,134.357832466378,135.088484104361),
 .UNSPECIFIED.);
#6622=B_SPLINE_CURVE_WITH_KNOTS('',3,(#257106,#257107,#257108,#257109,#257110,
#257111,#257112,#257113,#257114,#257115,#257116),.UNSPECIFIED.,.F.,.F.,
(4,1,1,1,1,1,1,1,4),(128.805298797182,129.054459290984,130.052368230972,
131.05027717096,132.048186110949,133.046095050937,134.044003990925,135.041912930914,
135.088484104361),.UNSPECIFIED.);
#6623=B_SPLINE_CURVE_WITH_KNOTS('',3,(#257121,#257122,#257123,#257124,#257125,
#257126,#257127,#257128,#257129,#257130),.UNSPECIFIED.,.F.,.F.,(4,1,1,1,
1,1,1,4),(122.522113490002,123.380834126507,124.378743066495,125.376652006483,
126.374560946471,127.37246988646,128.370378826448,128.805298797182),
 .UNSPECIFIED.);
#6624=B_SPLINE_CURVE_WITH_KNOTS('',3,(#257131,#257132,#257133,#257134,#257135,
#257136,#257137,#257138,#257139,#257140),.UNSPECIFIED.,.F.,.F.,(4,1,1,1,
1,1,1,4),(122.522113490002,123.067005651054,124.064914591042,125.062823531031,
126.060732471019,127.058641411007,128.056550350996,128.805298797182),
 .UNSPECIFIED.);
#6625=B_SPLINE_CURVE_WITH_KNOTS('',3,(#257145,#257146,#257147,#257148,#257149,
#257150,#257151,#257152,#257153,#257154,#257155),.UNSPECIFIED.,.F.,.F.,
(4,1,1,1,1,1,1,1,4),(116.238928182822,116.395471546589,117.393380486577,
118.391289426565,119.389198366553,120.387107306542,121.38501624653,122.382925186518,
122.522113490002),.UNSPECIFIED.);
#6626=B_SPLINE_CURVE_WITH_KNOTS('',3,(#257156,#257157,#257158,#257159,#257160,
#257161,#257162,#257163,#257164,#257165),.UNSPECIFIED.,.F.,.F.,(4,1,1,1,
1,1,1,4),(116.238928182822,117.079552011124,118.077460951113,119.075369891101,
120.073278831089,121.071187771078,122.069096711066,122.522113490002),
 .UNSPECIFIED.);
#6627=B_SPLINE_CURVE_WITH_KNOTS('',3,(#257170,#257171,#257172,#257173,#257174,
#257175,#257176,#257177,#257178,#257179),.UNSPECIFIED.,.F.,.F.,(4,1,1,1,
1,1,1,4),(109.955742875643,110.408017906659,111.405926846647,112.403835786635,
113.401744726624,114.399653666612,115.3975626066,116.238928182822),
 .UNSPECIFIED.);
#6628=B_SPLINE_CURVE_WITH_KNOTS('',3,(#257180,#257181,#257182,#257183,#257184,
#257185,#257186,#257187,#257188,#257189,#257190),.UNSPECIFIED.,.F.,.F.,
(4,1,1,1,1,1,1,1,4),(109.955742875643,110.094189431206,111.092098371195,
112.090007311183,113.087916251171,114.08582519116,115.083734131148,116.081643071136,
116.238928182822),.UNSPECIFIED.);
#6629=B_SPLINE_CURVE_WITH_KNOTS('',3,(#257195,#257196,#257197,#257198,#257199,
#257200,#257201,#257202,#257203,#257204),.UNSPECIFIED.,.F.,.F.,(4,1,1,1,
1,1,1,4),(103.672557568463,104.420564266729,105.418473206717,106.416382146706,
107.414291086694,108.412200026682,109.41010896667,109.955742875643),
 .UNSPECIFIED.);
#6630=B_SPLINE_CURVE_WITH_KNOTS('',3,(#257205,#257206,#257207,#257208,#257209,
#257210,#257211,#257212,#257213,#257214),.UNSPECIFIED.,.F.,.F.,(4,1,1,1,
1,1,1,4),(103.672557568463,104.106735791277,105.104644731265,106.102553671253,
107.100462611242,108.09837155123,109.096280491218,109.955742875643),
 .UNSPECIFIED.);
#6631=B_SPLINE_CURVE_WITH_KNOTS('',3,(#257219,#257220,#257221,#257222,#257223,
#257224,#257225,#257226,#257227,#257228,#257229),.UNSPECIFIED.,.F.,.F.,
(4,1,1,1,1,1,1,1,4),(97.3893722612836,97.435201686811,98.4331106267993,
99.4310195667876,100.428928506776,101.426837446764,102.424746386752,103.422655326741,
103.672557568463),.UNSPECIFIED.);
#6632=B_SPLINE_CURVE_WITH_KNOTS('',3,(#257230,#257231,#257232,#257233,#257234,
#257235,#257236,#257237,#257238,#257239),.UNSPECIFIED.,.F.,.F.,(4,1,1,1,
1,1,1,4),(97.3893722612836,98.119282151347,99.1171910913353,100.115100031324,
101.113008971312,102.1109179113,103.108826851288,103.672557568463),
 .UNSPECIFIED.);
#6633=B_SPLINE_CURVE_WITH_KNOTS('',3,(#257244,#257245,#257246,#257247,#257248,
#257249,#257250,#257251,#257252,#257253),.UNSPECIFIED.,.F.,.F.,(4,1,1,1,
1,1,1,4),(91.106186954104,91.4477480468813,92.4456569868696,93.4435659268579,
94.4414748668462,95.4393838068345,96.4372927468227,97.3893722612836),
 .UNSPECIFIED.);
#6634=B_SPLINE_CURVE_WITH_KNOTS('',3,(#257254,#257255,#257256,#257257,#257258,
#257259,#257260,#257261,#257262,#257263,#257264),.UNSPECIFIED.,.F.,.F.,
(4,1,1,1,1,1,1,1,4),(91.106186954104,91.133919571429,92.1318285114173,93.1297374514056,
94.1276463913938,95.1255553313821,96.1234642713704,97.1213732113587,97.3893722612836),
 .UNSPECIFIED.);
#6635=B_SPLINE_CURVE_WITH_KNOTS('',3,(#257269,#257270,#257271,#257272,#257273,
#257274,#257275,#257276,#257277,#257278),.UNSPECIFIED.,.F.,.F.,(4,1,1,1,
1,1,1,4),(84.8230016469244,85.4602944069516,86.4582033469399,87.4561122869281,
88.4540212269164,89.4519301669047,90.449839106893,91.106186954104),
 .UNSPECIFIED.);
#6636=B_SPLINE_CURVE_WITH_KNOTS('',3,(#257279,#257280,#257281,#257282,#257283,
#257284,#257285,#257286,#257287,#257288),.UNSPECIFIED.,.F.,.F.,(4,1,1,1,
1,1,1,4),(84.8230016469244,85.1464659314993,86.1443748714875,87.1422838114758,
88.1401927514641,89.1381016914524,90.1360106314407,91.106186954104),
 .UNSPECIFIED.);
#6637=B_SPLINE_CURVE_WITH_KNOTS('',3,(#257293,#257294,#257295,#257296,#257297,
#257298,#257299,#257300,#257301,#257302),.UNSPECIFIED.,.F.,.F.,(4,1,1,1,
1,1,1,4),(78.5398163397448,79.4728407670218,80.4707497070101,81.4686586469984,
82.4665675869867,83.464476526975,84.4623854669633,84.8230016469244),
 .UNSPECIFIED.);
#6638=B_SPLINE_CURVE_WITH_KNOTS('',3,(#257303,#257304,#257305,#257306,#257307,
#257308,#257309,#257310,#257311,#257312),.UNSPECIFIED.,.F.,.F.,(4,1,1,1,
1,1,1,4),(78.5398163397448,79.1590122915695,80.1569212315578,81.1548301715461,
82.1527391115344,83.1506480515227,84.148556991511,84.8230016469244),
 .UNSPECIFIED.);
#6639=B_SPLINE_CURVE_WITH_KNOTS('',3,(#257317,#257318,#257319,#257320,#257321,
#257322,#257323,#257324,#257325,#257326,#257327),.UNSPECIFIED.,.F.,.F.,
(4,1,1,1,1,1,1,1,4),(72.2566310325652,72.4874781871038,73.4853871270921,
74.4832960670804,75.4812050070687,76.479113947057,77.4770228870453,78.4749318270335,
78.5398163397448),.UNSPECIFIED.);
#6640=B_SPLINE_CURVE_WITH_KNOTS('',3,(#257328,#257329,#257330,#257331,#257332,
#257333,#257334,#257335,#257336,#257337),.UNSPECIFIED.,.F.,.F.,(4,1,1,1,
1,1,1,4),(72.2566310325652,73.1715586516398,74.1694675916281,75.1673765316164,
76.1652854716046,77.1631944115929,78.1611033515812,78.5398163397448),
 .UNSPECIFIED.);
#6641=B_SPLINE_CURVE_WITH_KNOTS('',3,(#257342,#257343,#257344,#257345,#257346,
#257347,#257348,#257349,#257350,#257351),.UNSPECIFIED.,.F.,.F.,(4,1,1,1,
1,1,1,4),(65.9734457253856,66.5000245471741,67.4979334871624,68.4958424271507,
69.493751367139,70.4916603071272,71.4895692471155,72.2566310325652),
 .UNSPECIFIED.);
#6642=B_SPLINE_CURVE_WITH_KNOTS('',3,(#257352,#257353,#257354,#257355,#257356,
#257357,#257358,#257359,#257360,#257361,#257362),.UNSPECIFIED.,.F.,.F.,
(4,1,1,1,1,1,1,1,4),(65.9734457253856,66.1861960717218,67.1841050117101,
68.1820139516983,69.1799228916866,70.1778318316749,71.1757407716632,72.1736497116515,
72.2566310325652),.UNSPECIFIED.);
#6643=B_SPLINE_CURVE_WITH_KNOTS('',3,(#257367,#257368,#257369,#257370,#257371,
#257372,#257373,#257374,#257375,#257376),.UNSPECIFIED.,.F.,.F.,(4,1,1,1,
1,1,1,4),(59.690260418206,60.5125709072444,61.5104798472327,62.5083887872209,
63.5062977272092,64.5042066671975,65.5021156071858,65.9734457253856),
 .UNSPECIFIED.);
#6644=B_SPLINE_CURVE_WITH_KNOTS('',3,(#257377,#257378,#257379,#257380,#257381,
#257382,#257383,#257384,#257385,#257386),.UNSPECIFIED.,.F.,.F.,(4,1,1,1,
1,1,1,4),(59.690260418206,60.198742431792,61.1966513717803,62.1945603117686,
63.1924692517569,64.1903781917452,65.1882871317335,65.9734457253856),
 .UNSPECIFIED.);
#6645=B_SPLINE_CURVE_WITH_KNOTS('',3,(#257391,#257392,#257393,#257394,#257395,
#257396,#257397,#257398,#257399,#257400,#257401),.UNSPECIFIED.,.F.,.F.,
(4,1,1,1,1,1,1,1,4),(53.4070751110264,53.5272083273263,54.5251172673146,
55.5230262073029,56.5209351472912,57.5188440872795,58.5167530272678,59.5146619672561,
59.690260418206),.UNSPECIFIED.);
#6646=B_SPLINE_CURVE_WITH_KNOTS('',3,(#257402,#257403,#257404,#257405,#257406,
#257407,#257408,#257409,#257410,#257411),.UNSPECIFIED.,.F.,.F.,(4,1,1,1,
1,1,1,4),(53.4070751110264,54.2112887918623,55.2091977318506,56.2071066718389,
57.2050156118272,58.2029245518155,59.2008334918037,59.690260418206),
 .UNSPECIFIED.);
#6647=B_SPLINE_CURVE_WITH_KNOTS('',3,(#257416,#257417,#257418,#257419,#257420,
#257421,#257422,#257423,#257424,#257425),.UNSPECIFIED.,.F.,.F.,(4,1,1,1,
1,1,1,4),(47.1238898038468,47.5397546873966,48.5376636273849,49.5355725673732,
50.5334815073615,51.5313904473498,52.5292993873381,53.4070751110264),
 .UNSPECIFIED.);
#6648=B_SPLINE_CURVE_WITH_KNOTS('',3,(#257426,#257427,#257428,#257429,#257430,
#257431,#257432,#257433,#257434,#257435,#257436),.UNSPECIFIED.,.F.,.F.,
(4,1,1,1,1,1,1,1,4),(47.1238898038468,47.2259262119443,48.2238351519326,
49.2217440919209,50.2196530319092,51.2175619718974,52.2154709118857,53.213379851874,
53.4070751110264),.UNSPECIFIED.);
#6649=B_SPLINE_CURVE_WITH_KNOTS('',3,(#257441,#257442,#257443,#257444,#257445,
#257446,#257447,#257448,#257449,#257450),.UNSPECIFIED.,.F.,.F.,(4,1,1,1,
1,1,1,4),(40.8407044966673,41.5523010474669,42.5502099874552,43.5481189274435,
44.5460278674318,45.54393680742,46.5418457474083,47.1238898038468),
 .UNSPECIFIED.);
#6650=B_SPLINE_CURVE_WITH_KNOTS('',3,(#257451,#257452,#257453,#257454,#257455,
#257456,#257457,#257458,#257459,#257460),.UNSPECIFIED.,.F.,.F.,(4,1,1,1,
1,1,1,4),(40.8407044966672,41.2384725720146,42.2363815120028,43.2342904519911,
44.2321993919794,45.2301083319677,46.228017271956,47.1238898038468),
 .UNSPECIFIED.);
#6651=B_SPLINE_CURVE_WITH_KNOTS('',3,(#257465,#257466,#257467,#257468,#257469,
#257470,#257471,#257472,#257473,#257474,#257475),.UNSPECIFIED.,.F.,.F.,
(4,1,1,1,1,1,1,1,4),(34.5575191894877,34.5669384675489,35.5648474075372,
36.5627563475255,37.5606652875137,38.558574227502,39.5564831674903,40.5543921074786,
40.8407044966673),.UNSPECIFIED.);
#6652=B_SPLINE_CURVE_WITH_KNOTS('',3,(#257476,#257477,#257478,#257479,#257480,
#257481,#257482,#257483,#257484,#257485),.UNSPECIFIED.,.F.,.F.,(4,1,1,1,
1,1,1,4),(34.5575191894876,35.2510189320848,36.2489278720731,37.2468368120614,
38.2447457520497,39.242654692038,40.2405636320263,40.8407044966672),
 .UNSPECIFIED.);
#6653=B_SPLINE_CURVE_WITH_KNOTS('',3,(#257490,#257491,#257492,#257493,#257494,
#257495,#257496,#257497,#257498,#257499),.UNSPECIFIED.,.F.,.F.,(4,1,1,1,
1,1,1,4),(28.2743338823081,28.5794848276191,29.5773937676074,30.5753027075957,
31.573211647584,32.5711205875723,33.5690295275606,34.5575191894877),
 .UNSPECIFIED.);
#6654=B_SPLINE_CURVE_WITH_KNOTS('',3,(#257500,#257501,#257502,#257503,#257504,
#257505,#257506,#257507,#257508,#257509),.UNSPECIFIED.,.F.,.F.,(4,1,1,1,
1,1,1,4),(28.274333882308,29.2635652921551,30.2614742321434,31.2593831721317,
32.25729211212,33.2552010521082,34.2531099920965,34.5575191894876),
 .UNSPECIFIED.);
#6655=B_SPLINE_CURVE_WITH_KNOTS('',3,(#257514,#257515,#257516,#257517,#257518,
#257519,#257520,#257521,#257522,#257523),.UNSPECIFIED.,.F.,.F.,(4,1,1,1,
1,1,1,4),(21.9911485751285,22.5920311876894,23.5899401276777,24.587849067666,
25.5857580076543,26.5836669476426,27.5815758876309,28.2743338823081),
 .UNSPECIFIED.);
#6656=B_SPLINE_CURVE_WITH_KNOTS('',3,(#257524,#257525,#257526,#257527,#257528,
#257529,#257530,#257531,#257532,#257533,#257534),.UNSPECIFIED.,.F.,.F.,
(4,1,1,1,1,1,1,1,4),(21.9911485751285,22.2782027122371,23.2761116522254,
24.2740205922137,25.2719295322019,26.2698384721902,27.2677474121785,28.2656563521668,
28.274333882308),.UNSPECIFIED.);
#6657=B_SPLINE_CURVE_WITH_KNOTS('',3,(#257539,#257540,#257541,#257542,#257543,
#257544,#257545,#257546,#257547,#257548),.UNSPECIFIED.,.F.,.F.,(4,1,1,1,
1,1,1,4),(15.7079632679489,16.6045775477597,17.602486487748,18.6003954277363,
19.5983043677246,20.5962133077128,21.5941222477011,21.9911485751285),
 .UNSPECIFIED.);
#6658=B_SPLINE_CURVE_WITH_KNOTS('',3,(#257549,#257550,#257551,#257552,#257553,
#257554,#257555,#257556,#257557,#257558),.UNSPECIFIED.,.F.,.F.,(4,1,1,1,
1,1,1,4),(15.7079632679489,16.2907490723073,17.2886580122956,18.2865669522839,
19.2844758922722,20.2823848322605,21.2802937722488,21.9911485751285),
 .UNSPECIFIED.);
#6659=B_SPLINE_CURVE_WITH_KNOTS('',3,(#258084,#258085,#258086,#258087,#258088,
#258089,#258090,#258091,#258092,#258093,#258094,#258095,#258096,#258097,
#258098,#258099,#258100,#258101,#258102,#258103,#258104,#258105,#258106,
#258107,#258108,#258109,#258110,#258111,#258112,#258113,#258114,#258115,
#258116,#258117,#258118,#258119,#258120,#258121,#258122,#258123,#258124,
#258125,#258126,#258127,#258128,#258129,#258130,#258131,#258132,#258133,
#258134,#258135,#258136,#258137,#258138,#258139,#258140,#258141,#258142,
#258143,#258144,#258145,#258146,#258147,#258148,#258149,#258150,#258151,
#258152,#258153,#258154,#258155,#258156,#258157,#258158,#258159,#258160,
#258161,#258162,#258163,#258164,#258165,#258166,#258167,#258168,#258169,
#258170,#258171,#258172,#258173,#258174,#258175,#258176,#258177),
 .UNSPECIFIED.,.F.,.F.,(4,3,3,3,3,3,3,3,3,3,3,3,3,3,3,3,3,3,3,3,3,3,3,3,
3,3,3,3,3,3,3,4),(0.,0.0214813781660272,0.0505838925157975,0.0801385137508181,
0.107869705803836,0.112249638361506,0.116543512167008,0.145302650472993,
0.173939300969273,0.202061984063935,0.214552742327813,0.219720566839256,
0.223842900337521,0.251414063494629,0.278198363192956,0.301988050174959,
0.317818346313982,0.324029978565244,0.32770651927853,0.354360364834322,
0.381465816558906,0.408283310310737,0.418960437375512,0.42405923749684,
0.428492269676655,0.454806508102233,0.479923078176503,0.488621420709103,
0.494617238321095,0.519888501204842,0.544444359268273,0.555272788399315),
 .UNSPECIFIED.);
#6660=B_SPLINE_CURVE_WITH_KNOTS('',3,(#258178,#258179,#258180,#258181,#258182,
#258183,#258184,#258185,#258186,#258187,#258188,#258189,#258190,#258191,
#258192,#258193,#258194,#258195,#258196),.UNSPECIFIED.,.F.,.F.,(4,3,3,3,
3,3,4),(120.49782124478,120.746981738583,121.744890678571,122.742799618559,
123.740708558548,124.738617498536,125.663706143592),.UNSPECIFIED.);
#6661=B_SPLINE_CURVE_WITH_KNOTS('',3,(#258198,#258199,#258200,#258201,#258202,
#258203,#258204,#258205,#258206,#258207,#258208,#258209,#258210,#258211,
#258212,#258213,#258214,#258215,#258216,#258217,#258218,#258219,#258220,
#258221,#258222,#258223,#258224,#258225,#258226,#258227,#258228,#258229,
#258230,#258231,#258232,#258233,#258234,#258235,#258236,#258237,#258238,
#258239,#258240,#258241,#258242,#258243,#258244,#258245,#258246,#258247,
#258248,#258249,#258250,#258251,#258252,#258253,#258254,#258255,#258256,
#258257,#258258,#258259,#258260,#258261,#258262,#258263,#258264,#258265,
#258266,#258267,#258268,#258269,#258270,#258271,#258272,#258273,#258274,
#258275,#258276,#258277,#258278,#258279,#258280,#258281,#258282,#258283,
#258284,#258285,#258286,#258287,#258288),.UNSPECIFIED.,.F.,.F.,(4,3,3,3,
3,3,3,3,3,3,3,3,3,3,3,3,3,3,3,3,3,3,3,3,3,3,3,3,3,3,4),(-0.555272788399385,
-0.537726899847036,-0.513026435229613,-0.498613221691405,-0.492625231873332,
-0.487809143577052,-0.462024881019996,-0.439573648219782,-0.428798046855543,
-0.422005334072263,-0.395415250860688,-0.367165192800086,-0.345977649254635,
-0.330086991595546,-0.325505463211475,-0.320909481568035,-0.29299338650926,
-0.282415018618281,-0.255477639534726,-0.227997281807658,-0.221175758878058,
-0.216725875147774,-0.188767948011568,-0.160274771921768,-0.131545233209308,
-0.114320663149408,-0.109573931193616,-0.0800988261300781,-0.0505532193626863,
-0.0215812432970796,0.),.UNSPECIFIED.);
#6662=B_SPLINE_CURVE_WITH_KNOTS('',3,(#258289,#258290,#258291,#258292,#258293,
#258294,#258295,#258296,#258297),.UNSPECIFIED.,.F.,.F.,(4,1,1,1,1,1,4),
(10.3761157273101,11.3012043723659,12.2991133123542,13.2970222523425,14.2949311923308,
15.2928401323191,15.7079632679489),.UNSPECIFIED.);
#6663=B_SPLINE_CURVE_WITH_KNOTS('',3,(#258301,#258302,#258303,#258304,#258305,
#258306,#258307,#258308),.UNSPECIFIED.,.F.,.F.,(4,1,1,1,1,4),(11.6150328478182,
12.6129417878065,13.6108507277948,14.6087596677831,15.6066686077714,15.7079632679489),
 .UNSPECIFIED.);
#6664=B_SPLINE_CURVE_WITH_KNOTS('',3,(#258834,#258835,#258836,#258837,#258838,
#258839,#258840,#258841,#258842,#258843,#258844,#258845,#258846,#258847,
#258848,#258849,#258850,#258851,#258852,#258853,#258854,#258855,#258856,
#258857,#258858,#258859,#258860,#258861,#258862,#258863,#258864,#258865,
#258866,#258867,#258868,#258869,#258870,#258871,#258872,#258873,#258874,
#258875,#258876,#258877,#258878,#258879,#258880,#258881,#258882,#258883,
#258884,#258885,#258886,#258887,#258888,#258889,#258890,#258891,#258892,
#258893,#258894,#258895,#258896,#258897,#258898,#258899,#258900,#258901,
#258902,#258903,#258904,#258905,#258906,#258907,#258908,#258909,#258910,
#258911,#258912,#258913,#258914,#258915,#258916,#258917,#258918,#258919,
#258920,#258921,#258922,#258923,#258924),.UNSPECIFIED.,.F.,.F.,(4,3,3,3,
3,3,3,3,3,3,3,3,3,3,3,3,3,3,3,3,3,3,3,3,3,3,3,3,3,3,4),(0.,0.0174849238431529,
0.0419332631972337,0.0670144196872723,0.0926255346196509,0.0967052298288898,
0.122652670304572,0.149131552056777,0.175815054013557,0.187861423102457,
0.191997608729776,0.196039596500592,0.22346916945053,0.25081354005042,0.271903339146301,
0.289455966598097,0.293928127619864,0.298389623387338,0.325243438674775,
0.353681181137308,0.378564205792025,0.391569876135391,0.398068460749488,
0.403833210492476,0.432614996310579,0.462647591826694,0.472326582643484,
0.479347066777485,0.508920261877254,0.538120658281837,0.552745378375041),
 .UNSPECIFIED.);
#6665=B_SPLINE_CURVE_WITH_KNOTS('',3,(#258925,#258926,#258927,#258928,#258929,
#258930,#258931,#258932,#258933,#258934,#258935,#258936,#258937,#258938,
#258939,#258940,#258941,#258942,#258943,#258944,#258945,#258946,#258947,
#258948,#258949,#258950,#258951,#258952,#258953,#258954,#258955,#258956,
#258957,#258958,#258959,#258960,#258961,#258962,#258963,#258964,#258965,
#258966,#258967,#258968,#258969,#258970,#258971,#258972,#258973,#258974,
#258975,#258976,#258977,#258978,#258979,#258980,#258981,#258982,#258983,
#258984,#258985,#258986,#258987,#258988,#258989,#258990,#258991,#258992,
#258993,#258994,#258995,#258996,#258997,#258998,#258999,#259000,#259001,
#259002,#259003,#259004,#259005,#259006,#259007,#259008,#259009,#259010,
#259011,#259012,#259013,#259014,#259015,#259016,#259017,#259018),
 .UNSPECIFIED.,.F.,.F.,(4,3,3,3,3,3,3,3,3,3,3,3,3,3,3,3,3,3,3,3,3,3,3,3,
3,3,3,3,3,3,3,4),(-0.552745378375042,-0.531365175220741,-0.50199118119805,
-0.486392955571644,-0.478698871637525,-0.472093120190076,-0.443039610913716,
-0.419212105946447,-0.408417630877946,-0.402068045911971,-0.397493898918164,
-0.369186424191986,-0.339994710937879,-0.31287506792229,-0.297350354313209,
-0.291440280452355,-0.264636789556101,-0.252419571175559,-0.225055087621416,
-0.196923201668739,-0.192596225544785,-0.188249308569056,-0.161608602690815,
-0.135009133177477,-0.108835418443703,-0.0999141223704662,-0.0941324867604078,
-0.0901669524830973,-0.0646229578829025,-0.0394810387994913,-0.0151229871705641,
0.),.UNSPECIFIED.);
#6666=B_SPLINE_CURVE_WITH_KNOTS('',3,(#259019,#259020,#259021,#259022,#259023,
#259024,#259025,#259026,#259027,#259028,#259029,#259030,#259031,#259032,
#259033,#259034),.UNSPECIFIED.,.F.,.F.,(4,3,3,3,3,4),(-127.732344318501,
-126.734435378513,-125.736526438524,-124.738617498536,-123.740708558548,
-123.473451256543),.UNSPECIFIED.);
#6667=LINE('',#32410,#7852);
#6668=LINE('',#32419,#7853);
#6669=LINE('',#32436,#7854);
#6670=LINE('',#32487,#7855);
#6671=LINE('',#32538,#7856);
#6672=LINE('',#32586,#7857);
#6673=LINE('',#32637,#7858);
#6674=LINE('',#32688,#7859);
#6675=LINE('',#32736,#7860);
#6676=LINE('',#32787,#7861);
#6677=LINE('',#32838,#7862);
#6678=LINE('',#32886,#7863);
#6679=LINE('',#32937,#7864);
#6680=LINE('',#32988,#7865);
#6681=LINE('',#33036,#7866);
#6682=LINE('',#33087,#7867);
#6683=LINE('',#33126,#7868);
#6684=LINE('',#33150,#7869);
#6685=LINE('',#33174,#7870);
#6686=LINE('',#33199,#7871);
#6687=LINE('',#33224,#7872);
#6688=LINE('',#33248,#7873);
#6689=LINE('',#33273,#7874);
#6690=LINE('',#33298,#7875);
#6691=LINE('',#33322,#7876);
#6692=LINE('',#33347,#7877);
#6693=LINE('',#33372,#7878);
#6694=LINE('',#33396,#7879);
#6695=LINE('',#33421,#7880);
#6696=LINE('',#33446,#7881);
#6697=LINE('',#33470,#7882);
#6698=LINE('',#33487,#7883);
#6699=LINE('',#33496,#7884);
#6700=LINE('',#33513,#7885);
#6701=LINE('',#33564,#7886);
#6702=LINE('',#33615,#7887);
#6703=LINE('',#33663,#7888);
#6704=LINE('',#33714,#7889);
#6705=LINE('',#33765,#7890);
#6706=LINE('',#33813,#7891);
#6707=LINE('',#33864,#7892);
#6708=LINE('',#33915,#7893);
#6709=LINE('',#33963,#7894);
#6710=LINE('',#34014,#7895);
#6711=LINE('',#34065,#7896);
#6712=LINE('',#34113,#7897);
#6713=LINE('',#34164,#7898);
#6714=LINE('',#34203,#7899);
#6715=LINE('',#34227,#7900);
#6716=LINE('',#34251,#7901);
#6717=LINE('',#34276,#7902);
#6718=LINE('',#34301,#7903);
#6719=LINE('',#34325,#7904);
#6720=LINE('',#34350,#7905);
#6721=LINE('',#34375,#7906);
#6722=LINE('',#34399,#7907);
#6723=LINE('',#34424,#7908);
#6724=LINE('',#34449,#7909);
#6725=LINE('',#34473,#7910);
#6726=LINE('',#34498,#7911);
#6727=LINE('',#34523,#7912);
#6728=LINE('',#34547,#7913);
#6729=LINE('',#34564,#7914);
#6730=LINE('',#34573,#7915);
#6731=LINE('',#34590,#7916);
#6732=LINE('',#34641,#7917);
#6733=LINE('',#34692,#7918);
#6734=LINE('',#34740,#7919);
#6735=LINE('',#34791,#7920);
#6736=LINE('',#34842,#7921);
#6737=LINE('',#34890,#7922);
#6738=LINE('',#34941,#7923);
#6739=LINE('',#34992,#7924);
#6740=LINE('',#35040,#7925);
#6741=LINE('',#35091,#7926);
#6742=LINE('',#35142,#7927);
#6743=LINE('',#35190,#7928);
#6744=LINE('',#35241,#7929);
#6745=LINE('',#35280,#7930);
#6746=LINE('',#35304,#7931);
#6747=LINE('',#35328,#7932);
#6748=LINE('',#35353,#7933);
#6749=LINE('',#35378,#7934);
#6750=LINE('',#35402,#7935);
#6751=LINE('',#35427,#7936);
#6752=LINE('',#35452,#7937);
#6753=LINE('',#35476,#7938);
#6754=LINE('',#35501,#7939);
#6755=LINE('',#35526,#7940);
#6756=LINE('',#35550,#7941);
#6757=LINE('',#35575,#7942);
#6758=LINE('',#35600,#7943);
#6759=LINE('',#35624,#7944);
#6760=LINE('',#35641,#7945);
#6761=LINE('',#35650,#7946);
#6762=LINE('',#35667,#7947);
#6763=LINE('',#35718,#7948);
#6764=LINE('',#35769,#7949);
#6765=LINE('',#35817,#7950);
#6766=LINE('',#35868,#7951);
#6767=LINE('',#35919,#7952);
#6768=LINE('',#35967,#7953);
#6769=LINE('',#36018,#7954);
#6770=LINE('',#36069,#7955);
#6771=LINE('',#36117,#7956);
#6772=LINE('',#36168,#7957);
#6773=LINE('',#36219,#7958);
#6774=LINE('',#36267,#7959);
#6775=LINE('',#36318,#7960);
#6776=LINE('',#36357,#7961);
#6777=LINE('',#36381,#7962);
#6778=LINE('',#36405,#7963);
#6779=LINE('',#36430,#7964);
#6780=LINE('',#36455,#7965);
#6781=LINE('',#36479,#7966);
#6782=LINE('',#36504,#7967);
#6783=LINE('',#36529,#7968);
#6784=LINE('',#36553,#7969);
#6785=LINE('',#36578,#7970);
#6786=LINE('',#36603,#7971);
#6787=LINE('',#36627,#7972);
#6788=LINE('',#36652,#7973);
#6789=LINE('',#36677,#7974);
#6790=LINE('',#36701,#7975);
#6791=LINE('',#36718,#7976);
#6792=LINE('',#36727,#7977);
#6793=LINE('',#36744,#7978);
#6794=LINE('',#36795,#7979);
#6795=LINE('',#36846,#7980);
#6796=LINE('',#36894,#7981);
#6797=LINE('',#36945,#7982);
#6798=LINE('',#36996,#7983);
#6799=LINE('',#37044,#7984);
#6800=LINE('',#37095,#7985);
#6801=LINE('',#37146,#7986);
#6802=LINE('',#37194,#7987);
#6803=LINE('',#37245,#7988);
#6804=LINE('',#37296,#7989);
#6805=LINE('',#37344,#7990);
#6806=LINE('',#37395,#7991);
#6807=LINE('',#37434,#7992);
#6808=LINE('',#37458,#7993);
#6809=LINE('',#37482,#7994);
#6810=LINE('',#37507,#7995);
#6811=LINE('',#37532,#7996);
#6812=LINE('',#37556,#7997);
#6813=LINE('',#37581,#7998);
#6814=LINE('',#37606,#7999);
#6815=LINE('',#37630,#8000);
#6816=LINE('',#37655,#8001);
#6817=LINE('',#37680,#8002);
#6818=LINE('',#37704,#8003);
#6819=LINE('',#37729,#8004);
#6820=LINE('',#37754,#8005);
#6821=LINE('',#37778,#8006);
#6822=LINE('',#37795,#8007);
#6823=LINE('',#37804,#8008);
#6824=LINE('',#37821,#8009);
#6825=LINE('',#37872,#8010);
#6826=LINE('',#37923,#8011);
#6827=LINE('',#37971,#8012);
#6828=LINE('',#38022,#8013);
#6829=LINE('',#38073,#8014);
#6830=LINE('',#38121,#8015);
#6831=LINE('',#38172,#8016);
#6832=LINE('',#38223,#8017);
#6833=LINE('',#38271,#8018);
#6834=LINE('',#38322,#8019);
#6835=LINE('',#38373,#8020);
#6836=LINE('',#38421,#8021);
#6837=LINE('',#38472,#8022);
#6838=LINE('',#38511,#8023);
#6839=LINE('',#38535,#8024);
#6840=LINE('',#38559,#8025);
#6841=LINE('',#38584,#8026);
#6842=LINE('',#38609,#8027);
#6843=LINE('',#38633,#8028);
#6844=LINE('',#38658,#8029);
#6845=LINE('',#38683,#8030);
#6846=LINE('',#38707,#8031);
#6847=LINE('',#38732,#8032);
#6848=LINE('',#38757,#8033);
#6849=LINE('',#38781,#8034);
#6850=LINE('',#38806,#8035);
#6851=LINE('',#38831,#8036);
#6852=LINE('',#38855,#8037);
#6853=LINE('',#38872,#8038);
#6854=LINE('',#38881,#8039);
#6855=LINE('',#38898,#8040);
#6856=LINE('',#38949,#8041);
#6857=LINE('',#39000,#8042);
#6858=LINE('',#39048,#8043);
#6859=LINE('',#39099,#8044);
#6860=LINE('',#39150,#8045);
#6861=LINE('',#39198,#8046);
#6862=LINE('',#39249,#8047);
#6863=LINE('',#39300,#8048);
#6864=LINE('',#39348,#8049);
#6865=LINE('',#39399,#8050);
#6866=LINE('',#39450,#8051);
#6867=LINE('',#39498,#8052);
#6868=LINE('',#39549,#8053);
#6869=LINE('',#39588,#8054);
#6870=LINE('',#39612,#8055);
#6871=LINE('',#39636,#8056);
#6872=LINE('',#39661,#8057);
#6873=LINE('',#39686,#8058);
#6874=LINE('',#39710,#8059);
#6875=LINE('',#39735,#8060);
#6876=LINE('',#39760,#8061);
#6877=LINE('',#39784,#8062);
#6878=LINE('',#39809,#8063);
#6879=LINE('',#39834,#8064);
#6880=LINE('',#39858,#8065);
#6881=LINE('',#39883,#8066);
#6882=LINE('',#39908,#8067);
#6883=LINE('',#39932,#8068);
#6884=LINE('',#39949,#8069);
#6885=LINE('',#39958,#8070);
#6886=LINE('',#39975,#8071);
#6887=LINE('',#40026,#8072);
#6888=LINE('',#40077,#8073);
#6889=LINE('',#40125,#8074);
#6890=LINE('',#40176,#8075);
#6891=LINE('',#40227,#8076);
#6892=LINE('',#40275,#8077);
#6893=LINE('',#40326,#8078);
#6894=LINE('',#40377,#8079);
#6895=LINE('',#40425,#8080);
#6896=LINE('',#40476,#8081);
#6897=LINE('',#40527,#8082);
#6898=LINE('',#40575,#8083);
#6899=LINE('',#40626,#8084);
#6900=LINE('',#40665,#8085);
#6901=LINE('',#40689,#8086);
#6902=LINE('',#40713,#8087);
#6903=LINE('',#40738,#8088);
#6904=LINE('',#40763,#8089);
#6905=LINE('',#40787,#8090);
#6906=LINE('',#40812,#8091);
#6907=LINE('',#40837,#8092);
#6908=LINE('',#40861,#8093);
#6909=LINE('',#40886,#8094);
#6910=LINE('',#40911,#8095);
#6911=LINE('',#40935,#8096);
#6912=LINE('',#40960,#8097);
#6913=LINE('',#40985,#8098);
#6914=LINE('',#41009,#8099);
#6915=LINE('',#41045,#8100);
#6916=LINE('',#41143,#8101);
#6917=LINE('',#41214,#8102);
#6918=LINE('',#41298,#8103);
#6919=LINE('',#41365,#8104);
#6920=LINE('',#41463,#8105);
#6921=LINE('',#41534,#8106);
#6922=LINE('',#41618,#8107);
#6923=LINE('',#41685,#8108);
#6924=LINE('',#41783,#8109);
#6925=LINE('',#41854,#8110);
#6926=LINE('',#41938,#8111);
#6927=LINE('',#51971,#8112);
#6928=LINE('',#51977,#8113);
#6929=LINE('',#51983,#8114);
#6930=LINE('',#51989,#8115);
#6931=LINE('',#51995,#8116);
#6932=LINE('',#52003,#8117);
#6933=LINE('',#52004,#8118);
#6934=LINE('',#52005,#8119);
#6935=LINE('',#52007,#8120);
#6936=LINE('',#52012,#8121);
#6937=LINE('',#52013,#8122);
#6938=LINE('',#52014,#8123);
#6939=LINE('',#52016,#8124);
#6940=LINE('',#52024,#8125);
#6941=LINE('',#52028,#8126);
#6942=LINE('',#52055,#8127);
#6943=LINE('',#52118,#8128);
#6944=LINE('',#52154,#8129);
#6945=LINE('',#52200,#8130);
#6946=LINE('',#52217,#8131);
#6947=LINE('',#52222,#8132);
#6948=LINE('',#52224,#8133);
#6949=LINE('',#52233,#8134);
#6950=LINE('',#52239,#8135);
#6951=LINE('',#52245,#8136);
#6952=LINE('',#52251,#8137);
#6953=LINE('',#52257,#8138);
#6954=LINE('',#52263,#8139);
#6955=LINE('',#52269,#8140);
#6956=LINE('',#52275,#8141);
#6957=LINE('',#52281,#8142);
#6958=LINE('',#52287,#8143);
#6959=LINE('',#52295,#8144);
#6960=LINE('',#52297,#8145);
#6961=LINE('',#52299,#8146);
#6962=LINE('',#52300,#8147);
#6963=LINE('',#52305,#8148);
#6964=LINE('',#52306,#8149);
#6965=LINE('',#52309,#8150);
#6966=LINE('',#52311,#8151);
#6967=LINE('',#52312,#8152);
#6968=LINE('',#52314,#8153);
#6969=LINE('',#52321,#8154);
#6970=LINE('',#52332,#8155);
#6971=LINE('',#52337,#8156);
#6972=LINE('',#52348,#8157);
#6973=LINE('',#52360,#8158);
#6974=LINE('',#52363,#8159);
#6975=LINE('',#52374,#8160);
#6976=LINE('',#52377,#8161);
#6977=LINE('',#52380,#8162);
#6978=LINE('',#52386,#8163);
#6979=LINE('',#52392,#8164);
#6980=LINE('',#52418,#8165);
#6981=LINE('',#52481,#8166);
#6982=LINE('',#52517,#8167);
#6983=LINE('',#52563,#8168);
#6984=LINE('',#53228,#8169);
#6985=LINE('',#54124,#8170);
#6986=LINE('',#55020,#8171);
#6987=LINE('',#55916,#8172);
#6988=LINE('',#56812,#8173);
#6989=LINE('',#57708,#8174);
#6990=LINE('',#58604,#8175);
#6991=LINE('',#59500,#8176);
#6992=LINE('',#60396,#8177);
#6993=LINE('',#61292,#8178);
#6994=LINE('',#62188,#8179);
#6995=LINE('',#63084,#8180);
#6996=LINE('',#63980,#8181);
#6997=LINE('',#64876,#8182);
#6998=LINE('',#65772,#8183);
#6999=LINE('',#66668,#8184);
#7000=LINE('',#67564,#8185);
#7001=LINE('',#68460,#8186);
#7002=LINE('',#69356,#8187);
#7003=LINE('',#70252,#8188);
#7004=LINE('',#71148,#8189);
#7005=LINE('',#72044,#8190);
#7006=LINE('',#72940,#8191);
#7007=LINE('',#73836,#8192);
#7008=LINE('',#74732,#8193);
#7009=LINE('',#75628,#8194);
#7010=LINE('',#76524,#8195);
#7011=LINE('',#77420,#8196);
#7012=LINE('',#78316,#8197);
#7013=LINE('',#79212,#8198);
#7014=LINE('',#80108,#8199);
#7015=LINE('',#81004,#8200);
#7016=LINE('',#81900,#8201);
#7017=LINE('',#82796,#8202);
#7018=LINE('',#83692,#8203);
#7019=LINE('',#84588,#8204);
#7020=LINE('',#85484,#8205);
#7021=LINE('',#86380,#8206);
#7022=LINE('',#87276,#8207);
#7023=LINE('',#88172,#8208);
#7024=LINE('',#89068,#8209);
#7025=LINE('',#89964,#8210);
#7026=LINE('',#90860,#8211);
#7027=LINE('',#91756,#8212);
#7028=LINE('',#92652,#8213);
#7029=LINE('',#93548,#8214);
#7030=LINE('',#94444,#8215);
#7031=LINE('',#95340,#8216);
#7032=LINE('',#96236,#8217);
#7033=LINE('',#97132,#8218);
#7034=LINE('',#98028,#8219);
#7035=LINE('',#98924,#8220);
#7036=LINE('',#99820,#8221);
#7037=LINE('',#100716,#8222);
#7038=LINE('',#101612,#8223);
#7039=LINE('',#102508,#8224);
#7040=LINE('',#103404,#8225);
#7041=LINE('',#104300,#8226);
#7042=LINE('',#105196,#8227);
#7043=LINE('',#106092,#8228);
#7044=LINE('',#106988,#8229);
#7045=LINE('',#107884,#8230);
#7046=LINE('',#108780,#8231);
#7047=LINE('',#109676,#8232);
#7048=LINE('',#110572,#8233);
#7049=LINE('',#111468,#8234);
#7050=LINE('',#112364,#8235);
#7051=LINE('',#113260,#8236);
#7052=LINE('',#114156,#8237);
#7053=LINE('',#115052,#8238);
#7054=LINE('',#115948,#8239);
#7055=LINE('',#116798,#8240);
#7056=LINE('',#117599,#8241);
#7057=LINE('',#118400,#8242);
#7058=LINE('',#119201,#8243);
#7059=LINE('',#120002,#8244);
#7060=LINE('',#120803,#8245);
#7061=LINE('',#121604,#8246);
#7062=LINE('',#122405,#8247);
#7063=LINE('',#123206,#8248);
#7064=LINE('',#124007,#8249);
#7065=LINE('',#124808,#8250);
#7066=LINE('',#125609,#8251);
#7067=LINE('',#126410,#8252);
#7068=LINE('',#127211,#8253);
#7069=LINE('',#128012,#8254);
#7070=LINE('',#128813,#8255);
#7071=LINE('',#129614,#8256);
#7072=LINE('',#130415,#8257);
#7073=LINE('',#131216,#8258);
#7074=LINE('',#132017,#8259);
#7075=LINE('',#132818,#8260);
#7076=LINE('',#133619,#8261);
#7077=LINE('',#134420,#8262);
#7078=LINE('',#135221,#8263);
#7079=LINE('',#136022,#8264);
#7080=LINE('',#136823,#8265);
#7081=LINE('',#137624,#8266);
#7082=LINE('',#138425,#8267);
#7083=LINE('',#139226,#8268);
#7084=LINE('',#140027,#8269);
#7085=LINE('',#140828,#8270);
#7086=LINE('',#141629,#8271);
#7087=LINE('',#142430,#8272);
#7088=LINE('',#143231,#8273);
#7089=LINE('',#144032,#8274);
#7090=LINE('',#144833,#8275);
#7091=LINE('',#145634,#8276);
#7092=LINE('',#146435,#8277);
#7093=LINE('',#147236,#8278);
#7094=LINE('',#148037,#8279);
#7095=LINE('',#148838,#8280);
#7096=LINE('',#149639,#8281);
#7097=LINE('',#150440,#8282);
#7098=LINE('',#151241,#8283);
#7099=LINE('',#152042,#8284);
#7100=LINE('',#152843,#8285);
#7101=LINE('',#153644,#8286);
#7102=LINE('',#154445,#8287);
#7103=LINE('',#155246,#8288);
#7104=LINE('',#156047,#8289);
#7105=LINE('',#156848,#8290);
#7106=LINE('',#157649,#8291);
#7107=LINE('',#158450,#8292);
#7108=LINE('',#159251,#8293);
#7109=LINE('',#160052,#8294);
#7110=LINE('',#160853,#8295);
#7111=LINE('',#161654,#8296);
#7112=LINE('',#162455,#8297);
#7113=LINE('',#163256,#8298);
#7114=LINE('',#164057,#8299);
#7115=LINE('',#164858,#8300);
#7116=LINE('',#165659,#8301);
#7117=LINE('',#166460,#8302);
#7118=LINE('',#167261,#8303);
#7119=LINE('',#168062,#8304);
#7120=LINE('',#168863,#8305);
#7121=LINE('',#169664,#8306);
#7122=LINE('',#170465,#8307);
#7123=LINE('',#171266,#8308);
#7124=LINE('',#172067,#8309);
#7125=LINE('',#172868,#8310);
#7126=LINE('',#173067,#8311);
#7127=LINE('',#173280,#8312);
#7128=LINE('',#174980,#8313);
#7129=LINE('',#174982,#8314);
#7130=LINE('',#174989,#8315);
#7131=LINE('',#174991,#8316);
#7132=LINE('',#174993,#8317);
#7133=LINE('',#174994,#8318);
#7134=LINE('',#174998,#8319);
#7135=LINE('',#175000,#8320);
#7136=LINE('',#175002,#8321);
#7137=LINE('',#175003,#8322);
#7138=LINE('',#175005,#8323);
#7139=LINE('',#175006,#8324);
#7140=LINE('',#175427,#8325);
#7141=LINE('',#175435,#8326);
#7142=LINE('',#175851,#8327);
#7143=LINE('',#175859,#8328);
#7144=LINE('',#176275,#8329);
#7145=LINE('',#176283,#8330);
#7146=LINE('',#176699,#8331);
#7147=LINE('',#176707,#8332);
#7148=LINE('',#177123,#8333);
#7149=LINE('',#177131,#8334);
#7150=LINE('',#177547,#8335);
#7151=LINE('',#177555,#8336);
#7152=LINE('',#177971,#8337);
#7153=LINE('',#177979,#8338);
#7154=LINE('',#178395,#8339);
#7155=LINE('',#178403,#8340);
#7156=LINE('',#178819,#8341);
#7157=LINE('',#178827,#8342);
#7158=LINE('',#179243,#8343);
#7159=LINE('',#179251,#8344);
#7160=LINE('',#179667,#8345);
#7161=LINE('',#179675,#8346);
#7162=LINE('',#180091,#8347);
#7163=LINE('',#180099,#8348);
#7164=LINE('',#180515,#8349);
#7165=LINE('',#180523,#8350);
#7166=LINE('',#180939,#8351);
#7167=LINE('',#180947,#8352);
#7168=LINE('',#181363,#8353);
#7169=LINE('',#181371,#8354);
#7170=LINE('',#181787,#8355);
#7171=LINE('',#181795,#8356);
#7172=LINE('',#182211,#8357);
#7173=LINE('',#182219,#8358);
#7174=LINE('',#182635,#8359);
#7175=LINE('',#182643,#8360);
#7176=LINE('',#183059,#8361);
#7177=LINE('',#183067,#8362);
#7178=LINE('',#183483,#8363);
#7179=LINE('',#183491,#8364);
#7180=LINE('',#183907,#8365);
#7181=LINE('',#183915,#8366);
#7182=LINE('',#184331,#8367);
#7183=LINE('',#184339,#8368);
#7184=LINE('',#184755,#8369);
#7185=LINE('',#184763,#8370);
#7186=LINE('',#185179,#8371);
#7187=LINE('',#185186,#8372);
#7188=LINE('',#185191,#8373);
#7189=LINE('',#185192,#8374);
#7190=LINE('',#185195,#8375);
#7191=LINE('',#185196,#8376);
#7192=LINE('',#185201,#8377);
#7193=LINE('',#185202,#8378);
#7194=LINE('',#185209,#8379);
#7195=LINE('',#185210,#8380);
#7196=LINE('',#185213,#8381);
#7197=LINE('',#185214,#8382);
#7198=LINE('',#185219,#8383);
#7199=LINE('',#185220,#8384);
#7200=LINE('',#185227,#8385);
#7201=LINE('',#185228,#8386);
#7202=LINE('',#185231,#8387);
#7203=LINE('',#185232,#8388);
#7204=LINE('',#185237,#8389);
#7205=LINE('',#185238,#8390);
#7206=LINE('',#185245,#8391);
#7207=LINE('',#185246,#8392);
#7208=LINE('',#185249,#8393);
#7209=LINE('',#185250,#8394);
#7210=LINE('',#185255,#8395);
#7211=LINE('',#185256,#8396);
#7212=LINE('',#185263,#8397);
#7213=LINE('',#185264,#8398);
#7214=LINE('',#185267,#8399);
#7215=LINE('',#185268,#8400);
#7216=LINE('',#185273,#8401);
#7217=LINE('',#185274,#8402);
#7218=LINE('',#185281,#8403);
#7219=LINE('',#185282,#8404);
#7220=LINE('',#185285,#8405);
#7221=LINE('',#185286,#8406);
#7222=LINE('',#185291,#8407);
#7223=LINE('',#185292,#8408);
#7224=LINE('',#185299,#8409);
#7225=LINE('',#185300,#8410);
#7226=LINE('',#185303,#8411);
#7227=LINE('',#185304,#8412);
#7228=LINE('',#185309,#8413);
#7229=LINE('',#185310,#8414);
#7230=LINE('',#185317,#8415);
#7231=LINE('',#185318,#8416);
#7232=LINE('',#185321,#8417);
#7233=LINE('',#185322,#8418);
#7234=LINE('',#185327,#8419);
#7235=LINE('',#185328,#8420);
#7236=LINE('',#185335,#8421);
#7237=LINE('',#185336,#8422);
#7238=LINE('',#185339,#8423);
#7239=LINE('',#185340,#8424);
#7240=LINE('',#185345,#8425);
#7241=LINE('',#185346,#8426);
#7242=LINE('',#185353,#8427);
#7243=LINE('',#185354,#8428);
#7244=LINE('',#185357,#8429);
#7245=LINE('',#185358,#8430);
#7246=LINE('',#185363,#8431);
#7247=LINE('',#185364,#8432);
#7248=LINE('',#185371,#8433);
#7249=LINE('',#185372,#8434);
#7250=LINE('',#185375,#8435);
#7251=LINE('',#185376,#8436);
#7252=LINE('',#185381,#8437);
#7253=LINE('',#185382,#8438);
#7254=LINE('',#185389,#8439);
#7255=LINE('',#185390,#8440);
#7256=LINE('',#185393,#8441);
#7257=LINE('',#185394,#8442);
#7258=LINE('',#185399,#8443);
#7259=LINE('',#185400,#8444);
#7260=LINE('',#185407,#8445);
#7261=LINE('',#185408,#8446);
#7262=LINE('',#185411,#8447);
#7263=LINE('',#185412,#8448);
#7264=LINE('',#185417,#8449);
#7265=LINE('',#185418,#8450);
#7266=LINE('',#185425,#8451);
#7267=LINE('',#185426,#8452);
#7268=LINE('',#185429,#8453);
#7269=LINE('',#185430,#8454);
#7270=LINE('',#185435,#8455);
#7271=LINE('',#185436,#8456);
#7272=LINE('',#185443,#8457);
#7273=LINE('',#185444,#8458);
#7274=LINE('',#185447,#8459);
#7275=LINE('',#185448,#8460);
#7276=LINE('',#185453,#8461);
#7277=LINE('',#185454,#8462);
#7278=LINE('',#185461,#8463);
#7279=LINE('',#185462,#8464);
#7280=LINE('',#185465,#8465);
#7281=LINE('',#185466,#8466);
#7282=LINE('',#185471,#8467);
#7283=LINE('',#185472,#8468);
#7284=LINE('',#185479,#8469);
#7285=LINE('',#185480,#8470);
#7286=LINE('',#185483,#8471);
#7287=LINE('',#185484,#8472);
#7288=LINE('',#185489,#8473);
#7289=LINE('',#185490,#8474);
#7290=LINE('',#185497,#8475);
#7291=LINE('',#185498,#8476);
#7292=LINE('',#185501,#8477);
#7293=LINE('',#185502,#8478);
#7294=LINE('',#185507,#8479);
#7295=LINE('',#185508,#8480);
#7296=LINE('',#185515,#8481);
#7297=LINE('',#185516,#8482);
#7298=LINE('',#185519,#8483);
#7299=LINE('',#185520,#8484);
#7300=LINE('',#185525,#8485);
#7301=LINE('',#185526,#8486);
#7302=LINE('',#185533,#8487);
#7303=LINE('',#185534,#8488);
#7304=LINE('',#185537,#8489);
#7305=LINE('',#185538,#8490);
#7306=LINE('',#185543,#8491);
#7307=LINE('',#185544,#8492);
#7308=LINE('',#185551,#8493);
#7309=LINE('',#185552,#8494);
#7310=LINE('',#185555,#8495);
#7311=LINE('',#185556,#8496);
#7312=LINE('',#185561,#8497);
#7313=LINE('',#185562,#8498);
#7314=LINE('',#185569,#8499);
#7315=LINE('',#185570,#8500);
#7316=LINE('',#185573,#8501);
#7317=LINE('',#185574,#8502);
#7318=LINE('',#185579,#8503);
#7319=LINE('',#185580,#8504);
#7320=LINE('',#185587,#8505);
#7321=LINE('',#185588,#8506);
#7322=LINE('',#185591,#8507);
#7323=LINE('',#185592,#8508);
#7324=LINE('',#185597,#8509);
#7325=LINE('',#185598,#8510);
#7326=LINE('',#185603,#8511);
#7327=LINE('',#185604,#8512);
#7328=LINE('',#186221,#8513);
#7329=LINE('',#186838,#8514);
#7330=LINE('',#186841,#8515);
#7331=LINE('',#186842,#8516);
#7332=LINE('',#187459,#8517);
#7333=LINE('',#188076,#8518);
#7334=LINE('',#188079,#8519);
#7335=LINE('',#188080,#8520);
#7336=LINE('',#188697,#8521);
#7337=LINE('',#189314,#8522);
#7338=LINE('',#189317,#8523);
#7339=LINE('',#189318,#8524);
#7340=LINE('',#189935,#8525);
#7341=LINE('',#190552,#8526);
#7342=LINE('',#190555,#8527);
#7343=LINE('',#190556,#8528);
#7344=LINE('',#191173,#8529);
#7345=LINE('',#191790,#8530);
#7346=LINE('',#191793,#8531);
#7347=LINE('',#191794,#8532);
#7348=LINE('',#192411,#8533);
#7349=LINE('',#193028,#8534);
#7350=LINE('',#193031,#8535);
#7351=LINE('',#193032,#8536);
#7352=LINE('',#193649,#8537);
#7353=LINE('',#194266,#8538);
#7354=LINE('',#194269,#8539);
#7355=LINE('',#194270,#8540);
#7356=LINE('',#194887,#8541);
#7357=LINE('',#195504,#8542);
#7358=LINE('',#195507,#8543);
#7359=LINE('',#195508,#8544);
#7360=LINE('',#196125,#8545);
#7361=LINE('',#196742,#8546);
#7362=LINE('',#196745,#8547);
#7363=LINE('',#196746,#8548);
#7364=LINE('',#197363,#8549);
#7365=LINE('',#197980,#8550);
#7366=LINE('',#197983,#8551);
#7367=LINE('',#197984,#8552);
#7368=LINE('',#198601,#8553);
#7369=LINE('',#199218,#8554);
#7370=LINE('',#199221,#8555);
#7371=LINE('',#199222,#8556);
#7372=LINE('',#199839,#8557);
#7373=LINE('',#200456,#8558);
#7374=LINE('',#200459,#8559);
#7375=LINE('',#200460,#8560);
#7376=LINE('',#201077,#8561);
#7377=LINE('',#201694,#8562);
#7378=LINE('',#201697,#8563);
#7379=LINE('',#201698,#8564);
#7380=LINE('',#202315,#8565);
#7381=LINE('',#202932,#8566);
#7382=LINE('',#202935,#8567);
#7383=LINE('',#202936,#8568);
#7384=LINE('',#203553,#8569);
#7385=LINE('',#204170,#8570);
#7386=LINE('',#204173,#8571);
#7387=LINE('',#204174,#8572);
#7388=LINE('',#204791,#8573);
#7389=LINE('',#205408,#8574);
#7390=LINE('',#205411,#8575);
#7391=LINE('',#205412,#8576);
#7392=LINE('',#206029,#8577);
#7393=LINE('',#206646,#8578);
#7394=LINE('',#206649,#8579);
#7395=LINE('',#206650,#8580);
#7396=LINE('',#207267,#8581);
#7397=LINE('',#207884,#8582);
#7398=LINE('',#207887,#8583);
#7399=LINE('',#207888,#8584);
#7400=LINE('',#208505,#8585);
#7401=LINE('',#209122,#8586);
#7402=LINE('',#209125,#8587);
#7403=LINE('',#209126,#8588);
#7404=LINE('',#209743,#8589);
#7405=LINE('',#210360,#8590);
#7406=LINE('',#210363,#8591);
#7407=LINE('',#210364,#8592);
#7408=LINE('',#210981,#8593);
#7409=LINE('',#211598,#8594);
#7410=LINE('',#211601,#8595);
#7411=LINE('',#211602,#8596);
#7412=LINE('',#212219,#8597);
#7413=LINE('',#212836,#8598);
#7414=LINE('',#212839,#8599);
#7415=LINE('',#212840,#8600);
#7416=LINE('',#213457,#8601);
#7417=LINE('',#214074,#8602);
#7418=LINE('',#214307,#8603);
#7419=LINE('',#214315,#8604);
#7420=LINE('',#214524,#8605);
#7421=LINE('',#214548,#8606);
#7422=LINE('',#214549,#8607);
#7423=LINE('',#214551,#8608);
#7424=LINE('',#214553,#8609);
#7425=LINE('',#214554,#8610);
#7426=LINE('',#214557,#8611);
#7427=LINE('',#215378,#8612);
#7428=LINE('',#215386,#8613);
#7429=LINE('',#215389,#8614);
#7430=LINE('',#215392,#8615);
#7431=LINE('',#215394,#8616);
#7432=LINE('',#215395,#8617);
#7433=LINE('',#215401,#8618);
#7434=LINE('',#215404,#8619);
#7435=LINE('',#215413,#8620);
#7436=LINE('',#215416,#8621);
#7437=LINE('',#215419,#8622);
#7438=LINE('',#215421,#8623);
#7439=LINE('',#215422,#8624);
#7440=LINE('',#215428,#8625);
#7441=LINE('',#215431,#8626);
#7442=LINE('',#215440,#8627);
#7443=LINE('',#215443,#8628);
#7444=LINE('',#215446,#8629);
#7445=LINE('',#215448,#8630);
#7446=LINE('',#215449,#8631);
#7447=LINE('',#215455,#8632);
#7448=LINE('',#215458,#8633);
#7449=LINE('',#215467,#8634);
#7450=LINE('',#215470,#8635);
#7451=LINE('',#215473,#8636);
#7452=LINE('',#215475,#8637);
#7453=LINE('',#215476,#8638);
#7454=LINE('',#215482,#8639);
#7455=LINE('',#215485,#8640);
#7456=LINE('',#215494,#8641);
#7457=LINE('',#215497,#8642);
#7458=LINE('',#215500,#8643);
#7459=LINE('',#215502,#8644);
#7460=LINE('',#215503,#8645);
#7461=LINE('',#215509,#8646);
#7462=LINE('',#215512,#8647);
#7463=LINE('',#215521,#8648);
#7464=LINE('',#215524,#8649);
#7465=LINE('',#215527,#8650);
#7466=LINE('',#215529,#8651);
#7467=LINE('',#215530,#8652);
#7468=LINE('',#215536,#8653);
#7469=LINE('',#215539,#8654);
#7470=LINE('',#215548,#8655);
#7471=LINE('',#215551,#8656);
#7472=LINE('',#215554,#8657);
#7473=LINE('',#215556,#8658);
#7474=LINE('',#215557,#8659);
#7475=LINE('',#215563,#8660);
#7476=LINE('',#215566,#8661);
#7477=LINE('',#215575,#8662);
#7478=LINE('',#215578,#8663);
#7479=LINE('',#215581,#8664);
#7480=LINE('',#215583,#8665);
#7481=LINE('',#215584,#8666);
#7482=LINE('',#215590,#8667);
#7483=LINE('',#215593,#8668);
#7484=LINE('',#215602,#8669);
#7485=LINE('',#215605,#8670);
#7486=LINE('',#215608,#8671);
#7487=LINE('',#215610,#8672);
#7488=LINE('',#215611,#8673);
#7489=LINE('',#215617,#8674);
#7490=LINE('',#215620,#8675);
#7491=LINE('',#215629,#8676);
#7492=LINE('',#215632,#8677);
#7493=LINE('',#215635,#8678);
#7494=LINE('',#215637,#8679);
#7495=LINE('',#215638,#8680);
#7496=LINE('',#215644,#8681);
#7497=LINE('',#215647,#8682);
#7498=LINE('',#215656,#8683);
#7499=LINE('',#215659,#8684);
#7500=LINE('',#215662,#8685);
#7501=LINE('',#215664,#8686);
#7502=LINE('',#215665,#8687);
#7503=LINE('',#215671,#8688);
#7504=LINE('',#215674,#8689);
#7505=LINE('',#215683,#8690);
#7506=LINE('',#215686,#8691);
#7507=LINE('',#215689,#8692);
#7508=LINE('',#215691,#8693);
#7509=LINE('',#215692,#8694);
#7510=LINE('',#215698,#8695);
#7511=LINE('',#215701,#8696);
#7512=LINE('',#215710,#8697);
#7513=LINE('',#215713,#8698);
#7514=LINE('',#215716,#8699);
#7515=LINE('',#215718,#8700);
#7516=LINE('',#215719,#8701);
#7517=LINE('',#215725,#8702);
#7518=LINE('',#215728,#8703);
#7519=LINE('',#215737,#8704);
#7520=LINE('',#215740,#8705);
#7521=LINE('',#215743,#8706);
#7522=LINE('',#215745,#8707);
#7523=LINE('',#215746,#8708);
#7524=LINE('',#215752,#8709);
#7525=LINE('',#215755,#8710);
#7526=LINE('',#215764,#8711);
#7527=LINE('',#215767,#8712);
#7528=LINE('',#215770,#8713);
#7529=LINE('',#215772,#8714);
#7530=LINE('',#215773,#8715);
#7531=LINE('',#215779,#8716);
#7532=LINE('',#215782,#8717);
#7533=LINE('',#215791,#8718);
#7534=LINE('',#215794,#8719);
#7535=LINE('',#215797,#8720);
#7536=LINE('',#215799,#8721);
#7537=LINE('',#215800,#8722);
#7538=LINE('',#215806,#8723);
#7539=LINE('',#215809,#8724);
#7540=LINE('',#215818,#8725);
#7541=LINE('',#215821,#8726);
#7542=LINE('',#215824,#8727);
#7543=LINE('',#215826,#8728);
#7544=LINE('',#215827,#8729);
#7545=LINE('',#215833,#8730);
#7546=LINE('',#215836,#8731);
#7547=LINE('',#215845,#8732);
#7548=LINE('',#215848,#8733);
#7549=LINE('',#215851,#8734);
#7550=LINE('',#215853,#8735);
#7551=LINE('',#215854,#8736);
#7552=LINE('',#215860,#8737);
#7553=LINE('',#215863,#8738);
#7554=LINE('',#215872,#8739);
#7555=LINE('',#215875,#8740);
#7556=LINE('',#215878,#8741);
#7557=LINE('',#215880,#8742);
#7558=LINE('',#215881,#8743);
#7559=LINE('',#215887,#8744);
#7560=LINE('',#215890,#8745);
#7561=LINE('',#215899,#8746);
#7562=LINE('',#215902,#8747);
#7563=LINE('',#215905,#8748);
#7564=LINE('',#215907,#8749);
#7565=LINE('',#215908,#8750);
#7566=LINE('',#215914,#8751);
#7567=LINE('',#215917,#8752);
#7568=LINE('',#215926,#8753);
#7569=LINE('',#215929,#8754);
#7570=LINE('',#215932,#8755);
#7571=LINE('',#215934,#8756);
#7572=LINE('',#215935,#8757);
#7573=LINE('',#215941,#8758);
#7574=LINE('',#215944,#8759);
#7575=LINE('',#215953,#8760);
#7576=LINE('',#215956,#8761);
#7577=LINE('',#215959,#8762);
#7578=LINE('',#215961,#8763);
#7579=LINE('',#215962,#8764);
#7580=LINE('',#215968,#8765);
#7581=LINE('',#215971,#8766);
#7582=LINE('',#215980,#8767);
#7583=LINE('',#215983,#8768);
#7584=LINE('',#215986,#8769);
#7585=LINE('',#215988,#8770);
#7586=LINE('',#215989,#8771);
#7587=LINE('',#215995,#8772);
#7588=LINE('',#215998,#8773);
#7589=LINE('',#216004,#8774);
#7590=LINE('',#216006,#8775);
#7591=LINE('',#216007,#8776);
#7592=LINE('',#216625,#8777);
#7593=LINE('',#217653,#8778);
#7594=LINE('',#217656,#8779);
#7595=LINE('',#217658,#8780);
#7596=LINE('',#217659,#8781);
#7597=LINE('',#218277,#8782);
#7598=LINE('',#219305,#8783);
#7599=LINE('',#219308,#8784);
#7600=LINE('',#219310,#8785);
#7601=LINE('',#219311,#8786);
#7602=LINE('',#219929,#8787);
#7603=LINE('',#220957,#8788);
#7604=LINE('',#220960,#8789);
#7605=LINE('',#220962,#8790);
#7606=LINE('',#220963,#8791);
#7607=LINE('',#221581,#8792);
#7608=LINE('',#222609,#8793);
#7609=LINE('',#222612,#8794);
#7610=LINE('',#222614,#8795);
#7611=LINE('',#222615,#8796);
#7612=LINE('',#223233,#8797);
#7613=LINE('',#224261,#8798);
#7614=LINE('',#224264,#8799);
#7615=LINE('',#224266,#8800);
#7616=LINE('',#224267,#8801);
#7617=LINE('',#224885,#8802);
#7618=LINE('',#225913,#8803);
#7619=LINE('',#225916,#8804);
#7620=LINE('',#225918,#8805);
#7621=LINE('',#225919,#8806);
#7622=LINE('',#226537,#8807);
#7623=LINE('',#227565,#8808);
#7624=LINE('',#227568,#8809);
#7625=LINE('',#227570,#8810);
#7626=LINE('',#227571,#8811);
#7627=LINE('',#228189,#8812);
#7628=LINE('',#229217,#8813);
#7629=LINE('',#229220,#8814);
#7630=LINE('',#229222,#8815);
#7631=LINE('',#229223,#8816);
#7632=LINE('',#229841,#8817);
#7633=LINE('',#230869,#8818);
#7634=LINE('',#230872,#8819);
#7635=LINE('',#230874,#8820);
#7636=LINE('',#230875,#8821);
#7637=LINE('',#231493,#8822);
#7638=LINE('',#232521,#8823);
#7639=LINE('',#232524,#8824);
#7640=LINE('',#232526,#8825);
#7641=LINE('',#232527,#8826);
#7642=LINE('',#233145,#8827);
#7643=LINE('',#234173,#8828);
#7644=LINE('',#234176,#8829);
#7645=LINE('',#234178,#8830);
#7646=LINE('',#234179,#8831);
#7647=LINE('',#234797,#8832);
#7648=LINE('',#235825,#8833);
#7649=LINE('',#235828,#8834);
#7650=LINE('',#235830,#8835);
#7651=LINE('',#235831,#8836);
#7652=LINE('',#236449,#8837);
#7653=LINE('',#237477,#8838);
#7654=LINE('',#237480,#8839);
#7655=LINE('',#237482,#8840);
#7656=LINE('',#237483,#8841);
#7657=LINE('',#238101,#8842);
#7658=LINE('',#239129,#8843);
#7659=LINE('',#239132,#8844);
#7660=LINE('',#239134,#8845);
#7661=LINE('',#239135,#8846);
#7662=LINE('',#239753,#8847);
#7663=LINE('',#240781,#8848);
#7664=LINE('',#240784,#8849);
#7665=LINE('',#240786,#8850);
#7666=LINE('',#240787,#8851);
#7667=LINE('',#241405,#8852);
#7668=LINE('',#242433,#8853);
#7669=LINE('',#242436,#8854);
#7670=LINE('',#242438,#8855);
#7671=LINE('',#242439,#8856);
#7672=LINE('',#243057,#8857);
#7673=LINE('',#244085,#8858);
#7674=LINE('',#244088,#8859);
#7675=LINE('',#244090,#8860);
#7676=LINE('',#244091,#8861);
#7677=LINE('',#244709,#8862);
#7678=LINE('',#245737,#8863);
#7679=LINE('',#245740,#8864);
#7680=LINE('',#245742,#8865);
#7681=LINE('',#245743,#8866);
#7682=LINE('',#246361,#8867);
#7683=LINE('',#247389,#8868);
#7684=LINE('',#247392,#8869);
#7685=LINE('',#247394,#8870);
#7686=LINE('',#247395,#8871);
#7687=LINE('',#248013,#8872);
#7688=LINE('',#249041,#8873);
#7689=LINE('',#249044,#8874);
#7690=LINE('',#249046,#8875);
#7691=LINE('',#249047,#8876);
#7692=LINE('',#249665,#8877);
#7693=LINE('',#250693,#8878);
#7694=LINE('',#250696,#8879);
#7695=LINE('',#250698,#8880);
#7696=LINE('',#250699,#8881);
#7697=LINE('',#251317,#8882);
#7698=LINE('',#252345,#8883);
#7699=LINE('',#252348,#8884);
#7700=LINE('',#252350,#8885);
#7701=LINE('',#252351,#8886);
#7702=LINE('',#252969,#8887);
#7703=LINE('',#253997,#8888);
#7704=LINE('',#254230,#8889);
#7705=LINE('',#254238,#8890);
#7706=LINE('',#254658,#8891);
#7707=LINE('',#254666,#8892);
#7708=LINE('',#254899,#8893);
#7709=LINE('',#254923,#8894);
#7710=LINE('',#254924,#8895);
#7711=LINE('',#254926,#8896);
#7712=LINE('',#254928,#8897);
#7713=LINE('',#254929,#8898);
#7714=LINE('',#254932,#8899);
#7715=LINE('',#255753,#8900);
#7716=LINE('',#255755,#8901);
#7717=LINE('',#255762,#8902);
#7718=LINE('',#255768,#8903);
#7719=LINE('',#255776,#8904);
#7720=LINE('',#255778,#8905);
#7721=LINE('',#255780,#8906);
#7722=LINE('',#255781,#8907);
#7723=LINE('',#255786,#8908);
#7724=LINE('',#255787,#8909);
#7725=LINE('',#255790,#8910);
#7726=LINE('',#255792,#8911);
#7727=LINE('',#255793,#8912);
#7728=LINE('',#255795,#8913);
#7729=LINE('',#255802,#8914);
#7730=LINE('',#255813,#8915);
#7731=LINE('',#255818,#8916);
#7732=LINE('',#255829,#8917);
#7733=LINE('',#255834,#8918);
#7734=LINE('',#255840,#8919);
#7735=LINE('',#255846,#8920);
#7736=LINE('',#255859,#8921);
#7737=LINE('',#255862,#8922);
#7738=LINE('',#255865,#8923);
#7739=LINE('',#255878,#8924);
#7740=LINE('',#255881,#8925);
#7741=LINE('',#255887,#8926);
#7742=LINE('',#255891,#8927);
#7743=LINE('',#255897,#8928);
#7744=LINE('',#255905,#8929);
#7745=LINE('',#255907,#8930);
#7746=LINE('',#255909,#8931);
#7747=LINE('',#255910,#8932);
#7748=LINE('',#255913,#8933);
#7749=LINE('',#255915,#8934);
#7750=LINE('',#255916,#8935);
#7751=LINE('',#255919,#8936);
#7752=LINE('',#255921,#8937);
#7753=LINE('',#255922,#8938);
#7754=LINE('',#255924,#8939);
#7755=LINE('',#255925,#8940);
#7756=LINE('',#255933,#8941);
#7757=LINE('',#255939,#8942);
#7758=LINE('',#255948,#8943);
#7759=LINE('',#255959,#8944);
#7760=LINE('',#255967,#8945);
#7761=LINE('',#255971,#8946);
#7762=LINE('',#255977,#8947);
#7763=LINE('',#255979,#8948);
#7764=LINE('',#255981,#8949);
#7765=LINE('',#255982,#8950);
#7766=LINE('',#255986,#8951);
#7767=LINE('',#255988,#8952);
#7768=LINE('',#255990,#8953);
#7769=LINE('',#255991,#8954);
#7770=LINE('',#256005,#8955);
#7771=LINE('',#256011,#8956);
#7772=LINE('',#256020,#8957);
#7773=LINE('',#256026,#8958);
#7774=LINE('',#256035,#8959);
#7775=LINE('',#256041,#8960);
#7776=LINE('',#256049,#8961);
#7777=LINE('',#256051,#8962);
#7778=LINE('',#256053,#8963);
#7779=LINE('',#256054,#8964);
#7780=LINE('',#256058,#8965);
#7781=LINE('',#256060,#8966);
#7782=LINE('',#256062,#8967);
#7783=LINE('',#256063,#8968);
#7784=LINE('',#256076,#8969);
#7785=LINE('',#256078,#8970);
#7786=LINE('',#256080,#8971);
#7787=LINE('',#256081,#8972);
#7788=LINE('',#256085,#8973);
#7789=LINE('',#256087,#8974);
#7790=LINE('',#256089,#8975);
#7791=LINE('',#256090,#8976);
#7792=LINE('',#256104,#8977);
#7793=LINE('',#256112,#8978);
#7794=LINE('',#256136,#8979);
#7795=LINE('',#256184,#8980);
#7796=LINE('',#256232,#8981);
#7797=LINE('',#256283,#8982);
#7798=LINE('',#256334,#8983);
#7799=LINE('',#256382,#8984);
#7800=LINE('',#256430,#8985);
#7801=LINE('',#256484,#8986);
#7802=LINE('',#256532,#8987);
#7803=LINE('',#256580,#8988);
#7804=LINE('',#256634,#8989);
#7805=LINE('',#256682,#8990);
#7806=LINE('',#256730,#8991);
#7807=LINE('',#256778,#8992);
#7808=LINE('',#256832,#8993);
#7809=LINE('',#256880,#8994);
#7810=LINE('',#256928,#8995);
#7811=LINE('',#256982,#8996);
#7812=LINE('',#257030,#8997);
#7813=LINE('',#257078,#8998);
#7814=LINE('',#257095,#8999);
#7815=LINE('',#257120,#9000);
#7816=LINE('',#257144,#9001);
#7817=LINE('',#257169,#9002);
#7818=LINE('',#257194,#9003);
#7819=LINE('',#257218,#9004);
#7820=LINE('',#257243,#9005);
#7821=LINE('',#257268,#9006);
#7822=LINE('',#257292,#9007);
#7823=LINE('',#257316,#9008);
#7824=LINE('',#257341,#9009);
#7825=LINE('',#257366,#9010);
#7826=LINE('',#257390,#9011);
#7827=LINE('',#257415,#9012);
#7828=LINE('',#257440,#9013);
#7829=LINE('',#257464,#9014);
#7830=LINE('',#257489,#9015);
#7831=LINE('',#257513,#9016);
#7832=LINE('',#257538,#9017);
#7833=LINE('',#259040,#9018);
#7834=LINE('',#259042,#9019);
#7835=LINE('',#259044,#9020);
#7836=LINE('',#259045,#9021);
#7837=LINE('',#259048,#9022);
#7838=LINE('',#259050,#9023);
#7839=LINE('',#259051,#9024);
#7840=LINE('',#259054,#9025);
#7841=LINE('',#259056,#9026);
#7842=LINE('',#259057,#9027);
#7843=LINE('',#259060,#9028);
#7844=LINE('',#259062,#9029);
#7845=LINE('',#259063,#9030);
#7846=LINE('',#259066,#9031);
#7847=LINE('',#259068,#9032);
#7848=LINE('',#259069,#9033);
#7849=LINE('',#259071,#9034);
#7850=LINE('',#259072,#9035);
#7851=LINE('',#259079,#9036);
#7852=VECTOR('',#27340,3.);
#7853=VECTOR('',#27343,3.);
#7854=VECTOR('',#27350,3.);
#7855=VECTOR('',#27353,3.);
#7856=VECTOR('',#27356,3.);
#7857=VECTOR('',#27359,3.);
#7858=VECTOR('',#27362,3.);
#7859=VECTOR('',#27365,3.);
#7860=VECTOR('',#27368,3.);
#7861=VECTOR('',#27371,3.);
#7862=VECTOR('',#27374,3.);
#7863=VECTOR('',#27377,3.);
#7864=VECTOR('',#27380,3.);
#7865=VECTOR('',#27383,3.);
#7866=VECTOR('',#27386,3.);
#7867=VECTOR('',#27389,3.);
#7868=VECTOR('',#27394,3.0735);
#7869=VECTOR('',#27399,3.0735);
#7870=VECTOR('',#27402,3.0735);
#7871=VECTOR('',#27405,3.0735);
#7872=VECTOR('',#27408,3.0735);
#7873=VECTOR('',#27411,3.0735);
#7874=VECTOR('',#27414,3.0735);
#7875=VECTOR('',#27417,3.0735);
#7876=VECTOR('',#27420,3.0735);
#7877=VECTOR('',#27423,3.0735);
#7878=VECTOR('',#27426,3.0735);
#7879=VECTOR('',#27429,3.0735);
#7880=VECTOR('',#27432,3.0735);
#7881=VECTOR('',#27435,3.0735);
#7882=VECTOR('',#27438,3.0735);
#7883=VECTOR('',#27443,3.);
#7884=VECTOR('',#27446,3.);
#7885=VECTOR('',#27453,3.);
#7886=VECTOR('',#27456,3.);
#7887=VECTOR('',#27459,3.);
#7888=VECTOR('',#27462,3.);
#7889=VECTOR('',#27465,3.);
#7890=VECTOR('',#27468,3.);
#7891=VECTOR('',#27471,3.);
#7892=VECTOR('',#27474,3.);
#7893=VECTOR('',#27477,3.);
#7894=VECTOR('',#27480,3.);
#7895=VECTOR('',#27483,3.);
#7896=VECTOR('',#27486,3.);
#7897=VECTOR('',#27489,3.);
#7898=VECTOR('',#27492,3.);
#7899=VECTOR('',#27497,3.0735);
#7900=VECTOR('',#27502,3.0735);
#7901=VECTOR('',#27505,3.0735);
#7902=VECTOR('',#27508,3.0735);
#7903=VECTOR('',#27511,3.0735);
#7904=VECTOR('',#27514,3.0735);
#7905=VECTOR('',#27517,3.0735);
#7906=VECTOR('',#27520,3.0735);
#7907=VECTOR('',#27523,3.0735);
#7908=VECTOR('',#27526,3.0735);
#7909=VECTOR('',#27529,3.0735);
#7910=VECTOR('',#27532,3.0735);
#7911=VECTOR('',#27535,3.0735);
#7912=VECTOR('',#27538,3.0735);
#7913=VECTOR('',#27541,3.0735);
#7914=VECTOR('',#27546,3.);
#7915=VECTOR('',#27549,3.);
#7916=VECTOR('',#27556,3.);
#7917=VECTOR('',#27559,3.);
#7918=VECTOR('',#27562,3.);
#7919=VECTOR('',#27565,3.);
#7920=VECTOR('',#27568,3.);
#7921=VECTOR('',#27571,3.);
#7922=VECTOR('',#27574,3.);
#7923=VECTOR('',#27577,3.);
#7924=VECTOR('',#27580,3.);
#7925=VECTOR('',#27583,3.);
#7926=VECTOR('',#27586,3.);
#7927=VECTOR('',#27589,3.);
#7928=VECTOR('',#27592,3.);
#7929=VECTOR('',#27595,3.);
#7930=VECTOR('',#27600,3.0735);
#7931=VECTOR('',#27605,3.0735);
#7932=VECTOR('',#27608,3.0735);
#7933=VECTOR('',#27611,3.0735);
#7934=VECTOR('',#27614,3.0735);
#7935=VECTOR('',#27617,3.0735);
#7936=VECTOR('',#27620,3.0735);
#7937=VECTOR('',#27623,3.0735);
#7938=VECTOR('',#27626,3.0735);
#7939=VECTOR('',#27629,3.0735);
#7940=VECTOR('',#27632,3.0735);
#7941=VECTOR('',#27635,3.0735);
#7942=VECTOR('',#27638,3.0735);
#7943=VECTOR('',#27641,3.0735);
#7944=VECTOR('',#27644,3.0735);
#7945=VECTOR('',#27649,3.);
#7946=VECTOR('',#27652,3.);
#7947=VECTOR('',#27659,3.);
#7948=VECTOR('',#27662,3.);
#7949=VECTOR('',#27665,3.);
#7950=VECTOR('',#27668,3.);
#7951=VECTOR('',#27671,3.);
#7952=VECTOR('',#27674,3.);
#7953=VECTOR('',#27677,3.);
#7954=VECTOR('',#27680,3.);
#7955=VECTOR('',#27683,3.);
#7956=VECTOR('',#27686,3.);
#7957=VECTOR('',#27689,3.);
#7958=VECTOR('',#27692,3.);
#7959=VECTOR('',#27695,3.);
#7960=VECTOR('',#27698,3.);
#7961=VECTOR('',#27703,3.0735);
#7962=VECTOR('',#27708,3.0735);
#7963=VECTOR('',#27711,3.0735);
#7964=VECTOR('',#27714,3.0735);
#7965=VECTOR('',#27717,3.0735);
#7966=VECTOR('',#27720,3.0735);
#7967=VECTOR('',#27723,3.0735);
#7968=VECTOR('',#27726,3.0735);
#7969=VECTOR('',#27729,3.0735);
#7970=VECTOR('',#27732,3.0735);
#7971=VECTOR('',#27735,3.0735);
#7972=VECTOR('',#27738,3.0735);
#7973=VECTOR('',#27741,3.0735);
#7974=VECTOR('',#27744,3.0735);
#7975=VECTOR('',#27747,3.0735);
#7976=VECTOR('',#27752,3.);
#7977=VECTOR('',#27755,3.);
#7978=VECTOR('',#27762,3.);
#7979=VECTOR('',#27765,3.);
#7980=VECTOR('',#27768,3.);
#7981=VECTOR('',#27771,3.);
#7982=VECTOR('',#27774,3.);
#7983=VECTOR('',#27777,3.);
#7984=VECTOR('',#27780,3.);
#7985=VECTOR('',#27783,3.);
#7986=VECTOR('',#27786,3.);
#7987=VECTOR('',#27789,3.);
#7988=VECTOR('',#27792,3.);
#7989=VECTOR('',#27795,3.);
#7990=VECTOR('',#27798,3.);
#7991=VECTOR('',#27801,3.);
#7992=VECTOR('',#27806,3.0735);
#7993=VECTOR('',#27811,3.0735);
#7994=VECTOR('',#27814,3.0735);
#7995=VECTOR('',#27817,3.0735);
#7996=VECTOR('',#27820,3.0735);
#7997=VECTOR('',#27823,3.0735);
#7998=VECTOR('',#27826,3.0735);
#7999=VECTOR('',#27829,3.0735);
#8000=VECTOR('',#27832,3.0735);
#8001=VECTOR('',#27835,3.0735);
#8002=VECTOR('',#27838,3.0735);
#8003=VECTOR('',#27841,3.0735);
#8004=VECTOR('',#27844,3.0735);
#8005=VECTOR('',#27847,3.0735);
#8006=VECTOR('',#27850,3.0735);
#8007=VECTOR('',#27855,3.);
#8008=VECTOR('',#27858,3.);
#8009=VECTOR('',#27865,3.);
#8010=VECTOR('',#27868,3.);
#8011=VECTOR('',#27871,3.);
#8012=VECTOR('',#27874,3.);
#8013=VECTOR('',#27877,3.);
#8014=VECTOR('',#27880,3.);
#8015=VECTOR('',#27883,3.);
#8016=VECTOR('',#27886,3.);
#8017=VECTOR('',#27889,3.);
#8018=VECTOR('',#27892,3.);
#8019=VECTOR('',#27895,3.);
#8020=VECTOR('',#27898,3.);
#8021=VECTOR('',#27901,3.);
#8022=VECTOR('',#27904,3.);
#8023=VECTOR('',#27909,3.0735);
#8024=VECTOR('',#27914,3.0735);
#8025=VECTOR('',#27917,3.0735);
#8026=VECTOR('',#27920,3.0735);
#8027=VECTOR('',#27923,3.0735);
#8028=VECTOR('',#27926,3.0735);
#8029=VECTOR('',#27929,3.0735);
#8030=VECTOR('',#27932,3.0735);
#8031=VECTOR('',#27935,3.0735);
#8032=VECTOR('',#27938,3.0735);
#8033=VECTOR('',#27941,3.0735);
#8034=VECTOR('',#27944,3.0735);
#8035=VECTOR('',#27947,3.0735);
#8036=VECTOR('',#27950,3.0735);
#8037=VECTOR('',#27953,3.0735);
#8038=VECTOR('',#27958,3.);
#8039=VECTOR('',#27961,3.);
#8040=VECTOR('',#27968,3.);
#8041=VECTOR('',#27971,3.);
#8042=VECTOR('',#27974,3.);
#8043=VECTOR('',#27977,3.);
#8044=VECTOR('',#27980,3.);
#8045=VECTOR('',#27983,3.);
#8046=VECTOR('',#27986,3.);
#8047=VECTOR('',#27989,3.);
#8048=VECTOR('',#27992,3.);
#8049=VECTOR('',#27995,3.);
#8050=VECTOR('',#27998,3.);
#8051=VECTOR('',#28001,3.);
#8052=VECTOR('',#28004,3.);
#8053=VECTOR('',#28007,3.);
#8054=VECTOR('',#28012,3.0735);
#8055=VECTOR('',#28017,3.0735);
#8056=VECTOR('',#28020,3.0735);
#8057=VECTOR('',#28023,3.0735);
#8058=VECTOR('',#28026,3.0735);
#8059=VECTOR('',#28029,3.0735);
#8060=VECTOR('',#28032,3.0735);
#8061=VECTOR('',#28035,3.0735);
#8062=VECTOR('',#28038,3.0735);
#8063=VECTOR('',#28041,3.0735);
#8064=VECTOR('',#28044,3.0735);
#8065=VECTOR('',#28047,3.0735);
#8066=VECTOR('',#28050,3.0735);
#8067=VECTOR('',#28053,3.0735);
#8068=VECTOR('',#28056,3.0735);
#8069=VECTOR('',#28061,3.);
#8070=VECTOR('',#28064,3.);
#8071=VECTOR('',#28071,3.);
#8072=VECTOR('',#28074,3.);
#8073=VECTOR('',#28077,3.);
#8074=VECTOR('',#28080,3.);
#8075=VECTOR('',#28083,3.);
#8076=VECTOR('',#28086,3.);
#8077=VECTOR('',#28089,3.);
#8078=VECTOR('',#28092,3.);
#8079=VECTOR('',#28095,3.);
#8080=VECTOR('',#28098,3.);
#8081=VECTOR('',#28101,3.);
#8082=VECTOR('',#28104,3.);
#8083=VECTOR('',#28107,3.);
#8084=VECTOR('',#28110,3.);
#8085=VECTOR('',#28115,3.0735);
#8086=VECTOR('',#28120,3.0735);
#8087=VECTOR('',#28123,3.0735);
#8088=VECTOR('',#28126,3.0735);
#8089=VECTOR('',#28129,3.0735);
#8090=VECTOR('',#28132,3.0735);
#8091=VECTOR('',#28135,3.0735);
#8092=VECTOR('',#28138,3.0735);
#8093=VECTOR('',#28141,3.0735);
#8094=VECTOR('',#28144,3.0735);
#8095=VECTOR('',#28147,3.0735);
#8096=VECTOR('',#28150,3.0735);
#8097=VECTOR('',#28153,3.0735);
#8098=VECTOR('',#28156,3.0735);
#8099=VECTOR('',#28159,3.0735);
#8100=VECTOR('',#28164,2.);
#8101=VECTOR('',#28167,2.);
#8102=VECTOR('',#28170,2.);
#8103=VECTOR('',#28173,2.);
#8104=VECTOR('',#28176,2.);
#8105=VECTOR('',#28179,2.);
#8106=VECTOR('',#28182,2.);
#8107=VECTOR('',#28185,2.);
#8108=VECTOR('',#28188,2.);
#8109=VECTOR('',#28191,2.);
#8110=VECTOR('',#28194,2.);
#8111=VECTOR('',#28197,2.);
#8112=VECTOR('',#28266,5.5);
#8113=VECTOR('',#28273,5.5);
#8114=VECTOR('',#28280,5.5);
#8115=VECTOR('',#28287,5.5);
#8116=VECTOR('',#28294,18.);
#8117=VECTOR('',#28305,90.);
#8118=VECTOR('',#28306,90.);
#8119=VECTOR('',#28307,90.);
#8120=VECTOR('',#28308,90.);
#8121=VECTOR('',#28315,100.);
#8122=VECTOR('',#28316,100.);
#8123=VECTOR('',#28317,100.);
#8124=VECTOR('',#28318,100.);
#8125=VECTOR('',#28329,17.);
#8126=VECTOR('',#28334,130.);
#8127=VECTOR('',#28345,2.);
#8128=VECTOR('',#28352,2.);
#8129=VECTOR('',#28359,2.);
#8130=VECTOR('',#28366,2.);
#8131=VECTOR('',#28375,18.);
#8132=VECTOR('',#28382,90.);
#8133=VECTOR('',#28383,90.);
#8134=VECTOR('',#28396,3.5);
#8135=VECTOR('',#28403,3.5);
#8136=VECTOR('',#28410,3.5);
#8137=VECTOR('',#28417,3.5);
#8138=VECTOR('',#28424,3.5);
#8139=VECTOR('',#28431,3.5);
#8140=VECTOR('',#28438,3.5);
#8141=VECTOR('',#28445,3.5);
#8142=VECTOR('',#28452,18.);
#8143=VECTOR('',#28459,100.);
#8144=VECTOR('',#28470,10.);
#8145=VECTOR('',#28471,10.);
#8146=VECTOR('',#28472,10.);
#8147=VECTOR('',#28473,10.);
#8148=VECTOR('',#28478,10.);
#8149=VECTOR('',#28479,10.);
#8150=VECTOR('',#28482,10.);
#8151=VECTOR('',#28483,10.);
#8152=VECTOR('',#28484,10.);
#8153=VECTOR('',#28487,10.);
#8154=VECTOR('',#28496,7.);
#8155=VECTOR('',#28511,8.);
#8156=VECTOR('',#28516,15.);
#8157=VECTOR('',#28531,16.);
#8158=VECTOR('',#28546,11.);
#8159=VECTOR('',#28549,8.);
#8160=VECTOR('',#28564,20.);
#8161=VECTOR('',#28567,16.);
#8162=VECTOR('',#28572,8.);
#8163=VECTOR('',#28579,8.);
#8164=VECTOR('',#28588,16.);
#8165=VECTOR('',#28597,2.);
#8166=VECTOR('',#28604,2.);
#8167=VECTOR('',#28611,2.);
#8168=VECTOR('',#28618,2.);
#8169=VECTOR('',#28623,10.);
#8170=VECTOR('',#28630,10.);
#8171=VECTOR('',#28637,10.);
#8172=VECTOR('',#28644,10.);
#8173=VECTOR('',#28651,10.);
#8174=VECTOR('',#28658,10.);
#8175=VECTOR('',#28665,10.);
#8176=VECTOR('',#28672,10.);
#8177=VECTOR('',#28679,10.);
#8178=VECTOR('',#28686,10.);
#8179=VECTOR('',#28693,10.);
#8180=VECTOR('',#28700,10.);
#8181=VECTOR('',#28707,10.);
#8182=VECTOR('',#28714,10.);
#8183=VECTOR('',#28721,10.);
#8184=VECTOR('',#28728,10.);
#8185=VECTOR('',#28735,10.);
#8186=VECTOR('',#28742,10.);
#8187=VECTOR('',#28749,10.);
#8188=VECTOR('',#28756,10.);
#8189=VECTOR('',#28763,10.);
#8190=VECTOR('',#28770,10.);
#8191=VECTOR('',#28777,10.);
#8192=VECTOR('',#28784,10.);
#8193=VECTOR('',#28791,10.);
#8194=VECTOR('',#28798,10.);
#8195=VECTOR('',#28805,10.);
#8196=VECTOR('',#28812,10.);
#8197=VECTOR('',#28819,10.);
#8198=VECTOR('',#28826,10.);
#8199=VECTOR('',#28833,10.);
#8200=VECTOR('',#28840,10.);
#8201=VECTOR('',#28847,10.);
#8202=VECTOR('',#28854,10.);
#8203=VECTOR('',#28861,10.);
#8204=VECTOR('',#28868,10.);
#8205=VECTOR('',#28875,10.);
#8206=VECTOR('',#28882,10.);
#8207=VECTOR('',#28889,10.);
#8208=VECTOR('',#28896,10.);
#8209=VECTOR('',#28903,10.);
#8210=VECTOR('',#28910,10.);
#8211=VECTOR('',#28917,10.);
#8212=VECTOR('',#28924,10.);
#8213=VECTOR('',#28931,10.);
#8214=VECTOR('',#28938,10.);
#8215=VECTOR('',#28945,10.);
#8216=VECTOR('',#28952,10.);
#8217=VECTOR('',#28959,10.);
#8218=VECTOR('',#28966,10.);
#8219=VECTOR('',#28973,10.);
#8220=VECTOR('',#28980,10.);
#8221=VECTOR('',#28987,10.);
#8222=VECTOR('',#28994,10.);
#8223=VECTOR('',#29001,10.);
#8224=VECTOR('',#29008,10.);
#8225=VECTOR('',#29015,10.);
#8226=VECTOR('',#29022,10.);
#8227=VECTOR('',#29029,10.);
#8228=VECTOR('',#29036,10.);
#8229=VECTOR('',#29043,10.);
#8230=VECTOR('',#29050,10.);
#8231=VECTOR('',#29057,10.);
#8232=VECTOR('',#29064,10.);
#8233=VECTOR('',#29071,10.);
#8234=VECTOR('',#29078,10.);
#8235=VECTOR('',#29085,10.);
#8236=VECTOR('',#29092,10.);
#8237=VECTOR('',#29099,10.);
#8238=VECTOR('',#29106,10.);
#8239=VECTOR('',#29113,10.);
#8240=VECTOR('',#29120,10.);
#8241=VECTOR('',#29121,10.);
#8242=VECTOR('',#29122,10.);
#8243=VECTOR('',#29123,10.);
#8244=VECTOR('',#29124,10.);
#8245=VECTOR('',#29125,10.);
#8246=VECTOR('',#29126,10.);
#8247=VECTOR('',#29127,10.);
#8248=VECTOR('',#29128,10.);
#8249=VECTOR('',#29129,10.);
#8250=VECTOR('',#29130,10.);
#8251=VECTOR('',#29131,10.);
#8252=VECTOR('',#29132,10.);
#8253=VECTOR('',#29133,10.);
#8254=VECTOR('',#29134,10.);
#8255=VECTOR('',#29135,10.);
#8256=VECTOR('',#29136,10.);
#8257=VECTOR('',#29137,10.);
#8258=VECTOR('',#29138,10.);
#8259=VECTOR('',#29139,10.);
#8260=VECTOR('',#29140,10.);
#8261=VECTOR('',#29141,10.);
#8262=VECTOR('',#29142,10.);
#8263=VECTOR('',#29143,10.);
#8264=VECTOR('',#29144,10.);
#8265=VECTOR('',#29145,10.);
#8266=VECTOR('',#29146,10.);
#8267=VECTOR('',#29147,10.);
#8268=VECTOR('',#29148,10.);
#8269=VECTOR('',#29149,10.);
#8270=VECTOR('',#29150,10.);
#8271=VECTOR('',#29151,10.);
#8272=VECTOR('',#29152,10.);
#8273=VECTOR('',#29153,10.);
#8274=VECTOR('',#29154,10.);
#8275=VECTOR('',#29155,10.);
#8276=VECTOR('',#29156,10.);
#8277=VECTOR('',#29157,10.);
#8278=VECTOR('',#29158,10.);
#8279=VECTOR('',#29159,10.);
#8280=VECTOR('',#29160,10.);
#8281=VECTOR('',#29161,10.);
#8282=VECTOR('',#29162,10.);
#8283=VECTOR('',#29163,10.);
#8284=VECTOR('',#29164,10.);
#8285=VECTOR('',#29165,10.);
#8286=VECTOR('',#29166,10.);
#8287=VECTOR('',#29167,10.);
#8288=VECTOR('',#29168,10.);
#8289=VECTOR('',#29169,10.);
#8290=VECTOR('',#29170,10.);
#8291=VECTOR('',#29171,10.);
#8292=VECTOR('',#29172,10.);
#8293=VECTOR('',#29173,10.);
#8294=VECTOR('',#29174,10.);
#8295=VECTOR('',#29175,10.);
#8296=VECTOR('',#29176,10.);
#8297=VECTOR('',#29177,10.);
#8298=VECTOR('',#29178,10.);
#8299=VECTOR('',#29179,10.);
#8300=VECTOR('',#29180,10.);
#8301=VECTOR('',#29181,10.);
#8302=VECTOR('',#29182,10.);
#8303=VECTOR('',#29183,10.);
#8304=VECTOR('',#29184,10.);
#8305=VECTOR('',#29185,10.);
#8306=VECTOR('',#29186,10.);
#8307=VECTOR('',#29187,10.);
#8308=VECTOR('',#29188,10.);
#8309=VECTOR('',#29189,10.);
#8310=VECTOR('',#29190,10.);
#8311=VECTOR('',#29195,10.);
#8312=VECTOR('',#29616,10.);
#8313=VECTOR('',#29637,90.);
#8314=VECTOR('',#29638,90.);
#8315=VECTOR('',#29647,10.);
#8316=VECTOR('',#29648,10.);
#8317=VECTOR('',#29649,10.);
#8318=VECTOR('',#29650,10.);
#8319=VECTOR('',#29653,10.);
#8320=VECTOR('',#29654,10.);
#8321=VECTOR('',#29655,10.);
#8322=VECTOR('',#29656,10.);
#8323=VECTOR('',#29659,10.);
#8324=VECTOR('',#29660,10.);
#8325=VECTOR('',#29671,10.);
#8326=VECTOR('',#29678,10.);
#8327=VECTOR('',#29681,10.);
#8328=VECTOR('',#29688,10.);
#8329=VECTOR('',#29691,10.);
#8330=VECTOR('',#29698,10.);
#8331=VECTOR('',#29701,10.);
#8332=VECTOR('',#29708,10.);
#8333=VECTOR('',#29711,10.);
#8334=VECTOR('',#29718,10.);
#8335=VECTOR('',#29721,10.);
#8336=VECTOR('',#29728,10.);
#8337=VECTOR('',#29731,10.);
#8338=VECTOR('',#29738,10.);
#8339=VECTOR('',#29741,10.);
#8340=VECTOR('',#29748,10.);
#8341=VECTOR('',#29751,10.);
#8342=VECTOR('',#29758,10.);
#8343=VECTOR('',#29761,10.);
#8344=VECTOR('',#29768,10.);
#8345=VECTOR('',#29771,10.);
#8346=VECTOR('',#29778,10.);
#8347=VECTOR('',#29781,10.);
#8348=VECTOR('',#29788,10.);
#8349=VECTOR('',#29791,10.);
#8350=VECTOR('',#29798,10.);
#8351=VECTOR('',#29801,10.);
#8352=VECTOR('',#29808,10.);
#8353=VECTOR('',#29811,10.);
#8354=VECTOR('',#29818,10.);
#8355=VECTOR('',#29821,10.);
#8356=VECTOR('',#29828,10.);
#8357=VECTOR('',#29831,10.);
#8358=VECTOR('',#29838,10.);
#8359=VECTOR('',#29841,10.);
#8360=VECTOR('',#29848,10.);
#8361=VECTOR('',#29851,10.);
#8362=VECTOR('',#29858,10.);
#8363=VECTOR('',#29861,10.);
#8364=VECTOR('',#29868,10.);
#8365=VECTOR('',#29871,10.);
#8366=VECTOR('',#29878,10.);
#8367=VECTOR('',#29881,10.);
#8368=VECTOR('',#29888,10.);
#8369=VECTOR('',#29891,10.);
#8370=VECTOR('',#29898,10.);
#8371=VECTOR('',#29901,10.);
#8372=VECTOR('',#29908,10.);
#8373=VECTOR('',#29913,10.);
#8374=VECTOR('',#29914,10.);
#8375=VECTOR('',#29917,10.);
#8376=VECTOR('',#29918,10.);
#8377=VECTOR('',#29923,10.);
#8378=VECTOR('',#29924,10.);
#8379=VECTOR('',#29933,10.);
#8380=VECTOR('',#29934,10.);
#8381=VECTOR('',#29937,10.);
#8382=VECTOR('',#29938,10.);
#8383=VECTOR('',#29943,10.);
#8384=VECTOR('',#29944,10.);
#8385=VECTOR('',#29953,10.);
#8386=VECTOR('',#29954,10.);
#8387=VECTOR('',#29957,10.);
#8388=VECTOR('',#29958,10.);
#8389=VECTOR('',#29963,10.);
#8390=VECTOR('',#29964,10.);
#8391=VECTOR('',#29973,10.);
#8392=VECTOR('',#29974,10.);
#8393=VECTOR('',#29977,10.);
#8394=VECTOR('',#29978,10.);
#8395=VECTOR('',#29983,10.);
#8396=VECTOR('',#29984,10.);
#8397=VECTOR('',#29993,10.);
#8398=VECTOR('',#29994,10.);
#8399=VECTOR('',#29997,10.);
#8400=VECTOR('',#29998,10.);
#8401=VECTOR('',#30003,10.);
#8402=VECTOR('',#30004,10.);
#8403=VECTOR('',#30013,10.);
#8404=VECTOR('',#30014,10.);
#8405=VECTOR('',#30017,10.);
#8406=VECTOR('',#30018,10.);
#8407=VECTOR('',#30023,10.);
#8408=VECTOR('',#30024,10.);
#8409=VECTOR('',#30033,10.);
#8410=VECTOR('',#30034,10.);
#8411=VECTOR('',#30037,10.);
#8412=VECTOR('',#30038,10.);
#8413=VECTOR('',#30043,10.);
#8414=VECTOR('',#30044,10.);
#8415=VECTOR('',#30053,10.);
#8416=VECTOR('',#30054,10.);
#8417=VECTOR('',#30057,10.);
#8418=VECTOR('',#30058,10.);
#8419=VECTOR('',#30063,10.);
#8420=VECTOR('',#30064,10.);
#8421=VECTOR('',#30073,10.);
#8422=VECTOR('',#30074,10.);
#8423=VECTOR('',#30077,10.);
#8424=VECTOR('',#30078,10.);
#8425=VECTOR('',#30083,10.);
#8426=VECTOR('',#30084,10.);
#8427=VECTOR('',#30093,10.);
#8428=VECTOR('',#30094,10.);
#8429=VECTOR('',#30097,10.);
#8430=VECTOR('',#30098,10.);
#8431=VECTOR('',#30103,10.);
#8432=VECTOR('',#30104,10.);
#8433=VECTOR('',#30113,10.);
#8434=VECTOR('',#30114,10.);
#8435=VECTOR('',#30117,10.);
#8436=VECTOR('',#30118,10.);
#8437=VECTOR('',#30123,10.);
#8438=VECTOR('',#30124,10.);
#8439=VECTOR('',#30133,10.);
#8440=VECTOR('',#30134,10.);
#8441=VECTOR('',#30137,10.);
#8442=VECTOR('',#30138,10.);
#8443=VECTOR('',#30143,10.);
#8444=VECTOR('',#30144,10.);
#8445=VECTOR('',#30153,10.);
#8446=VECTOR('',#30154,10.);
#8447=VECTOR('',#30157,10.);
#8448=VECTOR('',#30158,10.);
#8449=VECTOR('',#30163,10.);
#8450=VECTOR('',#30164,10.);
#8451=VECTOR('',#30173,10.);
#8452=VECTOR('',#30174,10.);
#8453=VECTOR('',#30177,10.);
#8454=VECTOR('',#30178,10.);
#8455=VECTOR('',#30183,10.);
#8456=VECTOR('',#30184,10.);
#8457=VECTOR('',#30193,10.);
#8458=VECTOR('',#30194,10.);
#8459=VECTOR('',#30197,10.);
#8460=VECTOR('',#30198,10.);
#8461=VECTOR('',#30203,10.);
#8462=VECTOR('',#30204,10.);
#8463=VECTOR('',#30213,10.);
#8464=VECTOR('',#30214,10.);
#8465=VECTOR('',#30217,10.);
#8466=VECTOR('',#30218,10.);
#8467=VECTOR('',#30223,10.);
#8468=VECTOR('',#30224,10.);
#8469=VECTOR('',#30233,10.);
#8470=VECTOR('',#30234,10.);
#8471=VECTOR('',#30237,10.);
#8472=VECTOR('',#30238,10.);
#8473=VECTOR('',#30243,10.);
#8474=VECTOR('',#30244,10.);
#8475=VECTOR('',#30253,10.);
#8476=VECTOR('',#30254,10.);
#8477=VECTOR('',#30257,10.);
#8478=VECTOR('',#30258,10.);
#8479=VECTOR('',#30263,10.);
#8480=VECTOR('',#30264,10.);
#8481=VECTOR('',#30273,10.);
#8482=VECTOR('',#30274,10.);
#8483=VECTOR('',#30277,10.);
#8484=VECTOR('',#30278,10.);
#8485=VECTOR('',#30283,10.);
#8486=VECTOR('',#30284,10.);
#8487=VECTOR('',#30293,10.);
#8488=VECTOR('',#30294,10.);
#8489=VECTOR('',#30297,10.);
#8490=VECTOR('',#30298,10.);
#8491=VECTOR('',#30303,10.);
#8492=VECTOR('',#30304,10.);
#8493=VECTOR('',#30313,10.);
#8494=VECTOR('',#30314,10.);
#8495=VECTOR('',#30317,10.);
#8496=VECTOR('',#30318,10.);
#8497=VECTOR('',#30323,10.);
#8498=VECTOR('',#30324,10.);
#8499=VECTOR('',#30333,10.);
#8500=VECTOR('',#30334,10.);
#8501=VECTOR('',#30337,10.);
#8502=VECTOR('',#30338,10.);
#8503=VECTOR('',#30343,10.);
#8504=VECTOR('',#30344,10.);
#8505=VECTOR('',#30353,10.);
#8506=VECTOR('',#30354,10.);
#8507=VECTOR('',#30357,10.);
#8508=VECTOR('',#30358,10.);
#8509=VECTOR('',#30363,10.);
#8510=VECTOR('',#30364,10.);
#8511=VECTOR('',#30371,10.);
#8512=VECTOR('',#30372,10.);
#8513=VECTOR('',#30373,10.);
#8514=VECTOR('',#30374,10.);
#8515=VECTOR('',#30377,10.);
#8516=VECTOR('',#30378,10.);
#8517=VECTOR('',#30379,10.);
#8518=VECTOR('',#30380,10.);
#8519=VECTOR('',#30383,10.);
#8520=VECTOR('',#30384,10.);
#8521=VECTOR('',#30385,10.);
#8522=VECTOR('',#30386,10.);
#8523=VECTOR('',#30389,10.);
#8524=VECTOR('',#30390,10.);
#8525=VECTOR('',#30391,10.);
#8526=VECTOR('',#30392,10.);
#8527=VECTOR('',#30395,10.);
#8528=VECTOR('',#30396,10.);
#8529=VECTOR('',#30397,10.);
#8530=VECTOR('',#30398,10.);
#8531=VECTOR('',#30401,10.);
#8532=VECTOR('',#30402,10.);
#8533=VECTOR('',#30403,10.);
#8534=VECTOR('',#30404,10.);
#8535=VECTOR('',#30407,10.);
#8536=VECTOR('',#30408,10.);
#8537=VECTOR('',#30409,10.);
#8538=VECTOR('',#30410,10.);
#8539=VECTOR('',#30413,10.);
#8540=VECTOR('',#30414,10.);
#8541=VECTOR('',#30415,10.);
#8542=VECTOR('',#30416,10.);
#8543=VECTOR('',#30419,10.);
#8544=VECTOR('',#30420,10.);
#8545=VECTOR('',#30421,10.);
#8546=VECTOR('',#30422,10.);
#8547=VECTOR('',#30425,10.);
#8548=VECTOR('',#30426,10.);
#8549=VECTOR('',#30427,10.);
#8550=VECTOR('',#30428,10.);
#8551=VECTOR('',#30431,10.);
#8552=VECTOR('',#30432,10.);
#8553=VECTOR('',#30433,10.);
#8554=VECTOR('',#30434,10.);
#8555=VECTOR('',#30437,10.);
#8556=VECTOR('',#30438,10.);
#8557=VECTOR('',#30439,10.);
#8558=VECTOR('',#30440,10.);
#8559=VECTOR('',#30443,10.);
#8560=VECTOR('',#30444,10.);
#8561=VECTOR('',#30445,10.);
#8562=VECTOR('',#30446,10.);
#8563=VECTOR('',#30449,10.);
#8564=VECTOR('',#30450,10.);
#8565=VECTOR('',#30451,10.);
#8566=VECTOR('',#30452,10.);
#8567=VECTOR('',#30455,10.);
#8568=VECTOR('',#30456,10.);
#8569=VECTOR('',#30457,10.);
#8570=VECTOR('',#30458,10.);
#8571=VECTOR('',#30461,10.);
#8572=VECTOR('',#30462,10.);
#8573=VECTOR('',#30463,10.);
#8574=VECTOR('',#30464,10.);
#8575=VECTOR('',#30467,10.);
#8576=VECTOR('',#30468,10.);
#8577=VECTOR('',#30469,10.);
#8578=VECTOR('',#30470,10.);
#8579=VECTOR('',#30473,10.);
#8580=VECTOR('',#30474,10.);
#8581=VECTOR('',#30475,10.);
#8582=VECTOR('',#30476,10.);
#8583=VECTOR('',#30479,10.);
#8584=VECTOR('',#30480,10.);
#8585=VECTOR('',#30481,10.);
#8586=VECTOR('',#30482,10.);
#8587=VECTOR('',#30485,10.);
#8588=VECTOR('',#30486,10.);
#8589=VECTOR('',#30487,10.);
#8590=VECTOR('',#30488,10.);
#8591=VECTOR('',#30491,10.);
#8592=VECTOR('',#30492,10.);
#8593=VECTOR('',#30493,10.);
#8594=VECTOR('',#30494,10.);
#8595=VECTOR('',#30497,10.);
#8596=VECTOR('',#30498,10.);
#8597=VECTOR('',#30499,10.);
#8598=VECTOR('',#30500,10.);
#8599=VECTOR('',#30503,10.);
#8600=VECTOR('',#30504,10.);
#8601=VECTOR('',#30505,10.);
#8602=VECTOR('',#30506,10.);
#8603=VECTOR('',#30555,10.);
#8604=VECTOR('',#30562,10.);
#8605=VECTOR('',#30567,10.);
#8606=VECTOR('',#30614,10.);
#8607=VECTOR('',#30615,10.);
#8608=VECTOR('',#30618,10.);
#8609=VECTOR('',#30621,10.);
#8610=VECTOR('',#30622,10.);
#8611=VECTOR('',#30627,10.);
#8612=VECTOR('',#30628,10.);
#8613=VECTOR('',#30637,10.);
#8614=VECTOR('',#30640,10.);
#8615=VECTOR('',#30643,10.);
#8616=VECTOR('',#30644,10.);
#8617=VECTOR('',#30645,10.);
#8618=VECTOR('',#30650,10.);
#8619=VECTOR('',#30653,10.);
#8620=VECTOR('',#30664,10.);
#8621=VECTOR('',#30667,10.);
#8622=VECTOR('',#30670,10.);
#8623=VECTOR('',#30671,10.);
#8624=VECTOR('',#30672,10.);
#8625=VECTOR('',#30677,10.);
#8626=VECTOR('',#30680,10.);
#8627=VECTOR('',#30691,10.);
#8628=VECTOR('',#30694,10.);
#8629=VECTOR('',#30697,10.);
#8630=VECTOR('',#30698,10.);
#8631=VECTOR('',#30699,10.);
#8632=VECTOR('',#30704,10.);
#8633=VECTOR('',#30707,10.);
#8634=VECTOR('',#30718,10.);
#8635=VECTOR('',#30721,10.);
#8636=VECTOR('',#30724,10.);
#8637=VECTOR('',#30725,10.);
#8638=VECTOR('',#30726,10.);
#8639=VECTOR('',#30731,10.);
#8640=VECTOR('',#30734,10.);
#8641=VECTOR('',#30745,10.);
#8642=VECTOR('',#30748,10.);
#8643=VECTOR('',#30751,10.);
#8644=VECTOR('',#30752,10.);
#8645=VECTOR('',#30753,10.);
#8646=VECTOR('',#30758,10.);
#8647=VECTOR('',#30761,10.);
#8648=VECTOR('',#30772,10.);
#8649=VECTOR('',#30775,10.);
#8650=VECTOR('',#30778,10.);
#8651=VECTOR('',#30779,10.);
#8652=VECTOR('',#30780,10.);
#8653=VECTOR('',#30785,10.);
#8654=VECTOR('',#30788,10.);
#8655=VECTOR('',#30799,10.);
#8656=VECTOR('',#30802,10.);
#8657=VECTOR('',#30805,10.);
#8658=VECTOR('',#30806,10.);
#8659=VECTOR('',#30807,10.);
#8660=VECTOR('',#30812,10.);
#8661=VECTOR('',#30815,10.);
#8662=VECTOR('',#30826,10.);
#8663=VECTOR('',#30829,10.);
#8664=VECTOR('',#30832,10.);
#8665=VECTOR('',#30833,10.);
#8666=VECTOR('',#30834,10.);
#8667=VECTOR('',#30839,10.);
#8668=VECTOR('',#30842,10.);
#8669=VECTOR('',#30853,10.);
#8670=VECTOR('',#30856,10.);
#8671=VECTOR('',#30859,10.);
#8672=VECTOR('',#30860,10.);
#8673=VECTOR('',#30861,10.);
#8674=VECTOR('',#30866,10.);
#8675=VECTOR('',#30869,10.);
#8676=VECTOR('',#30880,10.);
#8677=VECTOR('',#30883,10.);
#8678=VECTOR('',#30886,10.);
#8679=VECTOR('',#30887,10.);
#8680=VECTOR('',#30888,10.);
#8681=VECTOR('',#30893,10.);
#8682=VECTOR('',#30896,10.);
#8683=VECTOR('',#30907,10.);
#8684=VECTOR('',#30910,10.);
#8685=VECTOR('',#30913,10.);
#8686=VECTOR('',#30914,10.);
#8687=VECTOR('',#30915,10.);
#8688=VECTOR('',#30920,10.);
#8689=VECTOR('',#30923,10.);
#8690=VECTOR('',#30934,10.);
#8691=VECTOR('',#30937,10.);
#8692=VECTOR('',#30940,10.);
#8693=VECTOR('',#30941,10.);
#8694=VECTOR('',#30942,10.);
#8695=VECTOR('',#30947,10.);
#8696=VECTOR('',#30950,10.);
#8697=VECTOR('',#30961,10.);
#8698=VECTOR('',#30964,10.);
#8699=VECTOR('',#30967,10.);
#8700=VECTOR('',#30968,10.);
#8701=VECTOR('',#30969,10.);
#8702=VECTOR('',#30974,10.);
#8703=VECTOR('',#30977,10.);
#8704=VECTOR('',#30988,10.);
#8705=VECTOR('',#30991,10.);
#8706=VECTOR('',#30994,10.);
#8707=VECTOR('',#30995,10.);
#8708=VECTOR('',#30996,10.);
#8709=VECTOR('',#31001,10.);
#8710=VECTOR('',#31004,10.);
#8711=VECTOR('',#31015,10.);
#8712=VECTOR('',#31018,10.);
#8713=VECTOR('',#31021,10.);
#8714=VECTOR('',#31022,10.);
#8715=VECTOR('',#31023,10.);
#8716=VECTOR('',#31028,10.);
#8717=VECTOR('',#31031,10.);
#8718=VECTOR('',#31042,10.);
#8719=VECTOR('',#31045,10.);
#8720=VECTOR('',#31048,10.);
#8721=VECTOR('',#31049,10.);
#8722=VECTOR('',#31050,10.);
#8723=VECTOR('',#31055,10.);
#8724=VECTOR('',#31058,10.);
#8725=VECTOR('',#31069,10.);
#8726=VECTOR('',#31072,10.);
#8727=VECTOR('',#31075,10.);
#8728=VECTOR('',#31076,10.);
#8729=VECTOR('',#31077,10.);
#8730=VECTOR('',#31082,10.);
#8731=VECTOR('',#31085,10.);
#8732=VECTOR('',#31096,10.);
#8733=VECTOR('',#31099,10.);
#8734=VECTOR('',#31102,10.);
#8735=VECTOR('',#31103,10.);
#8736=VECTOR('',#31104,10.);
#8737=VECTOR('',#31109,10.);
#8738=VECTOR('',#31112,10.);
#8739=VECTOR('',#31123,10.);
#8740=VECTOR('',#31126,10.);
#8741=VECTOR('',#31129,10.);
#8742=VECTOR('',#31130,10.);
#8743=VECTOR('',#31131,10.);
#8744=VECTOR('',#31136,10.);
#8745=VECTOR('',#31139,10.);
#8746=VECTOR('',#31150,10.);
#8747=VECTOR('',#31153,10.);
#8748=VECTOR('',#31156,10.);
#8749=VECTOR('',#31157,10.);
#8750=VECTOR('',#31158,10.);
#8751=VECTOR('',#31163,10.);
#8752=VECTOR('',#31166,10.);
#8753=VECTOR('',#31177,10.);
#8754=VECTOR('',#31180,10.);
#8755=VECTOR('',#31183,10.);
#8756=VECTOR('',#31184,10.);
#8757=VECTOR('',#31185,10.);
#8758=VECTOR('',#31190,10.);
#8759=VECTOR('',#31193,10.);
#8760=VECTOR('',#31204,10.);
#8761=VECTOR('',#31207,10.);
#8762=VECTOR('',#31210,10.);
#8763=VECTOR('',#31211,10.);
#8764=VECTOR('',#31212,10.);
#8765=VECTOR('',#31217,10.);
#8766=VECTOR('',#31220,10.);
#8767=VECTOR('',#31231,10.);
#8768=VECTOR('',#31234,10.);
#8769=VECTOR('',#31237,10.);
#8770=VECTOR('',#31238,10.);
#8771=VECTOR('',#31239,10.);
#8772=VECTOR('',#31244,10.);
#8773=VECTOR('',#31247,10.);
#8774=VECTOR('',#31256,10.);
#8775=VECTOR('',#31257,10.);
#8776=VECTOR('',#31258,10.);
#8777=VECTOR('',#31259,10.);
#8778=VECTOR('',#31260,10.);
#8779=VECTOR('',#31263,10.);
#8780=VECTOR('',#31264,10.);
#8781=VECTOR('',#31265,10.);
#8782=VECTOR('',#31266,10.);
#8783=VECTOR('',#31267,10.);
#8784=VECTOR('',#31270,10.);
#8785=VECTOR('',#31271,10.);
#8786=VECTOR('',#31272,10.);
#8787=VECTOR('',#31273,10.);
#8788=VECTOR('',#31274,10.);
#8789=VECTOR('',#31277,10.);
#8790=VECTOR('',#31278,10.);
#8791=VECTOR('',#31279,10.);
#8792=VECTOR('',#31280,10.);
#8793=VECTOR('',#31281,10.);
#8794=VECTOR('',#31284,10.);
#8795=VECTOR('',#31285,10.);
#8796=VECTOR('',#31286,10.);
#8797=VECTOR('',#31287,10.);
#8798=VECTOR('',#31288,10.);
#8799=VECTOR('',#31291,10.);
#8800=VECTOR('',#31292,10.);
#8801=VECTOR('',#31293,10.);
#8802=VECTOR('',#31294,10.);
#8803=VECTOR('',#31295,10.);
#8804=VECTOR('',#31298,10.);
#8805=VECTOR('',#31299,10.);
#8806=VECTOR('',#31300,10.);
#8807=VECTOR('',#31301,10.);
#8808=VECTOR('',#31302,10.);
#8809=VECTOR('',#31305,10.);
#8810=VECTOR('',#31306,10.);
#8811=VECTOR('',#31307,10.);
#8812=VECTOR('',#31308,10.);
#8813=VECTOR('',#31309,10.);
#8814=VECTOR('',#31312,10.);
#8815=VECTOR('',#31313,10.);
#8816=VECTOR('',#31314,10.);
#8817=VECTOR('',#31315,10.);
#8818=VECTOR('',#31316,10.);
#8819=VECTOR('',#31319,10.);
#8820=VECTOR('',#31320,10.);
#8821=VECTOR('',#31321,10.);
#8822=VECTOR('',#31322,10.);
#8823=VECTOR('',#31323,10.);
#8824=VECTOR('',#31326,10.);
#8825=VECTOR('',#31327,10.);
#8826=VECTOR('',#31328,10.);
#8827=VECTOR('',#31329,10.);
#8828=VECTOR('',#31330,10.);
#8829=VECTOR('',#31333,10.);
#8830=VECTOR('',#31334,10.);
#8831=VECTOR('',#31335,10.);
#8832=VECTOR('',#31336,10.);
#8833=VECTOR('',#31337,10.);
#8834=VECTOR('',#31340,10.);
#8835=VECTOR('',#31341,10.);
#8836=VECTOR('',#31342,10.);
#8837=VECTOR('',#31343,10.);
#8838=VECTOR('',#31344,10.);
#8839=VECTOR('',#31347,10.);
#8840=VECTOR('',#31348,10.);
#8841=VECTOR('',#31349,10.);
#8842=VECTOR('',#31350,10.);
#8843=VECTOR('',#31351,10.);
#8844=VECTOR('',#31354,10.);
#8845=VECTOR('',#31355,10.);
#8846=VECTOR('',#31356,10.);
#8847=VECTOR('',#31357,10.);
#8848=VECTOR('',#31358,10.);
#8849=VECTOR('',#31361,10.);
#8850=VECTOR('',#31362,10.);
#8851=VECTOR('',#31363,10.);
#8852=VECTOR('',#31364,10.);
#8853=VECTOR('',#31365,10.);
#8854=VECTOR('',#31368,10.);
#8855=VECTOR('',#31369,10.);
#8856=VECTOR('',#31370,10.);
#8857=VECTOR('',#31371,10.);
#8858=VECTOR('',#31372,10.);
#8859=VECTOR('',#31375,10.);
#8860=VECTOR('',#31376,10.);
#8861=VECTOR('',#31377,10.);
#8862=VECTOR('',#31378,10.);
#8863=VECTOR('',#31379,10.);
#8864=VECTOR('',#31382,10.);
#8865=VECTOR('',#31383,10.);
#8866=VECTOR('',#31384,10.);
#8867=VECTOR('',#31385,10.);
#8868=VECTOR('',#31386,10.);
#8869=VECTOR('',#31389,10.);
#8870=VECTOR('',#31390,10.);
#8871=VECTOR('',#31391,10.);
#8872=VECTOR('',#31392,10.);
#8873=VECTOR('',#31393,10.);
#8874=VECTOR('',#31396,10.);
#8875=VECTOR('',#31397,10.);
#8876=VECTOR('',#31398,10.);
#8877=VECTOR('',#31399,10.);
#8878=VECTOR('',#31400,10.);
#8879=VECTOR('',#31403,10.);
#8880=VECTOR('',#31404,10.);
#8881=VECTOR('',#31405,10.);
#8882=VECTOR('',#31406,10.);
#8883=VECTOR('',#31407,10.);
#8884=VECTOR('',#31410,10.);
#8885=VECTOR('',#31411,10.);
#8886=VECTOR('',#31412,10.);
#8887=VECTOR('',#31413,10.);
#8888=VECTOR('',#31414,10.);
#8889=VECTOR('',#31463,10.);
#8890=VECTOR('',#31470,10.);
#8891=VECTOR('',#31479,10.);
#8892=VECTOR('',#31486,10.);
#8893=VECTOR('',#31537,10.);
#8894=VECTOR('',#31584,10.);
#8895=VECTOR('',#31585,10.);
#8896=VECTOR('',#31588,10.);
#8897=VECTOR('',#31591,10.);
#8898=VECTOR('',#31592,10.);
#8899=VECTOR('',#31597,10.);
#8900=VECTOR('',#31598,10.);
#8901=VECTOR('',#31601,7.);
#8902=VECTOR('',#31610,16.);
#8903=VECTOR('',#31617,18.);
#8904=VECTOR('',#31628,10.);
#8905=VECTOR('',#31629,10.);
#8906=VECTOR('',#31630,10.);
#8907=VECTOR('',#31631,10.);
#8908=VECTOR('',#31636,10.);
#8909=VECTOR('',#31637,10.);
#8910=VECTOR('',#31640,10.);
#8911=VECTOR('',#31641,10.);
#8912=VECTOR('',#31642,10.);
#8913=VECTOR('',#31645,10.);
#8914=VECTOR('',#31654,7.);
#8915=VECTOR('',#31669,8.);
#8916=VECTOR('',#31674,15.);
#8917=VECTOR('',#31689,16.);
#8918=VECTOR('',#31694,5.);
#8919=VECTOR('',#31701,5.);
#8920=VECTOR('',#31708,5.);
#8921=VECTOR('',#31725,11.);
#8922=VECTOR('',#31728,8.);
#8923=VECTOR('',#31733,8.);
#8924=VECTOR('',#31750,20.);
#8925=VECTOR('',#31753,16.);
#8926=VECTOR('',#31762,16.);
#8927=VECTOR('',#31767,12.);
#8928=VECTOR('',#31774,70.);
#8929=VECTOR('',#31785,10.);
#8930=VECTOR('',#31786,10.);
#8931=VECTOR('',#31787,10.);
#8932=VECTOR('',#31788,10.);
#8933=VECTOR('',#31791,10.);
#8934=VECTOR('',#31792,10.);
#8935=VECTOR('',#31793,10.);
#8936=VECTOR('',#31796,10.);
#8937=VECTOR('',#31797,10.);
#8938=VECTOR('',#31798,10.);
#8939=VECTOR('',#31801,10.);
#8940=VECTOR('',#31802,10.);
#8941=VECTOR('',#31813,5.);
#8942=VECTOR('',#31820,7.);
#8943=VECTOR('',#31833,4.);
#8944=VECTOR('',#31848,5.);
#8945=VECTOR('',#31857,8.);
#8946=VECTOR('',#31864,5.);
#8947=VECTOR('',#31871,10.);
#8948=VECTOR('',#31872,10.);
#8949=VECTOR('',#31873,10.);
#8950=VECTOR('',#31874,10.);
#8951=VECTOR('',#31877,10.);
#8952=VECTOR('',#31878,10.);
#8953=VECTOR('',#31879,10.);
#8954=VECTOR('',#31880,10.);
#8955=VECTOR('',#31903,5.);
#8956=VECTOR('',#31910,10.);
#8957=VECTOR('',#31923,8.);
#8958=VECTOR('',#31930,11.);
#8959=VECTOR('',#31943,16.);
#8960=VECTOR('',#31950,20.);
#8961=VECTOR('',#31961,10.);
#8962=VECTOR('',#31962,10.);
#8963=VECTOR('',#31963,10.);
#8964=VECTOR('',#31964,10.);
#8965=VECTOR('',#31967,10.);
#8966=VECTOR('',#31968,10.);
#8967=VECTOR('',#31969,10.);
#8968=VECTOR('',#31970,10.);
#8969=VECTOR('',#31991,10.);
#8970=VECTOR('',#31992,10.);
#8971=VECTOR('',#31993,10.);
#8972=VECTOR('',#31994,10.);
#8973=VECTOR('',#31997,10.);
#8974=VECTOR('',#31998,10.);
#8975=VECTOR('',#31999,10.);
#8976=VECTOR('',#32000,10.);
#8977=VECTOR('',#32023,2.);
#8978=VECTOR('',#32034,3.);
#8979=VECTOR('',#32039,3.);
#8980=VECTOR('',#32042,3.);
#8981=VECTOR('',#32045,3.);
#8982=VECTOR('',#32048,3.);
#8983=VECTOR('',#32051,3.);
#8984=VECTOR('',#32054,3.);
#8985=VECTOR('',#32057,3.);
#8986=VECTOR('',#32060,3.);
#8987=VECTOR('',#32063,3.);
#8988=VECTOR('',#32066,3.);
#8989=VECTOR('',#32069,3.);
#8990=VECTOR('',#32072,3.);
#8991=VECTOR('',#32075,3.);
#8992=VECTOR('',#32078,3.);
#8993=VECTOR('',#32081,3.);
#8994=VECTOR('',#32084,3.);
#8995=VECTOR('',#32087,3.);
#8996=VECTOR('',#32090,3.);
#8997=VECTOR('',#32093,3.);
#8998=VECTOR('',#32096,2.37175);
#8999=VECTOR('',#32101,2.37175);
#9000=VECTOR('',#32104,2.37175);
#9001=VECTOR('',#32107,2.37175);
#9002=VECTOR('',#32110,2.37175);
#9003=VECTOR('',#32113,2.37175);
#9004=VECTOR('',#32116,2.37175);
#9005=VECTOR('',#32119,2.37175);
#9006=VECTOR('',#32122,2.37175);
#9007=VECTOR('',#32125,2.37175);
#9008=VECTOR('',#32128,2.37175);
#9009=VECTOR('',#32131,2.37175);
#9010=VECTOR('',#32134,2.37175);
#9011=VECTOR('',#32137,2.37175);
#9012=VECTOR('',#32140,2.37175);
#9013=VECTOR('',#32143,2.37175);
#9014=VECTOR('',#32146,2.37175);
#9015=VECTOR('',#32149,2.37175);
#9016=VECTOR('',#32152,2.37175);
#9017=VECTOR('',#32155,2.37175);
#9018=VECTOR('',#32166,10.);
#9019=VECTOR('',#32167,10.);
#9020=VECTOR('',#32168,10.);
#9021=VECTOR('',#32169,10.);
#9022=VECTOR('',#32172,10.);
#9023=VECTOR('',#32173,10.);
#9024=VECTOR('',#32174,10.);
#9025=VECTOR('',#32177,10.);
#9026=VECTOR('',#32178,10.);
#9027=VECTOR('',#32179,10.);
#9028=VECTOR('',#32182,10.);
#9029=VECTOR('',#32183,10.);
#9030=VECTOR('',#32184,10.);
#9031=VECTOR('',#32187,10.);
#9032=VECTOR('',#32188,10.);
#9033=VECTOR('',#32189,10.);
#9034=VECTOR('',#32192,10.);
#9035=VECTOR('',#32193,10.);
#9036=VECTOR('',#32202,5.);
#9037=VERTEX_POINT('',#32408);
#9038=VERTEX_POINT('',#32409);
#9039=VERTEX_POINT('',#32411);
#9040=VERTEX_POINT('',#32416);
#9041=VERTEX_POINT('',#32418);
#9042=VERTEX_POINT('',#32421);
#9043=VERTEX_POINT('',#32434);
#9044=VERTEX_POINT('',#32435);
#9045=VERTEX_POINT('',#32485);
#9046=VERTEX_POINT('',#32486);
#9047=VERTEX_POINT('',#32536);
#9048=VERTEX_POINT('',#32537);
#9049=VERTEX_POINT('',#32584);
#9050=VERTEX_POINT('',#32585);
#9051=VERTEX_POINT('',#32635);
#9052=VERTEX_POINT('',#32636);
#9053=VERTEX_POINT('',#32686);
#9054=VERTEX_POINT('',#32687);
#9055=VERTEX_POINT('',#32734);
#9056=VERTEX_POINT('',#32735);
#9057=VERTEX_POINT('',#32785);
#9058=VERTEX_POINT('',#32786);
#9059=VERTEX_POINT('',#32836);
#9060=VERTEX_POINT('',#32837);
#9061=VERTEX_POINT('',#32884);
#9062=VERTEX_POINT('',#32885);
#9063=VERTEX_POINT('',#32935);
#9064=VERTEX_POINT('',#32936);
#9065=VERTEX_POINT('',#32986);
#9066=VERTEX_POINT('',#32987);
#9067=VERTEX_POINT('',#33034);
#9068=VERTEX_POINT('',#33035);
#9069=VERTEX_POINT('',#33085);
#9070=VERTEX_POINT('',#33086);
#9071=VERTEX_POINT('',#33088);
#9072=VERTEX_POINT('',#33102);
#9073=VERTEX_POINT('',#33124);
#9074=VERTEX_POINT('',#33125);
#9075=VERTEX_POINT('',#33127);
#9076=VERTEX_POINT('',#33136);
#9077=VERTEX_POINT('',#33148);
#9078=VERTEX_POINT('',#33149);
#9079=VERTEX_POINT('',#33172);
#9080=VERTEX_POINT('',#33173);
#9081=VERTEX_POINT('',#33197);
#9082=VERTEX_POINT('',#33198);
#9083=VERTEX_POINT('',#33222);
#9084=VERTEX_POINT('',#33223);
#9085=VERTEX_POINT('',#33246);
#9086=VERTEX_POINT('',#33247);
#9087=VERTEX_POINT('',#33271);
#9088=VERTEX_POINT('',#33272);
#9089=VERTEX_POINT('',#33296);
#9090=VERTEX_POINT('',#33297);
#9091=VERTEX_POINT('',#33320);
#9092=VERTEX_POINT('',#33321);
#9093=VERTEX_POINT('',#33345);
#9094=VERTEX_POINT('',#33346);
#9095=VERTEX_POINT('',#33370);
#9096=VERTEX_POINT('',#33371);
#9097=VERTEX_POINT('',#33394);
#9098=VERTEX_POINT('',#33395);
#9099=VERTEX_POINT('',#33419);
#9100=VERTEX_POINT('',#33420);
#9101=VERTEX_POINT('',#33444);
#9102=VERTEX_POINT('',#33445);
#9103=VERTEX_POINT('',#33468);
#9104=VERTEX_POINT('',#33469);
#9105=VERTEX_POINT('',#33471);
#9106=VERTEX_POINT('',#33477);
#9107=VERTEX_POINT('',#33485);
#9108=VERTEX_POINT('',#33486);
#9109=VERTEX_POINT('',#33488);
#9110=VERTEX_POINT('',#33493);
#9111=VERTEX_POINT('',#33495);
#9112=VERTEX_POINT('',#33498);
#9113=VERTEX_POINT('',#33511);
#9114=VERTEX_POINT('',#33512);
#9115=VERTEX_POINT('',#33562);
#9116=VERTEX_POINT('',#33563);
#9117=VERTEX_POINT('',#33613);
#9118=VERTEX_POINT('',#33614);
#9119=VERTEX_POINT('',#33661);
#9120=VERTEX_POINT('',#33662);
#9121=VERTEX_POINT('',#33712);
#9122=VERTEX_POINT('',#33713);
#9123=VERTEX_POINT('',#33763);
#9124=VERTEX_POINT('',#33764);
#9125=VERTEX_POINT('',#33811);
#9126=VERTEX_POINT('',#33812);
#9127=VERTEX_POINT('',#33862);
#9128=VERTEX_POINT('',#33863);
#9129=VERTEX_POINT('',#33913);
#9130=VERTEX_POINT('',#33914);
#9131=VERTEX_POINT('',#33961);
#9132=VERTEX_POINT('',#33962);
#9133=VERTEX_POINT('',#34012);
#9134=VERTEX_POINT('',#34013);
#9135=VERTEX_POINT('',#34063);
#9136=VERTEX_POINT('',#34064);
#9137=VERTEX_POINT('',#34111);
#9138=VERTEX_POINT('',#34112);
#9139=VERTEX_POINT('',#34162);
#9140=VERTEX_POINT('',#34163);
#9141=VERTEX_POINT('',#34165);
#9142=VERTEX_POINT('',#34179);
#9143=VERTEX_POINT('',#34201);
#9144=VERTEX_POINT('',#34202);
#9145=VERTEX_POINT('',#34204);
#9146=VERTEX_POINT('',#34213);
#9147=VERTEX_POINT('',#34225);
#9148=VERTEX_POINT('',#34226);
#9149=VERTEX_POINT('',#34249);
#9150=VERTEX_POINT('',#34250);
#9151=VERTEX_POINT('',#34274);
#9152=VERTEX_POINT('',#34275);
#9153=VERTEX_POINT('',#34299);
#9154=VERTEX_POINT('',#34300);
#9155=VERTEX_POINT('',#34323);
#9156=VERTEX_POINT('',#34324);
#9157=VERTEX_POINT('',#34348);
#9158=VERTEX_POINT('',#34349);
#9159=VERTEX_POINT('',#34373);
#9160=VERTEX_POINT('',#34374);
#9161=VERTEX_POINT('',#34397);
#9162=VERTEX_POINT('',#34398);
#9163=VERTEX_POINT('',#34422);
#9164=VERTEX_POINT('',#34423);
#9165=VERTEX_POINT('',#34447);
#9166=VERTEX_POINT('',#34448);
#9167=VERTEX_POINT('',#34471);
#9168=VERTEX_POINT('',#34472);
#9169=VERTEX_POINT('',#34496);
#9170=VERTEX_POINT('',#34497);
#9171=VERTEX_POINT('',#34521);
#9172=VERTEX_POINT('',#34522);
#9173=VERTEX_POINT('',#34545);
#9174=VERTEX_POINT('',#34546);
#9175=VERTEX_POINT('',#34548);
#9176=VERTEX_POINT('',#34554);
#9177=VERTEX_POINT('',#34562);
#9178=VERTEX_POINT('',#34563);
#9179=VERTEX_POINT('',#34565);
#9180=VERTEX_POINT('',#34570);
#9181=VERTEX_POINT('',#34572);
#9182=VERTEX_POINT('',#34575);
#9183=VERTEX_POINT('',#34588);
#9184=VERTEX_POINT('',#34589);
#9185=VERTEX_POINT('',#34639);
#9186=VERTEX_POINT('',#34640);
#9187=VERTEX_POINT('',#34690);
#9188=VERTEX_POINT('',#34691);
#9189=VERTEX_POINT('',#34738);
#9190=VERTEX_POINT('',#34739);
#9191=VERTEX_POINT('',#34789);
#9192=VERTEX_POINT('',#34790);
#9193=VERTEX_POINT('',#34840);
#9194=VERTEX_POINT('',#34841);
#9195=VERTEX_POINT('',#34888);
#9196=VERTEX_POINT('',#34889);
#9197=VERTEX_POINT('',#34939);
#9198=VERTEX_POINT('',#34940);
#9199=VERTEX_POINT('',#34990);
#9200=VERTEX_POINT('',#34991);
#9201=VERTEX_POINT('',#35038);
#9202=VERTEX_POINT('',#35039);
#9203=VERTEX_POINT('',#35089);
#9204=VERTEX_POINT('',#35090);
#9205=VERTEX_POINT('',#35140);
#9206=VERTEX_POINT('',#35141);
#9207=VERTEX_POINT('',#35188);
#9208=VERTEX_POINT('',#35189);
#9209=VERTEX_POINT('',#35239);
#9210=VERTEX_POINT('',#35240);
#9211=VERTEX_POINT('',#35242);
#9212=VERTEX_POINT('',#35256);
#9213=VERTEX_POINT('',#35278);
#9214=VERTEX_POINT('',#35279);
#9215=VERTEX_POINT('',#35281);
#9216=VERTEX_POINT('',#35290);
#9217=VERTEX_POINT('',#35302);
#9218=VERTEX_POINT('',#35303);
#9219=VERTEX_POINT('',#35326);
#9220=VERTEX_POINT('',#35327);
#9221=VERTEX_POINT('',#35351);
#9222=VERTEX_POINT('',#35352);
#9223=VERTEX_POINT('',#35376);
#9224=VERTEX_POINT('',#35377);
#9225=VERTEX_POINT('',#35400);
#9226=VERTEX_POINT('',#35401);
#9227=VERTEX_POINT('',#35425);
#9228=VERTEX_POINT('',#35426);
#9229=VERTEX_POINT('',#35450);
#9230=VERTEX_POINT('',#35451);
#9231=VERTEX_POINT('',#35474);
#9232=VERTEX_POINT('',#35475);
#9233=VERTEX_POINT('',#35499);
#9234=VERTEX_POINT('',#35500);
#9235=VERTEX_POINT('',#35524);
#9236=VERTEX_POINT('',#35525);
#9237=VERTEX_POINT('',#35548);
#9238=VERTEX_POINT('',#35549);
#9239=VERTEX_POINT('',#35573);
#9240=VERTEX_POINT('',#35574);
#9241=VERTEX_POINT('',#35598);
#9242=VERTEX_POINT('',#35599);
#9243=VERTEX_POINT('',#35622);
#9244=VERTEX_POINT('',#35623);
#9245=VERTEX_POINT('',#35625);
#9246=VERTEX_POINT('',#35631);
#9247=VERTEX_POINT('',#35639);
#9248=VERTEX_POINT('',#35640);
#9249=VERTEX_POINT('',#35642);
#9250=VERTEX_POINT('',#35647);
#9251=VERTEX_POINT('',#35649);
#9252=VERTEX_POINT('',#35652);
#9253=VERTEX_POINT('',#35665);
#9254=VERTEX_POINT('',#35666);
#9255=VERTEX_POINT('',#35716);
#9256=VERTEX_POINT('',#35717);
#9257=VERTEX_POINT('',#35767);
#9258=VERTEX_POINT('',#35768);
#9259=VERTEX_POINT('',#35815);
#9260=VERTEX_POINT('',#35816);
#9261=VERTEX_POINT('',#35866);
#9262=VERTEX_POINT('',#35867);
#9263=VERTEX_POINT('',#35917);
#9264=VERTEX_POINT('',#35918);
#9265=VERTEX_POINT('',#35965);
#9266=VERTEX_POINT('',#35966);
#9267=VERTEX_POINT('',#36016);
#9268=VERTEX_POINT('',#36017);
#9269=VERTEX_POINT('',#36067);
#9270=VERTEX_POINT('',#36068);
#9271=VERTEX_POINT('',#36115);
#9272=VERTEX_POINT('',#36116);
#9273=VERTEX_POINT('',#36166);
#9274=VERTEX_POINT('',#36167);
#9275=VERTEX_POINT('',#36217);
#9276=VERTEX_POINT('',#36218);
#9277=VERTEX_POINT('',#36265);
#9278=VERTEX_POINT('',#36266);
#9279=VERTEX_POINT('',#36316);
#9280=VERTEX_POINT('',#36317);
#9281=VERTEX_POINT('',#36319);
#9282=VERTEX_POINT('',#36333);
#9283=VERTEX_POINT('',#36355);
#9284=VERTEX_POINT('',#36356);
#9285=VERTEX_POINT('',#36358);
#9286=VERTEX_POINT('',#36367);
#9287=VERTEX_POINT('',#36379);
#9288=VERTEX_POINT('',#36380);
#9289=VERTEX_POINT('',#36403);
#9290=VERTEX_POINT('',#36404);
#9291=VERTEX_POINT('',#36428);
#9292=VERTEX_POINT('',#36429);
#9293=VERTEX_POINT('',#36453);
#9294=VERTEX_POINT('',#36454);
#9295=VERTEX_POINT('',#36477);
#9296=VERTEX_POINT('',#36478);
#9297=VERTEX_POINT('',#36502);
#9298=VERTEX_POINT('',#36503);
#9299=VERTEX_POINT('',#36527);
#9300=VERTEX_POINT('',#36528);
#9301=VERTEX_POINT('',#36551);
#9302=VERTEX_POINT('',#36552);
#9303=VERTEX_POINT('',#36576);
#9304=VERTEX_POINT('',#36577);
#9305=VERTEX_POINT('',#36601);
#9306=VERTEX_POINT('',#36602);
#9307=VERTEX_POINT('',#36625);
#9308=VERTEX_POINT('',#36626);
#9309=VERTEX_POINT('',#36650);
#9310=VERTEX_POINT('',#36651);
#9311=VERTEX_POINT('',#36675);
#9312=VERTEX_POINT('',#36676);
#9313=VERTEX_POINT('',#36699);
#9314=VERTEX_POINT('',#36700);
#9315=VERTEX_POINT('',#36702);
#9316=VERTEX_POINT('',#36708);
#9317=VERTEX_POINT('',#36716);
#9318=VERTEX_POINT('',#36717);
#9319=VERTEX_POINT('',#36719);
#9320=VERTEX_POINT('',#36724);
#9321=VERTEX_POINT('',#36726);
#9322=VERTEX_POINT('',#36729);
#9323=VERTEX_POINT('',#36742);
#9324=VERTEX_POINT('',#36743);
#9325=VERTEX_POINT('',#36793);
#9326=VERTEX_POINT('',#36794);
#9327=VERTEX_POINT('',#36844);
#9328=VERTEX_POINT('',#36845);
#9329=VERTEX_POINT('',#36892);
#9330=VERTEX_POINT('',#36893);
#9331=VERTEX_POINT('',#36943);
#9332=VERTEX_POINT('',#36944);
#9333=VERTEX_POINT('',#36994);
#9334=VERTEX_POINT('',#36995);
#9335=VERTEX_POINT('',#37042);
#9336=VERTEX_POINT('',#37043);
#9337=VERTEX_POINT('',#37093);
#9338=VERTEX_POINT('',#37094);
#9339=VERTEX_POINT('',#37144);
#9340=VERTEX_POINT('',#37145);
#9341=VERTEX_POINT('',#37192);
#9342=VERTEX_POINT('',#37193);
#9343=VERTEX_POINT('',#37243);
#9344=VERTEX_POINT('',#37244);
#9345=VERTEX_POINT('',#37294);
#9346=VERTEX_POINT('',#37295);
#9347=VERTEX_POINT('',#37342);
#9348=VERTEX_POINT('',#37343);
#9349=VERTEX_POINT('',#37393);
#9350=VERTEX_POINT('',#37394);
#9351=VERTEX_POINT('',#37396);
#9352=VERTEX_POINT('',#37410);
#9353=VERTEX_POINT('',#37432);
#9354=VERTEX_POINT('',#37433);
#9355=VERTEX_POINT('',#37435);
#9356=VERTEX_POINT('',#37444);
#9357=VERTEX_POINT('',#37456);
#9358=VERTEX_POINT('',#37457);
#9359=VERTEX_POINT('',#37480);
#9360=VERTEX_POINT('',#37481);
#9361=VERTEX_POINT('',#37505);
#9362=VERTEX_POINT('',#37506);
#9363=VERTEX_POINT('',#37530);
#9364=VERTEX_POINT('',#37531);
#9365=VERTEX_POINT('',#37554);
#9366=VERTEX_POINT('',#37555);
#9367=VERTEX_POINT('',#37579);
#9368=VERTEX_POINT('',#37580);
#9369=VERTEX_POINT('',#37604);
#9370=VERTEX_POINT('',#37605);
#9371=VERTEX_POINT('',#37628);
#9372=VERTEX_POINT('',#37629);
#9373=VERTEX_POINT('',#37653);
#9374=VERTEX_POINT('',#37654);
#9375=VERTEX_POINT('',#37678);
#9376=VERTEX_POINT('',#37679);
#9377=VERTEX_POINT('',#37702);
#9378=VERTEX_POINT('',#37703);
#9379=VERTEX_POINT('',#37727);
#9380=VERTEX_POINT('',#37728);
#9381=VERTEX_POINT('',#37752);
#9382=VERTEX_POINT('',#37753);
#9383=VERTEX_POINT('',#37776);
#9384=VERTEX_POINT('',#37777);
#9385=VERTEX_POINT('',#37779);
#9386=VERTEX_POINT('',#37785);
#9387=VERTEX_POINT('',#37793);
#9388=VERTEX_POINT('',#37794);
#9389=VERTEX_POINT('',#37796);
#9390=VERTEX_POINT('',#37801);
#9391=VERTEX_POINT('',#37803);
#9392=VERTEX_POINT('',#37806);
#9393=VERTEX_POINT('',#37819);
#9394=VERTEX_POINT('',#37820);
#9395=VERTEX_POINT('',#37870);
#9396=VERTEX_POINT('',#37871);
#9397=VERTEX_POINT('',#37921);
#9398=VERTEX_POINT('',#37922);
#9399=VERTEX_POINT('',#37969);
#9400=VERTEX_POINT('',#37970);
#9401=VERTEX_POINT('',#38020);
#9402=VERTEX_POINT('',#38021);
#9403=VERTEX_POINT('',#38071);
#9404=VERTEX_POINT('',#38072);
#9405=VERTEX_POINT('',#38119);
#9406=VERTEX_POINT('',#38120);
#9407=VERTEX_POINT('',#38170);
#9408=VERTEX_POINT('',#38171);
#9409=VERTEX_POINT('',#38221);
#9410=VERTEX_POINT('',#38222);
#9411=VERTEX_POINT('',#38269);
#9412=VERTEX_POINT('',#38270);
#9413=VERTEX_POINT('',#38320);
#9414=VERTEX_POINT('',#38321);
#9415=VERTEX_POINT('',#38371);
#9416=VERTEX_POINT('',#38372);
#9417=VERTEX_POINT('',#38419);
#9418=VERTEX_POINT('',#38420);
#9419=VERTEX_POINT('',#38470);
#9420=VERTEX_POINT('',#38471);
#9421=VERTEX_POINT('',#38473);
#9422=VERTEX_POINT('',#38487);
#9423=VERTEX_POINT('',#38509);
#9424=VERTEX_POINT('',#38510);
#9425=VERTEX_POINT('',#38512);
#9426=VERTEX_POINT('',#38521);
#9427=VERTEX_POINT('',#38533);
#9428=VERTEX_POINT('',#38534);
#9429=VERTEX_POINT('',#38557);
#9430=VERTEX_POINT('',#38558);
#9431=VERTEX_POINT('',#38582);
#9432=VERTEX_POINT('',#38583);
#9433=VERTEX_POINT('',#38607);
#9434=VERTEX_POINT('',#38608);
#9435=VERTEX_POINT('',#38631);
#9436=VERTEX_POINT('',#38632);
#9437=VERTEX_POINT('',#38656);
#9438=VERTEX_POINT('',#38657);
#9439=VERTEX_POINT('',#38681);
#9440=VERTEX_POINT('',#38682);
#9441=VERTEX_POINT('',#38705);
#9442=VERTEX_POINT('',#38706);
#9443=VERTEX_POINT('',#38730);
#9444=VERTEX_POINT('',#38731);
#9445=VERTEX_POINT('',#38755);
#9446=VERTEX_POINT('',#38756);
#9447=VERTEX_POINT('',#38779);
#9448=VERTEX_POINT('',#38780);
#9449=VERTEX_POINT('',#38804);
#9450=VERTEX_POINT('',#38805);
#9451=VERTEX_POINT('',#38829);
#9452=VERTEX_POINT('',#38830);
#9453=VERTEX_POINT('',#38853);
#9454=VERTEX_POINT('',#38854);
#9455=VERTEX_POINT('',#38856);
#9456=VERTEX_POINT('',#38862);
#9457=VERTEX_POINT('',#38870);
#9458=VERTEX_POINT('',#38871);
#9459=VERTEX_POINT('',#38873);
#9460=VERTEX_POINT('',#38878);
#9461=VERTEX_POINT('',#38880);
#9462=VERTEX_POINT('',#38883);
#9463=VERTEX_POINT('',#38896);
#9464=VERTEX_POINT('',#38897);
#9465=VERTEX_POINT('',#38947);
#9466=VERTEX_POINT('',#38948);
#9467=VERTEX_POINT('',#38998);
#9468=VERTEX_POINT('',#38999);
#9469=VERTEX_POINT('',#39046);
#9470=VERTEX_POINT('',#39047);
#9471=VERTEX_POINT('',#39097);
#9472=VERTEX_POINT('',#39098);
#9473=VERTEX_POINT('',#39148);
#9474=VERTEX_POINT('',#39149);
#9475=VERTEX_POINT('',#39196);
#9476=VERTEX_POINT('',#39197);
#9477=VERTEX_POINT('',#39247);
#9478=VERTEX_POINT('',#39248);
#9479=VERTEX_POINT('',#39298);
#9480=VERTEX_POINT('',#39299);
#9481=VERTEX_POINT('',#39346);
#9482=VERTEX_POINT('',#39347);
#9483=VERTEX_POINT('',#39397);
#9484=VERTEX_POINT('',#39398);
#9485=VERTEX_POINT('',#39448);
#9486=VERTEX_POINT('',#39449);
#9487=VERTEX_POINT('',#39496);
#9488=VERTEX_POINT('',#39497);
#9489=VERTEX_POINT('',#39547);
#9490=VERTEX_POINT('',#39548);
#9491=VERTEX_POINT('',#39550);
#9492=VERTEX_POINT('',#39564);
#9493=VERTEX_POINT('',#39586);
#9494=VERTEX_POINT('',#39587);
#9495=VERTEX_POINT('',#39589);
#9496=VERTEX_POINT('',#39598);
#9497=VERTEX_POINT('',#39610);
#9498=VERTEX_POINT('',#39611);
#9499=VERTEX_POINT('',#39634);
#9500=VERTEX_POINT('',#39635);
#9501=VERTEX_POINT('',#39659);
#9502=VERTEX_POINT('',#39660);
#9503=VERTEX_POINT('',#39684);
#9504=VERTEX_POINT('',#39685);
#9505=VERTEX_POINT('',#39708);
#9506=VERTEX_POINT('',#39709);
#9507=VERTEX_POINT('',#39733);
#9508=VERTEX_POINT('',#39734);
#9509=VERTEX_POINT('',#39758);
#9510=VERTEX_POINT('',#39759);
#9511=VERTEX_POINT('',#39782);
#9512=VERTEX_POINT('',#39783);
#9513=VERTEX_POINT('',#39807);
#9514=VERTEX_POINT('',#39808);
#9515=VERTEX_POINT('',#39832);
#9516=VERTEX_POINT('',#39833);
#9517=VERTEX_POINT('',#39856);
#9518=VERTEX_POINT('',#39857);
#9519=VERTEX_POINT('',#39881);
#9520=VERTEX_POINT('',#39882);
#9521=VERTEX_POINT('',#39906);
#9522=VERTEX_POINT('',#39907);
#9523=VERTEX_POINT('',#39930);
#9524=VERTEX_POINT('',#39931);
#9525=VERTEX_POINT('',#39933);
#9526=VERTEX_POINT('',#39939);
#9527=VERTEX_POINT('',#39947);
#9528=VERTEX_POINT('',#39948);
#9529=VERTEX_POINT('',#39950);
#9530=VERTEX_POINT('',#39955);
#9531=VERTEX_POINT('',#39957);
#9532=VERTEX_POINT('',#39960);
#9533=VERTEX_POINT('',#39973);
#9534=VERTEX_POINT('',#39974);
#9535=VERTEX_POINT('',#40024);
#9536=VERTEX_POINT('',#40025);
#9537=VERTEX_POINT('',#40075);
#9538=VERTEX_POINT('',#40076);
#9539=VERTEX_POINT('',#40123);
#9540=VERTEX_POINT('',#40124);
#9541=VERTEX_POINT('',#40174);
#9542=VERTEX_POINT('',#40175);
#9543=VERTEX_POINT('',#40225);
#9544=VERTEX_POINT('',#40226);
#9545=VERTEX_POINT('',#40273);
#9546=VERTEX_POINT('',#40274);
#9547=VERTEX_POINT('',#40324);
#9548=VERTEX_POINT('',#40325);
#9549=VERTEX_POINT('',#40375);
#9550=VERTEX_POINT('',#40376);
#9551=VERTEX_POINT('',#40423);
#9552=VERTEX_POINT('',#40424);
#9553=VERTEX_POINT('',#40474);
#9554=VERTEX_POINT('',#40475);
#9555=VERTEX_POINT('',#40525);
#9556=VERTEX_POINT('',#40526);
#9557=VERTEX_POINT('',#40573);
#9558=VERTEX_POINT('',#40574);
#9559=VERTEX_POINT('',#40624);
#9560=VERTEX_POINT('',#40625);
#9561=VERTEX_POINT('',#40627);
#9562=VERTEX_POINT('',#40641);
#9563=VERTEX_POINT('',#40663);
#9564=VERTEX_POINT('',#40664);
#9565=VERTEX_POINT('',#40666);
#9566=VERTEX_POINT('',#40675);
#9567=VERTEX_POINT('',#40687);
#9568=VERTEX_POINT('',#40688);
#9569=VERTEX_POINT('',#40711);
#9570=VERTEX_POINT('',#40712);
#9571=VERTEX_POINT('',#40736);
#9572=VERTEX_POINT('',#40737);
#9573=VERTEX_POINT('',#40761);
#9574=VERTEX_POINT('',#40762);
#9575=VERTEX_POINT('',#40785);
#9576=VERTEX_POINT('',#40786);
#9577=VERTEX_POINT('',#40810);
#9578=VERTEX_POINT('',#40811);
#9579=VERTEX_POINT('',#40835);
#9580=VERTEX_POINT('',#40836);
#9581=VERTEX_POINT('',#40859);
#9582=VERTEX_POINT('',#40860);
#9583=VERTEX_POINT('',#40884);
#9584=VERTEX_POINT('',#40885);
#9585=VERTEX_POINT('',#40909);
#9586=VERTEX_POINT('',#40910);
#9587=VERTEX_POINT('',#40933);
#9588=VERTEX_POINT('',#40934);
#9589=VERTEX_POINT('',#40958);
#9590=VERTEX_POINT('',#40959);
#9591=VERTEX_POINT('',#40983);
#9592=VERTEX_POINT('',#40984);
#9593=VERTEX_POINT('',#41007);
#9594=VERTEX_POINT('',#41008);
#9595=VERTEX_POINT('',#41010);
#9596=VERTEX_POINT('',#41016);
#9597=VERTEX_POINT('',#41024);
#9598=VERTEX_POINT('',#41025);
#9599=VERTEX_POINT('',#41044);
#9600=VERTEX_POINT('',#41046);
#9601=VERTEX_POINT('',#41103);
#9602=VERTEX_POINT('',#41104);
#9603=VERTEX_POINT('',#41142);
#9604=VERTEX_POINT('',#41144);
#9605=VERTEX_POINT('',#41182);
#9606=VERTEX_POINT('',#41183);
#9607=VERTEX_POINT('',#41202);
#9608=VERTEX_POINT('',#41213);
#9609=VERTEX_POINT('',#41215);
#9610=VERTEX_POINT('',#41226);
#9611=VERTEX_POINT('',#41266);
#9612=VERTEX_POINT('',#41267);
#9613=VERTEX_POINT('',#41286);
#9614=VERTEX_POINT('',#41297);
#9615=VERTEX_POINT('',#41344);
#9616=VERTEX_POINT('',#41345);
#9617=VERTEX_POINT('',#41364);
#9618=VERTEX_POINT('',#41366);
#9619=VERTEX_POINT('',#41423);
#9620=VERTEX_POINT('',#41424);
#9621=VERTEX_POINT('',#41462);
#9622=VERTEX_POINT('',#41464);
#9623=VERTEX_POINT('',#41502);
#9624=VERTEX_POINT('',#41503);
#9625=VERTEX_POINT('',#41522);
#9626=VERTEX_POINT('',#41533);
#9627=VERTEX_POINT('',#41535);
#9628=VERTEX_POINT('',#41546);
#9629=VERTEX_POINT('',#41586);
#9630=VERTEX_POINT('',#41587);
#9631=VERTEX_POINT('',#41606);
#9632=VERTEX_POINT('',#41617);
#9633=VERTEX_POINT('',#41664);
#9634=VERTEX_POINT('',#41665);
#9635=VERTEX_POINT('',#41684);
#9636=VERTEX_POINT('',#41686);
#9637=VERTEX_POINT('',#41743);
#9638=VERTEX_POINT('',#41744);
#9639=VERTEX_POINT('',#41782);
#9640=VERTEX_POINT('',#41784);
#9641=VERTEX_POINT('',#41822);
#9642=VERTEX_POINT('',#41823);
#9643=VERTEX_POINT('',#41842);
#9644=VERTEX_POINT('',#41853);
#9645=VERTEX_POINT('',#41855);
#9646=VERTEX_POINT('',#41866);
#9647=VERTEX_POINT('',#41906);
#9648=VERTEX_POINT('',#41907);
#9649=VERTEX_POINT('',#41926);
#9650=VERTEX_POINT('',#41937);
#9651=VERTEX_POINT('',#51968);
#9652=VERTEX_POINT('',#51970);
#9653=VERTEX_POINT('',#51974);
#9654=VERTEX_POINT('',#51976);
#9655=VERTEX_POINT('',#51980);
#9656=VERTEX_POINT('',#51982);
#9657=VERTEX_POINT('',#51986);
#9658=VERTEX_POINT('',#51988);
#9659=VERTEX_POINT('',#51992);
#9660=VERTEX_POINT('',#51994);
#9661=VERTEX_POINT('',#51998);
#9662=VERTEX_POINT('',#52001);
#9663=VERTEX_POINT('',#52006);
#9664=VERTEX_POINT('',#52010);
#9665=VERTEX_POINT('',#52015);
#9666=VERTEX_POINT('',#52020);
#9667=VERTEX_POINT('',#52023);
#9668=VERTEX_POINT('',#52027);
#9669=VERTEX_POINT('',#52034);
#9670=VERTEX_POINT('',#52035);
#9671=VERTEX_POINT('',#52054);
#9672=VERTEX_POINT('',#52078);
#9673=VERTEX_POINT('',#52079);
#9674=VERTEX_POINT('',#52117);
#9675=VERTEX_POINT('',#52122);
#9676=VERTEX_POINT('',#52123);
#9677=VERTEX_POINT('',#52142);
#9678=VERTEX_POINT('',#52153);
#9679=VERTEX_POINT('',#52168);
#9680=VERTEX_POINT('',#52169);
#9681=VERTEX_POINT('',#52188);
#9682=VERTEX_POINT('',#52199);
#9683=VERTEX_POINT('',#52214);
#9684=VERTEX_POINT('',#52216);
#9685=VERTEX_POINT('',#52220);
#9686=VERTEX_POINT('',#52223);
#9687=VERTEX_POINT('',#52230);
#9688=VERTEX_POINT('',#52232);
#9689=VERTEX_POINT('',#52236);
#9690=VERTEX_POINT('',#52238);
#9691=VERTEX_POINT('',#52242);
#9692=VERTEX_POINT('',#52244);
#9693=VERTEX_POINT('',#52248);
#9694=VERTEX_POINT('',#52250);
#9695=VERTEX_POINT('',#52254);
#9696=VERTEX_POINT('',#52256);
#9697=VERTEX_POINT('',#52260);
#9698=VERTEX_POINT('',#52262);
#9699=VERTEX_POINT('',#52266);
#9700=VERTEX_POINT('',#52268);
#9701=VERTEX_POINT('',#52272);
#9702=VERTEX_POINT('',#52274);
#9703=VERTEX_POINT('',#52278);
#9704=VERTEX_POINT('',#52280);
#9705=VERTEX_POINT('',#52284);
#9706=VERTEX_POINT('',#52286);
#9707=VERTEX_POINT('',#52293);
#9708=VERTEX_POINT('',#52294);
#9709=VERTEX_POINT('',#52296);
#9710=VERTEX_POINT('',#52298);
#9711=VERTEX_POINT('',#52302);
#9712=VERTEX_POINT('',#52304);
#9713=VERTEX_POINT('',#52308);
#9714=VERTEX_POINT('',#52310);
#9715=VERTEX_POINT('',#52318);
#9716=VERTEX_POINT('',#52320);
#9717=VERTEX_POINT('',#52324);
#9718=VERTEX_POINT('',#52327);
#9719=VERTEX_POINT('',#52330);
#9720=VERTEX_POINT('',#52334);
#9721=VERTEX_POINT('',#52336);
#9722=VERTEX_POINT('',#52340);
#9723=VERTEX_POINT('',#52343);
#9724=VERTEX_POINT('',#52346);
#9725=VERTEX_POINT('',#52350);
#9726=VERTEX_POINT('',#52352);
#9727=VERTEX_POINT('',#52355);
#9728=VERTEX_POINT('',#52357);
#9729=VERTEX_POINT('',#52362);
#9730=VERTEX_POINT('',#52366);
#9731=VERTEX_POINT('',#52368);
#9732=VERTEX_POINT('',#52371);
#9733=VERTEX_POINT('',#52376);
#9734=VERTEX_POINT('',#52383);
#9735=VERTEX_POINT('',#52385);
#9736=VERTEX_POINT('',#52390);
#9737=VERTEX_POINT('',#52397);
#9738=VERTEX_POINT('',#52398);
#9739=VERTEX_POINT('',#52417);
#9740=VERTEX_POINT('',#52441);
#9741=VERTEX_POINT('',#52442);
#9742=VERTEX_POINT('',#52480);
#9743=VERTEX_POINT('',#52485);
#9744=VERTEX_POINT('',#52486);
#9745=VERTEX_POINT('',#52505);
#9746=VERTEX_POINT('',#52516);
#9747=VERTEX_POINT('',#52531);
#9748=VERTEX_POINT('',#52532);
#9749=VERTEX_POINT('',#52551);
#9750=VERTEX_POINT('',#52562);
#9751=VERTEX_POINT('',#52596);
#9752=VERTEX_POINT('',#52597);
#9753=VERTEX_POINT('',#52605);
#9754=VERTEX_POINT('',#52610);
#9755=VERTEX_POINT('',#53032);
#9756=VERTEX_POINT('',#53227);
#9757=VERTEX_POINT('',#53443);
#9758=VERTEX_POINT('',#53444);
#9759=VERTEX_POINT('',#53452);
#9760=VERTEX_POINT('',#53457);
#9761=VERTEX_POINT('',#53492);
#9762=VERTEX_POINT('',#53493);
#9763=VERTEX_POINT('',#53501);
#9764=VERTEX_POINT('',#53506);
#9765=VERTEX_POINT('',#53928);
#9766=VERTEX_POINT('',#54123);
#9767=VERTEX_POINT('',#54339);
#9768=VERTEX_POINT('',#54340);
#9769=VERTEX_POINT('',#54348);
#9770=VERTEX_POINT('',#54353);
#9771=VERTEX_POINT('',#54388);
#9772=VERTEX_POINT('',#54389);
#9773=VERTEX_POINT('',#54397);
#9774=VERTEX_POINT('',#54402);
#9775=VERTEX_POINT('',#54824);
#9776=VERTEX_POINT('',#55019);
#9777=VERTEX_POINT('',#55235);
#9778=VERTEX_POINT('',#55236);
#9779=VERTEX_POINT('',#55244);
#9780=VERTEX_POINT('',#55249);
#9781=VERTEX_POINT('',#55284);
#9782=VERTEX_POINT('',#55285);
#9783=VERTEX_POINT('',#55293);
#9784=VERTEX_POINT('',#55298);
#9785=VERTEX_POINT('',#55720);
#9786=VERTEX_POINT('',#55915);
#9787=VERTEX_POINT('',#56131);
#9788=VERTEX_POINT('',#56132);
#9789=VERTEX_POINT('',#56140);
#9790=VERTEX_POINT('',#56145);
#9791=VERTEX_POINT('',#56180);
#9792=VERTEX_POINT('',#56181);
#9793=VERTEX_POINT('',#56189);
#9794=VERTEX_POINT('',#56194);
#9795=VERTEX_POINT('',#56616);
#9796=VERTEX_POINT('',#56811);
#9797=VERTEX_POINT('',#57027);
#9798=VERTEX_POINT('',#57028);
#9799=VERTEX_POINT('',#57036);
#9800=VERTEX_POINT('',#57041);
#9801=VERTEX_POINT('',#57076);
#9802=VERTEX_POINT('',#57077);
#9803=VERTEX_POINT('',#57085);
#9804=VERTEX_POINT('',#57090);
#9805=VERTEX_POINT('',#57512);
#9806=VERTEX_POINT('',#57707);
#9807=VERTEX_POINT('',#57923);
#9808=VERTEX_POINT('',#57924);
#9809=VERTEX_POINT('',#57932);
#9810=VERTEX_POINT('',#57937);
#9811=VERTEX_POINT('',#57972);
#9812=VERTEX_POINT('',#57973);
#9813=VERTEX_POINT('',#57981);
#9814=VERTEX_POINT('',#57986);
#9815=VERTEX_POINT('',#58408);
#9816=VERTEX_POINT('',#58603);
#9817=VERTEX_POINT('',#58819);
#9818=VERTEX_POINT('',#58820);
#9819=VERTEX_POINT('',#58828);
#9820=VERTEX_POINT('',#58833);
#9821=VERTEX_POINT('',#58868);
#9822=VERTEX_POINT('',#58869);
#9823=VERTEX_POINT('',#58877);
#9824=VERTEX_POINT('',#58882);
#9825=VERTEX_POINT('',#59304);
#9826=VERTEX_POINT('',#59499);
#9827=VERTEX_POINT('',#59715);
#9828=VERTEX_POINT('',#59716);
#9829=VERTEX_POINT('',#59724);
#9830=VERTEX_POINT('',#59729);
#9831=VERTEX_POINT('',#59764);
#9832=VERTEX_POINT('',#59765);
#9833=VERTEX_POINT('',#59773);
#9834=VERTEX_POINT('',#59778);
#9835=VERTEX_POINT('',#60200);
#9836=VERTEX_POINT('',#60395);
#9837=VERTEX_POINT('',#60611);
#9838=VERTEX_POINT('',#60612);
#9839=VERTEX_POINT('',#60620);
#9840=VERTEX_POINT('',#60625);
#9841=VERTEX_POINT('',#60660);
#9842=VERTEX_POINT('',#60661);
#9843=VERTEX_POINT('',#60669);
#9844=VERTEX_POINT('',#60674);
#9845=VERTEX_POINT('',#61096);
#9846=VERTEX_POINT('',#61291);
#9847=VERTEX_POINT('',#61507);
#9848=VERTEX_POINT('',#61508);
#9849=VERTEX_POINT('',#61516);
#9850=VERTEX_POINT('',#61521);
#9851=VERTEX_POINT('',#61556);
#9852=VERTEX_POINT('',#61557);
#9853=VERTEX_POINT('',#61565);
#9854=VERTEX_POINT('',#61570);
#9855=VERTEX_POINT('',#61992);
#9856=VERTEX_POINT('',#62187);
#9857=VERTEX_POINT('',#62403);
#9858=VERTEX_POINT('',#62404);
#9859=VERTEX_POINT('',#62412);
#9860=VERTEX_POINT('',#62417);
#9861=VERTEX_POINT('',#62452);
#9862=VERTEX_POINT('',#62453);
#9863=VERTEX_POINT('',#62461);
#9864=VERTEX_POINT('',#62466);
#9865=VERTEX_POINT('',#62888);
#9866=VERTEX_POINT('',#63083);
#9867=VERTEX_POINT('',#63299);
#9868=VERTEX_POINT('',#63300);
#9869=VERTEX_POINT('',#63308);
#9870=VERTEX_POINT('',#63313);
#9871=VERTEX_POINT('',#63348);
#9872=VERTEX_POINT('',#63349);
#9873=VERTEX_POINT('',#63357);
#9874=VERTEX_POINT('',#63362);
#9875=VERTEX_POINT('',#63784);
#9876=VERTEX_POINT('',#63979);
#9877=VERTEX_POINT('',#64195);
#9878=VERTEX_POINT('',#64196);
#9879=VERTEX_POINT('',#64204);
#9880=VERTEX_POINT('',#64209);
#9881=VERTEX_POINT('',#64244);
#9882=VERTEX_POINT('',#64245);
#9883=VERTEX_POINT('',#64253);
#9884=VERTEX_POINT('',#64258);
#9885=VERTEX_POINT('',#64680);
#9886=VERTEX_POINT('',#64875);
#9887=VERTEX_POINT('',#65091);
#9888=VERTEX_POINT('',#65092);
#9889=VERTEX_POINT('',#65100);
#9890=VERTEX_POINT('',#65105);
#9891=VERTEX_POINT('',#65140);
#9892=VERTEX_POINT('',#65141);
#9893=VERTEX_POINT('',#65149);
#9894=VERTEX_POINT('',#65154);
#9895=VERTEX_POINT('',#65576);
#9896=VERTEX_POINT('',#65771);
#9897=VERTEX_POINT('',#65987);
#9898=VERTEX_POINT('',#65988);
#9899=VERTEX_POINT('',#65996);
#9900=VERTEX_POINT('',#66001);
#9901=VERTEX_POINT('',#66036);
#9902=VERTEX_POINT('',#66037);
#9903=VERTEX_POINT('',#66045);
#9904=VERTEX_POINT('',#66050);
#9905=VERTEX_POINT('',#66472);
#9906=VERTEX_POINT('',#66667);
#9907=VERTEX_POINT('',#66883);
#9908=VERTEX_POINT('',#66884);
#9909=VERTEX_POINT('',#66892);
#9910=VERTEX_POINT('',#66897);
#9911=VERTEX_POINT('',#66932);
#9912=VERTEX_POINT('',#66933);
#9913=VERTEX_POINT('',#66941);
#9914=VERTEX_POINT('',#66946);
#9915=VERTEX_POINT('',#67368);
#9916=VERTEX_POINT('',#67563);
#9917=VERTEX_POINT('',#67779);
#9918=VERTEX_POINT('',#67780);
#9919=VERTEX_POINT('',#67788);
#9920=VERTEX_POINT('',#67793);
#9921=VERTEX_POINT('',#67828);
#9922=VERTEX_POINT('',#67829);
#9923=VERTEX_POINT('',#67837);
#9924=VERTEX_POINT('',#67842);
#9925=VERTEX_POINT('',#68264);
#9926=VERTEX_POINT('',#68459);
#9927=VERTEX_POINT('',#68675);
#9928=VERTEX_POINT('',#68676);
#9929=VERTEX_POINT('',#68684);
#9930=VERTEX_POINT('',#68689);
#9931=VERTEX_POINT('',#68724);
#9932=VERTEX_POINT('',#68725);
#9933=VERTEX_POINT('',#68733);
#9934=VERTEX_POINT('',#68738);
#9935=VERTEX_POINT('',#69160);
#9936=VERTEX_POINT('',#69355);
#9937=VERTEX_POINT('',#69571);
#9938=VERTEX_POINT('',#69572);
#9939=VERTEX_POINT('',#69580);
#9940=VERTEX_POINT('',#69585);
#9941=VERTEX_POINT('',#69620);
#9942=VERTEX_POINT('',#69621);
#9943=VERTEX_POINT('',#69629);
#9944=VERTEX_POINT('',#69634);
#9945=VERTEX_POINT('',#70056);
#9946=VERTEX_POINT('',#70251);
#9947=VERTEX_POINT('',#70467);
#9948=VERTEX_POINT('',#70468);
#9949=VERTEX_POINT('',#70476);
#9950=VERTEX_POINT('',#70481);
#9951=VERTEX_POINT('',#70516);
#9952=VERTEX_POINT('',#70517);
#9953=VERTEX_POINT('',#70525);
#9954=VERTEX_POINT('',#70530);
#9955=VERTEX_POINT('',#70952);
#9956=VERTEX_POINT('',#71147);
#9957=VERTEX_POINT('',#71363);
#9958=VERTEX_POINT('',#71364);
#9959=VERTEX_POINT('',#71372);
#9960=VERTEX_POINT('',#71377);
#9961=VERTEX_POINT('',#71412);
#9962=VERTEX_POINT('',#71413);
#9963=VERTEX_POINT('',#71421);
#9964=VERTEX_POINT('',#71426);
#9965=VERTEX_POINT('',#71848);
#9966=VERTEX_POINT('',#72043);
#9967=VERTEX_POINT('',#72259);
#9968=VERTEX_POINT('',#72260);
#9969=VERTEX_POINT('',#72268);
#9970=VERTEX_POINT('',#72273);
#9971=VERTEX_POINT('',#72308);
#9972=VERTEX_POINT('',#72309);
#9973=VERTEX_POINT('',#72317);
#9974=VERTEX_POINT('',#72322);
#9975=VERTEX_POINT('',#72744);
#9976=VERTEX_POINT('',#72939);
#9977=VERTEX_POINT('',#73155);
#9978=VERTEX_POINT('',#73156);
#9979=VERTEX_POINT('',#73164);
#9980=VERTEX_POINT('',#73169);
#9981=VERTEX_POINT('',#73204);
#9982=VERTEX_POINT('',#73205);
#9983=VERTEX_POINT('',#73213);
#9984=VERTEX_POINT('',#73218);
#9985=VERTEX_POINT('',#73640);
#9986=VERTEX_POINT('',#73835);
#9987=VERTEX_POINT('',#74051);
#9988=VERTEX_POINT('',#74052);
#9989=VERTEX_POINT('',#74060);
#9990=VERTEX_POINT('',#74065);
#9991=VERTEX_POINT('',#74100);
#9992=VERTEX_POINT('',#74101);
#9993=VERTEX_POINT('',#74109);
#9994=VERTEX_POINT('',#74114);
#9995=VERTEX_POINT('',#74536);
#9996=VERTEX_POINT('',#74731);
#9997=VERTEX_POINT('',#74947);
#9998=VERTEX_POINT('',#74948);
#9999=VERTEX_POINT('',#74956);
#10000=VERTEX_POINT('',#74961);
#10001=VERTEX_POINT('',#74996);
#10002=VERTEX_POINT('',#74997);
#10003=VERTEX_POINT('',#75005);
#10004=VERTEX_POINT('',#75010);
#10005=VERTEX_POINT('',#75432);
#10006=VERTEX_POINT('',#75627);
#10007=VERTEX_POINT('',#75843);
#10008=VERTEX_POINT('',#75844);
#10009=VERTEX_POINT('',#75852);
#10010=VERTEX_POINT('',#75857);
#10011=VERTEX_POINT('',#75892);
#10012=VERTEX_POINT('',#75893);
#10013=VERTEX_POINT('',#75901);
#10014=VERTEX_POINT('',#75906);
#10015=VERTEX_POINT('',#76328);
#10016=VERTEX_POINT('',#76523);
#10017=VERTEX_POINT('',#76739);
#10018=VERTEX_POINT('',#76740);
#10019=VERTEX_POINT('',#76748);
#10020=VERTEX_POINT('',#76753);
#10021=VERTEX_POINT('',#76788);
#10022=VERTEX_POINT('',#76789);
#10023=VERTEX_POINT('',#76797);
#10024=VERTEX_POINT('',#76802);
#10025=VERTEX_POINT('',#77224);
#10026=VERTEX_POINT('',#77419);
#10027=VERTEX_POINT('',#77635);
#10028=VERTEX_POINT('',#77636);
#10029=VERTEX_POINT('',#77644);
#10030=VERTEX_POINT('',#77649);
#10031=VERTEX_POINT('',#77684);
#10032=VERTEX_POINT('',#77685);
#10033=VERTEX_POINT('',#77693);
#10034=VERTEX_POINT('',#77698);
#10035=VERTEX_POINT('',#78120);
#10036=VERTEX_POINT('',#78315);
#10037=VERTEX_POINT('',#78531);
#10038=VERTEX_POINT('',#78532);
#10039=VERTEX_POINT('',#78540);
#10040=VERTEX_POINT('',#78545);
#10041=VERTEX_POINT('',#78580);
#10042=VERTEX_POINT('',#78581);
#10043=VERTEX_POINT('',#78589);
#10044=VERTEX_POINT('',#78594);
#10045=VERTEX_POINT('',#79016);
#10046=VERTEX_POINT('',#79211);
#10047=VERTEX_POINT('',#79427);
#10048=VERTEX_POINT('',#79428);
#10049=VERTEX_POINT('',#79436);
#10050=VERTEX_POINT('',#79441);
#10051=VERTEX_POINT('',#79476);
#10052=VERTEX_POINT('',#79477);
#10053=VERTEX_POINT('',#79485);
#10054=VERTEX_POINT('',#79490);
#10055=VERTEX_POINT('',#79912);
#10056=VERTEX_POINT('',#80107);
#10057=VERTEX_POINT('',#80323);
#10058=VERTEX_POINT('',#80324);
#10059=VERTEX_POINT('',#80332);
#10060=VERTEX_POINT('',#80337);
#10061=VERTEX_POINT('',#80372);
#10062=VERTEX_POINT('',#80373);
#10063=VERTEX_POINT('',#80381);
#10064=VERTEX_POINT('',#80386);
#10065=VERTEX_POINT('',#80808);
#10066=VERTEX_POINT('',#81003);
#10067=VERTEX_POINT('',#81219);
#10068=VERTEX_POINT('',#81220);
#10069=VERTEX_POINT('',#81228);
#10070=VERTEX_POINT('',#81233);
#10071=VERTEX_POINT('',#81268);
#10072=VERTEX_POINT('',#81269);
#10073=VERTEX_POINT('',#81277);
#10074=VERTEX_POINT('',#81282);
#10075=VERTEX_POINT('',#81704);
#10076=VERTEX_POINT('',#81899);
#10077=VERTEX_POINT('',#82115);
#10078=VERTEX_POINT('',#82116);
#10079=VERTEX_POINT('',#82124);
#10080=VERTEX_POINT('',#82129);
#10081=VERTEX_POINT('',#82164);
#10082=VERTEX_POINT('',#82165);
#10083=VERTEX_POINT('',#82173);
#10084=VERTEX_POINT('',#82178);
#10085=VERTEX_POINT('',#82600);
#10086=VERTEX_POINT('',#82795);
#10087=VERTEX_POINT('',#83011);
#10088=VERTEX_POINT('',#83012);
#10089=VERTEX_POINT('',#83020);
#10090=VERTEX_POINT('',#83025);
#10091=VERTEX_POINT('',#83060);
#10092=VERTEX_POINT('',#83061);
#10093=VERTEX_POINT('',#83069);
#10094=VERTEX_POINT('',#83074);
#10095=VERTEX_POINT('',#83496);
#10096=VERTEX_POINT('',#83691);
#10097=VERTEX_POINT('',#83907);
#10098=VERTEX_POINT('',#83908);
#10099=VERTEX_POINT('',#83916);
#10100=VERTEX_POINT('',#83921);
#10101=VERTEX_POINT('',#83956);
#10102=VERTEX_POINT('',#83957);
#10103=VERTEX_POINT('',#83965);
#10104=VERTEX_POINT('',#83970);
#10105=VERTEX_POINT('',#84392);
#10106=VERTEX_POINT('',#84587);
#10107=VERTEX_POINT('',#84803);
#10108=VERTEX_POINT('',#84804);
#10109=VERTEX_POINT('',#84812);
#10110=VERTEX_POINT('',#84817);
#10111=VERTEX_POINT('',#84852);
#10112=VERTEX_POINT('',#84853);
#10113=VERTEX_POINT('',#84861);
#10114=VERTEX_POINT('',#84866);
#10115=VERTEX_POINT('',#85288);
#10116=VERTEX_POINT('',#85483);
#10117=VERTEX_POINT('',#85699);
#10118=VERTEX_POINT('',#85700);
#10119=VERTEX_POINT('',#85708);
#10120=VERTEX_POINT('',#85713);
#10121=VERTEX_POINT('',#85748);
#10122=VERTEX_POINT('',#85749);
#10123=VERTEX_POINT('',#85757);
#10124=VERTEX_POINT('',#85762);
#10125=VERTEX_POINT('',#86184);
#10126=VERTEX_POINT('',#86379);
#10127=VERTEX_POINT('',#86595);
#10128=VERTEX_POINT('',#86596);
#10129=VERTEX_POINT('',#86604);
#10130=VERTEX_POINT('',#86609);
#10131=VERTEX_POINT('',#86644);
#10132=VERTEX_POINT('',#86645);
#10133=VERTEX_POINT('',#86653);
#10134=VERTEX_POINT('',#86658);
#10135=VERTEX_POINT('',#87080);
#10136=VERTEX_POINT('',#87275);
#10137=VERTEX_POINT('',#87491);
#10138=VERTEX_POINT('',#87492);
#10139=VERTEX_POINT('',#87500);
#10140=VERTEX_POINT('',#87505);
#10141=VERTEX_POINT('',#87540);
#10142=VERTEX_POINT('',#87541);
#10143=VERTEX_POINT('',#87549);
#10144=VERTEX_POINT('',#87554);
#10145=VERTEX_POINT('',#87976);
#10146=VERTEX_POINT('',#88171);
#10147=VERTEX_POINT('',#88387);
#10148=VERTEX_POINT('',#88388);
#10149=VERTEX_POINT('',#88396);
#10150=VERTEX_POINT('',#88401);
#10151=VERTEX_POINT('',#88436);
#10152=VERTEX_POINT('',#88437);
#10153=VERTEX_POINT('',#88445);
#10154=VERTEX_POINT('',#88450);
#10155=VERTEX_POINT('',#88872);
#10156=VERTEX_POINT('',#89067);
#10157=VERTEX_POINT('',#89283);
#10158=VERTEX_POINT('',#89284);
#10159=VERTEX_POINT('',#89292);
#10160=VERTEX_POINT('',#89297);
#10161=VERTEX_POINT('',#89332);
#10162=VERTEX_POINT('',#89333);
#10163=VERTEX_POINT('',#89341);
#10164=VERTEX_POINT('',#89346);
#10165=VERTEX_POINT('',#89768);
#10166=VERTEX_POINT('',#89963);
#10167=VERTEX_POINT('',#90179);
#10168=VERTEX_POINT('',#90180);
#10169=VERTEX_POINT('',#90188);
#10170=VERTEX_POINT('',#90193);
#10171=VERTEX_POINT('',#90228);
#10172=VERTEX_POINT('',#90229);
#10173=VERTEX_POINT('',#90237);
#10174=VERTEX_POINT('',#90242);
#10175=VERTEX_POINT('',#90664);
#10176=VERTEX_POINT('',#90859);
#10177=VERTEX_POINT('',#91075);
#10178=VERTEX_POINT('',#91076);
#10179=VERTEX_POINT('',#91084);
#10180=VERTEX_POINT('',#91089);
#10181=VERTEX_POINT('',#91124);
#10182=VERTEX_POINT('',#91125);
#10183=VERTEX_POINT('',#91133);
#10184=VERTEX_POINT('',#91138);
#10185=VERTEX_POINT('',#91560);
#10186=VERTEX_POINT('',#91755);
#10187=VERTEX_POINT('',#91971);
#10188=VERTEX_POINT('',#91972);
#10189=VERTEX_POINT('',#91980);
#10190=VERTEX_POINT('',#91985);
#10191=VERTEX_POINT('',#92020);
#10192=VERTEX_POINT('',#92021);
#10193=VERTEX_POINT('',#92029);
#10194=VERTEX_POINT('',#92034);
#10195=VERTEX_POINT('',#92456);
#10196=VERTEX_POINT('',#92651);
#10197=VERTEX_POINT('',#92867);
#10198=VERTEX_POINT('',#92868);
#10199=VERTEX_POINT('',#92876);
#10200=VERTEX_POINT('',#92881);
#10201=VERTEX_POINT('',#92916);
#10202=VERTEX_POINT('',#92917);
#10203=VERTEX_POINT('',#92925);
#10204=VERTEX_POINT('',#92930);
#10205=VERTEX_POINT('',#93352);
#10206=VERTEX_POINT('',#93547);
#10207=VERTEX_POINT('',#93763);
#10208=VERTEX_POINT('',#93764);
#10209=VERTEX_POINT('',#93772);
#10210=VERTEX_POINT('',#93777);
#10211=VERTEX_POINT('',#93812);
#10212=VERTEX_POINT('',#93813);
#10213=VERTEX_POINT('',#93821);
#10214=VERTEX_POINT('',#93826);
#10215=VERTEX_POINT('',#94248);
#10216=VERTEX_POINT('',#94443);
#10217=VERTEX_POINT('',#94659);
#10218=VERTEX_POINT('',#94660);
#10219=VERTEX_POINT('',#94668);
#10220=VERTEX_POINT('',#94673);
#10221=VERTEX_POINT('',#94708);
#10222=VERTEX_POINT('',#94709);
#10223=VERTEX_POINT('',#94717);
#10224=VERTEX_POINT('',#94722);
#10225=VERTEX_POINT('',#95144);
#10226=VERTEX_POINT('',#95339);
#10227=VERTEX_POINT('',#95555);
#10228=VERTEX_POINT('',#95556);
#10229=VERTEX_POINT('',#95564);
#10230=VERTEX_POINT('',#95569);
#10231=VERTEX_POINT('',#95604);
#10232=VERTEX_POINT('',#95605);
#10233=VERTEX_POINT('',#95613);
#10234=VERTEX_POINT('',#95618);
#10235=VERTEX_POINT('',#96040);
#10236=VERTEX_POINT('',#96235);
#10237=VERTEX_POINT('',#96451);
#10238=VERTEX_POINT('',#96452);
#10239=VERTEX_POINT('',#96460);
#10240=VERTEX_POINT('',#96465);
#10241=VERTEX_POINT('',#96500);
#10242=VERTEX_POINT('',#96501);
#10243=VERTEX_POINT('',#96509);
#10244=VERTEX_POINT('',#96514);
#10245=VERTEX_POINT('',#96936);
#10246=VERTEX_POINT('',#97131);
#10247=VERTEX_POINT('',#97347);
#10248=VERTEX_POINT('',#97348);
#10249=VERTEX_POINT('',#97356);
#10250=VERTEX_POINT('',#97361);
#10251=VERTEX_POINT('',#97396);
#10252=VERTEX_POINT('',#97397);
#10253=VERTEX_POINT('',#97405);
#10254=VERTEX_POINT('',#97410);
#10255=VERTEX_POINT('',#97832);
#10256=VERTEX_POINT('',#98027);
#10257=VERTEX_POINT('',#98243);
#10258=VERTEX_POINT('',#98244);
#10259=VERTEX_POINT('',#98252);
#10260=VERTEX_POINT('',#98257);
#10261=VERTEX_POINT('',#98292);
#10262=VERTEX_POINT('',#98293);
#10263=VERTEX_POINT('',#98301);
#10264=VERTEX_POINT('',#98306);
#10265=VERTEX_POINT('',#98728);
#10266=VERTEX_POINT('',#98923);
#10267=VERTEX_POINT('',#99139);
#10268=VERTEX_POINT('',#99140);
#10269=VERTEX_POINT('',#99148);
#10270=VERTEX_POINT('',#99153);
#10271=VERTEX_POINT('',#99188);
#10272=VERTEX_POINT('',#99189);
#10273=VERTEX_POINT('',#99197);
#10274=VERTEX_POINT('',#99202);
#10275=VERTEX_POINT('',#99624);
#10276=VERTEX_POINT('',#99819);
#10277=VERTEX_POINT('',#100035);
#10278=VERTEX_POINT('',#100036);
#10279=VERTEX_POINT('',#100044);
#10280=VERTEX_POINT('',#100049);
#10281=VERTEX_POINT('',#100084);
#10282=VERTEX_POINT('',#100085);
#10283=VERTEX_POINT('',#100093);
#10284=VERTEX_POINT('',#100098);
#10285=VERTEX_POINT('',#100520);
#10286=VERTEX_POINT('',#100715);
#10287=VERTEX_POINT('',#100931);
#10288=VERTEX_POINT('',#100932);
#10289=VERTEX_POINT('',#100940);
#10290=VERTEX_POINT('',#100945);
#10291=VERTEX_POINT('',#100980);
#10292=VERTEX_POINT('',#100981);
#10293=VERTEX_POINT('',#100989);
#10294=VERTEX_POINT('',#100994);
#10295=VERTEX_POINT('',#101416);
#10296=VERTEX_POINT('',#101611);
#10297=VERTEX_POINT('',#101827);
#10298=VERTEX_POINT('',#101828);
#10299=VERTEX_POINT('',#101836);
#10300=VERTEX_POINT('',#101841);
#10301=VERTEX_POINT('',#101876);
#10302=VERTEX_POINT('',#101877);
#10303=VERTEX_POINT('',#101885);
#10304=VERTEX_POINT('',#101890);
#10305=VERTEX_POINT('',#102312);
#10306=VERTEX_POINT('',#102507);
#10307=VERTEX_POINT('',#102723);
#10308=VERTEX_POINT('',#102724);
#10309=VERTEX_POINT('',#102732);
#10310=VERTEX_POINT('',#102737);
#10311=VERTEX_POINT('',#102772);
#10312=VERTEX_POINT('',#102773);
#10313=VERTEX_POINT('',#102781);
#10314=VERTEX_POINT('',#102786);
#10315=VERTEX_POINT('',#103208);
#10316=VERTEX_POINT('',#103403);
#10317=VERTEX_POINT('',#103619);
#10318=VERTEX_POINT('',#103620);
#10319=VERTEX_POINT('',#103628);
#10320=VERTEX_POINT('',#103633);
#10321=VERTEX_POINT('',#103668);
#10322=VERTEX_POINT('',#103669);
#10323=VERTEX_POINT('',#103677);
#10324=VERTEX_POINT('',#103682);
#10325=VERTEX_POINT('',#104104);
#10326=VERTEX_POINT('',#104299);
#10327=VERTEX_POINT('',#104515);
#10328=VERTEX_POINT('',#104516);
#10329=VERTEX_POINT('',#104524);
#10330=VERTEX_POINT('',#104529);
#10331=VERTEX_POINT('',#104564);
#10332=VERTEX_POINT('',#104565);
#10333=VERTEX_POINT('',#104573);
#10334=VERTEX_POINT('',#104578);
#10335=VERTEX_POINT('',#105000);
#10336=VERTEX_POINT('',#105195);
#10337=VERTEX_POINT('',#105411);
#10338=VERTEX_POINT('',#105412);
#10339=VERTEX_POINT('',#105420);
#10340=VERTEX_POINT('',#105425);
#10341=VERTEX_POINT('',#105460);
#10342=VERTEX_POINT('',#105461);
#10343=VERTEX_POINT('',#105469);
#10344=VERTEX_POINT('',#105474);
#10345=VERTEX_POINT('',#105896);
#10346=VERTEX_POINT('',#106091);
#10347=VERTEX_POINT('',#106307);
#10348=VERTEX_POINT('',#106308);
#10349=VERTEX_POINT('',#106316);
#10350=VERTEX_POINT('',#106321);
#10351=VERTEX_POINT('',#106356);
#10352=VERTEX_POINT('',#106357);
#10353=VERTEX_POINT('',#106365);
#10354=VERTEX_POINT('',#106370);
#10355=VERTEX_POINT('',#106792);
#10356=VERTEX_POINT('',#106987);
#10357=VERTEX_POINT('',#107203);
#10358=VERTEX_POINT('',#107204);
#10359=VERTEX_POINT('',#107212);
#10360=VERTEX_POINT('',#107217);
#10361=VERTEX_POINT('',#107252);
#10362=VERTEX_POINT('',#107253);
#10363=VERTEX_POINT('',#107261);
#10364=VERTEX_POINT('',#107266);
#10365=VERTEX_POINT('',#107688);
#10366=VERTEX_POINT('',#107883);
#10367=VERTEX_POINT('',#108099);
#10368=VERTEX_POINT('',#108100);
#10369=VERTEX_POINT('',#108108);
#10370=VERTEX_POINT('',#108113);
#10371=VERTEX_POINT('',#108148);
#10372=VERTEX_POINT('',#108149);
#10373=VERTEX_POINT('',#108157);
#10374=VERTEX_POINT('',#108162);
#10375=VERTEX_POINT('',#108584);
#10376=VERTEX_POINT('',#108779);
#10377=VERTEX_POINT('',#108995);
#10378=VERTEX_POINT('',#108996);
#10379=VERTEX_POINT('',#109004);
#10380=VERTEX_POINT('',#109009);
#10381=VERTEX_POINT('',#109044);
#10382=VERTEX_POINT('',#109045);
#10383=VERTEX_POINT('',#109053);
#10384=VERTEX_POINT('',#109058);
#10385=VERTEX_POINT('',#109480);
#10386=VERTEX_POINT('',#109675);
#10387=VERTEX_POINT('',#109891);
#10388=VERTEX_POINT('',#109892);
#10389=VERTEX_POINT('',#109900);
#10390=VERTEX_POINT('',#109905);
#10391=VERTEX_POINT('',#109940);
#10392=VERTEX_POINT('',#109941);
#10393=VERTEX_POINT('',#109949);
#10394=VERTEX_POINT('',#109954);
#10395=VERTEX_POINT('',#110376);
#10396=VERTEX_POINT('',#110571);
#10397=VERTEX_POINT('',#110787);
#10398=VERTEX_POINT('',#110788);
#10399=VERTEX_POINT('',#110796);
#10400=VERTEX_POINT('',#110801);
#10401=VERTEX_POINT('',#110836);
#10402=VERTEX_POINT('',#110837);
#10403=VERTEX_POINT('',#110845);
#10404=VERTEX_POINT('',#110850);
#10405=VERTEX_POINT('',#111272);
#10406=VERTEX_POINT('',#111467);
#10407=VERTEX_POINT('',#111683);
#10408=VERTEX_POINT('',#111684);
#10409=VERTEX_POINT('',#111692);
#10410=VERTEX_POINT('',#111697);
#10411=VERTEX_POINT('',#111732);
#10412=VERTEX_POINT('',#111733);
#10413=VERTEX_POINT('',#111741);
#10414=VERTEX_POINT('',#111746);
#10415=VERTEX_POINT('',#112168);
#10416=VERTEX_POINT('',#112363);
#10417=VERTEX_POINT('',#112579);
#10418=VERTEX_POINT('',#112580);
#10419=VERTEX_POINT('',#112588);
#10420=VERTEX_POINT('',#112593);
#10421=VERTEX_POINT('',#112628);
#10422=VERTEX_POINT('',#112629);
#10423=VERTEX_POINT('',#112637);
#10424=VERTEX_POINT('',#112642);
#10425=VERTEX_POINT('',#113064);
#10426=VERTEX_POINT('',#113259);
#10427=VERTEX_POINT('',#113475);
#10428=VERTEX_POINT('',#113476);
#10429=VERTEX_POINT('',#113484);
#10430=VERTEX_POINT('',#113489);
#10431=VERTEX_POINT('',#113524);
#10432=VERTEX_POINT('',#113525);
#10433=VERTEX_POINT('',#113533);
#10434=VERTEX_POINT('',#113538);
#10435=VERTEX_POINT('',#113960);
#10436=VERTEX_POINT('',#114155);
#10437=VERTEX_POINT('',#114371);
#10438=VERTEX_POINT('',#114372);
#10439=VERTEX_POINT('',#114380);
#10440=VERTEX_POINT('',#114385);
#10441=VERTEX_POINT('',#114420);
#10442=VERTEX_POINT('',#114421);
#10443=VERTEX_POINT('',#114429);
#10444=VERTEX_POINT('',#114434);
#10445=VERTEX_POINT('',#114856);
#10446=VERTEX_POINT('',#115051);
#10447=VERTEX_POINT('',#115267);
#10448=VERTEX_POINT('',#115268);
#10449=VERTEX_POINT('',#115276);
#10450=VERTEX_POINT('',#115281);
#10451=VERTEX_POINT('',#115316);
#10452=VERTEX_POINT('',#115317);
#10453=VERTEX_POINT('',#115325);
#10454=VERTEX_POINT('',#115330);
#10455=VERTEX_POINT('',#115752);
#10456=VERTEX_POINT('',#115947);
#10457=VERTEX_POINT('',#116163);
#10458=VERTEX_POINT('',#116164);
#10459=VERTEX_POINT('',#116172);
#10460=VERTEX_POINT('',#116177);
#10461=VERTEX_POINT('',#116602);
#10462=VERTEX_POINT('',#116797);
#10463=VERTEX_POINT('',#117403);
#10464=VERTEX_POINT('',#117598);
#10465=VERTEX_POINT('',#118204);
#10466=VERTEX_POINT('',#118399);
#10467=VERTEX_POINT('',#119005);
#10468=VERTEX_POINT('',#119200);
#10469=VERTEX_POINT('',#119806);
#10470=VERTEX_POINT('',#120001);
#10471=VERTEX_POINT('',#120607);
#10472=VERTEX_POINT('',#120802);
#10473=VERTEX_POINT('',#121408);
#10474=VERTEX_POINT('',#121603);
#10475=VERTEX_POINT('',#122209);
#10476=VERTEX_POINT('',#122404);
#10477=VERTEX_POINT('',#123010);
#10478=VERTEX_POINT('',#123205);
#10479=VERTEX_POINT('',#123811);
#10480=VERTEX_POINT('',#124006);
#10481=VERTEX_POINT('',#124612);
#10482=VERTEX_POINT('',#124807);
#10483=VERTEX_POINT('',#125413);
#10484=VERTEX_POINT('',#125608);
#10485=VERTEX_POINT('',#126214);
#10486=VERTEX_POINT('',#126409);
#10487=VERTEX_POINT('',#127015);
#10488=VERTEX_POINT('',#127210);
#10489=VERTEX_POINT('',#127816);
#10490=VERTEX_POINT('',#128011);
#10491=VERTEX_POINT('',#128617);
#10492=VERTEX_POINT('',#128812);
#10493=VERTEX_POINT('',#129418);
#10494=VERTEX_POINT('',#129613);
#10495=VERTEX_POINT('',#130219);
#10496=VERTEX_POINT('',#130414);
#10497=VERTEX_POINT('',#131020);
#10498=VERTEX_POINT('',#131215);
#10499=VERTEX_POINT('',#131821);
#10500=VERTEX_POINT('',#132016);
#10501=VERTEX_POINT('',#132622);
#10502=VERTEX_POINT('',#132817);
#10503=VERTEX_POINT('',#133423);
#10504=VERTEX_POINT('',#133618);
#10505=VERTEX_POINT('',#134224);
#10506=VERTEX_POINT('',#134419);
#10507=VERTEX_POINT('',#135025);
#10508=VERTEX_POINT('',#135220);
#10509=VERTEX_POINT('',#135826);
#10510=VERTEX_POINT('',#136021);
#10511=VERTEX_POINT('',#136627);
#10512=VERTEX_POINT('',#136822);
#10513=VERTEX_POINT('',#137428);
#10514=VERTEX_POINT('',#137623);
#10515=VERTEX_POINT('',#138229);
#10516=VERTEX_POINT('',#138424);
#10517=VERTEX_POINT('',#139030);
#10518=VERTEX_POINT('',#139225);
#10519=VERTEX_POINT('',#139831);
#10520=VERTEX_POINT('',#140026);
#10521=VERTEX_POINT('',#140632);
#10522=VERTEX_POINT('',#140827);
#10523=VERTEX_POINT('',#141433);
#10524=VERTEX_POINT('',#141628);
#10525=VERTEX_POINT('',#142234);
#10526=VERTEX_POINT('',#142429);
#10527=VERTEX_POINT('',#143035);
#10528=VERTEX_POINT('',#143230);
#10529=VERTEX_POINT('',#143836);
#10530=VERTEX_POINT('',#144031);
#10531=VERTEX_POINT('',#144637);
#10532=VERTEX_POINT('',#144832);
#10533=VERTEX_POINT('',#145438);
#10534=VERTEX_POINT('',#145633);
#10535=VERTEX_POINT('',#146239);
#10536=VERTEX_POINT('',#146434);
#10537=VERTEX_POINT('',#147040);
#10538=VERTEX_POINT('',#147235);
#10539=VERTEX_POINT('',#147841);
#10540=VERTEX_POINT('',#148036);
#10541=VERTEX_POINT('',#148642);
#10542=VERTEX_POINT('',#148837);
#10543=VERTEX_POINT('',#149443);
#10544=VERTEX_POINT('',#149638);
#10545=VERTEX_POINT('',#150244);
#10546=VERTEX_POINT('',#150439);
#10547=VERTEX_POINT('',#151045);
#10548=VERTEX_POINT('',#151240);
#10549=VERTEX_POINT('',#151846);
#10550=VERTEX_POINT('',#152041);
#10551=VERTEX_POINT('',#152647);
#10552=VERTEX_POINT('',#152842);
#10553=VERTEX_POINT('',#153448);
#10554=VERTEX_POINT('',#153643);
#10555=VERTEX_POINT('',#154249);
#10556=VERTEX_POINT('',#154444);
#10557=VERTEX_POINT('',#155050);
#10558=VERTEX_POINT('',#155245);
#10559=VERTEX_POINT('',#155851);
#10560=VERTEX_POINT('',#156046);
#10561=VERTEX_POINT('',#156652);
#10562=VERTEX_POINT('',#156847);
#10563=VERTEX_POINT('',#157453);
#10564=VERTEX_POINT('',#157648);
#10565=VERTEX_POINT('',#158254);
#10566=VERTEX_POINT('',#158449);
#10567=VERTEX_POINT('',#159055);
#10568=VERTEX_POINT('',#159250);
#10569=VERTEX_POINT('',#159856);
#10570=VERTEX_POINT('',#160051);
#10571=VERTEX_POINT('',#160657);
#10572=VERTEX_POINT('',#160852);
#10573=VERTEX_POINT('',#161458);
#10574=VERTEX_POINT('',#161653);
#10575=VERTEX_POINT('',#162259);
#10576=VERTEX_POINT('',#162454);
#10577=VERTEX_POINT('',#163060);
#10578=VERTEX_POINT('',#163255);
#10579=VERTEX_POINT('',#163861);
#10580=VERTEX_POINT('',#164056);
#10581=VERTEX_POINT('',#164662);
#10582=VERTEX_POINT('',#164857);
#10583=VERTEX_POINT('',#165463);
#10584=VERTEX_POINT('',#165658);
#10585=VERTEX_POINT('',#166264);
#10586=VERTEX_POINT('',#166459);
#10587=VERTEX_POINT('',#167065);
#10588=VERTEX_POINT('',#167260);
#10589=VERTEX_POINT('',#167866);
#10590=VERTEX_POINT('',#168061);
#10591=VERTEX_POINT('',#168667);
#10592=VERTEX_POINT('',#168862);
#10593=VERTEX_POINT('',#169468);
#10594=VERTEX_POINT('',#169663);
#10595=VERTEX_POINT('',#170269);
#10596=VERTEX_POINT('',#170464);
#10597=VERTEX_POINT('',#171070);
#10598=VERTEX_POINT('',#171265);
#10599=VERTEX_POINT('',#171871);
#10600=VERTEX_POINT('',#172066);
#10601=VERTEX_POINT('',#172672);
#10602=VERTEX_POINT('',#172867);
#10603=VERTEX_POINT('',#173064);
#10604=VERTEX_POINT('',#173066);
#10605=VERTEX_POINT('',#173277);
#10606=VERTEX_POINT('',#173279);
#10607=VERTEX_POINT('',#173302);
#10608=VERTEX_POINT('',#173303);
#10609=VERTEX_POINT('',#173311);
#10610=VERTEX_POINT('',#173316);
#10611=VERTEX_POINT('',#174146);
#10612=VERTEX_POINT('',#174147);
#10613=VERTEX_POINT('',#174155);
#10614=VERTEX_POINT('',#174160);
#10615=VERTEX_POINT('',#174974);
#10616=VERTEX_POINT('',#174981);
#10617=VERTEX_POINT('',#174987);
#10618=VERTEX_POINT('',#174988);
#10619=VERTEX_POINT('',#174990);
#10620=VERTEX_POINT('',#174992);
#10621=VERTEX_POINT('',#174996);
#10622=VERTEX_POINT('',#174997);
#10623=VERTEX_POINT('',#174999);
#10624=VERTEX_POINT('',#175001);
#10625=VERTEX_POINT('',#175011);
#10626=VERTEX_POINT('',#175012);
#10627=VERTEX_POINT('',#175218);
#10628=VERTEX_POINT('',#175220);
#10629=VERTEX_POINT('',#175426);
#10630=VERTEX_POINT('',#175428);
#10631=VERTEX_POINT('',#175430);
#10632=VERTEX_POINT('',#175432);
#10633=VERTEX_POINT('',#175434);
#10634=VERTEX_POINT('',#175436);
#10635=VERTEX_POINT('',#175642);
#10636=VERTEX_POINT('',#175644);
#10637=VERTEX_POINT('',#175850);
#10638=VERTEX_POINT('',#175852);
#10639=VERTEX_POINT('',#175854);
#10640=VERTEX_POINT('',#175856);
#10641=VERTEX_POINT('',#175858);
#10642=VERTEX_POINT('',#175860);
#10643=VERTEX_POINT('',#176066);
#10644=VERTEX_POINT('',#176068);
#10645=VERTEX_POINT('',#176274);
#10646=VERTEX_POINT('',#176276);
#10647=VERTEX_POINT('',#176278);
#10648=VERTEX_POINT('',#176280);
#10649=VERTEX_POINT('',#176282);
#10650=VERTEX_POINT('',#176284);
#10651=VERTEX_POINT('',#176490);
#10652=VERTEX_POINT('',#176492);
#10653=VERTEX_POINT('',#176698);
#10654=VERTEX_POINT('',#176700);
#10655=VERTEX_POINT('',#176702);
#10656=VERTEX_POINT('',#176704);
#10657=VERTEX_POINT('',#176706);
#10658=VERTEX_POINT('',#176708);
#10659=VERTEX_POINT('',#176914);
#10660=VERTEX_POINT('',#176916);
#10661=VERTEX_POINT('',#177122);
#10662=VERTEX_POINT('',#177124);
#10663=VERTEX_POINT('',#177126);
#10664=VERTEX_POINT('',#177128);
#10665=VERTEX_POINT('',#177130);
#10666=VERTEX_POINT('',#177132);
#10667=VERTEX_POINT('',#177338);
#10668=VERTEX_POINT('',#177340);
#10669=VERTEX_POINT('',#177546);
#10670=VERTEX_POINT('',#177548);
#10671=VERTEX_POINT('',#177550);
#10672=VERTEX_POINT('',#177552);
#10673=VERTEX_POINT('',#177554);
#10674=VERTEX_POINT('',#177556);
#10675=VERTEX_POINT('',#177762);
#10676=VERTEX_POINT('',#177764);
#10677=VERTEX_POINT('',#177970);
#10678=VERTEX_POINT('',#177972);
#10679=VERTEX_POINT('',#177974);
#10680=VERTEX_POINT('',#177976);
#10681=VERTEX_POINT('',#177978);
#10682=VERTEX_POINT('',#177980);
#10683=VERTEX_POINT('',#178186);
#10684=VERTEX_POINT('',#178188);
#10685=VERTEX_POINT('',#178394);
#10686=VERTEX_POINT('',#178396);
#10687=VERTEX_POINT('',#178398);
#10688=VERTEX_POINT('',#178400);
#10689=VERTEX_POINT('',#178402);
#10690=VERTEX_POINT('',#178404);
#10691=VERTEX_POINT('',#178610);
#10692=VERTEX_POINT('',#178612);
#10693=VERTEX_POINT('',#178818);
#10694=VERTEX_POINT('',#178820);
#10695=VERTEX_POINT('',#178822);
#10696=VERTEX_POINT('',#178824);
#10697=VERTEX_POINT('',#178826);
#10698=VERTEX_POINT('',#178828);
#10699=VERTEX_POINT('',#179034);
#10700=VERTEX_POINT('',#179036);
#10701=VERTEX_POINT('',#179242);
#10702=VERTEX_POINT('',#179244);
#10703=VERTEX_POINT('',#179246);
#10704=VERTEX_POINT('',#179248);
#10705=VERTEX_POINT('',#179250);
#10706=VERTEX_POINT('',#179252);
#10707=VERTEX_POINT('',#179458);
#10708=VERTEX_POINT('',#179460);
#10709=VERTEX_POINT('',#179666);
#10710=VERTEX_POINT('',#179668);
#10711=VERTEX_POINT('',#179670);
#10712=VERTEX_POINT('',#179672);
#10713=VERTEX_POINT('',#179674);
#10714=VERTEX_POINT('',#179676);
#10715=VERTEX_POINT('',#179882);
#10716=VERTEX_POINT('',#179884);
#10717=VERTEX_POINT('',#180090);
#10718=VERTEX_POINT('',#180092);
#10719=VERTEX_POINT('',#180094);
#10720=VERTEX_POINT('',#180096);
#10721=VERTEX_POINT('',#180098);
#10722=VERTEX_POINT('',#180100);
#10723=VERTEX_POINT('',#180306);
#10724=VERTEX_POINT('',#180308);
#10725=VERTEX_POINT('',#180514);
#10726=VERTEX_POINT('',#180516);
#10727=VERTEX_POINT('',#180518);
#10728=VERTEX_POINT('',#180520);
#10729=VERTEX_POINT('',#180522);
#10730=VERTEX_POINT('',#180524);
#10731=VERTEX_POINT('',#180730);
#10732=VERTEX_POINT('',#180732);
#10733=VERTEX_POINT('',#180938);
#10734=VERTEX_POINT('',#180940);
#10735=VERTEX_POINT('',#180942);
#10736=VERTEX_POINT('',#180944);
#10737=VERTEX_POINT('',#180946);
#10738=VERTEX_POINT('',#180948);
#10739=VERTEX_POINT('',#181154);
#10740=VERTEX_POINT('',#181156);
#10741=VERTEX_POINT('',#181362);
#10742=VERTEX_POINT('',#181364);
#10743=VERTEX_POINT('',#181366);
#10744=VERTEX_POINT('',#181368);
#10745=VERTEX_POINT('',#181370);
#10746=VERTEX_POINT('',#181372);
#10747=VERTEX_POINT('',#181578);
#10748=VERTEX_POINT('',#181580);
#10749=VERTEX_POINT('',#181786);
#10750=VERTEX_POINT('',#181788);
#10751=VERTEX_POINT('',#181790);
#10752=VERTEX_POINT('',#181792);
#10753=VERTEX_POINT('',#181794);
#10754=VERTEX_POINT('',#181796);
#10755=VERTEX_POINT('',#182002);
#10756=VERTEX_POINT('',#182004);
#10757=VERTEX_POINT('',#182210);
#10758=VERTEX_POINT('',#182212);
#10759=VERTEX_POINT('',#182214);
#10760=VERTEX_POINT('',#182216);
#10761=VERTEX_POINT('',#182218);
#10762=VERTEX_POINT('',#182220);
#10763=VERTEX_POINT('',#182426);
#10764=VERTEX_POINT('',#182428);
#10765=VERTEX_POINT('',#182634);
#10766=VERTEX_POINT('',#182636);
#10767=VERTEX_POINT('',#182638);
#10768=VERTEX_POINT('',#182640);
#10769=VERTEX_POINT('',#182642);
#10770=VERTEX_POINT('',#182644);
#10771=VERTEX_POINT('',#182850);
#10772=VERTEX_POINT('',#182852);
#10773=VERTEX_POINT('',#183058);
#10774=VERTEX_POINT('',#183060);
#10775=VERTEX_POINT('',#183062);
#10776=VERTEX_POINT('',#183064);
#10777=VERTEX_POINT('',#183066);
#10778=VERTEX_POINT('',#183068);
#10779=VERTEX_POINT('',#183274);
#10780=VERTEX_POINT('',#183276);
#10781=VERTEX_POINT('',#183482);
#10782=VERTEX_POINT('',#183484);
#10783=VERTEX_POINT('',#183486);
#10784=VERTEX_POINT('',#183488);
#10785=VERTEX_POINT('',#183490);
#10786=VERTEX_POINT('',#183492);
#10787=VERTEX_POINT('',#183698);
#10788=VERTEX_POINT('',#183700);
#10789=VERTEX_POINT('',#183906);
#10790=VERTEX_POINT('',#183908);
#10791=VERTEX_POINT('',#183910);
#10792=VERTEX_POINT('',#183912);
#10793=VERTEX_POINT('',#183914);
#10794=VERTEX_POINT('',#183916);
#10795=VERTEX_POINT('',#184122);
#10796=VERTEX_POINT('',#184124);
#10797=VERTEX_POINT('',#184330);
#10798=VERTEX_POINT('',#184332);
#10799=VERTEX_POINT('',#184334);
#10800=VERTEX_POINT('',#184336);
#10801=VERTEX_POINT('',#184338);
#10802=VERTEX_POINT('',#184340);
#10803=VERTEX_POINT('',#184546);
#10804=VERTEX_POINT('',#184548);
#10805=VERTEX_POINT('',#184754);
#10806=VERTEX_POINT('',#184756);
#10807=VERTEX_POINT('',#184758);
#10808=VERTEX_POINT('',#184760);
#10809=VERTEX_POINT('',#184762);
#10810=VERTEX_POINT('',#184764);
#10811=VERTEX_POINT('',#184970);
#10812=VERTEX_POINT('',#184972);
#10813=VERTEX_POINT('',#185178);
#10814=VERTEX_POINT('',#185180);
#10815=VERTEX_POINT('',#185182);
#10816=VERTEX_POINT('',#185184);
#10817=VERTEX_POINT('',#185188);
#10818=VERTEX_POINT('',#185189);
#10819=VERTEX_POINT('',#185194);
#10820=VERTEX_POINT('',#185198);
#10821=VERTEX_POINT('',#185199);
#10822=VERTEX_POINT('',#185206);
#10823=VERTEX_POINT('',#185207);
#10824=VERTEX_POINT('',#185212);
#10825=VERTEX_POINT('',#185216);
#10826=VERTEX_POINT('',#185217);
#10827=VERTEX_POINT('',#185224);
#10828=VERTEX_POINT('',#185225);
#10829=VERTEX_POINT('',#185230);
#10830=VERTEX_POINT('',#185234);
#10831=VERTEX_POINT('',#185235);
#10832=VERTEX_POINT('',#185242);
#10833=VERTEX_POINT('',#185243);
#10834=VERTEX_POINT('',#185248);
#10835=VERTEX_POINT('',#185252);
#10836=VERTEX_POINT('',#185253);
#10837=VERTEX_POINT('',#185260);
#10838=VERTEX_POINT('',#185261);
#10839=VERTEX_POINT('',#185266);
#10840=VERTEX_POINT('',#185270);
#10841=VERTEX_POINT('',#185271);
#10842=VERTEX_POINT('',#185278);
#10843=VERTEX_POINT('',#185279);
#10844=VERTEX_POINT('',#185284);
#10845=VERTEX_POINT('',#185288);
#10846=VERTEX_POINT('',#185289);
#10847=VERTEX_POINT('',#185296);
#10848=VERTEX_POINT('',#185297);
#10849=VERTEX_POINT('',#185302);
#10850=VERTEX_POINT('',#185306);
#10851=VERTEX_POINT('',#185307);
#10852=VERTEX_POINT('',#185314);
#10853=VERTEX_POINT('',#185315);
#10854=VERTEX_POINT('',#185320);
#10855=VERTEX_POINT('',#185324);
#10856=VERTEX_POINT('',#185325);
#10857=VERTEX_POINT('',#185332);
#10858=VERTEX_POINT('',#185333);
#10859=VERTEX_POINT('',#185338);
#10860=VERTEX_POINT('',#185342);
#10861=VERTEX_POINT('',#185343);
#10862=VERTEX_POINT('',#185350);
#10863=VERTEX_POINT('',#185351);
#10864=VERTEX_POINT('',#185356);
#10865=VERTEX_POINT('',#185360);
#10866=VERTEX_POINT('',#185361);
#10867=VERTEX_POINT('',#185368);
#10868=VERTEX_POINT('',#185369);
#10869=VERTEX_POINT('',#185374);
#10870=VERTEX_POINT('',#185378);
#10871=VERTEX_POINT('',#185379);
#10872=VERTEX_POINT('',#185386);
#10873=VERTEX_POINT('',#185387);
#10874=VERTEX_POINT('',#185392);
#10875=VERTEX_POINT('',#185396);
#10876=VERTEX_POINT('',#185397);
#10877=VERTEX_POINT('',#185404);
#10878=VERTEX_POINT('',#185405);
#10879=VERTEX_POINT('',#185410);
#10880=VERTEX_POINT('',#185414);
#10881=VERTEX_POINT('',#185415);
#10882=VERTEX_POINT('',#185422);
#10883=VERTEX_POINT('',#185423);
#10884=VERTEX_POINT('',#185428);
#10885=VERTEX_POINT('',#185432);
#10886=VERTEX_POINT('',#185433);
#10887=VERTEX_POINT('',#185440);
#10888=VERTEX_POINT('',#185441);
#10889=VERTEX_POINT('',#185446);
#10890=VERTEX_POINT('',#185450);
#10891=VERTEX_POINT('',#185451);
#10892=VERTEX_POINT('',#185458);
#10893=VERTEX_POINT('',#185459);
#10894=VERTEX_POINT('',#185464);
#10895=VERTEX_POINT('',#185468);
#10896=VERTEX_POINT('',#185469);
#10897=VERTEX_POINT('',#185476);
#10898=VERTEX_POINT('',#185477);
#10899=VERTEX_POINT('',#185482);
#10900=VERTEX_POINT('',#185486);
#10901=VERTEX_POINT('',#185487);
#10902=VERTEX_POINT('',#185494);
#10903=VERTEX_POINT('',#185495);
#10904=VERTEX_POINT('',#185500);
#10905=VERTEX_POINT('',#185504);
#10906=VERTEX_POINT('',#185505);
#10907=VERTEX_POINT('',#185512);
#10908=VERTEX_POINT('',#185513);
#10909=VERTEX_POINT('',#185518);
#10910=VERTEX_POINT('',#185522);
#10911=VERTEX_POINT('',#185523);
#10912=VERTEX_POINT('',#185530);
#10913=VERTEX_POINT('',#185531);
#10914=VERTEX_POINT('',#185536);
#10915=VERTEX_POINT('',#185540);
#10916=VERTEX_POINT('',#185541);
#10917=VERTEX_POINT('',#185548);
#10918=VERTEX_POINT('',#185549);
#10919=VERTEX_POINT('',#185554);
#10920=VERTEX_POINT('',#185558);
#10921=VERTEX_POINT('',#185559);
#10922=VERTEX_POINT('',#185566);
#10923=VERTEX_POINT('',#185567);
#10924=VERTEX_POINT('',#185572);
#10925=VERTEX_POINT('',#185576);
#10926=VERTEX_POINT('',#185577);
#10927=VERTEX_POINT('',#185584);
#10928=VERTEX_POINT('',#185585);
#10929=VERTEX_POINT('',#185590);
#10930=VERTEX_POINT('',#185594);
#10931=VERTEX_POINT('',#185595);
#10932=VERTEX_POINT('',#185602);
#10933=VERTEX_POINT('',#186015);
#10934=VERTEX_POINT('',#186632);
#10935=VERTEX_POINT('',#186840);
#10936=VERTEX_POINT('',#187253);
#10937=VERTEX_POINT('',#187870);
#10938=VERTEX_POINT('',#188078);
#10939=VERTEX_POINT('',#188491);
#10940=VERTEX_POINT('',#189108);
#10941=VERTEX_POINT('',#189316);
#10942=VERTEX_POINT('',#189729);
#10943=VERTEX_POINT('',#190346);
#10944=VERTEX_POINT('',#190554);
#10945=VERTEX_POINT('',#190967);
#10946=VERTEX_POINT('',#191584);
#10947=VERTEX_POINT('',#191792);
#10948=VERTEX_POINT('',#192205);
#10949=VERTEX_POINT('',#192822);
#10950=VERTEX_POINT('',#193030);
#10951=VERTEX_POINT('',#193443);
#10952=VERTEX_POINT('',#194060);
#10953=VERTEX_POINT('',#194268);
#10954=VERTEX_POINT('',#194681);
#10955=VERTEX_POINT('',#195298);
#10956=VERTEX_POINT('',#195506);
#10957=VERTEX_POINT('',#195919);
#10958=VERTEX_POINT('',#196536);
#10959=VERTEX_POINT('',#196744);
#10960=VERTEX_POINT('',#197157);
#10961=VERTEX_POINT('',#197774);
#10962=VERTEX_POINT('',#197982);
#10963=VERTEX_POINT('',#198395);
#10964=VERTEX_POINT('',#199012);
#10965=VERTEX_POINT('',#199220);
#10966=VERTEX_POINT('',#199633);
#10967=VERTEX_POINT('',#200250);
#10968=VERTEX_POINT('',#200458);
#10969=VERTEX_POINT('',#200871);
#10970=VERTEX_POINT('',#201488);
#10971=VERTEX_POINT('',#201696);
#10972=VERTEX_POINT('',#202109);
#10973=VERTEX_POINT('',#202726);
#10974=VERTEX_POINT('',#202934);
#10975=VERTEX_POINT('',#203347);
#10976=VERTEX_POINT('',#203964);
#10977=VERTEX_POINT('',#204172);
#10978=VERTEX_POINT('',#204585);
#10979=VERTEX_POINT('',#205202);
#10980=VERTEX_POINT('',#205410);
#10981=VERTEX_POINT('',#205823);
#10982=VERTEX_POINT('',#206440);
#10983=VERTEX_POINT('',#206648);
#10984=VERTEX_POINT('',#207061);
#10985=VERTEX_POINT('',#207678);
#10986=VERTEX_POINT('',#207886);
#10987=VERTEX_POINT('',#208299);
#10988=VERTEX_POINT('',#208916);
#10989=VERTEX_POINT('',#209124);
#10990=VERTEX_POINT('',#209537);
#10991=VERTEX_POINT('',#210154);
#10992=VERTEX_POINT('',#210362);
#10993=VERTEX_POINT('',#210775);
#10994=VERTEX_POINT('',#211392);
#10995=VERTEX_POINT('',#211600);
#10996=VERTEX_POINT('',#212013);
#10997=VERTEX_POINT('',#212630);
#10998=VERTEX_POINT('',#212838);
#10999=VERTEX_POINT('',#213251);
#11000=VERTEX_POINT('',#213868);
#11001=VERTEX_POINT('',#214098);
#11002=VERTEX_POINT('',#214100);
#11003=VERTEX_POINT('',#214306);
#11004=VERTEX_POINT('',#214308);
#11005=VERTEX_POINT('',#214310);
#11006=VERTEX_POINT('',#214312);
#11007=VERTEX_POINT('',#214314);
#11008=VERTEX_POINT('',#214316);
#11009=VERTEX_POINT('',#215382);
#11010=VERTEX_POINT('',#215383);
#11011=VERTEX_POINT('',#215385);
#11012=VERTEX_POINT('',#215387);
#11013=VERTEX_POINT('',#215391);
#11014=VERTEX_POINT('',#215393);
#11015=VERTEX_POINT('',#215397);
#11016=VERTEX_POINT('',#215398);
#11017=VERTEX_POINT('',#215400);
#11018=VERTEX_POINT('',#215402);
#11019=VERTEX_POINT('',#215409);
#11020=VERTEX_POINT('',#215410);
#11021=VERTEX_POINT('',#215412);
#11022=VERTEX_POINT('',#215414);
#11023=VERTEX_POINT('',#215418);
#11024=VERTEX_POINT('',#215420);
#11025=VERTEX_POINT('',#215424);
#11026=VERTEX_POINT('',#215425);
#11027=VERTEX_POINT('',#215427);
#11028=VERTEX_POINT('',#215429);
#11029=VERTEX_POINT('',#215436);
#11030=VERTEX_POINT('',#215437);
#11031=VERTEX_POINT('',#215439);
#11032=VERTEX_POINT('',#215441);
#11033=VERTEX_POINT('',#215445);
#11034=VERTEX_POINT('',#215447);
#11035=VERTEX_POINT('',#215451);
#11036=VERTEX_POINT('',#215452);
#11037=VERTEX_POINT('',#215454);
#11038=VERTEX_POINT('',#215456);
#11039=VERTEX_POINT('',#215463);
#11040=VERTEX_POINT('',#215464);
#11041=VERTEX_POINT('',#215466);
#11042=VERTEX_POINT('',#215468);
#11043=VERTEX_POINT('',#215472);
#11044=VERTEX_POINT('',#215474);
#11045=VERTEX_POINT('',#215478);
#11046=VERTEX_POINT('',#215479);
#11047=VERTEX_POINT('',#215481);
#11048=VERTEX_POINT('',#215483);
#11049=VERTEX_POINT('',#215490);
#11050=VERTEX_POINT('',#215491);
#11051=VERTEX_POINT('',#215493);
#11052=VERTEX_POINT('',#215495);
#11053=VERTEX_POINT('',#215499);
#11054=VERTEX_POINT('',#215501);
#11055=VERTEX_POINT('',#215505);
#11056=VERTEX_POINT('',#215506);
#11057=VERTEX_POINT('',#215508);
#11058=VERTEX_POINT('',#215510);
#11059=VERTEX_POINT('',#215517);
#11060=VERTEX_POINT('',#215518);
#11061=VERTEX_POINT('',#215520);
#11062=VERTEX_POINT('',#215522);
#11063=VERTEX_POINT('',#215526);
#11064=VERTEX_POINT('',#215528);
#11065=VERTEX_POINT('',#215532);
#11066=VERTEX_POINT('',#215533);
#11067=VERTEX_POINT('',#215535);
#11068=VERTEX_POINT('',#215537);
#11069=VERTEX_POINT('',#215544);
#11070=VERTEX_POINT('',#215545);
#11071=VERTEX_POINT('',#215547);
#11072=VERTEX_POINT('',#215549);
#11073=VERTEX_POINT('',#215553);
#11074=VERTEX_POINT('',#215555);
#11075=VERTEX_POINT('',#215559);
#11076=VERTEX_POINT('',#215560);
#11077=VERTEX_POINT('',#215562);
#11078=VERTEX_POINT('',#215564);
#11079=VERTEX_POINT('',#215571);
#11080=VERTEX_POINT('',#215572);
#11081=VERTEX_POINT('',#215574);
#11082=VERTEX_POINT('',#215576);
#11083=VERTEX_POINT('',#215580);
#11084=VERTEX_POINT('',#215582);
#11085=VERTEX_POINT('',#215586);
#11086=VERTEX_POINT('',#215587);
#11087=VERTEX_POINT('',#215589);
#11088=VERTEX_POINT('',#215591);
#11089=VERTEX_POINT('',#215598);
#11090=VERTEX_POINT('',#215599);
#11091=VERTEX_POINT('',#215601);
#11092=VERTEX_POINT('',#215603);
#11093=VERTEX_POINT('',#215607);
#11094=VERTEX_POINT('',#215609);
#11095=VERTEX_POINT('',#215613);
#11096=VERTEX_POINT('',#215614);
#11097=VERTEX_POINT('',#215616);
#11098=VERTEX_POINT('',#215618);
#11099=VERTEX_POINT('',#215625);
#11100=VERTEX_POINT('',#215626);
#11101=VERTEX_POINT('',#215628);
#11102=VERTEX_POINT('',#215630);
#11103=VERTEX_POINT('',#215634);
#11104=VERTEX_POINT('',#215636);
#11105=VERTEX_POINT('',#215640);
#11106=VERTEX_POINT('',#215641);
#11107=VERTEX_POINT('',#215643);
#11108=VERTEX_POINT('',#215645);
#11109=VERTEX_POINT('',#215652);
#11110=VERTEX_POINT('',#215653);
#11111=VERTEX_POINT('',#215655);
#11112=VERTEX_POINT('',#215657);
#11113=VERTEX_POINT('',#215661);
#11114=VERTEX_POINT('',#215663);
#11115=VERTEX_POINT('',#215667);
#11116=VERTEX_POINT('',#215668);
#11117=VERTEX_POINT('',#215670);
#11118=VERTEX_POINT('',#215672);
#11119=VERTEX_POINT('',#215679);
#11120=VERTEX_POINT('',#215680);
#11121=VERTEX_POINT('',#215682);
#11122=VERTEX_POINT('',#215684);
#11123=VERTEX_POINT('',#215688);
#11124=VERTEX_POINT('',#215690);
#11125=VERTEX_POINT('',#215694);
#11126=VERTEX_POINT('',#215695);
#11127=VERTEX_POINT('',#215697);
#11128=VERTEX_POINT('',#215699);
#11129=VERTEX_POINT('',#215706);
#11130=VERTEX_POINT('',#215707);
#11131=VERTEX_POINT('',#215709);
#11132=VERTEX_POINT('',#215711);
#11133=VERTEX_POINT('',#215715);
#11134=VERTEX_POINT('',#215717);
#11135=VERTEX_POINT('',#215721);
#11136=VERTEX_POINT('',#215722);
#11137=VERTEX_POINT('',#215724);
#11138=VERTEX_POINT('',#215726);
#11139=VERTEX_POINT('',#215733);
#11140=VERTEX_POINT('',#215734);
#11141=VERTEX_POINT('',#215736);
#11142=VERTEX_POINT('',#215738);
#11143=VERTEX_POINT('',#215742);
#11144=VERTEX_POINT('',#215744);
#11145=VERTEX_POINT('',#215748);
#11146=VERTEX_POINT('',#215749);
#11147=VERTEX_POINT('',#215751);
#11148=VERTEX_POINT('',#215753);
#11149=VERTEX_POINT('',#215760);
#11150=VERTEX_POINT('',#215761);
#11151=VERTEX_POINT('',#215763);
#11152=VERTEX_POINT('',#215765);
#11153=VERTEX_POINT('',#215769);
#11154=VERTEX_POINT('',#215771);
#11155=VERTEX_POINT('',#215775);
#11156=VERTEX_POINT('',#215776);
#11157=VERTEX_POINT('',#215778);
#11158=VERTEX_POINT('',#215780);
#11159=VERTEX_POINT('',#215787);
#11160=VERTEX_POINT('',#215788);
#11161=VERTEX_POINT('',#215790);
#11162=VERTEX_POINT('',#215792);
#11163=VERTEX_POINT('',#215796);
#11164=VERTEX_POINT('',#215798);
#11165=VERTEX_POINT('',#215802);
#11166=VERTEX_POINT('',#215803);
#11167=VERTEX_POINT('',#215805);
#11168=VERTEX_POINT('',#215807);
#11169=VERTEX_POINT('',#215814);
#11170=VERTEX_POINT('',#215815);
#11171=VERTEX_POINT('',#215817);
#11172=VERTEX_POINT('',#215819);
#11173=VERTEX_POINT('',#215823);
#11174=VERTEX_POINT('',#215825);
#11175=VERTEX_POINT('',#215829);
#11176=VERTEX_POINT('',#215830);
#11177=VERTEX_POINT('',#215832);
#11178=VERTEX_POINT('',#215834);
#11179=VERTEX_POINT('',#215841);
#11180=VERTEX_POINT('',#215842);
#11181=VERTEX_POINT('',#215844);
#11182=VERTEX_POINT('',#215846);
#11183=VERTEX_POINT('',#215850);
#11184=VERTEX_POINT('',#215852);
#11185=VERTEX_POINT('',#215856);
#11186=VERTEX_POINT('',#215857);
#11187=VERTEX_POINT('',#215859);
#11188=VERTEX_POINT('',#215861);
#11189=VERTEX_POINT('',#215868);
#11190=VERTEX_POINT('',#215869);
#11191=VERTEX_POINT('',#215871);
#11192=VERTEX_POINT('',#215873);
#11193=VERTEX_POINT('',#215877);
#11194=VERTEX_POINT('',#215879);
#11195=VERTEX_POINT('',#215883);
#11196=VERTEX_POINT('',#215884);
#11197=VERTEX_POINT('',#215886);
#11198=VERTEX_POINT('',#215888);
#11199=VERTEX_POINT('',#215895);
#11200=VERTEX_POINT('',#215896);
#11201=VERTEX_POINT('',#215898);
#11202=VERTEX_POINT('',#215900);
#11203=VERTEX_POINT('',#215904);
#11204=VERTEX_POINT('',#215906);
#11205=VERTEX_POINT('',#215910);
#11206=VERTEX_POINT('',#215911);
#11207=VERTEX_POINT('',#215913);
#11208=VERTEX_POINT('',#215915);
#11209=VERTEX_POINT('',#215922);
#11210=VERTEX_POINT('',#215923);
#11211=VERTEX_POINT('',#215925);
#11212=VERTEX_POINT('',#215927);
#11213=VERTEX_POINT('',#215931);
#11214=VERTEX_POINT('',#215933);
#11215=VERTEX_POINT('',#215937);
#11216=VERTEX_POINT('',#215938);
#11217=VERTEX_POINT('',#215940);
#11218=VERTEX_POINT('',#215942);
#11219=VERTEX_POINT('',#215949);
#11220=VERTEX_POINT('',#215950);
#11221=VERTEX_POINT('',#215952);
#11222=VERTEX_POINT('',#215954);
#11223=VERTEX_POINT('',#215958);
#11224=VERTEX_POINT('',#215960);
#11225=VERTEX_POINT('',#215964);
#11226=VERTEX_POINT('',#215965);
#11227=VERTEX_POINT('',#215967);
#11228=VERTEX_POINT('',#215969);
#11229=VERTEX_POINT('',#215976);
#11230=VERTEX_POINT('',#215977);
#11231=VERTEX_POINT('',#215979);
#11232=VERTEX_POINT('',#215981);
#11233=VERTEX_POINT('',#215985);
#11234=VERTEX_POINT('',#215987);
#11235=VERTEX_POINT('',#215991);
#11236=VERTEX_POINT('',#215992);
#11237=VERTEX_POINT('',#215994);
#11238=VERTEX_POINT('',#215996);
#11239=VERTEX_POINT('',#216003);
#11240=VERTEX_POINT('',#216005);
#11241=VERTEX_POINT('',#216418);
#11242=VERTEX_POINT('',#216624);
#11243=VERTEX_POINT('',#217241);
#11244=VERTEX_POINT('',#217447);
#11245=VERTEX_POINT('',#217655);
#11246=VERTEX_POINT('',#217657);
#11247=VERTEX_POINT('',#218070);
#11248=VERTEX_POINT('',#218276);
#11249=VERTEX_POINT('',#218893);
#11250=VERTEX_POINT('',#219099);
#11251=VERTEX_POINT('',#219307);
#11252=VERTEX_POINT('',#219309);
#11253=VERTEX_POINT('',#219722);
#11254=VERTEX_POINT('',#219928);
#11255=VERTEX_POINT('',#220545);
#11256=VERTEX_POINT('',#220751);
#11257=VERTEX_POINT('',#220959);
#11258=VERTEX_POINT('',#220961);
#11259=VERTEX_POINT('',#221374);
#11260=VERTEX_POINT('',#221580);
#11261=VERTEX_POINT('',#222197);
#11262=VERTEX_POINT('',#222403);
#11263=VERTEX_POINT('',#222611);
#11264=VERTEX_POINT('',#222613);
#11265=VERTEX_POINT('',#223026);
#11266=VERTEX_POINT('',#223232);
#11267=VERTEX_POINT('',#223849);
#11268=VERTEX_POINT('',#224055);
#11269=VERTEX_POINT('',#224263);
#11270=VERTEX_POINT('',#224265);
#11271=VERTEX_POINT('',#224678);
#11272=VERTEX_POINT('',#224884);
#11273=VERTEX_POINT('',#225501);
#11274=VERTEX_POINT('',#225707);
#11275=VERTEX_POINT('',#225915);
#11276=VERTEX_POINT('',#225917);
#11277=VERTEX_POINT('',#226330);
#11278=VERTEX_POINT('',#226536);
#11279=VERTEX_POINT('',#227153);
#11280=VERTEX_POINT('',#227359);
#11281=VERTEX_POINT('',#227567);
#11282=VERTEX_POINT('',#227569);
#11283=VERTEX_POINT('',#227982);
#11284=VERTEX_POINT('',#228188);
#11285=VERTEX_POINT('',#228805);
#11286=VERTEX_POINT('',#229011);
#11287=VERTEX_POINT('',#229219);
#11288=VERTEX_POINT('',#229221);
#11289=VERTEX_POINT('',#229634);
#11290=VERTEX_POINT('',#229840);
#11291=VERTEX_POINT('',#230457);
#11292=VERTEX_POINT('',#230663);
#11293=VERTEX_POINT('',#230871);
#11294=VERTEX_POINT('',#230873);
#11295=VERTEX_POINT('',#231286);
#11296=VERTEX_POINT('',#231492);
#11297=VERTEX_POINT('',#232109);
#11298=VERTEX_POINT('',#232315);
#11299=VERTEX_POINT('',#232523);
#11300=VERTEX_POINT('',#232525);
#11301=VERTEX_POINT('',#232938);
#11302=VERTEX_POINT('',#233144);
#11303=VERTEX_POINT('',#233761);
#11304=VERTEX_POINT('',#233967);
#11305=VERTEX_POINT('',#234175);
#11306=VERTEX_POINT('',#234177);
#11307=VERTEX_POINT('',#234590);
#11308=VERTEX_POINT('',#234796);
#11309=VERTEX_POINT('',#235413);
#11310=VERTEX_POINT('',#235619);
#11311=VERTEX_POINT('',#235827);
#11312=VERTEX_POINT('',#235829);
#11313=VERTEX_POINT('',#236242);
#11314=VERTEX_POINT('',#236448);
#11315=VERTEX_POINT('',#237065);
#11316=VERTEX_POINT('',#237271);
#11317=VERTEX_POINT('',#237479);
#11318=VERTEX_POINT('',#237481);
#11319=VERTEX_POINT('',#237894);
#11320=VERTEX_POINT('',#238100);
#11321=VERTEX_POINT('',#238717);
#11322=VERTEX_POINT('',#238923);
#11323=VERTEX_POINT('',#239131);
#11324=VERTEX_POINT('',#239133);
#11325=VERTEX_POINT('',#239546);
#11326=VERTEX_POINT('',#239752);
#11327=VERTEX_POINT('',#240369);
#11328=VERTEX_POINT('',#240575);
#11329=VERTEX_POINT('',#240783);
#11330=VERTEX_POINT('',#240785);
#11331=VERTEX_POINT('',#241198);
#11332=VERTEX_POINT('',#241404);
#11333=VERTEX_POINT('',#242021);
#11334=VERTEX_POINT('',#242227);
#11335=VERTEX_POINT('',#242435);
#11336=VERTEX_POINT('',#242437);
#11337=VERTEX_POINT('',#242850);
#11338=VERTEX_POINT('',#243056);
#11339=VERTEX_POINT('',#243673);
#11340=VERTEX_POINT('',#243879);
#11341=VERTEX_POINT('',#244087);
#11342=VERTEX_POINT('',#244089);
#11343=VERTEX_POINT('',#244502);
#11344=VERTEX_POINT('',#244708);
#11345=VERTEX_POINT('',#245325);
#11346=VERTEX_POINT('',#245531);
#11347=VERTEX_POINT('',#245739);
#11348=VERTEX_POINT('',#245741);
#11349=VERTEX_POINT('',#246154);
#11350=VERTEX_POINT('',#246360);
#11351=VERTEX_POINT('',#246977);
#11352=VERTEX_POINT('',#247183);
#11353=VERTEX_POINT('',#247391);
#11354=VERTEX_POINT('',#247393);
#11355=VERTEX_POINT('',#247806);
#11356=VERTEX_POINT('',#248012);
#11357=VERTEX_POINT('',#248629);
#11358=VERTEX_POINT('',#248835);
#11359=VERTEX_POINT('',#249043);
#11360=VERTEX_POINT('',#249045);
#11361=VERTEX_POINT('',#249458);
#11362=VERTEX_POINT('',#249664);
#11363=VERTEX_POINT('',#250281);
#11364=VERTEX_POINT('',#250487);
#11365=VERTEX_POINT('',#250695);
#11366=VERTEX_POINT('',#250697);
#11367=VERTEX_POINT('',#251110);
#11368=VERTEX_POINT('',#251316);
#11369=VERTEX_POINT('',#251933);
#11370=VERTEX_POINT('',#252139);
#11371=VERTEX_POINT('',#252347);
#11372=VERTEX_POINT('',#252349);
#11373=VERTEX_POINT('',#252762);
#11374=VERTEX_POINT('',#252968);
#11375=VERTEX_POINT('',#253585);
#11376=VERTEX_POINT('',#253791);
#11377=VERTEX_POINT('',#254021);
#11378=VERTEX_POINT('',#254023);
#11379=VERTEX_POINT('',#254229);
#11380=VERTEX_POINT('',#254231);
#11381=VERTEX_POINT('',#254233);
#11382=VERTEX_POINT('',#254235);
#11383=VERTEX_POINT('',#254237);
#11384=VERTEX_POINT('',#254239);
#11385=VERTEX_POINT('',#254446);
#11386=VERTEX_POINT('',#254449);
#11387=VERTEX_POINT('',#254451);
#11388=VERTEX_POINT('',#254657);
#11389=VERTEX_POINT('',#254659);
#11390=VERTEX_POINT('',#254661);
#11391=VERTEX_POINT('',#254663);
#11392=VERTEX_POINT('',#254665);
#11393=VERTEX_POINT('',#254667);
#11394=VERTEX_POINT('',#254896);
#11395=VERTEX_POINT('',#255759);
#11396=VERTEX_POINT('',#255761);
#11397=VERTEX_POINT('',#255765);
#11398=VERTEX_POINT('',#255767);
#11399=VERTEX_POINT('',#255774);
#11400=VERTEX_POINT('',#255775);
#11401=VERTEX_POINT('',#255777);
#11402=VERTEX_POINT('',#255779);
#11403=VERTEX_POINT('',#255783);
#11404=VERTEX_POINT('',#255785);
#11405=VERTEX_POINT('',#255789);
#11406=VERTEX_POINT('',#255791);
#11407=VERTEX_POINT('',#255799);
#11408=VERTEX_POINT('',#255801);
#11409=VERTEX_POINT('',#255805);
#11410=VERTEX_POINT('',#255808);
#11411=VERTEX_POINT('',#255811);
#11412=VERTEX_POINT('',#255815);
#11413=VERTEX_POINT('',#255817);
#11414=VERTEX_POINT('',#255821);
#11415=VERTEX_POINT('',#255824);
#11416=VERTEX_POINT('',#255827);
#11417=VERTEX_POINT('',#255831);
#11418=VERTEX_POINT('',#255833);
#11419=VERTEX_POINT('',#255837);
#11420=VERTEX_POINT('',#255839);
#11421=VERTEX_POINT('',#255843);
#11422=VERTEX_POINT('',#255845);
#11423=VERTEX_POINT('',#255849);
#11424=VERTEX_POINT('',#255851);
#11425=VERTEX_POINT('',#255854);
#11426=VERTEX_POINT('',#255856);
#11427=VERTEX_POINT('',#255861);
#11428=VERTEX_POINT('',#255868);
#11429=VERTEX_POINT('',#255870);
#11430=VERTEX_POINT('',#255873);
#11431=VERTEX_POINT('',#255875);
#11432=VERTEX_POINT('',#255880);
#11433=VERTEX_POINT('',#255884);
#11434=VERTEX_POINT('',#255890);
#11435=VERTEX_POINT('',#255894);
#11436=VERTEX_POINT('',#255896);
#11437=VERTEX_POINT('',#255903);
#11438=VERTEX_POINT('',#255904);
#11439=VERTEX_POINT('',#255906);
#11440=VERTEX_POINT('',#255908);
#11441=VERTEX_POINT('',#255912);
#11442=VERTEX_POINT('',#255914);
#11443=VERTEX_POINT('',#255918);
#11444=VERTEX_POINT('',#255920);
#11445=VERTEX_POINT('',#255930);
#11446=VERTEX_POINT('',#255932);
#11447=VERTEX_POINT('',#255936);
#11448=VERTEX_POINT('',#255938);
#11449=VERTEX_POINT('',#255945);
#11450=VERTEX_POINT('',#255947);
#11451=VERTEX_POINT('',#255951);
#11452=VERTEX_POINT('',#255954);
#11453=VERTEX_POINT('',#255957);
#11454=VERTEX_POINT('',#255961);
#11455=VERTEX_POINT('',#255963);
#11456=VERTEX_POINT('',#255966);
#11457=VERTEX_POINT('',#255975);
#11458=VERTEX_POINT('',#255976);
#11459=VERTEX_POINT('',#255978);
#11460=VERTEX_POINT('',#255980);
#11461=VERTEX_POINT('',#255984);
#11462=VERTEX_POINT('',#255985);
#11463=VERTEX_POINT('',#255987);
#11464=VERTEX_POINT('',#255989);
#11465=VERTEX_POINT('',#256002);
#11466=VERTEX_POINT('',#256004);
#11467=VERTEX_POINT('',#256008);
#11468=VERTEX_POINT('',#256010);
#11469=VERTEX_POINT('',#256017);
#11470=VERTEX_POINT('',#256019);
#11471=VERTEX_POINT('',#256023);
#11472=VERTEX_POINT('',#256025);
#11473=VERTEX_POINT('',#256032);
#11474=VERTEX_POINT('',#256034);
#11475=VERTEX_POINT('',#256038);
#11476=VERTEX_POINT('',#256040);
#11477=VERTEX_POINT('',#256047);
#11478=VERTEX_POINT('',#256048);
#11479=VERTEX_POINT('',#256050);
#11480=VERTEX_POINT('',#256052);
#11481=VERTEX_POINT('',#256056);
#11482=VERTEX_POINT('',#256057);
#11483=VERTEX_POINT('',#256059);
#11484=VERTEX_POINT('',#256061);
#11485=VERTEX_POINT('',#256074);
#11486=VERTEX_POINT('',#256075);
#11487=VERTEX_POINT('',#256077);
#11488=VERTEX_POINT('',#256079);
#11489=VERTEX_POINT('',#256083);
#11490=VERTEX_POINT('',#256084);
#11491=VERTEX_POINT('',#256086);
#11492=VERTEX_POINT('',#256088);
#11493=VERTEX_POINT('',#256101);
#11494=VERTEX_POINT('',#256103);
#11495=VERTEX_POINT('',#256110);
#11496=VERTEX_POINT('',#256111);
#11497=VERTEX_POINT('',#256113);
#11498=VERTEX_POINT('',#256124);
#11499=VERTEX_POINT('',#256134);
#11500=VERTEX_POINT('',#256135);
#11501=VERTEX_POINT('',#256182);
#11502=VERTEX_POINT('',#256183);
#11503=VERTEX_POINT('',#256230);
#11504=VERTEX_POINT('',#256231);
#11505=VERTEX_POINT('',#256281);
#11506=VERTEX_POINT('',#256282);
#11507=VERTEX_POINT('',#256332);
#11508=VERTEX_POINT('',#256333);
#11509=VERTEX_POINT('',#256380);
#11510=VERTEX_POINT('',#256381);
#11511=VERTEX_POINT('',#256428);
#11512=VERTEX_POINT('',#256429);
#11513=VERTEX_POINT('',#256482);
#11514=VERTEX_POINT('',#256483);
#11515=VERTEX_POINT('',#256530);
#11516=VERTEX_POINT('',#256531);
#11517=VERTEX_POINT('',#256578);
#11518=VERTEX_POINT('',#256579);
#11519=VERTEX_POINT('',#256632);
#11520=VERTEX_POINT('',#256633);
#11521=VERTEX_POINT('',#256680);
#11522=VERTEX_POINT('',#256681);
#11523=VERTEX_POINT('',#256728);
#11524=VERTEX_POINT('',#256729);
#11525=VERTEX_POINT('',#256776);
#11526=VERTEX_POINT('',#256777);
#11527=VERTEX_POINT('',#256830);
#11528=VERTEX_POINT('',#256831);
#11529=VERTEX_POINT('',#256878);
#11530=VERTEX_POINT('',#256879);
#11531=VERTEX_POINT('',#256926);
#11532=VERTEX_POINT('',#256927);
#11533=VERTEX_POINT('',#256980);
#11534=VERTEX_POINT('',#256981);
#11535=VERTEX_POINT('',#257028);
#11536=VERTEX_POINT('',#257029);
#11537=VERTEX_POINT('',#257076);
#11538=VERTEX_POINT('',#257077);
#11539=VERTEX_POINT('',#257079);
#11540=VERTEX_POINT('',#257086);
#11541=VERTEX_POINT('',#257093);
#11542=VERTEX_POINT('',#257094);
#11543=VERTEX_POINT('',#257118);
#11544=VERTEX_POINT('',#257119);
#11545=VERTEX_POINT('',#257142);
#11546=VERTEX_POINT('',#257143);
#11547=VERTEX_POINT('',#257167);
#11548=VERTEX_POINT('',#257168);
#11549=VERTEX_POINT('',#257192);
#11550=VERTEX_POINT('',#257193);
#11551=VERTEX_POINT('',#257216);
#11552=VERTEX_POINT('',#257217);
#11553=VERTEX_POINT('',#257241);
#11554=VERTEX_POINT('',#257242);
#11555=VERTEX_POINT('',#257266);
#11556=VERTEX_POINT('',#257267);
#11557=VERTEX_POINT('',#257290);
#11558=VERTEX_POINT('',#257291);
#11559=VERTEX_POINT('',#257314);
#11560=VERTEX_POINT('',#257315);
#11561=VERTEX_POINT('',#257339);
#11562=VERTEX_POINT('',#257340);
#11563=VERTEX_POINT('',#257364);
#11564=VERTEX_POINT('',#257365);
#11565=VERTEX_POINT('',#257388);
#11566=VERTEX_POINT('',#257389);
#11567=VERTEX_POINT('',#257413);
#11568=VERTEX_POINT('',#257414);
#11569=VERTEX_POINT('',#257438);
#11570=VERTEX_POINT('',#257439);
#11571=VERTEX_POINT('',#257462);
#11572=VERTEX_POINT('',#257463);
#11573=VERTEX_POINT('',#257487);
#11574=VERTEX_POINT('',#257488);
#11575=VERTEX_POINT('',#257511);
#11576=VERTEX_POINT('',#257512);
#11577=VERTEX_POINT('',#257536);
#11578=VERTEX_POINT('',#257537);
#11579=VERTEX_POINT('',#258083);
#11580=VERTEX_POINT('',#258197);
#11581=VERTEX_POINT('',#258299);
#11582=VERTEX_POINT('',#258833);
#11583=VERTEX_POINT('',#259038);
#11584=VERTEX_POINT('',#259039);
#11585=VERTEX_POINT('',#259041);
#11586=VERTEX_POINT('',#259043);
#11587=VERTEX_POINT('',#259047);
#11588=VERTEX_POINT('',#259049);
#11589=VERTEX_POINT('',#259053);
#11590=VERTEX_POINT('',#259055);
#11591=VERTEX_POINT('',#259059);
#11592=VERTEX_POINT('',#259061);
#11593=VERTEX_POINT('',#259065);
#11594=VERTEX_POINT('',#259067);
#11595=VERTEX_POINT('',#259075);
#11596=VERTEX_POINT('',#259078);
#11597=EDGE_CURVE('',#9037,#9038,#6667,.T.);
#11598=EDGE_CURVE('',#9038,#9039,#5385,.T.);
#11599=EDGE_CURVE('',#9039,#9040,#4505,.T.);
#11600=EDGE_CURVE('',#9040,#9041,#6668,.T.);
#11601=EDGE_CURVE('',#9041,#9041,#4506,.F.);
#11602=EDGE_CURVE('',#9040,#9042,#4507,.T.);
#11603=EDGE_CURVE('',#9042,#9037,#5386,.T.);
#11604=EDGE_CURVE('',#9043,#9044,#6669,.T.);
#11605=EDGE_CURVE('',#9044,#9038,#5387,.T.);
#11606=EDGE_CURVE('',#9037,#9043,#5388,.T.);
#11607=EDGE_CURVE('',#9045,#9046,#6670,.T.);
#11608=EDGE_CURVE('',#9046,#9044,#5389,.T.);
#11609=EDGE_CURVE('',#9043,#9045,#5390,.T.);
#11610=EDGE_CURVE('',#9047,#9048,#6671,.T.);
#11611=EDGE_CURVE('',#9048,#9046,#5391,.T.);
#11612=EDGE_CURVE('',#9045,#9047,#5392,.T.);
#11613=EDGE_CURVE('',#9049,#9050,#6672,.T.);
#11614=EDGE_CURVE('',#9050,#9048,#5393,.T.);
#11615=EDGE_CURVE('',#9047,#9049,#5394,.T.);
#11616=EDGE_CURVE('',#9051,#9052,#6673,.T.);
#11617=EDGE_CURVE('',#9052,#9050,#5395,.T.);
#11618=EDGE_CURVE('',#9049,#9051,#5396,.T.);
#11619=EDGE_CURVE('',#9053,#9054,#6674,.T.);
#11620=EDGE_CURVE('',#9054,#9052,#5397,.T.);
#11621=EDGE_CURVE('',#9051,#9053,#5398,.T.);
#11622=EDGE_CURVE('',#9055,#9056,#6675,.T.);
#11623=EDGE_CURVE('',#9056,#9054,#5399,.T.);
#11624=EDGE_CURVE('',#9053,#9055,#5400,.T.);
#11625=EDGE_CURVE('',#9057,#9058,#6676,.T.);
#11626=EDGE_CURVE('',#9058,#9056,#5401,.T.);
#11627=EDGE_CURVE('',#9055,#9057,#5402,.T.);
#11628=EDGE_CURVE('',#9059,#9060,#6677,.T.);
#11629=EDGE_CURVE('',#9060,#9058,#5403,.T.);
#11630=EDGE_CURVE('',#9057,#9059,#5404,.T.);
#11631=EDGE_CURVE('',#9061,#9062,#6678,.T.);
#11632=EDGE_CURVE('',#9062,#9060,#5405,.T.);
#11633=EDGE_CURVE('',#9059,#9061,#5406,.T.);
#11634=EDGE_CURVE('',#9063,#9064,#6679,.T.);
#11635=EDGE_CURVE('',#9064,#9062,#5407,.T.);
#11636=EDGE_CURVE('',#9061,#9063,#5408,.T.);
#11637=EDGE_CURVE('',#9065,#9066,#6680,.T.);
#11638=EDGE_CURVE('',#9066,#9064,#5409,.T.);
#11639=EDGE_CURVE('',#9063,#9065,#5410,.T.);
#11640=EDGE_CURVE('',#9067,#9068,#6681,.T.);
#11641=EDGE_CURVE('',#9068,#9066,#5411,.T.);
#11642=EDGE_CURVE('',#9065,#9067,#5412,.T.);
#11643=EDGE_CURVE('',#9069,#9070,#6682,.T.);
#11644=EDGE_CURVE('',#9069,#9071,#5413,.T.);
#11645=EDGE_CURVE('',#9072,#9071,#4508,.T.);
#11646=EDGE_CURVE('',#9072,#9070,#5414,.T.);
#11647=EDGE_CURVE('',#9073,#9074,#6683,.T.);
#11648=EDGE_CURVE('',#9074,#9075,#5415,.T.);
#11649=EDGE_CURVE('',#9076,#9075,#4509,.T.);
#11650=EDGE_CURVE('',#9073,#9076,#5416,.T.);
#11651=EDGE_CURVE('',#9077,#9078,#6684,.T.);
#11652=EDGE_CURVE('',#9078,#9074,#5417,.T.);
#11653=EDGE_CURVE('',#9077,#9073,#5418,.T.);
#11654=EDGE_CURVE('',#9079,#9080,#6685,.T.);
#11655=EDGE_CURVE('',#9080,#9078,#5419,.T.);
#11656=EDGE_CURVE('',#9079,#9077,#5420,.T.);
#11657=EDGE_CURVE('',#9081,#9082,#6686,.T.);
#11658=EDGE_CURVE('',#9082,#9080,#5421,.T.);
#11659=EDGE_CURVE('',#9081,#9079,#5422,.T.);
#11660=EDGE_CURVE('',#9083,#9084,#6687,.T.);
#11661=EDGE_CURVE('',#9084,#9082,#5423,.T.);
#11662=EDGE_CURVE('',#9083,#9081,#5424,.T.);
#11663=EDGE_CURVE('',#9085,#9086,#6688,.T.);
#11664=EDGE_CURVE('',#9086,#9084,#5425,.T.);
#11665=EDGE_CURVE('',#9085,#9083,#5426,.T.);
#11666=EDGE_CURVE('',#9087,#9088,#6689,.T.);
#11667=EDGE_CURVE('',#9088,#9086,#5427,.T.);
#11668=EDGE_CURVE('',#9087,#9085,#5428,.T.);
#11669=EDGE_CURVE('',#9089,#9090,#6690,.T.);
#11670=EDGE_CURVE('',#9090,#9088,#5429,.T.);
#11671=EDGE_CURVE('',#9089,#9087,#5430,.T.);
#11672=EDGE_CURVE('',#9091,#9092,#6691,.T.);
#11673=EDGE_CURVE('',#9092,#9090,#5431,.T.);
#11674=EDGE_CURVE('',#9091,#9089,#5432,.T.);
#11675=EDGE_CURVE('',#9093,#9094,#6692,.T.);
#11676=EDGE_CURVE('',#9094,#9092,#5433,.T.);
#11677=EDGE_CURVE('',#9093,#9091,#5434,.T.);
#11678=EDGE_CURVE('',#9095,#9096,#6693,.T.);
#11679=EDGE_CURVE('',#9096,#9094,#5435,.T.);
#11680=EDGE_CURVE('',#9095,#9093,#5436,.T.);
#11681=EDGE_CURVE('',#9097,#9098,#6694,.T.);
#11682=EDGE_CURVE('',#9098,#9096,#5437,.T.);
#11683=EDGE_CURVE('',#9097,#9095,#5438,.T.);
#11684=EDGE_CURVE('',#9099,#9100,#6695,.T.);
#11685=EDGE_CURVE('',#9100,#9098,#5439,.T.);
#11686=EDGE_CURVE('',#9099,#9097,#5440,.T.);
#11687=EDGE_CURVE('',#9101,#9102,#6696,.T.);
#11688=EDGE_CURVE('',#9102,#9100,#5441,.T.);
#11689=EDGE_CURVE('',#9101,#9099,#5442,.T.);
#11690=EDGE_CURVE('',#9103,#9104,#6697,.T.);
#11691=EDGE_CURVE('',#9105,#9103,#5443,.T.);
#11692=EDGE_CURVE('',#9106,#9105,#4510,.T.);
#11693=EDGE_CURVE('',#9106,#9104,#5444,.T.);
#11694=EDGE_CURVE('',#9107,#9108,#6698,.T.);
#11695=EDGE_CURVE('',#9108,#9109,#5445,.T.);
#11696=EDGE_CURVE('',#9109,#9110,#4511,.T.);
#11697=EDGE_CURVE('',#9110,#9111,#6699,.T.);
#11698=EDGE_CURVE('',#9111,#9111,#4512,.F.);
#11699=EDGE_CURVE('',#9110,#9112,#4513,.T.);
#11700=EDGE_CURVE('',#9112,#9107,#5446,.T.);
#11701=EDGE_CURVE('',#9113,#9114,#6700,.T.);
#11702=EDGE_CURVE('',#9114,#9108,#5447,.T.);
#11703=EDGE_CURVE('',#9107,#9113,#5448,.T.);
#11704=EDGE_CURVE('',#9115,#9116,#6701,.T.);
#11705=EDGE_CURVE('',#9116,#9114,#5449,.T.);
#11706=EDGE_CURVE('',#9113,#9115,#5450,.T.);
#11707=EDGE_CURVE('',#9117,#9118,#6702,.T.);
#11708=EDGE_CURVE('',#9118,#9116,#5451,.T.);
#11709=EDGE_CURVE('',#9115,#9117,#5452,.T.);
#11710=EDGE_CURVE('',#9119,#9120,#6703,.T.);
#11711=EDGE_CURVE('',#9120,#9118,#5453,.T.);
#11712=EDGE_CURVE('',#9117,#9119,#5454,.T.);
#11713=EDGE_CURVE('',#9121,#9122,#6704,.T.);
#11714=EDGE_CURVE('',#9122,#9120,#5455,.T.);
#11715=EDGE_CURVE('',#9119,#9121,#5456,.T.);
#11716=EDGE_CURVE('',#9123,#9124,#6705,.T.);
#11717=EDGE_CURVE('',#9124,#9122,#5457,.T.);
#11718=EDGE_CURVE('',#9121,#9123,#5458,.T.);
#11719=EDGE_CURVE('',#9125,#9126,#6706,.T.);
#11720=EDGE_CURVE('',#9126,#9124,#5459,.T.);
#11721=EDGE_CURVE('',#9123,#9125,#5460,.T.);
#11722=EDGE_CURVE('',#9127,#9128,#6707,.T.);
#11723=EDGE_CURVE('',#9128,#9126,#5461,.T.);
#11724=EDGE_CURVE('',#9125,#9127,#5462,.T.);
#11725=EDGE_CURVE('',#9129,#9130,#6708,.T.);
#11726=EDGE_CURVE('',#9130,#9128,#5463,.T.);
#11727=EDGE_CURVE('',#9127,#9129,#5464,.T.);
#11728=EDGE_CURVE('',#9131,#9132,#6709,.T.);
#11729=EDGE_CURVE('',#9132,#9130,#5465,.T.);
#11730=EDGE_CURVE('',#9129,#9131,#5466,.T.);
#11731=EDGE_CURVE('',#9133,#9134,#6710,.T.);
#11732=EDGE_CURVE('',#9134,#9132,#5467,.T.);
#11733=EDGE_CURVE('',#9131,#9133,#5468,.T.);
#11734=EDGE_CURVE('',#9135,#9136,#6711,.T.);
#11735=EDGE_CURVE('',#9136,#9134,#5469,.T.);
#11736=EDGE_CURVE('',#9133,#9135,#5470,.T.);
#11737=EDGE_CURVE('',#9137,#9138,#6712,.T.);
#11738=EDGE_CURVE('',#9138,#9136,#5471,.T.);
#11739=EDGE_CURVE('',#9135,#9137,#5472,.T.);
#11740=EDGE_CURVE('',#9139,#9140,#6713,.T.);
#11741=EDGE_CURVE('',#9139,#9141,#5473,.T.);
#11742=EDGE_CURVE('',#9142,#9141,#4514,.T.);
#11743=EDGE_CURVE('',#9142,#9140,#5474,.T.);
#11744=EDGE_CURVE('',#9143,#9144,#6714,.T.);
#11745=EDGE_CURVE('',#9144,#9145,#5475,.T.);
#11746=EDGE_CURVE('',#9146,#9145,#4515,.T.);
#11747=EDGE_CURVE('',#9143,#9146,#5476,.T.);
#11748=EDGE_CURVE('',#9147,#9148,#6715,.T.);
#11749=EDGE_CURVE('',#9148,#9144,#5477,.T.);
#11750=EDGE_CURVE('',#9147,#9143,#5478,.T.);
#11751=EDGE_CURVE('',#9149,#9150,#6716,.T.);
#11752=EDGE_CURVE('',#9150,#9148,#5479,.T.);
#11753=EDGE_CURVE('',#9149,#9147,#5480,.T.);
#11754=EDGE_CURVE('',#9151,#9152,#6717,.T.);
#11755=EDGE_CURVE('',#9152,#9150,#5481,.T.);
#11756=EDGE_CURVE('',#9151,#9149,#5482,.T.);
#11757=EDGE_CURVE('',#9153,#9154,#6718,.T.);
#11758=EDGE_CURVE('',#9154,#9152,#5483,.T.);
#11759=EDGE_CURVE('',#9153,#9151,#5484,.T.);
#11760=EDGE_CURVE('',#9155,#9156,#6719,.T.);
#11761=EDGE_CURVE('',#9156,#9154,#5485,.T.);
#11762=EDGE_CURVE('',#9155,#9153,#5486,.T.);
#11763=EDGE_CURVE('',#9157,#9158,#6720,.T.);
#11764=EDGE_CURVE('',#9158,#9156,#5487,.T.);
#11765=EDGE_CURVE('',#9157,#9155,#5488,.T.);
#11766=EDGE_CURVE('',#9159,#9160,#6721,.T.);
#11767=EDGE_CURVE('',#9160,#9158,#5489,.T.);
#11768=EDGE_CURVE('',#9159,#9157,#5490,.T.);
#11769=EDGE_CURVE('',#9161,#9162,#6722,.T.);
#11770=EDGE_CURVE('',#9162,#9160,#5491,.T.);
#11771=EDGE_CURVE('',#9161,#9159,#5492,.T.);
#11772=EDGE_CURVE('',#9163,#9164,#6723,.T.);
#11773=EDGE_CURVE('',#9164,#9162,#5493,.T.);
#11774=EDGE_CURVE('',#9163,#9161,#5494,.T.);
#11775=EDGE_CURVE('',#9165,#9166,#6724,.T.);
#11776=EDGE_CURVE('',#9166,#9164,#5495,.T.);
#11777=EDGE_CURVE('',#9165,#9163,#5496,.T.);
#11778=EDGE_CURVE('',#9167,#9168,#6725,.T.);
#11779=EDGE_CURVE('',#9168,#9166,#5497,.T.);
#11780=EDGE_CURVE('',#9167,#9165,#5498,.T.);
#11781=EDGE_CURVE('',#9169,#9170,#6726,.T.);
#11782=EDGE_CURVE('',#9170,#9168,#5499,.T.);
#11783=EDGE_CURVE('',#9169,#9167,#5500,.T.);
#11784=EDGE_CURVE('',#9171,#9172,#6727,.T.);
#11785=EDGE_CURVE('',#9172,#9170,#5501,.T.);
#11786=EDGE_CURVE('',#9171,#9169,#5502,.T.);
#11787=EDGE_CURVE('',#9173,#9174,#6728,.T.);
#11788=EDGE_CURVE('',#9175,#9173,#5503,.T.);
#11789=EDGE_CURVE('',#9176,#9175,#4516,.T.);
#11790=EDGE_CURVE('',#9176,#9174,#5504,.T.);
#11791=EDGE_CURVE('',#9177,#9178,#6729,.T.);
#11792=EDGE_CURVE('',#9178,#9179,#5505,.T.);
#11793=EDGE_CURVE('',#9179,#9180,#4517,.T.);
#11794=EDGE_CURVE('',#9180,#9181,#6730,.T.);
#11795=EDGE_CURVE('',#9181,#9181,#4518,.F.);
#11796=EDGE_CURVE('',#9180,#9182,#4519,.T.);
#11797=EDGE_CURVE('',#9182,#9177,#5506,.T.);
#11798=EDGE_CURVE('',#9183,#9184,#6731,.T.);
#11799=EDGE_CURVE('',#9184,#9178,#5507,.T.);
#11800=EDGE_CURVE('',#9177,#9183,#5508,.T.);
#11801=EDGE_CURVE('',#9185,#9186,#6732,.T.);
#11802=EDGE_CURVE('',#9186,#9184,#5509,.T.);
#11803=EDGE_CURVE('',#9183,#9185,#5510,.T.);
#11804=EDGE_CURVE('',#9187,#9188,#6733,.T.);
#11805=EDGE_CURVE('',#9188,#9186,#5511,.T.);
#11806=EDGE_CURVE('',#9185,#9187,#5512,.T.);
#11807=EDGE_CURVE('',#9189,#9190,#6734,.T.);
#11808=EDGE_CURVE('',#9190,#9188,#5513,.T.);
#11809=EDGE_CURVE('',#9187,#9189,#5514,.T.);
#11810=EDGE_CURVE('',#9191,#9192,#6735,.T.);
#11811=EDGE_CURVE('',#9192,#9190,#5515,.T.);
#11812=EDGE_CURVE('',#9189,#9191,#5516,.T.);
#11813=EDGE_CURVE('',#9193,#9194,#6736,.T.);
#11814=EDGE_CURVE('',#9194,#9192,#5517,.T.);
#11815=EDGE_CURVE('',#9191,#9193,#5518,.T.);
#11816=EDGE_CURVE('',#9195,#9196,#6737,.T.);
#11817=EDGE_CURVE('',#9196,#9194,#5519,.T.);
#11818=EDGE_CURVE('',#9193,#9195,#5520,.T.);
#11819=EDGE_CURVE('',#9197,#9198,#6738,.T.);
#11820=EDGE_CURVE('',#9198,#9196,#5521,.T.);
#11821=EDGE_CURVE('',#9195,#9197,#5522,.T.);
#11822=EDGE_CURVE('',#9199,#9200,#6739,.T.);
#11823=EDGE_CURVE('',#9200,#9198,#5523,.T.);
#11824=EDGE_CURVE('',#9197,#9199,#5524,.T.);
#11825=EDGE_CURVE('',#9201,#9202,#6740,.T.);
#11826=EDGE_CURVE('',#9202,#9200,#5525,.T.);
#11827=EDGE_CURVE('',#9199,#9201,#5526,.T.);
#11828=EDGE_CURVE('',#9203,#9204,#6741,.T.);
#11829=EDGE_CURVE('',#9204,#9202,#5527,.T.);
#11830=EDGE_CURVE('',#9201,#9203,#5528,.T.);
#11831=EDGE_CURVE('',#9205,#9206,#6742,.T.);
#11832=EDGE_CURVE('',#9206,#9204,#5529,.T.);
#11833=EDGE_CURVE('',#9203,#9205,#5530,.T.);
#11834=EDGE_CURVE('',#9207,#9208,#6743,.T.);
#11835=EDGE_CURVE('',#9208,#9206,#5531,.T.);
#11836=EDGE_CURVE('',#9205,#9207,#5532,.T.);
#11837=EDGE_CURVE('',#9209,#9210,#6744,.T.);
#11838=EDGE_CURVE('',#9209,#9211,#5533,.T.);
#11839=EDGE_CURVE('',#9212,#9211,#4520,.T.);
#11840=EDGE_CURVE('',#9212,#9210,#5534,.T.);
#11841=EDGE_CURVE('',#9213,#9214,#6745,.T.);
#11842=EDGE_CURVE('',#9214,#9215,#5535,.T.);
#11843=EDGE_CURVE('',#9216,#9215,#4521,.T.);
#11844=EDGE_CURVE('',#9213,#9216,#5536,.T.);
#11845=EDGE_CURVE('',#9217,#9218,#6746,.T.);
#11846=EDGE_CURVE('',#9218,#9214,#5537,.T.);
#11847=EDGE_CURVE('',#9217,#9213,#5538,.T.);
#11848=EDGE_CURVE('',#9219,#9220,#6747,.T.);
#11849=EDGE_CURVE('',#9220,#9218,#5539,.T.);
#11850=EDGE_CURVE('',#9219,#9217,#5540,.T.);
#11851=EDGE_CURVE('',#9221,#9222,#6748,.T.);
#11852=EDGE_CURVE('',#9222,#9220,#5541,.T.);
#11853=EDGE_CURVE('',#9221,#9219,#5542,.T.);
#11854=EDGE_CURVE('',#9223,#9224,#6749,.T.);
#11855=EDGE_CURVE('',#9224,#9222,#5543,.T.);
#11856=EDGE_CURVE('',#9223,#9221,#5544,.T.);
#11857=EDGE_CURVE('',#9225,#9226,#6750,.T.);
#11858=EDGE_CURVE('',#9226,#9224,#5545,.T.);
#11859=EDGE_CURVE('',#9225,#9223,#5546,.T.);
#11860=EDGE_CURVE('',#9227,#9228,#6751,.T.);
#11861=EDGE_CURVE('',#9228,#9226,#5547,.T.);
#11862=EDGE_CURVE('',#9227,#9225,#5548,.T.);
#11863=EDGE_CURVE('',#9229,#9230,#6752,.T.);
#11864=EDGE_CURVE('',#9230,#9228,#5549,.T.);
#11865=EDGE_CURVE('',#9229,#9227,#5550,.T.);
#11866=EDGE_CURVE('',#9231,#9232,#6753,.T.);
#11867=EDGE_CURVE('',#9232,#9230,#5551,.T.);
#11868=EDGE_CURVE('',#9231,#9229,#5552,.T.);
#11869=EDGE_CURVE('',#9233,#9234,#6754,.T.);
#11870=EDGE_CURVE('',#9234,#9232,#5553,.T.);
#11871=EDGE_CURVE('',#9233,#9231,#5554,.T.);
#11872=EDGE_CURVE('',#9235,#9236,#6755,.T.);
#11873=EDGE_CURVE('',#9236,#9234,#5555,.T.);
#11874=EDGE_CURVE('',#9235,#9233,#5556,.T.);
#11875=EDGE_CURVE('',#9237,#9238,#6756,.T.);
#11876=EDGE_CURVE('',#9238,#9236,#5557,.T.);
#11877=EDGE_CURVE('',#9237,#9235,#5558,.T.);
#11878=EDGE_CURVE('',#9239,#9240,#6757,.T.);
#11879=EDGE_CURVE('',#9240,#9238,#5559,.T.);
#11880=EDGE_CURVE('',#9239,#9237,#5560,.T.);
#11881=EDGE_CURVE('',#9241,#9242,#6758,.T.);
#11882=EDGE_CURVE('',#9242,#9240,#5561,.T.);
#11883=EDGE_CURVE('',#9241,#9239,#5562,.T.);
#11884=EDGE_CURVE('',#9243,#9244,#6759,.T.);
#11885=EDGE_CURVE('',#9245,#9243,#5563,.T.);
#11886=EDGE_CURVE('',#9246,#9245,#4522,.T.);
#11887=EDGE_CURVE('',#9246,#9244,#5564,.T.);
#11888=EDGE_CURVE('',#9247,#9248,#6760,.T.);
#11889=EDGE_CURVE('',#9248,#9249,#5565,.T.);
#11890=EDGE_CURVE('',#9249,#9250,#4523,.T.);
#11891=EDGE_CURVE('',#9250,#9251,#6761,.T.);
#11892=EDGE_CURVE('',#9251,#9251,#4524,.F.);
#11893=EDGE_CURVE('',#9250,#9252,#4525,.T.);
#11894=EDGE_CURVE('',#9252,#9247,#5566,.T.);
#11895=EDGE_CURVE('',#9253,#9254,#6762,.T.);
#11896=EDGE_CURVE('',#9254,#9248,#5567,.T.);
#11897=EDGE_CURVE('',#9247,#9253,#5568,.T.);
#11898=EDGE_CURVE('',#9255,#9256,#6763,.T.);
#11899=EDGE_CURVE('',#9256,#9254,#5569,.T.);
#11900=EDGE_CURVE('',#9253,#9255,#5570,.T.);
#11901=EDGE_CURVE('',#9257,#9258,#6764,.T.);
#11902=EDGE_CURVE('',#9258,#9256,#5571,.T.);
#11903=EDGE_CURVE('',#9255,#9257,#5572,.T.);
#11904=EDGE_CURVE('',#9259,#9260,#6765,.T.);
#11905=EDGE_CURVE('',#9260,#9258,#5573,.T.);
#11906=EDGE_CURVE('',#9257,#9259,#5574,.T.);
#11907=EDGE_CURVE('',#9261,#9262,#6766,.T.);
#11908=EDGE_CURVE('',#9262,#9260,#5575,.T.);
#11909=EDGE_CURVE('',#9259,#9261,#5576,.T.);
#11910=EDGE_CURVE('',#9263,#9264,#6767,.T.);
#11911=EDGE_CURVE('',#9264,#9262,#5577,.T.);
#11912=EDGE_CURVE('',#9261,#9263,#5578,.T.);
#11913=EDGE_CURVE('',#9265,#9266,#6768,.T.);
#11914=EDGE_CURVE('',#9266,#9264,#5579,.T.);
#11915=EDGE_CURVE('',#9263,#9265,#5580,.T.);
#11916=EDGE_CURVE('',#9267,#9268,#6769,.T.);
#11917=EDGE_CURVE('',#9268,#9266,#5581,.T.);
#11918=EDGE_CURVE('',#9265,#9267,#5582,.T.);
#11919=EDGE_CURVE('',#9269,#9270,#6770,.T.);
#11920=EDGE_CURVE('',#9270,#9268,#5583,.T.);
#11921=EDGE_CURVE('',#9267,#9269,#5584,.T.);
#11922=EDGE_CURVE('',#9271,#9272,#6771,.T.);
#11923=EDGE_CURVE('',#9272,#9270,#5585,.T.);
#11924=EDGE_CURVE('',#9269,#9271,#5586,.T.);
#11925=EDGE_CURVE('',#9273,#9274,#6772,.T.);
#11926=EDGE_CURVE('',#9274,#9272,#5587,.T.);
#11927=EDGE_CURVE('',#9271,#9273,#5588,.T.);
#11928=EDGE_CURVE('',#9275,#9276,#6773,.T.);
#11929=EDGE_CURVE('',#9276,#9274,#5589,.T.);
#11930=EDGE_CURVE('',#9273,#9275,#5590,.T.);
#11931=EDGE_CURVE('',#9277,#9278,#6774,.T.);
#11932=EDGE_CURVE('',#9278,#9276,#5591,.T.);
#11933=EDGE_CURVE('',#9275,#9277,#5592,.T.);
#11934=EDGE_CURVE('',#9279,#9280,#6775,.T.);
#11935=EDGE_CURVE('',#9279,#9281,#5593,.T.);
#11936=EDGE_CURVE('',#9282,#9281,#4526,.T.);
#11937=EDGE_CURVE('',#9282,#9280,#5594,.T.);
#11938=EDGE_CURVE('',#9283,#9284,#6776,.T.);
#11939=EDGE_CURVE('',#9284,#9285,#5595,.T.);
#11940=EDGE_CURVE('',#9286,#9285,#4527,.T.);
#11941=EDGE_CURVE('',#9283,#9286,#5596,.T.);
#11942=EDGE_CURVE('',#9287,#9288,#6777,.T.);
#11943=EDGE_CURVE('',#9288,#9284,#5597,.T.);
#11944=EDGE_CURVE('',#9287,#9283,#5598,.T.);
#11945=EDGE_CURVE('',#9289,#9290,#6778,.T.);
#11946=EDGE_CURVE('',#9290,#9288,#5599,.T.);
#11947=EDGE_CURVE('',#9289,#9287,#5600,.T.);
#11948=EDGE_CURVE('',#9291,#9292,#6779,.T.);
#11949=EDGE_CURVE('',#9292,#9290,#5601,.T.);
#11950=EDGE_CURVE('',#9291,#9289,#5602,.T.);
#11951=EDGE_CURVE('',#9293,#9294,#6780,.T.);
#11952=EDGE_CURVE('',#9294,#9292,#5603,.T.);
#11953=EDGE_CURVE('',#9293,#9291,#5604,.T.);
#11954=EDGE_CURVE('',#9295,#9296,#6781,.T.);
#11955=EDGE_CURVE('',#9296,#9294,#5605,.T.);
#11956=EDGE_CURVE('',#9295,#9293,#5606,.T.);
#11957=EDGE_CURVE('',#9297,#9298,#6782,.T.);
#11958=EDGE_CURVE('',#9298,#9296,#5607,.T.);
#11959=EDGE_CURVE('',#9297,#9295,#5608,.T.);
#11960=EDGE_CURVE('',#9299,#9300,#6783,.T.);
#11961=EDGE_CURVE('',#9300,#9298,#5609,.T.);
#11962=EDGE_CURVE('',#9299,#9297,#5610,.T.);
#11963=EDGE_CURVE('',#9301,#9302,#6784,.T.);
#11964=EDGE_CURVE('',#9302,#9300,#5611,.T.);
#11965=EDGE_CURVE('',#9301,#9299,#5612,.T.);
#11966=EDGE_CURVE('',#9303,#9304,#6785,.T.);
#11967=EDGE_CURVE('',#9304,#9302,#5613,.T.);
#11968=EDGE_CURVE('',#9303,#9301,#5614,.T.);
#11969=EDGE_CURVE('',#9305,#9306,#6786,.T.);
#11970=EDGE_CURVE('',#9306,#9304,#5615,.T.);
#11971=EDGE_CURVE('',#9305,#9303,#5616,.T.);
#11972=EDGE_CURVE('',#9307,#9308,#6787,.T.);
#11973=EDGE_CURVE('',#9308,#9306,#5617,.T.);
#11974=EDGE_CURVE('',#9307,#9305,#5618,.T.);
#11975=EDGE_CURVE('',#9309,#9310,#6788,.T.);
#11976=EDGE_CURVE('',#9310,#9308,#5619,.T.);
#11977=EDGE_CURVE('',#9309,#9307,#5620,.T.);
#11978=EDGE_CURVE('',#9311,#9312,#6789,.T.);
#11979=EDGE_CURVE('',#9312,#9310,#5621,.T.);
#11980=EDGE_CURVE('',#9311,#9309,#5622,.T.);
#11981=EDGE_CURVE('',#9313,#9314,#6790,.T.);
#11982=EDGE_CURVE('',#9315,#9313,#5623,.T.);
#11983=EDGE_CURVE('',#9316,#9315,#4528,.T.);
#11984=EDGE_CURVE('',#9316,#9314,#5624,.T.);
#11985=EDGE_CURVE('',#9317,#9318,#6791,.T.);
#11986=EDGE_CURVE('',#9318,#9319,#5625,.T.);
#11987=EDGE_CURVE('',#9319,#9320,#4529,.T.);
#11988=EDGE_CURVE('',#9320,#9321,#6792,.T.);
#11989=EDGE_CURVE('',#9321,#9321,#4530,.F.);
#11990=EDGE_CURVE('',#9320,#9322,#4531,.T.);
#11991=EDGE_CURVE('',#9322,#9317,#5626,.T.);
#11992=EDGE_CURVE('',#9323,#9324,#6793,.T.);
#11993=EDGE_CURVE('',#9324,#9318,#5627,.T.);
#11994=EDGE_CURVE('',#9317,#9323,#5628,.T.);
#11995=EDGE_CURVE('',#9325,#9326,#6794,.T.);
#11996=EDGE_CURVE('',#9326,#9324,#5629,.T.);
#11997=EDGE_CURVE('',#9323,#9325,#5630,.T.);
#11998=EDGE_CURVE('',#9327,#9328,#6795,.T.);
#11999=EDGE_CURVE('',#9328,#9326,#5631,.T.);
#12000=EDGE_CURVE('',#9325,#9327,#5632,.T.);
#12001=EDGE_CURVE('',#9329,#9330,#6796,.T.);
#12002=EDGE_CURVE('',#9330,#9328,#5633,.T.);
#12003=EDGE_CURVE('',#9327,#9329,#5634,.T.);
#12004=EDGE_CURVE('',#9331,#9332,#6797,.T.);
#12005=EDGE_CURVE('',#9332,#9330,#5635,.T.);
#12006=EDGE_CURVE('',#9329,#9331,#5636,.T.);
#12007=EDGE_CURVE('',#9333,#9334,#6798,.T.);
#12008=EDGE_CURVE('',#9334,#9332,#5637,.T.);
#12009=EDGE_CURVE('',#9331,#9333,#5638,.T.);
#12010=EDGE_CURVE('',#9335,#9336,#6799,.T.);
#12011=EDGE_CURVE('',#9336,#9334,#5639,.T.);
#12012=EDGE_CURVE('',#9333,#9335,#5640,.T.);
#12013=EDGE_CURVE('',#9337,#9338,#6800,.T.);
#12014=EDGE_CURVE('',#9338,#9336,#5641,.T.);
#12015=EDGE_CURVE('',#9335,#9337,#5642,.T.);
#12016=EDGE_CURVE('',#9339,#9340,#6801,.T.);
#12017=EDGE_CURVE('',#9340,#9338,#5643,.T.);
#12018=EDGE_CURVE('',#9337,#9339,#5644,.T.);
#12019=EDGE_CURVE('',#9341,#9342,#6802,.T.);
#12020=EDGE_CURVE('',#9342,#9340,#5645,.T.);
#12021=EDGE_CURVE('',#9339,#9341,#5646,.T.);
#12022=EDGE_CURVE('',#9343,#9344,#6803,.T.);
#12023=EDGE_CURVE('',#9344,#9342,#5647,.T.);
#12024=EDGE_CURVE('',#9341,#9343,#5648,.T.);
#12025=EDGE_CURVE('',#9345,#9346,#6804,.T.);
#12026=EDGE_CURVE('',#9346,#9344,#5649,.T.);
#12027=EDGE_CURVE('',#9343,#9345,#5650,.T.);
#12028=EDGE_CURVE('',#9347,#9348,#6805,.T.);
#12029=EDGE_CURVE('',#9348,#9346,#5651,.T.);
#12030=EDGE_CURVE('',#9345,#9347,#5652,.T.);
#12031=EDGE_CURVE('',#9349,#9350,#6806,.T.);
#12032=EDGE_CURVE('',#9349,#9351,#5653,.T.);
#12033=EDGE_CURVE('',#9352,#9351,#4532,.T.);
#12034=EDGE_CURVE('',#9352,#9350,#5654,.T.);
#12035=EDGE_CURVE('',#9353,#9354,#6807,.T.);
#12036=EDGE_CURVE('',#9354,#9355,#5655,.T.);
#12037=EDGE_CURVE('',#9356,#9355,#4533,.T.);
#12038=EDGE_CURVE('',#9353,#9356,#5656,.T.);
#12039=EDGE_CURVE('',#9357,#9358,#6808,.T.);
#12040=EDGE_CURVE('',#9358,#9354,#5657,.T.);
#12041=EDGE_CURVE('',#9357,#9353,#5658,.T.);
#12042=EDGE_CURVE('',#9359,#9360,#6809,.T.);
#12043=EDGE_CURVE('',#9360,#9358,#5659,.T.);
#12044=EDGE_CURVE('',#9359,#9357,#5660,.T.);
#12045=EDGE_CURVE('',#9361,#9362,#6810,.T.);
#12046=EDGE_CURVE('',#9362,#9360,#5661,.T.);
#12047=EDGE_CURVE('',#9361,#9359,#5662,.T.);
#12048=EDGE_CURVE('',#9363,#9364,#6811,.T.);
#12049=EDGE_CURVE('',#9364,#9362,#5663,.T.);
#12050=EDGE_CURVE('',#9363,#9361,#5664,.T.);
#12051=EDGE_CURVE('',#9365,#9366,#6812,.T.);
#12052=EDGE_CURVE('',#9366,#9364,#5665,.T.);
#12053=EDGE_CURVE('',#9365,#9363,#5666,.T.);
#12054=EDGE_CURVE('',#9367,#9368,#6813,.T.);
#12055=EDGE_CURVE('',#9368,#9366,#5667,.T.);
#12056=EDGE_CURVE('',#9367,#9365,#5668,.T.);
#12057=EDGE_CURVE('',#9369,#9370,#6814,.T.);
#12058=EDGE_CURVE('',#9370,#9368,#5669,.T.);
#12059=EDGE_CURVE('',#9369,#9367,#5670,.T.);
#12060=EDGE_CURVE('',#9371,#9372,#6815,.T.);
#12061=EDGE_CURVE('',#9372,#9370,#5671,.T.);
#12062=EDGE_CURVE('',#9371,#9369,#5672,.T.);
#12063=EDGE_CURVE('',#9373,#9374,#6816,.T.);
#12064=EDGE_CURVE('',#9374,#9372,#5673,.T.);
#12065=EDGE_CURVE('',#9373,#9371,#5674,.T.);
#12066=EDGE_CURVE('',#9375,#9376,#6817,.T.);
#12067=EDGE_CURVE('',#9376,#9374,#5675,.T.);
#12068=EDGE_CURVE('',#9375,#9373,#5676,.T.);
#12069=EDGE_CURVE('',#9377,#9378,#6818,.T.);
#12070=EDGE_CURVE('',#9378,#9376,#5677,.T.);
#12071=EDGE_CURVE('',#9377,#9375,#5678,.T.);
#12072=EDGE_CURVE('',#9379,#9380,#6819,.T.);
#12073=EDGE_CURVE('',#9380,#9378,#5679,.T.);
#12074=EDGE_CURVE('',#9379,#9377,#5680,.T.);
#12075=EDGE_CURVE('',#9381,#9382,#6820,.T.);
#12076=EDGE_CURVE('',#9382,#9380,#5681,.T.);
#12077=EDGE_CURVE('',#9381,#9379,#5682,.T.);
#12078=EDGE_CURVE('',#9383,#9384,#6821,.T.);
#12079=EDGE_CURVE('',#9385,#9383,#5683,.T.);
#12080=EDGE_CURVE('',#9386,#9385,#4534,.T.);
#12081=EDGE_CURVE('',#9386,#9384,#5684,.T.);
#12082=EDGE_CURVE('',#9387,#9388,#6822,.T.);
#12083=EDGE_CURVE('',#9388,#9389,#5685,.T.);
#12084=EDGE_CURVE('',#9389,#9390,#4535,.T.);
#12085=EDGE_CURVE('',#9390,#9391,#6823,.T.);
#12086=EDGE_CURVE('',#9391,#9391,#4536,.F.);
#12087=EDGE_CURVE('',#9390,#9392,#4537,.T.);
#12088=EDGE_CURVE('',#9392,#9387,#5686,.T.);
#12089=EDGE_CURVE('',#9393,#9394,#6824,.T.);
#12090=EDGE_CURVE('',#9394,#9388,#5687,.T.);
#12091=EDGE_CURVE('',#9387,#9393,#5688,.T.);
#12092=EDGE_CURVE('',#9395,#9396,#6825,.T.);
#12093=EDGE_CURVE('',#9396,#9394,#5689,.T.);
#12094=EDGE_CURVE('',#9393,#9395,#5690,.T.);
#12095=EDGE_CURVE('',#9397,#9398,#6826,.T.);
#12096=EDGE_CURVE('',#9398,#9396,#5691,.T.);
#12097=EDGE_CURVE('',#9395,#9397,#5692,.T.);
#12098=EDGE_CURVE('',#9399,#9400,#6827,.T.);
#12099=EDGE_CURVE('',#9400,#9398,#5693,.T.);
#12100=EDGE_CURVE('',#9397,#9399,#5694,.T.);
#12101=EDGE_CURVE('',#9401,#9402,#6828,.T.);
#12102=EDGE_CURVE('',#9402,#9400,#5695,.T.);
#12103=EDGE_CURVE('',#9399,#9401,#5696,.T.);
#12104=EDGE_CURVE('',#9403,#9404,#6829,.T.);
#12105=EDGE_CURVE('',#9404,#9402,#5697,.T.);
#12106=EDGE_CURVE('',#9401,#9403,#5698,.T.);
#12107=EDGE_CURVE('',#9405,#9406,#6830,.T.);
#12108=EDGE_CURVE('',#9406,#9404,#5699,.T.);
#12109=EDGE_CURVE('',#9403,#9405,#5700,.T.);
#12110=EDGE_CURVE('',#9407,#9408,#6831,.T.);
#12111=EDGE_CURVE('',#9408,#9406,#5701,.T.);
#12112=EDGE_CURVE('',#9405,#9407,#5702,.T.);
#12113=EDGE_CURVE('',#9409,#9410,#6832,.T.);
#12114=EDGE_CURVE('',#9410,#9408,#5703,.T.);
#12115=EDGE_CURVE('',#9407,#9409,#5704,.T.);
#12116=EDGE_CURVE('',#9411,#9412,#6833,.T.);
#12117=EDGE_CURVE('',#9412,#9410,#5705,.T.);
#12118=EDGE_CURVE('',#9409,#9411,#5706,.T.);
#12119=EDGE_CURVE('',#9413,#9414,#6834,.T.);
#12120=EDGE_CURVE('',#9414,#9412,#5707,.T.);
#12121=EDGE_CURVE('',#9411,#9413,#5708,.T.);
#12122=EDGE_CURVE('',#9415,#9416,#6835,.T.);
#12123=EDGE_CURVE('',#9416,#9414,#5709,.T.);
#12124=EDGE_CURVE('',#9413,#9415,#5710,.T.);
#12125=EDGE_CURVE('',#9417,#9418,#6836,.T.);
#12126=EDGE_CURVE('',#9418,#9416,#5711,.T.);
#12127=EDGE_CURVE('',#9415,#9417,#5712,.T.);
#12128=EDGE_CURVE('',#9419,#9420,#6837,.T.);
#12129=EDGE_CURVE('',#9419,#9421,#5713,.T.);
#12130=EDGE_CURVE('',#9422,#9421,#4538,.T.);
#12131=EDGE_CURVE('',#9422,#9420,#5714,.T.);
#12132=EDGE_CURVE('',#9423,#9424,#6838,.T.);
#12133=EDGE_CURVE('',#9424,#9425,#5715,.T.);
#12134=EDGE_CURVE('',#9426,#9425,#4539,.T.);
#12135=EDGE_CURVE('',#9423,#9426,#5716,.T.);
#12136=EDGE_CURVE('',#9427,#9428,#6839,.T.);
#12137=EDGE_CURVE('',#9428,#9424,#5717,.T.);
#12138=EDGE_CURVE('',#9427,#9423,#5718,.T.);
#12139=EDGE_CURVE('',#9429,#9430,#6840,.T.);
#12140=EDGE_CURVE('',#9430,#9428,#5719,.T.);
#12141=EDGE_CURVE('',#9429,#9427,#5720,.T.);
#12142=EDGE_CURVE('',#9431,#9432,#6841,.T.);
#12143=EDGE_CURVE('',#9432,#9430,#5721,.T.);
#12144=EDGE_CURVE('',#9431,#9429,#5722,.T.);
#12145=EDGE_CURVE('',#9433,#9434,#6842,.T.);
#12146=EDGE_CURVE('',#9434,#9432,#5723,.T.);
#12147=EDGE_CURVE('',#9433,#9431,#5724,.T.);
#12148=EDGE_CURVE('',#9435,#9436,#6843,.T.);
#12149=EDGE_CURVE('',#9436,#9434,#5725,.T.);
#12150=EDGE_CURVE('',#9435,#9433,#5726,.T.);
#12151=EDGE_CURVE('',#9437,#9438,#6844,.T.);
#12152=EDGE_CURVE('',#9438,#9436,#5727,.T.);
#12153=EDGE_CURVE('',#9437,#9435,#5728,.T.);
#12154=EDGE_CURVE('',#9439,#9440,#6845,.T.);
#12155=EDGE_CURVE('',#9440,#9438,#5729,.T.);
#12156=EDGE_CURVE('',#9439,#9437,#5730,.T.);
#12157=EDGE_CURVE('',#9441,#9442,#6846,.T.);
#12158=EDGE_CURVE('',#9442,#9440,#5731,.T.);
#12159=EDGE_CURVE('',#9441,#9439,#5732,.T.);
#12160=EDGE_CURVE('',#9443,#9444,#6847,.T.);
#12161=EDGE_CURVE('',#9444,#9442,#5733,.T.);
#12162=EDGE_CURVE('',#9443,#9441,#5734,.T.);
#12163=EDGE_CURVE('',#9445,#9446,#6848,.T.);
#12164=EDGE_CURVE('',#9446,#9444,#5735,.T.);
#12165=EDGE_CURVE('',#9445,#9443,#5736,.T.);
#12166=EDGE_CURVE('',#9447,#9448,#6849,.T.);
#12167=EDGE_CURVE('',#9448,#9446,#5737,.T.);
#12168=EDGE_CURVE('',#9447,#9445,#5738,.T.);
#12169=EDGE_CURVE('',#9449,#9450,#6850,.T.);
#12170=EDGE_CURVE('',#9450,#9448,#5739,.T.);
#12171=EDGE_CURVE('',#9449,#9447,#5740,.T.);
#12172=EDGE_CURVE('',#9451,#9452,#6851,.T.);
#12173=EDGE_CURVE('',#9452,#9450,#5741,.T.);
#12174=EDGE_CURVE('',#9451,#9449,#5742,.T.);
#12175=EDGE_CURVE('',#9453,#9454,#6852,.T.);
#12176=EDGE_CURVE('',#9455,#9453,#5743,.T.);
#12177=EDGE_CURVE('',#9456,#9455,#4540,.T.);
#12178=EDGE_CURVE('',#9456,#9454,#5744,.T.);
#12179=EDGE_CURVE('',#9457,#9458,#6853,.T.);
#12180=EDGE_CURVE('',#9458,#9459,#5745,.T.);
#12181=EDGE_CURVE('',#9459,#9460,#4541,.T.);
#12182=EDGE_CURVE('',#9460,#9461,#6854,.T.);
#12183=EDGE_CURVE('',#9461,#9461,#4542,.F.);
#12184=EDGE_CURVE('',#9460,#9462,#4543,.T.);
#12185=EDGE_CURVE('',#9462,#9457,#5746,.T.);
#12186=EDGE_CURVE('',#9463,#9464,#6855,.T.);
#12187=EDGE_CURVE('',#9464,#9458,#5747,.T.);
#12188=EDGE_CURVE('',#9457,#9463,#5748,.T.);
#12189=EDGE_CURVE('',#9465,#9466,#6856,.T.);
#12190=EDGE_CURVE('',#9466,#9464,#5749,.T.);
#12191=EDGE_CURVE('',#9463,#9465,#5750,.T.);
#12192=EDGE_CURVE('',#9467,#9468,#6857,.T.);
#12193=EDGE_CURVE('',#9468,#9466,#5751,.T.);
#12194=EDGE_CURVE('',#9465,#9467,#5752,.T.);
#12195=EDGE_CURVE('',#9469,#9470,#6858,.T.);
#12196=EDGE_CURVE('',#9470,#9468,#5753,.T.);
#12197=EDGE_CURVE('',#9467,#9469,#5754,.T.);
#12198=EDGE_CURVE('',#9471,#9472,#6859,.T.);
#12199=EDGE_CURVE('',#9472,#9470,#5755,.T.);
#12200=EDGE_CURVE('',#9469,#9471,#5756,.T.);
#12201=EDGE_CURVE('',#9473,#9474,#6860,.T.);
#12202=EDGE_CURVE('',#9474,#9472,#5757,.T.);
#12203=EDGE_CURVE('',#9471,#9473,#5758,.T.);
#12204=EDGE_CURVE('',#9475,#9476,#6861,.T.);
#12205=EDGE_CURVE('',#9476,#9474,#5759,.T.);
#12206=EDGE_CURVE('',#9473,#9475,#5760,.T.);
#12207=EDGE_CURVE('',#9477,#9478,#6862,.T.);
#12208=EDGE_CURVE('',#9478,#9476,#5761,.T.);
#12209=EDGE_CURVE('',#9475,#9477,#5762,.T.);
#12210=EDGE_CURVE('',#9479,#9480,#6863,.T.);
#12211=EDGE_CURVE('',#9480,#9478,#5763,.T.);
#12212=EDGE_CURVE('',#9477,#9479,#5764,.T.);
#12213=EDGE_CURVE('',#9481,#9482,#6864,.T.);
#12214=EDGE_CURVE('',#9482,#9480,#5765,.T.);
#12215=EDGE_CURVE('',#9479,#9481,#5766,.T.);
#12216=EDGE_CURVE('',#9483,#9484,#6865,.T.);
#12217=EDGE_CURVE('',#9484,#9482,#5767,.T.);
#12218=EDGE_CURVE('',#9481,#9483,#5768,.T.);
#12219=EDGE_CURVE('',#9485,#9486,#6866,.T.);
#12220=EDGE_CURVE('',#9486,#9484,#5769,.T.);
#12221=EDGE_CURVE('',#9483,#9485,#5770,.T.);
#12222=EDGE_CURVE('',#9487,#9488,#6867,.T.);
#12223=EDGE_CURVE('',#9488,#9486,#5771,.T.);
#12224=EDGE_CURVE('',#9485,#9487,#5772,.T.);
#12225=EDGE_CURVE('',#9489,#9490,#6868,.T.);
#12226=EDGE_CURVE('',#9489,#9491,#5773,.T.);
#12227=EDGE_CURVE('',#9492,#9491,#4544,.T.);
#12228=EDGE_CURVE('',#9492,#9490,#5774,.T.);
#12229=EDGE_CURVE('',#9493,#9494,#6869,.T.);
#12230=EDGE_CURVE('',#9494,#9495,#5775,.T.);
#12231=EDGE_CURVE('',#9496,#9495,#4545,.T.);
#12232=EDGE_CURVE('',#9493,#9496,#5776,.T.);
#12233=EDGE_CURVE('',#9497,#9498,#6870,.T.);
#12234=EDGE_CURVE('',#9498,#9494,#5777,.T.);
#12235=EDGE_CURVE('',#9497,#9493,#5778,.T.);
#12236=EDGE_CURVE('',#9499,#9500,#6871,.T.);
#12237=EDGE_CURVE('',#9500,#9498,#5779,.T.);
#12238=EDGE_CURVE('',#9499,#9497,#5780,.T.);
#12239=EDGE_CURVE('',#9501,#9502,#6872,.T.);
#12240=EDGE_CURVE('',#9502,#9500,#5781,.T.);
#12241=EDGE_CURVE('',#9501,#9499,#5782,.T.);
#12242=EDGE_CURVE('',#9503,#9504,#6873,.T.);
#12243=EDGE_CURVE('',#9504,#9502,#5783,.T.);
#12244=EDGE_CURVE('',#9503,#9501,#5784,.T.);
#12245=EDGE_CURVE('',#9505,#9506,#6874,.T.);
#12246=EDGE_CURVE('',#9506,#9504,#5785,.T.);
#12247=EDGE_CURVE('',#9505,#9503,#5786,.T.);
#12248=EDGE_CURVE('',#9507,#9508,#6875,.T.);
#12249=EDGE_CURVE('',#9508,#9506,#5787,.T.);
#12250=EDGE_CURVE('',#9507,#9505,#5788,.T.);
#12251=EDGE_CURVE('',#9509,#9510,#6876,.T.);
#12252=EDGE_CURVE('',#9510,#9508,#5789,.T.);
#12253=EDGE_CURVE('',#9509,#9507,#5790,.T.);
#12254=EDGE_CURVE('',#9511,#9512,#6877,.T.);
#12255=EDGE_CURVE('',#9512,#9510,#5791,.T.);
#12256=EDGE_CURVE('',#9511,#9509,#5792,.T.);
#12257=EDGE_CURVE('',#9513,#9514,#6878,.T.);
#12258=EDGE_CURVE('',#9514,#9512,#5793,.T.);
#12259=EDGE_CURVE('',#9513,#9511,#5794,.T.);
#12260=EDGE_CURVE('',#9515,#9516,#6879,.T.);
#12261=EDGE_CURVE('',#9516,#9514,#5795,.T.);
#12262=EDGE_CURVE('',#9515,#9513,#5796,.T.);
#12263=EDGE_CURVE('',#9517,#9518,#6880,.T.);
#12264=EDGE_CURVE('',#9518,#9516,#5797,.T.);
#12265=EDGE_CURVE('',#9517,#9515,#5798,.T.);
#12266=EDGE_CURVE('',#9519,#9520,#6881,.T.);
#12267=EDGE_CURVE('',#9520,#9518,#5799,.T.);
#12268=EDGE_CURVE('',#9519,#9517,#5800,.T.);
#12269=EDGE_CURVE('',#9521,#9522,#6882,.T.);
#12270=EDGE_CURVE('',#9522,#9520,#5801,.T.);
#12271=EDGE_CURVE('',#9521,#9519,#5802,.T.);
#12272=EDGE_CURVE('',#9523,#9524,#6883,.T.);
#12273=EDGE_CURVE('',#9525,#9523,#5803,.T.);
#12274=EDGE_CURVE('',#9526,#9525,#4546,.T.);
#12275=EDGE_CURVE('',#9526,#9524,#5804,.T.);
#12276=EDGE_CURVE('',#9527,#9528,#6884,.T.);
#12277=EDGE_CURVE('',#9528,#9529,#5805,.T.);
#12278=EDGE_CURVE('',#9529,#9530,#4547,.T.);
#12279=EDGE_CURVE('',#9530,#9531,#6885,.T.);
#12280=EDGE_CURVE('',#9531,#9531,#4548,.F.);
#12281=EDGE_CURVE('',#9530,#9532,#4549,.T.);
#12282=EDGE_CURVE('',#9532,#9527,#5806,.T.);
#12283=EDGE_CURVE('',#9533,#9534,#6886,.T.);
#12284=EDGE_CURVE('',#9534,#9528,#5807,.T.);
#12285=EDGE_CURVE('',#9527,#9533,#5808,.T.);
#12286=EDGE_CURVE('',#9535,#9536,#6887,.T.);
#12287=EDGE_CURVE('',#9536,#9534,#5809,.T.);
#12288=EDGE_CURVE('',#9533,#9535,#5810,.T.);
#12289=EDGE_CURVE('',#9537,#9538,#6888,.T.);
#12290=EDGE_CURVE('',#9538,#9536,#5811,.T.);
#12291=EDGE_CURVE('',#9535,#9537,#5812,.T.);
#12292=EDGE_CURVE('',#9539,#9540,#6889,.T.);
#12293=EDGE_CURVE('',#9540,#9538,#5813,.T.);
#12294=EDGE_CURVE('',#9537,#9539,#5814,.T.);
#12295=EDGE_CURVE('',#9541,#9542,#6890,.T.);
#12296=EDGE_CURVE('',#9542,#9540,#5815,.T.);
#12297=EDGE_CURVE('',#9539,#9541,#5816,.T.);
#12298=EDGE_CURVE('',#9543,#9544,#6891,.T.);
#12299=EDGE_CURVE('',#9544,#9542,#5817,.T.);
#12300=EDGE_CURVE('',#9541,#9543,#5818,.T.);
#12301=EDGE_CURVE('',#9545,#9546,#6892,.T.);
#12302=EDGE_CURVE('',#9546,#9544,#5819,.T.);
#12303=EDGE_CURVE('',#9543,#9545,#5820,.T.);
#12304=EDGE_CURVE('',#9547,#9548,#6893,.T.);
#12305=EDGE_CURVE('',#9548,#9546,#5821,.T.);
#12306=EDGE_CURVE('',#9545,#9547,#5822,.T.);
#12307=EDGE_CURVE('',#9549,#9550,#6894,.T.);
#12308=EDGE_CURVE('',#9550,#9548,#5823,.T.);
#12309=EDGE_CURVE('',#9547,#9549,#5824,.T.);
#12310=EDGE_CURVE('',#9551,#9552,#6895,.T.);
#12311=EDGE_CURVE('',#9552,#9550,#5825,.T.);
#12312=EDGE_CURVE('',#9549,#9551,#5826,.T.);
#12313=EDGE_CURVE('',#9553,#9554,#6896,.T.);
#12314=EDGE_CURVE('',#9554,#9552,#5827,.T.);
#12315=EDGE_CURVE('',#9551,#9553,#5828,.T.);
#12316=EDGE_CURVE('',#9555,#9556,#6897,.T.);
#12317=EDGE_CURVE('',#9556,#9554,#5829,.T.);
#12318=EDGE_CURVE('',#9553,#9555,#5830,.T.);
#12319=EDGE_CURVE('',#9557,#9558,#6898,.T.);
#12320=EDGE_CURVE('',#9558,#9556,#5831,.T.);
#12321=EDGE_CURVE('',#9555,#9557,#5832,.T.);
#12322=EDGE_CURVE('',#9559,#9560,#6899,.T.);
#12323=EDGE_CURVE('',#9559,#9561,#5833,.T.);
#12324=EDGE_CURVE('',#9562,#9561,#4550,.T.);
#12325=EDGE_CURVE('',#9562,#9560,#5834,.T.);
#12326=EDGE_CURVE('',#9563,#9564,#6900,.T.);
#12327=EDGE_CURVE('',#9564,#9565,#5835,.T.);
#12328=EDGE_CURVE('',#9566,#9565,#4551,.T.);
#12329=EDGE_CURVE('',#9563,#9566,#5836,.T.);
#12330=EDGE_CURVE('',#9567,#9568,#6901,.T.);
#12331=EDGE_CURVE('',#9568,#9564,#5837,.T.);
#12332=EDGE_CURVE('',#9567,#9563,#5838,.T.);
#12333=EDGE_CURVE('',#9569,#9570,#6902,.T.);
#12334=EDGE_CURVE('',#9570,#9568,#5839,.T.);
#12335=EDGE_CURVE('',#9569,#9567,#5840,.T.);
#12336=EDGE_CURVE('',#9571,#9572,#6903,.T.);
#12337=EDGE_CURVE('',#9572,#9570,#5841,.T.);
#12338=EDGE_CURVE('',#9571,#9569,#5842,.T.);
#12339=EDGE_CURVE('',#9573,#9574,#6904,.T.);
#12340=EDGE_CURVE('',#9574,#9572,#5843,.T.);
#12341=EDGE_CURVE('',#9573,#9571,#5844,.T.);
#12342=EDGE_CURVE('',#9575,#9576,#6905,.T.);
#12343=EDGE_CURVE('',#9576,#9574,#5845,.T.);
#12344=EDGE_CURVE('',#9575,#9573,#5846,.T.);
#12345=EDGE_CURVE('',#9577,#9578,#6906,.T.);
#12346=EDGE_CURVE('',#9578,#9576,#5847,.T.);
#12347=EDGE_CURVE('',#9577,#9575,#5848,.T.);
#12348=EDGE_CURVE('',#9579,#9580,#6907,.T.);
#12349=EDGE_CURVE('',#9580,#9578,#5849,.T.);
#12350=EDGE_CURVE('',#9579,#9577,#5850,.T.);
#12351=EDGE_CURVE('',#9581,#9582,#6908,.T.);
#12352=EDGE_CURVE('',#9582,#9580,#5851,.T.);
#12353=EDGE_CURVE('',#9581,#9579,#5852,.T.);
#12354=EDGE_CURVE('',#9583,#9584,#6909,.T.);
#12355=EDGE_CURVE('',#9584,#9582,#5853,.T.);
#12356=EDGE_CURVE('',#9583,#9581,#5854,.T.);
#12357=EDGE_CURVE('',#9585,#9586,#6910,.T.);
#12358=EDGE_CURVE('',#9586,#9584,#5855,.T.);
#12359=EDGE_CURVE('',#9585,#9583,#5856,.T.);
#12360=EDGE_CURVE('',#9587,#9588,#6911,.T.);
#12361=EDGE_CURVE('',#9588,#9586,#5857,.T.);
#12362=EDGE_CURVE('',#9587,#9585,#5858,.T.);
#12363=EDGE_CURVE('',#9589,#9590,#6912,.T.);
#12364=EDGE_CURVE('',#9590,#9588,#5859,.T.);
#12365=EDGE_CURVE('',#9589,#9587,#5860,.T.);
#12366=EDGE_CURVE('',#9591,#9592,#6913,.T.);
#12367=EDGE_CURVE('',#9592,#9590,#5861,.T.);
#12368=EDGE_CURVE('',#9591,#9589,#5862,.T.);
#12369=EDGE_CURVE('',#9593,#9594,#6914,.T.);
#12370=EDGE_CURVE('',#9595,#9593,#5863,.T.);
#12371=EDGE_CURVE('',#9596,#9595,#4552,.T.);
#12372=EDGE_CURVE('',#9596,#9594,#5864,.T.);
#12373=EDGE_CURVE('',#9597,#9598,#5865,.T.);
#12374=EDGE_CURVE('',#9597,#9599,#6915,.T.);
#12375=EDGE_CURVE('',#9600,#9599,#5866,.T.);
#12376=EDGE_CURVE('',#9599,#9600,#5867,.T.);
#12377=EDGE_CURVE('',#9598,#9597,#5868,.T.);
#12378=EDGE_CURVE('',#9601,#9602,#5869,.T.);
#12379=EDGE_CURVE('',#9602,#9601,#5870,.T.);
#12380=EDGE_CURVE('',#9602,#9603,#6916,.T.);
#12381=EDGE_CURVE('',#9604,#9603,#5871,.T.);
#12382=EDGE_CURVE('',#9603,#9604,#5872,.T.);
#12383=EDGE_CURVE('',#9605,#9606,#5873,.T.);
#12384=EDGE_CURVE('',#9607,#9605,#5874,.T.);
#12385=EDGE_CURVE('',#9607,#9608,#6917,.T.);
#12386=EDGE_CURVE('',#9609,#9608,#5875,.T.);
#12387=EDGE_CURVE('',#9610,#9609,#5876,.T.);
#12388=EDGE_CURVE('',#9608,#9610,#5877,.T.);
#12389=EDGE_CURVE('',#9606,#9607,#5878,.T.);
#12390=EDGE_CURVE('',#9611,#9612,#5879,.T.);
#12391=EDGE_CURVE('',#9613,#9611,#5880,.T.);
#12392=EDGE_CURVE('',#9613,#9614,#6918,.T.);
#12393=EDGE_CURVE('',#9614,#9614,#5881,.T.);
#12394=EDGE_CURVE('',#9612,#9613,#5882,.T.);
#12395=EDGE_CURVE('',#9615,#9616,#5883,.T.);
#12396=EDGE_CURVE('',#9615,#9617,#6919,.T.);
#12397=EDGE_CURVE('',#9618,#9617,#5884,.T.);
#12398=EDGE_CURVE('',#9617,#9618,#5885,.T.);
#12399=EDGE_CURVE('',#9616,#9615,#5886,.T.);
#12400=EDGE_CURVE('',#9619,#9620,#5887,.T.);
#12401=EDGE_CURVE('',#9620,#9619,#5888,.T.);
#12402=EDGE_CURVE('',#9620,#9621,#6920,.T.);
#12403=EDGE_CURVE('',#9622,#9621,#5889,.T.);
#12404=EDGE_CURVE('',#9621,#9622,#5890,.T.);
#12405=EDGE_CURVE('',#9623,#9624,#5891,.T.);
#12406=EDGE_CURVE('',#9625,#9623,#5892,.T.);
#12407=EDGE_CURVE('',#9625,#9626,#6921,.T.);
#12408=EDGE_CURVE('',#9627,#9626,#5893,.T.);
#12409=EDGE_CURVE('',#9628,#9627,#5894,.T.);
#12410=EDGE_CURVE('',#9626,#9628,#5895,.T.);
#12411=EDGE_CURVE('',#9624,#9625,#5896,.T.);
#12412=EDGE_CURVE('',#9629,#9630,#5897,.T.);
#12413=EDGE_CURVE('',#9631,#9629,#5898,.T.);
#12414=EDGE_CURVE('',#9631,#9632,#6922,.T.);
#12415=EDGE_CURVE('',#9632,#9632,#5899,.T.);
#12416=EDGE_CURVE('',#9630,#9631,#5900,.T.);
#12417=EDGE_CURVE('',#9633,#9634,#5901,.T.);
#12418=EDGE_CURVE('',#9633,#9635,#6923,.T.);
#12419=EDGE_CURVE('',#9636,#9635,#5902,.T.);
#12420=EDGE_CURVE('',#9635,#9636,#5903,.T.);
#12421=EDGE_CURVE('',#9634,#9633,#5904,.T.);
#12422=EDGE_CURVE('',#9637,#9638,#5905,.T.);
#12423=EDGE_CURVE('',#9638,#9637,#5906,.T.);
#12424=EDGE_CURVE('',#9638,#9639,#6924,.T.);
#12425=EDGE_CURVE('',#9640,#9639,#5907,.T.);
#12426=EDGE_CURVE('',#9639,#9640,#5908,.T.);
#12427=EDGE_CURVE('',#9641,#9642,#5909,.T.);
#12428=EDGE_CURVE('',#9643,#9641,#5910,.T.);
#12429=EDGE_CURVE('',#9643,#9644,#6925,.T.);
#12430=EDGE_CURVE('',#9645,#9644,#5911,.T.);
#12431=EDGE_CURVE('',#9646,#9645,#5912,.T.);
#12432=EDGE_CURVE('',#9644,#9646,#5913,.T.);
#12433=EDGE_CURVE('',#9642,#9643,#5914,.T.);
#12434=EDGE_CURVE('',#9647,#9648,#5915,.T.);
#12435=EDGE_CURVE('',#9649,#9647,#5916,.T.);
#12436=EDGE_CURVE('',#9649,#9650,#6926,.T.);
#12437=EDGE_CURVE('',#9650,#9650,#5917,.T.);
#12438=EDGE_CURVE('',#9648,#9649,#5918,.T.);
#12439=EDGE_CURVE('',#9529,#9566,#5919,.T.);
#12440=EDGE_CURVE('',#9565,#9532,#5920,.T.);
#12441=EDGE_CURVE('',#9594,#9592,#5921,.T.);
#12442=EDGE_CURVE('',#9593,#9591,#5922,.T.);
#12443=EDGE_CURVE('',#9561,#9596,#5923,.T.);
#12444=EDGE_CURVE('',#9557,#9559,#5924,.T.);
#12445=EDGE_CURVE('',#9560,#9558,#5925,.T.);
#12446=EDGE_CURVE('',#9595,#9562,#5926,.T.);
#12447=EDGE_CURVE('',#9459,#9496,#5927,.T.);
#12448=EDGE_CURVE('',#9495,#9462,#5928,.T.);
#12449=EDGE_CURVE('',#9524,#9522,#5929,.T.);
#12450=EDGE_CURVE('',#9523,#9521,#5930,.T.);
#12451=EDGE_CURVE('',#9491,#9526,#5931,.T.);
#12452=EDGE_CURVE('',#9487,#9489,#5932,.T.);
#12453=EDGE_CURVE('',#9490,#9488,#5933,.T.);
#12454=EDGE_CURVE('',#9525,#9492,#5934,.T.);
#12455=EDGE_CURVE('',#9389,#9426,#5935,.T.);
#12456=EDGE_CURVE('',#9425,#9392,#5936,.T.);
#12457=EDGE_CURVE('',#9454,#9452,#5937,.T.);
#12458=EDGE_CURVE('',#9453,#9451,#5938,.T.);
#12459=EDGE_CURVE('',#9421,#9456,#5939,.T.);
#12460=EDGE_CURVE('',#9417,#9419,#5940,.T.);
#12461=EDGE_CURVE('',#9420,#9418,#5941,.T.);
#12462=EDGE_CURVE('',#9455,#9422,#5942,.T.);
#12463=EDGE_CURVE('',#9319,#9356,#5943,.T.);
#12464=EDGE_CURVE('',#9355,#9322,#5944,.T.);
#12465=EDGE_CURVE('',#9384,#9382,#5945,.T.);
#12466=EDGE_CURVE('',#9383,#9381,#5946,.T.);
#12467=EDGE_CURVE('',#9351,#9386,#5947,.T.);
#12468=EDGE_CURVE('',#9347,#9349,#5948,.T.);
#12469=EDGE_CURVE('',#9350,#9348,#5949,.T.);
#12470=EDGE_CURVE('',#9385,#9352,#5950,.T.);
#12471=EDGE_CURVE('',#9249,#9286,#5951,.T.);
#12472=EDGE_CURVE('',#9285,#9252,#5952,.T.);
#12473=EDGE_CURVE('',#9314,#9312,#5953,.T.);
#12474=EDGE_CURVE('',#9313,#9311,#5954,.T.);
#12475=EDGE_CURVE('',#9281,#9316,#5955,.T.);
#12476=EDGE_CURVE('',#9277,#9279,#5956,.T.);
#12477=EDGE_CURVE('',#9280,#9278,#5957,.T.);
#12478=EDGE_CURVE('',#9315,#9282,#5958,.T.);
#12479=EDGE_CURVE('',#9179,#9216,#5959,.T.);
#12480=EDGE_CURVE('',#9215,#9182,#5960,.T.);
#12481=EDGE_CURVE('',#9244,#9242,#5961,.T.);
#12482=EDGE_CURVE('',#9243,#9241,#5962,.T.);
#12483=EDGE_CURVE('',#9211,#9246,#5963,.T.);
#12484=EDGE_CURVE('',#9207,#9209,#5964,.T.);
#12485=EDGE_CURVE('',#9210,#9208,#5965,.T.);
#12486=EDGE_CURVE('',#9245,#9212,#5966,.T.);
#12487=EDGE_CURVE('',#9109,#9146,#5967,.T.);
#12488=EDGE_CURVE('',#9145,#9112,#5968,.T.);
#12489=EDGE_CURVE('',#9174,#9172,#5969,.T.);
#12490=EDGE_CURVE('',#9173,#9171,#5970,.T.);
#12491=EDGE_CURVE('',#9141,#9176,#5971,.T.);
#12492=EDGE_CURVE('',#9137,#9139,#5972,.T.);
#12493=EDGE_CURVE('',#9140,#9138,#5973,.T.);
#12494=EDGE_CURVE('',#9175,#9142,#5974,.T.);
#12495=EDGE_CURVE('',#9039,#9076,#5975,.T.);
#12496=EDGE_CURVE('',#9075,#9042,#5976,.T.);
#12497=EDGE_CURVE('',#9104,#9102,#5977,.T.);
#12498=EDGE_CURVE('',#9103,#9101,#5978,.T.);
#12499=EDGE_CURVE('',#9071,#9106,#5979,.T.);
#12500=EDGE_CURVE('',#9067,#9069,#5980,.T.);
#12501=EDGE_CURVE('',#9070,#9068,#5981,.T.);
#12502=EDGE_CURVE('',#9105,#9072,#5982,.T.);
#12503=EDGE_CURVE('',#9651,#9651,#4553,.T.);
#12504=EDGE_CURVE('',#9651,#9652,#6927,.T.);
#12505=EDGE_CURVE('',#9652,#9652,#4554,.T.);
#12506=EDGE_CURVE('',#9653,#9653,#4555,.T.);
#12507=EDGE_CURVE('',#9653,#9654,#6928,.T.);
#12508=EDGE_CURVE('',#9654,#9654,#4556,.T.);
#12509=EDGE_CURVE('',#9655,#9655,#4557,.T.);
#12510=EDGE_CURVE('',#9655,#9656,#6929,.T.);
#12511=EDGE_CURVE('',#9656,#9656,#4558,.T.);
#12512=EDGE_CURVE('',#9657,#9657,#4559,.T.);
#12513=EDGE_CURVE('',#9657,#9658,#6930,.T.);
#12514=EDGE_CURVE('',#9658,#9658,#4560,.T.);
#12515=EDGE_CURVE('',#9659,#9659,#4561,.T.);
#12516=EDGE_CURVE('',#9659,#9660,#6931,.T.);
#12517=EDGE_CURVE('',#9660,#9660,#4562,.T.);
#12518=EDGE_CURVE('',#9661,#9661,#4563,.T.);
#12519=EDGE_CURVE('',#9662,#9662,#4564,.T.);
#12520=EDGE_CURVE('',#9662,#9609,#6932,.T.);
#12521=EDGE_CURVE('',#9610,#9627,#6933,.T.);
#12522=EDGE_CURVE('',#9628,#9645,#6934,.T.);
#12523=EDGE_CURVE('',#9646,#9663,#6935,.T.);
#12524=EDGE_CURVE('',#9663,#9663,#4565,.T.);
#12525=EDGE_CURVE('',#9664,#9664,#4566,.T.);
#12526=EDGE_CURVE('',#9664,#9605,#6936,.T.);
#12527=EDGE_CURVE('',#9606,#9623,#6937,.T.);
#12528=EDGE_CURVE('',#9624,#9641,#6938,.T.);
#12529=EDGE_CURVE('',#9642,#9665,#6939,.T.);
#12530=EDGE_CURVE('',#9665,#9665,#4567,.T.);
#12531=EDGE_CURVE('',#9666,#9666,#4568,.F.);
#12532=EDGE_CURVE('',#9661,#9667,#6940,.T.);
#12533=EDGE_CURVE('',#9667,#9667,#4569,.T.);
#12534=EDGE_CURVE('',#9666,#9668,#6941,.T.);
#12535=EDGE_CURVE('',#9668,#9668,#4570,.F.);
#12536=EDGE_CURVE('',#9669,#9670,#5983,.T.);
#12537=EDGE_CURVE('',#9669,#9671,#6942,.T.);
#12538=EDGE_CURVE('',#9671,#9671,#4571,.T.);
#12539=EDGE_CURVE('',#9670,#9669,#5984,.T.);
#12540=EDGE_CURVE('',#9672,#9673,#5985,.T.);
#12541=EDGE_CURVE('',#9673,#9672,#5986,.T.);
#12542=EDGE_CURVE('',#9673,#9674,#6943,.T.);
#12543=EDGE_CURVE('',#9674,#9674,#4572,.T.);
#12544=EDGE_CURVE('',#9675,#9676,#5987,.T.);
#12545=EDGE_CURVE('',#9677,#9675,#5988,.T.);
#12546=EDGE_CURVE('',#9677,#9678,#6944,.T.);
#12547=EDGE_CURVE('',#9678,#9678,#4573,.T.);
#12548=EDGE_CURVE('',#9676,#9677,#5989,.T.);
#12549=EDGE_CURVE('',#9679,#9680,#5990,.T.);
#12550=EDGE_CURVE('',#9681,#9679,#5991,.T.);
#12551=EDGE_CURVE('',#9681,#9682,#6945,.T.);
#12552=EDGE_CURVE('',#9682,#9682,#4574,.T.);
#12553=EDGE_CURVE('',#9680,#9681,#5992,.T.);
#12554=EDGE_CURVE('',#9683,#9683,#4575,.T.);
#12555=EDGE_CURVE('',#9683,#9684,#6946,.T.);
#12556=EDGE_CURVE('',#9684,#9684,#4576,.T.);
#12557=EDGE_CURVE('',#9685,#9685,#4577,.T.);
#12558=EDGE_CURVE('',#9685,#9675,#6947,.T.);
#12559=EDGE_CURVE('',#9676,#9686,#6948,.T.);
#12560=EDGE_CURVE('',#9686,#9686,#4578,.T.);
#12561=EDGE_CURVE('',#9687,#9687,#4579,.T.);
#12562=EDGE_CURVE('',#9687,#9688,#6949,.T.);
#12563=EDGE_CURVE('',#9688,#9688,#4580,.T.);
#12564=EDGE_CURVE('',#9689,#9689,#4581,.T.);
#12565=EDGE_CURVE('',#9689,#9690,#6950,.T.);
#12566=EDGE_CURVE('',#9690,#9690,#4582,.T.);
#12567=EDGE_CURVE('',#9691,#9691,#4583,.T.);
#12568=EDGE_CURVE('',#9691,#9692,#6951,.T.);
#12569=EDGE_CURVE('',#9692,#9692,#4584,.T.);
#12570=EDGE_CURVE('',#9693,#9693,#4585,.T.);
#12571=EDGE_CURVE('',#9693,#9694,#6952,.T.);
#12572=EDGE_CURVE('',#9694,#9694,#4586,.T.);
#12573=EDGE_CURVE('',#9695,#9695,#4587,.T.);
#12574=EDGE_CURVE('',#9695,#9696,#6953,.T.);
#12575=EDGE_CURVE('',#9696,#9696,#4588,.T.);
#12576=EDGE_CURVE('',#9697,#9697,#4589,.T.);
#12577=EDGE_CURVE('',#9697,#9698,#6954,.T.);
#12578=EDGE_CURVE('',#9698,#9698,#4590,.T.);
#12579=EDGE_CURVE('',#9699,#9699,#4591,.T.);
#12580=EDGE_CURVE('',#9699,#9700,#6955,.T.);
#12581=EDGE_CURVE('',#9700,#9700,#4592,.T.);
#12582=EDGE_CURVE('',#9701,#9701,#4593,.T.);
#12583=EDGE_CURVE('',#9701,#9702,#6956,.T.);
#12584=EDGE_CURVE('',#9702,#9702,#4594,.T.);
#12585=EDGE_CURVE('',#9703,#9703,#4595,.T.);
#12586=EDGE_CURVE('',#9703,#9704,#6957,.T.);
#12587=EDGE_CURVE('',#9704,#9704,#4596,.T.);
#12588=EDGE_CURVE('',#9705,#9705,#4597,.T.);
#12589=EDGE_CURVE('',#9705,#9706,#6958,.T.);
#12590=EDGE_CURVE('',#9706,#9706,#4598,.T.);
#12591=EDGE_CURVE('',#9707,#9708,#6959,.T.);
#12592=EDGE_CURVE('',#9707,#9709,#6960,.T.);
#12593=EDGE_CURVE('',#9710,#9709,#6961,.T.);
#12594=EDGE_CURVE('',#9710,#9708,#6962,.T.);
#12595=EDGE_CURVE('',#9708,#9711,#4599,.T.);
#12596=EDGE_CURVE('',#9712,#9710,#6963,.T.);
#12597=EDGE_CURVE('',#9711,#9712,#6964,.T.);
#12598=EDGE_CURVE('',#9711,#9713,#6965,.T.);
#12599=EDGE_CURVE('',#9712,#9714,#6966,.T.);
#12600=EDGE_CURVE('',#9714,#9713,#6967,.T.);
#12601=EDGE_CURVE('',#9709,#9714,#6968,.T.);
#12602=EDGE_CURVE('',#9713,#9707,#4600,.T.);
#12603=EDGE_CURVE('',#9715,#9715,#4601,.T.);
#12604=EDGE_CURVE('',#9715,#9716,#6969,.T.);
#12605=EDGE_CURVE('',#9716,#9716,#4602,.T.);
#12606=EDGE_CURVE('',#9717,#9717,#4603,.T.);
#12607=EDGE_CURVE('',#9718,#9718,#4604,.T.);
#12608=EDGE_CURVE('',#9719,#9719,#4605,.T.);
#12609=EDGE_CURVE('',#9719,#9718,#6970,.T.);
#12610=EDGE_CURVE('',#9720,#9720,#4606,.T.);
#12611=EDGE_CURVE('',#9720,#9721,#6971,.T.);
#12612=EDGE_CURVE('',#9721,#9721,#4607,.T.);
#12613=EDGE_CURVE('',#9722,#9722,#4608,.T.);
#12614=EDGE_CURVE('',#9723,#9723,#4609,.T.);
#12615=EDGE_CURVE('',#9724,#9724,#4610,.T.);
#12616=EDGE_CURVE('',#9724,#9723,#6972,.T.);
#12617=EDGE_CURVE('',#9725,#9725,#4611,.T.);
#12618=EDGE_CURVE('',#9726,#9726,#4612,.T.);
#12619=EDGE_CURVE('',#9727,#9727,#4613,.T.);
#12620=EDGE_CURVE('',#9728,#9728,#4614,.T.);
#12621=EDGE_CURVE('',#9725,#9727,#6973,.T.);
#12622=EDGE_CURVE('',#9728,#9729,#6974,.T.);
#12623=EDGE_CURVE('',#9729,#9729,#4615,.T.);
#12624=EDGE_CURVE('',#9730,#9730,#4616,.T.);
#12625=EDGE_CURVE('',#9731,#9731,#4617,.T.);
#12626=EDGE_CURVE('',#9732,#9732,#4618,.T.);
#12627=EDGE_CURVE('',#9730,#9732,#6975,.T.);
#12628=EDGE_CURVE('',#9722,#9733,#6976,.T.);
#12629=EDGE_CURVE('',#9733,#9733,#4619,.T.);
#12630=EDGE_CURVE('',#9717,#9726,#6977,.T.);
#12631=EDGE_CURVE('',#9734,#9734,#4620,.T.);
#12632=EDGE_CURVE('',#9734,#9735,#6978,.T.);
#12633=EDGE_CURVE('',#9735,#9735,#4621,.T.);
#12634=EDGE_CURVE('',#9736,#9736,#4622,.T.);
#12635=EDGE_CURVE('',#9736,#9731,#6979,.T.);
#12636=EDGE_CURVE('',#9737,#9738,#5993,.T.);
#12637=EDGE_CURVE('',#9737,#9739,#6980,.T.);
#12638=EDGE_CURVE('',#9739,#9739,#4623,.T.);
#12639=EDGE_CURVE('',#9738,#9737,#5994,.T.);
#12640=EDGE_CURVE('',#9740,#9741,#5995,.T.);
#12641=EDGE_CURVE('',#9741,#9740,#5996,.T.);
#12642=EDGE_CURVE('',#9741,#9742,#6981,.T.);
#12643=EDGE_CURVE('',#9742,#9742,#4624,.T.);
#12644=EDGE_CURVE('',#9743,#9744,#5997,.T.);
#12645=EDGE_CURVE('',#9745,#9743,#5998,.T.);
#12646=EDGE_CURVE('',#9745,#9746,#6982,.T.);
#12647=EDGE_CURVE('',#9746,#9746,#4625,.T.);
#12648=EDGE_CURVE('',#9744,#9745,#5999,.T.);
#12649=EDGE_CURVE('',#9747,#9748,#6000,.T.);
#12650=EDGE_CURVE('',#9749,#9747,#6001,.T.);
#12651=EDGE_CURVE('',#9749,#9750,#6983,.T.);
#12652=EDGE_CURVE('',#9750,#9750,#4626,.T.);
#12653=EDGE_CURVE('',#9748,#9749,#6002,.T.);
#12654=EDGE_CURVE('',#9751,#9752,#6003,.T.);
#12655=EDGE_CURVE('',#9752,#9753,#6004,.T.);
#12656=EDGE_CURVE('',#9753,#9754,#6005,.T.);
#12657=EDGE_CURVE('',#9754,#9751,#6006,.T.);
#12658=EDGE_CURVE('',#9755,#9752,#403,.T.);
#12659=EDGE_CURVE('',#9756,#9755,#6984,.T.);
#12660=EDGE_CURVE('',#9753,#9756,#404,.T.);
#12661=EDGE_CURVE('',#9757,#9758,#6007,.T.);
#12662=EDGE_CURVE('',#9758,#9759,#6008,.T.);
#12663=EDGE_CURVE('',#9759,#9760,#6009,.T.);
#12664=EDGE_CURVE('',#9760,#9757,#6010,.T.);
#12665=EDGE_CURVE('',#9759,#9754,#4627,.T.);
#12666=EDGE_CURVE('',#9751,#9758,#4628,.T.);
#12667=EDGE_CURVE('',#9761,#9762,#6011,.T.);
#12668=EDGE_CURVE('',#9762,#9763,#6012,.T.);
#12669=EDGE_CURVE('',#9763,#9764,#6013,.T.);
#12670=EDGE_CURVE('',#9764,#9761,#6014,.T.);
#12671=EDGE_CURVE('',#9765,#9762,#405,.T.);
#12672=EDGE_CURVE('',#9766,#9765,#6985,.T.);
#12673=EDGE_CURVE('',#9763,#9766,#406,.T.);
#12674=EDGE_CURVE('',#9767,#9768,#6015,.T.);
#12675=EDGE_CURVE('',#9768,#9769,#6016,.T.);
#12676=EDGE_CURVE('',#9769,#9770,#6017,.T.);
#12677=EDGE_CURVE('',#9770,#9767,#6018,.T.);
#12678=EDGE_CURVE('',#9769,#9764,#4629,.T.);
#12679=EDGE_CURVE('',#9761,#9768,#4630,.T.);
#12680=EDGE_CURVE('',#9771,#9772,#6019,.T.);
#12681=EDGE_CURVE('',#9772,#9773,#6020,.T.);
#12682=EDGE_CURVE('',#9773,#9774,#6021,.T.);
#12683=EDGE_CURVE('',#9774,#9771,#6022,.T.);
#12684=EDGE_CURVE('',#9775,#9772,#407,.T.);
#12685=EDGE_CURVE('',#9776,#9775,#6986,.T.);
#12686=EDGE_CURVE('',#9773,#9776,#408,.T.);
#12687=EDGE_CURVE('',#9777,#9778,#6023,.T.);
#12688=EDGE_CURVE('',#9778,#9779,#6024,.T.);
#12689=EDGE_CURVE('',#9779,#9780,#6025,.T.);
#12690=EDGE_CURVE('',#9780,#9777,#6026,.T.);
#12691=EDGE_CURVE('',#9779,#9774,#4631,.T.);
#12692=EDGE_CURVE('',#9771,#9778,#4632,.T.);
#12693=EDGE_CURVE('',#9781,#9782,#6027,.T.);
#12694=EDGE_CURVE('',#9782,#9783,#6028,.T.);
#12695=EDGE_CURVE('',#9783,#9784,#6029,.T.);
#12696=EDGE_CURVE('',#9784,#9781,#6030,.T.);
#12697=EDGE_CURVE('',#9785,#9782,#409,.T.);
#12698=EDGE_CURVE('',#9786,#9785,#6987,.T.);
#12699=EDGE_CURVE('',#9783,#9786,#410,.T.);
#12700=EDGE_CURVE('',#9787,#9788,#6031,.T.);
#12701=EDGE_CURVE('',#9788,#9789,#6032,.T.);
#12702=EDGE_CURVE('',#9789,#9790,#6033,.T.);
#12703=EDGE_CURVE('',#9790,#9787,#6034,.T.);
#12704=EDGE_CURVE('',#9789,#9784,#4633,.T.);
#12705=EDGE_CURVE('',#9781,#9788,#4634,.T.);
#12706=EDGE_CURVE('',#9791,#9792,#6035,.T.);
#12707=EDGE_CURVE('',#9792,#9793,#6036,.T.);
#12708=EDGE_CURVE('',#9793,#9794,#6037,.T.);
#12709=EDGE_CURVE('',#9794,#9791,#6038,.T.);
#12710=EDGE_CURVE('',#9795,#9792,#411,.T.);
#12711=EDGE_CURVE('',#9796,#9795,#6988,.T.);
#12712=EDGE_CURVE('',#9793,#9796,#412,.T.);
#12713=EDGE_CURVE('',#9797,#9798,#6039,.T.);
#12714=EDGE_CURVE('',#9798,#9799,#6040,.T.);
#12715=EDGE_CURVE('',#9799,#9800,#6041,.T.);
#12716=EDGE_CURVE('',#9800,#9797,#6042,.T.);
#12717=EDGE_CURVE('',#9799,#9794,#4635,.T.);
#12718=EDGE_CURVE('',#9791,#9798,#4636,.T.);
#12719=EDGE_CURVE('',#9801,#9802,#6043,.T.);
#12720=EDGE_CURVE('',#9802,#9803,#6044,.T.);
#12721=EDGE_CURVE('',#9803,#9804,#6045,.T.);
#12722=EDGE_CURVE('',#9804,#9801,#6046,.T.);
#12723=EDGE_CURVE('',#9805,#9802,#413,.T.);
#12724=EDGE_CURVE('',#9806,#9805,#6989,.T.);
#12725=EDGE_CURVE('',#9803,#9806,#414,.T.);
#12726=EDGE_CURVE('',#9807,#9808,#6047,.T.);
#12727=EDGE_CURVE('',#9808,#9809,#6048,.T.);
#12728=EDGE_CURVE('',#9809,#9810,#6049,.T.);
#12729=EDGE_CURVE('',#9810,#9807,#6050,.T.);
#12730=EDGE_CURVE('',#9809,#9804,#4637,.T.);
#12731=EDGE_CURVE('',#9801,#9808,#4638,.T.);
#12732=EDGE_CURVE('',#9811,#9812,#6051,.T.);
#12733=EDGE_CURVE('',#9812,#9813,#6052,.T.);
#12734=EDGE_CURVE('',#9813,#9814,#6053,.T.);
#12735=EDGE_CURVE('',#9814,#9811,#6054,.T.);
#12736=EDGE_CURVE('',#9815,#9812,#415,.T.);
#12737=EDGE_CURVE('',#9816,#9815,#6990,.T.);
#12738=EDGE_CURVE('',#9813,#9816,#416,.T.);
#12739=EDGE_CURVE('',#9817,#9818,#6055,.T.);
#12740=EDGE_CURVE('',#9818,#9819,#6056,.T.);
#12741=EDGE_CURVE('',#9819,#9820,#6057,.T.);
#12742=EDGE_CURVE('',#9820,#9817,#6058,.T.);
#12743=EDGE_CURVE('',#9819,#9814,#4639,.T.);
#12744=EDGE_CURVE('',#9811,#9818,#4640,.T.);
#12745=EDGE_CURVE('',#9821,#9822,#6059,.T.);
#12746=EDGE_CURVE('',#9822,#9823,#6060,.T.);
#12747=EDGE_CURVE('',#9823,#9824,#6061,.T.);
#12748=EDGE_CURVE('',#9824,#9821,#6062,.T.);
#12749=EDGE_CURVE('',#9825,#9822,#417,.T.);
#12750=EDGE_CURVE('',#9826,#9825,#6991,.T.);
#12751=EDGE_CURVE('',#9823,#9826,#418,.T.);
#12752=EDGE_CURVE('',#9827,#9828,#6063,.T.);
#12753=EDGE_CURVE('',#9828,#9829,#6064,.T.);
#12754=EDGE_CURVE('',#9829,#9830,#6065,.T.);
#12755=EDGE_CURVE('',#9830,#9827,#6066,.T.);
#12756=EDGE_CURVE('',#9829,#9824,#4641,.T.);
#12757=EDGE_CURVE('',#9821,#9828,#4642,.T.);
#12758=EDGE_CURVE('',#9831,#9832,#6067,.T.);
#12759=EDGE_CURVE('',#9832,#9833,#6068,.T.);
#12760=EDGE_CURVE('',#9833,#9834,#6069,.T.);
#12761=EDGE_CURVE('',#9834,#9831,#6070,.T.);
#12762=EDGE_CURVE('',#9835,#9832,#419,.T.);
#12763=EDGE_CURVE('',#9836,#9835,#6992,.T.);
#12764=EDGE_CURVE('',#9833,#9836,#420,.T.);
#12765=EDGE_CURVE('',#9837,#9838,#6071,.T.);
#12766=EDGE_CURVE('',#9838,#9839,#6072,.T.);
#12767=EDGE_CURVE('',#9839,#9840,#6073,.T.);
#12768=EDGE_CURVE('',#9840,#9837,#6074,.T.);
#12769=EDGE_CURVE('',#9839,#9834,#4643,.T.);
#12770=EDGE_CURVE('',#9831,#9838,#4644,.T.);
#12771=EDGE_CURVE('',#9841,#9842,#6075,.T.);
#12772=EDGE_CURVE('',#9842,#9843,#6076,.T.);
#12773=EDGE_CURVE('',#9843,#9844,#6077,.T.);
#12774=EDGE_CURVE('',#9844,#9841,#6078,.T.);
#12775=EDGE_CURVE('',#9845,#9842,#421,.T.);
#12776=EDGE_CURVE('',#9846,#9845,#6993,.T.);
#12777=EDGE_CURVE('',#9843,#9846,#422,.T.);
#12778=EDGE_CURVE('',#9847,#9848,#6079,.T.);
#12779=EDGE_CURVE('',#9848,#9849,#6080,.T.);
#12780=EDGE_CURVE('',#9849,#9850,#6081,.T.);
#12781=EDGE_CURVE('',#9850,#9847,#6082,.T.);
#12782=EDGE_CURVE('',#9849,#9844,#4645,.T.);
#12783=EDGE_CURVE('',#9841,#9848,#4646,.T.);
#12784=EDGE_CURVE('',#9851,#9852,#6083,.T.);
#12785=EDGE_CURVE('',#9852,#9853,#6084,.T.);
#12786=EDGE_CURVE('',#9853,#9854,#6085,.T.);
#12787=EDGE_CURVE('',#9854,#9851,#6086,.T.);
#12788=EDGE_CURVE('',#9855,#9852,#423,.T.);
#12789=EDGE_CURVE('',#9856,#9855,#6994,.T.);
#12790=EDGE_CURVE('',#9853,#9856,#424,.T.);
#12791=EDGE_CURVE('',#9857,#9858,#6087,.T.);
#12792=EDGE_CURVE('',#9858,#9859,#6088,.T.);
#12793=EDGE_CURVE('',#9859,#9860,#6089,.T.);
#12794=EDGE_CURVE('',#9860,#9857,#6090,.T.);
#12795=EDGE_CURVE('',#9859,#9854,#4647,.T.);
#12796=EDGE_CURVE('',#9851,#9858,#4648,.T.);
#12797=EDGE_CURVE('',#9861,#9862,#6091,.T.);
#12798=EDGE_CURVE('',#9862,#9863,#6092,.T.);
#12799=EDGE_CURVE('',#9863,#9864,#6093,.T.);
#12800=EDGE_CURVE('',#9864,#9861,#6094,.T.);
#12801=EDGE_CURVE('',#9865,#9862,#425,.T.);
#12802=EDGE_CURVE('',#9866,#9865,#6995,.T.);
#12803=EDGE_CURVE('',#9863,#9866,#426,.T.);
#12804=EDGE_CURVE('',#9867,#9868,#6095,.T.);
#12805=EDGE_CURVE('',#9868,#9869,#6096,.T.);
#12806=EDGE_CURVE('',#9869,#9870,#6097,.T.);
#12807=EDGE_CURVE('',#9870,#9867,#6098,.T.);
#12808=EDGE_CURVE('',#9869,#9864,#4649,.T.);
#12809=EDGE_CURVE('',#9861,#9868,#4650,.T.);
#12810=EDGE_CURVE('',#9871,#9872,#6099,.T.);
#12811=EDGE_CURVE('',#9872,#9873,#6100,.T.);
#12812=EDGE_CURVE('',#9873,#9874,#6101,.T.);
#12813=EDGE_CURVE('',#9874,#9871,#6102,.T.);
#12814=EDGE_CURVE('',#9875,#9872,#427,.T.);
#12815=EDGE_CURVE('',#9876,#9875,#6996,.T.);
#12816=EDGE_CURVE('',#9873,#9876,#428,.T.);
#12817=EDGE_CURVE('',#9877,#9878,#6103,.T.);
#12818=EDGE_CURVE('',#9878,#9879,#6104,.T.);
#12819=EDGE_CURVE('',#9879,#9880,#6105,.T.);
#12820=EDGE_CURVE('',#9880,#9877,#6106,.T.);
#12821=EDGE_CURVE('',#9879,#9874,#4651,.T.);
#12822=EDGE_CURVE('',#9871,#9878,#4652,.T.);
#12823=EDGE_CURVE('',#9881,#9882,#6107,.T.);
#12824=EDGE_CURVE('',#9882,#9883,#6108,.T.);
#12825=EDGE_CURVE('',#9883,#9884,#6109,.T.);
#12826=EDGE_CURVE('',#9884,#9881,#6110,.T.);
#12827=EDGE_CURVE('',#9885,#9882,#429,.T.);
#12828=EDGE_CURVE('',#9886,#9885,#6997,.T.);
#12829=EDGE_CURVE('',#9883,#9886,#430,.T.);
#12830=EDGE_CURVE('',#9887,#9888,#6111,.T.);
#12831=EDGE_CURVE('',#9888,#9889,#6112,.T.);
#12832=EDGE_CURVE('',#9889,#9890,#6113,.T.);
#12833=EDGE_CURVE('',#9890,#9887,#6114,.T.);
#12834=EDGE_CURVE('',#9889,#9884,#4653,.T.);
#12835=EDGE_CURVE('',#9881,#9888,#4654,.T.);
#12836=EDGE_CURVE('',#9891,#9892,#6115,.T.);
#12837=EDGE_CURVE('',#9892,#9893,#6116,.T.);
#12838=EDGE_CURVE('',#9893,#9894,#6117,.T.);
#12839=EDGE_CURVE('',#9894,#9891,#6118,.T.);
#12840=EDGE_CURVE('',#9895,#9892,#431,.T.);
#12841=EDGE_CURVE('',#9896,#9895,#6998,.T.);
#12842=EDGE_CURVE('',#9893,#9896,#432,.T.);
#12843=EDGE_CURVE('',#9897,#9898,#6119,.T.);
#12844=EDGE_CURVE('',#9898,#9899,#6120,.T.);
#12845=EDGE_CURVE('',#9899,#9900,#6121,.T.);
#12846=EDGE_CURVE('',#9900,#9897,#6122,.T.);
#12847=EDGE_CURVE('',#9899,#9894,#4655,.T.);
#12848=EDGE_CURVE('',#9891,#9898,#4656,.T.);
#12849=EDGE_CURVE('',#9901,#9902,#6123,.T.);
#12850=EDGE_CURVE('',#9902,#9903,#6124,.T.);
#12851=EDGE_CURVE('',#9903,#9904,#6125,.T.);
#12852=EDGE_CURVE('',#9904,#9901,#6126,.T.);
#12853=EDGE_CURVE('',#9905,#9902,#433,.T.);
#12854=EDGE_CURVE('',#9906,#9905,#6999,.T.);
#12855=EDGE_CURVE('',#9903,#9906,#434,.T.);
#12856=EDGE_CURVE('',#9907,#9908,#6127,.T.);
#12857=EDGE_CURVE('',#9908,#9909,#6128,.T.);
#12858=EDGE_CURVE('',#9909,#9910,#6129,.T.);
#12859=EDGE_CURVE('',#9910,#9907,#6130,.T.);
#12860=EDGE_CURVE('',#9909,#9904,#4657,.T.);
#12861=EDGE_CURVE('',#9901,#9908,#4658,.T.);
#12862=EDGE_CURVE('',#9911,#9912,#6131,.T.);
#12863=EDGE_CURVE('',#9912,#9913,#6132,.T.);
#12864=EDGE_CURVE('',#9913,#9914,#6133,.T.);
#12865=EDGE_CURVE('',#9914,#9911,#6134,.T.);
#12866=EDGE_CURVE('',#9915,#9912,#435,.T.);
#12867=EDGE_CURVE('',#9916,#9915,#7000,.T.);
#12868=EDGE_CURVE('',#9913,#9916,#436,.T.);
#12869=EDGE_CURVE('',#9917,#9918,#6135,.T.);
#12870=EDGE_CURVE('',#9918,#9919,#6136,.T.);
#12871=EDGE_CURVE('',#9919,#9920,#6137,.T.);
#12872=EDGE_CURVE('',#9920,#9917,#6138,.T.);
#12873=EDGE_CURVE('',#9919,#9914,#4659,.T.);
#12874=EDGE_CURVE('',#9911,#9918,#4660,.T.);
#12875=EDGE_CURVE('',#9921,#9922,#6139,.T.);
#12876=EDGE_CURVE('',#9922,#9923,#6140,.T.);
#12877=EDGE_CURVE('',#9923,#9924,#6141,.T.);
#12878=EDGE_CURVE('',#9924,#9921,#6142,.T.);
#12879=EDGE_CURVE('',#9925,#9922,#437,.T.);
#12880=EDGE_CURVE('',#9926,#9925,#7001,.T.);
#12881=EDGE_CURVE('',#9923,#9926,#438,.T.);
#12882=EDGE_CURVE('',#9927,#9928,#6143,.T.);
#12883=EDGE_CURVE('',#9928,#9929,#6144,.T.);
#12884=EDGE_CURVE('',#9929,#9930,#6145,.T.);
#12885=EDGE_CURVE('',#9930,#9927,#6146,.T.);
#12886=EDGE_CURVE('',#9929,#9924,#4661,.T.);
#12887=EDGE_CURVE('',#9921,#9928,#4662,.T.);
#12888=EDGE_CURVE('',#9931,#9932,#6147,.T.);
#12889=EDGE_CURVE('',#9932,#9933,#6148,.T.);
#12890=EDGE_CURVE('',#9933,#9934,#6149,.T.);
#12891=EDGE_CURVE('',#9934,#9931,#6150,.T.);
#12892=EDGE_CURVE('',#9935,#9932,#439,.T.);
#12893=EDGE_CURVE('',#9936,#9935,#7002,.T.);
#12894=EDGE_CURVE('',#9933,#9936,#440,.T.);
#12895=EDGE_CURVE('',#9937,#9938,#6151,.T.);
#12896=EDGE_CURVE('',#9938,#9939,#6152,.T.);
#12897=EDGE_CURVE('',#9939,#9940,#6153,.T.);
#12898=EDGE_CURVE('',#9940,#9937,#6154,.T.);
#12899=EDGE_CURVE('',#9939,#9934,#4663,.T.);
#12900=EDGE_CURVE('',#9931,#9938,#4664,.T.);
#12901=EDGE_CURVE('',#9941,#9942,#6155,.T.);
#12902=EDGE_CURVE('',#9942,#9943,#6156,.T.);
#12903=EDGE_CURVE('',#9943,#9944,#6157,.T.);
#12904=EDGE_CURVE('',#9944,#9941,#6158,.T.);
#12905=EDGE_CURVE('',#9945,#9942,#441,.T.);
#12906=EDGE_CURVE('',#9946,#9945,#7003,.T.);
#12907=EDGE_CURVE('',#9943,#9946,#442,.T.);
#12908=EDGE_CURVE('',#9947,#9948,#6159,.T.);
#12909=EDGE_CURVE('',#9948,#9949,#6160,.T.);
#12910=EDGE_CURVE('',#9949,#9950,#6161,.T.);
#12911=EDGE_CURVE('',#9950,#9947,#6162,.T.);
#12912=EDGE_CURVE('',#9949,#9944,#4665,.T.);
#12913=EDGE_CURVE('',#9941,#9948,#4666,.T.);
#12914=EDGE_CURVE('',#9951,#9952,#6163,.T.);
#12915=EDGE_CURVE('',#9952,#9953,#6164,.T.);
#12916=EDGE_CURVE('',#9953,#9954,#6165,.T.);
#12917=EDGE_CURVE('',#9954,#9951,#6166,.T.);
#12918=EDGE_CURVE('',#9955,#9952,#443,.T.);
#12919=EDGE_CURVE('',#9956,#9955,#7004,.T.);
#12920=EDGE_CURVE('',#9953,#9956,#444,.T.);
#12921=EDGE_CURVE('',#9957,#9958,#6167,.T.);
#12922=EDGE_CURVE('',#9958,#9959,#6168,.T.);
#12923=EDGE_CURVE('',#9959,#9960,#6169,.T.);
#12924=EDGE_CURVE('',#9960,#9957,#6170,.T.);
#12925=EDGE_CURVE('',#9959,#9954,#4667,.T.);
#12926=EDGE_CURVE('',#9951,#9958,#4668,.T.);
#12927=EDGE_CURVE('',#9961,#9962,#6171,.T.);
#12928=EDGE_CURVE('',#9962,#9963,#6172,.T.);
#12929=EDGE_CURVE('',#9963,#9964,#6173,.T.);
#12930=EDGE_CURVE('',#9964,#9961,#6174,.T.);
#12931=EDGE_CURVE('',#9965,#9962,#445,.T.);
#12932=EDGE_CURVE('',#9966,#9965,#7005,.T.);
#12933=EDGE_CURVE('',#9963,#9966,#446,.T.);
#12934=EDGE_CURVE('',#9967,#9968,#6175,.T.);
#12935=EDGE_CURVE('',#9968,#9969,#6176,.T.);
#12936=EDGE_CURVE('',#9969,#9970,#6177,.T.);
#12937=EDGE_CURVE('',#9970,#9967,#6178,.T.);
#12938=EDGE_CURVE('',#9969,#9964,#4669,.T.);
#12939=EDGE_CURVE('',#9961,#9968,#4670,.T.);
#12940=EDGE_CURVE('',#9971,#9972,#6179,.T.);
#12941=EDGE_CURVE('',#9972,#9973,#6180,.T.);
#12942=EDGE_CURVE('',#9973,#9974,#6181,.T.);
#12943=EDGE_CURVE('',#9974,#9971,#6182,.T.);
#12944=EDGE_CURVE('',#9975,#9972,#447,.T.);
#12945=EDGE_CURVE('',#9976,#9975,#7006,.T.);
#12946=EDGE_CURVE('',#9973,#9976,#448,.T.);
#12947=EDGE_CURVE('',#9977,#9978,#6183,.T.);
#12948=EDGE_CURVE('',#9978,#9979,#6184,.T.);
#12949=EDGE_CURVE('',#9979,#9980,#6185,.T.);
#12950=EDGE_CURVE('',#9980,#9977,#6186,.T.);
#12951=EDGE_CURVE('',#9979,#9974,#4671,.T.);
#12952=EDGE_CURVE('',#9971,#9978,#4672,.T.);
#12953=EDGE_CURVE('',#9981,#9982,#6187,.T.);
#12954=EDGE_CURVE('',#9982,#9983,#6188,.T.);
#12955=EDGE_CURVE('',#9983,#9984,#6189,.T.);
#12956=EDGE_CURVE('',#9984,#9981,#6190,.T.);
#12957=EDGE_CURVE('',#9985,#9982,#449,.T.);
#12958=EDGE_CURVE('',#9986,#9985,#7007,.T.);
#12959=EDGE_CURVE('',#9983,#9986,#450,.T.);
#12960=EDGE_CURVE('',#9987,#9988,#6191,.T.);
#12961=EDGE_CURVE('',#9988,#9989,#6192,.T.);
#12962=EDGE_CURVE('',#9989,#9990,#6193,.T.);
#12963=EDGE_CURVE('',#9990,#9987,#6194,.T.);
#12964=EDGE_CURVE('',#9989,#9984,#4673,.T.);
#12965=EDGE_CURVE('',#9981,#9988,#4674,.T.);
#12966=EDGE_CURVE('',#9991,#9992,#6195,.T.);
#12967=EDGE_CURVE('',#9992,#9993,#6196,.T.);
#12968=EDGE_CURVE('',#9993,#9994,#6197,.T.);
#12969=EDGE_CURVE('',#9994,#9991,#6198,.T.);
#12970=EDGE_CURVE('',#9995,#9992,#451,.T.);
#12971=EDGE_CURVE('',#9996,#9995,#7008,.T.);
#12972=EDGE_CURVE('',#9993,#9996,#452,.T.);
#12973=EDGE_CURVE('',#9997,#9998,#6199,.T.);
#12974=EDGE_CURVE('',#9998,#9999,#6200,.T.);
#12975=EDGE_CURVE('',#9999,#10000,#6201,.T.);
#12976=EDGE_CURVE('',#10000,#9997,#6202,.T.);
#12977=EDGE_CURVE('',#9999,#9994,#4675,.T.);
#12978=EDGE_CURVE('',#9991,#9998,#4676,.T.);
#12979=EDGE_CURVE('',#10001,#10002,#6203,.T.);
#12980=EDGE_CURVE('',#10002,#10003,#6204,.T.);
#12981=EDGE_CURVE('',#10003,#10004,#6205,.T.);
#12982=EDGE_CURVE('',#10004,#10001,#6206,.T.);
#12983=EDGE_CURVE('',#10005,#10002,#453,.T.);
#12984=EDGE_CURVE('',#10006,#10005,#7009,.T.);
#12985=EDGE_CURVE('',#10003,#10006,#454,.T.);
#12986=EDGE_CURVE('',#10007,#10008,#6207,.T.);
#12987=EDGE_CURVE('',#10008,#10009,#6208,.T.);
#12988=EDGE_CURVE('',#10009,#10010,#6209,.T.);
#12989=EDGE_CURVE('',#10010,#10007,#6210,.T.);
#12990=EDGE_CURVE('',#10009,#10004,#4677,.T.);
#12991=EDGE_CURVE('',#10001,#10008,#4678,.T.);
#12992=EDGE_CURVE('',#10011,#10012,#6211,.T.);
#12993=EDGE_CURVE('',#10012,#10013,#6212,.T.);
#12994=EDGE_CURVE('',#10013,#10014,#6213,.T.);
#12995=EDGE_CURVE('',#10014,#10011,#6214,.T.);
#12996=EDGE_CURVE('',#10015,#10012,#455,.T.);
#12997=EDGE_CURVE('',#10016,#10015,#7010,.T.);
#12998=EDGE_CURVE('',#10013,#10016,#456,.T.);
#12999=EDGE_CURVE('',#10017,#10018,#6215,.T.);
#13000=EDGE_CURVE('',#10018,#10019,#6216,.T.);
#13001=EDGE_CURVE('',#10019,#10020,#6217,.T.);
#13002=EDGE_CURVE('',#10020,#10017,#6218,.T.);
#13003=EDGE_CURVE('',#10019,#10014,#4679,.T.);
#13004=EDGE_CURVE('',#10011,#10018,#4680,.T.);
#13005=EDGE_CURVE('',#10021,#10022,#6219,.T.);
#13006=EDGE_CURVE('',#10022,#10023,#6220,.T.);
#13007=EDGE_CURVE('',#10023,#10024,#6221,.T.);
#13008=EDGE_CURVE('',#10024,#10021,#6222,.T.);
#13009=EDGE_CURVE('',#10025,#10022,#457,.T.);
#13010=EDGE_CURVE('',#10026,#10025,#7011,.T.);
#13011=EDGE_CURVE('',#10023,#10026,#458,.T.);
#13012=EDGE_CURVE('',#10027,#10028,#6223,.T.);
#13013=EDGE_CURVE('',#10028,#10029,#6224,.T.);
#13014=EDGE_CURVE('',#10029,#10030,#6225,.T.);
#13015=EDGE_CURVE('',#10030,#10027,#6226,.T.);
#13016=EDGE_CURVE('',#10029,#10024,#4681,.T.);
#13017=EDGE_CURVE('',#10021,#10028,#4682,.T.);
#13018=EDGE_CURVE('',#10031,#10032,#6227,.T.);
#13019=EDGE_CURVE('',#10032,#10033,#6228,.T.);
#13020=EDGE_CURVE('',#10033,#10034,#6229,.T.);
#13021=EDGE_CURVE('',#10034,#10031,#6230,.T.);
#13022=EDGE_CURVE('',#10035,#10032,#459,.T.);
#13023=EDGE_CURVE('',#10036,#10035,#7012,.T.);
#13024=EDGE_CURVE('',#10033,#10036,#460,.T.);
#13025=EDGE_CURVE('',#10037,#10038,#6231,.T.);
#13026=EDGE_CURVE('',#10038,#10039,#6232,.T.);
#13027=EDGE_CURVE('',#10039,#10040,#6233,.T.);
#13028=EDGE_CURVE('',#10040,#10037,#6234,.T.);
#13029=EDGE_CURVE('',#10039,#10034,#4683,.T.);
#13030=EDGE_CURVE('',#10031,#10038,#4684,.T.);
#13031=EDGE_CURVE('',#10041,#10042,#6235,.T.);
#13032=EDGE_CURVE('',#10042,#10043,#6236,.T.);
#13033=EDGE_CURVE('',#10043,#10044,#6237,.T.);
#13034=EDGE_CURVE('',#10044,#10041,#6238,.T.);
#13035=EDGE_CURVE('',#10045,#10042,#461,.T.);
#13036=EDGE_CURVE('',#10046,#10045,#7013,.T.);
#13037=EDGE_CURVE('',#10043,#10046,#462,.T.);
#13038=EDGE_CURVE('',#10047,#10048,#6239,.T.);
#13039=EDGE_CURVE('',#10048,#10049,#6240,.T.);
#13040=EDGE_CURVE('',#10049,#10050,#6241,.T.);
#13041=EDGE_CURVE('',#10050,#10047,#6242,.T.);
#13042=EDGE_CURVE('',#10049,#10044,#4685,.T.);
#13043=EDGE_CURVE('',#10041,#10048,#4686,.T.);
#13044=EDGE_CURVE('',#10051,#10052,#6243,.T.);
#13045=EDGE_CURVE('',#10052,#10053,#6244,.T.);
#13046=EDGE_CURVE('',#10053,#10054,#6245,.T.);
#13047=EDGE_CURVE('',#10054,#10051,#6246,.T.);
#13048=EDGE_CURVE('',#10055,#10052,#463,.T.);
#13049=EDGE_CURVE('',#10056,#10055,#7014,.T.);
#13050=EDGE_CURVE('',#10053,#10056,#464,.T.);
#13051=EDGE_CURVE('',#10057,#10058,#6247,.T.);
#13052=EDGE_CURVE('',#10058,#10059,#6248,.T.);
#13053=EDGE_CURVE('',#10059,#10060,#6249,.T.);
#13054=EDGE_CURVE('',#10060,#10057,#6250,.T.);
#13055=EDGE_CURVE('',#10059,#10054,#4687,.T.);
#13056=EDGE_CURVE('',#10051,#10058,#4688,.T.);
#13057=EDGE_CURVE('',#10061,#10062,#6251,.T.);
#13058=EDGE_CURVE('',#10062,#10063,#6252,.T.);
#13059=EDGE_CURVE('',#10063,#10064,#6253,.T.);
#13060=EDGE_CURVE('',#10064,#10061,#6254,.T.);
#13061=EDGE_CURVE('',#10065,#10062,#465,.T.);
#13062=EDGE_CURVE('',#10066,#10065,#7015,.T.);
#13063=EDGE_CURVE('',#10063,#10066,#466,.T.);
#13064=EDGE_CURVE('',#10067,#10068,#6255,.T.);
#13065=EDGE_CURVE('',#10068,#10069,#6256,.T.);
#13066=EDGE_CURVE('',#10069,#10070,#6257,.T.);
#13067=EDGE_CURVE('',#10070,#10067,#6258,.T.);
#13068=EDGE_CURVE('',#10069,#10064,#4689,.T.);
#13069=EDGE_CURVE('',#10061,#10068,#4690,.T.);
#13070=EDGE_CURVE('',#10071,#10072,#6259,.T.);
#13071=EDGE_CURVE('',#10072,#10073,#6260,.T.);
#13072=EDGE_CURVE('',#10073,#10074,#6261,.T.);
#13073=EDGE_CURVE('',#10074,#10071,#6262,.T.);
#13074=EDGE_CURVE('',#10075,#10072,#467,.T.);
#13075=EDGE_CURVE('',#10076,#10075,#7016,.T.);
#13076=EDGE_CURVE('',#10073,#10076,#468,.T.);
#13077=EDGE_CURVE('',#10077,#10078,#6263,.T.);
#13078=EDGE_CURVE('',#10078,#10079,#6264,.T.);
#13079=EDGE_CURVE('',#10079,#10080,#6265,.T.);
#13080=EDGE_CURVE('',#10080,#10077,#6266,.T.);
#13081=EDGE_CURVE('',#10079,#10074,#4691,.T.);
#13082=EDGE_CURVE('',#10071,#10078,#4692,.T.);
#13083=EDGE_CURVE('',#10081,#10082,#6267,.T.);
#13084=EDGE_CURVE('',#10082,#10083,#6268,.T.);
#13085=EDGE_CURVE('',#10083,#10084,#6269,.T.);
#13086=EDGE_CURVE('',#10084,#10081,#6270,.T.);
#13087=EDGE_CURVE('',#10085,#10082,#469,.T.);
#13088=EDGE_CURVE('',#10086,#10085,#7017,.T.);
#13089=EDGE_CURVE('',#10083,#10086,#470,.T.);
#13090=EDGE_CURVE('',#10087,#10088,#6271,.T.);
#13091=EDGE_CURVE('',#10088,#10089,#6272,.T.);
#13092=EDGE_CURVE('',#10089,#10090,#6273,.T.);
#13093=EDGE_CURVE('',#10090,#10087,#6274,.T.);
#13094=EDGE_CURVE('',#10089,#10084,#4693,.T.);
#13095=EDGE_CURVE('',#10081,#10088,#4694,.T.);
#13096=EDGE_CURVE('',#10091,#10092,#6275,.T.);
#13097=EDGE_CURVE('',#10092,#10093,#6276,.T.);
#13098=EDGE_CURVE('',#10093,#10094,#6277,.T.);
#13099=EDGE_CURVE('',#10094,#10091,#6278,.T.);
#13100=EDGE_CURVE('',#10095,#10092,#471,.T.);
#13101=EDGE_CURVE('',#10096,#10095,#7018,.T.);
#13102=EDGE_CURVE('',#10093,#10096,#472,.T.);
#13103=EDGE_CURVE('',#10097,#10098,#6279,.T.);
#13104=EDGE_CURVE('',#10098,#10099,#6280,.T.);
#13105=EDGE_CURVE('',#10099,#10100,#6281,.T.);
#13106=EDGE_CURVE('',#10100,#10097,#6282,.T.);
#13107=EDGE_CURVE('',#10099,#10094,#4695,.T.);
#13108=EDGE_CURVE('',#10091,#10098,#4696,.T.);
#13109=EDGE_CURVE('',#10101,#10102,#6283,.T.);
#13110=EDGE_CURVE('',#10102,#10103,#6284,.T.);
#13111=EDGE_CURVE('',#10103,#10104,#6285,.T.);
#13112=EDGE_CURVE('',#10104,#10101,#6286,.T.);
#13113=EDGE_CURVE('',#10105,#10102,#473,.T.);
#13114=EDGE_CURVE('',#10106,#10105,#7019,.T.);
#13115=EDGE_CURVE('',#10103,#10106,#474,.T.);
#13116=EDGE_CURVE('',#10107,#10108,#6287,.T.);
#13117=EDGE_CURVE('',#10108,#10109,#6288,.T.);
#13118=EDGE_CURVE('',#10109,#10110,#6289,.T.);
#13119=EDGE_CURVE('',#10110,#10107,#6290,.T.);
#13120=EDGE_CURVE('',#10109,#10104,#4697,.T.);
#13121=EDGE_CURVE('',#10101,#10108,#4698,.T.);
#13122=EDGE_CURVE('',#10111,#10112,#6291,.T.);
#13123=EDGE_CURVE('',#10112,#10113,#6292,.T.);
#13124=EDGE_CURVE('',#10113,#10114,#6293,.T.);
#13125=EDGE_CURVE('',#10114,#10111,#6294,.T.);
#13126=EDGE_CURVE('',#10115,#10112,#475,.T.);
#13127=EDGE_CURVE('',#10116,#10115,#7020,.T.);
#13128=EDGE_CURVE('',#10113,#10116,#476,.T.);
#13129=EDGE_CURVE('',#10117,#10118,#6295,.T.);
#13130=EDGE_CURVE('',#10118,#10119,#6296,.T.);
#13131=EDGE_CURVE('',#10119,#10120,#6297,.T.);
#13132=EDGE_CURVE('',#10120,#10117,#6298,.T.);
#13133=EDGE_CURVE('',#10119,#10114,#4699,.T.);
#13134=EDGE_CURVE('',#10111,#10118,#4700,.T.);
#13135=EDGE_CURVE('',#10121,#10122,#6299,.T.);
#13136=EDGE_CURVE('',#10122,#10123,#6300,.T.);
#13137=EDGE_CURVE('',#10123,#10124,#6301,.T.);
#13138=EDGE_CURVE('',#10124,#10121,#6302,.T.);
#13139=EDGE_CURVE('',#10125,#10122,#477,.T.);
#13140=EDGE_CURVE('',#10126,#10125,#7021,.T.);
#13141=EDGE_CURVE('',#10123,#10126,#478,.T.);
#13142=EDGE_CURVE('',#10127,#10128,#6303,.T.);
#13143=EDGE_CURVE('',#10128,#10129,#6304,.T.);
#13144=EDGE_CURVE('',#10129,#10130,#6305,.T.);
#13145=EDGE_CURVE('',#10130,#10127,#6306,.T.);
#13146=EDGE_CURVE('',#10129,#10124,#4701,.T.);
#13147=EDGE_CURVE('',#10121,#10128,#4702,.T.);
#13148=EDGE_CURVE('',#10131,#10132,#6307,.T.);
#13149=EDGE_CURVE('',#10132,#10133,#6308,.T.);
#13150=EDGE_CURVE('',#10133,#10134,#6309,.T.);
#13151=EDGE_CURVE('',#10134,#10131,#6310,.T.);
#13152=EDGE_CURVE('',#10135,#10132,#479,.T.);
#13153=EDGE_CURVE('',#10136,#10135,#7022,.T.);
#13154=EDGE_CURVE('',#10133,#10136,#480,.T.);
#13155=EDGE_CURVE('',#10137,#10138,#6311,.T.);
#13156=EDGE_CURVE('',#10138,#10139,#6312,.T.);
#13157=EDGE_CURVE('',#10139,#10140,#6313,.T.);
#13158=EDGE_CURVE('',#10140,#10137,#6314,.T.);
#13159=EDGE_CURVE('',#10139,#10134,#4703,.T.);
#13160=EDGE_CURVE('',#10131,#10138,#4704,.T.);
#13161=EDGE_CURVE('',#10141,#10142,#6315,.T.);
#13162=EDGE_CURVE('',#10142,#10143,#6316,.T.);
#13163=EDGE_CURVE('',#10143,#10144,#6317,.T.);
#13164=EDGE_CURVE('',#10144,#10141,#6318,.T.);
#13165=EDGE_CURVE('',#10145,#10142,#481,.T.);
#13166=EDGE_CURVE('',#10146,#10145,#7023,.T.);
#13167=EDGE_CURVE('',#10143,#10146,#482,.T.);
#13168=EDGE_CURVE('',#10147,#10148,#6319,.T.);
#13169=EDGE_CURVE('',#10148,#10149,#6320,.T.);
#13170=EDGE_CURVE('',#10149,#10150,#6321,.T.);
#13171=EDGE_CURVE('',#10150,#10147,#6322,.T.);
#13172=EDGE_CURVE('',#10149,#10144,#4705,.T.);
#13173=EDGE_CURVE('',#10141,#10148,#4706,.T.);
#13174=EDGE_CURVE('',#10151,#10152,#6323,.T.);
#13175=EDGE_CURVE('',#10152,#10153,#6324,.T.);
#13176=EDGE_CURVE('',#10153,#10154,#6325,.T.);
#13177=EDGE_CURVE('',#10154,#10151,#6326,.T.);
#13178=EDGE_CURVE('',#10155,#10152,#483,.T.);
#13179=EDGE_CURVE('',#10156,#10155,#7024,.T.);
#13180=EDGE_CURVE('',#10153,#10156,#484,.T.);
#13181=EDGE_CURVE('',#10157,#10158,#6327,.T.);
#13182=EDGE_CURVE('',#10158,#10159,#6328,.T.);
#13183=EDGE_CURVE('',#10159,#10160,#6329,.T.);
#13184=EDGE_CURVE('',#10160,#10157,#6330,.T.);
#13185=EDGE_CURVE('',#10159,#10154,#4707,.T.);
#13186=EDGE_CURVE('',#10151,#10158,#4708,.T.);
#13187=EDGE_CURVE('',#10161,#10162,#6331,.T.);
#13188=EDGE_CURVE('',#10162,#10163,#6332,.T.);
#13189=EDGE_CURVE('',#10163,#10164,#6333,.T.);
#13190=EDGE_CURVE('',#10164,#10161,#6334,.T.);
#13191=EDGE_CURVE('',#10165,#10162,#485,.T.);
#13192=EDGE_CURVE('',#10166,#10165,#7025,.T.);
#13193=EDGE_CURVE('',#10163,#10166,#486,.T.);
#13194=EDGE_CURVE('',#10167,#10168,#6335,.T.);
#13195=EDGE_CURVE('',#10168,#10169,#6336,.T.);
#13196=EDGE_CURVE('',#10169,#10170,#6337,.T.);
#13197=EDGE_CURVE('',#10170,#10167,#6338,.T.);
#13198=EDGE_CURVE('',#10169,#10164,#4709,.T.);
#13199=EDGE_CURVE('',#10161,#10168,#4710,.T.);
#13200=EDGE_CURVE('',#10171,#10172,#6339,.T.);
#13201=EDGE_CURVE('',#10172,#10173,#6340,.T.);
#13202=EDGE_CURVE('',#10173,#10174,#6341,.T.);
#13203=EDGE_CURVE('',#10174,#10171,#6342,.T.);
#13204=EDGE_CURVE('',#10175,#10172,#487,.T.);
#13205=EDGE_CURVE('',#10176,#10175,#7026,.T.);
#13206=EDGE_CURVE('',#10173,#10176,#488,.T.);
#13207=EDGE_CURVE('',#10177,#10178,#6343,.T.);
#13208=EDGE_CURVE('',#10178,#10179,#6344,.T.);
#13209=EDGE_CURVE('',#10179,#10180,#6345,.T.);
#13210=EDGE_CURVE('',#10180,#10177,#6346,.T.);
#13211=EDGE_CURVE('',#10179,#10174,#4711,.T.);
#13212=EDGE_CURVE('',#10171,#10178,#4712,.T.);
#13213=EDGE_CURVE('',#10181,#10182,#6347,.T.);
#13214=EDGE_CURVE('',#10182,#10183,#6348,.T.);
#13215=EDGE_CURVE('',#10183,#10184,#6349,.T.);
#13216=EDGE_CURVE('',#10184,#10181,#6350,.T.);
#13217=EDGE_CURVE('',#10185,#10182,#489,.T.);
#13218=EDGE_CURVE('',#10186,#10185,#7027,.T.);
#13219=EDGE_CURVE('',#10183,#10186,#490,.T.);
#13220=EDGE_CURVE('',#10187,#10188,#6351,.T.);
#13221=EDGE_CURVE('',#10188,#10189,#6352,.T.);
#13222=EDGE_CURVE('',#10189,#10190,#6353,.T.);
#13223=EDGE_CURVE('',#10190,#10187,#6354,.T.);
#13224=EDGE_CURVE('',#10189,#10184,#4713,.T.);
#13225=EDGE_CURVE('',#10181,#10188,#4714,.T.);
#13226=EDGE_CURVE('',#10191,#10192,#6355,.T.);
#13227=EDGE_CURVE('',#10192,#10193,#6356,.T.);
#13228=EDGE_CURVE('',#10193,#10194,#6357,.T.);
#13229=EDGE_CURVE('',#10194,#10191,#6358,.T.);
#13230=EDGE_CURVE('',#10195,#10192,#491,.T.);
#13231=EDGE_CURVE('',#10196,#10195,#7028,.T.);
#13232=EDGE_CURVE('',#10193,#10196,#492,.T.);
#13233=EDGE_CURVE('',#10197,#10198,#6359,.T.);
#13234=EDGE_CURVE('',#10198,#10199,#6360,.T.);
#13235=EDGE_CURVE('',#10199,#10200,#6361,.T.);
#13236=EDGE_CURVE('',#10200,#10197,#6362,.T.);
#13237=EDGE_CURVE('',#10199,#10194,#4715,.T.);
#13238=EDGE_CURVE('',#10191,#10198,#4716,.T.);
#13239=EDGE_CURVE('',#10201,#10202,#6363,.T.);
#13240=EDGE_CURVE('',#10202,#10203,#6364,.T.);
#13241=EDGE_CURVE('',#10203,#10204,#6365,.T.);
#13242=EDGE_CURVE('',#10204,#10201,#6366,.T.);
#13243=EDGE_CURVE('',#10205,#10202,#493,.T.);
#13244=EDGE_CURVE('',#10206,#10205,#7029,.T.);
#13245=EDGE_CURVE('',#10203,#10206,#494,.T.);
#13246=EDGE_CURVE('',#10207,#10208,#6367,.T.);
#13247=EDGE_CURVE('',#10208,#10209,#6368,.T.);
#13248=EDGE_CURVE('',#10209,#10210,#6369,.T.);
#13249=EDGE_CURVE('',#10210,#10207,#6370,.T.);
#13250=EDGE_CURVE('',#10209,#10204,#4717,.T.);
#13251=EDGE_CURVE('',#10201,#10208,#4718,.T.);
#13252=EDGE_CURVE('',#10211,#10212,#6371,.T.);
#13253=EDGE_CURVE('',#10212,#10213,#6372,.T.);
#13254=EDGE_CURVE('',#10213,#10214,#6373,.T.);
#13255=EDGE_CURVE('',#10214,#10211,#6374,.T.);
#13256=EDGE_CURVE('',#10215,#10212,#495,.T.);
#13257=EDGE_CURVE('',#10216,#10215,#7030,.T.);
#13258=EDGE_CURVE('',#10213,#10216,#496,.T.);
#13259=EDGE_CURVE('',#10217,#10218,#6375,.T.);
#13260=EDGE_CURVE('',#10218,#10219,#6376,.T.);
#13261=EDGE_CURVE('',#10219,#10220,#6377,.T.);
#13262=EDGE_CURVE('',#10220,#10217,#6378,.T.);
#13263=EDGE_CURVE('',#10219,#10214,#4719,.T.);
#13264=EDGE_CURVE('',#10211,#10218,#4720,.T.);
#13265=EDGE_CURVE('',#10221,#10222,#6379,.T.);
#13266=EDGE_CURVE('',#10222,#10223,#6380,.T.);
#13267=EDGE_CURVE('',#10223,#10224,#6381,.T.);
#13268=EDGE_CURVE('',#10224,#10221,#6382,.T.);
#13269=EDGE_CURVE('',#10225,#10222,#497,.T.);
#13270=EDGE_CURVE('',#10226,#10225,#7031,.T.);
#13271=EDGE_CURVE('',#10223,#10226,#498,.T.);
#13272=EDGE_CURVE('',#10227,#10228,#6383,.T.);
#13273=EDGE_CURVE('',#10228,#10229,#6384,.T.);
#13274=EDGE_CURVE('',#10229,#10230,#6385,.T.);
#13275=EDGE_CURVE('',#10230,#10227,#6386,.T.);
#13276=EDGE_CURVE('',#10229,#10224,#4721,.T.);
#13277=EDGE_CURVE('',#10221,#10228,#4722,.T.);
#13278=EDGE_CURVE('',#10231,#10232,#6387,.T.);
#13279=EDGE_CURVE('',#10232,#10233,#6388,.T.);
#13280=EDGE_CURVE('',#10233,#10234,#6389,.T.);
#13281=EDGE_CURVE('',#10234,#10231,#6390,.T.);
#13282=EDGE_CURVE('',#10235,#10232,#499,.T.);
#13283=EDGE_CURVE('',#10236,#10235,#7032,.T.);
#13284=EDGE_CURVE('',#10233,#10236,#500,.T.);
#13285=EDGE_CURVE('',#10237,#10238,#6391,.T.);
#13286=EDGE_CURVE('',#10238,#10239,#6392,.T.);
#13287=EDGE_CURVE('',#10239,#10240,#6393,.T.);
#13288=EDGE_CURVE('',#10240,#10237,#6394,.T.);
#13289=EDGE_CURVE('',#10239,#10234,#4723,.T.);
#13290=EDGE_CURVE('',#10231,#10238,#4724,.T.);
#13291=EDGE_CURVE('',#10241,#10242,#6395,.T.);
#13292=EDGE_CURVE('',#10242,#10243,#6396,.T.);
#13293=EDGE_CURVE('',#10243,#10244,#6397,.T.);
#13294=EDGE_CURVE('',#10244,#10241,#6398,.T.);
#13295=EDGE_CURVE('',#10245,#10242,#501,.T.);
#13296=EDGE_CURVE('',#10246,#10245,#7033,.T.);
#13297=EDGE_CURVE('',#10243,#10246,#502,.T.);
#13298=EDGE_CURVE('',#10247,#10248,#6399,.T.);
#13299=EDGE_CURVE('',#10248,#10249,#6400,.T.);
#13300=EDGE_CURVE('',#10249,#10250,#6401,.T.);
#13301=EDGE_CURVE('',#10250,#10247,#6402,.T.);
#13302=EDGE_CURVE('',#10249,#10244,#4725,.T.);
#13303=EDGE_CURVE('',#10241,#10248,#4726,.T.);
#13304=EDGE_CURVE('',#10251,#10252,#6403,.T.);
#13305=EDGE_CURVE('',#10252,#10253,#6404,.T.);
#13306=EDGE_CURVE('',#10253,#10254,#6405,.T.);
#13307=EDGE_CURVE('',#10254,#10251,#6406,.T.);
#13308=EDGE_CURVE('',#10255,#10252,#503,.T.);
#13309=EDGE_CURVE('',#10256,#10255,#7034,.T.);
#13310=EDGE_CURVE('',#10253,#10256,#504,.T.);
#13311=EDGE_CURVE('',#10257,#10258,#6407,.T.);
#13312=EDGE_CURVE('',#10258,#10259,#6408,.T.);
#13313=EDGE_CURVE('',#10259,#10260,#6409,.T.);
#13314=EDGE_CURVE('',#10260,#10257,#6410,.T.);
#13315=EDGE_CURVE('',#10259,#10254,#4727,.T.);
#13316=EDGE_CURVE('',#10251,#10258,#4728,.T.);
#13317=EDGE_CURVE('',#10261,#10262,#6411,.T.);
#13318=EDGE_CURVE('',#10262,#10263,#6412,.T.);
#13319=EDGE_CURVE('',#10263,#10264,#6413,.T.);
#13320=EDGE_CURVE('',#10264,#10261,#6414,.T.);
#13321=EDGE_CURVE('',#10265,#10262,#505,.T.);
#13322=EDGE_CURVE('',#10266,#10265,#7035,.T.);
#13323=EDGE_CURVE('',#10263,#10266,#506,.T.);
#13324=EDGE_CURVE('',#10267,#10268,#6415,.T.);
#13325=EDGE_CURVE('',#10268,#10269,#6416,.T.);
#13326=EDGE_CURVE('',#10269,#10270,#6417,.T.);
#13327=EDGE_CURVE('',#10270,#10267,#6418,.T.);
#13328=EDGE_CURVE('',#10269,#10264,#4729,.T.);
#13329=EDGE_CURVE('',#10261,#10268,#4730,.T.);
#13330=EDGE_CURVE('',#10271,#10272,#6419,.T.);
#13331=EDGE_CURVE('',#10272,#10273,#6420,.T.);
#13332=EDGE_CURVE('',#10273,#10274,#6421,.T.);
#13333=EDGE_CURVE('',#10274,#10271,#6422,.T.);
#13334=EDGE_CURVE('',#10275,#10272,#507,.T.);
#13335=EDGE_CURVE('',#10276,#10275,#7036,.T.);
#13336=EDGE_CURVE('',#10273,#10276,#508,.T.);
#13337=EDGE_CURVE('',#10277,#10278,#6423,.T.);
#13338=EDGE_CURVE('',#10278,#10279,#6424,.T.);
#13339=EDGE_CURVE('',#10279,#10280,#6425,.T.);
#13340=EDGE_CURVE('',#10280,#10277,#6426,.T.);
#13341=EDGE_CURVE('',#10279,#10274,#4731,.T.);
#13342=EDGE_CURVE('',#10271,#10278,#4732,.T.);
#13343=EDGE_CURVE('',#10281,#10282,#6427,.T.);
#13344=EDGE_CURVE('',#10282,#10283,#6428,.T.);
#13345=EDGE_CURVE('',#10283,#10284,#6429,.T.);
#13346=EDGE_CURVE('',#10284,#10281,#6430,.T.);
#13347=EDGE_CURVE('',#10285,#10282,#509,.T.);
#13348=EDGE_CURVE('',#10286,#10285,#7037,.T.);
#13349=EDGE_CURVE('',#10283,#10286,#510,.T.);
#13350=EDGE_CURVE('',#10287,#10288,#6431,.T.);
#13351=EDGE_CURVE('',#10288,#10289,#6432,.T.);
#13352=EDGE_CURVE('',#10289,#10290,#6433,.T.);
#13353=EDGE_CURVE('',#10290,#10287,#6434,.T.);
#13354=EDGE_CURVE('',#10289,#10284,#4733,.T.);
#13355=EDGE_CURVE('',#10281,#10288,#4734,.T.);
#13356=EDGE_CURVE('',#10291,#10292,#6435,.T.);
#13357=EDGE_CURVE('',#10292,#10293,#6436,.T.);
#13358=EDGE_CURVE('',#10293,#10294,#6437,.T.);
#13359=EDGE_CURVE('',#10294,#10291,#6438,.T.);
#13360=EDGE_CURVE('',#10295,#10292,#511,.T.);
#13361=EDGE_CURVE('',#10296,#10295,#7038,.T.);
#13362=EDGE_CURVE('',#10293,#10296,#512,.T.);
#13363=EDGE_CURVE('',#10297,#10298,#6439,.T.);
#13364=EDGE_CURVE('',#10298,#10299,#6440,.T.);
#13365=EDGE_CURVE('',#10299,#10300,#6441,.T.);
#13366=EDGE_CURVE('',#10300,#10297,#6442,.T.);
#13367=EDGE_CURVE('',#10299,#10294,#4735,.T.);
#13368=EDGE_CURVE('',#10291,#10298,#4736,.T.);
#13369=EDGE_CURVE('',#10301,#10302,#6443,.T.);
#13370=EDGE_CURVE('',#10302,#10303,#6444,.T.);
#13371=EDGE_CURVE('',#10303,#10304,#6445,.T.);
#13372=EDGE_CURVE('',#10304,#10301,#6446,.T.);
#13373=EDGE_CURVE('',#10305,#10302,#513,.T.);
#13374=EDGE_CURVE('',#10306,#10305,#7039,.T.);
#13375=EDGE_CURVE('',#10303,#10306,#514,.T.);
#13376=EDGE_CURVE('',#10307,#10308,#6447,.T.);
#13377=EDGE_CURVE('',#10308,#10309,#6448,.T.);
#13378=EDGE_CURVE('',#10309,#10310,#6449,.T.);
#13379=EDGE_CURVE('',#10310,#10307,#6450,.T.);
#13380=EDGE_CURVE('',#10309,#10304,#4737,.T.);
#13381=EDGE_CURVE('',#10301,#10308,#4738,.T.);
#13382=EDGE_CURVE('',#10311,#10312,#6451,.T.);
#13383=EDGE_CURVE('',#10312,#10313,#6452,.T.);
#13384=EDGE_CURVE('',#10313,#10314,#6453,.T.);
#13385=EDGE_CURVE('',#10314,#10311,#6454,.T.);
#13386=EDGE_CURVE('',#10315,#10312,#515,.T.);
#13387=EDGE_CURVE('',#10316,#10315,#7040,.T.);
#13388=EDGE_CURVE('',#10313,#10316,#516,.T.);
#13389=EDGE_CURVE('',#10317,#10318,#6455,.T.);
#13390=EDGE_CURVE('',#10318,#10319,#6456,.T.);
#13391=EDGE_CURVE('',#10319,#10320,#6457,.T.);
#13392=EDGE_CURVE('',#10320,#10317,#6458,.T.);
#13393=EDGE_CURVE('',#10319,#10314,#4739,.T.);
#13394=EDGE_CURVE('',#10311,#10318,#4740,.T.);
#13395=EDGE_CURVE('',#10321,#10322,#6459,.T.);
#13396=EDGE_CURVE('',#10322,#10323,#6460,.T.);
#13397=EDGE_CURVE('',#10323,#10324,#6461,.T.);
#13398=EDGE_CURVE('',#10324,#10321,#6462,.T.);
#13399=EDGE_CURVE('',#10325,#10322,#517,.T.);
#13400=EDGE_CURVE('',#10326,#10325,#7041,.T.);
#13401=EDGE_CURVE('',#10323,#10326,#518,.T.);
#13402=EDGE_CURVE('',#10327,#10328,#6463,.T.);
#13403=EDGE_CURVE('',#10328,#10329,#6464,.T.);
#13404=EDGE_CURVE('',#10329,#10330,#6465,.T.);
#13405=EDGE_CURVE('',#10330,#10327,#6466,.T.);
#13406=EDGE_CURVE('',#10329,#10324,#4741,.T.);
#13407=EDGE_CURVE('',#10321,#10328,#4742,.T.);
#13408=EDGE_CURVE('',#10331,#10332,#6467,.T.);
#13409=EDGE_CURVE('',#10332,#10333,#6468,.T.);
#13410=EDGE_CURVE('',#10333,#10334,#6469,.T.);
#13411=EDGE_CURVE('',#10334,#10331,#6470,.T.);
#13412=EDGE_CURVE('',#10335,#10332,#519,.T.);
#13413=EDGE_CURVE('',#10336,#10335,#7042,.T.);
#13414=EDGE_CURVE('',#10333,#10336,#520,.T.);
#13415=EDGE_CURVE('',#10337,#10338,#6471,.T.);
#13416=EDGE_CURVE('',#10338,#10339,#6472,.T.);
#13417=EDGE_CURVE('',#10339,#10340,#6473,.T.);
#13418=EDGE_CURVE('',#10340,#10337,#6474,.T.);
#13419=EDGE_CURVE('',#10339,#10334,#4743,.T.);
#13420=EDGE_CURVE('',#10331,#10338,#4744,.T.);
#13421=EDGE_CURVE('',#10341,#10342,#6475,.T.);
#13422=EDGE_CURVE('',#10342,#10343,#6476,.T.);
#13423=EDGE_CURVE('',#10343,#10344,#6477,.T.);
#13424=EDGE_CURVE('',#10344,#10341,#6478,.T.);
#13425=EDGE_CURVE('',#10345,#10342,#521,.T.);
#13426=EDGE_CURVE('',#10346,#10345,#7043,.T.);
#13427=EDGE_CURVE('',#10343,#10346,#522,.T.);
#13428=EDGE_CURVE('',#10347,#10348,#6479,.T.);
#13429=EDGE_CURVE('',#10348,#10349,#6480,.T.);
#13430=EDGE_CURVE('',#10349,#10350,#6481,.T.);
#13431=EDGE_CURVE('',#10350,#10347,#6482,.T.);
#13432=EDGE_CURVE('',#10349,#10344,#4745,.T.);
#13433=EDGE_CURVE('',#10341,#10348,#4746,.T.);
#13434=EDGE_CURVE('',#10351,#10352,#6483,.T.);
#13435=EDGE_CURVE('',#10352,#10353,#6484,.T.);
#13436=EDGE_CURVE('',#10353,#10354,#6485,.T.);
#13437=EDGE_CURVE('',#10354,#10351,#6486,.T.);
#13438=EDGE_CURVE('',#10355,#10352,#523,.T.);
#13439=EDGE_CURVE('',#10356,#10355,#7044,.T.);
#13440=EDGE_CURVE('',#10353,#10356,#524,.T.);
#13441=EDGE_CURVE('',#10357,#10358,#6487,.T.);
#13442=EDGE_CURVE('',#10358,#10359,#6488,.T.);
#13443=EDGE_CURVE('',#10359,#10360,#6489,.T.);
#13444=EDGE_CURVE('',#10360,#10357,#6490,.T.);
#13445=EDGE_CURVE('',#10359,#10354,#4747,.T.);
#13446=EDGE_CURVE('',#10351,#10358,#4748,.T.);
#13447=EDGE_CURVE('',#10361,#10362,#6491,.T.);
#13448=EDGE_CURVE('',#10362,#10363,#6492,.T.);
#13449=EDGE_CURVE('',#10363,#10364,#6493,.T.);
#13450=EDGE_CURVE('',#10364,#10361,#6494,.T.);
#13451=EDGE_CURVE('',#10365,#10362,#525,.T.);
#13452=EDGE_CURVE('',#10366,#10365,#7045,.T.);
#13453=EDGE_CURVE('',#10363,#10366,#526,.T.);
#13454=EDGE_CURVE('',#10367,#10368,#6495,.T.);
#13455=EDGE_CURVE('',#10368,#10369,#6496,.T.);
#13456=EDGE_CURVE('',#10369,#10370,#6497,.T.);
#13457=EDGE_CURVE('',#10370,#10367,#6498,.T.);
#13458=EDGE_CURVE('',#10369,#10364,#4749,.T.);
#13459=EDGE_CURVE('',#10361,#10368,#4750,.T.);
#13460=EDGE_CURVE('',#10371,#10372,#6499,.T.);
#13461=EDGE_CURVE('',#10372,#10373,#6500,.T.);
#13462=EDGE_CURVE('',#10373,#10374,#6501,.T.);
#13463=EDGE_CURVE('',#10374,#10371,#6502,.T.);
#13464=EDGE_CURVE('',#10375,#10372,#527,.T.);
#13465=EDGE_CURVE('',#10376,#10375,#7046,.T.);
#13466=EDGE_CURVE('',#10373,#10376,#528,.T.);
#13467=EDGE_CURVE('',#10377,#10378,#6503,.T.);
#13468=EDGE_CURVE('',#10378,#10379,#6504,.T.);
#13469=EDGE_CURVE('',#10379,#10380,#6505,.T.);
#13470=EDGE_CURVE('',#10380,#10377,#6506,.T.);
#13471=EDGE_CURVE('',#10379,#10374,#4751,.T.);
#13472=EDGE_CURVE('',#10371,#10378,#4752,.T.);
#13473=EDGE_CURVE('',#10381,#10382,#6507,.T.);
#13474=EDGE_CURVE('',#10382,#10383,#6508,.T.);
#13475=EDGE_CURVE('',#10383,#10384,#6509,.T.);
#13476=EDGE_CURVE('',#10384,#10381,#6510,.T.);
#13477=EDGE_CURVE('',#10385,#10382,#529,.T.);
#13478=EDGE_CURVE('',#10386,#10385,#7047,.T.);
#13479=EDGE_CURVE('',#10383,#10386,#530,.T.);
#13480=EDGE_CURVE('',#10387,#10388,#6511,.T.);
#13481=EDGE_CURVE('',#10388,#10389,#6512,.T.);
#13482=EDGE_CURVE('',#10389,#10390,#6513,.T.);
#13483=EDGE_CURVE('',#10390,#10387,#6514,.T.);
#13484=EDGE_CURVE('',#10389,#10384,#4753,.T.);
#13485=EDGE_CURVE('',#10381,#10388,#4754,.T.);
#13486=EDGE_CURVE('',#10391,#10392,#6515,.T.);
#13487=EDGE_CURVE('',#10392,#10393,#6516,.T.);
#13488=EDGE_CURVE('',#10393,#10394,#6517,.T.);
#13489=EDGE_CURVE('',#10394,#10391,#6518,.T.);
#13490=EDGE_CURVE('',#10395,#10392,#531,.T.);
#13491=EDGE_CURVE('',#10396,#10395,#7048,.T.);
#13492=EDGE_CURVE('',#10393,#10396,#532,.T.);
#13493=EDGE_CURVE('',#10397,#10398,#6519,.T.);
#13494=EDGE_CURVE('',#10398,#10399,#6520,.T.);
#13495=EDGE_CURVE('',#10399,#10400,#6521,.T.);
#13496=EDGE_CURVE('',#10400,#10397,#6522,.T.);
#13497=EDGE_CURVE('',#10399,#10394,#4755,.T.);
#13498=EDGE_CURVE('',#10391,#10398,#4756,.T.);
#13499=EDGE_CURVE('',#10401,#10402,#6523,.T.);
#13500=EDGE_CURVE('',#10402,#10403,#6524,.T.);
#13501=EDGE_CURVE('',#10403,#10404,#6525,.T.);
#13502=EDGE_CURVE('',#10404,#10401,#6526,.T.);
#13503=EDGE_CURVE('',#10405,#10402,#533,.T.);
#13504=EDGE_CURVE('',#10406,#10405,#7049,.T.);
#13505=EDGE_CURVE('',#10403,#10406,#534,.T.);
#13506=EDGE_CURVE('',#10407,#10408,#6527,.T.);
#13507=EDGE_CURVE('',#10408,#10409,#6528,.T.);
#13508=EDGE_CURVE('',#10409,#10410,#6529,.T.);
#13509=EDGE_CURVE('',#10410,#10407,#6530,.T.);
#13510=EDGE_CURVE('',#10409,#10404,#4757,.T.);
#13511=EDGE_CURVE('',#10401,#10408,#4758,.T.);
#13512=EDGE_CURVE('',#10411,#10412,#6531,.T.);
#13513=EDGE_CURVE('',#10412,#10413,#6532,.T.);
#13514=EDGE_CURVE('',#10413,#10414,#6533,.T.);
#13515=EDGE_CURVE('',#10414,#10411,#6534,.T.);
#13516=EDGE_CURVE('',#10415,#10412,#535,.T.);
#13517=EDGE_CURVE('',#10416,#10415,#7050,.T.);
#13518=EDGE_CURVE('',#10413,#10416,#536,.T.);
#13519=EDGE_CURVE('',#10417,#10418,#6535,.T.);
#13520=EDGE_CURVE('',#10418,#10419,#6536,.T.);
#13521=EDGE_CURVE('',#10419,#10420,#6537,.T.);
#13522=EDGE_CURVE('',#10420,#10417,#6538,.T.);
#13523=EDGE_CURVE('',#10419,#10414,#4759,.T.);
#13524=EDGE_CURVE('',#10411,#10418,#4760,.T.);
#13525=EDGE_CURVE('',#10421,#10422,#6539,.T.);
#13526=EDGE_CURVE('',#10422,#10423,#6540,.T.);
#13527=EDGE_CURVE('',#10423,#10424,#6541,.T.);
#13528=EDGE_CURVE('',#10424,#10421,#6542,.T.);
#13529=EDGE_CURVE('',#10425,#10422,#537,.T.);
#13530=EDGE_CURVE('',#10426,#10425,#7051,.T.);
#13531=EDGE_CURVE('',#10423,#10426,#538,.T.);
#13532=EDGE_CURVE('',#10427,#10428,#6543,.T.);
#13533=EDGE_CURVE('',#10428,#10429,#6544,.T.);
#13534=EDGE_CURVE('',#10429,#10430,#6545,.T.);
#13535=EDGE_CURVE('',#10430,#10427,#6546,.T.);
#13536=EDGE_CURVE('',#10429,#10424,#4761,.T.);
#13537=EDGE_CURVE('',#10421,#10428,#4762,.T.);
#13538=EDGE_CURVE('',#10431,#10432,#6547,.T.);
#13539=EDGE_CURVE('',#10432,#10433,#6548,.T.);
#13540=EDGE_CURVE('',#10433,#10434,#6549,.T.);
#13541=EDGE_CURVE('',#10434,#10431,#6550,.T.);
#13542=EDGE_CURVE('',#10435,#10432,#539,.T.);
#13543=EDGE_CURVE('',#10436,#10435,#7052,.T.);
#13544=EDGE_CURVE('',#10433,#10436,#540,.T.);
#13545=EDGE_CURVE('',#10437,#10438,#6551,.T.);
#13546=EDGE_CURVE('',#10438,#10439,#6552,.T.);
#13547=EDGE_CURVE('',#10439,#10440,#6553,.T.);
#13548=EDGE_CURVE('',#10440,#10437,#6554,.T.);
#13549=EDGE_CURVE('',#10439,#10434,#4763,.T.);
#13550=EDGE_CURVE('',#10431,#10438,#4764,.T.);
#13551=EDGE_CURVE('',#10441,#10442,#6555,.T.);
#13552=EDGE_CURVE('',#10442,#10443,#6556,.T.);
#13553=EDGE_CURVE('',#10443,#10444,#6557,.T.);
#13554=EDGE_CURVE('',#10444,#10441,#6558,.T.);
#13555=EDGE_CURVE('',#10445,#10442,#541,.T.);
#13556=EDGE_CURVE('',#10446,#10445,#7053,.T.);
#13557=EDGE_CURVE('',#10443,#10446,#542,.T.);
#13558=EDGE_CURVE('',#10447,#10448,#6559,.T.);
#13559=EDGE_CURVE('',#10448,#10449,#6560,.T.);
#13560=EDGE_CURVE('',#10449,#10450,#6561,.T.);
#13561=EDGE_CURVE('',#10450,#10447,#6562,.T.);
#13562=EDGE_CURVE('',#10449,#10444,#4765,.T.);
#13563=EDGE_CURVE('',#10441,#10448,#4766,.T.);
#13564=EDGE_CURVE('',#10451,#10452,#6563,.T.);
#13565=EDGE_CURVE('',#10452,#10453,#6564,.T.);
#13566=EDGE_CURVE('',#10453,#10454,#6565,.T.);
#13567=EDGE_CURVE('',#10454,#10451,#6566,.T.);
#13568=EDGE_CURVE('',#10455,#10452,#543,.T.);
#13569=EDGE_CURVE('',#10456,#10455,#7054,.T.);
#13570=EDGE_CURVE('',#10453,#10456,#544,.T.);
#13571=EDGE_CURVE('',#10457,#10458,#6567,.T.);
#13572=EDGE_CURVE('',#10458,#10459,#6568,.T.);
#13573=EDGE_CURVE('',#10459,#10460,#6569,.T.);
#13574=EDGE_CURVE('',#10460,#10457,#6570,.T.);
#13575=EDGE_CURVE('',#10459,#10454,#4767,.T.);
#13576=EDGE_CURVE('',#10451,#10458,#4768,.T.);
#13577=EDGE_CURVE('',#10461,#9760,#545,.T.);
#13578=EDGE_CURVE('',#10462,#10461,#7055,.T.);
#13579=EDGE_CURVE('',#9757,#10462,#546,.T.);
#13580=EDGE_CURVE('',#10463,#9770,#547,.T.);
#13581=EDGE_CURVE('',#10464,#10463,#7056,.T.);
#13582=EDGE_CURVE('',#9767,#10464,#548,.T.);
#13583=EDGE_CURVE('',#10465,#9780,#549,.T.);
#13584=EDGE_CURVE('',#10466,#10465,#7057,.T.);
#13585=EDGE_CURVE('',#9777,#10466,#550,.T.);
#13586=EDGE_CURVE('',#10467,#9790,#551,.T.);
#13587=EDGE_CURVE('',#10468,#10467,#7058,.T.);
#13588=EDGE_CURVE('',#9787,#10468,#552,.T.);
#13589=EDGE_CURVE('',#10469,#9800,#553,.T.);
#13590=EDGE_CURVE('',#10470,#10469,#7059,.T.);
#13591=EDGE_CURVE('',#9797,#10470,#554,.T.);
#13592=EDGE_CURVE('',#10471,#9810,#555,.T.);
#13593=EDGE_CURVE('',#10472,#10471,#7060,.T.);
#13594=EDGE_CURVE('',#9807,#10472,#556,.T.);
#13595=EDGE_CURVE('',#10473,#9820,#557,.T.);
#13596=EDGE_CURVE('',#10474,#10473,#7061,.T.);
#13597=EDGE_CURVE('',#9817,#10474,#558,.T.);
#13598=EDGE_CURVE('',#10475,#9830,#559,.T.);
#13599=EDGE_CURVE('',#10476,#10475,#7062,.T.);
#13600=EDGE_CURVE('',#9827,#10476,#560,.T.);
#13601=EDGE_CURVE('',#10477,#9840,#561,.T.);
#13602=EDGE_CURVE('',#10478,#10477,#7063,.T.);
#13603=EDGE_CURVE('',#9837,#10478,#562,.T.);
#13604=EDGE_CURVE('',#10479,#9850,#563,.T.);
#13605=EDGE_CURVE('',#10480,#10479,#7064,.T.);
#13606=EDGE_CURVE('',#9847,#10480,#564,.T.);
#13607=EDGE_CURVE('',#10481,#9860,#565,.T.);
#13608=EDGE_CURVE('',#10482,#10481,#7065,.T.);
#13609=EDGE_CURVE('',#9857,#10482,#566,.T.);
#13610=EDGE_CURVE('',#10483,#9870,#567,.T.);
#13611=EDGE_CURVE('',#10484,#10483,#7066,.T.);
#13612=EDGE_CURVE('',#9867,#10484,#568,.T.);
#13613=EDGE_CURVE('',#10485,#9880,#569,.T.);
#13614=EDGE_CURVE('',#10486,#10485,#7067,.T.);
#13615=EDGE_CURVE('',#9877,#10486,#570,.T.);
#13616=EDGE_CURVE('',#10487,#9890,#571,.T.);
#13617=EDGE_CURVE('',#10488,#10487,#7068,.T.);
#13618=EDGE_CURVE('',#9887,#10488,#572,.T.);
#13619=EDGE_CURVE('',#10489,#9900,#573,.T.);
#13620=EDGE_CURVE('',#10490,#10489,#7069,.T.);
#13621=EDGE_CURVE('',#9897,#10490,#574,.T.);
#13622=EDGE_CURVE('',#10491,#9910,#575,.T.);
#13623=EDGE_CURVE('',#10492,#10491,#7070,.T.);
#13624=EDGE_CURVE('',#9907,#10492,#576,.T.);
#13625=EDGE_CURVE('',#10493,#9920,#577,.T.);
#13626=EDGE_CURVE('',#10494,#10493,#7071,.T.);
#13627=EDGE_CURVE('',#9917,#10494,#578,.T.);
#13628=EDGE_CURVE('',#10495,#9930,#579,.T.);
#13629=EDGE_CURVE('',#10496,#10495,#7072,.T.);
#13630=EDGE_CURVE('',#9927,#10496,#580,.T.);
#13631=EDGE_CURVE('',#10497,#9940,#581,.T.);
#13632=EDGE_CURVE('',#10498,#10497,#7073,.T.);
#13633=EDGE_CURVE('',#9937,#10498,#582,.T.);
#13634=EDGE_CURVE('',#10499,#9950,#583,.T.);
#13635=EDGE_CURVE('',#10500,#10499,#7074,.T.);
#13636=EDGE_CURVE('',#9947,#10500,#584,.T.);
#13637=EDGE_CURVE('',#10501,#9960,#585,.T.);
#13638=EDGE_CURVE('',#10502,#10501,#7075,.T.);
#13639=EDGE_CURVE('',#9957,#10502,#586,.T.);
#13640=EDGE_CURVE('',#10503,#9970,#587,.T.);
#13641=EDGE_CURVE('',#10504,#10503,#7076,.T.);
#13642=EDGE_CURVE('',#9967,#10504,#588,.T.);
#13643=EDGE_CURVE('',#10505,#9980,#589,.T.);
#13644=EDGE_CURVE('',#10506,#10505,#7077,.T.);
#13645=EDGE_CURVE('',#9977,#10506,#590,.T.);
#13646=EDGE_CURVE('',#10507,#9990,#591,.T.);
#13647=EDGE_CURVE('',#10508,#10507,#7078,.T.);
#13648=EDGE_CURVE('',#9987,#10508,#592,.T.);
#13649=EDGE_CURVE('',#10509,#10000,#593,.T.);
#13650=EDGE_CURVE('',#10510,#10509,#7079,.T.);
#13651=EDGE_CURVE('',#9997,#10510,#594,.T.);
#13652=EDGE_CURVE('',#10511,#10010,#595,.T.);
#13653=EDGE_CURVE('',#10512,#10511,#7080,.T.);
#13654=EDGE_CURVE('',#10007,#10512,#596,.T.);
#13655=EDGE_CURVE('',#10513,#10020,#597,.T.);
#13656=EDGE_CURVE('',#10514,#10513,#7081,.T.);
#13657=EDGE_CURVE('',#10017,#10514,#598,.T.);
#13658=EDGE_CURVE('',#10515,#10030,#599,.T.);
#13659=EDGE_CURVE('',#10516,#10515,#7082,.T.);
#13660=EDGE_CURVE('',#10027,#10516,#600,.T.);
#13661=EDGE_CURVE('',#10517,#10040,#601,.T.);
#13662=EDGE_CURVE('',#10518,#10517,#7083,.T.);
#13663=EDGE_CURVE('',#10037,#10518,#602,.T.);
#13664=EDGE_CURVE('',#10519,#10050,#603,.T.);
#13665=EDGE_CURVE('',#10520,#10519,#7084,.T.);
#13666=EDGE_CURVE('',#10047,#10520,#604,.T.);
#13667=EDGE_CURVE('',#10521,#10060,#605,.T.);
#13668=EDGE_CURVE('',#10522,#10521,#7085,.T.);
#13669=EDGE_CURVE('',#10057,#10522,#606,.T.);
#13670=EDGE_CURVE('',#10523,#10070,#607,.T.);
#13671=EDGE_CURVE('',#10524,#10523,#7086,.T.);
#13672=EDGE_CURVE('',#10067,#10524,#608,.T.);
#13673=EDGE_CURVE('',#10525,#10080,#609,.T.);
#13674=EDGE_CURVE('',#10526,#10525,#7087,.T.);
#13675=EDGE_CURVE('',#10077,#10526,#610,.T.);
#13676=EDGE_CURVE('',#10527,#10090,#611,.T.);
#13677=EDGE_CURVE('',#10528,#10527,#7088,.T.);
#13678=EDGE_CURVE('',#10087,#10528,#612,.T.);
#13679=EDGE_CURVE('',#10529,#10100,#613,.T.);
#13680=EDGE_CURVE('',#10530,#10529,#7089,.T.);
#13681=EDGE_CURVE('',#10097,#10530,#614,.T.);
#13682=EDGE_CURVE('',#10531,#10110,#615,.T.);
#13683=EDGE_CURVE('',#10532,#10531,#7090,.T.);
#13684=EDGE_CURVE('',#10107,#10532,#616,.T.);
#13685=EDGE_CURVE('',#10533,#10120,#617,.T.);
#13686=EDGE_CURVE('',#10534,#10533,#7091,.T.);
#13687=EDGE_CURVE('',#10117,#10534,#618,.T.);
#13688=EDGE_CURVE('',#10535,#10130,#619,.T.);
#13689=EDGE_CURVE('',#10536,#10535,#7092,.T.);
#13690=EDGE_CURVE('',#10127,#10536,#620,.T.);
#13691=EDGE_CURVE('',#10537,#10140,#621,.T.);
#13692=EDGE_CURVE('',#10538,#10537,#7093,.T.);
#13693=EDGE_CURVE('',#10137,#10538,#622,.T.);
#13694=EDGE_CURVE('',#10539,#10150,#623,.T.);
#13695=EDGE_CURVE('',#10540,#10539,#7094,.T.);
#13696=EDGE_CURVE('',#10147,#10540,#624,.T.);
#13697=EDGE_CURVE('',#10541,#10160,#625,.T.);
#13698=EDGE_CURVE('',#10542,#10541,#7095,.T.);
#13699=EDGE_CURVE('',#10157,#10542,#626,.T.);
#13700=EDGE_CURVE('',#10543,#10170,#627,.T.);
#13701=EDGE_CURVE('',#10544,#10543,#7096,.T.);
#13702=EDGE_CURVE('',#10167,#10544,#628,.T.);
#13703=EDGE_CURVE('',#10545,#10180,#629,.T.);
#13704=EDGE_CURVE('',#10546,#10545,#7097,.T.);
#13705=EDGE_CURVE('',#10177,#10546,#630,.T.);
#13706=EDGE_CURVE('',#10547,#10190,#631,.T.);
#13707=EDGE_CURVE('',#10548,#10547,#7098,.T.);
#13708=EDGE_CURVE('',#10187,#10548,#632,.T.);
#13709=EDGE_CURVE('',#10549,#10200,#633,.T.);
#13710=EDGE_CURVE('',#10550,#10549,#7099,.T.);
#13711=EDGE_CURVE('',#10197,#10550,#634,.T.);
#13712=EDGE_CURVE('',#10551,#10210,#635,.T.);
#13713=EDGE_CURVE('',#10552,#10551,#7100,.T.);
#13714=EDGE_CURVE('',#10207,#10552,#636,.T.);
#13715=EDGE_CURVE('',#10553,#10220,#637,.T.);
#13716=EDGE_CURVE('',#10554,#10553,#7101,.T.);
#13717=EDGE_CURVE('',#10217,#10554,#638,.T.);
#13718=EDGE_CURVE('',#10555,#10230,#639,.T.);
#13719=EDGE_CURVE('',#10556,#10555,#7102,.T.);
#13720=EDGE_CURVE('',#10227,#10556,#640,.T.);
#13721=EDGE_CURVE('',#10557,#10240,#641,.T.);
#13722=EDGE_CURVE('',#10558,#10557,#7103,.T.);
#13723=EDGE_CURVE('',#10237,#10558,#642,.T.);
#13724=EDGE_CURVE('',#10559,#10250,#643,.T.);
#13725=EDGE_CURVE('',#10560,#10559,#7104,.T.);
#13726=EDGE_CURVE('',#10247,#10560,#644,.T.);
#13727=EDGE_CURVE('',#10561,#10260,#645,.T.);
#13728=EDGE_CURVE('',#10562,#10561,#7105,.T.);
#13729=EDGE_CURVE('',#10257,#10562,#646,.T.);
#13730=EDGE_CURVE('',#10563,#10270,#647,.T.);
#13731=EDGE_CURVE('',#10564,#10563,#7106,.T.);
#13732=EDGE_CURVE('',#10267,#10564,#648,.T.);
#13733=EDGE_CURVE('',#10565,#10280,#649,.T.);
#13734=EDGE_CURVE('',#10566,#10565,#7107,.T.);
#13735=EDGE_CURVE('',#10277,#10566,#650,.T.);
#13736=EDGE_CURVE('',#10567,#10290,#651,.T.);
#13737=EDGE_CURVE('',#10568,#10567,#7108,.T.);
#13738=EDGE_CURVE('',#10287,#10568,#652,.T.);
#13739=EDGE_CURVE('',#10569,#10300,#653,.T.);
#13740=EDGE_CURVE('',#10570,#10569,#7109,.T.);
#13741=EDGE_CURVE('',#10297,#10570,#654,.T.);
#13742=EDGE_CURVE('',#10571,#10310,#655,.T.);
#13743=EDGE_CURVE('',#10572,#10571,#7110,.T.);
#13744=EDGE_CURVE('',#10307,#10572,#656,.T.);
#13745=EDGE_CURVE('',#10573,#10320,#657,.T.);
#13746=EDGE_CURVE('',#10574,#10573,#7111,.T.);
#13747=EDGE_CURVE('',#10317,#10574,#658,.T.);
#13748=EDGE_CURVE('',#10575,#10330,#659,.T.);
#13749=EDGE_CURVE('',#10576,#10575,#7112,.T.);
#13750=EDGE_CURVE('',#10327,#10576,#660,.T.);
#13751=EDGE_CURVE('',#10577,#10340,#661,.T.);
#13752=EDGE_CURVE('',#10578,#10577,#7113,.T.);
#13753=EDGE_CURVE('',#10337,#10578,#662,.T.);
#13754=EDGE_CURVE('',#10579,#10350,#663,.T.);
#13755=EDGE_CURVE('',#10580,#10579,#7114,.T.);
#13756=EDGE_CURVE('',#10347,#10580,#664,.T.);
#13757=EDGE_CURVE('',#10581,#10360,#665,.T.);
#13758=EDGE_CURVE('',#10582,#10581,#7115,.T.);
#13759=EDGE_CURVE('',#10357,#10582,#666,.T.);
#13760=EDGE_CURVE('',#10583,#10370,#667,.T.);
#13761=EDGE_CURVE('',#10584,#10583,#7116,.T.);
#13762=EDGE_CURVE('',#10367,#10584,#668,.T.);
#13763=EDGE_CURVE('',#10585,#10380,#669,.T.);
#13764=EDGE_CURVE('',#10586,#10585,#7117,.T.);
#13765=EDGE_CURVE('',#10377,#10586,#670,.T.);
#13766=EDGE_CURVE('',#10587,#10390,#671,.T.);
#13767=EDGE_CURVE('',#10588,#10587,#7118,.T.);
#13768=EDGE_CURVE('',#10387,#10588,#672,.T.);
#13769=EDGE_CURVE('',#10589,#10400,#673,.T.);
#13770=EDGE_CURVE('',#10590,#10589,#7119,.T.);
#13771=EDGE_CURVE('',#10397,#10590,#674,.T.);
#13772=EDGE_CURVE('',#10591,#10410,#675,.T.);
#13773=EDGE_CURVE('',#10592,#10591,#7120,.T.);
#13774=EDGE_CURVE('',#10407,#10592,#676,.T.);
#13775=EDGE_CURVE('',#10593,#10420,#677,.T.);
#13776=EDGE_CURVE('',#10594,#10593,#7121,.T.);
#13777=EDGE_CURVE('',#10417,#10594,#678,.T.);
#13778=EDGE_CURVE('',#10595,#10430,#679,.T.);
#13779=EDGE_CURVE('',#10596,#10595,#7122,.T.);
#13780=EDGE_CURVE('',#10427,#10596,#680,.T.);
#13781=EDGE_CURVE('',#10597,#10440,#681,.T.);
#13782=EDGE_CURVE('',#10598,#10597,#7123,.T.);
#13783=EDGE_CURVE('',#10437,#10598,#682,.T.);
#13784=EDGE_CURVE('',#10599,#10450,#683,.T.);
#13785=EDGE_CURVE('',#10600,#10599,#7124,.T.);
#13786=EDGE_CURVE('',#10447,#10600,#684,.T.);
#13787=EDGE_CURVE('',#10601,#10460,#685,.T.);
#13788=EDGE_CURVE('',#10602,#10601,#7125,.T.);
#13789=EDGE_CURVE('',#10457,#10602,#686,.T.);
#13790=EDGE_CURVE('',#10455,#10603,#4769,.T.);
#13791=EDGE_CURVE('',#10603,#10604,#7126,.T.);
#13792=EDGE_CURVE('',#10456,#10604,#4770,.T.);
#13793=EDGE_CURVE('',#10445,#10602,#4771,.T.);
#13794=EDGE_CURVE('',#10446,#10601,#4772,.T.);
#13795=EDGE_CURVE('',#10435,#10600,#4773,.T.);
#13796=EDGE_CURVE('',#10436,#10599,#4774,.T.);
#13797=EDGE_CURVE('',#10425,#10598,#4775,.T.);
#13798=EDGE_CURVE('',#10426,#10597,#4776,.T.);
#13799=EDGE_CURVE('',#10415,#10596,#4777,.T.);
#13800=EDGE_CURVE('',#10416,#10595,#4778,.T.);
#13801=EDGE_CURVE('',#10405,#10594,#4779,.T.);
#13802=EDGE_CURVE('',#10406,#10593,#4780,.T.);
#13803=EDGE_CURVE('',#10395,#10592,#4781,.T.);
#13804=EDGE_CURVE('',#10396,#10591,#4782,.T.);
#13805=EDGE_CURVE('',#10385,#10590,#4783,.T.);
#13806=EDGE_CURVE('',#10386,#10589,#4784,.T.);
#13807=EDGE_CURVE('',#10375,#10588,#4785,.T.);
#13808=EDGE_CURVE('',#10376,#10587,#4786,.T.);
#13809=EDGE_CURVE('',#10365,#10586,#4787,.T.);
#13810=EDGE_CURVE('',#10366,#10585,#4788,.T.);
#13811=EDGE_CURVE('',#10355,#10584,#4789,.T.);
#13812=EDGE_CURVE('',#10356,#10583,#4790,.T.);
#13813=EDGE_CURVE('',#10345,#10582,#4791,.T.);
#13814=EDGE_CURVE('',#10346,#10581,#4792,.T.);
#13815=EDGE_CURVE('',#10335,#10580,#4793,.T.);
#13816=EDGE_CURVE('',#10336,#10579,#4794,.T.);
#13817=EDGE_CURVE('',#10325,#10578,#4795,.T.);
#13818=EDGE_CURVE('',#10326,#10577,#4796,.T.);
#13819=EDGE_CURVE('',#10315,#10576,#4797,.T.);
#13820=EDGE_CURVE('',#10316,#10575,#4798,.T.);
#13821=EDGE_CURVE('',#10305,#10574,#4799,.T.);
#13822=EDGE_CURVE('',#10306,#10573,#4800,.T.);
#13823=EDGE_CURVE('',#10295,#10572,#4801,.T.);
#13824=EDGE_CURVE('',#10296,#10571,#4802,.T.);
#13825=EDGE_CURVE('',#10285,#10570,#4803,.T.);
#13826=EDGE_CURVE('',#10286,#10569,#4804,.T.);
#13827=EDGE_CURVE('',#10275,#10568,#4805,.T.);
#13828=EDGE_CURVE('',#10276,#10567,#4806,.T.);
#13829=EDGE_CURVE('',#10265,#10566,#4807,.T.);
#13830=EDGE_CURVE('',#10266,#10565,#4808,.T.);
#13831=EDGE_CURVE('',#10255,#10564,#4809,.T.);
#13832=EDGE_CURVE('',#10256,#10563,#4810,.T.);
#13833=EDGE_CURVE('',#10245,#10562,#4811,.T.);
#13834=EDGE_CURVE('',#10246,#10561,#4812,.T.);
#13835=EDGE_CURVE('',#10235,#10560,#4813,.T.);
#13836=EDGE_CURVE('',#10236,#10559,#4814,.T.);
#13837=EDGE_CURVE('',#10225,#10558,#4815,.T.);
#13838=EDGE_CURVE('',#10226,#10557,#4816,.T.);
#13839=EDGE_CURVE('',#10215,#10556,#4817,.T.);
#13840=EDGE_CURVE('',#10216,#10555,#4818,.T.);
#13841=EDGE_CURVE('',#10205,#10554,#4819,.T.);
#13842=EDGE_CURVE('',#10206,#10553,#4820,.T.);
#13843=EDGE_CURVE('',#10195,#10552,#4821,.T.);
#13844=EDGE_CURVE('',#10196,#10551,#4822,.T.);
#13845=EDGE_CURVE('',#10185,#10550,#4823,.T.);
#13846=EDGE_CURVE('',#10186,#10549,#4824,.T.);
#13847=EDGE_CURVE('',#10175,#10548,#4825,.T.);
#13848=EDGE_CURVE('',#10176,#10547,#4826,.T.);
#13849=EDGE_CURVE('',#10165,#10546,#4827,.T.);
#13850=EDGE_CURVE('',#10166,#10545,#4828,.T.);
#13851=EDGE_CURVE('',#10155,#10544,#4829,.T.);
#13852=EDGE_CURVE('',#10156,#10543,#4830,.T.);
#13853=EDGE_CURVE('',#10145,#10542,#4831,.T.);
#13854=EDGE_CURVE('',#10146,#10541,#4832,.T.);
#13855=EDGE_CURVE('',#10135,#10540,#4833,.T.);
#13856=EDGE_CURVE('',#10136,#10539,#4834,.T.);
#13857=EDGE_CURVE('',#10125,#10538,#4835,.T.);
#13858=EDGE_CURVE('',#10126,#10537,#4836,.T.);
#13859=EDGE_CURVE('',#10115,#10536,#4837,.T.);
#13860=EDGE_CURVE('',#10116,#10535,#4838,.T.);
#13861=EDGE_CURVE('',#10105,#10534,#4839,.T.);
#13862=EDGE_CURVE('',#10106,#10533,#4840,.T.);
#13863=EDGE_CURVE('',#10095,#10532,#4841,.T.);
#13864=EDGE_CURVE('',#10096,#10531,#4842,.T.);
#13865=EDGE_CURVE('',#10085,#10530,#4843,.T.);
#13866=EDGE_CURVE('',#10086,#10529,#4844,.T.);
#13867=EDGE_CURVE('',#10075,#10528,#4845,.T.);
#13868=EDGE_CURVE('',#10076,#10527,#4846,.T.);
#13869=EDGE_CURVE('',#10065,#10526,#4847,.T.);
#13870=EDGE_CURVE('',#10066,#10525,#4848,.T.);
#13871=EDGE_CURVE('',#10055,#10524,#4849,.T.);
#13872=EDGE_CURVE('',#10056,#10523,#4850,.T.);
#13873=EDGE_CURVE('',#10045,#10522,#4851,.T.);
#13874=EDGE_CURVE('',#10046,#10521,#4852,.T.);
#13875=EDGE_CURVE('',#10035,#10520,#4853,.T.);
#13876=EDGE_CURVE('',#10036,#10519,#4854,.T.);
#13877=EDGE_CURVE('',#10025,#10518,#4855,.T.);
#13878=EDGE_CURVE('',#10026,#10517,#4856,.T.);
#13879=EDGE_CURVE('',#10015,#10516,#4857,.T.);
#13880=EDGE_CURVE('',#10016,#10515,#4858,.T.);
#13881=EDGE_CURVE('',#10005,#10514,#4859,.T.);
#13882=EDGE_CURVE('',#10006,#10513,#4860,.T.);
#13883=EDGE_CURVE('',#9995,#10512,#4861,.T.);
#13884=EDGE_CURVE('',#9996,#10511,#4862,.T.);
#13885=EDGE_CURVE('',#9985,#10510,#4863,.T.);
#13886=EDGE_CURVE('',#9986,#10509,#4864,.T.);
#13887=EDGE_CURVE('',#9975,#10508,#4865,.T.);
#13888=EDGE_CURVE('',#9976,#10507,#4866,.T.);
#13889=EDGE_CURVE('',#9965,#10506,#4867,.T.);
#13890=EDGE_CURVE('',#9966,#10505,#4868,.T.);
#13891=EDGE_CURVE('',#9955,#10504,#4869,.T.);
#13892=EDGE_CURVE('',#9956,#10503,#4870,.T.);
#13893=EDGE_CURVE('',#9945,#10502,#4871,.T.);
#13894=EDGE_CURVE('',#9946,#10501,#4872,.T.);
#13895=EDGE_CURVE('',#9935,#10500,#4873,.T.);
#13896=EDGE_CURVE('',#9936,#10499,#4874,.T.);
#13897=EDGE_CURVE('',#9925,#10498,#4875,.T.);
#13898=EDGE_CURVE('',#9926,#10497,#4876,.T.);
#13899=EDGE_CURVE('',#9915,#10496,#4877,.T.);
#13900=EDGE_CURVE('',#9916,#10495,#4878,.T.);
#13901=EDGE_CURVE('',#9905,#10494,#4879,.T.);
#13902=EDGE_CURVE('',#9906,#10493,#4880,.T.);
#13903=EDGE_CURVE('',#9895,#10492,#4881,.T.);
#13904=EDGE_CURVE('',#9896,#10491,#4882,.T.);
#13905=EDGE_CURVE('',#9885,#10490,#4883,.T.);
#13906=EDGE_CURVE('',#9886,#10489,#4884,.T.);
#13907=EDGE_CURVE('',#9875,#10488,#4885,.T.);
#13908=EDGE_CURVE('',#9876,#10487,#4886,.T.);
#13909=EDGE_CURVE('',#9865,#10486,#4887,.T.);
#13910=EDGE_CURVE('',#9866,#10485,#4888,.T.);
#13911=EDGE_CURVE('',#9855,#10484,#4889,.T.);
#13912=EDGE_CURVE('',#9856,#10483,#4890,.T.);
#13913=EDGE_CURVE('',#9845,#10482,#4891,.T.);
#13914=EDGE_CURVE('',#9846,#10481,#4892,.T.);
#13915=EDGE_CURVE('',#9835,#10480,#4893,.T.);
#13916=EDGE_CURVE('',#9836,#10479,#4894,.T.);
#13917=EDGE_CURVE('',#9825,#10478,#4895,.T.);
#13918=EDGE_CURVE('',#9826,#10477,#4896,.T.);
#13919=EDGE_CURVE('',#9815,#10476,#4897,.T.);
#13920=EDGE_CURVE('',#9816,#10475,#4898,.T.);
#13921=EDGE_CURVE('',#9805,#10474,#4899,.T.);
#13922=EDGE_CURVE('',#9806,#10473,#4900,.T.);
#13923=EDGE_CURVE('',#9795,#10472,#4901,.T.);
#13924=EDGE_CURVE('',#9796,#10471,#4902,.T.);
#13925=EDGE_CURVE('',#9785,#10470,#4903,.T.);
#13926=EDGE_CURVE('',#9786,#10469,#4904,.T.);
#13927=EDGE_CURVE('',#9775,#10468,#4905,.T.);
#13928=EDGE_CURVE('',#9776,#10467,#4906,.T.);
#13929=EDGE_CURVE('',#9765,#10466,#4907,.T.);
#13930=EDGE_CURVE('',#9766,#10465,#4908,.T.);
#13931=EDGE_CURVE('',#10605,#10461,#4909,.T.);
#13932=EDGE_CURVE('',#10605,#10606,#7127,.T.);
#13933=EDGE_CURVE('',#10606,#10462,#4910,.T.);
#13934=EDGE_CURVE('',#10607,#10608,#6571,.T.);
#13935=EDGE_CURVE('',#10608,#10609,#6572,.T.);
#13936=EDGE_CURVE('',#10609,#10610,#6573,.T.);
#13937=EDGE_CURVE('',#10610,#10607,#6574,.T.);
#13938=EDGE_CURVE('',#10606,#10608,#687,.T.);
#13939=EDGE_CURVE('',#10609,#10605,#688,.T.);
#13940=EDGE_CURVE('',#10611,#10612,#6575,.T.);
#13941=EDGE_CURVE('',#10612,#10613,#6576,.T.);
#13942=EDGE_CURVE('',#10613,#10614,#6577,.T.);
#13943=EDGE_CURVE('',#10614,#10611,#6578,.T.);
#13944=EDGE_CURVE('',#10613,#10610,#4911,.T.);
#13945=EDGE_CURVE('',#10607,#10612,#4912,.T.);
#13946=EDGE_CURVE('',#10604,#10614,#689,.T.);
#13947=EDGE_CURVE('',#10611,#10603,#690,.T.);
#13948=EDGE_CURVE('',#10615,#10615,#4913,.T.);
#13949=EDGE_CURVE('',#9756,#10463,#4914,.T.);
#13950=EDGE_CURVE('',#9755,#10464,#4915,.T.);
#13951=EDGE_CURVE('',#10615,#9743,#7128,.T.);
#13952=EDGE_CURVE('',#9744,#10616,#7129,.T.);
#13953=EDGE_CURVE('',#10616,#10616,#4916,.T.);
#13954=EDGE_CURVE('',#10617,#10618,#7130,.T.);
#13955=EDGE_CURVE('',#10619,#10617,#7131,.T.);
#13956=EDGE_CURVE('',#10620,#10619,#7132,.T.);
#13957=EDGE_CURVE('',#10618,#10620,#7133,.T.);
#13958=EDGE_CURVE('',#10621,#10622,#7134,.T.);
#13959=EDGE_CURVE('',#10623,#10621,#7135,.T.);
#13960=EDGE_CURVE('',#10623,#10624,#7136,.T.);
#13961=EDGE_CURVE('',#10622,#10624,#7137,.T.);
#13962=EDGE_CURVE('',#10620,#10623,#7138,.T.);
#13963=EDGE_CURVE('',#10624,#10619,#7139,.T.);
#13964=EDGE_CURVE('',#10621,#10618,#4917,.T.);
#13965=EDGE_CURVE('',#10622,#10617,#4918,.T.);
#13966=EDGE_CURVE('',#10625,#10626,#691,.T.);
#13967=EDGE_CURVE('',#10626,#10627,#4919,.T.);
#13968=EDGE_CURVE('',#10627,#10628,#692,.T.);
#13969=EDGE_CURVE('',#10628,#10629,#7140,.T.);
#13970=EDGE_CURVE('',#10630,#10629,#4920,.T.);
#13971=EDGE_CURVE('',#10630,#10631,#4921,.T.);
#13972=EDGE_CURVE('',#10632,#10631,#4922,.T.);
#13973=EDGE_CURVE('',#10632,#10633,#7141,.T.);
#13974=EDGE_CURVE('',#10633,#10634,#693,.T.);
#13975=EDGE_CURVE('',#10634,#10635,#4923,.T.);
#13976=EDGE_CURVE('',#10635,#10636,#694,.T.);
#13977=EDGE_CURVE('',#10636,#10637,#7142,.T.);
#13978=EDGE_CURVE('',#10638,#10637,#4924,.T.);
#13979=EDGE_CURVE('',#10638,#10639,#4925,.T.);
#13980=EDGE_CURVE('',#10640,#10639,#4926,.T.);
#13981=EDGE_CURVE('',#10640,#10641,#7143,.T.);
#13982=EDGE_CURVE('',#10641,#10642,#695,.T.);
#13983=EDGE_CURVE('',#10642,#10643,#4927,.T.);
#13984=EDGE_CURVE('',#10643,#10644,#696,.T.);
#13985=EDGE_CURVE('',#10644,#10645,#7144,.T.);
#13986=EDGE_CURVE('',#10646,#10645,#4928,.T.);
#13987=EDGE_CURVE('',#10646,#10647,#4929,.T.);
#13988=EDGE_CURVE('',#10648,#10647,#4930,.T.);
#13989=EDGE_CURVE('',#10648,#10649,#7145,.T.);
#13990=EDGE_CURVE('',#10649,#10650,#697,.T.);
#13991=EDGE_CURVE('',#10650,#10651,#4931,.T.);
#13992=EDGE_CURVE('',#10651,#10652,#698,.T.);
#13993=EDGE_CURVE('',#10652,#10653,#7146,.T.);
#13994=EDGE_CURVE('',#10654,#10653,#4932,.T.);
#13995=EDGE_CURVE('',#10654,#10655,#4933,.T.);
#13996=EDGE_CURVE('',#10656,#10655,#4934,.T.);
#13997=EDGE_CURVE('',#10656,#10657,#7147,.T.);
#13998=EDGE_CURVE('',#10657,#10658,#699,.T.);
#13999=EDGE_CURVE('',#10658,#10659,#4935,.T.);
#14000=EDGE_CURVE('',#10659,#10660,#700,.T.);
#14001=EDGE_CURVE('',#10660,#10661,#7148,.T.);
#14002=EDGE_CURVE('',#10662,#10661,#4936,.T.);
#14003=EDGE_CURVE('',#10662,#10663,#4937,.T.);
#14004=EDGE_CURVE('',#10664,#10663,#4938,.T.);
#14005=EDGE_CURVE('',#10664,#10665,#7149,.T.);
#14006=EDGE_CURVE('',#10665,#10666,#701,.T.);
#14007=EDGE_CURVE('',#10666,#10667,#4939,.T.);
#14008=EDGE_CURVE('',#10667,#10668,#702,.T.);
#14009=EDGE_CURVE('',#10668,#10669,#7150,.T.);
#14010=EDGE_CURVE('',#10670,#10669,#4940,.T.);
#14011=EDGE_CURVE('',#10670,#10671,#4941,.T.);
#14012=EDGE_CURVE('',#10672,#10671,#4942,.T.);
#14013=EDGE_CURVE('',#10672,#10673,#7151,.T.);
#14014=EDGE_CURVE('',#10673,#10674,#703,.T.);
#14015=EDGE_CURVE('',#10674,#10675,#4943,.T.);
#14016=EDGE_CURVE('',#10675,#10676,#704,.T.);
#14017=EDGE_CURVE('',#10676,#10677,#7152,.T.);
#14018=EDGE_CURVE('',#10678,#10677,#4944,.T.);
#14019=EDGE_CURVE('',#10678,#10679,#4945,.T.);
#14020=EDGE_CURVE('',#10680,#10679,#4946,.T.);
#14021=EDGE_CURVE('',#10680,#10681,#7153,.T.);
#14022=EDGE_CURVE('',#10681,#10682,#705,.T.);
#14023=EDGE_CURVE('',#10682,#10683,#4947,.T.);
#14024=EDGE_CURVE('',#10683,#10684,#706,.T.);
#14025=EDGE_CURVE('',#10684,#10685,#7154,.T.);
#14026=EDGE_CURVE('',#10686,#10685,#4948,.T.);
#14027=EDGE_CURVE('',#10686,#10687,#4949,.T.);
#14028=EDGE_CURVE('',#10688,#10687,#4950,.T.);
#14029=EDGE_CURVE('',#10688,#10689,#7155,.T.);
#14030=EDGE_CURVE('',#10689,#10690,#707,.T.);
#14031=EDGE_CURVE('',#10690,#10691,#4951,.T.);
#14032=EDGE_CURVE('',#10691,#10692,#708,.T.);
#14033=EDGE_CURVE('',#10692,#10693,#7156,.T.);
#14034=EDGE_CURVE('',#10694,#10693,#4952,.T.);
#14035=EDGE_CURVE('',#10694,#10695,#4953,.T.);
#14036=EDGE_CURVE('',#10696,#10695,#4954,.T.);
#14037=EDGE_CURVE('',#10696,#10697,#7157,.T.);
#14038=EDGE_CURVE('',#10697,#10698,#709,.T.);
#14039=EDGE_CURVE('',#10698,#10699,#4955,.T.);
#14040=EDGE_CURVE('',#10699,#10700,#710,.T.);
#14041=EDGE_CURVE('',#10700,#10701,#7158,.T.);
#14042=EDGE_CURVE('',#10702,#10701,#4956,.T.);
#14043=EDGE_CURVE('',#10702,#10703,#4957,.T.);
#14044=EDGE_CURVE('',#10704,#10703,#4958,.T.);
#14045=EDGE_CURVE('',#10704,#10705,#7159,.T.);
#14046=EDGE_CURVE('',#10705,#10706,#711,.T.);
#14047=EDGE_CURVE('',#10706,#10707,#4959,.T.);
#14048=EDGE_CURVE('',#10707,#10708,#712,.T.);
#14049=EDGE_CURVE('',#10708,#10709,#7160,.T.);
#14050=EDGE_CURVE('',#10710,#10709,#4960,.T.);
#14051=EDGE_CURVE('',#10710,#10711,#4961,.T.);
#14052=EDGE_CURVE('',#10712,#10711,#4962,.T.);
#14053=EDGE_CURVE('',#10712,#10713,#7161,.T.);
#14054=EDGE_CURVE('',#10713,#10714,#713,.T.);
#14055=EDGE_CURVE('',#10714,#10715,#4963,.T.);
#14056=EDGE_CURVE('',#10715,#10716,#714,.T.);
#14057=EDGE_CURVE('',#10716,#10717,#7162,.T.);
#14058=EDGE_CURVE('',#10718,#10717,#4964,.T.);
#14059=EDGE_CURVE('',#10718,#10719,#4965,.T.);
#14060=EDGE_CURVE('',#10720,#10719,#4966,.T.);
#14061=EDGE_CURVE('',#10720,#10721,#7163,.T.);
#14062=EDGE_CURVE('',#10721,#10722,#715,.T.);
#14063=EDGE_CURVE('',#10722,#10723,#4967,.T.);
#14064=EDGE_CURVE('',#10723,#10724,#716,.T.);
#14065=EDGE_CURVE('',#10724,#10725,#7164,.T.);
#14066=EDGE_CURVE('',#10726,#10725,#4968,.T.);
#14067=EDGE_CURVE('',#10726,#10727,#4969,.T.);
#14068=EDGE_CURVE('',#10728,#10727,#4970,.T.);
#14069=EDGE_CURVE('',#10728,#10729,#7165,.T.);
#14070=EDGE_CURVE('',#10729,#10730,#717,.T.);
#14071=EDGE_CURVE('',#10730,#10731,#4971,.T.);
#14072=EDGE_CURVE('',#10731,#10732,#718,.T.);
#14073=EDGE_CURVE('',#10732,#10733,#7166,.T.);
#14074=EDGE_CURVE('',#10734,#10733,#4972,.T.);
#14075=EDGE_CURVE('',#10734,#10735,#4973,.T.);
#14076=EDGE_CURVE('',#10736,#10735,#4974,.T.);
#14077=EDGE_CURVE('',#10736,#10737,#7167,.T.);
#14078=EDGE_CURVE('',#10737,#10738,#719,.T.);
#14079=EDGE_CURVE('',#10738,#10739,#4975,.T.);
#14080=EDGE_CURVE('',#10739,#10740,#720,.T.);
#14081=EDGE_CURVE('',#10740,#10741,#7168,.T.);
#14082=EDGE_CURVE('',#10742,#10741,#4976,.T.);
#14083=EDGE_CURVE('',#10742,#10743,#4977,.T.);
#14084=EDGE_CURVE('',#10744,#10743,#4978,.T.);
#14085=EDGE_CURVE('',#10744,#10745,#7169,.T.);
#14086=EDGE_CURVE('',#10745,#10746,#721,.T.);
#14087=EDGE_CURVE('',#10746,#10747,#4979,.T.);
#14088=EDGE_CURVE('',#10747,#10748,#722,.T.);
#14089=EDGE_CURVE('',#10748,#10749,#7170,.T.);
#14090=EDGE_CURVE('',#10750,#10749,#4980,.T.);
#14091=EDGE_CURVE('',#10750,#10751,#4981,.T.);
#14092=EDGE_CURVE('',#10752,#10751,#4982,.T.);
#14093=EDGE_CURVE('',#10752,#10753,#7171,.T.);
#14094=EDGE_CURVE('',#10753,#10754,#723,.T.);
#14095=EDGE_CURVE('',#10754,#10755,#4983,.T.);
#14096=EDGE_CURVE('',#10755,#10756,#724,.T.);
#14097=EDGE_CURVE('',#10756,#10757,#7172,.T.);
#14098=EDGE_CURVE('',#10758,#10757,#4984,.T.);
#14099=EDGE_CURVE('',#10758,#10759,#4985,.T.);
#14100=EDGE_CURVE('',#10760,#10759,#4986,.T.);
#14101=EDGE_CURVE('',#10760,#10761,#7173,.T.);
#14102=EDGE_CURVE('',#10761,#10762,#725,.T.);
#14103=EDGE_CURVE('',#10762,#10763,#4987,.T.);
#14104=EDGE_CURVE('',#10763,#10764,#726,.T.);
#14105=EDGE_CURVE('',#10764,#10765,#7174,.T.);
#14106=EDGE_CURVE('',#10766,#10765,#4988,.T.);
#14107=EDGE_CURVE('',#10766,#10767,#4989,.T.);
#14108=EDGE_CURVE('',#10768,#10767,#4990,.T.);
#14109=EDGE_CURVE('',#10768,#10769,#7175,.T.);
#14110=EDGE_CURVE('',#10769,#10770,#727,.T.);
#14111=EDGE_CURVE('',#10770,#10771,#4991,.T.);
#14112=EDGE_CURVE('',#10771,#10772,#728,.T.);
#14113=EDGE_CURVE('',#10772,#10773,#7176,.T.);
#14114=EDGE_CURVE('',#10774,#10773,#4992,.T.);
#14115=EDGE_CURVE('',#10774,#10775,#4993,.T.);
#14116=EDGE_CURVE('',#10776,#10775,#4994,.T.);
#14117=EDGE_CURVE('',#10776,#10777,#7177,.T.);
#14118=EDGE_CURVE('',#10777,#10778,#729,.T.);
#14119=EDGE_CURVE('',#10778,#10779,#4995,.T.);
#14120=EDGE_CURVE('',#10779,#10780,#730,.T.);
#14121=EDGE_CURVE('',#10780,#10781,#7178,.T.);
#14122=EDGE_CURVE('',#10782,#10781,#4996,.T.);
#14123=EDGE_CURVE('',#10782,#10783,#4997,.T.);
#14124=EDGE_CURVE('',#10784,#10783,#4998,.T.);
#14125=EDGE_CURVE('',#10784,#10785,#7179,.T.);
#14126=EDGE_CURVE('',#10785,#10786,#731,.T.);
#14127=EDGE_CURVE('',#10786,#10787,#4999,.T.);
#14128=EDGE_CURVE('',#10787,#10788,#732,.T.);
#14129=EDGE_CURVE('',#10788,#10789,#7180,.T.);
#14130=EDGE_CURVE('',#10790,#10789,#5000,.T.);
#14131=EDGE_CURVE('',#10790,#10791,#5001,.T.);
#14132=EDGE_CURVE('',#10792,#10791,#5002,.T.);
#14133=EDGE_CURVE('',#10792,#10793,#7181,.T.);
#14134=EDGE_CURVE('',#10793,#10794,#733,.T.);
#14135=EDGE_CURVE('',#10794,#10795,#5003,.T.);
#14136=EDGE_CURVE('',#10795,#10796,#734,.T.);
#14137=EDGE_CURVE('',#10796,#10797,#7182,.T.);
#14138=EDGE_CURVE('',#10798,#10797,#5004,.T.);
#14139=EDGE_CURVE('',#10798,#10799,#5005,.T.);
#14140=EDGE_CURVE('',#10800,#10799,#5006,.T.);
#14141=EDGE_CURVE('',#10800,#10801,#7183,.T.);
#14142=EDGE_CURVE('',#10801,#10802,#735,.T.);
#14143=EDGE_CURVE('',#10802,#10803,#5007,.T.);
#14144=EDGE_CURVE('',#10803,#10804,#736,.T.);
#14145=EDGE_CURVE('',#10804,#10805,#7184,.T.);
#14146=EDGE_CURVE('',#10806,#10805,#5008,.T.);
#14147=EDGE_CURVE('',#10806,#10807,#5009,.T.);
#14148=EDGE_CURVE('',#10808,#10807,#5010,.T.);
#14149=EDGE_CURVE('',#10808,#10809,#7185,.T.);
#14150=EDGE_CURVE('',#10809,#10810,#737,.T.);
#14151=EDGE_CURVE('',#10810,#10811,#5011,.T.);
#14152=EDGE_CURVE('',#10811,#10812,#738,.T.);
#14153=EDGE_CURVE('',#10812,#10813,#7186,.T.);
#14154=EDGE_CURVE('',#10814,#10813,#5012,.T.);
#14155=EDGE_CURVE('',#10814,#10815,#5013,.T.);
#14156=EDGE_CURVE('',#10816,#10815,#5014,.T.);
#14157=EDGE_CURVE('',#10816,#10625,#7187,.T.);
#14158=EDGE_CURVE('',#10817,#10818,#5015,.T.);
#14159=EDGE_CURVE('',#10818,#10816,#7188,.T.);
#14160=EDGE_CURVE('',#10815,#10817,#7189,.T.);
#14161=EDGE_CURVE('',#10819,#10818,#7190,.T.);
#14162=EDGE_CURVE('',#10819,#10625,#7191,.T.);
#14163=EDGE_CURVE('',#10820,#10821,#5016,.T.);
#14164=EDGE_CURVE('',#10821,#10814,#7192,.T.);
#14165=EDGE_CURVE('',#10813,#10820,#7193,.T.);
#14166=EDGE_CURVE('',#10817,#10821,#5017,.T.);
#14167=EDGE_CURVE('',#10822,#10823,#5018,.T.);
#14168=EDGE_CURVE('',#10823,#10808,#7194,.T.);
#14169=EDGE_CURVE('',#10807,#10822,#7195,.T.);
#14170=EDGE_CURVE('',#10824,#10823,#7196,.T.);
#14171=EDGE_CURVE('',#10824,#10809,#7197,.T.);
#14172=EDGE_CURVE('',#10825,#10826,#5019,.T.);
#14173=EDGE_CURVE('',#10826,#10806,#7198,.T.);
#14174=EDGE_CURVE('',#10805,#10825,#7199,.T.);
#14175=EDGE_CURVE('',#10822,#10826,#5020,.T.);
#14176=EDGE_CURVE('',#10827,#10828,#5021,.T.);
#14177=EDGE_CURVE('',#10828,#10800,#7200,.T.);
#14178=EDGE_CURVE('',#10799,#10827,#7201,.T.);
#14179=EDGE_CURVE('',#10829,#10828,#7202,.T.);
#14180=EDGE_CURVE('',#10829,#10801,#7203,.T.);
#14181=EDGE_CURVE('',#10830,#10831,#5022,.T.);
#14182=EDGE_CURVE('',#10831,#10798,#7204,.T.);
#14183=EDGE_CURVE('',#10797,#10830,#7205,.T.);
#14184=EDGE_CURVE('',#10827,#10831,#5023,.T.);
#14185=EDGE_CURVE('',#10832,#10833,#5024,.T.);
#14186=EDGE_CURVE('',#10833,#10792,#7206,.T.);
#14187=EDGE_CURVE('',#10791,#10832,#7207,.T.);
#14188=EDGE_CURVE('',#10834,#10833,#7208,.T.);
#14189=EDGE_CURVE('',#10834,#10793,#7209,.T.);
#14190=EDGE_CURVE('',#10835,#10836,#5025,.T.);
#14191=EDGE_CURVE('',#10836,#10790,#7210,.T.);
#14192=EDGE_CURVE('',#10789,#10835,#7211,.T.);
#14193=EDGE_CURVE('',#10832,#10836,#5026,.T.);
#14194=EDGE_CURVE('',#10837,#10838,#5027,.T.);
#14195=EDGE_CURVE('',#10838,#10784,#7212,.T.);
#14196=EDGE_CURVE('',#10783,#10837,#7213,.T.);
#14197=EDGE_CURVE('',#10839,#10838,#7214,.T.);
#14198=EDGE_CURVE('',#10839,#10785,#7215,.T.);
#14199=EDGE_CURVE('',#10840,#10841,#5028,.T.);
#14200=EDGE_CURVE('',#10841,#10782,#7216,.T.);
#14201=EDGE_CURVE('',#10781,#10840,#7217,.T.);
#14202=EDGE_CURVE('',#10837,#10841,#5029,.T.);
#14203=EDGE_CURVE('',#10842,#10843,#5030,.T.);
#14204=EDGE_CURVE('',#10843,#10776,#7218,.T.);
#14205=EDGE_CURVE('',#10775,#10842,#7219,.T.);
#14206=EDGE_CURVE('',#10844,#10843,#7220,.T.);
#14207=EDGE_CURVE('',#10844,#10777,#7221,.T.);
#14208=EDGE_CURVE('',#10845,#10846,#5031,.T.);
#14209=EDGE_CURVE('',#10846,#10774,#7222,.T.);
#14210=EDGE_CURVE('',#10773,#10845,#7223,.T.);
#14211=EDGE_CURVE('',#10842,#10846,#5032,.T.);
#14212=EDGE_CURVE('',#10847,#10848,#5033,.T.);
#14213=EDGE_CURVE('',#10848,#10768,#7224,.T.);
#14214=EDGE_CURVE('',#10767,#10847,#7225,.T.);
#14215=EDGE_CURVE('',#10849,#10848,#7226,.T.);
#14216=EDGE_CURVE('',#10849,#10769,#7227,.T.);
#14217=EDGE_CURVE('',#10850,#10851,#5034,.T.);
#14218=EDGE_CURVE('',#10851,#10766,#7228,.T.);
#14219=EDGE_CURVE('',#10765,#10850,#7229,.T.);
#14220=EDGE_CURVE('',#10847,#10851,#5035,.T.);
#14221=EDGE_CURVE('',#10852,#10853,#5036,.T.);
#14222=EDGE_CURVE('',#10853,#10760,#7230,.T.);
#14223=EDGE_CURVE('',#10759,#10852,#7231,.T.);
#14224=EDGE_CURVE('',#10854,#10853,#7232,.T.);
#14225=EDGE_CURVE('',#10854,#10761,#7233,.T.);
#14226=EDGE_CURVE('',#10855,#10856,#5037,.T.);
#14227=EDGE_CURVE('',#10856,#10758,#7234,.T.);
#14228=EDGE_CURVE('',#10757,#10855,#7235,.T.);
#14229=EDGE_CURVE('',#10852,#10856,#5038,.T.);
#14230=EDGE_CURVE('',#10857,#10858,#5039,.T.);
#14231=EDGE_CURVE('',#10858,#10752,#7236,.T.);
#14232=EDGE_CURVE('',#10751,#10857,#7237,.T.);
#14233=EDGE_CURVE('',#10859,#10858,#7238,.T.);
#14234=EDGE_CURVE('',#10859,#10753,#7239,.T.);
#14235=EDGE_CURVE('',#10860,#10861,#5040,.T.);
#14236=EDGE_CURVE('',#10861,#10750,#7240,.T.);
#14237=EDGE_CURVE('',#10749,#10860,#7241,.T.);
#14238=EDGE_CURVE('',#10857,#10861,#5041,.T.);
#14239=EDGE_CURVE('',#10862,#10863,#5042,.T.);
#14240=EDGE_CURVE('',#10863,#10744,#7242,.T.);
#14241=EDGE_CURVE('',#10743,#10862,#7243,.T.);
#14242=EDGE_CURVE('',#10864,#10863,#7244,.T.);
#14243=EDGE_CURVE('',#10864,#10745,#7245,.T.);
#14244=EDGE_CURVE('',#10865,#10866,#5043,.T.);
#14245=EDGE_CURVE('',#10866,#10742,#7246,.T.);
#14246=EDGE_CURVE('',#10741,#10865,#7247,.T.);
#14247=EDGE_CURVE('',#10862,#10866,#5044,.T.);
#14248=EDGE_CURVE('',#10867,#10868,#5045,.T.);
#14249=EDGE_CURVE('',#10868,#10736,#7248,.T.);
#14250=EDGE_CURVE('',#10735,#10867,#7249,.T.);
#14251=EDGE_CURVE('',#10869,#10868,#7250,.T.);
#14252=EDGE_CURVE('',#10869,#10737,#7251,.T.);
#14253=EDGE_CURVE('',#10870,#10871,#5046,.T.);
#14254=EDGE_CURVE('',#10871,#10734,#7252,.T.);
#14255=EDGE_CURVE('',#10733,#10870,#7253,.T.);
#14256=EDGE_CURVE('',#10867,#10871,#5047,.T.);
#14257=EDGE_CURVE('',#10872,#10873,#5048,.T.);
#14258=EDGE_CURVE('',#10873,#10728,#7254,.T.);
#14259=EDGE_CURVE('',#10727,#10872,#7255,.T.);
#14260=EDGE_CURVE('',#10874,#10873,#7256,.T.);
#14261=EDGE_CURVE('',#10874,#10729,#7257,.T.);
#14262=EDGE_CURVE('',#10875,#10876,#5049,.T.);
#14263=EDGE_CURVE('',#10876,#10726,#7258,.T.);
#14264=EDGE_CURVE('',#10725,#10875,#7259,.T.);
#14265=EDGE_CURVE('',#10872,#10876,#5050,.T.);
#14266=EDGE_CURVE('',#10877,#10878,#5051,.T.);
#14267=EDGE_CURVE('',#10878,#10720,#7260,.T.);
#14268=EDGE_CURVE('',#10719,#10877,#7261,.T.);
#14269=EDGE_CURVE('',#10879,#10878,#7262,.T.);
#14270=EDGE_CURVE('',#10879,#10721,#7263,.T.);
#14271=EDGE_CURVE('',#10880,#10881,#5052,.T.);
#14272=EDGE_CURVE('',#10881,#10718,#7264,.T.);
#14273=EDGE_CURVE('',#10717,#10880,#7265,.T.);
#14274=EDGE_CURVE('',#10877,#10881,#5053,.T.);
#14275=EDGE_CURVE('',#10882,#10883,#5054,.T.);
#14276=EDGE_CURVE('',#10883,#10712,#7266,.T.);
#14277=EDGE_CURVE('',#10711,#10882,#7267,.T.);
#14278=EDGE_CURVE('',#10884,#10883,#7268,.T.);
#14279=EDGE_CURVE('',#10884,#10713,#7269,.T.);
#14280=EDGE_CURVE('',#10885,#10886,#5055,.T.);
#14281=EDGE_CURVE('',#10886,#10710,#7270,.T.);
#14282=EDGE_CURVE('',#10709,#10885,#7271,.T.);
#14283=EDGE_CURVE('',#10882,#10886,#5056,.T.);
#14284=EDGE_CURVE('',#10887,#10888,#5057,.T.);
#14285=EDGE_CURVE('',#10888,#10704,#7272,.T.);
#14286=EDGE_CURVE('',#10703,#10887,#7273,.T.);
#14287=EDGE_CURVE('',#10889,#10888,#7274,.T.);
#14288=EDGE_CURVE('',#10889,#10705,#7275,.T.);
#14289=EDGE_CURVE('',#10890,#10891,#5058,.T.);
#14290=EDGE_CURVE('',#10891,#10702,#7276,.T.);
#14291=EDGE_CURVE('',#10701,#10890,#7277,.T.);
#14292=EDGE_CURVE('',#10887,#10891,#5059,.T.);
#14293=EDGE_CURVE('',#10892,#10893,#5060,.T.);
#14294=EDGE_CURVE('',#10893,#10696,#7278,.T.);
#14295=EDGE_CURVE('',#10695,#10892,#7279,.T.);
#14296=EDGE_CURVE('',#10894,#10893,#7280,.T.);
#14297=EDGE_CURVE('',#10894,#10697,#7281,.T.);
#14298=EDGE_CURVE('',#10895,#10896,#5061,.T.);
#14299=EDGE_CURVE('',#10896,#10694,#7282,.T.);
#14300=EDGE_CURVE('',#10693,#10895,#7283,.T.);
#14301=EDGE_CURVE('',#10892,#10896,#5062,.T.);
#14302=EDGE_CURVE('',#10897,#10898,#5063,.T.);
#14303=EDGE_CURVE('',#10898,#10688,#7284,.T.);
#14304=EDGE_CURVE('',#10687,#10897,#7285,.T.);
#14305=EDGE_CURVE('',#10899,#10898,#7286,.T.);
#14306=EDGE_CURVE('',#10899,#10689,#7287,.T.);
#14307=EDGE_CURVE('',#10900,#10901,#5064,.T.);
#14308=EDGE_CURVE('',#10901,#10686,#7288,.T.);
#14309=EDGE_CURVE('',#10685,#10900,#7289,.T.);
#14310=EDGE_CURVE('',#10897,#10901,#5065,.T.);
#14311=EDGE_CURVE('',#10902,#10903,#5066,.T.);
#14312=EDGE_CURVE('',#10903,#10680,#7290,.T.);
#14313=EDGE_CURVE('',#10679,#10902,#7291,.T.);
#14314=EDGE_CURVE('',#10904,#10903,#7292,.T.);
#14315=EDGE_CURVE('',#10904,#10681,#7293,.T.);
#14316=EDGE_CURVE('',#10905,#10906,#5067,.T.);
#14317=EDGE_CURVE('',#10906,#10678,#7294,.T.);
#14318=EDGE_CURVE('',#10677,#10905,#7295,.T.);
#14319=EDGE_CURVE('',#10902,#10906,#5068,.T.);
#14320=EDGE_CURVE('',#10907,#10908,#5069,.T.);
#14321=EDGE_CURVE('',#10908,#10672,#7296,.T.);
#14322=EDGE_CURVE('',#10671,#10907,#7297,.T.);
#14323=EDGE_CURVE('',#10909,#10908,#7298,.T.);
#14324=EDGE_CURVE('',#10909,#10673,#7299,.T.);
#14325=EDGE_CURVE('',#10910,#10911,#5070,.T.);
#14326=EDGE_CURVE('',#10911,#10670,#7300,.T.);
#14327=EDGE_CURVE('',#10669,#10910,#7301,.T.);
#14328=EDGE_CURVE('',#10907,#10911,#5071,.T.);
#14329=EDGE_CURVE('',#10912,#10913,#5072,.T.);
#14330=EDGE_CURVE('',#10913,#10664,#7302,.T.);
#14331=EDGE_CURVE('',#10663,#10912,#7303,.T.);
#14332=EDGE_CURVE('',#10914,#10913,#7304,.T.);
#14333=EDGE_CURVE('',#10914,#10665,#7305,.T.);
#14334=EDGE_CURVE('',#10915,#10916,#5073,.T.);
#14335=EDGE_CURVE('',#10916,#10662,#7306,.T.);
#14336=EDGE_CURVE('',#10661,#10915,#7307,.T.);
#14337=EDGE_CURVE('',#10912,#10916,#5074,.T.);
#14338=EDGE_CURVE('',#10917,#10918,#5075,.T.);
#14339=EDGE_CURVE('',#10918,#10656,#7308,.T.);
#14340=EDGE_CURVE('',#10655,#10917,#7309,.T.);
#14341=EDGE_CURVE('',#10919,#10918,#7310,.T.);
#14342=EDGE_CURVE('',#10919,#10657,#7311,.T.);
#14343=EDGE_CURVE('',#10920,#10921,#5076,.T.);
#14344=EDGE_CURVE('',#10921,#10654,#7312,.T.);
#14345=EDGE_CURVE('',#10653,#10920,#7313,.T.);
#14346=EDGE_CURVE('',#10917,#10921,#5077,.T.);
#14347=EDGE_CURVE('',#10922,#10923,#5078,.T.);
#14348=EDGE_CURVE('',#10923,#10648,#7314,.T.);
#14349=EDGE_CURVE('',#10647,#10922,#7315,.T.);
#14350=EDGE_CURVE('',#10924,#10923,#7316,.T.);
#14351=EDGE_CURVE('',#10924,#10649,#7317,.T.);
#14352=EDGE_CURVE('',#10925,#10926,#5079,.T.);
#14353=EDGE_CURVE('',#10926,#10646,#7318,.T.);
#14354=EDGE_CURVE('',#10645,#10925,#7319,.T.);
#14355=EDGE_CURVE('',#10922,#10926,#5080,.T.);
#14356=EDGE_CURVE('',#10927,#10928,#5081,.T.);
#14357=EDGE_CURVE('',#10928,#10640,#7320,.T.);
#14358=EDGE_CURVE('',#10639,#10927,#7321,.T.);
#14359=EDGE_CURVE('',#10929,#10928,#7322,.T.);
#14360=EDGE_CURVE('',#10929,#10641,#7323,.T.);
#14361=EDGE_CURVE('',#10930,#10931,#5082,.T.);
#14362=EDGE_CURVE('',#10931,#10638,#7324,.T.);
#14363=EDGE_CURVE('',#10637,#10930,#7325,.T.);
#14364=EDGE_CURVE('',#10927,#10931,#5083,.T.);
#14365=EDGE_CURVE('',#10932,#10812,#7326,.T.);
#14366=EDGE_CURVE('',#10820,#10932,#7327,.T.);
#14367=EDGE_CURVE('',#10933,#10819,#739,.T.);
#14368=EDGE_CURVE('',#10626,#10933,#7328,.T.);
#14369=EDGE_CURVE('',#10932,#10934,#740,.T.);
#14370=EDGE_CURVE('',#10934,#10811,#7329,.T.);
#14371=EDGE_CURVE('',#10935,#10804,#7330,.T.);
#14372=EDGE_CURVE('',#10825,#10935,#7331,.T.);
#14373=EDGE_CURVE('',#10936,#10824,#741,.T.);
#14374=EDGE_CURVE('',#10810,#10936,#7332,.T.);
#14375=EDGE_CURVE('',#10935,#10937,#742,.T.);
#14376=EDGE_CURVE('',#10937,#10803,#7333,.T.);
#14377=EDGE_CURVE('',#10938,#10796,#7334,.T.);
#14378=EDGE_CURVE('',#10830,#10938,#7335,.T.);
#14379=EDGE_CURVE('',#10939,#10829,#743,.T.);
#14380=EDGE_CURVE('',#10802,#10939,#7336,.T.);
#14381=EDGE_CURVE('',#10938,#10940,#744,.T.);
#14382=EDGE_CURVE('',#10940,#10795,#7337,.T.);
#14383=EDGE_CURVE('',#10941,#10788,#7338,.T.);
#14384=EDGE_CURVE('',#10835,#10941,#7339,.T.);
#14385=EDGE_CURVE('',#10942,#10834,#745,.T.);
#14386=EDGE_CURVE('',#10794,#10942,#7340,.T.);
#14387=EDGE_CURVE('',#10941,#10943,#746,.T.);
#14388=EDGE_CURVE('',#10943,#10787,#7341,.T.);
#14389=EDGE_CURVE('',#10944,#10780,#7342,.T.);
#14390=EDGE_CURVE('',#10840,#10944,#7343,.T.);
#14391=EDGE_CURVE('',#10945,#10839,#747,.T.);
#14392=EDGE_CURVE('',#10786,#10945,#7344,.T.);
#14393=EDGE_CURVE('',#10944,#10946,#748,.T.);
#14394=EDGE_CURVE('',#10946,#10779,#7345,.T.);
#14395=EDGE_CURVE('',#10947,#10772,#7346,.T.);
#14396=EDGE_CURVE('',#10845,#10947,#7347,.T.);
#14397=EDGE_CURVE('',#10948,#10844,#749,.T.);
#14398=EDGE_CURVE('',#10778,#10948,#7348,.T.);
#14399=EDGE_CURVE('',#10947,#10949,#750,.T.);
#14400=EDGE_CURVE('',#10949,#10771,#7349,.T.);
#14401=EDGE_CURVE('',#10950,#10764,#7350,.T.);
#14402=EDGE_CURVE('',#10850,#10950,#7351,.T.);
#14403=EDGE_CURVE('',#10951,#10849,#751,.T.);
#14404=EDGE_CURVE('',#10770,#10951,#7352,.T.);
#14405=EDGE_CURVE('',#10950,#10952,#752,.T.);
#14406=EDGE_CURVE('',#10952,#10763,#7353,.T.);
#14407=EDGE_CURVE('',#10953,#10756,#7354,.T.);
#14408=EDGE_CURVE('',#10855,#10953,#7355,.T.);
#14409=EDGE_CURVE('',#10954,#10854,#753,.T.);
#14410=EDGE_CURVE('',#10762,#10954,#7356,.T.);
#14411=EDGE_CURVE('',#10953,#10955,#754,.T.);
#14412=EDGE_CURVE('',#10955,#10755,#7357,.T.);
#14413=EDGE_CURVE('',#10956,#10748,#7358,.T.);
#14414=EDGE_CURVE('',#10860,#10956,#7359,.T.);
#14415=EDGE_CURVE('',#10957,#10859,#755,.T.);
#14416=EDGE_CURVE('',#10754,#10957,#7360,.T.);
#14417=EDGE_CURVE('',#10956,#10958,#756,.T.);
#14418=EDGE_CURVE('',#10958,#10747,#7361,.T.);
#14419=EDGE_CURVE('',#10959,#10740,#7362,.T.);
#14420=EDGE_CURVE('',#10865,#10959,#7363,.T.);
#14421=EDGE_CURVE('',#10960,#10864,#757,.T.);
#14422=EDGE_CURVE('',#10746,#10960,#7364,.T.);
#14423=EDGE_CURVE('',#10959,#10961,#758,.T.);
#14424=EDGE_CURVE('',#10961,#10739,#7365,.T.);
#14425=EDGE_CURVE('',#10962,#10732,#7366,.T.);
#14426=EDGE_CURVE('',#10870,#10962,#7367,.T.);
#14427=EDGE_CURVE('',#10963,#10869,#759,.T.);
#14428=EDGE_CURVE('',#10738,#10963,#7368,.T.);
#14429=EDGE_CURVE('',#10962,#10964,#760,.T.);
#14430=EDGE_CURVE('',#10964,#10731,#7369,.T.);
#14431=EDGE_CURVE('',#10965,#10724,#7370,.T.);
#14432=EDGE_CURVE('',#10875,#10965,#7371,.T.);
#14433=EDGE_CURVE('',#10966,#10874,#761,.T.);
#14434=EDGE_CURVE('',#10730,#10966,#7372,.T.);
#14435=EDGE_CURVE('',#10965,#10967,#762,.T.);
#14436=EDGE_CURVE('',#10967,#10723,#7373,.T.);
#14437=EDGE_CURVE('',#10968,#10716,#7374,.T.);
#14438=EDGE_CURVE('',#10880,#10968,#7375,.T.);
#14439=EDGE_CURVE('',#10969,#10879,#763,.T.);
#14440=EDGE_CURVE('',#10722,#10969,#7376,.T.);
#14441=EDGE_CURVE('',#10968,#10970,#764,.T.);
#14442=EDGE_CURVE('',#10970,#10715,#7377,.T.);
#14443=EDGE_CURVE('',#10971,#10708,#7378,.T.);
#14444=EDGE_CURVE('',#10885,#10971,#7379,.T.);
#14445=EDGE_CURVE('',#10972,#10884,#765,.T.);
#14446=EDGE_CURVE('',#10714,#10972,#7380,.T.);
#14447=EDGE_CURVE('',#10971,#10973,#766,.T.);
#14448=EDGE_CURVE('',#10973,#10707,#7381,.T.);
#14449=EDGE_CURVE('',#10974,#10700,#7382,.T.);
#14450=EDGE_CURVE('',#10890,#10974,#7383,.T.);
#14451=EDGE_CURVE('',#10975,#10889,#767,.T.);
#14452=EDGE_CURVE('',#10706,#10975,#7384,.T.);
#14453=EDGE_CURVE('',#10974,#10976,#768,.T.);
#14454=EDGE_CURVE('',#10976,#10699,#7385,.T.);
#14455=EDGE_CURVE('',#10977,#10692,#7386,.T.);
#14456=EDGE_CURVE('',#10895,#10977,#7387,.T.);
#14457=EDGE_CURVE('',#10978,#10894,#769,.T.);
#14458=EDGE_CURVE('',#10698,#10978,#7388,.T.);
#14459=EDGE_CURVE('',#10977,#10979,#770,.T.);
#14460=EDGE_CURVE('',#10979,#10691,#7389,.T.);
#14461=EDGE_CURVE('',#10980,#10684,#7390,.T.);
#14462=EDGE_CURVE('',#10900,#10980,#7391,.T.);
#14463=EDGE_CURVE('',#10981,#10899,#771,.T.);
#14464=EDGE_CURVE('',#10690,#10981,#7392,.T.);
#14465=EDGE_CURVE('',#10980,#10982,#772,.T.);
#14466=EDGE_CURVE('',#10982,#10683,#7393,.T.);
#14467=EDGE_CURVE('',#10983,#10676,#7394,.T.);
#14468=EDGE_CURVE('',#10905,#10983,#7395,.T.);
#14469=EDGE_CURVE('',#10984,#10904,#773,.T.);
#14470=EDGE_CURVE('',#10682,#10984,#7396,.T.);
#14471=EDGE_CURVE('',#10983,#10985,#774,.T.);
#14472=EDGE_CURVE('',#10985,#10675,#7397,.T.);
#14473=EDGE_CURVE('',#10986,#10668,#7398,.T.);
#14474=EDGE_CURVE('',#10910,#10986,#7399,.T.);
#14475=EDGE_CURVE('',#10987,#10909,#775,.T.);
#14476=EDGE_CURVE('',#10674,#10987,#7400,.T.);
#14477=EDGE_CURVE('',#10986,#10988,#776,.T.);
#14478=EDGE_CURVE('',#10988,#10667,#7401,.T.);
#14479=EDGE_CURVE('',#10989,#10660,#7402,.T.);
#14480=EDGE_CURVE('',#10915,#10989,#7403,.T.);
#14481=EDGE_CURVE('',#10990,#10914,#777,.T.);
#14482=EDGE_CURVE('',#10666,#10990,#7404,.T.);
#14483=EDGE_CURVE('',#10989,#10991,#778,.T.);
#14484=EDGE_CURVE('',#10991,#10659,#7405,.T.);
#14485=EDGE_CURVE('',#10992,#10652,#7406,.T.);
#14486=EDGE_CURVE('',#10920,#10992,#7407,.T.);
#14487=EDGE_CURVE('',#10993,#10919,#779,.T.);
#14488=EDGE_CURVE('',#10658,#10993,#7408,.T.);
#14489=EDGE_CURVE('',#10992,#10994,#780,.T.);
#14490=EDGE_CURVE('',#10994,#10651,#7409,.T.);
#14491=EDGE_CURVE('',#10995,#10644,#7410,.T.);
#14492=EDGE_CURVE('',#10925,#10995,#7411,.T.);
#14493=EDGE_CURVE('',#10996,#10924,#781,.T.);
#14494=EDGE_CURVE('',#10650,#10996,#7412,.T.);
#14495=EDGE_CURVE('',#10995,#10997,#782,.T.);
#14496=EDGE_CURVE('',#10997,#10643,#7413,.T.);
#14497=EDGE_CURVE('',#10998,#10636,#7414,.T.);
#14498=EDGE_CURVE('',#10930,#10998,#7415,.T.);
#14499=EDGE_CURVE('',#10999,#10929,#783,.T.);
#14500=EDGE_CURVE('',#10642,#10999,#7416,.T.);
#14501=EDGE_CURVE('',#10998,#11000,#784,.T.);
#14502=EDGE_CURVE('',#11000,#10635,#7417,.T.);
#14503=EDGE_CURVE('',#10936,#10934,#5084,.T.);
#14504=EDGE_CURVE('',#10939,#10937,#5085,.T.);
#14505=EDGE_CURVE('',#10942,#10940,#5086,.T.);
#14506=EDGE_CURVE('',#10945,#10943,#5087,.T.);
#14507=EDGE_CURVE('',#10948,#10946,#5088,.T.);
#14508=EDGE_CURVE('',#10951,#10949,#5089,.T.);
#14509=EDGE_CURVE('',#10954,#10952,#5090,.T.);
#14510=EDGE_CURVE('',#10957,#10955,#5091,.T.);
#14511=EDGE_CURVE('',#10960,#10958,#5092,.T.);
#14512=EDGE_CURVE('',#10963,#10961,#5093,.T.);
#14513=EDGE_CURVE('',#10966,#10964,#5094,.T.);
#14514=EDGE_CURVE('',#10969,#10967,#5095,.T.);
#14515=EDGE_CURVE('',#10972,#10970,#5096,.T.);
#14516=EDGE_CURVE('',#10975,#10973,#5097,.T.);
#14517=EDGE_CURVE('',#10978,#10976,#5098,.T.);
#14518=EDGE_CURVE('',#10981,#10979,#5099,.T.);
#14519=EDGE_CURVE('',#10984,#10982,#5100,.T.);
#14520=EDGE_CURVE('',#10987,#10985,#5101,.T.);
#14521=EDGE_CURVE('',#10990,#10988,#5102,.T.);
#14522=EDGE_CURVE('',#10993,#10991,#5103,.T.);
#14523=EDGE_CURVE('',#10996,#10994,#5104,.T.);
#14524=EDGE_CURVE('',#10999,#10997,#5105,.T.);
#14525=EDGE_CURVE('',#11001,#11000,#5106,.T.);
#14526=EDGE_CURVE('',#11001,#11002,#785,.T.);
#14527=EDGE_CURVE('',#11002,#11003,#7418,.T.);
#14528=EDGE_CURVE('',#11004,#11003,#5107,.T.);
#14529=EDGE_CURVE('',#11004,#11005,#5108,.T.);
#14530=EDGE_CURVE('',#11006,#11005,#5109,.T.);
#14531=EDGE_CURVE('',#11006,#11007,#7419,.T.);
#14532=EDGE_CURVE('',#11007,#11008,#786,.T.);
#14533=EDGE_CURVE('',#10933,#11008,#5110,.T.);
#14534=EDGE_CURVE('',#10634,#11001,#7420,.T.);
#14535=EDGE_CURVE('',#11003,#10632,#7421,.T.);
#14536=EDGE_CURVE('',#10631,#11004,#7422,.T.);
#14537=EDGE_CURVE('',#11002,#10633,#7423,.T.);
#14538=EDGE_CURVE('',#11005,#10630,#7424,.T.);
#14539=EDGE_CURVE('',#10629,#11006,#7425,.T.);
#14540=EDGE_CURVE('',#11007,#10628,#7426,.T.);
#14541=EDGE_CURVE('',#11008,#10627,#7427,.T.);
#14542=EDGE_CURVE('',#11009,#11010,#5111,.T.);
#14543=EDGE_CURVE('',#11010,#11011,#7428,.T.);
#14544=EDGE_CURVE('',#11011,#11012,#5112,.T.);
#14545=EDGE_CURVE('',#11012,#11009,#7429,.T.);
#14546=EDGE_CURVE('',#11013,#11010,#7430,.T.);
#14547=EDGE_CURVE('',#11013,#11014,#7431,.T.);
#14548=EDGE_CURVE('',#11011,#11014,#7432,.T.);
#14549=EDGE_CURVE('',#11015,#11016,#5113,.T.);
#14550=EDGE_CURVE('',#11016,#11017,#7433,.T.);
#14551=EDGE_CURVE('',#11017,#11018,#5114,.T.);
#14552=EDGE_CURVE('',#11018,#11015,#7434,.T.);
#14553=EDGE_CURVE('',#11017,#11012,#5115,.T.);
#14554=EDGE_CURVE('',#11009,#11016,#5116,.T.);
#14555=EDGE_CURVE('',#11019,#11020,#5117,.T.);
#14556=EDGE_CURVE('',#11020,#11021,#7435,.T.);
#14557=EDGE_CURVE('',#11021,#11022,#5118,.T.);
#14558=EDGE_CURVE('',#11022,#11019,#7436,.T.);
#14559=EDGE_CURVE('',#11023,#11020,#7437,.T.);
#14560=EDGE_CURVE('',#11023,#11024,#7438,.T.);
#14561=EDGE_CURVE('',#11021,#11024,#7439,.T.);
#14562=EDGE_CURVE('',#11025,#11026,#5119,.T.);
#14563=EDGE_CURVE('',#11026,#11027,#7440,.T.);
#14564=EDGE_CURVE('',#11027,#11028,#5120,.T.);
#14565=EDGE_CURVE('',#11028,#11025,#7441,.T.);
#14566=EDGE_CURVE('',#11027,#11022,#5121,.T.);
#14567=EDGE_CURVE('',#11019,#11026,#5122,.T.);
#14568=EDGE_CURVE('',#11029,#11030,#5123,.T.);
#14569=EDGE_CURVE('',#11030,#11031,#7442,.T.);
#14570=EDGE_CURVE('',#11031,#11032,#5124,.T.);
#14571=EDGE_CURVE('',#11032,#11029,#7443,.T.);
#14572=EDGE_CURVE('',#11033,#11030,#7444,.T.);
#14573=EDGE_CURVE('',#11033,#11034,#7445,.T.);
#14574=EDGE_CURVE('',#11031,#11034,#7446,.T.);
#14575=EDGE_CURVE('',#11035,#11036,#5125,.T.);
#14576=EDGE_CURVE('',#11036,#11037,#7447,.T.);
#14577=EDGE_CURVE('',#11037,#11038,#5126,.T.);
#14578=EDGE_CURVE('',#11038,#11035,#7448,.T.);
#14579=EDGE_CURVE('',#11037,#11032,#5127,.T.);
#14580=EDGE_CURVE('',#11029,#11036,#5128,.T.);
#14581=EDGE_CURVE('',#11039,#11040,#5129,.T.);
#14582=EDGE_CURVE('',#11040,#11041,#7449,.T.);
#14583=EDGE_CURVE('',#11041,#11042,#5130,.T.);
#14584=EDGE_CURVE('',#11042,#11039,#7450,.T.);
#14585=EDGE_CURVE('',#11043,#11040,#7451,.T.);
#14586=EDGE_CURVE('',#11043,#11044,#7452,.T.);
#14587=EDGE_CURVE('',#11041,#11044,#7453,.T.);
#14588=EDGE_CURVE('',#11045,#11046,#5131,.T.);
#14589=EDGE_CURVE('',#11046,#11047,#7454,.T.);
#14590=EDGE_CURVE('',#11047,#11048,#5132,.T.);
#14591=EDGE_CURVE('',#11048,#11045,#7455,.T.);
#14592=EDGE_CURVE('',#11047,#11042,#5133,.T.);
#14593=EDGE_CURVE('',#11039,#11046,#5134,.T.);
#14594=EDGE_CURVE('',#11049,#11050,#5135,.T.);
#14595=EDGE_CURVE('',#11050,#11051,#7456,.T.);
#14596=EDGE_CURVE('',#11051,#11052,#5136,.T.);
#14597=EDGE_CURVE('',#11052,#11049,#7457,.T.);
#14598=EDGE_CURVE('',#11053,#11050,#7458,.T.);
#14599=EDGE_CURVE('',#11053,#11054,#7459,.T.);
#14600=EDGE_CURVE('',#11051,#11054,#7460,.T.);
#14601=EDGE_CURVE('',#11055,#11056,#5137,.T.);
#14602=EDGE_CURVE('',#11056,#11057,#7461,.T.);
#14603=EDGE_CURVE('',#11057,#11058,#5138,.T.);
#14604=EDGE_CURVE('',#11058,#11055,#7462,.T.);
#14605=EDGE_CURVE('',#11057,#11052,#5139,.T.);
#14606=EDGE_CURVE('',#11049,#11056,#5140,.T.);
#14607=EDGE_CURVE('',#11059,#11060,#5141,.T.);
#14608=EDGE_CURVE('',#11060,#11061,#7463,.T.);
#14609=EDGE_CURVE('',#11061,#11062,#5142,.T.);
#14610=EDGE_CURVE('',#11062,#11059,#7464,.T.);
#14611=EDGE_CURVE('',#11063,#11060,#7465,.T.);
#14612=EDGE_CURVE('',#11063,#11064,#7466,.T.);
#14613=EDGE_CURVE('',#11061,#11064,#7467,.T.);
#14614=EDGE_CURVE('',#11065,#11066,#5143,.T.);
#14615=EDGE_CURVE('',#11066,#11067,#7468,.T.);
#14616=EDGE_CURVE('',#11067,#11068,#5144,.T.);
#14617=EDGE_CURVE('',#11068,#11065,#7469,.T.);
#14618=EDGE_CURVE('',#11067,#11062,#5145,.T.);
#14619=EDGE_CURVE('',#11059,#11066,#5146,.T.);
#14620=EDGE_CURVE('',#11069,#11070,#5147,.T.);
#14621=EDGE_CURVE('',#11070,#11071,#7470,.T.);
#14622=EDGE_CURVE('',#11071,#11072,#5148,.T.);
#14623=EDGE_CURVE('',#11072,#11069,#7471,.T.);
#14624=EDGE_CURVE('',#11073,#11070,#7472,.T.);
#14625=EDGE_CURVE('',#11073,#11074,#7473,.T.);
#14626=EDGE_CURVE('',#11071,#11074,#7474,.T.);
#14627=EDGE_CURVE('',#11075,#11076,#5149,.T.);
#14628=EDGE_CURVE('',#11076,#11077,#7475,.T.);
#14629=EDGE_CURVE('',#11077,#11078,#5150,.T.);
#14630=EDGE_CURVE('',#11078,#11075,#7476,.T.);
#14631=EDGE_CURVE('',#11077,#11072,#5151,.T.);
#14632=EDGE_CURVE('',#11069,#11076,#5152,.T.);
#14633=EDGE_CURVE('',#11079,#11080,#5153,.T.);
#14634=EDGE_CURVE('',#11080,#11081,#7477,.T.);
#14635=EDGE_CURVE('',#11081,#11082,#5154,.T.);
#14636=EDGE_CURVE('',#11082,#11079,#7478,.T.);
#14637=EDGE_CURVE('',#11083,#11080,#7479,.T.);
#14638=EDGE_CURVE('',#11083,#11084,#7480,.T.);
#14639=EDGE_CURVE('',#11081,#11084,#7481,.T.);
#14640=EDGE_CURVE('',#11085,#11086,#5155,.T.);
#14641=EDGE_CURVE('',#11086,#11087,#7482,.T.);
#14642=EDGE_CURVE('',#11087,#11088,#5156,.T.);
#14643=EDGE_CURVE('',#11088,#11085,#7483,.T.);
#14644=EDGE_CURVE('',#11087,#11082,#5157,.T.);
#14645=EDGE_CURVE('',#11079,#11086,#5158,.T.);
#14646=EDGE_CURVE('',#11089,#11090,#5159,.T.);
#14647=EDGE_CURVE('',#11090,#11091,#7484,.T.);
#14648=EDGE_CURVE('',#11091,#11092,#5160,.T.);
#14649=EDGE_CURVE('',#11092,#11089,#7485,.T.);
#14650=EDGE_CURVE('',#11093,#11090,#7486,.T.);
#14651=EDGE_CURVE('',#11093,#11094,#7487,.T.);
#14652=EDGE_CURVE('',#11091,#11094,#7488,.T.);
#14653=EDGE_CURVE('',#11095,#11096,#5161,.T.);
#14654=EDGE_CURVE('',#11096,#11097,#7489,.T.);
#14655=EDGE_CURVE('',#11097,#11098,#5162,.T.);
#14656=EDGE_CURVE('',#11098,#11095,#7490,.T.);
#14657=EDGE_CURVE('',#11097,#11092,#5163,.T.);
#14658=EDGE_CURVE('',#11089,#11096,#5164,.T.);
#14659=EDGE_CURVE('',#11099,#11100,#5165,.T.);
#14660=EDGE_CURVE('',#11100,#11101,#7491,.T.);
#14661=EDGE_CURVE('',#11101,#11102,#5166,.T.);
#14662=EDGE_CURVE('',#11102,#11099,#7492,.T.);
#14663=EDGE_CURVE('',#11103,#11100,#7493,.T.);
#14664=EDGE_CURVE('',#11103,#11104,#7494,.T.);
#14665=EDGE_CURVE('',#11101,#11104,#7495,.T.);
#14666=EDGE_CURVE('',#11105,#11106,#5167,.T.);
#14667=EDGE_CURVE('',#11106,#11107,#7496,.T.);
#14668=EDGE_CURVE('',#11107,#11108,#5168,.T.);
#14669=EDGE_CURVE('',#11108,#11105,#7497,.T.);
#14670=EDGE_CURVE('',#11107,#11102,#5169,.T.);
#14671=EDGE_CURVE('',#11099,#11106,#5170,.T.);
#14672=EDGE_CURVE('',#11109,#11110,#5171,.T.);
#14673=EDGE_CURVE('',#11110,#11111,#7498,.T.);
#14674=EDGE_CURVE('',#11111,#11112,#5172,.T.);
#14675=EDGE_CURVE('',#11112,#11109,#7499,.T.);
#14676=EDGE_CURVE('',#11113,#11110,#7500,.T.);
#14677=EDGE_CURVE('',#11113,#11114,#7501,.T.);
#14678=EDGE_CURVE('',#11111,#11114,#7502,.T.);
#14679=EDGE_CURVE('',#11115,#11116,#5173,.T.);
#14680=EDGE_CURVE('',#11116,#11117,#7503,.T.);
#14681=EDGE_CURVE('',#11117,#11118,#5174,.T.);
#14682=EDGE_CURVE('',#11118,#11115,#7504,.T.);
#14683=EDGE_CURVE('',#11117,#11112,#5175,.T.);
#14684=EDGE_CURVE('',#11109,#11116,#5176,.T.);
#14685=EDGE_CURVE('',#11119,#11120,#5177,.T.);
#14686=EDGE_CURVE('',#11120,#11121,#7505,.T.);
#14687=EDGE_CURVE('',#11121,#11122,#5178,.T.);
#14688=EDGE_CURVE('',#11122,#11119,#7506,.T.);
#14689=EDGE_CURVE('',#11123,#11120,#7507,.T.);
#14690=EDGE_CURVE('',#11123,#11124,#7508,.T.);
#14691=EDGE_CURVE('',#11121,#11124,#7509,.T.);
#14692=EDGE_CURVE('',#11125,#11126,#5179,.T.);
#14693=EDGE_CURVE('',#11126,#11127,#7510,.T.);
#14694=EDGE_CURVE('',#11127,#11128,#5180,.T.);
#14695=EDGE_CURVE('',#11128,#11125,#7511,.T.);
#14696=EDGE_CURVE('',#11127,#11122,#5181,.T.);
#14697=EDGE_CURVE('',#11119,#11126,#5182,.T.);
#14698=EDGE_CURVE('',#11129,#11130,#5183,.T.);
#14699=EDGE_CURVE('',#11130,#11131,#7512,.T.);
#14700=EDGE_CURVE('',#11131,#11132,#5184,.T.);
#14701=EDGE_CURVE('',#11132,#11129,#7513,.T.);
#14702=EDGE_CURVE('',#11133,#11130,#7514,.T.);
#14703=EDGE_CURVE('',#11133,#11134,#7515,.T.);
#14704=EDGE_CURVE('',#11131,#11134,#7516,.T.);
#14705=EDGE_CURVE('',#11135,#11136,#5185,.T.);
#14706=EDGE_CURVE('',#11136,#11137,#7517,.T.);
#14707=EDGE_CURVE('',#11137,#11138,#5186,.T.);
#14708=EDGE_CURVE('',#11138,#11135,#7518,.T.);
#14709=EDGE_CURVE('',#11137,#11132,#5187,.T.);
#14710=EDGE_CURVE('',#11129,#11136,#5188,.T.);
#14711=EDGE_CURVE('',#11139,#11140,#5189,.T.);
#14712=EDGE_CURVE('',#11140,#11141,#7519,.T.);
#14713=EDGE_CURVE('',#11141,#11142,#5190,.T.);
#14714=EDGE_CURVE('',#11142,#11139,#7520,.T.);
#14715=EDGE_CURVE('',#11143,#11140,#7521,.T.);
#14716=EDGE_CURVE('',#11143,#11144,#7522,.T.);
#14717=EDGE_CURVE('',#11141,#11144,#7523,.T.);
#14718=EDGE_CURVE('',#11145,#11146,#5191,.T.);
#14719=EDGE_CURVE('',#11146,#11147,#7524,.T.);
#14720=EDGE_CURVE('',#11147,#11148,#5192,.T.);
#14721=EDGE_CURVE('',#11148,#11145,#7525,.T.);
#14722=EDGE_CURVE('',#11147,#11142,#5193,.T.);
#14723=EDGE_CURVE('',#11139,#11146,#5194,.T.);
#14724=EDGE_CURVE('',#11149,#11150,#5195,.T.);
#14725=EDGE_CURVE('',#11150,#11151,#7526,.T.);
#14726=EDGE_CURVE('',#11151,#11152,#5196,.T.);
#14727=EDGE_CURVE('',#11152,#11149,#7527,.T.);
#14728=EDGE_CURVE('',#11153,#11150,#7528,.T.);
#14729=EDGE_CURVE('',#11153,#11154,#7529,.T.);
#14730=EDGE_CURVE('',#11151,#11154,#7530,.T.);
#14731=EDGE_CURVE('',#11155,#11156,#5197,.T.);
#14732=EDGE_CURVE('',#11156,#11157,#7531,.T.);
#14733=EDGE_CURVE('',#11157,#11158,#5198,.T.);
#14734=EDGE_CURVE('',#11158,#11155,#7532,.T.);
#14735=EDGE_CURVE('',#11157,#11152,#5199,.T.);
#14736=EDGE_CURVE('',#11149,#11156,#5200,.T.);
#14737=EDGE_CURVE('',#11159,#11160,#5201,.T.);
#14738=EDGE_CURVE('',#11160,#11161,#7533,.T.);
#14739=EDGE_CURVE('',#11161,#11162,#5202,.T.);
#14740=EDGE_CURVE('',#11162,#11159,#7534,.T.);
#14741=EDGE_CURVE('',#11163,#11160,#7535,.T.);
#14742=EDGE_CURVE('',#11163,#11164,#7536,.T.);
#14743=EDGE_CURVE('',#11161,#11164,#7537,.T.);
#14744=EDGE_CURVE('',#11165,#11166,#5203,.T.);
#14745=EDGE_CURVE('',#11166,#11167,#7538,.T.);
#14746=EDGE_CURVE('',#11167,#11168,#5204,.T.);
#14747=EDGE_CURVE('',#11168,#11165,#7539,.T.);
#14748=EDGE_CURVE('',#11167,#11162,#5205,.T.);
#14749=EDGE_CURVE('',#11159,#11166,#5206,.T.);
#14750=EDGE_CURVE('',#11169,#11170,#5207,.T.);
#14751=EDGE_CURVE('',#11170,#11171,#7540,.T.);
#14752=EDGE_CURVE('',#11171,#11172,#5208,.T.);
#14753=EDGE_CURVE('',#11172,#11169,#7541,.T.);
#14754=EDGE_CURVE('',#11173,#11170,#7542,.T.);
#14755=EDGE_CURVE('',#11173,#11174,#7543,.T.);
#14756=EDGE_CURVE('',#11171,#11174,#7544,.T.);
#14757=EDGE_CURVE('',#11175,#11176,#5209,.T.);
#14758=EDGE_CURVE('',#11176,#11177,#7545,.T.);
#14759=EDGE_CURVE('',#11177,#11178,#5210,.T.);
#14760=EDGE_CURVE('',#11178,#11175,#7546,.T.);
#14761=EDGE_CURVE('',#11177,#11172,#5211,.T.);
#14762=EDGE_CURVE('',#11169,#11176,#5212,.T.);
#14763=EDGE_CURVE('',#11179,#11180,#5213,.T.);
#14764=EDGE_CURVE('',#11180,#11181,#7547,.T.);
#14765=EDGE_CURVE('',#11181,#11182,#5214,.T.);
#14766=EDGE_CURVE('',#11182,#11179,#7548,.T.);
#14767=EDGE_CURVE('',#11183,#11180,#7549,.T.);
#14768=EDGE_CURVE('',#11183,#11184,#7550,.T.);
#14769=EDGE_CURVE('',#11181,#11184,#7551,.T.);
#14770=EDGE_CURVE('',#11185,#11186,#5215,.T.);
#14771=EDGE_CURVE('',#11186,#11187,#7552,.T.);
#14772=EDGE_CURVE('',#11187,#11188,#5216,.T.);
#14773=EDGE_CURVE('',#11188,#11185,#7553,.T.);
#14774=EDGE_CURVE('',#11187,#11182,#5217,.T.);
#14775=EDGE_CURVE('',#11179,#11186,#5218,.T.);
#14776=EDGE_CURVE('',#11189,#11190,#5219,.T.);
#14777=EDGE_CURVE('',#11190,#11191,#7554,.T.);
#14778=EDGE_CURVE('',#11191,#11192,#5220,.T.);
#14779=EDGE_CURVE('',#11192,#11189,#7555,.T.);
#14780=EDGE_CURVE('',#11193,#11190,#7556,.T.);
#14781=EDGE_CURVE('',#11193,#11194,#7557,.T.);
#14782=EDGE_CURVE('',#11191,#11194,#7558,.T.);
#14783=EDGE_CURVE('',#11195,#11196,#5221,.T.);
#14784=EDGE_CURVE('',#11196,#11197,#7559,.T.);
#14785=EDGE_CURVE('',#11197,#11198,#5222,.T.);
#14786=EDGE_CURVE('',#11198,#11195,#7560,.T.);
#14787=EDGE_CURVE('',#11197,#11192,#5223,.T.);
#14788=EDGE_CURVE('',#11189,#11196,#5224,.T.);
#14789=EDGE_CURVE('',#11199,#11200,#5225,.T.);
#14790=EDGE_CURVE('',#11200,#11201,#7561,.T.);
#14791=EDGE_CURVE('',#11201,#11202,#5226,.T.);
#14792=EDGE_CURVE('',#11202,#11199,#7562,.T.);
#14793=EDGE_CURVE('',#11203,#11200,#7563,.T.);
#14794=EDGE_CURVE('',#11203,#11204,#7564,.T.);
#14795=EDGE_CURVE('',#11201,#11204,#7565,.T.);
#14796=EDGE_CURVE('',#11205,#11206,#5227,.T.);
#14797=EDGE_CURVE('',#11206,#11207,#7566,.T.);
#14798=EDGE_CURVE('',#11207,#11208,#5228,.T.);
#14799=EDGE_CURVE('',#11208,#11205,#7567,.T.);
#14800=EDGE_CURVE('',#11207,#11202,#5229,.T.);
#14801=EDGE_CURVE('',#11199,#11206,#5230,.T.);
#14802=EDGE_CURVE('',#11209,#11210,#5231,.T.);
#14803=EDGE_CURVE('',#11210,#11211,#7568,.T.);
#14804=EDGE_CURVE('',#11211,#11212,#5232,.T.);
#14805=EDGE_CURVE('',#11212,#11209,#7569,.T.);
#14806=EDGE_CURVE('',#11213,#11210,#7570,.T.);
#14807=EDGE_CURVE('',#11213,#11214,#7571,.T.);
#14808=EDGE_CURVE('',#11211,#11214,#7572,.T.);
#14809=EDGE_CURVE('',#11215,#11216,#5233,.T.);
#14810=EDGE_CURVE('',#11216,#11217,#7573,.T.);
#14811=EDGE_CURVE('',#11217,#11218,#5234,.T.);
#14812=EDGE_CURVE('',#11218,#11215,#7574,.T.);
#14813=EDGE_CURVE('',#11217,#11212,#5235,.T.);
#14814=EDGE_CURVE('',#11209,#11216,#5236,.T.);
#14815=EDGE_CURVE('',#11219,#11220,#5237,.T.);
#14816=EDGE_CURVE('',#11220,#11221,#7575,.T.);
#14817=EDGE_CURVE('',#11221,#11222,#5238,.T.);
#14818=EDGE_CURVE('',#11222,#11219,#7576,.T.);
#14819=EDGE_CURVE('',#11223,#11220,#7577,.T.);
#14820=EDGE_CURVE('',#11223,#11224,#7578,.T.);
#14821=EDGE_CURVE('',#11221,#11224,#7579,.T.);
#14822=EDGE_CURVE('',#11225,#11226,#5239,.T.);
#14823=EDGE_CURVE('',#11226,#11227,#7580,.T.);
#14824=EDGE_CURVE('',#11227,#11228,#5240,.T.);
#14825=EDGE_CURVE('',#11228,#11225,#7581,.T.);
#14826=EDGE_CURVE('',#11227,#11222,#5241,.T.);
#14827=EDGE_CURVE('',#11219,#11226,#5242,.T.);
#14828=EDGE_CURVE('',#11229,#11230,#5243,.T.);
#14829=EDGE_CURVE('',#11230,#11231,#7582,.T.);
#14830=EDGE_CURVE('',#11231,#11232,#5244,.T.);
#14831=EDGE_CURVE('',#11232,#11229,#7583,.T.);
#14832=EDGE_CURVE('',#11233,#11230,#7584,.T.);
#14833=EDGE_CURVE('',#11233,#11234,#7585,.T.);
#14834=EDGE_CURVE('',#11231,#11234,#7586,.T.);
#14835=EDGE_CURVE('',#11235,#11236,#5245,.T.);
#14836=EDGE_CURVE('',#11236,#11237,#7587,.T.);
#14837=EDGE_CURVE('',#11237,#11238,#5246,.T.);
#14838=EDGE_CURVE('',#11238,#11235,#7588,.T.);
#14839=EDGE_CURVE('',#11237,#11232,#5247,.T.);
#14840=EDGE_CURVE('',#11229,#11236,#5248,.T.);
#14841=EDGE_CURVE('',#11239,#11018,#7589,.T.);
#14842=EDGE_CURVE('',#11240,#11239,#7590,.T.);
#14843=EDGE_CURVE('',#11015,#11240,#7591,.T.);
#14844=EDGE_CURVE('',#11241,#11013,#787,.T.);
#14845=EDGE_CURVE('',#11242,#11241,#7592,.T.);
#14846=EDGE_CURVE('',#11014,#11242,#788,.T.);
#14847=EDGE_CURVE('',#11240,#11243,#789,.T.);
#14848=EDGE_CURVE('',#11244,#11239,#790,.T.);
#14849=EDGE_CURVE('',#11243,#11244,#7593,.T.);
#14850=EDGE_CURVE('',#11245,#11028,#7594,.T.);
#14851=EDGE_CURVE('',#11246,#11245,#7595,.T.);
#14852=EDGE_CURVE('',#11025,#11246,#7596,.T.);
#14853=EDGE_CURVE('',#11247,#11023,#791,.T.);
#14854=EDGE_CURVE('',#11248,#11247,#7597,.T.);
#14855=EDGE_CURVE('',#11024,#11248,#792,.T.);
#14856=EDGE_CURVE('',#11246,#11249,#793,.T.);
#14857=EDGE_CURVE('',#11250,#11245,#794,.T.);
#14858=EDGE_CURVE('',#11249,#11250,#7598,.T.);
#14859=EDGE_CURVE('',#11251,#11038,#7599,.T.);
#14860=EDGE_CURVE('',#11252,#11251,#7600,.T.);
#14861=EDGE_CURVE('',#11035,#11252,#7601,.T.);
#14862=EDGE_CURVE('',#11253,#11033,#795,.T.);
#14863=EDGE_CURVE('',#11254,#11253,#7602,.T.);
#14864=EDGE_CURVE('',#11034,#11254,#796,.T.);
#14865=EDGE_CURVE('',#11252,#11255,#797,.T.);
#14866=EDGE_CURVE('',#11256,#11251,#798,.T.);
#14867=EDGE_CURVE('',#11255,#11256,#7603,.T.);
#14868=EDGE_CURVE('',#11257,#11048,#7604,.T.);
#14869=EDGE_CURVE('',#11258,#11257,#7605,.T.);
#14870=EDGE_CURVE('',#11045,#11258,#7606,.T.);
#14871=EDGE_CURVE('',#11259,#11043,#799,.T.);
#14872=EDGE_CURVE('',#11260,#11259,#7607,.T.);
#14873=EDGE_CURVE('',#11044,#11260,#800,.T.);
#14874=EDGE_CURVE('',#11258,#11261,#801,.T.);
#14875=EDGE_CURVE('',#11262,#11257,#802,.T.);
#14876=EDGE_CURVE('',#11261,#11262,#7608,.T.);
#14877=EDGE_CURVE('',#11263,#11058,#7609,.T.);
#14878=EDGE_CURVE('',#11264,#11263,#7610,.T.);
#14879=EDGE_CURVE('',#11055,#11264,#7611,.T.);
#14880=EDGE_CURVE('',#11265,#11053,#803,.T.);
#14881=EDGE_CURVE('',#11266,#11265,#7612,.T.);
#14882=EDGE_CURVE('',#11054,#11266,#804,.T.);
#14883=EDGE_CURVE('',#11264,#11267,#805,.T.);
#14884=EDGE_CURVE('',#11268,#11263,#806,.T.);
#14885=EDGE_CURVE('',#11267,#11268,#7613,.T.);
#14886=EDGE_CURVE('',#11269,#11068,#7614,.T.);
#14887=EDGE_CURVE('',#11270,#11269,#7615,.T.);
#14888=EDGE_CURVE('',#11065,#11270,#7616,.T.);
#14889=EDGE_CURVE('',#11271,#11063,#807,.T.);
#14890=EDGE_CURVE('',#11272,#11271,#7617,.T.);
#14891=EDGE_CURVE('',#11064,#11272,#808,.T.);
#14892=EDGE_CURVE('',#11270,#11273,#809,.T.);
#14893=EDGE_CURVE('',#11274,#11269,#810,.T.);
#14894=EDGE_CURVE('',#11273,#11274,#7618,.T.);
#14895=EDGE_CURVE('',#11275,#11078,#7619,.T.);
#14896=EDGE_CURVE('',#11276,#11275,#7620,.T.);
#14897=EDGE_CURVE('',#11075,#11276,#7621,.T.);
#14898=EDGE_CURVE('',#11277,#11073,#811,.T.);
#14899=EDGE_CURVE('',#11278,#11277,#7622,.T.);
#14900=EDGE_CURVE('',#11074,#11278,#812,.T.);
#14901=EDGE_CURVE('',#11276,#11279,#813,.T.);
#14902=EDGE_CURVE('',#11280,#11275,#814,.T.);
#14903=EDGE_CURVE('',#11279,#11280,#7623,.T.);
#14904=EDGE_CURVE('',#11281,#11088,#7624,.T.);
#14905=EDGE_CURVE('',#11282,#11281,#7625,.T.);
#14906=EDGE_CURVE('',#11085,#11282,#7626,.T.);
#14907=EDGE_CURVE('',#11283,#11083,#815,.T.);
#14908=EDGE_CURVE('',#11284,#11283,#7627,.T.);
#14909=EDGE_CURVE('',#11084,#11284,#816,.T.);
#14910=EDGE_CURVE('',#11282,#11285,#817,.T.);
#14911=EDGE_CURVE('',#11286,#11281,#818,.T.);
#14912=EDGE_CURVE('',#11285,#11286,#7628,.T.);
#14913=EDGE_CURVE('',#11287,#11098,#7629,.T.);
#14914=EDGE_CURVE('',#11288,#11287,#7630,.T.);
#14915=EDGE_CURVE('',#11095,#11288,#7631,.T.);
#14916=EDGE_CURVE('',#11289,#11093,#819,.T.);
#14917=EDGE_CURVE('',#11290,#11289,#7632,.T.);
#14918=EDGE_CURVE('',#11094,#11290,#820,.T.);
#14919=EDGE_CURVE('',#11288,#11291,#821,.T.);
#14920=EDGE_CURVE('',#11292,#11287,#822,.T.);
#14921=EDGE_CURVE('',#11291,#11292,#7633,.T.);
#14922=EDGE_CURVE('',#11293,#11108,#7634,.T.);
#14923=EDGE_CURVE('',#11294,#11293,#7635,.T.);
#14924=EDGE_CURVE('',#11105,#11294,#7636,.T.);
#14925=EDGE_CURVE('',#11295,#11103,#823,.T.);
#14926=EDGE_CURVE('',#11296,#11295,#7637,.T.);
#14927=EDGE_CURVE('',#11104,#11296,#824,.T.);
#14928=EDGE_CURVE('',#11294,#11297,#825,.T.);
#14929=EDGE_CURVE('',#11298,#11293,#826,.T.);
#14930=EDGE_CURVE('',#11297,#11298,#7638,.T.);
#14931=EDGE_CURVE('',#11299,#11118,#7639,.T.);
#14932=EDGE_CURVE('',#11300,#11299,#7640,.T.);
#14933=EDGE_CURVE('',#11115,#11300,#7641,.T.);
#14934=EDGE_CURVE('',#11301,#11113,#827,.T.);
#14935=EDGE_CURVE('',#11302,#11301,#7642,.T.);
#14936=EDGE_CURVE('',#11114,#11302,#828,.T.);
#14937=EDGE_CURVE('',#11300,#11303,#829,.T.);
#14938=EDGE_CURVE('',#11304,#11299,#830,.T.);
#14939=EDGE_CURVE('',#11303,#11304,#7643,.T.);
#14940=EDGE_CURVE('',#11305,#11128,#7644,.T.);
#14941=EDGE_CURVE('',#11306,#11305,#7645,.T.);
#14942=EDGE_CURVE('',#11125,#11306,#7646,.T.);
#14943=EDGE_CURVE('',#11307,#11123,#831,.T.);
#14944=EDGE_CURVE('',#11308,#11307,#7647,.T.);
#14945=EDGE_CURVE('',#11124,#11308,#832,.T.);
#14946=EDGE_CURVE('',#11306,#11309,#833,.T.);
#14947=EDGE_CURVE('',#11310,#11305,#834,.T.);
#14948=EDGE_CURVE('',#11309,#11310,#7648,.T.);
#14949=EDGE_CURVE('',#11311,#11138,#7649,.T.);
#14950=EDGE_CURVE('',#11312,#11311,#7650,.T.);
#14951=EDGE_CURVE('',#11135,#11312,#7651,.T.);
#14952=EDGE_CURVE('',#11313,#11133,#835,.T.);
#14953=EDGE_CURVE('',#11314,#11313,#7652,.T.);
#14954=EDGE_CURVE('',#11134,#11314,#836,.T.);
#14955=EDGE_CURVE('',#11312,#11315,#837,.T.);
#14956=EDGE_CURVE('',#11316,#11311,#838,.T.);
#14957=EDGE_CURVE('',#11315,#11316,#7653,.T.);
#14958=EDGE_CURVE('',#11317,#11148,#7654,.T.);
#14959=EDGE_CURVE('',#11318,#11317,#7655,.T.);
#14960=EDGE_CURVE('',#11145,#11318,#7656,.T.);
#14961=EDGE_CURVE('',#11319,#11143,#839,.T.);
#14962=EDGE_CURVE('',#11320,#11319,#7657,.T.);
#14963=EDGE_CURVE('',#11144,#11320,#840,.T.);
#14964=EDGE_CURVE('',#11318,#11321,#841,.T.);
#14965=EDGE_CURVE('',#11322,#11317,#842,.T.);
#14966=EDGE_CURVE('',#11321,#11322,#7658,.T.);
#14967=EDGE_CURVE('',#11323,#11158,#7659,.T.);
#14968=EDGE_CURVE('',#11324,#11323,#7660,.T.);
#14969=EDGE_CURVE('',#11155,#11324,#7661,.T.);
#14970=EDGE_CURVE('',#11325,#11153,#843,.T.);
#14971=EDGE_CURVE('',#11326,#11325,#7662,.T.);
#14972=EDGE_CURVE('',#11154,#11326,#844,.T.);
#14973=EDGE_CURVE('',#11324,#11327,#845,.T.);
#14974=EDGE_CURVE('',#11328,#11323,#846,.T.);
#14975=EDGE_CURVE('',#11327,#11328,#7663,.T.);
#14976=EDGE_CURVE('',#11329,#11168,#7664,.T.);
#14977=EDGE_CURVE('',#11330,#11329,#7665,.T.);
#14978=EDGE_CURVE('',#11165,#11330,#7666,.T.);
#14979=EDGE_CURVE('',#11331,#11163,#847,.T.);
#14980=EDGE_CURVE('',#11332,#11331,#7667,.T.);
#14981=EDGE_CURVE('',#11164,#11332,#848,.T.);
#14982=EDGE_CURVE('',#11330,#11333,#849,.T.);
#14983=EDGE_CURVE('',#11334,#11329,#850,.T.);
#14984=EDGE_CURVE('',#11333,#11334,#7668,.T.);
#14985=EDGE_CURVE('',#11335,#11178,#7669,.T.);
#14986=EDGE_CURVE('',#11336,#11335,#7670,.T.);
#14987=EDGE_CURVE('',#11175,#11336,#7671,.T.);
#14988=EDGE_CURVE('',#11337,#11173,#851,.T.);
#14989=EDGE_CURVE('',#11338,#11337,#7672,.T.);
#14990=EDGE_CURVE('',#11174,#11338,#852,.T.);
#14991=EDGE_CURVE('',#11336,#11339,#853,.T.);
#14992=EDGE_CURVE('',#11340,#11335,#854,.T.);
#14993=EDGE_CURVE('',#11339,#11340,#7673,.T.);
#14994=EDGE_CURVE('',#11341,#11188,#7674,.T.);
#14995=EDGE_CURVE('',#11342,#11341,#7675,.T.);
#14996=EDGE_CURVE('',#11185,#11342,#7676,.T.);
#14997=EDGE_CURVE('',#11343,#11183,#855,.T.);
#14998=EDGE_CURVE('',#11344,#11343,#7677,.T.);
#14999=EDGE_CURVE('',#11184,#11344,#856,.T.);
#15000=EDGE_CURVE('',#11342,#11345,#857,.T.);
#15001=EDGE_CURVE('',#11346,#11341,#858,.T.);
#15002=EDGE_CURVE('',#11345,#11346,#7678,.T.);
#15003=EDGE_CURVE('',#11347,#11198,#7679,.T.);
#15004=EDGE_CURVE('',#11348,#11347,#7680,.T.);
#15005=EDGE_CURVE('',#11195,#11348,#7681,.T.);
#15006=EDGE_CURVE('',#11349,#11193,#859,.T.);
#15007=EDGE_CURVE('',#11350,#11349,#7682,.T.);
#15008=EDGE_CURVE('',#11194,#11350,#860,.T.);
#15009=EDGE_CURVE('',#11348,#11351,#861,.T.);
#15010=EDGE_CURVE('',#11352,#11347,#862,.T.);
#15011=EDGE_CURVE('',#11351,#11352,#7683,.T.);
#15012=EDGE_CURVE('',#11353,#11208,#7684,.T.);
#15013=EDGE_CURVE('',#11354,#11353,#7685,.T.);
#15014=EDGE_CURVE('',#11205,#11354,#7686,.T.);
#15015=EDGE_CURVE('',#11355,#11203,#863,.T.);
#15016=EDGE_CURVE('',#11356,#11355,#7687,.T.);
#15017=EDGE_CURVE('',#11204,#11356,#864,.T.);
#15018=EDGE_CURVE('',#11354,#11357,#865,.T.);
#15019=EDGE_CURVE('',#11358,#11353,#866,.T.);
#15020=EDGE_CURVE('',#11357,#11358,#7688,.T.);
#15021=EDGE_CURVE('',#11359,#11218,#7689,.T.);
#15022=EDGE_CURVE('',#11360,#11359,#7690,.T.);
#15023=EDGE_CURVE('',#11215,#11360,#7691,.T.);
#15024=EDGE_CURVE('',#11361,#11213,#867,.T.);
#15025=EDGE_CURVE('',#11362,#11361,#7692,.T.);
#15026=EDGE_CURVE('',#11214,#11362,#868,.T.);
#15027=EDGE_CURVE('',#11360,#11363,#869,.T.);
#15028=EDGE_CURVE('',#11364,#11359,#870,.T.);
#15029=EDGE_CURVE('',#11363,#11364,#7693,.T.);
#15030=EDGE_CURVE('',#11365,#11228,#7694,.T.);
#15031=EDGE_CURVE('',#11366,#11365,#7695,.T.);
#15032=EDGE_CURVE('',#11225,#11366,#7696,.T.);
#15033=EDGE_CURVE('',#11367,#11223,#871,.T.);
#15034=EDGE_CURVE('',#11368,#11367,#7697,.T.);
#15035=EDGE_CURVE('',#11224,#11368,#872,.T.);
#15036=EDGE_CURVE('',#11366,#11369,#873,.T.);
#15037=EDGE_CURVE('',#11370,#11365,#874,.T.);
#15038=EDGE_CURVE('',#11369,#11370,#7698,.T.);
#15039=EDGE_CURVE('',#11371,#11238,#7699,.T.);
#15040=EDGE_CURVE('',#11372,#11371,#7700,.T.);
#15041=EDGE_CURVE('',#11235,#11372,#7701,.T.);
#15042=EDGE_CURVE('',#11373,#11233,#875,.T.);
#15043=EDGE_CURVE('',#11374,#11373,#7702,.T.);
#15044=EDGE_CURVE('',#11234,#11374,#876,.T.);
#15045=EDGE_CURVE('',#11372,#11375,#877,.T.);
#15046=EDGE_CURVE('',#11376,#11371,#878,.T.);
#15047=EDGE_CURVE('',#11375,#11376,#7703,.T.);
#15048=EDGE_CURVE('',#11247,#11243,#5249,.T.);
#15049=EDGE_CURVE('',#11253,#11249,#5250,.T.);
#15050=EDGE_CURVE('',#11259,#11255,#5251,.T.);
#15051=EDGE_CURVE('',#11265,#11261,#5252,.T.);
#15052=EDGE_CURVE('',#11271,#11267,#5253,.T.);
#15053=EDGE_CURVE('',#11277,#11273,#5254,.T.);
#15054=EDGE_CURVE('',#11283,#11279,#5255,.T.);
#15055=EDGE_CURVE('',#11289,#11285,#5256,.T.);
#15056=EDGE_CURVE('',#11295,#11291,#5257,.T.);
#15057=EDGE_CURVE('',#11301,#11297,#5258,.T.);
#15058=EDGE_CURVE('',#11307,#11303,#5259,.T.);
#15059=EDGE_CURVE('',#11313,#11309,#5260,.T.);
#15060=EDGE_CURVE('',#11319,#11315,#5261,.T.);
#15061=EDGE_CURVE('',#11325,#11321,#5262,.T.);
#15062=EDGE_CURVE('',#11331,#11327,#5263,.T.);
#15063=EDGE_CURVE('',#11337,#11333,#5264,.T.);
#15064=EDGE_CURVE('',#11343,#11339,#5265,.T.);
#15065=EDGE_CURVE('',#11349,#11345,#5266,.T.);
#15066=EDGE_CURVE('',#11355,#11351,#5267,.T.);
#15067=EDGE_CURVE('',#11361,#11357,#5268,.T.);
#15068=EDGE_CURVE('',#11367,#11363,#5269,.T.);
#15069=EDGE_CURVE('',#11373,#11369,#5270,.T.);
#15070=EDGE_CURVE('',#11377,#11375,#5271,.T.);
#15071=EDGE_CURVE('',#11377,#11378,#879,.T.);
#15072=EDGE_CURVE('',#11378,#11379,#7704,.T.);
#15073=EDGE_CURVE('',#11380,#11379,#5272,.T.);
#15074=EDGE_CURVE('',#11380,#11381,#5273,.T.);
#15075=EDGE_CURVE('',#11382,#11381,#5274,.T.);
#15076=EDGE_CURVE('',#11382,#11383,#7705,.T.);
#15077=EDGE_CURVE('',#11383,#11384,#880,.T.);
#15078=EDGE_CURVE('',#11241,#11384,#5275,.T.);
#15079=EDGE_CURVE('',#11385,#11385,#5276,.T.);
#15080=EDGE_CURVE('',#11242,#11386,#5277,.T.);
#15081=EDGE_CURVE('',#11386,#11387,#881,.T.);
#15082=EDGE_CURVE('',#11387,#11388,#7706,.T.);
#15083=EDGE_CURVE('',#11389,#11388,#5278,.T.);
#15084=EDGE_CURVE('',#11389,#11390,#5279,.T.);
#15085=EDGE_CURVE('',#11391,#11390,#5280,.T.);
#15086=EDGE_CURVE('',#11391,#11392,#7707,.T.);
#15087=EDGE_CURVE('',#11392,#11393,#882,.T.);
#15088=EDGE_CURVE('',#11393,#11376,#5281,.T.);
#15089=EDGE_CURVE('',#11374,#11370,#5282,.T.);
#15090=EDGE_CURVE('',#11368,#11364,#5283,.T.);
#15091=EDGE_CURVE('',#11362,#11358,#5284,.T.);
#15092=EDGE_CURVE('',#11356,#11352,#5285,.T.);
#15093=EDGE_CURVE('',#11350,#11346,#5286,.T.);
#15094=EDGE_CURVE('',#11344,#11340,#5287,.T.);
#15095=EDGE_CURVE('',#11338,#11334,#5288,.T.);
#15096=EDGE_CURVE('',#11332,#11328,#5289,.T.);
#15097=EDGE_CURVE('',#11326,#11322,#5290,.T.);
#15098=EDGE_CURVE('',#11320,#11316,#5291,.T.);
#15099=EDGE_CURVE('',#11314,#11310,#5292,.T.);
#15100=EDGE_CURVE('',#11308,#11304,#5293,.T.);
#15101=EDGE_CURVE('',#11302,#11298,#5294,.T.);
#15102=EDGE_CURVE('',#11296,#11292,#5295,.T.);
#15103=EDGE_CURVE('',#11290,#11286,#5296,.T.);
#15104=EDGE_CURVE('',#11284,#11280,#5297,.T.);
#15105=EDGE_CURVE('',#11278,#11274,#5298,.T.);
#15106=EDGE_CURVE('',#11272,#11268,#5299,.T.);
#15107=EDGE_CURVE('',#11266,#11262,#5300,.T.);
#15108=EDGE_CURVE('',#11260,#11256,#5301,.T.);
#15109=EDGE_CURVE('',#11254,#11250,#5302,.T.);
#15110=EDGE_CURVE('',#11248,#11244,#5303,.T.);
#15111=EDGE_CURVE('',#11394,#11394,#5304,.T.);
#15112=EDGE_CURVE('',#11393,#11377,#7708,.T.);
#15113=EDGE_CURVE('',#11379,#11391,#7709,.T.);
#15114=EDGE_CURVE('',#11390,#11380,#7710,.T.);
#15115=EDGE_CURVE('',#11378,#11392,#7711,.T.);
#15116=EDGE_CURVE('',#11381,#11389,#7712,.T.);
#15117=EDGE_CURVE('',#11388,#11382,#7713,.T.);
#15118=EDGE_CURVE('',#11383,#11387,#7714,.T.);
#15119=EDGE_CURVE('',#11384,#11386,#7715,.T.);
#15120=EDGE_CURVE('',#11394,#11385,#7716,.T.);
#15121=EDGE_CURVE('',#11395,#11395,#5305,.T.);
#15122=EDGE_CURVE('',#11395,#11396,#7717,.T.);
#15123=EDGE_CURVE('',#11396,#11396,#5306,.T.);
#15124=EDGE_CURVE('',#11397,#11397,#5307,.T.);
#15125=EDGE_CURVE('',#11397,#11398,#7718,.T.);
#15126=EDGE_CURVE('',#11398,#11398,#5308,.T.);
#15127=EDGE_CURVE('',#11399,#11400,#7719,.T.);
#15128=EDGE_CURVE('',#11399,#11401,#7720,.T.);
#15129=EDGE_CURVE('',#11402,#11401,#7721,.T.);
#15130=EDGE_CURVE('',#11402,#11400,#7722,.T.);
#15131=EDGE_CURVE('',#11400,#11403,#5309,.T.);
#15132=EDGE_CURVE('',#11404,#11402,#7723,.T.);
#15133=EDGE_CURVE('',#11403,#11404,#7724,.T.);
#15134=EDGE_CURVE('',#11403,#11405,#7725,.T.);
#15135=EDGE_CURVE('',#11404,#11406,#7726,.T.);
#15136=EDGE_CURVE('',#11406,#11405,#7727,.T.);
#15137=EDGE_CURVE('',#11401,#11406,#7728,.T.);
#15138=EDGE_CURVE('',#11405,#11399,#5310,.T.);
#15139=EDGE_CURVE('',#11407,#11407,#5311,.T.);
#15140=EDGE_CURVE('',#11407,#11408,#7729,.T.);
#15141=EDGE_CURVE('',#11408,#11408,#5312,.T.);
#15142=EDGE_CURVE('',#11409,#11409,#5313,.T.);
#15143=EDGE_CURVE('',#11410,#11410,#5314,.T.);
#15144=EDGE_CURVE('',#11411,#11411,#5315,.T.);
#15145=EDGE_CURVE('',#11411,#11410,#7730,.T.);
#15146=EDGE_CURVE('',#11412,#11412,#5316,.T.);
#15147=EDGE_CURVE('',#11412,#11413,#7731,.T.);
#15148=EDGE_CURVE('',#11413,#11413,#5317,.T.);
#15149=EDGE_CURVE('',#11414,#11414,#5318,.T.);
#15150=EDGE_CURVE('',#11415,#11415,#5319,.T.);
#15151=EDGE_CURVE('',#11416,#11416,#5320,.T.);
#15152=EDGE_CURVE('',#11416,#11415,#7732,.T.);
#15153=EDGE_CURVE('',#11417,#11417,#5321,.T.);
#15154=EDGE_CURVE('',#11417,#11418,#7733,.T.);
#15155=EDGE_CURVE('',#11418,#11418,#5322,.T.);
#15156=EDGE_CURVE('',#11419,#11419,#5323,.T.);
#15157=EDGE_CURVE('',#11419,#11420,#7734,.T.);
#15158=EDGE_CURVE('',#11420,#11420,#5324,.T.);
#15159=EDGE_CURVE('',#11421,#11421,#5325,.T.);
#15160=EDGE_CURVE('',#11421,#11422,#7735,.T.);
#15161=EDGE_CURVE('',#11422,#11422,#5326,.T.);
#15162=EDGE_CURVE('',#11423,#11423,#5327,.T.);
#15163=EDGE_CURVE('',#11424,#11424,#5328,.T.);
#15164=EDGE_CURVE('',#11425,#11425,#5329,.T.);
#15165=EDGE_CURVE('',#11426,#11426,#5330,.T.);
#15166=EDGE_CURVE('',#11423,#11425,#7736,.T.);
#15167=EDGE_CURVE('',#11426,#11427,#7737,.T.);
#15168=EDGE_CURVE('',#11427,#11427,#5331,.T.);
#15169=EDGE_CURVE('',#11409,#11424,#7738,.T.);
#15170=EDGE_CURVE('',#11428,#11428,#5332,.T.);
#15171=EDGE_CURVE('',#11429,#11429,#5333,.T.);
#15172=EDGE_CURVE('',#11430,#11430,#5334,.T.);
#15173=EDGE_CURVE('',#11431,#11431,#5335,.T.);
#15174=EDGE_CURVE('',#11428,#11430,#7739,.T.);
#15175=EDGE_CURVE('',#11431,#11432,#7740,.T.);
#15176=EDGE_CURVE('',#11432,#11432,#5336,.T.);
#15177=EDGE_CURVE('',#11433,#11433,#5337,.T.);
#15178=EDGE_CURVE('',#11414,#11429,#7741,.T.);
#15179=EDGE_CURVE('',#11433,#11434,#7742,.T.);
#15180=EDGE_CURVE('',#11434,#11434,#5338,.T.);
#15181=EDGE_CURVE('',#11435,#11435,#5339,.T.);
#15182=EDGE_CURVE('',#11435,#11436,#7743,.T.);
#15183=EDGE_CURVE('',#11436,#11436,#5340,.T.);
#15184=EDGE_CURVE('',#11437,#11438,#7744,.T.);
#15185=EDGE_CURVE('',#11438,#11439,#7745,.T.);
#15186=EDGE_CURVE('',#11440,#11439,#7746,.T.);
#15187=EDGE_CURVE('',#11437,#11440,#7747,.T.);
#15188=EDGE_CURVE('',#11441,#11437,#7748,.T.);
#15189=EDGE_CURVE('',#11442,#11440,#7749,.T.);
#15190=EDGE_CURVE('',#11441,#11442,#7750,.T.);
#15191=EDGE_CURVE('',#11443,#11441,#7751,.T.);
#15192=EDGE_CURVE('',#11444,#11442,#7752,.T.);
#15193=EDGE_CURVE('',#11443,#11444,#7753,.T.);
#15194=EDGE_CURVE('',#11438,#11443,#7754,.T.);
#15195=EDGE_CURVE('',#11439,#11444,#7755,.T.);
#15196=EDGE_CURVE('',#11445,#11445,#5341,.T.);
#15197=EDGE_CURVE('',#11445,#11446,#7756,.T.);
#15198=EDGE_CURVE('',#11446,#11446,#5342,.T.);
#15199=EDGE_CURVE('',#11447,#11447,#5343,.T.);
#15200=EDGE_CURVE('',#11447,#11448,#7757,.T.);
#15201=EDGE_CURVE('',#11448,#11448,#5344,.T.);
#15202=EDGE_CURVE('',#11449,#11449,#5345,.T.);
#15203=EDGE_CURVE('',#11449,#11450,#7758,.T.);
#15204=EDGE_CURVE('',#11450,#11450,#5346,.T.);
#15205=EDGE_CURVE('',#11451,#11451,#5347,.T.);
#15206=EDGE_CURVE('',#11452,#11452,#5348,.T.);
#15207=EDGE_CURVE('',#11453,#11453,#5349,.T.);
#15208=EDGE_CURVE('',#11453,#11452,#7759,.T.);
#15209=EDGE_CURVE('',#11454,#11454,#5350,.T.);
#15210=EDGE_CURVE('',#11455,#11455,#5351,.T.);
#15211=EDGE_CURVE('',#11454,#11456,#7760,.T.);
#15212=EDGE_CURVE('',#11456,#11456,#5352,.T.);
#15213=EDGE_CURVE('',#11451,#11455,#7761,.T.);
#15214=EDGE_CURVE('',#11457,#11458,#7762,.T.);
#15215=EDGE_CURVE('',#11459,#11457,#7763,.T.);
#15216=EDGE_CURVE('',#11460,#11459,#7764,.T.);
#15217=EDGE_CURVE('',#11458,#11460,#7765,.T.);
#15218=EDGE_CURVE('',#11461,#11462,#7766,.T.);
#15219=EDGE_CURVE('',#11463,#11461,#7767,.T.);
#15220=EDGE_CURVE('',#11464,#11463,#7768,.T.);
#15221=EDGE_CURVE('',#11462,#11464,#7769,.T.);
#15222=EDGE_CURVE('',#11459,#11464,#5353,.T.);
#15223=EDGE_CURVE('',#11462,#11457,#5354,.T.);
#15224=EDGE_CURVE('',#11461,#11458,#5355,.T.);
#15225=EDGE_CURVE('',#11460,#11463,#5356,.T.);
#15226=EDGE_CURVE('',#11465,#11465,#5357,.T.);
#15227=EDGE_CURVE('',#11465,#11466,#7770,.T.);
#15228=EDGE_CURVE('',#11466,#11466,#5358,.T.);
#15229=EDGE_CURVE('',#11467,#11467,#5359,.T.);
#15230=EDGE_CURVE('',#11467,#11468,#7771,.T.);
#15231=EDGE_CURVE('',#11468,#11468,#5360,.T.);
#15232=EDGE_CURVE('',#11469,#11469,#5361,.T.);
#15233=EDGE_CURVE('',#11469,#11470,#7772,.T.);
#15234=EDGE_CURVE('',#11470,#11470,#5362,.T.);
#15235=EDGE_CURVE('',#11471,#11471,#5363,.T.);
#15236=EDGE_CURVE('',#11471,#11472,#7773,.T.);
#15237=EDGE_CURVE('',#11472,#11472,#5364,.T.);
#15238=EDGE_CURVE('',#11473,#11473,#5365,.T.);
#15239=EDGE_CURVE('',#11473,#11474,#7774,.T.);
#15240=EDGE_CURVE('',#11474,#11474,#5366,.T.);
#15241=EDGE_CURVE('',#11475,#11475,#5367,.T.);
#15242=EDGE_CURVE('',#11475,#11476,#7775,.T.);
#15243=EDGE_CURVE('',#11476,#11476,#5368,.T.);
#15244=EDGE_CURVE('',#11477,#11478,#7776,.T.);
#15245=EDGE_CURVE('',#11479,#11477,#7777,.T.);
#15246=EDGE_CURVE('',#11480,#11479,#7778,.T.);
#15247=EDGE_CURVE('',#11478,#11480,#7779,.T.);
#15248=EDGE_CURVE('',#11481,#11482,#7780,.T.);
#15249=EDGE_CURVE('',#11483,#11481,#7781,.T.);
#15250=EDGE_CURVE('',#11484,#11483,#7782,.T.);
#15251=EDGE_CURVE('',#11482,#11484,#7783,.T.);
#15252=EDGE_CURVE('',#11479,#11484,#5369,.T.);
#15253=EDGE_CURVE('',#11482,#11477,#5370,.T.);
#15254=EDGE_CURVE('',#11481,#11478,#5371,.T.);
#15255=EDGE_CURVE('',#11480,#11483,#5372,.T.);
#15256=EDGE_CURVE('',#11485,#11486,#7784,.T.);
#15257=EDGE_CURVE('',#11487,#11485,#7785,.T.);
#15258=EDGE_CURVE('',#11488,#11487,#7786,.T.);
#15259=EDGE_CURVE('',#11486,#11488,#7787,.T.);
#15260=EDGE_CURVE('',#11489,#11490,#7788,.T.);
#15261=EDGE_CURVE('',#11491,#11489,#7789,.T.);
#15262=EDGE_CURVE('',#11492,#11491,#7790,.T.);
#15263=EDGE_CURVE('',#11490,#11492,#7791,.T.);
#15264=EDGE_CURVE('',#11487,#11492,#5373,.T.);
#15265=EDGE_CURVE('',#11490,#11485,#5374,.T.);
#15266=EDGE_CURVE('',#11489,#11486,#5375,.T.);
#15267=EDGE_CURVE('',#11488,#11491,#5376,.T.);
#15268=EDGE_CURVE('',#11493,#11493,#5377,.T.);
#15269=EDGE_CURVE('',#11493,#11494,#7792,.T.);
#15270=EDGE_CURVE('',#11494,#11494,#5378,.T.);
#15271=EDGE_CURVE('',#11495,#11496,#7793,.T.);
#15272=EDGE_CURVE('',#11495,#11497,#6579,.T.);
#15273=EDGE_CURVE('',#11497,#11498,#5379,.F.);
#15274=EDGE_CURVE('',#11498,#11496,#6580,.T.);
#15275=EDGE_CURVE('',#11499,#11500,#7794,.T.);
#15276=EDGE_CURVE('',#11499,#11495,#6581,.T.);
#15277=EDGE_CURVE('',#11496,#11500,#6582,.T.);
#15278=EDGE_CURVE('',#11501,#11502,#7795,.T.);
#15279=EDGE_CURVE('',#11501,#11499,#6583,.T.);
#15280=EDGE_CURVE('',#11500,#11502,#6584,.T.);
#15281=EDGE_CURVE('',#11503,#11504,#7796,.T.);
#15282=EDGE_CURVE('',#11503,#11501,#6585,.T.);
#15283=EDGE_CURVE('',#11502,#11504,#6586,.T.);
#15284=EDGE_CURVE('',#11505,#11506,#7797,.T.);
#15285=EDGE_CURVE('',#11505,#11503,#6587,.T.);
#15286=EDGE_CURVE('',#11504,#11506,#6588,.T.);
#15287=EDGE_CURVE('',#11507,#11508,#7798,.T.);
#15288=EDGE_CURVE('',#11507,#11505,#6589,.T.);
#15289=EDGE_CURVE('',#11506,#11508,#6590,.T.);
#15290=EDGE_CURVE('',#11509,#11510,#7799,.T.);
#15291=EDGE_CURVE('',#11509,#11507,#6591,.T.);
#15292=EDGE_CURVE('',#11508,#11510,#6592,.T.);
#15293=EDGE_CURVE('',#11511,#11512,#7800,.T.);
#15294=EDGE_CURVE('',#11511,#11509,#6593,.T.);
#15295=EDGE_CURVE('',#11510,#11512,#6594,.T.);
#15296=EDGE_CURVE('',#11513,#11514,#7801,.T.);
#15297=EDGE_CURVE('',#11513,#11511,#6595,.T.);
#15298=EDGE_CURVE('',#11512,#11514,#6596,.T.);
#15299=EDGE_CURVE('',#11515,#11516,#7802,.T.);
#15300=EDGE_CURVE('',#11515,#11513,#6597,.T.);
#15301=EDGE_CURVE('',#11514,#11516,#6598,.T.);
#15302=EDGE_CURVE('',#11517,#11518,#7803,.T.);
#15303=EDGE_CURVE('',#11517,#11515,#6599,.T.);
#15304=EDGE_CURVE('',#11516,#11518,#6600,.T.);
#15305=EDGE_CURVE('',#11519,#11520,#7804,.T.);
#15306=EDGE_CURVE('',#11519,#11517,#6601,.T.);
#15307=EDGE_CURVE('',#11518,#11520,#6602,.T.);
#15308=EDGE_CURVE('',#11521,#11522,#7805,.T.);
#15309=EDGE_CURVE('',#11521,#11519,#6603,.T.);
#15310=EDGE_CURVE('',#11520,#11522,#6604,.T.);
#15311=EDGE_CURVE('',#11523,#11524,#7806,.T.);
#15312=EDGE_CURVE('',#11523,#11521,#6605,.T.);
#15313=EDGE_CURVE('',#11522,#11524,#6606,.T.);
#15314=EDGE_CURVE('',#11525,#11526,#7807,.T.);
#15315=EDGE_CURVE('',#11525,#11523,#6607,.T.);
#15316=EDGE_CURVE('',#11524,#11526,#6608,.T.);
#15317=EDGE_CURVE('',#11527,#11528,#7808,.T.);
#15318=EDGE_CURVE('',#11527,#11525,#6609,.T.);
#15319=EDGE_CURVE('',#11526,#11528,#6610,.T.);
#15320=EDGE_CURVE('',#11529,#11530,#7809,.T.);
#15321=EDGE_CURVE('',#11529,#11527,#6611,.T.);
#15322=EDGE_CURVE('',#11528,#11530,#6612,.T.);
#15323=EDGE_CURVE('',#11531,#11532,#7810,.T.);
#15324=EDGE_CURVE('',#11531,#11529,#6613,.T.);
#15325=EDGE_CURVE('',#11530,#11532,#6614,.T.);
#15326=EDGE_CURVE('',#11533,#11534,#7811,.T.);
#15327=EDGE_CURVE('',#11533,#11531,#6615,.T.);
#15328=EDGE_CURVE('',#11532,#11534,#6616,.T.);
#15329=EDGE_CURVE('',#11535,#11536,#7812,.T.);
#15330=EDGE_CURVE('',#11535,#11533,#6617,.T.);
#15331=EDGE_CURVE('',#11534,#11536,#6618,.T.);
#15332=EDGE_CURVE('',#11537,#11538,#7813,.T.);
#15333=EDGE_CURVE('',#11537,#11539,#6619,.T.);
#15334=EDGE_CURVE('',#11540,#11539,#5380,.T.);
#15335=EDGE_CURVE('',#11538,#11540,#6620,.T.);
#15336=EDGE_CURVE('',#11541,#11542,#7814,.T.);
#15337=EDGE_CURVE('',#11541,#11537,#6621,.T.);
#15338=EDGE_CURVE('',#11542,#11538,#6622,.T.);
#15339=EDGE_CURVE('',#11543,#11544,#7815,.T.);
#15340=EDGE_CURVE('',#11543,#11541,#6623,.T.);
#15341=EDGE_CURVE('',#11544,#11542,#6624,.T.);
#15342=EDGE_CURVE('',#11545,#11546,#7816,.T.);
#15343=EDGE_CURVE('',#11545,#11543,#6625,.T.);
#15344=EDGE_CURVE('',#11546,#11544,#6626,.T.);
#15345=EDGE_CURVE('',#11547,#11548,#7817,.T.);
#15346=EDGE_CURVE('',#11547,#11545,#6627,.T.);
#15347=EDGE_CURVE('',#11548,#11546,#6628,.T.);
#15348=EDGE_CURVE('',#11549,#11550,#7818,.T.);
#15349=EDGE_CURVE('',#11549,#11547,#6629,.T.);
#15350=EDGE_CURVE('',#11550,#11548,#6630,.T.);
#15351=EDGE_CURVE('',#11551,#11552,#7819,.T.);
#15352=EDGE_CURVE('',#11551,#11549,#6631,.T.);
#15353=EDGE_CURVE('',#11552,#11550,#6632,.T.);
#15354=EDGE_CURVE('',#11553,#11554,#7820,.T.);
#15355=EDGE_CURVE('',#11553,#11551,#6633,.T.);
#15356=EDGE_CURVE('',#11554,#11552,#6634,.T.);
#15357=EDGE_CURVE('',#11555,#11556,#7821,.T.);
#15358=EDGE_CURVE('',#11555,#11553,#6635,.T.);
#15359=EDGE_CURVE('',#11556,#11554,#6636,.T.);
#15360=EDGE_CURVE('',#11557,#11558,#7822,.T.);
#15361=EDGE_CURVE('',#11557,#11555,#6637,.T.);
#15362=EDGE_CURVE('',#11558,#11556,#6638,.T.);
#15363=EDGE_CURVE('',#11559,#11560,#7823,.T.);
#15364=EDGE_CURVE('',#11559,#11557,#6639,.T.);
#15365=EDGE_CURVE('',#11560,#11558,#6640,.T.);
#15366=EDGE_CURVE('',#11561,#11562,#7824,.T.);
#15367=EDGE_CURVE('',#11561,#11559,#6641,.T.);
#15368=EDGE_CURVE('',#11562,#11560,#6642,.T.);
#15369=EDGE_CURVE('',#11563,#11564,#7825,.T.);
#15370=EDGE_CURVE('',#11563,#11561,#6643,.T.);
#15371=EDGE_CURVE('',#11564,#11562,#6644,.T.);
#15372=EDGE_CURVE('',#11565,#11566,#7826,.T.);
#15373=EDGE_CURVE('',#11565,#11563,#6645,.T.);
#15374=EDGE_CURVE('',#11566,#11564,#6646,.T.);
#15375=EDGE_CURVE('',#11567,#11568,#7827,.T.);
#15376=EDGE_CURVE('',#11567,#11565,#6647,.T.);
#15377=EDGE_CURVE('',#11568,#11566,#6648,.T.);
#15378=EDGE_CURVE('',#11569,#11570,#7828,.T.);
#15379=EDGE_CURVE('',#11569,#11567,#6649,.T.);
#15380=EDGE_CURVE('',#11570,#11568,#6650,.T.);
#15381=EDGE_CURVE('',#11571,#11572,#7829,.T.);
#15382=EDGE_CURVE('',#11571,#11569,#6651,.T.);
#15383=EDGE_CURVE('',#11572,#11570,#6652,.T.);
#15384=EDGE_CURVE('',#11573,#11574,#7830,.T.);
#15385=EDGE_CURVE('',#11573,#11571,#6653,.T.);
#15386=EDGE_CURVE('',#11574,#11572,#6654,.T.);
#15387=EDGE_CURVE('',#11575,#11576,#7831,.T.);
#15388=EDGE_CURVE('',#11575,#11573,#6655,.T.);
#15389=EDGE_CURVE('',#11576,#11574,#6656,.T.);
#15390=EDGE_CURVE('',#11577,#11578,#7832,.T.);
#15391=EDGE_CURVE('',#11577,#11575,#6657,.T.);
#15392=EDGE_CURVE('',#11578,#11576,#6658,.T.);
#15393=EDGE_CURVE('',#11579,#11540,#6659,.T.);
#15394=EDGE_CURVE('',#11536,#11579,#6660,.T.);
#15395=EDGE_CURVE('',#11580,#11498,#6661,.T.);
#15396=EDGE_CURVE('',#11580,#11578,#6662,.T.);
#15397=EDGE_CURVE('',#11581,#11580,#5381,.T.);
#15398=EDGE_CURVE('',#11581,#11577,#6663,.T.);
#15399=EDGE_CURVE('',#11539,#11582,#6664,.T.);
#15400=EDGE_CURVE('',#11497,#11581,#6665,.T.);
#15401=EDGE_CURVE('',#11582,#11535,#6666,.T.);
#15402=EDGE_CURVE('',#11582,#11579,#5382,.F.);
#15403=EDGE_CURVE('',#11583,#11584,#7833,.T.);
#15404=EDGE_CURVE('',#11583,#11585,#7834,.T.);
#15405=EDGE_CURVE('',#11585,#11586,#7835,.T.);
#15406=EDGE_CURVE('',#11584,#11586,#7836,.T.);
#15407=EDGE_CURVE('',#11587,#11583,#7837,.T.);
#15408=EDGE_CURVE('',#11587,#11588,#7838,.T.);
#15409=EDGE_CURVE('',#11588,#11585,#7839,.T.);
#15410=EDGE_CURVE('',#11589,#11587,#7840,.T.);
#15411=EDGE_CURVE('',#11589,#11590,#7841,.T.);
#15412=EDGE_CURVE('',#11590,#11588,#7842,.T.);
#15413=EDGE_CURVE('',#11591,#11589,#7843,.T.);
#15414=EDGE_CURVE('',#11591,#11592,#7844,.T.);
#15415=EDGE_CURVE('',#11592,#11590,#7845,.T.);
#15416=EDGE_CURVE('',#11593,#11591,#7846,.T.);
#15417=EDGE_CURVE('',#11593,#11594,#7847,.T.);
#15418=EDGE_CURVE('',#11594,#11592,#7848,.T.);
#15419=EDGE_CURVE('',#11584,#11593,#7849,.T.);
#15420=EDGE_CURVE('',#11586,#11594,#7850,.T.);
#15421=EDGE_CURVE('',#11595,#11595,#5383,.T.);
#15422=EDGE_CURVE('',#11595,#11596,#7851,.T.);
#15423=EDGE_CURVE('',#11596,#11596,#5384,.T.);
#15424=ORIENTED_EDGE('',*,*,#11597,.T.);
#15425=ORIENTED_EDGE('',*,*,#11598,.T.);
#15426=ORIENTED_EDGE('',*,*,#11599,.T.);
#15427=ORIENTED_EDGE('',*,*,#11600,.T.);
#15428=ORIENTED_EDGE('',*,*,#11601,.T.);
#15429=ORIENTED_EDGE('',*,*,#11600,.F.);
#15430=ORIENTED_EDGE('',*,*,#11602,.T.);
#15431=ORIENTED_EDGE('',*,*,#11603,.T.);
#15432=ORIENTED_EDGE('',*,*,#11604,.T.);
#15433=ORIENTED_EDGE('',*,*,#11605,.T.);
#15434=ORIENTED_EDGE('',*,*,#11597,.F.);
#15435=ORIENTED_EDGE('',*,*,#11606,.T.);
#15436=ORIENTED_EDGE('',*,*,#11607,.T.);
#15437=ORIENTED_EDGE('',*,*,#11608,.T.);
#15438=ORIENTED_EDGE('',*,*,#11604,.F.);
#15439=ORIENTED_EDGE('',*,*,#11609,.T.);
#15440=ORIENTED_EDGE('',*,*,#11610,.T.);
#15441=ORIENTED_EDGE('',*,*,#11611,.T.);
#15442=ORIENTED_EDGE('',*,*,#11607,.F.);
#15443=ORIENTED_EDGE('',*,*,#11612,.T.);
#15444=ORIENTED_EDGE('',*,*,#11613,.T.);
#15445=ORIENTED_EDGE('',*,*,#11614,.T.);
#15446=ORIENTED_EDGE('',*,*,#11610,.F.);
#15447=ORIENTED_EDGE('',*,*,#11615,.T.);
#15448=ORIENTED_EDGE('',*,*,#11616,.T.);
#15449=ORIENTED_EDGE('',*,*,#11617,.T.);
#15450=ORIENTED_EDGE('',*,*,#11613,.F.);
#15451=ORIENTED_EDGE('',*,*,#11618,.T.);
#15452=ORIENTED_EDGE('',*,*,#11619,.T.);
#15453=ORIENTED_EDGE('',*,*,#11620,.T.);
#15454=ORIENTED_EDGE('',*,*,#11616,.F.);
#15455=ORIENTED_EDGE('',*,*,#11621,.T.);
#15456=ORIENTED_EDGE('',*,*,#11622,.T.);
#15457=ORIENTED_EDGE('',*,*,#11623,.T.);
#15458=ORIENTED_EDGE('',*,*,#11619,.F.);
#15459=ORIENTED_EDGE('',*,*,#11624,.T.);
#15460=ORIENTED_EDGE('',*,*,#11625,.T.);
#15461=ORIENTED_EDGE('',*,*,#11626,.T.);
#15462=ORIENTED_EDGE('',*,*,#11622,.F.);
#15463=ORIENTED_EDGE('',*,*,#11627,.T.);
#15464=ORIENTED_EDGE('',*,*,#11628,.T.);
#15465=ORIENTED_EDGE('',*,*,#11629,.T.);
#15466=ORIENTED_EDGE('',*,*,#11625,.F.);
#15467=ORIENTED_EDGE('',*,*,#11630,.T.);
#15468=ORIENTED_EDGE('',*,*,#11631,.T.);
#15469=ORIENTED_EDGE('',*,*,#11632,.T.);
#15470=ORIENTED_EDGE('',*,*,#11628,.F.);
#15471=ORIENTED_EDGE('',*,*,#11633,.T.);
#15472=ORIENTED_EDGE('',*,*,#11634,.T.);
#15473=ORIENTED_EDGE('',*,*,#11635,.T.);
#15474=ORIENTED_EDGE('',*,*,#11631,.F.);
#15475=ORIENTED_EDGE('',*,*,#11636,.T.);
#15476=ORIENTED_EDGE('',*,*,#11637,.T.);
#15477=ORIENTED_EDGE('',*,*,#11638,.T.);
#15478=ORIENTED_EDGE('',*,*,#11634,.F.);
#15479=ORIENTED_EDGE('',*,*,#11639,.T.);
#15480=ORIENTED_EDGE('',*,*,#11640,.T.);
#15481=ORIENTED_EDGE('',*,*,#11641,.T.);
#15482=ORIENTED_EDGE('',*,*,#11637,.F.);
#15483=ORIENTED_EDGE('',*,*,#11642,.T.);
#15484=ORIENTED_EDGE('',*,*,#11643,.F.);
#15485=ORIENTED_EDGE('',*,*,#11644,.T.);
#15486=ORIENTED_EDGE('',*,*,#11645,.F.);
#15487=ORIENTED_EDGE('',*,*,#11646,.T.);
#15488=ORIENTED_EDGE('',*,*,#11647,.T.);
#15489=ORIENTED_EDGE('',*,*,#11648,.T.);
#15490=ORIENTED_EDGE('',*,*,#11649,.F.);
#15491=ORIENTED_EDGE('',*,*,#11650,.F.);
#15492=ORIENTED_EDGE('',*,*,#11651,.T.);
#15493=ORIENTED_EDGE('',*,*,#11652,.T.);
#15494=ORIENTED_EDGE('',*,*,#11647,.F.);
#15495=ORIENTED_EDGE('',*,*,#11653,.F.);
#15496=ORIENTED_EDGE('',*,*,#11654,.T.);
#15497=ORIENTED_EDGE('',*,*,#11655,.T.);
#15498=ORIENTED_EDGE('',*,*,#11651,.F.);
#15499=ORIENTED_EDGE('',*,*,#11656,.F.);
#15500=ORIENTED_EDGE('',*,*,#11657,.T.);
#15501=ORIENTED_EDGE('',*,*,#11658,.T.);
#15502=ORIENTED_EDGE('',*,*,#11654,.F.);
#15503=ORIENTED_EDGE('',*,*,#11659,.F.);
#15504=ORIENTED_EDGE('',*,*,#11660,.T.);
#15505=ORIENTED_EDGE('',*,*,#11661,.T.);
#15506=ORIENTED_EDGE('',*,*,#11657,.F.);
#15507=ORIENTED_EDGE('',*,*,#11662,.F.);
#15508=ORIENTED_EDGE('',*,*,#11663,.T.);
#15509=ORIENTED_EDGE('',*,*,#11664,.T.);
#15510=ORIENTED_EDGE('',*,*,#11660,.F.);
#15511=ORIENTED_EDGE('',*,*,#11665,.F.);
#15512=ORIENTED_EDGE('',*,*,#11666,.T.);
#15513=ORIENTED_EDGE('',*,*,#11667,.T.);
#15514=ORIENTED_EDGE('',*,*,#11663,.F.);
#15515=ORIENTED_EDGE('',*,*,#11668,.F.);
#15516=ORIENTED_EDGE('',*,*,#11669,.T.);
#15517=ORIENTED_EDGE('',*,*,#11670,.T.);
#15518=ORIENTED_EDGE('',*,*,#11666,.F.);
#15519=ORIENTED_EDGE('',*,*,#11671,.F.);
#15520=ORIENTED_EDGE('',*,*,#11672,.T.);
#15521=ORIENTED_EDGE('',*,*,#11673,.T.);
#15522=ORIENTED_EDGE('',*,*,#11669,.F.);
#15523=ORIENTED_EDGE('',*,*,#11674,.F.);
#15524=ORIENTED_EDGE('',*,*,#11675,.T.);
#15525=ORIENTED_EDGE('',*,*,#11676,.T.);
#15526=ORIENTED_EDGE('',*,*,#11672,.F.);
#15527=ORIENTED_EDGE('',*,*,#11677,.F.);
#15528=ORIENTED_EDGE('',*,*,#11678,.T.);
#15529=ORIENTED_EDGE('',*,*,#11679,.T.);
#15530=ORIENTED_EDGE('',*,*,#11675,.F.);
#15531=ORIENTED_EDGE('',*,*,#11680,.F.);
#15532=ORIENTED_EDGE('',*,*,#11681,.T.);
#15533=ORIENTED_EDGE('',*,*,#11682,.T.);
#15534=ORIENTED_EDGE('',*,*,#11678,.F.);
#15535=ORIENTED_EDGE('',*,*,#11683,.F.);
#15536=ORIENTED_EDGE('',*,*,#11684,.T.);
#15537=ORIENTED_EDGE('',*,*,#11685,.T.);
#15538=ORIENTED_EDGE('',*,*,#11681,.F.);
#15539=ORIENTED_EDGE('',*,*,#11686,.F.);
#15540=ORIENTED_EDGE('',*,*,#11687,.T.);
#15541=ORIENTED_EDGE('',*,*,#11688,.T.);
#15542=ORIENTED_EDGE('',*,*,#11684,.F.);
#15543=ORIENTED_EDGE('',*,*,#11689,.F.);
#15544=ORIENTED_EDGE('',*,*,#11690,.F.);
#15545=ORIENTED_EDGE('',*,*,#11691,.F.);
#15546=ORIENTED_EDGE('',*,*,#11692,.F.);
#15547=ORIENTED_EDGE('',*,*,#11693,.T.);
#15548=ORIENTED_EDGE('',*,*,#11694,.T.);
#15549=ORIENTED_EDGE('',*,*,#11695,.T.);
#15550=ORIENTED_EDGE('',*,*,#11696,.T.);
#15551=ORIENTED_EDGE('',*,*,#11697,.T.);
#15552=ORIENTED_EDGE('',*,*,#11698,.T.);
#15553=ORIENTED_EDGE('',*,*,#11697,.F.);
#15554=ORIENTED_EDGE('',*,*,#11699,.T.);
#15555=ORIENTED_EDGE('',*,*,#11700,.T.);
#15556=ORIENTED_EDGE('',*,*,#11701,.T.);
#15557=ORIENTED_EDGE('',*,*,#11702,.T.);
#15558=ORIENTED_EDGE('',*,*,#11694,.F.);
#15559=ORIENTED_EDGE('',*,*,#11703,.T.);
#15560=ORIENTED_EDGE('',*,*,#11704,.T.);
#15561=ORIENTED_EDGE('',*,*,#11705,.T.);
#15562=ORIENTED_EDGE('',*,*,#11701,.F.);
#15563=ORIENTED_EDGE('',*,*,#11706,.T.);
#15564=ORIENTED_EDGE('',*,*,#11707,.T.);
#15565=ORIENTED_EDGE('',*,*,#11708,.T.);
#15566=ORIENTED_EDGE('',*,*,#11704,.F.);
#15567=ORIENTED_EDGE('',*,*,#11709,.T.);
#15568=ORIENTED_EDGE('',*,*,#11710,.T.);
#15569=ORIENTED_EDGE('',*,*,#11711,.T.);
#15570=ORIENTED_EDGE('',*,*,#11707,.F.);
#15571=ORIENTED_EDGE('',*,*,#11712,.T.);
#15572=ORIENTED_EDGE('',*,*,#11713,.T.);
#15573=ORIENTED_EDGE('',*,*,#11714,.T.);
#15574=ORIENTED_EDGE('',*,*,#11710,.F.);
#15575=ORIENTED_EDGE('',*,*,#11715,.T.);
#15576=ORIENTED_EDGE('',*,*,#11716,.T.);
#15577=ORIENTED_EDGE('',*,*,#11717,.T.);
#15578=ORIENTED_EDGE('',*,*,#11713,.F.);
#15579=ORIENTED_EDGE('',*,*,#11718,.T.);
#15580=ORIENTED_EDGE('',*,*,#11719,.T.);
#15581=ORIENTED_EDGE('',*,*,#11720,.T.);
#15582=ORIENTED_EDGE('',*,*,#11716,.F.);
#15583=ORIENTED_EDGE('',*,*,#11721,.T.);
#15584=ORIENTED_EDGE('',*,*,#11722,.T.);
#15585=ORIENTED_EDGE('',*,*,#11723,.T.);
#15586=ORIENTED_EDGE('',*,*,#11719,.F.);
#15587=ORIENTED_EDGE('',*,*,#11724,.T.);
#15588=ORIENTED_EDGE('',*,*,#11725,.T.);
#15589=ORIENTED_EDGE('',*,*,#11726,.T.);
#15590=ORIENTED_EDGE('',*,*,#11722,.F.);
#15591=ORIENTED_EDGE('',*,*,#11727,.T.);
#15592=ORIENTED_EDGE('',*,*,#11728,.T.);
#15593=ORIENTED_EDGE('',*,*,#11729,.T.);
#15594=ORIENTED_EDGE('',*,*,#11725,.F.);
#15595=ORIENTED_EDGE('',*,*,#11730,.T.);
#15596=ORIENTED_EDGE('',*,*,#11731,.T.);
#15597=ORIENTED_EDGE('',*,*,#11732,.T.);
#15598=ORIENTED_EDGE('',*,*,#11728,.F.);
#15599=ORIENTED_EDGE('',*,*,#11733,.T.);
#15600=ORIENTED_EDGE('',*,*,#11734,.T.);
#15601=ORIENTED_EDGE('',*,*,#11735,.T.);
#15602=ORIENTED_EDGE('',*,*,#11731,.F.);
#15603=ORIENTED_EDGE('',*,*,#11736,.T.);
#15604=ORIENTED_EDGE('',*,*,#11737,.T.);
#15605=ORIENTED_EDGE('',*,*,#11738,.T.);
#15606=ORIENTED_EDGE('',*,*,#11734,.F.);
#15607=ORIENTED_EDGE('',*,*,#11739,.T.);
#15608=ORIENTED_EDGE('',*,*,#11740,.F.);
#15609=ORIENTED_EDGE('',*,*,#11741,.T.);
#15610=ORIENTED_EDGE('',*,*,#11742,.F.);
#15611=ORIENTED_EDGE('',*,*,#11743,.T.);
#15612=ORIENTED_EDGE('',*,*,#11744,.T.);
#15613=ORIENTED_EDGE('',*,*,#11745,.T.);
#15614=ORIENTED_EDGE('',*,*,#11746,.F.);
#15615=ORIENTED_EDGE('',*,*,#11747,.F.);
#15616=ORIENTED_EDGE('',*,*,#11748,.T.);
#15617=ORIENTED_EDGE('',*,*,#11749,.T.);
#15618=ORIENTED_EDGE('',*,*,#11744,.F.);
#15619=ORIENTED_EDGE('',*,*,#11750,.F.);
#15620=ORIENTED_EDGE('',*,*,#11751,.T.);
#15621=ORIENTED_EDGE('',*,*,#11752,.T.);
#15622=ORIENTED_EDGE('',*,*,#11748,.F.);
#15623=ORIENTED_EDGE('',*,*,#11753,.F.);
#15624=ORIENTED_EDGE('',*,*,#11754,.T.);
#15625=ORIENTED_EDGE('',*,*,#11755,.T.);
#15626=ORIENTED_EDGE('',*,*,#11751,.F.);
#15627=ORIENTED_EDGE('',*,*,#11756,.F.);
#15628=ORIENTED_EDGE('',*,*,#11757,.T.);
#15629=ORIENTED_EDGE('',*,*,#11758,.T.);
#15630=ORIENTED_EDGE('',*,*,#11754,.F.);
#15631=ORIENTED_EDGE('',*,*,#11759,.F.);
#15632=ORIENTED_EDGE('',*,*,#11760,.T.);
#15633=ORIENTED_EDGE('',*,*,#11761,.T.);
#15634=ORIENTED_EDGE('',*,*,#11757,.F.);
#15635=ORIENTED_EDGE('',*,*,#11762,.F.);
#15636=ORIENTED_EDGE('',*,*,#11763,.T.);
#15637=ORIENTED_EDGE('',*,*,#11764,.T.);
#15638=ORIENTED_EDGE('',*,*,#11760,.F.);
#15639=ORIENTED_EDGE('',*,*,#11765,.F.);
#15640=ORIENTED_EDGE('',*,*,#11766,.T.);
#15641=ORIENTED_EDGE('',*,*,#11767,.T.);
#15642=ORIENTED_EDGE('',*,*,#11763,.F.);
#15643=ORIENTED_EDGE('',*,*,#11768,.F.);
#15644=ORIENTED_EDGE('',*,*,#11769,.T.);
#15645=ORIENTED_EDGE('',*,*,#11770,.T.);
#15646=ORIENTED_EDGE('',*,*,#11766,.F.);
#15647=ORIENTED_EDGE('',*,*,#11771,.F.);
#15648=ORIENTED_EDGE('',*,*,#11772,.T.);
#15649=ORIENTED_EDGE('',*,*,#11773,.T.);
#15650=ORIENTED_EDGE('',*,*,#11769,.F.);
#15651=ORIENTED_EDGE('',*,*,#11774,.F.);
#15652=ORIENTED_EDGE('',*,*,#11775,.T.);
#15653=ORIENTED_EDGE('',*,*,#11776,.T.);
#15654=ORIENTED_EDGE('',*,*,#11772,.F.);
#15655=ORIENTED_EDGE('',*,*,#11777,.F.);
#15656=ORIENTED_EDGE('',*,*,#11778,.T.);
#15657=ORIENTED_EDGE('',*,*,#11779,.T.);
#15658=ORIENTED_EDGE('',*,*,#11775,.F.);
#15659=ORIENTED_EDGE('',*,*,#11780,.F.);
#15660=ORIENTED_EDGE('',*,*,#11781,.T.);
#15661=ORIENTED_EDGE('',*,*,#11782,.T.);
#15662=ORIENTED_EDGE('',*,*,#11778,.F.);
#15663=ORIENTED_EDGE('',*,*,#11783,.F.);
#15664=ORIENTED_EDGE('',*,*,#11784,.T.);
#15665=ORIENTED_EDGE('',*,*,#11785,.T.);
#15666=ORIENTED_EDGE('',*,*,#11781,.F.);
#15667=ORIENTED_EDGE('',*,*,#11786,.F.);
#15668=ORIENTED_EDGE('',*,*,#11787,.F.);
#15669=ORIENTED_EDGE('',*,*,#11788,.F.);
#15670=ORIENTED_EDGE('',*,*,#11789,.F.);
#15671=ORIENTED_EDGE('',*,*,#11790,.T.);
#15672=ORIENTED_EDGE('',*,*,#11791,.T.);
#15673=ORIENTED_EDGE('',*,*,#11792,.T.);
#15674=ORIENTED_EDGE('',*,*,#11793,.T.);
#15675=ORIENTED_EDGE('',*,*,#11794,.T.);
#15676=ORIENTED_EDGE('',*,*,#11795,.T.);
#15677=ORIENTED_EDGE('',*,*,#11794,.F.);
#15678=ORIENTED_EDGE('',*,*,#11796,.T.);
#15679=ORIENTED_EDGE('',*,*,#11797,.T.);
#15680=ORIENTED_EDGE('',*,*,#11798,.T.);
#15681=ORIENTED_EDGE('',*,*,#11799,.T.);
#15682=ORIENTED_EDGE('',*,*,#11791,.F.);
#15683=ORIENTED_EDGE('',*,*,#11800,.T.);
#15684=ORIENTED_EDGE('',*,*,#11801,.T.);
#15685=ORIENTED_EDGE('',*,*,#11802,.T.);
#15686=ORIENTED_EDGE('',*,*,#11798,.F.);
#15687=ORIENTED_EDGE('',*,*,#11803,.T.);
#15688=ORIENTED_EDGE('',*,*,#11804,.T.);
#15689=ORIENTED_EDGE('',*,*,#11805,.T.);
#15690=ORIENTED_EDGE('',*,*,#11801,.F.);
#15691=ORIENTED_EDGE('',*,*,#11806,.T.);
#15692=ORIENTED_EDGE('',*,*,#11807,.T.);
#15693=ORIENTED_EDGE('',*,*,#11808,.T.);
#15694=ORIENTED_EDGE('',*,*,#11804,.F.);
#15695=ORIENTED_EDGE('',*,*,#11809,.T.);
#15696=ORIENTED_EDGE('',*,*,#11810,.T.);
#15697=ORIENTED_EDGE('',*,*,#11811,.T.);
#15698=ORIENTED_EDGE('',*,*,#11807,.F.);
#15699=ORIENTED_EDGE('',*,*,#11812,.T.);
#15700=ORIENTED_EDGE('',*,*,#11813,.T.);
#15701=ORIENTED_EDGE('',*,*,#11814,.T.);
#15702=ORIENTED_EDGE('',*,*,#11810,.F.);
#15703=ORIENTED_EDGE('',*,*,#11815,.T.);
#15704=ORIENTED_EDGE('',*,*,#11816,.T.);
#15705=ORIENTED_EDGE('',*,*,#11817,.T.);
#15706=ORIENTED_EDGE('',*,*,#11813,.F.);
#15707=ORIENTED_EDGE('',*,*,#11818,.T.);
#15708=ORIENTED_EDGE('',*,*,#11819,.T.);
#15709=ORIENTED_EDGE('',*,*,#11820,.T.);
#15710=ORIENTED_EDGE('',*,*,#11816,.F.);
#15711=ORIENTED_EDGE('',*,*,#11821,.T.);
#15712=ORIENTED_EDGE('',*,*,#11822,.T.);
#15713=ORIENTED_EDGE('',*,*,#11823,.T.);
#15714=ORIENTED_EDGE('',*,*,#11819,.F.);
#15715=ORIENTED_EDGE('',*,*,#11824,.T.);
#15716=ORIENTED_EDGE('',*,*,#11825,.T.);
#15717=ORIENTED_EDGE('',*,*,#11826,.T.);
#15718=ORIENTED_EDGE('',*,*,#11822,.F.);
#15719=ORIENTED_EDGE('',*,*,#11827,.T.);
#15720=ORIENTED_EDGE('',*,*,#11828,.T.);
#15721=ORIENTED_EDGE('',*,*,#11829,.T.);
#15722=ORIENTED_EDGE('',*,*,#11825,.F.);
#15723=ORIENTED_EDGE('',*,*,#11830,.T.);
#15724=ORIENTED_EDGE('',*,*,#11831,.T.);
#15725=ORIENTED_EDGE('',*,*,#11832,.T.);
#15726=ORIENTED_EDGE('',*,*,#11828,.F.);
#15727=ORIENTED_EDGE('',*,*,#11833,.T.);
#15728=ORIENTED_EDGE('',*,*,#11834,.T.);
#15729=ORIENTED_EDGE('',*,*,#11835,.T.);
#15730=ORIENTED_EDGE('',*,*,#11831,.F.);
#15731=ORIENTED_EDGE('',*,*,#11836,.T.);
#15732=ORIENTED_EDGE('',*,*,#11837,.F.);
#15733=ORIENTED_EDGE('',*,*,#11838,.T.);
#15734=ORIENTED_EDGE('',*,*,#11839,.F.);
#15735=ORIENTED_EDGE('',*,*,#11840,.T.);
#15736=ORIENTED_EDGE('',*,*,#11841,.T.);
#15737=ORIENTED_EDGE('',*,*,#11842,.T.);
#15738=ORIENTED_EDGE('',*,*,#11843,.F.);
#15739=ORIENTED_EDGE('',*,*,#11844,.F.);
#15740=ORIENTED_EDGE('',*,*,#11845,.T.);
#15741=ORIENTED_EDGE('',*,*,#11846,.T.);
#15742=ORIENTED_EDGE('',*,*,#11841,.F.);
#15743=ORIENTED_EDGE('',*,*,#11847,.F.);
#15744=ORIENTED_EDGE('',*,*,#11848,.T.);
#15745=ORIENTED_EDGE('',*,*,#11849,.T.);
#15746=ORIENTED_EDGE('',*,*,#11845,.F.);
#15747=ORIENTED_EDGE('',*,*,#11850,.F.);
#15748=ORIENTED_EDGE('',*,*,#11851,.T.);
#15749=ORIENTED_EDGE('',*,*,#11852,.T.);
#15750=ORIENTED_EDGE('',*,*,#11848,.F.);
#15751=ORIENTED_EDGE('',*,*,#11853,.F.);
#15752=ORIENTED_EDGE('',*,*,#11854,.T.);
#15753=ORIENTED_EDGE('',*,*,#11855,.T.);
#15754=ORIENTED_EDGE('',*,*,#11851,.F.);
#15755=ORIENTED_EDGE('',*,*,#11856,.F.);
#15756=ORIENTED_EDGE('',*,*,#11857,.T.);
#15757=ORIENTED_EDGE('',*,*,#11858,.T.);
#15758=ORIENTED_EDGE('',*,*,#11854,.F.);
#15759=ORIENTED_EDGE('',*,*,#11859,.F.);
#15760=ORIENTED_EDGE('',*,*,#11860,.T.);
#15761=ORIENTED_EDGE('',*,*,#11861,.T.);
#15762=ORIENTED_EDGE('',*,*,#11857,.F.);
#15763=ORIENTED_EDGE('',*,*,#11862,.F.);
#15764=ORIENTED_EDGE('',*,*,#11863,.T.);
#15765=ORIENTED_EDGE('',*,*,#11864,.T.);
#15766=ORIENTED_EDGE('',*,*,#11860,.F.);
#15767=ORIENTED_EDGE('',*,*,#11865,.F.);
#15768=ORIENTED_EDGE('',*,*,#11866,.T.);
#15769=ORIENTED_EDGE('',*,*,#11867,.T.);
#15770=ORIENTED_EDGE('',*,*,#11863,.F.);
#15771=ORIENTED_EDGE('',*,*,#11868,.F.);
#15772=ORIENTED_EDGE('',*,*,#11869,.T.);
#15773=ORIENTED_EDGE('',*,*,#11870,.T.);
#15774=ORIENTED_EDGE('',*,*,#11866,.F.);
#15775=ORIENTED_EDGE('',*,*,#11871,.F.);
#15776=ORIENTED_EDGE('',*,*,#11872,.T.);
#15777=ORIENTED_EDGE('',*,*,#11873,.T.);
#15778=ORIENTED_EDGE('',*,*,#11869,.F.);
#15779=ORIENTED_EDGE('',*,*,#11874,.F.);
#15780=ORIENTED_EDGE('',*,*,#11875,.T.);
#15781=ORIENTED_EDGE('',*,*,#11876,.T.);
#15782=ORIENTED_EDGE('',*,*,#11872,.F.);
#15783=ORIENTED_EDGE('',*,*,#11877,.F.);
#15784=ORIENTED_EDGE('',*,*,#11878,.T.);
#15785=ORIENTED_EDGE('',*,*,#11879,.T.);
#15786=ORIENTED_EDGE('',*,*,#11875,.F.);
#15787=ORIENTED_EDGE('',*,*,#11880,.F.);
#15788=ORIENTED_EDGE('',*,*,#11881,.T.);
#15789=ORIENTED_EDGE('',*,*,#11882,.T.);
#15790=ORIENTED_EDGE('',*,*,#11878,.F.);
#15791=ORIENTED_EDGE('',*,*,#11883,.F.);
#15792=ORIENTED_EDGE('',*,*,#11884,.F.);
#15793=ORIENTED_EDGE('',*,*,#11885,.F.);
#15794=ORIENTED_EDGE('',*,*,#11886,.F.);
#15795=ORIENTED_EDGE('',*,*,#11887,.T.);
#15796=ORIENTED_EDGE('',*,*,#11888,.T.);
#15797=ORIENTED_EDGE('',*,*,#11889,.T.);
#15798=ORIENTED_EDGE('',*,*,#11890,.T.);
#15799=ORIENTED_EDGE('',*,*,#11891,.T.);
#15800=ORIENTED_EDGE('',*,*,#11892,.T.);
#15801=ORIENTED_EDGE('',*,*,#11891,.F.);
#15802=ORIENTED_EDGE('',*,*,#11893,.T.);
#15803=ORIENTED_EDGE('',*,*,#11894,.T.);
#15804=ORIENTED_EDGE('',*,*,#11895,.T.);
#15805=ORIENTED_EDGE('',*,*,#11896,.T.);
#15806=ORIENTED_EDGE('',*,*,#11888,.F.);
#15807=ORIENTED_EDGE('',*,*,#11897,.T.);
#15808=ORIENTED_EDGE('',*,*,#11898,.T.);
#15809=ORIENTED_EDGE('',*,*,#11899,.T.);
#15810=ORIENTED_EDGE('',*,*,#11895,.F.);
#15811=ORIENTED_EDGE('',*,*,#11900,.T.);
#15812=ORIENTED_EDGE('',*,*,#11901,.T.);
#15813=ORIENTED_EDGE('',*,*,#11902,.T.);
#15814=ORIENTED_EDGE('',*,*,#11898,.F.);
#15815=ORIENTED_EDGE('',*,*,#11903,.T.);
#15816=ORIENTED_EDGE('',*,*,#11904,.T.);
#15817=ORIENTED_EDGE('',*,*,#11905,.T.);
#15818=ORIENTED_EDGE('',*,*,#11901,.F.);
#15819=ORIENTED_EDGE('',*,*,#11906,.T.);
#15820=ORIENTED_EDGE('',*,*,#11907,.T.);
#15821=ORIENTED_EDGE('',*,*,#11908,.T.);
#15822=ORIENTED_EDGE('',*,*,#11904,.F.);
#15823=ORIENTED_EDGE('',*,*,#11909,.T.);
#15824=ORIENTED_EDGE('',*,*,#11910,.T.);
#15825=ORIENTED_EDGE('',*,*,#11911,.T.);
#15826=ORIENTED_EDGE('',*,*,#11907,.F.);
#15827=ORIENTED_EDGE('',*,*,#11912,.T.);
#15828=ORIENTED_EDGE('',*,*,#11913,.T.);
#15829=ORIENTED_EDGE('',*,*,#11914,.T.);
#15830=ORIENTED_EDGE('',*,*,#11910,.F.);
#15831=ORIENTED_EDGE('',*,*,#11915,.T.);
#15832=ORIENTED_EDGE('',*,*,#11916,.T.);
#15833=ORIENTED_EDGE('',*,*,#11917,.T.);
#15834=ORIENTED_EDGE('',*,*,#11913,.F.);
#15835=ORIENTED_EDGE('',*,*,#11918,.T.);
#15836=ORIENTED_EDGE('',*,*,#11919,.T.);
#15837=ORIENTED_EDGE('',*,*,#11920,.T.);
#15838=ORIENTED_EDGE('',*,*,#11916,.F.);
#15839=ORIENTED_EDGE('',*,*,#11921,.T.);
#15840=ORIENTED_EDGE('',*,*,#11922,.T.);
#15841=ORIENTED_EDGE('',*,*,#11923,.T.);
#15842=ORIENTED_EDGE('',*,*,#11919,.F.);
#15843=ORIENTED_EDGE('',*,*,#11924,.T.);
#15844=ORIENTED_EDGE('',*,*,#11925,.T.);
#15845=ORIENTED_EDGE('',*,*,#11926,.T.);
#15846=ORIENTED_EDGE('',*,*,#11922,.F.);
#15847=ORIENTED_EDGE('',*,*,#11927,.T.);
#15848=ORIENTED_EDGE('',*,*,#11928,.T.);
#15849=ORIENTED_EDGE('',*,*,#11929,.T.);
#15850=ORIENTED_EDGE('',*,*,#11925,.F.);
#15851=ORIENTED_EDGE('',*,*,#11930,.T.);
#15852=ORIENTED_EDGE('',*,*,#11931,.T.);
#15853=ORIENTED_EDGE('',*,*,#11932,.T.);
#15854=ORIENTED_EDGE('',*,*,#11928,.F.);
#15855=ORIENTED_EDGE('',*,*,#11933,.T.);
#15856=ORIENTED_EDGE('',*,*,#11934,.F.);
#15857=ORIENTED_EDGE('',*,*,#11935,.T.);
#15858=ORIENTED_EDGE('',*,*,#11936,.F.);
#15859=ORIENTED_EDGE('',*,*,#11937,.T.);
#15860=ORIENTED_EDGE('',*,*,#11938,.T.);
#15861=ORIENTED_EDGE('',*,*,#11939,.T.);
#15862=ORIENTED_EDGE('',*,*,#11940,.F.);
#15863=ORIENTED_EDGE('',*,*,#11941,.F.);
#15864=ORIENTED_EDGE('',*,*,#11942,.T.);
#15865=ORIENTED_EDGE('',*,*,#11943,.T.);
#15866=ORIENTED_EDGE('',*,*,#11938,.F.);
#15867=ORIENTED_EDGE('',*,*,#11944,.F.);
#15868=ORIENTED_EDGE('',*,*,#11945,.T.);
#15869=ORIENTED_EDGE('',*,*,#11946,.T.);
#15870=ORIENTED_EDGE('',*,*,#11942,.F.);
#15871=ORIENTED_EDGE('',*,*,#11947,.F.);
#15872=ORIENTED_EDGE('',*,*,#11948,.T.);
#15873=ORIENTED_EDGE('',*,*,#11949,.T.);
#15874=ORIENTED_EDGE('',*,*,#11945,.F.);
#15875=ORIENTED_EDGE('',*,*,#11950,.F.);
#15876=ORIENTED_EDGE('',*,*,#11951,.T.);
#15877=ORIENTED_EDGE('',*,*,#11952,.T.);
#15878=ORIENTED_EDGE('',*,*,#11948,.F.);
#15879=ORIENTED_EDGE('',*,*,#11953,.F.);
#15880=ORIENTED_EDGE('',*,*,#11954,.T.);
#15881=ORIENTED_EDGE('',*,*,#11955,.T.);
#15882=ORIENTED_EDGE('',*,*,#11951,.F.);
#15883=ORIENTED_EDGE('',*,*,#11956,.F.);
#15884=ORIENTED_EDGE('',*,*,#11957,.T.);
#15885=ORIENTED_EDGE('',*,*,#11958,.T.);
#15886=ORIENTED_EDGE('',*,*,#11954,.F.);
#15887=ORIENTED_EDGE('',*,*,#11959,.F.);
#15888=ORIENTED_EDGE('',*,*,#11960,.T.);
#15889=ORIENTED_EDGE('',*,*,#11961,.T.);
#15890=ORIENTED_EDGE('',*,*,#11957,.F.);
#15891=ORIENTED_EDGE('',*,*,#11962,.F.);
#15892=ORIENTED_EDGE('',*,*,#11963,.T.);
#15893=ORIENTED_EDGE('',*,*,#11964,.T.);
#15894=ORIENTED_EDGE('',*,*,#11960,.F.);
#15895=ORIENTED_EDGE('',*,*,#11965,.F.);
#15896=ORIENTED_EDGE('',*,*,#11966,.T.);
#15897=ORIENTED_EDGE('',*,*,#11967,.T.);
#15898=ORIENTED_EDGE('',*,*,#11963,.F.);
#15899=ORIENTED_EDGE('',*,*,#11968,.F.);
#15900=ORIENTED_EDGE('',*,*,#11969,.T.);
#15901=ORIENTED_EDGE('',*,*,#11970,.T.);
#15902=ORIENTED_EDGE('',*,*,#11966,.F.);
#15903=ORIENTED_EDGE('',*,*,#11971,.F.);
#15904=ORIENTED_EDGE('',*,*,#11972,.T.);
#15905=ORIENTED_EDGE('',*,*,#11973,.T.);
#15906=ORIENTED_EDGE('',*,*,#11969,.F.);
#15907=ORIENTED_EDGE('',*,*,#11974,.F.);
#15908=ORIENTED_EDGE('',*,*,#11975,.T.);
#15909=ORIENTED_EDGE('',*,*,#11976,.T.);
#15910=ORIENTED_EDGE('',*,*,#11972,.F.);
#15911=ORIENTED_EDGE('',*,*,#11977,.F.);
#15912=ORIENTED_EDGE('',*,*,#11978,.T.);
#15913=ORIENTED_EDGE('',*,*,#11979,.T.);
#15914=ORIENTED_EDGE('',*,*,#11975,.F.);
#15915=ORIENTED_EDGE('',*,*,#11980,.F.);
#15916=ORIENTED_EDGE('',*,*,#11981,.F.);
#15917=ORIENTED_EDGE('',*,*,#11982,.F.);
#15918=ORIENTED_EDGE('',*,*,#11983,.F.);
#15919=ORIENTED_EDGE('',*,*,#11984,.T.);
#15920=ORIENTED_EDGE('',*,*,#11985,.T.);
#15921=ORIENTED_EDGE('',*,*,#11986,.T.);
#15922=ORIENTED_EDGE('',*,*,#11987,.T.);
#15923=ORIENTED_EDGE('',*,*,#11988,.T.);
#15924=ORIENTED_EDGE('',*,*,#11989,.T.);
#15925=ORIENTED_EDGE('',*,*,#11988,.F.);
#15926=ORIENTED_EDGE('',*,*,#11990,.T.);
#15927=ORIENTED_EDGE('',*,*,#11991,.T.);
#15928=ORIENTED_EDGE('',*,*,#11992,.T.);
#15929=ORIENTED_EDGE('',*,*,#11993,.T.);
#15930=ORIENTED_EDGE('',*,*,#11985,.F.);
#15931=ORIENTED_EDGE('',*,*,#11994,.T.);
#15932=ORIENTED_EDGE('',*,*,#11995,.T.);
#15933=ORIENTED_EDGE('',*,*,#11996,.T.);
#15934=ORIENTED_EDGE('',*,*,#11992,.F.);
#15935=ORIENTED_EDGE('',*,*,#11997,.T.);
#15936=ORIENTED_EDGE('',*,*,#11998,.T.);
#15937=ORIENTED_EDGE('',*,*,#11999,.T.);
#15938=ORIENTED_EDGE('',*,*,#11995,.F.);
#15939=ORIENTED_EDGE('',*,*,#12000,.T.);
#15940=ORIENTED_EDGE('',*,*,#12001,.T.);
#15941=ORIENTED_EDGE('',*,*,#12002,.T.);
#15942=ORIENTED_EDGE('',*,*,#11998,.F.);
#15943=ORIENTED_EDGE('',*,*,#12003,.T.);
#15944=ORIENTED_EDGE('',*,*,#12004,.T.);
#15945=ORIENTED_EDGE('',*,*,#12005,.T.);
#15946=ORIENTED_EDGE('',*,*,#12001,.F.);
#15947=ORIENTED_EDGE('',*,*,#12006,.T.);
#15948=ORIENTED_EDGE('',*,*,#12007,.T.);
#15949=ORIENTED_EDGE('',*,*,#12008,.T.);
#15950=ORIENTED_EDGE('',*,*,#12004,.F.);
#15951=ORIENTED_EDGE('',*,*,#12009,.T.);
#15952=ORIENTED_EDGE('',*,*,#12010,.T.);
#15953=ORIENTED_EDGE('',*,*,#12011,.T.);
#15954=ORIENTED_EDGE('',*,*,#12007,.F.);
#15955=ORIENTED_EDGE('',*,*,#12012,.T.);
#15956=ORIENTED_EDGE('',*,*,#12013,.T.);
#15957=ORIENTED_EDGE('',*,*,#12014,.T.);
#15958=ORIENTED_EDGE('',*,*,#12010,.F.);
#15959=ORIENTED_EDGE('',*,*,#12015,.T.);
#15960=ORIENTED_EDGE('',*,*,#12016,.T.);
#15961=ORIENTED_EDGE('',*,*,#12017,.T.);
#15962=ORIENTED_EDGE('',*,*,#12013,.F.);
#15963=ORIENTED_EDGE('',*,*,#12018,.T.);
#15964=ORIENTED_EDGE('',*,*,#12019,.T.);
#15965=ORIENTED_EDGE('',*,*,#12020,.T.);
#15966=ORIENTED_EDGE('',*,*,#12016,.F.);
#15967=ORIENTED_EDGE('',*,*,#12021,.T.);
#15968=ORIENTED_EDGE('',*,*,#12022,.T.);
#15969=ORIENTED_EDGE('',*,*,#12023,.T.);
#15970=ORIENTED_EDGE('',*,*,#12019,.F.);
#15971=ORIENTED_EDGE('',*,*,#12024,.T.);
#15972=ORIENTED_EDGE('',*,*,#12025,.T.);
#15973=ORIENTED_EDGE('',*,*,#12026,.T.);
#15974=ORIENTED_EDGE('',*,*,#12022,.F.);
#15975=ORIENTED_EDGE('',*,*,#12027,.T.);
#15976=ORIENTED_EDGE('',*,*,#12028,.T.);
#15977=ORIENTED_EDGE('',*,*,#12029,.T.);
#15978=ORIENTED_EDGE('',*,*,#12025,.F.);
#15979=ORIENTED_EDGE('',*,*,#12030,.T.);
#15980=ORIENTED_EDGE('',*,*,#12031,.F.);
#15981=ORIENTED_EDGE('',*,*,#12032,.T.);
#15982=ORIENTED_EDGE('',*,*,#12033,.F.);
#15983=ORIENTED_EDGE('',*,*,#12034,.T.);
#15984=ORIENTED_EDGE('',*,*,#12035,.T.);
#15985=ORIENTED_EDGE('',*,*,#12036,.T.);
#15986=ORIENTED_EDGE('',*,*,#12037,.F.);
#15987=ORIENTED_EDGE('',*,*,#12038,.F.);
#15988=ORIENTED_EDGE('',*,*,#12039,.T.);
#15989=ORIENTED_EDGE('',*,*,#12040,.T.);
#15990=ORIENTED_EDGE('',*,*,#12035,.F.);
#15991=ORIENTED_EDGE('',*,*,#12041,.F.);
#15992=ORIENTED_EDGE('',*,*,#12042,.T.);
#15993=ORIENTED_EDGE('',*,*,#12043,.T.);
#15994=ORIENTED_EDGE('',*,*,#12039,.F.);
#15995=ORIENTED_EDGE('',*,*,#12044,.F.);
#15996=ORIENTED_EDGE('',*,*,#12045,.T.);
#15997=ORIENTED_EDGE('',*,*,#12046,.T.);
#15998=ORIENTED_EDGE('',*,*,#12042,.F.);
#15999=ORIENTED_EDGE('',*,*,#12047,.F.);
#16000=ORIENTED_EDGE('',*,*,#12048,.T.);
#16001=ORIENTED_EDGE('',*,*,#12049,.T.);
#16002=ORIENTED_EDGE('',*,*,#12045,.F.);
#16003=ORIENTED_EDGE('',*,*,#12050,.F.);
#16004=ORIENTED_EDGE('',*,*,#12051,.T.);
#16005=ORIENTED_EDGE('',*,*,#12052,.T.);
#16006=ORIENTED_EDGE('',*,*,#12048,.F.);
#16007=ORIENTED_EDGE('',*,*,#12053,.F.);
#16008=ORIENTED_EDGE('',*,*,#12054,.T.);
#16009=ORIENTED_EDGE('',*,*,#12055,.T.);
#16010=ORIENTED_EDGE('',*,*,#12051,.F.);
#16011=ORIENTED_EDGE('',*,*,#12056,.F.);
#16012=ORIENTED_EDGE('',*,*,#12057,.T.);
#16013=ORIENTED_EDGE('',*,*,#12058,.T.);
#16014=ORIENTED_EDGE('',*,*,#12054,.F.);
#16015=ORIENTED_EDGE('',*,*,#12059,.F.);
#16016=ORIENTED_EDGE('',*,*,#12060,.T.);
#16017=ORIENTED_EDGE('',*,*,#12061,.T.);
#16018=ORIENTED_EDGE('',*,*,#12057,.F.);
#16019=ORIENTED_EDGE('',*,*,#12062,.F.);
#16020=ORIENTED_EDGE('',*,*,#12063,.T.);
#16021=ORIENTED_EDGE('',*,*,#12064,.T.);
#16022=ORIENTED_EDGE('',*,*,#12060,.F.);
#16023=ORIENTED_EDGE('',*,*,#12065,.F.);
#16024=ORIENTED_EDGE('',*,*,#12066,.T.);
#16025=ORIENTED_EDGE('',*,*,#12067,.T.);
#16026=ORIENTED_EDGE('',*,*,#12063,.F.);
#16027=ORIENTED_EDGE('',*,*,#12068,.F.);
#16028=ORIENTED_EDGE('',*,*,#12069,.T.);
#16029=ORIENTED_EDGE('',*,*,#12070,.T.);
#16030=ORIENTED_EDGE('',*,*,#12066,.F.);
#16031=ORIENTED_EDGE('',*,*,#12071,.F.);
#16032=ORIENTED_EDGE('',*,*,#12072,.T.);
#16033=ORIENTED_EDGE('',*,*,#12073,.T.);
#16034=ORIENTED_EDGE('',*,*,#12069,.F.);
#16035=ORIENTED_EDGE('',*,*,#12074,.F.);
#16036=ORIENTED_EDGE('',*,*,#12075,.T.);
#16037=ORIENTED_EDGE('',*,*,#12076,.T.);
#16038=ORIENTED_EDGE('',*,*,#12072,.F.);
#16039=ORIENTED_EDGE('',*,*,#12077,.F.);
#16040=ORIENTED_EDGE('',*,*,#12078,.F.);
#16041=ORIENTED_EDGE('',*,*,#12079,.F.);
#16042=ORIENTED_EDGE('',*,*,#12080,.F.);
#16043=ORIENTED_EDGE('',*,*,#12081,.T.);
#16044=ORIENTED_EDGE('',*,*,#12082,.T.);
#16045=ORIENTED_EDGE('',*,*,#12083,.T.);
#16046=ORIENTED_EDGE('',*,*,#12084,.T.);
#16047=ORIENTED_EDGE('',*,*,#12085,.T.);
#16048=ORIENTED_EDGE('',*,*,#12086,.T.);
#16049=ORIENTED_EDGE('',*,*,#12085,.F.);
#16050=ORIENTED_EDGE('',*,*,#12087,.T.);
#16051=ORIENTED_EDGE('',*,*,#12088,.T.);
#16052=ORIENTED_EDGE('',*,*,#12089,.T.);
#16053=ORIENTED_EDGE('',*,*,#12090,.T.);
#16054=ORIENTED_EDGE('',*,*,#12082,.F.);
#16055=ORIENTED_EDGE('',*,*,#12091,.T.);
#16056=ORIENTED_EDGE('',*,*,#12092,.T.);
#16057=ORIENTED_EDGE('',*,*,#12093,.T.);
#16058=ORIENTED_EDGE('',*,*,#12089,.F.);
#16059=ORIENTED_EDGE('',*,*,#12094,.T.);
#16060=ORIENTED_EDGE('',*,*,#12095,.T.);
#16061=ORIENTED_EDGE('',*,*,#12096,.T.);
#16062=ORIENTED_EDGE('',*,*,#12092,.F.);
#16063=ORIENTED_EDGE('',*,*,#12097,.T.);
#16064=ORIENTED_EDGE('',*,*,#12098,.T.);
#16065=ORIENTED_EDGE('',*,*,#12099,.T.);
#16066=ORIENTED_EDGE('',*,*,#12095,.F.);
#16067=ORIENTED_EDGE('',*,*,#12100,.T.);
#16068=ORIENTED_EDGE('',*,*,#12101,.T.);
#16069=ORIENTED_EDGE('',*,*,#12102,.T.);
#16070=ORIENTED_EDGE('',*,*,#12098,.F.);
#16071=ORIENTED_EDGE('',*,*,#12103,.T.);
#16072=ORIENTED_EDGE('',*,*,#12104,.T.);
#16073=ORIENTED_EDGE('',*,*,#12105,.T.);
#16074=ORIENTED_EDGE('',*,*,#12101,.F.);
#16075=ORIENTED_EDGE('',*,*,#12106,.T.);
#16076=ORIENTED_EDGE('',*,*,#12107,.T.);
#16077=ORIENTED_EDGE('',*,*,#12108,.T.);
#16078=ORIENTED_EDGE('',*,*,#12104,.F.);
#16079=ORIENTED_EDGE('',*,*,#12109,.T.);
#16080=ORIENTED_EDGE('',*,*,#12110,.T.);
#16081=ORIENTED_EDGE('',*,*,#12111,.T.);
#16082=ORIENTED_EDGE('',*,*,#12107,.F.);
#16083=ORIENTED_EDGE('',*,*,#12112,.T.);
#16084=ORIENTED_EDGE('',*,*,#12113,.T.);
#16085=ORIENTED_EDGE('',*,*,#12114,.T.);
#16086=ORIENTED_EDGE('',*,*,#12110,.F.);
#16087=ORIENTED_EDGE('',*,*,#12115,.T.);
#16088=ORIENTED_EDGE('',*,*,#12116,.T.);
#16089=ORIENTED_EDGE('',*,*,#12117,.T.);
#16090=ORIENTED_EDGE('',*,*,#12113,.F.);
#16091=ORIENTED_EDGE('',*,*,#12118,.T.);
#16092=ORIENTED_EDGE('',*,*,#12119,.T.);
#16093=ORIENTED_EDGE('',*,*,#12120,.T.);
#16094=ORIENTED_EDGE('',*,*,#12116,.F.);
#16095=ORIENTED_EDGE('',*,*,#12121,.T.);
#16096=ORIENTED_EDGE('',*,*,#12122,.T.);
#16097=ORIENTED_EDGE('',*,*,#12123,.T.);
#16098=ORIENTED_EDGE('',*,*,#12119,.F.);
#16099=ORIENTED_EDGE('',*,*,#12124,.T.);
#16100=ORIENTED_EDGE('',*,*,#12125,.T.);
#16101=ORIENTED_EDGE('',*,*,#12126,.T.);
#16102=ORIENTED_EDGE('',*,*,#12122,.F.);
#16103=ORIENTED_EDGE('',*,*,#12127,.T.);
#16104=ORIENTED_EDGE('',*,*,#12128,.F.);
#16105=ORIENTED_EDGE('',*,*,#12129,.T.);
#16106=ORIENTED_EDGE('',*,*,#12130,.F.);
#16107=ORIENTED_EDGE('',*,*,#12131,.T.);
#16108=ORIENTED_EDGE('',*,*,#12132,.T.);
#16109=ORIENTED_EDGE('',*,*,#12133,.T.);
#16110=ORIENTED_EDGE('',*,*,#12134,.F.);
#16111=ORIENTED_EDGE('',*,*,#12135,.F.);
#16112=ORIENTED_EDGE('',*,*,#12136,.T.);
#16113=ORIENTED_EDGE('',*,*,#12137,.T.);
#16114=ORIENTED_EDGE('',*,*,#12132,.F.);
#16115=ORIENTED_EDGE('',*,*,#12138,.F.);
#16116=ORIENTED_EDGE('',*,*,#12139,.T.);
#16117=ORIENTED_EDGE('',*,*,#12140,.T.);
#16118=ORIENTED_EDGE('',*,*,#12136,.F.);
#16119=ORIENTED_EDGE('',*,*,#12141,.F.);
#16120=ORIENTED_EDGE('',*,*,#12142,.T.);
#16121=ORIENTED_EDGE('',*,*,#12143,.T.);
#16122=ORIENTED_EDGE('',*,*,#12139,.F.);
#16123=ORIENTED_EDGE('',*,*,#12144,.F.);
#16124=ORIENTED_EDGE('',*,*,#12145,.T.);
#16125=ORIENTED_EDGE('',*,*,#12146,.T.);
#16126=ORIENTED_EDGE('',*,*,#12142,.F.);
#16127=ORIENTED_EDGE('',*,*,#12147,.F.);
#16128=ORIENTED_EDGE('',*,*,#12148,.T.);
#16129=ORIENTED_EDGE('',*,*,#12149,.T.);
#16130=ORIENTED_EDGE('',*,*,#12145,.F.);
#16131=ORIENTED_EDGE('',*,*,#12150,.F.);
#16132=ORIENTED_EDGE('',*,*,#12151,.T.);
#16133=ORIENTED_EDGE('',*,*,#12152,.T.);
#16134=ORIENTED_EDGE('',*,*,#12148,.F.);
#16135=ORIENTED_EDGE('',*,*,#12153,.F.);
#16136=ORIENTED_EDGE('',*,*,#12154,.T.);
#16137=ORIENTED_EDGE('',*,*,#12155,.T.);
#16138=ORIENTED_EDGE('',*,*,#12151,.F.);
#16139=ORIENTED_EDGE('',*,*,#12156,.F.);
#16140=ORIENTED_EDGE('',*,*,#12157,.T.);
#16141=ORIENTED_EDGE('',*,*,#12158,.T.);
#16142=ORIENTED_EDGE('',*,*,#12154,.F.);
#16143=ORIENTED_EDGE('',*,*,#12159,.F.);
#16144=ORIENTED_EDGE('',*,*,#12160,.T.);
#16145=ORIENTED_EDGE('',*,*,#12161,.T.);
#16146=ORIENTED_EDGE('',*,*,#12157,.F.);
#16147=ORIENTED_EDGE('',*,*,#12162,.F.);
#16148=ORIENTED_EDGE('',*,*,#12163,.T.);
#16149=ORIENTED_EDGE('',*,*,#12164,.T.);
#16150=ORIENTED_EDGE('',*,*,#12160,.F.);
#16151=ORIENTED_EDGE('',*,*,#12165,.F.);
#16152=ORIENTED_EDGE('',*,*,#12166,.T.);
#16153=ORIENTED_EDGE('',*,*,#12167,.T.);
#16154=ORIENTED_EDGE('',*,*,#12163,.F.);
#16155=ORIENTED_EDGE('',*,*,#12168,.F.);
#16156=ORIENTED_EDGE('',*,*,#12169,.T.);
#16157=ORIENTED_EDGE('',*,*,#12170,.T.);
#16158=ORIENTED_EDGE('',*,*,#12166,.F.);
#16159=ORIENTED_EDGE('',*,*,#12171,.F.);
#16160=ORIENTED_EDGE('',*,*,#12172,.T.);
#16161=ORIENTED_EDGE('',*,*,#12173,.T.);
#16162=ORIENTED_EDGE('',*,*,#12169,.F.);
#16163=ORIENTED_EDGE('',*,*,#12174,.F.);
#16164=ORIENTED_EDGE('',*,*,#12175,.F.);
#16165=ORIENTED_EDGE('',*,*,#12176,.F.);
#16166=ORIENTED_EDGE('',*,*,#12177,.F.);
#16167=ORIENTED_EDGE('',*,*,#12178,.T.);
#16168=ORIENTED_EDGE('',*,*,#12179,.T.);
#16169=ORIENTED_EDGE('',*,*,#12180,.T.);
#16170=ORIENTED_EDGE('',*,*,#12181,.T.);
#16171=ORIENTED_EDGE('',*,*,#12182,.T.);
#16172=ORIENTED_EDGE('',*,*,#12183,.T.);
#16173=ORIENTED_EDGE('',*,*,#12182,.F.);
#16174=ORIENTED_EDGE('',*,*,#12184,.T.);
#16175=ORIENTED_EDGE('',*,*,#12185,.T.);
#16176=ORIENTED_EDGE('',*,*,#12186,.T.);
#16177=ORIENTED_EDGE('',*,*,#12187,.T.);
#16178=ORIENTED_EDGE('',*,*,#12179,.F.);
#16179=ORIENTED_EDGE('',*,*,#12188,.T.);
#16180=ORIENTED_EDGE('',*,*,#12189,.T.);
#16181=ORIENTED_EDGE('',*,*,#12190,.T.);
#16182=ORIENTED_EDGE('',*,*,#12186,.F.);
#16183=ORIENTED_EDGE('',*,*,#12191,.T.);
#16184=ORIENTED_EDGE('',*,*,#12192,.T.);
#16185=ORIENTED_EDGE('',*,*,#12193,.T.);
#16186=ORIENTED_EDGE('',*,*,#12189,.F.);
#16187=ORIENTED_EDGE('',*,*,#12194,.T.);
#16188=ORIENTED_EDGE('',*,*,#12195,.T.);
#16189=ORIENTED_EDGE('',*,*,#12196,.T.);
#16190=ORIENTED_EDGE('',*,*,#12192,.F.);
#16191=ORIENTED_EDGE('',*,*,#12197,.T.);
#16192=ORIENTED_EDGE('',*,*,#12198,.T.);
#16193=ORIENTED_EDGE('',*,*,#12199,.T.);
#16194=ORIENTED_EDGE('',*,*,#12195,.F.);
#16195=ORIENTED_EDGE('',*,*,#12200,.T.);
#16196=ORIENTED_EDGE('',*,*,#12201,.T.);
#16197=ORIENTED_EDGE('',*,*,#12202,.T.);
#16198=ORIENTED_EDGE('',*,*,#12198,.F.);
#16199=ORIENTED_EDGE('',*,*,#12203,.T.);
#16200=ORIENTED_EDGE('',*,*,#12204,.T.);
#16201=ORIENTED_EDGE('',*,*,#12205,.T.);
#16202=ORIENTED_EDGE('',*,*,#12201,.F.);
#16203=ORIENTED_EDGE('',*,*,#12206,.T.);
#16204=ORIENTED_EDGE('',*,*,#12207,.T.);
#16205=ORIENTED_EDGE('',*,*,#12208,.T.);
#16206=ORIENTED_EDGE('',*,*,#12204,.F.);
#16207=ORIENTED_EDGE('',*,*,#12209,.T.);
#16208=ORIENTED_EDGE('',*,*,#12210,.T.);
#16209=ORIENTED_EDGE('',*,*,#12211,.T.);
#16210=ORIENTED_EDGE('',*,*,#12207,.F.);
#16211=ORIENTED_EDGE('',*,*,#12212,.T.);
#16212=ORIENTED_EDGE('',*,*,#12213,.T.);
#16213=ORIENTED_EDGE('',*,*,#12214,.T.);
#16214=ORIENTED_EDGE('',*,*,#12210,.F.);
#16215=ORIENTED_EDGE('',*,*,#12215,.T.);
#16216=ORIENTED_EDGE('',*,*,#12216,.T.);
#16217=ORIENTED_EDGE('',*,*,#12217,.T.);
#16218=ORIENTED_EDGE('',*,*,#12213,.F.);
#16219=ORIENTED_EDGE('',*,*,#12218,.T.);
#16220=ORIENTED_EDGE('',*,*,#12219,.T.);
#16221=ORIENTED_EDGE('',*,*,#12220,.T.);
#16222=ORIENTED_EDGE('',*,*,#12216,.F.);
#16223=ORIENTED_EDGE('',*,*,#12221,.T.);
#16224=ORIENTED_EDGE('',*,*,#12222,.T.);
#16225=ORIENTED_EDGE('',*,*,#12223,.T.);
#16226=ORIENTED_EDGE('',*,*,#12219,.F.);
#16227=ORIENTED_EDGE('',*,*,#12224,.T.);
#16228=ORIENTED_EDGE('',*,*,#12225,.F.);
#16229=ORIENTED_EDGE('',*,*,#12226,.T.);
#16230=ORIENTED_EDGE('',*,*,#12227,.F.);
#16231=ORIENTED_EDGE('',*,*,#12228,.T.);
#16232=ORIENTED_EDGE('',*,*,#12229,.T.);
#16233=ORIENTED_EDGE('',*,*,#12230,.T.);
#16234=ORIENTED_EDGE('',*,*,#12231,.F.);
#16235=ORIENTED_EDGE('',*,*,#12232,.F.);
#16236=ORIENTED_EDGE('',*,*,#12233,.T.);
#16237=ORIENTED_EDGE('',*,*,#12234,.T.);
#16238=ORIENTED_EDGE('',*,*,#12229,.F.);
#16239=ORIENTED_EDGE('',*,*,#12235,.F.);
#16240=ORIENTED_EDGE('',*,*,#12236,.T.);
#16241=ORIENTED_EDGE('',*,*,#12237,.T.);
#16242=ORIENTED_EDGE('',*,*,#12233,.F.);
#16243=ORIENTED_EDGE('',*,*,#12238,.F.);
#16244=ORIENTED_EDGE('',*,*,#12239,.T.);
#16245=ORIENTED_EDGE('',*,*,#12240,.T.);
#16246=ORIENTED_EDGE('',*,*,#12236,.F.);
#16247=ORIENTED_EDGE('',*,*,#12241,.F.);
#16248=ORIENTED_EDGE('',*,*,#12242,.T.);
#16249=ORIENTED_EDGE('',*,*,#12243,.T.);
#16250=ORIENTED_EDGE('',*,*,#12239,.F.);
#16251=ORIENTED_EDGE('',*,*,#12244,.F.);
#16252=ORIENTED_EDGE('',*,*,#12245,.T.);
#16253=ORIENTED_EDGE('',*,*,#12246,.T.);
#16254=ORIENTED_EDGE('',*,*,#12242,.F.);
#16255=ORIENTED_EDGE('',*,*,#12247,.F.);
#16256=ORIENTED_EDGE('',*,*,#12248,.T.);
#16257=ORIENTED_EDGE('',*,*,#12249,.T.);
#16258=ORIENTED_EDGE('',*,*,#12245,.F.);
#16259=ORIENTED_EDGE('',*,*,#12250,.F.);
#16260=ORIENTED_EDGE('',*,*,#12251,.T.);
#16261=ORIENTED_EDGE('',*,*,#12252,.T.);
#16262=ORIENTED_EDGE('',*,*,#12248,.F.);
#16263=ORIENTED_EDGE('',*,*,#12253,.F.);
#16264=ORIENTED_EDGE('',*,*,#12254,.T.);
#16265=ORIENTED_EDGE('',*,*,#12255,.T.);
#16266=ORIENTED_EDGE('',*,*,#12251,.F.);
#16267=ORIENTED_EDGE('',*,*,#12256,.F.);
#16268=ORIENTED_EDGE('',*,*,#12257,.T.);
#16269=ORIENTED_EDGE('',*,*,#12258,.T.);
#16270=ORIENTED_EDGE('',*,*,#12254,.F.);
#16271=ORIENTED_EDGE('',*,*,#12259,.F.);
#16272=ORIENTED_EDGE('',*,*,#12260,.T.);
#16273=ORIENTED_EDGE('',*,*,#12261,.T.);
#16274=ORIENTED_EDGE('',*,*,#12257,.F.);
#16275=ORIENTED_EDGE('',*,*,#12262,.F.);
#16276=ORIENTED_EDGE('',*,*,#12263,.T.);
#16277=ORIENTED_EDGE('',*,*,#12264,.T.);
#16278=ORIENTED_EDGE('',*,*,#12260,.F.);
#16279=ORIENTED_EDGE('',*,*,#12265,.F.);
#16280=ORIENTED_EDGE('',*,*,#12266,.T.);
#16281=ORIENTED_EDGE('',*,*,#12267,.T.);
#16282=ORIENTED_EDGE('',*,*,#12263,.F.);
#16283=ORIENTED_EDGE('',*,*,#12268,.F.);
#16284=ORIENTED_EDGE('',*,*,#12269,.T.);
#16285=ORIENTED_EDGE('',*,*,#12270,.T.);
#16286=ORIENTED_EDGE('',*,*,#12266,.F.);
#16287=ORIENTED_EDGE('',*,*,#12271,.F.);
#16288=ORIENTED_EDGE('',*,*,#12272,.F.);
#16289=ORIENTED_EDGE('',*,*,#12273,.F.);
#16290=ORIENTED_EDGE('',*,*,#12274,.F.);
#16291=ORIENTED_EDGE('',*,*,#12275,.T.);
#16292=ORIENTED_EDGE('',*,*,#12276,.T.);
#16293=ORIENTED_EDGE('',*,*,#12277,.T.);
#16294=ORIENTED_EDGE('',*,*,#12278,.T.);
#16295=ORIENTED_EDGE('',*,*,#12279,.T.);
#16296=ORIENTED_EDGE('',*,*,#12280,.T.);
#16297=ORIENTED_EDGE('',*,*,#12279,.F.);
#16298=ORIENTED_EDGE('',*,*,#12281,.T.);
#16299=ORIENTED_EDGE('',*,*,#12282,.T.);
#16300=ORIENTED_EDGE('',*,*,#12283,.T.);
#16301=ORIENTED_EDGE('',*,*,#12284,.T.);
#16302=ORIENTED_EDGE('',*,*,#12276,.F.);
#16303=ORIENTED_EDGE('',*,*,#12285,.T.);
#16304=ORIENTED_EDGE('',*,*,#12286,.T.);
#16305=ORIENTED_EDGE('',*,*,#12287,.T.);
#16306=ORIENTED_EDGE('',*,*,#12283,.F.);
#16307=ORIENTED_EDGE('',*,*,#12288,.T.);
#16308=ORIENTED_EDGE('',*,*,#12289,.T.);
#16309=ORIENTED_EDGE('',*,*,#12290,.T.);
#16310=ORIENTED_EDGE('',*,*,#12286,.F.);
#16311=ORIENTED_EDGE('',*,*,#12291,.T.);
#16312=ORIENTED_EDGE('',*,*,#12292,.T.);
#16313=ORIENTED_EDGE('',*,*,#12293,.T.);
#16314=ORIENTED_EDGE('',*,*,#12289,.F.);
#16315=ORIENTED_EDGE('',*,*,#12294,.T.);
#16316=ORIENTED_EDGE('',*,*,#12295,.T.);
#16317=ORIENTED_EDGE('',*,*,#12296,.T.);
#16318=ORIENTED_EDGE('',*,*,#12292,.F.);
#16319=ORIENTED_EDGE('',*,*,#12297,.T.);
#16320=ORIENTED_EDGE('',*,*,#12298,.T.);
#16321=ORIENTED_EDGE('',*,*,#12299,.T.);
#16322=ORIENTED_EDGE('',*,*,#12295,.F.);
#16323=ORIENTED_EDGE('',*,*,#12300,.T.);
#16324=ORIENTED_EDGE('',*,*,#12301,.T.);
#16325=ORIENTED_EDGE('',*,*,#12302,.T.);
#16326=ORIENTED_EDGE('',*,*,#12298,.F.);
#16327=ORIENTED_EDGE('',*,*,#12303,.T.);
#16328=ORIENTED_EDGE('',*,*,#12304,.T.);
#16329=ORIENTED_EDGE('',*,*,#12305,.T.);
#16330=ORIENTED_EDGE('',*,*,#12301,.F.);
#16331=ORIENTED_EDGE('',*,*,#12306,.T.);
#16332=ORIENTED_EDGE('',*,*,#12307,.T.);
#16333=ORIENTED_EDGE('',*,*,#12308,.T.);
#16334=ORIENTED_EDGE('',*,*,#12304,.F.);
#16335=ORIENTED_EDGE('',*,*,#12309,.T.);
#16336=ORIENTED_EDGE('',*,*,#12310,.T.);
#16337=ORIENTED_EDGE('',*,*,#12311,.T.);
#16338=ORIENTED_EDGE('',*,*,#12307,.F.);
#16339=ORIENTED_EDGE('',*,*,#12312,.T.);
#16340=ORIENTED_EDGE('',*,*,#12313,.T.);
#16341=ORIENTED_EDGE('',*,*,#12314,.T.);
#16342=ORIENTED_EDGE('',*,*,#12310,.F.);
#16343=ORIENTED_EDGE('',*,*,#12315,.T.);
#16344=ORIENTED_EDGE('',*,*,#12316,.T.);
#16345=ORIENTED_EDGE('',*,*,#12317,.T.);
#16346=ORIENTED_EDGE('',*,*,#12313,.F.);
#16347=ORIENTED_EDGE('',*,*,#12318,.T.);
#16348=ORIENTED_EDGE('',*,*,#12319,.T.);
#16349=ORIENTED_EDGE('',*,*,#12320,.T.);
#16350=ORIENTED_EDGE('',*,*,#12316,.F.);
#16351=ORIENTED_EDGE('',*,*,#12321,.T.);
#16352=ORIENTED_EDGE('',*,*,#12322,.F.);
#16353=ORIENTED_EDGE('',*,*,#12323,.T.);
#16354=ORIENTED_EDGE('',*,*,#12324,.F.);
#16355=ORIENTED_EDGE('',*,*,#12325,.T.);
#16356=ORIENTED_EDGE('',*,*,#12326,.T.);
#16357=ORIENTED_EDGE('',*,*,#12327,.T.);
#16358=ORIENTED_EDGE('',*,*,#12328,.F.);
#16359=ORIENTED_EDGE('',*,*,#12329,.F.);
#16360=ORIENTED_EDGE('',*,*,#12330,.T.);
#16361=ORIENTED_EDGE('',*,*,#12331,.T.);
#16362=ORIENTED_EDGE('',*,*,#12326,.F.);
#16363=ORIENTED_EDGE('',*,*,#12332,.F.);
#16364=ORIENTED_EDGE('',*,*,#12333,.T.);
#16365=ORIENTED_EDGE('',*,*,#12334,.T.);
#16366=ORIENTED_EDGE('',*,*,#12330,.F.);
#16367=ORIENTED_EDGE('',*,*,#12335,.F.);
#16368=ORIENTED_EDGE('',*,*,#12336,.T.);
#16369=ORIENTED_EDGE('',*,*,#12337,.T.);
#16370=ORIENTED_EDGE('',*,*,#12333,.F.);
#16371=ORIENTED_EDGE('',*,*,#12338,.F.);
#16372=ORIENTED_EDGE('',*,*,#12339,.T.);
#16373=ORIENTED_EDGE('',*,*,#12340,.T.);
#16374=ORIENTED_EDGE('',*,*,#12336,.F.);
#16375=ORIENTED_EDGE('',*,*,#12341,.F.);
#16376=ORIENTED_EDGE('',*,*,#12342,.T.);
#16377=ORIENTED_EDGE('',*,*,#12343,.T.);
#16378=ORIENTED_EDGE('',*,*,#12339,.F.);
#16379=ORIENTED_EDGE('',*,*,#12344,.F.);
#16380=ORIENTED_EDGE('',*,*,#12345,.T.);
#16381=ORIENTED_EDGE('',*,*,#12346,.T.);
#16382=ORIENTED_EDGE('',*,*,#12342,.F.);
#16383=ORIENTED_EDGE('',*,*,#12347,.F.);
#16384=ORIENTED_EDGE('',*,*,#12348,.T.);
#16385=ORIENTED_EDGE('',*,*,#12349,.T.);
#16386=ORIENTED_EDGE('',*,*,#12345,.F.);
#16387=ORIENTED_EDGE('',*,*,#12350,.F.);
#16388=ORIENTED_EDGE('',*,*,#12351,.T.);
#16389=ORIENTED_EDGE('',*,*,#12352,.T.);
#16390=ORIENTED_EDGE('',*,*,#12348,.F.);
#16391=ORIENTED_EDGE('',*,*,#12353,.F.);
#16392=ORIENTED_EDGE('',*,*,#12354,.T.);
#16393=ORIENTED_EDGE('',*,*,#12355,.T.);
#16394=ORIENTED_EDGE('',*,*,#12351,.F.);
#16395=ORIENTED_EDGE('',*,*,#12356,.F.);
#16396=ORIENTED_EDGE('',*,*,#12357,.T.);
#16397=ORIENTED_EDGE('',*,*,#12358,.T.);
#16398=ORIENTED_EDGE('',*,*,#12354,.F.);
#16399=ORIENTED_EDGE('',*,*,#12359,.F.);
#16400=ORIENTED_EDGE('',*,*,#12360,.T.);
#16401=ORIENTED_EDGE('',*,*,#12361,.T.);
#16402=ORIENTED_EDGE('',*,*,#12357,.F.);
#16403=ORIENTED_EDGE('',*,*,#12362,.F.);
#16404=ORIENTED_EDGE('',*,*,#12363,.T.);
#16405=ORIENTED_EDGE('',*,*,#12364,.T.);
#16406=ORIENTED_EDGE('',*,*,#12360,.F.);
#16407=ORIENTED_EDGE('',*,*,#12365,.F.);
#16408=ORIENTED_EDGE('',*,*,#12366,.T.);
#16409=ORIENTED_EDGE('',*,*,#12367,.T.);
#16410=ORIENTED_EDGE('',*,*,#12363,.F.);
#16411=ORIENTED_EDGE('',*,*,#12368,.F.);
#16412=ORIENTED_EDGE('',*,*,#12369,.F.);
#16413=ORIENTED_EDGE('',*,*,#12370,.F.);
#16414=ORIENTED_EDGE('',*,*,#12371,.F.);
#16415=ORIENTED_EDGE('',*,*,#12372,.T.);
#16416=ORIENTED_EDGE('',*,*,#12373,.F.);
#16417=ORIENTED_EDGE('',*,*,#12374,.T.);
#16418=ORIENTED_EDGE('',*,*,#12375,.F.);
#16419=ORIENTED_EDGE('',*,*,#12376,.F.);
#16420=ORIENTED_EDGE('',*,*,#12374,.F.);
#16421=ORIENTED_EDGE('',*,*,#12377,.F.);
#16422=ORIENTED_EDGE('',*,*,#12378,.F.);
#16423=ORIENTED_EDGE('',*,*,#12379,.F.);
#16424=ORIENTED_EDGE('',*,*,#12380,.T.);
#16425=ORIENTED_EDGE('',*,*,#12381,.F.);
#16426=ORIENTED_EDGE('',*,*,#12382,.F.);
#16427=ORIENTED_EDGE('',*,*,#12380,.F.);
#16428=ORIENTED_EDGE('',*,*,#12383,.F.);
#16429=ORIENTED_EDGE('',*,*,#12384,.F.);
#16430=ORIENTED_EDGE('',*,*,#12385,.T.);
#16431=ORIENTED_EDGE('',*,*,#12386,.F.);
#16432=ORIENTED_EDGE('',*,*,#12387,.F.);
#16433=ORIENTED_EDGE('',*,*,#12388,.F.);
#16434=ORIENTED_EDGE('',*,*,#12385,.F.);
#16435=ORIENTED_EDGE('',*,*,#12389,.F.);
#16436=ORIENTED_EDGE('',*,*,#12390,.F.);
#16437=ORIENTED_EDGE('',*,*,#12391,.F.);
#16438=ORIENTED_EDGE('',*,*,#12392,.T.);
#16439=ORIENTED_EDGE('',*,*,#12393,.F.);
#16440=ORIENTED_EDGE('',*,*,#12392,.F.);
#16441=ORIENTED_EDGE('',*,*,#12394,.F.);
#16442=ORIENTED_EDGE('',*,*,#12395,.F.);
#16443=ORIENTED_EDGE('',*,*,#12396,.T.);
#16444=ORIENTED_EDGE('',*,*,#12397,.F.);
#16445=ORIENTED_EDGE('',*,*,#12398,.F.);
#16446=ORIENTED_EDGE('',*,*,#12396,.F.);
#16447=ORIENTED_EDGE('',*,*,#12399,.F.);
#16448=ORIENTED_EDGE('',*,*,#12400,.F.);
#16449=ORIENTED_EDGE('',*,*,#12401,.F.);
#16450=ORIENTED_EDGE('',*,*,#12402,.T.);
#16451=ORIENTED_EDGE('',*,*,#12403,.F.);
#16452=ORIENTED_EDGE('',*,*,#12404,.F.);
#16453=ORIENTED_EDGE('',*,*,#12402,.F.);
#16454=ORIENTED_EDGE('',*,*,#12405,.F.);
#16455=ORIENTED_EDGE('',*,*,#12406,.F.);
#16456=ORIENTED_EDGE('',*,*,#12407,.T.);
#16457=ORIENTED_EDGE('',*,*,#12408,.F.);
#16458=ORIENTED_EDGE('',*,*,#12409,.F.);
#16459=ORIENTED_EDGE('',*,*,#12410,.F.);
#16460=ORIENTED_EDGE('',*,*,#12407,.F.);
#16461=ORIENTED_EDGE('',*,*,#12411,.F.);
#16462=ORIENTED_EDGE('',*,*,#12412,.F.);
#16463=ORIENTED_EDGE('',*,*,#12413,.F.);
#16464=ORIENTED_EDGE('',*,*,#12414,.T.);
#16465=ORIENTED_EDGE('',*,*,#12415,.F.);
#16466=ORIENTED_EDGE('',*,*,#12414,.F.);
#16467=ORIENTED_EDGE('',*,*,#12416,.F.);
#16468=ORIENTED_EDGE('',*,*,#12417,.F.);
#16469=ORIENTED_EDGE('',*,*,#12418,.T.);
#16470=ORIENTED_EDGE('',*,*,#12419,.F.);
#16471=ORIENTED_EDGE('',*,*,#12420,.F.);
#16472=ORIENTED_EDGE('',*,*,#12418,.F.);
#16473=ORIENTED_EDGE('',*,*,#12421,.F.);
#16474=ORIENTED_EDGE('',*,*,#12422,.F.);
#16475=ORIENTED_EDGE('',*,*,#12423,.F.);
#16476=ORIENTED_EDGE('',*,*,#12424,.T.);
#16477=ORIENTED_EDGE('',*,*,#12425,.F.);
#16478=ORIENTED_EDGE('',*,*,#12426,.F.);
#16479=ORIENTED_EDGE('',*,*,#12424,.F.);
#16480=ORIENTED_EDGE('',*,*,#12427,.F.);
#16481=ORIENTED_EDGE('',*,*,#12428,.F.);
#16482=ORIENTED_EDGE('',*,*,#12429,.T.);
#16483=ORIENTED_EDGE('',*,*,#12430,.F.);
#16484=ORIENTED_EDGE('',*,*,#12431,.F.);
#16485=ORIENTED_EDGE('',*,*,#12432,.F.);
#16486=ORIENTED_EDGE('',*,*,#12429,.F.);
#16487=ORIENTED_EDGE('',*,*,#12433,.F.);
#16488=ORIENTED_EDGE('',*,*,#12434,.F.);
#16489=ORIENTED_EDGE('',*,*,#12435,.F.);
#16490=ORIENTED_EDGE('',*,*,#12436,.T.);
#16491=ORIENTED_EDGE('',*,*,#12437,.F.);
#16492=ORIENTED_EDGE('',*,*,#12436,.F.);
#16493=ORIENTED_EDGE('',*,*,#12438,.F.);
#16494=ORIENTED_EDGE('',*,*,#12278,.F.);
#16495=ORIENTED_EDGE('',*,*,#12439,.T.);
#16496=ORIENTED_EDGE('',*,*,#12328,.T.);
#16497=ORIENTED_EDGE('',*,*,#12440,.T.);
#16498=ORIENTED_EDGE('',*,*,#12281,.F.);
#16499=ORIENTED_EDGE('',*,*,#12369,.T.);
#16500=ORIENTED_EDGE('',*,*,#12441,.T.);
#16501=ORIENTED_EDGE('',*,*,#12366,.F.);
#16502=ORIENTED_EDGE('',*,*,#12442,.F.);
#16503=ORIENTED_EDGE('',*,*,#12440,.F.);
#16504=ORIENTED_EDGE('',*,*,#12327,.F.);
#16505=ORIENTED_EDGE('',*,*,#12331,.F.);
#16506=ORIENTED_EDGE('',*,*,#12334,.F.);
#16507=ORIENTED_EDGE('',*,*,#12337,.F.);
#16508=ORIENTED_EDGE('',*,*,#12340,.F.);
#16509=ORIENTED_EDGE('',*,*,#12343,.F.);
#16510=ORIENTED_EDGE('',*,*,#12346,.F.);
#16511=ORIENTED_EDGE('',*,*,#12349,.F.);
#16512=ORIENTED_EDGE('',*,*,#12352,.F.);
#16513=ORIENTED_EDGE('',*,*,#12355,.F.);
#16514=ORIENTED_EDGE('',*,*,#12358,.F.);
#16515=ORIENTED_EDGE('',*,*,#12361,.F.);
#16516=ORIENTED_EDGE('',*,*,#12364,.F.);
#16517=ORIENTED_EDGE('',*,*,#12367,.F.);
#16518=ORIENTED_EDGE('',*,*,#12441,.F.);
#16519=ORIENTED_EDGE('',*,*,#12372,.F.);
#16520=ORIENTED_EDGE('',*,*,#12443,.F.);
#16521=ORIENTED_EDGE('',*,*,#12323,.F.);
#16522=ORIENTED_EDGE('',*,*,#12444,.F.);
#16523=ORIENTED_EDGE('',*,*,#12321,.F.);
#16524=ORIENTED_EDGE('',*,*,#12318,.F.);
#16525=ORIENTED_EDGE('',*,*,#12315,.F.);
#16526=ORIENTED_EDGE('',*,*,#12312,.F.);
#16527=ORIENTED_EDGE('',*,*,#12309,.F.);
#16528=ORIENTED_EDGE('',*,*,#12306,.F.);
#16529=ORIENTED_EDGE('',*,*,#12303,.F.);
#16530=ORIENTED_EDGE('',*,*,#12300,.F.);
#16531=ORIENTED_EDGE('',*,*,#12297,.F.);
#16532=ORIENTED_EDGE('',*,*,#12294,.F.);
#16533=ORIENTED_EDGE('',*,*,#12291,.F.);
#16534=ORIENTED_EDGE('',*,*,#12288,.F.);
#16535=ORIENTED_EDGE('',*,*,#12285,.F.);
#16536=ORIENTED_EDGE('',*,*,#12282,.F.);
#16537=ORIENTED_EDGE('',*,*,#12439,.F.);
#16538=ORIENTED_EDGE('',*,*,#12277,.F.);
#16539=ORIENTED_EDGE('',*,*,#12284,.F.);
#16540=ORIENTED_EDGE('',*,*,#12287,.F.);
#16541=ORIENTED_EDGE('',*,*,#12290,.F.);
#16542=ORIENTED_EDGE('',*,*,#12293,.F.);
#16543=ORIENTED_EDGE('',*,*,#12296,.F.);
#16544=ORIENTED_EDGE('',*,*,#12299,.F.);
#16545=ORIENTED_EDGE('',*,*,#12302,.F.);
#16546=ORIENTED_EDGE('',*,*,#12305,.F.);
#16547=ORIENTED_EDGE('',*,*,#12308,.F.);
#16548=ORIENTED_EDGE('',*,*,#12311,.F.);
#16549=ORIENTED_EDGE('',*,*,#12314,.F.);
#16550=ORIENTED_EDGE('',*,*,#12317,.F.);
#16551=ORIENTED_EDGE('',*,*,#12320,.F.);
#16552=ORIENTED_EDGE('',*,*,#12445,.F.);
#16553=ORIENTED_EDGE('',*,*,#12325,.F.);
#16554=ORIENTED_EDGE('',*,*,#12446,.F.);
#16555=ORIENTED_EDGE('',*,*,#12370,.T.);
#16556=ORIENTED_EDGE('',*,*,#12442,.T.);
#16557=ORIENTED_EDGE('',*,*,#12368,.T.);
#16558=ORIENTED_EDGE('',*,*,#12365,.T.);
#16559=ORIENTED_EDGE('',*,*,#12362,.T.);
#16560=ORIENTED_EDGE('',*,*,#12359,.T.);
#16561=ORIENTED_EDGE('',*,*,#12356,.T.);
#16562=ORIENTED_EDGE('',*,*,#12353,.T.);
#16563=ORIENTED_EDGE('',*,*,#12350,.T.);
#16564=ORIENTED_EDGE('',*,*,#12347,.T.);
#16565=ORIENTED_EDGE('',*,*,#12344,.T.);
#16566=ORIENTED_EDGE('',*,*,#12341,.T.);
#16567=ORIENTED_EDGE('',*,*,#12338,.T.);
#16568=ORIENTED_EDGE('',*,*,#12335,.T.);
#16569=ORIENTED_EDGE('',*,*,#12332,.T.);
#16570=ORIENTED_EDGE('',*,*,#12329,.T.);
#16571=ORIENTED_EDGE('',*,*,#12322,.T.);
#16572=ORIENTED_EDGE('',*,*,#12445,.T.);
#16573=ORIENTED_EDGE('',*,*,#12319,.F.);
#16574=ORIENTED_EDGE('',*,*,#12444,.T.);
#16575=ORIENTED_EDGE('',*,*,#12181,.F.);
#16576=ORIENTED_EDGE('',*,*,#12447,.T.);
#16577=ORIENTED_EDGE('',*,*,#12231,.T.);
#16578=ORIENTED_EDGE('',*,*,#12448,.T.);
#16579=ORIENTED_EDGE('',*,*,#12184,.F.);
#16580=ORIENTED_EDGE('',*,*,#12272,.T.);
#16581=ORIENTED_EDGE('',*,*,#12449,.T.);
#16582=ORIENTED_EDGE('',*,*,#12269,.F.);
#16583=ORIENTED_EDGE('',*,*,#12450,.F.);
#16584=ORIENTED_EDGE('',*,*,#12448,.F.);
#16585=ORIENTED_EDGE('',*,*,#12230,.F.);
#16586=ORIENTED_EDGE('',*,*,#12234,.F.);
#16587=ORIENTED_EDGE('',*,*,#12237,.F.);
#16588=ORIENTED_EDGE('',*,*,#12240,.F.);
#16589=ORIENTED_EDGE('',*,*,#12243,.F.);
#16590=ORIENTED_EDGE('',*,*,#12246,.F.);
#16591=ORIENTED_EDGE('',*,*,#12249,.F.);
#16592=ORIENTED_EDGE('',*,*,#12252,.F.);
#16593=ORIENTED_EDGE('',*,*,#12255,.F.);
#16594=ORIENTED_EDGE('',*,*,#12258,.F.);
#16595=ORIENTED_EDGE('',*,*,#12261,.F.);
#16596=ORIENTED_EDGE('',*,*,#12264,.F.);
#16597=ORIENTED_EDGE('',*,*,#12267,.F.);
#16598=ORIENTED_EDGE('',*,*,#12270,.F.);
#16599=ORIENTED_EDGE('',*,*,#12449,.F.);
#16600=ORIENTED_EDGE('',*,*,#12275,.F.);
#16601=ORIENTED_EDGE('',*,*,#12451,.F.);
#16602=ORIENTED_EDGE('',*,*,#12226,.F.);
#16603=ORIENTED_EDGE('',*,*,#12452,.F.);
#16604=ORIENTED_EDGE('',*,*,#12224,.F.);
#16605=ORIENTED_EDGE('',*,*,#12221,.F.);
#16606=ORIENTED_EDGE('',*,*,#12218,.F.);
#16607=ORIENTED_EDGE('',*,*,#12215,.F.);
#16608=ORIENTED_EDGE('',*,*,#12212,.F.);
#16609=ORIENTED_EDGE('',*,*,#12209,.F.);
#16610=ORIENTED_EDGE('',*,*,#12206,.F.);
#16611=ORIENTED_EDGE('',*,*,#12203,.F.);
#16612=ORIENTED_EDGE('',*,*,#12200,.F.);
#16613=ORIENTED_EDGE('',*,*,#12197,.F.);
#16614=ORIENTED_EDGE('',*,*,#12194,.F.);
#16615=ORIENTED_EDGE('',*,*,#12191,.F.);
#16616=ORIENTED_EDGE('',*,*,#12188,.F.);
#16617=ORIENTED_EDGE('',*,*,#12185,.F.);
#16618=ORIENTED_EDGE('',*,*,#12447,.F.);
#16619=ORIENTED_EDGE('',*,*,#12180,.F.);
#16620=ORIENTED_EDGE('',*,*,#12187,.F.);
#16621=ORIENTED_EDGE('',*,*,#12190,.F.);
#16622=ORIENTED_EDGE('',*,*,#12193,.F.);
#16623=ORIENTED_EDGE('',*,*,#12196,.F.);
#16624=ORIENTED_EDGE('',*,*,#12199,.F.);
#16625=ORIENTED_EDGE('',*,*,#12202,.F.);
#16626=ORIENTED_EDGE('',*,*,#12205,.F.);
#16627=ORIENTED_EDGE('',*,*,#12208,.F.);
#16628=ORIENTED_EDGE('',*,*,#12211,.F.);
#16629=ORIENTED_EDGE('',*,*,#12214,.F.);
#16630=ORIENTED_EDGE('',*,*,#12217,.F.);
#16631=ORIENTED_EDGE('',*,*,#12220,.F.);
#16632=ORIENTED_EDGE('',*,*,#12223,.F.);
#16633=ORIENTED_EDGE('',*,*,#12453,.F.);
#16634=ORIENTED_EDGE('',*,*,#12228,.F.);
#16635=ORIENTED_EDGE('',*,*,#12454,.F.);
#16636=ORIENTED_EDGE('',*,*,#12273,.T.);
#16637=ORIENTED_EDGE('',*,*,#12450,.T.);
#16638=ORIENTED_EDGE('',*,*,#12271,.T.);
#16639=ORIENTED_EDGE('',*,*,#12268,.T.);
#16640=ORIENTED_EDGE('',*,*,#12265,.T.);
#16641=ORIENTED_EDGE('',*,*,#12262,.T.);
#16642=ORIENTED_EDGE('',*,*,#12259,.T.);
#16643=ORIENTED_EDGE('',*,*,#12256,.T.);
#16644=ORIENTED_EDGE('',*,*,#12253,.T.);
#16645=ORIENTED_EDGE('',*,*,#12250,.T.);
#16646=ORIENTED_EDGE('',*,*,#12247,.T.);
#16647=ORIENTED_EDGE('',*,*,#12244,.T.);
#16648=ORIENTED_EDGE('',*,*,#12241,.T.);
#16649=ORIENTED_EDGE('',*,*,#12238,.T.);
#16650=ORIENTED_EDGE('',*,*,#12235,.T.);
#16651=ORIENTED_EDGE('',*,*,#12232,.T.);
#16652=ORIENTED_EDGE('',*,*,#12225,.T.);
#16653=ORIENTED_EDGE('',*,*,#12453,.T.);
#16654=ORIENTED_EDGE('',*,*,#12222,.F.);
#16655=ORIENTED_EDGE('',*,*,#12452,.T.);
#16656=ORIENTED_EDGE('',*,*,#12084,.F.);
#16657=ORIENTED_EDGE('',*,*,#12455,.T.);
#16658=ORIENTED_EDGE('',*,*,#12134,.T.);
#16659=ORIENTED_EDGE('',*,*,#12456,.T.);
#16660=ORIENTED_EDGE('',*,*,#12087,.F.);
#16661=ORIENTED_EDGE('',*,*,#12175,.T.);
#16662=ORIENTED_EDGE('',*,*,#12457,.T.);
#16663=ORIENTED_EDGE('',*,*,#12172,.F.);
#16664=ORIENTED_EDGE('',*,*,#12458,.F.);
#16665=ORIENTED_EDGE('',*,*,#12456,.F.);
#16666=ORIENTED_EDGE('',*,*,#12133,.F.);
#16667=ORIENTED_EDGE('',*,*,#12137,.F.);
#16668=ORIENTED_EDGE('',*,*,#12140,.F.);
#16669=ORIENTED_EDGE('',*,*,#12143,.F.);
#16670=ORIENTED_EDGE('',*,*,#12146,.F.);
#16671=ORIENTED_EDGE('',*,*,#12149,.F.);
#16672=ORIENTED_EDGE('',*,*,#12152,.F.);
#16673=ORIENTED_EDGE('',*,*,#12155,.F.);
#16674=ORIENTED_EDGE('',*,*,#12158,.F.);
#16675=ORIENTED_EDGE('',*,*,#12161,.F.);
#16676=ORIENTED_EDGE('',*,*,#12164,.F.);
#16677=ORIENTED_EDGE('',*,*,#12167,.F.);
#16678=ORIENTED_EDGE('',*,*,#12170,.F.);
#16679=ORIENTED_EDGE('',*,*,#12173,.F.);
#16680=ORIENTED_EDGE('',*,*,#12457,.F.);
#16681=ORIENTED_EDGE('',*,*,#12178,.F.);
#16682=ORIENTED_EDGE('',*,*,#12459,.F.);
#16683=ORIENTED_EDGE('',*,*,#12129,.F.);
#16684=ORIENTED_EDGE('',*,*,#12460,.F.);
#16685=ORIENTED_EDGE('',*,*,#12127,.F.);
#16686=ORIENTED_EDGE('',*,*,#12124,.F.);
#16687=ORIENTED_EDGE('',*,*,#12121,.F.);
#16688=ORIENTED_EDGE('',*,*,#12118,.F.);
#16689=ORIENTED_EDGE('',*,*,#12115,.F.);
#16690=ORIENTED_EDGE('',*,*,#12112,.F.);
#16691=ORIENTED_EDGE('',*,*,#12109,.F.);
#16692=ORIENTED_EDGE('',*,*,#12106,.F.);
#16693=ORIENTED_EDGE('',*,*,#12103,.F.);
#16694=ORIENTED_EDGE('',*,*,#12100,.F.);
#16695=ORIENTED_EDGE('',*,*,#12097,.F.);
#16696=ORIENTED_EDGE('',*,*,#12094,.F.);
#16697=ORIENTED_EDGE('',*,*,#12091,.F.);
#16698=ORIENTED_EDGE('',*,*,#12088,.F.);
#16699=ORIENTED_EDGE('',*,*,#12455,.F.);
#16700=ORIENTED_EDGE('',*,*,#12083,.F.);
#16701=ORIENTED_EDGE('',*,*,#12090,.F.);
#16702=ORIENTED_EDGE('',*,*,#12093,.F.);
#16703=ORIENTED_EDGE('',*,*,#12096,.F.);
#16704=ORIENTED_EDGE('',*,*,#12099,.F.);
#16705=ORIENTED_EDGE('',*,*,#12102,.F.);
#16706=ORIENTED_EDGE('',*,*,#12105,.F.);
#16707=ORIENTED_EDGE('',*,*,#12108,.F.);
#16708=ORIENTED_EDGE('',*,*,#12111,.F.);
#16709=ORIENTED_EDGE('',*,*,#12114,.F.);
#16710=ORIENTED_EDGE('',*,*,#12117,.F.);
#16711=ORIENTED_EDGE('',*,*,#12120,.F.);
#16712=ORIENTED_EDGE('',*,*,#12123,.F.);
#16713=ORIENTED_EDGE('',*,*,#12126,.F.);
#16714=ORIENTED_EDGE('',*,*,#12461,.F.);
#16715=ORIENTED_EDGE('',*,*,#12131,.F.);
#16716=ORIENTED_EDGE('',*,*,#12462,.F.);
#16717=ORIENTED_EDGE('',*,*,#12176,.T.);
#16718=ORIENTED_EDGE('',*,*,#12458,.T.);
#16719=ORIENTED_EDGE('',*,*,#12174,.T.);
#16720=ORIENTED_EDGE('',*,*,#12171,.T.);
#16721=ORIENTED_EDGE('',*,*,#12168,.T.);
#16722=ORIENTED_EDGE('',*,*,#12165,.T.);
#16723=ORIENTED_EDGE('',*,*,#12162,.T.);
#16724=ORIENTED_EDGE('',*,*,#12159,.T.);
#16725=ORIENTED_EDGE('',*,*,#12156,.T.);
#16726=ORIENTED_EDGE('',*,*,#12153,.T.);
#16727=ORIENTED_EDGE('',*,*,#12150,.T.);
#16728=ORIENTED_EDGE('',*,*,#12147,.T.);
#16729=ORIENTED_EDGE('',*,*,#12144,.T.);
#16730=ORIENTED_EDGE('',*,*,#12141,.T.);
#16731=ORIENTED_EDGE('',*,*,#12138,.T.);
#16732=ORIENTED_EDGE('',*,*,#12135,.T.);
#16733=ORIENTED_EDGE('',*,*,#12128,.T.);
#16734=ORIENTED_EDGE('',*,*,#12461,.T.);
#16735=ORIENTED_EDGE('',*,*,#12125,.F.);
#16736=ORIENTED_EDGE('',*,*,#12460,.T.);
#16737=ORIENTED_EDGE('',*,*,#11987,.F.);
#16738=ORIENTED_EDGE('',*,*,#12463,.T.);
#16739=ORIENTED_EDGE('',*,*,#12037,.T.);
#16740=ORIENTED_EDGE('',*,*,#12464,.T.);
#16741=ORIENTED_EDGE('',*,*,#11990,.F.);
#16742=ORIENTED_EDGE('',*,*,#12078,.T.);
#16743=ORIENTED_EDGE('',*,*,#12465,.T.);
#16744=ORIENTED_EDGE('',*,*,#12075,.F.);
#16745=ORIENTED_EDGE('',*,*,#12466,.F.);
#16746=ORIENTED_EDGE('',*,*,#12464,.F.);
#16747=ORIENTED_EDGE('',*,*,#12036,.F.);
#16748=ORIENTED_EDGE('',*,*,#12040,.F.);
#16749=ORIENTED_EDGE('',*,*,#12043,.F.);
#16750=ORIENTED_EDGE('',*,*,#12046,.F.);
#16751=ORIENTED_EDGE('',*,*,#12049,.F.);
#16752=ORIENTED_EDGE('',*,*,#12052,.F.);
#16753=ORIENTED_EDGE('',*,*,#12055,.F.);
#16754=ORIENTED_EDGE('',*,*,#12058,.F.);
#16755=ORIENTED_EDGE('',*,*,#12061,.F.);
#16756=ORIENTED_EDGE('',*,*,#12064,.F.);
#16757=ORIENTED_EDGE('',*,*,#12067,.F.);
#16758=ORIENTED_EDGE('',*,*,#12070,.F.);
#16759=ORIENTED_EDGE('',*,*,#12073,.F.);
#16760=ORIENTED_EDGE('',*,*,#12076,.F.);
#16761=ORIENTED_EDGE('',*,*,#12465,.F.);
#16762=ORIENTED_EDGE('',*,*,#12081,.F.);
#16763=ORIENTED_EDGE('',*,*,#12467,.F.);
#16764=ORIENTED_EDGE('',*,*,#12032,.F.);
#16765=ORIENTED_EDGE('',*,*,#12468,.F.);
#16766=ORIENTED_EDGE('',*,*,#12030,.F.);
#16767=ORIENTED_EDGE('',*,*,#12027,.F.);
#16768=ORIENTED_EDGE('',*,*,#12024,.F.);
#16769=ORIENTED_EDGE('',*,*,#12021,.F.);
#16770=ORIENTED_EDGE('',*,*,#12018,.F.);
#16771=ORIENTED_EDGE('',*,*,#12015,.F.);
#16772=ORIENTED_EDGE('',*,*,#12012,.F.);
#16773=ORIENTED_EDGE('',*,*,#12009,.F.);
#16774=ORIENTED_EDGE('',*,*,#12006,.F.);
#16775=ORIENTED_EDGE('',*,*,#12003,.F.);
#16776=ORIENTED_EDGE('',*,*,#12000,.F.);
#16777=ORIENTED_EDGE('',*,*,#11997,.F.);
#16778=ORIENTED_EDGE('',*,*,#11994,.F.);
#16779=ORIENTED_EDGE('',*,*,#11991,.F.);
#16780=ORIENTED_EDGE('',*,*,#12463,.F.);
#16781=ORIENTED_EDGE('',*,*,#11986,.F.);
#16782=ORIENTED_EDGE('',*,*,#11993,.F.);
#16783=ORIENTED_EDGE('',*,*,#11996,.F.);
#16784=ORIENTED_EDGE('',*,*,#11999,.F.);
#16785=ORIENTED_EDGE('',*,*,#12002,.F.);
#16786=ORIENTED_EDGE('',*,*,#12005,.F.);
#16787=ORIENTED_EDGE('',*,*,#12008,.F.);
#16788=ORIENTED_EDGE('',*,*,#12011,.F.);
#16789=ORIENTED_EDGE('',*,*,#12014,.F.);
#16790=ORIENTED_EDGE('',*,*,#12017,.F.);
#16791=ORIENTED_EDGE('',*,*,#12020,.F.);
#16792=ORIENTED_EDGE('',*,*,#12023,.F.);
#16793=ORIENTED_EDGE('',*,*,#12026,.F.);
#16794=ORIENTED_EDGE('',*,*,#12029,.F.);
#16795=ORIENTED_EDGE('',*,*,#12469,.F.);
#16796=ORIENTED_EDGE('',*,*,#12034,.F.);
#16797=ORIENTED_EDGE('',*,*,#12470,.F.);
#16798=ORIENTED_EDGE('',*,*,#12079,.T.);
#16799=ORIENTED_EDGE('',*,*,#12466,.T.);
#16800=ORIENTED_EDGE('',*,*,#12077,.T.);
#16801=ORIENTED_EDGE('',*,*,#12074,.T.);
#16802=ORIENTED_EDGE('',*,*,#12071,.T.);
#16803=ORIENTED_EDGE('',*,*,#12068,.T.);
#16804=ORIENTED_EDGE('',*,*,#12065,.T.);
#16805=ORIENTED_EDGE('',*,*,#12062,.T.);
#16806=ORIENTED_EDGE('',*,*,#12059,.T.);
#16807=ORIENTED_EDGE('',*,*,#12056,.T.);
#16808=ORIENTED_EDGE('',*,*,#12053,.T.);
#16809=ORIENTED_EDGE('',*,*,#12050,.T.);
#16810=ORIENTED_EDGE('',*,*,#12047,.T.);
#16811=ORIENTED_EDGE('',*,*,#12044,.T.);
#16812=ORIENTED_EDGE('',*,*,#12041,.T.);
#16813=ORIENTED_EDGE('',*,*,#12038,.T.);
#16814=ORIENTED_EDGE('',*,*,#12031,.T.);
#16815=ORIENTED_EDGE('',*,*,#12469,.T.);
#16816=ORIENTED_EDGE('',*,*,#12028,.F.);
#16817=ORIENTED_EDGE('',*,*,#12468,.T.);
#16818=ORIENTED_EDGE('',*,*,#11890,.F.);
#16819=ORIENTED_EDGE('',*,*,#12471,.T.);
#16820=ORIENTED_EDGE('',*,*,#11940,.T.);
#16821=ORIENTED_EDGE('',*,*,#12472,.T.);
#16822=ORIENTED_EDGE('',*,*,#11893,.F.);
#16823=ORIENTED_EDGE('',*,*,#11981,.T.);
#16824=ORIENTED_EDGE('',*,*,#12473,.T.);
#16825=ORIENTED_EDGE('',*,*,#11978,.F.);
#16826=ORIENTED_EDGE('',*,*,#12474,.F.);
#16827=ORIENTED_EDGE('',*,*,#12472,.F.);
#16828=ORIENTED_EDGE('',*,*,#11939,.F.);
#16829=ORIENTED_EDGE('',*,*,#11943,.F.);
#16830=ORIENTED_EDGE('',*,*,#11946,.F.);
#16831=ORIENTED_EDGE('',*,*,#11949,.F.);
#16832=ORIENTED_EDGE('',*,*,#11952,.F.);
#16833=ORIENTED_EDGE('',*,*,#11955,.F.);
#16834=ORIENTED_EDGE('',*,*,#11958,.F.);
#16835=ORIENTED_EDGE('',*,*,#11961,.F.);
#16836=ORIENTED_EDGE('',*,*,#11964,.F.);
#16837=ORIENTED_EDGE('',*,*,#11967,.F.);
#16838=ORIENTED_EDGE('',*,*,#11970,.F.);
#16839=ORIENTED_EDGE('',*,*,#11973,.F.);
#16840=ORIENTED_EDGE('',*,*,#11976,.F.);
#16841=ORIENTED_EDGE('',*,*,#11979,.F.);
#16842=ORIENTED_EDGE('',*,*,#12473,.F.);
#16843=ORIENTED_EDGE('',*,*,#11984,.F.);
#16844=ORIENTED_EDGE('',*,*,#12475,.F.);
#16845=ORIENTED_EDGE('',*,*,#11935,.F.);
#16846=ORIENTED_EDGE('',*,*,#12476,.F.);
#16847=ORIENTED_EDGE('',*,*,#11933,.F.);
#16848=ORIENTED_EDGE('',*,*,#11930,.F.);
#16849=ORIENTED_EDGE('',*,*,#11927,.F.);
#16850=ORIENTED_EDGE('',*,*,#11924,.F.);
#16851=ORIENTED_EDGE('',*,*,#11921,.F.);
#16852=ORIENTED_EDGE('',*,*,#11918,.F.);
#16853=ORIENTED_EDGE('',*,*,#11915,.F.);
#16854=ORIENTED_EDGE('',*,*,#11912,.F.);
#16855=ORIENTED_EDGE('',*,*,#11909,.F.);
#16856=ORIENTED_EDGE('',*,*,#11906,.F.);
#16857=ORIENTED_EDGE('',*,*,#11903,.F.);
#16858=ORIENTED_EDGE('',*,*,#11900,.F.);
#16859=ORIENTED_EDGE('',*,*,#11897,.F.);
#16860=ORIENTED_EDGE('',*,*,#11894,.F.);
#16861=ORIENTED_EDGE('',*,*,#12471,.F.);
#16862=ORIENTED_EDGE('',*,*,#11889,.F.);
#16863=ORIENTED_EDGE('',*,*,#11896,.F.);
#16864=ORIENTED_EDGE('',*,*,#11899,.F.);
#16865=ORIENTED_EDGE('',*,*,#11902,.F.);
#16866=ORIENTED_EDGE('',*,*,#11905,.F.);
#16867=ORIENTED_EDGE('',*,*,#11908,.F.);
#16868=ORIENTED_EDGE('',*,*,#11911,.F.);
#16869=ORIENTED_EDGE('',*,*,#11914,.F.);
#16870=ORIENTED_EDGE('',*,*,#11917,.F.);
#16871=ORIENTED_EDGE('',*,*,#11920,.F.);
#16872=ORIENTED_EDGE('',*,*,#11923,.F.);
#16873=ORIENTED_EDGE('',*,*,#11926,.F.);
#16874=ORIENTED_EDGE('',*,*,#11929,.F.);
#16875=ORIENTED_EDGE('',*,*,#11932,.F.);
#16876=ORIENTED_EDGE('',*,*,#12477,.F.);
#16877=ORIENTED_EDGE('',*,*,#11937,.F.);
#16878=ORIENTED_EDGE('',*,*,#12478,.F.);
#16879=ORIENTED_EDGE('',*,*,#11982,.T.);
#16880=ORIENTED_EDGE('',*,*,#12474,.T.);
#16881=ORIENTED_EDGE('',*,*,#11980,.T.);
#16882=ORIENTED_EDGE('',*,*,#11977,.T.);
#16883=ORIENTED_EDGE('',*,*,#11974,.T.);
#16884=ORIENTED_EDGE('',*,*,#11971,.T.);
#16885=ORIENTED_EDGE('',*,*,#11968,.T.);
#16886=ORIENTED_EDGE('',*,*,#11965,.T.);
#16887=ORIENTED_EDGE('',*,*,#11962,.T.);
#16888=ORIENTED_EDGE('',*,*,#11959,.T.);
#16889=ORIENTED_EDGE('',*,*,#11956,.T.);
#16890=ORIENTED_EDGE('',*,*,#11953,.T.);
#16891=ORIENTED_EDGE('',*,*,#11950,.T.);
#16892=ORIENTED_EDGE('',*,*,#11947,.T.);
#16893=ORIENTED_EDGE('',*,*,#11944,.T.);
#16894=ORIENTED_EDGE('',*,*,#11941,.T.);
#16895=ORIENTED_EDGE('',*,*,#11934,.T.);
#16896=ORIENTED_EDGE('',*,*,#12477,.T.);
#16897=ORIENTED_EDGE('',*,*,#11931,.F.);
#16898=ORIENTED_EDGE('',*,*,#12476,.T.);
#16899=ORIENTED_EDGE('',*,*,#11793,.F.);
#16900=ORIENTED_EDGE('',*,*,#12479,.T.);
#16901=ORIENTED_EDGE('',*,*,#11843,.T.);
#16902=ORIENTED_EDGE('',*,*,#12480,.T.);
#16903=ORIENTED_EDGE('',*,*,#11796,.F.);
#16904=ORIENTED_EDGE('',*,*,#11884,.T.);
#16905=ORIENTED_EDGE('',*,*,#12481,.T.);
#16906=ORIENTED_EDGE('',*,*,#11881,.F.);
#16907=ORIENTED_EDGE('',*,*,#12482,.F.);
#16908=ORIENTED_EDGE('',*,*,#12480,.F.);
#16909=ORIENTED_EDGE('',*,*,#11842,.F.);
#16910=ORIENTED_EDGE('',*,*,#11846,.F.);
#16911=ORIENTED_EDGE('',*,*,#11849,.F.);
#16912=ORIENTED_EDGE('',*,*,#11852,.F.);
#16913=ORIENTED_EDGE('',*,*,#11855,.F.);
#16914=ORIENTED_EDGE('',*,*,#11858,.F.);
#16915=ORIENTED_EDGE('',*,*,#11861,.F.);
#16916=ORIENTED_EDGE('',*,*,#11864,.F.);
#16917=ORIENTED_EDGE('',*,*,#11867,.F.);
#16918=ORIENTED_EDGE('',*,*,#11870,.F.);
#16919=ORIENTED_EDGE('',*,*,#11873,.F.);
#16920=ORIENTED_EDGE('',*,*,#11876,.F.);
#16921=ORIENTED_EDGE('',*,*,#11879,.F.);
#16922=ORIENTED_EDGE('',*,*,#11882,.F.);
#16923=ORIENTED_EDGE('',*,*,#12481,.F.);
#16924=ORIENTED_EDGE('',*,*,#11887,.F.);
#16925=ORIENTED_EDGE('',*,*,#12483,.F.);
#16926=ORIENTED_EDGE('',*,*,#11838,.F.);
#16927=ORIENTED_EDGE('',*,*,#12484,.F.);
#16928=ORIENTED_EDGE('',*,*,#11836,.F.);
#16929=ORIENTED_EDGE('',*,*,#11833,.F.);
#16930=ORIENTED_EDGE('',*,*,#11830,.F.);
#16931=ORIENTED_EDGE('',*,*,#11827,.F.);
#16932=ORIENTED_EDGE('',*,*,#11824,.F.);
#16933=ORIENTED_EDGE('',*,*,#11821,.F.);
#16934=ORIENTED_EDGE('',*,*,#11818,.F.);
#16935=ORIENTED_EDGE('',*,*,#11815,.F.);
#16936=ORIENTED_EDGE('',*,*,#11812,.F.);
#16937=ORIENTED_EDGE('',*,*,#11809,.F.);
#16938=ORIENTED_EDGE('',*,*,#11806,.F.);
#16939=ORIENTED_EDGE('',*,*,#11803,.F.);
#16940=ORIENTED_EDGE('',*,*,#11800,.F.);
#16941=ORIENTED_EDGE('',*,*,#11797,.F.);
#16942=ORIENTED_EDGE('',*,*,#12479,.F.);
#16943=ORIENTED_EDGE('',*,*,#11792,.F.);
#16944=ORIENTED_EDGE('',*,*,#11799,.F.);
#16945=ORIENTED_EDGE('',*,*,#11802,.F.);
#16946=ORIENTED_EDGE('',*,*,#11805,.F.);
#16947=ORIENTED_EDGE('',*,*,#11808,.F.);
#16948=ORIENTED_EDGE('',*,*,#11811,.F.);
#16949=ORIENTED_EDGE('',*,*,#11814,.F.);
#16950=ORIENTED_EDGE('',*,*,#11817,.F.);
#16951=ORIENTED_EDGE('',*,*,#11820,.F.);
#16952=ORIENTED_EDGE('',*,*,#11823,.F.);
#16953=ORIENTED_EDGE('',*,*,#11826,.F.);
#16954=ORIENTED_EDGE('',*,*,#11829,.F.);
#16955=ORIENTED_EDGE('',*,*,#11832,.F.);
#16956=ORIENTED_EDGE('',*,*,#11835,.F.);
#16957=ORIENTED_EDGE('',*,*,#12485,.F.);
#16958=ORIENTED_EDGE('',*,*,#11840,.F.);
#16959=ORIENTED_EDGE('',*,*,#12486,.F.);
#16960=ORIENTED_EDGE('',*,*,#11885,.T.);
#16961=ORIENTED_EDGE('',*,*,#12482,.T.);
#16962=ORIENTED_EDGE('',*,*,#11883,.T.);
#16963=ORIENTED_EDGE('',*,*,#11880,.T.);
#16964=ORIENTED_EDGE('',*,*,#11877,.T.);
#16965=ORIENTED_EDGE('',*,*,#11874,.T.);
#16966=ORIENTED_EDGE('',*,*,#11871,.T.);
#16967=ORIENTED_EDGE('',*,*,#11868,.T.);
#16968=ORIENTED_EDGE('',*,*,#11865,.T.);
#16969=ORIENTED_EDGE('',*,*,#11862,.T.);
#16970=ORIENTED_EDGE('',*,*,#11859,.T.);
#16971=ORIENTED_EDGE('',*,*,#11856,.T.);
#16972=ORIENTED_EDGE('',*,*,#11853,.T.);
#16973=ORIENTED_EDGE('',*,*,#11850,.T.);
#16974=ORIENTED_EDGE('',*,*,#11847,.T.);
#16975=ORIENTED_EDGE('',*,*,#11844,.T.);
#16976=ORIENTED_EDGE('',*,*,#11837,.T.);
#16977=ORIENTED_EDGE('',*,*,#12485,.T.);
#16978=ORIENTED_EDGE('',*,*,#11834,.F.);
#16979=ORIENTED_EDGE('',*,*,#12484,.T.);
#16980=ORIENTED_EDGE('',*,*,#11696,.F.);
#16981=ORIENTED_EDGE('',*,*,#12487,.T.);
#16982=ORIENTED_EDGE('',*,*,#11746,.T.);
#16983=ORIENTED_EDGE('',*,*,#12488,.T.);
#16984=ORIENTED_EDGE('',*,*,#11699,.F.);
#16985=ORIENTED_EDGE('',*,*,#11787,.T.);
#16986=ORIENTED_EDGE('',*,*,#12489,.T.);
#16987=ORIENTED_EDGE('',*,*,#11784,.F.);
#16988=ORIENTED_EDGE('',*,*,#12490,.F.);
#16989=ORIENTED_EDGE('',*,*,#12488,.F.);
#16990=ORIENTED_EDGE('',*,*,#11745,.F.);
#16991=ORIENTED_EDGE('',*,*,#11749,.F.);
#16992=ORIENTED_EDGE('',*,*,#11752,.F.);
#16993=ORIENTED_EDGE('',*,*,#11755,.F.);
#16994=ORIENTED_EDGE('',*,*,#11758,.F.);
#16995=ORIENTED_EDGE('',*,*,#11761,.F.);
#16996=ORIENTED_EDGE('',*,*,#11764,.F.);
#16997=ORIENTED_EDGE('',*,*,#11767,.F.);
#16998=ORIENTED_EDGE('',*,*,#11770,.F.);
#16999=ORIENTED_EDGE('',*,*,#11773,.F.);
#17000=ORIENTED_EDGE('',*,*,#11776,.F.);
#17001=ORIENTED_EDGE('',*,*,#11779,.F.);
#17002=ORIENTED_EDGE('',*,*,#11782,.F.);
#17003=ORIENTED_EDGE('',*,*,#11785,.F.);
#17004=ORIENTED_EDGE('',*,*,#12489,.F.);
#17005=ORIENTED_EDGE('',*,*,#11790,.F.);
#17006=ORIENTED_EDGE('',*,*,#12491,.F.);
#17007=ORIENTED_EDGE('',*,*,#11741,.F.);
#17008=ORIENTED_EDGE('',*,*,#12492,.F.);
#17009=ORIENTED_EDGE('',*,*,#11739,.F.);
#17010=ORIENTED_EDGE('',*,*,#11736,.F.);
#17011=ORIENTED_EDGE('',*,*,#11733,.F.);
#17012=ORIENTED_EDGE('',*,*,#11730,.F.);
#17013=ORIENTED_EDGE('',*,*,#11727,.F.);
#17014=ORIENTED_EDGE('',*,*,#11724,.F.);
#17015=ORIENTED_EDGE('',*,*,#11721,.F.);
#17016=ORIENTED_EDGE('',*,*,#11718,.F.);
#17017=ORIENTED_EDGE('',*,*,#11715,.F.);
#17018=ORIENTED_EDGE('',*,*,#11712,.F.);
#17019=ORIENTED_EDGE('',*,*,#11709,.F.);
#17020=ORIENTED_EDGE('',*,*,#11706,.F.);
#17021=ORIENTED_EDGE('',*,*,#11703,.F.);
#17022=ORIENTED_EDGE('',*,*,#11700,.F.);
#17023=ORIENTED_EDGE('',*,*,#12487,.F.);
#17024=ORIENTED_EDGE('',*,*,#11695,.F.);
#17025=ORIENTED_EDGE('',*,*,#11702,.F.);
#17026=ORIENTED_EDGE('',*,*,#11705,.F.);
#17027=ORIENTED_EDGE('',*,*,#11708,.F.);
#17028=ORIENTED_EDGE('',*,*,#11711,.F.);
#17029=ORIENTED_EDGE('',*,*,#11714,.F.);
#17030=ORIENTED_EDGE('',*,*,#11717,.F.);
#17031=ORIENTED_EDGE('',*,*,#11720,.F.);
#17032=ORIENTED_EDGE('',*,*,#11723,.F.);
#17033=ORIENTED_EDGE('',*,*,#11726,.F.);
#17034=ORIENTED_EDGE('',*,*,#11729,.F.);
#17035=ORIENTED_EDGE('',*,*,#11732,.F.);
#17036=ORIENTED_EDGE('',*,*,#11735,.F.);
#17037=ORIENTED_EDGE('',*,*,#11738,.F.);
#17038=ORIENTED_EDGE('',*,*,#12493,.F.);
#17039=ORIENTED_EDGE('',*,*,#11743,.F.);
#17040=ORIENTED_EDGE('',*,*,#12494,.F.);
#17041=ORIENTED_EDGE('',*,*,#11788,.T.);
#17042=ORIENTED_EDGE('',*,*,#12490,.T.);
#17043=ORIENTED_EDGE('',*,*,#11786,.T.);
#17044=ORIENTED_EDGE('',*,*,#11783,.T.);
#17045=ORIENTED_EDGE('',*,*,#11780,.T.);
#17046=ORIENTED_EDGE('',*,*,#11777,.T.);
#17047=ORIENTED_EDGE('',*,*,#11774,.T.);
#17048=ORIENTED_EDGE('',*,*,#11771,.T.);
#17049=ORIENTED_EDGE('',*,*,#11768,.T.);
#17050=ORIENTED_EDGE('',*,*,#11765,.T.);
#17051=ORIENTED_EDGE('',*,*,#11762,.T.);
#17052=ORIENTED_EDGE('',*,*,#11759,.T.);
#17053=ORIENTED_EDGE('',*,*,#11756,.T.);
#17054=ORIENTED_EDGE('',*,*,#11753,.T.);
#17055=ORIENTED_EDGE('',*,*,#11750,.T.);
#17056=ORIENTED_EDGE('',*,*,#11747,.T.);
#17057=ORIENTED_EDGE('',*,*,#11740,.T.);
#17058=ORIENTED_EDGE('',*,*,#12493,.T.);
#17059=ORIENTED_EDGE('',*,*,#11737,.F.);
#17060=ORIENTED_EDGE('',*,*,#12492,.T.);
#17061=ORIENTED_EDGE('',*,*,#11599,.F.);
#17062=ORIENTED_EDGE('',*,*,#12495,.T.);
#17063=ORIENTED_EDGE('',*,*,#11649,.T.);
#17064=ORIENTED_EDGE('',*,*,#12496,.T.);
#17065=ORIENTED_EDGE('',*,*,#11602,.F.);
#17066=ORIENTED_EDGE('',*,*,#11690,.T.);
#17067=ORIENTED_EDGE('',*,*,#12497,.T.);
#17068=ORIENTED_EDGE('',*,*,#11687,.F.);
#17069=ORIENTED_EDGE('',*,*,#12498,.F.);
#17070=ORIENTED_EDGE('',*,*,#12496,.F.);
#17071=ORIENTED_EDGE('',*,*,#11648,.F.);
#17072=ORIENTED_EDGE('',*,*,#11652,.F.);
#17073=ORIENTED_EDGE('',*,*,#11655,.F.);
#17074=ORIENTED_EDGE('',*,*,#11658,.F.);
#17075=ORIENTED_EDGE('',*,*,#11661,.F.);
#17076=ORIENTED_EDGE('',*,*,#11664,.F.);
#17077=ORIENTED_EDGE('',*,*,#11667,.F.);
#17078=ORIENTED_EDGE('',*,*,#11670,.F.);
#17079=ORIENTED_EDGE('',*,*,#11673,.F.);
#17080=ORIENTED_EDGE('',*,*,#11676,.F.);
#17081=ORIENTED_EDGE('',*,*,#11679,.F.);
#17082=ORIENTED_EDGE('',*,*,#11682,.F.);
#17083=ORIENTED_EDGE('',*,*,#11685,.F.);
#17084=ORIENTED_EDGE('',*,*,#11688,.F.);
#17085=ORIENTED_EDGE('',*,*,#12497,.F.);
#17086=ORIENTED_EDGE('',*,*,#11693,.F.);
#17087=ORIENTED_EDGE('',*,*,#12499,.F.);
#17088=ORIENTED_EDGE('',*,*,#11644,.F.);
#17089=ORIENTED_EDGE('',*,*,#12500,.F.);
#17090=ORIENTED_EDGE('',*,*,#11642,.F.);
#17091=ORIENTED_EDGE('',*,*,#11639,.F.);
#17092=ORIENTED_EDGE('',*,*,#11636,.F.);
#17093=ORIENTED_EDGE('',*,*,#11633,.F.);
#17094=ORIENTED_EDGE('',*,*,#11630,.F.);
#17095=ORIENTED_EDGE('',*,*,#11627,.F.);
#17096=ORIENTED_EDGE('',*,*,#11624,.F.);
#17097=ORIENTED_EDGE('',*,*,#11621,.F.);
#17098=ORIENTED_EDGE('',*,*,#11618,.F.);
#17099=ORIENTED_EDGE('',*,*,#11615,.F.);
#17100=ORIENTED_EDGE('',*,*,#11612,.F.);
#17101=ORIENTED_EDGE('',*,*,#11609,.F.);
#17102=ORIENTED_EDGE('',*,*,#11606,.F.);
#17103=ORIENTED_EDGE('',*,*,#11603,.F.);
#17104=ORIENTED_EDGE('',*,*,#12495,.F.);
#17105=ORIENTED_EDGE('',*,*,#11598,.F.);
#17106=ORIENTED_EDGE('',*,*,#11605,.F.);
#17107=ORIENTED_EDGE('',*,*,#11608,.F.);
#17108=ORIENTED_EDGE('',*,*,#11611,.F.);
#17109=ORIENTED_EDGE('',*,*,#11614,.F.);
#17110=ORIENTED_EDGE('',*,*,#11617,.F.);
#17111=ORIENTED_EDGE('',*,*,#11620,.F.);
#17112=ORIENTED_EDGE('',*,*,#11623,.F.);
#17113=ORIENTED_EDGE('',*,*,#11626,.F.);
#17114=ORIENTED_EDGE('',*,*,#11629,.F.);
#17115=ORIENTED_EDGE('',*,*,#11632,.F.);
#17116=ORIENTED_EDGE('',*,*,#11635,.F.);
#17117=ORIENTED_EDGE('',*,*,#11638,.F.);
#17118=ORIENTED_EDGE('',*,*,#11641,.F.);
#17119=ORIENTED_EDGE('',*,*,#12501,.F.);
#17120=ORIENTED_EDGE('',*,*,#11646,.F.);
#17121=ORIENTED_EDGE('',*,*,#12502,.F.);
#17122=ORIENTED_EDGE('',*,*,#11691,.T.);
#17123=ORIENTED_EDGE('',*,*,#12498,.T.);
#17124=ORIENTED_EDGE('',*,*,#11689,.T.);
#17125=ORIENTED_EDGE('',*,*,#11686,.T.);
#17126=ORIENTED_EDGE('',*,*,#11683,.T.);
#17127=ORIENTED_EDGE('',*,*,#11680,.T.);
#17128=ORIENTED_EDGE('',*,*,#11677,.T.);
#17129=ORIENTED_EDGE('',*,*,#11674,.T.);
#17130=ORIENTED_EDGE('',*,*,#11671,.T.);
#17131=ORIENTED_EDGE('',*,*,#11668,.T.);
#17132=ORIENTED_EDGE('',*,*,#11665,.T.);
#17133=ORIENTED_EDGE('',*,*,#11662,.T.);
#17134=ORIENTED_EDGE('',*,*,#11659,.T.);
#17135=ORIENTED_EDGE('',*,*,#11656,.T.);
#17136=ORIENTED_EDGE('',*,*,#11653,.T.);
#17137=ORIENTED_EDGE('',*,*,#11650,.T.);
#17138=ORIENTED_EDGE('',*,*,#11643,.T.);
#17139=ORIENTED_EDGE('',*,*,#12501,.T.);
#17140=ORIENTED_EDGE('',*,*,#11640,.F.);
#17141=ORIENTED_EDGE('',*,*,#12500,.T.);
#17142=ORIENTED_EDGE('',*,*,#12183,.F.);
#17143=ORIENTED_EDGE('',*,*,#12086,.F.);
#17144=ORIENTED_EDGE('',*,*,#12280,.F.);
#17145=ORIENTED_EDGE('',*,*,#11892,.F.);
#17146=ORIENTED_EDGE('',*,*,#11795,.F.);
#17147=ORIENTED_EDGE('',*,*,#11601,.F.);
#17148=ORIENTED_EDGE('',*,*,#11989,.F.);
#17149=ORIENTED_EDGE('',*,*,#11698,.F.);
#17150=ORIENTED_EDGE('',*,*,#12503,.F.);
#17151=ORIENTED_EDGE('',*,*,#12504,.T.);
#17152=ORIENTED_EDGE('',*,*,#12505,.F.);
#17153=ORIENTED_EDGE('',*,*,#12504,.F.);
#17154=ORIENTED_EDGE('',*,*,#12506,.F.);
#17155=ORIENTED_EDGE('',*,*,#12507,.T.);
#17156=ORIENTED_EDGE('',*,*,#12508,.F.);
#17157=ORIENTED_EDGE('',*,*,#12507,.F.);
#17158=ORIENTED_EDGE('',*,*,#12509,.F.);
#17159=ORIENTED_EDGE('',*,*,#12510,.T.);
#17160=ORIENTED_EDGE('',*,*,#12511,.F.);
#17161=ORIENTED_EDGE('',*,*,#12510,.F.);
#17162=ORIENTED_EDGE('',*,*,#12512,.F.);
#17163=ORIENTED_EDGE('',*,*,#12513,.T.);
#17164=ORIENTED_EDGE('',*,*,#12514,.F.);
#17165=ORIENTED_EDGE('',*,*,#12513,.F.);
#17166=ORIENTED_EDGE('',*,*,#12515,.F.);
#17167=ORIENTED_EDGE('',*,*,#12516,.T.);
#17168=ORIENTED_EDGE('',*,*,#12517,.T.);
#17169=ORIENTED_EDGE('',*,*,#12516,.F.);
#17170=ORIENTED_EDGE('',*,*,#12517,.F.);
#17171=ORIENTED_EDGE('',*,*,#12518,.F.);
#17172=ORIENTED_EDGE('',*,*,#12519,.F.);
#17173=ORIENTED_EDGE('',*,*,#12520,.T.);
#17174=ORIENTED_EDGE('',*,*,#12386,.T.);
#17175=ORIENTED_EDGE('',*,*,#12388,.T.);
#17176=ORIENTED_EDGE('',*,*,#12521,.T.);
#17177=ORIENTED_EDGE('',*,*,#12408,.T.);
#17178=ORIENTED_EDGE('',*,*,#12410,.T.);
#17179=ORIENTED_EDGE('',*,*,#12522,.T.);
#17180=ORIENTED_EDGE('',*,*,#12430,.T.);
#17181=ORIENTED_EDGE('',*,*,#12432,.T.);
#17182=ORIENTED_EDGE('',*,*,#12523,.T.);
#17183=ORIENTED_EDGE('',*,*,#12524,.F.);
#17184=ORIENTED_EDGE('',*,*,#12523,.F.);
#17185=ORIENTED_EDGE('',*,*,#12431,.T.);
#17186=ORIENTED_EDGE('',*,*,#12522,.F.);
#17187=ORIENTED_EDGE('',*,*,#12409,.T.);
#17188=ORIENTED_EDGE('',*,*,#12521,.F.);
#17189=ORIENTED_EDGE('',*,*,#12387,.T.);
#17190=ORIENTED_EDGE('',*,*,#12520,.F.);
#17191=ORIENTED_EDGE('',*,*,#12375,.T.);
#17192=ORIENTED_EDGE('',*,*,#12376,.T.);
#17193=ORIENTED_EDGE('',*,*,#12381,.T.);
#17194=ORIENTED_EDGE('',*,*,#12382,.T.);
#17195=ORIENTED_EDGE('',*,*,#12393,.T.);
#17196=ORIENTED_EDGE('',*,*,#12397,.T.);
#17197=ORIENTED_EDGE('',*,*,#12398,.T.);
#17198=ORIENTED_EDGE('',*,*,#12403,.T.);
#17199=ORIENTED_EDGE('',*,*,#12404,.T.);
#17200=ORIENTED_EDGE('',*,*,#12415,.T.);
#17201=ORIENTED_EDGE('',*,*,#12419,.T.);
#17202=ORIENTED_EDGE('',*,*,#12420,.T.);
#17203=ORIENTED_EDGE('',*,*,#12425,.T.);
#17204=ORIENTED_EDGE('',*,*,#12426,.T.);
#17205=ORIENTED_EDGE('',*,*,#12437,.T.);
#17206=ORIENTED_EDGE('',*,*,#12525,.F.);
#17207=ORIENTED_EDGE('',*,*,#12526,.T.);
#17208=ORIENTED_EDGE('',*,*,#12383,.T.);
#17209=ORIENTED_EDGE('',*,*,#12527,.T.);
#17210=ORIENTED_EDGE('',*,*,#12405,.T.);
#17211=ORIENTED_EDGE('',*,*,#12528,.T.);
#17212=ORIENTED_EDGE('',*,*,#12427,.T.);
#17213=ORIENTED_EDGE('',*,*,#12529,.T.);
#17214=ORIENTED_EDGE('',*,*,#12530,.F.);
#17215=ORIENTED_EDGE('',*,*,#12529,.F.);
#17216=ORIENTED_EDGE('',*,*,#12433,.T.);
#17217=ORIENTED_EDGE('',*,*,#12428,.T.);
#17218=ORIENTED_EDGE('',*,*,#12528,.F.);
#17219=ORIENTED_EDGE('',*,*,#12411,.T.);
#17220=ORIENTED_EDGE('',*,*,#12406,.T.);
#17221=ORIENTED_EDGE('',*,*,#12527,.F.);
#17222=ORIENTED_EDGE('',*,*,#12389,.T.);
#17223=ORIENTED_EDGE('',*,*,#12384,.T.);
#17224=ORIENTED_EDGE('',*,*,#12526,.F.);
#17225=ORIENTED_EDGE('',*,*,#12373,.T.);
#17226=ORIENTED_EDGE('',*,*,#12377,.T.);
#17227=ORIENTED_EDGE('',*,*,#12378,.T.);
#17228=ORIENTED_EDGE('',*,*,#12379,.T.);
#17229=ORIENTED_EDGE('',*,*,#12390,.T.);
#17230=ORIENTED_EDGE('',*,*,#12394,.T.);
#17231=ORIENTED_EDGE('',*,*,#12391,.T.);
#17232=ORIENTED_EDGE('',*,*,#12395,.T.);
#17233=ORIENTED_EDGE('',*,*,#12399,.T.);
#17234=ORIENTED_EDGE('',*,*,#12400,.T.);
#17235=ORIENTED_EDGE('',*,*,#12401,.T.);
#17236=ORIENTED_EDGE('',*,*,#12412,.T.);
#17237=ORIENTED_EDGE('',*,*,#12416,.T.);
#17238=ORIENTED_EDGE('',*,*,#12413,.T.);
#17239=ORIENTED_EDGE('',*,*,#12417,.T.);
#17240=ORIENTED_EDGE('',*,*,#12421,.T.);
#17241=ORIENTED_EDGE('',*,*,#12422,.T.);
#17242=ORIENTED_EDGE('',*,*,#12423,.T.);
#17243=ORIENTED_EDGE('',*,*,#12434,.T.);
#17244=ORIENTED_EDGE('',*,*,#12438,.T.);
#17245=ORIENTED_EDGE('',*,*,#12435,.T.);
#17246=ORIENTED_EDGE('',*,*,#12525,.T.);
#17247=ORIENTED_EDGE('',*,*,#12454,.T.);
#17248=ORIENTED_EDGE('',*,*,#12227,.T.);
#17249=ORIENTED_EDGE('',*,*,#12451,.T.);
#17250=ORIENTED_EDGE('',*,*,#12274,.T.);
#17251=ORIENTED_EDGE('',*,*,#12470,.T.);
#17252=ORIENTED_EDGE('',*,*,#12033,.T.);
#17253=ORIENTED_EDGE('',*,*,#12467,.T.);
#17254=ORIENTED_EDGE('',*,*,#12080,.T.);
#17255=ORIENTED_EDGE('',*,*,#12486,.T.);
#17256=ORIENTED_EDGE('',*,*,#11839,.T.);
#17257=ORIENTED_EDGE('',*,*,#12483,.T.);
#17258=ORIENTED_EDGE('',*,*,#11886,.T.);
#17259=ORIENTED_EDGE('',*,*,#12502,.T.);
#17260=ORIENTED_EDGE('',*,*,#11645,.T.);
#17261=ORIENTED_EDGE('',*,*,#12499,.T.);
#17262=ORIENTED_EDGE('',*,*,#11692,.T.);
#17263=ORIENTED_EDGE('',*,*,#12519,.T.);
#17264=ORIENTED_EDGE('',*,*,#12494,.T.);
#17265=ORIENTED_EDGE('',*,*,#11742,.T.);
#17266=ORIENTED_EDGE('',*,*,#12491,.T.);
#17267=ORIENTED_EDGE('',*,*,#11789,.T.);
#17268=ORIENTED_EDGE('',*,*,#12478,.T.);
#17269=ORIENTED_EDGE('',*,*,#11936,.T.);
#17270=ORIENTED_EDGE('',*,*,#12475,.T.);
#17271=ORIENTED_EDGE('',*,*,#11983,.T.);
#17272=ORIENTED_EDGE('',*,*,#12462,.T.);
#17273=ORIENTED_EDGE('',*,*,#12130,.T.);
#17274=ORIENTED_EDGE('',*,*,#12459,.T.);
#17275=ORIENTED_EDGE('',*,*,#12177,.T.);
#17276=ORIENTED_EDGE('',*,*,#12446,.T.);
#17277=ORIENTED_EDGE('',*,*,#12324,.T.);
#17278=ORIENTED_EDGE('',*,*,#12443,.T.);
#17279=ORIENTED_EDGE('',*,*,#12371,.T.);
#17280=ORIENTED_EDGE('',*,*,#12531,.T.);
#17281=ORIENTED_EDGE('',*,*,#12530,.T.);
#17282=ORIENTED_EDGE('',*,*,#12512,.T.);
#17283=ORIENTED_EDGE('',*,*,#12509,.T.);
#17284=ORIENTED_EDGE('',*,*,#12506,.T.);
#17285=ORIENTED_EDGE('',*,*,#12503,.T.);
#17286=ORIENTED_EDGE('',*,*,#12518,.T.);
#17287=ORIENTED_EDGE('',*,*,#12532,.T.);
#17288=ORIENTED_EDGE('',*,*,#12533,.T.);
#17289=ORIENTED_EDGE('',*,*,#12532,.F.);
#17290=ORIENTED_EDGE('',*,*,#12531,.F.);
#17291=ORIENTED_EDGE('',*,*,#12534,.T.);
#17292=ORIENTED_EDGE('',*,*,#12535,.T.);
#17293=ORIENTED_EDGE('',*,*,#12534,.F.);
#17294=ORIENTED_EDGE('',*,*,#12524,.T.);
#17295=ORIENTED_EDGE('',*,*,#12515,.T.);
#17296=ORIENTED_EDGE('',*,*,#12535,.F.);
#17297=ORIENTED_EDGE('',*,*,#12533,.F.);
#17298=ORIENTED_EDGE('',*,*,#12514,.T.);
#17299=ORIENTED_EDGE('',*,*,#12511,.T.);
#17300=ORIENTED_EDGE('',*,*,#12508,.T.);
#17301=ORIENTED_EDGE('',*,*,#12505,.T.);
#17302=ORIENTED_EDGE('',*,*,#12536,.F.);
#17303=ORIENTED_EDGE('',*,*,#12537,.T.);
#17304=ORIENTED_EDGE('',*,*,#12538,.T.);
#17305=ORIENTED_EDGE('',*,*,#12537,.F.);
#17306=ORIENTED_EDGE('',*,*,#12539,.F.);
#17307=ORIENTED_EDGE('',*,*,#12538,.F.);
#17308=ORIENTED_EDGE('',*,*,#12540,.F.);
#17309=ORIENTED_EDGE('',*,*,#12541,.F.);
#17310=ORIENTED_EDGE('',*,*,#12542,.T.);
#17311=ORIENTED_EDGE('',*,*,#12543,.T.);
#17312=ORIENTED_EDGE('',*,*,#12542,.F.);
#17313=ORIENTED_EDGE('',*,*,#12543,.F.);
#17314=ORIENTED_EDGE('',*,*,#12544,.F.);
#17315=ORIENTED_EDGE('',*,*,#12545,.F.);
#17316=ORIENTED_EDGE('',*,*,#12546,.T.);
#17317=ORIENTED_EDGE('',*,*,#12547,.T.);
#17318=ORIENTED_EDGE('',*,*,#12546,.F.);
#17319=ORIENTED_EDGE('',*,*,#12548,.F.);
#17320=ORIENTED_EDGE('',*,*,#12547,.F.);
#17321=ORIENTED_EDGE('',*,*,#12549,.F.);
#17322=ORIENTED_EDGE('',*,*,#12550,.F.);
#17323=ORIENTED_EDGE('',*,*,#12551,.T.);
#17324=ORIENTED_EDGE('',*,*,#12552,.T.);
#17325=ORIENTED_EDGE('',*,*,#12551,.F.);
#17326=ORIENTED_EDGE('',*,*,#12553,.F.);
#17327=ORIENTED_EDGE('',*,*,#12552,.F.);
#17328=ORIENTED_EDGE('',*,*,#12554,.F.);
#17329=ORIENTED_EDGE('',*,*,#12555,.T.);
#17330=ORIENTED_EDGE('',*,*,#12556,.T.);
#17331=ORIENTED_EDGE('',*,*,#12555,.F.);
#17332=ORIENTED_EDGE('',*,*,#12557,.F.);
#17333=ORIENTED_EDGE('',*,*,#12558,.T.);
#17334=ORIENTED_EDGE('',*,*,#12544,.T.);
#17335=ORIENTED_EDGE('',*,*,#12559,.T.);
#17336=ORIENTED_EDGE('',*,*,#12560,.T.);
#17337=ORIENTED_EDGE('',*,*,#12559,.F.);
#17338=ORIENTED_EDGE('',*,*,#12548,.T.);
#17339=ORIENTED_EDGE('',*,*,#12545,.T.);
#17340=ORIENTED_EDGE('',*,*,#12558,.F.);
#17341=ORIENTED_EDGE('',*,*,#12536,.T.);
#17342=ORIENTED_EDGE('',*,*,#12539,.T.);
#17343=ORIENTED_EDGE('',*,*,#12540,.T.);
#17344=ORIENTED_EDGE('',*,*,#12541,.T.);
#17345=ORIENTED_EDGE('',*,*,#12549,.T.);
#17346=ORIENTED_EDGE('',*,*,#12553,.T.);
#17347=ORIENTED_EDGE('',*,*,#12550,.T.);
#17348=ORIENTED_EDGE('',*,*,#12557,.T.);
#17349=ORIENTED_EDGE('',*,*,#12554,.T.);
#17350=ORIENTED_EDGE('',*,*,#12560,.F.);
#17351=ORIENTED_EDGE('',*,*,#12556,.F.);
#17352=ORIENTED_EDGE('',*,*,#12561,.F.);
#17353=ORIENTED_EDGE('',*,*,#12562,.T.);
#17354=ORIENTED_EDGE('',*,*,#12563,.F.);
#17355=ORIENTED_EDGE('',*,*,#12562,.F.);
#17356=ORIENTED_EDGE('',*,*,#12564,.F.);
#17357=ORIENTED_EDGE('',*,*,#12565,.T.);
#17358=ORIENTED_EDGE('',*,*,#12566,.F.);
#17359=ORIENTED_EDGE('',*,*,#12565,.F.);
#17360=ORIENTED_EDGE('',*,*,#12567,.F.);
#17361=ORIENTED_EDGE('',*,*,#12568,.T.);
#17362=ORIENTED_EDGE('',*,*,#12569,.F.);
#17363=ORIENTED_EDGE('',*,*,#12568,.F.);
#17364=ORIENTED_EDGE('',*,*,#12570,.F.);
#17365=ORIENTED_EDGE('',*,*,#12571,.T.);
#17366=ORIENTED_EDGE('',*,*,#12572,.F.);
#17367=ORIENTED_EDGE('',*,*,#12571,.F.);
#17368=ORIENTED_EDGE('',*,*,#12573,.F.);
#17369=ORIENTED_EDGE('',*,*,#12574,.T.);
#17370=ORIENTED_EDGE('',*,*,#12575,.F.);
#17371=ORIENTED_EDGE('',*,*,#12574,.F.);
#17372=ORIENTED_EDGE('',*,*,#12576,.F.);
#17373=ORIENTED_EDGE('',*,*,#12577,.T.);
#17374=ORIENTED_EDGE('',*,*,#12578,.F.);
#17375=ORIENTED_EDGE('',*,*,#12577,.F.);
#17376=ORIENTED_EDGE('',*,*,#12579,.F.);
#17377=ORIENTED_EDGE('',*,*,#12580,.T.);
#17378=ORIENTED_EDGE('',*,*,#12581,.F.);
#17379=ORIENTED_EDGE('',*,*,#12580,.F.);
#17380=ORIENTED_EDGE('',*,*,#12582,.F.);
#17381=ORIENTED_EDGE('',*,*,#12583,.T.);
#17382=ORIENTED_EDGE('',*,*,#12584,.F.);
#17383=ORIENTED_EDGE('',*,*,#12583,.F.);
#17384=ORIENTED_EDGE('',*,*,#12585,.F.);
#17385=ORIENTED_EDGE('',*,*,#12586,.T.);
#17386=ORIENTED_EDGE('',*,*,#12587,.T.);
#17387=ORIENTED_EDGE('',*,*,#12586,.F.);
#17388=ORIENTED_EDGE('',*,*,#12588,.F.);
#17389=ORIENTED_EDGE('',*,*,#12589,.T.);
#17390=ORIENTED_EDGE('',*,*,#12590,.T.);
#17391=ORIENTED_EDGE('',*,*,#12589,.F.);
#17392=ORIENTED_EDGE('',*,*,#12588,.T.);
#17393=ORIENTED_EDGE('',*,*,#12585,.T.);
#17394=ORIENTED_EDGE('',*,*,#12582,.T.);
#17395=ORIENTED_EDGE('',*,*,#12579,.T.);
#17396=ORIENTED_EDGE('',*,*,#12576,.T.);
#17397=ORIENTED_EDGE('',*,*,#12573,.T.);
#17398=ORIENTED_EDGE('',*,*,#12570,.T.);
#17399=ORIENTED_EDGE('',*,*,#12567,.T.);
#17400=ORIENTED_EDGE('',*,*,#12564,.T.);
#17401=ORIENTED_EDGE('',*,*,#12561,.T.);
#17402=ORIENTED_EDGE('',*,*,#12590,.F.);
#17403=ORIENTED_EDGE('',*,*,#12587,.F.);
#17404=ORIENTED_EDGE('',*,*,#12584,.T.);
#17405=ORIENTED_EDGE('',*,*,#12581,.T.);
#17406=ORIENTED_EDGE('',*,*,#12578,.T.);
#17407=ORIENTED_EDGE('',*,*,#12575,.T.);
#17408=ORIENTED_EDGE('',*,*,#12572,.T.);
#17409=ORIENTED_EDGE('',*,*,#12569,.T.);
#17410=ORIENTED_EDGE('',*,*,#12566,.T.);
#17411=ORIENTED_EDGE('',*,*,#12563,.T.);
#17412=ORIENTED_EDGE('',*,*,#12591,.F.);
#17413=ORIENTED_EDGE('',*,*,#12592,.T.);
#17414=ORIENTED_EDGE('',*,*,#12593,.F.);
#17415=ORIENTED_EDGE('',*,*,#12594,.T.);
#17416=ORIENTED_EDGE('',*,*,#12595,.F.);
#17417=ORIENTED_EDGE('',*,*,#12594,.F.);
#17418=ORIENTED_EDGE('',*,*,#12596,.F.);
#17419=ORIENTED_EDGE('',*,*,#12597,.F.);
#17420=ORIENTED_EDGE('',*,*,#12598,.F.);
#17421=ORIENTED_EDGE('',*,*,#12597,.T.);
#17422=ORIENTED_EDGE('',*,*,#12599,.T.);
#17423=ORIENTED_EDGE('',*,*,#12600,.T.);
#17424=ORIENTED_EDGE('',*,*,#12596,.T.);
#17425=ORIENTED_EDGE('',*,*,#12593,.T.);
#17426=ORIENTED_EDGE('',*,*,#12601,.T.);
#17427=ORIENTED_EDGE('',*,*,#12599,.F.);
#17428=ORIENTED_EDGE('',*,*,#12602,.F.);
#17429=ORIENTED_EDGE('',*,*,#12600,.F.);
#17430=ORIENTED_EDGE('',*,*,#12601,.F.);
#17431=ORIENTED_EDGE('',*,*,#12592,.F.);
#17432=ORIENTED_EDGE('',*,*,#12603,.T.);
#17433=ORIENTED_EDGE('',*,*,#12604,.T.);
#17434=ORIENTED_EDGE('',*,*,#12605,.F.);
#17435=ORIENTED_EDGE('',*,*,#12604,.F.);
#17436=ORIENTED_EDGE('',*,*,#12606,.F.);
#17437=ORIENTED_EDGE('',*,*,#12603,.F.);
#17438=ORIENTED_EDGE('',*,*,#12607,.F.);
#17439=ORIENTED_EDGE('',*,*,#12605,.T.);
#17440=ORIENTED_EDGE('',*,*,#12608,.F.);
#17441=ORIENTED_EDGE('',*,*,#12609,.T.);
#17442=ORIENTED_EDGE('',*,*,#12607,.T.);
#17443=ORIENTED_EDGE('',*,*,#12609,.F.);
#17444=ORIENTED_EDGE('',*,*,#12610,.T.);
#17445=ORIENTED_EDGE('',*,*,#12611,.T.);
#17446=ORIENTED_EDGE('',*,*,#12612,.F.);
#17447=ORIENTED_EDGE('',*,*,#12611,.F.);
#17448=ORIENTED_EDGE('',*,*,#12613,.F.);
#17449=ORIENTED_EDGE('',*,*,#12610,.F.);
#17450=ORIENTED_EDGE('',*,*,#12614,.F.);
#17451=ORIENTED_EDGE('',*,*,#12612,.T.);
#17452=ORIENTED_EDGE('',*,*,#12615,.T.);
#17453=ORIENTED_EDGE('',*,*,#12616,.T.);
#17454=ORIENTED_EDGE('',*,*,#12614,.T.);
#17455=ORIENTED_EDGE('',*,*,#12616,.F.);
#17456=ORIENTED_EDGE('',*,*,#12617,.T.);
#17457=ORIENTED_EDGE('',*,*,#12618,.F.);
#17458=ORIENTED_EDGE('',*,*,#12619,.F.);
#17459=ORIENTED_EDGE('',*,*,#12620,.F.);
#17460=ORIENTED_EDGE('',*,*,#12617,.F.);
#17461=ORIENTED_EDGE('',*,*,#12621,.T.);
#17462=ORIENTED_EDGE('',*,*,#12619,.T.);
#17463=ORIENTED_EDGE('',*,*,#12621,.F.);
#17464=ORIENTED_EDGE('',*,*,#12620,.T.);
#17465=ORIENTED_EDGE('',*,*,#12622,.T.);
#17466=ORIENTED_EDGE('',*,*,#12623,.F.);
#17467=ORIENTED_EDGE('',*,*,#12622,.F.);
#17468=ORIENTED_EDGE('',*,*,#12624,.T.);
#17469=ORIENTED_EDGE('',*,*,#12625,.F.);
#17470=ORIENTED_EDGE('',*,*,#12626,.F.);
#17471=ORIENTED_EDGE('',*,*,#12615,.F.);
#17472=ORIENTED_EDGE('',*,*,#12624,.F.);
#17473=ORIENTED_EDGE('',*,*,#12627,.T.);
#17474=ORIENTED_EDGE('',*,*,#12626,.T.);
#17475=ORIENTED_EDGE('',*,*,#12627,.F.);
#17476=ORIENTED_EDGE('',*,*,#12613,.T.);
#17477=ORIENTED_EDGE('',*,*,#12628,.T.);
#17478=ORIENTED_EDGE('',*,*,#12629,.T.);
#17479=ORIENTED_EDGE('',*,*,#12628,.F.);
#17480=ORIENTED_EDGE('',*,*,#12606,.T.);
#17481=ORIENTED_EDGE('',*,*,#12630,.T.);
#17482=ORIENTED_EDGE('',*,*,#12618,.T.);
#17483=ORIENTED_EDGE('',*,*,#12630,.F.);
#17484=ORIENTED_EDGE('',*,*,#12598,.T.);
#17485=ORIENTED_EDGE('',*,*,#12602,.T.);
#17486=ORIENTED_EDGE('',*,*,#12591,.T.);
#17487=ORIENTED_EDGE('',*,*,#12595,.T.);
#17488=ORIENTED_EDGE('',*,*,#12608,.T.);
#17489=ORIENTED_EDGE('',*,*,#12631,.F.);
#17490=ORIENTED_EDGE('',*,*,#12632,.T.);
#17491=ORIENTED_EDGE('',*,*,#12633,.T.);
#17492=ORIENTED_EDGE('',*,*,#12632,.F.);
#17493=ORIENTED_EDGE('',*,*,#12633,.F.);
#17494=ORIENTED_EDGE('',*,*,#12634,.F.);
#17495=ORIENTED_EDGE('',*,*,#12635,.T.);
#17496=ORIENTED_EDGE('',*,*,#12625,.T.);
#17497=ORIENTED_EDGE('',*,*,#12635,.F.);
#17498=ORIENTED_EDGE('',*,*,#12634,.T.);
#17499=ORIENTED_EDGE('',*,*,#12623,.T.);
#17500=ORIENTED_EDGE('',*,*,#12629,.F.);
#17501=ORIENTED_EDGE('',*,*,#12631,.T.);
#17502=ORIENTED_EDGE('',*,*,#12636,.F.);
#17503=ORIENTED_EDGE('',*,*,#12637,.T.);
#17504=ORIENTED_EDGE('',*,*,#12638,.T.);
#17505=ORIENTED_EDGE('',*,*,#12637,.F.);
#17506=ORIENTED_EDGE('',*,*,#12639,.F.);
#17507=ORIENTED_EDGE('',*,*,#12638,.F.);
#17508=ORIENTED_EDGE('',*,*,#12640,.F.);
#17509=ORIENTED_EDGE('',*,*,#12641,.F.);
#17510=ORIENTED_EDGE('',*,*,#12642,.T.);
#17511=ORIENTED_EDGE('',*,*,#12643,.T.);
#17512=ORIENTED_EDGE('',*,*,#12642,.F.);
#17513=ORIENTED_EDGE('',*,*,#12643,.F.);
#17514=ORIENTED_EDGE('',*,*,#12644,.F.);
#17515=ORIENTED_EDGE('',*,*,#12645,.F.);
#17516=ORIENTED_EDGE('',*,*,#12646,.T.);
#17517=ORIENTED_EDGE('',*,*,#12647,.T.);
#17518=ORIENTED_EDGE('',*,*,#12646,.F.);
#17519=ORIENTED_EDGE('',*,*,#12648,.F.);
#17520=ORIENTED_EDGE('',*,*,#12647,.F.);
#17521=ORIENTED_EDGE('',*,*,#12649,.F.);
#17522=ORIENTED_EDGE('',*,*,#12650,.F.);
#17523=ORIENTED_EDGE('',*,*,#12651,.T.);
#17524=ORIENTED_EDGE('',*,*,#12652,.T.);
#17525=ORIENTED_EDGE('',*,*,#12651,.F.);
#17526=ORIENTED_EDGE('',*,*,#12653,.F.);
#17527=ORIENTED_EDGE('',*,*,#12652,.F.);
#17528=ORIENTED_EDGE('',*,*,#12654,.T.);
#17529=ORIENTED_EDGE('',*,*,#12655,.T.);
#17530=ORIENTED_EDGE('',*,*,#12656,.T.);
#17531=ORIENTED_EDGE('',*,*,#12657,.T.);
#17532=ORIENTED_EDGE('',*,*,#12655,.F.);
#17533=ORIENTED_EDGE('',*,*,#12658,.F.);
#17534=ORIENTED_EDGE('',*,*,#12659,.F.);
#17535=ORIENTED_EDGE('',*,*,#12660,.F.);
#17536=ORIENTED_EDGE('',*,*,#12661,.T.);
#17537=ORIENTED_EDGE('',*,*,#12662,.T.);
#17538=ORIENTED_EDGE('',*,*,#12663,.T.);
#17539=ORIENTED_EDGE('',*,*,#12664,.T.);
#17540=ORIENTED_EDGE('',*,*,#12657,.F.);
#17541=ORIENTED_EDGE('',*,*,#12665,.F.);
#17542=ORIENTED_EDGE('',*,*,#12662,.F.);
#17543=ORIENTED_EDGE('',*,*,#12666,.F.);
#17544=ORIENTED_EDGE('',*,*,#12667,.T.);
#17545=ORIENTED_EDGE('',*,*,#12668,.T.);
#17546=ORIENTED_EDGE('',*,*,#12669,.T.);
#17547=ORIENTED_EDGE('',*,*,#12670,.T.);
#17548=ORIENTED_EDGE('',*,*,#12668,.F.);
#17549=ORIENTED_EDGE('',*,*,#12671,.F.);
#17550=ORIENTED_EDGE('',*,*,#12672,.F.);
#17551=ORIENTED_EDGE('',*,*,#12673,.F.);
#17552=ORIENTED_EDGE('',*,*,#12674,.T.);
#17553=ORIENTED_EDGE('',*,*,#12675,.T.);
#17554=ORIENTED_EDGE('',*,*,#12676,.T.);
#17555=ORIENTED_EDGE('',*,*,#12677,.T.);
#17556=ORIENTED_EDGE('',*,*,#12670,.F.);
#17557=ORIENTED_EDGE('',*,*,#12678,.F.);
#17558=ORIENTED_EDGE('',*,*,#12675,.F.);
#17559=ORIENTED_EDGE('',*,*,#12679,.F.);
#17560=ORIENTED_EDGE('',*,*,#12680,.T.);
#17561=ORIENTED_EDGE('',*,*,#12681,.T.);
#17562=ORIENTED_EDGE('',*,*,#12682,.T.);
#17563=ORIENTED_EDGE('',*,*,#12683,.T.);
#17564=ORIENTED_EDGE('',*,*,#12681,.F.);
#17565=ORIENTED_EDGE('',*,*,#12684,.F.);
#17566=ORIENTED_EDGE('',*,*,#12685,.F.);
#17567=ORIENTED_EDGE('',*,*,#12686,.F.);
#17568=ORIENTED_EDGE('',*,*,#12687,.T.);
#17569=ORIENTED_EDGE('',*,*,#12688,.T.);
#17570=ORIENTED_EDGE('',*,*,#12689,.T.);
#17571=ORIENTED_EDGE('',*,*,#12690,.T.);
#17572=ORIENTED_EDGE('',*,*,#12683,.F.);
#17573=ORIENTED_EDGE('',*,*,#12691,.F.);
#17574=ORIENTED_EDGE('',*,*,#12688,.F.);
#17575=ORIENTED_EDGE('',*,*,#12692,.F.);
#17576=ORIENTED_EDGE('',*,*,#12693,.T.);
#17577=ORIENTED_EDGE('',*,*,#12694,.T.);
#17578=ORIENTED_EDGE('',*,*,#12695,.T.);
#17579=ORIENTED_EDGE('',*,*,#12696,.T.);
#17580=ORIENTED_EDGE('',*,*,#12694,.F.);
#17581=ORIENTED_EDGE('',*,*,#12697,.F.);
#17582=ORIENTED_EDGE('',*,*,#12698,.F.);
#17583=ORIENTED_EDGE('',*,*,#12699,.F.);
#17584=ORIENTED_EDGE('',*,*,#12700,.T.);
#17585=ORIENTED_EDGE('',*,*,#12701,.T.);
#17586=ORIENTED_EDGE('',*,*,#12702,.T.);
#17587=ORIENTED_EDGE('',*,*,#12703,.T.);
#17588=ORIENTED_EDGE('',*,*,#12696,.F.);
#17589=ORIENTED_EDGE('',*,*,#12704,.F.);
#17590=ORIENTED_EDGE('',*,*,#12701,.F.);
#17591=ORIENTED_EDGE('',*,*,#12705,.F.);
#17592=ORIENTED_EDGE('',*,*,#12706,.T.);
#17593=ORIENTED_EDGE('',*,*,#12707,.T.);
#17594=ORIENTED_EDGE('',*,*,#12708,.T.);
#17595=ORIENTED_EDGE('',*,*,#12709,.T.);
#17596=ORIENTED_EDGE('',*,*,#12707,.F.);
#17597=ORIENTED_EDGE('',*,*,#12710,.F.);
#17598=ORIENTED_EDGE('',*,*,#12711,.F.);
#17599=ORIENTED_EDGE('',*,*,#12712,.F.);
#17600=ORIENTED_EDGE('',*,*,#12713,.T.);
#17601=ORIENTED_EDGE('',*,*,#12714,.T.);
#17602=ORIENTED_EDGE('',*,*,#12715,.T.);
#17603=ORIENTED_EDGE('',*,*,#12716,.T.);
#17604=ORIENTED_EDGE('',*,*,#12709,.F.);
#17605=ORIENTED_EDGE('',*,*,#12717,.F.);
#17606=ORIENTED_EDGE('',*,*,#12714,.F.);
#17607=ORIENTED_EDGE('',*,*,#12718,.F.);
#17608=ORIENTED_EDGE('',*,*,#12719,.T.);
#17609=ORIENTED_EDGE('',*,*,#12720,.T.);
#17610=ORIENTED_EDGE('',*,*,#12721,.T.);
#17611=ORIENTED_EDGE('',*,*,#12722,.T.);
#17612=ORIENTED_EDGE('',*,*,#12720,.F.);
#17613=ORIENTED_EDGE('',*,*,#12723,.F.);
#17614=ORIENTED_EDGE('',*,*,#12724,.F.);
#17615=ORIENTED_EDGE('',*,*,#12725,.F.);
#17616=ORIENTED_EDGE('',*,*,#12726,.T.);
#17617=ORIENTED_EDGE('',*,*,#12727,.T.);
#17618=ORIENTED_EDGE('',*,*,#12728,.T.);
#17619=ORIENTED_EDGE('',*,*,#12729,.T.);
#17620=ORIENTED_EDGE('',*,*,#12722,.F.);
#17621=ORIENTED_EDGE('',*,*,#12730,.F.);
#17622=ORIENTED_EDGE('',*,*,#12727,.F.);
#17623=ORIENTED_EDGE('',*,*,#12731,.F.);
#17624=ORIENTED_EDGE('',*,*,#12732,.T.);
#17625=ORIENTED_EDGE('',*,*,#12733,.T.);
#17626=ORIENTED_EDGE('',*,*,#12734,.T.);
#17627=ORIENTED_EDGE('',*,*,#12735,.T.);
#17628=ORIENTED_EDGE('',*,*,#12733,.F.);
#17629=ORIENTED_EDGE('',*,*,#12736,.F.);
#17630=ORIENTED_EDGE('',*,*,#12737,.F.);
#17631=ORIENTED_EDGE('',*,*,#12738,.F.);
#17632=ORIENTED_EDGE('',*,*,#12739,.T.);
#17633=ORIENTED_EDGE('',*,*,#12740,.T.);
#17634=ORIENTED_EDGE('',*,*,#12741,.T.);
#17635=ORIENTED_EDGE('',*,*,#12742,.T.);
#17636=ORIENTED_EDGE('',*,*,#12735,.F.);
#17637=ORIENTED_EDGE('',*,*,#12743,.F.);
#17638=ORIENTED_EDGE('',*,*,#12740,.F.);
#17639=ORIENTED_EDGE('',*,*,#12744,.F.);
#17640=ORIENTED_EDGE('',*,*,#12745,.T.);
#17641=ORIENTED_EDGE('',*,*,#12746,.T.);
#17642=ORIENTED_EDGE('',*,*,#12747,.T.);
#17643=ORIENTED_EDGE('',*,*,#12748,.T.);
#17644=ORIENTED_EDGE('',*,*,#12746,.F.);
#17645=ORIENTED_EDGE('',*,*,#12749,.F.);
#17646=ORIENTED_EDGE('',*,*,#12750,.F.);
#17647=ORIENTED_EDGE('',*,*,#12751,.F.);
#17648=ORIENTED_EDGE('',*,*,#12752,.T.);
#17649=ORIENTED_EDGE('',*,*,#12753,.T.);
#17650=ORIENTED_EDGE('',*,*,#12754,.T.);
#17651=ORIENTED_EDGE('',*,*,#12755,.T.);
#17652=ORIENTED_EDGE('',*,*,#12748,.F.);
#17653=ORIENTED_EDGE('',*,*,#12756,.F.);
#17654=ORIENTED_EDGE('',*,*,#12753,.F.);
#17655=ORIENTED_EDGE('',*,*,#12757,.F.);
#17656=ORIENTED_EDGE('',*,*,#12758,.T.);
#17657=ORIENTED_EDGE('',*,*,#12759,.T.);
#17658=ORIENTED_EDGE('',*,*,#12760,.T.);
#17659=ORIENTED_EDGE('',*,*,#12761,.T.);
#17660=ORIENTED_EDGE('',*,*,#12759,.F.);
#17661=ORIENTED_EDGE('',*,*,#12762,.F.);
#17662=ORIENTED_EDGE('',*,*,#12763,.F.);
#17663=ORIENTED_EDGE('',*,*,#12764,.F.);
#17664=ORIENTED_EDGE('',*,*,#12765,.T.);
#17665=ORIENTED_EDGE('',*,*,#12766,.T.);
#17666=ORIENTED_EDGE('',*,*,#12767,.T.);
#17667=ORIENTED_EDGE('',*,*,#12768,.T.);
#17668=ORIENTED_EDGE('',*,*,#12761,.F.);
#17669=ORIENTED_EDGE('',*,*,#12769,.F.);
#17670=ORIENTED_EDGE('',*,*,#12766,.F.);
#17671=ORIENTED_EDGE('',*,*,#12770,.F.);
#17672=ORIENTED_EDGE('',*,*,#12771,.T.);
#17673=ORIENTED_EDGE('',*,*,#12772,.T.);
#17674=ORIENTED_EDGE('',*,*,#12773,.T.);
#17675=ORIENTED_EDGE('',*,*,#12774,.T.);
#17676=ORIENTED_EDGE('',*,*,#12772,.F.);
#17677=ORIENTED_EDGE('',*,*,#12775,.F.);
#17678=ORIENTED_EDGE('',*,*,#12776,.F.);
#17679=ORIENTED_EDGE('',*,*,#12777,.F.);
#17680=ORIENTED_EDGE('',*,*,#12778,.T.);
#17681=ORIENTED_EDGE('',*,*,#12779,.T.);
#17682=ORIENTED_EDGE('',*,*,#12780,.T.);
#17683=ORIENTED_EDGE('',*,*,#12781,.T.);
#17684=ORIENTED_EDGE('',*,*,#12774,.F.);
#17685=ORIENTED_EDGE('',*,*,#12782,.F.);
#17686=ORIENTED_EDGE('',*,*,#12779,.F.);
#17687=ORIENTED_EDGE('',*,*,#12783,.F.);
#17688=ORIENTED_EDGE('',*,*,#12784,.T.);
#17689=ORIENTED_EDGE('',*,*,#12785,.T.);
#17690=ORIENTED_EDGE('',*,*,#12786,.T.);
#17691=ORIENTED_EDGE('',*,*,#12787,.T.);
#17692=ORIENTED_EDGE('',*,*,#12785,.F.);
#17693=ORIENTED_EDGE('',*,*,#12788,.F.);
#17694=ORIENTED_EDGE('',*,*,#12789,.F.);
#17695=ORIENTED_EDGE('',*,*,#12790,.F.);
#17696=ORIENTED_EDGE('',*,*,#12791,.T.);
#17697=ORIENTED_EDGE('',*,*,#12792,.T.);
#17698=ORIENTED_EDGE('',*,*,#12793,.T.);
#17699=ORIENTED_EDGE('',*,*,#12794,.T.);
#17700=ORIENTED_EDGE('',*,*,#12787,.F.);
#17701=ORIENTED_EDGE('',*,*,#12795,.F.);
#17702=ORIENTED_EDGE('',*,*,#12792,.F.);
#17703=ORIENTED_EDGE('',*,*,#12796,.F.);
#17704=ORIENTED_EDGE('',*,*,#12797,.T.);
#17705=ORIENTED_EDGE('',*,*,#12798,.T.);
#17706=ORIENTED_EDGE('',*,*,#12799,.T.);
#17707=ORIENTED_EDGE('',*,*,#12800,.T.);
#17708=ORIENTED_EDGE('',*,*,#12798,.F.);
#17709=ORIENTED_EDGE('',*,*,#12801,.F.);
#17710=ORIENTED_EDGE('',*,*,#12802,.F.);
#17711=ORIENTED_EDGE('',*,*,#12803,.F.);
#17712=ORIENTED_EDGE('',*,*,#12804,.T.);
#17713=ORIENTED_EDGE('',*,*,#12805,.T.);
#17714=ORIENTED_EDGE('',*,*,#12806,.T.);
#17715=ORIENTED_EDGE('',*,*,#12807,.T.);
#17716=ORIENTED_EDGE('',*,*,#12800,.F.);
#17717=ORIENTED_EDGE('',*,*,#12808,.F.);
#17718=ORIENTED_EDGE('',*,*,#12805,.F.);
#17719=ORIENTED_EDGE('',*,*,#12809,.F.);
#17720=ORIENTED_EDGE('',*,*,#12810,.T.);
#17721=ORIENTED_EDGE('',*,*,#12811,.T.);
#17722=ORIENTED_EDGE('',*,*,#12812,.T.);
#17723=ORIENTED_EDGE('',*,*,#12813,.T.);
#17724=ORIENTED_EDGE('',*,*,#12811,.F.);
#17725=ORIENTED_EDGE('',*,*,#12814,.F.);
#17726=ORIENTED_EDGE('',*,*,#12815,.F.);
#17727=ORIENTED_EDGE('',*,*,#12816,.F.);
#17728=ORIENTED_EDGE('',*,*,#12817,.T.);
#17729=ORIENTED_EDGE('',*,*,#12818,.T.);
#17730=ORIENTED_EDGE('',*,*,#12819,.T.);
#17731=ORIENTED_EDGE('',*,*,#12820,.T.);
#17732=ORIENTED_EDGE('',*,*,#12813,.F.);
#17733=ORIENTED_EDGE('',*,*,#12821,.F.);
#17734=ORIENTED_EDGE('',*,*,#12818,.F.);
#17735=ORIENTED_EDGE('',*,*,#12822,.F.);
#17736=ORIENTED_EDGE('',*,*,#12823,.T.);
#17737=ORIENTED_EDGE('',*,*,#12824,.T.);
#17738=ORIENTED_EDGE('',*,*,#12825,.T.);
#17739=ORIENTED_EDGE('',*,*,#12826,.T.);
#17740=ORIENTED_EDGE('',*,*,#12824,.F.);
#17741=ORIENTED_EDGE('',*,*,#12827,.F.);
#17742=ORIENTED_EDGE('',*,*,#12828,.F.);
#17743=ORIENTED_EDGE('',*,*,#12829,.F.);
#17744=ORIENTED_EDGE('',*,*,#12830,.T.);
#17745=ORIENTED_EDGE('',*,*,#12831,.T.);
#17746=ORIENTED_EDGE('',*,*,#12832,.T.);
#17747=ORIENTED_EDGE('',*,*,#12833,.T.);
#17748=ORIENTED_EDGE('',*,*,#12826,.F.);
#17749=ORIENTED_EDGE('',*,*,#12834,.F.);
#17750=ORIENTED_EDGE('',*,*,#12831,.F.);
#17751=ORIENTED_EDGE('',*,*,#12835,.F.);
#17752=ORIENTED_EDGE('',*,*,#12836,.T.);
#17753=ORIENTED_EDGE('',*,*,#12837,.T.);
#17754=ORIENTED_EDGE('',*,*,#12838,.T.);
#17755=ORIENTED_EDGE('',*,*,#12839,.T.);
#17756=ORIENTED_EDGE('',*,*,#12837,.F.);
#17757=ORIENTED_EDGE('',*,*,#12840,.F.);
#17758=ORIENTED_EDGE('',*,*,#12841,.F.);
#17759=ORIENTED_EDGE('',*,*,#12842,.F.);
#17760=ORIENTED_EDGE('',*,*,#12843,.T.);
#17761=ORIENTED_EDGE('',*,*,#12844,.T.);
#17762=ORIENTED_EDGE('',*,*,#12845,.T.);
#17763=ORIENTED_EDGE('',*,*,#12846,.T.);
#17764=ORIENTED_EDGE('',*,*,#12839,.F.);
#17765=ORIENTED_EDGE('',*,*,#12847,.F.);
#17766=ORIENTED_EDGE('',*,*,#12844,.F.);
#17767=ORIENTED_EDGE('',*,*,#12848,.F.);
#17768=ORIENTED_EDGE('',*,*,#12849,.T.);
#17769=ORIENTED_EDGE('',*,*,#12850,.T.);
#17770=ORIENTED_EDGE('',*,*,#12851,.T.);
#17771=ORIENTED_EDGE('',*,*,#12852,.T.);
#17772=ORIENTED_EDGE('',*,*,#12850,.F.);
#17773=ORIENTED_EDGE('',*,*,#12853,.F.);
#17774=ORIENTED_EDGE('',*,*,#12854,.F.);
#17775=ORIENTED_EDGE('',*,*,#12855,.F.);
#17776=ORIENTED_EDGE('',*,*,#12856,.T.);
#17777=ORIENTED_EDGE('',*,*,#12857,.T.);
#17778=ORIENTED_EDGE('',*,*,#12858,.T.);
#17779=ORIENTED_EDGE('',*,*,#12859,.T.);
#17780=ORIENTED_EDGE('',*,*,#12852,.F.);
#17781=ORIENTED_EDGE('',*,*,#12860,.F.);
#17782=ORIENTED_EDGE('',*,*,#12857,.F.);
#17783=ORIENTED_EDGE('',*,*,#12861,.F.);
#17784=ORIENTED_EDGE('',*,*,#12862,.T.);
#17785=ORIENTED_EDGE('',*,*,#12863,.T.);
#17786=ORIENTED_EDGE('',*,*,#12864,.T.);
#17787=ORIENTED_EDGE('',*,*,#12865,.T.);
#17788=ORIENTED_EDGE('',*,*,#12863,.F.);
#17789=ORIENTED_EDGE('',*,*,#12866,.F.);
#17790=ORIENTED_EDGE('',*,*,#12867,.F.);
#17791=ORIENTED_EDGE('',*,*,#12868,.F.);
#17792=ORIENTED_EDGE('',*,*,#12869,.T.);
#17793=ORIENTED_EDGE('',*,*,#12870,.T.);
#17794=ORIENTED_EDGE('',*,*,#12871,.T.);
#17795=ORIENTED_EDGE('',*,*,#12872,.T.);
#17796=ORIENTED_EDGE('',*,*,#12865,.F.);
#17797=ORIENTED_EDGE('',*,*,#12873,.F.);
#17798=ORIENTED_EDGE('',*,*,#12870,.F.);
#17799=ORIENTED_EDGE('',*,*,#12874,.F.);
#17800=ORIENTED_EDGE('',*,*,#12875,.T.);
#17801=ORIENTED_EDGE('',*,*,#12876,.T.);
#17802=ORIENTED_EDGE('',*,*,#12877,.T.);
#17803=ORIENTED_EDGE('',*,*,#12878,.T.);
#17804=ORIENTED_EDGE('',*,*,#12876,.F.);
#17805=ORIENTED_EDGE('',*,*,#12879,.F.);
#17806=ORIENTED_EDGE('',*,*,#12880,.F.);
#17807=ORIENTED_EDGE('',*,*,#12881,.F.);
#17808=ORIENTED_EDGE('',*,*,#12882,.T.);
#17809=ORIENTED_EDGE('',*,*,#12883,.T.);
#17810=ORIENTED_EDGE('',*,*,#12884,.T.);
#17811=ORIENTED_EDGE('',*,*,#12885,.T.);
#17812=ORIENTED_EDGE('',*,*,#12878,.F.);
#17813=ORIENTED_EDGE('',*,*,#12886,.F.);
#17814=ORIENTED_EDGE('',*,*,#12883,.F.);
#17815=ORIENTED_EDGE('',*,*,#12887,.F.);
#17816=ORIENTED_EDGE('',*,*,#12888,.T.);
#17817=ORIENTED_EDGE('',*,*,#12889,.T.);
#17818=ORIENTED_EDGE('',*,*,#12890,.T.);
#17819=ORIENTED_EDGE('',*,*,#12891,.T.);
#17820=ORIENTED_EDGE('',*,*,#12889,.F.);
#17821=ORIENTED_EDGE('',*,*,#12892,.F.);
#17822=ORIENTED_EDGE('',*,*,#12893,.F.);
#17823=ORIENTED_EDGE('',*,*,#12894,.F.);
#17824=ORIENTED_EDGE('',*,*,#12895,.T.);
#17825=ORIENTED_EDGE('',*,*,#12896,.T.);
#17826=ORIENTED_EDGE('',*,*,#12897,.T.);
#17827=ORIENTED_EDGE('',*,*,#12898,.T.);
#17828=ORIENTED_EDGE('',*,*,#12891,.F.);
#17829=ORIENTED_EDGE('',*,*,#12899,.F.);
#17830=ORIENTED_EDGE('',*,*,#12896,.F.);
#17831=ORIENTED_EDGE('',*,*,#12900,.F.);
#17832=ORIENTED_EDGE('',*,*,#12901,.T.);
#17833=ORIENTED_EDGE('',*,*,#12902,.T.);
#17834=ORIENTED_EDGE('',*,*,#12903,.T.);
#17835=ORIENTED_EDGE('',*,*,#12904,.T.);
#17836=ORIENTED_EDGE('',*,*,#12902,.F.);
#17837=ORIENTED_EDGE('',*,*,#12905,.F.);
#17838=ORIENTED_EDGE('',*,*,#12906,.F.);
#17839=ORIENTED_EDGE('',*,*,#12907,.F.);
#17840=ORIENTED_EDGE('',*,*,#12908,.T.);
#17841=ORIENTED_EDGE('',*,*,#12909,.T.);
#17842=ORIENTED_EDGE('',*,*,#12910,.T.);
#17843=ORIENTED_EDGE('',*,*,#12911,.T.);
#17844=ORIENTED_EDGE('',*,*,#12904,.F.);
#17845=ORIENTED_EDGE('',*,*,#12912,.F.);
#17846=ORIENTED_EDGE('',*,*,#12909,.F.);
#17847=ORIENTED_EDGE('',*,*,#12913,.F.);
#17848=ORIENTED_EDGE('',*,*,#12914,.T.);
#17849=ORIENTED_EDGE('',*,*,#12915,.T.);
#17850=ORIENTED_EDGE('',*,*,#12916,.T.);
#17851=ORIENTED_EDGE('',*,*,#12917,.T.);
#17852=ORIENTED_EDGE('',*,*,#12915,.F.);
#17853=ORIENTED_EDGE('',*,*,#12918,.F.);
#17854=ORIENTED_EDGE('',*,*,#12919,.F.);
#17855=ORIENTED_EDGE('',*,*,#12920,.F.);
#17856=ORIENTED_EDGE('',*,*,#12921,.T.);
#17857=ORIENTED_EDGE('',*,*,#12922,.T.);
#17858=ORIENTED_EDGE('',*,*,#12923,.T.);
#17859=ORIENTED_EDGE('',*,*,#12924,.T.);
#17860=ORIENTED_EDGE('',*,*,#12917,.F.);
#17861=ORIENTED_EDGE('',*,*,#12925,.F.);
#17862=ORIENTED_EDGE('',*,*,#12922,.F.);
#17863=ORIENTED_EDGE('',*,*,#12926,.F.);
#17864=ORIENTED_EDGE('',*,*,#12927,.T.);
#17865=ORIENTED_EDGE('',*,*,#12928,.T.);
#17866=ORIENTED_EDGE('',*,*,#12929,.T.);
#17867=ORIENTED_EDGE('',*,*,#12930,.T.);
#17868=ORIENTED_EDGE('',*,*,#12928,.F.);
#17869=ORIENTED_EDGE('',*,*,#12931,.F.);
#17870=ORIENTED_EDGE('',*,*,#12932,.F.);
#17871=ORIENTED_EDGE('',*,*,#12933,.F.);
#17872=ORIENTED_EDGE('',*,*,#12934,.T.);
#17873=ORIENTED_EDGE('',*,*,#12935,.T.);
#17874=ORIENTED_EDGE('',*,*,#12936,.T.);
#17875=ORIENTED_EDGE('',*,*,#12937,.T.);
#17876=ORIENTED_EDGE('',*,*,#12930,.F.);
#17877=ORIENTED_EDGE('',*,*,#12938,.F.);
#17878=ORIENTED_EDGE('',*,*,#12935,.F.);
#17879=ORIENTED_EDGE('',*,*,#12939,.F.);
#17880=ORIENTED_EDGE('',*,*,#12940,.T.);
#17881=ORIENTED_EDGE('',*,*,#12941,.T.);
#17882=ORIENTED_EDGE('',*,*,#12942,.T.);
#17883=ORIENTED_EDGE('',*,*,#12943,.T.);
#17884=ORIENTED_EDGE('',*,*,#12941,.F.);
#17885=ORIENTED_EDGE('',*,*,#12944,.F.);
#17886=ORIENTED_EDGE('',*,*,#12945,.F.);
#17887=ORIENTED_EDGE('',*,*,#12946,.F.);
#17888=ORIENTED_EDGE('',*,*,#12947,.T.);
#17889=ORIENTED_EDGE('',*,*,#12948,.T.);
#17890=ORIENTED_EDGE('',*,*,#12949,.T.);
#17891=ORIENTED_EDGE('',*,*,#12950,.T.);
#17892=ORIENTED_EDGE('',*,*,#12943,.F.);
#17893=ORIENTED_EDGE('',*,*,#12951,.F.);
#17894=ORIENTED_EDGE('',*,*,#12948,.F.);
#17895=ORIENTED_EDGE('',*,*,#12952,.F.);
#17896=ORIENTED_EDGE('',*,*,#12953,.T.);
#17897=ORIENTED_EDGE('',*,*,#12954,.T.);
#17898=ORIENTED_EDGE('',*,*,#12955,.T.);
#17899=ORIENTED_EDGE('',*,*,#12956,.T.);
#17900=ORIENTED_EDGE('',*,*,#12954,.F.);
#17901=ORIENTED_EDGE('',*,*,#12957,.F.);
#17902=ORIENTED_EDGE('',*,*,#12958,.F.);
#17903=ORIENTED_EDGE('',*,*,#12959,.F.);
#17904=ORIENTED_EDGE('',*,*,#12960,.T.);
#17905=ORIENTED_EDGE('',*,*,#12961,.T.);
#17906=ORIENTED_EDGE('',*,*,#12962,.T.);
#17907=ORIENTED_EDGE('',*,*,#12963,.T.);
#17908=ORIENTED_EDGE('',*,*,#12956,.F.);
#17909=ORIENTED_EDGE('',*,*,#12964,.F.);
#17910=ORIENTED_EDGE('',*,*,#12961,.F.);
#17911=ORIENTED_EDGE('',*,*,#12965,.F.);
#17912=ORIENTED_EDGE('',*,*,#12966,.T.);
#17913=ORIENTED_EDGE('',*,*,#12967,.T.);
#17914=ORIENTED_EDGE('',*,*,#12968,.T.);
#17915=ORIENTED_EDGE('',*,*,#12969,.T.);
#17916=ORIENTED_EDGE('',*,*,#12967,.F.);
#17917=ORIENTED_EDGE('',*,*,#12970,.F.);
#17918=ORIENTED_EDGE('',*,*,#12971,.F.);
#17919=ORIENTED_EDGE('',*,*,#12972,.F.);
#17920=ORIENTED_EDGE('',*,*,#12973,.T.);
#17921=ORIENTED_EDGE('',*,*,#12974,.T.);
#17922=ORIENTED_EDGE('',*,*,#12975,.T.);
#17923=ORIENTED_EDGE('',*,*,#12976,.T.);
#17924=ORIENTED_EDGE('',*,*,#12969,.F.);
#17925=ORIENTED_EDGE('',*,*,#12977,.F.);
#17926=ORIENTED_EDGE('',*,*,#12974,.F.);
#17927=ORIENTED_EDGE('',*,*,#12978,.F.);
#17928=ORIENTED_EDGE('',*,*,#12979,.T.);
#17929=ORIENTED_EDGE('',*,*,#12980,.T.);
#17930=ORIENTED_EDGE('',*,*,#12981,.T.);
#17931=ORIENTED_EDGE('',*,*,#12982,.T.);
#17932=ORIENTED_EDGE('',*,*,#12980,.F.);
#17933=ORIENTED_EDGE('',*,*,#12983,.F.);
#17934=ORIENTED_EDGE('',*,*,#12984,.F.);
#17935=ORIENTED_EDGE('',*,*,#12985,.F.);
#17936=ORIENTED_EDGE('',*,*,#12986,.T.);
#17937=ORIENTED_EDGE('',*,*,#12987,.T.);
#17938=ORIENTED_EDGE('',*,*,#12988,.T.);
#17939=ORIENTED_EDGE('',*,*,#12989,.T.);
#17940=ORIENTED_EDGE('',*,*,#12982,.F.);
#17941=ORIENTED_EDGE('',*,*,#12990,.F.);
#17942=ORIENTED_EDGE('',*,*,#12987,.F.);
#17943=ORIENTED_EDGE('',*,*,#12991,.F.);
#17944=ORIENTED_EDGE('',*,*,#12992,.T.);
#17945=ORIENTED_EDGE('',*,*,#12993,.T.);
#17946=ORIENTED_EDGE('',*,*,#12994,.T.);
#17947=ORIENTED_EDGE('',*,*,#12995,.T.);
#17948=ORIENTED_EDGE('',*,*,#12993,.F.);
#17949=ORIENTED_EDGE('',*,*,#12996,.F.);
#17950=ORIENTED_EDGE('',*,*,#12997,.F.);
#17951=ORIENTED_EDGE('',*,*,#12998,.F.);
#17952=ORIENTED_EDGE('',*,*,#12999,.T.);
#17953=ORIENTED_EDGE('',*,*,#13000,.T.);
#17954=ORIENTED_EDGE('',*,*,#13001,.T.);
#17955=ORIENTED_EDGE('',*,*,#13002,.T.);
#17956=ORIENTED_EDGE('',*,*,#12995,.F.);
#17957=ORIENTED_EDGE('',*,*,#13003,.F.);
#17958=ORIENTED_EDGE('',*,*,#13000,.F.);
#17959=ORIENTED_EDGE('',*,*,#13004,.F.);
#17960=ORIENTED_EDGE('',*,*,#13005,.T.);
#17961=ORIENTED_EDGE('',*,*,#13006,.T.);
#17962=ORIENTED_EDGE('',*,*,#13007,.T.);
#17963=ORIENTED_EDGE('',*,*,#13008,.T.);
#17964=ORIENTED_EDGE('',*,*,#13006,.F.);
#17965=ORIENTED_EDGE('',*,*,#13009,.F.);
#17966=ORIENTED_EDGE('',*,*,#13010,.F.);
#17967=ORIENTED_EDGE('',*,*,#13011,.F.);
#17968=ORIENTED_EDGE('',*,*,#13012,.T.);
#17969=ORIENTED_EDGE('',*,*,#13013,.T.);
#17970=ORIENTED_EDGE('',*,*,#13014,.T.);
#17971=ORIENTED_EDGE('',*,*,#13015,.T.);
#17972=ORIENTED_EDGE('',*,*,#13008,.F.);
#17973=ORIENTED_EDGE('',*,*,#13016,.F.);
#17974=ORIENTED_EDGE('',*,*,#13013,.F.);
#17975=ORIENTED_EDGE('',*,*,#13017,.F.);
#17976=ORIENTED_EDGE('',*,*,#13018,.T.);
#17977=ORIENTED_EDGE('',*,*,#13019,.T.);
#17978=ORIENTED_EDGE('',*,*,#13020,.T.);
#17979=ORIENTED_EDGE('',*,*,#13021,.T.);
#17980=ORIENTED_EDGE('',*,*,#13019,.F.);
#17981=ORIENTED_EDGE('',*,*,#13022,.F.);
#17982=ORIENTED_EDGE('',*,*,#13023,.F.);
#17983=ORIENTED_EDGE('',*,*,#13024,.F.);
#17984=ORIENTED_EDGE('',*,*,#13025,.T.);
#17985=ORIENTED_EDGE('',*,*,#13026,.T.);
#17986=ORIENTED_EDGE('',*,*,#13027,.T.);
#17987=ORIENTED_EDGE('',*,*,#13028,.T.);
#17988=ORIENTED_EDGE('',*,*,#13021,.F.);
#17989=ORIENTED_EDGE('',*,*,#13029,.F.);
#17990=ORIENTED_EDGE('',*,*,#13026,.F.);
#17991=ORIENTED_EDGE('',*,*,#13030,.F.);
#17992=ORIENTED_EDGE('',*,*,#13031,.T.);
#17993=ORIENTED_EDGE('',*,*,#13032,.T.);
#17994=ORIENTED_EDGE('',*,*,#13033,.T.);
#17995=ORIENTED_EDGE('',*,*,#13034,.T.);
#17996=ORIENTED_EDGE('',*,*,#13032,.F.);
#17997=ORIENTED_EDGE('',*,*,#13035,.F.);
#17998=ORIENTED_EDGE('',*,*,#13036,.F.);
#17999=ORIENTED_EDGE('',*,*,#13037,.F.);
#18000=ORIENTED_EDGE('',*,*,#13038,.T.);
#18001=ORIENTED_EDGE('',*,*,#13039,.T.);
#18002=ORIENTED_EDGE('',*,*,#13040,.T.);
#18003=ORIENTED_EDGE('',*,*,#13041,.T.);
#18004=ORIENTED_EDGE('',*,*,#13034,.F.);
#18005=ORIENTED_EDGE('',*,*,#13042,.F.);
#18006=ORIENTED_EDGE('',*,*,#13039,.F.);
#18007=ORIENTED_EDGE('',*,*,#13043,.F.);
#18008=ORIENTED_EDGE('',*,*,#13044,.T.);
#18009=ORIENTED_EDGE('',*,*,#13045,.T.);
#18010=ORIENTED_EDGE('',*,*,#13046,.T.);
#18011=ORIENTED_EDGE('',*,*,#13047,.T.);
#18012=ORIENTED_EDGE('',*,*,#13045,.F.);
#18013=ORIENTED_EDGE('',*,*,#13048,.F.);
#18014=ORIENTED_EDGE('',*,*,#13049,.F.);
#18015=ORIENTED_EDGE('',*,*,#13050,.F.);
#18016=ORIENTED_EDGE('',*,*,#13051,.T.);
#18017=ORIENTED_EDGE('',*,*,#13052,.T.);
#18018=ORIENTED_EDGE('',*,*,#13053,.T.);
#18019=ORIENTED_EDGE('',*,*,#13054,.T.);
#18020=ORIENTED_EDGE('',*,*,#13047,.F.);
#18021=ORIENTED_EDGE('',*,*,#13055,.F.);
#18022=ORIENTED_EDGE('',*,*,#13052,.F.);
#18023=ORIENTED_EDGE('',*,*,#13056,.F.);
#18024=ORIENTED_EDGE('',*,*,#13057,.T.);
#18025=ORIENTED_EDGE('',*,*,#13058,.T.);
#18026=ORIENTED_EDGE('',*,*,#13059,.T.);
#18027=ORIENTED_EDGE('',*,*,#13060,.T.);
#18028=ORIENTED_EDGE('',*,*,#13058,.F.);
#18029=ORIENTED_EDGE('',*,*,#13061,.F.);
#18030=ORIENTED_EDGE('',*,*,#13062,.F.);
#18031=ORIENTED_EDGE('',*,*,#13063,.F.);
#18032=ORIENTED_EDGE('',*,*,#13064,.T.);
#18033=ORIENTED_EDGE('',*,*,#13065,.T.);
#18034=ORIENTED_EDGE('',*,*,#13066,.T.);
#18035=ORIENTED_EDGE('',*,*,#13067,.T.);
#18036=ORIENTED_EDGE('',*,*,#13060,.F.);
#18037=ORIENTED_EDGE('',*,*,#13068,.F.);
#18038=ORIENTED_EDGE('',*,*,#13065,.F.);
#18039=ORIENTED_EDGE('',*,*,#13069,.F.);
#18040=ORIENTED_EDGE('',*,*,#13070,.T.);
#18041=ORIENTED_EDGE('',*,*,#13071,.T.);
#18042=ORIENTED_EDGE('',*,*,#13072,.T.);
#18043=ORIENTED_EDGE('',*,*,#13073,.T.);
#18044=ORIENTED_EDGE('',*,*,#13071,.F.);
#18045=ORIENTED_EDGE('',*,*,#13074,.F.);
#18046=ORIENTED_EDGE('',*,*,#13075,.F.);
#18047=ORIENTED_EDGE('',*,*,#13076,.F.);
#18048=ORIENTED_EDGE('',*,*,#13077,.T.);
#18049=ORIENTED_EDGE('',*,*,#13078,.T.);
#18050=ORIENTED_EDGE('',*,*,#13079,.T.);
#18051=ORIENTED_EDGE('',*,*,#13080,.T.);
#18052=ORIENTED_EDGE('',*,*,#13073,.F.);
#18053=ORIENTED_EDGE('',*,*,#13081,.F.);
#18054=ORIENTED_EDGE('',*,*,#13078,.F.);
#18055=ORIENTED_EDGE('',*,*,#13082,.F.);
#18056=ORIENTED_EDGE('',*,*,#13083,.T.);
#18057=ORIENTED_EDGE('',*,*,#13084,.T.);
#18058=ORIENTED_EDGE('',*,*,#13085,.T.);
#18059=ORIENTED_EDGE('',*,*,#13086,.T.);
#18060=ORIENTED_EDGE('',*,*,#13084,.F.);
#18061=ORIENTED_EDGE('',*,*,#13087,.F.);
#18062=ORIENTED_EDGE('',*,*,#13088,.F.);
#18063=ORIENTED_EDGE('',*,*,#13089,.F.);
#18064=ORIENTED_EDGE('',*,*,#13090,.T.);
#18065=ORIENTED_EDGE('',*,*,#13091,.T.);
#18066=ORIENTED_EDGE('',*,*,#13092,.T.);
#18067=ORIENTED_EDGE('',*,*,#13093,.T.);
#18068=ORIENTED_EDGE('',*,*,#13086,.F.);
#18069=ORIENTED_EDGE('',*,*,#13094,.F.);
#18070=ORIENTED_EDGE('',*,*,#13091,.F.);
#18071=ORIENTED_EDGE('',*,*,#13095,.F.);
#18072=ORIENTED_EDGE('',*,*,#13096,.T.);
#18073=ORIENTED_EDGE('',*,*,#13097,.T.);
#18074=ORIENTED_EDGE('',*,*,#13098,.T.);
#18075=ORIENTED_EDGE('',*,*,#13099,.T.);
#18076=ORIENTED_EDGE('',*,*,#13097,.F.);
#18077=ORIENTED_EDGE('',*,*,#13100,.F.);
#18078=ORIENTED_EDGE('',*,*,#13101,.F.);
#18079=ORIENTED_EDGE('',*,*,#13102,.F.);
#18080=ORIENTED_EDGE('',*,*,#13103,.T.);
#18081=ORIENTED_EDGE('',*,*,#13104,.T.);
#18082=ORIENTED_EDGE('',*,*,#13105,.T.);
#18083=ORIENTED_EDGE('',*,*,#13106,.T.);
#18084=ORIENTED_EDGE('',*,*,#13099,.F.);
#18085=ORIENTED_EDGE('',*,*,#13107,.F.);
#18086=ORIENTED_EDGE('',*,*,#13104,.F.);
#18087=ORIENTED_EDGE('',*,*,#13108,.F.);
#18088=ORIENTED_EDGE('',*,*,#13109,.T.);
#18089=ORIENTED_EDGE('',*,*,#13110,.T.);
#18090=ORIENTED_EDGE('',*,*,#13111,.T.);
#18091=ORIENTED_EDGE('',*,*,#13112,.T.);
#18092=ORIENTED_EDGE('',*,*,#13110,.F.);
#18093=ORIENTED_EDGE('',*,*,#13113,.F.);
#18094=ORIENTED_EDGE('',*,*,#13114,.F.);
#18095=ORIENTED_EDGE('',*,*,#13115,.F.);
#18096=ORIENTED_EDGE('',*,*,#13116,.T.);
#18097=ORIENTED_EDGE('',*,*,#13117,.T.);
#18098=ORIENTED_EDGE('',*,*,#13118,.T.);
#18099=ORIENTED_EDGE('',*,*,#13119,.T.);
#18100=ORIENTED_EDGE('',*,*,#13112,.F.);
#18101=ORIENTED_EDGE('',*,*,#13120,.F.);
#18102=ORIENTED_EDGE('',*,*,#13117,.F.);
#18103=ORIENTED_EDGE('',*,*,#13121,.F.);
#18104=ORIENTED_EDGE('',*,*,#13122,.T.);
#18105=ORIENTED_EDGE('',*,*,#13123,.T.);
#18106=ORIENTED_EDGE('',*,*,#13124,.T.);
#18107=ORIENTED_EDGE('',*,*,#13125,.T.);
#18108=ORIENTED_EDGE('',*,*,#13123,.F.);
#18109=ORIENTED_EDGE('',*,*,#13126,.F.);
#18110=ORIENTED_EDGE('',*,*,#13127,.F.);
#18111=ORIENTED_EDGE('',*,*,#13128,.F.);
#18112=ORIENTED_EDGE('',*,*,#13129,.T.);
#18113=ORIENTED_EDGE('',*,*,#13130,.T.);
#18114=ORIENTED_EDGE('',*,*,#13131,.T.);
#18115=ORIENTED_EDGE('',*,*,#13132,.T.);
#18116=ORIENTED_EDGE('',*,*,#13125,.F.);
#18117=ORIENTED_EDGE('',*,*,#13133,.F.);
#18118=ORIENTED_EDGE('',*,*,#13130,.F.);
#18119=ORIENTED_EDGE('',*,*,#13134,.F.);
#18120=ORIENTED_EDGE('',*,*,#13135,.T.);
#18121=ORIENTED_EDGE('',*,*,#13136,.T.);
#18122=ORIENTED_EDGE('',*,*,#13137,.T.);
#18123=ORIENTED_EDGE('',*,*,#13138,.T.);
#18124=ORIENTED_EDGE('',*,*,#13136,.F.);
#18125=ORIENTED_EDGE('',*,*,#13139,.F.);
#18126=ORIENTED_EDGE('',*,*,#13140,.F.);
#18127=ORIENTED_EDGE('',*,*,#13141,.F.);
#18128=ORIENTED_EDGE('',*,*,#13142,.T.);
#18129=ORIENTED_EDGE('',*,*,#13143,.T.);
#18130=ORIENTED_EDGE('',*,*,#13144,.T.);
#18131=ORIENTED_EDGE('',*,*,#13145,.T.);
#18132=ORIENTED_EDGE('',*,*,#13138,.F.);
#18133=ORIENTED_EDGE('',*,*,#13146,.F.);
#18134=ORIENTED_EDGE('',*,*,#13143,.F.);
#18135=ORIENTED_EDGE('',*,*,#13147,.F.);
#18136=ORIENTED_EDGE('',*,*,#13148,.T.);
#18137=ORIENTED_EDGE('',*,*,#13149,.T.);
#18138=ORIENTED_EDGE('',*,*,#13150,.T.);
#18139=ORIENTED_EDGE('',*,*,#13151,.T.);
#18140=ORIENTED_EDGE('',*,*,#13149,.F.);
#18141=ORIENTED_EDGE('',*,*,#13152,.F.);
#18142=ORIENTED_EDGE('',*,*,#13153,.F.);
#18143=ORIENTED_EDGE('',*,*,#13154,.F.);
#18144=ORIENTED_EDGE('',*,*,#13155,.T.);
#18145=ORIENTED_EDGE('',*,*,#13156,.T.);
#18146=ORIENTED_EDGE('',*,*,#13157,.T.);
#18147=ORIENTED_EDGE('',*,*,#13158,.T.);
#18148=ORIENTED_EDGE('',*,*,#13151,.F.);
#18149=ORIENTED_EDGE('',*,*,#13159,.F.);
#18150=ORIENTED_EDGE('',*,*,#13156,.F.);
#18151=ORIENTED_EDGE('',*,*,#13160,.F.);
#18152=ORIENTED_EDGE('',*,*,#13161,.T.);
#18153=ORIENTED_EDGE('',*,*,#13162,.T.);
#18154=ORIENTED_EDGE('',*,*,#13163,.T.);
#18155=ORIENTED_EDGE('',*,*,#13164,.T.);
#18156=ORIENTED_EDGE('',*,*,#13162,.F.);
#18157=ORIENTED_EDGE('',*,*,#13165,.F.);
#18158=ORIENTED_EDGE('',*,*,#13166,.F.);
#18159=ORIENTED_EDGE('',*,*,#13167,.F.);
#18160=ORIENTED_EDGE('',*,*,#13168,.T.);
#18161=ORIENTED_EDGE('',*,*,#13169,.T.);
#18162=ORIENTED_EDGE('',*,*,#13170,.T.);
#18163=ORIENTED_EDGE('',*,*,#13171,.T.);
#18164=ORIENTED_EDGE('',*,*,#13164,.F.);
#18165=ORIENTED_EDGE('',*,*,#13172,.F.);
#18166=ORIENTED_EDGE('',*,*,#13169,.F.);
#18167=ORIENTED_EDGE('',*,*,#13173,.F.);
#18168=ORIENTED_EDGE('',*,*,#13174,.T.);
#18169=ORIENTED_EDGE('',*,*,#13175,.T.);
#18170=ORIENTED_EDGE('',*,*,#13176,.T.);
#18171=ORIENTED_EDGE('',*,*,#13177,.T.);
#18172=ORIENTED_EDGE('',*,*,#13175,.F.);
#18173=ORIENTED_EDGE('',*,*,#13178,.F.);
#18174=ORIENTED_EDGE('',*,*,#13179,.F.);
#18175=ORIENTED_EDGE('',*,*,#13180,.F.);
#18176=ORIENTED_EDGE('',*,*,#13181,.T.);
#18177=ORIENTED_EDGE('',*,*,#13182,.T.);
#18178=ORIENTED_EDGE('',*,*,#13183,.T.);
#18179=ORIENTED_EDGE('',*,*,#13184,.T.);
#18180=ORIENTED_EDGE('',*,*,#13177,.F.);
#18181=ORIENTED_EDGE('',*,*,#13185,.F.);
#18182=ORIENTED_EDGE('',*,*,#13182,.F.);
#18183=ORIENTED_EDGE('',*,*,#13186,.F.);
#18184=ORIENTED_EDGE('',*,*,#13187,.T.);
#18185=ORIENTED_EDGE('',*,*,#13188,.T.);
#18186=ORIENTED_EDGE('',*,*,#13189,.T.);
#18187=ORIENTED_EDGE('',*,*,#13190,.T.);
#18188=ORIENTED_EDGE('',*,*,#13188,.F.);
#18189=ORIENTED_EDGE('',*,*,#13191,.F.);
#18190=ORIENTED_EDGE('',*,*,#13192,.F.);
#18191=ORIENTED_EDGE('',*,*,#13193,.F.);
#18192=ORIENTED_EDGE('',*,*,#13194,.T.);
#18193=ORIENTED_EDGE('',*,*,#13195,.T.);
#18194=ORIENTED_EDGE('',*,*,#13196,.T.);
#18195=ORIENTED_EDGE('',*,*,#13197,.T.);
#18196=ORIENTED_EDGE('',*,*,#13190,.F.);
#18197=ORIENTED_EDGE('',*,*,#13198,.F.);
#18198=ORIENTED_EDGE('',*,*,#13195,.F.);
#18199=ORIENTED_EDGE('',*,*,#13199,.F.);
#18200=ORIENTED_EDGE('',*,*,#13200,.T.);
#18201=ORIENTED_EDGE('',*,*,#13201,.T.);
#18202=ORIENTED_EDGE('',*,*,#13202,.T.);
#18203=ORIENTED_EDGE('',*,*,#13203,.T.);
#18204=ORIENTED_EDGE('',*,*,#13201,.F.);
#18205=ORIENTED_EDGE('',*,*,#13204,.F.);
#18206=ORIENTED_EDGE('',*,*,#13205,.F.);
#18207=ORIENTED_EDGE('',*,*,#13206,.F.);
#18208=ORIENTED_EDGE('',*,*,#13207,.T.);
#18209=ORIENTED_EDGE('',*,*,#13208,.T.);
#18210=ORIENTED_EDGE('',*,*,#13209,.T.);
#18211=ORIENTED_EDGE('',*,*,#13210,.T.);
#18212=ORIENTED_EDGE('',*,*,#13203,.F.);
#18213=ORIENTED_EDGE('',*,*,#13211,.F.);
#18214=ORIENTED_EDGE('',*,*,#13208,.F.);
#18215=ORIENTED_EDGE('',*,*,#13212,.F.);
#18216=ORIENTED_EDGE('',*,*,#13213,.T.);
#18217=ORIENTED_EDGE('',*,*,#13214,.T.);
#18218=ORIENTED_EDGE('',*,*,#13215,.T.);
#18219=ORIENTED_EDGE('',*,*,#13216,.T.);
#18220=ORIENTED_EDGE('',*,*,#13214,.F.);
#18221=ORIENTED_EDGE('',*,*,#13217,.F.);
#18222=ORIENTED_EDGE('',*,*,#13218,.F.);
#18223=ORIENTED_EDGE('',*,*,#13219,.F.);
#18224=ORIENTED_EDGE('',*,*,#13220,.T.);
#18225=ORIENTED_EDGE('',*,*,#13221,.T.);
#18226=ORIENTED_EDGE('',*,*,#13222,.T.);
#18227=ORIENTED_EDGE('',*,*,#13223,.T.);
#18228=ORIENTED_EDGE('',*,*,#13216,.F.);
#18229=ORIENTED_EDGE('',*,*,#13224,.F.);
#18230=ORIENTED_EDGE('',*,*,#13221,.F.);
#18231=ORIENTED_EDGE('',*,*,#13225,.F.);
#18232=ORIENTED_EDGE('',*,*,#13226,.T.);
#18233=ORIENTED_EDGE('',*,*,#13227,.T.);
#18234=ORIENTED_EDGE('',*,*,#13228,.T.);
#18235=ORIENTED_EDGE('',*,*,#13229,.T.);
#18236=ORIENTED_EDGE('',*,*,#13227,.F.);
#18237=ORIENTED_EDGE('',*,*,#13230,.F.);
#18238=ORIENTED_EDGE('',*,*,#13231,.F.);
#18239=ORIENTED_EDGE('',*,*,#13232,.F.);
#18240=ORIENTED_EDGE('',*,*,#13233,.T.);
#18241=ORIENTED_EDGE('',*,*,#13234,.T.);
#18242=ORIENTED_EDGE('',*,*,#13235,.T.);
#18243=ORIENTED_EDGE('',*,*,#13236,.T.);
#18244=ORIENTED_EDGE('',*,*,#13229,.F.);
#18245=ORIENTED_EDGE('',*,*,#13237,.F.);
#18246=ORIENTED_EDGE('',*,*,#13234,.F.);
#18247=ORIENTED_EDGE('',*,*,#13238,.F.);
#18248=ORIENTED_EDGE('',*,*,#13239,.T.);
#18249=ORIENTED_EDGE('',*,*,#13240,.T.);
#18250=ORIENTED_EDGE('',*,*,#13241,.T.);
#18251=ORIENTED_EDGE('',*,*,#13242,.T.);
#18252=ORIENTED_EDGE('',*,*,#13240,.F.);
#18253=ORIENTED_EDGE('',*,*,#13243,.F.);
#18254=ORIENTED_EDGE('',*,*,#13244,.F.);
#18255=ORIENTED_EDGE('',*,*,#13245,.F.);
#18256=ORIENTED_EDGE('',*,*,#13246,.T.);
#18257=ORIENTED_EDGE('',*,*,#13247,.T.);
#18258=ORIENTED_EDGE('',*,*,#13248,.T.);
#18259=ORIENTED_EDGE('',*,*,#13249,.T.);
#18260=ORIENTED_EDGE('',*,*,#13242,.F.);
#18261=ORIENTED_EDGE('',*,*,#13250,.F.);
#18262=ORIENTED_EDGE('',*,*,#13247,.F.);
#18263=ORIENTED_EDGE('',*,*,#13251,.F.);
#18264=ORIENTED_EDGE('',*,*,#13252,.T.);
#18265=ORIENTED_EDGE('',*,*,#13253,.T.);
#18266=ORIENTED_EDGE('',*,*,#13254,.T.);
#18267=ORIENTED_EDGE('',*,*,#13255,.T.);
#18268=ORIENTED_EDGE('',*,*,#13253,.F.);
#18269=ORIENTED_EDGE('',*,*,#13256,.F.);
#18270=ORIENTED_EDGE('',*,*,#13257,.F.);
#18271=ORIENTED_EDGE('',*,*,#13258,.F.);
#18272=ORIENTED_EDGE('',*,*,#13259,.T.);
#18273=ORIENTED_EDGE('',*,*,#13260,.T.);
#18274=ORIENTED_EDGE('',*,*,#13261,.T.);
#18275=ORIENTED_EDGE('',*,*,#13262,.T.);
#18276=ORIENTED_EDGE('',*,*,#13255,.F.);
#18277=ORIENTED_EDGE('',*,*,#13263,.F.);
#18278=ORIENTED_EDGE('',*,*,#13260,.F.);
#18279=ORIENTED_EDGE('',*,*,#13264,.F.);
#18280=ORIENTED_EDGE('',*,*,#13265,.T.);
#18281=ORIENTED_EDGE('',*,*,#13266,.T.);
#18282=ORIENTED_EDGE('',*,*,#13267,.T.);
#18283=ORIENTED_EDGE('',*,*,#13268,.T.);
#18284=ORIENTED_EDGE('',*,*,#13266,.F.);
#18285=ORIENTED_EDGE('',*,*,#13269,.F.);
#18286=ORIENTED_EDGE('',*,*,#13270,.F.);
#18287=ORIENTED_EDGE('',*,*,#13271,.F.);
#18288=ORIENTED_EDGE('',*,*,#13272,.T.);
#18289=ORIENTED_EDGE('',*,*,#13273,.T.);
#18290=ORIENTED_EDGE('',*,*,#13274,.T.);
#18291=ORIENTED_EDGE('',*,*,#13275,.T.);
#18292=ORIENTED_EDGE('',*,*,#13268,.F.);
#18293=ORIENTED_EDGE('',*,*,#13276,.F.);
#18294=ORIENTED_EDGE('',*,*,#13273,.F.);
#18295=ORIENTED_EDGE('',*,*,#13277,.F.);
#18296=ORIENTED_EDGE('',*,*,#13278,.T.);
#18297=ORIENTED_EDGE('',*,*,#13279,.T.);
#18298=ORIENTED_EDGE('',*,*,#13280,.T.);
#18299=ORIENTED_EDGE('',*,*,#13281,.T.);
#18300=ORIENTED_EDGE('',*,*,#13279,.F.);
#18301=ORIENTED_EDGE('',*,*,#13282,.F.);
#18302=ORIENTED_EDGE('',*,*,#13283,.F.);
#18303=ORIENTED_EDGE('',*,*,#13284,.F.);
#18304=ORIENTED_EDGE('',*,*,#13285,.T.);
#18305=ORIENTED_EDGE('',*,*,#13286,.T.);
#18306=ORIENTED_EDGE('',*,*,#13287,.T.);
#18307=ORIENTED_EDGE('',*,*,#13288,.T.);
#18308=ORIENTED_EDGE('',*,*,#13281,.F.);
#18309=ORIENTED_EDGE('',*,*,#13289,.F.);
#18310=ORIENTED_EDGE('',*,*,#13286,.F.);
#18311=ORIENTED_EDGE('',*,*,#13290,.F.);
#18312=ORIENTED_EDGE('',*,*,#13291,.T.);
#18313=ORIENTED_EDGE('',*,*,#13292,.T.);
#18314=ORIENTED_EDGE('',*,*,#13293,.T.);
#18315=ORIENTED_EDGE('',*,*,#13294,.T.);
#18316=ORIENTED_EDGE('',*,*,#13292,.F.);
#18317=ORIENTED_EDGE('',*,*,#13295,.F.);
#18318=ORIENTED_EDGE('',*,*,#13296,.F.);
#18319=ORIENTED_EDGE('',*,*,#13297,.F.);
#18320=ORIENTED_EDGE('',*,*,#13298,.T.);
#18321=ORIENTED_EDGE('',*,*,#13299,.T.);
#18322=ORIENTED_EDGE('',*,*,#13300,.T.);
#18323=ORIENTED_EDGE('',*,*,#13301,.T.);
#18324=ORIENTED_EDGE('',*,*,#13294,.F.);
#18325=ORIENTED_EDGE('',*,*,#13302,.F.);
#18326=ORIENTED_EDGE('',*,*,#13299,.F.);
#18327=ORIENTED_EDGE('',*,*,#13303,.F.);
#18328=ORIENTED_EDGE('',*,*,#13304,.T.);
#18329=ORIENTED_EDGE('',*,*,#13305,.T.);
#18330=ORIENTED_EDGE('',*,*,#13306,.T.);
#18331=ORIENTED_EDGE('',*,*,#13307,.T.);
#18332=ORIENTED_EDGE('',*,*,#13305,.F.);
#18333=ORIENTED_EDGE('',*,*,#13308,.F.);
#18334=ORIENTED_EDGE('',*,*,#13309,.F.);
#18335=ORIENTED_EDGE('',*,*,#13310,.F.);
#18336=ORIENTED_EDGE('',*,*,#13311,.T.);
#18337=ORIENTED_EDGE('',*,*,#13312,.T.);
#18338=ORIENTED_EDGE('',*,*,#13313,.T.);
#18339=ORIENTED_EDGE('',*,*,#13314,.T.);
#18340=ORIENTED_EDGE('',*,*,#13307,.F.);
#18341=ORIENTED_EDGE('',*,*,#13315,.F.);
#18342=ORIENTED_EDGE('',*,*,#13312,.F.);
#18343=ORIENTED_EDGE('',*,*,#13316,.F.);
#18344=ORIENTED_EDGE('',*,*,#13317,.T.);
#18345=ORIENTED_EDGE('',*,*,#13318,.T.);
#18346=ORIENTED_EDGE('',*,*,#13319,.T.);
#18347=ORIENTED_EDGE('',*,*,#13320,.T.);
#18348=ORIENTED_EDGE('',*,*,#13318,.F.);
#18349=ORIENTED_EDGE('',*,*,#13321,.F.);
#18350=ORIENTED_EDGE('',*,*,#13322,.F.);
#18351=ORIENTED_EDGE('',*,*,#13323,.F.);
#18352=ORIENTED_EDGE('',*,*,#13324,.T.);
#18353=ORIENTED_EDGE('',*,*,#13325,.T.);
#18354=ORIENTED_EDGE('',*,*,#13326,.T.);
#18355=ORIENTED_EDGE('',*,*,#13327,.T.);
#18356=ORIENTED_EDGE('',*,*,#13320,.F.);
#18357=ORIENTED_EDGE('',*,*,#13328,.F.);
#18358=ORIENTED_EDGE('',*,*,#13325,.F.);
#18359=ORIENTED_EDGE('',*,*,#13329,.F.);
#18360=ORIENTED_EDGE('',*,*,#13330,.T.);
#18361=ORIENTED_EDGE('',*,*,#13331,.T.);
#18362=ORIENTED_EDGE('',*,*,#13332,.T.);
#18363=ORIENTED_EDGE('',*,*,#13333,.T.);
#18364=ORIENTED_EDGE('',*,*,#13331,.F.);
#18365=ORIENTED_EDGE('',*,*,#13334,.F.);
#18366=ORIENTED_EDGE('',*,*,#13335,.F.);
#18367=ORIENTED_EDGE('',*,*,#13336,.F.);
#18368=ORIENTED_EDGE('',*,*,#13337,.T.);
#18369=ORIENTED_EDGE('',*,*,#13338,.T.);
#18370=ORIENTED_EDGE('',*,*,#13339,.T.);
#18371=ORIENTED_EDGE('',*,*,#13340,.T.);
#18372=ORIENTED_EDGE('',*,*,#13333,.F.);
#18373=ORIENTED_EDGE('',*,*,#13341,.F.);
#18374=ORIENTED_EDGE('',*,*,#13338,.F.);
#18375=ORIENTED_EDGE('',*,*,#13342,.F.);
#18376=ORIENTED_EDGE('',*,*,#13343,.T.);
#18377=ORIENTED_EDGE('',*,*,#13344,.T.);
#18378=ORIENTED_EDGE('',*,*,#13345,.T.);
#18379=ORIENTED_EDGE('',*,*,#13346,.T.);
#18380=ORIENTED_EDGE('',*,*,#13344,.F.);
#18381=ORIENTED_EDGE('',*,*,#13347,.F.);
#18382=ORIENTED_EDGE('',*,*,#13348,.F.);
#18383=ORIENTED_EDGE('',*,*,#13349,.F.);
#18384=ORIENTED_EDGE('',*,*,#13350,.T.);
#18385=ORIENTED_EDGE('',*,*,#13351,.T.);
#18386=ORIENTED_EDGE('',*,*,#13352,.T.);
#18387=ORIENTED_EDGE('',*,*,#13353,.T.);
#18388=ORIENTED_EDGE('',*,*,#13346,.F.);
#18389=ORIENTED_EDGE('',*,*,#13354,.F.);
#18390=ORIENTED_EDGE('',*,*,#13351,.F.);
#18391=ORIENTED_EDGE('',*,*,#13355,.F.);
#18392=ORIENTED_EDGE('',*,*,#13356,.T.);
#18393=ORIENTED_EDGE('',*,*,#13357,.T.);
#18394=ORIENTED_EDGE('',*,*,#13358,.T.);
#18395=ORIENTED_EDGE('',*,*,#13359,.T.);
#18396=ORIENTED_EDGE('',*,*,#13357,.F.);
#18397=ORIENTED_EDGE('',*,*,#13360,.F.);
#18398=ORIENTED_EDGE('',*,*,#13361,.F.);
#18399=ORIENTED_EDGE('',*,*,#13362,.F.);
#18400=ORIENTED_EDGE('',*,*,#13363,.T.);
#18401=ORIENTED_EDGE('',*,*,#13364,.T.);
#18402=ORIENTED_EDGE('',*,*,#13365,.T.);
#18403=ORIENTED_EDGE('',*,*,#13366,.T.);
#18404=ORIENTED_EDGE('',*,*,#13359,.F.);
#18405=ORIENTED_EDGE('',*,*,#13367,.F.);
#18406=ORIENTED_EDGE('',*,*,#13364,.F.);
#18407=ORIENTED_EDGE('',*,*,#13368,.F.);
#18408=ORIENTED_EDGE('',*,*,#13369,.T.);
#18409=ORIENTED_EDGE('',*,*,#13370,.T.);
#18410=ORIENTED_EDGE('',*,*,#13371,.T.);
#18411=ORIENTED_EDGE('',*,*,#13372,.T.);
#18412=ORIENTED_EDGE('',*,*,#13370,.F.);
#18413=ORIENTED_EDGE('',*,*,#13373,.F.);
#18414=ORIENTED_EDGE('',*,*,#13374,.F.);
#18415=ORIENTED_EDGE('',*,*,#13375,.F.);
#18416=ORIENTED_EDGE('',*,*,#13376,.T.);
#18417=ORIENTED_EDGE('',*,*,#13377,.T.);
#18418=ORIENTED_EDGE('',*,*,#13378,.T.);
#18419=ORIENTED_EDGE('',*,*,#13379,.T.);
#18420=ORIENTED_EDGE('',*,*,#13372,.F.);
#18421=ORIENTED_EDGE('',*,*,#13380,.F.);
#18422=ORIENTED_EDGE('',*,*,#13377,.F.);
#18423=ORIENTED_EDGE('',*,*,#13381,.F.);
#18424=ORIENTED_EDGE('',*,*,#13382,.T.);
#18425=ORIENTED_EDGE('',*,*,#13383,.T.);
#18426=ORIENTED_EDGE('',*,*,#13384,.T.);
#18427=ORIENTED_EDGE('',*,*,#13385,.T.);
#18428=ORIENTED_EDGE('',*,*,#13383,.F.);
#18429=ORIENTED_EDGE('',*,*,#13386,.F.);
#18430=ORIENTED_EDGE('',*,*,#13387,.F.);
#18431=ORIENTED_EDGE('',*,*,#13388,.F.);
#18432=ORIENTED_EDGE('',*,*,#13389,.T.);
#18433=ORIENTED_EDGE('',*,*,#13390,.T.);
#18434=ORIENTED_EDGE('',*,*,#13391,.T.);
#18435=ORIENTED_EDGE('',*,*,#13392,.T.);
#18436=ORIENTED_EDGE('',*,*,#13385,.F.);
#18437=ORIENTED_EDGE('',*,*,#13393,.F.);
#18438=ORIENTED_EDGE('',*,*,#13390,.F.);
#18439=ORIENTED_EDGE('',*,*,#13394,.F.);
#18440=ORIENTED_EDGE('',*,*,#13395,.T.);
#18441=ORIENTED_EDGE('',*,*,#13396,.T.);
#18442=ORIENTED_EDGE('',*,*,#13397,.T.);
#18443=ORIENTED_EDGE('',*,*,#13398,.T.);
#18444=ORIENTED_EDGE('',*,*,#13396,.F.);
#18445=ORIENTED_EDGE('',*,*,#13399,.F.);
#18446=ORIENTED_EDGE('',*,*,#13400,.F.);
#18447=ORIENTED_EDGE('',*,*,#13401,.F.);
#18448=ORIENTED_EDGE('',*,*,#13402,.T.);
#18449=ORIENTED_EDGE('',*,*,#13403,.T.);
#18450=ORIENTED_EDGE('',*,*,#13404,.T.);
#18451=ORIENTED_EDGE('',*,*,#13405,.T.);
#18452=ORIENTED_EDGE('',*,*,#13398,.F.);
#18453=ORIENTED_EDGE('',*,*,#13406,.F.);
#18454=ORIENTED_EDGE('',*,*,#13403,.F.);
#18455=ORIENTED_EDGE('',*,*,#13407,.F.);
#18456=ORIENTED_EDGE('',*,*,#13408,.T.);
#18457=ORIENTED_EDGE('',*,*,#13409,.T.);
#18458=ORIENTED_EDGE('',*,*,#13410,.T.);
#18459=ORIENTED_EDGE('',*,*,#13411,.T.);
#18460=ORIENTED_EDGE('',*,*,#13409,.F.);
#18461=ORIENTED_EDGE('',*,*,#13412,.F.);
#18462=ORIENTED_EDGE('',*,*,#13413,.F.);
#18463=ORIENTED_EDGE('',*,*,#13414,.F.);
#18464=ORIENTED_EDGE('',*,*,#13415,.T.);
#18465=ORIENTED_EDGE('',*,*,#13416,.T.);
#18466=ORIENTED_EDGE('',*,*,#13417,.T.);
#18467=ORIENTED_EDGE('',*,*,#13418,.T.);
#18468=ORIENTED_EDGE('',*,*,#13411,.F.);
#18469=ORIENTED_EDGE('',*,*,#13419,.F.);
#18470=ORIENTED_EDGE('',*,*,#13416,.F.);
#18471=ORIENTED_EDGE('',*,*,#13420,.F.);
#18472=ORIENTED_EDGE('',*,*,#13421,.T.);
#18473=ORIENTED_EDGE('',*,*,#13422,.T.);
#18474=ORIENTED_EDGE('',*,*,#13423,.T.);
#18475=ORIENTED_EDGE('',*,*,#13424,.T.);
#18476=ORIENTED_EDGE('',*,*,#13422,.F.);
#18477=ORIENTED_EDGE('',*,*,#13425,.F.);
#18478=ORIENTED_EDGE('',*,*,#13426,.F.);
#18479=ORIENTED_EDGE('',*,*,#13427,.F.);
#18480=ORIENTED_EDGE('',*,*,#13428,.T.);
#18481=ORIENTED_EDGE('',*,*,#13429,.T.);
#18482=ORIENTED_EDGE('',*,*,#13430,.T.);
#18483=ORIENTED_EDGE('',*,*,#13431,.T.);
#18484=ORIENTED_EDGE('',*,*,#13424,.F.);
#18485=ORIENTED_EDGE('',*,*,#13432,.F.);
#18486=ORIENTED_EDGE('',*,*,#13429,.F.);
#18487=ORIENTED_EDGE('',*,*,#13433,.F.);
#18488=ORIENTED_EDGE('',*,*,#13434,.T.);
#18489=ORIENTED_EDGE('',*,*,#13435,.T.);
#18490=ORIENTED_EDGE('',*,*,#13436,.T.);
#18491=ORIENTED_EDGE('',*,*,#13437,.T.);
#18492=ORIENTED_EDGE('',*,*,#13435,.F.);
#18493=ORIENTED_EDGE('',*,*,#13438,.F.);
#18494=ORIENTED_EDGE('',*,*,#13439,.F.);
#18495=ORIENTED_EDGE('',*,*,#13440,.F.);
#18496=ORIENTED_EDGE('',*,*,#13441,.T.);
#18497=ORIENTED_EDGE('',*,*,#13442,.T.);
#18498=ORIENTED_EDGE('',*,*,#13443,.T.);
#18499=ORIENTED_EDGE('',*,*,#13444,.T.);
#18500=ORIENTED_EDGE('',*,*,#13437,.F.);
#18501=ORIENTED_EDGE('',*,*,#13445,.F.);
#18502=ORIENTED_EDGE('',*,*,#13442,.F.);
#18503=ORIENTED_EDGE('',*,*,#13446,.F.);
#18504=ORIENTED_EDGE('',*,*,#13447,.T.);
#18505=ORIENTED_EDGE('',*,*,#13448,.T.);
#18506=ORIENTED_EDGE('',*,*,#13449,.T.);
#18507=ORIENTED_EDGE('',*,*,#13450,.T.);
#18508=ORIENTED_EDGE('',*,*,#13448,.F.);
#18509=ORIENTED_EDGE('',*,*,#13451,.F.);
#18510=ORIENTED_EDGE('',*,*,#13452,.F.);
#18511=ORIENTED_EDGE('',*,*,#13453,.F.);
#18512=ORIENTED_EDGE('',*,*,#13454,.T.);
#18513=ORIENTED_EDGE('',*,*,#13455,.T.);
#18514=ORIENTED_EDGE('',*,*,#13456,.T.);
#18515=ORIENTED_EDGE('',*,*,#13457,.T.);
#18516=ORIENTED_EDGE('',*,*,#13450,.F.);
#18517=ORIENTED_EDGE('',*,*,#13458,.F.);
#18518=ORIENTED_EDGE('',*,*,#13455,.F.);
#18519=ORIENTED_EDGE('',*,*,#13459,.F.);
#18520=ORIENTED_EDGE('',*,*,#13460,.T.);
#18521=ORIENTED_EDGE('',*,*,#13461,.T.);
#18522=ORIENTED_EDGE('',*,*,#13462,.T.);
#18523=ORIENTED_EDGE('',*,*,#13463,.T.);
#18524=ORIENTED_EDGE('',*,*,#13461,.F.);
#18525=ORIENTED_EDGE('',*,*,#13464,.F.);
#18526=ORIENTED_EDGE('',*,*,#13465,.F.);
#18527=ORIENTED_EDGE('',*,*,#13466,.F.);
#18528=ORIENTED_EDGE('',*,*,#13467,.T.);
#18529=ORIENTED_EDGE('',*,*,#13468,.T.);
#18530=ORIENTED_EDGE('',*,*,#13469,.T.);
#18531=ORIENTED_EDGE('',*,*,#13470,.T.);
#18532=ORIENTED_EDGE('',*,*,#13463,.F.);
#18533=ORIENTED_EDGE('',*,*,#13471,.F.);
#18534=ORIENTED_EDGE('',*,*,#13468,.F.);
#18535=ORIENTED_EDGE('',*,*,#13472,.F.);
#18536=ORIENTED_EDGE('',*,*,#13473,.T.);
#18537=ORIENTED_EDGE('',*,*,#13474,.T.);
#18538=ORIENTED_EDGE('',*,*,#13475,.T.);
#18539=ORIENTED_EDGE('',*,*,#13476,.T.);
#18540=ORIENTED_EDGE('',*,*,#13474,.F.);
#18541=ORIENTED_EDGE('',*,*,#13477,.F.);
#18542=ORIENTED_EDGE('',*,*,#13478,.F.);
#18543=ORIENTED_EDGE('',*,*,#13479,.F.);
#18544=ORIENTED_EDGE('',*,*,#13480,.T.);
#18545=ORIENTED_EDGE('',*,*,#13481,.T.);
#18546=ORIENTED_EDGE('',*,*,#13482,.T.);
#18547=ORIENTED_EDGE('',*,*,#13483,.T.);
#18548=ORIENTED_EDGE('',*,*,#13476,.F.);
#18549=ORIENTED_EDGE('',*,*,#13484,.F.);
#18550=ORIENTED_EDGE('',*,*,#13481,.F.);
#18551=ORIENTED_EDGE('',*,*,#13485,.F.);
#18552=ORIENTED_EDGE('',*,*,#13486,.T.);
#18553=ORIENTED_EDGE('',*,*,#13487,.T.);
#18554=ORIENTED_EDGE('',*,*,#13488,.T.);
#18555=ORIENTED_EDGE('',*,*,#13489,.T.);
#18556=ORIENTED_EDGE('',*,*,#13487,.F.);
#18557=ORIENTED_EDGE('',*,*,#13490,.F.);
#18558=ORIENTED_EDGE('',*,*,#13491,.F.);
#18559=ORIENTED_EDGE('',*,*,#13492,.F.);
#18560=ORIENTED_EDGE('',*,*,#13493,.T.);
#18561=ORIENTED_EDGE('',*,*,#13494,.T.);
#18562=ORIENTED_EDGE('',*,*,#13495,.T.);
#18563=ORIENTED_EDGE('',*,*,#13496,.T.);
#18564=ORIENTED_EDGE('',*,*,#13489,.F.);
#18565=ORIENTED_EDGE('',*,*,#13497,.F.);
#18566=ORIENTED_EDGE('',*,*,#13494,.F.);
#18567=ORIENTED_EDGE('',*,*,#13498,.F.);
#18568=ORIENTED_EDGE('',*,*,#13499,.T.);
#18569=ORIENTED_EDGE('',*,*,#13500,.T.);
#18570=ORIENTED_EDGE('',*,*,#13501,.T.);
#18571=ORIENTED_EDGE('',*,*,#13502,.T.);
#18572=ORIENTED_EDGE('',*,*,#13500,.F.);
#18573=ORIENTED_EDGE('',*,*,#13503,.F.);
#18574=ORIENTED_EDGE('',*,*,#13504,.F.);
#18575=ORIENTED_EDGE('',*,*,#13505,.F.);
#18576=ORIENTED_EDGE('',*,*,#13506,.T.);
#18577=ORIENTED_EDGE('',*,*,#13507,.T.);
#18578=ORIENTED_EDGE('',*,*,#13508,.T.);
#18579=ORIENTED_EDGE('',*,*,#13509,.T.);
#18580=ORIENTED_EDGE('',*,*,#13502,.F.);
#18581=ORIENTED_EDGE('',*,*,#13510,.F.);
#18582=ORIENTED_EDGE('',*,*,#13507,.F.);
#18583=ORIENTED_EDGE('',*,*,#13511,.F.);
#18584=ORIENTED_EDGE('',*,*,#13512,.T.);
#18585=ORIENTED_EDGE('',*,*,#13513,.T.);
#18586=ORIENTED_EDGE('',*,*,#13514,.T.);
#18587=ORIENTED_EDGE('',*,*,#13515,.T.);
#18588=ORIENTED_EDGE('',*,*,#13513,.F.);
#18589=ORIENTED_EDGE('',*,*,#13516,.F.);
#18590=ORIENTED_EDGE('',*,*,#13517,.F.);
#18591=ORIENTED_EDGE('',*,*,#13518,.F.);
#18592=ORIENTED_EDGE('',*,*,#13519,.T.);
#18593=ORIENTED_EDGE('',*,*,#13520,.T.);
#18594=ORIENTED_EDGE('',*,*,#13521,.T.);
#18595=ORIENTED_EDGE('',*,*,#13522,.T.);
#18596=ORIENTED_EDGE('',*,*,#13515,.F.);
#18597=ORIENTED_EDGE('',*,*,#13523,.F.);
#18598=ORIENTED_EDGE('',*,*,#13520,.F.);
#18599=ORIENTED_EDGE('',*,*,#13524,.F.);
#18600=ORIENTED_EDGE('',*,*,#13525,.T.);
#18601=ORIENTED_EDGE('',*,*,#13526,.T.);
#18602=ORIENTED_EDGE('',*,*,#13527,.T.);
#18603=ORIENTED_EDGE('',*,*,#13528,.T.);
#18604=ORIENTED_EDGE('',*,*,#13526,.F.);
#18605=ORIENTED_EDGE('',*,*,#13529,.F.);
#18606=ORIENTED_EDGE('',*,*,#13530,.F.);
#18607=ORIENTED_EDGE('',*,*,#13531,.F.);
#18608=ORIENTED_EDGE('',*,*,#13532,.T.);
#18609=ORIENTED_EDGE('',*,*,#13533,.T.);
#18610=ORIENTED_EDGE('',*,*,#13534,.T.);
#18611=ORIENTED_EDGE('',*,*,#13535,.T.);
#18612=ORIENTED_EDGE('',*,*,#13528,.F.);
#18613=ORIENTED_EDGE('',*,*,#13536,.F.);
#18614=ORIENTED_EDGE('',*,*,#13533,.F.);
#18615=ORIENTED_EDGE('',*,*,#13537,.F.);
#18616=ORIENTED_EDGE('',*,*,#13538,.T.);
#18617=ORIENTED_EDGE('',*,*,#13539,.T.);
#18618=ORIENTED_EDGE('',*,*,#13540,.T.);
#18619=ORIENTED_EDGE('',*,*,#13541,.T.);
#18620=ORIENTED_EDGE('',*,*,#13539,.F.);
#18621=ORIENTED_EDGE('',*,*,#13542,.F.);
#18622=ORIENTED_EDGE('',*,*,#13543,.F.);
#18623=ORIENTED_EDGE('',*,*,#13544,.F.);
#18624=ORIENTED_EDGE('',*,*,#13545,.T.);
#18625=ORIENTED_EDGE('',*,*,#13546,.T.);
#18626=ORIENTED_EDGE('',*,*,#13547,.T.);
#18627=ORIENTED_EDGE('',*,*,#13548,.T.);
#18628=ORIENTED_EDGE('',*,*,#13541,.F.);
#18629=ORIENTED_EDGE('',*,*,#13549,.F.);
#18630=ORIENTED_EDGE('',*,*,#13546,.F.);
#18631=ORIENTED_EDGE('',*,*,#13550,.F.);
#18632=ORIENTED_EDGE('',*,*,#13551,.T.);
#18633=ORIENTED_EDGE('',*,*,#13552,.T.);
#18634=ORIENTED_EDGE('',*,*,#13553,.T.);
#18635=ORIENTED_EDGE('',*,*,#13554,.T.);
#18636=ORIENTED_EDGE('',*,*,#13552,.F.);
#18637=ORIENTED_EDGE('',*,*,#13555,.F.);
#18638=ORIENTED_EDGE('',*,*,#13556,.F.);
#18639=ORIENTED_EDGE('',*,*,#13557,.F.);
#18640=ORIENTED_EDGE('',*,*,#13558,.T.);
#18641=ORIENTED_EDGE('',*,*,#13559,.T.);
#18642=ORIENTED_EDGE('',*,*,#13560,.T.);
#18643=ORIENTED_EDGE('',*,*,#13561,.T.);
#18644=ORIENTED_EDGE('',*,*,#13554,.F.);
#18645=ORIENTED_EDGE('',*,*,#13562,.F.);
#18646=ORIENTED_EDGE('',*,*,#13559,.F.);
#18647=ORIENTED_EDGE('',*,*,#13563,.F.);
#18648=ORIENTED_EDGE('',*,*,#13564,.T.);
#18649=ORIENTED_EDGE('',*,*,#13565,.T.);
#18650=ORIENTED_EDGE('',*,*,#13566,.T.);
#18651=ORIENTED_EDGE('',*,*,#13567,.T.);
#18652=ORIENTED_EDGE('',*,*,#13565,.F.);
#18653=ORIENTED_EDGE('',*,*,#13568,.F.);
#18654=ORIENTED_EDGE('',*,*,#13569,.F.);
#18655=ORIENTED_EDGE('',*,*,#13570,.F.);
#18656=ORIENTED_EDGE('',*,*,#13571,.T.);
#18657=ORIENTED_EDGE('',*,*,#13572,.T.);
#18658=ORIENTED_EDGE('',*,*,#13573,.T.);
#18659=ORIENTED_EDGE('',*,*,#13574,.T.);
#18660=ORIENTED_EDGE('',*,*,#13567,.F.);
#18661=ORIENTED_EDGE('',*,*,#13575,.F.);
#18662=ORIENTED_EDGE('',*,*,#13572,.F.);
#18663=ORIENTED_EDGE('',*,*,#13576,.F.);
#18664=ORIENTED_EDGE('',*,*,#12664,.F.);
#18665=ORIENTED_EDGE('',*,*,#13577,.F.);
#18666=ORIENTED_EDGE('',*,*,#13578,.F.);
#18667=ORIENTED_EDGE('',*,*,#13579,.F.);
#18668=ORIENTED_EDGE('',*,*,#12677,.F.);
#18669=ORIENTED_EDGE('',*,*,#13580,.F.);
#18670=ORIENTED_EDGE('',*,*,#13581,.F.);
#18671=ORIENTED_EDGE('',*,*,#13582,.F.);
#18672=ORIENTED_EDGE('',*,*,#12690,.F.);
#18673=ORIENTED_EDGE('',*,*,#13583,.F.);
#18674=ORIENTED_EDGE('',*,*,#13584,.F.);
#18675=ORIENTED_EDGE('',*,*,#13585,.F.);
#18676=ORIENTED_EDGE('',*,*,#12703,.F.);
#18677=ORIENTED_EDGE('',*,*,#13586,.F.);
#18678=ORIENTED_EDGE('',*,*,#13587,.F.);
#18679=ORIENTED_EDGE('',*,*,#13588,.F.);
#18680=ORIENTED_EDGE('',*,*,#12716,.F.);
#18681=ORIENTED_EDGE('',*,*,#13589,.F.);
#18682=ORIENTED_EDGE('',*,*,#13590,.F.);
#18683=ORIENTED_EDGE('',*,*,#13591,.F.);
#18684=ORIENTED_EDGE('',*,*,#12729,.F.);
#18685=ORIENTED_EDGE('',*,*,#13592,.F.);
#18686=ORIENTED_EDGE('',*,*,#13593,.F.);
#18687=ORIENTED_EDGE('',*,*,#13594,.F.);
#18688=ORIENTED_EDGE('',*,*,#12742,.F.);
#18689=ORIENTED_EDGE('',*,*,#13595,.F.);
#18690=ORIENTED_EDGE('',*,*,#13596,.F.);
#18691=ORIENTED_EDGE('',*,*,#13597,.F.);
#18692=ORIENTED_EDGE('',*,*,#12755,.F.);
#18693=ORIENTED_EDGE('',*,*,#13598,.F.);
#18694=ORIENTED_EDGE('',*,*,#13599,.F.);
#18695=ORIENTED_EDGE('',*,*,#13600,.F.);
#18696=ORIENTED_EDGE('',*,*,#12768,.F.);
#18697=ORIENTED_EDGE('',*,*,#13601,.F.);
#18698=ORIENTED_EDGE('',*,*,#13602,.F.);
#18699=ORIENTED_EDGE('',*,*,#13603,.F.);
#18700=ORIENTED_EDGE('',*,*,#12781,.F.);
#18701=ORIENTED_EDGE('',*,*,#13604,.F.);
#18702=ORIENTED_EDGE('',*,*,#13605,.F.);
#18703=ORIENTED_EDGE('',*,*,#13606,.F.);
#18704=ORIENTED_EDGE('',*,*,#12794,.F.);
#18705=ORIENTED_EDGE('',*,*,#13607,.F.);
#18706=ORIENTED_EDGE('',*,*,#13608,.F.);
#18707=ORIENTED_EDGE('',*,*,#13609,.F.);
#18708=ORIENTED_EDGE('',*,*,#12807,.F.);
#18709=ORIENTED_EDGE('',*,*,#13610,.F.);
#18710=ORIENTED_EDGE('',*,*,#13611,.F.);
#18711=ORIENTED_EDGE('',*,*,#13612,.F.);
#18712=ORIENTED_EDGE('',*,*,#12820,.F.);
#18713=ORIENTED_EDGE('',*,*,#13613,.F.);
#18714=ORIENTED_EDGE('',*,*,#13614,.F.);
#18715=ORIENTED_EDGE('',*,*,#13615,.F.);
#18716=ORIENTED_EDGE('',*,*,#12833,.F.);
#18717=ORIENTED_EDGE('',*,*,#13616,.F.);
#18718=ORIENTED_EDGE('',*,*,#13617,.F.);
#18719=ORIENTED_EDGE('',*,*,#13618,.F.);
#18720=ORIENTED_EDGE('',*,*,#12846,.F.);
#18721=ORIENTED_EDGE('',*,*,#13619,.F.);
#18722=ORIENTED_EDGE('',*,*,#13620,.F.);
#18723=ORIENTED_EDGE('',*,*,#13621,.F.);
#18724=ORIENTED_EDGE('',*,*,#12859,.F.);
#18725=ORIENTED_EDGE('',*,*,#13622,.F.);
#18726=ORIENTED_EDGE('',*,*,#13623,.F.);
#18727=ORIENTED_EDGE('',*,*,#13624,.F.);
#18728=ORIENTED_EDGE('',*,*,#12872,.F.);
#18729=ORIENTED_EDGE('',*,*,#13625,.F.);
#18730=ORIENTED_EDGE('',*,*,#13626,.F.);
#18731=ORIENTED_EDGE('',*,*,#13627,.F.);
#18732=ORIENTED_EDGE('',*,*,#12885,.F.);
#18733=ORIENTED_EDGE('',*,*,#13628,.F.);
#18734=ORIENTED_EDGE('',*,*,#13629,.F.);
#18735=ORIENTED_EDGE('',*,*,#13630,.F.);
#18736=ORIENTED_EDGE('',*,*,#12898,.F.);
#18737=ORIENTED_EDGE('',*,*,#13631,.F.);
#18738=ORIENTED_EDGE('',*,*,#13632,.F.);
#18739=ORIENTED_EDGE('',*,*,#13633,.F.);
#18740=ORIENTED_EDGE('',*,*,#12911,.F.);
#18741=ORIENTED_EDGE('',*,*,#13634,.F.);
#18742=ORIENTED_EDGE('',*,*,#13635,.F.);
#18743=ORIENTED_EDGE('',*,*,#13636,.F.);
#18744=ORIENTED_EDGE('',*,*,#12924,.F.);
#18745=ORIENTED_EDGE('',*,*,#13637,.F.);
#18746=ORIENTED_EDGE('',*,*,#13638,.F.);
#18747=ORIENTED_EDGE('',*,*,#13639,.F.);
#18748=ORIENTED_EDGE('',*,*,#12937,.F.);
#18749=ORIENTED_EDGE('',*,*,#13640,.F.);
#18750=ORIENTED_EDGE('',*,*,#13641,.F.);
#18751=ORIENTED_EDGE('',*,*,#13642,.F.);
#18752=ORIENTED_EDGE('',*,*,#12950,.F.);
#18753=ORIENTED_EDGE('',*,*,#13643,.F.);
#18754=ORIENTED_EDGE('',*,*,#13644,.F.);
#18755=ORIENTED_EDGE('',*,*,#13645,.F.);
#18756=ORIENTED_EDGE('',*,*,#12963,.F.);
#18757=ORIENTED_EDGE('',*,*,#13646,.F.);
#18758=ORIENTED_EDGE('',*,*,#13647,.F.);
#18759=ORIENTED_EDGE('',*,*,#13648,.F.);
#18760=ORIENTED_EDGE('',*,*,#12976,.F.);
#18761=ORIENTED_EDGE('',*,*,#13649,.F.);
#18762=ORIENTED_EDGE('',*,*,#13650,.F.);
#18763=ORIENTED_EDGE('',*,*,#13651,.F.);
#18764=ORIENTED_EDGE('',*,*,#12989,.F.);
#18765=ORIENTED_EDGE('',*,*,#13652,.F.);
#18766=ORIENTED_EDGE('',*,*,#13653,.F.);
#18767=ORIENTED_EDGE('',*,*,#13654,.F.);
#18768=ORIENTED_EDGE('',*,*,#13002,.F.);
#18769=ORIENTED_EDGE('',*,*,#13655,.F.);
#18770=ORIENTED_EDGE('',*,*,#13656,.F.);
#18771=ORIENTED_EDGE('',*,*,#13657,.F.);
#18772=ORIENTED_EDGE('',*,*,#13015,.F.);
#18773=ORIENTED_EDGE('',*,*,#13658,.F.);
#18774=ORIENTED_EDGE('',*,*,#13659,.F.);
#18775=ORIENTED_EDGE('',*,*,#13660,.F.);
#18776=ORIENTED_EDGE('',*,*,#13028,.F.);
#18777=ORIENTED_EDGE('',*,*,#13661,.F.);
#18778=ORIENTED_EDGE('',*,*,#13662,.F.);
#18779=ORIENTED_EDGE('',*,*,#13663,.F.);
#18780=ORIENTED_EDGE('',*,*,#13041,.F.);
#18781=ORIENTED_EDGE('',*,*,#13664,.F.);
#18782=ORIENTED_EDGE('',*,*,#13665,.F.);
#18783=ORIENTED_EDGE('',*,*,#13666,.F.);
#18784=ORIENTED_EDGE('',*,*,#13054,.F.);
#18785=ORIENTED_EDGE('',*,*,#13667,.F.);
#18786=ORIENTED_EDGE('',*,*,#13668,.F.);
#18787=ORIENTED_EDGE('',*,*,#13669,.F.);
#18788=ORIENTED_EDGE('',*,*,#13067,.F.);
#18789=ORIENTED_EDGE('',*,*,#13670,.F.);
#18790=ORIENTED_EDGE('',*,*,#13671,.F.);
#18791=ORIENTED_EDGE('',*,*,#13672,.F.);
#18792=ORIENTED_EDGE('',*,*,#13080,.F.);
#18793=ORIENTED_EDGE('',*,*,#13673,.F.);
#18794=ORIENTED_EDGE('',*,*,#13674,.F.);
#18795=ORIENTED_EDGE('',*,*,#13675,.F.);
#18796=ORIENTED_EDGE('',*,*,#13093,.F.);
#18797=ORIENTED_EDGE('',*,*,#13676,.F.);
#18798=ORIENTED_EDGE('',*,*,#13677,.F.);
#18799=ORIENTED_EDGE('',*,*,#13678,.F.);
#18800=ORIENTED_EDGE('',*,*,#13106,.F.);
#18801=ORIENTED_EDGE('',*,*,#13679,.F.);
#18802=ORIENTED_EDGE('',*,*,#13680,.F.);
#18803=ORIENTED_EDGE('',*,*,#13681,.F.);
#18804=ORIENTED_EDGE('',*,*,#13119,.F.);
#18805=ORIENTED_EDGE('',*,*,#13682,.F.);
#18806=ORIENTED_EDGE('',*,*,#13683,.F.);
#18807=ORIENTED_EDGE('',*,*,#13684,.F.);
#18808=ORIENTED_EDGE('',*,*,#13132,.F.);
#18809=ORIENTED_EDGE('',*,*,#13685,.F.);
#18810=ORIENTED_EDGE('',*,*,#13686,.F.);
#18811=ORIENTED_EDGE('',*,*,#13687,.F.);
#18812=ORIENTED_EDGE('',*,*,#13145,.F.);
#18813=ORIENTED_EDGE('',*,*,#13688,.F.);
#18814=ORIENTED_EDGE('',*,*,#13689,.F.);
#18815=ORIENTED_EDGE('',*,*,#13690,.F.);
#18816=ORIENTED_EDGE('',*,*,#13158,.F.);
#18817=ORIENTED_EDGE('',*,*,#13691,.F.);
#18818=ORIENTED_EDGE('',*,*,#13692,.F.);
#18819=ORIENTED_EDGE('',*,*,#13693,.F.);
#18820=ORIENTED_EDGE('',*,*,#13171,.F.);
#18821=ORIENTED_EDGE('',*,*,#13694,.F.);
#18822=ORIENTED_EDGE('',*,*,#13695,.F.);
#18823=ORIENTED_EDGE('',*,*,#13696,.F.);
#18824=ORIENTED_EDGE('',*,*,#13184,.F.);
#18825=ORIENTED_EDGE('',*,*,#13697,.F.);
#18826=ORIENTED_EDGE('',*,*,#13698,.F.);
#18827=ORIENTED_EDGE('',*,*,#13699,.F.);
#18828=ORIENTED_EDGE('',*,*,#13197,.F.);
#18829=ORIENTED_EDGE('',*,*,#13700,.F.);
#18830=ORIENTED_EDGE('',*,*,#13701,.F.);
#18831=ORIENTED_EDGE('',*,*,#13702,.F.);
#18832=ORIENTED_EDGE('',*,*,#13210,.F.);
#18833=ORIENTED_EDGE('',*,*,#13703,.F.);
#18834=ORIENTED_EDGE('',*,*,#13704,.F.);
#18835=ORIENTED_EDGE('',*,*,#13705,.F.);
#18836=ORIENTED_EDGE('',*,*,#13223,.F.);
#18837=ORIENTED_EDGE('',*,*,#13706,.F.);
#18838=ORIENTED_EDGE('',*,*,#13707,.F.);
#18839=ORIENTED_EDGE('',*,*,#13708,.F.);
#18840=ORIENTED_EDGE('',*,*,#13236,.F.);
#18841=ORIENTED_EDGE('',*,*,#13709,.F.);
#18842=ORIENTED_EDGE('',*,*,#13710,.F.);
#18843=ORIENTED_EDGE('',*,*,#13711,.F.);
#18844=ORIENTED_EDGE('',*,*,#13249,.F.);
#18845=ORIENTED_EDGE('',*,*,#13712,.F.);
#18846=ORIENTED_EDGE('',*,*,#13713,.F.);
#18847=ORIENTED_EDGE('',*,*,#13714,.F.);
#18848=ORIENTED_EDGE('',*,*,#13262,.F.);
#18849=ORIENTED_EDGE('',*,*,#13715,.F.);
#18850=ORIENTED_EDGE('',*,*,#13716,.F.);
#18851=ORIENTED_EDGE('',*,*,#13717,.F.);
#18852=ORIENTED_EDGE('',*,*,#13275,.F.);
#18853=ORIENTED_EDGE('',*,*,#13718,.F.);
#18854=ORIENTED_EDGE('',*,*,#13719,.F.);
#18855=ORIENTED_EDGE('',*,*,#13720,.F.);
#18856=ORIENTED_EDGE('',*,*,#13288,.F.);
#18857=ORIENTED_EDGE('',*,*,#13721,.F.);
#18858=ORIENTED_EDGE('',*,*,#13722,.F.);
#18859=ORIENTED_EDGE('',*,*,#13723,.F.);
#18860=ORIENTED_EDGE('',*,*,#13301,.F.);
#18861=ORIENTED_EDGE('',*,*,#13724,.F.);
#18862=ORIENTED_EDGE('',*,*,#13725,.F.);
#18863=ORIENTED_EDGE('',*,*,#13726,.F.);
#18864=ORIENTED_EDGE('',*,*,#13314,.F.);
#18865=ORIENTED_EDGE('',*,*,#13727,.F.);
#18866=ORIENTED_EDGE('',*,*,#13728,.F.);
#18867=ORIENTED_EDGE('',*,*,#13729,.F.);
#18868=ORIENTED_EDGE('',*,*,#13327,.F.);
#18869=ORIENTED_EDGE('',*,*,#13730,.F.);
#18870=ORIENTED_EDGE('',*,*,#13731,.F.);
#18871=ORIENTED_EDGE('',*,*,#13732,.F.);
#18872=ORIENTED_EDGE('',*,*,#13340,.F.);
#18873=ORIENTED_EDGE('',*,*,#13733,.F.);
#18874=ORIENTED_EDGE('',*,*,#13734,.F.);
#18875=ORIENTED_EDGE('',*,*,#13735,.F.);
#18876=ORIENTED_EDGE('',*,*,#13353,.F.);
#18877=ORIENTED_EDGE('',*,*,#13736,.F.);
#18878=ORIENTED_EDGE('',*,*,#13737,.F.);
#18879=ORIENTED_EDGE('',*,*,#13738,.F.);
#18880=ORIENTED_EDGE('',*,*,#13366,.F.);
#18881=ORIENTED_EDGE('',*,*,#13739,.F.);
#18882=ORIENTED_EDGE('',*,*,#13740,.F.);
#18883=ORIENTED_EDGE('',*,*,#13741,.F.);
#18884=ORIENTED_EDGE('',*,*,#13379,.F.);
#18885=ORIENTED_EDGE('',*,*,#13742,.F.);
#18886=ORIENTED_EDGE('',*,*,#13743,.F.);
#18887=ORIENTED_EDGE('',*,*,#13744,.F.);
#18888=ORIENTED_EDGE('',*,*,#13392,.F.);
#18889=ORIENTED_EDGE('',*,*,#13745,.F.);
#18890=ORIENTED_EDGE('',*,*,#13746,.F.);
#18891=ORIENTED_EDGE('',*,*,#13747,.F.);
#18892=ORIENTED_EDGE('',*,*,#13405,.F.);
#18893=ORIENTED_EDGE('',*,*,#13748,.F.);
#18894=ORIENTED_EDGE('',*,*,#13749,.F.);
#18895=ORIENTED_EDGE('',*,*,#13750,.F.);
#18896=ORIENTED_EDGE('',*,*,#13418,.F.);
#18897=ORIENTED_EDGE('',*,*,#13751,.F.);
#18898=ORIENTED_EDGE('',*,*,#13752,.F.);
#18899=ORIENTED_EDGE('',*,*,#13753,.F.);
#18900=ORIENTED_EDGE('',*,*,#13431,.F.);
#18901=ORIENTED_EDGE('',*,*,#13754,.F.);
#18902=ORIENTED_EDGE('',*,*,#13755,.F.);
#18903=ORIENTED_EDGE('',*,*,#13756,.F.);
#18904=ORIENTED_EDGE('',*,*,#13444,.F.);
#18905=ORIENTED_EDGE('',*,*,#13757,.F.);
#18906=ORIENTED_EDGE('',*,*,#13758,.F.);
#18907=ORIENTED_EDGE('',*,*,#13759,.F.);
#18908=ORIENTED_EDGE('',*,*,#13457,.F.);
#18909=ORIENTED_EDGE('',*,*,#13760,.F.);
#18910=ORIENTED_EDGE('',*,*,#13761,.F.);
#18911=ORIENTED_EDGE('',*,*,#13762,.F.);
#18912=ORIENTED_EDGE('',*,*,#13470,.F.);
#18913=ORIENTED_EDGE('',*,*,#13763,.F.);
#18914=ORIENTED_EDGE('',*,*,#13764,.F.);
#18915=ORIENTED_EDGE('',*,*,#13765,.F.);
#18916=ORIENTED_EDGE('',*,*,#13483,.F.);
#18917=ORIENTED_EDGE('',*,*,#13766,.F.);
#18918=ORIENTED_EDGE('',*,*,#13767,.F.);
#18919=ORIENTED_EDGE('',*,*,#13768,.F.);
#18920=ORIENTED_EDGE('',*,*,#13496,.F.);
#18921=ORIENTED_EDGE('',*,*,#13769,.F.);
#18922=ORIENTED_EDGE('',*,*,#13770,.F.);
#18923=ORIENTED_EDGE('',*,*,#13771,.F.);
#18924=ORIENTED_EDGE('',*,*,#13509,.F.);
#18925=ORIENTED_EDGE('',*,*,#13772,.F.);
#18926=ORIENTED_EDGE('',*,*,#13773,.F.);
#18927=ORIENTED_EDGE('',*,*,#13774,.F.);
#18928=ORIENTED_EDGE('',*,*,#13522,.F.);
#18929=ORIENTED_EDGE('',*,*,#13775,.F.);
#18930=ORIENTED_EDGE('',*,*,#13776,.F.);
#18931=ORIENTED_EDGE('',*,*,#13777,.F.);
#18932=ORIENTED_EDGE('',*,*,#13535,.F.);
#18933=ORIENTED_EDGE('',*,*,#13778,.F.);
#18934=ORIENTED_EDGE('',*,*,#13779,.F.);
#18935=ORIENTED_EDGE('',*,*,#13780,.F.);
#18936=ORIENTED_EDGE('',*,*,#13548,.F.);
#18937=ORIENTED_EDGE('',*,*,#13781,.F.);
#18938=ORIENTED_EDGE('',*,*,#13782,.F.);
#18939=ORIENTED_EDGE('',*,*,#13783,.F.);
#18940=ORIENTED_EDGE('',*,*,#13561,.F.);
#18941=ORIENTED_EDGE('',*,*,#13784,.F.);
#18942=ORIENTED_EDGE('',*,*,#13785,.F.);
#18943=ORIENTED_EDGE('',*,*,#13786,.F.);
#18944=ORIENTED_EDGE('',*,*,#13574,.F.);
#18945=ORIENTED_EDGE('',*,*,#13787,.F.);
#18946=ORIENTED_EDGE('',*,*,#13788,.F.);
#18947=ORIENTED_EDGE('',*,*,#13789,.F.);
#18948=ORIENTED_EDGE('',*,*,#13569,.T.);
#18949=ORIENTED_EDGE('',*,*,#13790,.T.);
#18950=ORIENTED_EDGE('',*,*,#13791,.T.);
#18951=ORIENTED_EDGE('',*,*,#13792,.F.);
#18952=ORIENTED_EDGE('',*,*,#13556,.T.);
#18953=ORIENTED_EDGE('',*,*,#13793,.T.);
#18954=ORIENTED_EDGE('',*,*,#13788,.T.);
#18955=ORIENTED_EDGE('',*,*,#13794,.F.);
#18956=ORIENTED_EDGE('',*,*,#13543,.T.);
#18957=ORIENTED_EDGE('',*,*,#13795,.T.);
#18958=ORIENTED_EDGE('',*,*,#13785,.T.);
#18959=ORIENTED_EDGE('',*,*,#13796,.F.);
#18960=ORIENTED_EDGE('',*,*,#13530,.T.);
#18961=ORIENTED_EDGE('',*,*,#13797,.T.);
#18962=ORIENTED_EDGE('',*,*,#13782,.T.);
#18963=ORIENTED_EDGE('',*,*,#13798,.F.);
#18964=ORIENTED_EDGE('',*,*,#13517,.T.);
#18965=ORIENTED_EDGE('',*,*,#13799,.T.);
#18966=ORIENTED_EDGE('',*,*,#13779,.T.);
#18967=ORIENTED_EDGE('',*,*,#13800,.F.);
#18968=ORIENTED_EDGE('',*,*,#13504,.T.);
#18969=ORIENTED_EDGE('',*,*,#13801,.T.);
#18970=ORIENTED_EDGE('',*,*,#13776,.T.);
#18971=ORIENTED_EDGE('',*,*,#13802,.F.);
#18972=ORIENTED_EDGE('',*,*,#13491,.T.);
#18973=ORIENTED_EDGE('',*,*,#13803,.T.);
#18974=ORIENTED_EDGE('',*,*,#13773,.T.);
#18975=ORIENTED_EDGE('',*,*,#13804,.F.);
#18976=ORIENTED_EDGE('',*,*,#13478,.T.);
#18977=ORIENTED_EDGE('',*,*,#13805,.T.);
#18978=ORIENTED_EDGE('',*,*,#13770,.T.);
#18979=ORIENTED_EDGE('',*,*,#13806,.F.);
#18980=ORIENTED_EDGE('',*,*,#13465,.T.);
#18981=ORIENTED_EDGE('',*,*,#13807,.T.);
#18982=ORIENTED_EDGE('',*,*,#13767,.T.);
#18983=ORIENTED_EDGE('',*,*,#13808,.F.);
#18984=ORIENTED_EDGE('',*,*,#13452,.T.);
#18985=ORIENTED_EDGE('',*,*,#13809,.T.);
#18986=ORIENTED_EDGE('',*,*,#13764,.T.);
#18987=ORIENTED_EDGE('',*,*,#13810,.F.);
#18988=ORIENTED_EDGE('',*,*,#13439,.T.);
#18989=ORIENTED_EDGE('',*,*,#13811,.T.);
#18990=ORIENTED_EDGE('',*,*,#13761,.T.);
#18991=ORIENTED_EDGE('',*,*,#13812,.F.);
#18992=ORIENTED_EDGE('',*,*,#13426,.T.);
#18993=ORIENTED_EDGE('',*,*,#13813,.T.);
#18994=ORIENTED_EDGE('',*,*,#13758,.T.);
#18995=ORIENTED_EDGE('',*,*,#13814,.F.);
#18996=ORIENTED_EDGE('',*,*,#13413,.T.);
#18997=ORIENTED_EDGE('',*,*,#13815,.T.);
#18998=ORIENTED_EDGE('',*,*,#13755,.T.);
#18999=ORIENTED_EDGE('',*,*,#13816,.F.);
#19000=ORIENTED_EDGE('',*,*,#13400,.T.);
#19001=ORIENTED_EDGE('',*,*,#13817,.T.);
#19002=ORIENTED_EDGE('',*,*,#13752,.T.);
#19003=ORIENTED_EDGE('',*,*,#13818,.F.);
#19004=ORIENTED_EDGE('',*,*,#13387,.T.);
#19005=ORIENTED_EDGE('',*,*,#13819,.T.);
#19006=ORIENTED_EDGE('',*,*,#13749,.T.);
#19007=ORIENTED_EDGE('',*,*,#13820,.F.);
#19008=ORIENTED_EDGE('',*,*,#13374,.T.);
#19009=ORIENTED_EDGE('',*,*,#13821,.T.);
#19010=ORIENTED_EDGE('',*,*,#13746,.T.);
#19011=ORIENTED_EDGE('',*,*,#13822,.F.);
#19012=ORIENTED_EDGE('',*,*,#13361,.T.);
#19013=ORIENTED_EDGE('',*,*,#13823,.T.);
#19014=ORIENTED_EDGE('',*,*,#13743,.T.);
#19015=ORIENTED_EDGE('',*,*,#13824,.F.);
#19016=ORIENTED_EDGE('',*,*,#13348,.T.);
#19017=ORIENTED_EDGE('',*,*,#13825,.T.);
#19018=ORIENTED_EDGE('',*,*,#13740,.T.);
#19019=ORIENTED_EDGE('',*,*,#13826,.F.);
#19020=ORIENTED_EDGE('',*,*,#13335,.T.);
#19021=ORIENTED_EDGE('',*,*,#13827,.T.);
#19022=ORIENTED_EDGE('',*,*,#13737,.T.);
#19023=ORIENTED_EDGE('',*,*,#13828,.F.);
#19024=ORIENTED_EDGE('',*,*,#13322,.T.);
#19025=ORIENTED_EDGE('',*,*,#13829,.T.);
#19026=ORIENTED_EDGE('',*,*,#13734,.T.);
#19027=ORIENTED_EDGE('',*,*,#13830,.F.);
#19028=ORIENTED_EDGE('',*,*,#13309,.T.);
#19029=ORIENTED_EDGE('',*,*,#13831,.T.);
#19030=ORIENTED_EDGE('',*,*,#13731,.T.);
#19031=ORIENTED_EDGE('',*,*,#13832,.F.);
#19032=ORIENTED_EDGE('',*,*,#13296,.T.);
#19033=ORIENTED_EDGE('',*,*,#13833,.T.);
#19034=ORIENTED_EDGE('',*,*,#13728,.T.);
#19035=ORIENTED_EDGE('',*,*,#13834,.F.);
#19036=ORIENTED_EDGE('',*,*,#13283,.T.);
#19037=ORIENTED_EDGE('',*,*,#13835,.T.);
#19038=ORIENTED_EDGE('',*,*,#13725,.T.);
#19039=ORIENTED_EDGE('',*,*,#13836,.F.);
#19040=ORIENTED_EDGE('',*,*,#13270,.T.);
#19041=ORIENTED_EDGE('',*,*,#13837,.T.);
#19042=ORIENTED_EDGE('',*,*,#13722,.T.);
#19043=ORIENTED_EDGE('',*,*,#13838,.F.);
#19044=ORIENTED_EDGE('',*,*,#13257,.T.);
#19045=ORIENTED_EDGE('',*,*,#13839,.T.);
#19046=ORIENTED_EDGE('',*,*,#13719,.T.);
#19047=ORIENTED_EDGE('',*,*,#13840,.F.);
#19048=ORIENTED_EDGE('',*,*,#13244,.T.);
#19049=ORIENTED_EDGE('',*,*,#13841,.T.);
#19050=ORIENTED_EDGE('',*,*,#13716,.T.);
#19051=ORIENTED_EDGE('',*,*,#13842,.F.);
#19052=ORIENTED_EDGE('',*,*,#13231,.T.);
#19053=ORIENTED_EDGE('',*,*,#13843,.T.);
#19054=ORIENTED_EDGE('',*,*,#13713,.T.);
#19055=ORIENTED_EDGE('',*,*,#13844,.F.);
#19056=ORIENTED_EDGE('',*,*,#13218,.T.);
#19057=ORIENTED_EDGE('',*,*,#13845,.T.);
#19058=ORIENTED_EDGE('',*,*,#13710,.T.);
#19059=ORIENTED_EDGE('',*,*,#13846,.F.);
#19060=ORIENTED_EDGE('',*,*,#13205,.T.);
#19061=ORIENTED_EDGE('',*,*,#13847,.T.);
#19062=ORIENTED_EDGE('',*,*,#13707,.T.);
#19063=ORIENTED_EDGE('',*,*,#13848,.F.);
#19064=ORIENTED_EDGE('',*,*,#13192,.T.);
#19065=ORIENTED_EDGE('',*,*,#13849,.T.);
#19066=ORIENTED_EDGE('',*,*,#13704,.T.);
#19067=ORIENTED_EDGE('',*,*,#13850,.F.);
#19068=ORIENTED_EDGE('',*,*,#13179,.T.);
#19069=ORIENTED_EDGE('',*,*,#13851,.T.);
#19070=ORIENTED_EDGE('',*,*,#13701,.T.);
#19071=ORIENTED_EDGE('',*,*,#13852,.F.);
#19072=ORIENTED_EDGE('',*,*,#13166,.T.);
#19073=ORIENTED_EDGE('',*,*,#13853,.T.);
#19074=ORIENTED_EDGE('',*,*,#13698,.T.);
#19075=ORIENTED_EDGE('',*,*,#13854,.F.);
#19076=ORIENTED_EDGE('',*,*,#13153,.T.);
#19077=ORIENTED_EDGE('',*,*,#13855,.T.);
#19078=ORIENTED_EDGE('',*,*,#13695,.T.);
#19079=ORIENTED_EDGE('',*,*,#13856,.F.);
#19080=ORIENTED_EDGE('',*,*,#13140,.T.);
#19081=ORIENTED_EDGE('',*,*,#13857,.T.);
#19082=ORIENTED_EDGE('',*,*,#13692,.T.);
#19083=ORIENTED_EDGE('',*,*,#13858,.F.);
#19084=ORIENTED_EDGE('',*,*,#13127,.T.);
#19085=ORIENTED_EDGE('',*,*,#13859,.T.);
#19086=ORIENTED_EDGE('',*,*,#13689,.T.);
#19087=ORIENTED_EDGE('',*,*,#13860,.F.);
#19088=ORIENTED_EDGE('',*,*,#13114,.T.);
#19089=ORIENTED_EDGE('',*,*,#13861,.T.);
#19090=ORIENTED_EDGE('',*,*,#13686,.T.);
#19091=ORIENTED_EDGE('',*,*,#13862,.F.);
#19092=ORIENTED_EDGE('',*,*,#13101,.T.);
#19093=ORIENTED_EDGE('',*,*,#13863,.T.);
#19094=ORIENTED_EDGE('',*,*,#13683,.T.);
#19095=ORIENTED_EDGE('',*,*,#13864,.F.);
#19096=ORIENTED_EDGE('',*,*,#13088,.T.);
#19097=ORIENTED_EDGE('',*,*,#13865,.T.);
#19098=ORIENTED_EDGE('',*,*,#13680,.T.);
#19099=ORIENTED_EDGE('',*,*,#13866,.F.);
#19100=ORIENTED_EDGE('',*,*,#13075,.T.);
#19101=ORIENTED_EDGE('',*,*,#13867,.T.);
#19102=ORIENTED_EDGE('',*,*,#13677,.T.);
#19103=ORIENTED_EDGE('',*,*,#13868,.F.);
#19104=ORIENTED_EDGE('',*,*,#13062,.T.);
#19105=ORIENTED_EDGE('',*,*,#13869,.T.);
#19106=ORIENTED_EDGE('',*,*,#13674,.T.);
#19107=ORIENTED_EDGE('',*,*,#13870,.F.);
#19108=ORIENTED_EDGE('',*,*,#13049,.T.);
#19109=ORIENTED_EDGE('',*,*,#13871,.T.);
#19110=ORIENTED_EDGE('',*,*,#13671,.T.);
#19111=ORIENTED_EDGE('',*,*,#13872,.F.);
#19112=ORIENTED_EDGE('',*,*,#13036,.T.);
#19113=ORIENTED_EDGE('',*,*,#13873,.T.);
#19114=ORIENTED_EDGE('',*,*,#13668,.T.);
#19115=ORIENTED_EDGE('',*,*,#13874,.F.);
#19116=ORIENTED_EDGE('',*,*,#13023,.T.);
#19117=ORIENTED_EDGE('',*,*,#13875,.T.);
#19118=ORIENTED_EDGE('',*,*,#13665,.T.);
#19119=ORIENTED_EDGE('',*,*,#13876,.F.);
#19120=ORIENTED_EDGE('',*,*,#13010,.T.);
#19121=ORIENTED_EDGE('',*,*,#13877,.T.);
#19122=ORIENTED_EDGE('',*,*,#13662,.T.);
#19123=ORIENTED_EDGE('',*,*,#13878,.F.);
#19124=ORIENTED_EDGE('',*,*,#12997,.T.);
#19125=ORIENTED_EDGE('',*,*,#13879,.T.);
#19126=ORIENTED_EDGE('',*,*,#13659,.T.);
#19127=ORIENTED_EDGE('',*,*,#13880,.F.);
#19128=ORIENTED_EDGE('',*,*,#12984,.T.);
#19129=ORIENTED_EDGE('',*,*,#13881,.T.);
#19130=ORIENTED_EDGE('',*,*,#13656,.T.);
#19131=ORIENTED_EDGE('',*,*,#13882,.F.);
#19132=ORIENTED_EDGE('',*,*,#12971,.T.);
#19133=ORIENTED_EDGE('',*,*,#13883,.T.);
#19134=ORIENTED_EDGE('',*,*,#13653,.T.);
#19135=ORIENTED_EDGE('',*,*,#13884,.F.);
#19136=ORIENTED_EDGE('',*,*,#12958,.T.);
#19137=ORIENTED_EDGE('',*,*,#13885,.T.);
#19138=ORIENTED_EDGE('',*,*,#13650,.T.);
#19139=ORIENTED_EDGE('',*,*,#13886,.F.);
#19140=ORIENTED_EDGE('',*,*,#12945,.T.);
#19141=ORIENTED_EDGE('',*,*,#13887,.T.);
#19142=ORIENTED_EDGE('',*,*,#13647,.T.);
#19143=ORIENTED_EDGE('',*,*,#13888,.F.);
#19144=ORIENTED_EDGE('',*,*,#12932,.T.);
#19145=ORIENTED_EDGE('',*,*,#13889,.T.);
#19146=ORIENTED_EDGE('',*,*,#13644,.T.);
#19147=ORIENTED_EDGE('',*,*,#13890,.F.);
#19148=ORIENTED_EDGE('',*,*,#12919,.T.);
#19149=ORIENTED_EDGE('',*,*,#13891,.T.);
#19150=ORIENTED_EDGE('',*,*,#13641,.T.);
#19151=ORIENTED_EDGE('',*,*,#13892,.F.);
#19152=ORIENTED_EDGE('',*,*,#12906,.T.);
#19153=ORIENTED_EDGE('',*,*,#13893,.T.);
#19154=ORIENTED_EDGE('',*,*,#13638,.T.);
#19155=ORIENTED_EDGE('',*,*,#13894,.F.);
#19156=ORIENTED_EDGE('',*,*,#12893,.T.);
#19157=ORIENTED_EDGE('',*,*,#13895,.T.);
#19158=ORIENTED_EDGE('',*,*,#13635,.T.);
#19159=ORIENTED_EDGE('',*,*,#13896,.F.);
#19160=ORIENTED_EDGE('',*,*,#12880,.T.);
#19161=ORIENTED_EDGE('',*,*,#13897,.T.);
#19162=ORIENTED_EDGE('',*,*,#13632,.T.);
#19163=ORIENTED_EDGE('',*,*,#13898,.F.);
#19164=ORIENTED_EDGE('',*,*,#12867,.T.);
#19165=ORIENTED_EDGE('',*,*,#13899,.T.);
#19166=ORIENTED_EDGE('',*,*,#13629,.T.);
#19167=ORIENTED_EDGE('',*,*,#13900,.F.);
#19168=ORIENTED_EDGE('',*,*,#12854,.T.);
#19169=ORIENTED_EDGE('',*,*,#13901,.T.);
#19170=ORIENTED_EDGE('',*,*,#13626,.T.);
#19171=ORIENTED_EDGE('',*,*,#13902,.F.);
#19172=ORIENTED_EDGE('',*,*,#12841,.T.);
#19173=ORIENTED_EDGE('',*,*,#13903,.T.);
#19174=ORIENTED_EDGE('',*,*,#13623,.T.);
#19175=ORIENTED_EDGE('',*,*,#13904,.F.);
#19176=ORIENTED_EDGE('',*,*,#12828,.T.);
#19177=ORIENTED_EDGE('',*,*,#13905,.T.);
#19178=ORIENTED_EDGE('',*,*,#13620,.T.);
#19179=ORIENTED_EDGE('',*,*,#13906,.F.);
#19180=ORIENTED_EDGE('',*,*,#12815,.T.);
#19181=ORIENTED_EDGE('',*,*,#13907,.T.);
#19182=ORIENTED_EDGE('',*,*,#13617,.T.);
#19183=ORIENTED_EDGE('',*,*,#13908,.F.);
#19184=ORIENTED_EDGE('',*,*,#12802,.T.);
#19185=ORIENTED_EDGE('',*,*,#13909,.T.);
#19186=ORIENTED_EDGE('',*,*,#13614,.T.);
#19187=ORIENTED_EDGE('',*,*,#13910,.F.);
#19188=ORIENTED_EDGE('',*,*,#12789,.T.);
#19189=ORIENTED_EDGE('',*,*,#13911,.T.);
#19190=ORIENTED_EDGE('',*,*,#13611,.T.);
#19191=ORIENTED_EDGE('',*,*,#13912,.F.);
#19192=ORIENTED_EDGE('',*,*,#12776,.T.);
#19193=ORIENTED_EDGE('',*,*,#13913,.T.);
#19194=ORIENTED_EDGE('',*,*,#13608,.T.);
#19195=ORIENTED_EDGE('',*,*,#13914,.F.);
#19196=ORIENTED_EDGE('',*,*,#12763,.T.);
#19197=ORIENTED_EDGE('',*,*,#13915,.T.);
#19198=ORIENTED_EDGE('',*,*,#13605,.T.);
#19199=ORIENTED_EDGE('',*,*,#13916,.F.);
#19200=ORIENTED_EDGE('',*,*,#12750,.T.);
#19201=ORIENTED_EDGE('',*,*,#13917,.T.);
#19202=ORIENTED_EDGE('',*,*,#13602,.T.);
#19203=ORIENTED_EDGE('',*,*,#13918,.F.);
#19204=ORIENTED_EDGE('',*,*,#12737,.T.);
#19205=ORIENTED_EDGE('',*,*,#13919,.T.);
#19206=ORIENTED_EDGE('',*,*,#13599,.T.);
#19207=ORIENTED_EDGE('',*,*,#13920,.F.);
#19208=ORIENTED_EDGE('',*,*,#12724,.T.);
#19209=ORIENTED_EDGE('',*,*,#13921,.T.);
#19210=ORIENTED_EDGE('',*,*,#13596,.T.);
#19211=ORIENTED_EDGE('',*,*,#13922,.F.);
#19212=ORIENTED_EDGE('',*,*,#12711,.T.);
#19213=ORIENTED_EDGE('',*,*,#13923,.T.);
#19214=ORIENTED_EDGE('',*,*,#13593,.T.);
#19215=ORIENTED_EDGE('',*,*,#13924,.F.);
#19216=ORIENTED_EDGE('',*,*,#12698,.T.);
#19217=ORIENTED_EDGE('',*,*,#13925,.T.);
#19218=ORIENTED_EDGE('',*,*,#13590,.T.);
#19219=ORIENTED_EDGE('',*,*,#13926,.F.);
#19220=ORIENTED_EDGE('',*,*,#12685,.T.);
#19221=ORIENTED_EDGE('',*,*,#13927,.T.);
#19222=ORIENTED_EDGE('',*,*,#13587,.T.);
#19223=ORIENTED_EDGE('',*,*,#13928,.F.);
#19224=ORIENTED_EDGE('',*,*,#12672,.T.);
#19225=ORIENTED_EDGE('',*,*,#13929,.T.);
#19226=ORIENTED_EDGE('',*,*,#13584,.T.);
#19227=ORIENTED_EDGE('',*,*,#13930,.F.);
#19228=ORIENTED_EDGE('',*,*,#13578,.T.);
#19229=ORIENTED_EDGE('',*,*,#13931,.F.);
#19230=ORIENTED_EDGE('',*,*,#13932,.T.);
#19231=ORIENTED_EDGE('',*,*,#13933,.T.);
#19232=ORIENTED_EDGE('',*,*,#13934,.T.);
#19233=ORIENTED_EDGE('',*,*,#13935,.T.);
#19234=ORIENTED_EDGE('',*,*,#13936,.T.);
#19235=ORIENTED_EDGE('',*,*,#13937,.T.);
#19236=ORIENTED_EDGE('',*,*,#13935,.F.);
#19237=ORIENTED_EDGE('',*,*,#13938,.F.);
#19238=ORIENTED_EDGE('',*,*,#13932,.F.);
#19239=ORIENTED_EDGE('',*,*,#13939,.F.);
#19240=ORIENTED_EDGE('',*,*,#13940,.T.);
#19241=ORIENTED_EDGE('',*,*,#13941,.T.);
#19242=ORIENTED_EDGE('',*,*,#13942,.T.);
#19243=ORIENTED_EDGE('',*,*,#13943,.T.);
#19244=ORIENTED_EDGE('',*,*,#13937,.F.);
#19245=ORIENTED_EDGE('',*,*,#13944,.F.);
#19246=ORIENTED_EDGE('',*,*,#13941,.F.);
#19247=ORIENTED_EDGE('',*,*,#13945,.F.);
#19248=ORIENTED_EDGE('',*,*,#13943,.F.);
#19249=ORIENTED_EDGE('',*,*,#13946,.F.);
#19250=ORIENTED_EDGE('',*,*,#13791,.F.);
#19251=ORIENTED_EDGE('',*,*,#13947,.F.);
#19252=ORIENTED_EDGE('',*,*,#13948,.T.);
#19253=ORIENTED_EDGE('',*,*,#12660,.T.);
#19254=ORIENTED_EDGE('',*,*,#13949,.T.);
#19255=ORIENTED_EDGE('',*,*,#13580,.T.);
#19256=ORIENTED_EDGE('',*,*,#12676,.F.);
#19257=ORIENTED_EDGE('',*,*,#12678,.T.);
#19258=ORIENTED_EDGE('',*,*,#12669,.F.);
#19259=ORIENTED_EDGE('',*,*,#12673,.T.);
#19260=ORIENTED_EDGE('',*,*,#13930,.T.);
#19261=ORIENTED_EDGE('',*,*,#13583,.T.);
#19262=ORIENTED_EDGE('',*,*,#12689,.F.);
#19263=ORIENTED_EDGE('',*,*,#12691,.T.);
#19264=ORIENTED_EDGE('',*,*,#12682,.F.);
#19265=ORIENTED_EDGE('',*,*,#12686,.T.);
#19266=ORIENTED_EDGE('',*,*,#13928,.T.);
#19267=ORIENTED_EDGE('',*,*,#13586,.T.);
#19268=ORIENTED_EDGE('',*,*,#12702,.F.);
#19269=ORIENTED_EDGE('',*,*,#12704,.T.);
#19270=ORIENTED_EDGE('',*,*,#12695,.F.);
#19271=ORIENTED_EDGE('',*,*,#12699,.T.);
#19272=ORIENTED_EDGE('',*,*,#13926,.T.);
#19273=ORIENTED_EDGE('',*,*,#13589,.T.);
#19274=ORIENTED_EDGE('',*,*,#12715,.F.);
#19275=ORIENTED_EDGE('',*,*,#12717,.T.);
#19276=ORIENTED_EDGE('',*,*,#12708,.F.);
#19277=ORIENTED_EDGE('',*,*,#12712,.T.);
#19278=ORIENTED_EDGE('',*,*,#13924,.T.);
#19279=ORIENTED_EDGE('',*,*,#13592,.T.);
#19280=ORIENTED_EDGE('',*,*,#12728,.F.);
#19281=ORIENTED_EDGE('',*,*,#12730,.T.);
#19282=ORIENTED_EDGE('',*,*,#12721,.F.);
#19283=ORIENTED_EDGE('',*,*,#12725,.T.);
#19284=ORIENTED_EDGE('',*,*,#13922,.T.);
#19285=ORIENTED_EDGE('',*,*,#13595,.T.);
#19286=ORIENTED_EDGE('',*,*,#12741,.F.);
#19287=ORIENTED_EDGE('',*,*,#12743,.T.);
#19288=ORIENTED_EDGE('',*,*,#12734,.F.);
#19289=ORIENTED_EDGE('',*,*,#12738,.T.);
#19290=ORIENTED_EDGE('',*,*,#13920,.T.);
#19291=ORIENTED_EDGE('',*,*,#13598,.T.);
#19292=ORIENTED_EDGE('',*,*,#12754,.F.);
#19293=ORIENTED_EDGE('',*,*,#12756,.T.);
#19294=ORIENTED_EDGE('',*,*,#12747,.F.);
#19295=ORIENTED_EDGE('',*,*,#12751,.T.);
#19296=ORIENTED_EDGE('',*,*,#13918,.T.);
#19297=ORIENTED_EDGE('',*,*,#13601,.T.);
#19298=ORIENTED_EDGE('',*,*,#12767,.F.);
#19299=ORIENTED_EDGE('',*,*,#12769,.T.);
#19300=ORIENTED_EDGE('',*,*,#12760,.F.);
#19301=ORIENTED_EDGE('',*,*,#12764,.T.);
#19302=ORIENTED_EDGE('',*,*,#13916,.T.);
#19303=ORIENTED_EDGE('',*,*,#13604,.T.);
#19304=ORIENTED_EDGE('',*,*,#12780,.F.);
#19305=ORIENTED_EDGE('',*,*,#12782,.T.);
#19306=ORIENTED_EDGE('',*,*,#12773,.F.);
#19307=ORIENTED_EDGE('',*,*,#12777,.T.);
#19308=ORIENTED_EDGE('',*,*,#13914,.T.);
#19309=ORIENTED_EDGE('',*,*,#13607,.T.);
#19310=ORIENTED_EDGE('',*,*,#12793,.F.);
#19311=ORIENTED_EDGE('',*,*,#12795,.T.);
#19312=ORIENTED_EDGE('',*,*,#12786,.F.);
#19313=ORIENTED_EDGE('',*,*,#12790,.T.);
#19314=ORIENTED_EDGE('',*,*,#13912,.T.);
#19315=ORIENTED_EDGE('',*,*,#13610,.T.);
#19316=ORIENTED_EDGE('',*,*,#12806,.F.);
#19317=ORIENTED_EDGE('',*,*,#12808,.T.);
#19318=ORIENTED_EDGE('',*,*,#12799,.F.);
#19319=ORIENTED_EDGE('',*,*,#12803,.T.);
#19320=ORIENTED_EDGE('',*,*,#13910,.T.);
#19321=ORIENTED_EDGE('',*,*,#13613,.T.);
#19322=ORIENTED_EDGE('',*,*,#12819,.F.);
#19323=ORIENTED_EDGE('',*,*,#12821,.T.);
#19324=ORIENTED_EDGE('',*,*,#12812,.F.);
#19325=ORIENTED_EDGE('',*,*,#12816,.T.);
#19326=ORIENTED_EDGE('',*,*,#13908,.T.);
#19327=ORIENTED_EDGE('',*,*,#13616,.T.);
#19328=ORIENTED_EDGE('',*,*,#12832,.F.);
#19329=ORIENTED_EDGE('',*,*,#12834,.T.);
#19330=ORIENTED_EDGE('',*,*,#12825,.F.);
#19331=ORIENTED_EDGE('',*,*,#12829,.T.);
#19332=ORIENTED_EDGE('',*,*,#13906,.T.);
#19333=ORIENTED_EDGE('',*,*,#13619,.T.);
#19334=ORIENTED_EDGE('',*,*,#12845,.F.);
#19335=ORIENTED_EDGE('',*,*,#12847,.T.);
#19336=ORIENTED_EDGE('',*,*,#12838,.F.);
#19337=ORIENTED_EDGE('',*,*,#12842,.T.);
#19338=ORIENTED_EDGE('',*,*,#13904,.T.);
#19339=ORIENTED_EDGE('',*,*,#13622,.T.);
#19340=ORIENTED_EDGE('',*,*,#12858,.F.);
#19341=ORIENTED_EDGE('',*,*,#12860,.T.);
#19342=ORIENTED_EDGE('',*,*,#12851,.F.);
#19343=ORIENTED_EDGE('',*,*,#12855,.T.);
#19344=ORIENTED_EDGE('',*,*,#13902,.T.);
#19345=ORIENTED_EDGE('',*,*,#13625,.T.);
#19346=ORIENTED_EDGE('',*,*,#12871,.F.);
#19347=ORIENTED_EDGE('',*,*,#12873,.T.);
#19348=ORIENTED_EDGE('',*,*,#12864,.F.);
#19349=ORIENTED_EDGE('',*,*,#12868,.T.);
#19350=ORIENTED_EDGE('',*,*,#13900,.T.);
#19351=ORIENTED_EDGE('',*,*,#13628,.T.);
#19352=ORIENTED_EDGE('',*,*,#12884,.F.);
#19353=ORIENTED_EDGE('',*,*,#12886,.T.);
#19354=ORIENTED_EDGE('',*,*,#12877,.F.);
#19355=ORIENTED_EDGE('',*,*,#12881,.T.);
#19356=ORIENTED_EDGE('',*,*,#13898,.T.);
#19357=ORIENTED_EDGE('',*,*,#13631,.T.);
#19358=ORIENTED_EDGE('',*,*,#12897,.F.);
#19359=ORIENTED_EDGE('',*,*,#12899,.T.);
#19360=ORIENTED_EDGE('',*,*,#12890,.F.);
#19361=ORIENTED_EDGE('',*,*,#12894,.T.);
#19362=ORIENTED_EDGE('',*,*,#13896,.T.);
#19363=ORIENTED_EDGE('',*,*,#13634,.T.);
#19364=ORIENTED_EDGE('',*,*,#12910,.F.);
#19365=ORIENTED_EDGE('',*,*,#12912,.T.);
#19366=ORIENTED_EDGE('',*,*,#12903,.F.);
#19367=ORIENTED_EDGE('',*,*,#12907,.T.);
#19368=ORIENTED_EDGE('',*,*,#13894,.T.);
#19369=ORIENTED_EDGE('',*,*,#13637,.T.);
#19370=ORIENTED_EDGE('',*,*,#12923,.F.);
#19371=ORIENTED_EDGE('',*,*,#12925,.T.);
#19372=ORIENTED_EDGE('',*,*,#12916,.F.);
#19373=ORIENTED_EDGE('',*,*,#12920,.T.);
#19374=ORIENTED_EDGE('',*,*,#13892,.T.);
#19375=ORIENTED_EDGE('',*,*,#13640,.T.);
#19376=ORIENTED_EDGE('',*,*,#12936,.F.);
#19377=ORIENTED_EDGE('',*,*,#12938,.T.);
#19378=ORIENTED_EDGE('',*,*,#12929,.F.);
#19379=ORIENTED_EDGE('',*,*,#12933,.T.);
#19380=ORIENTED_EDGE('',*,*,#13890,.T.);
#19381=ORIENTED_EDGE('',*,*,#13643,.T.);
#19382=ORIENTED_EDGE('',*,*,#12949,.F.);
#19383=ORIENTED_EDGE('',*,*,#12951,.T.);
#19384=ORIENTED_EDGE('',*,*,#12942,.F.);
#19385=ORIENTED_EDGE('',*,*,#12946,.T.);
#19386=ORIENTED_EDGE('',*,*,#13888,.T.);
#19387=ORIENTED_EDGE('',*,*,#13646,.T.);
#19388=ORIENTED_EDGE('',*,*,#12962,.F.);
#19389=ORIENTED_EDGE('',*,*,#12964,.T.);
#19390=ORIENTED_EDGE('',*,*,#12955,.F.);
#19391=ORIENTED_EDGE('',*,*,#12959,.T.);
#19392=ORIENTED_EDGE('',*,*,#13886,.T.);
#19393=ORIENTED_EDGE('',*,*,#13649,.T.);
#19394=ORIENTED_EDGE('',*,*,#12975,.F.);
#19395=ORIENTED_EDGE('',*,*,#12977,.T.);
#19396=ORIENTED_EDGE('',*,*,#12968,.F.);
#19397=ORIENTED_EDGE('',*,*,#12972,.T.);
#19398=ORIENTED_EDGE('',*,*,#13884,.T.);
#19399=ORIENTED_EDGE('',*,*,#13652,.T.);
#19400=ORIENTED_EDGE('',*,*,#12988,.F.);
#19401=ORIENTED_EDGE('',*,*,#12990,.T.);
#19402=ORIENTED_EDGE('',*,*,#12981,.F.);
#19403=ORIENTED_EDGE('',*,*,#12985,.T.);
#19404=ORIENTED_EDGE('',*,*,#13882,.T.);
#19405=ORIENTED_EDGE('',*,*,#13655,.T.);
#19406=ORIENTED_EDGE('',*,*,#13001,.F.);
#19407=ORIENTED_EDGE('',*,*,#13003,.T.);
#19408=ORIENTED_EDGE('',*,*,#12994,.F.);
#19409=ORIENTED_EDGE('',*,*,#12998,.T.);
#19410=ORIENTED_EDGE('',*,*,#13880,.T.);
#19411=ORIENTED_EDGE('',*,*,#13658,.T.);
#19412=ORIENTED_EDGE('',*,*,#13014,.F.);
#19413=ORIENTED_EDGE('',*,*,#13016,.T.);
#19414=ORIENTED_EDGE('',*,*,#13007,.F.);
#19415=ORIENTED_EDGE('',*,*,#13011,.T.);
#19416=ORIENTED_EDGE('',*,*,#13878,.T.);
#19417=ORIENTED_EDGE('',*,*,#13661,.T.);
#19418=ORIENTED_EDGE('',*,*,#13027,.F.);
#19419=ORIENTED_EDGE('',*,*,#13029,.T.);
#19420=ORIENTED_EDGE('',*,*,#13020,.F.);
#19421=ORIENTED_EDGE('',*,*,#13024,.T.);
#19422=ORIENTED_EDGE('',*,*,#13876,.T.);
#19423=ORIENTED_EDGE('',*,*,#13664,.T.);
#19424=ORIENTED_EDGE('',*,*,#13040,.F.);
#19425=ORIENTED_EDGE('',*,*,#13042,.T.);
#19426=ORIENTED_EDGE('',*,*,#13033,.F.);
#19427=ORIENTED_EDGE('',*,*,#13037,.T.);
#19428=ORIENTED_EDGE('',*,*,#13874,.T.);
#19429=ORIENTED_EDGE('',*,*,#13667,.T.);
#19430=ORIENTED_EDGE('',*,*,#13053,.F.);
#19431=ORIENTED_EDGE('',*,*,#13055,.T.);
#19432=ORIENTED_EDGE('',*,*,#13046,.F.);
#19433=ORIENTED_EDGE('',*,*,#13050,.T.);
#19434=ORIENTED_EDGE('',*,*,#13872,.T.);
#19435=ORIENTED_EDGE('',*,*,#13670,.T.);
#19436=ORIENTED_EDGE('',*,*,#13066,.F.);
#19437=ORIENTED_EDGE('',*,*,#13068,.T.);
#19438=ORIENTED_EDGE('',*,*,#13059,.F.);
#19439=ORIENTED_EDGE('',*,*,#13063,.T.);
#19440=ORIENTED_EDGE('',*,*,#13870,.T.);
#19441=ORIENTED_EDGE('',*,*,#13673,.T.);
#19442=ORIENTED_EDGE('',*,*,#13079,.F.);
#19443=ORIENTED_EDGE('',*,*,#13081,.T.);
#19444=ORIENTED_EDGE('',*,*,#13072,.F.);
#19445=ORIENTED_EDGE('',*,*,#13076,.T.);
#19446=ORIENTED_EDGE('',*,*,#13868,.T.);
#19447=ORIENTED_EDGE('',*,*,#13676,.T.);
#19448=ORIENTED_EDGE('',*,*,#13092,.F.);
#19449=ORIENTED_EDGE('',*,*,#13094,.T.);
#19450=ORIENTED_EDGE('',*,*,#13085,.F.);
#19451=ORIENTED_EDGE('',*,*,#13089,.T.);
#19452=ORIENTED_EDGE('',*,*,#13866,.T.);
#19453=ORIENTED_EDGE('',*,*,#13679,.T.);
#19454=ORIENTED_EDGE('',*,*,#13105,.F.);
#19455=ORIENTED_EDGE('',*,*,#13107,.T.);
#19456=ORIENTED_EDGE('',*,*,#13098,.F.);
#19457=ORIENTED_EDGE('',*,*,#13102,.T.);
#19458=ORIENTED_EDGE('',*,*,#13864,.T.);
#19459=ORIENTED_EDGE('',*,*,#13682,.T.);
#19460=ORIENTED_EDGE('',*,*,#13118,.F.);
#19461=ORIENTED_EDGE('',*,*,#13120,.T.);
#19462=ORIENTED_EDGE('',*,*,#13111,.F.);
#19463=ORIENTED_EDGE('',*,*,#13115,.T.);
#19464=ORIENTED_EDGE('',*,*,#13862,.T.);
#19465=ORIENTED_EDGE('',*,*,#13685,.T.);
#19466=ORIENTED_EDGE('',*,*,#13131,.F.);
#19467=ORIENTED_EDGE('',*,*,#13133,.T.);
#19468=ORIENTED_EDGE('',*,*,#13124,.F.);
#19469=ORIENTED_EDGE('',*,*,#13128,.T.);
#19470=ORIENTED_EDGE('',*,*,#13860,.T.);
#19471=ORIENTED_EDGE('',*,*,#13688,.T.);
#19472=ORIENTED_EDGE('',*,*,#13144,.F.);
#19473=ORIENTED_EDGE('',*,*,#13146,.T.);
#19474=ORIENTED_EDGE('',*,*,#13137,.F.);
#19475=ORIENTED_EDGE('',*,*,#13141,.T.);
#19476=ORIENTED_EDGE('',*,*,#13858,.T.);
#19477=ORIENTED_EDGE('',*,*,#13691,.T.);
#19478=ORIENTED_EDGE('',*,*,#13157,.F.);
#19479=ORIENTED_EDGE('',*,*,#13159,.T.);
#19480=ORIENTED_EDGE('',*,*,#13150,.F.);
#19481=ORIENTED_EDGE('',*,*,#13154,.T.);
#19482=ORIENTED_EDGE('',*,*,#13856,.T.);
#19483=ORIENTED_EDGE('',*,*,#13694,.T.);
#19484=ORIENTED_EDGE('',*,*,#13170,.F.);
#19485=ORIENTED_EDGE('',*,*,#13172,.T.);
#19486=ORIENTED_EDGE('',*,*,#13163,.F.);
#19487=ORIENTED_EDGE('',*,*,#13167,.T.);
#19488=ORIENTED_EDGE('',*,*,#13854,.T.);
#19489=ORIENTED_EDGE('',*,*,#13697,.T.);
#19490=ORIENTED_EDGE('',*,*,#13183,.F.);
#19491=ORIENTED_EDGE('',*,*,#13185,.T.);
#19492=ORIENTED_EDGE('',*,*,#13176,.F.);
#19493=ORIENTED_EDGE('',*,*,#13180,.T.);
#19494=ORIENTED_EDGE('',*,*,#13852,.T.);
#19495=ORIENTED_EDGE('',*,*,#13700,.T.);
#19496=ORIENTED_EDGE('',*,*,#13196,.F.);
#19497=ORIENTED_EDGE('',*,*,#13198,.T.);
#19498=ORIENTED_EDGE('',*,*,#13189,.F.);
#19499=ORIENTED_EDGE('',*,*,#13193,.T.);
#19500=ORIENTED_EDGE('',*,*,#13850,.T.);
#19501=ORIENTED_EDGE('',*,*,#13703,.T.);
#19502=ORIENTED_EDGE('',*,*,#13209,.F.);
#19503=ORIENTED_EDGE('',*,*,#13211,.T.);
#19504=ORIENTED_EDGE('',*,*,#13202,.F.);
#19505=ORIENTED_EDGE('',*,*,#13206,.T.);
#19506=ORIENTED_EDGE('',*,*,#13848,.T.);
#19507=ORIENTED_EDGE('',*,*,#13706,.T.);
#19508=ORIENTED_EDGE('',*,*,#13222,.F.);
#19509=ORIENTED_EDGE('',*,*,#13224,.T.);
#19510=ORIENTED_EDGE('',*,*,#13215,.F.);
#19511=ORIENTED_EDGE('',*,*,#13219,.T.);
#19512=ORIENTED_EDGE('',*,*,#13846,.T.);
#19513=ORIENTED_EDGE('',*,*,#13709,.T.);
#19514=ORIENTED_EDGE('',*,*,#13235,.F.);
#19515=ORIENTED_EDGE('',*,*,#13237,.T.);
#19516=ORIENTED_EDGE('',*,*,#13228,.F.);
#19517=ORIENTED_EDGE('',*,*,#13232,.T.);
#19518=ORIENTED_EDGE('',*,*,#13844,.T.);
#19519=ORIENTED_EDGE('',*,*,#13712,.T.);
#19520=ORIENTED_EDGE('',*,*,#13248,.F.);
#19521=ORIENTED_EDGE('',*,*,#13250,.T.);
#19522=ORIENTED_EDGE('',*,*,#13241,.F.);
#19523=ORIENTED_EDGE('',*,*,#13245,.T.);
#19524=ORIENTED_EDGE('',*,*,#13842,.T.);
#19525=ORIENTED_EDGE('',*,*,#13715,.T.);
#19526=ORIENTED_EDGE('',*,*,#13261,.F.);
#19527=ORIENTED_EDGE('',*,*,#13263,.T.);
#19528=ORIENTED_EDGE('',*,*,#13254,.F.);
#19529=ORIENTED_EDGE('',*,*,#13258,.T.);
#19530=ORIENTED_EDGE('',*,*,#13840,.T.);
#19531=ORIENTED_EDGE('',*,*,#13718,.T.);
#19532=ORIENTED_EDGE('',*,*,#13274,.F.);
#19533=ORIENTED_EDGE('',*,*,#13276,.T.);
#19534=ORIENTED_EDGE('',*,*,#13267,.F.);
#19535=ORIENTED_EDGE('',*,*,#13271,.T.);
#19536=ORIENTED_EDGE('',*,*,#13838,.T.);
#19537=ORIENTED_EDGE('',*,*,#13721,.T.);
#19538=ORIENTED_EDGE('',*,*,#13287,.F.);
#19539=ORIENTED_EDGE('',*,*,#13289,.T.);
#19540=ORIENTED_EDGE('',*,*,#13280,.F.);
#19541=ORIENTED_EDGE('',*,*,#13284,.T.);
#19542=ORIENTED_EDGE('',*,*,#13836,.T.);
#19543=ORIENTED_EDGE('',*,*,#13724,.T.);
#19544=ORIENTED_EDGE('',*,*,#13300,.F.);
#19545=ORIENTED_EDGE('',*,*,#13302,.T.);
#19546=ORIENTED_EDGE('',*,*,#13293,.F.);
#19547=ORIENTED_EDGE('',*,*,#13297,.T.);
#19548=ORIENTED_EDGE('',*,*,#13834,.T.);
#19549=ORIENTED_EDGE('',*,*,#13727,.T.);
#19550=ORIENTED_EDGE('',*,*,#13313,.F.);
#19551=ORIENTED_EDGE('',*,*,#13315,.T.);
#19552=ORIENTED_EDGE('',*,*,#13306,.F.);
#19553=ORIENTED_EDGE('',*,*,#13310,.T.);
#19554=ORIENTED_EDGE('',*,*,#13832,.T.);
#19555=ORIENTED_EDGE('',*,*,#13730,.T.);
#19556=ORIENTED_EDGE('',*,*,#13326,.F.);
#19557=ORIENTED_EDGE('',*,*,#13328,.T.);
#19558=ORIENTED_EDGE('',*,*,#13319,.F.);
#19559=ORIENTED_EDGE('',*,*,#13323,.T.);
#19560=ORIENTED_EDGE('',*,*,#13830,.T.);
#19561=ORIENTED_EDGE('',*,*,#13733,.T.);
#19562=ORIENTED_EDGE('',*,*,#13339,.F.);
#19563=ORIENTED_EDGE('',*,*,#13341,.T.);
#19564=ORIENTED_EDGE('',*,*,#13332,.F.);
#19565=ORIENTED_EDGE('',*,*,#13336,.T.);
#19566=ORIENTED_EDGE('',*,*,#13828,.T.);
#19567=ORIENTED_EDGE('',*,*,#13736,.T.);
#19568=ORIENTED_EDGE('',*,*,#13352,.F.);
#19569=ORIENTED_EDGE('',*,*,#13354,.T.);
#19570=ORIENTED_EDGE('',*,*,#13345,.F.);
#19571=ORIENTED_EDGE('',*,*,#13349,.T.);
#19572=ORIENTED_EDGE('',*,*,#13826,.T.);
#19573=ORIENTED_EDGE('',*,*,#13739,.T.);
#19574=ORIENTED_EDGE('',*,*,#13365,.F.);
#19575=ORIENTED_EDGE('',*,*,#13367,.T.);
#19576=ORIENTED_EDGE('',*,*,#13358,.F.);
#19577=ORIENTED_EDGE('',*,*,#13362,.T.);
#19578=ORIENTED_EDGE('',*,*,#13824,.T.);
#19579=ORIENTED_EDGE('',*,*,#13742,.T.);
#19580=ORIENTED_EDGE('',*,*,#13378,.F.);
#19581=ORIENTED_EDGE('',*,*,#13380,.T.);
#19582=ORIENTED_EDGE('',*,*,#13371,.F.);
#19583=ORIENTED_EDGE('',*,*,#13375,.T.);
#19584=ORIENTED_EDGE('',*,*,#13822,.T.);
#19585=ORIENTED_EDGE('',*,*,#13745,.T.);
#19586=ORIENTED_EDGE('',*,*,#13391,.F.);
#19587=ORIENTED_EDGE('',*,*,#13393,.T.);
#19588=ORIENTED_EDGE('',*,*,#13384,.F.);
#19589=ORIENTED_EDGE('',*,*,#13388,.T.);
#19590=ORIENTED_EDGE('',*,*,#13820,.T.);
#19591=ORIENTED_EDGE('',*,*,#13748,.T.);
#19592=ORIENTED_EDGE('',*,*,#13404,.F.);
#19593=ORIENTED_EDGE('',*,*,#13406,.T.);
#19594=ORIENTED_EDGE('',*,*,#13397,.F.);
#19595=ORIENTED_EDGE('',*,*,#13401,.T.);
#19596=ORIENTED_EDGE('',*,*,#13818,.T.);
#19597=ORIENTED_EDGE('',*,*,#13751,.T.);
#19598=ORIENTED_EDGE('',*,*,#13417,.F.);
#19599=ORIENTED_EDGE('',*,*,#13419,.T.);
#19600=ORIENTED_EDGE('',*,*,#13410,.F.);
#19601=ORIENTED_EDGE('',*,*,#13414,.T.);
#19602=ORIENTED_EDGE('',*,*,#13816,.T.);
#19603=ORIENTED_EDGE('',*,*,#13754,.T.);
#19604=ORIENTED_EDGE('',*,*,#13430,.F.);
#19605=ORIENTED_EDGE('',*,*,#13432,.T.);
#19606=ORIENTED_EDGE('',*,*,#13423,.F.);
#19607=ORIENTED_EDGE('',*,*,#13427,.T.);
#19608=ORIENTED_EDGE('',*,*,#13814,.T.);
#19609=ORIENTED_EDGE('',*,*,#13757,.T.);
#19610=ORIENTED_EDGE('',*,*,#13443,.F.);
#19611=ORIENTED_EDGE('',*,*,#13445,.T.);
#19612=ORIENTED_EDGE('',*,*,#13436,.F.);
#19613=ORIENTED_EDGE('',*,*,#13440,.T.);
#19614=ORIENTED_EDGE('',*,*,#13812,.T.);
#19615=ORIENTED_EDGE('',*,*,#13760,.T.);
#19616=ORIENTED_EDGE('',*,*,#13456,.F.);
#19617=ORIENTED_EDGE('',*,*,#13458,.T.);
#19618=ORIENTED_EDGE('',*,*,#13449,.F.);
#19619=ORIENTED_EDGE('',*,*,#13453,.T.);
#19620=ORIENTED_EDGE('',*,*,#13810,.T.);
#19621=ORIENTED_EDGE('',*,*,#13763,.T.);
#19622=ORIENTED_EDGE('',*,*,#13469,.F.);
#19623=ORIENTED_EDGE('',*,*,#13471,.T.);
#19624=ORIENTED_EDGE('',*,*,#13462,.F.);
#19625=ORIENTED_EDGE('',*,*,#13466,.T.);
#19626=ORIENTED_EDGE('',*,*,#13808,.T.);
#19627=ORIENTED_EDGE('',*,*,#13766,.T.);
#19628=ORIENTED_EDGE('',*,*,#13482,.F.);
#19629=ORIENTED_EDGE('',*,*,#13484,.T.);
#19630=ORIENTED_EDGE('',*,*,#13475,.F.);
#19631=ORIENTED_EDGE('',*,*,#13479,.T.);
#19632=ORIENTED_EDGE('',*,*,#13806,.T.);
#19633=ORIENTED_EDGE('',*,*,#13769,.T.);
#19634=ORIENTED_EDGE('',*,*,#13495,.F.);
#19635=ORIENTED_EDGE('',*,*,#13497,.T.);
#19636=ORIENTED_EDGE('',*,*,#13488,.F.);
#19637=ORIENTED_EDGE('',*,*,#13492,.T.);
#19638=ORIENTED_EDGE('',*,*,#13804,.T.);
#19639=ORIENTED_EDGE('',*,*,#13772,.T.);
#19640=ORIENTED_EDGE('',*,*,#13508,.F.);
#19641=ORIENTED_EDGE('',*,*,#13510,.T.);
#19642=ORIENTED_EDGE('',*,*,#13501,.F.);
#19643=ORIENTED_EDGE('',*,*,#13505,.T.);
#19644=ORIENTED_EDGE('',*,*,#13802,.T.);
#19645=ORIENTED_EDGE('',*,*,#13775,.T.);
#19646=ORIENTED_EDGE('',*,*,#13521,.F.);
#19647=ORIENTED_EDGE('',*,*,#13523,.T.);
#19648=ORIENTED_EDGE('',*,*,#13514,.F.);
#19649=ORIENTED_EDGE('',*,*,#13518,.T.);
#19650=ORIENTED_EDGE('',*,*,#13800,.T.);
#19651=ORIENTED_EDGE('',*,*,#13778,.T.);
#19652=ORIENTED_EDGE('',*,*,#13534,.F.);
#19653=ORIENTED_EDGE('',*,*,#13536,.T.);
#19654=ORIENTED_EDGE('',*,*,#13527,.F.);
#19655=ORIENTED_EDGE('',*,*,#13531,.T.);
#19656=ORIENTED_EDGE('',*,*,#13798,.T.);
#19657=ORIENTED_EDGE('',*,*,#13781,.T.);
#19658=ORIENTED_EDGE('',*,*,#13547,.F.);
#19659=ORIENTED_EDGE('',*,*,#13549,.T.);
#19660=ORIENTED_EDGE('',*,*,#13540,.F.);
#19661=ORIENTED_EDGE('',*,*,#13544,.T.);
#19662=ORIENTED_EDGE('',*,*,#13796,.T.);
#19663=ORIENTED_EDGE('',*,*,#13784,.T.);
#19664=ORIENTED_EDGE('',*,*,#13560,.F.);
#19665=ORIENTED_EDGE('',*,*,#13562,.T.);
#19666=ORIENTED_EDGE('',*,*,#13553,.F.);
#19667=ORIENTED_EDGE('',*,*,#13557,.T.);
#19668=ORIENTED_EDGE('',*,*,#13794,.T.);
#19669=ORIENTED_EDGE('',*,*,#13787,.T.);
#19670=ORIENTED_EDGE('',*,*,#13573,.F.);
#19671=ORIENTED_EDGE('',*,*,#13575,.T.);
#19672=ORIENTED_EDGE('',*,*,#13566,.F.);
#19673=ORIENTED_EDGE('',*,*,#13570,.T.);
#19674=ORIENTED_EDGE('',*,*,#13792,.T.);
#19675=ORIENTED_EDGE('',*,*,#13946,.T.);
#19676=ORIENTED_EDGE('',*,*,#13942,.F.);
#19677=ORIENTED_EDGE('',*,*,#13944,.T.);
#19678=ORIENTED_EDGE('',*,*,#13936,.F.);
#19679=ORIENTED_EDGE('',*,*,#13939,.T.);
#19680=ORIENTED_EDGE('',*,*,#13931,.T.);
#19681=ORIENTED_EDGE('',*,*,#13577,.T.);
#19682=ORIENTED_EDGE('',*,*,#12663,.F.);
#19683=ORIENTED_EDGE('',*,*,#12665,.T.);
#19684=ORIENTED_EDGE('',*,*,#12656,.F.);
#19685=ORIENTED_EDGE('',*,*,#12659,.T.);
#19686=ORIENTED_EDGE('',*,*,#13950,.T.);
#19687=ORIENTED_EDGE('',*,*,#13581,.T.);
#19688=ORIENTED_EDGE('',*,*,#13949,.F.);
#19689=ORIENTED_EDGE('',*,*,#13948,.F.);
#19690=ORIENTED_EDGE('',*,*,#13951,.T.);
#19691=ORIENTED_EDGE('',*,*,#12644,.T.);
#19692=ORIENTED_EDGE('',*,*,#13952,.T.);
#19693=ORIENTED_EDGE('',*,*,#13953,.T.);
#19694=ORIENTED_EDGE('',*,*,#13952,.F.);
#19695=ORIENTED_EDGE('',*,*,#12648,.T.);
#19696=ORIENTED_EDGE('',*,*,#12645,.T.);
#19697=ORIENTED_EDGE('',*,*,#13951,.F.);
#19698=ORIENTED_EDGE('',*,*,#12636,.T.);
#19699=ORIENTED_EDGE('',*,*,#12639,.T.);
#19700=ORIENTED_EDGE('',*,*,#12640,.T.);
#19701=ORIENTED_EDGE('',*,*,#12641,.T.);
#19702=ORIENTED_EDGE('',*,*,#12649,.T.);
#19703=ORIENTED_EDGE('',*,*,#12653,.T.);
#19704=ORIENTED_EDGE('',*,*,#12650,.T.);
#19705=ORIENTED_EDGE('',*,*,#13953,.F.);
#19706=ORIENTED_EDGE('',*,*,#12658,.T.);
#19707=ORIENTED_EDGE('',*,*,#12654,.F.);
#19708=ORIENTED_EDGE('',*,*,#12666,.T.);
#19709=ORIENTED_EDGE('',*,*,#12661,.F.);
#19710=ORIENTED_EDGE('',*,*,#13579,.T.);
#19711=ORIENTED_EDGE('',*,*,#13933,.F.);
#19712=ORIENTED_EDGE('',*,*,#13938,.T.);
#19713=ORIENTED_EDGE('',*,*,#13934,.F.);
#19714=ORIENTED_EDGE('',*,*,#13945,.T.);
#19715=ORIENTED_EDGE('',*,*,#13940,.F.);
#19716=ORIENTED_EDGE('',*,*,#13947,.T.);
#19717=ORIENTED_EDGE('',*,*,#13790,.F.);
#19718=ORIENTED_EDGE('',*,*,#13568,.T.);
#19719=ORIENTED_EDGE('',*,*,#13564,.F.);
#19720=ORIENTED_EDGE('',*,*,#13576,.T.);
#19721=ORIENTED_EDGE('',*,*,#13571,.F.);
#19722=ORIENTED_EDGE('',*,*,#13789,.T.);
#19723=ORIENTED_EDGE('',*,*,#13793,.F.);
#19724=ORIENTED_EDGE('',*,*,#13555,.T.);
#19725=ORIENTED_EDGE('',*,*,#13551,.F.);
#19726=ORIENTED_EDGE('',*,*,#13563,.T.);
#19727=ORIENTED_EDGE('',*,*,#13558,.F.);
#19728=ORIENTED_EDGE('',*,*,#13786,.T.);
#19729=ORIENTED_EDGE('',*,*,#13795,.F.);
#19730=ORIENTED_EDGE('',*,*,#13542,.T.);
#19731=ORIENTED_EDGE('',*,*,#13538,.F.);
#19732=ORIENTED_EDGE('',*,*,#13550,.T.);
#19733=ORIENTED_EDGE('',*,*,#13545,.F.);
#19734=ORIENTED_EDGE('',*,*,#13783,.T.);
#19735=ORIENTED_EDGE('',*,*,#13797,.F.);
#19736=ORIENTED_EDGE('',*,*,#13529,.T.);
#19737=ORIENTED_EDGE('',*,*,#13525,.F.);
#19738=ORIENTED_EDGE('',*,*,#13537,.T.);
#19739=ORIENTED_EDGE('',*,*,#13532,.F.);
#19740=ORIENTED_EDGE('',*,*,#13780,.T.);
#19741=ORIENTED_EDGE('',*,*,#13799,.F.);
#19742=ORIENTED_EDGE('',*,*,#13516,.T.);
#19743=ORIENTED_EDGE('',*,*,#13512,.F.);
#19744=ORIENTED_EDGE('',*,*,#13524,.T.);
#19745=ORIENTED_EDGE('',*,*,#13519,.F.);
#19746=ORIENTED_EDGE('',*,*,#13777,.T.);
#19747=ORIENTED_EDGE('',*,*,#13801,.F.);
#19748=ORIENTED_EDGE('',*,*,#13503,.T.);
#19749=ORIENTED_EDGE('',*,*,#13499,.F.);
#19750=ORIENTED_EDGE('',*,*,#13511,.T.);
#19751=ORIENTED_EDGE('',*,*,#13506,.F.);
#19752=ORIENTED_EDGE('',*,*,#13774,.T.);
#19753=ORIENTED_EDGE('',*,*,#13803,.F.);
#19754=ORIENTED_EDGE('',*,*,#13490,.T.);
#19755=ORIENTED_EDGE('',*,*,#13486,.F.);
#19756=ORIENTED_EDGE('',*,*,#13498,.T.);
#19757=ORIENTED_EDGE('',*,*,#13493,.F.);
#19758=ORIENTED_EDGE('',*,*,#13771,.T.);
#19759=ORIENTED_EDGE('',*,*,#13805,.F.);
#19760=ORIENTED_EDGE('',*,*,#13477,.T.);
#19761=ORIENTED_EDGE('',*,*,#13473,.F.);
#19762=ORIENTED_EDGE('',*,*,#13485,.T.);
#19763=ORIENTED_EDGE('',*,*,#13480,.F.);
#19764=ORIENTED_EDGE('',*,*,#13768,.T.);
#19765=ORIENTED_EDGE('',*,*,#13807,.F.);
#19766=ORIENTED_EDGE('',*,*,#13464,.T.);
#19767=ORIENTED_EDGE('',*,*,#13460,.F.);
#19768=ORIENTED_EDGE('',*,*,#13472,.T.);
#19769=ORIENTED_EDGE('',*,*,#13467,.F.);
#19770=ORIENTED_EDGE('',*,*,#13765,.T.);
#19771=ORIENTED_EDGE('',*,*,#13809,.F.);
#19772=ORIENTED_EDGE('',*,*,#13451,.T.);
#19773=ORIENTED_EDGE('',*,*,#13447,.F.);
#19774=ORIENTED_EDGE('',*,*,#13459,.T.);
#19775=ORIENTED_EDGE('',*,*,#13454,.F.);
#19776=ORIENTED_EDGE('',*,*,#13762,.T.);
#19777=ORIENTED_EDGE('',*,*,#13811,.F.);
#19778=ORIENTED_EDGE('',*,*,#13438,.T.);
#19779=ORIENTED_EDGE('',*,*,#13434,.F.);
#19780=ORIENTED_EDGE('',*,*,#13446,.T.);
#19781=ORIENTED_EDGE('',*,*,#13441,.F.);
#19782=ORIENTED_EDGE('',*,*,#13759,.T.);
#19783=ORIENTED_EDGE('',*,*,#13813,.F.);
#19784=ORIENTED_EDGE('',*,*,#13425,.T.);
#19785=ORIENTED_EDGE('',*,*,#13421,.F.);
#19786=ORIENTED_EDGE('',*,*,#13433,.T.);
#19787=ORIENTED_EDGE('',*,*,#13428,.F.);
#19788=ORIENTED_EDGE('',*,*,#13756,.T.);
#19789=ORIENTED_EDGE('',*,*,#13815,.F.);
#19790=ORIENTED_EDGE('',*,*,#13412,.T.);
#19791=ORIENTED_EDGE('',*,*,#13408,.F.);
#19792=ORIENTED_EDGE('',*,*,#13420,.T.);
#19793=ORIENTED_EDGE('',*,*,#13415,.F.);
#19794=ORIENTED_EDGE('',*,*,#13753,.T.);
#19795=ORIENTED_EDGE('',*,*,#13817,.F.);
#19796=ORIENTED_EDGE('',*,*,#13399,.T.);
#19797=ORIENTED_EDGE('',*,*,#13395,.F.);
#19798=ORIENTED_EDGE('',*,*,#13407,.T.);
#19799=ORIENTED_EDGE('',*,*,#13402,.F.);
#19800=ORIENTED_EDGE('',*,*,#13750,.T.);
#19801=ORIENTED_EDGE('',*,*,#13819,.F.);
#19802=ORIENTED_EDGE('',*,*,#13386,.T.);
#19803=ORIENTED_EDGE('',*,*,#13382,.F.);
#19804=ORIENTED_EDGE('',*,*,#13394,.T.);
#19805=ORIENTED_EDGE('',*,*,#13389,.F.);
#19806=ORIENTED_EDGE('',*,*,#13747,.T.);
#19807=ORIENTED_EDGE('',*,*,#13821,.F.);
#19808=ORIENTED_EDGE('',*,*,#13373,.T.);
#19809=ORIENTED_EDGE('',*,*,#13369,.F.);
#19810=ORIENTED_EDGE('',*,*,#13381,.T.);
#19811=ORIENTED_EDGE('',*,*,#13376,.F.);
#19812=ORIENTED_EDGE('',*,*,#13744,.T.);
#19813=ORIENTED_EDGE('',*,*,#13823,.F.);
#19814=ORIENTED_EDGE('',*,*,#13360,.T.);
#19815=ORIENTED_EDGE('',*,*,#13356,.F.);
#19816=ORIENTED_EDGE('',*,*,#13368,.T.);
#19817=ORIENTED_EDGE('',*,*,#13363,.F.);
#19818=ORIENTED_EDGE('',*,*,#13741,.T.);
#19819=ORIENTED_EDGE('',*,*,#13825,.F.);
#19820=ORIENTED_EDGE('',*,*,#13347,.T.);
#19821=ORIENTED_EDGE('',*,*,#13343,.F.);
#19822=ORIENTED_EDGE('',*,*,#13355,.T.);
#19823=ORIENTED_EDGE('',*,*,#13350,.F.);
#19824=ORIENTED_EDGE('',*,*,#13738,.T.);
#19825=ORIENTED_EDGE('',*,*,#13827,.F.);
#19826=ORIENTED_EDGE('',*,*,#13334,.T.);
#19827=ORIENTED_EDGE('',*,*,#13330,.F.);
#19828=ORIENTED_EDGE('',*,*,#13342,.T.);
#19829=ORIENTED_EDGE('',*,*,#13337,.F.);
#19830=ORIENTED_EDGE('',*,*,#13735,.T.);
#19831=ORIENTED_EDGE('',*,*,#13829,.F.);
#19832=ORIENTED_EDGE('',*,*,#13321,.T.);
#19833=ORIENTED_EDGE('',*,*,#13317,.F.);
#19834=ORIENTED_EDGE('',*,*,#13329,.T.);
#19835=ORIENTED_EDGE('',*,*,#13324,.F.);
#19836=ORIENTED_EDGE('',*,*,#13732,.T.);
#19837=ORIENTED_EDGE('',*,*,#13831,.F.);
#19838=ORIENTED_EDGE('',*,*,#13308,.T.);
#19839=ORIENTED_EDGE('',*,*,#13304,.F.);
#19840=ORIENTED_EDGE('',*,*,#13316,.T.);
#19841=ORIENTED_EDGE('',*,*,#13311,.F.);
#19842=ORIENTED_EDGE('',*,*,#13729,.T.);
#19843=ORIENTED_EDGE('',*,*,#13833,.F.);
#19844=ORIENTED_EDGE('',*,*,#13295,.T.);
#19845=ORIENTED_EDGE('',*,*,#13291,.F.);
#19846=ORIENTED_EDGE('',*,*,#13303,.T.);
#19847=ORIENTED_EDGE('',*,*,#13298,.F.);
#19848=ORIENTED_EDGE('',*,*,#13726,.T.);
#19849=ORIENTED_EDGE('',*,*,#13835,.F.);
#19850=ORIENTED_EDGE('',*,*,#13282,.T.);
#19851=ORIENTED_EDGE('',*,*,#13278,.F.);
#19852=ORIENTED_EDGE('',*,*,#13290,.T.);
#19853=ORIENTED_EDGE('',*,*,#13285,.F.);
#19854=ORIENTED_EDGE('',*,*,#13723,.T.);
#19855=ORIENTED_EDGE('',*,*,#13837,.F.);
#19856=ORIENTED_EDGE('',*,*,#13269,.T.);
#19857=ORIENTED_EDGE('',*,*,#13265,.F.);
#19858=ORIENTED_EDGE('',*,*,#13277,.T.);
#19859=ORIENTED_EDGE('',*,*,#13272,.F.);
#19860=ORIENTED_EDGE('',*,*,#13720,.T.);
#19861=ORIENTED_EDGE('',*,*,#13839,.F.);
#19862=ORIENTED_EDGE('',*,*,#13256,.T.);
#19863=ORIENTED_EDGE('',*,*,#13252,.F.);
#19864=ORIENTED_EDGE('',*,*,#13264,.T.);
#19865=ORIENTED_EDGE('',*,*,#13259,.F.);
#19866=ORIENTED_EDGE('',*,*,#13717,.T.);
#19867=ORIENTED_EDGE('',*,*,#13841,.F.);
#19868=ORIENTED_EDGE('',*,*,#13243,.T.);
#19869=ORIENTED_EDGE('',*,*,#13239,.F.);
#19870=ORIENTED_EDGE('',*,*,#13251,.T.);
#19871=ORIENTED_EDGE('',*,*,#13246,.F.);
#19872=ORIENTED_EDGE('',*,*,#13714,.T.);
#19873=ORIENTED_EDGE('',*,*,#13843,.F.);
#19874=ORIENTED_EDGE('',*,*,#13230,.T.);
#19875=ORIENTED_EDGE('',*,*,#13226,.F.);
#19876=ORIENTED_EDGE('',*,*,#13238,.T.);
#19877=ORIENTED_EDGE('',*,*,#13233,.F.);
#19878=ORIENTED_EDGE('',*,*,#13711,.T.);
#19879=ORIENTED_EDGE('',*,*,#13845,.F.);
#19880=ORIENTED_EDGE('',*,*,#13217,.T.);
#19881=ORIENTED_EDGE('',*,*,#13213,.F.);
#19882=ORIENTED_EDGE('',*,*,#13225,.T.);
#19883=ORIENTED_EDGE('',*,*,#13220,.F.);
#19884=ORIENTED_EDGE('',*,*,#13708,.T.);
#19885=ORIENTED_EDGE('',*,*,#13847,.F.);
#19886=ORIENTED_EDGE('',*,*,#13204,.T.);
#19887=ORIENTED_EDGE('',*,*,#13200,.F.);
#19888=ORIENTED_EDGE('',*,*,#13212,.T.);
#19889=ORIENTED_EDGE('',*,*,#13207,.F.);
#19890=ORIENTED_EDGE('',*,*,#13705,.T.);
#19891=ORIENTED_EDGE('',*,*,#13849,.F.);
#19892=ORIENTED_EDGE('',*,*,#13191,.T.);
#19893=ORIENTED_EDGE('',*,*,#13187,.F.);
#19894=ORIENTED_EDGE('',*,*,#13199,.T.);
#19895=ORIENTED_EDGE('',*,*,#13194,.F.);
#19896=ORIENTED_EDGE('',*,*,#13702,.T.);
#19897=ORIENTED_EDGE('',*,*,#13851,.F.);
#19898=ORIENTED_EDGE('',*,*,#13178,.T.);
#19899=ORIENTED_EDGE('',*,*,#13174,.F.);
#19900=ORIENTED_EDGE('',*,*,#13186,.T.);
#19901=ORIENTED_EDGE('',*,*,#13181,.F.);
#19902=ORIENTED_EDGE('',*,*,#13699,.T.);
#19903=ORIENTED_EDGE('',*,*,#13853,.F.);
#19904=ORIENTED_EDGE('',*,*,#13165,.T.);
#19905=ORIENTED_EDGE('',*,*,#13161,.F.);
#19906=ORIENTED_EDGE('',*,*,#13173,.T.);
#19907=ORIENTED_EDGE('',*,*,#13168,.F.);
#19908=ORIENTED_EDGE('',*,*,#13696,.T.);
#19909=ORIENTED_EDGE('',*,*,#13855,.F.);
#19910=ORIENTED_EDGE('',*,*,#13152,.T.);
#19911=ORIENTED_EDGE('',*,*,#13148,.F.);
#19912=ORIENTED_EDGE('',*,*,#13160,.T.);
#19913=ORIENTED_EDGE('',*,*,#13155,.F.);
#19914=ORIENTED_EDGE('',*,*,#13693,.T.);
#19915=ORIENTED_EDGE('',*,*,#13857,.F.);
#19916=ORIENTED_EDGE('',*,*,#13139,.T.);
#19917=ORIENTED_EDGE('',*,*,#13135,.F.);
#19918=ORIENTED_EDGE('',*,*,#13147,.T.);
#19919=ORIENTED_EDGE('',*,*,#13142,.F.);
#19920=ORIENTED_EDGE('',*,*,#13690,.T.);
#19921=ORIENTED_EDGE('',*,*,#13859,.F.);
#19922=ORIENTED_EDGE('',*,*,#13126,.T.);
#19923=ORIENTED_EDGE('',*,*,#13122,.F.);
#19924=ORIENTED_EDGE('',*,*,#13134,.T.);
#19925=ORIENTED_EDGE('',*,*,#13129,.F.);
#19926=ORIENTED_EDGE('',*,*,#13687,.T.);
#19927=ORIENTED_EDGE('',*,*,#13861,.F.);
#19928=ORIENTED_EDGE('',*,*,#13113,.T.);
#19929=ORIENTED_EDGE('',*,*,#13109,.F.);
#19930=ORIENTED_EDGE('',*,*,#13121,.T.);
#19931=ORIENTED_EDGE('',*,*,#13116,.F.);
#19932=ORIENTED_EDGE('',*,*,#13684,.T.);
#19933=ORIENTED_EDGE('',*,*,#13863,.F.);
#19934=ORIENTED_EDGE('',*,*,#13100,.T.);
#19935=ORIENTED_EDGE('',*,*,#13096,.F.);
#19936=ORIENTED_EDGE('',*,*,#13108,.T.);
#19937=ORIENTED_EDGE('',*,*,#13103,.F.);
#19938=ORIENTED_EDGE('',*,*,#13681,.T.);
#19939=ORIENTED_EDGE('',*,*,#13865,.F.);
#19940=ORIENTED_EDGE('',*,*,#13087,.T.);
#19941=ORIENTED_EDGE('',*,*,#13083,.F.);
#19942=ORIENTED_EDGE('',*,*,#13095,.T.);
#19943=ORIENTED_EDGE('',*,*,#13090,.F.);
#19944=ORIENTED_EDGE('',*,*,#13678,.T.);
#19945=ORIENTED_EDGE('',*,*,#13867,.F.);
#19946=ORIENTED_EDGE('',*,*,#13074,.T.);
#19947=ORIENTED_EDGE('',*,*,#13070,.F.);
#19948=ORIENTED_EDGE('',*,*,#13082,.T.);
#19949=ORIENTED_EDGE('',*,*,#13077,.F.);
#19950=ORIENTED_EDGE('',*,*,#13675,.T.);
#19951=ORIENTED_EDGE('',*,*,#13869,.F.);
#19952=ORIENTED_EDGE('',*,*,#13061,.T.);
#19953=ORIENTED_EDGE('',*,*,#13057,.F.);
#19954=ORIENTED_EDGE('',*,*,#13069,.T.);
#19955=ORIENTED_EDGE('',*,*,#13064,.F.);
#19956=ORIENTED_EDGE('',*,*,#13672,.T.);
#19957=ORIENTED_EDGE('',*,*,#13871,.F.);
#19958=ORIENTED_EDGE('',*,*,#13048,.T.);
#19959=ORIENTED_EDGE('',*,*,#13044,.F.);
#19960=ORIENTED_EDGE('',*,*,#13056,.T.);
#19961=ORIENTED_EDGE('',*,*,#13051,.F.);
#19962=ORIENTED_EDGE('',*,*,#13669,.T.);
#19963=ORIENTED_EDGE('',*,*,#13873,.F.);
#19964=ORIENTED_EDGE('',*,*,#13035,.T.);
#19965=ORIENTED_EDGE('',*,*,#13031,.F.);
#19966=ORIENTED_EDGE('',*,*,#13043,.T.);
#19967=ORIENTED_EDGE('',*,*,#13038,.F.);
#19968=ORIENTED_EDGE('',*,*,#13666,.T.);
#19969=ORIENTED_EDGE('',*,*,#13875,.F.);
#19970=ORIENTED_EDGE('',*,*,#13022,.T.);
#19971=ORIENTED_EDGE('',*,*,#13018,.F.);
#19972=ORIENTED_EDGE('',*,*,#13030,.T.);
#19973=ORIENTED_EDGE('',*,*,#13025,.F.);
#19974=ORIENTED_EDGE('',*,*,#13663,.T.);
#19975=ORIENTED_EDGE('',*,*,#13877,.F.);
#19976=ORIENTED_EDGE('',*,*,#13009,.T.);
#19977=ORIENTED_EDGE('',*,*,#13005,.F.);
#19978=ORIENTED_EDGE('',*,*,#13017,.T.);
#19979=ORIENTED_EDGE('',*,*,#13012,.F.);
#19980=ORIENTED_EDGE('',*,*,#13660,.T.);
#19981=ORIENTED_EDGE('',*,*,#13879,.F.);
#19982=ORIENTED_EDGE('',*,*,#12996,.T.);
#19983=ORIENTED_EDGE('',*,*,#12992,.F.);
#19984=ORIENTED_EDGE('',*,*,#13004,.T.);
#19985=ORIENTED_EDGE('',*,*,#12999,.F.);
#19986=ORIENTED_EDGE('',*,*,#13657,.T.);
#19987=ORIENTED_EDGE('',*,*,#13881,.F.);
#19988=ORIENTED_EDGE('',*,*,#12983,.T.);
#19989=ORIENTED_EDGE('',*,*,#12979,.F.);
#19990=ORIENTED_EDGE('',*,*,#12991,.T.);
#19991=ORIENTED_EDGE('',*,*,#12986,.F.);
#19992=ORIENTED_EDGE('',*,*,#13654,.T.);
#19993=ORIENTED_EDGE('',*,*,#13883,.F.);
#19994=ORIENTED_EDGE('',*,*,#12970,.T.);
#19995=ORIENTED_EDGE('',*,*,#12966,.F.);
#19996=ORIENTED_EDGE('',*,*,#12978,.T.);
#19997=ORIENTED_EDGE('',*,*,#12973,.F.);
#19998=ORIENTED_EDGE('',*,*,#13651,.T.);
#19999=ORIENTED_EDGE('',*,*,#13885,.F.);
#20000=ORIENTED_EDGE('',*,*,#12957,.T.);
#20001=ORIENTED_EDGE('',*,*,#12953,.F.);
#20002=ORIENTED_EDGE('',*,*,#12965,.T.);
#20003=ORIENTED_EDGE('',*,*,#12960,.F.);
#20004=ORIENTED_EDGE('',*,*,#13648,.T.);
#20005=ORIENTED_EDGE('',*,*,#13887,.F.);
#20006=ORIENTED_EDGE('',*,*,#12944,.T.);
#20007=ORIENTED_EDGE('',*,*,#12940,.F.);
#20008=ORIENTED_EDGE('',*,*,#12952,.T.);
#20009=ORIENTED_EDGE('',*,*,#12947,.F.);
#20010=ORIENTED_EDGE('',*,*,#13645,.T.);
#20011=ORIENTED_EDGE('',*,*,#13889,.F.);
#20012=ORIENTED_EDGE('',*,*,#12931,.T.);
#20013=ORIENTED_EDGE('',*,*,#12927,.F.);
#20014=ORIENTED_EDGE('',*,*,#12939,.T.);
#20015=ORIENTED_EDGE('',*,*,#12934,.F.);
#20016=ORIENTED_EDGE('',*,*,#13642,.T.);
#20017=ORIENTED_EDGE('',*,*,#13891,.F.);
#20018=ORIENTED_EDGE('',*,*,#12918,.T.);
#20019=ORIENTED_EDGE('',*,*,#12914,.F.);
#20020=ORIENTED_EDGE('',*,*,#12926,.T.);
#20021=ORIENTED_EDGE('',*,*,#12921,.F.);
#20022=ORIENTED_EDGE('',*,*,#13639,.T.);
#20023=ORIENTED_EDGE('',*,*,#13893,.F.);
#20024=ORIENTED_EDGE('',*,*,#12905,.T.);
#20025=ORIENTED_EDGE('',*,*,#12901,.F.);
#20026=ORIENTED_EDGE('',*,*,#12913,.T.);
#20027=ORIENTED_EDGE('',*,*,#12908,.F.);
#20028=ORIENTED_EDGE('',*,*,#13636,.T.);
#20029=ORIENTED_EDGE('',*,*,#13895,.F.);
#20030=ORIENTED_EDGE('',*,*,#12892,.T.);
#20031=ORIENTED_EDGE('',*,*,#12888,.F.);
#20032=ORIENTED_EDGE('',*,*,#12900,.T.);
#20033=ORIENTED_EDGE('',*,*,#12895,.F.);
#20034=ORIENTED_EDGE('',*,*,#13633,.T.);
#20035=ORIENTED_EDGE('',*,*,#13897,.F.);
#20036=ORIENTED_EDGE('',*,*,#12879,.T.);
#20037=ORIENTED_EDGE('',*,*,#12875,.F.);
#20038=ORIENTED_EDGE('',*,*,#12887,.T.);
#20039=ORIENTED_EDGE('',*,*,#12882,.F.);
#20040=ORIENTED_EDGE('',*,*,#13630,.T.);
#20041=ORIENTED_EDGE('',*,*,#13899,.F.);
#20042=ORIENTED_EDGE('',*,*,#12866,.T.);
#20043=ORIENTED_EDGE('',*,*,#12862,.F.);
#20044=ORIENTED_EDGE('',*,*,#12874,.T.);
#20045=ORIENTED_EDGE('',*,*,#12869,.F.);
#20046=ORIENTED_EDGE('',*,*,#13627,.T.);
#20047=ORIENTED_EDGE('',*,*,#13901,.F.);
#20048=ORIENTED_EDGE('',*,*,#12853,.T.);
#20049=ORIENTED_EDGE('',*,*,#12849,.F.);
#20050=ORIENTED_EDGE('',*,*,#12861,.T.);
#20051=ORIENTED_EDGE('',*,*,#12856,.F.);
#20052=ORIENTED_EDGE('',*,*,#13624,.T.);
#20053=ORIENTED_EDGE('',*,*,#13903,.F.);
#20054=ORIENTED_EDGE('',*,*,#12840,.T.);
#20055=ORIENTED_EDGE('',*,*,#12836,.F.);
#20056=ORIENTED_EDGE('',*,*,#12848,.T.);
#20057=ORIENTED_EDGE('',*,*,#12843,.F.);
#20058=ORIENTED_EDGE('',*,*,#13621,.T.);
#20059=ORIENTED_EDGE('',*,*,#13905,.F.);
#20060=ORIENTED_EDGE('',*,*,#12827,.T.);
#20061=ORIENTED_EDGE('',*,*,#12823,.F.);
#20062=ORIENTED_EDGE('',*,*,#12835,.T.);
#20063=ORIENTED_EDGE('',*,*,#12830,.F.);
#20064=ORIENTED_EDGE('',*,*,#13618,.T.);
#20065=ORIENTED_EDGE('',*,*,#13907,.F.);
#20066=ORIENTED_EDGE('',*,*,#12814,.T.);
#20067=ORIENTED_EDGE('',*,*,#12810,.F.);
#20068=ORIENTED_EDGE('',*,*,#12822,.T.);
#20069=ORIENTED_EDGE('',*,*,#12817,.F.);
#20070=ORIENTED_EDGE('',*,*,#13615,.T.);
#20071=ORIENTED_EDGE('',*,*,#13909,.F.);
#20072=ORIENTED_EDGE('',*,*,#12801,.T.);
#20073=ORIENTED_EDGE('',*,*,#12797,.F.);
#20074=ORIENTED_EDGE('',*,*,#12809,.T.);
#20075=ORIENTED_EDGE('',*,*,#12804,.F.);
#20076=ORIENTED_EDGE('',*,*,#13612,.T.);
#20077=ORIENTED_EDGE('',*,*,#13911,.F.);
#20078=ORIENTED_EDGE('',*,*,#12788,.T.);
#20079=ORIENTED_EDGE('',*,*,#12784,.F.);
#20080=ORIENTED_EDGE('',*,*,#12796,.T.);
#20081=ORIENTED_EDGE('',*,*,#12791,.F.);
#20082=ORIENTED_EDGE('',*,*,#13609,.T.);
#20083=ORIENTED_EDGE('',*,*,#13913,.F.);
#20084=ORIENTED_EDGE('',*,*,#12775,.T.);
#20085=ORIENTED_EDGE('',*,*,#12771,.F.);
#20086=ORIENTED_EDGE('',*,*,#12783,.T.);
#20087=ORIENTED_EDGE('',*,*,#12778,.F.);
#20088=ORIENTED_EDGE('',*,*,#13606,.T.);
#20089=ORIENTED_EDGE('',*,*,#13915,.F.);
#20090=ORIENTED_EDGE('',*,*,#12762,.T.);
#20091=ORIENTED_EDGE('',*,*,#12758,.F.);
#20092=ORIENTED_EDGE('',*,*,#12770,.T.);
#20093=ORIENTED_EDGE('',*,*,#12765,.F.);
#20094=ORIENTED_EDGE('',*,*,#13603,.T.);
#20095=ORIENTED_EDGE('',*,*,#13917,.F.);
#20096=ORIENTED_EDGE('',*,*,#12749,.T.);
#20097=ORIENTED_EDGE('',*,*,#12745,.F.);
#20098=ORIENTED_EDGE('',*,*,#12757,.T.);
#20099=ORIENTED_EDGE('',*,*,#12752,.F.);
#20100=ORIENTED_EDGE('',*,*,#13600,.T.);
#20101=ORIENTED_EDGE('',*,*,#13919,.F.);
#20102=ORIENTED_EDGE('',*,*,#12736,.T.);
#20103=ORIENTED_EDGE('',*,*,#12732,.F.);
#20104=ORIENTED_EDGE('',*,*,#12744,.T.);
#20105=ORIENTED_EDGE('',*,*,#12739,.F.);
#20106=ORIENTED_EDGE('',*,*,#13597,.T.);
#20107=ORIENTED_EDGE('',*,*,#13921,.F.);
#20108=ORIENTED_EDGE('',*,*,#12723,.T.);
#20109=ORIENTED_EDGE('',*,*,#12719,.F.);
#20110=ORIENTED_EDGE('',*,*,#12731,.T.);
#20111=ORIENTED_EDGE('',*,*,#12726,.F.);
#20112=ORIENTED_EDGE('',*,*,#13594,.T.);
#20113=ORIENTED_EDGE('',*,*,#13923,.F.);
#20114=ORIENTED_EDGE('',*,*,#12710,.T.);
#20115=ORIENTED_EDGE('',*,*,#12706,.F.);
#20116=ORIENTED_EDGE('',*,*,#12718,.T.);
#20117=ORIENTED_EDGE('',*,*,#12713,.F.);
#20118=ORIENTED_EDGE('',*,*,#13591,.T.);
#20119=ORIENTED_EDGE('',*,*,#13925,.F.);
#20120=ORIENTED_EDGE('',*,*,#12697,.T.);
#20121=ORIENTED_EDGE('',*,*,#12693,.F.);
#20122=ORIENTED_EDGE('',*,*,#12705,.T.);
#20123=ORIENTED_EDGE('',*,*,#12700,.F.);
#20124=ORIENTED_EDGE('',*,*,#13588,.T.);
#20125=ORIENTED_EDGE('',*,*,#13927,.F.);
#20126=ORIENTED_EDGE('',*,*,#12684,.T.);
#20127=ORIENTED_EDGE('',*,*,#12680,.F.);
#20128=ORIENTED_EDGE('',*,*,#12692,.T.);
#20129=ORIENTED_EDGE('',*,*,#12687,.F.);
#20130=ORIENTED_EDGE('',*,*,#13585,.T.);
#20131=ORIENTED_EDGE('',*,*,#13929,.F.);
#20132=ORIENTED_EDGE('',*,*,#12671,.T.);
#20133=ORIENTED_EDGE('',*,*,#12667,.F.);
#20134=ORIENTED_EDGE('',*,*,#12679,.T.);
#20135=ORIENTED_EDGE('',*,*,#12674,.F.);
#20136=ORIENTED_EDGE('',*,*,#13582,.T.);
#20137=ORIENTED_EDGE('',*,*,#13950,.F.);
#20138=ORIENTED_EDGE('',*,*,#13954,.F.);
#20139=ORIENTED_EDGE('',*,*,#13955,.F.);
#20140=ORIENTED_EDGE('',*,*,#13956,.F.);
#20141=ORIENTED_EDGE('',*,*,#13957,.F.);
#20142=ORIENTED_EDGE('',*,*,#13958,.F.);
#20143=ORIENTED_EDGE('',*,*,#13959,.F.);
#20144=ORIENTED_EDGE('',*,*,#13960,.T.);
#20145=ORIENTED_EDGE('',*,*,#13961,.F.);
#20146=ORIENTED_EDGE('',*,*,#13962,.F.);
#20147=ORIENTED_EDGE('',*,*,#13956,.T.);
#20148=ORIENTED_EDGE('',*,*,#13963,.F.);
#20149=ORIENTED_EDGE('',*,*,#13960,.F.);
#20150=ORIENTED_EDGE('',*,*,#13954,.T.);
#20151=ORIENTED_EDGE('',*,*,#13964,.F.);
#20152=ORIENTED_EDGE('',*,*,#13958,.T.);
#20153=ORIENTED_EDGE('',*,*,#13965,.T.);
#20154=ORIENTED_EDGE('',*,*,#13966,.T.);
#20155=ORIENTED_EDGE('',*,*,#13967,.T.);
#20156=ORIENTED_EDGE('',*,*,#13968,.T.);
#20157=ORIENTED_EDGE('',*,*,#13969,.T.);
#20158=ORIENTED_EDGE('',*,*,#13970,.F.);
#20159=ORIENTED_EDGE('',*,*,#13971,.T.);
#20160=ORIENTED_EDGE('',*,*,#13972,.F.);
#20161=ORIENTED_EDGE('',*,*,#13973,.T.);
#20162=ORIENTED_EDGE('',*,*,#13974,.T.);
#20163=ORIENTED_EDGE('',*,*,#13975,.T.);
#20164=ORIENTED_EDGE('',*,*,#13976,.T.);
#20165=ORIENTED_EDGE('',*,*,#13977,.T.);
#20166=ORIENTED_EDGE('',*,*,#13978,.F.);
#20167=ORIENTED_EDGE('',*,*,#13979,.T.);
#20168=ORIENTED_EDGE('',*,*,#13980,.F.);
#20169=ORIENTED_EDGE('',*,*,#13981,.T.);
#20170=ORIENTED_EDGE('',*,*,#13982,.T.);
#20171=ORIENTED_EDGE('',*,*,#13983,.T.);
#20172=ORIENTED_EDGE('',*,*,#13984,.T.);
#20173=ORIENTED_EDGE('',*,*,#13985,.T.);
#20174=ORIENTED_EDGE('',*,*,#13986,.F.);
#20175=ORIENTED_EDGE('',*,*,#13987,.T.);
#20176=ORIENTED_EDGE('',*,*,#13988,.F.);
#20177=ORIENTED_EDGE('',*,*,#13989,.T.);
#20178=ORIENTED_EDGE('',*,*,#13990,.T.);
#20179=ORIENTED_EDGE('',*,*,#13991,.T.);
#20180=ORIENTED_EDGE('',*,*,#13992,.T.);
#20181=ORIENTED_EDGE('',*,*,#13993,.T.);
#20182=ORIENTED_EDGE('',*,*,#13994,.F.);
#20183=ORIENTED_EDGE('',*,*,#13995,.T.);
#20184=ORIENTED_EDGE('',*,*,#13996,.F.);
#20185=ORIENTED_EDGE('',*,*,#13997,.T.);
#20186=ORIENTED_EDGE('',*,*,#13998,.T.);
#20187=ORIENTED_EDGE('',*,*,#13999,.T.);
#20188=ORIENTED_EDGE('',*,*,#14000,.T.);
#20189=ORIENTED_EDGE('',*,*,#14001,.T.);
#20190=ORIENTED_EDGE('',*,*,#14002,.F.);
#20191=ORIENTED_EDGE('',*,*,#14003,.T.);
#20192=ORIENTED_EDGE('',*,*,#14004,.F.);
#20193=ORIENTED_EDGE('',*,*,#14005,.T.);
#20194=ORIENTED_EDGE('',*,*,#14006,.T.);
#20195=ORIENTED_EDGE('',*,*,#14007,.T.);
#20196=ORIENTED_EDGE('',*,*,#14008,.T.);
#20197=ORIENTED_EDGE('',*,*,#14009,.T.);
#20198=ORIENTED_EDGE('',*,*,#14010,.F.);
#20199=ORIENTED_EDGE('',*,*,#14011,.T.);
#20200=ORIENTED_EDGE('',*,*,#14012,.F.);
#20201=ORIENTED_EDGE('',*,*,#14013,.T.);
#20202=ORIENTED_EDGE('',*,*,#14014,.T.);
#20203=ORIENTED_EDGE('',*,*,#14015,.T.);
#20204=ORIENTED_EDGE('',*,*,#14016,.T.);
#20205=ORIENTED_EDGE('',*,*,#14017,.T.);
#20206=ORIENTED_EDGE('',*,*,#14018,.F.);
#20207=ORIENTED_EDGE('',*,*,#14019,.T.);
#20208=ORIENTED_EDGE('',*,*,#14020,.F.);
#20209=ORIENTED_EDGE('',*,*,#14021,.T.);
#20210=ORIENTED_EDGE('',*,*,#14022,.T.);
#20211=ORIENTED_EDGE('',*,*,#14023,.T.);
#20212=ORIENTED_EDGE('',*,*,#14024,.T.);
#20213=ORIENTED_EDGE('',*,*,#14025,.T.);
#20214=ORIENTED_EDGE('',*,*,#14026,.F.);
#20215=ORIENTED_EDGE('',*,*,#14027,.T.);
#20216=ORIENTED_EDGE('',*,*,#14028,.F.);
#20217=ORIENTED_EDGE('',*,*,#14029,.T.);
#20218=ORIENTED_EDGE('',*,*,#14030,.T.);
#20219=ORIENTED_EDGE('',*,*,#14031,.T.);
#20220=ORIENTED_EDGE('',*,*,#14032,.T.);
#20221=ORIENTED_EDGE('',*,*,#14033,.T.);
#20222=ORIENTED_EDGE('',*,*,#14034,.F.);
#20223=ORIENTED_EDGE('',*,*,#14035,.T.);
#20224=ORIENTED_EDGE('',*,*,#14036,.F.);
#20225=ORIENTED_EDGE('',*,*,#14037,.T.);
#20226=ORIENTED_EDGE('',*,*,#14038,.T.);
#20227=ORIENTED_EDGE('',*,*,#14039,.T.);
#20228=ORIENTED_EDGE('',*,*,#14040,.T.);
#20229=ORIENTED_EDGE('',*,*,#14041,.T.);
#20230=ORIENTED_EDGE('',*,*,#14042,.F.);
#20231=ORIENTED_EDGE('',*,*,#14043,.T.);
#20232=ORIENTED_EDGE('',*,*,#14044,.F.);
#20233=ORIENTED_EDGE('',*,*,#14045,.T.);
#20234=ORIENTED_EDGE('',*,*,#14046,.T.);
#20235=ORIENTED_EDGE('',*,*,#14047,.T.);
#20236=ORIENTED_EDGE('',*,*,#14048,.T.);
#20237=ORIENTED_EDGE('',*,*,#14049,.T.);
#20238=ORIENTED_EDGE('',*,*,#14050,.F.);
#20239=ORIENTED_EDGE('',*,*,#14051,.T.);
#20240=ORIENTED_EDGE('',*,*,#14052,.F.);
#20241=ORIENTED_EDGE('',*,*,#14053,.T.);
#20242=ORIENTED_EDGE('',*,*,#14054,.T.);
#20243=ORIENTED_EDGE('',*,*,#14055,.T.);
#20244=ORIENTED_EDGE('',*,*,#14056,.T.);
#20245=ORIENTED_EDGE('',*,*,#14057,.T.);
#20246=ORIENTED_EDGE('',*,*,#14058,.F.);
#20247=ORIENTED_EDGE('',*,*,#14059,.T.);
#20248=ORIENTED_EDGE('',*,*,#14060,.F.);
#20249=ORIENTED_EDGE('',*,*,#14061,.T.);
#20250=ORIENTED_EDGE('',*,*,#14062,.T.);
#20251=ORIENTED_EDGE('',*,*,#14063,.T.);
#20252=ORIENTED_EDGE('',*,*,#14064,.T.);
#20253=ORIENTED_EDGE('',*,*,#14065,.T.);
#20254=ORIENTED_EDGE('',*,*,#14066,.F.);
#20255=ORIENTED_EDGE('',*,*,#14067,.T.);
#20256=ORIENTED_EDGE('',*,*,#14068,.F.);
#20257=ORIENTED_EDGE('',*,*,#14069,.T.);
#20258=ORIENTED_EDGE('',*,*,#14070,.T.);
#20259=ORIENTED_EDGE('',*,*,#14071,.T.);
#20260=ORIENTED_EDGE('',*,*,#14072,.T.);
#20261=ORIENTED_EDGE('',*,*,#14073,.T.);
#20262=ORIENTED_EDGE('',*,*,#14074,.F.);
#20263=ORIENTED_EDGE('',*,*,#14075,.T.);
#20264=ORIENTED_EDGE('',*,*,#14076,.F.);
#20265=ORIENTED_EDGE('',*,*,#14077,.T.);
#20266=ORIENTED_EDGE('',*,*,#14078,.T.);
#20267=ORIENTED_EDGE('',*,*,#14079,.T.);
#20268=ORIENTED_EDGE('',*,*,#14080,.T.);
#20269=ORIENTED_EDGE('',*,*,#14081,.T.);
#20270=ORIENTED_EDGE('',*,*,#14082,.F.);
#20271=ORIENTED_EDGE('',*,*,#14083,.T.);
#20272=ORIENTED_EDGE('',*,*,#14084,.F.);
#20273=ORIENTED_EDGE('',*,*,#14085,.T.);
#20274=ORIENTED_EDGE('',*,*,#14086,.T.);
#20275=ORIENTED_EDGE('',*,*,#14087,.T.);
#20276=ORIENTED_EDGE('',*,*,#14088,.T.);
#20277=ORIENTED_EDGE('',*,*,#14089,.T.);
#20278=ORIENTED_EDGE('',*,*,#14090,.F.);
#20279=ORIENTED_EDGE('',*,*,#14091,.T.);
#20280=ORIENTED_EDGE('',*,*,#14092,.F.);
#20281=ORIENTED_EDGE('',*,*,#14093,.T.);
#20282=ORIENTED_EDGE('',*,*,#14094,.T.);
#20283=ORIENTED_EDGE('',*,*,#14095,.T.);
#20284=ORIENTED_EDGE('',*,*,#14096,.T.);
#20285=ORIENTED_EDGE('',*,*,#14097,.T.);
#20286=ORIENTED_EDGE('',*,*,#14098,.F.);
#20287=ORIENTED_EDGE('',*,*,#14099,.T.);
#20288=ORIENTED_EDGE('',*,*,#14100,.F.);
#20289=ORIENTED_EDGE('',*,*,#14101,.T.);
#20290=ORIENTED_EDGE('',*,*,#14102,.T.);
#20291=ORIENTED_EDGE('',*,*,#14103,.T.);
#20292=ORIENTED_EDGE('',*,*,#14104,.T.);
#20293=ORIENTED_EDGE('',*,*,#14105,.T.);
#20294=ORIENTED_EDGE('',*,*,#14106,.F.);
#20295=ORIENTED_EDGE('',*,*,#14107,.T.);
#20296=ORIENTED_EDGE('',*,*,#14108,.F.);
#20297=ORIENTED_EDGE('',*,*,#14109,.T.);
#20298=ORIENTED_EDGE('',*,*,#14110,.T.);
#20299=ORIENTED_EDGE('',*,*,#14111,.T.);
#20300=ORIENTED_EDGE('',*,*,#14112,.T.);
#20301=ORIENTED_EDGE('',*,*,#14113,.T.);
#20302=ORIENTED_EDGE('',*,*,#14114,.F.);
#20303=ORIENTED_EDGE('',*,*,#14115,.T.);
#20304=ORIENTED_EDGE('',*,*,#14116,.F.);
#20305=ORIENTED_EDGE('',*,*,#14117,.T.);
#20306=ORIENTED_EDGE('',*,*,#14118,.T.);
#20307=ORIENTED_EDGE('',*,*,#14119,.T.);
#20308=ORIENTED_EDGE('',*,*,#14120,.T.);
#20309=ORIENTED_EDGE('',*,*,#14121,.T.);
#20310=ORIENTED_EDGE('',*,*,#14122,.F.);
#20311=ORIENTED_EDGE('',*,*,#14123,.T.);
#20312=ORIENTED_EDGE('',*,*,#14124,.F.);
#20313=ORIENTED_EDGE('',*,*,#14125,.T.);
#20314=ORIENTED_EDGE('',*,*,#14126,.T.);
#20315=ORIENTED_EDGE('',*,*,#14127,.T.);
#20316=ORIENTED_EDGE('',*,*,#14128,.T.);
#20317=ORIENTED_EDGE('',*,*,#14129,.T.);
#20318=ORIENTED_EDGE('',*,*,#14130,.F.);
#20319=ORIENTED_EDGE('',*,*,#14131,.T.);
#20320=ORIENTED_EDGE('',*,*,#14132,.F.);
#20321=ORIENTED_EDGE('',*,*,#14133,.T.);
#20322=ORIENTED_EDGE('',*,*,#14134,.T.);
#20323=ORIENTED_EDGE('',*,*,#14135,.T.);
#20324=ORIENTED_EDGE('',*,*,#14136,.T.);
#20325=ORIENTED_EDGE('',*,*,#14137,.T.);
#20326=ORIENTED_EDGE('',*,*,#14138,.F.);
#20327=ORIENTED_EDGE('',*,*,#14139,.T.);
#20328=ORIENTED_EDGE('',*,*,#14140,.F.);
#20329=ORIENTED_EDGE('',*,*,#14141,.T.);
#20330=ORIENTED_EDGE('',*,*,#14142,.T.);
#20331=ORIENTED_EDGE('',*,*,#14143,.T.);
#20332=ORIENTED_EDGE('',*,*,#14144,.T.);
#20333=ORIENTED_EDGE('',*,*,#14145,.T.);
#20334=ORIENTED_EDGE('',*,*,#14146,.F.);
#20335=ORIENTED_EDGE('',*,*,#14147,.T.);
#20336=ORIENTED_EDGE('',*,*,#14148,.F.);
#20337=ORIENTED_EDGE('',*,*,#14149,.T.);
#20338=ORIENTED_EDGE('',*,*,#14150,.T.);
#20339=ORIENTED_EDGE('',*,*,#14151,.T.);
#20340=ORIENTED_EDGE('',*,*,#14152,.T.);
#20341=ORIENTED_EDGE('',*,*,#14153,.T.);
#20342=ORIENTED_EDGE('',*,*,#14154,.F.);
#20343=ORIENTED_EDGE('',*,*,#14155,.T.);
#20344=ORIENTED_EDGE('',*,*,#14156,.F.);
#20345=ORIENTED_EDGE('',*,*,#14157,.T.);
#20346=ORIENTED_EDGE('',*,*,#13957,.T.);
#20347=ORIENTED_EDGE('',*,*,#13962,.T.);
#20348=ORIENTED_EDGE('',*,*,#13959,.T.);
#20349=ORIENTED_EDGE('',*,*,#13964,.T.);
#20350=ORIENTED_EDGE('',*,*,#14158,.T.);
#20351=ORIENTED_EDGE('',*,*,#14159,.T.);
#20352=ORIENTED_EDGE('',*,*,#14156,.T.);
#20353=ORIENTED_EDGE('',*,*,#14160,.T.);
#20354=ORIENTED_EDGE('',*,*,#14159,.F.);
#20355=ORIENTED_EDGE('',*,*,#14161,.F.);
#20356=ORIENTED_EDGE('',*,*,#14162,.T.);
#20357=ORIENTED_EDGE('',*,*,#14157,.F.);
#20358=ORIENTED_EDGE('',*,*,#14163,.T.);
#20359=ORIENTED_EDGE('',*,*,#14164,.T.);
#20360=ORIENTED_EDGE('',*,*,#14154,.T.);
#20361=ORIENTED_EDGE('',*,*,#14165,.T.);
#20362=ORIENTED_EDGE('',*,*,#14160,.F.);
#20363=ORIENTED_EDGE('',*,*,#14155,.F.);
#20364=ORIENTED_EDGE('',*,*,#14164,.F.);
#20365=ORIENTED_EDGE('',*,*,#14166,.F.);
#20366=ORIENTED_EDGE('',*,*,#14167,.T.);
#20367=ORIENTED_EDGE('',*,*,#14168,.T.);
#20368=ORIENTED_EDGE('',*,*,#14148,.T.);
#20369=ORIENTED_EDGE('',*,*,#14169,.T.);
#20370=ORIENTED_EDGE('',*,*,#14168,.F.);
#20371=ORIENTED_EDGE('',*,*,#14170,.F.);
#20372=ORIENTED_EDGE('',*,*,#14171,.T.);
#20373=ORIENTED_EDGE('',*,*,#14149,.F.);
#20374=ORIENTED_EDGE('',*,*,#14172,.T.);
#20375=ORIENTED_EDGE('',*,*,#14173,.T.);
#20376=ORIENTED_EDGE('',*,*,#14146,.T.);
#20377=ORIENTED_EDGE('',*,*,#14174,.T.);
#20378=ORIENTED_EDGE('',*,*,#14169,.F.);
#20379=ORIENTED_EDGE('',*,*,#14147,.F.);
#20380=ORIENTED_EDGE('',*,*,#14173,.F.);
#20381=ORIENTED_EDGE('',*,*,#14175,.F.);
#20382=ORIENTED_EDGE('',*,*,#14176,.T.);
#20383=ORIENTED_EDGE('',*,*,#14177,.T.);
#20384=ORIENTED_EDGE('',*,*,#14140,.T.);
#20385=ORIENTED_EDGE('',*,*,#14178,.T.);
#20386=ORIENTED_EDGE('',*,*,#14177,.F.);
#20387=ORIENTED_EDGE('',*,*,#14179,.F.);
#20388=ORIENTED_EDGE('',*,*,#14180,.T.);
#20389=ORIENTED_EDGE('',*,*,#14141,.F.);
#20390=ORIENTED_EDGE('',*,*,#14181,.T.);
#20391=ORIENTED_EDGE('',*,*,#14182,.T.);
#20392=ORIENTED_EDGE('',*,*,#14138,.T.);
#20393=ORIENTED_EDGE('',*,*,#14183,.T.);
#20394=ORIENTED_EDGE('',*,*,#14178,.F.);
#20395=ORIENTED_EDGE('',*,*,#14139,.F.);
#20396=ORIENTED_EDGE('',*,*,#14182,.F.);
#20397=ORIENTED_EDGE('',*,*,#14184,.F.);
#20398=ORIENTED_EDGE('',*,*,#14185,.T.);
#20399=ORIENTED_EDGE('',*,*,#14186,.T.);
#20400=ORIENTED_EDGE('',*,*,#14132,.T.);
#20401=ORIENTED_EDGE('',*,*,#14187,.T.);
#20402=ORIENTED_EDGE('',*,*,#14186,.F.);
#20403=ORIENTED_EDGE('',*,*,#14188,.F.);
#20404=ORIENTED_EDGE('',*,*,#14189,.T.);
#20405=ORIENTED_EDGE('',*,*,#14133,.F.);
#20406=ORIENTED_EDGE('',*,*,#14190,.T.);
#20407=ORIENTED_EDGE('',*,*,#14191,.T.);
#20408=ORIENTED_EDGE('',*,*,#14130,.T.);
#20409=ORIENTED_EDGE('',*,*,#14192,.T.);
#20410=ORIENTED_EDGE('',*,*,#14187,.F.);
#20411=ORIENTED_EDGE('',*,*,#14131,.F.);
#20412=ORIENTED_EDGE('',*,*,#14191,.F.);
#20413=ORIENTED_EDGE('',*,*,#14193,.F.);
#20414=ORIENTED_EDGE('',*,*,#14194,.T.);
#20415=ORIENTED_EDGE('',*,*,#14195,.T.);
#20416=ORIENTED_EDGE('',*,*,#14124,.T.);
#20417=ORIENTED_EDGE('',*,*,#14196,.T.);
#20418=ORIENTED_EDGE('',*,*,#14195,.F.);
#20419=ORIENTED_EDGE('',*,*,#14197,.F.);
#20420=ORIENTED_EDGE('',*,*,#14198,.T.);
#20421=ORIENTED_EDGE('',*,*,#14125,.F.);
#20422=ORIENTED_EDGE('',*,*,#14199,.T.);
#20423=ORIENTED_EDGE('',*,*,#14200,.T.);
#20424=ORIENTED_EDGE('',*,*,#14122,.T.);
#20425=ORIENTED_EDGE('',*,*,#14201,.T.);
#20426=ORIENTED_EDGE('',*,*,#14196,.F.);
#20427=ORIENTED_EDGE('',*,*,#14123,.F.);
#20428=ORIENTED_EDGE('',*,*,#14200,.F.);
#20429=ORIENTED_EDGE('',*,*,#14202,.F.);
#20430=ORIENTED_EDGE('',*,*,#14203,.T.);
#20431=ORIENTED_EDGE('',*,*,#14204,.T.);
#20432=ORIENTED_EDGE('',*,*,#14116,.T.);
#20433=ORIENTED_EDGE('',*,*,#14205,.T.);
#20434=ORIENTED_EDGE('',*,*,#14204,.F.);
#20435=ORIENTED_EDGE('',*,*,#14206,.F.);
#20436=ORIENTED_EDGE('',*,*,#14207,.T.);
#20437=ORIENTED_EDGE('',*,*,#14117,.F.);
#20438=ORIENTED_EDGE('',*,*,#14208,.T.);
#20439=ORIENTED_EDGE('',*,*,#14209,.T.);
#20440=ORIENTED_EDGE('',*,*,#14114,.T.);
#20441=ORIENTED_EDGE('',*,*,#14210,.T.);
#20442=ORIENTED_EDGE('',*,*,#14205,.F.);
#20443=ORIENTED_EDGE('',*,*,#14115,.F.);
#20444=ORIENTED_EDGE('',*,*,#14209,.F.);
#20445=ORIENTED_EDGE('',*,*,#14211,.F.);
#20446=ORIENTED_EDGE('',*,*,#14212,.T.);
#20447=ORIENTED_EDGE('',*,*,#14213,.T.);
#20448=ORIENTED_EDGE('',*,*,#14108,.T.);
#20449=ORIENTED_EDGE('',*,*,#14214,.T.);
#20450=ORIENTED_EDGE('',*,*,#14213,.F.);
#20451=ORIENTED_EDGE('',*,*,#14215,.F.);
#20452=ORIENTED_EDGE('',*,*,#14216,.T.);
#20453=ORIENTED_EDGE('',*,*,#14109,.F.);
#20454=ORIENTED_EDGE('',*,*,#14217,.T.);
#20455=ORIENTED_EDGE('',*,*,#14218,.T.);
#20456=ORIENTED_EDGE('',*,*,#14106,.T.);
#20457=ORIENTED_EDGE('',*,*,#14219,.T.);
#20458=ORIENTED_EDGE('',*,*,#14214,.F.);
#20459=ORIENTED_EDGE('',*,*,#14107,.F.);
#20460=ORIENTED_EDGE('',*,*,#14218,.F.);
#20461=ORIENTED_EDGE('',*,*,#14220,.F.);
#20462=ORIENTED_EDGE('',*,*,#14221,.T.);
#20463=ORIENTED_EDGE('',*,*,#14222,.T.);
#20464=ORIENTED_EDGE('',*,*,#14100,.T.);
#20465=ORIENTED_EDGE('',*,*,#14223,.T.);
#20466=ORIENTED_EDGE('',*,*,#14222,.F.);
#20467=ORIENTED_EDGE('',*,*,#14224,.F.);
#20468=ORIENTED_EDGE('',*,*,#14225,.T.);
#20469=ORIENTED_EDGE('',*,*,#14101,.F.);
#20470=ORIENTED_EDGE('',*,*,#14226,.T.);
#20471=ORIENTED_EDGE('',*,*,#14227,.T.);
#20472=ORIENTED_EDGE('',*,*,#14098,.T.);
#20473=ORIENTED_EDGE('',*,*,#14228,.T.);
#20474=ORIENTED_EDGE('',*,*,#14223,.F.);
#20475=ORIENTED_EDGE('',*,*,#14099,.F.);
#20476=ORIENTED_EDGE('',*,*,#14227,.F.);
#20477=ORIENTED_EDGE('',*,*,#14229,.F.);
#20478=ORIENTED_EDGE('',*,*,#14230,.T.);
#20479=ORIENTED_EDGE('',*,*,#14231,.T.);
#20480=ORIENTED_EDGE('',*,*,#14092,.T.);
#20481=ORIENTED_EDGE('',*,*,#14232,.T.);
#20482=ORIENTED_EDGE('',*,*,#14231,.F.);
#20483=ORIENTED_EDGE('',*,*,#14233,.F.);
#20484=ORIENTED_EDGE('',*,*,#14234,.T.);
#20485=ORIENTED_EDGE('',*,*,#14093,.F.);
#20486=ORIENTED_EDGE('',*,*,#14235,.T.);
#20487=ORIENTED_EDGE('',*,*,#14236,.T.);
#20488=ORIENTED_EDGE('',*,*,#14090,.T.);
#20489=ORIENTED_EDGE('',*,*,#14237,.T.);
#20490=ORIENTED_EDGE('',*,*,#14232,.F.);
#20491=ORIENTED_EDGE('',*,*,#14091,.F.);
#20492=ORIENTED_EDGE('',*,*,#14236,.F.);
#20493=ORIENTED_EDGE('',*,*,#14238,.F.);
#20494=ORIENTED_EDGE('',*,*,#14239,.T.);
#20495=ORIENTED_EDGE('',*,*,#14240,.T.);
#20496=ORIENTED_EDGE('',*,*,#14084,.T.);
#20497=ORIENTED_EDGE('',*,*,#14241,.T.);
#20498=ORIENTED_EDGE('',*,*,#14240,.F.);
#20499=ORIENTED_EDGE('',*,*,#14242,.F.);
#20500=ORIENTED_EDGE('',*,*,#14243,.T.);
#20501=ORIENTED_EDGE('',*,*,#14085,.F.);
#20502=ORIENTED_EDGE('',*,*,#14244,.T.);
#20503=ORIENTED_EDGE('',*,*,#14245,.T.);
#20504=ORIENTED_EDGE('',*,*,#14082,.T.);
#20505=ORIENTED_EDGE('',*,*,#14246,.T.);
#20506=ORIENTED_EDGE('',*,*,#14241,.F.);
#20507=ORIENTED_EDGE('',*,*,#14083,.F.);
#20508=ORIENTED_EDGE('',*,*,#14245,.F.);
#20509=ORIENTED_EDGE('',*,*,#14247,.F.);
#20510=ORIENTED_EDGE('',*,*,#14248,.T.);
#20511=ORIENTED_EDGE('',*,*,#14249,.T.);
#20512=ORIENTED_EDGE('',*,*,#14076,.T.);
#20513=ORIENTED_EDGE('',*,*,#14250,.T.);
#20514=ORIENTED_EDGE('',*,*,#14249,.F.);
#20515=ORIENTED_EDGE('',*,*,#14251,.F.);
#20516=ORIENTED_EDGE('',*,*,#14252,.T.);
#20517=ORIENTED_EDGE('',*,*,#14077,.F.);
#20518=ORIENTED_EDGE('',*,*,#14253,.T.);
#20519=ORIENTED_EDGE('',*,*,#14254,.T.);
#20520=ORIENTED_EDGE('',*,*,#14074,.T.);
#20521=ORIENTED_EDGE('',*,*,#14255,.T.);
#20522=ORIENTED_EDGE('',*,*,#14250,.F.);
#20523=ORIENTED_EDGE('',*,*,#14075,.F.);
#20524=ORIENTED_EDGE('',*,*,#14254,.F.);
#20525=ORIENTED_EDGE('',*,*,#14256,.F.);
#20526=ORIENTED_EDGE('',*,*,#14257,.T.);
#20527=ORIENTED_EDGE('',*,*,#14258,.T.);
#20528=ORIENTED_EDGE('',*,*,#14068,.T.);
#20529=ORIENTED_EDGE('',*,*,#14259,.T.);
#20530=ORIENTED_EDGE('',*,*,#14258,.F.);
#20531=ORIENTED_EDGE('',*,*,#14260,.F.);
#20532=ORIENTED_EDGE('',*,*,#14261,.T.);
#20533=ORIENTED_EDGE('',*,*,#14069,.F.);
#20534=ORIENTED_EDGE('',*,*,#14262,.T.);
#20535=ORIENTED_EDGE('',*,*,#14263,.T.);
#20536=ORIENTED_EDGE('',*,*,#14066,.T.);
#20537=ORIENTED_EDGE('',*,*,#14264,.T.);
#20538=ORIENTED_EDGE('',*,*,#14259,.F.);
#20539=ORIENTED_EDGE('',*,*,#14067,.F.);
#20540=ORIENTED_EDGE('',*,*,#14263,.F.);
#20541=ORIENTED_EDGE('',*,*,#14265,.F.);
#20542=ORIENTED_EDGE('',*,*,#14266,.T.);
#20543=ORIENTED_EDGE('',*,*,#14267,.T.);
#20544=ORIENTED_EDGE('',*,*,#14060,.T.);
#20545=ORIENTED_EDGE('',*,*,#14268,.T.);
#20546=ORIENTED_EDGE('',*,*,#14267,.F.);
#20547=ORIENTED_EDGE('',*,*,#14269,.F.);
#20548=ORIENTED_EDGE('',*,*,#14270,.T.);
#20549=ORIENTED_EDGE('',*,*,#14061,.F.);
#20550=ORIENTED_EDGE('',*,*,#14271,.T.);
#20551=ORIENTED_EDGE('',*,*,#14272,.T.);
#20552=ORIENTED_EDGE('',*,*,#14058,.T.);
#20553=ORIENTED_EDGE('',*,*,#14273,.T.);
#20554=ORIENTED_EDGE('',*,*,#14268,.F.);
#20555=ORIENTED_EDGE('',*,*,#14059,.F.);
#20556=ORIENTED_EDGE('',*,*,#14272,.F.);
#20557=ORIENTED_EDGE('',*,*,#14274,.F.);
#20558=ORIENTED_EDGE('',*,*,#14275,.T.);
#20559=ORIENTED_EDGE('',*,*,#14276,.T.);
#20560=ORIENTED_EDGE('',*,*,#14052,.T.);
#20561=ORIENTED_EDGE('',*,*,#14277,.T.);
#20562=ORIENTED_EDGE('',*,*,#14276,.F.);
#20563=ORIENTED_EDGE('',*,*,#14278,.F.);
#20564=ORIENTED_EDGE('',*,*,#14279,.T.);
#20565=ORIENTED_EDGE('',*,*,#14053,.F.);
#20566=ORIENTED_EDGE('',*,*,#14280,.T.);
#20567=ORIENTED_EDGE('',*,*,#14281,.T.);
#20568=ORIENTED_EDGE('',*,*,#14050,.T.);
#20569=ORIENTED_EDGE('',*,*,#14282,.T.);
#20570=ORIENTED_EDGE('',*,*,#14277,.F.);
#20571=ORIENTED_EDGE('',*,*,#14051,.F.);
#20572=ORIENTED_EDGE('',*,*,#14281,.F.);
#20573=ORIENTED_EDGE('',*,*,#14283,.F.);
#20574=ORIENTED_EDGE('',*,*,#14284,.T.);
#20575=ORIENTED_EDGE('',*,*,#14285,.T.);
#20576=ORIENTED_EDGE('',*,*,#14044,.T.);
#20577=ORIENTED_EDGE('',*,*,#14286,.T.);
#20578=ORIENTED_EDGE('',*,*,#14285,.F.);
#20579=ORIENTED_EDGE('',*,*,#14287,.F.);
#20580=ORIENTED_EDGE('',*,*,#14288,.T.);
#20581=ORIENTED_EDGE('',*,*,#14045,.F.);
#20582=ORIENTED_EDGE('',*,*,#14289,.T.);
#20583=ORIENTED_EDGE('',*,*,#14290,.T.);
#20584=ORIENTED_EDGE('',*,*,#14042,.T.);
#20585=ORIENTED_EDGE('',*,*,#14291,.T.);
#20586=ORIENTED_EDGE('',*,*,#14286,.F.);
#20587=ORIENTED_EDGE('',*,*,#14043,.F.);
#20588=ORIENTED_EDGE('',*,*,#14290,.F.);
#20589=ORIENTED_EDGE('',*,*,#14292,.F.);
#20590=ORIENTED_EDGE('',*,*,#14293,.T.);
#20591=ORIENTED_EDGE('',*,*,#14294,.T.);
#20592=ORIENTED_EDGE('',*,*,#14036,.T.);
#20593=ORIENTED_EDGE('',*,*,#14295,.T.);
#20594=ORIENTED_EDGE('',*,*,#14294,.F.);
#20595=ORIENTED_EDGE('',*,*,#14296,.F.);
#20596=ORIENTED_EDGE('',*,*,#14297,.T.);
#20597=ORIENTED_EDGE('',*,*,#14037,.F.);
#20598=ORIENTED_EDGE('',*,*,#14298,.T.);
#20599=ORIENTED_EDGE('',*,*,#14299,.T.);
#20600=ORIENTED_EDGE('',*,*,#14034,.T.);
#20601=ORIENTED_EDGE('',*,*,#14300,.T.);
#20602=ORIENTED_EDGE('',*,*,#14295,.F.);
#20603=ORIENTED_EDGE('',*,*,#14035,.F.);
#20604=ORIENTED_EDGE('',*,*,#14299,.F.);
#20605=ORIENTED_EDGE('',*,*,#14301,.F.);
#20606=ORIENTED_EDGE('',*,*,#14302,.T.);
#20607=ORIENTED_EDGE('',*,*,#14303,.T.);
#20608=ORIENTED_EDGE('',*,*,#14028,.T.);
#20609=ORIENTED_EDGE('',*,*,#14304,.T.);
#20610=ORIENTED_EDGE('',*,*,#14303,.F.);
#20611=ORIENTED_EDGE('',*,*,#14305,.F.);
#20612=ORIENTED_EDGE('',*,*,#14306,.T.);
#20613=ORIENTED_EDGE('',*,*,#14029,.F.);
#20614=ORIENTED_EDGE('',*,*,#14307,.T.);
#20615=ORIENTED_EDGE('',*,*,#14308,.T.);
#20616=ORIENTED_EDGE('',*,*,#14026,.T.);
#20617=ORIENTED_EDGE('',*,*,#14309,.T.);
#20618=ORIENTED_EDGE('',*,*,#14304,.F.);
#20619=ORIENTED_EDGE('',*,*,#14027,.F.);
#20620=ORIENTED_EDGE('',*,*,#14308,.F.);
#20621=ORIENTED_EDGE('',*,*,#14310,.F.);
#20622=ORIENTED_EDGE('',*,*,#14311,.T.);
#20623=ORIENTED_EDGE('',*,*,#14312,.T.);
#20624=ORIENTED_EDGE('',*,*,#14020,.T.);
#20625=ORIENTED_EDGE('',*,*,#14313,.T.);
#20626=ORIENTED_EDGE('',*,*,#14312,.F.);
#20627=ORIENTED_EDGE('',*,*,#14314,.F.);
#20628=ORIENTED_EDGE('',*,*,#14315,.T.);
#20629=ORIENTED_EDGE('',*,*,#14021,.F.);
#20630=ORIENTED_EDGE('',*,*,#14316,.T.);
#20631=ORIENTED_EDGE('',*,*,#14317,.T.);
#20632=ORIENTED_EDGE('',*,*,#14018,.T.);
#20633=ORIENTED_EDGE('',*,*,#14318,.T.);
#20634=ORIENTED_EDGE('',*,*,#14313,.F.);
#20635=ORIENTED_EDGE('',*,*,#14019,.F.);
#20636=ORIENTED_EDGE('',*,*,#14317,.F.);
#20637=ORIENTED_EDGE('',*,*,#14319,.F.);
#20638=ORIENTED_EDGE('',*,*,#14320,.T.);
#20639=ORIENTED_EDGE('',*,*,#14321,.T.);
#20640=ORIENTED_EDGE('',*,*,#14012,.T.);
#20641=ORIENTED_EDGE('',*,*,#14322,.T.);
#20642=ORIENTED_EDGE('',*,*,#14321,.F.);
#20643=ORIENTED_EDGE('',*,*,#14323,.F.);
#20644=ORIENTED_EDGE('',*,*,#14324,.T.);
#20645=ORIENTED_EDGE('',*,*,#14013,.F.);
#20646=ORIENTED_EDGE('',*,*,#14325,.T.);
#20647=ORIENTED_EDGE('',*,*,#14326,.T.);
#20648=ORIENTED_EDGE('',*,*,#14010,.T.);
#20649=ORIENTED_EDGE('',*,*,#14327,.T.);
#20650=ORIENTED_EDGE('',*,*,#14322,.F.);
#20651=ORIENTED_EDGE('',*,*,#14011,.F.);
#20652=ORIENTED_EDGE('',*,*,#14326,.F.);
#20653=ORIENTED_EDGE('',*,*,#14328,.F.);
#20654=ORIENTED_EDGE('',*,*,#14329,.T.);
#20655=ORIENTED_EDGE('',*,*,#14330,.T.);
#20656=ORIENTED_EDGE('',*,*,#14004,.T.);
#20657=ORIENTED_EDGE('',*,*,#14331,.T.);
#20658=ORIENTED_EDGE('',*,*,#14330,.F.);
#20659=ORIENTED_EDGE('',*,*,#14332,.F.);
#20660=ORIENTED_EDGE('',*,*,#14333,.T.);
#20661=ORIENTED_EDGE('',*,*,#14005,.F.);
#20662=ORIENTED_EDGE('',*,*,#14334,.T.);
#20663=ORIENTED_EDGE('',*,*,#14335,.T.);
#20664=ORIENTED_EDGE('',*,*,#14002,.T.);
#20665=ORIENTED_EDGE('',*,*,#14336,.T.);
#20666=ORIENTED_EDGE('',*,*,#14331,.F.);
#20667=ORIENTED_EDGE('',*,*,#14003,.F.);
#20668=ORIENTED_EDGE('',*,*,#14335,.F.);
#20669=ORIENTED_EDGE('',*,*,#14337,.F.);
#20670=ORIENTED_EDGE('',*,*,#14338,.T.);
#20671=ORIENTED_EDGE('',*,*,#14339,.T.);
#20672=ORIENTED_EDGE('',*,*,#13996,.T.);
#20673=ORIENTED_EDGE('',*,*,#14340,.T.);
#20674=ORIENTED_EDGE('',*,*,#14339,.F.);
#20675=ORIENTED_EDGE('',*,*,#14341,.F.);
#20676=ORIENTED_EDGE('',*,*,#14342,.T.);
#20677=ORIENTED_EDGE('',*,*,#13997,.F.);
#20678=ORIENTED_EDGE('',*,*,#14343,.T.);
#20679=ORIENTED_EDGE('',*,*,#14344,.T.);
#20680=ORIENTED_EDGE('',*,*,#13994,.T.);
#20681=ORIENTED_EDGE('',*,*,#14345,.T.);
#20682=ORIENTED_EDGE('',*,*,#14340,.F.);
#20683=ORIENTED_EDGE('',*,*,#13995,.F.);
#20684=ORIENTED_EDGE('',*,*,#14344,.F.);
#20685=ORIENTED_EDGE('',*,*,#14346,.F.);
#20686=ORIENTED_EDGE('',*,*,#14347,.T.);
#20687=ORIENTED_EDGE('',*,*,#14348,.T.);
#20688=ORIENTED_EDGE('',*,*,#13988,.T.);
#20689=ORIENTED_EDGE('',*,*,#14349,.T.);
#20690=ORIENTED_EDGE('',*,*,#14348,.F.);
#20691=ORIENTED_EDGE('',*,*,#14350,.F.);
#20692=ORIENTED_EDGE('',*,*,#14351,.T.);
#20693=ORIENTED_EDGE('',*,*,#13989,.F.);
#20694=ORIENTED_EDGE('',*,*,#14352,.T.);
#20695=ORIENTED_EDGE('',*,*,#14353,.T.);
#20696=ORIENTED_EDGE('',*,*,#13986,.T.);
#20697=ORIENTED_EDGE('',*,*,#14354,.T.);
#20698=ORIENTED_EDGE('',*,*,#14349,.F.);
#20699=ORIENTED_EDGE('',*,*,#13987,.F.);
#20700=ORIENTED_EDGE('',*,*,#14353,.F.);
#20701=ORIENTED_EDGE('',*,*,#14355,.F.);
#20702=ORIENTED_EDGE('',*,*,#14356,.T.);
#20703=ORIENTED_EDGE('',*,*,#14357,.T.);
#20704=ORIENTED_EDGE('',*,*,#13980,.T.);
#20705=ORIENTED_EDGE('',*,*,#14358,.T.);
#20706=ORIENTED_EDGE('',*,*,#14357,.F.);
#20707=ORIENTED_EDGE('',*,*,#14359,.F.);
#20708=ORIENTED_EDGE('',*,*,#14360,.T.);
#20709=ORIENTED_EDGE('',*,*,#13981,.F.);
#20710=ORIENTED_EDGE('',*,*,#14361,.T.);
#20711=ORIENTED_EDGE('',*,*,#14362,.T.);
#20712=ORIENTED_EDGE('',*,*,#13978,.T.);
#20713=ORIENTED_EDGE('',*,*,#14363,.T.);
#20714=ORIENTED_EDGE('',*,*,#14358,.F.);
#20715=ORIENTED_EDGE('',*,*,#13979,.F.);
#20716=ORIENTED_EDGE('',*,*,#14362,.F.);
#20717=ORIENTED_EDGE('',*,*,#14364,.F.);
#20718=ORIENTED_EDGE('',*,*,#14165,.F.);
#20719=ORIENTED_EDGE('',*,*,#14153,.F.);
#20720=ORIENTED_EDGE('',*,*,#14365,.F.);
#20721=ORIENTED_EDGE('',*,*,#14366,.F.);
#20722=ORIENTED_EDGE('',*,*,#14367,.F.);
#20723=ORIENTED_EDGE('',*,*,#14368,.F.);
#20724=ORIENTED_EDGE('',*,*,#13966,.F.);
#20725=ORIENTED_EDGE('',*,*,#14162,.F.);
#20726=ORIENTED_EDGE('',*,*,#14369,.F.);
#20727=ORIENTED_EDGE('',*,*,#14365,.T.);
#20728=ORIENTED_EDGE('',*,*,#14152,.F.);
#20729=ORIENTED_EDGE('',*,*,#14370,.F.);
#20730=ORIENTED_EDGE('',*,*,#14174,.F.);
#20731=ORIENTED_EDGE('',*,*,#14145,.F.);
#20732=ORIENTED_EDGE('',*,*,#14371,.F.);
#20733=ORIENTED_EDGE('',*,*,#14372,.F.);
#20734=ORIENTED_EDGE('',*,*,#14373,.F.);
#20735=ORIENTED_EDGE('',*,*,#14374,.F.);
#20736=ORIENTED_EDGE('',*,*,#14150,.F.);
#20737=ORIENTED_EDGE('',*,*,#14171,.F.);
#20738=ORIENTED_EDGE('',*,*,#14375,.F.);
#20739=ORIENTED_EDGE('',*,*,#14371,.T.);
#20740=ORIENTED_EDGE('',*,*,#14144,.F.);
#20741=ORIENTED_EDGE('',*,*,#14376,.F.);
#20742=ORIENTED_EDGE('',*,*,#14183,.F.);
#20743=ORIENTED_EDGE('',*,*,#14137,.F.);
#20744=ORIENTED_EDGE('',*,*,#14377,.F.);
#20745=ORIENTED_EDGE('',*,*,#14378,.F.);
#20746=ORIENTED_EDGE('',*,*,#14379,.F.);
#20747=ORIENTED_EDGE('',*,*,#14380,.F.);
#20748=ORIENTED_EDGE('',*,*,#14142,.F.);
#20749=ORIENTED_EDGE('',*,*,#14180,.F.);
#20750=ORIENTED_EDGE('',*,*,#14381,.F.);
#20751=ORIENTED_EDGE('',*,*,#14377,.T.);
#20752=ORIENTED_EDGE('',*,*,#14136,.F.);
#20753=ORIENTED_EDGE('',*,*,#14382,.F.);
#20754=ORIENTED_EDGE('',*,*,#14192,.F.);
#20755=ORIENTED_EDGE('',*,*,#14129,.F.);
#20756=ORIENTED_EDGE('',*,*,#14383,.F.);
#20757=ORIENTED_EDGE('',*,*,#14384,.F.);
#20758=ORIENTED_EDGE('',*,*,#14385,.F.);
#20759=ORIENTED_EDGE('',*,*,#14386,.F.);
#20760=ORIENTED_EDGE('',*,*,#14134,.F.);
#20761=ORIENTED_EDGE('',*,*,#14189,.F.);
#20762=ORIENTED_EDGE('',*,*,#14387,.F.);
#20763=ORIENTED_EDGE('',*,*,#14383,.T.);
#20764=ORIENTED_EDGE('',*,*,#14128,.F.);
#20765=ORIENTED_EDGE('',*,*,#14388,.F.);
#20766=ORIENTED_EDGE('',*,*,#14201,.F.);
#20767=ORIENTED_EDGE('',*,*,#14121,.F.);
#20768=ORIENTED_EDGE('',*,*,#14389,.F.);
#20769=ORIENTED_EDGE('',*,*,#14390,.F.);
#20770=ORIENTED_EDGE('',*,*,#14391,.F.);
#20771=ORIENTED_EDGE('',*,*,#14392,.F.);
#20772=ORIENTED_EDGE('',*,*,#14126,.F.);
#20773=ORIENTED_EDGE('',*,*,#14198,.F.);
#20774=ORIENTED_EDGE('',*,*,#14393,.F.);
#20775=ORIENTED_EDGE('',*,*,#14389,.T.);
#20776=ORIENTED_EDGE('',*,*,#14120,.F.);
#20777=ORIENTED_EDGE('',*,*,#14394,.F.);
#20778=ORIENTED_EDGE('',*,*,#14210,.F.);
#20779=ORIENTED_EDGE('',*,*,#14113,.F.);
#20780=ORIENTED_EDGE('',*,*,#14395,.F.);
#20781=ORIENTED_EDGE('',*,*,#14396,.F.);
#20782=ORIENTED_EDGE('',*,*,#14397,.F.);
#20783=ORIENTED_EDGE('',*,*,#14398,.F.);
#20784=ORIENTED_EDGE('',*,*,#14118,.F.);
#20785=ORIENTED_EDGE('',*,*,#14207,.F.);
#20786=ORIENTED_EDGE('',*,*,#14399,.F.);
#20787=ORIENTED_EDGE('',*,*,#14395,.T.);
#20788=ORIENTED_EDGE('',*,*,#14112,.F.);
#20789=ORIENTED_EDGE('',*,*,#14400,.F.);
#20790=ORIENTED_EDGE('',*,*,#14219,.F.);
#20791=ORIENTED_EDGE('',*,*,#14105,.F.);
#20792=ORIENTED_EDGE('',*,*,#14401,.F.);
#20793=ORIENTED_EDGE('',*,*,#14402,.F.);
#20794=ORIENTED_EDGE('',*,*,#14403,.F.);
#20795=ORIENTED_EDGE('',*,*,#14404,.F.);
#20796=ORIENTED_EDGE('',*,*,#14110,.F.);
#20797=ORIENTED_EDGE('',*,*,#14216,.F.);
#20798=ORIENTED_EDGE('',*,*,#14405,.F.);
#20799=ORIENTED_EDGE('',*,*,#14401,.T.);
#20800=ORIENTED_EDGE('',*,*,#14104,.F.);
#20801=ORIENTED_EDGE('',*,*,#14406,.F.);
#20802=ORIENTED_EDGE('',*,*,#14228,.F.);
#20803=ORIENTED_EDGE('',*,*,#14097,.F.);
#20804=ORIENTED_EDGE('',*,*,#14407,.F.);
#20805=ORIENTED_EDGE('',*,*,#14408,.F.);
#20806=ORIENTED_EDGE('',*,*,#14409,.F.);
#20807=ORIENTED_EDGE('',*,*,#14410,.F.);
#20808=ORIENTED_EDGE('',*,*,#14102,.F.);
#20809=ORIENTED_EDGE('',*,*,#14225,.F.);
#20810=ORIENTED_EDGE('',*,*,#14411,.F.);
#20811=ORIENTED_EDGE('',*,*,#14407,.T.);
#20812=ORIENTED_EDGE('',*,*,#14096,.F.);
#20813=ORIENTED_EDGE('',*,*,#14412,.F.);
#20814=ORIENTED_EDGE('',*,*,#14237,.F.);
#20815=ORIENTED_EDGE('',*,*,#14089,.F.);
#20816=ORIENTED_EDGE('',*,*,#14413,.F.);
#20817=ORIENTED_EDGE('',*,*,#14414,.F.);
#20818=ORIENTED_EDGE('',*,*,#14415,.F.);
#20819=ORIENTED_EDGE('',*,*,#14416,.F.);
#20820=ORIENTED_EDGE('',*,*,#14094,.F.);
#20821=ORIENTED_EDGE('',*,*,#14234,.F.);
#20822=ORIENTED_EDGE('',*,*,#14417,.F.);
#20823=ORIENTED_EDGE('',*,*,#14413,.T.);
#20824=ORIENTED_EDGE('',*,*,#14088,.F.);
#20825=ORIENTED_EDGE('',*,*,#14418,.F.);
#20826=ORIENTED_EDGE('',*,*,#14246,.F.);
#20827=ORIENTED_EDGE('',*,*,#14081,.F.);
#20828=ORIENTED_EDGE('',*,*,#14419,.F.);
#20829=ORIENTED_EDGE('',*,*,#14420,.F.);
#20830=ORIENTED_EDGE('',*,*,#14421,.F.);
#20831=ORIENTED_EDGE('',*,*,#14422,.F.);
#20832=ORIENTED_EDGE('',*,*,#14086,.F.);
#20833=ORIENTED_EDGE('',*,*,#14243,.F.);
#20834=ORIENTED_EDGE('',*,*,#14423,.F.);
#20835=ORIENTED_EDGE('',*,*,#14419,.T.);
#20836=ORIENTED_EDGE('',*,*,#14080,.F.);
#20837=ORIENTED_EDGE('',*,*,#14424,.F.);
#20838=ORIENTED_EDGE('',*,*,#14255,.F.);
#20839=ORIENTED_EDGE('',*,*,#14073,.F.);
#20840=ORIENTED_EDGE('',*,*,#14425,.F.);
#20841=ORIENTED_EDGE('',*,*,#14426,.F.);
#20842=ORIENTED_EDGE('',*,*,#14427,.F.);
#20843=ORIENTED_EDGE('',*,*,#14428,.F.);
#20844=ORIENTED_EDGE('',*,*,#14078,.F.);
#20845=ORIENTED_EDGE('',*,*,#14252,.F.);
#20846=ORIENTED_EDGE('',*,*,#14429,.F.);
#20847=ORIENTED_EDGE('',*,*,#14425,.T.);
#20848=ORIENTED_EDGE('',*,*,#14072,.F.);
#20849=ORIENTED_EDGE('',*,*,#14430,.F.);
#20850=ORIENTED_EDGE('',*,*,#14264,.F.);
#20851=ORIENTED_EDGE('',*,*,#14065,.F.);
#20852=ORIENTED_EDGE('',*,*,#14431,.F.);
#20853=ORIENTED_EDGE('',*,*,#14432,.F.);
#20854=ORIENTED_EDGE('',*,*,#14433,.F.);
#20855=ORIENTED_EDGE('',*,*,#14434,.F.);
#20856=ORIENTED_EDGE('',*,*,#14070,.F.);
#20857=ORIENTED_EDGE('',*,*,#14261,.F.);
#20858=ORIENTED_EDGE('',*,*,#14435,.F.);
#20859=ORIENTED_EDGE('',*,*,#14431,.T.);
#20860=ORIENTED_EDGE('',*,*,#14064,.F.);
#20861=ORIENTED_EDGE('',*,*,#14436,.F.);
#20862=ORIENTED_EDGE('',*,*,#14273,.F.);
#20863=ORIENTED_EDGE('',*,*,#14057,.F.);
#20864=ORIENTED_EDGE('',*,*,#14437,.F.);
#20865=ORIENTED_EDGE('',*,*,#14438,.F.);
#20866=ORIENTED_EDGE('',*,*,#14439,.F.);
#20867=ORIENTED_EDGE('',*,*,#14440,.F.);
#20868=ORIENTED_EDGE('',*,*,#14062,.F.);
#20869=ORIENTED_EDGE('',*,*,#14270,.F.);
#20870=ORIENTED_EDGE('',*,*,#14441,.F.);
#20871=ORIENTED_EDGE('',*,*,#14437,.T.);
#20872=ORIENTED_EDGE('',*,*,#14056,.F.);
#20873=ORIENTED_EDGE('',*,*,#14442,.F.);
#20874=ORIENTED_EDGE('',*,*,#14282,.F.);
#20875=ORIENTED_EDGE('',*,*,#14049,.F.);
#20876=ORIENTED_EDGE('',*,*,#14443,.F.);
#20877=ORIENTED_EDGE('',*,*,#14444,.F.);
#20878=ORIENTED_EDGE('',*,*,#14445,.F.);
#20879=ORIENTED_EDGE('',*,*,#14446,.F.);
#20880=ORIENTED_EDGE('',*,*,#14054,.F.);
#20881=ORIENTED_EDGE('',*,*,#14279,.F.);
#20882=ORIENTED_EDGE('',*,*,#14447,.F.);
#20883=ORIENTED_EDGE('',*,*,#14443,.T.);
#20884=ORIENTED_EDGE('',*,*,#14048,.F.);
#20885=ORIENTED_EDGE('',*,*,#14448,.F.);
#20886=ORIENTED_EDGE('',*,*,#14291,.F.);
#20887=ORIENTED_EDGE('',*,*,#14041,.F.);
#20888=ORIENTED_EDGE('',*,*,#14449,.F.);
#20889=ORIENTED_EDGE('',*,*,#14450,.F.);
#20890=ORIENTED_EDGE('',*,*,#14451,.F.);
#20891=ORIENTED_EDGE('',*,*,#14452,.F.);
#20892=ORIENTED_EDGE('',*,*,#14046,.F.);
#20893=ORIENTED_EDGE('',*,*,#14288,.F.);
#20894=ORIENTED_EDGE('',*,*,#14453,.F.);
#20895=ORIENTED_EDGE('',*,*,#14449,.T.);
#20896=ORIENTED_EDGE('',*,*,#14040,.F.);
#20897=ORIENTED_EDGE('',*,*,#14454,.F.);
#20898=ORIENTED_EDGE('',*,*,#14300,.F.);
#20899=ORIENTED_EDGE('',*,*,#14033,.F.);
#20900=ORIENTED_EDGE('',*,*,#14455,.F.);
#20901=ORIENTED_EDGE('',*,*,#14456,.F.);
#20902=ORIENTED_EDGE('',*,*,#14457,.F.);
#20903=ORIENTED_EDGE('',*,*,#14458,.F.);
#20904=ORIENTED_EDGE('',*,*,#14038,.F.);
#20905=ORIENTED_EDGE('',*,*,#14297,.F.);
#20906=ORIENTED_EDGE('',*,*,#14459,.F.);
#20907=ORIENTED_EDGE('',*,*,#14455,.T.);
#20908=ORIENTED_EDGE('',*,*,#14032,.F.);
#20909=ORIENTED_EDGE('',*,*,#14460,.F.);
#20910=ORIENTED_EDGE('',*,*,#14309,.F.);
#20911=ORIENTED_EDGE('',*,*,#14025,.F.);
#20912=ORIENTED_EDGE('',*,*,#14461,.F.);
#20913=ORIENTED_EDGE('',*,*,#14462,.F.);
#20914=ORIENTED_EDGE('',*,*,#14463,.F.);
#20915=ORIENTED_EDGE('',*,*,#14464,.F.);
#20916=ORIENTED_EDGE('',*,*,#14030,.F.);
#20917=ORIENTED_EDGE('',*,*,#14306,.F.);
#20918=ORIENTED_EDGE('',*,*,#14465,.F.);
#20919=ORIENTED_EDGE('',*,*,#14461,.T.);
#20920=ORIENTED_EDGE('',*,*,#14024,.F.);
#20921=ORIENTED_EDGE('',*,*,#14466,.F.);
#20922=ORIENTED_EDGE('',*,*,#14318,.F.);
#20923=ORIENTED_EDGE('',*,*,#14017,.F.);
#20924=ORIENTED_EDGE('',*,*,#14467,.F.);
#20925=ORIENTED_EDGE('',*,*,#14468,.F.);
#20926=ORIENTED_EDGE('',*,*,#14469,.F.);
#20927=ORIENTED_EDGE('',*,*,#14470,.F.);
#20928=ORIENTED_EDGE('',*,*,#14022,.F.);
#20929=ORIENTED_EDGE('',*,*,#14315,.F.);
#20930=ORIENTED_EDGE('',*,*,#14471,.F.);
#20931=ORIENTED_EDGE('',*,*,#14467,.T.);
#20932=ORIENTED_EDGE('',*,*,#14016,.F.);
#20933=ORIENTED_EDGE('',*,*,#14472,.F.);
#20934=ORIENTED_EDGE('',*,*,#14327,.F.);
#20935=ORIENTED_EDGE('',*,*,#14009,.F.);
#20936=ORIENTED_EDGE('',*,*,#14473,.F.);
#20937=ORIENTED_EDGE('',*,*,#14474,.F.);
#20938=ORIENTED_EDGE('',*,*,#14475,.F.);
#20939=ORIENTED_EDGE('',*,*,#14476,.F.);
#20940=ORIENTED_EDGE('',*,*,#14014,.F.);
#20941=ORIENTED_EDGE('',*,*,#14324,.F.);
#20942=ORIENTED_EDGE('',*,*,#14477,.F.);
#20943=ORIENTED_EDGE('',*,*,#14473,.T.);
#20944=ORIENTED_EDGE('',*,*,#14008,.F.);
#20945=ORIENTED_EDGE('',*,*,#14478,.F.);
#20946=ORIENTED_EDGE('',*,*,#14336,.F.);
#20947=ORIENTED_EDGE('',*,*,#14001,.F.);
#20948=ORIENTED_EDGE('',*,*,#14479,.F.);
#20949=ORIENTED_EDGE('',*,*,#14480,.F.);
#20950=ORIENTED_EDGE('',*,*,#14481,.F.);
#20951=ORIENTED_EDGE('',*,*,#14482,.F.);
#20952=ORIENTED_EDGE('',*,*,#14006,.F.);
#20953=ORIENTED_EDGE('',*,*,#14333,.F.);
#20954=ORIENTED_EDGE('',*,*,#14483,.F.);
#20955=ORIENTED_EDGE('',*,*,#14479,.T.);
#20956=ORIENTED_EDGE('',*,*,#14000,.F.);
#20957=ORIENTED_EDGE('',*,*,#14484,.F.);
#20958=ORIENTED_EDGE('',*,*,#14345,.F.);
#20959=ORIENTED_EDGE('',*,*,#13993,.F.);
#20960=ORIENTED_EDGE('',*,*,#14485,.F.);
#20961=ORIENTED_EDGE('',*,*,#14486,.F.);
#20962=ORIENTED_EDGE('',*,*,#14487,.F.);
#20963=ORIENTED_EDGE('',*,*,#14488,.F.);
#20964=ORIENTED_EDGE('',*,*,#13998,.F.);
#20965=ORIENTED_EDGE('',*,*,#14342,.F.);
#20966=ORIENTED_EDGE('',*,*,#14489,.F.);
#20967=ORIENTED_EDGE('',*,*,#14485,.T.);
#20968=ORIENTED_EDGE('',*,*,#13992,.F.);
#20969=ORIENTED_EDGE('',*,*,#14490,.F.);
#20970=ORIENTED_EDGE('',*,*,#14354,.F.);
#20971=ORIENTED_EDGE('',*,*,#13985,.F.);
#20972=ORIENTED_EDGE('',*,*,#14491,.F.);
#20973=ORIENTED_EDGE('',*,*,#14492,.F.);
#20974=ORIENTED_EDGE('',*,*,#14493,.F.);
#20975=ORIENTED_EDGE('',*,*,#14494,.F.);
#20976=ORIENTED_EDGE('',*,*,#13990,.F.);
#20977=ORIENTED_EDGE('',*,*,#14351,.F.);
#20978=ORIENTED_EDGE('',*,*,#14495,.F.);
#20979=ORIENTED_EDGE('',*,*,#14491,.T.);
#20980=ORIENTED_EDGE('',*,*,#13984,.F.);
#20981=ORIENTED_EDGE('',*,*,#14496,.F.);
#20982=ORIENTED_EDGE('',*,*,#14363,.F.);
#20983=ORIENTED_EDGE('',*,*,#13977,.F.);
#20984=ORIENTED_EDGE('',*,*,#14497,.F.);
#20985=ORIENTED_EDGE('',*,*,#14498,.F.);
#20986=ORIENTED_EDGE('',*,*,#14499,.F.);
#20987=ORIENTED_EDGE('',*,*,#14500,.F.);
#20988=ORIENTED_EDGE('',*,*,#13982,.F.);
#20989=ORIENTED_EDGE('',*,*,#14360,.F.);
#20990=ORIENTED_EDGE('',*,*,#14501,.F.);
#20991=ORIENTED_EDGE('',*,*,#14497,.T.);
#20992=ORIENTED_EDGE('',*,*,#13976,.F.);
#20993=ORIENTED_EDGE('',*,*,#14502,.F.);
#20994=ORIENTED_EDGE('',*,*,#14367,.T.);
#20995=ORIENTED_EDGE('',*,*,#14161,.T.);
#20996=ORIENTED_EDGE('',*,*,#14158,.F.);
#20997=ORIENTED_EDGE('',*,*,#14166,.T.);
#20998=ORIENTED_EDGE('',*,*,#14163,.F.);
#20999=ORIENTED_EDGE('',*,*,#14366,.T.);
#21000=ORIENTED_EDGE('',*,*,#14369,.T.);
#21001=ORIENTED_EDGE('',*,*,#14503,.F.);
#21002=ORIENTED_EDGE('',*,*,#14373,.T.);
#21003=ORIENTED_EDGE('',*,*,#14170,.T.);
#21004=ORIENTED_EDGE('',*,*,#14167,.F.);
#21005=ORIENTED_EDGE('',*,*,#14175,.T.);
#21006=ORIENTED_EDGE('',*,*,#14172,.F.);
#21007=ORIENTED_EDGE('',*,*,#14372,.T.);
#21008=ORIENTED_EDGE('',*,*,#14375,.T.);
#21009=ORIENTED_EDGE('',*,*,#14504,.F.);
#21010=ORIENTED_EDGE('',*,*,#14379,.T.);
#21011=ORIENTED_EDGE('',*,*,#14179,.T.);
#21012=ORIENTED_EDGE('',*,*,#14176,.F.);
#21013=ORIENTED_EDGE('',*,*,#14184,.T.);
#21014=ORIENTED_EDGE('',*,*,#14181,.F.);
#21015=ORIENTED_EDGE('',*,*,#14378,.T.);
#21016=ORIENTED_EDGE('',*,*,#14381,.T.);
#21017=ORIENTED_EDGE('',*,*,#14505,.F.);
#21018=ORIENTED_EDGE('',*,*,#14385,.T.);
#21019=ORIENTED_EDGE('',*,*,#14188,.T.);
#21020=ORIENTED_EDGE('',*,*,#14185,.F.);
#21021=ORIENTED_EDGE('',*,*,#14193,.T.);
#21022=ORIENTED_EDGE('',*,*,#14190,.F.);
#21023=ORIENTED_EDGE('',*,*,#14384,.T.);
#21024=ORIENTED_EDGE('',*,*,#14387,.T.);
#21025=ORIENTED_EDGE('',*,*,#14506,.F.);
#21026=ORIENTED_EDGE('',*,*,#14391,.T.);
#21027=ORIENTED_EDGE('',*,*,#14197,.T.);
#21028=ORIENTED_EDGE('',*,*,#14194,.F.);
#21029=ORIENTED_EDGE('',*,*,#14202,.T.);
#21030=ORIENTED_EDGE('',*,*,#14199,.F.);
#21031=ORIENTED_EDGE('',*,*,#14390,.T.);
#21032=ORIENTED_EDGE('',*,*,#14393,.T.);
#21033=ORIENTED_EDGE('',*,*,#14507,.F.);
#21034=ORIENTED_EDGE('',*,*,#14397,.T.);
#21035=ORIENTED_EDGE('',*,*,#14206,.T.);
#21036=ORIENTED_EDGE('',*,*,#14203,.F.);
#21037=ORIENTED_EDGE('',*,*,#14211,.T.);
#21038=ORIENTED_EDGE('',*,*,#14208,.F.);
#21039=ORIENTED_EDGE('',*,*,#14396,.T.);
#21040=ORIENTED_EDGE('',*,*,#14399,.T.);
#21041=ORIENTED_EDGE('',*,*,#14508,.F.);
#21042=ORIENTED_EDGE('',*,*,#14403,.T.);
#21043=ORIENTED_EDGE('',*,*,#14215,.T.);
#21044=ORIENTED_EDGE('',*,*,#14212,.F.);
#21045=ORIENTED_EDGE('',*,*,#14220,.T.);
#21046=ORIENTED_EDGE('',*,*,#14217,.F.);
#21047=ORIENTED_EDGE('',*,*,#14402,.T.);
#21048=ORIENTED_EDGE('',*,*,#14405,.T.);
#21049=ORIENTED_EDGE('',*,*,#14509,.F.);
#21050=ORIENTED_EDGE('',*,*,#14409,.T.);
#21051=ORIENTED_EDGE('',*,*,#14224,.T.);
#21052=ORIENTED_EDGE('',*,*,#14221,.F.);
#21053=ORIENTED_EDGE('',*,*,#14229,.T.);
#21054=ORIENTED_EDGE('',*,*,#14226,.F.);
#21055=ORIENTED_EDGE('',*,*,#14408,.T.);
#21056=ORIENTED_EDGE('',*,*,#14411,.T.);
#21057=ORIENTED_EDGE('',*,*,#14510,.F.);
#21058=ORIENTED_EDGE('',*,*,#14415,.T.);
#21059=ORIENTED_EDGE('',*,*,#14233,.T.);
#21060=ORIENTED_EDGE('',*,*,#14230,.F.);
#21061=ORIENTED_EDGE('',*,*,#14238,.T.);
#21062=ORIENTED_EDGE('',*,*,#14235,.F.);
#21063=ORIENTED_EDGE('',*,*,#14414,.T.);
#21064=ORIENTED_EDGE('',*,*,#14417,.T.);
#21065=ORIENTED_EDGE('',*,*,#14511,.F.);
#21066=ORIENTED_EDGE('',*,*,#14421,.T.);
#21067=ORIENTED_EDGE('',*,*,#14242,.T.);
#21068=ORIENTED_EDGE('',*,*,#14239,.F.);
#21069=ORIENTED_EDGE('',*,*,#14247,.T.);
#21070=ORIENTED_EDGE('',*,*,#14244,.F.);
#21071=ORIENTED_EDGE('',*,*,#14420,.T.);
#21072=ORIENTED_EDGE('',*,*,#14423,.T.);
#21073=ORIENTED_EDGE('',*,*,#14512,.F.);
#21074=ORIENTED_EDGE('',*,*,#14427,.T.);
#21075=ORIENTED_EDGE('',*,*,#14251,.T.);
#21076=ORIENTED_EDGE('',*,*,#14248,.F.);
#21077=ORIENTED_EDGE('',*,*,#14256,.T.);
#21078=ORIENTED_EDGE('',*,*,#14253,.F.);
#21079=ORIENTED_EDGE('',*,*,#14426,.T.);
#21080=ORIENTED_EDGE('',*,*,#14429,.T.);
#21081=ORIENTED_EDGE('',*,*,#14513,.F.);
#21082=ORIENTED_EDGE('',*,*,#14433,.T.);
#21083=ORIENTED_EDGE('',*,*,#14260,.T.);
#21084=ORIENTED_EDGE('',*,*,#14257,.F.);
#21085=ORIENTED_EDGE('',*,*,#14265,.T.);
#21086=ORIENTED_EDGE('',*,*,#14262,.F.);
#21087=ORIENTED_EDGE('',*,*,#14432,.T.);
#21088=ORIENTED_EDGE('',*,*,#14435,.T.);
#21089=ORIENTED_EDGE('',*,*,#14514,.F.);
#21090=ORIENTED_EDGE('',*,*,#14439,.T.);
#21091=ORIENTED_EDGE('',*,*,#14269,.T.);
#21092=ORIENTED_EDGE('',*,*,#14266,.F.);
#21093=ORIENTED_EDGE('',*,*,#14274,.T.);
#21094=ORIENTED_EDGE('',*,*,#14271,.F.);
#21095=ORIENTED_EDGE('',*,*,#14438,.T.);
#21096=ORIENTED_EDGE('',*,*,#14441,.T.);
#21097=ORIENTED_EDGE('',*,*,#14515,.F.);
#21098=ORIENTED_EDGE('',*,*,#14445,.T.);
#21099=ORIENTED_EDGE('',*,*,#14278,.T.);
#21100=ORIENTED_EDGE('',*,*,#14275,.F.);
#21101=ORIENTED_EDGE('',*,*,#14283,.T.);
#21102=ORIENTED_EDGE('',*,*,#14280,.F.);
#21103=ORIENTED_EDGE('',*,*,#14444,.T.);
#21104=ORIENTED_EDGE('',*,*,#14447,.T.);
#21105=ORIENTED_EDGE('',*,*,#14516,.F.);
#21106=ORIENTED_EDGE('',*,*,#14451,.T.);
#21107=ORIENTED_EDGE('',*,*,#14287,.T.);
#21108=ORIENTED_EDGE('',*,*,#14284,.F.);
#21109=ORIENTED_EDGE('',*,*,#14292,.T.);
#21110=ORIENTED_EDGE('',*,*,#14289,.F.);
#21111=ORIENTED_EDGE('',*,*,#14450,.T.);
#21112=ORIENTED_EDGE('',*,*,#14453,.T.);
#21113=ORIENTED_EDGE('',*,*,#14517,.F.);
#21114=ORIENTED_EDGE('',*,*,#14457,.T.);
#21115=ORIENTED_EDGE('',*,*,#14296,.T.);
#21116=ORIENTED_EDGE('',*,*,#14293,.F.);
#21117=ORIENTED_EDGE('',*,*,#14301,.T.);
#21118=ORIENTED_EDGE('',*,*,#14298,.F.);
#21119=ORIENTED_EDGE('',*,*,#14456,.T.);
#21120=ORIENTED_EDGE('',*,*,#14459,.T.);
#21121=ORIENTED_EDGE('',*,*,#14518,.F.);
#21122=ORIENTED_EDGE('',*,*,#14463,.T.);
#21123=ORIENTED_EDGE('',*,*,#14305,.T.);
#21124=ORIENTED_EDGE('',*,*,#14302,.F.);
#21125=ORIENTED_EDGE('',*,*,#14310,.T.);
#21126=ORIENTED_EDGE('',*,*,#14307,.F.);
#21127=ORIENTED_EDGE('',*,*,#14462,.T.);
#21128=ORIENTED_EDGE('',*,*,#14465,.T.);
#21129=ORIENTED_EDGE('',*,*,#14519,.F.);
#21130=ORIENTED_EDGE('',*,*,#14469,.T.);
#21131=ORIENTED_EDGE('',*,*,#14314,.T.);
#21132=ORIENTED_EDGE('',*,*,#14311,.F.);
#21133=ORIENTED_EDGE('',*,*,#14319,.T.);
#21134=ORIENTED_EDGE('',*,*,#14316,.F.);
#21135=ORIENTED_EDGE('',*,*,#14468,.T.);
#21136=ORIENTED_EDGE('',*,*,#14471,.T.);
#21137=ORIENTED_EDGE('',*,*,#14520,.F.);
#21138=ORIENTED_EDGE('',*,*,#14475,.T.);
#21139=ORIENTED_EDGE('',*,*,#14323,.T.);
#21140=ORIENTED_EDGE('',*,*,#14320,.F.);
#21141=ORIENTED_EDGE('',*,*,#14328,.T.);
#21142=ORIENTED_EDGE('',*,*,#14325,.F.);
#21143=ORIENTED_EDGE('',*,*,#14474,.T.);
#21144=ORIENTED_EDGE('',*,*,#14477,.T.);
#21145=ORIENTED_EDGE('',*,*,#14521,.F.);
#21146=ORIENTED_EDGE('',*,*,#14481,.T.);
#21147=ORIENTED_EDGE('',*,*,#14332,.T.);
#21148=ORIENTED_EDGE('',*,*,#14329,.F.);
#21149=ORIENTED_EDGE('',*,*,#14337,.T.);
#21150=ORIENTED_EDGE('',*,*,#14334,.F.);
#21151=ORIENTED_EDGE('',*,*,#14480,.T.);
#21152=ORIENTED_EDGE('',*,*,#14483,.T.);
#21153=ORIENTED_EDGE('',*,*,#14522,.F.);
#21154=ORIENTED_EDGE('',*,*,#14487,.T.);
#21155=ORIENTED_EDGE('',*,*,#14341,.T.);
#21156=ORIENTED_EDGE('',*,*,#14338,.F.);
#21157=ORIENTED_EDGE('',*,*,#14346,.T.);
#21158=ORIENTED_EDGE('',*,*,#14343,.F.);
#21159=ORIENTED_EDGE('',*,*,#14486,.T.);
#21160=ORIENTED_EDGE('',*,*,#14489,.T.);
#21161=ORIENTED_EDGE('',*,*,#14523,.F.);
#21162=ORIENTED_EDGE('',*,*,#14493,.T.);
#21163=ORIENTED_EDGE('',*,*,#14350,.T.);
#21164=ORIENTED_EDGE('',*,*,#14347,.F.);
#21165=ORIENTED_EDGE('',*,*,#14355,.T.);
#21166=ORIENTED_EDGE('',*,*,#14352,.F.);
#21167=ORIENTED_EDGE('',*,*,#14492,.T.);
#21168=ORIENTED_EDGE('',*,*,#14495,.T.);
#21169=ORIENTED_EDGE('',*,*,#14524,.F.);
#21170=ORIENTED_EDGE('',*,*,#14499,.T.);
#21171=ORIENTED_EDGE('',*,*,#14359,.T.);
#21172=ORIENTED_EDGE('',*,*,#14356,.F.);
#21173=ORIENTED_EDGE('',*,*,#14364,.T.);
#21174=ORIENTED_EDGE('',*,*,#14361,.F.);
#21175=ORIENTED_EDGE('',*,*,#14498,.T.);
#21176=ORIENTED_EDGE('',*,*,#14501,.T.);
#21177=ORIENTED_EDGE('',*,*,#14525,.F.);
#21178=ORIENTED_EDGE('',*,*,#14526,.T.);
#21179=ORIENTED_EDGE('',*,*,#14527,.T.);
#21180=ORIENTED_EDGE('',*,*,#14528,.F.);
#21181=ORIENTED_EDGE('',*,*,#14529,.T.);
#21182=ORIENTED_EDGE('',*,*,#14530,.F.);
#21183=ORIENTED_EDGE('',*,*,#14531,.T.);
#21184=ORIENTED_EDGE('',*,*,#14532,.T.);
#21185=ORIENTED_EDGE('',*,*,#14533,.F.);
#21186=ORIENTED_EDGE('',*,*,#13955,.T.);
#21187=ORIENTED_EDGE('',*,*,#13965,.F.);
#21188=ORIENTED_EDGE('',*,*,#13961,.T.);
#21189=ORIENTED_EDGE('',*,*,#13963,.T.);
#21190=ORIENTED_EDGE('',*,*,#14502,.T.);
#21191=ORIENTED_EDGE('',*,*,#13975,.F.);
#21192=ORIENTED_EDGE('',*,*,#14534,.T.);
#21193=ORIENTED_EDGE('',*,*,#14525,.T.);
#21194=ORIENTED_EDGE('',*,*,#14496,.T.);
#21195=ORIENTED_EDGE('',*,*,#13983,.F.);
#21196=ORIENTED_EDGE('',*,*,#14500,.T.);
#21197=ORIENTED_EDGE('',*,*,#14524,.T.);
#21198=ORIENTED_EDGE('',*,*,#14490,.T.);
#21199=ORIENTED_EDGE('',*,*,#13991,.F.);
#21200=ORIENTED_EDGE('',*,*,#14494,.T.);
#21201=ORIENTED_EDGE('',*,*,#14523,.T.);
#21202=ORIENTED_EDGE('',*,*,#14484,.T.);
#21203=ORIENTED_EDGE('',*,*,#13999,.F.);
#21204=ORIENTED_EDGE('',*,*,#14488,.T.);
#21205=ORIENTED_EDGE('',*,*,#14522,.T.);
#21206=ORIENTED_EDGE('',*,*,#14478,.T.);
#21207=ORIENTED_EDGE('',*,*,#14007,.F.);
#21208=ORIENTED_EDGE('',*,*,#14482,.T.);
#21209=ORIENTED_EDGE('',*,*,#14521,.T.);
#21210=ORIENTED_EDGE('',*,*,#14472,.T.);
#21211=ORIENTED_EDGE('',*,*,#14015,.F.);
#21212=ORIENTED_EDGE('',*,*,#14476,.T.);
#21213=ORIENTED_EDGE('',*,*,#14520,.T.);
#21214=ORIENTED_EDGE('',*,*,#14466,.T.);
#21215=ORIENTED_EDGE('',*,*,#14023,.F.);
#21216=ORIENTED_EDGE('',*,*,#14470,.T.);
#21217=ORIENTED_EDGE('',*,*,#14519,.T.);
#21218=ORIENTED_EDGE('',*,*,#14460,.T.);
#21219=ORIENTED_EDGE('',*,*,#14031,.F.);
#21220=ORIENTED_EDGE('',*,*,#14464,.T.);
#21221=ORIENTED_EDGE('',*,*,#14518,.T.);
#21222=ORIENTED_EDGE('',*,*,#14454,.T.);
#21223=ORIENTED_EDGE('',*,*,#14039,.F.);
#21224=ORIENTED_EDGE('',*,*,#14458,.T.);
#21225=ORIENTED_EDGE('',*,*,#14517,.T.);
#21226=ORIENTED_EDGE('',*,*,#14448,.T.);
#21227=ORIENTED_EDGE('',*,*,#14047,.F.);
#21228=ORIENTED_EDGE('',*,*,#14452,.T.);
#21229=ORIENTED_EDGE('',*,*,#14516,.T.);
#21230=ORIENTED_EDGE('',*,*,#14442,.T.);
#21231=ORIENTED_EDGE('',*,*,#14055,.F.);
#21232=ORIENTED_EDGE('',*,*,#14446,.T.);
#21233=ORIENTED_EDGE('',*,*,#14515,.T.);
#21234=ORIENTED_EDGE('',*,*,#14436,.T.);
#21235=ORIENTED_EDGE('',*,*,#14063,.F.);
#21236=ORIENTED_EDGE('',*,*,#14440,.T.);
#21237=ORIENTED_EDGE('',*,*,#14514,.T.);
#21238=ORIENTED_EDGE('',*,*,#14430,.T.);
#21239=ORIENTED_EDGE('',*,*,#14071,.F.);
#21240=ORIENTED_EDGE('',*,*,#14434,.T.);
#21241=ORIENTED_EDGE('',*,*,#14513,.T.);
#21242=ORIENTED_EDGE('',*,*,#14424,.T.);
#21243=ORIENTED_EDGE('',*,*,#14079,.F.);
#21244=ORIENTED_EDGE('',*,*,#14428,.T.);
#21245=ORIENTED_EDGE('',*,*,#14512,.T.);
#21246=ORIENTED_EDGE('',*,*,#14418,.T.);
#21247=ORIENTED_EDGE('',*,*,#14087,.F.);
#21248=ORIENTED_EDGE('',*,*,#14422,.T.);
#21249=ORIENTED_EDGE('',*,*,#14511,.T.);
#21250=ORIENTED_EDGE('',*,*,#14412,.T.);
#21251=ORIENTED_EDGE('',*,*,#14095,.F.);
#21252=ORIENTED_EDGE('',*,*,#14416,.T.);
#21253=ORIENTED_EDGE('',*,*,#14510,.T.);
#21254=ORIENTED_EDGE('',*,*,#14406,.T.);
#21255=ORIENTED_EDGE('',*,*,#14103,.F.);
#21256=ORIENTED_EDGE('',*,*,#14410,.T.);
#21257=ORIENTED_EDGE('',*,*,#14509,.T.);
#21258=ORIENTED_EDGE('',*,*,#14400,.T.);
#21259=ORIENTED_EDGE('',*,*,#14111,.F.);
#21260=ORIENTED_EDGE('',*,*,#14404,.T.);
#21261=ORIENTED_EDGE('',*,*,#14508,.T.);
#21262=ORIENTED_EDGE('',*,*,#14394,.T.);
#21263=ORIENTED_EDGE('',*,*,#14119,.F.);
#21264=ORIENTED_EDGE('',*,*,#14398,.T.);
#21265=ORIENTED_EDGE('',*,*,#14507,.T.);
#21266=ORIENTED_EDGE('',*,*,#14388,.T.);
#21267=ORIENTED_EDGE('',*,*,#14127,.F.);
#21268=ORIENTED_EDGE('',*,*,#14392,.T.);
#21269=ORIENTED_EDGE('',*,*,#14506,.T.);
#21270=ORIENTED_EDGE('',*,*,#14382,.T.);
#21271=ORIENTED_EDGE('',*,*,#14135,.F.);
#21272=ORIENTED_EDGE('',*,*,#14386,.T.);
#21273=ORIENTED_EDGE('',*,*,#14505,.T.);
#21274=ORIENTED_EDGE('',*,*,#14376,.T.);
#21275=ORIENTED_EDGE('',*,*,#14143,.F.);
#21276=ORIENTED_EDGE('',*,*,#14380,.T.);
#21277=ORIENTED_EDGE('',*,*,#14504,.T.);
#21278=ORIENTED_EDGE('',*,*,#14370,.T.);
#21279=ORIENTED_EDGE('',*,*,#14151,.F.);
#21280=ORIENTED_EDGE('',*,*,#14374,.T.);
#21281=ORIENTED_EDGE('',*,*,#14503,.T.);
#21282=ORIENTED_EDGE('',*,*,#14528,.T.);
#21283=ORIENTED_EDGE('',*,*,#14535,.T.);
#21284=ORIENTED_EDGE('',*,*,#13972,.T.);
#21285=ORIENTED_EDGE('',*,*,#14536,.T.);
#21286=ORIENTED_EDGE('',*,*,#14535,.F.);
#21287=ORIENTED_EDGE('',*,*,#14527,.F.);
#21288=ORIENTED_EDGE('',*,*,#14537,.T.);
#21289=ORIENTED_EDGE('',*,*,#13973,.F.);
#21290=ORIENTED_EDGE('',*,*,#14530,.T.);
#21291=ORIENTED_EDGE('',*,*,#14538,.T.);
#21292=ORIENTED_EDGE('',*,*,#13970,.T.);
#21293=ORIENTED_EDGE('',*,*,#14539,.T.);
#21294=ORIENTED_EDGE('',*,*,#14536,.F.);
#21295=ORIENTED_EDGE('',*,*,#13971,.F.);
#21296=ORIENTED_EDGE('',*,*,#14538,.F.);
#21297=ORIENTED_EDGE('',*,*,#14529,.F.);
#21298=ORIENTED_EDGE('',*,*,#14539,.F.);
#21299=ORIENTED_EDGE('',*,*,#13969,.F.);
#21300=ORIENTED_EDGE('',*,*,#14540,.F.);
#21301=ORIENTED_EDGE('',*,*,#14531,.F.);
#21302=ORIENTED_EDGE('',*,*,#14526,.F.);
#21303=ORIENTED_EDGE('',*,*,#14534,.F.);
#21304=ORIENTED_EDGE('',*,*,#13974,.F.);
#21305=ORIENTED_EDGE('',*,*,#14537,.F.);
#21306=ORIENTED_EDGE('',*,*,#14532,.F.);
#21307=ORIENTED_EDGE('',*,*,#14540,.T.);
#21308=ORIENTED_EDGE('',*,*,#13968,.F.);
#21309=ORIENTED_EDGE('',*,*,#14541,.F.);
#21310=ORIENTED_EDGE('',*,*,#14368,.T.);
#21311=ORIENTED_EDGE('',*,*,#14533,.T.);
#21312=ORIENTED_EDGE('',*,*,#14541,.T.);
#21313=ORIENTED_EDGE('',*,*,#13967,.F.);
#21314=ORIENTED_EDGE('',*,*,#14542,.T.);
#21315=ORIENTED_EDGE('',*,*,#14543,.T.);
#21316=ORIENTED_EDGE('',*,*,#14544,.T.);
#21317=ORIENTED_EDGE('',*,*,#14545,.T.);
#21318=ORIENTED_EDGE('',*,*,#14543,.F.);
#21319=ORIENTED_EDGE('',*,*,#14546,.F.);
#21320=ORIENTED_EDGE('',*,*,#14547,.T.);
#21321=ORIENTED_EDGE('',*,*,#14548,.F.);
#21322=ORIENTED_EDGE('',*,*,#14549,.T.);
#21323=ORIENTED_EDGE('',*,*,#14550,.T.);
#21324=ORIENTED_EDGE('',*,*,#14551,.T.);
#21325=ORIENTED_EDGE('',*,*,#14552,.T.);
#21326=ORIENTED_EDGE('',*,*,#14545,.F.);
#21327=ORIENTED_EDGE('',*,*,#14553,.F.);
#21328=ORIENTED_EDGE('',*,*,#14550,.F.);
#21329=ORIENTED_EDGE('',*,*,#14554,.F.);
#21330=ORIENTED_EDGE('',*,*,#14555,.T.);
#21331=ORIENTED_EDGE('',*,*,#14556,.T.);
#21332=ORIENTED_EDGE('',*,*,#14557,.T.);
#21333=ORIENTED_EDGE('',*,*,#14558,.T.);
#21334=ORIENTED_EDGE('',*,*,#14556,.F.);
#21335=ORIENTED_EDGE('',*,*,#14559,.F.);
#21336=ORIENTED_EDGE('',*,*,#14560,.T.);
#21337=ORIENTED_EDGE('',*,*,#14561,.F.);
#21338=ORIENTED_EDGE('',*,*,#14562,.T.);
#21339=ORIENTED_EDGE('',*,*,#14563,.T.);
#21340=ORIENTED_EDGE('',*,*,#14564,.T.);
#21341=ORIENTED_EDGE('',*,*,#14565,.T.);
#21342=ORIENTED_EDGE('',*,*,#14558,.F.);
#21343=ORIENTED_EDGE('',*,*,#14566,.F.);
#21344=ORIENTED_EDGE('',*,*,#14563,.F.);
#21345=ORIENTED_EDGE('',*,*,#14567,.F.);
#21346=ORIENTED_EDGE('',*,*,#14568,.T.);
#21347=ORIENTED_EDGE('',*,*,#14569,.T.);
#21348=ORIENTED_EDGE('',*,*,#14570,.T.);
#21349=ORIENTED_EDGE('',*,*,#14571,.T.);
#21350=ORIENTED_EDGE('',*,*,#14569,.F.);
#21351=ORIENTED_EDGE('',*,*,#14572,.F.);
#21352=ORIENTED_EDGE('',*,*,#14573,.T.);
#21353=ORIENTED_EDGE('',*,*,#14574,.F.);
#21354=ORIENTED_EDGE('',*,*,#14575,.T.);
#21355=ORIENTED_EDGE('',*,*,#14576,.T.);
#21356=ORIENTED_EDGE('',*,*,#14577,.T.);
#21357=ORIENTED_EDGE('',*,*,#14578,.T.);
#21358=ORIENTED_EDGE('',*,*,#14571,.F.);
#21359=ORIENTED_EDGE('',*,*,#14579,.F.);
#21360=ORIENTED_EDGE('',*,*,#14576,.F.);
#21361=ORIENTED_EDGE('',*,*,#14580,.F.);
#21362=ORIENTED_EDGE('',*,*,#14581,.T.);
#21363=ORIENTED_EDGE('',*,*,#14582,.T.);
#21364=ORIENTED_EDGE('',*,*,#14583,.T.);
#21365=ORIENTED_EDGE('',*,*,#14584,.T.);
#21366=ORIENTED_EDGE('',*,*,#14582,.F.);
#21367=ORIENTED_EDGE('',*,*,#14585,.F.);
#21368=ORIENTED_EDGE('',*,*,#14586,.T.);
#21369=ORIENTED_EDGE('',*,*,#14587,.F.);
#21370=ORIENTED_EDGE('',*,*,#14588,.T.);
#21371=ORIENTED_EDGE('',*,*,#14589,.T.);
#21372=ORIENTED_EDGE('',*,*,#14590,.T.);
#21373=ORIENTED_EDGE('',*,*,#14591,.T.);
#21374=ORIENTED_EDGE('',*,*,#14584,.F.);
#21375=ORIENTED_EDGE('',*,*,#14592,.F.);
#21376=ORIENTED_EDGE('',*,*,#14589,.F.);
#21377=ORIENTED_EDGE('',*,*,#14593,.F.);
#21378=ORIENTED_EDGE('',*,*,#14594,.T.);
#21379=ORIENTED_EDGE('',*,*,#14595,.T.);
#21380=ORIENTED_EDGE('',*,*,#14596,.T.);
#21381=ORIENTED_EDGE('',*,*,#14597,.T.);
#21382=ORIENTED_EDGE('',*,*,#14595,.F.);
#21383=ORIENTED_EDGE('',*,*,#14598,.F.);
#21384=ORIENTED_EDGE('',*,*,#14599,.T.);
#21385=ORIENTED_EDGE('',*,*,#14600,.F.);
#21386=ORIENTED_EDGE('',*,*,#14601,.T.);
#21387=ORIENTED_EDGE('',*,*,#14602,.T.);
#21388=ORIENTED_EDGE('',*,*,#14603,.T.);
#21389=ORIENTED_EDGE('',*,*,#14604,.T.);
#21390=ORIENTED_EDGE('',*,*,#14597,.F.);
#21391=ORIENTED_EDGE('',*,*,#14605,.F.);
#21392=ORIENTED_EDGE('',*,*,#14602,.F.);
#21393=ORIENTED_EDGE('',*,*,#14606,.F.);
#21394=ORIENTED_EDGE('',*,*,#14607,.T.);
#21395=ORIENTED_EDGE('',*,*,#14608,.T.);
#21396=ORIENTED_EDGE('',*,*,#14609,.T.);
#21397=ORIENTED_EDGE('',*,*,#14610,.T.);
#21398=ORIENTED_EDGE('',*,*,#14608,.F.);
#21399=ORIENTED_EDGE('',*,*,#14611,.F.);
#21400=ORIENTED_EDGE('',*,*,#14612,.T.);
#21401=ORIENTED_EDGE('',*,*,#14613,.F.);
#21402=ORIENTED_EDGE('',*,*,#14614,.T.);
#21403=ORIENTED_EDGE('',*,*,#14615,.T.);
#21404=ORIENTED_EDGE('',*,*,#14616,.T.);
#21405=ORIENTED_EDGE('',*,*,#14617,.T.);
#21406=ORIENTED_EDGE('',*,*,#14610,.F.);
#21407=ORIENTED_EDGE('',*,*,#14618,.F.);
#21408=ORIENTED_EDGE('',*,*,#14615,.F.);
#21409=ORIENTED_EDGE('',*,*,#14619,.F.);
#21410=ORIENTED_EDGE('',*,*,#14620,.T.);
#21411=ORIENTED_EDGE('',*,*,#14621,.T.);
#21412=ORIENTED_EDGE('',*,*,#14622,.T.);
#21413=ORIENTED_EDGE('',*,*,#14623,.T.);
#21414=ORIENTED_EDGE('',*,*,#14621,.F.);
#21415=ORIENTED_EDGE('',*,*,#14624,.F.);
#21416=ORIENTED_EDGE('',*,*,#14625,.T.);
#21417=ORIENTED_EDGE('',*,*,#14626,.F.);
#21418=ORIENTED_EDGE('',*,*,#14627,.T.);
#21419=ORIENTED_EDGE('',*,*,#14628,.T.);
#21420=ORIENTED_EDGE('',*,*,#14629,.T.);
#21421=ORIENTED_EDGE('',*,*,#14630,.T.);
#21422=ORIENTED_EDGE('',*,*,#14623,.F.);
#21423=ORIENTED_EDGE('',*,*,#14631,.F.);
#21424=ORIENTED_EDGE('',*,*,#14628,.F.);
#21425=ORIENTED_EDGE('',*,*,#14632,.F.);
#21426=ORIENTED_EDGE('',*,*,#14633,.T.);
#21427=ORIENTED_EDGE('',*,*,#14634,.T.);
#21428=ORIENTED_EDGE('',*,*,#14635,.T.);
#21429=ORIENTED_EDGE('',*,*,#14636,.T.);
#21430=ORIENTED_EDGE('',*,*,#14634,.F.);
#21431=ORIENTED_EDGE('',*,*,#14637,.F.);
#21432=ORIENTED_EDGE('',*,*,#14638,.T.);
#21433=ORIENTED_EDGE('',*,*,#14639,.F.);
#21434=ORIENTED_EDGE('',*,*,#14640,.T.);
#21435=ORIENTED_EDGE('',*,*,#14641,.T.);
#21436=ORIENTED_EDGE('',*,*,#14642,.T.);
#21437=ORIENTED_EDGE('',*,*,#14643,.T.);
#21438=ORIENTED_EDGE('',*,*,#14636,.F.);
#21439=ORIENTED_EDGE('',*,*,#14644,.F.);
#21440=ORIENTED_EDGE('',*,*,#14641,.F.);
#21441=ORIENTED_EDGE('',*,*,#14645,.F.);
#21442=ORIENTED_EDGE('',*,*,#14646,.T.);
#21443=ORIENTED_EDGE('',*,*,#14647,.T.);
#21444=ORIENTED_EDGE('',*,*,#14648,.T.);
#21445=ORIENTED_EDGE('',*,*,#14649,.T.);
#21446=ORIENTED_EDGE('',*,*,#14647,.F.);
#21447=ORIENTED_EDGE('',*,*,#14650,.F.);
#21448=ORIENTED_EDGE('',*,*,#14651,.T.);
#21449=ORIENTED_EDGE('',*,*,#14652,.F.);
#21450=ORIENTED_EDGE('',*,*,#14653,.T.);
#21451=ORIENTED_EDGE('',*,*,#14654,.T.);
#21452=ORIENTED_EDGE('',*,*,#14655,.T.);
#21453=ORIENTED_EDGE('',*,*,#14656,.T.);
#21454=ORIENTED_EDGE('',*,*,#14649,.F.);
#21455=ORIENTED_EDGE('',*,*,#14657,.F.);
#21456=ORIENTED_EDGE('',*,*,#14654,.F.);
#21457=ORIENTED_EDGE('',*,*,#14658,.F.);
#21458=ORIENTED_EDGE('',*,*,#14659,.T.);
#21459=ORIENTED_EDGE('',*,*,#14660,.T.);
#21460=ORIENTED_EDGE('',*,*,#14661,.T.);
#21461=ORIENTED_EDGE('',*,*,#14662,.T.);
#21462=ORIENTED_EDGE('',*,*,#14660,.F.);
#21463=ORIENTED_EDGE('',*,*,#14663,.F.);
#21464=ORIENTED_EDGE('',*,*,#14664,.T.);
#21465=ORIENTED_EDGE('',*,*,#14665,.F.);
#21466=ORIENTED_EDGE('',*,*,#14666,.T.);
#21467=ORIENTED_EDGE('',*,*,#14667,.T.);
#21468=ORIENTED_EDGE('',*,*,#14668,.T.);
#21469=ORIENTED_EDGE('',*,*,#14669,.T.);
#21470=ORIENTED_EDGE('',*,*,#14662,.F.);
#21471=ORIENTED_EDGE('',*,*,#14670,.F.);
#21472=ORIENTED_EDGE('',*,*,#14667,.F.);
#21473=ORIENTED_EDGE('',*,*,#14671,.F.);
#21474=ORIENTED_EDGE('',*,*,#14672,.T.);
#21475=ORIENTED_EDGE('',*,*,#14673,.T.);
#21476=ORIENTED_EDGE('',*,*,#14674,.T.);
#21477=ORIENTED_EDGE('',*,*,#14675,.T.);
#21478=ORIENTED_EDGE('',*,*,#14673,.F.);
#21479=ORIENTED_EDGE('',*,*,#14676,.F.);
#21480=ORIENTED_EDGE('',*,*,#14677,.T.);
#21481=ORIENTED_EDGE('',*,*,#14678,.F.);
#21482=ORIENTED_EDGE('',*,*,#14679,.T.);
#21483=ORIENTED_EDGE('',*,*,#14680,.T.);
#21484=ORIENTED_EDGE('',*,*,#14681,.T.);
#21485=ORIENTED_EDGE('',*,*,#14682,.T.);
#21486=ORIENTED_EDGE('',*,*,#14675,.F.);
#21487=ORIENTED_EDGE('',*,*,#14683,.F.);
#21488=ORIENTED_EDGE('',*,*,#14680,.F.);
#21489=ORIENTED_EDGE('',*,*,#14684,.F.);
#21490=ORIENTED_EDGE('',*,*,#14685,.T.);
#21491=ORIENTED_EDGE('',*,*,#14686,.T.);
#21492=ORIENTED_EDGE('',*,*,#14687,.T.);
#21493=ORIENTED_EDGE('',*,*,#14688,.T.);
#21494=ORIENTED_EDGE('',*,*,#14686,.F.);
#21495=ORIENTED_EDGE('',*,*,#14689,.F.);
#21496=ORIENTED_EDGE('',*,*,#14690,.T.);
#21497=ORIENTED_EDGE('',*,*,#14691,.F.);
#21498=ORIENTED_EDGE('',*,*,#14692,.T.);
#21499=ORIENTED_EDGE('',*,*,#14693,.T.);
#21500=ORIENTED_EDGE('',*,*,#14694,.T.);
#21501=ORIENTED_EDGE('',*,*,#14695,.T.);
#21502=ORIENTED_EDGE('',*,*,#14688,.F.);
#21503=ORIENTED_EDGE('',*,*,#14696,.F.);
#21504=ORIENTED_EDGE('',*,*,#14693,.F.);
#21505=ORIENTED_EDGE('',*,*,#14697,.F.);
#21506=ORIENTED_EDGE('',*,*,#14698,.T.);
#21507=ORIENTED_EDGE('',*,*,#14699,.T.);
#21508=ORIENTED_EDGE('',*,*,#14700,.T.);
#21509=ORIENTED_EDGE('',*,*,#14701,.T.);
#21510=ORIENTED_EDGE('',*,*,#14699,.F.);
#21511=ORIENTED_EDGE('',*,*,#14702,.F.);
#21512=ORIENTED_EDGE('',*,*,#14703,.T.);
#21513=ORIENTED_EDGE('',*,*,#14704,.F.);
#21514=ORIENTED_EDGE('',*,*,#14705,.T.);
#21515=ORIENTED_EDGE('',*,*,#14706,.T.);
#21516=ORIENTED_EDGE('',*,*,#14707,.T.);
#21517=ORIENTED_EDGE('',*,*,#14708,.T.);
#21518=ORIENTED_EDGE('',*,*,#14701,.F.);
#21519=ORIENTED_EDGE('',*,*,#14709,.F.);
#21520=ORIENTED_EDGE('',*,*,#14706,.F.);
#21521=ORIENTED_EDGE('',*,*,#14710,.F.);
#21522=ORIENTED_EDGE('',*,*,#14711,.T.);
#21523=ORIENTED_EDGE('',*,*,#14712,.T.);
#21524=ORIENTED_EDGE('',*,*,#14713,.T.);
#21525=ORIENTED_EDGE('',*,*,#14714,.T.);
#21526=ORIENTED_EDGE('',*,*,#14712,.F.);
#21527=ORIENTED_EDGE('',*,*,#14715,.F.);
#21528=ORIENTED_EDGE('',*,*,#14716,.T.);
#21529=ORIENTED_EDGE('',*,*,#14717,.F.);
#21530=ORIENTED_EDGE('',*,*,#14718,.T.);
#21531=ORIENTED_EDGE('',*,*,#14719,.T.);
#21532=ORIENTED_EDGE('',*,*,#14720,.T.);
#21533=ORIENTED_EDGE('',*,*,#14721,.T.);
#21534=ORIENTED_EDGE('',*,*,#14714,.F.);
#21535=ORIENTED_EDGE('',*,*,#14722,.F.);
#21536=ORIENTED_EDGE('',*,*,#14719,.F.);
#21537=ORIENTED_EDGE('',*,*,#14723,.F.);
#21538=ORIENTED_EDGE('',*,*,#14724,.T.);
#21539=ORIENTED_EDGE('',*,*,#14725,.T.);
#21540=ORIENTED_EDGE('',*,*,#14726,.T.);
#21541=ORIENTED_EDGE('',*,*,#14727,.T.);
#21542=ORIENTED_EDGE('',*,*,#14725,.F.);
#21543=ORIENTED_EDGE('',*,*,#14728,.F.);
#21544=ORIENTED_EDGE('',*,*,#14729,.T.);
#21545=ORIENTED_EDGE('',*,*,#14730,.F.);
#21546=ORIENTED_EDGE('',*,*,#14731,.T.);
#21547=ORIENTED_EDGE('',*,*,#14732,.T.);
#21548=ORIENTED_EDGE('',*,*,#14733,.T.);
#21549=ORIENTED_EDGE('',*,*,#14734,.T.);
#21550=ORIENTED_EDGE('',*,*,#14727,.F.);
#21551=ORIENTED_EDGE('',*,*,#14735,.F.);
#21552=ORIENTED_EDGE('',*,*,#14732,.F.);
#21553=ORIENTED_EDGE('',*,*,#14736,.F.);
#21554=ORIENTED_EDGE('',*,*,#14737,.T.);
#21555=ORIENTED_EDGE('',*,*,#14738,.T.);
#21556=ORIENTED_EDGE('',*,*,#14739,.T.);
#21557=ORIENTED_EDGE('',*,*,#14740,.T.);
#21558=ORIENTED_EDGE('',*,*,#14738,.F.);
#21559=ORIENTED_EDGE('',*,*,#14741,.F.);
#21560=ORIENTED_EDGE('',*,*,#14742,.T.);
#21561=ORIENTED_EDGE('',*,*,#14743,.F.);
#21562=ORIENTED_EDGE('',*,*,#14744,.T.);
#21563=ORIENTED_EDGE('',*,*,#14745,.T.);
#21564=ORIENTED_EDGE('',*,*,#14746,.T.);
#21565=ORIENTED_EDGE('',*,*,#14747,.T.);
#21566=ORIENTED_EDGE('',*,*,#14740,.F.);
#21567=ORIENTED_EDGE('',*,*,#14748,.F.);
#21568=ORIENTED_EDGE('',*,*,#14745,.F.);
#21569=ORIENTED_EDGE('',*,*,#14749,.F.);
#21570=ORIENTED_EDGE('',*,*,#14750,.T.);
#21571=ORIENTED_EDGE('',*,*,#14751,.T.);
#21572=ORIENTED_EDGE('',*,*,#14752,.T.);
#21573=ORIENTED_EDGE('',*,*,#14753,.T.);
#21574=ORIENTED_EDGE('',*,*,#14751,.F.);
#21575=ORIENTED_EDGE('',*,*,#14754,.F.);
#21576=ORIENTED_EDGE('',*,*,#14755,.T.);
#21577=ORIENTED_EDGE('',*,*,#14756,.F.);
#21578=ORIENTED_EDGE('',*,*,#14757,.T.);
#21579=ORIENTED_EDGE('',*,*,#14758,.T.);
#21580=ORIENTED_EDGE('',*,*,#14759,.T.);
#21581=ORIENTED_EDGE('',*,*,#14760,.T.);
#21582=ORIENTED_EDGE('',*,*,#14753,.F.);
#21583=ORIENTED_EDGE('',*,*,#14761,.F.);
#21584=ORIENTED_EDGE('',*,*,#14758,.F.);
#21585=ORIENTED_EDGE('',*,*,#14762,.F.);
#21586=ORIENTED_EDGE('',*,*,#14763,.T.);
#21587=ORIENTED_EDGE('',*,*,#14764,.T.);
#21588=ORIENTED_EDGE('',*,*,#14765,.T.);
#21589=ORIENTED_EDGE('',*,*,#14766,.T.);
#21590=ORIENTED_EDGE('',*,*,#14764,.F.);
#21591=ORIENTED_EDGE('',*,*,#14767,.F.);
#21592=ORIENTED_EDGE('',*,*,#14768,.T.);
#21593=ORIENTED_EDGE('',*,*,#14769,.F.);
#21594=ORIENTED_EDGE('',*,*,#14770,.T.);
#21595=ORIENTED_EDGE('',*,*,#14771,.T.);
#21596=ORIENTED_EDGE('',*,*,#14772,.T.);
#21597=ORIENTED_EDGE('',*,*,#14773,.T.);
#21598=ORIENTED_EDGE('',*,*,#14766,.F.);
#21599=ORIENTED_EDGE('',*,*,#14774,.F.);
#21600=ORIENTED_EDGE('',*,*,#14771,.F.);
#21601=ORIENTED_EDGE('',*,*,#14775,.F.);
#21602=ORIENTED_EDGE('',*,*,#14776,.T.);
#21603=ORIENTED_EDGE('',*,*,#14777,.T.);
#21604=ORIENTED_EDGE('',*,*,#14778,.T.);
#21605=ORIENTED_EDGE('',*,*,#14779,.T.);
#21606=ORIENTED_EDGE('',*,*,#14777,.F.);
#21607=ORIENTED_EDGE('',*,*,#14780,.F.);
#21608=ORIENTED_EDGE('',*,*,#14781,.T.);
#21609=ORIENTED_EDGE('',*,*,#14782,.F.);
#21610=ORIENTED_EDGE('',*,*,#14783,.T.);
#21611=ORIENTED_EDGE('',*,*,#14784,.T.);
#21612=ORIENTED_EDGE('',*,*,#14785,.T.);
#21613=ORIENTED_EDGE('',*,*,#14786,.T.);
#21614=ORIENTED_EDGE('',*,*,#14779,.F.);
#21615=ORIENTED_EDGE('',*,*,#14787,.F.);
#21616=ORIENTED_EDGE('',*,*,#14784,.F.);
#21617=ORIENTED_EDGE('',*,*,#14788,.F.);
#21618=ORIENTED_EDGE('',*,*,#14789,.T.);
#21619=ORIENTED_EDGE('',*,*,#14790,.T.);
#21620=ORIENTED_EDGE('',*,*,#14791,.T.);
#21621=ORIENTED_EDGE('',*,*,#14792,.T.);
#21622=ORIENTED_EDGE('',*,*,#14790,.F.);
#21623=ORIENTED_EDGE('',*,*,#14793,.F.);
#21624=ORIENTED_EDGE('',*,*,#14794,.T.);
#21625=ORIENTED_EDGE('',*,*,#14795,.F.);
#21626=ORIENTED_EDGE('',*,*,#14796,.T.);
#21627=ORIENTED_EDGE('',*,*,#14797,.T.);
#21628=ORIENTED_EDGE('',*,*,#14798,.T.);
#21629=ORIENTED_EDGE('',*,*,#14799,.T.);
#21630=ORIENTED_EDGE('',*,*,#14792,.F.);
#21631=ORIENTED_EDGE('',*,*,#14800,.F.);
#21632=ORIENTED_EDGE('',*,*,#14797,.F.);
#21633=ORIENTED_EDGE('',*,*,#14801,.F.);
#21634=ORIENTED_EDGE('',*,*,#14802,.T.);
#21635=ORIENTED_EDGE('',*,*,#14803,.T.);
#21636=ORIENTED_EDGE('',*,*,#14804,.T.);
#21637=ORIENTED_EDGE('',*,*,#14805,.T.);
#21638=ORIENTED_EDGE('',*,*,#14803,.F.);
#21639=ORIENTED_EDGE('',*,*,#14806,.F.);
#21640=ORIENTED_EDGE('',*,*,#14807,.T.);
#21641=ORIENTED_EDGE('',*,*,#14808,.F.);
#21642=ORIENTED_EDGE('',*,*,#14809,.T.);
#21643=ORIENTED_EDGE('',*,*,#14810,.T.);
#21644=ORIENTED_EDGE('',*,*,#14811,.T.);
#21645=ORIENTED_EDGE('',*,*,#14812,.T.);
#21646=ORIENTED_EDGE('',*,*,#14805,.F.);
#21647=ORIENTED_EDGE('',*,*,#14813,.F.);
#21648=ORIENTED_EDGE('',*,*,#14810,.F.);
#21649=ORIENTED_EDGE('',*,*,#14814,.F.);
#21650=ORIENTED_EDGE('',*,*,#14815,.T.);
#21651=ORIENTED_EDGE('',*,*,#14816,.T.);
#21652=ORIENTED_EDGE('',*,*,#14817,.T.);
#21653=ORIENTED_EDGE('',*,*,#14818,.T.);
#21654=ORIENTED_EDGE('',*,*,#14816,.F.);
#21655=ORIENTED_EDGE('',*,*,#14819,.F.);
#21656=ORIENTED_EDGE('',*,*,#14820,.T.);
#21657=ORIENTED_EDGE('',*,*,#14821,.F.);
#21658=ORIENTED_EDGE('',*,*,#14822,.T.);
#21659=ORIENTED_EDGE('',*,*,#14823,.T.);
#21660=ORIENTED_EDGE('',*,*,#14824,.T.);
#21661=ORIENTED_EDGE('',*,*,#14825,.T.);
#21662=ORIENTED_EDGE('',*,*,#14818,.F.);
#21663=ORIENTED_EDGE('',*,*,#14826,.F.);
#21664=ORIENTED_EDGE('',*,*,#14823,.F.);
#21665=ORIENTED_EDGE('',*,*,#14827,.F.);
#21666=ORIENTED_EDGE('',*,*,#14828,.T.);
#21667=ORIENTED_EDGE('',*,*,#14829,.T.);
#21668=ORIENTED_EDGE('',*,*,#14830,.T.);
#21669=ORIENTED_EDGE('',*,*,#14831,.T.);
#21670=ORIENTED_EDGE('',*,*,#14829,.F.);
#21671=ORIENTED_EDGE('',*,*,#14832,.F.);
#21672=ORIENTED_EDGE('',*,*,#14833,.T.);
#21673=ORIENTED_EDGE('',*,*,#14834,.F.);
#21674=ORIENTED_EDGE('',*,*,#14835,.T.);
#21675=ORIENTED_EDGE('',*,*,#14836,.T.);
#21676=ORIENTED_EDGE('',*,*,#14837,.T.);
#21677=ORIENTED_EDGE('',*,*,#14838,.T.);
#21678=ORIENTED_EDGE('',*,*,#14831,.F.);
#21679=ORIENTED_EDGE('',*,*,#14839,.F.);
#21680=ORIENTED_EDGE('',*,*,#14836,.F.);
#21681=ORIENTED_EDGE('',*,*,#14840,.F.);
#21682=ORIENTED_EDGE('',*,*,#14552,.F.);
#21683=ORIENTED_EDGE('',*,*,#14841,.F.);
#21684=ORIENTED_EDGE('',*,*,#14842,.F.);
#21685=ORIENTED_EDGE('',*,*,#14843,.F.);
#21686=ORIENTED_EDGE('',*,*,#14844,.F.);
#21687=ORIENTED_EDGE('',*,*,#14845,.F.);
#21688=ORIENTED_EDGE('',*,*,#14846,.F.);
#21689=ORIENTED_EDGE('',*,*,#14547,.F.);
#21690=ORIENTED_EDGE('',*,*,#14847,.F.);
#21691=ORIENTED_EDGE('',*,*,#14842,.T.);
#21692=ORIENTED_EDGE('',*,*,#14848,.F.);
#21693=ORIENTED_EDGE('',*,*,#14849,.F.);
#21694=ORIENTED_EDGE('',*,*,#14565,.F.);
#21695=ORIENTED_EDGE('',*,*,#14850,.F.);
#21696=ORIENTED_EDGE('',*,*,#14851,.F.);
#21697=ORIENTED_EDGE('',*,*,#14852,.F.);
#21698=ORIENTED_EDGE('',*,*,#14853,.F.);
#21699=ORIENTED_EDGE('',*,*,#14854,.F.);
#21700=ORIENTED_EDGE('',*,*,#14855,.F.);
#21701=ORIENTED_EDGE('',*,*,#14560,.F.);
#21702=ORIENTED_EDGE('',*,*,#14856,.F.);
#21703=ORIENTED_EDGE('',*,*,#14851,.T.);
#21704=ORIENTED_EDGE('',*,*,#14857,.F.);
#21705=ORIENTED_EDGE('',*,*,#14858,.F.);
#21706=ORIENTED_EDGE('',*,*,#14578,.F.);
#21707=ORIENTED_EDGE('',*,*,#14859,.F.);
#21708=ORIENTED_EDGE('',*,*,#14860,.F.);
#21709=ORIENTED_EDGE('',*,*,#14861,.F.);
#21710=ORIENTED_EDGE('',*,*,#14862,.F.);
#21711=ORIENTED_EDGE('',*,*,#14863,.F.);
#21712=ORIENTED_EDGE('',*,*,#14864,.F.);
#21713=ORIENTED_EDGE('',*,*,#14573,.F.);
#21714=ORIENTED_EDGE('',*,*,#14865,.F.);
#21715=ORIENTED_EDGE('',*,*,#14860,.T.);
#21716=ORIENTED_EDGE('',*,*,#14866,.F.);
#21717=ORIENTED_EDGE('',*,*,#14867,.F.);
#21718=ORIENTED_EDGE('',*,*,#14591,.F.);
#21719=ORIENTED_EDGE('',*,*,#14868,.F.);
#21720=ORIENTED_EDGE('',*,*,#14869,.F.);
#21721=ORIENTED_EDGE('',*,*,#14870,.F.);
#21722=ORIENTED_EDGE('',*,*,#14871,.F.);
#21723=ORIENTED_EDGE('',*,*,#14872,.F.);
#21724=ORIENTED_EDGE('',*,*,#14873,.F.);
#21725=ORIENTED_EDGE('',*,*,#14586,.F.);
#21726=ORIENTED_EDGE('',*,*,#14874,.F.);
#21727=ORIENTED_EDGE('',*,*,#14869,.T.);
#21728=ORIENTED_EDGE('',*,*,#14875,.F.);
#21729=ORIENTED_EDGE('',*,*,#14876,.F.);
#21730=ORIENTED_EDGE('',*,*,#14604,.F.);
#21731=ORIENTED_EDGE('',*,*,#14877,.F.);
#21732=ORIENTED_EDGE('',*,*,#14878,.F.);
#21733=ORIENTED_EDGE('',*,*,#14879,.F.);
#21734=ORIENTED_EDGE('',*,*,#14880,.F.);
#21735=ORIENTED_EDGE('',*,*,#14881,.F.);
#21736=ORIENTED_EDGE('',*,*,#14882,.F.);
#21737=ORIENTED_EDGE('',*,*,#14599,.F.);
#21738=ORIENTED_EDGE('',*,*,#14883,.F.);
#21739=ORIENTED_EDGE('',*,*,#14878,.T.);
#21740=ORIENTED_EDGE('',*,*,#14884,.F.);
#21741=ORIENTED_EDGE('',*,*,#14885,.F.);
#21742=ORIENTED_EDGE('',*,*,#14617,.F.);
#21743=ORIENTED_EDGE('',*,*,#14886,.F.);
#21744=ORIENTED_EDGE('',*,*,#14887,.F.);
#21745=ORIENTED_EDGE('',*,*,#14888,.F.);
#21746=ORIENTED_EDGE('',*,*,#14889,.F.);
#21747=ORIENTED_EDGE('',*,*,#14890,.F.);
#21748=ORIENTED_EDGE('',*,*,#14891,.F.);
#21749=ORIENTED_EDGE('',*,*,#14612,.F.);
#21750=ORIENTED_EDGE('',*,*,#14892,.F.);
#21751=ORIENTED_EDGE('',*,*,#14887,.T.);
#21752=ORIENTED_EDGE('',*,*,#14893,.F.);
#21753=ORIENTED_EDGE('',*,*,#14894,.F.);
#21754=ORIENTED_EDGE('',*,*,#14630,.F.);
#21755=ORIENTED_EDGE('',*,*,#14895,.F.);
#21756=ORIENTED_EDGE('',*,*,#14896,.F.);
#21757=ORIENTED_EDGE('',*,*,#14897,.F.);
#21758=ORIENTED_EDGE('',*,*,#14898,.F.);
#21759=ORIENTED_EDGE('',*,*,#14899,.F.);
#21760=ORIENTED_EDGE('',*,*,#14900,.F.);
#21761=ORIENTED_EDGE('',*,*,#14625,.F.);
#21762=ORIENTED_EDGE('',*,*,#14901,.F.);
#21763=ORIENTED_EDGE('',*,*,#14896,.T.);
#21764=ORIENTED_EDGE('',*,*,#14902,.F.);
#21765=ORIENTED_EDGE('',*,*,#14903,.F.);
#21766=ORIENTED_EDGE('',*,*,#14643,.F.);
#21767=ORIENTED_EDGE('',*,*,#14904,.F.);
#21768=ORIENTED_EDGE('',*,*,#14905,.F.);
#21769=ORIENTED_EDGE('',*,*,#14906,.F.);
#21770=ORIENTED_EDGE('',*,*,#14907,.F.);
#21771=ORIENTED_EDGE('',*,*,#14908,.F.);
#21772=ORIENTED_EDGE('',*,*,#14909,.F.);
#21773=ORIENTED_EDGE('',*,*,#14638,.F.);
#21774=ORIENTED_EDGE('',*,*,#14910,.F.);
#21775=ORIENTED_EDGE('',*,*,#14905,.T.);
#21776=ORIENTED_EDGE('',*,*,#14911,.F.);
#21777=ORIENTED_EDGE('',*,*,#14912,.F.);
#21778=ORIENTED_EDGE('',*,*,#14656,.F.);
#21779=ORIENTED_EDGE('',*,*,#14913,.F.);
#21780=ORIENTED_EDGE('',*,*,#14914,.F.);
#21781=ORIENTED_EDGE('',*,*,#14915,.F.);
#21782=ORIENTED_EDGE('',*,*,#14916,.F.);
#21783=ORIENTED_EDGE('',*,*,#14917,.F.);
#21784=ORIENTED_EDGE('',*,*,#14918,.F.);
#21785=ORIENTED_EDGE('',*,*,#14651,.F.);
#21786=ORIENTED_EDGE('',*,*,#14919,.F.);
#21787=ORIENTED_EDGE('',*,*,#14914,.T.);
#21788=ORIENTED_EDGE('',*,*,#14920,.F.);
#21789=ORIENTED_EDGE('',*,*,#14921,.F.);
#21790=ORIENTED_EDGE('',*,*,#14669,.F.);
#21791=ORIENTED_EDGE('',*,*,#14922,.F.);
#21792=ORIENTED_EDGE('',*,*,#14923,.F.);
#21793=ORIENTED_EDGE('',*,*,#14924,.F.);
#21794=ORIENTED_EDGE('',*,*,#14925,.F.);
#21795=ORIENTED_EDGE('',*,*,#14926,.F.);
#21796=ORIENTED_EDGE('',*,*,#14927,.F.);
#21797=ORIENTED_EDGE('',*,*,#14664,.F.);
#21798=ORIENTED_EDGE('',*,*,#14928,.F.);
#21799=ORIENTED_EDGE('',*,*,#14923,.T.);
#21800=ORIENTED_EDGE('',*,*,#14929,.F.);
#21801=ORIENTED_EDGE('',*,*,#14930,.F.);
#21802=ORIENTED_EDGE('',*,*,#14682,.F.);
#21803=ORIENTED_EDGE('',*,*,#14931,.F.);
#21804=ORIENTED_EDGE('',*,*,#14932,.F.);
#21805=ORIENTED_EDGE('',*,*,#14933,.F.);
#21806=ORIENTED_EDGE('',*,*,#14934,.F.);
#21807=ORIENTED_EDGE('',*,*,#14935,.F.);
#21808=ORIENTED_EDGE('',*,*,#14936,.F.);
#21809=ORIENTED_EDGE('',*,*,#14677,.F.);
#21810=ORIENTED_EDGE('',*,*,#14937,.F.);
#21811=ORIENTED_EDGE('',*,*,#14932,.T.);
#21812=ORIENTED_EDGE('',*,*,#14938,.F.);
#21813=ORIENTED_EDGE('',*,*,#14939,.F.);
#21814=ORIENTED_EDGE('',*,*,#14695,.F.);
#21815=ORIENTED_EDGE('',*,*,#14940,.F.);
#21816=ORIENTED_EDGE('',*,*,#14941,.F.);
#21817=ORIENTED_EDGE('',*,*,#14942,.F.);
#21818=ORIENTED_EDGE('',*,*,#14943,.F.);
#21819=ORIENTED_EDGE('',*,*,#14944,.F.);
#21820=ORIENTED_EDGE('',*,*,#14945,.F.);
#21821=ORIENTED_EDGE('',*,*,#14690,.F.);
#21822=ORIENTED_EDGE('',*,*,#14946,.F.);
#21823=ORIENTED_EDGE('',*,*,#14941,.T.);
#21824=ORIENTED_EDGE('',*,*,#14947,.F.);
#21825=ORIENTED_EDGE('',*,*,#14948,.F.);
#21826=ORIENTED_EDGE('',*,*,#14708,.F.);
#21827=ORIENTED_EDGE('',*,*,#14949,.F.);
#21828=ORIENTED_EDGE('',*,*,#14950,.F.);
#21829=ORIENTED_EDGE('',*,*,#14951,.F.);
#21830=ORIENTED_EDGE('',*,*,#14952,.F.);
#21831=ORIENTED_EDGE('',*,*,#14953,.F.);
#21832=ORIENTED_EDGE('',*,*,#14954,.F.);
#21833=ORIENTED_EDGE('',*,*,#14703,.F.);
#21834=ORIENTED_EDGE('',*,*,#14955,.F.);
#21835=ORIENTED_EDGE('',*,*,#14950,.T.);
#21836=ORIENTED_EDGE('',*,*,#14956,.F.);
#21837=ORIENTED_EDGE('',*,*,#14957,.F.);
#21838=ORIENTED_EDGE('',*,*,#14721,.F.);
#21839=ORIENTED_EDGE('',*,*,#14958,.F.);
#21840=ORIENTED_EDGE('',*,*,#14959,.F.);
#21841=ORIENTED_EDGE('',*,*,#14960,.F.);
#21842=ORIENTED_EDGE('',*,*,#14961,.F.);
#21843=ORIENTED_EDGE('',*,*,#14962,.F.);
#21844=ORIENTED_EDGE('',*,*,#14963,.F.);
#21845=ORIENTED_EDGE('',*,*,#14716,.F.);
#21846=ORIENTED_EDGE('',*,*,#14964,.F.);
#21847=ORIENTED_EDGE('',*,*,#14959,.T.);
#21848=ORIENTED_EDGE('',*,*,#14965,.F.);
#21849=ORIENTED_EDGE('',*,*,#14966,.F.);
#21850=ORIENTED_EDGE('',*,*,#14734,.F.);
#21851=ORIENTED_EDGE('',*,*,#14967,.F.);
#21852=ORIENTED_EDGE('',*,*,#14968,.F.);
#21853=ORIENTED_EDGE('',*,*,#14969,.F.);
#21854=ORIENTED_EDGE('',*,*,#14970,.F.);
#21855=ORIENTED_EDGE('',*,*,#14971,.F.);
#21856=ORIENTED_EDGE('',*,*,#14972,.F.);
#21857=ORIENTED_EDGE('',*,*,#14729,.F.);
#21858=ORIENTED_EDGE('',*,*,#14973,.F.);
#21859=ORIENTED_EDGE('',*,*,#14968,.T.);
#21860=ORIENTED_EDGE('',*,*,#14974,.F.);
#21861=ORIENTED_EDGE('',*,*,#14975,.F.);
#21862=ORIENTED_EDGE('',*,*,#14747,.F.);
#21863=ORIENTED_EDGE('',*,*,#14976,.F.);
#21864=ORIENTED_EDGE('',*,*,#14977,.F.);
#21865=ORIENTED_EDGE('',*,*,#14978,.F.);
#21866=ORIENTED_EDGE('',*,*,#14979,.F.);
#21867=ORIENTED_EDGE('',*,*,#14980,.F.);
#21868=ORIENTED_EDGE('',*,*,#14981,.F.);
#21869=ORIENTED_EDGE('',*,*,#14742,.F.);
#21870=ORIENTED_EDGE('',*,*,#14982,.F.);
#21871=ORIENTED_EDGE('',*,*,#14977,.T.);
#21872=ORIENTED_EDGE('',*,*,#14983,.F.);
#21873=ORIENTED_EDGE('',*,*,#14984,.F.);
#21874=ORIENTED_EDGE('',*,*,#14760,.F.);
#21875=ORIENTED_EDGE('',*,*,#14985,.F.);
#21876=ORIENTED_EDGE('',*,*,#14986,.F.);
#21877=ORIENTED_EDGE('',*,*,#14987,.F.);
#21878=ORIENTED_EDGE('',*,*,#14988,.F.);
#21879=ORIENTED_EDGE('',*,*,#14989,.F.);
#21880=ORIENTED_EDGE('',*,*,#14990,.F.);
#21881=ORIENTED_EDGE('',*,*,#14755,.F.);
#21882=ORIENTED_EDGE('',*,*,#14991,.F.);
#21883=ORIENTED_EDGE('',*,*,#14986,.T.);
#21884=ORIENTED_EDGE('',*,*,#14992,.F.);
#21885=ORIENTED_EDGE('',*,*,#14993,.F.);
#21886=ORIENTED_EDGE('',*,*,#14773,.F.);
#21887=ORIENTED_EDGE('',*,*,#14994,.F.);
#21888=ORIENTED_EDGE('',*,*,#14995,.F.);
#21889=ORIENTED_EDGE('',*,*,#14996,.F.);
#21890=ORIENTED_EDGE('',*,*,#14997,.F.);
#21891=ORIENTED_EDGE('',*,*,#14998,.F.);
#21892=ORIENTED_EDGE('',*,*,#14999,.F.);
#21893=ORIENTED_EDGE('',*,*,#14768,.F.);
#21894=ORIENTED_EDGE('',*,*,#15000,.F.);
#21895=ORIENTED_EDGE('',*,*,#14995,.T.);
#21896=ORIENTED_EDGE('',*,*,#15001,.F.);
#21897=ORIENTED_EDGE('',*,*,#15002,.F.);
#21898=ORIENTED_EDGE('',*,*,#14786,.F.);
#21899=ORIENTED_EDGE('',*,*,#15003,.F.);
#21900=ORIENTED_EDGE('',*,*,#15004,.F.);
#21901=ORIENTED_EDGE('',*,*,#15005,.F.);
#21902=ORIENTED_EDGE('',*,*,#15006,.F.);
#21903=ORIENTED_EDGE('',*,*,#15007,.F.);
#21904=ORIENTED_EDGE('',*,*,#15008,.F.);
#21905=ORIENTED_EDGE('',*,*,#14781,.F.);
#21906=ORIENTED_EDGE('',*,*,#15009,.F.);
#21907=ORIENTED_EDGE('',*,*,#15004,.T.);
#21908=ORIENTED_EDGE('',*,*,#15010,.F.);
#21909=ORIENTED_EDGE('',*,*,#15011,.F.);
#21910=ORIENTED_EDGE('',*,*,#14799,.F.);
#21911=ORIENTED_EDGE('',*,*,#15012,.F.);
#21912=ORIENTED_EDGE('',*,*,#15013,.F.);
#21913=ORIENTED_EDGE('',*,*,#15014,.F.);
#21914=ORIENTED_EDGE('',*,*,#15015,.F.);
#21915=ORIENTED_EDGE('',*,*,#15016,.F.);
#21916=ORIENTED_EDGE('',*,*,#15017,.F.);
#21917=ORIENTED_EDGE('',*,*,#14794,.F.);
#21918=ORIENTED_EDGE('',*,*,#15018,.F.);
#21919=ORIENTED_EDGE('',*,*,#15013,.T.);
#21920=ORIENTED_EDGE('',*,*,#15019,.F.);
#21921=ORIENTED_EDGE('',*,*,#15020,.F.);
#21922=ORIENTED_EDGE('',*,*,#14812,.F.);
#21923=ORIENTED_EDGE('',*,*,#15021,.F.);
#21924=ORIENTED_EDGE('',*,*,#15022,.F.);
#21925=ORIENTED_EDGE('',*,*,#15023,.F.);
#21926=ORIENTED_EDGE('',*,*,#15024,.F.);
#21927=ORIENTED_EDGE('',*,*,#15025,.F.);
#21928=ORIENTED_EDGE('',*,*,#15026,.F.);
#21929=ORIENTED_EDGE('',*,*,#14807,.F.);
#21930=ORIENTED_EDGE('',*,*,#15027,.F.);
#21931=ORIENTED_EDGE('',*,*,#15022,.T.);
#21932=ORIENTED_EDGE('',*,*,#15028,.F.);
#21933=ORIENTED_EDGE('',*,*,#15029,.F.);
#21934=ORIENTED_EDGE('',*,*,#14825,.F.);
#21935=ORIENTED_EDGE('',*,*,#15030,.F.);
#21936=ORIENTED_EDGE('',*,*,#15031,.F.);
#21937=ORIENTED_EDGE('',*,*,#15032,.F.);
#21938=ORIENTED_EDGE('',*,*,#15033,.F.);
#21939=ORIENTED_EDGE('',*,*,#15034,.F.);
#21940=ORIENTED_EDGE('',*,*,#15035,.F.);
#21941=ORIENTED_EDGE('',*,*,#14820,.F.);
#21942=ORIENTED_EDGE('',*,*,#15036,.F.);
#21943=ORIENTED_EDGE('',*,*,#15031,.T.);
#21944=ORIENTED_EDGE('',*,*,#15037,.F.);
#21945=ORIENTED_EDGE('',*,*,#15038,.F.);
#21946=ORIENTED_EDGE('',*,*,#14838,.F.);
#21947=ORIENTED_EDGE('',*,*,#15039,.F.);
#21948=ORIENTED_EDGE('',*,*,#15040,.F.);
#21949=ORIENTED_EDGE('',*,*,#15041,.F.);
#21950=ORIENTED_EDGE('',*,*,#15042,.F.);
#21951=ORIENTED_EDGE('',*,*,#15043,.F.);
#21952=ORIENTED_EDGE('',*,*,#15044,.F.);
#21953=ORIENTED_EDGE('',*,*,#14833,.F.);
#21954=ORIENTED_EDGE('',*,*,#15045,.F.);
#21955=ORIENTED_EDGE('',*,*,#15040,.T.);
#21956=ORIENTED_EDGE('',*,*,#15046,.F.);
#21957=ORIENTED_EDGE('',*,*,#15047,.F.);
#21958=ORIENTED_EDGE('',*,*,#14844,.T.);
#21959=ORIENTED_EDGE('',*,*,#14546,.T.);
#21960=ORIENTED_EDGE('',*,*,#14542,.F.);
#21961=ORIENTED_EDGE('',*,*,#14554,.T.);
#21962=ORIENTED_EDGE('',*,*,#14549,.F.);
#21963=ORIENTED_EDGE('',*,*,#14843,.T.);
#21964=ORIENTED_EDGE('',*,*,#14847,.T.);
#21965=ORIENTED_EDGE('',*,*,#15048,.F.);
#21966=ORIENTED_EDGE('',*,*,#14853,.T.);
#21967=ORIENTED_EDGE('',*,*,#14559,.T.);
#21968=ORIENTED_EDGE('',*,*,#14555,.F.);
#21969=ORIENTED_EDGE('',*,*,#14567,.T.);
#21970=ORIENTED_EDGE('',*,*,#14562,.F.);
#21971=ORIENTED_EDGE('',*,*,#14852,.T.);
#21972=ORIENTED_EDGE('',*,*,#14856,.T.);
#21973=ORIENTED_EDGE('',*,*,#15049,.F.);
#21974=ORIENTED_EDGE('',*,*,#14862,.T.);
#21975=ORIENTED_EDGE('',*,*,#14572,.T.);
#21976=ORIENTED_EDGE('',*,*,#14568,.F.);
#21977=ORIENTED_EDGE('',*,*,#14580,.T.);
#21978=ORIENTED_EDGE('',*,*,#14575,.F.);
#21979=ORIENTED_EDGE('',*,*,#14861,.T.);
#21980=ORIENTED_EDGE('',*,*,#14865,.T.);
#21981=ORIENTED_EDGE('',*,*,#15050,.F.);
#21982=ORIENTED_EDGE('',*,*,#14871,.T.);
#21983=ORIENTED_EDGE('',*,*,#14585,.T.);
#21984=ORIENTED_EDGE('',*,*,#14581,.F.);
#21985=ORIENTED_EDGE('',*,*,#14593,.T.);
#21986=ORIENTED_EDGE('',*,*,#14588,.F.);
#21987=ORIENTED_EDGE('',*,*,#14870,.T.);
#21988=ORIENTED_EDGE('',*,*,#14874,.T.);
#21989=ORIENTED_EDGE('',*,*,#15051,.F.);
#21990=ORIENTED_EDGE('',*,*,#14880,.T.);
#21991=ORIENTED_EDGE('',*,*,#14598,.T.);
#21992=ORIENTED_EDGE('',*,*,#14594,.F.);
#21993=ORIENTED_EDGE('',*,*,#14606,.T.);
#21994=ORIENTED_EDGE('',*,*,#14601,.F.);
#21995=ORIENTED_EDGE('',*,*,#14879,.T.);
#21996=ORIENTED_EDGE('',*,*,#14883,.T.);
#21997=ORIENTED_EDGE('',*,*,#15052,.F.);
#21998=ORIENTED_EDGE('',*,*,#14889,.T.);
#21999=ORIENTED_EDGE('',*,*,#14611,.T.);
#22000=ORIENTED_EDGE('',*,*,#14607,.F.);
#22001=ORIENTED_EDGE('',*,*,#14619,.T.);
#22002=ORIENTED_EDGE('',*,*,#14614,.F.);
#22003=ORIENTED_EDGE('',*,*,#14888,.T.);
#22004=ORIENTED_EDGE('',*,*,#14892,.T.);
#22005=ORIENTED_EDGE('',*,*,#15053,.F.);
#22006=ORIENTED_EDGE('',*,*,#14898,.T.);
#22007=ORIENTED_EDGE('',*,*,#14624,.T.);
#22008=ORIENTED_EDGE('',*,*,#14620,.F.);
#22009=ORIENTED_EDGE('',*,*,#14632,.T.);
#22010=ORIENTED_EDGE('',*,*,#14627,.F.);
#22011=ORIENTED_EDGE('',*,*,#14897,.T.);
#22012=ORIENTED_EDGE('',*,*,#14901,.T.);
#22013=ORIENTED_EDGE('',*,*,#15054,.F.);
#22014=ORIENTED_EDGE('',*,*,#14907,.T.);
#22015=ORIENTED_EDGE('',*,*,#14637,.T.);
#22016=ORIENTED_EDGE('',*,*,#14633,.F.);
#22017=ORIENTED_EDGE('',*,*,#14645,.T.);
#22018=ORIENTED_EDGE('',*,*,#14640,.F.);
#22019=ORIENTED_EDGE('',*,*,#14906,.T.);
#22020=ORIENTED_EDGE('',*,*,#14910,.T.);
#22021=ORIENTED_EDGE('',*,*,#15055,.F.);
#22022=ORIENTED_EDGE('',*,*,#14916,.T.);
#22023=ORIENTED_EDGE('',*,*,#14650,.T.);
#22024=ORIENTED_EDGE('',*,*,#14646,.F.);
#22025=ORIENTED_EDGE('',*,*,#14658,.T.);
#22026=ORIENTED_EDGE('',*,*,#14653,.F.);
#22027=ORIENTED_EDGE('',*,*,#14915,.T.);
#22028=ORIENTED_EDGE('',*,*,#14919,.T.);
#22029=ORIENTED_EDGE('',*,*,#15056,.F.);
#22030=ORIENTED_EDGE('',*,*,#14925,.T.);
#22031=ORIENTED_EDGE('',*,*,#14663,.T.);
#22032=ORIENTED_EDGE('',*,*,#14659,.F.);
#22033=ORIENTED_EDGE('',*,*,#14671,.T.);
#22034=ORIENTED_EDGE('',*,*,#14666,.F.);
#22035=ORIENTED_EDGE('',*,*,#14924,.T.);
#22036=ORIENTED_EDGE('',*,*,#14928,.T.);
#22037=ORIENTED_EDGE('',*,*,#15057,.F.);
#22038=ORIENTED_EDGE('',*,*,#14934,.T.);
#22039=ORIENTED_EDGE('',*,*,#14676,.T.);
#22040=ORIENTED_EDGE('',*,*,#14672,.F.);
#22041=ORIENTED_EDGE('',*,*,#14684,.T.);
#22042=ORIENTED_EDGE('',*,*,#14679,.F.);
#22043=ORIENTED_EDGE('',*,*,#14933,.T.);
#22044=ORIENTED_EDGE('',*,*,#14937,.T.);
#22045=ORIENTED_EDGE('',*,*,#15058,.F.);
#22046=ORIENTED_EDGE('',*,*,#14943,.T.);
#22047=ORIENTED_EDGE('',*,*,#14689,.T.);
#22048=ORIENTED_EDGE('',*,*,#14685,.F.);
#22049=ORIENTED_EDGE('',*,*,#14697,.T.);
#22050=ORIENTED_EDGE('',*,*,#14692,.F.);
#22051=ORIENTED_EDGE('',*,*,#14942,.T.);
#22052=ORIENTED_EDGE('',*,*,#14946,.T.);
#22053=ORIENTED_EDGE('',*,*,#15059,.F.);
#22054=ORIENTED_EDGE('',*,*,#14952,.T.);
#22055=ORIENTED_EDGE('',*,*,#14702,.T.);
#22056=ORIENTED_EDGE('',*,*,#14698,.F.);
#22057=ORIENTED_EDGE('',*,*,#14710,.T.);
#22058=ORIENTED_EDGE('',*,*,#14705,.F.);
#22059=ORIENTED_EDGE('',*,*,#14951,.T.);
#22060=ORIENTED_EDGE('',*,*,#14955,.T.);
#22061=ORIENTED_EDGE('',*,*,#15060,.F.);
#22062=ORIENTED_EDGE('',*,*,#14961,.T.);
#22063=ORIENTED_EDGE('',*,*,#14715,.T.);
#22064=ORIENTED_EDGE('',*,*,#14711,.F.);
#22065=ORIENTED_EDGE('',*,*,#14723,.T.);
#22066=ORIENTED_EDGE('',*,*,#14718,.F.);
#22067=ORIENTED_EDGE('',*,*,#14960,.T.);
#22068=ORIENTED_EDGE('',*,*,#14964,.T.);
#22069=ORIENTED_EDGE('',*,*,#15061,.F.);
#22070=ORIENTED_EDGE('',*,*,#14970,.T.);
#22071=ORIENTED_EDGE('',*,*,#14728,.T.);
#22072=ORIENTED_EDGE('',*,*,#14724,.F.);
#22073=ORIENTED_EDGE('',*,*,#14736,.T.);
#22074=ORIENTED_EDGE('',*,*,#14731,.F.);
#22075=ORIENTED_EDGE('',*,*,#14969,.T.);
#22076=ORIENTED_EDGE('',*,*,#14973,.T.);
#22077=ORIENTED_EDGE('',*,*,#15062,.F.);
#22078=ORIENTED_EDGE('',*,*,#14979,.T.);
#22079=ORIENTED_EDGE('',*,*,#14741,.T.);
#22080=ORIENTED_EDGE('',*,*,#14737,.F.);
#22081=ORIENTED_EDGE('',*,*,#14749,.T.);
#22082=ORIENTED_EDGE('',*,*,#14744,.F.);
#22083=ORIENTED_EDGE('',*,*,#14978,.T.);
#22084=ORIENTED_EDGE('',*,*,#14982,.T.);
#22085=ORIENTED_EDGE('',*,*,#15063,.F.);
#22086=ORIENTED_EDGE('',*,*,#14988,.T.);
#22087=ORIENTED_EDGE('',*,*,#14754,.T.);
#22088=ORIENTED_EDGE('',*,*,#14750,.F.);
#22089=ORIENTED_EDGE('',*,*,#14762,.T.);
#22090=ORIENTED_EDGE('',*,*,#14757,.F.);
#22091=ORIENTED_EDGE('',*,*,#14987,.T.);
#22092=ORIENTED_EDGE('',*,*,#14991,.T.);
#22093=ORIENTED_EDGE('',*,*,#15064,.F.);
#22094=ORIENTED_EDGE('',*,*,#14997,.T.);
#22095=ORIENTED_EDGE('',*,*,#14767,.T.);
#22096=ORIENTED_EDGE('',*,*,#14763,.F.);
#22097=ORIENTED_EDGE('',*,*,#14775,.T.);
#22098=ORIENTED_EDGE('',*,*,#14770,.F.);
#22099=ORIENTED_EDGE('',*,*,#14996,.T.);
#22100=ORIENTED_EDGE('',*,*,#15000,.T.);
#22101=ORIENTED_EDGE('',*,*,#15065,.F.);
#22102=ORIENTED_EDGE('',*,*,#15006,.T.);
#22103=ORIENTED_EDGE('',*,*,#14780,.T.);
#22104=ORIENTED_EDGE('',*,*,#14776,.F.);
#22105=ORIENTED_EDGE('',*,*,#14788,.T.);
#22106=ORIENTED_EDGE('',*,*,#14783,.F.);
#22107=ORIENTED_EDGE('',*,*,#15005,.T.);
#22108=ORIENTED_EDGE('',*,*,#15009,.T.);
#22109=ORIENTED_EDGE('',*,*,#15066,.F.);
#22110=ORIENTED_EDGE('',*,*,#15015,.T.);
#22111=ORIENTED_EDGE('',*,*,#14793,.T.);
#22112=ORIENTED_EDGE('',*,*,#14789,.F.);
#22113=ORIENTED_EDGE('',*,*,#14801,.T.);
#22114=ORIENTED_EDGE('',*,*,#14796,.F.);
#22115=ORIENTED_EDGE('',*,*,#15014,.T.);
#22116=ORIENTED_EDGE('',*,*,#15018,.T.);
#22117=ORIENTED_EDGE('',*,*,#15067,.F.);
#22118=ORIENTED_EDGE('',*,*,#15024,.T.);
#22119=ORIENTED_EDGE('',*,*,#14806,.T.);
#22120=ORIENTED_EDGE('',*,*,#14802,.F.);
#22121=ORIENTED_EDGE('',*,*,#14814,.T.);
#22122=ORIENTED_EDGE('',*,*,#14809,.F.);
#22123=ORIENTED_EDGE('',*,*,#15023,.T.);
#22124=ORIENTED_EDGE('',*,*,#15027,.T.);
#22125=ORIENTED_EDGE('',*,*,#15068,.F.);
#22126=ORIENTED_EDGE('',*,*,#15033,.T.);
#22127=ORIENTED_EDGE('',*,*,#14819,.T.);
#22128=ORIENTED_EDGE('',*,*,#14815,.F.);
#22129=ORIENTED_EDGE('',*,*,#14827,.T.);
#22130=ORIENTED_EDGE('',*,*,#14822,.F.);
#22131=ORIENTED_EDGE('',*,*,#15032,.T.);
#22132=ORIENTED_EDGE('',*,*,#15036,.T.);
#22133=ORIENTED_EDGE('',*,*,#15069,.F.);
#22134=ORIENTED_EDGE('',*,*,#15042,.T.);
#22135=ORIENTED_EDGE('',*,*,#14832,.T.);
#22136=ORIENTED_EDGE('',*,*,#14828,.F.);
#22137=ORIENTED_EDGE('',*,*,#14840,.T.);
#22138=ORIENTED_EDGE('',*,*,#14835,.F.);
#22139=ORIENTED_EDGE('',*,*,#15041,.T.);
#22140=ORIENTED_EDGE('',*,*,#15045,.T.);
#22141=ORIENTED_EDGE('',*,*,#15070,.F.);
#22142=ORIENTED_EDGE('',*,*,#15071,.T.);
#22143=ORIENTED_EDGE('',*,*,#15072,.T.);
#22144=ORIENTED_EDGE('',*,*,#15073,.F.);
#22145=ORIENTED_EDGE('',*,*,#15074,.T.);
#22146=ORIENTED_EDGE('',*,*,#15075,.F.);
#22147=ORIENTED_EDGE('',*,*,#15076,.T.);
#22148=ORIENTED_EDGE('',*,*,#15077,.T.);
#22149=ORIENTED_EDGE('',*,*,#15078,.F.);
#22150=ORIENTED_EDGE('',*,*,#15079,.F.);
#22151=ORIENTED_EDGE('',*,*,#14846,.T.);
#22152=ORIENTED_EDGE('',*,*,#15080,.T.);
#22153=ORIENTED_EDGE('',*,*,#15081,.T.);
#22154=ORIENTED_EDGE('',*,*,#15082,.T.);
#22155=ORIENTED_EDGE('',*,*,#15083,.F.);
#22156=ORIENTED_EDGE('',*,*,#15084,.T.);
#22157=ORIENTED_EDGE('',*,*,#15085,.F.);
#22158=ORIENTED_EDGE('',*,*,#15086,.T.);
#22159=ORIENTED_EDGE('',*,*,#15087,.T.);
#22160=ORIENTED_EDGE('',*,*,#15088,.T.);
#22161=ORIENTED_EDGE('',*,*,#15046,.T.);
#22162=ORIENTED_EDGE('',*,*,#15039,.T.);
#22163=ORIENTED_EDGE('',*,*,#14837,.F.);
#22164=ORIENTED_EDGE('',*,*,#14839,.T.);
#22165=ORIENTED_EDGE('',*,*,#14830,.F.);
#22166=ORIENTED_EDGE('',*,*,#14834,.T.);
#22167=ORIENTED_EDGE('',*,*,#15044,.T.);
#22168=ORIENTED_EDGE('',*,*,#15089,.T.);
#22169=ORIENTED_EDGE('',*,*,#15037,.T.);
#22170=ORIENTED_EDGE('',*,*,#15030,.T.);
#22171=ORIENTED_EDGE('',*,*,#14824,.F.);
#22172=ORIENTED_EDGE('',*,*,#14826,.T.);
#22173=ORIENTED_EDGE('',*,*,#14817,.F.);
#22174=ORIENTED_EDGE('',*,*,#14821,.T.);
#22175=ORIENTED_EDGE('',*,*,#15035,.T.);
#22176=ORIENTED_EDGE('',*,*,#15090,.T.);
#22177=ORIENTED_EDGE('',*,*,#15028,.T.);
#22178=ORIENTED_EDGE('',*,*,#15021,.T.);
#22179=ORIENTED_EDGE('',*,*,#14811,.F.);
#22180=ORIENTED_EDGE('',*,*,#14813,.T.);
#22181=ORIENTED_EDGE('',*,*,#14804,.F.);
#22182=ORIENTED_EDGE('',*,*,#14808,.T.);
#22183=ORIENTED_EDGE('',*,*,#15026,.T.);
#22184=ORIENTED_EDGE('',*,*,#15091,.T.);
#22185=ORIENTED_EDGE('',*,*,#15019,.T.);
#22186=ORIENTED_EDGE('',*,*,#15012,.T.);
#22187=ORIENTED_EDGE('',*,*,#14798,.F.);
#22188=ORIENTED_EDGE('',*,*,#14800,.T.);
#22189=ORIENTED_EDGE('',*,*,#14791,.F.);
#22190=ORIENTED_EDGE('',*,*,#14795,.T.);
#22191=ORIENTED_EDGE('',*,*,#15017,.T.);
#22192=ORIENTED_EDGE('',*,*,#15092,.T.);
#22193=ORIENTED_EDGE('',*,*,#15010,.T.);
#22194=ORIENTED_EDGE('',*,*,#15003,.T.);
#22195=ORIENTED_EDGE('',*,*,#14785,.F.);
#22196=ORIENTED_EDGE('',*,*,#14787,.T.);
#22197=ORIENTED_EDGE('',*,*,#14778,.F.);
#22198=ORIENTED_EDGE('',*,*,#14782,.T.);
#22199=ORIENTED_EDGE('',*,*,#15008,.T.);
#22200=ORIENTED_EDGE('',*,*,#15093,.T.);
#22201=ORIENTED_EDGE('',*,*,#15001,.T.);
#22202=ORIENTED_EDGE('',*,*,#14994,.T.);
#22203=ORIENTED_EDGE('',*,*,#14772,.F.);
#22204=ORIENTED_EDGE('',*,*,#14774,.T.);
#22205=ORIENTED_EDGE('',*,*,#14765,.F.);
#22206=ORIENTED_EDGE('',*,*,#14769,.T.);
#22207=ORIENTED_EDGE('',*,*,#14999,.T.);
#22208=ORIENTED_EDGE('',*,*,#15094,.T.);
#22209=ORIENTED_EDGE('',*,*,#14992,.T.);
#22210=ORIENTED_EDGE('',*,*,#14985,.T.);
#22211=ORIENTED_EDGE('',*,*,#14759,.F.);
#22212=ORIENTED_EDGE('',*,*,#14761,.T.);
#22213=ORIENTED_EDGE('',*,*,#14752,.F.);
#22214=ORIENTED_EDGE('',*,*,#14756,.T.);
#22215=ORIENTED_EDGE('',*,*,#14990,.T.);
#22216=ORIENTED_EDGE('',*,*,#15095,.T.);
#22217=ORIENTED_EDGE('',*,*,#14983,.T.);
#22218=ORIENTED_EDGE('',*,*,#14976,.T.);
#22219=ORIENTED_EDGE('',*,*,#14746,.F.);
#22220=ORIENTED_EDGE('',*,*,#14748,.T.);
#22221=ORIENTED_EDGE('',*,*,#14739,.F.);
#22222=ORIENTED_EDGE('',*,*,#14743,.T.);
#22223=ORIENTED_EDGE('',*,*,#14981,.T.);
#22224=ORIENTED_EDGE('',*,*,#15096,.T.);
#22225=ORIENTED_EDGE('',*,*,#14974,.T.);
#22226=ORIENTED_EDGE('',*,*,#14967,.T.);
#22227=ORIENTED_EDGE('',*,*,#14733,.F.);
#22228=ORIENTED_EDGE('',*,*,#14735,.T.);
#22229=ORIENTED_EDGE('',*,*,#14726,.F.);
#22230=ORIENTED_EDGE('',*,*,#14730,.T.);
#22231=ORIENTED_EDGE('',*,*,#14972,.T.);
#22232=ORIENTED_EDGE('',*,*,#15097,.T.);
#22233=ORIENTED_EDGE('',*,*,#14965,.T.);
#22234=ORIENTED_EDGE('',*,*,#14958,.T.);
#22235=ORIENTED_EDGE('',*,*,#14720,.F.);
#22236=ORIENTED_EDGE('',*,*,#14722,.T.);
#22237=ORIENTED_EDGE('',*,*,#14713,.F.);
#22238=ORIENTED_EDGE('',*,*,#14717,.T.);
#22239=ORIENTED_EDGE('',*,*,#14963,.T.);
#22240=ORIENTED_EDGE('',*,*,#15098,.T.);
#22241=ORIENTED_EDGE('',*,*,#14956,.T.);
#22242=ORIENTED_EDGE('',*,*,#14949,.T.);
#22243=ORIENTED_EDGE('',*,*,#14707,.F.);
#22244=ORIENTED_EDGE('',*,*,#14709,.T.);
#22245=ORIENTED_EDGE('',*,*,#14700,.F.);
#22246=ORIENTED_EDGE('',*,*,#14704,.T.);
#22247=ORIENTED_EDGE('',*,*,#14954,.T.);
#22248=ORIENTED_EDGE('',*,*,#15099,.T.);
#22249=ORIENTED_EDGE('',*,*,#14947,.T.);
#22250=ORIENTED_EDGE('',*,*,#14940,.T.);
#22251=ORIENTED_EDGE('',*,*,#14694,.F.);
#22252=ORIENTED_EDGE('',*,*,#14696,.T.);
#22253=ORIENTED_EDGE('',*,*,#14687,.F.);
#22254=ORIENTED_EDGE('',*,*,#14691,.T.);
#22255=ORIENTED_EDGE('',*,*,#14945,.T.);
#22256=ORIENTED_EDGE('',*,*,#15100,.T.);
#22257=ORIENTED_EDGE('',*,*,#14938,.T.);
#22258=ORIENTED_EDGE('',*,*,#14931,.T.);
#22259=ORIENTED_EDGE('',*,*,#14681,.F.);
#22260=ORIENTED_EDGE('',*,*,#14683,.T.);
#22261=ORIENTED_EDGE('',*,*,#14674,.F.);
#22262=ORIENTED_EDGE('',*,*,#14678,.T.);
#22263=ORIENTED_EDGE('',*,*,#14936,.T.);
#22264=ORIENTED_EDGE('',*,*,#15101,.T.);
#22265=ORIENTED_EDGE('',*,*,#14929,.T.);
#22266=ORIENTED_EDGE('',*,*,#14922,.T.);
#22267=ORIENTED_EDGE('',*,*,#14668,.F.);
#22268=ORIENTED_EDGE('',*,*,#14670,.T.);
#22269=ORIENTED_EDGE('',*,*,#14661,.F.);
#22270=ORIENTED_EDGE('',*,*,#14665,.T.);
#22271=ORIENTED_EDGE('',*,*,#14927,.T.);
#22272=ORIENTED_EDGE('',*,*,#15102,.T.);
#22273=ORIENTED_EDGE('',*,*,#14920,.T.);
#22274=ORIENTED_EDGE('',*,*,#14913,.T.);
#22275=ORIENTED_EDGE('',*,*,#14655,.F.);
#22276=ORIENTED_EDGE('',*,*,#14657,.T.);
#22277=ORIENTED_EDGE('',*,*,#14648,.F.);
#22278=ORIENTED_EDGE('',*,*,#14652,.T.);
#22279=ORIENTED_EDGE('',*,*,#14918,.T.);
#22280=ORIENTED_EDGE('',*,*,#15103,.T.);
#22281=ORIENTED_EDGE('',*,*,#14911,.T.);
#22282=ORIENTED_EDGE('',*,*,#14904,.T.);
#22283=ORIENTED_EDGE('',*,*,#14642,.F.);
#22284=ORIENTED_EDGE('',*,*,#14644,.T.);
#22285=ORIENTED_EDGE('',*,*,#14635,.F.);
#22286=ORIENTED_EDGE('',*,*,#14639,.T.);
#22287=ORIENTED_EDGE('',*,*,#14909,.T.);
#22288=ORIENTED_EDGE('',*,*,#15104,.T.);
#22289=ORIENTED_EDGE('',*,*,#14902,.T.);
#22290=ORIENTED_EDGE('',*,*,#14895,.T.);
#22291=ORIENTED_EDGE('',*,*,#14629,.F.);
#22292=ORIENTED_EDGE('',*,*,#14631,.T.);
#22293=ORIENTED_EDGE('',*,*,#14622,.F.);
#22294=ORIENTED_EDGE('',*,*,#14626,.T.);
#22295=ORIENTED_EDGE('',*,*,#14900,.T.);
#22296=ORIENTED_EDGE('',*,*,#15105,.T.);
#22297=ORIENTED_EDGE('',*,*,#14893,.T.);
#22298=ORIENTED_EDGE('',*,*,#14886,.T.);
#22299=ORIENTED_EDGE('',*,*,#14616,.F.);
#22300=ORIENTED_EDGE('',*,*,#14618,.T.);
#22301=ORIENTED_EDGE('',*,*,#14609,.F.);
#22302=ORIENTED_EDGE('',*,*,#14613,.T.);
#22303=ORIENTED_EDGE('',*,*,#14891,.T.);
#22304=ORIENTED_EDGE('',*,*,#15106,.T.);
#22305=ORIENTED_EDGE('',*,*,#14884,.T.);
#22306=ORIENTED_EDGE('',*,*,#14877,.T.);
#22307=ORIENTED_EDGE('',*,*,#14603,.F.);
#22308=ORIENTED_EDGE('',*,*,#14605,.T.);
#22309=ORIENTED_EDGE('',*,*,#14596,.F.);
#22310=ORIENTED_EDGE('',*,*,#14600,.T.);
#22311=ORIENTED_EDGE('',*,*,#14882,.T.);
#22312=ORIENTED_EDGE('',*,*,#15107,.T.);
#22313=ORIENTED_EDGE('',*,*,#14875,.T.);
#22314=ORIENTED_EDGE('',*,*,#14868,.T.);
#22315=ORIENTED_EDGE('',*,*,#14590,.F.);
#22316=ORIENTED_EDGE('',*,*,#14592,.T.);
#22317=ORIENTED_EDGE('',*,*,#14583,.F.);
#22318=ORIENTED_EDGE('',*,*,#14587,.T.);
#22319=ORIENTED_EDGE('',*,*,#14873,.T.);
#22320=ORIENTED_EDGE('',*,*,#15108,.T.);
#22321=ORIENTED_EDGE('',*,*,#14866,.T.);
#22322=ORIENTED_EDGE('',*,*,#14859,.T.);
#22323=ORIENTED_EDGE('',*,*,#14577,.F.);
#22324=ORIENTED_EDGE('',*,*,#14579,.T.);
#22325=ORIENTED_EDGE('',*,*,#14570,.F.);
#22326=ORIENTED_EDGE('',*,*,#14574,.T.);
#22327=ORIENTED_EDGE('',*,*,#14864,.T.);
#22328=ORIENTED_EDGE('',*,*,#15109,.T.);
#22329=ORIENTED_EDGE('',*,*,#14857,.T.);
#22330=ORIENTED_EDGE('',*,*,#14850,.T.);
#22331=ORIENTED_EDGE('',*,*,#14564,.F.);
#22332=ORIENTED_EDGE('',*,*,#14566,.T.);
#22333=ORIENTED_EDGE('',*,*,#14557,.F.);
#22334=ORIENTED_EDGE('',*,*,#14561,.T.);
#22335=ORIENTED_EDGE('',*,*,#14855,.T.);
#22336=ORIENTED_EDGE('',*,*,#15110,.T.);
#22337=ORIENTED_EDGE('',*,*,#14848,.T.);
#22338=ORIENTED_EDGE('',*,*,#14841,.T.);
#22339=ORIENTED_EDGE('',*,*,#14551,.F.);
#22340=ORIENTED_EDGE('',*,*,#14553,.T.);
#22341=ORIENTED_EDGE('',*,*,#14544,.F.);
#22342=ORIENTED_EDGE('',*,*,#14548,.T.);
#22343=ORIENTED_EDGE('',*,*,#15111,.T.);
#22344=ORIENTED_EDGE('',*,*,#15047,.T.);
#22345=ORIENTED_EDGE('',*,*,#15088,.F.);
#22346=ORIENTED_EDGE('',*,*,#15112,.T.);
#22347=ORIENTED_EDGE('',*,*,#15070,.T.);
#22348=ORIENTED_EDGE('',*,*,#15038,.T.);
#22349=ORIENTED_EDGE('',*,*,#15089,.F.);
#22350=ORIENTED_EDGE('',*,*,#15043,.T.);
#22351=ORIENTED_EDGE('',*,*,#15069,.T.);
#22352=ORIENTED_EDGE('',*,*,#15029,.T.);
#22353=ORIENTED_EDGE('',*,*,#15090,.F.);
#22354=ORIENTED_EDGE('',*,*,#15034,.T.);
#22355=ORIENTED_EDGE('',*,*,#15068,.T.);
#22356=ORIENTED_EDGE('',*,*,#15020,.T.);
#22357=ORIENTED_EDGE('',*,*,#15091,.F.);
#22358=ORIENTED_EDGE('',*,*,#15025,.T.);
#22359=ORIENTED_EDGE('',*,*,#15067,.T.);
#22360=ORIENTED_EDGE('',*,*,#15011,.T.);
#22361=ORIENTED_EDGE('',*,*,#15092,.F.);
#22362=ORIENTED_EDGE('',*,*,#15016,.T.);
#22363=ORIENTED_EDGE('',*,*,#15066,.T.);
#22364=ORIENTED_EDGE('',*,*,#15002,.T.);
#22365=ORIENTED_EDGE('',*,*,#15093,.F.);
#22366=ORIENTED_EDGE('',*,*,#15007,.T.);
#22367=ORIENTED_EDGE('',*,*,#15065,.T.);
#22368=ORIENTED_EDGE('',*,*,#14993,.T.);
#22369=ORIENTED_EDGE('',*,*,#15094,.F.);
#22370=ORIENTED_EDGE('',*,*,#14998,.T.);
#22371=ORIENTED_EDGE('',*,*,#15064,.T.);
#22372=ORIENTED_EDGE('',*,*,#14984,.T.);
#22373=ORIENTED_EDGE('',*,*,#15095,.F.);
#22374=ORIENTED_EDGE('',*,*,#14989,.T.);
#22375=ORIENTED_EDGE('',*,*,#15063,.T.);
#22376=ORIENTED_EDGE('',*,*,#14975,.T.);
#22377=ORIENTED_EDGE('',*,*,#15096,.F.);
#22378=ORIENTED_EDGE('',*,*,#14980,.T.);
#22379=ORIENTED_EDGE('',*,*,#15062,.T.);
#22380=ORIENTED_EDGE('',*,*,#14966,.T.);
#22381=ORIENTED_EDGE('',*,*,#15097,.F.);
#22382=ORIENTED_EDGE('',*,*,#14971,.T.);
#22383=ORIENTED_EDGE('',*,*,#15061,.T.);
#22384=ORIENTED_EDGE('',*,*,#14957,.T.);
#22385=ORIENTED_EDGE('',*,*,#15098,.F.);
#22386=ORIENTED_EDGE('',*,*,#14962,.T.);
#22387=ORIENTED_EDGE('',*,*,#15060,.T.);
#22388=ORIENTED_EDGE('',*,*,#14948,.T.);
#22389=ORIENTED_EDGE('',*,*,#15099,.F.);
#22390=ORIENTED_EDGE('',*,*,#14953,.T.);
#22391=ORIENTED_EDGE('',*,*,#15059,.T.);
#22392=ORIENTED_EDGE('',*,*,#14939,.T.);
#22393=ORIENTED_EDGE('',*,*,#15100,.F.);
#22394=ORIENTED_EDGE('',*,*,#14944,.T.);
#22395=ORIENTED_EDGE('',*,*,#15058,.T.);
#22396=ORIENTED_EDGE('',*,*,#14930,.T.);
#22397=ORIENTED_EDGE('',*,*,#15101,.F.);
#22398=ORIENTED_EDGE('',*,*,#14935,.T.);
#22399=ORIENTED_EDGE('',*,*,#15057,.T.);
#22400=ORIENTED_EDGE('',*,*,#14921,.T.);
#22401=ORIENTED_EDGE('',*,*,#15102,.F.);
#22402=ORIENTED_EDGE('',*,*,#14926,.T.);
#22403=ORIENTED_EDGE('',*,*,#15056,.T.);
#22404=ORIENTED_EDGE('',*,*,#14912,.T.);
#22405=ORIENTED_EDGE('',*,*,#15103,.F.);
#22406=ORIENTED_EDGE('',*,*,#14917,.T.);
#22407=ORIENTED_EDGE('',*,*,#15055,.T.);
#22408=ORIENTED_EDGE('',*,*,#14903,.T.);
#22409=ORIENTED_EDGE('',*,*,#15104,.F.);
#22410=ORIENTED_EDGE('',*,*,#14908,.T.);
#22411=ORIENTED_EDGE('',*,*,#15054,.T.);
#22412=ORIENTED_EDGE('',*,*,#14894,.T.);
#22413=ORIENTED_EDGE('',*,*,#15105,.F.);
#22414=ORIENTED_EDGE('',*,*,#14899,.T.);
#22415=ORIENTED_EDGE('',*,*,#15053,.T.);
#22416=ORIENTED_EDGE('',*,*,#14885,.T.);
#22417=ORIENTED_EDGE('',*,*,#15106,.F.);
#22418=ORIENTED_EDGE('',*,*,#14890,.T.);
#22419=ORIENTED_EDGE('',*,*,#15052,.T.);
#22420=ORIENTED_EDGE('',*,*,#14876,.T.);
#22421=ORIENTED_EDGE('',*,*,#15107,.F.);
#22422=ORIENTED_EDGE('',*,*,#14881,.T.);
#22423=ORIENTED_EDGE('',*,*,#15051,.T.);
#22424=ORIENTED_EDGE('',*,*,#14867,.T.);
#22425=ORIENTED_EDGE('',*,*,#15108,.F.);
#22426=ORIENTED_EDGE('',*,*,#14872,.T.);
#22427=ORIENTED_EDGE('',*,*,#15050,.T.);
#22428=ORIENTED_EDGE('',*,*,#14858,.T.);
#22429=ORIENTED_EDGE('',*,*,#15109,.F.);
#22430=ORIENTED_EDGE('',*,*,#14863,.T.);
#22431=ORIENTED_EDGE('',*,*,#15049,.T.);
#22432=ORIENTED_EDGE('',*,*,#14849,.T.);
#22433=ORIENTED_EDGE('',*,*,#15110,.F.);
#22434=ORIENTED_EDGE('',*,*,#14854,.T.);
#22435=ORIENTED_EDGE('',*,*,#15048,.T.);
#22436=ORIENTED_EDGE('',*,*,#15073,.T.);
#22437=ORIENTED_EDGE('',*,*,#15113,.T.);
#22438=ORIENTED_EDGE('',*,*,#15085,.T.);
#22439=ORIENTED_EDGE('',*,*,#15114,.T.);
#22440=ORIENTED_EDGE('',*,*,#15113,.F.);
#22441=ORIENTED_EDGE('',*,*,#15072,.F.);
#22442=ORIENTED_EDGE('',*,*,#15115,.T.);
#22443=ORIENTED_EDGE('',*,*,#15086,.F.);
#22444=ORIENTED_EDGE('',*,*,#15075,.T.);
#22445=ORIENTED_EDGE('',*,*,#15116,.T.);
#22446=ORIENTED_EDGE('',*,*,#15083,.T.);
#22447=ORIENTED_EDGE('',*,*,#15117,.T.);
#22448=ORIENTED_EDGE('',*,*,#15114,.F.);
#22449=ORIENTED_EDGE('',*,*,#15084,.F.);
#22450=ORIENTED_EDGE('',*,*,#15116,.F.);
#22451=ORIENTED_EDGE('',*,*,#15074,.F.);
#22452=ORIENTED_EDGE('',*,*,#15117,.F.);
#22453=ORIENTED_EDGE('',*,*,#15082,.F.);
#22454=ORIENTED_EDGE('',*,*,#15118,.F.);
#22455=ORIENTED_EDGE('',*,*,#15076,.F.);
#22456=ORIENTED_EDGE('',*,*,#15071,.F.);
#22457=ORIENTED_EDGE('',*,*,#15112,.F.);
#22458=ORIENTED_EDGE('',*,*,#15087,.F.);
#22459=ORIENTED_EDGE('',*,*,#15115,.F.);
#22460=ORIENTED_EDGE('',*,*,#15077,.F.);
#22461=ORIENTED_EDGE('',*,*,#15118,.T.);
#22462=ORIENTED_EDGE('',*,*,#15081,.F.);
#22463=ORIENTED_EDGE('',*,*,#15119,.F.);
#22464=ORIENTED_EDGE('',*,*,#15111,.F.);
#22465=ORIENTED_EDGE('',*,*,#15120,.T.);
#22466=ORIENTED_EDGE('',*,*,#15079,.T.);
#22467=ORIENTED_EDGE('',*,*,#15120,.F.);
#22468=ORIENTED_EDGE('',*,*,#14845,.T.);
#22469=ORIENTED_EDGE('',*,*,#15078,.T.);
#22470=ORIENTED_EDGE('',*,*,#15119,.T.);
#22471=ORIENTED_EDGE('',*,*,#15080,.F.);
#22472=ORIENTED_EDGE('',*,*,#15121,.F.);
#22473=ORIENTED_EDGE('',*,*,#15122,.T.);
#22474=ORIENTED_EDGE('',*,*,#15123,.T.);
#22475=ORIENTED_EDGE('',*,*,#15122,.F.);
#22476=ORIENTED_EDGE('',*,*,#15124,.F.);
#22477=ORIENTED_EDGE('',*,*,#15125,.T.);
#22478=ORIENTED_EDGE('',*,*,#15126,.T.);
#22479=ORIENTED_EDGE('',*,*,#15125,.F.);
#22480=ORIENTED_EDGE('',*,*,#15124,.T.);
#22481=ORIENTED_EDGE('',*,*,#15121,.T.);
#22482=ORIENTED_EDGE('',*,*,#15126,.F.);
#22483=ORIENTED_EDGE('',*,*,#15123,.F.);
#22484=ORIENTED_EDGE('',*,*,#15127,.F.);
#22485=ORIENTED_EDGE('',*,*,#15128,.T.);
#22486=ORIENTED_EDGE('',*,*,#15129,.F.);
#22487=ORIENTED_EDGE('',*,*,#15130,.T.);
#22488=ORIENTED_EDGE('',*,*,#15131,.F.);
#22489=ORIENTED_EDGE('',*,*,#15130,.F.);
#22490=ORIENTED_EDGE('',*,*,#15132,.F.);
#22491=ORIENTED_EDGE('',*,*,#15133,.F.);
#22492=ORIENTED_EDGE('',*,*,#15134,.F.);
#22493=ORIENTED_EDGE('',*,*,#15133,.T.);
#22494=ORIENTED_EDGE('',*,*,#15135,.T.);
#22495=ORIENTED_EDGE('',*,*,#15136,.T.);
#22496=ORIENTED_EDGE('',*,*,#15132,.T.);
#22497=ORIENTED_EDGE('',*,*,#15129,.T.);
#22498=ORIENTED_EDGE('',*,*,#15137,.T.);
#22499=ORIENTED_EDGE('',*,*,#15135,.F.);
#22500=ORIENTED_EDGE('',*,*,#15138,.F.);
#22501=ORIENTED_EDGE('',*,*,#15136,.F.);
#22502=ORIENTED_EDGE('',*,*,#15137,.F.);
#22503=ORIENTED_EDGE('',*,*,#15128,.F.);
#22504=ORIENTED_EDGE('',*,*,#15139,.T.);
#22505=ORIENTED_EDGE('',*,*,#15140,.T.);
#22506=ORIENTED_EDGE('',*,*,#15141,.F.);
#22507=ORIENTED_EDGE('',*,*,#15140,.F.);
#22508=ORIENTED_EDGE('',*,*,#15142,.F.);
#22509=ORIENTED_EDGE('',*,*,#15139,.F.);
#22510=ORIENTED_EDGE('',*,*,#15143,.F.);
#22511=ORIENTED_EDGE('',*,*,#15141,.T.);
#22512=ORIENTED_EDGE('',*,*,#15144,.F.);
#22513=ORIENTED_EDGE('',*,*,#15145,.T.);
#22514=ORIENTED_EDGE('',*,*,#15143,.T.);
#22515=ORIENTED_EDGE('',*,*,#15145,.F.);
#22516=ORIENTED_EDGE('',*,*,#15146,.T.);
#22517=ORIENTED_EDGE('',*,*,#15147,.T.);
#22518=ORIENTED_EDGE('',*,*,#15148,.F.);
#22519=ORIENTED_EDGE('',*,*,#15147,.F.);
#22520=ORIENTED_EDGE('',*,*,#15149,.F.);
#22521=ORIENTED_EDGE('',*,*,#15146,.F.);
#22522=ORIENTED_EDGE('',*,*,#15150,.F.);
#22523=ORIENTED_EDGE('',*,*,#15148,.T.);
#22524=ORIENTED_EDGE('',*,*,#15151,.F.);
#22525=ORIENTED_EDGE('',*,*,#15152,.T.);
#22526=ORIENTED_EDGE('',*,*,#15150,.T.);
#22527=ORIENTED_EDGE('',*,*,#15152,.F.);
#22528=ORIENTED_EDGE('',*,*,#15153,.F.);
#22529=ORIENTED_EDGE('',*,*,#15154,.T.);
#22530=ORIENTED_EDGE('',*,*,#15155,.F.);
#22531=ORIENTED_EDGE('',*,*,#15154,.F.);
#22532=ORIENTED_EDGE('',*,*,#15156,.F.);
#22533=ORIENTED_EDGE('',*,*,#15157,.T.);
#22534=ORIENTED_EDGE('',*,*,#15158,.F.);
#22535=ORIENTED_EDGE('',*,*,#15157,.F.);
#22536=ORIENTED_EDGE('',*,*,#15159,.F.);
#22537=ORIENTED_EDGE('',*,*,#15160,.T.);
#22538=ORIENTED_EDGE('',*,*,#15161,.F.);
#22539=ORIENTED_EDGE('',*,*,#15160,.F.);
#22540=ORIENTED_EDGE('',*,*,#15162,.T.);
#22541=ORIENTED_EDGE('',*,*,#15163,.F.);
#22542=ORIENTED_EDGE('',*,*,#15164,.F.);
#22543=ORIENTED_EDGE('',*,*,#15165,.F.);
#22544=ORIENTED_EDGE('',*,*,#15162,.F.);
#22545=ORIENTED_EDGE('',*,*,#15166,.T.);
#22546=ORIENTED_EDGE('',*,*,#15164,.T.);
#22547=ORIENTED_EDGE('',*,*,#15166,.F.);
#22548=ORIENTED_EDGE('',*,*,#15165,.T.);
#22549=ORIENTED_EDGE('',*,*,#15167,.T.);
#22550=ORIENTED_EDGE('',*,*,#15168,.F.);
#22551=ORIENTED_EDGE('',*,*,#15167,.F.);
#22552=ORIENTED_EDGE('',*,*,#15142,.T.);
#22553=ORIENTED_EDGE('',*,*,#15169,.T.);
#22554=ORIENTED_EDGE('',*,*,#15163,.T.);
#22555=ORIENTED_EDGE('',*,*,#15169,.F.);
#22556=ORIENTED_EDGE('',*,*,#15134,.T.);
#22557=ORIENTED_EDGE('',*,*,#15138,.T.);
#22558=ORIENTED_EDGE('',*,*,#15127,.T.);
#22559=ORIENTED_EDGE('',*,*,#15131,.T.);
#22560=ORIENTED_EDGE('',*,*,#15144,.T.);
#22561=ORIENTED_EDGE('',*,*,#15170,.T.);
#22562=ORIENTED_EDGE('',*,*,#15171,.F.);
#22563=ORIENTED_EDGE('',*,*,#15172,.F.);
#22564=ORIENTED_EDGE('',*,*,#15173,.F.);
#22565=ORIENTED_EDGE('',*,*,#15170,.F.);
#22566=ORIENTED_EDGE('',*,*,#15174,.T.);
#22567=ORIENTED_EDGE('',*,*,#15172,.T.);
#22568=ORIENTED_EDGE('',*,*,#15174,.F.);
#22569=ORIENTED_EDGE('',*,*,#15173,.T.);
#22570=ORIENTED_EDGE('',*,*,#15175,.T.);
#22571=ORIENTED_EDGE('',*,*,#15176,.F.);
#22572=ORIENTED_EDGE('',*,*,#15175,.F.);
#22573=ORIENTED_EDGE('',*,*,#15177,.T.);
#22574=ORIENTED_EDGE('',*,*,#15149,.T.);
#22575=ORIENTED_EDGE('',*,*,#15178,.T.);
#22576=ORIENTED_EDGE('',*,*,#15171,.T.);
#22577=ORIENTED_EDGE('',*,*,#15178,.F.);
#22578=ORIENTED_EDGE('',*,*,#15151,.T.);
#22579=ORIENTED_EDGE('',*,*,#15168,.T.);
#22580=ORIENTED_EDGE('',*,*,#15177,.F.);
#22581=ORIENTED_EDGE('',*,*,#15179,.T.);
#22582=ORIENTED_EDGE('',*,*,#15180,.T.);
#22583=ORIENTED_EDGE('',*,*,#15179,.F.);
#22584=ORIENTED_EDGE('',*,*,#15181,.F.);
#22585=ORIENTED_EDGE('',*,*,#15182,.T.);
#22586=ORIENTED_EDGE('',*,*,#15183,.T.);
#22587=ORIENTED_EDGE('',*,*,#15182,.F.);
#22588=ORIENTED_EDGE('',*,*,#15181,.T.);
#22589=ORIENTED_EDGE('',*,*,#15153,.T.);
#22590=ORIENTED_EDGE('',*,*,#15156,.T.);
#22591=ORIENTED_EDGE('',*,*,#15159,.T.);
#22592=ORIENTED_EDGE('',*,*,#15176,.T.);
#22593=ORIENTED_EDGE('',*,*,#15183,.F.);
#22594=ORIENTED_EDGE('',*,*,#15155,.T.);
#22595=ORIENTED_EDGE('',*,*,#15158,.T.);
#22596=ORIENTED_EDGE('',*,*,#15161,.T.);
#22597=ORIENTED_EDGE('',*,*,#15180,.F.);
#22598=ORIENTED_EDGE('',*,*,#15184,.T.);
#22599=ORIENTED_EDGE('',*,*,#15185,.T.);
#22600=ORIENTED_EDGE('',*,*,#15186,.F.);
#22601=ORIENTED_EDGE('',*,*,#15187,.F.);
#22602=ORIENTED_EDGE('',*,*,#15188,.T.);
#22603=ORIENTED_EDGE('',*,*,#15187,.T.);
#22604=ORIENTED_EDGE('',*,*,#15189,.F.);
#22605=ORIENTED_EDGE('',*,*,#15190,.F.);
#22606=ORIENTED_EDGE('',*,*,#15191,.T.);
#22607=ORIENTED_EDGE('',*,*,#15190,.T.);
#22608=ORIENTED_EDGE('',*,*,#15192,.F.);
#22609=ORIENTED_EDGE('',*,*,#15193,.F.);
#22610=ORIENTED_EDGE('',*,*,#15194,.T.);
#22611=ORIENTED_EDGE('',*,*,#15193,.T.);
#22612=ORIENTED_EDGE('',*,*,#15195,.F.);
#22613=ORIENTED_EDGE('',*,*,#15185,.F.);
#22614=ORIENTED_EDGE('',*,*,#15195,.T.);
#22615=ORIENTED_EDGE('',*,*,#15192,.T.);
#22616=ORIENTED_EDGE('',*,*,#15189,.T.);
#22617=ORIENTED_EDGE('',*,*,#15186,.T.);
#22618=ORIENTED_EDGE('',*,*,#15194,.F.);
#22619=ORIENTED_EDGE('',*,*,#15184,.F.);
#22620=ORIENTED_EDGE('',*,*,#15188,.F.);
#22621=ORIENTED_EDGE('',*,*,#15191,.F.);
#22622=ORIENTED_EDGE('',*,*,#15196,.F.);
#22623=ORIENTED_EDGE('',*,*,#15197,.T.);
#22624=ORIENTED_EDGE('',*,*,#15198,.T.);
#22625=ORIENTED_EDGE('',*,*,#15197,.F.);
#22626=ORIENTED_EDGE('',*,*,#15199,.F.);
#22627=ORIENTED_EDGE('',*,*,#15200,.T.);
#22628=ORIENTED_EDGE('',*,*,#15201,.T.);
#22629=ORIENTED_EDGE('',*,*,#15200,.F.);
#22630=ORIENTED_EDGE('',*,*,#15199,.T.);
#22631=ORIENTED_EDGE('',*,*,#15196,.T.);
#22632=ORIENTED_EDGE('',*,*,#15201,.F.);
#22633=ORIENTED_EDGE('',*,*,#15198,.F.);
#22634=ORIENTED_EDGE('',*,*,#15202,.T.);
#22635=ORIENTED_EDGE('',*,*,#15203,.T.);
#22636=ORIENTED_EDGE('',*,*,#15204,.F.);
#22637=ORIENTED_EDGE('',*,*,#15203,.F.);
#22638=ORIENTED_EDGE('',*,*,#15205,.F.);
#22639=ORIENTED_EDGE('',*,*,#15202,.F.);
#22640=ORIENTED_EDGE('',*,*,#15206,.F.);
#22641=ORIENTED_EDGE('',*,*,#15204,.T.);
#22642=ORIENTED_EDGE('',*,*,#15207,.F.);
#22643=ORIENTED_EDGE('',*,*,#15208,.T.);
#22644=ORIENTED_EDGE('',*,*,#15206,.T.);
#22645=ORIENTED_EDGE('',*,*,#15208,.F.);
#22646=ORIENTED_EDGE('',*,*,#15209,.T.);
#22647=ORIENTED_EDGE('',*,*,#15210,.F.);
#22648=ORIENTED_EDGE('',*,*,#15209,.F.);
#22649=ORIENTED_EDGE('',*,*,#15211,.T.);
#22650=ORIENTED_EDGE('',*,*,#15212,.T.);
#22651=ORIENTED_EDGE('',*,*,#15211,.F.);
#22652=ORIENTED_EDGE('',*,*,#15212,.F.);
#22653=ORIENTED_EDGE('',*,*,#15205,.T.);
#22654=ORIENTED_EDGE('',*,*,#15213,.T.);
#22655=ORIENTED_EDGE('',*,*,#15210,.T.);
#22656=ORIENTED_EDGE('',*,*,#15213,.F.);
#22657=ORIENTED_EDGE('',*,*,#15207,.T.);
#22658=ORIENTED_EDGE('',*,*,#15214,.F.);
#22659=ORIENTED_EDGE('',*,*,#15215,.F.);
#22660=ORIENTED_EDGE('',*,*,#15216,.F.);
#22661=ORIENTED_EDGE('',*,*,#15217,.F.);
#22662=ORIENTED_EDGE('',*,*,#15218,.F.);
#22663=ORIENTED_EDGE('',*,*,#15219,.F.);
#22664=ORIENTED_EDGE('',*,*,#15220,.F.);
#22665=ORIENTED_EDGE('',*,*,#15221,.F.);
#22666=ORIENTED_EDGE('',*,*,#15221,.T.);
#22667=ORIENTED_EDGE('',*,*,#15222,.F.);
#22668=ORIENTED_EDGE('',*,*,#15215,.T.);
#22669=ORIENTED_EDGE('',*,*,#15223,.F.);
#22670=ORIENTED_EDGE('',*,*,#15218,.T.);
#22671=ORIENTED_EDGE('',*,*,#15223,.T.);
#22672=ORIENTED_EDGE('',*,*,#15214,.T.);
#22673=ORIENTED_EDGE('',*,*,#15224,.F.);
#22674=ORIENTED_EDGE('',*,*,#15220,.T.);
#22675=ORIENTED_EDGE('',*,*,#15225,.F.);
#22676=ORIENTED_EDGE('',*,*,#15216,.T.);
#22677=ORIENTED_EDGE('',*,*,#15222,.T.);
#22678=ORIENTED_EDGE('',*,*,#15219,.T.);
#22679=ORIENTED_EDGE('',*,*,#15224,.T.);
#22680=ORIENTED_EDGE('',*,*,#15217,.T.);
#22681=ORIENTED_EDGE('',*,*,#15225,.T.);
#22682=ORIENTED_EDGE('',*,*,#15226,.F.);
#22683=ORIENTED_EDGE('',*,*,#15227,.T.);
#22684=ORIENTED_EDGE('',*,*,#15228,.T.);
#22685=ORIENTED_EDGE('',*,*,#15227,.F.);
#22686=ORIENTED_EDGE('',*,*,#15229,.F.);
#22687=ORIENTED_EDGE('',*,*,#15230,.T.);
#22688=ORIENTED_EDGE('',*,*,#15231,.T.);
#22689=ORIENTED_EDGE('',*,*,#15230,.F.);
#22690=ORIENTED_EDGE('',*,*,#15229,.T.);
#22691=ORIENTED_EDGE('',*,*,#15226,.T.);
#22692=ORIENTED_EDGE('',*,*,#15231,.F.);
#22693=ORIENTED_EDGE('',*,*,#15228,.F.);
#22694=ORIENTED_EDGE('',*,*,#15232,.F.);
#22695=ORIENTED_EDGE('',*,*,#15233,.T.);
#22696=ORIENTED_EDGE('',*,*,#15234,.T.);
#22697=ORIENTED_EDGE('',*,*,#15233,.F.);
#22698=ORIENTED_EDGE('',*,*,#15235,.F.);
#22699=ORIENTED_EDGE('',*,*,#15236,.T.);
#22700=ORIENTED_EDGE('',*,*,#15237,.T.);
#22701=ORIENTED_EDGE('',*,*,#15236,.F.);
#22702=ORIENTED_EDGE('',*,*,#15235,.T.);
#22703=ORIENTED_EDGE('',*,*,#15232,.T.);
#22704=ORIENTED_EDGE('',*,*,#15237,.F.);
#22705=ORIENTED_EDGE('',*,*,#15234,.F.);
#22706=ORIENTED_EDGE('',*,*,#15238,.F.);
#22707=ORIENTED_EDGE('',*,*,#15239,.T.);
#22708=ORIENTED_EDGE('',*,*,#15240,.T.);
#22709=ORIENTED_EDGE('',*,*,#15239,.F.);
#22710=ORIENTED_EDGE('',*,*,#15241,.F.);
#22711=ORIENTED_EDGE('',*,*,#15242,.T.);
#22712=ORIENTED_EDGE('',*,*,#15243,.T.);
#22713=ORIENTED_EDGE('',*,*,#15242,.F.);
#22714=ORIENTED_EDGE('',*,*,#15241,.T.);
#22715=ORIENTED_EDGE('',*,*,#15238,.T.);
#22716=ORIENTED_EDGE('',*,*,#15243,.F.);
#22717=ORIENTED_EDGE('',*,*,#15240,.F.);
#22718=ORIENTED_EDGE('',*,*,#15244,.F.);
#22719=ORIENTED_EDGE('',*,*,#15245,.F.);
#22720=ORIENTED_EDGE('',*,*,#15246,.F.);
#22721=ORIENTED_EDGE('',*,*,#15247,.F.);
#22722=ORIENTED_EDGE('',*,*,#15248,.F.);
#22723=ORIENTED_EDGE('',*,*,#15249,.F.);
#22724=ORIENTED_EDGE('',*,*,#15250,.F.);
#22725=ORIENTED_EDGE('',*,*,#15251,.F.);
#22726=ORIENTED_EDGE('',*,*,#15251,.T.);
#22727=ORIENTED_EDGE('',*,*,#15252,.F.);
#22728=ORIENTED_EDGE('',*,*,#15245,.T.);
#22729=ORIENTED_EDGE('',*,*,#15253,.F.);
#22730=ORIENTED_EDGE('',*,*,#15248,.T.);
#22731=ORIENTED_EDGE('',*,*,#15253,.T.);
#22732=ORIENTED_EDGE('',*,*,#15244,.T.);
#22733=ORIENTED_EDGE('',*,*,#15254,.F.);
#22734=ORIENTED_EDGE('',*,*,#15250,.T.);
#22735=ORIENTED_EDGE('',*,*,#15255,.F.);
#22736=ORIENTED_EDGE('',*,*,#15246,.T.);
#22737=ORIENTED_EDGE('',*,*,#15252,.T.);
#22738=ORIENTED_EDGE('',*,*,#15249,.T.);
#22739=ORIENTED_EDGE('',*,*,#15254,.T.);
#22740=ORIENTED_EDGE('',*,*,#15247,.T.);
#22741=ORIENTED_EDGE('',*,*,#15255,.T.);
#22742=ORIENTED_EDGE('',*,*,#15256,.F.);
#22743=ORIENTED_EDGE('',*,*,#15257,.F.);
#22744=ORIENTED_EDGE('',*,*,#15258,.F.);
#22745=ORIENTED_EDGE('',*,*,#15259,.F.);
#22746=ORIENTED_EDGE('',*,*,#15260,.F.);
#22747=ORIENTED_EDGE('',*,*,#15261,.F.);
#22748=ORIENTED_EDGE('',*,*,#15262,.F.);
#22749=ORIENTED_EDGE('',*,*,#15263,.F.);
#22750=ORIENTED_EDGE('',*,*,#15263,.T.);
#22751=ORIENTED_EDGE('',*,*,#15264,.F.);
#22752=ORIENTED_EDGE('',*,*,#15257,.T.);
#22753=ORIENTED_EDGE('',*,*,#15265,.F.);
#22754=ORIENTED_EDGE('',*,*,#15260,.T.);
#22755=ORIENTED_EDGE('',*,*,#15265,.T.);
#22756=ORIENTED_EDGE('',*,*,#15256,.T.);
#22757=ORIENTED_EDGE('',*,*,#15266,.F.);
#22758=ORIENTED_EDGE('',*,*,#15262,.T.);
#22759=ORIENTED_EDGE('',*,*,#15267,.F.);
#22760=ORIENTED_EDGE('',*,*,#15258,.T.);
#22761=ORIENTED_EDGE('',*,*,#15264,.T.);
#22762=ORIENTED_EDGE('',*,*,#15261,.T.);
#22763=ORIENTED_EDGE('',*,*,#15266,.T.);
#22764=ORIENTED_EDGE('',*,*,#15259,.T.);
#22765=ORIENTED_EDGE('',*,*,#15267,.T.);
#22766=ORIENTED_EDGE('',*,*,#15268,.F.);
#22767=ORIENTED_EDGE('',*,*,#15269,.T.);
#22768=ORIENTED_EDGE('',*,*,#15270,.T.);
#22769=ORIENTED_EDGE('',*,*,#15269,.F.);
#22770=ORIENTED_EDGE('',*,*,#15268,.T.);
#22771=ORIENTED_EDGE('',*,*,#15270,.F.);
#22772=ORIENTED_EDGE('',*,*,#15271,.F.);
#22773=ORIENTED_EDGE('',*,*,#15272,.T.);
#22774=ORIENTED_EDGE('',*,*,#15273,.T.);
#22775=ORIENTED_EDGE('',*,*,#15274,.T.);
#22776=ORIENTED_EDGE('',*,*,#15275,.F.);
#22777=ORIENTED_EDGE('',*,*,#15276,.T.);
#22778=ORIENTED_EDGE('',*,*,#15271,.T.);
#22779=ORIENTED_EDGE('',*,*,#15277,.T.);
#22780=ORIENTED_EDGE('',*,*,#15278,.F.);
#22781=ORIENTED_EDGE('',*,*,#15279,.T.);
#22782=ORIENTED_EDGE('',*,*,#15275,.T.);
#22783=ORIENTED_EDGE('',*,*,#15280,.T.);
#22784=ORIENTED_EDGE('',*,*,#15281,.F.);
#22785=ORIENTED_EDGE('',*,*,#15282,.T.);
#22786=ORIENTED_EDGE('',*,*,#15278,.T.);
#22787=ORIENTED_EDGE('',*,*,#15283,.T.);
#22788=ORIENTED_EDGE('',*,*,#15284,.F.);
#22789=ORIENTED_EDGE('',*,*,#15285,.T.);
#22790=ORIENTED_EDGE('',*,*,#15281,.T.);
#22791=ORIENTED_EDGE('',*,*,#15286,.T.);
#22792=ORIENTED_EDGE('',*,*,#15287,.F.);
#22793=ORIENTED_EDGE('',*,*,#15288,.T.);
#22794=ORIENTED_EDGE('',*,*,#15284,.T.);
#22795=ORIENTED_EDGE('',*,*,#15289,.T.);
#22796=ORIENTED_EDGE('',*,*,#15290,.F.);
#22797=ORIENTED_EDGE('',*,*,#15291,.T.);
#22798=ORIENTED_EDGE('',*,*,#15287,.T.);
#22799=ORIENTED_EDGE('',*,*,#15292,.T.);
#22800=ORIENTED_EDGE('',*,*,#15293,.F.);
#22801=ORIENTED_EDGE('',*,*,#15294,.T.);
#22802=ORIENTED_EDGE('',*,*,#15290,.T.);
#22803=ORIENTED_EDGE('',*,*,#15295,.T.);
#22804=ORIENTED_EDGE('',*,*,#15296,.F.);
#22805=ORIENTED_EDGE('',*,*,#15297,.T.);
#22806=ORIENTED_EDGE('',*,*,#15293,.T.);
#22807=ORIENTED_EDGE('',*,*,#15298,.T.);
#22808=ORIENTED_EDGE('',*,*,#15299,.F.);
#22809=ORIENTED_EDGE('',*,*,#15300,.T.);
#22810=ORIENTED_EDGE('',*,*,#15296,.T.);
#22811=ORIENTED_EDGE('',*,*,#15301,.T.);
#22812=ORIENTED_EDGE('',*,*,#15302,.F.);
#22813=ORIENTED_EDGE('',*,*,#15303,.T.);
#22814=ORIENTED_EDGE('',*,*,#15299,.T.);
#22815=ORIENTED_EDGE('',*,*,#15304,.T.);
#22816=ORIENTED_EDGE('',*,*,#15305,.F.);
#22817=ORIENTED_EDGE('',*,*,#15306,.T.);
#22818=ORIENTED_EDGE('',*,*,#15302,.T.);
#22819=ORIENTED_EDGE('',*,*,#15307,.T.);
#22820=ORIENTED_EDGE('',*,*,#15308,.F.);
#22821=ORIENTED_EDGE('',*,*,#15309,.T.);
#22822=ORIENTED_EDGE('',*,*,#15305,.T.);
#22823=ORIENTED_EDGE('',*,*,#15310,.T.);
#22824=ORIENTED_EDGE('',*,*,#15311,.F.);
#22825=ORIENTED_EDGE('',*,*,#15312,.T.);
#22826=ORIENTED_EDGE('',*,*,#15308,.T.);
#22827=ORIENTED_EDGE('',*,*,#15313,.T.);
#22828=ORIENTED_EDGE('',*,*,#15314,.F.);
#22829=ORIENTED_EDGE('',*,*,#15315,.T.);
#22830=ORIENTED_EDGE('',*,*,#15311,.T.);
#22831=ORIENTED_EDGE('',*,*,#15316,.T.);
#22832=ORIENTED_EDGE('',*,*,#15317,.F.);
#22833=ORIENTED_EDGE('',*,*,#15318,.T.);
#22834=ORIENTED_EDGE('',*,*,#15314,.T.);
#22835=ORIENTED_EDGE('',*,*,#15319,.T.);
#22836=ORIENTED_EDGE('',*,*,#15320,.F.);
#22837=ORIENTED_EDGE('',*,*,#15321,.T.);
#22838=ORIENTED_EDGE('',*,*,#15317,.T.);
#22839=ORIENTED_EDGE('',*,*,#15322,.T.);
#22840=ORIENTED_EDGE('',*,*,#15323,.F.);
#22841=ORIENTED_EDGE('',*,*,#15324,.T.);
#22842=ORIENTED_EDGE('',*,*,#15320,.T.);
#22843=ORIENTED_EDGE('',*,*,#15325,.T.);
#22844=ORIENTED_EDGE('',*,*,#15326,.F.);
#22845=ORIENTED_EDGE('',*,*,#15327,.T.);
#22846=ORIENTED_EDGE('',*,*,#15323,.T.);
#22847=ORIENTED_EDGE('',*,*,#15328,.T.);
#22848=ORIENTED_EDGE('',*,*,#15329,.F.);
#22849=ORIENTED_EDGE('',*,*,#15330,.T.);
#22850=ORIENTED_EDGE('',*,*,#15326,.T.);
#22851=ORIENTED_EDGE('',*,*,#15331,.T.);
#22852=ORIENTED_EDGE('',*,*,#15332,.F.);
#22853=ORIENTED_EDGE('',*,*,#15333,.T.);
#22854=ORIENTED_EDGE('',*,*,#15334,.F.);
#22855=ORIENTED_EDGE('',*,*,#15335,.F.);
#22856=ORIENTED_EDGE('',*,*,#15336,.F.);
#22857=ORIENTED_EDGE('',*,*,#15337,.T.);
#22858=ORIENTED_EDGE('',*,*,#15332,.T.);
#22859=ORIENTED_EDGE('',*,*,#15338,.F.);
#22860=ORIENTED_EDGE('',*,*,#15339,.F.);
#22861=ORIENTED_EDGE('',*,*,#15340,.T.);
#22862=ORIENTED_EDGE('',*,*,#15336,.T.);
#22863=ORIENTED_EDGE('',*,*,#15341,.F.);
#22864=ORIENTED_EDGE('',*,*,#15342,.F.);
#22865=ORIENTED_EDGE('',*,*,#15343,.T.);
#22866=ORIENTED_EDGE('',*,*,#15339,.T.);
#22867=ORIENTED_EDGE('',*,*,#15344,.F.);
#22868=ORIENTED_EDGE('',*,*,#15345,.F.);
#22869=ORIENTED_EDGE('',*,*,#15346,.T.);
#22870=ORIENTED_EDGE('',*,*,#15342,.T.);
#22871=ORIENTED_EDGE('',*,*,#15347,.F.);
#22872=ORIENTED_EDGE('',*,*,#15348,.F.);
#22873=ORIENTED_EDGE('',*,*,#15349,.T.);
#22874=ORIENTED_EDGE('',*,*,#15345,.T.);
#22875=ORIENTED_EDGE('',*,*,#15350,.F.);
#22876=ORIENTED_EDGE('',*,*,#15351,.F.);
#22877=ORIENTED_EDGE('',*,*,#15352,.T.);
#22878=ORIENTED_EDGE('',*,*,#15348,.T.);
#22879=ORIENTED_EDGE('',*,*,#15353,.F.);
#22880=ORIENTED_EDGE('',*,*,#15354,.F.);
#22881=ORIENTED_EDGE('',*,*,#15355,.T.);
#22882=ORIENTED_EDGE('',*,*,#15351,.T.);
#22883=ORIENTED_EDGE('',*,*,#15356,.F.);
#22884=ORIENTED_EDGE('',*,*,#15357,.F.);
#22885=ORIENTED_EDGE('',*,*,#15358,.T.);
#22886=ORIENTED_EDGE('',*,*,#15354,.T.);
#22887=ORIENTED_EDGE('',*,*,#15359,.F.);
#22888=ORIENTED_EDGE('',*,*,#15360,.F.);
#22889=ORIENTED_EDGE('',*,*,#15361,.T.);
#22890=ORIENTED_EDGE('',*,*,#15357,.T.);
#22891=ORIENTED_EDGE('',*,*,#15362,.F.);
#22892=ORIENTED_EDGE('',*,*,#15363,.F.);
#22893=ORIENTED_EDGE('',*,*,#15364,.T.);
#22894=ORIENTED_EDGE('',*,*,#15360,.T.);
#22895=ORIENTED_EDGE('',*,*,#15365,.F.);
#22896=ORIENTED_EDGE('',*,*,#15366,.F.);
#22897=ORIENTED_EDGE('',*,*,#15367,.T.);
#22898=ORIENTED_EDGE('',*,*,#15363,.T.);
#22899=ORIENTED_EDGE('',*,*,#15368,.F.);
#22900=ORIENTED_EDGE('',*,*,#15369,.F.);
#22901=ORIENTED_EDGE('',*,*,#15370,.T.);
#22902=ORIENTED_EDGE('',*,*,#15366,.T.);
#22903=ORIENTED_EDGE('',*,*,#15371,.F.);
#22904=ORIENTED_EDGE('',*,*,#15372,.F.);
#22905=ORIENTED_EDGE('',*,*,#15373,.T.);
#22906=ORIENTED_EDGE('',*,*,#15369,.T.);
#22907=ORIENTED_EDGE('',*,*,#15374,.F.);
#22908=ORIENTED_EDGE('',*,*,#15375,.F.);
#22909=ORIENTED_EDGE('',*,*,#15376,.T.);
#22910=ORIENTED_EDGE('',*,*,#15372,.T.);
#22911=ORIENTED_EDGE('',*,*,#15377,.F.);
#22912=ORIENTED_EDGE('',*,*,#15378,.F.);
#22913=ORIENTED_EDGE('',*,*,#15379,.T.);
#22914=ORIENTED_EDGE('',*,*,#15375,.T.);
#22915=ORIENTED_EDGE('',*,*,#15380,.F.);
#22916=ORIENTED_EDGE('',*,*,#15381,.F.);
#22917=ORIENTED_EDGE('',*,*,#15382,.T.);
#22918=ORIENTED_EDGE('',*,*,#15378,.T.);
#22919=ORIENTED_EDGE('',*,*,#15383,.F.);
#22920=ORIENTED_EDGE('',*,*,#15384,.F.);
#22921=ORIENTED_EDGE('',*,*,#15385,.T.);
#22922=ORIENTED_EDGE('',*,*,#15381,.T.);
#22923=ORIENTED_EDGE('',*,*,#15386,.F.);
#22924=ORIENTED_EDGE('',*,*,#15387,.F.);
#22925=ORIENTED_EDGE('',*,*,#15388,.T.);
#22926=ORIENTED_EDGE('',*,*,#15384,.T.);
#22927=ORIENTED_EDGE('',*,*,#15389,.F.);
#22928=ORIENTED_EDGE('',*,*,#15390,.F.);
#22929=ORIENTED_EDGE('',*,*,#15391,.T.);
#22930=ORIENTED_EDGE('',*,*,#15387,.T.);
#22931=ORIENTED_EDGE('',*,*,#15392,.F.);
#22932=ORIENTED_EDGE('',*,*,#15393,.F.);
#22933=ORIENTED_EDGE('',*,*,#15394,.F.);
#22934=ORIENTED_EDGE('',*,*,#15331,.F.);
#22935=ORIENTED_EDGE('',*,*,#15328,.F.);
#22936=ORIENTED_EDGE('',*,*,#15325,.F.);
#22937=ORIENTED_EDGE('',*,*,#15322,.F.);
#22938=ORIENTED_EDGE('',*,*,#15319,.F.);
#22939=ORIENTED_EDGE('',*,*,#15316,.F.);
#22940=ORIENTED_EDGE('',*,*,#15313,.F.);
#22941=ORIENTED_EDGE('',*,*,#15310,.F.);
#22942=ORIENTED_EDGE('',*,*,#15307,.F.);
#22943=ORIENTED_EDGE('',*,*,#15304,.F.);
#22944=ORIENTED_EDGE('',*,*,#15301,.F.);
#22945=ORIENTED_EDGE('',*,*,#15298,.F.);
#22946=ORIENTED_EDGE('',*,*,#15295,.F.);
#22947=ORIENTED_EDGE('',*,*,#15292,.F.);
#22948=ORIENTED_EDGE('',*,*,#15289,.F.);
#22949=ORIENTED_EDGE('',*,*,#15286,.F.);
#22950=ORIENTED_EDGE('',*,*,#15283,.F.);
#22951=ORIENTED_EDGE('',*,*,#15280,.F.);
#22952=ORIENTED_EDGE('',*,*,#15277,.F.);
#22953=ORIENTED_EDGE('',*,*,#15274,.F.);
#22954=ORIENTED_EDGE('',*,*,#15395,.F.);
#22955=ORIENTED_EDGE('',*,*,#15396,.T.);
#22956=ORIENTED_EDGE('',*,*,#15392,.T.);
#22957=ORIENTED_EDGE('',*,*,#15389,.T.);
#22958=ORIENTED_EDGE('',*,*,#15386,.T.);
#22959=ORIENTED_EDGE('',*,*,#15383,.T.);
#22960=ORIENTED_EDGE('',*,*,#15380,.T.);
#22961=ORIENTED_EDGE('',*,*,#15377,.T.);
#22962=ORIENTED_EDGE('',*,*,#15374,.T.);
#22963=ORIENTED_EDGE('',*,*,#15371,.T.);
#22964=ORIENTED_EDGE('',*,*,#15368,.T.);
#22965=ORIENTED_EDGE('',*,*,#15365,.T.);
#22966=ORIENTED_EDGE('',*,*,#15362,.T.);
#22967=ORIENTED_EDGE('',*,*,#15359,.T.);
#22968=ORIENTED_EDGE('',*,*,#15356,.T.);
#22969=ORIENTED_EDGE('',*,*,#15353,.T.);
#22970=ORIENTED_EDGE('',*,*,#15350,.T.);
#22971=ORIENTED_EDGE('',*,*,#15347,.T.);
#22972=ORIENTED_EDGE('',*,*,#15344,.T.);
#22973=ORIENTED_EDGE('',*,*,#15341,.T.);
#22974=ORIENTED_EDGE('',*,*,#15338,.T.);
#22975=ORIENTED_EDGE('',*,*,#15335,.T.);
#22976=ORIENTED_EDGE('',*,*,#15390,.T.);
#22977=ORIENTED_EDGE('',*,*,#15396,.F.);
#22978=ORIENTED_EDGE('',*,*,#15397,.F.);
#22979=ORIENTED_EDGE('',*,*,#15398,.T.);
#22980=ORIENTED_EDGE('',*,*,#15399,.F.);
#22981=ORIENTED_EDGE('',*,*,#15333,.F.);
#22982=ORIENTED_EDGE('',*,*,#15337,.F.);
#22983=ORIENTED_EDGE('',*,*,#15340,.F.);
#22984=ORIENTED_EDGE('',*,*,#15343,.F.);
#22985=ORIENTED_EDGE('',*,*,#15346,.F.);
#22986=ORIENTED_EDGE('',*,*,#15349,.F.);
#22987=ORIENTED_EDGE('',*,*,#15352,.F.);
#22988=ORIENTED_EDGE('',*,*,#15355,.F.);
#22989=ORIENTED_EDGE('',*,*,#15358,.F.);
#22990=ORIENTED_EDGE('',*,*,#15361,.F.);
#22991=ORIENTED_EDGE('',*,*,#15364,.F.);
#22992=ORIENTED_EDGE('',*,*,#15367,.F.);
#22993=ORIENTED_EDGE('',*,*,#15370,.F.);
#22994=ORIENTED_EDGE('',*,*,#15373,.F.);
#22995=ORIENTED_EDGE('',*,*,#15376,.F.);
#22996=ORIENTED_EDGE('',*,*,#15379,.F.);
#22997=ORIENTED_EDGE('',*,*,#15382,.F.);
#22998=ORIENTED_EDGE('',*,*,#15385,.F.);
#22999=ORIENTED_EDGE('',*,*,#15388,.F.);
#23000=ORIENTED_EDGE('',*,*,#15391,.F.);
#23001=ORIENTED_EDGE('',*,*,#15398,.F.);
#23002=ORIENTED_EDGE('',*,*,#15400,.F.);
#23003=ORIENTED_EDGE('',*,*,#15272,.F.);
#23004=ORIENTED_EDGE('',*,*,#15276,.F.);
#23005=ORIENTED_EDGE('',*,*,#15279,.F.);
#23006=ORIENTED_EDGE('',*,*,#15282,.F.);
#23007=ORIENTED_EDGE('',*,*,#15285,.F.);
#23008=ORIENTED_EDGE('',*,*,#15288,.F.);
#23009=ORIENTED_EDGE('',*,*,#15291,.F.);
#23010=ORIENTED_EDGE('',*,*,#15294,.F.);
#23011=ORIENTED_EDGE('',*,*,#15297,.F.);
#23012=ORIENTED_EDGE('',*,*,#15300,.F.);
#23013=ORIENTED_EDGE('',*,*,#15303,.F.);
#23014=ORIENTED_EDGE('',*,*,#15306,.F.);
#23015=ORIENTED_EDGE('',*,*,#15309,.F.);
#23016=ORIENTED_EDGE('',*,*,#15312,.F.);
#23017=ORIENTED_EDGE('',*,*,#15315,.F.);
#23018=ORIENTED_EDGE('',*,*,#15318,.F.);
#23019=ORIENTED_EDGE('',*,*,#15321,.F.);
#23020=ORIENTED_EDGE('',*,*,#15324,.F.);
#23021=ORIENTED_EDGE('',*,*,#15327,.F.);
#23022=ORIENTED_EDGE('',*,*,#15330,.F.);
#23023=ORIENTED_EDGE('',*,*,#15401,.F.);
#23024=ORIENTED_EDGE('',*,*,#15329,.T.);
#23025=ORIENTED_EDGE('',*,*,#15394,.T.);
#23026=ORIENTED_EDGE('',*,*,#15402,.F.);
#23027=ORIENTED_EDGE('',*,*,#15401,.T.);
#23028=ORIENTED_EDGE('',*,*,#15403,.F.);
#23029=ORIENTED_EDGE('',*,*,#15404,.T.);
#23030=ORIENTED_EDGE('',*,*,#15405,.T.);
#23031=ORIENTED_EDGE('',*,*,#15406,.F.);
#23032=ORIENTED_EDGE('',*,*,#15407,.F.);
#23033=ORIENTED_EDGE('',*,*,#15408,.T.);
#23034=ORIENTED_EDGE('',*,*,#15409,.T.);
#23035=ORIENTED_EDGE('',*,*,#15404,.F.);
#23036=ORIENTED_EDGE('',*,*,#15410,.F.);
#23037=ORIENTED_EDGE('',*,*,#15411,.T.);
#23038=ORIENTED_EDGE('',*,*,#15412,.T.);
#23039=ORIENTED_EDGE('',*,*,#15408,.F.);
#23040=ORIENTED_EDGE('',*,*,#15413,.F.);
#23041=ORIENTED_EDGE('',*,*,#15414,.T.);
#23042=ORIENTED_EDGE('',*,*,#15415,.T.);
#23043=ORIENTED_EDGE('',*,*,#15411,.F.);
#23044=ORIENTED_EDGE('',*,*,#15416,.F.);
#23045=ORIENTED_EDGE('',*,*,#15417,.T.);
#23046=ORIENTED_EDGE('',*,*,#15418,.T.);
#23047=ORIENTED_EDGE('',*,*,#15414,.F.);
#23048=ORIENTED_EDGE('',*,*,#15419,.F.);
#23049=ORIENTED_EDGE('',*,*,#15406,.T.);
#23050=ORIENTED_EDGE('',*,*,#15420,.T.);
#23051=ORIENTED_EDGE('',*,*,#15417,.F.);
#23052=ORIENTED_EDGE('',*,*,#15420,.F.);
#23053=ORIENTED_EDGE('',*,*,#15405,.F.);
#23054=ORIENTED_EDGE('',*,*,#15409,.F.);
#23055=ORIENTED_EDGE('',*,*,#15412,.F.);
#23056=ORIENTED_EDGE('',*,*,#15415,.F.);
#23057=ORIENTED_EDGE('',*,*,#15418,.F.);
#23058=ORIENTED_EDGE('',*,*,#15421,.T.);
#23059=ORIENTED_EDGE('',*,*,#15400,.T.);
#23060=ORIENTED_EDGE('',*,*,#15397,.T.);
#23061=ORIENTED_EDGE('',*,*,#15395,.T.);
#23062=ORIENTED_EDGE('',*,*,#15273,.F.);
#23063=ORIENTED_EDGE('',*,*,#15421,.F.);
#23064=ORIENTED_EDGE('',*,*,#15422,.T.);
#23065=ORIENTED_EDGE('',*,*,#15423,.T.);
#23066=ORIENTED_EDGE('',*,*,#15422,.F.);
#23067=ORIENTED_EDGE('',*,*,#15423,.F.);
#23068=ORIENTED_EDGE('',*,*,#15403,.T.);
#23069=ORIENTED_EDGE('',*,*,#15419,.T.);
#23070=ORIENTED_EDGE('',*,*,#15416,.T.);
#23071=ORIENTED_EDGE('',*,*,#15413,.T.);
#23072=ORIENTED_EDGE('',*,*,#15410,.T.);
#23073=ORIENTED_EDGE('',*,*,#15407,.T.);
#23074=ORIENTED_EDGE('',*,*,#15399,.T.);
#23075=ORIENTED_EDGE('',*,*,#15402,.T.);
#23076=ORIENTED_EDGE('',*,*,#15393,.T.);
#23077=ORIENTED_EDGE('',*,*,#15334,.T.);
#23078=CYLINDRICAL_SURFACE('',#25393,2.5175);
#23079=CYLINDRICAL_SURFACE('',#25397,2.5175);
#23080=CYLINDRICAL_SURFACE('',#25398,2.5175);
#23081=CYLINDRICAL_SURFACE('',#25399,2.5175);
#23082=CYLINDRICAL_SURFACE('',#25400,2.5175);
#23083=CYLINDRICAL_SURFACE('',#25401,2.5175);
#23084=CYLINDRICAL_SURFACE('',#25402,2.5175);
#23085=CYLINDRICAL_SURFACE('',#25403,2.5175);
#23086=CYLINDRICAL_SURFACE('',#25404,2.5175);
#23087=CYLINDRICAL_SURFACE('',#25405,2.5175);
#23088=CYLINDRICAL_SURFACE('',#25406,2.5175);
#23089=CYLINDRICAL_SURFACE('',#25407,2.5175);
#23090=CYLINDRICAL_SURFACE('',#25408,2.5175);
#23091=CYLINDRICAL_SURFACE('',#25409,2.5175);
#23092=CYLINDRICAL_SURFACE('',#25410,2.5175);
#23093=CYLINDRICAL_SURFACE('',#25412,3.0735);
#23094=CYLINDRICAL_SURFACE('',#25414,3.0735);
#23095=CYLINDRICAL_SURFACE('',#25415,3.0735);
#23096=CYLINDRICAL_SURFACE('',#25416,3.0735);
#23097=CYLINDRICAL_SURFACE('',#25417,3.0735);
#23098=CYLINDRICAL_SURFACE('',#25418,3.0735);
#23099=CYLINDRICAL_SURFACE('',#25419,3.0735);
#23100=CYLINDRICAL_SURFACE('',#25420,3.0735);
#23101=CYLINDRICAL_SURFACE('',#25421,3.0735);
#23102=CYLINDRICAL_SURFACE('',#25422,3.0735);
#23103=CYLINDRICAL_SURFACE('',#25423,3.0735);
#23104=CYLINDRICAL_SURFACE('',#25424,3.0735);
#23105=CYLINDRICAL_SURFACE('',#25425,3.0735);
#23106=CYLINDRICAL_SURFACE('',#25426,3.0735);
#23107=CYLINDRICAL_SURFACE('',#25427,3.0735);
#23108=CYLINDRICAL_SURFACE('',#25429,2.5175);
#23109=CYLINDRICAL_SURFACE('',#25433,2.5175);
#23110=CYLINDRICAL_SURFACE('',#25434,2.5175);
#23111=CYLINDRICAL_SURFACE('',#25435,2.5175);
#23112=CYLINDRICAL_SURFACE('',#25436,2.5175);
#23113=CYLINDRICAL_SURFACE('',#25437,2.5175);
#23114=CYLINDRICAL_SURFACE('',#25438,2.5175);
#23115=CYLINDRICAL_SURFACE('',#25439,2.5175);
#23116=CYLINDRICAL_SURFACE('',#25440,2.5175);
#23117=CYLINDRICAL_SURFACE('',#25441,2.5175);
#23118=CYLINDRICAL_SURFACE('',#25442,2.5175);
#23119=CYLINDRICAL_SURFACE('',#25443,2.5175);
#23120=CYLINDRICAL_SURFACE('',#25444,2.5175);
#23121=CYLINDRICAL_SURFACE('',#25445,2.5175);
#23122=CYLINDRICAL_SURFACE('',#25446,2.5175);
#23123=CYLINDRICAL_SURFACE('',#25448,3.0735);
#23124=CYLINDRICAL_SURFACE('',#25450,3.0735);
#23125=CYLINDRICAL_SURFACE('',#25451,3.0735);
#23126=CYLINDRICAL_SURFACE('',#25452,3.0735);
#23127=CYLINDRICAL_SURFACE('',#25453,3.0735);
#23128=CYLINDRICAL_SURFACE('',#25454,3.0735);
#23129=CYLINDRICAL_SURFACE('',#25455,3.0735);
#23130=CYLINDRICAL_SURFACE('',#25456,3.0735);
#23131=CYLINDRICAL_SURFACE('',#25457,3.0735);
#23132=CYLINDRICAL_SURFACE('',#25458,3.0735);
#23133=CYLINDRICAL_SURFACE('',#25459,3.0735);
#23134=CYLINDRICAL_SURFACE('',#25460,3.0735);
#23135=CYLINDRICAL_SURFACE('',#25461,3.0735);
#23136=CYLINDRICAL_SURFACE('',#25462,3.0735);
#23137=CYLINDRICAL_SURFACE('',#25463,3.0735);
#23138=CYLINDRICAL_SURFACE('',#25465,2.5175);
#23139=CYLINDRICAL_SURFACE('',#25469,2.5175);
#23140=CYLINDRICAL_SURFACE('',#25470,2.5175);
#23141=CYLINDRICAL_SURFACE('',#25471,2.5175);
#23142=CYLINDRICAL_SURFACE('',#25472,2.5175);
#23143=CYLINDRICAL_SURFACE('',#25473,2.5175);
#23144=CYLINDRICAL_SURFACE('',#25474,2.5175);
#23145=CYLINDRICAL_SURFACE('',#25475,2.5175);
#23146=CYLINDRICAL_SURFACE('',#25476,2.5175);
#23147=CYLINDRICAL_SURFACE('',#25477,2.5175);
#23148=CYLINDRICAL_SURFACE('',#25478,2.5175);
#23149=CYLINDRICAL_SURFACE('',#25479,2.5175);
#23150=CYLINDRICAL_SURFACE('',#25480,2.5175);
#23151=CYLINDRICAL_SURFACE('',#25481,2.5175);
#23152=CYLINDRICAL_SURFACE('',#25482,2.5175);
#23153=CYLINDRICAL_SURFACE('',#25484,3.0735);
#23154=CYLINDRICAL_SURFACE('',#25486,3.0735);
#23155=CYLINDRICAL_SURFACE('',#25487,3.0735);
#23156=CYLINDRICAL_SURFACE('',#25488,3.0735);
#23157=CYLINDRICAL_SURFACE('',#25489,3.0735);
#23158=CYLINDRICAL_SURFACE('',#25490,3.0735);
#23159=CYLINDRICAL_SURFACE('',#25491,3.0735);
#23160=CYLINDRICAL_SURFACE('',#25492,3.0735);
#23161=CYLINDRICAL_SURFACE('',#25493,3.0735);
#23162=CYLINDRICAL_SURFACE('',#25494,3.0735);
#23163=CYLINDRICAL_SURFACE('',#25495,3.0735);
#23164=CYLINDRICAL_SURFACE('',#25496,3.0735);
#23165=CYLINDRICAL_SURFACE('',#25497,3.0735);
#23166=CYLINDRICAL_SURFACE('',#25498,3.0735);
#23167=CYLINDRICAL_SURFACE('',#25499,3.0735);
#23168=CYLINDRICAL_SURFACE('',#25501,2.5175);
#23169=CYLINDRICAL_SURFACE('',#25505,2.5175);
#23170=CYLINDRICAL_SURFACE('',#25506,2.5175);
#23171=CYLINDRICAL_SURFACE('',#25507,2.5175);
#23172=CYLINDRICAL_SURFACE('',#25508,2.5175);
#23173=CYLINDRICAL_SURFACE('',#25509,2.5175);
#23174=CYLINDRICAL_SURFACE('',#25510,2.5175);
#23175=CYLINDRICAL_SURFACE('',#25511,2.5175);
#23176=CYLINDRICAL_SURFACE('',#25512,2.5175);
#23177=CYLINDRICAL_SURFACE('',#25513,2.5175);
#23178=CYLINDRICAL_SURFACE('',#25514,2.5175);
#23179=CYLINDRICAL_SURFACE('',#25515,2.5175);
#23180=CYLINDRICAL_SURFACE('',#25516,2.5175);
#23181=CYLINDRICAL_SURFACE('',#25517,2.5175);
#23182=CYLINDRICAL_SURFACE('',#25518,2.5175);
#23183=CYLINDRICAL_SURFACE('',#25520,3.0735);
#23184=CYLINDRICAL_SURFACE('',#25522,3.0735);
#23185=CYLINDRICAL_SURFACE('',#25523,3.0735);
#23186=CYLINDRICAL_SURFACE('',#25524,3.0735);
#23187=CYLINDRICAL_SURFACE('',#25525,3.0735);
#23188=CYLINDRICAL_SURFACE('',#25526,3.0735);
#23189=CYLINDRICAL_SURFACE('',#25527,3.0735);
#23190=CYLINDRICAL_SURFACE('',#25528,3.0735);
#23191=CYLINDRICAL_SURFACE('',#25529,3.0735);
#23192=CYLINDRICAL_SURFACE('',#25530,3.0735);
#23193=CYLINDRICAL_SURFACE('',#25531,3.0735);
#23194=CYLINDRICAL_SURFACE('',#25532,3.0735);
#23195=CYLINDRICAL_SURFACE('',#25533,3.0735);
#23196=CYLINDRICAL_SURFACE('',#25534,3.0735);
#23197=CYLINDRICAL_SURFACE('',#25535,3.0735);
#23198=CYLINDRICAL_SURFACE('',#25537,2.5175);
#23199=CYLINDRICAL_SURFACE('',#25541,2.5175);
#23200=CYLINDRICAL_SURFACE('',#25542,2.5175);
#23201=CYLINDRICAL_SURFACE('',#25543,2.5175);
#23202=CYLINDRICAL_SURFACE('',#25544,2.5175);
#23203=CYLINDRICAL_SURFACE('',#25545,2.5175);
#23204=CYLINDRICAL_SURFACE('',#25546,2.5175);
#23205=CYLINDRICAL_SURFACE('',#25547,2.5175);
#23206=CYLINDRICAL_SURFACE('',#25548,2.5175);
#23207=CYLINDRICAL_SURFACE('',#25549,2.5175);
#23208=CYLINDRICAL_SURFACE('',#25550,2.5175);
#23209=CYLINDRICAL_SURFACE('',#25551,2.5175);
#23210=CYLINDRICAL_SURFACE('',#25552,2.5175);
#23211=CYLINDRICAL_SURFACE('',#25553,2.5175);
#23212=CYLINDRICAL_SURFACE('',#25554,2.5175);
#23213=CYLINDRICAL_SURFACE('',#25556,3.0735);
#23214=CYLINDRICAL_SURFACE('',#25558,3.0735);
#23215=CYLINDRICAL_SURFACE('',#25559,3.0735);
#23216=CYLINDRICAL_SURFACE('',#25560,3.0735);
#23217=CYLINDRICAL_SURFACE('',#25561,3.0735);
#23218=CYLINDRICAL_SURFACE('',#25562,3.0735);
#23219=CYLINDRICAL_SURFACE('',#25563,3.0735);
#23220=CYLINDRICAL_SURFACE('',#25564,3.0735);
#23221=CYLINDRICAL_SURFACE('',#25565,3.0735);
#23222=CYLINDRICAL_SURFACE('',#25566,3.0735);
#23223=CYLINDRICAL_SURFACE('',#25567,3.0735);
#23224=CYLINDRICAL_SURFACE('',#25568,3.0735);
#23225=CYLINDRICAL_SURFACE('',#25569,3.0735);
#23226=CYLINDRICAL_SURFACE('',#25570,3.0735);
#23227=CYLINDRICAL_SURFACE('',#25571,3.0735);
#23228=CYLINDRICAL_SURFACE('',#25573,2.5175);
#23229=CYLINDRICAL_SURFACE('',#25577,2.5175);
#23230=CYLINDRICAL_SURFACE('',#25578,2.5175);
#23231=CYLINDRICAL_SURFACE('',#25579,2.5175);
#23232=CYLINDRICAL_SURFACE('',#25580,2.5175);
#23233=CYLINDRICAL_SURFACE('',#25581,2.5175);
#23234=CYLINDRICAL_SURFACE('',#25582,2.5175);
#23235=CYLINDRICAL_SURFACE('',#25583,2.5175);
#23236=CYLINDRICAL_SURFACE('',#25584,2.5175);
#23237=CYLINDRICAL_SURFACE('',#25585,2.5175);
#23238=CYLINDRICAL_SURFACE('',#25586,2.5175);
#23239=CYLINDRICAL_SURFACE('',#25587,2.5175);
#23240=CYLINDRICAL_SURFACE('',#25588,2.5175);
#23241=CYLINDRICAL_SURFACE('',#25589,2.5175);
#23242=CYLINDRICAL_SURFACE('',#25590,2.5175);
#23243=CYLINDRICAL_SURFACE('',#25592,3.0735);
#23244=CYLINDRICAL_SURFACE('',#25594,3.0735);
#23245=CYLINDRICAL_SURFACE('',#25595,3.0735);
#23246=CYLINDRICAL_SURFACE('',#25596,3.0735);
#23247=CYLINDRICAL_SURFACE('',#25597,3.0735);
#23248=CYLINDRICAL_SURFACE('',#25598,3.0735);
#23249=CYLINDRICAL_SURFACE('',#25599,3.0735);
#23250=CYLINDRICAL_SURFACE('',#25600,3.0735);
#23251=CYLINDRICAL_SURFACE('',#25601,3.0735);
#23252=CYLINDRICAL_SURFACE('',#25602,3.0735);
#23253=CYLINDRICAL_SURFACE('',#25603,3.0735);
#23254=CYLINDRICAL_SURFACE('',#25604,3.0735);
#23255=CYLINDRICAL_SURFACE('',#25605,3.0735);
#23256=CYLINDRICAL_SURFACE('',#25606,3.0735);
#23257=CYLINDRICAL_SURFACE('',#25607,3.0735);
#23258=CYLINDRICAL_SURFACE('',#25609,2.5175);
#23259=CYLINDRICAL_SURFACE('',#25613,2.5175);
#23260=CYLINDRICAL_SURFACE('',#25614,2.5175);
#23261=CYLINDRICAL_SURFACE('',#25615,2.5175);
#23262=CYLINDRICAL_SURFACE('',#25616,2.5175);
#23263=CYLINDRICAL_SURFACE('',#25617,2.5175);
#23264=CYLINDRICAL_SURFACE('',#25618,2.5175);
#23265=CYLINDRICAL_SURFACE('',#25619,2.5175);
#23266=CYLINDRICAL_SURFACE('',#25620,2.5175);
#23267=CYLINDRICAL_SURFACE('',#25621,2.5175);
#23268=CYLINDRICAL_SURFACE('',#25622,2.5175);
#23269=CYLINDRICAL_SURFACE('',#25623,2.5175);
#23270=CYLINDRICAL_SURFACE('',#25624,2.5175);
#23271=CYLINDRICAL_SURFACE('',#25625,2.5175);
#23272=CYLINDRICAL_SURFACE('',#25626,2.5175);
#23273=CYLINDRICAL_SURFACE('',#25628,3.0735);
#23274=CYLINDRICAL_SURFACE('',#25630,3.0735);
#23275=CYLINDRICAL_SURFACE('',#25631,3.0735);
#23276=CYLINDRICAL_SURFACE('',#25632,3.0735);
#23277=CYLINDRICAL_SURFACE('',#25633,3.0735);
#23278=CYLINDRICAL_SURFACE('',#25634,3.0735);
#23279=CYLINDRICAL_SURFACE('',#25635,3.0735);
#23280=CYLINDRICAL_SURFACE('',#25636,3.0735);
#23281=CYLINDRICAL_SURFACE('',#25637,3.0735);
#23282=CYLINDRICAL_SURFACE('',#25638,3.0735);
#23283=CYLINDRICAL_SURFACE('',#25639,3.0735);
#23284=CYLINDRICAL_SURFACE('',#25640,3.0735);
#23285=CYLINDRICAL_SURFACE('',#25641,3.0735);
#23286=CYLINDRICAL_SURFACE('',#25642,3.0735);
#23287=CYLINDRICAL_SURFACE('',#25643,3.0735);
#23288=CYLINDRICAL_SURFACE('',#25645,2.5175);
#23289=CYLINDRICAL_SURFACE('',#25649,2.5175);
#23290=CYLINDRICAL_SURFACE('',#25650,2.5175);
#23291=CYLINDRICAL_SURFACE('',#25651,2.5175);
#23292=CYLINDRICAL_SURFACE('',#25652,2.5175);
#23293=CYLINDRICAL_SURFACE('',#25653,2.5175);
#23294=CYLINDRICAL_SURFACE('',#25654,2.5175);
#23295=CYLINDRICAL_SURFACE('',#25655,2.5175);
#23296=CYLINDRICAL_SURFACE('',#25656,2.5175);
#23297=CYLINDRICAL_SURFACE('',#25657,2.5175);
#23298=CYLINDRICAL_SURFACE('',#25658,2.5175);
#23299=CYLINDRICAL_SURFACE('',#25659,2.5175);
#23300=CYLINDRICAL_SURFACE('',#25660,2.5175);
#23301=CYLINDRICAL_SURFACE('',#25661,2.5175);
#23302=CYLINDRICAL_SURFACE('',#25662,2.5175);
#23303=CYLINDRICAL_SURFACE('',#25664,3.0735);
#23304=CYLINDRICAL_SURFACE('',#25666,3.0735);
#23305=CYLINDRICAL_SURFACE('',#25667,3.0735);
#23306=CYLINDRICAL_SURFACE('',#25668,3.0735);
#23307=CYLINDRICAL_SURFACE('',#25669,3.0735);
#23308=CYLINDRICAL_SURFACE('',#25670,3.0735);
#23309=CYLINDRICAL_SURFACE('',#25671,3.0735);
#23310=CYLINDRICAL_SURFACE('',#25672,3.0735);
#23311=CYLINDRICAL_SURFACE('',#25673,3.0735);
#23312=CYLINDRICAL_SURFACE('',#25674,3.0735);
#23313=CYLINDRICAL_SURFACE('',#25675,3.0735);
#23314=CYLINDRICAL_SURFACE('',#25676,3.0735);
#23315=CYLINDRICAL_SURFACE('',#25677,3.0735);
#23316=CYLINDRICAL_SURFACE('',#25678,3.0735);
#23317=CYLINDRICAL_SURFACE('',#25679,3.0735);
#23318=CYLINDRICAL_SURFACE('',#25681,2.);
#23319=CYLINDRICAL_SURFACE('',#25682,2.);
#23320=CYLINDRICAL_SURFACE('',#25683,2.);
#23321=CYLINDRICAL_SURFACE('',#25684,2.);
#23322=CYLINDRICAL_SURFACE('',#25685,2.);
#23323=CYLINDRICAL_SURFACE('',#25686,2.);
#23324=CYLINDRICAL_SURFACE('',#25687,2.);
#23325=CYLINDRICAL_SURFACE('',#25688,2.);
#23326=CYLINDRICAL_SURFACE('',#25689,2.);
#23327=CYLINDRICAL_SURFACE('',#25690,2.);
#23328=CYLINDRICAL_SURFACE('',#25691,2.);
#23329=CYLINDRICAL_SURFACE('',#25692,2.);
#23330=CYLINDRICAL_SURFACE('',#25694,3.0735);
#23331=CYLINDRICAL_SURFACE('',#25695,2.5175);
#23332=CYLINDRICAL_SURFACE('',#25697,3.0735);
#23333=CYLINDRICAL_SURFACE('',#25698,2.5175);
#23334=CYLINDRICAL_SURFACE('',#25700,3.0735);
#23335=CYLINDRICAL_SURFACE('',#25701,2.5175);
#23336=CYLINDRICAL_SURFACE('',#25703,3.0735);
#23337=CYLINDRICAL_SURFACE('',#25704,2.5175);
#23338=CYLINDRICAL_SURFACE('',#25706,3.0735);
#23339=CYLINDRICAL_SURFACE('',#25707,2.5175);
#23340=CYLINDRICAL_SURFACE('',#25709,3.0735);
#23341=CYLINDRICAL_SURFACE('',#25710,2.5175);
#23342=CYLINDRICAL_SURFACE('',#25712,3.0735);
#23343=CYLINDRICAL_SURFACE('',#25713,2.5175);
#23344=CYLINDRICAL_SURFACE('',#25715,3.0735);
#23345=CYLINDRICAL_SURFACE('',#25716,2.5175);
#23346=CYLINDRICAL_SURFACE('',#25725,5.5);
#23347=CYLINDRICAL_SURFACE('',#25728,5.5);
#23348=CYLINDRICAL_SURFACE('',#25731,5.5);
#23349=CYLINDRICAL_SURFACE('',#25734,5.5);
#23350=CYLINDRICAL_SURFACE('',#25737,18.);
#23351=CYLINDRICAL_SURFACE('',#25742,90.);
#23352=CYLINDRICAL_SURFACE('',#25745,100.);
#23353=CYLINDRICAL_SURFACE('',#25751,17.);
#23354=CYLINDRICAL_SURFACE('',#25753,140.);
#23355=CYLINDRICAL_SURFACE('',#25758,2.);
#23356=CYLINDRICAL_SURFACE('',#25761,2.);
#23357=CYLINDRICAL_SURFACE('',#25764,2.);
#23358=CYLINDRICAL_SURFACE('',#25767,2.);
#23359=CYLINDRICAL_SURFACE('',#25770,18.);
#23360=CYLINDRICAL_SURFACE('',#25773,90.);
#23361=CYLINDRICAL_SURFACE('',#25779,3.5);
#23362=CYLINDRICAL_SURFACE('',#25782,3.5);
#23363=CYLINDRICAL_SURFACE('',#25785,3.5);
#23364=CYLINDRICAL_SURFACE('',#25788,3.5);
#23365=CYLINDRICAL_SURFACE('',#25791,3.5);
#23366=CYLINDRICAL_SURFACE('',#25794,3.5);
#23367=CYLINDRICAL_SURFACE('',#25797,3.5);
#23368=CYLINDRICAL_SURFACE('',#25800,3.5);
#23369=CYLINDRICAL_SURFACE('',#25803,18.);
#23370=CYLINDRICAL_SURFACE('',#25806,100.);
#23371=CYLINDRICAL_SURFACE('',#25819,7.);
#23372=CYLINDRICAL_SURFACE('',#25826,8.);
#23373=CYLINDRICAL_SURFACE('',#25828,15.);
#23374=CYLINDRICAL_SURFACE('',#25835,16.);
#23375=CYLINDRICAL_SURFACE('',#25843,11.);
#23376=CYLINDRICAL_SURFACE('',#25844,8.);
#23377=CYLINDRICAL_SURFACE('',#25851,20.);
#23378=CYLINDRICAL_SURFACE('',#25852,16.);
#23379=CYLINDRICAL_SURFACE('',#25854,8.);
#23380=CYLINDRICAL_SURFACE('',#25856,8.);
#23381=CYLINDRICAL_SURFACE('',#25860,16.);
#23382=CYLINDRICAL_SURFACE('',#25865,2.);
#23383=CYLINDRICAL_SURFACE('',#25868,2.);
#23384=CYLINDRICAL_SURFACE('',#25871,2.);
#23385=CYLINDRICAL_SURFACE('',#25874,2.);
#23386=CYLINDRICAL_SURFACE('',#25877,74.4999999996252);
#23387=CYLINDRICAL_SURFACE('',#25880,74.4999999996252);
#23388=CYLINDRICAL_SURFACE('',#25883,74.4999999996252);
#23389=CYLINDRICAL_SURFACE('',#25886,74.4999999996252);
#23390=CYLINDRICAL_SURFACE('',#25889,74.4999999996252);
#23391=CYLINDRICAL_SURFACE('',#25892,74.4999999996252);
#23392=CYLINDRICAL_SURFACE('',#25895,74.4999999996252);
#23393=CYLINDRICAL_SURFACE('',#25898,74.4999999996252);
#23394=CYLINDRICAL_SURFACE('',#25901,74.4999999996252);
#23395=CYLINDRICAL_SURFACE('',#25904,74.4999999996252);
#23396=CYLINDRICAL_SURFACE('',#25907,74.4999999996252);
#23397=CYLINDRICAL_SURFACE('',#25910,74.4999999996252);
#23398=CYLINDRICAL_SURFACE('',#25913,74.4999999996252);
#23399=CYLINDRICAL_SURFACE('',#25916,74.4999999996252);
#23400=CYLINDRICAL_SURFACE('',#25919,74.4999999996252);
#23401=CYLINDRICAL_SURFACE('',#25922,74.4999999996252);
#23402=CYLINDRICAL_SURFACE('',#25925,74.4999999996252);
#23403=CYLINDRICAL_SURFACE('',#25928,74.4999999996252);
#23404=CYLINDRICAL_SURFACE('',#25931,74.4999999996252);
#23405=CYLINDRICAL_SURFACE('',#25934,74.4999999996252);
#23406=CYLINDRICAL_SURFACE('',#25937,74.4999999996252);
#23407=CYLINDRICAL_SURFACE('',#25940,74.4999999996252);
#23408=CYLINDRICAL_SURFACE('',#25943,74.4999999996252);
#23409=CYLINDRICAL_SURFACE('',#25946,74.4999999996252);
#23410=CYLINDRICAL_SURFACE('',#25949,74.4999999996252);
#23411=CYLINDRICAL_SURFACE('',#25952,74.4999999996252);
#23412=CYLINDRICAL_SURFACE('',#25955,74.4999999996252);
#23413=CYLINDRICAL_SURFACE('',#25958,74.4999999996252);
#23414=CYLINDRICAL_SURFACE('',#25961,74.4999999996252);
#23415=CYLINDRICAL_SURFACE('',#25964,74.4999999996252);
#23416=CYLINDRICAL_SURFACE('',#25967,74.4999999996252);
#23417=CYLINDRICAL_SURFACE('',#25970,74.4999999996252);
#23418=CYLINDRICAL_SURFACE('',#25973,74.4999999996252);
#23419=CYLINDRICAL_SURFACE('',#25976,74.4999999996252);
#23420=CYLINDRICAL_SURFACE('',#25979,74.4999999996252);
#23421=CYLINDRICAL_SURFACE('',#25982,74.4999999996252);
#23422=CYLINDRICAL_SURFACE('',#25985,74.4999999996252);
#23423=CYLINDRICAL_SURFACE('',#25988,74.4999999996252);
#23424=CYLINDRICAL_SURFACE('',#25991,74.4999999996252);
#23425=CYLINDRICAL_SURFACE('',#25994,74.4999999996252);
#23426=CYLINDRICAL_SURFACE('',#25997,74.4999999996252);
#23427=CYLINDRICAL_SURFACE('',#26000,74.4999999996252);
#23428=CYLINDRICAL_SURFACE('',#26003,74.4999999996252);
#23429=CYLINDRICAL_SURFACE('',#26006,74.4999999996252);
#23430=CYLINDRICAL_SURFACE('',#26009,74.4999999996252);
#23431=CYLINDRICAL_SURFACE('',#26012,74.4999999996252);
#23432=CYLINDRICAL_SURFACE('',#26015,74.4999999996252);
#23433=CYLINDRICAL_SURFACE('',#26018,74.4999999996252);
#23434=CYLINDRICAL_SURFACE('',#26021,74.4999999996252);
#23435=CYLINDRICAL_SURFACE('',#26024,74.4999999996252);
#23436=CYLINDRICAL_SURFACE('',#26027,74.4999999996252);
#23437=CYLINDRICAL_SURFACE('',#26030,74.4999999996252);
#23438=CYLINDRICAL_SURFACE('',#26033,74.4999999996252);
#23439=CYLINDRICAL_SURFACE('',#26036,74.4999999996252);
#23440=CYLINDRICAL_SURFACE('',#26039,74.4999999996252);
#23441=CYLINDRICAL_SURFACE('',#26042,74.4999999996252);
#23442=CYLINDRICAL_SURFACE('',#26045,74.4999999996252);
#23443=CYLINDRICAL_SURFACE('',#26048,74.4999999996252);
#23444=CYLINDRICAL_SURFACE('',#26051,74.4999999996252);
#23445=CYLINDRICAL_SURFACE('',#26054,74.4999999996252);
#23446=CYLINDRICAL_SURFACE('',#26057,74.4999999996252);
#23447=CYLINDRICAL_SURFACE('',#26060,74.4999999996252);
#23448=CYLINDRICAL_SURFACE('',#26063,74.4999999996252);
#23449=CYLINDRICAL_SURFACE('',#26066,74.4999999996252);
#23450=CYLINDRICAL_SURFACE('',#26069,74.4999999996252);
#23451=CYLINDRICAL_SURFACE('',#26072,74.4999999996252);
#23452=CYLINDRICAL_SURFACE('',#26075,74.4999999996252);
#23453=CYLINDRICAL_SURFACE('',#26078,74.4999999996252);
#23454=CYLINDRICAL_SURFACE('',#26081,74.4999999996252);
#23455=CYLINDRICAL_SURFACE('',#26084,74.4999999996252);
#23456=CYLINDRICAL_SURFACE('',#26087,74.4999999996252);
#23457=CYLINDRICAL_SURFACE('',#26090,70.);
#23458=CYLINDRICAL_SURFACE('',#26093,70.);
#23459=CYLINDRICAL_SURFACE('',#26096,70.);
#23460=CYLINDRICAL_SURFACE('',#26099,70.);
#23461=CYLINDRICAL_SURFACE('',#26102,70.);
#23462=CYLINDRICAL_SURFACE('',#26105,70.);
#23463=CYLINDRICAL_SURFACE('',#26108,70.);
#23464=CYLINDRICAL_SURFACE('',#26111,70.);
#23465=CYLINDRICAL_SURFACE('',#26114,70.);
#23466=CYLINDRICAL_SURFACE('',#26117,70.);
#23467=CYLINDRICAL_SURFACE('',#26120,70.);
#23468=CYLINDRICAL_SURFACE('',#26123,70.);
#23469=CYLINDRICAL_SURFACE('',#26126,70.);
#23470=CYLINDRICAL_SURFACE('',#26129,70.);
#23471=CYLINDRICAL_SURFACE('',#26132,70.);
#23472=CYLINDRICAL_SURFACE('',#26135,70.);
#23473=CYLINDRICAL_SURFACE('',#26138,70.);
#23474=CYLINDRICAL_SURFACE('',#26141,70.);
#23475=CYLINDRICAL_SURFACE('',#26144,70.);
#23476=CYLINDRICAL_SURFACE('',#26147,70.);
#23477=CYLINDRICAL_SURFACE('',#26150,70.);
#23478=CYLINDRICAL_SURFACE('',#26153,70.);
#23479=CYLINDRICAL_SURFACE('',#26156,70.);
#23480=CYLINDRICAL_SURFACE('',#26159,70.);
#23481=CYLINDRICAL_SURFACE('',#26162,70.);
#23482=CYLINDRICAL_SURFACE('',#26165,70.);
#23483=CYLINDRICAL_SURFACE('',#26168,70.);
#23484=CYLINDRICAL_SURFACE('',#26171,70.);
#23485=CYLINDRICAL_SURFACE('',#26174,70.);
#23486=CYLINDRICAL_SURFACE('',#26177,70.);
#23487=CYLINDRICAL_SURFACE('',#26180,70.);
#23488=CYLINDRICAL_SURFACE('',#26183,70.);
#23489=CYLINDRICAL_SURFACE('',#26186,70.);
#23490=CYLINDRICAL_SURFACE('',#26189,70.);
#23491=CYLINDRICAL_SURFACE('',#26192,70.);
#23492=CYLINDRICAL_SURFACE('',#26195,70.);
#23493=CYLINDRICAL_SURFACE('',#26198,70.);
#23494=CYLINDRICAL_SURFACE('',#26201,70.);
#23495=CYLINDRICAL_SURFACE('',#26204,70.);
#23496=CYLINDRICAL_SURFACE('',#26207,70.);
#23497=CYLINDRICAL_SURFACE('',#26210,70.);
#23498=CYLINDRICAL_SURFACE('',#26213,70.);
#23499=CYLINDRICAL_SURFACE('',#26216,70.);
#23500=CYLINDRICAL_SURFACE('',#26219,70.);
#23501=CYLINDRICAL_SURFACE('',#26222,70.);
#23502=CYLINDRICAL_SURFACE('',#26225,70.);
#23503=CYLINDRICAL_SURFACE('',#26228,70.);
#23504=CYLINDRICAL_SURFACE('',#26231,70.);
#23505=CYLINDRICAL_SURFACE('',#26234,70.);
#23506=CYLINDRICAL_SURFACE('',#26237,70.);
#23507=CYLINDRICAL_SURFACE('',#26240,70.);
#23508=CYLINDRICAL_SURFACE('',#26243,70.);
#23509=CYLINDRICAL_SURFACE('',#26246,70.);
#23510=CYLINDRICAL_SURFACE('',#26249,70.);
#23511=CYLINDRICAL_SURFACE('',#26252,70.);
#23512=CYLINDRICAL_SURFACE('',#26255,70.);
#23513=CYLINDRICAL_SURFACE('',#26258,70.);
#23514=CYLINDRICAL_SURFACE('',#26261,70.);
#23515=CYLINDRICAL_SURFACE('',#26264,70.);
#23516=CYLINDRICAL_SURFACE('',#26267,70.);
#23517=CYLINDRICAL_SURFACE('',#26270,70.);
#23518=CYLINDRICAL_SURFACE('',#26273,70.);
#23519=CYLINDRICAL_SURFACE('',#26276,70.);
#23520=CYLINDRICAL_SURFACE('',#26279,70.);
#23521=CYLINDRICAL_SURFACE('',#26282,70.);
#23522=CYLINDRICAL_SURFACE('',#26285,70.);
#23523=CYLINDRICAL_SURFACE('',#26288,70.);
#23524=CYLINDRICAL_SURFACE('',#26291,70.);
#23525=CYLINDRICAL_SURFACE('',#26294,70.);
#23526=CYLINDRICAL_SURFACE('',#26297,70.);
#23527=CYLINDRICAL_SURFACE('',#26300,70.);
#23528=CYLINDRICAL_SURFACE('',#26303,74.4999999996252);
#23529=CYLINDRICAL_SURFACE('',#26309,70.);
#23530=CYLINDRICAL_SURFACE('',#26311,90.);
#23531=CYLINDRICAL_SURFACE('',#26318,8.);
#23532=CYLINDRICAL_SURFACE('',#26418,0.5);
#23533=CYLINDRICAL_SURFACE('',#26421,0.5);
#23534=CYLINDRICAL_SURFACE('',#26423,21.4999999999992);
#23535=CYLINDRICAL_SURFACE('',#26425,0.5);
#23536=CYLINDRICAL_SURFACE('',#26428,0.5);
#23537=CYLINDRICAL_SURFACE('',#26430,21.4999999999992);
#23538=CYLINDRICAL_SURFACE('',#26432,0.5);
#23539=CYLINDRICAL_SURFACE('',#26435,0.5);
#23540=CYLINDRICAL_SURFACE('',#26437,21.4999999999992);
#23541=CYLINDRICAL_SURFACE('',#26439,0.5);
#23542=CYLINDRICAL_SURFACE('',#26442,0.5);
#23543=CYLINDRICAL_SURFACE('',#26444,21.4999999999992);
#23544=CYLINDRICAL_SURFACE('',#26446,0.5);
#23545=CYLINDRICAL_SURFACE('',#26449,0.5);
#23546=CYLINDRICAL_SURFACE('',#26451,21.4999999999992);
#23547=CYLINDRICAL_SURFACE('',#26453,0.5);
#23548=CYLINDRICAL_SURFACE('',#26456,0.5);
#23549=CYLINDRICAL_SURFACE('',#26458,21.4999999999992);
#23550=CYLINDRICAL_SURFACE('',#26460,0.5);
#23551=CYLINDRICAL_SURFACE('',#26463,0.5);
#23552=CYLINDRICAL_SURFACE('',#26465,21.4999999999992);
#23553=CYLINDRICAL_SURFACE('',#26467,0.5);
#23554=CYLINDRICAL_SURFACE('',#26470,0.5);
#23555=CYLINDRICAL_SURFACE('',#26472,21.4999999999992);
#23556=CYLINDRICAL_SURFACE('',#26474,0.5);
#23557=CYLINDRICAL_SURFACE('',#26477,0.5);
#23558=CYLINDRICAL_SURFACE('',#26479,21.4999999999992);
#23559=CYLINDRICAL_SURFACE('',#26481,0.5);
#23560=CYLINDRICAL_SURFACE('',#26484,0.5);
#23561=CYLINDRICAL_SURFACE('',#26486,21.4999999999992);
#23562=CYLINDRICAL_SURFACE('',#26488,0.5);
#23563=CYLINDRICAL_SURFACE('',#26491,0.5);
#23564=CYLINDRICAL_SURFACE('',#26493,21.4999999999992);
#23565=CYLINDRICAL_SURFACE('',#26495,0.5);
#23566=CYLINDRICAL_SURFACE('',#26498,0.5);
#23567=CYLINDRICAL_SURFACE('',#26500,21.4999999999992);
#23568=CYLINDRICAL_SURFACE('',#26502,0.5);
#23569=CYLINDRICAL_SURFACE('',#26505,0.5);
#23570=CYLINDRICAL_SURFACE('',#26507,21.4999999999992);
#23571=CYLINDRICAL_SURFACE('',#26509,0.5);
#23572=CYLINDRICAL_SURFACE('',#26512,0.5);
#23573=CYLINDRICAL_SURFACE('',#26514,21.4999999999992);
#23574=CYLINDRICAL_SURFACE('',#26516,0.5);
#23575=CYLINDRICAL_SURFACE('',#26519,0.5);
#23576=CYLINDRICAL_SURFACE('',#26521,21.4999999999992);
#23577=CYLINDRICAL_SURFACE('',#26523,0.5);
#23578=CYLINDRICAL_SURFACE('',#26526,0.5);
#23579=CYLINDRICAL_SURFACE('',#26528,21.4999999999992);
#23580=CYLINDRICAL_SURFACE('',#26530,0.5);
#23581=CYLINDRICAL_SURFACE('',#26533,0.5);
#23582=CYLINDRICAL_SURFACE('',#26535,21.4999999999992);
#23583=CYLINDRICAL_SURFACE('',#26537,0.5);
#23584=CYLINDRICAL_SURFACE('',#26540,0.5);
#23585=CYLINDRICAL_SURFACE('',#26542,21.4999999999992);
#23586=CYLINDRICAL_SURFACE('',#26544,0.5);
#23587=CYLINDRICAL_SURFACE('',#26547,0.5);
#23588=CYLINDRICAL_SURFACE('',#26549,21.4999999999992);
#23589=CYLINDRICAL_SURFACE('',#26551,0.5);
#23590=CYLINDRICAL_SURFACE('',#26554,0.5);
#23591=CYLINDRICAL_SURFACE('',#26556,21.4999999999992);
#23592=CYLINDRICAL_SURFACE('',#26558,0.5);
#23593=CYLINDRICAL_SURFACE('',#26561,0.5);
#23594=CYLINDRICAL_SURFACE('',#26563,21.4999999999992);
#23595=CYLINDRICAL_SURFACE('',#26565,0.5);
#23596=CYLINDRICAL_SURFACE('',#26568,0.5);
#23597=CYLINDRICAL_SURFACE('',#26570,21.4999999999992);
#23598=CYLINDRICAL_SURFACE('',#26572,0.5);
#23599=CYLINDRICAL_SURFACE('',#26575,0.5);
#23600=CYLINDRICAL_SURFACE('',#26577,21.4999999999992);
#23601=CYLINDRICAL_SURFACE('',#26630,26.);
#23602=CYLINDRICAL_SURFACE('',#26631,26.);
#23603=CYLINDRICAL_SURFACE('',#26632,26.);
#23604=CYLINDRICAL_SURFACE('',#26633,26.);
#23605=CYLINDRICAL_SURFACE('',#26634,26.);
#23606=CYLINDRICAL_SURFACE('',#26635,26.);
#23607=CYLINDRICAL_SURFACE('',#26636,26.);
#23608=CYLINDRICAL_SURFACE('',#26637,26.);
#23609=CYLINDRICAL_SURFACE('',#26638,26.);
#23610=CYLINDRICAL_SURFACE('',#26639,26.);
#23611=CYLINDRICAL_SURFACE('',#26640,26.);
#23612=CYLINDRICAL_SURFACE('',#26641,26.);
#23613=CYLINDRICAL_SURFACE('',#26642,26.);
#23614=CYLINDRICAL_SURFACE('',#26643,26.);
#23615=CYLINDRICAL_SURFACE('',#26644,26.);
#23616=CYLINDRICAL_SURFACE('',#26645,26.);
#23617=CYLINDRICAL_SURFACE('',#26646,26.);
#23618=CYLINDRICAL_SURFACE('',#26647,26.);
#23619=CYLINDRICAL_SURFACE('',#26648,26.);
#23620=CYLINDRICAL_SURFACE('',#26649,26.);
#23621=CYLINDRICAL_SURFACE('',#26650,26.);
#23622=CYLINDRICAL_SURFACE('',#26651,26.);
#23623=CYLINDRICAL_SURFACE('',#26652,26.);
#23624=CYLINDRICAL_SURFACE('',#26653,0.5);
#23625=CYLINDRICAL_SURFACE('',#26655,0.5);
#23626=CYLINDRICAL_SURFACE('',#26656,21.4999999999992);
#23627=CYLINDRICAL_SURFACE('',#26658,26.);
#23628=CYLINDRICAL_SURFACE('',#26660,0.5);
#23629=CYLINDRICAL_SURFACE('',#26664,0.5);
#23630=CYLINDRICAL_SURFACE('',#26667,21.4999999999992);
#23631=CYLINDRICAL_SURFACE('',#26670,0.5);
#23632=CYLINDRICAL_SURFACE('',#26674,0.5);
#23633=CYLINDRICAL_SURFACE('',#26677,21.4999999999992);
#23634=CYLINDRICAL_SURFACE('',#26680,0.5);
#23635=CYLINDRICAL_SURFACE('',#26684,0.5);
#23636=CYLINDRICAL_SURFACE('',#26687,21.4999999999992);
#23637=CYLINDRICAL_SURFACE('',#26690,0.5);
#23638=CYLINDRICAL_SURFACE('',#26694,0.5);
#23639=CYLINDRICAL_SURFACE('',#26697,21.4999999999992);
#23640=CYLINDRICAL_SURFACE('',#26700,0.5);
#23641=CYLINDRICAL_SURFACE('',#26704,0.5);
#23642=CYLINDRICAL_SURFACE('',#26707,21.4999999999992);
#23643=CYLINDRICAL_SURFACE('',#26710,0.5);
#23644=CYLINDRICAL_SURFACE('',#26714,0.5);
#23645=CYLINDRICAL_SURFACE('',#26717,21.4999999999992);
#23646=CYLINDRICAL_SURFACE('',#26720,0.5);
#23647=CYLINDRICAL_SURFACE('',#26724,0.5);
#23648=CYLINDRICAL_SURFACE('',#26727,21.4999999999992);
#23649=CYLINDRICAL_SURFACE('',#26730,0.5);
#23650=CYLINDRICAL_SURFACE('',#26734,0.5);
#23651=CYLINDRICAL_SURFACE('',#26737,21.4999999999992);
#23652=CYLINDRICAL_SURFACE('',#26740,0.5);
#23653=CYLINDRICAL_SURFACE('',#26744,0.5);
#23654=CYLINDRICAL_SURFACE('',#26747,21.4999999999992);
#23655=CYLINDRICAL_SURFACE('',#26750,0.5);
#23656=CYLINDRICAL_SURFACE('',#26754,0.5);
#23657=CYLINDRICAL_SURFACE('',#26757,21.4999999999992);
#23658=CYLINDRICAL_SURFACE('',#26760,0.5);
#23659=CYLINDRICAL_SURFACE('',#26764,0.5);
#23660=CYLINDRICAL_SURFACE('',#26767,21.4999999999992);
#23661=CYLINDRICAL_SURFACE('',#26770,0.5);
#23662=CYLINDRICAL_SURFACE('',#26774,0.5);
#23663=CYLINDRICAL_SURFACE('',#26777,21.4999999999992);
#23664=CYLINDRICAL_SURFACE('',#26780,0.5);
#23665=CYLINDRICAL_SURFACE('',#26784,0.5);
#23666=CYLINDRICAL_SURFACE('',#26787,21.4999999999992);
#23667=CYLINDRICAL_SURFACE('',#26790,0.5);
#23668=CYLINDRICAL_SURFACE('',#26794,0.5);
#23669=CYLINDRICAL_SURFACE('',#26797,21.4999999999992);
#23670=CYLINDRICAL_SURFACE('',#26800,0.5);
#23671=CYLINDRICAL_SURFACE('',#26804,0.5);
#23672=CYLINDRICAL_SURFACE('',#26807,21.4999999999992);
#23673=CYLINDRICAL_SURFACE('',#26810,0.5);
#23674=CYLINDRICAL_SURFACE('',#26814,0.5);
#23675=CYLINDRICAL_SURFACE('',#26817,21.4999999999992);
#23676=CYLINDRICAL_SURFACE('',#26820,0.5);
#23677=CYLINDRICAL_SURFACE('',#26824,0.5);
#23678=CYLINDRICAL_SURFACE('',#26827,21.4999999999992);
#23679=CYLINDRICAL_SURFACE('',#26830,0.5);
#23680=CYLINDRICAL_SURFACE('',#26834,0.5);
#23681=CYLINDRICAL_SURFACE('',#26837,21.4999999999992);
#23682=CYLINDRICAL_SURFACE('',#26840,0.5);
#23683=CYLINDRICAL_SURFACE('',#26844,0.5);
#23684=CYLINDRICAL_SURFACE('',#26847,21.4999999999992);
#23685=CYLINDRICAL_SURFACE('',#26850,0.5);
#23686=CYLINDRICAL_SURFACE('',#26854,0.5);
#23687=CYLINDRICAL_SURFACE('',#26857,21.4999999999992);
#23688=CYLINDRICAL_SURFACE('',#26860,0.5);
#23689=CYLINDRICAL_SURFACE('',#26864,0.5);
#23690=CYLINDRICAL_SURFACE('',#26867,21.4999999999992);
#23691=CYLINDRICAL_SURFACE('',#26870,0.5);
#23692=CYLINDRICAL_SURFACE('',#26874,0.5);
#23693=CYLINDRICAL_SURFACE('',#26877,21.4999999999992);
#23694=CYLINDRICAL_SURFACE('',#26880,0.5);
#23695=CYLINDRICAL_SURFACE('',#26884,0.5);
#23696=CYLINDRICAL_SURFACE('',#26887,21.4999999999992);
#23697=CYLINDRICAL_SURFACE('',#26971,26.);
#23698=CYLINDRICAL_SURFACE('',#26972,26.);
#23699=CYLINDRICAL_SURFACE('',#26973,26.);
#23700=CYLINDRICAL_SURFACE('',#26974,26.);
#23701=CYLINDRICAL_SURFACE('',#26975,26.);
#23702=CYLINDRICAL_SURFACE('',#26976,26.);
#23703=CYLINDRICAL_SURFACE('',#26977,26.);
#23704=CYLINDRICAL_SURFACE('',#26978,26.);
#23705=CYLINDRICAL_SURFACE('',#26979,26.);
#23706=CYLINDRICAL_SURFACE('',#26980,26.);
#23707=CYLINDRICAL_SURFACE('',#26981,26.);
#23708=CYLINDRICAL_SURFACE('',#26982,26.);
#23709=CYLINDRICAL_SURFACE('',#26983,26.);
#23710=CYLINDRICAL_SURFACE('',#26984,26.);
#23711=CYLINDRICAL_SURFACE('',#26985,26.);
#23712=CYLINDRICAL_SURFACE('',#26986,26.);
#23713=CYLINDRICAL_SURFACE('',#26987,26.);
#23714=CYLINDRICAL_SURFACE('',#26988,26.);
#23715=CYLINDRICAL_SURFACE('',#26989,26.);
#23716=CYLINDRICAL_SURFACE('',#26990,26.);
#23717=CYLINDRICAL_SURFACE('',#26991,26.);
#23718=CYLINDRICAL_SURFACE('',#26992,26.);
#23719=CYLINDRICAL_SURFACE('',#26993,26.);
#23720=CYLINDRICAL_SURFACE('',#26994,0.5);
#23721=CYLINDRICAL_SURFACE('',#26996,0.5);
#23722=CYLINDRICAL_SURFACE('',#26997,21.4999999999992);
#23723=CYLINDRICAL_SURFACE('',#26999,7.);
#23724=CYLINDRICAL_SURFACE('',#27000,26.);
#23725=CYLINDRICAL_SURFACE('',#27002,16.);
#23726=CYLINDRICAL_SURFACE('',#27005,18.);
#23727=CYLINDRICAL_SURFACE('',#27018,7.);
#23728=CYLINDRICAL_SURFACE('',#27025,8.);
#23729=CYLINDRICAL_SURFACE('',#27027,15.);
#23730=CYLINDRICAL_SURFACE('',#27034,16.);
#23731=CYLINDRICAL_SURFACE('',#27036,5.);
#23732=CYLINDRICAL_SURFACE('',#27039,5.);
#23733=CYLINDRICAL_SURFACE('',#27042,5.);
#23734=CYLINDRICAL_SURFACE('',#27051,11.);
#23735=CYLINDRICAL_SURFACE('',#27052,8.);
#23736=CYLINDRICAL_SURFACE('',#27054,8.);
#23737=CYLINDRICAL_SURFACE('',#27062,20.);
#23738=CYLINDRICAL_SURFACE('',#27063,16.);
#23739=CYLINDRICAL_SURFACE('',#27067,16.);
#23740=CYLINDRICAL_SURFACE('',#27069,12.);
#23741=CYLINDRICAL_SURFACE('',#27071,70.);
#23742=CYLINDRICAL_SURFACE('',#27084,5.);
#23743=CYLINDRICAL_SURFACE('',#27087,7.);
#23744=CYLINDRICAL_SURFACE('',#27093,4.);
#23745=CYLINDRICAL_SURFACE('',#27100,5.);
#23746=CYLINDRICAL_SURFACE('',#27105,8.);
#23747=CYLINDRICAL_SURFACE('',#27108,5.);
#23748=CYLINDRICAL_SURFACE('',#27116,4.);
#23749=CYLINDRICAL_SURFACE('',#27118,8.);
#23750=CYLINDRICAL_SURFACE('',#27122,5.);
#23751=CYLINDRICAL_SURFACE('',#27125,10.);
#23752=CYLINDRICAL_SURFACE('',#27131,8.);
#23753=CYLINDRICAL_SURFACE('',#27134,11.);
#23754=CYLINDRICAL_SURFACE('',#27140,16.);
#23755=CYLINDRICAL_SURFACE('',#27143,20.);
#23756=CYLINDRICAL_SURFACE('',#27154,7.);
#23757=CYLINDRICAL_SURFACE('',#27156,11.);
#23758=CYLINDRICAL_SURFACE('',#27165,15.);
#23759=CYLINDRICAL_SURFACE('',#27167,20.);
#23760=CYLINDRICAL_SURFACE('',#27171,2.);
#23761=CYLINDRICAL_SURFACE('',#27177,2.942);
#23762=CYLINDRICAL_SURFACE('',#27179,2.942);
#23763=CYLINDRICAL_SURFACE('',#27180,2.942);
#23764=CYLINDRICAL_SURFACE('',#27181,2.942);
#23765=CYLINDRICAL_SURFACE('',#27182,2.942);
#23766=CYLINDRICAL_SURFACE('',#27183,2.942);
#23767=CYLINDRICAL_SURFACE('',#27184,2.942);
#23768=CYLINDRICAL_SURFACE('',#27185,2.942);
#23769=CYLINDRICAL_SURFACE('',#27186,2.942);
#23770=CYLINDRICAL_SURFACE('',#27187,2.942);
#23771=CYLINDRICAL_SURFACE('',#27188,2.942);
#23772=CYLINDRICAL_SURFACE('',#27189,2.942);
#23773=CYLINDRICAL_SURFACE('',#27190,2.942);
#23774=CYLINDRICAL_SURFACE('',#27191,2.942);
#23775=CYLINDRICAL_SURFACE('',#27192,2.942);
#23776=CYLINDRICAL_SURFACE('',#27193,2.942);
#23777=CYLINDRICAL_SURFACE('',#27194,2.942);
#23778=CYLINDRICAL_SURFACE('',#27195,2.942);
#23779=CYLINDRICAL_SURFACE('',#27196,2.942);
#23780=CYLINDRICAL_SURFACE('',#27197,2.942);
#23781=CYLINDRICAL_SURFACE('',#27198,2.37175);
#23782=CYLINDRICAL_SURFACE('',#27200,2.37175);
#23783=CYLINDRICAL_SURFACE('',#27201,2.37175);
#23784=CYLINDRICAL_SURFACE('',#27202,2.37175);
#23785=CYLINDRICAL_SURFACE('',#27203,2.37175);
#23786=CYLINDRICAL_SURFACE('',#27204,2.37175);
#23787=CYLINDRICAL_SURFACE('',#27205,2.37175);
#23788=CYLINDRICAL_SURFACE('',#27206,2.37175);
#23789=CYLINDRICAL_SURFACE('',#27207,2.37175);
#23790=CYLINDRICAL_SURFACE('',#27208,2.37175);
#23791=CYLINDRICAL_SURFACE('',#27209,2.37175);
#23792=CYLINDRICAL_SURFACE('',#27210,2.37175);
#23793=CYLINDRICAL_SURFACE('',#27211,2.37175);
#23794=CYLINDRICAL_SURFACE('',#27212,2.37175);
#23795=CYLINDRICAL_SURFACE('',#27213,2.37175);
#23796=CYLINDRICAL_SURFACE('',#27214,2.37175);
#23797=CYLINDRICAL_SURFACE('',#27215,2.37175);
#23798=CYLINDRICAL_SURFACE('',#27216,2.37175);
#23799=CYLINDRICAL_SURFACE('',#27217,2.37175);
#23800=CYLINDRICAL_SURFACE('',#27218,2.37175);
#23801=CYLINDRICAL_SURFACE('',#27219,2.37175);
#23802=CYLINDRICAL_SURFACE('',#27221,2.942);
#23803=CYLINDRICAL_SURFACE('',#27232,5.);
#23804=ADVANCED_FACE('',(#1698),#23078,.F.);
#23805=ADVANCED_FACE('',(#1699),#23079,.F.);
#23806=ADVANCED_FACE('',(#1700),#23080,.F.);
#23807=ADVANCED_FACE('',(#1701),#23081,.F.);
#23808=ADVANCED_FACE('',(#1702),#23082,.F.);
#23809=ADVANCED_FACE('',(#1703),#23083,.F.);
#23810=ADVANCED_FACE('',(#1704),#23084,.F.);
#23811=ADVANCED_FACE('',(#1705),#23085,.F.);
#23812=ADVANCED_FACE('',(#1706),#23086,.F.);
#23813=ADVANCED_FACE('',(#1707),#23087,.F.);
#23814=ADVANCED_FACE('',(#1708),#23088,.F.);
#23815=ADVANCED_FACE('',(#1709),#23089,.F.);
#23816=ADVANCED_FACE('',(#1710),#23090,.F.);
#23817=ADVANCED_FACE('',(#1711),#23091,.F.);
#23818=ADVANCED_FACE('',(#1712),#23092,.F.);
#23819=ADVANCED_FACE('',(#1713),#23093,.F.);
#23820=ADVANCED_FACE('',(#1714),#23094,.F.);
#23821=ADVANCED_FACE('',(#1715),#23095,.F.);
#23822=ADVANCED_FACE('',(#1716),#23096,.F.);
#23823=ADVANCED_FACE('',(#1717),#23097,.F.);
#23824=ADVANCED_FACE('',(#1718),#23098,.F.);
#23825=ADVANCED_FACE('',(#1719),#23099,.F.);
#23826=ADVANCED_FACE('',(#1720),#23100,.F.);
#23827=ADVANCED_FACE('',(#1721),#23101,.F.);
#23828=ADVANCED_FACE('',(#1722),#23102,.F.);
#23829=ADVANCED_FACE('',(#1723),#23103,.F.);
#23830=ADVANCED_FACE('',(#1724),#23104,.F.);
#23831=ADVANCED_FACE('',(#1725),#23105,.F.);
#23832=ADVANCED_FACE('',(#1726),#23106,.F.);
#23833=ADVANCED_FACE('',(#1727),#23107,.F.);
#23834=ADVANCED_FACE('',(#1728),#23108,.F.);
#23835=ADVANCED_FACE('',(#1729),#23109,.F.);
#23836=ADVANCED_FACE('',(#1730),#23110,.F.);
#23837=ADVANCED_FACE('',(#1731),#23111,.F.);
#23838=ADVANCED_FACE('',(#1732),#23112,.F.);
#23839=ADVANCED_FACE('',(#1733),#23113,.F.);
#23840=ADVANCED_FACE('',(#1734),#23114,.F.);
#23841=ADVANCED_FACE('',(#1735),#23115,.F.);
#23842=ADVANCED_FACE('',(#1736),#23116,.F.);
#23843=ADVANCED_FACE('',(#1737),#23117,.F.);
#23844=ADVANCED_FACE('',(#1738),#23118,.F.);
#23845=ADVANCED_FACE('',(#1739),#23119,.F.);
#23846=ADVANCED_FACE('',(#1740),#23120,.F.);
#23847=ADVANCED_FACE('',(#1741),#23121,.F.);
#23848=ADVANCED_FACE('',(#1742),#23122,.F.);
#23849=ADVANCED_FACE('',(#1743),#23123,.F.);
#23850=ADVANCED_FACE('',(#1744),#23124,.F.);
#23851=ADVANCED_FACE('',(#1745),#23125,.F.);
#23852=ADVANCED_FACE('',(#1746),#23126,.F.);
#23853=ADVANCED_FACE('',(#1747),#23127,.F.);
#23854=ADVANCED_FACE('',(#1748),#23128,.F.);
#23855=ADVANCED_FACE('',(#1749),#23129,.F.);
#23856=ADVANCED_FACE('',(#1750),#23130,.F.);
#23857=ADVANCED_FACE('',(#1751),#23131,.F.);
#23858=ADVANCED_FACE('',(#1752),#23132,.F.);
#23859=ADVANCED_FACE('',(#1753),#23133,.F.);
#23860=ADVANCED_FACE('',(#1754),#23134,.F.);
#23861=ADVANCED_FACE('',(#1755),#23135,.F.);
#23862=ADVANCED_FACE('',(#1756),#23136,.F.);
#23863=ADVANCED_FACE('',(#1757),#23137,.F.);
#23864=ADVANCED_FACE('',(#1758),#23138,.F.);
#23865=ADVANCED_FACE('',(#1759),#23139,.F.);
#23866=ADVANCED_FACE('',(#1760),#23140,.F.);
#23867=ADVANCED_FACE('',(#1761),#23141,.F.);
#23868=ADVANCED_FACE('',(#1762),#23142,.F.);
#23869=ADVANCED_FACE('',(#1763),#23143,.F.);
#23870=ADVANCED_FACE('',(#1764),#23144,.F.);
#23871=ADVANCED_FACE('',(#1765),#23145,.F.);
#23872=ADVANCED_FACE('',(#1766),#23146,.F.);
#23873=ADVANCED_FACE('',(#1767),#23147,.F.);
#23874=ADVANCED_FACE('',(#1768),#23148,.F.);
#23875=ADVANCED_FACE('',(#1769),#23149,.F.);
#23876=ADVANCED_FACE('',(#1770),#23150,.F.);
#23877=ADVANCED_FACE('',(#1771),#23151,.F.);
#23878=ADVANCED_FACE('',(#1772),#23152,.F.);
#23879=ADVANCED_FACE('',(#1773),#23153,.F.);
#23880=ADVANCED_FACE('',(#1774),#23154,.F.);
#23881=ADVANCED_FACE('',(#1775),#23155,.F.);
#23882=ADVANCED_FACE('',(#1776),#23156,.F.);
#23883=ADVANCED_FACE('',(#1777),#23157,.F.);
#23884=ADVANCED_FACE('',(#1778),#23158,.F.);
#23885=ADVANCED_FACE('',(#1779),#23159,.F.);
#23886=ADVANCED_FACE('',(#1780),#23160,.F.);
#23887=ADVANCED_FACE('',(#1781),#23161,.F.);
#23888=ADVANCED_FACE('',(#1782),#23162,.F.);
#23889=ADVANCED_FACE('',(#1783),#23163,.F.);
#23890=ADVANCED_FACE('',(#1784),#23164,.F.);
#23891=ADVANCED_FACE('',(#1785),#23165,.F.);
#23892=ADVANCED_FACE('',(#1786),#23166,.F.);
#23893=ADVANCED_FACE('',(#1787),#23167,.F.);
#23894=ADVANCED_FACE('',(#1788),#23168,.F.);
#23895=ADVANCED_FACE('',(#1789),#23169,.F.);
#23896=ADVANCED_FACE('',(#1790),#23170,.F.);
#23897=ADVANCED_FACE('',(#1791),#23171,.F.);
#23898=ADVANCED_FACE('',(#1792),#23172,.F.);
#23899=ADVANCED_FACE('',(#1793),#23173,.F.);
#23900=ADVANCED_FACE('',(#1794),#23174,.F.);
#23901=ADVANCED_FACE('',(#1795),#23175,.F.);
#23902=ADVANCED_FACE('',(#1796),#23176,.F.);
#23903=ADVANCED_FACE('',(#1797),#23177,.F.);
#23904=ADVANCED_FACE('',(#1798),#23178,.F.);
#23905=ADVANCED_FACE('',(#1799),#23179,.F.);
#23906=ADVANCED_FACE('',(#1800),#23180,.F.);
#23907=ADVANCED_FACE('',(#1801),#23181,.F.);
#23908=ADVANCED_FACE('',(#1802),#23182,.F.);
#23909=ADVANCED_FACE('',(#1803),#23183,.F.);
#23910=ADVANCED_FACE('',(#1804),#23184,.F.);
#23911=ADVANCED_FACE('',(#1805),#23185,.F.);
#23912=ADVANCED_FACE('',(#1806),#23186,.F.);
#23913=ADVANCED_FACE('',(#1807),#23187,.F.);
#23914=ADVANCED_FACE('',(#1808),#23188,.F.);
#23915=ADVANCED_FACE('',(#1809),#23189,.F.);
#23916=ADVANCED_FACE('',(#1810),#23190,.F.);
#23917=ADVANCED_FACE('',(#1811),#23191,.F.);
#23918=ADVANCED_FACE('',(#1812),#23192,.F.);
#23919=ADVANCED_FACE('',(#1813),#23193,.F.);
#23920=ADVANCED_FACE('',(#1814),#23194,.F.);
#23921=ADVANCED_FACE('',(#1815),#23195,.F.);
#23922=ADVANCED_FACE('',(#1816),#23196,.F.);
#23923=ADVANCED_FACE('',(#1817),#23197,.F.);
#23924=ADVANCED_FACE('',(#1818),#23198,.F.);
#23925=ADVANCED_FACE('',(#1819),#23199,.F.);
#23926=ADVANCED_FACE('',(#1820),#23200,.F.);
#23927=ADVANCED_FACE('',(#1821),#23201,.F.);
#23928=ADVANCED_FACE('',(#1822),#23202,.F.);
#23929=ADVANCED_FACE('',(#1823),#23203,.F.);
#23930=ADVANCED_FACE('',(#1824),#23204,.F.);
#23931=ADVANCED_FACE('',(#1825),#23205,.F.);
#23932=ADVANCED_FACE('',(#1826),#23206,.F.);
#23933=ADVANCED_FACE('',(#1827),#23207,.F.);
#23934=ADVANCED_FACE('',(#1828),#23208,.F.);
#23935=ADVANCED_FACE('',(#1829),#23209,.F.);
#23936=ADVANCED_FACE('',(#1830),#23210,.F.);
#23937=ADVANCED_FACE('',(#1831),#23211,.F.);
#23938=ADVANCED_FACE('',(#1832),#23212,.F.);
#23939=ADVANCED_FACE('',(#1833),#23213,.F.);
#23940=ADVANCED_FACE('',(#1834),#23214,.F.);
#23941=ADVANCED_FACE('',(#1835),#23215,.F.);
#23942=ADVANCED_FACE('',(#1836),#23216,.F.);
#23943=ADVANCED_FACE('',(#1837),#23217,.F.);
#23944=ADVANCED_FACE('',(#1838),#23218,.F.);
#23945=ADVANCED_FACE('',(#1839),#23219,.F.);
#23946=ADVANCED_FACE('',(#1840),#23220,.F.);
#23947=ADVANCED_FACE('',(#1841),#23221,.F.);
#23948=ADVANCED_FACE('',(#1842),#23222,.F.);
#23949=ADVANCED_FACE('',(#1843),#23223,.F.);
#23950=ADVANCED_FACE('',(#1844),#23224,.F.);
#23951=ADVANCED_FACE('',(#1845),#23225,.F.);
#23952=ADVANCED_FACE('',(#1846),#23226,.F.);
#23953=ADVANCED_FACE('',(#1847),#23227,.F.);
#23954=ADVANCED_FACE('',(#1848),#23228,.F.);
#23955=ADVANCED_FACE('',(#1849),#23229,.F.);
#23956=ADVANCED_FACE('',(#1850),#23230,.F.);
#23957=ADVANCED_FACE('',(#1851),#23231,.F.);
#23958=ADVANCED_FACE('',(#1852),#23232,.F.);
#23959=ADVANCED_FACE('',(#1853),#23233,.F.);
#23960=ADVANCED_FACE('',(#1854),#23234,.F.);
#23961=ADVANCED_FACE('',(#1855),#23235,.F.);
#23962=ADVANCED_FACE('',(#1856),#23236,.F.);
#23963=ADVANCED_FACE('',(#1857),#23237,.F.);
#23964=ADVANCED_FACE('',(#1858),#23238,.F.);
#23965=ADVANCED_FACE('',(#1859),#23239,.F.);
#23966=ADVANCED_FACE('',(#1860),#23240,.F.);
#23967=ADVANCED_FACE('',(#1861),#23241,.F.);
#23968=ADVANCED_FACE('',(#1862),#23242,.F.);
#23969=ADVANCED_FACE('',(#1863),#23243,.F.);
#23970=ADVANCED_FACE('',(#1864),#23244,.F.);
#23971=ADVANCED_FACE('',(#1865),#23245,.F.);
#23972=ADVANCED_FACE('',(#1866),#23246,.F.);
#23973=ADVANCED_FACE('',(#1867),#23247,.F.);
#23974=ADVANCED_FACE('',(#1868),#23248,.F.);
#23975=ADVANCED_FACE('',(#1869),#23249,.F.);
#23976=ADVANCED_FACE('',(#1870),#23250,.F.);
#23977=ADVANCED_FACE('',(#1871),#23251,.F.);
#23978=ADVANCED_FACE('',(#1872),#23252,.F.);
#23979=ADVANCED_FACE('',(#1873),#23253,.F.);
#23980=ADVANCED_FACE('',(#1874),#23254,.F.);
#23981=ADVANCED_FACE('',(#1875),#23255,.F.);
#23982=ADVANCED_FACE('',(#1876),#23256,.F.);
#23983=ADVANCED_FACE('',(#1877),#23257,.F.);
#23984=ADVANCED_FACE('',(#1878),#23258,.F.);
#23985=ADVANCED_FACE('',(#1879),#23259,.F.);
#23986=ADVANCED_FACE('',(#1880),#23260,.F.);
#23987=ADVANCED_FACE('',(#1881),#23261,.F.);
#23988=ADVANCED_FACE('',(#1882),#23262,.F.);
#23989=ADVANCED_FACE('',(#1883),#23263,.F.);
#23990=ADVANCED_FACE('',(#1884),#23264,.F.);
#23991=ADVANCED_FACE('',(#1885),#23265,.F.);
#23992=ADVANCED_FACE('',(#1886),#23266,.F.);
#23993=ADVANCED_FACE('',(#1887),#23267,.F.);
#23994=ADVANCED_FACE('',(#1888),#23268,.F.);
#23995=ADVANCED_FACE('',(#1889),#23269,.F.);
#23996=ADVANCED_FACE('',(#1890),#23270,.F.);
#23997=ADVANCED_FACE('',(#1891),#23271,.F.);
#23998=ADVANCED_FACE('',(#1892),#23272,.F.);
#23999=ADVANCED_FACE('',(#1893),#23273,.F.);
#24000=ADVANCED_FACE('',(#1894),#23274,.F.);
#24001=ADVANCED_FACE('',(#1895),#23275,.F.);
#24002=ADVANCED_FACE('',(#1896),#23276,.F.);
#24003=ADVANCED_FACE('',(#1897),#23277,.F.);
#24004=ADVANCED_FACE('',(#1898),#23278,.F.);
#24005=ADVANCED_FACE('',(#1899),#23279,.F.);
#24006=ADVANCED_FACE('',(#1900),#23280,.F.);
#24007=ADVANCED_FACE('',(#1901),#23281,.F.);
#24008=ADVANCED_FACE('',(#1902),#23282,.F.);
#24009=ADVANCED_FACE('',(#1903),#23283,.F.);
#24010=ADVANCED_FACE('',(#1904),#23284,.F.);
#24011=ADVANCED_FACE('',(#1905),#23285,.F.);
#24012=ADVANCED_FACE('',(#1906),#23286,.F.);
#24013=ADVANCED_FACE('',(#1907),#23287,.F.);
#24014=ADVANCED_FACE('',(#1908),#23288,.F.);
#24015=ADVANCED_FACE('',(#1909),#23289,.F.);
#24016=ADVANCED_FACE('',(#1910),#23290,.F.);
#24017=ADVANCED_FACE('',(#1911),#23291,.F.);
#24018=ADVANCED_FACE('',(#1912),#23292,.F.);
#24019=ADVANCED_FACE('',(#1913),#23293,.F.);
#24020=ADVANCED_FACE('',(#1914),#23294,.F.);
#24021=ADVANCED_FACE('',(#1915),#23295,.F.);
#24022=ADVANCED_FACE('',(#1916),#23296,.F.);
#24023=ADVANCED_FACE('',(#1917),#23297,.F.);
#24024=ADVANCED_FACE('',(#1918),#23298,.F.);
#24025=ADVANCED_FACE('',(#1919),#23299,.F.);
#24026=ADVANCED_FACE('',(#1920),#23300,.F.);
#24027=ADVANCED_FACE('',(#1921),#23301,.F.);
#24028=ADVANCED_FACE('',(#1922),#23302,.F.);
#24029=ADVANCED_FACE('',(#1923),#23303,.F.);
#24030=ADVANCED_FACE('',(#1924),#23304,.F.);
#24031=ADVANCED_FACE('',(#1925),#23305,.F.);
#24032=ADVANCED_FACE('',(#1926),#23306,.F.);
#24033=ADVANCED_FACE('',(#1927),#23307,.F.);
#24034=ADVANCED_FACE('',(#1928),#23308,.F.);
#24035=ADVANCED_FACE('',(#1929),#23309,.F.);
#24036=ADVANCED_FACE('',(#1930),#23310,.F.);
#24037=ADVANCED_FACE('',(#1931),#23311,.F.);
#24038=ADVANCED_FACE('',(#1932),#23312,.F.);
#24039=ADVANCED_FACE('',(#1933),#23313,.F.);
#24040=ADVANCED_FACE('',(#1934),#23314,.F.);
#24041=ADVANCED_FACE('',(#1935),#23315,.F.);
#24042=ADVANCED_FACE('',(#1936),#23316,.F.);
#24043=ADVANCED_FACE('',(#1937),#23317,.F.);
#24044=ADVANCED_FACE('',(#1938),#23318,.F.);
#24045=ADVANCED_FACE('',(#1939),#23319,.F.);
#24046=ADVANCED_FACE('',(#1940),#23320,.F.);
#24047=ADVANCED_FACE('',(#1941),#23321,.F.);
#24048=ADVANCED_FACE('',(#1942),#23322,.F.);
#24049=ADVANCED_FACE('',(#1943),#23323,.F.);
#24050=ADVANCED_FACE('',(#1944),#23324,.F.);
#24051=ADVANCED_FACE('',(#1945),#23325,.F.);
#24052=ADVANCED_FACE('',(#1946),#23326,.F.);
#24053=ADVANCED_FACE('',(#1947),#23327,.F.);
#24054=ADVANCED_FACE('',(#1948),#23328,.F.);
#24055=ADVANCED_FACE('',(#1949),#23329,.F.);
#24056=ADVANCED_FACE('',(#1950),#1480,.T.);
#24057=ADVANCED_FACE('',(#1951),#23330,.F.);
#24058=ADVANCED_FACE('',(#1952),#1318,.F.);
#24059=ADVANCED_FACE('',(#1953),#1319,.F.);
#24060=ADVANCED_FACE('',(#1954),#23331,.F.);
#24061=ADVANCED_FACE('',(#1955),#1481,.T.);
#24062=ADVANCED_FACE('',(#1956),#23332,.F.);
#24063=ADVANCED_FACE('',(#1957),#1320,.F.);
#24064=ADVANCED_FACE('',(#1958),#1321,.F.);
#24065=ADVANCED_FACE('',(#1959),#23333,.F.);
#24066=ADVANCED_FACE('',(#1960),#1482,.T.);
#24067=ADVANCED_FACE('',(#1961),#23334,.F.);
#24068=ADVANCED_FACE('',(#1962),#1322,.F.);
#24069=ADVANCED_FACE('',(#1963),#1323,.F.);
#24070=ADVANCED_FACE('',(#1964),#23335,.F.);
#24071=ADVANCED_FACE('',(#1965),#1483,.T.);
#24072=ADVANCED_FACE('',(#1966),#23336,.F.);
#24073=ADVANCED_FACE('',(#1967),#1324,.F.);
#24074=ADVANCED_FACE('',(#1968),#1325,.F.);
#24075=ADVANCED_FACE('',(#1969),#23337,.F.);
#24076=ADVANCED_FACE('',(#1970),#1484,.T.);
#24077=ADVANCED_FACE('',(#1971),#23338,.F.);
#24078=ADVANCED_FACE('',(#1972),#1326,.F.);
#24079=ADVANCED_FACE('',(#1973),#1327,.F.);
#24080=ADVANCED_FACE('',(#1974),#23339,.F.);
#24081=ADVANCED_FACE('',(#1975),#1485,.T.);
#24082=ADVANCED_FACE('',(#1976),#23340,.F.);
#24083=ADVANCED_FACE('',(#1977),#1328,.F.);
#24084=ADVANCED_FACE('',(#1978),#1329,.F.);
#24085=ADVANCED_FACE('',(#1979),#23341,.F.);
#24086=ADVANCED_FACE('',(#1980),#1486,.T.);
#24087=ADVANCED_FACE('',(#1981),#23342,.F.);
#24088=ADVANCED_FACE('',(#1982),#1330,.F.);
#24089=ADVANCED_FACE('',(#1983),#1331,.F.);
#24090=ADVANCED_FACE('',(#1984),#23343,.F.);
#24091=ADVANCED_FACE('',(#1985),#1487,.T.);
#24092=ADVANCED_FACE('',(#1986),#23344,.F.);
#24093=ADVANCED_FACE('',(#1987),#1332,.F.);
#24094=ADVANCED_FACE('',(#1988),#1333,.F.);
#24095=ADVANCED_FACE('',(#1989),#23345,.F.);
#24096=ADVANCED_FACE('',(#1990),#1488,.F.);
#24097=ADVANCED_FACE('',(#1991),#1489,.F.);
#24098=ADVANCED_FACE('',(#1992),#1490,.F.);
#24099=ADVANCED_FACE('',(#1993),#1491,.F.);
#24100=ADVANCED_FACE('',(#1994),#1492,.F.);
#24101=ADVANCED_FACE('',(#1995),#1493,.F.);
#24102=ADVANCED_FACE('',(#1996),#1494,.F.);
#24103=ADVANCED_FACE('',(#1997),#1495,.F.);
#24104=ADVANCED_FACE('',(#1998),#23346,.F.);
#24105=ADVANCED_FACE('',(#1999),#23347,.F.);
#24106=ADVANCED_FACE('',(#2000),#23348,.F.);
#24107=ADVANCED_FACE('',(#2001),#23349,.F.);
#24108=ADVANCED_FACE('',(#2002),#23350,.F.);
#24109=ADVANCED_FACE('',(#2003,#1203),#1496,.F.);
#24110=ADVANCED_FACE('',(#2004,#1204,#1205,#1206,#1207,#1208,#1209,#1210,
#1211,#1212),#23351,.F.);
#24111=ADVANCED_FACE('',(#2005,#1213,#1214,#1215,#1216,#1217,#1218,#1219,
#1220,#1221),#23352,.T.);
#24112=ADVANCED_FACE('',(#2006,#1222,#1223,#1224,#1225,#1226,#1227,#1228,
#1229,#1230),#1497,.T.);
#24113=ADVANCED_FACE('',(#2007,#1231,#1232,#1233,#1234,#1235),#1498,.T.);
#24114=ADVANCED_FACE('',(#2008),#23353,.F.);
#24115=ADVANCED_FACE('',(#2009),#23354,.T.);
#24116=ADVANCED_FACE('',(#2010,#1236),#1499,.T.);
#24117=ADVANCED_FACE('',(#2011,#1237,#1238,#1239,#1240,#1241),#1500,.F.);
#24118=ADVANCED_FACE('',(#2012),#23355,.F.);
#24119=ADVANCED_FACE('',(#2013),#1501,.F.);
#24120=ADVANCED_FACE('',(#2014),#23356,.F.);
#24121=ADVANCED_FACE('',(#2015),#1502,.F.);
#24122=ADVANCED_FACE('',(#2016),#23357,.F.);
#24123=ADVANCED_FACE('',(#2017),#1503,.F.);
#24124=ADVANCED_FACE('',(#2018),#23358,.F.);
#24125=ADVANCED_FACE('',(#2019),#1504,.F.);
#24126=ADVANCED_FACE('',(#2020),#23359,.F.);
#24127=ADVANCED_FACE('',(#2021,#1242,#1243,#1244),#23360,.T.);
#24128=ADVANCED_FACE('',(#2022,#1245),#1505,.T.);
#24129=ADVANCED_FACE('',(#2023,#1246),#1506,.F.);
#24130=ADVANCED_FACE('',(#2024),#23361,.F.);
#24131=ADVANCED_FACE('',(#2025),#23362,.F.);
#24132=ADVANCED_FACE('',(#2026),#23363,.F.);
#24133=ADVANCED_FACE('',(#2027),#23364,.F.);
#24134=ADVANCED_FACE('',(#2028),#23365,.F.);
#24135=ADVANCED_FACE('',(#2029),#23366,.F.);
#24136=ADVANCED_FACE('',(#2030),#23367,.F.);
#24137=ADVANCED_FACE('',(#2031),#23368,.F.);
#24138=ADVANCED_FACE('',(#2032),#23369,.F.);
#24139=ADVANCED_FACE('',(#2033),#23370,.T.);
#24140=ADVANCED_FACE('',(#2034,#1247,#1248,#1249,#1250,#1251,#1252,#1253,
#1254,#1255),#1507,.T.);
#24141=ADVANCED_FACE('',(#2035,#1256,#1257,#1258,#1259,#1260,#1261,#1262,
#1263,#1264),#1508,.F.);
#24142=ADVANCED_FACE('',(#2036),#1509,.F.);
#24143=ADVANCED_FACE('',(#2037),#1510,.F.);
#24144=ADVANCED_FACE('',(#2038),#1511,.F.);
#24145=ADVANCED_FACE('',(#2039),#1512,.F.);
#24146=ADVANCED_FACE('',(#2040),#1513,.F.);
#24147=ADVANCED_FACE('',(#2041),#23371,.T.);
#24148=ADVANCED_FACE('',(#2042,#1265),#1514,.F.);
#24149=ADVANCED_FACE('',(#2043,#1266),#1515,.F.);
#24150=ADVANCED_FACE('',(#2044),#23372,.T.);
#24151=ADVANCED_FACE('',(#2045),#23373,.T.);
#24152=ADVANCED_FACE('',(#2046,#1267),#1516,.F.);
#24153=ADVANCED_FACE('',(#2047,#1268),#1517,.F.);
#24154=ADVANCED_FACE('',(#2048),#23374,.T.);
#24155=ADVANCED_FACE('',(#2049,#1269),#1518,.T.);
#24156=ADVANCED_FACE('',(#2050,#1270),#1519,.F.);
#24157=ADVANCED_FACE('',(#2051),#23375,.T.);
#24158=ADVANCED_FACE('',(#2052),#23376,.T.);
#24159=ADVANCED_FACE('',(#2053,#1271),#1520,.T.);
#24160=ADVANCED_FACE('',(#2054,#1272),#1521,.F.);
#24161=ADVANCED_FACE('',(#2055),#23377,.T.);
#24162=ADVANCED_FACE('',(#2056),#23378,.T.);
#24163=ADVANCED_FACE('',(#2057,#1273),#23379,.T.);
#24164=ADVANCED_FACE('',(#2058),#1522,.T.);
#24165=ADVANCED_FACE('',(#2059),#23380,.T.);
#24166=ADVANCED_FACE('',(#2060),#1523,.F.);
#24167=ADVANCED_FACE('',(#2061),#23381,.T.);
#24168=ADVANCED_FACE('',(#2062,#1274),#1524,.T.);
#24169=ADVANCED_FACE('',(#2063,#1275),#1525,.F.);
#24170=ADVANCED_FACE('',(#2064),#23382,.F.);
#24171=ADVANCED_FACE('',(#2065),#1526,.F.);
#24172=ADVANCED_FACE('',(#2066),#23383,.F.);
#24173=ADVANCED_FACE('',(#2067),#1527,.F.);
#24174=ADVANCED_FACE('',(#2068),#23384,.F.);
#24175=ADVANCED_FACE('',(#2069),#1528,.F.);
#24176=ADVANCED_FACE('',(#2070),#23385,.F.);
#24177=ADVANCED_FACE('',(#2071),#1529,.F.);
#24178=ADVANCED_FACE('',(#2072),#1334,.T.);
#24179=ADVANCED_FACE('',(#2073),#883,.F.);
#24180=ADVANCED_FACE('',(#2074),#1335,.T.);
#24181=ADVANCED_FACE('',(#2075),#23386,.F.);
#24182=ADVANCED_FACE('',(#2076),#1336,.T.);
#24183=ADVANCED_FACE('',(#2077),#884,.F.);
#24184=ADVANCED_FACE('',(#2078),#1337,.T.);
#24185=ADVANCED_FACE('',(#2079),#23387,.F.);
#24186=ADVANCED_FACE('',(#2080),#1338,.T.);
#24187=ADVANCED_FACE('',(#2081),#885,.F.);
#24188=ADVANCED_FACE('',(#2082),#1339,.T.);
#24189=ADVANCED_FACE('',(#2083),#23388,.F.);
#24190=ADVANCED_FACE('',(#2084),#1340,.T.);
#24191=ADVANCED_FACE('',(#2085),#886,.F.);
#24192=ADVANCED_FACE('',(#2086),#1341,.T.);
#24193=ADVANCED_FACE('',(#2087),#23389,.F.);
#24194=ADVANCED_FACE('',(#2088),#1342,.T.);
#24195=ADVANCED_FACE('',(#2089),#887,.F.);
#24196=ADVANCED_FACE('',(#2090),#1343,.T.);
#24197=ADVANCED_FACE('',(#2091),#23390,.F.);
#24198=ADVANCED_FACE('',(#2092),#1344,.T.);
#24199=ADVANCED_FACE('',(#2093),#888,.F.);
#24200=ADVANCED_FACE('',(#2094),#1345,.T.);
#24201=ADVANCED_FACE('',(#2095),#23391,.F.);
#24202=ADVANCED_FACE('',(#2096),#1346,.T.);
#24203=ADVANCED_FACE('',(#2097),#889,.F.);
#24204=ADVANCED_FACE('',(#2098),#1347,.T.);
#24205=ADVANCED_FACE('',(#2099),#23392,.F.);
#24206=ADVANCED_FACE('',(#2100),#1348,.T.);
#24207=ADVANCED_FACE('',(#2101),#890,.F.);
#24208=ADVANCED_FACE('',(#2102),#1349,.T.);
#24209=ADVANCED_FACE('',(#2103),#23393,.F.);
#24210=ADVANCED_FACE('',(#2104),#1350,.T.);
#24211=ADVANCED_FACE('',(#2105),#891,.F.);
#24212=ADVANCED_FACE('',(#2106),#1351,.T.);
#24213=ADVANCED_FACE('',(#2107),#23394,.F.);
#24214=ADVANCED_FACE('',(#2108),#1352,.T.);
#24215=ADVANCED_FACE('',(#2109),#892,.F.);
#24216=ADVANCED_FACE('',(#2110),#1353,.T.);
#24217=ADVANCED_FACE('',(#2111),#23395,.F.);
#24218=ADVANCED_FACE('',(#2112),#1354,.T.);
#24219=ADVANCED_FACE('',(#2113),#893,.F.);
#24220=ADVANCED_FACE('',(#2114),#1355,.T.);
#24221=ADVANCED_FACE('',(#2115),#23396,.F.);
#24222=ADVANCED_FACE('',(#2116),#1356,.T.);
#24223=ADVANCED_FACE('',(#2117),#894,.F.);
#24224=ADVANCED_FACE('',(#2118),#1357,.T.);
#24225=ADVANCED_FACE('',(#2119),#23397,.F.);
#24226=ADVANCED_FACE('',(#2120),#1358,.T.);
#24227=ADVANCED_FACE('',(#2121),#895,.F.);
#24228=ADVANCED_FACE('',(#2122),#1359,.T.);
#24229=ADVANCED_FACE('',(#2123),#23398,.F.);
#24230=ADVANCED_FACE('',(#2124),#1360,.T.);
#24231=ADVANCED_FACE('',(#2125),#896,.F.);
#24232=ADVANCED_FACE('',(#2126),#1361,.T.);
#24233=ADVANCED_FACE('',(#2127),#23399,.F.);
#24234=ADVANCED_FACE('',(#2128),#1362,.T.);
#24235=ADVANCED_FACE('',(#2129),#897,.F.);
#24236=ADVANCED_FACE('',(#2130),#1363,.T.);
#24237=ADVANCED_FACE('',(#2131),#23400,.F.);
#24238=ADVANCED_FACE('',(#2132),#1364,.T.);
#24239=ADVANCED_FACE('',(#2133),#898,.F.);
#24240=ADVANCED_FACE('',(#2134),#1365,.T.);
#24241=ADVANCED_FACE('',(#2135),#23401,.F.);
#24242=ADVANCED_FACE('',(#2136),#1366,.T.);
#24243=ADVANCED_FACE('',(#2137),#899,.F.);
#24244=ADVANCED_FACE('',(#2138),#1367,.T.);
#24245=ADVANCED_FACE('',(#2139),#23402,.F.);
#24246=ADVANCED_FACE('',(#2140),#1368,.T.);
#24247=ADVANCED_FACE('',(#2141),#900,.F.);
#24248=ADVANCED_FACE('',(#2142),#1369,.T.);
#24249=ADVANCED_FACE('',(#2143),#23403,.F.);
#24250=ADVANCED_FACE('',(#2144),#1370,.T.);
#24251=ADVANCED_FACE('',(#2145),#901,.F.);
#24252=ADVANCED_FACE('',(#2146),#1371,.T.);
#24253=ADVANCED_FACE('',(#2147),#23404,.F.);
#24254=ADVANCED_FACE('',(#2148),#1372,.T.);
#24255=ADVANCED_FACE('',(#2149),#902,.F.);
#24256=ADVANCED_FACE('',(#2150),#1373,.T.);
#24257=ADVANCED_FACE('',(#2151),#23405,.F.);
#24258=ADVANCED_FACE('',(#2152),#1374,.T.);
#24259=ADVANCED_FACE('',(#2153),#903,.F.);
#24260=ADVANCED_FACE('',(#2154),#1375,.T.);
#24261=ADVANCED_FACE('',(#2155),#23406,.F.);
#24262=ADVANCED_FACE('',(#2156),#1376,.T.);
#24263=ADVANCED_FACE('',(#2157),#904,.F.);
#24264=ADVANCED_FACE('',(#2158),#1377,.T.);
#24265=ADVANCED_FACE('',(#2159),#23407,.F.);
#24266=ADVANCED_FACE('',(#2160),#1378,.T.);
#24267=ADVANCED_FACE('',(#2161),#905,.F.);
#24268=ADVANCED_FACE('',(#2162),#1379,.T.);
#24269=ADVANCED_FACE('',(#2163),#23408,.F.);
#24270=ADVANCED_FACE('',(#2164),#1380,.T.);
#24271=ADVANCED_FACE('',(#2165),#906,.F.);
#24272=ADVANCED_FACE('',(#2166),#1381,.T.);
#24273=ADVANCED_FACE('',(#2167),#23409,.F.);
#24274=ADVANCED_FACE('',(#2168),#1382,.T.);
#24275=ADVANCED_FACE('',(#2169),#907,.F.);
#24276=ADVANCED_FACE('',(#2170),#1383,.T.);
#24277=ADVANCED_FACE('',(#2171),#23410,.F.);
#24278=ADVANCED_FACE('',(#2172),#1384,.T.);
#24279=ADVANCED_FACE('',(#2173),#908,.F.);
#24280=ADVANCED_FACE('',(#2174),#1385,.T.);
#24281=ADVANCED_FACE('',(#2175),#23411,.F.);
#24282=ADVANCED_FACE('',(#2176),#1386,.T.);
#24283=ADVANCED_FACE('',(#2177),#909,.F.);
#24284=ADVANCED_FACE('',(#2178),#1387,.T.);
#24285=ADVANCED_FACE('',(#2179),#23412,.F.);
#24286=ADVANCED_FACE('',(#2180),#1388,.T.);
#24287=ADVANCED_FACE('',(#2181),#910,.F.);
#24288=ADVANCED_FACE('',(#2182),#1389,.T.);
#24289=ADVANCED_FACE('',(#2183),#23413,.F.);
#24290=ADVANCED_FACE('',(#2184),#1390,.T.);
#24291=ADVANCED_FACE('',(#2185),#911,.F.);
#24292=ADVANCED_FACE('',(#2186),#1391,.T.);
#24293=ADVANCED_FACE('',(#2187),#23414,.F.);
#24294=ADVANCED_FACE('',(#2188),#1392,.T.);
#24295=ADVANCED_FACE('',(#2189),#912,.F.);
#24296=ADVANCED_FACE('',(#2190),#1393,.T.);
#24297=ADVANCED_FACE('',(#2191),#23415,.F.);
#24298=ADVANCED_FACE('',(#2192),#1394,.T.);
#24299=ADVANCED_FACE('',(#2193),#913,.F.);
#24300=ADVANCED_FACE('',(#2194),#1395,.T.);
#24301=ADVANCED_FACE('',(#2195),#23416,.F.);
#24302=ADVANCED_FACE('',(#2196),#1396,.T.);
#24303=ADVANCED_FACE('',(#2197),#914,.F.);
#24304=ADVANCED_FACE('',(#2198),#1397,.T.);
#24305=ADVANCED_FACE('',(#2199),#23417,.F.);
#24306=ADVANCED_FACE('',(#2200),#1398,.T.);
#24307=ADVANCED_FACE('',(#2201),#915,.F.);
#24308=ADVANCED_FACE('',(#2202),#1399,.T.);
#24309=ADVANCED_FACE('',(#2203),#23418,.F.);
#24310=ADVANCED_FACE('',(#2204),#1400,.T.);
#24311=ADVANCED_FACE('',(#2205),#916,.F.);
#24312=ADVANCED_FACE('',(#2206),#1401,.T.);
#24313=ADVANCED_FACE('',(#2207),#23419,.F.);
#24314=ADVANCED_FACE('',(#2208),#1402,.T.);
#24315=ADVANCED_FACE('',(#2209),#917,.F.);
#24316=ADVANCED_FACE('',(#2210),#1403,.T.);
#24317=ADVANCED_FACE('',(#2211),#23420,.F.);
#24318=ADVANCED_FACE('',(#2212),#1404,.T.);
#24319=ADVANCED_FACE('',(#2213),#918,.F.);
#24320=ADVANCED_FACE('',(#2214),#1405,.T.);
#24321=ADVANCED_FACE('',(#2215),#23421,.F.);
#24322=ADVANCED_FACE('',(#2216),#1406,.T.);
#24323=ADVANCED_FACE('',(#2217),#919,.F.);
#24324=ADVANCED_FACE('',(#2218),#1407,.T.);
#24325=ADVANCED_FACE('',(#2219),#23422,.F.);
#24326=ADVANCED_FACE('',(#2220),#1408,.T.);
#24327=ADVANCED_FACE('',(#2221),#920,.F.);
#24328=ADVANCED_FACE('',(#2222),#1409,.T.);
#24329=ADVANCED_FACE('',(#2223),#23423,.F.);
#24330=ADVANCED_FACE('',(#2224),#1410,.T.);
#24331=ADVANCED_FACE('',(#2225),#921,.F.);
#24332=ADVANCED_FACE('',(#2226),#1411,.T.);
#24333=ADVANCED_FACE('',(#2227),#23424,.F.);
#24334=ADVANCED_FACE('',(#2228),#1412,.T.);
#24335=ADVANCED_FACE('',(#2229),#922,.F.);
#24336=ADVANCED_FACE('',(#2230),#1413,.T.);
#24337=ADVANCED_FACE('',(#2231),#23425,.F.);
#24338=ADVANCED_FACE('',(#2232),#1414,.T.);
#24339=ADVANCED_FACE('',(#2233),#923,.F.);
#24340=ADVANCED_FACE('',(#2234),#1415,.T.);
#24341=ADVANCED_FACE('',(#2235),#23426,.F.);
#24342=ADVANCED_FACE('',(#2236),#1416,.T.);
#24343=ADVANCED_FACE('',(#2237),#924,.F.);
#24344=ADVANCED_FACE('',(#2238),#1417,.T.);
#24345=ADVANCED_FACE('',(#2239),#23427,.F.);
#24346=ADVANCED_FACE('',(#2240),#1418,.T.);
#24347=ADVANCED_FACE('',(#2241),#925,.F.);
#24348=ADVANCED_FACE('',(#2242),#1419,.T.);
#24349=ADVANCED_FACE('',(#2243),#23428,.F.);
#24350=ADVANCED_FACE('',(#2244),#1420,.T.);
#24351=ADVANCED_FACE('',(#2245),#926,.F.);
#24352=ADVANCED_FACE('',(#2246),#1421,.T.);
#24353=ADVANCED_FACE('',(#2247),#23429,.F.);
#24354=ADVANCED_FACE('',(#2248),#1422,.T.);
#24355=ADVANCED_FACE('',(#2249),#927,.F.);
#24356=ADVANCED_FACE('',(#2250),#1423,.T.);
#24357=ADVANCED_FACE('',(#2251),#23430,.F.);
#24358=ADVANCED_FACE('',(#2252),#1424,.T.);
#24359=ADVANCED_FACE('',(#2253),#928,.F.);
#24360=ADVANCED_FACE('',(#2254),#1425,.T.);
#24361=ADVANCED_FACE('',(#2255),#23431,.F.);
#24362=ADVANCED_FACE('',(#2256),#1426,.T.);
#24363=ADVANCED_FACE('',(#2257),#929,.F.);
#24364=ADVANCED_FACE('',(#2258),#1427,.T.);
#24365=ADVANCED_FACE('',(#2259),#23432,.F.);
#24366=ADVANCED_FACE('',(#2260),#1428,.T.);
#24367=ADVANCED_FACE('',(#2261),#930,.F.);
#24368=ADVANCED_FACE('',(#2262),#1429,.T.);
#24369=ADVANCED_FACE('',(#2263),#23433,.F.);
#24370=ADVANCED_FACE('',(#2264),#1430,.T.);
#24371=ADVANCED_FACE('',(#2265),#931,.F.);
#24372=ADVANCED_FACE('',(#2266),#1431,.T.);
#24373=ADVANCED_FACE('',(#2267),#23434,.F.);
#24374=ADVANCED_FACE('',(#2268),#1432,.T.);
#24375=ADVANCED_FACE('',(#2269),#932,.F.);
#24376=ADVANCED_FACE('',(#2270),#1433,.T.);
#24377=ADVANCED_FACE('',(#2271),#23435,.F.);
#24378=ADVANCED_FACE('',(#2272),#1434,.T.);
#24379=ADVANCED_FACE('',(#2273),#933,.F.);
#24380=ADVANCED_FACE('',(#2274),#1435,.T.);
#24381=ADVANCED_FACE('',(#2275),#23436,.F.);
#24382=ADVANCED_FACE('',(#2276),#1436,.T.);
#24383=ADVANCED_FACE('',(#2277),#934,.F.);
#24384=ADVANCED_FACE('',(#2278),#1437,.T.);
#24385=ADVANCED_FACE('',(#2279),#23437,.F.);
#24386=ADVANCED_FACE('',(#2280),#1438,.T.);
#24387=ADVANCED_FACE('',(#2281),#935,.F.);
#24388=ADVANCED_FACE('',(#2282),#1439,.T.);
#24389=ADVANCED_FACE('',(#2283),#23438,.F.);
#24390=ADVANCED_FACE('',(#2284),#1440,.T.);
#24391=ADVANCED_FACE('',(#2285),#936,.F.);
#24392=ADVANCED_FACE('',(#2286),#1441,.T.);
#24393=ADVANCED_FACE('',(#2287),#23439,.F.);
#24394=ADVANCED_FACE('',(#2288),#1442,.T.);
#24395=ADVANCED_FACE('',(#2289),#937,.F.);
#24396=ADVANCED_FACE('',(#2290),#1443,.T.);
#24397=ADVANCED_FACE('',(#2291),#23440,.F.);
#24398=ADVANCED_FACE('',(#2292),#1444,.T.);
#24399=ADVANCED_FACE('',(#2293),#938,.F.);
#24400=ADVANCED_FACE('',(#2294),#1445,.T.);
#24401=ADVANCED_FACE('',(#2295),#23441,.F.);
#24402=ADVANCED_FACE('',(#2296),#1446,.T.);
#24403=ADVANCED_FACE('',(#2297),#939,.F.);
#24404=ADVANCED_FACE('',(#2298),#1447,.T.);
#24405=ADVANCED_FACE('',(#2299),#23442,.F.);
#24406=ADVANCED_FACE('',(#2300),#1448,.T.);
#24407=ADVANCED_FACE('',(#2301),#940,.F.);
#24408=ADVANCED_FACE('',(#2302),#1449,.T.);
#24409=ADVANCED_FACE('',(#2303),#23443,.F.);
#24410=ADVANCED_FACE('',(#2304),#1450,.T.);
#24411=ADVANCED_FACE('',(#2305),#941,.F.);
#24412=ADVANCED_FACE('',(#2306),#1451,.T.);
#24413=ADVANCED_FACE('',(#2307),#23444,.F.);
#24414=ADVANCED_FACE('',(#2308),#1452,.T.);
#24415=ADVANCED_FACE('',(#2309),#942,.F.);
#24416=ADVANCED_FACE('',(#2310),#1453,.T.);
#24417=ADVANCED_FACE('',(#2311),#23445,.F.);
#24418=ADVANCED_FACE('',(#2312),#1454,.T.);
#24419=ADVANCED_FACE('',(#2313),#943,.F.);
#24420=ADVANCED_FACE('',(#2314),#1455,.T.);
#24421=ADVANCED_FACE('',(#2315),#23446,.F.);
#24422=ADVANCED_FACE('',(#2316),#1456,.T.);
#24423=ADVANCED_FACE('',(#2317),#944,.F.);
#24424=ADVANCED_FACE('',(#2318),#1457,.T.);
#24425=ADVANCED_FACE('',(#2319),#23447,.F.);
#24426=ADVANCED_FACE('',(#2320),#1458,.T.);
#24427=ADVANCED_FACE('',(#2321),#945,.F.);
#24428=ADVANCED_FACE('',(#2322),#1459,.T.);
#24429=ADVANCED_FACE('',(#2323),#23448,.F.);
#24430=ADVANCED_FACE('',(#2324),#1460,.T.);
#24431=ADVANCED_FACE('',(#2325),#946,.F.);
#24432=ADVANCED_FACE('',(#2326),#1461,.T.);
#24433=ADVANCED_FACE('',(#2327),#23449,.F.);
#24434=ADVANCED_FACE('',(#2328),#1462,.T.);
#24435=ADVANCED_FACE('',(#2329),#947,.F.);
#24436=ADVANCED_FACE('',(#2330),#1463,.T.);
#24437=ADVANCED_FACE('',(#2331),#23450,.F.);
#24438=ADVANCED_FACE('',(#2332),#1464,.T.);
#24439=ADVANCED_FACE('',(#2333),#948,.F.);
#24440=ADVANCED_FACE('',(#2334),#1465,.T.);
#24441=ADVANCED_FACE('',(#2335),#23451,.F.);
#24442=ADVANCED_FACE('',(#2336),#1466,.T.);
#24443=ADVANCED_FACE('',(#2337),#949,.F.);
#24444=ADVANCED_FACE('',(#2338),#1467,.T.);
#24445=ADVANCED_FACE('',(#2339),#23452,.F.);
#24446=ADVANCED_FACE('',(#2340),#1468,.T.);
#24447=ADVANCED_FACE('',(#2341),#950,.F.);
#24448=ADVANCED_FACE('',(#2342),#1469,.T.);
#24449=ADVANCED_FACE('',(#2343),#23453,.F.);
#24450=ADVANCED_FACE('',(#2344),#1470,.T.);
#24451=ADVANCED_FACE('',(#2345),#951,.F.);
#24452=ADVANCED_FACE('',(#2346),#1471,.T.);
#24453=ADVANCED_FACE('',(#2347),#23454,.F.);
#24454=ADVANCED_FACE('',(#2348),#1472,.T.);
#24455=ADVANCED_FACE('',(#2349),#952,.F.);
#24456=ADVANCED_FACE('',(#2350),#1473,.T.);
#24457=ADVANCED_FACE('',(#2351),#23455,.F.);
#24458=ADVANCED_FACE('',(#2352),#1474,.T.);
#24459=ADVANCED_FACE('',(#2353),#953,.F.);
#24460=ADVANCED_FACE('',(#2354),#1475,.T.);
#24461=ADVANCED_FACE('',(#2355),#23456,.F.);
#24462=ADVANCED_FACE('',(#2356),#954,.F.);
#24463=ADVANCED_FACE('',(#2357),#955,.F.);
#24464=ADVANCED_FACE('',(#2358),#956,.F.);
#24465=ADVANCED_FACE('',(#2359),#957,.F.);
#24466=ADVANCED_FACE('',(#2360),#958,.F.);
#24467=ADVANCED_FACE('',(#2361),#959,.F.);
#24468=ADVANCED_FACE('',(#2362),#960,.F.);
#24469=ADVANCED_FACE('',(#2363),#961,.F.);
#24470=ADVANCED_FACE('',(#2364),#962,.F.);
#24471=ADVANCED_FACE('',(#2365),#963,.F.);
#24472=ADVANCED_FACE('',(#2366),#964,.F.);
#24473=ADVANCED_FACE('',(#2367),#965,.F.);
#24474=ADVANCED_FACE('',(#2368),#966,.F.);
#24475=ADVANCED_FACE('',(#2369),#967,.F.);
#24476=ADVANCED_FACE('',(#2370),#968,.F.);
#24477=ADVANCED_FACE('',(#2371),#969,.F.);
#24478=ADVANCED_FACE('',(#2372),#970,.F.);
#24479=ADVANCED_FACE('',(#2373),#971,.F.);
#24480=ADVANCED_FACE('',(#2374),#972,.F.);
#24481=ADVANCED_FACE('',(#2375),#973,.F.);
#24482=ADVANCED_FACE('',(#2376),#974,.F.);
#24483=ADVANCED_FACE('',(#2377),#975,.F.);
#24484=ADVANCED_FACE('',(#2378),#976,.F.);
#24485=ADVANCED_FACE('',(#2379),#977,.F.);
#24486=ADVANCED_FACE('',(#2380),#978,.F.);
#24487=ADVANCED_FACE('',(#2381),#979,.F.);
#24488=ADVANCED_FACE('',(#2382),#980,.F.);
#24489=ADVANCED_FACE('',(#2383),#981,.F.);
#24490=ADVANCED_FACE('',(#2384),#982,.F.);
#24491=ADVANCED_FACE('',(#2385),#983,.F.);
#24492=ADVANCED_FACE('',(#2386),#984,.F.);
#24493=ADVANCED_FACE('',(#2387),#985,.F.);
#24494=ADVANCED_FACE('',(#2388),#986,.F.);
#24495=ADVANCED_FACE('',(#2389),#987,.F.);
#24496=ADVANCED_FACE('',(#2390),#988,.F.);
#24497=ADVANCED_FACE('',(#2391),#989,.F.);
#24498=ADVANCED_FACE('',(#2392),#990,.F.);
#24499=ADVANCED_FACE('',(#2393),#991,.F.);
#24500=ADVANCED_FACE('',(#2394),#992,.F.);
#24501=ADVANCED_FACE('',(#2395),#993,.F.);
#24502=ADVANCED_FACE('',(#2396),#994,.F.);
#24503=ADVANCED_FACE('',(#2397),#995,.F.);
#24504=ADVANCED_FACE('',(#2398),#996,.F.);
#24505=ADVANCED_FACE('',(#2399),#997,.F.);
#24506=ADVANCED_FACE('',(#2400),#998,.F.);
#24507=ADVANCED_FACE('',(#2401),#999,.F.);
#24508=ADVANCED_FACE('',(#2402),#1000,.F.);
#24509=ADVANCED_FACE('',(#2403),#1001,.F.);
#24510=ADVANCED_FACE('',(#2404),#1002,.F.);
#24511=ADVANCED_FACE('',(#2405),#1003,.F.);
#24512=ADVANCED_FACE('',(#2406),#1004,.F.);
#24513=ADVANCED_FACE('',(#2407),#1005,.F.);
#24514=ADVANCED_FACE('',(#2408),#1006,.F.);
#24515=ADVANCED_FACE('',(#2409),#1007,.F.);
#24516=ADVANCED_FACE('',(#2410),#1008,.F.);
#24517=ADVANCED_FACE('',(#2411),#1009,.F.);
#24518=ADVANCED_FACE('',(#2412),#1010,.F.);
#24519=ADVANCED_FACE('',(#2413),#1011,.F.);
#24520=ADVANCED_FACE('',(#2414),#1012,.F.);
#24521=ADVANCED_FACE('',(#2415),#1013,.F.);
#24522=ADVANCED_FACE('',(#2416),#1014,.F.);
#24523=ADVANCED_FACE('',(#2417),#1015,.F.);
#24524=ADVANCED_FACE('',(#2418),#1016,.F.);
#24525=ADVANCED_FACE('',(#2419),#1017,.F.);
#24526=ADVANCED_FACE('',(#2420),#1018,.F.);
#24527=ADVANCED_FACE('',(#2421),#1019,.F.);
#24528=ADVANCED_FACE('',(#2422),#1020,.F.);
#24529=ADVANCED_FACE('',(#2423),#1021,.F.);
#24530=ADVANCED_FACE('',(#2424),#1022,.F.);
#24531=ADVANCED_FACE('',(#2425),#1023,.F.);
#24532=ADVANCED_FACE('',(#2426),#1024,.F.);
#24533=ADVANCED_FACE('',(#2427),#23457,.F.);
#24534=ADVANCED_FACE('',(#2428),#23458,.F.);
#24535=ADVANCED_FACE('',(#2429),#23459,.F.);
#24536=ADVANCED_FACE('',(#2430),#23460,.F.);
#24537=ADVANCED_FACE('',(#2431),#23461,.F.);
#24538=ADVANCED_FACE('',(#2432),#23462,.F.);
#24539=ADVANCED_FACE('',(#2433),#23463,.F.);
#24540=ADVANCED_FACE('',(#2434),#23464,.F.);
#24541=ADVANCED_FACE('',(#2435),#23465,.F.);
#24542=ADVANCED_FACE('',(#2436),#23466,.F.);
#24543=ADVANCED_FACE('',(#2437),#23467,.F.);
#24544=ADVANCED_FACE('',(#2438),#23468,.F.);
#24545=ADVANCED_FACE('',(#2439),#23469,.F.);
#24546=ADVANCED_FACE('',(#2440),#23470,.F.);
#24547=ADVANCED_FACE('',(#2441),#23471,.F.);
#24548=ADVANCED_FACE('',(#2442),#23472,.F.);
#24549=ADVANCED_FACE('',(#2443),#23473,.F.);
#24550=ADVANCED_FACE('',(#2444),#23474,.F.);
#24551=ADVANCED_FACE('',(#2445),#23475,.F.);
#24552=ADVANCED_FACE('',(#2446),#23476,.F.);
#24553=ADVANCED_FACE('',(#2447),#23477,.F.);
#24554=ADVANCED_FACE('',(#2448),#23478,.F.);
#24555=ADVANCED_FACE('',(#2449),#23479,.F.);
#24556=ADVANCED_FACE('',(#2450),#23480,.F.);
#24557=ADVANCED_FACE('',(#2451),#23481,.F.);
#24558=ADVANCED_FACE('',(#2452),#23482,.F.);
#24559=ADVANCED_FACE('',(#2453),#23483,.F.);
#24560=ADVANCED_FACE('',(#2454),#23484,.F.);
#24561=ADVANCED_FACE('',(#2455),#23485,.F.);
#24562=ADVANCED_FACE('',(#2456),#23486,.F.);
#24563=ADVANCED_FACE('',(#2457),#23487,.F.);
#24564=ADVANCED_FACE('',(#2458),#23488,.F.);
#24565=ADVANCED_FACE('',(#2459),#23489,.F.);
#24566=ADVANCED_FACE('',(#2460),#23490,.F.);
#24567=ADVANCED_FACE('',(#2461),#23491,.F.);
#24568=ADVANCED_FACE('',(#2462),#23492,.F.);
#24569=ADVANCED_FACE('',(#2463),#23493,.F.);
#24570=ADVANCED_FACE('',(#2464),#23494,.F.);
#24571=ADVANCED_FACE('',(#2465),#23495,.F.);
#24572=ADVANCED_FACE('',(#2466),#23496,.F.);
#24573=ADVANCED_FACE('',(#2467),#23497,.F.);
#24574=ADVANCED_FACE('',(#2468),#23498,.F.);
#24575=ADVANCED_FACE('',(#2469),#23499,.F.);
#24576=ADVANCED_FACE('',(#2470),#23500,.F.);
#24577=ADVANCED_FACE('',(#2471),#23501,.F.);
#24578=ADVANCED_FACE('',(#2472),#23502,.F.);
#24579=ADVANCED_FACE('',(#2473),#23503,.F.);
#24580=ADVANCED_FACE('',(#2474),#23504,.F.);
#24581=ADVANCED_FACE('',(#2475),#23505,.F.);
#24582=ADVANCED_FACE('',(#2476),#23506,.F.);
#24583=ADVANCED_FACE('',(#2477),#23507,.F.);
#24584=ADVANCED_FACE('',(#2478),#23508,.F.);
#24585=ADVANCED_FACE('',(#2479),#23509,.F.);
#24586=ADVANCED_FACE('',(#2480),#23510,.F.);
#24587=ADVANCED_FACE('',(#2481),#23511,.F.);
#24588=ADVANCED_FACE('',(#2482),#23512,.F.);
#24589=ADVANCED_FACE('',(#2483),#23513,.F.);
#24590=ADVANCED_FACE('',(#2484),#23514,.F.);
#24591=ADVANCED_FACE('',(#2485),#23515,.F.);
#24592=ADVANCED_FACE('',(#2486),#23516,.F.);
#24593=ADVANCED_FACE('',(#2487),#23517,.F.);
#24594=ADVANCED_FACE('',(#2488),#23518,.F.);
#24595=ADVANCED_FACE('',(#2489),#23519,.F.);
#24596=ADVANCED_FACE('',(#2490),#23520,.F.);
#24597=ADVANCED_FACE('',(#2491),#23521,.F.);
#24598=ADVANCED_FACE('',(#2492),#23522,.F.);
#24599=ADVANCED_FACE('',(#2493),#23523,.F.);
#24600=ADVANCED_FACE('',(#2494),#23524,.F.);
#24601=ADVANCED_FACE('',(#2495),#23525,.F.);
#24602=ADVANCED_FACE('',(#2496),#23526,.F.);
#24603=ADVANCED_FACE('',(#2497),#23527,.F.);
#24604=ADVANCED_FACE('',(#2498),#1476,.T.);
#24605=ADVANCED_FACE('',(#2499),#1025,.F.);
#24606=ADVANCED_FACE('',(#2500),#1477,.T.);
#24607=ADVANCED_FACE('',(#2501),#23528,.F.);
#24608=ADVANCED_FACE('',(#2502),#1026,.F.);
#24609=ADVANCED_FACE('',(#2503,#1276),#1530,.T.);
#24610=ADVANCED_FACE('',(#2504),#23529,.F.);
#24611=ADVANCED_FACE('',(#2505,#1277,#1278,#1279),#23530,.T.);
#24612=ADVANCED_FACE('',(#2506,#1280),#1531,.F.);
#24613=ADVANCED_FACE('',(#2507),#1532,.F.);
#24614=ADVANCED_FACE('',(#2508),#1533,.F.);
#24615=ADVANCED_FACE('',(#2509),#1534,.F.);
#24616=ADVANCED_FACE('',(#2510),#23531,.F.);
#24617=ADVANCED_FACE('',(#2511,#1281),#1535,.T.);
#24618=ADVANCED_FACE('',(#2512),#23532,.F.);
#24619=ADVANCED_FACE('',(#2513),#1536,.F.);
#24620=ADVANCED_FACE('',(#2514),#23533,.F.);
#24621=ADVANCED_FACE('',(#2515),#23534,.T.);
#24622=ADVANCED_FACE('',(#2516),#23535,.F.);
#24623=ADVANCED_FACE('',(#2517),#1537,.F.);
#24624=ADVANCED_FACE('',(#2518),#23536,.F.);
#24625=ADVANCED_FACE('',(#2519),#23537,.T.);
#24626=ADVANCED_FACE('',(#2520),#23538,.F.);
#24627=ADVANCED_FACE('',(#2521),#1538,.F.);
#24628=ADVANCED_FACE('',(#2522),#23539,.F.);
#24629=ADVANCED_FACE('',(#2523),#23540,.T.);
#24630=ADVANCED_FACE('',(#2524),#23541,.F.);
#24631=ADVANCED_FACE('',(#2525),#1539,.F.);
#24632=ADVANCED_FACE('',(#2526),#23542,.F.);
#24633=ADVANCED_FACE('',(#2527),#23543,.T.);
#24634=ADVANCED_FACE('',(#2528),#23544,.F.);
#24635=ADVANCED_FACE('',(#2529),#1540,.F.);
#24636=ADVANCED_FACE('',(#2530),#23545,.F.);
#24637=ADVANCED_FACE('',(#2531),#23546,.T.);
#24638=ADVANCED_FACE('',(#2532),#23547,.F.);
#24639=ADVANCED_FACE('',(#2533),#1541,.F.);
#24640=ADVANCED_FACE('',(#2534),#23548,.F.);
#24641=ADVANCED_FACE('',(#2535),#23549,.T.);
#24642=ADVANCED_FACE('',(#2536),#23550,.F.);
#24643=ADVANCED_FACE('',(#2537),#1542,.F.);
#24644=ADVANCED_FACE('',(#2538),#23551,.F.);
#24645=ADVANCED_FACE('',(#2539),#23552,.T.);
#24646=ADVANCED_FACE('',(#2540),#23553,.F.);
#24647=ADVANCED_FACE('',(#2541),#1543,.F.);
#24648=ADVANCED_FACE('',(#2542),#23554,.F.);
#24649=ADVANCED_FACE('',(#2543),#23555,.T.);
#24650=ADVANCED_FACE('',(#2544),#23556,.F.);
#24651=ADVANCED_FACE('',(#2545),#1544,.F.);
#24652=ADVANCED_FACE('',(#2546),#23557,.F.);
#24653=ADVANCED_FACE('',(#2547),#23558,.T.);
#24654=ADVANCED_FACE('',(#2548),#23559,.F.);
#24655=ADVANCED_FACE('',(#2549),#1545,.F.);
#24656=ADVANCED_FACE('',(#2550),#23560,.F.);
#24657=ADVANCED_FACE('',(#2551),#23561,.T.);
#24658=ADVANCED_FACE('',(#2552),#23562,.F.);
#24659=ADVANCED_FACE('',(#2553),#1546,.F.);
#24660=ADVANCED_FACE('',(#2554),#23563,.F.);
#24661=ADVANCED_FACE('',(#2555),#23564,.T.);
#24662=ADVANCED_FACE('',(#2556),#23565,.F.);
#24663=ADVANCED_FACE('',(#2557),#1547,.F.);
#24664=ADVANCED_FACE('',(#2558),#23566,.F.);
#24665=ADVANCED_FACE('',(#2559),#23567,.T.);
#24666=ADVANCED_FACE('',(#2560),#23568,.F.);
#24667=ADVANCED_FACE('',(#2561),#1548,.F.);
#24668=ADVANCED_FACE('',(#2562),#23569,.F.);
#24669=ADVANCED_FACE('',(#2563),#23570,.T.);
#24670=ADVANCED_FACE('',(#2564),#23571,.F.);
#24671=ADVANCED_FACE('',(#2565),#1549,.F.);
#24672=ADVANCED_FACE('',(#2566),#23572,.F.);
#24673=ADVANCED_FACE('',(#2567),#23573,.T.);
#24674=ADVANCED_FACE('',(#2568),#23574,.F.);
#24675=ADVANCED_FACE('',(#2569),#1550,.F.);
#24676=ADVANCED_FACE('',(#2570),#23575,.F.);
#24677=ADVANCED_FACE('',(#2571),#23576,.T.);
#24678=ADVANCED_FACE('',(#2572),#23577,.F.);
#24679=ADVANCED_FACE('',(#2573),#1551,.F.);
#24680=ADVANCED_FACE('',(#2574),#23578,.F.);
#24681=ADVANCED_FACE('',(#2575),#23579,.T.);
#24682=ADVANCED_FACE('',(#2576),#23580,.F.);
#24683=ADVANCED_FACE('',(#2577),#1552,.F.);
#24684=ADVANCED_FACE('',(#2578),#23581,.F.);
#24685=ADVANCED_FACE('',(#2579),#23582,.T.);
#24686=ADVANCED_FACE('',(#2580),#23583,.F.);
#24687=ADVANCED_FACE('',(#2581),#1553,.F.);
#24688=ADVANCED_FACE('',(#2582),#23584,.F.);
#24689=ADVANCED_FACE('',(#2583),#23585,.T.);
#24690=ADVANCED_FACE('',(#2584),#23586,.F.);
#24691=ADVANCED_FACE('',(#2585),#1554,.F.);
#24692=ADVANCED_FACE('',(#2586),#23587,.F.);
#24693=ADVANCED_FACE('',(#2587),#23588,.T.);
#24694=ADVANCED_FACE('',(#2588),#23589,.F.);
#24695=ADVANCED_FACE('',(#2589),#1555,.F.);
#24696=ADVANCED_FACE('',(#2590),#23590,.F.);
#24697=ADVANCED_FACE('',(#2591),#23591,.T.);
#24698=ADVANCED_FACE('',(#2592),#23592,.F.);
#24699=ADVANCED_FACE('',(#2593),#1556,.F.);
#24700=ADVANCED_FACE('',(#2594),#23593,.F.);
#24701=ADVANCED_FACE('',(#2595),#23594,.T.);
#24702=ADVANCED_FACE('',(#2596),#23595,.F.);
#24703=ADVANCED_FACE('',(#2597),#1557,.F.);
#24704=ADVANCED_FACE('',(#2598),#23596,.F.);
#24705=ADVANCED_FACE('',(#2599),#23597,.T.);
#24706=ADVANCED_FACE('',(#2600),#23598,.F.);
#24707=ADVANCED_FACE('',(#2601),#1558,.F.);
#24708=ADVANCED_FACE('',(#2602),#23599,.F.);
#24709=ADVANCED_FACE('',(#2603),#23600,.T.);
#24710=ADVANCED_FACE('',(#2604),#1559,.F.);
#24711=ADVANCED_FACE('',(#2605),#1027,.F.);
#24712=ADVANCED_FACE('',(#2606),#1028,.F.);
#24713=ADVANCED_FACE('',(#2607),#1560,.F.);
#24714=ADVANCED_FACE('',(#2608),#1029,.F.);
#24715=ADVANCED_FACE('',(#2609),#1030,.F.);
#24716=ADVANCED_FACE('',(#2610),#1561,.F.);
#24717=ADVANCED_FACE('',(#2611),#1031,.F.);
#24718=ADVANCED_FACE('',(#2612),#1032,.F.);
#24719=ADVANCED_FACE('',(#2613),#1562,.F.);
#24720=ADVANCED_FACE('',(#2614),#1033,.F.);
#24721=ADVANCED_FACE('',(#2615),#1034,.F.);
#24722=ADVANCED_FACE('',(#2616),#1563,.F.);
#24723=ADVANCED_FACE('',(#2617),#1035,.F.);
#24724=ADVANCED_FACE('',(#2618),#1036,.F.);
#24725=ADVANCED_FACE('',(#2619),#1564,.F.);
#24726=ADVANCED_FACE('',(#2620),#1037,.F.);
#24727=ADVANCED_FACE('',(#2621),#1038,.F.);
#24728=ADVANCED_FACE('',(#2622),#1565,.F.);
#24729=ADVANCED_FACE('',(#2623),#1039,.F.);
#24730=ADVANCED_FACE('',(#2624),#1040,.F.);
#24731=ADVANCED_FACE('',(#2625),#1566,.F.);
#24732=ADVANCED_FACE('',(#2626),#1041,.F.);
#24733=ADVANCED_FACE('',(#2627),#1042,.F.);
#24734=ADVANCED_FACE('',(#2628),#1567,.F.);
#24735=ADVANCED_FACE('',(#2629),#1043,.F.);
#24736=ADVANCED_FACE('',(#2630),#1044,.F.);
#24737=ADVANCED_FACE('',(#2631),#1568,.F.);
#24738=ADVANCED_FACE('',(#2632),#1045,.F.);
#24739=ADVANCED_FACE('',(#2633),#1046,.F.);
#24740=ADVANCED_FACE('',(#2634),#1569,.F.);
#24741=ADVANCED_FACE('',(#2635),#1047,.F.);
#24742=ADVANCED_FACE('',(#2636),#1048,.F.);
#24743=ADVANCED_FACE('',(#2637),#1570,.F.);
#24744=ADVANCED_FACE('',(#2638),#1049,.F.);
#24745=ADVANCED_FACE('',(#2639),#1050,.F.);
#24746=ADVANCED_FACE('',(#2640),#1571,.F.);
#24747=ADVANCED_FACE('',(#2641),#1051,.F.);
#24748=ADVANCED_FACE('',(#2642),#1052,.F.);
#24749=ADVANCED_FACE('',(#2643),#1572,.F.);
#24750=ADVANCED_FACE('',(#2644),#1053,.F.);
#24751=ADVANCED_FACE('',(#2645),#1054,.F.);
#24752=ADVANCED_FACE('',(#2646),#1573,.F.);
#24753=ADVANCED_FACE('',(#2647),#1055,.F.);
#24754=ADVANCED_FACE('',(#2648),#1056,.F.);
#24755=ADVANCED_FACE('',(#2649),#1574,.F.);
#24756=ADVANCED_FACE('',(#2650),#1057,.F.);
#24757=ADVANCED_FACE('',(#2651),#1058,.F.);
#24758=ADVANCED_FACE('',(#2652),#1575,.F.);
#24759=ADVANCED_FACE('',(#2653),#1059,.F.);
#24760=ADVANCED_FACE('',(#2654),#1060,.F.);
#24761=ADVANCED_FACE('',(#2655),#1576,.F.);
#24762=ADVANCED_FACE('',(#2656),#1061,.F.);
#24763=ADVANCED_FACE('',(#2657),#1062,.F.);
#24764=ADVANCED_FACE('',(#2658),#1577,.F.);
#24765=ADVANCED_FACE('',(#2659),#1063,.F.);
#24766=ADVANCED_FACE('',(#2660),#1064,.F.);
#24767=ADVANCED_FACE('',(#2661),#1578,.F.);
#24768=ADVANCED_FACE('',(#2662),#1065,.F.);
#24769=ADVANCED_FACE('',(#2663),#1066,.F.);
#24770=ADVANCED_FACE('',(#2664),#1579,.F.);
#24771=ADVANCED_FACE('',(#2665),#1067,.F.);
#24772=ADVANCED_FACE('',(#2666),#1068,.F.);
#24773=ADVANCED_FACE('',(#2667),#1580,.F.);
#24774=ADVANCED_FACE('',(#2668),#1069,.F.);
#24775=ADVANCED_FACE('',(#2669),#1070,.F.);
#24776=ADVANCED_FACE('',(#2670),#1581,.F.);
#24777=ADVANCED_FACE('',(#2671),#1071,.F.);
#24778=ADVANCED_FACE('',(#2672),#1072,.F.);
#24779=ADVANCED_FACE('',(#2673,#1282),#1582,.F.);
#24780=ADVANCED_FACE('',(#2674),#23601,.T.);
#24781=ADVANCED_FACE('',(#2675),#23602,.T.);
#24782=ADVANCED_FACE('',(#2676),#23603,.T.);
#24783=ADVANCED_FACE('',(#2677),#23604,.T.);
#24784=ADVANCED_FACE('',(#2678),#23605,.T.);
#24785=ADVANCED_FACE('',(#2679),#23606,.T.);
#24786=ADVANCED_FACE('',(#2680),#23607,.T.);
#24787=ADVANCED_FACE('',(#2681),#23608,.T.);
#24788=ADVANCED_FACE('',(#2682),#23609,.T.);
#24789=ADVANCED_FACE('',(#2683),#23610,.T.);
#24790=ADVANCED_FACE('',(#2684),#23611,.T.);
#24791=ADVANCED_FACE('',(#2685),#23612,.T.);
#24792=ADVANCED_FACE('',(#2686),#23613,.T.);
#24793=ADVANCED_FACE('',(#2687),#23614,.T.);
#24794=ADVANCED_FACE('',(#2688),#23615,.T.);
#24795=ADVANCED_FACE('',(#2689),#23616,.T.);
#24796=ADVANCED_FACE('',(#2690),#23617,.T.);
#24797=ADVANCED_FACE('',(#2691),#23618,.T.);
#24798=ADVANCED_FACE('',(#2692),#23619,.T.);
#24799=ADVANCED_FACE('',(#2693),#23620,.T.);
#24800=ADVANCED_FACE('',(#2694),#23621,.T.);
#24801=ADVANCED_FACE('',(#2695),#23622,.T.);
#24802=ADVANCED_FACE('',(#2696),#23623,.T.);
#24803=ADVANCED_FACE('',(#2697),#23624,.F.);
#24804=ADVANCED_FACE('',(#2698),#1583,.F.);
#24805=ADVANCED_FACE('',(#2699),#23625,.F.);
#24806=ADVANCED_FACE('',(#2700),#23626,.T.);
#24807=ADVANCED_FACE('',(#2701),#1584,.F.);
#24808=ADVANCED_FACE('',(#2702),#1073,.F.);
#24809=ADVANCED_FACE('',(#2703),#1074,.F.);
#24810=ADVANCED_FACE('',(#2704),#23627,.T.);
#24811=ADVANCED_FACE('',(#2705),#23628,.F.);
#24812=ADVANCED_FACE('',(#2706),#1585,.F.);
#24813=ADVANCED_FACE('',(#2707),#23629,.F.);
#24814=ADVANCED_FACE('',(#2708),#23630,.T.);
#24815=ADVANCED_FACE('',(#2709),#23631,.F.);
#24816=ADVANCED_FACE('',(#2710),#1586,.F.);
#24817=ADVANCED_FACE('',(#2711),#23632,.F.);
#24818=ADVANCED_FACE('',(#2712),#23633,.T.);
#24819=ADVANCED_FACE('',(#2713),#23634,.F.);
#24820=ADVANCED_FACE('',(#2714),#1587,.F.);
#24821=ADVANCED_FACE('',(#2715),#23635,.F.);
#24822=ADVANCED_FACE('',(#2716),#23636,.T.);
#24823=ADVANCED_FACE('',(#2717),#23637,.F.);
#24824=ADVANCED_FACE('',(#2718),#1588,.F.);
#24825=ADVANCED_FACE('',(#2719),#23638,.F.);
#24826=ADVANCED_FACE('',(#2720),#23639,.T.);
#24827=ADVANCED_FACE('',(#2721),#23640,.F.);
#24828=ADVANCED_FACE('',(#2722),#1589,.F.);
#24829=ADVANCED_FACE('',(#2723),#23641,.F.);
#24830=ADVANCED_FACE('',(#2724),#23642,.T.);
#24831=ADVANCED_FACE('',(#2725),#23643,.F.);
#24832=ADVANCED_FACE('',(#2726),#1590,.F.);
#24833=ADVANCED_FACE('',(#2727),#23644,.F.);
#24834=ADVANCED_FACE('',(#2728),#23645,.T.);
#24835=ADVANCED_FACE('',(#2729),#23646,.F.);
#24836=ADVANCED_FACE('',(#2730),#1591,.F.);
#24837=ADVANCED_FACE('',(#2731),#23647,.F.);
#24838=ADVANCED_FACE('',(#2732),#23648,.T.);
#24839=ADVANCED_FACE('',(#2733),#23649,.F.);
#24840=ADVANCED_FACE('',(#2734),#1592,.F.);
#24841=ADVANCED_FACE('',(#2735),#23650,.F.);
#24842=ADVANCED_FACE('',(#2736),#23651,.T.);
#24843=ADVANCED_FACE('',(#2737),#23652,.F.);
#24844=ADVANCED_FACE('',(#2738),#1593,.F.);
#24845=ADVANCED_FACE('',(#2739),#23653,.F.);
#24846=ADVANCED_FACE('',(#2740),#23654,.T.);
#24847=ADVANCED_FACE('',(#2741),#23655,.F.);
#24848=ADVANCED_FACE('',(#2742),#1594,.F.);
#24849=ADVANCED_FACE('',(#2743),#23656,.F.);
#24850=ADVANCED_FACE('',(#2744),#23657,.T.);
#24851=ADVANCED_FACE('',(#2745),#23658,.F.);
#24852=ADVANCED_FACE('',(#2746),#1595,.F.);
#24853=ADVANCED_FACE('',(#2747),#23659,.F.);
#24854=ADVANCED_FACE('',(#2748),#23660,.T.);
#24855=ADVANCED_FACE('',(#2749),#23661,.F.);
#24856=ADVANCED_FACE('',(#2750),#1596,.F.);
#24857=ADVANCED_FACE('',(#2751),#23662,.F.);
#24858=ADVANCED_FACE('',(#2752),#23663,.T.);
#24859=ADVANCED_FACE('',(#2753),#23664,.F.);
#24860=ADVANCED_FACE('',(#2754),#1597,.F.);
#24861=ADVANCED_FACE('',(#2755),#23665,.F.);
#24862=ADVANCED_FACE('',(#2756),#23666,.T.);
#24863=ADVANCED_FACE('',(#2757),#23667,.F.);
#24864=ADVANCED_FACE('',(#2758),#1598,.F.);
#24865=ADVANCED_FACE('',(#2759),#23668,.F.);
#24866=ADVANCED_FACE('',(#2760),#23669,.T.);
#24867=ADVANCED_FACE('',(#2761),#23670,.F.);
#24868=ADVANCED_FACE('',(#2762),#1599,.F.);
#24869=ADVANCED_FACE('',(#2763),#23671,.F.);
#24870=ADVANCED_FACE('',(#2764),#23672,.T.);
#24871=ADVANCED_FACE('',(#2765),#23673,.F.);
#24872=ADVANCED_FACE('',(#2766),#1600,.F.);
#24873=ADVANCED_FACE('',(#2767),#23674,.F.);
#24874=ADVANCED_FACE('',(#2768),#23675,.T.);
#24875=ADVANCED_FACE('',(#2769),#23676,.F.);
#24876=ADVANCED_FACE('',(#2770),#1601,.F.);
#24877=ADVANCED_FACE('',(#2771),#23677,.F.);
#24878=ADVANCED_FACE('',(#2772),#23678,.T.);
#24879=ADVANCED_FACE('',(#2773),#23679,.F.);
#24880=ADVANCED_FACE('',(#2774),#1602,.F.);
#24881=ADVANCED_FACE('',(#2775),#23680,.F.);
#24882=ADVANCED_FACE('',(#2776),#23681,.T.);
#24883=ADVANCED_FACE('',(#2777),#23682,.F.);
#24884=ADVANCED_FACE('',(#2778),#1603,.F.);
#24885=ADVANCED_FACE('',(#2779),#23683,.F.);
#24886=ADVANCED_FACE('',(#2780),#23684,.T.);
#24887=ADVANCED_FACE('',(#2781),#23685,.F.);
#24888=ADVANCED_FACE('',(#2782),#1604,.F.);
#24889=ADVANCED_FACE('',(#2783),#23686,.F.);
#24890=ADVANCED_FACE('',(#2784),#23687,.T.);
#24891=ADVANCED_FACE('',(#2785),#23688,.F.);
#24892=ADVANCED_FACE('',(#2786),#1605,.F.);
#24893=ADVANCED_FACE('',(#2787),#23689,.F.);
#24894=ADVANCED_FACE('',(#2788),#23690,.T.);
#24895=ADVANCED_FACE('',(#2789),#23691,.F.);
#24896=ADVANCED_FACE('',(#2790),#1606,.F.);
#24897=ADVANCED_FACE('',(#2791),#23692,.F.);
#24898=ADVANCED_FACE('',(#2792),#23693,.T.);
#24899=ADVANCED_FACE('',(#2793),#23694,.F.);
#24900=ADVANCED_FACE('',(#2794),#1607,.F.);
#24901=ADVANCED_FACE('',(#2795),#23695,.F.);
#24902=ADVANCED_FACE('',(#2796),#23696,.T.);
#24903=ADVANCED_FACE('',(#2797),#1608,.F.);
#24904=ADVANCED_FACE('',(#2798),#1075,.F.);
#24905=ADVANCED_FACE('',(#2799),#1076,.F.);
#24906=ADVANCED_FACE('',(#2800),#1609,.F.);
#24907=ADVANCED_FACE('',(#2801),#1077,.F.);
#24908=ADVANCED_FACE('',(#2802),#1078,.F.);
#24909=ADVANCED_FACE('',(#2803),#1610,.F.);
#24910=ADVANCED_FACE('',(#2804),#1079,.F.);
#24911=ADVANCED_FACE('',(#2805),#1080,.F.);
#24912=ADVANCED_FACE('',(#2806),#1611,.F.);
#24913=ADVANCED_FACE('',(#2807),#1081,.F.);
#24914=ADVANCED_FACE('',(#2808),#1082,.F.);
#24915=ADVANCED_FACE('',(#2809),#1612,.F.);
#24916=ADVANCED_FACE('',(#2810),#1083,.F.);
#24917=ADVANCED_FACE('',(#2811),#1084,.F.);
#24918=ADVANCED_FACE('',(#2812),#1613,.F.);
#24919=ADVANCED_FACE('',(#2813),#1085,.F.);
#24920=ADVANCED_FACE('',(#2814),#1086,.F.);
#24921=ADVANCED_FACE('',(#2815),#1614,.F.);
#24922=ADVANCED_FACE('',(#2816),#1087,.F.);
#24923=ADVANCED_FACE('',(#2817),#1088,.F.);
#24924=ADVANCED_FACE('',(#2818),#1615,.F.);
#24925=ADVANCED_FACE('',(#2819),#1089,.F.);
#24926=ADVANCED_FACE('',(#2820),#1090,.F.);
#24927=ADVANCED_FACE('',(#2821),#1616,.F.);
#24928=ADVANCED_FACE('',(#2822),#1091,.F.);
#24929=ADVANCED_FACE('',(#2823),#1092,.F.);
#24930=ADVANCED_FACE('',(#2824),#1617,.F.);
#24931=ADVANCED_FACE('',(#2825),#1093,.F.);
#24932=ADVANCED_FACE('',(#2826),#1094,.F.);
#24933=ADVANCED_FACE('',(#2827),#1618,.F.);
#24934=ADVANCED_FACE('',(#2828),#1095,.F.);
#24935=ADVANCED_FACE('',(#2829),#1096,.F.);
#24936=ADVANCED_FACE('',(#2830),#1619,.F.);
#24937=ADVANCED_FACE('',(#2831),#1097,.F.);
#24938=ADVANCED_FACE('',(#2832),#1098,.F.);
#24939=ADVANCED_FACE('',(#2833),#1620,.F.);
#24940=ADVANCED_FACE('',(#2834),#1099,.F.);
#24941=ADVANCED_FACE('',(#2835),#1100,.F.);
#24942=ADVANCED_FACE('',(#2836),#1621,.F.);
#24943=ADVANCED_FACE('',(#2837),#1101,.F.);
#24944=ADVANCED_FACE('',(#2838),#1102,.F.);
#24945=ADVANCED_FACE('',(#2839),#1622,.F.);
#24946=ADVANCED_FACE('',(#2840),#1103,.F.);
#24947=ADVANCED_FACE('',(#2841),#1104,.F.);
#24948=ADVANCED_FACE('',(#2842),#1623,.F.);
#24949=ADVANCED_FACE('',(#2843),#1105,.F.);
#24950=ADVANCED_FACE('',(#2844),#1106,.F.);
#24951=ADVANCED_FACE('',(#2845),#1624,.F.);
#24952=ADVANCED_FACE('',(#2846),#1107,.F.);
#24953=ADVANCED_FACE('',(#2847),#1108,.F.);
#24954=ADVANCED_FACE('',(#2848),#1625,.F.);
#24955=ADVANCED_FACE('',(#2849),#1109,.F.);
#24956=ADVANCED_FACE('',(#2850),#1110,.F.);
#24957=ADVANCED_FACE('',(#2851),#1626,.F.);
#24958=ADVANCED_FACE('',(#2852),#1111,.F.);
#24959=ADVANCED_FACE('',(#2853),#1112,.F.);
#24960=ADVANCED_FACE('',(#2854),#1627,.F.);
#24961=ADVANCED_FACE('',(#2855),#1113,.F.);
#24962=ADVANCED_FACE('',(#2856),#1114,.F.);
#24963=ADVANCED_FACE('',(#2857),#1628,.F.);
#24964=ADVANCED_FACE('',(#2858),#1115,.F.);
#24965=ADVANCED_FACE('',(#2859),#1116,.F.);
#24966=ADVANCED_FACE('',(#2860),#1629,.F.);
#24967=ADVANCED_FACE('',(#2861),#1117,.F.);
#24968=ADVANCED_FACE('',(#2862),#1118,.F.);
#24969=ADVANCED_FACE('',(#2863),#1630,.F.);
#24970=ADVANCED_FACE('',(#2864),#1119,.F.);
#24971=ADVANCED_FACE('',(#2865),#1120,.F.);
#24972=ADVANCED_FACE('',(#2866,#1283),#1631,.F.);
#24973=ADVANCED_FACE('',(#2867,#1284),#1632,.T.);
#24974=ADVANCED_FACE('',(#2868),#23697,.T.);
#24975=ADVANCED_FACE('',(#2869),#23698,.T.);
#24976=ADVANCED_FACE('',(#2870),#23699,.T.);
#24977=ADVANCED_FACE('',(#2871),#23700,.T.);
#24978=ADVANCED_FACE('',(#2872),#23701,.T.);
#24979=ADVANCED_FACE('',(#2873),#23702,.T.);
#24980=ADVANCED_FACE('',(#2874),#23703,.T.);
#24981=ADVANCED_FACE('',(#2875),#23704,.T.);
#24982=ADVANCED_FACE('',(#2876),#23705,.T.);
#24983=ADVANCED_FACE('',(#2877),#23706,.T.);
#24984=ADVANCED_FACE('',(#2878),#23707,.T.);
#24985=ADVANCED_FACE('',(#2879),#23708,.T.);
#24986=ADVANCED_FACE('',(#2880),#23709,.T.);
#24987=ADVANCED_FACE('',(#2881),#23710,.T.);
#24988=ADVANCED_FACE('',(#2882),#23711,.T.);
#24989=ADVANCED_FACE('',(#2883),#23712,.T.);
#24990=ADVANCED_FACE('',(#2884),#23713,.T.);
#24991=ADVANCED_FACE('',(#2885),#23714,.T.);
#24992=ADVANCED_FACE('',(#2886),#23715,.T.);
#24993=ADVANCED_FACE('',(#2887),#23716,.T.);
#24994=ADVANCED_FACE('',(#2888),#23717,.T.);
#24995=ADVANCED_FACE('',(#2889),#23718,.T.);
#24996=ADVANCED_FACE('',(#2890),#23719,.T.);
#24997=ADVANCED_FACE('',(#2891),#23720,.F.);
#24998=ADVANCED_FACE('',(#2892),#1633,.F.);
#24999=ADVANCED_FACE('',(#2893),#23721,.F.);
#25000=ADVANCED_FACE('',(#2894),#23722,.T.);
#25001=ADVANCED_FACE('',(#2895),#1634,.F.);
#25002=ADVANCED_FACE('',(#2896),#1121,.F.);
#25003=ADVANCED_FACE('',(#2897),#1122,.F.);
#25004=ADVANCED_FACE('',(#2898),#23723,.F.);
#25005=ADVANCED_FACE('',(#2899),#23724,.T.);
#25006=ADVANCED_FACE('',(#2900),#23725,.F.);
#25007=ADVANCED_FACE('',(#2901),#23726,.T.);
#25008=ADVANCED_FACE('',(#2902,#1285),#1635,.T.);
#25009=ADVANCED_FACE('',(#2903,#1286),#1636,.F.);
#25010=ADVANCED_FACE('',(#2904),#1637,.F.);
#25011=ADVANCED_FACE('',(#2905),#1638,.F.);
#25012=ADVANCED_FACE('',(#2906),#1639,.F.);
#25013=ADVANCED_FACE('',(#2907),#1640,.F.);
#25014=ADVANCED_FACE('',(#2908),#1641,.F.);
#25015=ADVANCED_FACE('',(#2909),#23727,.T.);
#25016=ADVANCED_FACE('',(#2910,#1287),#1642,.F.);
#25017=ADVANCED_FACE('',(#2911,#1288),#1643,.F.);
#25018=ADVANCED_FACE('',(#2912),#23728,.T.);
#25019=ADVANCED_FACE('',(#2913),#23729,.T.);
#25020=ADVANCED_FACE('',(#2914,#1289),#1644,.F.);
#25021=ADVANCED_FACE('',(#2915,#1290),#1645,.F.);
#25022=ADVANCED_FACE('',(#2916),#23730,.T.);
#25023=ADVANCED_FACE('',(#2917),#23731,.F.);
#25024=ADVANCED_FACE('',(#2918),#23732,.F.);
#25025=ADVANCED_FACE('',(#2919),#23733,.F.);
#25026=ADVANCED_FACE('',(#2920,#1291),#1646,.T.);
#25027=ADVANCED_FACE('',(#2921,#1292),#1647,.F.);
#25028=ADVANCED_FACE('',(#2922),#23734,.T.);
#25029=ADVANCED_FACE('',(#2923),#23735,.T.);
#25030=ADVANCED_FACE('',(#2924,#1293),#23736,.T.);
#25031=ADVANCED_FACE('',(#2925),#1648,.T.);
#25032=ADVANCED_FACE('',(#2926,#1294),#1649,.T.);
#25033=ADVANCED_FACE('',(#2927,#1295),#1650,.F.);
#25034=ADVANCED_FACE('',(#2928),#23737,.T.);
#25035=ADVANCED_FACE('',(#2929),#23738,.T.);
#25036=ADVANCED_FACE('',(#2930),#1651,.F.);
#25037=ADVANCED_FACE('',(#2931),#23739,.T.);
#25038=ADVANCED_FACE('',(#2932,#1296),#1652,.T.);
#25039=ADVANCED_FACE('',(#2933),#23740,.F.);
#25040=ADVANCED_FACE('',(#2934),#23741,.T.);
#25041=ADVANCED_FACE('',(#2935,#1297,#1298,#1299,#1300),#1653,.T.);
#25042=ADVANCED_FACE('',(#2936,#1301,#1302,#1303,#1304),#1654,.F.);
#25043=ADVANCED_FACE('',(#2937),#1655,.T.);
#25044=ADVANCED_FACE('',(#2938),#1656,.T.);
#25045=ADVANCED_FACE('',(#2939),#1657,.T.);
#25046=ADVANCED_FACE('',(#2940),#1658,.T.);
#25047=ADVANCED_FACE('',(#2941),#1659,.T.);
#25048=ADVANCED_FACE('',(#2942),#1660,.F.);
#25049=ADVANCED_FACE('',(#2943),#23742,.F.);
#25050=ADVANCED_FACE('',(#2944),#23743,.T.);
#25051=ADVANCED_FACE('',(#2945,#1305),#1661,.T.);
#25052=ADVANCED_FACE('',(#2946,#1306),#1662,.F.);
#25053=ADVANCED_FACE('',(#2947),#23744,.T.);
#25054=ADVANCED_FACE('',(#2948,#1307),#1663,.F.);
#25055=ADVANCED_FACE('',(#2949,#1308),#1664,.F.);
#25056=ADVANCED_FACE('',(#2950),#23745,.T.);
#25057=ADVANCED_FACE('',(#2951,#1309),#1665,.T.);
#25058=ADVANCED_FACE('',(#2952),#23746,.T.);
#25059=ADVANCED_FACE('',(#2953),#1666,.F.);
#25060=ADVANCED_FACE('',(#2954),#23747,.T.);
#25061=ADVANCED_FACE('',(#2955),#1667,.T.);
#25062=ADVANCED_FACE('',(#2956),#1668,.F.);
#25063=ADVANCED_FACE('',(#2957),#1669,.F.);
#25064=ADVANCED_FACE('',(#2958),#1670,.F.);
#25065=ADVANCED_FACE('',(#2959),#23748,.F.);
#25066=ADVANCED_FACE('',(#2960),#23749,.T.);
#25067=ADVANCED_FACE('',(#2961),#1671,.T.);
#25068=ADVANCED_FACE('',(#2962),#23750,.F.);
#25069=ADVANCED_FACE('',(#2963),#23751,.T.);
#25070=ADVANCED_FACE('',(#2964,#1310),#1672,.T.);
#25071=ADVANCED_FACE('',(#2965,#1311),#1673,.F.);
#25072=ADVANCED_FACE('',(#2966),#23752,.F.);
#25073=ADVANCED_FACE('',(#2967),#23753,.T.);
#25074=ADVANCED_FACE('',(#2968,#1312),#1674,.T.);
#25075=ADVANCED_FACE('',(#2969,#1313),#1675,.F.);
#25076=ADVANCED_FACE('',(#2970),#23754,.F.);
#25077=ADVANCED_FACE('',(#2971),#23755,.T.);
#25078=ADVANCED_FACE('',(#2972,#1314),#1676,.T.);
#25079=ADVANCED_FACE('',(#2973,#1315),#1677,.F.);
#25080=ADVANCED_FACE('',(#2974),#1678,.F.);
#25081=ADVANCED_FACE('',(#2975),#1679,.F.);
#25082=ADVANCED_FACE('',(#2976),#1680,.F.);
#25083=ADVANCED_FACE('',(#2977),#23756,.F.);
#25084=ADVANCED_FACE('',(#2978),#23757,.T.);
#25085=ADVANCED_FACE('',(#2979),#1681,.T.);
#25086=ADVANCED_FACE('',(#2980),#1682,.F.);
#25087=ADVANCED_FACE('',(#2981),#1683,.F.);
#25088=ADVANCED_FACE('',(#2982),#1684,.F.);
#25089=ADVANCED_FACE('',(#2983),#23758,.F.);
#25090=ADVANCED_FACE('',(#2984),#23759,.T.);
#25091=ADVANCED_FACE('',(#2985),#1685,.T.);
#25092=ADVANCED_FACE('',(#2986),#23760,.T.);
#25093=ADVANCED_FACE('',(#2987),#1686,.T.);
#25094=ADVANCED_FACE('',(#2988),#1687,.F.);
#25095=ADVANCED_FACE('',(#2989),#23761,.T.);
#25096=ADVANCED_FACE('',(#2990),#23762,.T.);
#25097=ADVANCED_FACE('',(#2991),#23763,.T.);
#25098=ADVANCED_FACE('',(#2992),#23764,.T.);
#25099=ADVANCED_FACE('',(#2993),#23765,.T.);
#25100=ADVANCED_FACE('',(#2994),#23766,.T.);
#25101=ADVANCED_FACE('',(#2995),#23767,.T.);
#25102=ADVANCED_FACE('',(#2996),#23768,.T.);
#25103=ADVANCED_FACE('',(#2997),#23769,.T.);
#25104=ADVANCED_FACE('',(#2998),#23770,.T.);
#25105=ADVANCED_FACE('',(#2999),#23771,.T.);
#25106=ADVANCED_FACE('',(#3000),#23772,.T.);
#25107=ADVANCED_FACE('',(#3001),#23773,.T.);
#25108=ADVANCED_FACE('',(#3002),#23774,.T.);
#25109=ADVANCED_FACE('',(#3003),#23775,.T.);
#25110=ADVANCED_FACE('',(#3004),#23776,.T.);
#25111=ADVANCED_FACE('',(#3005),#23777,.T.);
#25112=ADVANCED_FACE('',(#3006),#23778,.T.);
#25113=ADVANCED_FACE('',(#3007),#23779,.T.);
#25114=ADVANCED_FACE('',(#3008),#23780,.T.);
#25115=ADVANCED_FACE('',(#3009),#23781,.T.);
#25116=ADVANCED_FACE('',(#3010),#23782,.T.);
#25117=ADVANCED_FACE('',(#3011),#23783,.T.);
#25118=ADVANCED_FACE('',(#3012),#23784,.T.);
#25119=ADVANCED_FACE('',(#3013),#23785,.T.);
#25120=ADVANCED_FACE('',(#3014),#23786,.T.);
#25121=ADVANCED_FACE('',(#3015),#23787,.T.);
#25122=ADVANCED_FACE('',(#3016),#23788,.T.);
#25123=ADVANCED_FACE('',(#3017),#23789,.T.);
#25124=ADVANCED_FACE('',(#3018),#23790,.T.);
#25125=ADVANCED_FACE('',(#3019),#23791,.T.);
#25126=ADVANCED_FACE('',(#3020),#23792,.T.);
#25127=ADVANCED_FACE('',(#3021),#23793,.T.);
#25128=ADVANCED_FACE('',(#3022),#23794,.T.);
#25129=ADVANCED_FACE('',(#3023),#23795,.T.);
#25130=ADVANCED_FACE('',(#3024),#23796,.T.);
#25131=ADVANCED_FACE('',(#3025),#23797,.T.);
#25132=ADVANCED_FACE('',(#3026),#23798,.T.);
#25133=ADVANCED_FACE('',(#3027),#23799,.T.);
#25134=ADVANCED_FACE('',(#3028),#23800,.T.);
#25135=ADVANCED_FACE('',(#3029),#1478,.F.);
#25136=ADVANCED_FACE('',(#3030),#23801,.T.);
#25137=ADVANCED_FACE('',(#3031),#1479,.F.);
#25138=ADVANCED_FACE('',(#3032),#23802,.T.);
#25139=ADVANCED_FACE('',(#3033),#1688,.F.);
#25140=ADVANCED_FACE('',(#3034),#1689,.F.);
#25141=ADVANCED_FACE('',(#3035),#1690,.F.);
#25142=ADVANCED_FACE('',(#3036),#1691,.F.);
#25143=ADVANCED_FACE('',(#3037),#1692,.F.);
#25144=ADVANCED_FACE('',(#3038),#1693,.F.);
#25145=ADVANCED_FACE('',(#3039),#1694,.F.);
#25146=ADVANCED_FACE('',(#3040,#1316),#1695,.T.);
#25147=ADVANCED_FACE('',(#3041),#23803,.T.);
#25148=ADVANCED_FACE('',(#3042,#1317),#1696,.F.);
#25149=ADVANCED_FACE('',(#3043),#1697,.T.);
#25150=CLOSED_SHELL('',(#23804,#23805,#23806,#23807,#23808,#23809,#23810,
#23811,#23812,#23813,#23814,#23815,#23816,#23817,#23818,#23819,#23820,#23821,
#23822,#23823,#23824,#23825,#23826,#23827,#23828,#23829,#23830,#23831,#23832,
#23833,#23834,#23835,#23836,#23837,#23838,#23839,#23840,#23841,#23842,#23843,
#23844,#23845,#23846,#23847,#23848,#23849,#23850,#23851,#23852,#23853,#23854,
#23855,#23856,#23857,#23858,#23859,#23860,#23861,#23862,#23863,#23864,#23865,
#23866,#23867,#23868,#23869,#23870,#23871,#23872,#23873,#23874,#23875,#23876,
#23877,#23878,#23879,#23880,#23881,#23882,#23883,#23884,#23885,#23886,#23887,
#23888,#23889,#23890,#23891,#23892,#23893,#23894,#23895,#23896,#23897,#23898,
#23899,#23900,#23901,#23902,#23903,#23904,#23905,#23906,#23907,#23908,#23909,
#23910,#23911,#23912,#23913,#23914,#23915,#23916,#23917,#23918,#23919,#23920,
#23921,#23922,#23923,#23924,#23925,#23926,#23927,#23928,#23929,#23930,#23931,
#23932,#23933,#23934,#23935,#23936,#23937,#23938,#23939,#23940,#23941,#23942,
#23943,#23944,#23945,#23946,#23947,#23948,#23949,#23950,#23951,#23952,#23953,
#23954,#23955,#23956,#23957,#23958,#23959,#23960,#23961,#23962,#23963,#23964,
#23965,#23966,#23967,#23968,#23969,#23970,#23971,#23972,#23973,#23974,#23975,
#23976,#23977,#23978,#23979,#23980,#23981,#23982,#23983,#23984,#23985,#23986,
#23987,#23988,#23989,#23990,#23991,#23992,#23993,#23994,#23995,#23996,#23997,
#23998,#23999,#24000,#24001,#24002,#24003,#24004,#24005,#24006,#24007,#24008,
#24009,#24010,#24011,#24012,#24013,#24014,#24015,#24016,#24017,#24018,#24019,
#24020,#24021,#24022,#24023,#24024,#24025,#24026,#24027,#24028,#24029,#24030,
#24031,#24032,#24033,#24034,#24035,#24036,#24037,#24038,#24039,#24040,#24041,
#24042,#24043,#24044,#24045,#24046,#24047,#24048,#24049,#24050,#24051,#24052,
#24053,#24054,#24055,#24056,#24057,#24058,#24059,#24060,#24061,#24062,#24063,
#24064,#24065,#24066,#24067,#24068,#24069,#24070,#24071,#24072,#24073,#24074,
#24075,#24076,#24077,#24078,#24079,#24080,#24081,#24082,#24083,#24084,#24085,
#24086,#24087,#24088,#24089,#24090,#24091,#24092,#24093,#24094,#24095,#24096,
#24097,#24098,#24099,#24100,#24101,#24102,#24103,#24104,#24105,#24106,#24107,
#24108,#24109,#24110,#24111,#24112,#24113,#24114,#24115,#24116,#24117));
#25151=CLOSED_SHELL('',(#24118,#24119,#24120,#24121,#24122,#24123,#24124,
#24125,#24126,#24127,#24128,#24129));
#25152=CLOSED_SHELL('',(#24130,#24131,#24132,#24133,#24134,#24135,#24136,
#24137,#24138,#24139,#24140,#24141));
#25153=CLOSED_SHELL('',(#24142,#24143,#24144,#24145,#24146,#24147,#24148,
#24149,#24150,#24151,#24152,#24153,#24154,#24155,#24156,#24157,#24158,#24159,
#24160,#24161,#24162,#24163,#24164,#24165,#24166,#24167,#24168,#24169));
#25154=CLOSED_SHELL('',(#24170,#24171,#24172,#24173,#24174,#24175,#24176,
#24177,#24178,#24179,#24180,#24181,#24182,#24183,#24184,#24185,#24186,#24187,
#24188,#24189,#24190,#24191,#24192,#24193,#24194,#24195,#24196,#24197,#24198,
#24199,#24200,#24201,#24202,#24203,#24204,#24205,#24206,#24207,#24208,#24209,
#24210,#24211,#24212,#24213,#24214,#24215,#24216,#24217,#24218,#24219,#24220,
#24221,#24222,#24223,#24224,#24225,#24226,#24227,#24228,#24229,#24230,#24231,
#24232,#24233,#24234,#24235,#24236,#24237,#24238,#24239,#24240,#24241,#24242,
#24243,#24244,#24245,#24246,#24247,#24248,#24249,#24250,#24251,#24252,#24253,
#24254,#24255,#24256,#24257,#24258,#24259,#24260,#24261,#24262,#24263,#24264,
#24265,#24266,#24267,#24268,#24269,#24270,#24271,#24272,#24273,#24274,#24275,
#24276,#24277,#24278,#24279,#24280,#24281,#24282,#24283,#24284,#24285,#24286,
#24287,#24288,#24289,#24290,#24291,#24292,#24293,#24294,#24295,#24296,#24297,
#24298,#24299,#24300,#24301,#24302,#24303,#24304,#24305,#24306,#24307,#24308,
#24309,#24310,#24311,#24312,#24313,#24314,#24315,#24316,#24317,#24318,#24319,
#24320,#24321,#24322,#24323,#24324,#24325,#24326,#24327,#24328,#24329,#24330,
#24331,#24332,#24333,#24334,#24335,#24336,#24337,#24338,#24339,#24340,#24341,
#24342,#24343,#24344,#24345,#24346,#24347,#24348,#24349,#24350,#24351,#24352,
#24353,#24354,#24355,#24356,#24357,#24358,#24359,#24360,#24361,#24362,#24363,
#24364,#24365,#24366,#24367,#24368,#24369,#24370,#24371,#24372,#24373,#24374,
#24375,#24376,#24377,#24378,#24379,#24380,#24381,#24382,#24383,#24384,#24385,
#24386,#24387,#24388,#24389,#24390,#24391,#24392,#24393,#24394,#24395,#24396,
#24397,#24398,#24399,#24400,#24401,#24402,#24403,#24404,#24405,#24406,#24407,
#24408,#24409,#24410,#24411,#24412,#24413,#24414,#24415,#24416,#24417,#24418,
#24419,#24420,#24421,#24422,#24423,#24424,#24425,#24426,#24427,#24428,#24429,
#24430,#24431,#24432,#24433,#24434,#24435,#24436,#24437,#24438,#24439,#24440,
#24441,#24442,#24443,#24444,#24445,#24446,#24447,#24448,#24449,#24450,#24451,
#24452,#24453,#24454,#24455,#24456,#24457,#24458,#24459,#24460,#24461,#24462,
#24463,#24464,#24465,#24466,#24467,#24468,#24469,#24470,#24471,#24472,#24473,
#24474,#24475,#24476,#24477,#24478,#24479,#24480,#24481,#24482,#24483,#24484,
#24485,#24486,#24487,#24488,#24489,#24490,#24491,#24492,#24493,#24494,#24495,
#24496,#24497,#24498,#24499,#24500,#24501,#24502,#24503,#24504,#24505,#24506,
#24507,#24508,#24509,#24510,#24511,#24512,#24513,#24514,#24515,#24516,#24517,
#24518,#24519,#24520,#24521,#24522,#24523,#24524,#24525,#24526,#24527,#24528,
#24529,#24530,#24531,#24532,#24533,#24534,#24535,#24536,#24537,#24538,#24539,
#24540,#24541,#24542,#24543,#24544,#24545,#24546,#24547,#24548,#24549,#24550,
#24551,#24552,#24553,#24554,#24555,#24556,#24557,#24558,#24559,#24560,#24561,
#24562,#24563,#24564,#24565,#24566,#24567,#24568,#24569,#24570,#24571,#24572,
#24573,#24574,#24575,#24576,#24577,#24578,#24579,#24580,#24581,#24582,#24583,
#24584,#24585,#24586,#24587,#24588,#24589,#24590,#24591,#24592,#24593,#24594,
#24595,#24596,#24597,#24598,#24599,#24600,#24601,#24602,#24603,#24604,#24605,
#24606,#24607,#24608,#24609,#24610,#24611,#24612));
#25155=CLOSED_SHELL('',(#24613,#24614,#24615,#24616,#24617,#24618,#24619,
#24620,#24621,#24622,#24623,#24624,#24625,#24626,#24627,#24628,#24629,#24630,
#24631,#24632,#24633,#24634,#24635,#24636,#24637,#24638,#24639,#24640,#24641,
#24642,#24643,#24644,#24645,#24646,#24647,#24648,#24649,#24650,#24651,#24652,
#24653,#24654,#24655,#24656,#24657,#24658,#24659,#24660,#24661,#24662,#24663,
#24664,#24665,#24666,#24667,#24668,#24669,#24670,#24671,#24672,#24673,#24674,
#24675,#24676,#24677,#24678,#24679,#24680,#24681,#24682,#24683,#24684,#24685,
#24686,#24687,#24688,#24689,#24690,#24691,#24692,#24693,#24694,#24695,#24696,
#24697,#24698,#24699,#24700,#24701,#24702,#24703,#24704,#24705,#24706,#24707,
#24708,#24709,#24710,#24711,#24712,#24713,#24714,#24715,#24716,#24717,#24718,
#24719,#24720,#24721,#24722,#24723,#24724,#24725,#24726,#24727,#24728,#24729,
#24730,#24731,#24732,#24733,#24734,#24735,#24736,#24737,#24738,#24739,#24740,
#24741,#24742,#24743,#24744,#24745,#24746,#24747,#24748,#24749,#24750,#24751,
#24752,#24753,#24754,#24755,#24756,#24757,#24758,#24759,#24760,#24761,#24762,
#24763,#24764,#24765,#24766,#24767,#24768,#24769,#24770,#24771,#24772,#24773,
#24774,#24775,#24776,#24777,#24778,#24779,#24780,#24781,#24782,#24783,#24784,
#24785,#24786,#24787,#24788,#24789,#24790,#24791,#24792,#24793,#24794,#24795,
#24796,#24797,#24798,#24799,#24800,#24801,#24802,#24803,#24804,#24805,#24806,
#24807,#24808,#24809,#24810));
#25156=CLOSED_SHELL('',(#24811,#24812,#24813,#24814,#24815,#24816,#24817,
#24818,#24819,#24820,#24821,#24822,#24823,#24824,#24825,#24826,#24827,#24828,
#24829,#24830,#24831,#24832,#24833,#24834,#24835,#24836,#24837,#24838,#24839,
#24840,#24841,#24842,#24843,#24844,#24845,#24846,#24847,#24848,#24849,#24850,
#24851,#24852,#24853,#24854,#24855,#24856,#24857,#24858,#24859,#24860,#24861,
#24862,#24863,#24864,#24865,#24866,#24867,#24868,#24869,#24870,#24871,#24872,
#24873,#24874,#24875,#24876,#24877,#24878,#24879,#24880,#24881,#24882,#24883,
#24884,#24885,#24886,#24887,#24888,#24889,#24890,#24891,#24892,#24893,#24894,
#24895,#24896,#24897,#24898,#24899,#24900,#24901,#24902,#24903,#24904,#24905,
#24906,#24907,#24908,#24909,#24910,#24911,#24912,#24913,#24914,#24915,#24916,
#24917,#24918,#24919,#24920,#24921,#24922,#24923,#24924,#24925,#24926,#24927,
#24928,#24929,#24930,#24931,#24932,#24933,#24934,#24935,#24936,#24937,#24938,
#24939,#24940,#24941,#24942,#24943,#24944,#24945,#24946,#24947,#24948,#24949,
#24950,#24951,#24952,#24953,#24954,#24955,#24956,#24957,#24958,#24959,#24960,
#24961,#24962,#24963,#24964,#24965,#24966,#24967,#24968,#24969,#24970,#24971,
#24972,#24973,#24974,#24975,#24976,#24977,#24978,#24979,#24980,#24981,#24982,
#24983,#24984,#24985,#24986,#24987,#24988,#24989,#24990,#24991,#24992,#24993,
#24994,#24995,#24996,#24997,#24998,#24999,#25000,#25001,#25002,#25003,#25004,
#25005));
#25157=CLOSED_SHELL('',(#25006,#25007,#25008,#25009));
#25158=CLOSED_SHELL('',(#25010,#25011,#25012,#25013,#25014,#25015,#25016,
#25017,#25018,#25019,#25020,#25021,#25022,#25023,#25024,#25025,#25026,#25027,
#25028,#25029,#25030,#25031,#25032,#25033,#25034,#25035,#25036,#25037,#25038,
#25039,#25040,#25041,#25042));
#25159=CLOSED_SHELL('',(#25043,#25044,#25045,#25046,#25047,#25048));
#25160=CLOSED_SHELL('',(#25049,#25050,#25051,#25052));
#25161=CLOSED_SHELL('',(#25053,#25054,#25055,#25056,#25057,#25058,#25059,
#25060,#25061));
#25162=CLOSED_SHELL('',(#25062,#25063,#25064,#25065,#25066,#25067));
#25163=CLOSED_SHELL('',(#25068,#25069,#25070,#25071));
#25164=CLOSED_SHELL('',(#25072,#25073,#25074,#25075));
#25165=CLOSED_SHELL('',(#25076,#25077,#25078,#25079));
#25166=CLOSED_SHELL('',(#25080,#25081,#25082,#25083,#25084,#25085));
#25167=CLOSED_SHELL('',(#25086,#25087,#25088,#25089,#25090,#25091));
#25168=CLOSED_SHELL('',(#25092,#25093,#25094));
#25169=CLOSED_SHELL('',(#25095,#25096,#25097,#25098,#25099,#25100,#25101,
#25102,#25103,#25104,#25105,#25106,#25107,#25108,#25109,#25110,#25111,#25112,
#25113,#25114,#25115,#25116,#25117,#25118,#25119,#25120,#25121,#25122,#25123,
#25124,#25125,#25126,#25127,#25128,#25129,#25130,#25131,#25132,#25133,#25134,
#25135,#25136,#25137,#25138,#25139,#25140,#25141,#25142,#25143,#25144,#25145,
#25146,#25147,#25148,#25149));
#25170=DERIVED_UNIT_ELEMENT(#25210,1.);
#25171=DERIVED_UNIT_ELEMENT(#259226,-3.);
#25172=DERIVED_UNIT_ELEMENT(#25210,1.);
#25173=DERIVED_UNIT_ELEMENT(#259226,-3.);
#25174=DERIVED_UNIT_ELEMENT(#25210,1.);
#25175=DERIVED_UNIT_ELEMENT(#259226,-3.);
#25176=DERIVED_UNIT_ELEMENT(#25210,1.);
#25177=DERIVED_UNIT_ELEMENT(#259226,-3.);
#25178=DERIVED_UNIT_ELEMENT(#25210,1.);
#25179=DERIVED_UNIT_ELEMENT(#259226,-3.);
#25180=DERIVED_UNIT_ELEMENT(#25210,1.);
#25181=DERIVED_UNIT_ELEMENT(#259226,-3.);
#25182=DERIVED_UNIT_ELEMENT(#25210,1.);
#25183=DERIVED_UNIT_ELEMENT(#259226,-3.);
#25184=DERIVED_UNIT_ELEMENT(#25210,1.);
#25185=DERIVED_UNIT_ELEMENT(#259226,-3.);
#25186=DERIVED_UNIT_ELEMENT(#25210,1.);
#25187=DERIVED_UNIT_ELEMENT(#259226,-3.);
#25188=DERIVED_UNIT_ELEMENT(#25210,1.);
#25189=DERIVED_UNIT_ELEMENT(#259226,-3.);
#25190=DERIVED_UNIT_ELEMENT(#25210,1.);
#25191=DERIVED_UNIT_ELEMENT(#259226,-3.);
#25192=DERIVED_UNIT_ELEMENT(#25210,1.);
#25193=DERIVED_UNIT_ELEMENT(#259226,-3.);
#25194=DERIVED_UNIT_ELEMENT(#25210,1.);
#25195=DERIVED_UNIT_ELEMENT(#259226,-3.);
#25196=DERIVED_UNIT_ELEMENT(#25210,1.);
#25197=DERIVED_UNIT_ELEMENT(#259226,-3.);
#25198=DERIVED_UNIT_ELEMENT(#25210,1.);
#25199=DERIVED_UNIT_ELEMENT(#259226,-3.);
#25200=DERIVED_UNIT_ELEMENT(#25210,1.);
#25201=DERIVED_UNIT_ELEMENT(#259226,-3.);
#25202=DERIVED_UNIT_ELEMENT(#25210,1.);
#25203=DERIVED_UNIT_ELEMENT(#259226,-3.);
#25204=DERIVED_UNIT_ELEMENT(#25210,1.);
#25205=DERIVED_UNIT_ELEMENT(#259226,-3.);
#25206=DERIVED_UNIT_ELEMENT(#25210,1.);
#25207=DERIVED_UNIT_ELEMENT(#259226,-3.);
#25208=DERIVED_UNIT_ELEMENT(#25210,1.);
#25209=DERIVED_UNIT_ELEMENT(#259226,-3.);
#25210=(
MASS_UNIT()
NAMED_UNIT(*)
SI_UNIT(.KILO.,.GRAM.)
);
#25211=DERIVED_UNIT((#25170,#25171));
#25212=DERIVED_UNIT((#25172,#25173));
#25213=DERIVED_UNIT((#25174,#25175));
#25214=DERIVED_UNIT((#25176,#25177));
#25215=DERIVED_UNIT((#25178,#25179));
#25216=DERIVED_UNIT((#25180,#25181));
#25217=DERIVED_UNIT((#25182,#25183));
#25218=DERIVED_UNIT((#25184,#25185));
#25219=DERIVED_UNIT((#25186,#25187));
#25220=DERIVED_UNIT((#25188,#25189));
#25221=DERIVED_UNIT((#25190,#25191));
#25222=DERIVED_UNIT((#25192,#25193));
#25223=DERIVED_UNIT((#25194,#25195));
#25224=DERIVED_UNIT((#25196,#25197));
#25225=DERIVED_UNIT((#25198,#25199));
#25226=DERIVED_UNIT((#25200,#25201));
#25227=DERIVED_UNIT((#25202,#25203));
#25228=DERIVED_UNIT((#25204,#25205));
#25229=DERIVED_UNIT((#25206,#25207));
#25230=DERIVED_UNIT((#25208,#25209));
#25231=MEASURE_REPRESENTATION_ITEM('density measure',
POSITIVE_RATIO_MEASURE(7850.),#25211);
#25232=MEASURE_REPRESENTATION_ITEM('density measure',
POSITIVE_RATIO_MEASURE(7850.),#25212);
#25233=MEASURE_REPRESENTATION_ITEM('density measure',
POSITIVE_RATIO_MEASURE(7850.),#25213);
#25234=MEASURE_REPRESENTATION_ITEM('density measure',
POSITIVE_RATIO_MEASURE(7850.),#25214);
#25235=MEASURE_REPRESENTATION_ITEM('density measure',
POSITIVE_RATIO_MEASURE(7850.),#25215);
#25236=MEASURE_REPRESENTATION_ITEM('density measure',
POSITIVE_RATIO_MEASURE(7850.),#25216);
#25237=MEASURE_REPRESENTATION_ITEM('density measure',
POSITIVE_RATIO_MEASURE(7850.),#25217);
#25238=MEASURE_REPRESENTATION_ITEM('density measure',
POSITIVE_RATIO_MEASURE(8920.),#25218);
#25239=MEASURE_REPRESENTATION_ITEM('density measure',
POSITIVE_RATIO_MEASURE(7850.),#25219);
#25240=MEASURE_REPRESENTATION_ITEM('density measure',
POSITIVE_RATIO_MEASURE(7850.),#25220);
#25241=MEASURE_REPRESENTATION_ITEM('density measure',
POSITIVE_RATIO_MEASURE(8920.),#25221);
#25242=MEASURE_REPRESENTATION_ITEM('density measure',
POSITIVE_RATIO_MEASURE(7850.),#25222);
#25243=MEASURE_REPRESENTATION_ITEM('density measure',
POSITIVE_RATIO_MEASURE(7850.),#25223);
#25244=MEASURE_REPRESENTATION_ITEM('density measure',
POSITIVE_RATIO_MEASURE(7850.),#25224);
#25245=MEASURE_REPRESENTATION_ITEM('density measure',
POSITIVE_RATIO_MEASURE(8920.),#25225);
#25246=MEASURE_REPRESENTATION_ITEM('density measure',
POSITIVE_RATIO_MEASURE(8920.),#25226);
#25247=MEASURE_REPRESENTATION_ITEM('density measure',
POSITIVE_RATIO_MEASURE(7850.),#25227);
#25248=MEASURE_REPRESENTATION_ITEM('density measure',
POSITIVE_RATIO_MEASURE(7850.),#25228);
#25249=MEASURE_REPRESENTATION_ITEM('density measure',
POSITIVE_RATIO_MEASURE(7850.),#25229);
#25250=MEASURE_REPRESENTATION_ITEM('density measure',
POSITIVE_RATIO_MEASURE(7850.),#25230);
#25251=PROPERTY_DEFINITION_REPRESENTATION(#25351,#25291);
#25252=PROPERTY_DEFINITION_REPRESENTATION(#25352,#25292);
#25253=PROPERTY_DEFINITION_REPRESENTATION(#25353,#25293);
#25254=PROPERTY_DEFINITION_REPRESENTATION(#25354,#25294);
#25255=PROPERTY_DEFINITION_REPRESENTATION(#25355,#25295);
#25256=PROPERTY_DEFINITION_REPRESENTATION(#25356,#25296);
#25257=PROPERTY_DEFINITION_REPRESENTATION(#25357,#25297);
#25258=PROPERTY_DEFINITION_REPRESENTATION(#25358,#25298);
#25259=PROPERTY_DEFINITION_REPRESENTATION(#25359,#25299);
#25260=PROPERTY_DEFINITION_REPRESENTATION(#25360,#25300);
#25261=PROPERTY_DEFINITION_REPRESENTATION(#25361,#25301);
#25262=PROPERTY_DEFINITION_REPRESENTATION(#25362,#25302);
#25263=PROPERTY_DEFINITION_REPRESENTATION(#25363,#25303);
#25264=PROPERTY_DEFINITION_REPRESENTATION(#25364,#25304);
#25265=PROPERTY_DEFINITION_REPRESENTATION(#25365,#25305);
#25266=PROPERTY_DEFINITION_REPRESENTATION(#25366,#25306);
#25267=PROPERTY_DEFINITION_REPRESENTATION(#25367,#25307);
#25268=PROPERTY_DEFINITION_REPRESENTATION(#25368,#25308);
#25269=PROPERTY_DEFINITION_REPRESENTATION(#25369,#25309);
#25270=PROPERTY_DEFINITION_REPRESENTATION(#25370,#25310);
#25271=PROPERTY_DEFINITION_REPRESENTATION(#25371,#25311);
#25272=PROPERTY_DEFINITION_REPRESENTATION(#25372,#25312);
#25273=PROPERTY_DEFINITION_REPRESENTATION(#25373,#25313);
#25274=PROPERTY_DEFINITION_REPRESENTATION(#25374,#25314);
#25275=PROPERTY_DEFINITION_REPRESENTATION(#25375,#25315);
#25276=PROPERTY_DEFINITION_REPRESENTATION(#25376,#25316);
#25277=PROPERTY_DEFINITION_REPRESENTATION(#25377,#25317);
#25278=PROPERTY_DEFINITION_REPRESENTATION(#25378,#25318);
#25279=PROPERTY_DEFINITION_REPRESENTATION(#25379,#25319);
#25280=PROPERTY_DEFINITION_REPRESENTATION(#25380,#25320);
#25281=PROPERTY_DEFINITION_REPRESENTATION(#25381,#25321);
#25282=PROPERTY_DEFINITION_REPRESENTATION(#25382,#25322);
#25283=PROPERTY_DEFINITION_REPRESENTATION(#25383,#25323);
#25284=PROPERTY_DEFINITION_REPRESENTATION(#25384,#25324);
#25285=PROPERTY_DEFINITION_REPRESENTATION(#25385,#25325);
#25286=PROPERTY_DEFINITION_REPRESENTATION(#25386,#25326);
#25287=PROPERTY_DEFINITION_REPRESENTATION(#25387,#25327);
#25288=PROPERTY_DEFINITION_REPRESENTATION(#25388,#25328);
#25289=PROPERTY_DEFINITION_REPRESENTATION(#25389,#25329);
#25290=PROPERTY_DEFINITION_REPRESENTATION(#25390,#25330);
#25291=REPRESENTATION('material name',(#25331),#259204);
#25292=REPRESENTATION('density',(#25231),#259204);
#25293=REPRESENTATION('material name',(#25332),#259205);
#25294=REPRESENTATION('density',(#25232),#259205);
#25295=REPRESENTATION('material name',(#25333),#259206);
#25296=REPRESENTATION('density',(#25233),#259206);
#25297=REPRESENTATION('material name',(#25334),#259207);
#25298=REPRESENTATION('density',(#25234),#259207);
#25299=REPRESENTATION('material name',(#25335),#259208);
#25300=REPRESENTATION('density',(#25235),#259208);
#25301=REPRESENTATION('material name',(#25336),#259209);
#25302=REPRESENTATION('density',(#25236),#259209);
#25303=REPRESENTATION('material name',(#25337),#259210);
#25304=REPRESENTATION('density',(#25237),#259210);
#25305=REPRESENTATION('material name',(#25338),#259211);
#25306=REPRESENTATION('density',(#25238),#259211);
#25307=REPRESENTATION('material name',(#25339),#259212);
#25308=REPRESENTATION('density',(#25239),#259212);
#25309=REPRESENTATION('material name',(#25340),#259213);
#25310=REPRESENTATION('density',(#25240),#259213);
#25311=REPRESENTATION('material name',(#25341),#259214);
#25312=REPRESENTATION('density',(#25241),#259214);
#25313=REPRESENTATION('material name',(#25342),#259215);
#25314=REPRESENTATION('density',(#25242),#259215);
#25315=REPRESENTATION('material name',(#25343),#259216);
#25316=REPRESENTATION('density',(#25243),#259216);
#25317=REPRESENTATION('material name',(#25344),#259217);
#25318=REPRESENTATION('density',(#25244),#259217);
#25319=REPRESENTATION('material name',(#25345),#259218);
#25320=REPRESENTATION('density',(#25245),#259218);
#25321=REPRESENTATION('material name',(#25346),#259219);
#25322=REPRESENTATION('density',(#25246),#259219);
#25323=REPRESENTATION('material name',(#25347),#259220);
#25324=REPRESENTATION('density',(#25247),#259220);
#25325=REPRESENTATION('material name',(#25348),#259221);
#25326=REPRESENTATION('density',(#25248),#259221);
#25327=REPRESENTATION('material name',(#25349),#259222);
#25328=REPRESENTATION('density',(#25249),#259222);
#25329=REPRESENTATION('material name',(#25350),#259223);
#25330=REPRESENTATION('density',(#25250),#259223);
#25331=DESCRIPTIVE_REPRESENTATION_ITEM('Steel','Steel');
#25332=DESCRIPTIVE_REPRESENTATION_ITEM('Steel','Steel');
#25333=DESCRIPTIVE_REPRESENTATION_ITEM('Steel','Steel');
#25334=DESCRIPTIVE_REPRESENTATION_ITEM('Steel','Steel');
#25335=DESCRIPTIVE_REPRESENTATION_ITEM('Steel','Steel');
#25336=DESCRIPTIVE_REPRESENTATION_ITEM('Steel','Steel');
#25337=DESCRIPTIVE_REPRESENTATION_ITEM('Steel','Steel');
#25338=DESCRIPTIVE_REPRESENTATION_ITEM('Copper, Alloy','Copper, Alloy');
#25339=DESCRIPTIVE_REPRESENTATION_ITEM('Steel','Steel');
#25340=DESCRIPTIVE_REPRESENTATION_ITEM('Steel','Steel');
#25341=DESCRIPTIVE_REPRESENTATION_ITEM('Copper, Alloy','Copper, Alloy');
#25342=DESCRIPTIVE_REPRESENTATION_ITEM('Steel','Steel');
#25343=DESCRIPTIVE_REPRESENTATION_ITEM('Steel','Steel');
#25344=DESCRIPTIVE_REPRESENTATION_ITEM('Steel','Steel');
#25345=DESCRIPTIVE_REPRESENTATION_ITEM('Copper, Alloy','Copper, Alloy');
#25346=DESCRIPTIVE_REPRESENTATION_ITEM('Copper, Alloy','Copper, Alloy');
#25347=DESCRIPTIVE_REPRESENTATION_ITEM('Steel','Steel');
#25348=DESCRIPTIVE_REPRESENTATION_ITEM('Steel','Steel');
#25349=DESCRIPTIVE_REPRESENTATION_ITEM('Steel','Steel');
#25350=DESCRIPTIVE_REPRESENTATION_ITEM('Steel','Steel');
#25351=PROPERTY_DEFINITION('material property','material name',#259392);
#25352=PROPERTY_DEFINITION('material property','density of part',#259392);
#25353=PROPERTY_DEFINITION('material property','material name',#259393);
#25354=PROPERTY_DEFINITION('material property','density of part',#259393);
#25355=PROPERTY_DEFINITION('material property','material name',#259394);
#25356=PROPERTY_DEFINITION('material property','density of part',#259394);
#25357=PROPERTY_DEFINITION('material property','material name',#259395);
#25358=PROPERTY_DEFINITION('material property','density of part',#259395);
#25359=PROPERTY_DEFINITION('material property','material name',#259396);
#25360=PROPERTY_DEFINITION('material property','density of part',#259396);
#25361=PROPERTY_DEFINITION('material property','material name',#259397);
#25362=PROPERTY_DEFINITION('material property','density of part',#259397);
#25363=PROPERTY_DEFINITION('material property','material name',#259398);
#25364=PROPERTY_DEFINITION('material property','density of part',#259398);
#25365=PROPERTY_DEFINITION('material property','material name',#259399);
#25366=PROPERTY_DEFINITION('material property','density of part',#259399);
#25367=PROPERTY_DEFINITION('material property','material name',#259400);
#25368=PROPERTY_DEFINITION('material property','density of part',#259400);
#25369=PROPERTY_DEFINITION('material property','material name',#259401);
#25370=PROPERTY_DEFINITION('material property','density of part',#259401);
#25371=PROPERTY_DEFINITION('material property','material name',#259402);
#25372=PROPERTY_DEFINITION('material property','density of part',#259402);
#25373=PROPERTY_DEFINITION('material property','material name',#259403);
#25374=PROPERTY_DEFINITION('material property','density of part',#259403);
#25375=PROPERTY_DEFINITION('material property','material name',#259404);
#25376=PROPERTY_DEFINITION('material property','density of part',#259404);
#25377=PROPERTY_DEFINITION('material property','material name',#259405);
#25378=PROPERTY_DEFINITION('material property','density of part',#259405);
#25379=PROPERTY_DEFINITION('material property','material name',#259406);
#25380=PROPERTY_DEFINITION('material property','density of part',#259406);
#25381=PROPERTY_DEFINITION('material property','material name',#259407);
#25382=PROPERTY_DEFINITION('material property','density of part',#259407);
#25383=PROPERTY_DEFINITION('material property','material name',#259408);
#25384=PROPERTY_DEFINITION('material property','density of part',#259408);
#25385=PROPERTY_DEFINITION('material property','material name',#259409);
#25386=PROPERTY_DEFINITION('material property','density of part',#259409);
#25387=PROPERTY_DEFINITION('material property','material name',#259410);
#25388=PROPERTY_DEFINITION('material property','density of part',#259410);
#25389=PROPERTY_DEFINITION('material property','material name',#259411);
#25390=PROPERTY_DEFINITION('material property','density of part',#259411);
#25391=AXIS2_PLACEMENT_3D('',#32405,#27334,#27335);
#25392=AXIS2_PLACEMENT_3D('',#32406,#27336,#27337);
#25393=AXIS2_PLACEMENT_3D('',#32407,#27338,#27339);
#25394=AXIS2_PLACEMENT_3D('',#32417,#27341,#27342);
#25395=AXIS2_PLACEMENT_3D('',#32420,#27344,#27345);
#25396=AXIS2_PLACEMENT_3D('',#32422,#27346,#27347);
#25397=AXIS2_PLACEMENT_3D('',#32433,#27348,#27349);
#25398=AXIS2_PLACEMENT_3D('',#32484,#27351,#27352);
#25399=AXIS2_PLACEMENT_3D('',#32535,#27354,#27355);
#25400=AXIS2_PLACEMENT_3D('',#32583,#27357,#27358);
#25401=AXIS2_PLACEMENT_3D('',#32634,#27360,#27361);
#25402=AXIS2_PLACEMENT_3D('',#32685,#27363,#27364);
#25403=AXIS2_PLACEMENT_3D('',#32733,#27366,#27367);
#25404=AXIS2_PLACEMENT_3D('',#32784,#27369,#27370);
#25405=AXIS2_PLACEMENT_3D('',#32835,#27372,#27373);
#25406=AXIS2_PLACEMENT_3D('',#32883,#27375,#27376);
#25407=AXIS2_PLACEMENT_3D('',#32934,#27378,#27379);
#25408=AXIS2_PLACEMENT_3D('',#32985,#27381,#27382);
#25409=AXIS2_PLACEMENT_3D('',#33033,#27384,#27385);
#25410=AXIS2_PLACEMENT_3D('',#33084,#27387,#27388);
#25411=AXIS2_PLACEMENT_3D('',#33103,#27390,#27391);
#25412=AXIS2_PLACEMENT_3D('',#33123,#27392,#27393);
#25413=AXIS2_PLACEMENT_3D('',#33137,#27395,#27396);
#25414=AXIS2_PLACEMENT_3D('',#33147,#27397,#27398);
#25415=AXIS2_PLACEMENT_3D('',#33171,#27400,#27401);
#25416=AXIS2_PLACEMENT_3D('',#33196,#27403,#27404);
#25417=AXIS2_PLACEMENT_3D('',#33221,#27406,#27407);
#25418=AXIS2_PLACEMENT_3D('',#33245,#27409,#27410);
#25419=AXIS2_PLACEMENT_3D('',#33270,#27412,#27413);
#25420=AXIS2_PLACEMENT_3D('',#33295,#27415,#27416);
#25421=AXIS2_PLACEMENT_3D('',#33319,#27418,#27419);
#25422=AXIS2_PLACEMENT_3D('',#33344,#27421,#27422);
#25423=AXIS2_PLACEMENT_3D('',#33369,#27424,#27425);
#25424=AXIS2_PLACEMENT_3D('',#33393,#27427,#27428);
#25425=AXIS2_PLACEMENT_3D('',#33418,#27430,#27431);
#25426=AXIS2_PLACEMENT_3D('',#33443,#27433,#27434);
#25427=AXIS2_PLACEMENT_3D('',#33467,#27436,#27437);
#25428=AXIS2_PLACEMENT_3D('',#33478,#27439,#27440);
#25429=AXIS2_PLACEMENT_3D('',#33484,#27441,#27442);
#25430=AXIS2_PLACEMENT_3D('',#33494,#27444,#27445);
#25431=AXIS2_PLACEMENT_3D('',#33497,#27447,#27448);
#25432=AXIS2_PLACEMENT_3D('',#33499,#27449,#27450);
#25433=AXIS2_PLACEMENT_3D('',#33510,#27451,#27452);
#25434=AXIS2_PLACEMENT_3D('',#33561,#27454,#27455);
#25435=AXIS2_PLACEMENT_3D('',#33612,#27457,#27458);
#25436=AXIS2_PLACEMENT_3D('',#33660,#27460,#27461);
#25437=AXIS2_PLACEMENT_3D('',#33711,#27463,#27464);
#25438=AXIS2_PLACEMENT_3D('',#33762,#27466,#27467);
#25439=AXIS2_PLACEMENT_3D('',#33810,#27469,#27470);
#25440=AXIS2_PLACEMENT_3D('',#33861,#27472,#27473);
#25441=AXIS2_PLACEMENT_3D('',#33912,#27475,#27476);
#25442=AXIS2_PLACEMENT_3D('',#33960,#27478,#27479);
#25443=AXIS2_PLACEMENT_3D('',#34011,#27481,#27482);
#25444=AXIS2_PLACEMENT_3D('',#34062,#27484,#27485);
#25445=AXIS2_PLACEMENT_3D('',#34110,#27487,#27488);
#25446=AXIS2_PLACEMENT_3D('',#34161,#27490,#27491);
#25447=AXIS2_PLACEMENT_3D('',#34180,#27493,#27494);
#25448=AXIS2_PLACEMENT_3D('',#34200,#27495,#27496);
#25449=AXIS2_PLACEMENT_3D('',#34214,#27498,#27499);
#25450=AXIS2_PLACEMENT_3D('',#34224,#27500,#27501);
#25451=AXIS2_PLACEMENT_3D('',#34248,#27503,#27504);
#25452=AXIS2_PLACEMENT_3D('',#34273,#27506,#27507);
#25453=AXIS2_PLACEMENT_3D('',#34298,#27509,#27510);
#25454=AXIS2_PLACEMENT_3D('',#34322,#27512,#27513);
#25455=AXIS2_PLACEMENT_3D('',#34347,#27515,#27516);
#25456=AXIS2_PLACEMENT_3D('',#34372,#27518,#27519);
#25457=AXIS2_PLACEMENT_3D('',#34396,#27521,#27522);
#25458=AXIS2_PLACEMENT_3D('',#34421,#27524,#27525);
#25459=AXIS2_PLACEMENT_3D('',#34446,#27527,#27528);
#25460=AXIS2_PLACEMENT_3D('',#34470,#27530,#27531);
#25461=AXIS2_PLACEMENT_3D('',#34495,#27533,#27534);
#25462=AXIS2_PLACEMENT_3D('',#34520,#27536,#27537);
#25463=AXIS2_PLACEMENT_3D('',#34544,#27539,#27540);
#25464=AXIS2_PLACEMENT_3D('',#34555,#27542,#27543);
#25465=AXIS2_PLACEMENT_3D('',#34561,#27544,#27545);
#25466=AXIS2_PLACEMENT_3D('',#34571,#27547,#27548);
#25467=AXIS2_PLACEMENT_3D('',#34574,#27550,#27551);
#25468=AXIS2_PLACEMENT_3D('',#34576,#27552,#27553);
#25469=AXIS2_PLACEMENT_3D('',#34587,#27554,#27555);
#25470=AXIS2_PLACEMENT_3D('',#34638,#27557,#27558);
#25471=AXIS2_PLACEMENT_3D('',#34689,#27560,#27561);
#25472=AXIS2_PLACEMENT_3D('',#34737,#27563,#27564);
#25473=AXIS2_PLACEMENT_3D('',#34788,#27566,#27567);
#25474=AXIS2_PLACEMENT_3D('',#34839,#27569,#27570);
#25475=AXIS2_PLACEMENT_3D('',#34887,#27572,#27573);
#25476=AXIS2_PLACEMENT_3D('',#34938,#27575,#27576);
#25477=AXIS2_PLACEMENT_3D('',#34989,#27578,#27579);
#25478=AXIS2_PLACEMENT_3D('',#35037,#27581,#27582);
#25479=AXIS2_PLACEMENT_3D('',#35088,#27584,#27585);
#25480=AXIS2_PLACEMENT_3D('',#35139,#27587,#27588);
#25481=AXIS2_PLACEMENT_3D('',#35187,#27590,#27591);
#25482=AXIS2_PLACEMENT_3D('',#35238,#27593,#27594);
#25483=AXIS2_PLACEMENT_3D('',#35257,#27596,#27597);
#25484=AXIS2_PLACEMENT_3D('',#35277,#27598,#27599);
#25485=AXIS2_PLACEMENT_3D('',#35291,#27601,#27602);
#25486=AXIS2_PLACEMENT_3D('',#35301,#27603,#27604);
#25487=AXIS2_PLACEMENT_3D('',#35325,#27606,#27607);
#25488=AXIS2_PLACEMENT_3D('',#35350,#27609,#27610);
#25489=AXIS2_PLACEMENT_3D('',#35375,#27612,#27613);
#25490=AXIS2_PLACEMENT_3D('',#35399,#27615,#27616);
#25491=AXIS2_PLACEMENT_3D('',#35424,#27618,#27619);
#25492=AXIS2_PLACEMENT_3D('',#35449,#27621,#27622);
#25493=AXIS2_PLACEMENT_3D('',#35473,#27624,#27625);
#25494=AXIS2_PLACEMENT_3D('',#35498,#27627,#27628);
#25495=AXIS2_PLACEMENT_3D('',#35523,#27630,#27631);
#25496=AXIS2_PLACEMENT_3D('',#35547,#27633,#27634);
#25497=AXIS2_PLACEMENT_3D('',#35572,#27636,#27637);
#25498=AXIS2_PLACEMENT_3D('',#35597,#27639,#27640);
#25499=AXIS2_PLACEMENT_3D('',#35621,#27642,#27643);
#25500=AXIS2_PLACEMENT_3D('',#35632,#27645,#27646);
#25501=AXIS2_PLACEMENT_3D('',#35638,#27647,#27648);
#25502=AXIS2_PLACEMENT_3D('',#35648,#27650,#27651);
#25503=AXIS2_PLACEMENT_3D('',#35651,#27653,#27654);
#25504=AXIS2_PLACEMENT_3D('',#35653,#27655,#27656);
#25505=AXIS2_PLACEMENT_3D('',#35664,#27657,#27658);
#25506=AXIS2_PLACEMENT_3D('',#35715,#27660,#27661);
#25507=AXIS2_PLACEMENT_3D('',#35766,#27663,#27664);
#25508=AXIS2_PLACEMENT_3D('',#35814,#27666,#27667);
#25509=AXIS2_PLACEMENT_3D('',#35865,#27669,#27670);
#25510=AXIS2_PLACEMENT_3D('',#35916,#27672,#27673);
#25511=AXIS2_PLACEMENT_3D('',#35964,#27675,#27676);
#25512=AXIS2_PLACEMENT_3D('',#36015,#27678,#27679);
#25513=AXIS2_PLACEMENT_3D('',#36066,#27681,#27682);
#25514=AXIS2_PLACEMENT_3D('',#36114,#27684,#27685);
#25515=AXIS2_PLACEMENT_3D('',#36165,#27687,#27688);
#25516=AXIS2_PLACEMENT_3D('',#36216,#27690,#27691);
#25517=AXIS2_PLACEMENT_3D('',#36264,#27693,#27694);
#25518=AXIS2_PLACEMENT_3D('',#36315,#27696,#27697);
#25519=AXIS2_PLACEMENT_3D('',#36334,#27699,#27700);
#25520=AXIS2_PLACEMENT_3D('',#36354,#27701,#27702);
#25521=AXIS2_PLACEMENT_3D('',#36368,#27704,#27705);
#25522=AXIS2_PLACEMENT_3D('',#36378,#27706,#27707);
#25523=AXIS2_PLACEMENT_3D('',#36402,#27709,#27710);
#25524=AXIS2_PLACEMENT_3D('',#36427,#27712,#27713);
#25525=AXIS2_PLACEMENT_3D('',#36452,#27715,#27716);
#25526=AXIS2_PLACEMENT_3D('',#36476,#27718,#27719);
#25527=AXIS2_PLACEMENT_3D('',#36501,#27721,#27722);
#25528=AXIS2_PLACEMENT_3D('',#36526,#27724,#27725);
#25529=AXIS2_PLACEMENT_3D('',#36550,#27727,#27728);
#25530=AXIS2_PLACEMENT_3D('',#36575,#27730,#27731);
#25531=AXIS2_PLACEMENT_3D('',#36600,#27733,#27734);
#25532=AXIS2_PLACEMENT_3D('',#36624,#27736,#27737);
#25533=AXIS2_PLACEMENT_3D('',#36649,#27739,#27740);
#25534=AXIS2_PLACEMENT_3D('',#36674,#27742,#27743);
#25535=AXIS2_PLACEMENT_3D('',#36698,#27745,#27746);
#25536=AXIS2_PLACEMENT_3D('',#36709,#27748,#27749);
#25537=AXIS2_PLACEMENT_3D('',#36715,#27750,#27751);
#25538=AXIS2_PLACEMENT_3D('',#36725,#27753,#27754);
#25539=AXIS2_PLACEMENT_3D('',#36728,#27756,#27757);
#25540=AXIS2_PLACEMENT_3D('',#36730,#27758,#27759);
#25541=AXIS2_PLACEMENT_3D('',#36741,#27760,#27761);
#25542=AXIS2_PLACEMENT_3D('',#36792,#27763,#27764);
#25543=AXIS2_PLACEMENT_3D('',#36843,#27766,#27767);
#25544=AXIS2_PLACEMENT_3D('',#36891,#27769,#27770);
#25545=AXIS2_PLACEMENT_3D('',#36942,#27772,#27773);
#25546=AXIS2_PLACEMENT_3D('',#36993,#27775,#27776);
#25547=AXIS2_PLACEMENT_3D('',#37041,#27778,#27779);
#25548=AXIS2_PLACEMENT_3D('',#37092,#27781,#27782);
#25549=AXIS2_PLACEMENT_3D('',#37143,#27784,#27785);
#25550=AXIS2_PLACEMENT_3D('',#37191,#27787,#27788);
#25551=AXIS2_PLACEMENT_3D('',#37242,#27790,#27791);
#25552=AXIS2_PLACEMENT_3D('',#37293,#27793,#27794);
#25553=AXIS2_PLACEMENT_3D('',#37341,#27796,#27797);
#25554=AXIS2_PLACEMENT_3D('',#37392,#27799,#27800);
#25555=AXIS2_PLACEMENT_3D('',#37411,#27802,#27803);
#25556=AXIS2_PLACEMENT_3D('',#37431,#27804,#27805);
#25557=AXIS2_PLACEMENT_3D('',#37445,#27807,#27808);
#25558=AXIS2_PLACEMENT_3D('',#37455,#27809,#27810);
#25559=AXIS2_PLACEMENT_3D('',#37479,#27812,#27813);
#25560=AXIS2_PLACEMENT_3D('',#37504,#27815,#27816);
#25561=AXIS2_PLACEMENT_3D('',#37529,#27818,#27819);
#25562=AXIS2_PLACEMENT_3D('',#37553,#27821,#27822);
#25563=AXIS2_PLACEMENT_3D('',#37578,#27824,#27825);
#25564=AXIS2_PLACEMENT_3D('',#37603,#27827,#27828);
#25565=AXIS2_PLACEMENT_3D('',#37627,#27830,#27831);
#25566=AXIS2_PLACEMENT_3D('',#37652,#27833,#27834);
#25567=AXIS2_PLACEMENT_3D('',#37677,#27836,#27837);
#25568=AXIS2_PLACEMENT_3D('',#37701,#27839,#27840);
#25569=AXIS2_PLACEMENT_3D('',#37726,#27842,#27843);
#25570=AXIS2_PLACEMENT_3D('',#37751,#27845,#27846);
#25571=AXIS2_PLACEMENT_3D('',#37775,#27848,#27849);
#25572=AXIS2_PLACEMENT_3D('',#37786,#27851,#27852);
#25573=AXIS2_PLACEMENT_3D('',#37792,#27853,#27854);
#25574=AXIS2_PLACEMENT_3D('',#37802,#27856,#27857);
#25575=AXIS2_PLACEMENT_3D('',#37805,#27859,#27860);
#25576=AXIS2_PLACEMENT_3D('',#37807,#27861,#27862);
#25577=AXIS2_PLACEMENT_3D('',#37818,#27863,#27864);
#25578=AXIS2_PLACEMENT_3D('',#37869,#27866,#27867);
#25579=AXIS2_PLACEMENT_3D('',#37920,#27869,#27870);
#25580=AXIS2_PLACEMENT_3D('',#37968,#27872,#27873);
#25581=AXIS2_PLACEMENT_3D('',#38019,#27875,#27876);
#25582=AXIS2_PLACEMENT_3D('',#38070,#27878,#27879);
#25583=AXIS2_PLACEMENT_3D('',#38118,#27881,#27882);
#25584=AXIS2_PLACEMENT_3D('',#38169,#27884,#27885);
#25585=AXIS2_PLACEMENT_3D('',#38220,#27887,#27888);
#25586=AXIS2_PLACEMENT_3D('',#38268,#27890,#27891);
#25587=AXIS2_PLACEMENT_3D('',#38319,#27893,#27894);
#25588=AXIS2_PLACEMENT_3D('',#38370,#27896,#27897);
#25589=AXIS2_PLACEMENT_3D('',#38418,#27899,#27900);
#25590=AXIS2_PLACEMENT_3D('',#38469,#27902,#27903);
#25591=AXIS2_PLACEMENT_3D('',#38488,#27905,#27906);
#25592=AXIS2_PLACEMENT_3D('',#38508,#27907,#27908);
#25593=AXIS2_PLACEMENT_3D('',#38522,#27910,#27911);
#25594=AXIS2_PLACEMENT_3D('',#38532,#27912,#27913);
#25595=AXIS2_PLACEMENT_3D('',#38556,#27915,#27916);
#25596=AXIS2_PLACEMENT_3D('',#38581,#27918,#27919);
#25597=AXIS2_PLACEMENT_3D('',#38606,#27921,#27922);
#25598=AXIS2_PLACEMENT_3D('',#38630,#27924,#27925);
#25599=AXIS2_PLACEMENT_3D('',#38655,#27927,#27928);
#25600=AXIS2_PLACEMENT_3D('',#38680,#27930,#27931);
#25601=AXIS2_PLACEMENT_3D('',#38704,#27933,#27934);
#25602=AXIS2_PLACEMENT_3D('',#38729,#27936,#27937);
#25603=AXIS2_PLACEMENT_3D('',#38754,#27939,#27940);
#25604=AXIS2_PLACEMENT_3D('',#38778,#27942,#27943);
#25605=AXIS2_PLACEMENT_3D('',#38803,#27945,#27946);
#25606=AXIS2_PLACEMENT_3D('',#38828,#27948,#27949);
#25607=AXIS2_PLACEMENT_3D('',#38852,#27951,#27952);
#25608=AXIS2_PLACEMENT_3D('',#38863,#27954,#27955);
#25609=AXIS2_PLACEMENT_3D('',#38869,#27956,#27957);
#25610=AXIS2_PLACEMENT_3D('',#38879,#27959,#27960);
#25611=AXIS2_PLACEMENT_3D('',#38882,#27962,#27963);
#25612=AXIS2_PLACEMENT_3D('',#38884,#27964,#27965);
#25613=AXIS2_PLACEMENT_3D('',#38895,#27966,#27967);
#25614=AXIS2_PLACEMENT_3D('',#38946,#27969,#27970);
#25615=AXIS2_PLACEMENT_3D('',#38997,#27972,#27973);
#25616=AXIS2_PLACEMENT_3D('',#39045,#27975,#27976);
#25617=AXIS2_PLACEMENT_3D('',#39096,#27978,#27979);
#25618=AXIS2_PLACEMENT_3D('',#39147,#27981,#27982);
#25619=AXIS2_PLACEMENT_3D('',#39195,#27984,#27985);
#25620=AXIS2_PLACEMENT_3D('',#39246,#27987,#27988);
#25621=AXIS2_PLACEMENT_3D('',#39297,#27990,#27991);
#25622=AXIS2_PLACEMENT_3D('',#39345,#27993,#27994);
#25623=AXIS2_PLACEMENT_3D('',#39396,#27996,#27997);
#25624=AXIS2_PLACEMENT_3D('',#39447,#27999,#28000);
#25625=AXIS2_PLACEMENT_3D('',#39495,#28002,#28003);
#25626=AXIS2_PLACEMENT_3D('',#39546,#28005,#28006);
#25627=AXIS2_PLACEMENT_3D('',#39565,#28008,#28009);
#25628=AXIS2_PLACEMENT_3D('',#39585,#28010,#28011);
#25629=AXIS2_PLACEMENT_3D('',#39599,#28013,#28014);
#25630=AXIS2_PLACEMENT_3D('',#39609,#28015,#28016);
#25631=AXIS2_PLACEMENT_3D('',#39633,#28018,#28019);
#25632=AXIS2_PLACEMENT_3D('',#39658,#28021,#28022);
#25633=AXIS2_PLACEMENT_3D('',#39683,#28024,#28025);
#25634=AXIS2_PLACEMENT_3D('',#39707,#28027,#28028);
#25635=AXIS2_PLACEMENT_3D('',#39732,#28030,#28031);
#25636=AXIS2_PLACEMENT_3D('',#39757,#28033,#28034);
#25637=AXIS2_PLACEMENT_3D('',#39781,#28036,#28037);
#25638=AXIS2_PLACEMENT_3D('',#39806,#28039,#28040);
#25639=AXIS2_PLACEMENT_3D('',#39831,#28042,#28043);
#25640=AXIS2_PLACEMENT_3D('',#39855,#28045,#28046);
#25641=AXIS2_PLACEMENT_3D('',#39880,#28048,#28049);
#25642=AXIS2_PLACEMENT_3D('',#39905,#28051,#28052);
#25643=AXIS2_PLACEMENT_3D('',#39929,#28054,#28055);
#25644=AXIS2_PLACEMENT_3D('',#39940,#28057,#28058);
#25645=AXIS2_PLACEMENT_3D('',#39946,#28059,#28060);
#25646=AXIS2_PLACEMENT_3D('',#39956,#28062,#28063);
#25647=AXIS2_PLACEMENT_3D('',#39959,#28065,#28066);
#25648=AXIS2_PLACEMENT_3D('',#39961,#28067,#28068);
#25649=AXIS2_PLACEMENT_3D('',#39972,#28069,#28070);
#25650=AXIS2_PLACEMENT_3D('',#40023,#28072,#28073);
#25651=AXIS2_PLACEMENT_3D('',#40074,#28075,#28076);
#25652=AXIS2_PLACEMENT_3D('',#40122,#28078,#28079);
#25653=AXIS2_PLACEMENT_3D('',#40173,#28081,#28082);
#25654=AXIS2_PLACEMENT_3D('',#40224,#28084,#28085);
#25655=AXIS2_PLACEMENT_3D('',#40272,#28087,#28088);
#25656=AXIS2_PLACEMENT_3D('',#40323,#28090,#28091);
#25657=AXIS2_PLACEMENT_3D('',#40374,#28093,#28094);
#25658=AXIS2_PLACEMENT_3D('',#40422,#28096,#28097);
#25659=AXIS2_PLACEMENT_3D('',#40473,#28099,#28100);
#25660=AXIS2_PLACEMENT_3D('',#40524,#28102,#28103);
#25661=AXIS2_PLACEMENT_3D('',#40572,#28105,#28106);
#25662=AXIS2_PLACEMENT_3D('',#40623,#28108,#28109);
#25663=AXIS2_PLACEMENT_3D('',#40642,#28111,#28112);
#25664=AXIS2_PLACEMENT_3D('',#40662,#28113,#28114);
#25665=AXIS2_PLACEMENT_3D('',#40676,#28116,#28117);
#25666=AXIS2_PLACEMENT_3D('',#40686,#28118,#28119);
#25667=AXIS2_PLACEMENT_3D('',#40710,#28121,#28122);
#25668=AXIS2_PLACEMENT_3D('',#40735,#28124,#28125);
#25669=AXIS2_PLACEMENT_3D('',#40760,#28127,#28128);
#25670=AXIS2_PLACEMENT_3D('',#40784,#28130,#28131);
#25671=AXIS2_PLACEMENT_3D('',#40809,#28133,#28134);
#25672=AXIS2_PLACEMENT_3D('',#40834,#28136,#28137);
#25673=AXIS2_PLACEMENT_3D('',#40858,#28139,#28140);
#25674=AXIS2_PLACEMENT_3D('',#40883,#28142,#28143);
#25675=AXIS2_PLACEMENT_3D('',#40908,#28145,#28146);
#25676=AXIS2_PLACEMENT_3D('',#40932,#28148,#28149);
#25677=AXIS2_PLACEMENT_3D('',#40957,#28151,#28152);
#25678=AXIS2_PLACEMENT_3D('',#40982,#28154,#28155);
#25679=AXIS2_PLACEMENT_3D('',#41006,#28157,#28158);
#25680=AXIS2_PLACEMENT_3D('',#41017,#28160,#28161);
#25681=AXIS2_PLACEMENT_3D('',#41023,#28162,#28163);
#25682=AXIS2_PLACEMENT_3D('',#41102,#28165,#28166);
#25683=AXIS2_PLACEMENT_3D('',#41181,#28168,#28169);
#25684=AXIS2_PLACEMENT_3D('',#41265,#28171,#28172);
#25685=AXIS2_PLACEMENT_3D('',#41343,#28174,#28175);
#25686=AXIS2_PLACEMENT_3D('',#41422,#28177,#28178);
#25687=AXIS2_PLACEMENT_3D('',#41501,#28180,#28181);
#25688=AXIS2_PLACEMENT_3D('',#41585,#28183,#28184);
#25689=AXIS2_PLACEMENT_3D('',#41663,#28186,#28187);
#25690=AXIS2_PLACEMENT_3D('',#41742,#28189,#28190);
#25691=AXIS2_PLACEMENT_3D('',#41821,#28192,#28193);
#25692=AXIS2_PLACEMENT_3D('',#41905,#28195,#28196);
#25693=AXIS2_PLACEMENT_3D('',#41983,#28198,#28199);
#25694=AXIS2_PLACEMENT_3D('',#42175,#28200,#28201);
#25695=AXIS2_PLACEMENT_3D('',#43229,#28202,#28203);
#25696=AXIS2_PLACEMENT_3D('',#43230,#28204,#28205);
#25697=AXIS2_PLACEMENT_3D('',#43422,#28206,#28207);
#25698=AXIS2_PLACEMENT_3D('',#44476,#28208,#28209);
#25699=AXIS2_PLACEMENT_3D('',#44477,#28210,#28211);
#25700=AXIS2_PLACEMENT_3D('',#44669,#28212,#28213);
#25701=AXIS2_PLACEMENT_3D('',#45723,#28214,#28215);
#25702=AXIS2_PLACEMENT_3D('',#45724,#28216,#28217);
#25703=AXIS2_PLACEMENT_3D('',#45916,#28218,#28219);
#25704=AXIS2_PLACEMENT_3D('',#46970,#28220,#28221);
#25705=AXIS2_PLACEMENT_3D('',#46971,#28222,#28223);
#25706=AXIS2_PLACEMENT_3D('',#47163,#28224,#28225);
#25707=AXIS2_PLACEMENT_3D('',#48217,#28226,#28227);
#25708=AXIS2_PLACEMENT_3D('',#48218,#28228,#28229);
#25709=AXIS2_PLACEMENT_3D('',#48410,#28230,#28231);
#25710=AXIS2_PLACEMENT_3D('',#49464,#28232,#28233);
#25711=AXIS2_PLACEMENT_3D('',#49465,#28234,#28235);
#25712=AXIS2_PLACEMENT_3D('',#49657,#28236,#28237);
#25713=AXIS2_PLACEMENT_3D('',#50711,#28238,#28239);
#25714=AXIS2_PLACEMENT_3D('',#50712,#28240,#28241);
#25715=AXIS2_PLACEMENT_3D('',#50904,#28242,#28243);
#25716=AXIS2_PLACEMENT_3D('',#51958,#28244,#28245);
#25717=AXIS2_PLACEMENT_3D('',#51959,#28246,#28247);
#25718=AXIS2_PLACEMENT_3D('',#51960,#28248,#28249);
#25719=AXIS2_PLACEMENT_3D('',#51961,#28250,#28251);
#25720=AXIS2_PLACEMENT_3D('',#51962,#28252,#28253);
#25721=AXIS2_PLACEMENT_3D('',#51963,#28254,#28255);
#25722=AXIS2_PLACEMENT_3D('',#51964,#28256,#28257);
#25723=AXIS2_PLACEMENT_3D('',#51965,#28258,#28259);
#25724=AXIS2_PLACEMENT_3D('',#51966,#28260,#28261);
#25725=AXIS2_PLACEMENT_3D('',#51967,#28262,#28263);
#25726=AXIS2_PLACEMENT_3D('',#51969,#28264,#28265);
#25727=AXIS2_PLACEMENT_3D('',#51972,#28267,#28268);
#25728=AXIS2_PLACEMENT_3D('',#51973,#28269,#28270);
#25729=AXIS2_PLACEMENT_3D('',#51975,#28271,#28272);
#25730=AXIS2_PLACEMENT_3D('',#51978,#28274,#28275);
#25731=AXIS2_PLACEMENT_3D('',#51979,#28276,#28277);
#25732=AXIS2_PLACEMENT_3D('',#51981,#28278,#28279);
#25733=AXIS2_PLACEMENT_3D('',#51984,#28281,#28282);
#25734=AXIS2_PLACEMENT_3D('',#51985,#28283,#28284);
#25735=AXIS2_PLACEMENT_3D('',#51987,#28285,#28286);
#25736=AXIS2_PLACEMENT_3D('',#51990,#28288,#28289);
#25737=AXIS2_PLACEMENT_3D('',#51991,#28290,#28291);
#25738=AXIS2_PLACEMENT_3D('',#51993,#28292,#28293);
#25739=AXIS2_PLACEMENT_3D('',#51996,#28295,#28296);
#25740=AXIS2_PLACEMENT_3D('',#51997,#28297,#28298);
#25741=AXIS2_PLACEMENT_3D('',#51999,#28299,#28300);
#25742=AXIS2_PLACEMENT_3D('',#52000,#28301,#28302);
#25743=AXIS2_PLACEMENT_3D('',#52002,#28303,#28304);
#25744=AXIS2_PLACEMENT_3D('',#52008,#28309,#28310);
#25745=AXIS2_PLACEMENT_3D('',#52009,#28311,#28312);
#25746=AXIS2_PLACEMENT_3D('',#52011,#28313,#28314);
#25747=AXIS2_PLACEMENT_3D('',#52017,#28319,#28320);
#25748=AXIS2_PLACEMENT_3D('',#52018,#28321,#28322);
#25749=AXIS2_PLACEMENT_3D('',#52019,#28323,#28324);
#25750=AXIS2_PLACEMENT_3D('',#52021,#28325,#28326);
#25751=AXIS2_PLACEMENT_3D('',#52022,#28327,#28328);
#25752=AXIS2_PLACEMENT_3D('',#52025,#28330,#28331);
#25753=AXIS2_PLACEMENT_3D('',#52026,#28332,#28333);
#25754=AXIS2_PLACEMENT_3D('',#52029,#28335,#28336);
#25755=AXIS2_PLACEMENT_3D('',#52030,#28337,#28338);
#25756=AXIS2_PLACEMENT_3D('',#52031,#28339,#28340);
#25757=AXIS2_PLACEMENT_3D('',#52032,#28341,#28342);
#25758=AXIS2_PLACEMENT_3D('',#52033,#28343,#28344);
#25759=AXIS2_PLACEMENT_3D('',#52056,#28346,#28347);
#25760=AXIS2_PLACEMENT_3D('',#52076,#28348,#28349);
#25761=AXIS2_PLACEMENT_3D('',#52077,#28350,#28351);
#25762=AXIS2_PLACEMENT_3D('',#52119,#28353,#28354);
#25763=AXIS2_PLACEMENT_3D('',#52120,#28355,#28356);
#25764=AXIS2_PLACEMENT_3D('',#52121,#28357,#28358);
#25765=AXIS2_PLACEMENT_3D('',#52155,#28360,#28361);
#25766=AXIS2_PLACEMENT_3D('',#52166,#28362,#28363);
#25767=AXIS2_PLACEMENT_3D('',#52167,#28364,#28365);
#25768=AXIS2_PLACEMENT_3D('',#52201,#28367,#28368);
#25769=AXIS2_PLACEMENT_3D('',#52212,#28369,#28370);
#25770=AXIS2_PLACEMENT_3D('',#52213,#28371,#28372);
#25771=AXIS2_PLACEMENT_3D('',#52215,#28373,#28374);
#25772=AXIS2_PLACEMENT_3D('',#52218,#28376,#28377);
#25773=AXIS2_PLACEMENT_3D('',#52219,#28378,#28379);
#25774=AXIS2_PLACEMENT_3D('',#52221,#28380,#28381);
#25775=AXIS2_PLACEMENT_3D('',#52225,#28384,#28385);
#25776=AXIS2_PLACEMENT_3D('',#52226,#28386,#28387);
#25777=AXIS2_PLACEMENT_3D('',#52227,#28388,#28389);
#25778=AXIS2_PLACEMENT_3D('',#52228,#28390,#28391);
#25779=AXIS2_PLACEMENT_3D('',#52229,#28392,#28393);
#25780=AXIS2_PLACEMENT_3D('',#52231,#28394,#28395);
#25781=AXIS2_PLACEMENT_3D('',#52234,#28397,#28398);
#25782=AXIS2_PLACEMENT_3D('',#52235,#28399,#28400);
#25783=AXIS2_PLACEMENT_3D('',#52237,#28401,#28402);
#25784=AXIS2_PLACEMENT_3D('',#52240,#28404,#28405);
#25785=AXIS2_PLACEMENT_3D('',#52241,#28406,#28407);
#25786=AXIS2_PLACEMENT_3D('',#52243,#28408,#28409);
#25787=AXIS2_PLACEMENT_3D('',#52246,#28411,#28412);
#25788=AXIS2_PLACEMENT_3D('',#52247,#28413,#28414);
#25789=AXIS2_PLACEMENT_3D('',#52249,#28415,#28416);
#25790=AXIS2_PLACEMENT_3D('',#52252,#28418,#28419);
#25791=AXIS2_PLACEMENT_3D('',#52253,#28420,#28421);
#25792=AXIS2_PLACEMENT_3D('',#52255,#28422,#28423);
#25793=AXIS2_PLACEMENT_3D('',#52258,#28425,#28426);
#25794=AXIS2_PLACEMENT_3D('',#52259,#28427,#28428);
#25795=AXIS2_PLACEMENT_3D('',#52261,#28429,#28430);
#25796=AXIS2_PLACEMENT_3D('',#52264,#28432,#28433);
#25797=AXIS2_PLACEMENT_3D('',#52265,#28434,#28435);
#25798=AXIS2_PLACEMENT_3D('',#52267,#28436,#28437);
#25799=AXIS2_PLACEMENT_3D('',#52270,#28439,#28440);
#25800=AXIS2_PLACEMENT_3D('',#52271,#28441,#28442);
#25801=AXIS2_PLACEMENT_3D('',#52273,#28443,#28444);
#25802=AXIS2_PLACEMENT_3D('',#52276,#28446,#28447);
#25803=AXIS2_PLACEMENT_3D('',#52277,#28448,#28449);
#25804=AXIS2_PLACEMENT_3D('',#52279,#28450,#28451);
#25805=AXIS2_PLACEMENT_3D('',#52282,#28453,#28454);
#25806=AXIS2_PLACEMENT_3D('',#52283,#28455,#28456);
#25807=AXIS2_PLACEMENT_3D('',#52285,#28457,#28458);
#25808=AXIS2_PLACEMENT_3D('',#52288,#28460,#28461);
#25809=AXIS2_PLACEMENT_3D('',#52289,#28462,#28463);
#25810=AXIS2_PLACEMENT_3D('',#52290,#28464,#28465);
#25811=AXIS2_PLACEMENT_3D('',#52291,#28466,#28467);
#25812=AXIS2_PLACEMENT_3D('',#52292,#28468,#28469);
#25813=AXIS2_PLACEMENT_3D('',#52301,#28474,#28475);
#25814=AXIS2_PLACEMENT_3D('',#52303,#28476,#28477);
#25815=AXIS2_PLACEMENT_3D('',#52307,#28480,#28481);
#25816=AXIS2_PLACEMENT_3D('',#52313,#28485,#28486);
#25817=AXIS2_PLACEMENT_3D('',#52315,#28488,#28489);
#25818=AXIS2_PLACEMENT_3D('',#52316,#28490,#28491);
#25819=AXIS2_PLACEMENT_3D('',#52317,#28492,#28493);
#25820=AXIS2_PLACEMENT_3D('',#52319,#28494,#28495);
#25821=AXIS2_PLACEMENT_3D('',#52322,#28497,#28498);
#25822=AXIS2_PLACEMENT_3D('',#52323,#28499,#28500);
#25823=AXIS2_PLACEMENT_3D('',#52325,#28501,#28502);
#25824=AXIS2_PLACEMENT_3D('',#52326,#28503,#28504);
#25825=AXIS2_PLACEMENT_3D('',#52328,#28505,#28506);
#25826=AXIS2_PLACEMENT_3D('',#52329,#28507,#28508);
#25827=AXIS2_PLACEMENT_3D('',#52331,#28509,#28510);
#25828=AXIS2_PLACEMENT_3D('',#52333,#28512,#28513);
#25829=AXIS2_PLACEMENT_3D('',#52335,#28514,#28515);
#25830=AXIS2_PLACEMENT_3D('',#52338,#28517,#28518);
#25831=AXIS2_PLACEMENT_3D('',#52339,#28519,#28520);
#25832=AXIS2_PLACEMENT_3D('',#52341,#28521,#28522);
#25833=AXIS2_PLACEMENT_3D('',#52342,#28523,#28524);
#25834=AXIS2_PLACEMENT_3D('',#52344,#28525,#28526);
#25835=AXIS2_PLACEMENT_3D('',#52345,#28527,#28528);
#25836=AXIS2_PLACEMENT_3D('',#52347,#28529,#28530);
#25837=AXIS2_PLACEMENT_3D('',#52349,#28532,#28533);
#25838=AXIS2_PLACEMENT_3D('',#52351,#28534,#28535);
#25839=AXIS2_PLACEMENT_3D('',#52353,#28536,#28537);
#25840=AXIS2_PLACEMENT_3D('',#52354,#28538,#28539);
#25841=AXIS2_PLACEMENT_3D('',#52356,#28540,#28541);
#25842=AXIS2_PLACEMENT_3D('',#52358,#28542,#28543);
#25843=AXIS2_PLACEMENT_3D('',#52359,#28544,#28545);
#25844=AXIS2_PLACEMENT_3D('',#52361,#28547,#28548);
#25845=AXIS2_PLACEMENT_3D('',#52364,#28550,#28551);
#25846=AXIS2_PLACEMENT_3D('',#52365,#28552,#28553);
#25847=AXIS2_PLACEMENT_3D('',#52367,#28554,#28555);
#25848=AXIS2_PLACEMENT_3D('',#52369,#28556,#28557);
#25849=AXIS2_PLACEMENT_3D('',#52370,#28558,#28559);
#25850=AXIS2_PLACEMENT_3D('',#52372,#28560,#28561);
#25851=AXIS2_PLACEMENT_3D('',#52373,#28562,#28563);
#25852=AXIS2_PLACEMENT_3D('',#52375,#28565,#28566);
#25853=AXIS2_PLACEMENT_3D('',#52378,#28568,#28569);
#25854=AXIS2_PLACEMENT_3D('',#52379,#28570,#28571);
#25855=AXIS2_PLACEMENT_3D('',#52381,#28573,#28574);
#25856=AXIS2_PLACEMENT_3D('',#52382,#28575,#28576);
#25857=AXIS2_PLACEMENT_3D('',#52384,#28577,#28578);
#25858=AXIS2_PLACEMENT_3D('',#52387,#28580,#28581);
#25859=AXIS2_PLACEMENT_3D('',#52388,#28582,#28583);
#25860=AXIS2_PLACEMENT_3D('',#52389,#28584,#28585);
#25861=AXIS2_PLACEMENT_3D('',#52391,#28586,#28587);
#25862=AXIS2_PLACEMENT_3D('',#52393,#28589,#28590);
#25863=AXIS2_PLACEMENT_3D('',#52394,#28591,#28592);
#25864=AXIS2_PLACEMENT_3D('',#52395,#28593,#28594);
#25865=AXIS2_PLACEMENT_3D('',#52396,#28595,#28596);
#25866=AXIS2_PLACEMENT_3D('',#52419,#28598,#28599);
#25867=AXIS2_PLACEMENT_3D('',#52439,#28600,#28601);
#25868=AXIS2_PLACEMENT_3D('',#52440,#28602,#28603);
#25869=AXIS2_PLACEMENT_3D('',#52482,#28605,#28606);
#25870=AXIS2_PLACEMENT_3D('',#52483,#28607,#28608);
#25871=AXIS2_PLACEMENT_3D('',#52484,#28609,#28610);
#25872=AXIS2_PLACEMENT_3D('',#52518,#28612,#28613);
#25873=AXIS2_PLACEMENT_3D('',#52529,#28614,#28615);
#25874=AXIS2_PLACEMENT_3D('',#52530,#28616,#28617);
#25875=AXIS2_PLACEMENT_3D('',#52564,#28619,#28620);
#25876=AXIS2_PLACEMENT_3D('',#52575,#28621,#28622);
#25877=AXIS2_PLACEMENT_3D('',#53469,#28624,#28625);
#25878=AXIS2_PLACEMENT_3D('',#53470,#28626,#28627);
#25879=AXIS2_PLACEMENT_3D('',#53471,#28628,#28629);
#25880=AXIS2_PLACEMENT_3D('',#54365,#28631,#28632);
#25881=AXIS2_PLACEMENT_3D('',#54366,#28633,#28634);
#25882=AXIS2_PLACEMENT_3D('',#54367,#28635,#28636);
#25883=AXIS2_PLACEMENT_3D('',#55261,#28638,#28639);
#25884=AXIS2_PLACEMENT_3D('',#55262,#28640,#28641);
#25885=AXIS2_PLACEMENT_3D('',#55263,#28642,#28643);
#25886=AXIS2_PLACEMENT_3D('',#56157,#28645,#28646);
#25887=AXIS2_PLACEMENT_3D('',#56158,#28647,#28648);
#25888=AXIS2_PLACEMENT_3D('',#56159,#28649,#28650);
#25889=AXIS2_PLACEMENT_3D('',#57053,#28652,#28653);
#25890=AXIS2_PLACEMENT_3D('',#57054,#28654,#28655);
#25891=AXIS2_PLACEMENT_3D('',#57055,#28656,#28657);
#25892=AXIS2_PLACEMENT_3D('',#57949,#28659,#28660);
#25893=AXIS2_PLACEMENT_3D('',#57950,#28661,#28662);
#25894=AXIS2_PLACEMENT_3D('',#57951,#28663,#28664);
#25895=AXIS2_PLACEMENT_3D('',#58845,#28666,#28667);
#25896=AXIS2_PLACEMENT_3D('',#58846,#28668,#28669);
#25897=AXIS2_PLACEMENT_3D('',#58847,#28670,#28671);
#25898=AXIS2_PLACEMENT_3D('',#59741,#28673,#28674);
#25899=AXIS2_PLACEMENT_3D('',#59742,#28675,#28676);
#25900=AXIS2_PLACEMENT_3D('',#59743,#28677,#28678);
#25901=AXIS2_PLACEMENT_3D('',#60637,#28680,#28681);
#25902=AXIS2_PLACEMENT_3D('',#60638,#28682,#28683);
#25903=AXIS2_PLACEMENT_3D('',#60639,#28684,#28685);
#25904=AXIS2_PLACEMENT_3D('',#61533,#28687,#28688);
#25905=AXIS2_PLACEMENT_3D('',#61534,#28689,#28690);
#25906=AXIS2_PLACEMENT_3D('',#61535,#28691,#28692);
#25907=AXIS2_PLACEMENT_3D('',#62429,#28694,#28695);
#25908=AXIS2_PLACEMENT_3D('',#62430,#28696,#28697);
#25909=AXIS2_PLACEMENT_3D('',#62431,#28698,#28699);
#25910=AXIS2_PLACEMENT_3D('',#63325,#28701,#28702);
#25911=AXIS2_PLACEMENT_3D('',#63326,#28703,#28704);
#25912=AXIS2_PLACEMENT_3D('',#63327,#28705,#28706);
#25913=AXIS2_PLACEMENT_3D('',#64221,#28708,#28709);
#25914=AXIS2_PLACEMENT_3D('',#64222,#28710,#28711);
#25915=AXIS2_PLACEMENT_3D('',#64223,#28712,#28713);
#25916=AXIS2_PLACEMENT_3D('',#65117,#28715,#28716);
#25917=AXIS2_PLACEMENT_3D('',#65118,#28717,#28718);
#25918=AXIS2_PLACEMENT_3D('',#65119,#28719,#28720);
#25919=AXIS2_PLACEMENT_3D('',#66013,#28722,#28723);
#25920=AXIS2_PLACEMENT_3D('',#66014,#28724,#28725);
#25921=AXIS2_PLACEMENT_3D('',#66015,#28726,#28727);
#25922=AXIS2_PLACEMENT_3D('',#66909,#28729,#28730);
#25923=AXIS2_PLACEMENT_3D('',#66910,#28731,#28732);
#25924=AXIS2_PLACEMENT_3D('',#66911,#28733,#28734);
#25925=AXIS2_PLACEMENT_3D('',#67805,#28736,#28737);
#25926=AXIS2_PLACEMENT_3D('',#67806,#28738,#28739);
#25927=AXIS2_PLACEMENT_3D('',#67807,#28740,#28741);
#25928=AXIS2_PLACEMENT_3D('',#68701,#28743,#28744);
#25929=AXIS2_PLACEMENT_3D('',#68702,#28745,#28746);
#25930=AXIS2_PLACEMENT_3D('',#68703,#28747,#28748);
#25931=AXIS2_PLACEMENT_3D('',#69597,#28750,#28751);
#25932=AXIS2_PLACEMENT_3D('',#69598,#28752,#28753);
#25933=AXIS2_PLACEMENT_3D('',#69599,#28754,#28755);
#25934=AXIS2_PLACEMENT_3D('',#70493,#28757,#28758);
#25935=AXIS2_PLACEMENT_3D('',#70494,#28759,#28760);
#25936=AXIS2_PLACEMENT_3D('',#70495,#28761,#28762);
#25937=AXIS2_PLACEMENT_3D('',#71389,#28764,#28765);
#25938=AXIS2_PLACEMENT_3D('',#71390,#28766,#28767);
#25939=AXIS2_PLACEMENT_3D('',#71391,#28768,#28769);
#25940=AXIS2_PLACEMENT_3D('',#72285,#28771,#28772);
#25941=AXIS2_PLACEMENT_3D('',#72286,#28773,#28774);
#25942=AXIS2_PLACEMENT_3D('',#72287,#28775,#28776);
#25943=AXIS2_PLACEMENT_3D('',#73181,#28778,#28779);
#25944=AXIS2_PLACEMENT_3D('',#73182,#28780,#28781);
#25945=AXIS2_PLACEMENT_3D('',#73183,#28782,#28783);
#25946=AXIS2_PLACEMENT_3D('',#74077,#28785,#28786);
#25947=AXIS2_PLACEMENT_3D('',#74078,#28787,#28788);
#25948=AXIS2_PLACEMENT_3D('',#74079,#28789,#28790);
#25949=AXIS2_PLACEMENT_3D('',#74973,#28792,#28793);
#25950=AXIS2_PLACEMENT_3D('',#74974,#28794,#28795);
#25951=AXIS2_PLACEMENT_3D('',#74975,#28796,#28797);
#25952=AXIS2_PLACEMENT_3D('',#75869,#28799,#28800);
#25953=AXIS2_PLACEMENT_3D('',#75870,#28801,#28802);
#25954=AXIS2_PLACEMENT_3D('',#75871,#28803,#28804);
#25955=AXIS2_PLACEMENT_3D('',#76765,#28806,#28807);
#25956=AXIS2_PLACEMENT_3D('',#76766,#28808,#28809);
#25957=AXIS2_PLACEMENT_3D('',#76767,#28810,#28811);
#25958=AXIS2_PLACEMENT_3D('',#77661,#28813,#28814);
#25959=AXIS2_PLACEMENT_3D('',#77662,#28815,#28816);
#25960=AXIS2_PLACEMENT_3D('',#77663,#28817,#28818);
#25961=AXIS2_PLACEMENT_3D('',#78557,#28820,#28821);
#25962=AXIS2_PLACEMENT_3D('',#78558,#28822,#28823);
#25963=AXIS2_PLACEMENT_3D('',#78559,#28824,#28825);
#25964=AXIS2_PLACEMENT_3D('',#79453,#28827,#28828);
#25965=AXIS2_PLACEMENT_3D('',#79454,#28829,#28830);
#25966=AXIS2_PLACEMENT_3D('',#79455,#28831,#28832);
#25967=AXIS2_PLACEMENT_3D('',#80349,#28834,#28835);
#25968=AXIS2_PLACEMENT_3D('',#80350,#28836,#28837);
#25969=AXIS2_PLACEMENT_3D('',#80351,#28838,#28839);
#25970=AXIS2_PLACEMENT_3D('',#81245,#28841,#28842);
#25971=AXIS2_PLACEMENT_3D('',#81246,#28843,#28844);
#25972=AXIS2_PLACEMENT_3D('',#81247,#28845,#28846);
#25973=AXIS2_PLACEMENT_3D('',#82141,#28848,#28849);
#25974=AXIS2_PLACEMENT_3D('',#82142,#28850,#28851);
#25975=AXIS2_PLACEMENT_3D('',#82143,#28852,#28853);
#25976=AXIS2_PLACEMENT_3D('',#83037,#28855,#28856);
#25977=AXIS2_PLACEMENT_3D('',#83038,#28857,#28858);
#25978=AXIS2_PLACEMENT_3D('',#83039,#28859,#28860);
#25979=AXIS2_PLACEMENT_3D('',#83933,#28862,#28863);
#25980=AXIS2_PLACEMENT_3D('',#83934,#28864,#28865);
#25981=AXIS2_PLACEMENT_3D('',#83935,#28866,#28867);
#25982=AXIS2_PLACEMENT_3D('',#84829,#28869,#28870);
#25983=AXIS2_PLACEMENT_3D('',#84830,#28871,#28872);
#25984=AXIS2_PLACEMENT_3D('',#84831,#28873,#28874);
#25985=AXIS2_PLACEMENT_3D('',#85725,#28876,#28877);
#25986=AXIS2_PLACEMENT_3D('',#85726,#28878,#28879);
#25987=AXIS2_PLACEMENT_3D('',#85727,#28880,#28881);
#25988=AXIS2_PLACEMENT_3D('',#86621,#28883,#28884);
#25989=AXIS2_PLACEMENT_3D('',#86622,#28885,#28886);
#25990=AXIS2_PLACEMENT_3D('',#86623,#28887,#28888);
#25991=AXIS2_PLACEMENT_3D('',#87517,#28890,#28891);
#25992=AXIS2_PLACEMENT_3D('',#87518,#28892,#28893);
#25993=AXIS2_PLACEMENT_3D('',#87519,#28894,#28895);
#25994=AXIS2_PLACEMENT_3D('',#88413,#28897,#28898);
#25995=AXIS2_PLACEMENT_3D('',#88414,#28899,#28900);
#25996=AXIS2_PLACEMENT_3D('',#88415,#28901,#28902);
#25997=AXIS2_PLACEMENT_3D('',#89309,#28904,#28905);
#25998=AXIS2_PLACEMENT_3D('',#89310,#28906,#28907);
#25999=AXIS2_PLACEMENT_3D('',#89311,#28908,#28909);
#26000=AXIS2_PLACEMENT_3D('',#90205,#28911,#28912);
#26001=AXIS2_PLACEMENT_3D('',#90206,#28913,#28914);
#26002=AXIS2_PLACEMENT_3D('',#90207,#28915,#28916);
#26003=AXIS2_PLACEMENT_3D('',#91101,#28918,#28919);
#26004=AXIS2_PLACEMENT_3D('',#91102,#28920,#28921);
#26005=AXIS2_PLACEMENT_3D('',#91103,#28922,#28923);
#26006=AXIS2_PLACEMENT_3D('',#91997,#28925,#28926);
#26007=AXIS2_PLACEMENT_3D('',#91998,#28927,#28928);
#26008=AXIS2_PLACEMENT_3D('',#91999,#28929,#28930);
#26009=AXIS2_PLACEMENT_3D('',#92893,#28932,#28933);
#26010=AXIS2_PLACEMENT_3D('',#92894,#28934,#28935);
#26011=AXIS2_PLACEMENT_3D('',#92895,#28936,#28937);
#26012=AXIS2_PLACEMENT_3D('',#93789,#28939,#28940);
#26013=AXIS2_PLACEMENT_3D('',#93790,#28941,#28942);
#26014=AXIS2_PLACEMENT_3D('',#93791,#28943,#28944);
#26015=AXIS2_PLACEMENT_3D('',#94685,#28946,#28947);
#26016=AXIS2_PLACEMENT_3D('',#94686,#28948,#28949);
#26017=AXIS2_PLACEMENT_3D('',#94687,#28950,#28951);
#26018=AXIS2_PLACEMENT_3D('',#95581,#28953,#28954);
#26019=AXIS2_PLACEMENT_3D('',#95582,#28955,#28956);
#26020=AXIS2_PLACEMENT_3D('',#95583,#28957,#28958);
#26021=AXIS2_PLACEMENT_3D('',#96477,#28960,#28961);
#26022=AXIS2_PLACEMENT_3D('',#96478,#28962,#28963);
#26023=AXIS2_PLACEMENT_3D('',#96479,#28964,#28965);
#26024=AXIS2_PLACEMENT_3D('',#97373,#28967,#28968);
#26025=AXIS2_PLACEMENT_3D('',#97374,#28969,#28970);
#26026=AXIS2_PLACEMENT_3D('',#97375,#28971,#28972);
#26027=AXIS2_PLACEMENT_3D('',#98269,#28974,#28975);
#26028=AXIS2_PLACEMENT_3D('',#98270,#28976,#28977);
#26029=AXIS2_PLACEMENT_3D('',#98271,#28978,#28979);
#26030=AXIS2_PLACEMENT_3D('',#99165,#28981,#28982);
#26031=AXIS2_PLACEMENT_3D('',#99166,#28983,#28984);
#26032=AXIS2_PLACEMENT_3D('',#99167,#28985,#28986);
#26033=AXIS2_PLACEMENT_3D('',#100061,#28988,#28989);
#26034=AXIS2_PLACEMENT_3D('',#100062,#28990,#28991);
#26035=AXIS2_PLACEMENT_3D('',#100063,#28992,#28993);
#26036=AXIS2_PLACEMENT_3D('',#100957,#28995,#28996);
#26037=AXIS2_PLACEMENT_3D('',#100958,#28997,#28998);
#26038=AXIS2_PLACEMENT_3D('',#100959,#28999,#29000);
#26039=AXIS2_PLACEMENT_3D('',#101853,#29002,#29003);
#26040=AXIS2_PLACEMENT_3D('',#101854,#29004,#29005);
#26041=AXIS2_PLACEMENT_3D('',#101855,#29006,#29007);
#26042=AXIS2_PLACEMENT_3D('',#102749,#29009,#29010);
#26043=AXIS2_PLACEMENT_3D('',#102750,#29011,#29012);
#26044=AXIS2_PLACEMENT_3D('',#102751,#29013,#29014);
#26045=AXIS2_PLACEMENT_3D('',#103645,#29016,#29017);
#26046=AXIS2_PLACEMENT_3D('',#103646,#29018,#29019);
#26047=AXIS2_PLACEMENT_3D('',#103647,#29020,#29021);
#26048=AXIS2_PLACEMENT_3D('',#104541,#29023,#29024);
#26049=AXIS2_PLACEMENT_3D('',#104542,#29025,#29026);
#26050=AXIS2_PLACEMENT_3D('',#104543,#29027,#29028);
#26051=AXIS2_PLACEMENT_3D('',#105437,#29030,#29031);
#26052=AXIS2_PLACEMENT_3D('',#105438,#29032,#29033);
#26053=AXIS2_PLACEMENT_3D('',#105439,#29034,#29035);
#26054=AXIS2_PLACEMENT_3D('',#106333,#29037,#29038);
#26055=AXIS2_PLACEMENT_3D('',#106334,#29039,#29040);
#26056=AXIS2_PLACEMENT_3D('',#106335,#29041,#29042);
#26057=AXIS2_PLACEMENT_3D('',#107229,#29044,#29045);
#26058=AXIS2_PLACEMENT_3D('',#107230,#29046,#29047);
#26059=AXIS2_PLACEMENT_3D('',#107231,#29048,#29049);
#26060=AXIS2_PLACEMENT_3D('',#108125,#29051,#29052);
#26061=AXIS2_PLACEMENT_3D('',#108126,#29053,#29054);
#26062=AXIS2_PLACEMENT_3D('',#108127,#29055,#29056);
#26063=AXIS2_PLACEMENT_3D('',#109021,#29058,#29059);
#26064=AXIS2_PLACEMENT_3D('',#109022,#29060,#29061);
#26065=AXIS2_PLACEMENT_3D('',#109023,#29062,#29063);
#26066=AXIS2_PLACEMENT_3D('',#109917,#29065,#29066);
#26067=AXIS2_PLACEMENT_3D('',#109918,#29067,#29068);
#26068=AXIS2_PLACEMENT_3D('',#109919,#29069,#29070);
#26069=AXIS2_PLACEMENT_3D('',#110813,#29072,#29073);
#26070=AXIS2_PLACEMENT_3D('',#110814,#29074,#29075);
#26071=AXIS2_PLACEMENT_3D('',#110815,#29076,#29077);
#26072=AXIS2_PLACEMENT_3D('',#111709,#29079,#29080);
#26073=AXIS2_PLACEMENT_3D('',#111710,#29081,#29082);
#26074=AXIS2_PLACEMENT_3D('',#111711,#29083,#29084);
#26075=AXIS2_PLACEMENT_3D('',#112605,#29086,#29087);
#26076=AXIS2_PLACEMENT_3D('',#112606,#29088,#29089);
#26077=AXIS2_PLACEMENT_3D('',#112607,#29090,#29091);
#26078=AXIS2_PLACEMENT_3D('',#113501,#29093,#29094);
#26079=AXIS2_PLACEMENT_3D('',#113502,#29095,#29096);
#26080=AXIS2_PLACEMENT_3D('',#113503,#29097,#29098);
#26081=AXIS2_PLACEMENT_3D('',#114397,#29100,#29101);
#26082=AXIS2_PLACEMENT_3D('',#114398,#29102,#29103);
#26083=AXIS2_PLACEMENT_3D('',#114399,#29104,#29105);
#26084=AXIS2_PLACEMENT_3D('',#115293,#29107,#29108);
#26085=AXIS2_PLACEMENT_3D('',#115294,#29109,#29110);
#26086=AXIS2_PLACEMENT_3D('',#115295,#29111,#29112);
#26087=AXIS2_PLACEMENT_3D('',#116189,#29114,#29115);
#26088=AXIS2_PLACEMENT_3D('',#116190,#29116,#29117);
#26089=AXIS2_PLACEMENT_3D('',#116191,#29118,#29119);
#26090=AXIS2_PLACEMENT_3D('',#173063,#29191,#29192);
#26091=AXIS2_PLACEMENT_3D('',#173065,#29193,#29194);
#26092=AXIS2_PLACEMENT_3D('',#173068,#29196,#29197);
#26093=AXIS2_PLACEMENT_3D('',#173069,#29198,#29199);
#26094=AXIS2_PLACEMENT_3D('',#173070,#29200,#29201);
#26095=AXIS2_PLACEMENT_3D('',#173071,#29202,#29203);
#26096=AXIS2_PLACEMENT_3D('',#173072,#29204,#29205);
#26097=AXIS2_PLACEMENT_3D('',#173073,#29206,#29207);
#26098=AXIS2_PLACEMENT_3D('',#173074,#29208,#29209);
#26099=AXIS2_PLACEMENT_3D('',#173075,#29210,#29211);
#26100=AXIS2_PLACEMENT_3D('',#173076,#29212,#29213);
#26101=AXIS2_PLACEMENT_3D('',#173077,#29214,#29215);
#26102=AXIS2_PLACEMENT_3D('',#173078,#29216,#29217);
#26103=AXIS2_PLACEMENT_3D('',#173079,#29218,#29219);
#26104=AXIS2_PLACEMENT_3D('',#173080,#29220,#29221);
#26105=AXIS2_PLACEMENT_3D('',#173081,#29222,#29223);
#26106=AXIS2_PLACEMENT_3D('',#173082,#29224,#29225);
#26107=AXIS2_PLACEMENT_3D('',#173083,#29226,#29227);
#26108=AXIS2_PLACEMENT_3D('',#173084,#29228,#29229);
#26109=AXIS2_PLACEMENT_3D('',#173085,#29230,#29231);
#26110=AXIS2_PLACEMENT_3D('',#173086,#29232,#29233);
#26111=AXIS2_PLACEMENT_3D('',#173087,#29234,#29235);
#26112=AXIS2_PLACEMENT_3D('',#173088,#29236,#29237);
#26113=AXIS2_PLACEMENT_3D('',#173089,#29238,#29239);
#26114=AXIS2_PLACEMENT_3D('',#173090,#29240,#29241);
#26115=AXIS2_PLACEMENT_3D('',#173091,#29242,#29243);
#26116=AXIS2_PLACEMENT_3D('',#173092,#29244,#29245);
#26117=AXIS2_PLACEMENT_3D('',#173093,#29246,#29247);
#26118=AXIS2_PLACEMENT_3D('',#173094,#29248,#29249);
#26119=AXIS2_PLACEMENT_3D('',#173095,#29250,#29251);
#26120=AXIS2_PLACEMENT_3D('',#173096,#29252,#29253);
#26121=AXIS2_PLACEMENT_3D('',#173097,#29254,#29255);
#26122=AXIS2_PLACEMENT_3D('',#173098,#29256,#29257);
#26123=AXIS2_PLACEMENT_3D('',#173099,#29258,#29259);
#26124=AXIS2_PLACEMENT_3D('',#173100,#29260,#29261);
#26125=AXIS2_PLACEMENT_3D('',#173101,#29262,#29263);
#26126=AXIS2_PLACEMENT_3D('',#173102,#29264,#29265);
#26127=AXIS2_PLACEMENT_3D('',#173103,#29266,#29267);
#26128=AXIS2_PLACEMENT_3D('',#173104,#29268,#29269);
#26129=AXIS2_PLACEMENT_3D('',#173105,#29270,#29271);
#26130=AXIS2_PLACEMENT_3D('',#173106,#29272,#29273);
#26131=AXIS2_PLACEMENT_3D('',#173107,#29274,#29275);
#26132=AXIS2_PLACEMENT_3D('',#173108,#29276,#29277);
#26133=AXIS2_PLACEMENT_3D('',#173109,#29278,#29279);
#26134=AXIS2_PLACEMENT_3D('',#173110,#29280,#29281);
#26135=AXIS2_PLACEMENT_3D('',#173111,#29282,#29283);
#26136=AXIS2_PLACEMENT_3D('',#173112,#29284,#29285);
#26137=AXIS2_PLACEMENT_3D('',#173113,#29286,#29287);
#26138=AXIS2_PLACEMENT_3D('',#173114,#29288,#29289);
#26139=AXIS2_PLACEMENT_3D('',#173115,#29290,#29291);
#26140=AXIS2_PLACEMENT_3D('',#173116,#29292,#29293);
#26141=AXIS2_PLACEMENT_3D('',#173117,#29294,#29295);
#26142=AXIS2_PLACEMENT_3D('',#173118,#29296,#29297);
#26143=AXIS2_PLACEMENT_3D('',#173119,#29298,#29299);
#26144=AXIS2_PLACEMENT_3D('',#173120,#29300,#29301);
#26145=AXIS2_PLACEMENT_3D('',#173121,#29302,#29303);
#26146=AXIS2_PLACEMENT_3D('',#173122,#29304,#29305);
#26147=AXIS2_PLACEMENT_3D('',#173123,#29306,#29307);
#26148=AXIS2_PLACEMENT_3D('',#173124,#29308,#29309);
#26149=AXIS2_PLACEMENT_3D('',#173125,#29310,#29311);
#26150=AXIS2_PLACEMENT_3D('',#173126,#29312,#29313);
#26151=AXIS2_PLACEMENT_3D('',#173127,#29314,#29315);
#26152=AXIS2_PLACEMENT_3D('',#173128,#29316,#29317);
#26153=AXIS2_PLACEMENT_3D('',#173129,#29318,#29319);
#26154=AXIS2_PLACEMENT_3D('',#173130,#29320,#29321);
#26155=AXIS2_PLACEMENT_3D('',#173131,#29322,#29323);
#26156=AXIS2_PLACEMENT_3D('',#173132,#29324,#29325);
#26157=AXIS2_PLACEMENT_3D('',#173133,#29326,#29327);
#26158=AXIS2_PLACEMENT_3D('',#173134,#29328,#29329);
#26159=AXIS2_PLACEMENT_3D('',#173135,#29330,#29331);
#26160=AXIS2_PLACEMENT_3D('',#173136,#29332,#29333);
#26161=AXIS2_PLACEMENT_3D('',#173137,#29334,#29335);
#26162=AXIS2_PLACEMENT_3D('',#173138,#29336,#29337);
#26163=AXIS2_PLACEMENT_3D('',#173139,#29338,#29339);
#26164=AXIS2_PLACEMENT_3D('',#173140,#29340,#29341);
#26165=AXIS2_PLACEMENT_3D('',#173141,#29342,#29343);
#26166=AXIS2_PLACEMENT_3D('',#173142,#29344,#29345);
#26167=AXIS2_PLACEMENT_3D('',#173143,#29346,#29347);
#26168=AXIS2_PLACEMENT_3D('',#173144,#29348,#29349);
#26169=AXIS2_PLACEMENT_3D('',#173145,#29350,#29351);
#26170=AXIS2_PLACEMENT_3D('',#173146,#29352,#29353);
#26171=AXIS2_PLACEMENT_3D('',#173147,#29354,#29355);
#26172=AXIS2_PLACEMENT_3D('',#173148,#29356,#29357);
#26173=AXIS2_PLACEMENT_3D('',#173149,#29358,#29359);
#26174=AXIS2_PLACEMENT_3D('',#173150,#29360,#29361);
#26175=AXIS2_PLACEMENT_3D('',#173151,#29362,#29363);
#26176=AXIS2_PLACEMENT_3D('',#173152,#29364,#29365);
#26177=AXIS2_PLACEMENT_3D('',#173153,#29366,#29367);
#26178=AXIS2_PLACEMENT_3D('',#173154,#29368,#29369);
#26179=AXIS2_PLACEMENT_3D('',#173155,#29370,#29371);
#26180=AXIS2_PLACEMENT_3D('',#173156,#29372,#29373);
#26181=AXIS2_PLACEMENT_3D('',#173157,#29374,#29375);
#26182=AXIS2_PLACEMENT_3D('',#173158,#29376,#29377);
#26183=AXIS2_PLACEMENT_3D('',#173159,#29378,#29379);
#26184=AXIS2_PLACEMENT_3D('',#173160,#29380,#29381);
#26185=AXIS2_PLACEMENT_3D('',#173161,#29382,#29383);
#26186=AXIS2_PLACEMENT_3D('',#173162,#29384,#29385);
#26187=AXIS2_PLACEMENT_3D('',#173163,#29386,#29387);
#26188=AXIS2_PLACEMENT_3D('',#173164,#29388,#29389);
#26189=AXIS2_PLACEMENT_3D('',#173165,#29390,#29391);
#26190=AXIS2_PLACEMENT_3D('',#173166,#29392,#29393);
#26191=AXIS2_PLACEMENT_3D('',#173167,#29394,#29395);
#26192=AXIS2_PLACEMENT_3D('',#173168,#29396,#29397);
#26193=AXIS2_PLACEMENT_3D('',#173169,#29398,#29399);
#26194=AXIS2_PLACEMENT_3D('',#173170,#29400,#29401);
#26195=AXIS2_PLACEMENT_3D('',#173171,#29402,#29403);
#26196=AXIS2_PLACEMENT_3D('',#173172,#29404,#29405);
#26197=AXIS2_PLACEMENT_3D('',#173173,#29406,#29407);
#26198=AXIS2_PLACEMENT_3D('',#173174,#29408,#29409);
#26199=AXIS2_PLACEMENT_3D('',#173175,#29410,#29411);
#26200=AXIS2_PLACEMENT_3D('',#173176,#29412,#29413);
#26201=AXIS2_PLACEMENT_3D('',#173177,#29414,#29415);
#26202=AXIS2_PLACEMENT_3D('',#173178,#29416,#29417);
#26203=AXIS2_PLACEMENT_3D('',#173179,#29418,#29419);
#26204=AXIS2_PLACEMENT_3D('',#173180,#29420,#29421);
#26205=AXIS2_PLACEMENT_3D('',#173181,#29422,#29423);
#26206=AXIS2_PLACEMENT_3D('',#173182,#29424,#29425);
#26207=AXIS2_PLACEMENT_3D('',#173183,#29426,#29427);
#26208=AXIS2_PLACEMENT_3D('',#173184,#29428,#29429);
#26209=AXIS2_PLACEMENT_3D('',#173185,#29430,#29431);
#26210=AXIS2_PLACEMENT_3D('',#173186,#29432,#29433);
#26211=AXIS2_PLACEMENT_3D('',#173187,#29434,#29435);
#26212=AXIS2_PLACEMENT_3D('',#173188,#29436,#29437);
#26213=AXIS2_PLACEMENT_3D('',#173189,#29438,#29439);
#26214=AXIS2_PLACEMENT_3D('',#173190,#29440,#29441);
#26215=AXIS2_PLACEMENT_3D('',#173191,#29442,#29443);
#26216=AXIS2_PLACEMENT_3D('',#173192,#29444,#29445);
#26217=AXIS2_PLACEMENT_3D('',#173193,#29446,#29447);
#26218=AXIS2_PLACEMENT_3D('',#173194,#29448,#29449);
#26219=AXIS2_PLACEMENT_3D('',#173195,#29450,#29451);
#26220=AXIS2_PLACEMENT_3D('',#173196,#29452,#29453);
#26221=AXIS2_PLACEMENT_3D('',#173197,#29454,#29455);
#26222=AXIS2_PLACEMENT_3D('',#173198,#29456,#29457);
#26223=AXIS2_PLACEMENT_3D('',#173199,#29458,#29459);
#26224=AXIS2_PLACEMENT_3D('',#173200,#29460,#29461);
#26225=AXIS2_PLACEMENT_3D('',#173201,#29462,#29463);
#26226=AXIS2_PLACEMENT_3D('',#173202,#29464,#29465);
#26227=AXIS2_PLACEMENT_3D('',#173203,#29466,#29467);
#26228=AXIS2_PLACEMENT_3D('',#173204,#29468,#29469);
#26229=AXIS2_PLACEMENT_3D('',#173205,#29470,#29471);
#26230=AXIS2_PLACEMENT_3D('',#173206,#29472,#29473);
#26231=AXIS2_PLACEMENT_3D('',#173207,#29474,#29475);
#26232=AXIS2_PLACEMENT_3D('',#173208,#29476,#29477);
#26233=AXIS2_PLACEMENT_3D('',#173209,#29478,#29479);
#26234=AXIS2_PLACEMENT_3D('',#173210,#29480,#29481);
#26235=AXIS2_PLACEMENT_3D('',#173211,#29482,#29483);
#26236=AXIS2_PLACEMENT_3D('',#173212,#29484,#29485);
#26237=AXIS2_PLACEMENT_3D('',#173213,#29486,#29487);
#26238=AXIS2_PLACEMENT_3D('',#173214,#29488,#29489);
#26239=AXIS2_PLACEMENT_3D('',#173215,#29490,#29491);
#26240=AXIS2_PLACEMENT_3D('',#173216,#29492,#29493);
#26241=AXIS2_PLACEMENT_3D('',#173217,#29494,#29495);
#26242=AXIS2_PLACEMENT_3D('',#173218,#29496,#29497);
#26243=AXIS2_PLACEMENT_3D('',#173219,#29498,#29499);
#26244=AXIS2_PLACEMENT_3D('',#173220,#29500,#29501);
#26245=AXIS2_PLACEMENT_3D('',#173221,#29502,#29503);
#26246=AXIS2_PLACEMENT_3D('',#173222,#29504,#29505);
#26247=AXIS2_PLACEMENT_3D('',#173223,#29506,#29507);
#26248=AXIS2_PLACEMENT_3D('',#173224,#29508,#29509);
#26249=AXIS2_PLACEMENT_3D('',#173225,#29510,#29511);
#26250=AXIS2_PLACEMENT_3D('',#173226,#29512,#29513);
#26251=AXIS2_PLACEMENT_3D('',#173227,#29514,#29515);
#26252=AXIS2_PLACEMENT_3D('',#173228,#29516,#29517);
#26253=AXIS2_PLACEMENT_3D('',#173229,#29518,#29519);
#26254=AXIS2_PLACEMENT_3D('',#173230,#29520,#29521);
#26255=AXIS2_PLACEMENT_3D('',#173231,#29522,#29523);
#26256=AXIS2_PLACEMENT_3D('',#173232,#29524,#29525);
#26257=AXIS2_PLACEMENT_3D('',#173233,#29526,#29527);
#26258=AXIS2_PLACEMENT_3D('',#173234,#29528,#29529);
#26259=AXIS2_PLACEMENT_3D('',#173235,#29530,#29531);
#26260=AXIS2_PLACEMENT_3D('',#173236,#29532,#29533);
#26261=AXIS2_PLACEMENT_3D('',#173237,#29534,#29535);
#26262=AXIS2_PLACEMENT_3D('',#173238,#29536,#29537);
#26263=AXIS2_PLACEMENT_3D('',#173239,#29538,#29539);
#26264=AXIS2_PLACEMENT_3D('',#173240,#29540,#29541);
#26265=AXIS2_PLACEMENT_3D('',#173241,#29542,#29543);
#26266=AXIS2_PLACEMENT_3D('',#173242,#29544,#29545);
#26267=AXIS2_PLACEMENT_3D('',#173243,#29546,#29547);
#26268=AXIS2_PLACEMENT_3D('',#173244,#29548,#29549);
#26269=AXIS2_PLACEMENT_3D('',#173245,#29550,#29551);
#26270=AXIS2_PLACEMENT_3D('',#173246,#29552,#29553);
#26271=AXIS2_PLACEMENT_3D('',#173247,#29554,#29555);
#26272=AXIS2_PLACEMENT_3D('',#173248,#29556,#29557);
#26273=AXIS2_PLACEMENT_3D('',#173249,#29558,#29559);
#26274=AXIS2_PLACEMENT_3D('',#173250,#29560,#29561);
#26275=AXIS2_PLACEMENT_3D('',#173251,#29562,#29563);
#26276=AXIS2_PLACEMENT_3D('',#173252,#29564,#29565);
#26277=AXIS2_PLACEMENT_3D('',#173253,#29566,#29567);
#26278=AXIS2_PLACEMENT_3D('',#173254,#29568,#29569);
#26279=AXIS2_PLACEMENT_3D('',#173255,#29570,#29571);
#26280=AXIS2_PLACEMENT_3D('',#173256,#29572,#29573);
#26281=AXIS2_PLACEMENT_3D('',#173257,#29574,#29575);
#26282=AXIS2_PLACEMENT_3D('',#173258,#29576,#29577);
#26283=AXIS2_PLACEMENT_3D('',#173259,#29578,#29579);
#26284=AXIS2_PLACEMENT_3D('',#173260,#29580,#29581);
#26285=AXIS2_PLACEMENT_3D('',#173261,#29582,#29583);
#26286=AXIS2_PLACEMENT_3D('',#173262,#29584,#29585);
#26287=AXIS2_PLACEMENT_3D('',#173263,#29586,#29587);
#26288=AXIS2_PLACEMENT_3D('',#173264,#29588,#29589);
#26289=AXIS2_PLACEMENT_3D('',#173265,#29590,#29591);
#26290=AXIS2_PLACEMENT_3D('',#173266,#29592,#29593);
#26291=AXIS2_PLACEMENT_3D('',#173267,#29594,#29595);
#26292=AXIS2_PLACEMENT_3D('',#173268,#29596,#29597);
#26293=AXIS2_PLACEMENT_3D('',#173269,#29598,#29599);
#26294=AXIS2_PLACEMENT_3D('',#173270,#29600,#29601);
#26295=AXIS2_PLACEMENT_3D('',#173271,#29602,#29603);
#26296=AXIS2_PLACEMENT_3D('',#173272,#29604,#29605);
#26297=AXIS2_PLACEMENT_3D('',#173273,#29606,#29607);
#26298=AXIS2_PLACEMENT_3D('',#173274,#29608,#29609);
#26299=AXIS2_PLACEMENT_3D('',#173275,#29610,#29611);
#26300=AXIS2_PLACEMENT_3D('',#173276,#29612,#29613);
#26301=AXIS2_PLACEMENT_3D('',#173278,#29614,#29615);
#26302=AXIS2_PLACEMENT_3D('',#173281,#29617,#29618);
#26303=AXIS2_PLACEMENT_3D('',#174172,#29619,#29620);
#26304=AXIS2_PLACEMENT_3D('',#174173,#29621,#29622);
#26305=AXIS2_PLACEMENT_3D('',#174174,#29623,#29624);
#26306=AXIS2_PLACEMENT_3D('',#174973,#29625,#29626);
#26307=AXIS2_PLACEMENT_3D('',#174975,#29627,#29628);
#26308=AXIS2_PLACEMENT_3D('',#174976,#29629,#29630);
#26309=AXIS2_PLACEMENT_3D('',#174977,#29631,#29632);
#26310=AXIS2_PLACEMENT_3D('',#174978,#29633,#29634);
#26311=AXIS2_PLACEMENT_3D('',#174979,#29635,#29636);
#26312=AXIS2_PLACEMENT_3D('',#174983,#29639,#29640);
#26313=AXIS2_PLACEMENT_3D('',#174984,#29641,#29642);
#26314=AXIS2_PLACEMENT_3D('',#174985,#29643,#29644);
#26315=AXIS2_PLACEMENT_3D('',#174986,#29645,#29646);
#26316=AXIS2_PLACEMENT_3D('',#174995,#29651,#29652);
#26317=AXIS2_PLACEMENT_3D('',#175004,#29657,#29658);
#26318=AXIS2_PLACEMENT_3D('',#175007,#29661,#29662);
#26319=AXIS2_PLACEMENT_3D('',#175008,#29663,#29664);
#26320=AXIS2_PLACEMENT_3D('',#175009,#29665,#29666);
#26321=AXIS2_PLACEMENT_3D('',#175010,#29667,#29668);
#26322=AXIS2_PLACEMENT_3D('',#175219,#29669,#29670);
#26323=AXIS2_PLACEMENT_3D('',#175429,#29672,#29673);
#26324=AXIS2_PLACEMENT_3D('',#175431,#29674,#29675);
#26325=AXIS2_PLACEMENT_3D('',#175433,#29676,#29677);
#26326=AXIS2_PLACEMENT_3D('',#175643,#29679,#29680);
#26327=AXIS2_PLACEMENT_3D('',#175853,#29682,#29683);
#26328=AXIS2_PLACEMENT_3D('',#175855,#29684,#29685);
#26329=AXIS2_PLACEMENT_3D('',#175857,#29686,#29687);
#26330=AXIS2_PLACEMENT_3D('',#176067,#29689,#29690);
#26331=AXIS2_PLACEMENT_3D('',#176277,#29692,#29693);
#26332=AXIS2_PLACEMENT_3D('',#176279,#29694,#29695);
#26333=AXIS2_PLACEMENT_3D('',#176281,#29696,#29697);
#26334=AXIS2_PLACEMENT_3D('',#176491,#29699,#29700);
#26335=AXIS2_PLACEMENT_3D('',#176701,#29702,#29703);
#26336=AXIS2_PLACEMENT_3D('',#176703,#29704,#29705);
#26337=AXIS2_PLACEMENT_3D('',#176705,#29706,#29707);
#26338=AXIS2_PLACEMENT_3D('',#176915,#29709,#29710);
#26339=AXIS2_PLACEMENT_3D('',#177125,#29712,#29713);
#26340=AXIS2_PLACEMENT_3D('',#177127,#29714,#29715);
#26341=AXIS2_PLACEMENT_3D('',#177129,#29716,#29717);
#26342=AXIS2_PLACEMENT_3D('',#177339,#29719,#29720);
#26343=AXIS2_PLACEMENT_3D('',#177549,#29722,#29723);
#26344=AXIS2_PLACEMENT_3D('',#177551,#29724,#29725);
#26345=AXIS2_PLACEMENT_3D('',#177553,#29726,#29727);
#26346=AXIS2_PLACEMENT_3D('',#177763,#29729,#29730);
#26347=AXIS2_PLACEMENT_3D('',#177973,#29732,#29733);
#26348=AXIS2_PLACEMENT_3D('',#177975,#29734,#29735);
#26349=AXIS2_PLACEMENT_3D('',#177977,#29736,#29737);
#26350=AXIS2_PLACEMENT_3D('',#178187,#29739,#29740);
#26351=AXIS2_PLACEMENT_3D('',#178397,#29742,#29743);
#26352=AXIS2_PLACEMENT_3D('',#178399,#29744,#29745);
#26353=AXIS2_PLACEMENT_3D('',#178401,#29746,#29747);
#26354=AXIS2_PLACEMENT_3D('',#178611,#29749,#29750);
#26355=AXIS2_PLACEMENT_3D('',#178821,#29752,#29753);
#26356=AXIS2_PLACEMENT_3D('',#178823,#29754,#29755);
#26357=AXIS2_PLACEMENT_3D('',#178825,#29756,#29757);
#26358=AXIS2_PLACEMENT_3D('',#179035,#29759,#29760);
#26359=AXIS2_PLACEMENT_3D('',#179245,#29762,#29763);
#26360=AXIS2_PLACEMENT_3D('',#179247,#29764,#29765);
#26361=AXIS2_PLACEMENT_3D('',#179249,#29766,#29767);
#26362=AXIS2_PLACEMENT_3D('',#179459,#29769,#29770);
#26363=AXIS2_PLACEMENT_3D('',#179669,#29772,#29773);
#26364=AXIS2_PLACEMENT_3D('',#179671,#29774,#29775);
#26365=AXIS2_PLACEMENT_3D('',#179673,#29776,#29777);
#26366=AXIS2_PLACEMENT_3D('',#179883,#29779,#29780);
#26367=AXIS2_PLACEMENT_3D('',#180093,#29782,#29783);
#26368=AXIS2_PLACEMENT_3D('',#180095,#29784,#29785);
#26369=AXIS2_PLACEMENT_3D('',#180097,#29786,#29787);
#26370=AXIS2_PLACEMENT_3D('',#180307,#29789,#29790);
#26371=AXIS2_PLACEMENT_3D('',#180517,#29792,#29793);
#26372=AXIS2_PLACEMENT_3D('',#180519,#29794,#29795);
#26373=AXIS2_PLACEMENT_3D('',#180521,#29796,#29797);
#26374=AXIS2_PLACEMENT_3D('',#180731,#29799,#29800);
#26375=AXIS2_PLACEMENT_3D('',#180941,#29802,#29803);
#26376=AXIS2_PLACEMENT_3D('',#180943,#29804,#29805);
#26377=AXIS2_PLACEMENT_3D('',#180945,#29806,#29807);
#26378=AXIS2_PLACEMENT_3D('',#181155,#29809,#29810);
#26379=AXIS2_PLACEMENT_3D('',#181365,#29812,#29813);
#26380=AXIS2_PLACEMENT_3D('',#181367,#29814,#29815);
#26381=AXIS2_PLACEMENT_3D('',#181369,#29816,#29817);
#26382=AXIS2_PLACEMENT_3D('',#181579,#29819,#29820);
#26383=AXIS2_PLACEMENT_3D('',#181789,#29822,#29823);
#26384=AXIS2_PLACEMENT_3D('',#181791,#29824,#29825);
#26385=AXIS2_PLACEMENT_3D('',#181793,#29826,#29827);
#26386=AXIS2_PLACEMENT_3D('',#182003,#29829,#29830);
#26387=AXIS2_PLACEMENT_3D('',#182213,#29832,#29833);
#26388=AXIS2_PLACEMENT_3D('',#182215,#29834,#29835);
#26389=AXIS2_PLACEMENT_3D('',#182217,#29836,#29837);
#26390=AXIS2_PLACEMENT_3D('',#182427,#29839,#29840);
#26391=AXIS2_PLACEMENT_3D('',#182637,#29842,#29843);
#26392=AXIS2_PLACEMENT_3D('',#182639,#29844,#29845);
#26393=AXIS2_PLACEMENT_3D('',#182641,#29846,#29847);
#26394=AXIS2_PLACEMENT_3D('',#182851,#29849,#29850);
#26395=AXIS2_PLACEMENT_3D('',#183061,#29852,#29853);
#26396=AXIS2_PLACEMENT_3D('',#183063,#29854,#29855);
#26397=AXIS2_PLACEMENT_3D('',#183065,#29856,#29857);
#26398=AXIS2_PLACEMENT_3D('',#183275,#29859,#29860);
#26399=AXIS2_PLACEMENT_3D('',#183485,#29862,#29863);
#26400=AXIS2_PLACEMENT_3D('',#183487,#29864,#29865);
#26401=AXIS2_PLACEMENT_3D('',#183489,#29866,#29867);
#26402=AXIS2_PLACEMENT_3D('',#183699,#29869,#29870);
#26403=AXIS2_PLACEMENT_3D('',#183909,#29872,#29873);
#26404=AXIS2_PLACEMENT_3D('',#183911,#29874,#29875);
#26405=AXIS2_PLACEMENT_3D('',#183913,#29876,#29877);
#26406=AXIS2_PLACEMENT_3D('',#184123,#29879,#29880);
#26407=AXIS2_PLACEMENT_3D('',#184333,#29882,#29883);
#26408=AXIS2_PLACEMENT_3D('',#184335,#29884,#29885);
#26409=AXIS2_PLACEMENT_3D('',#184337,#29886,#29887);
#26410=AXIS2_PLACEMENT_3D('',#184547,#29889,#29890);
#26411=AXIS2_PLACEMENT_3D('',#184757,#29892,#29893);
#26412=AXIS2_PLACEMENT_3D('',#184759,#29894,#29895);
#26413=AXIS2_PLACEMENT_3D('',#184761,#29896,#29897);
#26414=AXIS2_PLACEMENT_3D('',#184971,#29899,#29900);
#26415=AXIS2_PLACEMENT_3D('',#185181,#29902,#29903);
#26416=AXIS2_PLACEMENT_3D('',#185183,#29904,#29905);
#26417=AXIS2_PLACEMENT_3D('',#185185,#29906,#29907);
#26418=AXIS2_PLACEMENT_3D('',#185187,#29909,#29910);
#26419=AXIS2_PLACEMENT_3D('',#185190,#29911,#29912);
#26420=AXIS2_PLACEMENT_3D('',#185193,#29915,#29916);
#26421=AXIS2_PLACEMENT_3D('',#185197,#29919,#29920);
#26422=AXIS2_PLACEMENT_3D('',#185200,#29921,#29922);
#26423=AXIS2_PLACEMENT_3D('',#185203,#29925,#29926);
#26424=AXIS2_PLACEMENT_3D('',#185204,#29927,#29928);
#26425=AXIS2_PLACEMENT_3D('',#185205,#29929,#29930);
#26426=AXIS2_PLACEMENT_3D('',#185208,#29931,#29932);
#26427=AXIS2_PLACEMENT_3D('',#185211,#29935,#29936);
#26428=AXIS2_PLACEMENT_3D('',#185215,#29939,#29940);
#26429=AXIS2_PLACEMENT_3D('',#185218,#29941,#29942);
#26430=AXIS2_PLACEMENT_3D('',#185221,#29945,#29946);
#26431=AXIS2_PLACEMENT_3D('',#185222,#29947,#29948);
#26432=AXIS2_PLACEMENT_3D('',#185223,#29949,#29950);
#26433=AXIS2_PLACEMENT_3D('',#185226,#29951,#29952);
#26434=AXIS2_PLACEMENT_3D('',#185229,#29955,#29956);
#26435=AXIS2_PLACEMENT_3D('',#185233,#29959,#29960);
#26436=AXIS2_PLACEMENT_3D('',#185236,#29961,#29962);
#26437=AXIS2_PLACEMENT_3D('',#185239,#29965,#29966);
#26438=AXIS2_PLACEMENT_3D('',#185240,#29967,#29968);
#26439=AXIS2_PLACEMENT_3D('',#185241,#29969,#29970);
#26440=AXIS2_PLACEMENT_3D('',#185244,#29971,#29972);
#26441=AXIS2_PLACEMENT_3D('',#185247,#29975,#29976);
#26442=AXIS2_PLACEMENT_3D('',#185251,#29979,#29980);
#26443=AXIS2_PLACEMENT_3D('',#185254,#29981,#29982);
#26444=AXIS2_PLACEMENT_3D('',#185257,#29985,#29986);
#26445=AXIS2_PLACEMENT_3D('',#185258,#29987,#29988);
#26446=AXIS2_PLACEMENT_3D('',#185259,#29989,#29990);
#26447=AXIS2_PLACEMENT_3D('',#185262,#29991,#29992);
#26448=AXIS2_PLACEMENT_3D('',#185265,#29995,#29996);
#26449=AXIS2_PLACEMENT_3D('',#185269,#29999,#30000);
#26450=AXIS2_PLACEMENT_3D('',#185272,#30001,#30002);
#26451=AXIS2_PLACEMENT_3D('',#185275,#30005,#30006);
#26452=AXIS2_PLACEMENT_3D('',#185276,#30007,#30008);
#26453=AXIS2_PLACEMENT_3D('',#185277,#30009,#30010);
#26454=AXIS2_PLACEMENT_3D('',#185280,#30011,#30012);
#26455=AXIS2_PLACEMENT_3D('',#185283,#30015,#30016);
#26456=AXIS2_PLACEMENT_3D('',#185287,#30019,#30020);
#26457=AXIS2_PLACEMENT_3D('',#185290,#30021,#30022);
#26458=AXIS2_PLACEMENT_3D('',#185293,#30025,#30026);
#26459=AXIS2_PLACEMENT_3D('',#185294,#30027,#30028);
#26460=AXIS2_PLACEMENT_3D('',#185295,#30029,#30030);
#26461=AXIS2_PLACEMENT_3D('',#185298,#30031,#30032);
#26462=AXIS2_PLACEMENT_3D('',#185301,#30035,#30036);
#26463=AXIS2_PLACEMENT_3D('',#185305,#30039,#30040);
#26464=AXIS2_PLACEMENT_3D('',#185308,#30041,#30042);
#26465=AXIS2_PLACEMENT_3D('',#185311,#30045,#30046);
#26466=AXIS2_PLACEMENT_3D('',#185312,#30047,#30048);
#26467=AXIS2_PLACEMENT_3D('',#185313,#30049,#30050);
#26468=AXIS2_PLACEMENT_3D('',#185316,#30051,#30052);
#26469=AXIS2_PLACEMENT_3D('',#185319,#30055,#30056);
#26470=AXIS2_PLACEMENT_3D('',#185323,#30059,#30060);
#26471=AXIS2_PLACEMENT_3D('',#185326,#30061,#30062);
#26472=AXIS2_PLACEMENT_3D('',#185329,#30065,#30066);
#26473=AXIS2_PLACEMENT_3D('',#185330,#30067,#30068);
#26474=AXIS2_PLACEMENT_3D('',#185331,#30069,#30070);
#26475=AXIS2_PLACEMENT_3D('',#185334,#30071,#30072);
#26476=AXIS2_PLACEMENT_3D('',#185337,#30075,#30076);
#26477=AXIS2_PLACEMENT_3D('',#185341,#30079,#30080);
#26478=AXIS2_PLACEMENT_3D('',#185344,#30081,#30082);
#26479=AXIS2_PLACEMENT_3D('',#185347,#30085,#30086);
#26480=AXIS2_PLACEMENT_3D('',#185348,#30087,#30088);
#26481=AXIS2_PLACEMENT_3D('',#185349,#30089,#30090);
#26482=AXIS2_PLACEMENT_3D('',#185352,#30091,#30092);
#26483=AXIS2_PLACEMENT_3D('',#185355,#30095,#30096);
#26484=AXIS2_PLACEMENT_3D('',#185359,#30099,#30100);
#26485=AXIS2_PLACEMENT_3D('',#185362,#30101,#30102);
#26486=AXIS2_PLACEMENT_3D('',#185365,#30105,#30106);
#26487=AXIS2_PLACEMENT_3D('',#185366,#30107,#30108);
#26488=AXIS2_PLACEMENT_3D('',#185367,#30109,#30110);
#26489=AXIS2_PLACEMENT_3D('',#185370,#30111,#30112);
#26490=AXIS2_PLACEMENT_3D('',#185373,#30115,#30116);
#26491=AXIS2_PLACEMENT_3D('',#185377,#30119,#30120);
#26492=AXIS2_PLACEMENT_3D('',#185380,#30121,#30122);
#26493=AXIS2_PLACEMENT_3D('',#185383,#30125,#30126);
#26494=AXIS2_PLACEMENT_3D('',#185384,#30127,#30128);
#26495=AXIS2_PLACEMENT_3D('',#185385,#30129,#30130);
#26496=AXIS2_PLACEMENT_3D('',#185388,#30131,#30132);
#26497=AXIS2_PLACEMENT_3D('',#185391,#30135,#30136);
#26498=AXIS2_PLACEMENT_3D('',#185395,#30139,#30140);
#26499=AXIS2_PLACEMENT_3D('',#185398,#30141,#30142);
#26500=AXIS2_PLACEMENT_3D('',#185401,#30145,#30146);
#26501=AXIS2_PLACEMENT_3D('',#185402,#30147,#30148);
#26502=AXIS2_PLACEMENT_3D('',#185403,#30149,#30150);
#26503=AXIS2_PLACEMENT_3D('',#185406,#30151,#30152);
#26504=AXIS2_PLACEMENT_3D('',#185409,#30155,#30156);
#26505=AXIS2_PLACEMENT_3D('',#185413,#30159,#30160);
#26506=AXIS2_PLACEMENT_3D('',#185416,#30161,#30162);
#26507=AXIS2_PLACEMENT_3D('',#185419,#30165,#30166);
#26508=AXIS2_PLACEMENT_3D('',#185420,#30167,#30168);
#26509=AXIS2_PLACEMENT_3D('',#185421,#30169,#30170);
#26510=AXIS2_PLACEMENT_3D('',#185424,#30171,#30172);
#26511=AXIS2_PLACEMENT_3D('',#185427,#30175,#30176);
#26512=AXIS2_PLACEMENT_3D('',#185431,#30179,#30180);
#26513=AXIS2_PLACEMENT_3D('',#185434,#30181,#30182);
#26514=AXIS2_PLACEMENT_3D('',#185437,#30185,#30186);
#26515=AXIS2_PLACEMENT_3D('',#185438,#30187,#30188);
#26516=AXIS2_PLACEMENT_3D('',#185439,#30189,#30190);
#26517=AXIS2_PLACEMENT_3D('',#185442,#30191,#30192);
#26518=AXIS2_PLACEMENT_3D('',#185445,#30195,#30196);
#26519=AXIS2_PLACEMENT_3D('',#185449,#30199,#30200);
#26520=AXIS2_PLACEMENT_3D('',#185452,#30201,#30202);
#26521=AXIS2_PLACEMENT_3D('',#185455,#30205,#30206);
#26522=AXIS2_PLACEMENT_3D('',#185456,#30207,#30208);
#26523=AXIS2_PLACEMENT_3D('',#185457,#30209,#30210);
#26524=AXIS2_PLACEMENT_3D('',#185460,#30211,#30212);
#26525=AXIS2_PLACEMENT_3D('',#185463,#30215,#30216);
#26526=AXIS2_PLACEMENT_3D('',#185467,#30219,#30220);
#26527=AXIS2_PLACEMENT_3D('',#185470,#30221,#30222);
#26528=AXIS2_PLACEMENT_3D('',#185473,#30225,#30226);
#26529=AXIS2_PLACEMENT_3D('',#185474,#30227,#30228);
#26530=AXIS2_PLACEMENT_3D('',#185475,#30229,#30230);
#26531=AXIS2_PLACEMENT_3D('',#185478,#30231,#30232);
#26532=AXIS2_PLACEMENT_3D('',#185481,#30235,#30236);
#26533=AXIS2_PLACEMENT_3D('',#185485,#30239,#30240);
#26534=AXIS2_PLACEMENT_3D('',#185488,#30241,#30242);
#26535=AXIS2_PLACEMENT_3D('',#185491,#30245,#30246);
#26536=AXIS2_PLACEMENT_3D('',#185492,#30247,#30248);
#26537=AXIS2_PLACEMENT_3D('',#185493,#30249,#30250);
#26538=AXIS2_PLACEMENT_3D('',#185496,#30251,#30252);
#26539=AXIS2_PLACEMENT_3D('',#185499,#30255,#30256);
#26540=AXIS2_PLACEMENT_3D('',#185503,#30259,#30260);
#26541=AXIS2_PLACEMENT_3D('',#185506,#30261,#30262);
#26542=AXIS2_PLACEMENT_3D('',#185509,#30265,#30266);
#26543=AXIS2_PLACEMENT_3D('',#185510,#30267,#30268);
#26544=AXIS2_PLACEMENT_3D('',#185511,#30269,#30270);
#26545=AXIS2_PLACEMENT_3D('',#185514,#30271,#30272);
#26546=AXIS2_PLACEMENT_3D('',#185517,#30275,#30276);
#26547=AXIS2_PLACEMENT_3D('',#185521,#30279,#30280);
#26548=AXIS2_PLACEMENT_3D('',#185524,#30281,#30282);
#26549=AXIS2_PLACEMENT_3D('',#185527,#30285,#30286);
#26550=AXIS2_PLACEMENT_3D('',#185528,#30287,#30288);
#26551=AXIS2_PLACEMENT_3D('',#185529,#30289,#30290);
#26552=AXIS2_PLACEMENT_3D('',#185532,#30291,#30292);
#26553=AXIS2_PLACEMENT_3D('',#185535,#30295,#30296);
#26554=AXIS2_PLACEMENT_3D('',#185539,#30299,#30300);
#26555=AXIS2_PLACEMENT_3D('',#185542,#30301,#30302);
#26556=AXIS2_PLACEMENT_3D('',#185545,#30305,#30306);
#26557=AXIS2_PLACEMENT_3D('',#185546,#30307,#30308);
#26558=AXIS2_PLACEMENT_3D('',#185547,#30309,#30310);
#26559=AXIS2_PLACEMENT_3D('',#185550,#30311,#30312);
#26560=AXIS2_PLACEMENT_3D('',#185553,#30315,#30316);
#26561=AXIS2_PLACEMENT_3D('',#185557,#30319,#30320);
#26562=AXIS2_PLACEMENT_3D('',#185560,#30321,#30322);
#26563=AXIS2_PLACEMENT_3D('',#185563,#30325,#30326);
#26564=AXIS2_PLACEMENT_3D('',#185564,#30327,#30328);
#26565=AXIS2_PLACEMENT_3D('',#185565,#30329,#30330);
#26566=AXIS2_PLACEMENT_3D('',#185568,#30331,#30332);
#26567=AXIS2_PLACEMENT_3D('',#185571,#30335,#30336);
#26568=AXIS2_PLACEMENT_3D('',#185575,#30339,#30340);
#26569=AXIS2_PLACEMENT_3D('',#185578,#30341,#30342);
#26570=AXIS2_PLACEMENT_3D('',#185581,#30345,#30346);
#26571=AXIS2_PLACEMENT_3D('',#185582,#30347,#30348);
#26572=AXIS2_PLACEMENT_3D('',#185583,#30349,#30350);
#26573=AXIS2_PLACEMENT_3D('',#185586,#30351,#30352);
#26574=AXIS2_PLACEMENT_3D('',#185589,#30355,#30356);
#26575=AXIS2_PLACEMENT_3D('',#185593,#30359,#30360);
#26576=AXIS2_PLACEMENT_3D('',#185596,#30361,#30362);
#26577=AXIS2_PLACEMENT_3D('',#185599,#30365,#30366);
#26578=AXIS2_PLACEMENT_3D('',#185600,#30367,#30368);
#26579=AXIS2_PLACEMENT_3D('',#185601,#30369,#30370);
#26580=AXIS2_PLACEMENT_3D('',#186839,#30375,#30376);
#26581=AXIS2_PLACEMENT_3D('',#188077,#30381,#30382);
#26582=AXIS2_PLACEMENT_3D('',#189315,#30387,#30388);
#26583=AXIS2_PLACEMENT_3D('',#190553,#30393,#30394);
#26584=AXIS2_PLACEMENT_3D('',#191791,#30399,#30400);
#26585=AXIS2_PLACEMENT_3D('',#193029,#30405,#30406);
#26586=AXIS2_PLACEMENT_3D('',#194267,#30411,#30412);
#26587=AXIS2_PLACEMENT_3D('',#195505,#30417,#30418);
#26588=AXIS2_PLACEMENT_3D('',#196743,#30423,#30424);
#26589=AXIS2_PLACEMENT_3D('',#197981,#30429,#30430);
#26590=AXIS2_PLACEMENT_3D('',#199219,#30435,#30436);
#26591=AXIS2_PLACEMENT_3D('',#200457,#30441,#30442);
#26592=AXIS2_PLACEMENT_3D('',#201695,#30447,#30448);
#26593=AXIS2_PLACEMENT_3D('',#202933,#30453,#30454);
#26594=AXIS2_PLACEMENT_3D('',#204171,#30459,#30460);
#26595=AXIS2_PLACEMENT_3D('',#205409,#30465,#30466);
#26596=AXIS2_PLACEMENT_3D('',#206647,#30471,#30472);
#26597=AXIS2_PLACEMENT_3D('',#207885,#30477,#30478);
#26598=AXIS2_PLACEMENT_3D('',#209123,#30483,#30484);
#26599=AXIS2_PLACEMENT_3D('',#210361,#30489,#30490);
#26600=AXIS2_PLACEMENT_3D('',#211599,#30495,#30496);
#26601=AXIS2_PLACEMENT_3D('',#212837,#30501,#30502);
#26602=AXIS2_PLACEMENT_3D('',#214075,#30507,#30508);
#26603=AXIS2_PLACEMENT_3D('',#214076,#30509,#30510);
#26604=AXIS2_PLACEMENT_3D('',#214077,#30511,#30512);
#26605=AXIS2_PLACEMENT_3D('',#214078,#30513,#30514);
#26606=AXIS2_PLACEMENT_3D('',#214079,#30515,#30516);
#26607=AXIS2_PLACEMENT_3D('',#214080,#30517,#30518);
#26608=AXIS2_PLACEMENT_3D('',#214081,#30519,#30520);
#26609=AXIS2_PLACEMENT_3D('',#214082,#30521,#30522);
#26610=AXIS2_PLACEMENT_3D('',#214083,#30523,#30524);
#26611=AXIS2_PLACEMENT_3D('',#214084,#30525,#30526);
#26612=AXIS2_PLACEMENT_3D('',#214085,#30527,#30528);
#26613=AXIS2_PLACEMENT_3D('',#214086,#30529,#30530);
#26614=AXIS2_PLACEMENT_3D('',#214087,#30531,#30532);
#26615=AXIS2_PLACEMENT_3D('',#214088,#30533,#30534);
#26616=AXIS2_PLACEMENT_3D('',#214089,#30535,#30536);
#26617=AXIS2_PLACEMENT_3D('',#214090,#30537,#30538);
#26618=AXIS2_PLACEMENT_3D('',#214091,#30539,#30540);
#26619=AXIS2_PLACEMENT_3D('',#214092,#30541,#30542);
#26620=AXIS2_PLACEMENT_3D('',#214093,#30543,#30544);
#26621=AXIS2_PLACEMENT_3D('',#214094,#30545,#30546);
#26622=AXIS2_PLACEMENT_3D('',#214095,#30547,#30548);
#26623=AXIS2_PLACEMENT_3D('',#214096,#30549,#30550);
#26624=AXIS2_PLACEMENT_3D('',#214097,#30551,#30552);
#26625=AXIS2_PLACEMENT_3D('',#214099,#30553,#30554);
#26626=AXIS2_PLACEMENT_3D('',#214309,#30556,#30557);
#26627=AXIS2_PLACEMENT_3D('',#214311,#30558,#30559);
#26628=AXIS2_PLACEMENT_3D('',#214313,#30560,#30561);
#26629=AXIS2_PLACEMENT_3D('',#214522,#30563,#30564);
#26630=AXIS2_PLACEMENT_3D('',#214523,#30565,#30566);
#26631=AXIS2_PLACEMENT_3D('',#214525,#30568,#30569);
#26632=AXIS2_PLACEMENT_3D('',#214526,#30570,#30571);
#26633=AXIS2_PLACEMENT_3D('',#214527,#30572,#30573);
#26634=AXIS2_PLACEMENT_3D('',#214528,#30574,#30575);
#26635=AXIS2_PLACEMENT_3D('',#214529,#30576,#30577);
#26636=AXIS2_PLACEMENT_3D('',#214530,#30578,#30579);
#26637=AXIS2_PLACEMENT_3D('',#214531,#30580,#30581);
#26638=AXIS2_PLACEMENT_3D('',#214532,#30582,#30583);
#26639=AXIS2_PLACEMENT_3D('',#214533,#30584,#30585);
#26640=AXIS2_PLACEMENT_3D('',#214534,#30586,#30587);
#26641=AXIS2_PLACEMENT_3D('',#214535,#30588,#30589);
#26642=AXIS2_PLACEMENT_3D('',#214536,#30590,#30591);
#26643=AXIS2_PLACEMENT_3D('',#214537,#30592,#30593);
#26644=AXIS2_PLACEMENT_3D('',#214538,#30594,#30595);
#26645=AXIS2_PLACEMENT_3D('',#214539,#30596,#30597);
#26646=AXIS2_PLACEMENT_3D('',#214540,#30598,#30599);
#26647=AXIS2_PLACEMENT_3D('',#214541,#30600,#30601);
#26648=AXIS2_PLACEMENT_3D('',#214542,#30602,#30603);
#26649=AXIS2_PLACEMENT_3D('',#214543,#30604,#30605);
#26650=AXIS2_PLACEMENT_3D('',#214544,#30606,#30607);
#26651=AXIS2_PLACEMENT_3D('',#214545,#30608,#30609);
#26652=AXIS2_PLACEMENT_3D('',#214546,#30610,#30611);
#26653=AXIS2_PLACEMENT_3D('',#214547,#30612,#30613);
#26654=AXIS2_PLACEMENT_3D('',#214550,#30616,#30617);
#26655=AXIS2_PLACEMENT_3D('',#214552,#30619,#30620);
#26656=AXIS2_PLACEMENT_3D('',#214555,#30623,#30624);
#26657=AXIS2_PLACEMENT_3D('',#214556,#30625,#30626);
#26658=AXIS2_PLACEMENT_3D('',#215379,#30629,#30630);
#26659=AXIS2_PLACEMENT_3D('',#215380,#30631,#30632);
#26660=AXIS2_PLACEMENT_3D('',#215381,#30633,#30634);
#26661=AXIS2_PLACEMENT_3D('',#215384,#30635,#30636);
#26662=AXIS2_PLACEMENT_3D('',#215388,#30638,#30639);
#26663=AXIS2_PLACEMENT_3D('',#215390,#30641,#30642);
#26664=AXIS2_PLACEMENT_3D('',#215396,#30646,#30647);
#26665=AXIS2_PLACEMENT_3D('',#215399,#30648,#30649);
#26666=AXIS2_PLACEMENT_3D('',#215403,#30651,#30652);
#26667=AXIS2_PLACEMENT_3D('',#215405,#30654,#30655);
#26668=AXIS2_PLACEMENT_3D('',#215406,#30656,#30657);
#26669=AXIS2_PLACEMENT_3D('',#215407,#30658,#30659);
#26670=AXIS2_PLACEMENT_3D('',#215408,#30660,#30661);
#26671=AXIS2_PLACEMENT_3D('',#215411,#30662,#30663);
#26672=AXIS2_PLACEMENT_3D('',#215415,#30665,#30666);
#26673=AXIS2_PLACEMENT_3D('',#215417,#30668,#30669);
#26674=AXIS2_PLACEMENT_3D('',#215423,#30673,#30674);
#26675=AXIS2_PLACEMENT_3D('',#215426,#30675,#30676);
#26676=AXIS2_PLACEMENT_3D('',#215430,#30678,#30679);
#26677=AXIS2_PLACEMENT_3D('',#215432,#30681,#30682);
#26678=AXIS2_PLACEMENT_3D('',#215433,#30683,#30684);
#26679=AXIS2_PLACEMENT_3D('',#215434,#30685,#30686);
#26680=AXIS2_PLACEMENT_3D('',#215435,#30687,#30688);
#26681=AXIS2_PLACEMENT_3D('',#215438,#30689,#30690);
#26682=AXIS2_PLACEMENT_3D('',#215442,#30692,#30693);
#26683=AXIS2_PLACEMENT_3D('',#215444,#30695,#30696);
#26684=AXIS2_PLACEMENT_3D('',#215450,#30700,#30701);
#26685=AXIS2_PLACEMENT_3D('',#215453,#30702,#30703);
#26686=AXIS2_PLACEMENT_3D('',#215457,#30705,#30706);
#26687=AXIS2_PLACEMENT_3D('',#215459,#30708,#30709);
#26688=AXIS2_PLACEMENT_3D('',#215460,#30710,#30711);
#26689=AXIS2_PLACEMENT_3D('',#215461,#30712,#30713);
#26690=AXIS2_PLACEMENT_3D('',#215462,#30714,#30715);
#26691=AXIS2_PLACEMENT_3D('',#215465,#30716,#30717);
#26692=AXIS2_PLACEMENT_3D('',#215469,#30719,#30720);
#26693=AXIS2_PLACEMENT_3D('',#215471,#30722,#30723);
#26694=AXIS2_PLACEMENT_3D('',#215477,#30727,#30728);
#26695=AXIS2_PLACEMENT_3D('',#215480,#30729,#30730);
#26696=AXIS2_PLACEMENT_3D('',#215484,#30732,#30733);
#26697=AXIS2_PLACEMENT_3D('',#215486,#30735,#30736);
#26698=AXIS2_PLACEMENT_3D('',#215487,#30737,#30738);
#26699=AXIS2_PLACEMENT_3D('',#215488,#30739,#30740);
#26700=AXIS2_PLACEMENT_3D('',#215489,#30741,#30742);
#26701=AXIS2_PLACEMENT_3D('',#215492,#30743,#30744);
#26702=AXIS2_PLACEMENT_3D('',#215496,#30746,#30747);
#26703=AXIS2_PLACEMENT_3D('',#215498,#30749,#30750);
#26704=AXIS2_PLACEMENT_3D('',#215504,#30754,#30755);
#26705=AXIS2_PLACEMENT_3D('',#215507,#30756,#30757);
#26706=AXIS2_PLACEMENT_3D('',#215511,#30759,#30760);
#26707=AXIS2_PLACEMENT_3D('',#215513,#30762,#30763);
#26708=AXIS2_PLACEMENT_3D('',#215514,#30764,#30765);
#26709=AXIS2_PLACEMENT_3D('',#215515,#30766,#30767);
#26710=AXIS2_PLACEMENT_3D('',#215516,#30768,#30769);
#26711=AXIS2_PLACEMENT_3D('',#215519,#30770,#30771);
#26712=AXIS2_PLACEMENT_3D('',#215523,#30773,#30774);
#26713=AXIS2_PLACEMENT_3D('',#215525,#30776,#30777);
#26714=AXIS2_PLACEMENT_3D('',#215531,#30781,#30782);
#26715=AXIS2_PLACEMENT_3D('',#215534,#30783,#30784);
#26716=AXIS2_PLACEMENT_3D('',#215538,#30786,#30787);
#26717=AXIS2_PLACEMENT_3D('',#215540,#30789,#30790);
#26718=AXIS2_PLACEMENT_3D('',#215541,#30791,#30792);
#26719=AXIS2_PLACEMENT_3D('',#215542,#30793,#30794);
#26720=AXIS2_PLACEMENT_3D('',#215543,#30795,#30796);
#26721=AXIS2_PLACEMENT_3D('',#215546,#30797,#30798);
#26722=AXIS2_PLACEMENT_3D('',#215550,#30800,#30801);
#26723=AXIS2_PLACEMENT_3D('',#215552,#30803,#30804);
#26724=AXIS2_PLACEMENT_3D('',#215558,#30808,#30809);
#26725=AXIS2_PLACEMENT_3D('',#215561,#30810,#30811);
#26726=AXIS2_PLACEMENT_3D('',#215565,#30813,#30814);
#26727=AXIS2_PLACEMENT_3D('',#215567,#30816,#30817);
#26728=AXIS2_PLACEMENT_3D('',#215568,#30818,#30819);
#26729=AXIS2_PLACEMENT_3D('',#215569,#30820,#30821);
#26730=AXIS2_PLACEMENT_3D('',#215570,#30822,#30823);
#26731=AXIS2_PLACEMENT_3D('',#215573,#30824,#30825);
#26732=AXIS2_PLACEMENT_3D('',#215577,#30827,#30828);
#26733=AXIS2_PLACEMENT_3D('',#215579,#30830,#30831);
#26734=AXIS2_PLACEMENT_3D('',#215585,#30835,#30836);
#26735=AXIS2_PLACEMENT_3D('',#215588,#30837,#30838);
#26736=AXIS2_PLACEMENT_3D('',#215592,#30840,#30841);
#26737=AXIS2_PLACEMENT_3D('',#215594,#30843,#30844);
#26738=AXIS2_PLACEMENT_3D('',#215595,#30845,#30846);
#26739=AXIS2_PLACEMENT_3D('',#215596,#30847,#30848);
#26740=AXIS2_PLACEMENT_3D('',#215597,#30849,#30850);
#26741=AXIS2_PLACEMENT_3D('',#215600,#30851,#30852);
#26742=AXIS2_PLACEMENT_3D('',#215604,#30854,#30855);
#26743=AXIS2_PLACEMENT_3D('',#215606,#30857,#30858);
#26744=AXIS2_PLACEMENT_3D('',#215612,#30862,#30863);
#26745=AXIS2_PLACEMENT_3D('',#215615,#30864,#30865);
#26746=AXIS2_PLACEMENT_3D('',#215619,#30867,#30868);
#26747=AXIS2_PLACEMENT_3D('',#215621,#30870,#30871);
#26748=AXIS2_PLACEMENT_3D('',#215622,#30872,#30873);
#26749=AXIS2_PLACEMENT_3D('',#215623,#30874,#30875);
#26750=AXIS2_PLACEMENT_3D('',#215624,#30876,#30877);
#26751=AXIS2_PLACEMENT_3D('',#215627,#30878,#30879);
#26752=AXIS2_PLACEMENT_3D('',#215631,#30881,#30882);
#26753=AXIS2_PLACEMENT_3D('',#215633,#30884,#30885);
#26754=AXIS2_PLACEMENT_3D('',#215639,#30889,#30890);
#26755=AXIS2_PLACEMENT_3D('',#215642,#30891,#30892);
#26756=AXIS2_PLACEMENT_3D('',#215646,#30894,#30895);
#26757=AXIS2_PLACEMENT_3D('',#215648,#30897,#30898);
#26758=AXIS2_PLACEMENT_3D('',#215649,#30899,#30900);
#26759=AXIS2_PLACEMENT_3D('',#215650,#30901,#30902);
#26760=AXIS2_PLACEMENT_3D('',#215651,#30903,#30904);
#26761=AXIS2_PLACEMENT_3D('',#215654,#30905,#30906);
#26762=AXIS2_PLACEMENT_3D('',#215658,#30908,#30909);
#26763=AXIS2_PLACEMENT_3D('',#215660,#30911,#30912);
#26764=AXIS2_PLACEMENT_3D('',#215666,#30916,#30917);
#26765=AXIS2_PLACEMENT_3D('',#215669,#30918,#30919);
#26766=AXIS2_PLACEMENT_3D('',#215673,#30921,#30922);
#26767=AXIS2_PLACEMENT_3D('',#215675,#30924,#30925);
#26768=AXIS2_PLACEMENT_3D('',#215676,#30926,#30927);
#26769=AXIS2_PLACEMENT_3D('',#215677,#30928,#30929);
#26770=AXIS2_PLACEMENT_3D('',#215678,#30930,#30931);
#26771=AXIS2_PLACEMENT_3D('',#215681,#30932,#30933);
#26772=AXIS2_PLACEMENT_3D('',#215685,#30935,#30936);
#26773=AXIS2_PLACEMENT_3D('',#215687,#30938,#30939);
#26774=AXIS2_PLACEMENT_3D('',#215693,#30943,#30944);
#26775=AXIS2_PLACEMENT_3D('',#215696,#30945,#30946);
#26776=AXIS2_PLACEMENT_3D('',#215700,#30948,#30949);
#26777=AXIS2_PLACEMENT_3D('',#215702,#30951,#30952);
#26778=AXIS2_PLACEMENT_3D('',#215703,#30953,#30954);
#26779=AXIS2_PLACEMENT_3D('',#215704,#30955,#30956);
#26780=AXIS2_PLACEMENT_3D('',#215705,#30957,#30958);
#26781=AXIS2_PLACEMENT_3D('',#215708,#30959,#30960);
#26782=AXIS2_PLACEMENT_3D('',#215712,#30962,#30963);
#26783=AXIS2_PLACEMENT_3D('',#215714,#30965,#30966);
#26784=AXIS2_PLACEMENT_3D('',#215720,#30970,#30971);
#26785=AXIS2_PLACEMENT_3D('',#215723,#30972,#30973);
#26786=AXIS2_PLACEMENT_3D('',#215727,#30975,#30976);
#26787=AXIS2_PLACEMENT_3D('',#215729,#30978,#30979);
#26788=AXIS2_PLACEMENT_3D('',#215730,#30980,#30981);
#26789=AXIS2_PLACEMENT_3D('',#215731,#30982,#30983);
#26790=AXIS2_PLACEMENT_3D('',#215732,#30984,#30985);
#26791=AXIS2_PLACEMENT_3D('',#215735,#30986,#30987);
#26792=AXIS2_PLACEMENT_3D('',#215739,#30989,#30990);
#26793=AXIS2_PLACEMENT_3D('',#215741,#30992,#30993);
#26794=AXIS2_PLACEMENT_3D('',#215747,#30997,#30998);
#26795=AXIS2_PLACEMENT_3D('',#215750,#30999,#31000);
#26796=AXIS2_PLACEMENT_3D('',#215754,#31002,#31003);
#26797=AXIS2_PLACEMENT_3D('',#215756,#31005,#31006);
#26798=AXIS2_PLACEMENT_3D('',#215757,#31007,#31008);
#26799=AXIS2_PLACEMENT_3D('',#215758,#31009,#31010);
#26800=AXIS2_PLACEMENT_3D('',#215759,#31011,#31012);
#26801=AXIS2_PLACEMENT_3D('',#215762,#31013,#31014);
#26802=AXIS2_PLACEMENT_3D('',#215766,#31016,#31017);
#26803=AXIS2_PLACEMENT_3D('',#215768,#31019,#31020);
#26804=AXIS2_PLACEMENT_3D('',#215774,#31024,#31025);
#26805=AXIS2_PLACEMENT_3D('',#215777,#31026,#31027);
#26806=AXIS2_PLACEMENT_3D('',#215781,#31029,#31030);
#26807=AXIS2_PLACEMENT_3D('',#215783,#31032,#31033);
#26808=AXIS2_PLACEMENT_3D('',#215784,#31034,#31035);
#26809=AXIS2_PLACEMENT_3D('',#215785,#31036,#31037);
#26810=AXIS2_PLACEMENT_3D('',#215786,#31038,#31039);
#26811=AXIS2_PLACEMENT_3D('',#215789,#31040,#31041);
#26812=AXIS2_PLACEMENT_3D('',#215793,#31043,#31044);
#26813=AXIS2_PLACEMENT_3D('',#215795,#31046,#31047);
#26814=AXIS2_PLACEMENT_3D('',#215801,#31051,#31052);
#26815=AXIS2_PLACEMENT_3D('',#215804,#31053,#31054);
#26816=AXIS2_PLACEMENT_3D('',#215808,#31056,#31057);
#26817=AXIS2_PLACEMENT_3D('',#215810,#31059,#31060);
#26818=AXIS2_PLACEMENT_3D('',#215811,#31061,#31062);
#26819=AXIS2_PLACEMENT_3D('',#215812,#31063,#31064);
#26820=AXIS2_PLACEMENT_3D('',#215813,#31065,#31066);
#26821=AXIS2_PLACEMENT_3D('',#215816,#31067,#31068);
#26822=AXIS2_PLACEMENT_3D('',#215820,#31070,#31071);
#26823=AXIS2_PLACEMENT_3D('',#215822,#31073,#31074);
#26824=AXIS2_PLACEMENT_3D('',#215828,#31078,#31079);
#26825=AXIS2_PLACEMENT_3D('',#215831,#31080,#31081);
#26826=AXIS2_PLACEMENT_3D('',#215835,#31083,#31084);
#26827=AXIS2_PLACEMENT_3D('',#215837,#31086,#31087);
#26828=AXIS2_PLACEMENT_3D('',#215838,#31088,#31089);
#26829=AXIS2_PLACEMENT_3D('',#215839,#31090,#31091);
#26830=AXIS2_PLACEMENT_3D('',#215840,#31092,#31093);
#26831=AXIS2_PLACEMENT_3D('',#215843,#31094,#31095);
#26832=AXIS2_PLACEMENT_3D('',#215847,#31097,#31098);
#26833=AXIS2_PLACEMENT_3D('',#215849,#31100,#31101);
#26834=AXIS2_PLACEMENT_3D('',#215855,#31105,#31106);
#26835=AXIS2_PLACEMENT_3D('',#215858,#31107,#31108);
#26836=AXIS2_PLACEMENT_3D('',#215862,#31110,#31111);
#26837=AXIS2_PLACEMENT_3D('',#215864,#31113,#31114);
#26838=AXIS2_PLACEMENT_3D('',#215865,#31115,#31116);
#26839=AXIS2_PLACEMENT_3D('',#215866,#31117,#31118);
#26840=AXIS2_PLACEMENT_3D('',#215867,#31119,#31120);
#26841=AXIS2_PLACEMENT_3D('',#215870,#31121,#31122);
#26842=AXIS2_PLACEMENT_3D('',#215874,#31124,#31125);
#26843=AXIS2_PLACEMENT_3D('',#215876,#31127,#31128);
#26844=AXIS2_PLACEMENT_3D('',#215882,#31132,#31133);
#26845=AXIS2_PLACEMENT_3D('',#215885,#31134,#31135);
#26846=AXIS2_PLACEMENT_3D('',#215889,#31137,#31138);
#26847=AXIS2_PLACEMENT_3D('',#215891,#31140,#31141);
#26848=AXIS2_PLACEMENT_3D('',#215892,#31142,#31143);
#26849=AXIS2_PLACEMENT_3D('',#215893,#31144,#31145);
#26850=AXIS2_PLACEMENT_3D('',#215894,#31146,#31147);
#26851=AXIS2_PLACEMENT_3D('',#215897,#31148,#31149);
#26852=AXIS2_PLACEMENT_3D('',#215901,#31151,#31152);
#26853=AXIS2_PLACEMENT_3D('',#215903,#31154,#31155);
#26854=AXIS2_PLACEMENT_3D('',#215909,#31159,#31160);
#26855=AXIS2_PLACEMENT_3D('',#215912,#31161,#31162);
#26856=AXIS2_PLACEMENT_3D('',#215916,#31164,#31165);
#26857=AXIS2_PLACEMENT_3D('',#215918,#31167,#31168);
#26858=AXIS2_PLACEMENT_3D('',#215919,#31169,#31170);
#26859=AXIS2_PLACEMENT_3D('',#215920,#31171,#31172);
#26860=AXIS2_PLACEMENT_3D('',#215921,#31173,#31174);
#26861=AXIS2_PLACEMENT_3D('',#215924,#31175,#31176);
#26862=AXIS2_PLACEMENT_3D('',#215928,#31178,#31179);
#26863=AXIS2_PLACEMENT_3D('',#215930,#31181,#31182);
#26864=AXIS2_PLACEMENT_3D('',#215936,#31186,#31187);
#26865=AXIS2_PLACEMENT_3D('',#215939,#31188,#31189);
#26866=AXIS2_PLACEMENT_3D('',#215943,#31191,#31192);
#26867=AXIS2_PLACEMENT_3D('',#215945,#31194,#31195);
#26868=AXIS2_PLACEMENT_3D('',#215946,#31196,#31197);
#26869=AXIS2_PLACEMENT_3D('',#215947,#31198,#31199);
#26870=AXIS2_PLACEMENT_3D('',#215948,#31200,#31201);
#26871=AXIS2_PLACEMENT_3D('',#215951,#31202,#31203);
#26872=AXIS2_PLACEMENT_3D('',#215955,#31205,#31206);
#26873=AXIS2_PLACEMENT_3D('',#215957,#31208,#31209);
#26874=AXIS2_PLACEMENT_3D('',#215963,#31213,#31214);
#26875=AXIS2_PLACEMENT_3D('',#215966,#31215,#31216);
#26876=AXIS2_PLACEMENT_3D('',#215970,#31218,#31219);
#26877=AXIS2_PLACEMENT_3D('',#215972,#31221,#31222);
#26878=AXIS2_PLACEMENT_3D('',#215973,#31223,#31224);
#26879=AXIS2_PLACEMENT_3D('',#215974,#31225,#31226);
#26880=AXIS2_PLACEMENT_3D('',#215975,#31227,#31228);
#26881=AXIS2_PLACEMENT_3D('',#215978,#31229,#31230);
#26882=AXIS2_PLACEMENT_3D('',#215982,#31232,#31233);
#26883=AXIS2_PLACEMENT_3D('',#215984,#31235,#31236);
#26884=AXIS2_PLACEMENT_3D('',#215990,#31240,#31241);
#26885=AXIS2_PLACEMENT_3D('',#215993,#31242,#31243);
#26886=AXIS2_PLACEMENT_3D('',#215997,#31245,#31246);
#26887=AXIS2_PLACEMENT_3D('',#215999,#31248,#31249);
#26888=AXIS2_PLACEMENT_3D('',#216000,#31250,#31251);
#26889=AXIS2_PLACEMENT_3D('',#216001,#31252,#31253);
#26890=AXIS2_PLACEMENT_3D('',#216002,#31254,#31255);
#26891=AXIS2_PLACEMENT_3D('',#217654,#31261,#31262);
#26892=AXIS2_PLACEMENT_3D('',#219306,#31268,#31269);
#26893=AXIS2_PLACEMENT_3D('',#220958,#31275,#31276);
#26894=AXIS2_PLACEMENT_3D('',#222610,#31282,#31283);
#26895=AXIS2_PLACEMENT_3D('',#224262,#31289,#31290);
#26896=AXIS2_PLACEMENT_3D('',#225914,#31296,#31297);
#26897=AXIS2_PLACEMENT_3D('',#227566,#31303,#31304);
#26898=AXIS2_PLACEMENT_3D('',#229218,#31310,#31311);
#26899=AXIS2_PLACEMENT_3D('',#230870,#31317,#31318);
#26900=AXIS2_PLACEMENT_3D('',#232522,#31324,#31325);
#26901=AXIS2_PLACEMENT_3D('',#234174,#31331,#31332);
#26902=AXIS2_PLACEMENT_3D('',#235826,#31338,#31339);
#26903=AXIS2_PLACEMENT_3D('',#237478,#31345,#31346);
#26904=AXIS2_PLACEMENT_3D('',#239130,#31352,#31353);
#26905=AXIS2_PLACEMENT_3D('',#240782,#31359,#31360);
#26906=AXIS2_PLACEMENT_3D('',#242434,#31366,#31367);
#26907=AXIS2_PLACEMENT_3D('',#244086,#31373,#31374);
#26908=AXIS2_PLACEMENT_3D('',#245738,#31380,#31381);
#26909=AXIS2_PLACEMENT_3D('',#247390,#31387,#31388);
#26910=AXIS2_PLACEMENT_3D('',#249042,#31394,#31395);
#26911=AXIS2_PLACEMENT_3D('',#250694,#31401,#31402);
#26912=AXIS2_PLACEMENT_3D('',#252346,#31408,#31409);
#26913=AXIS2_PLACEMENT_3D('',#253998,#31415,#31416);
#26914=AXIS2_PLACEMENT_3D('',#253999,#31417,#31418);
#26915=AXIS2_PLACEMENT_3D('',#254000,#31419,#31420);
#26916=AXIS2_PLACEMENT_3D('',#254001,#31421,#31422);
#26917=AXIS2_PLACEMENT_3D('',#254002,#31423,#31424);
#26918=AXIS2_PLACEMENT_3D('',#254003,#31425,#31426);
#26919=AXIS2_PLACEMENT_3D('',#254004,#31427,#31428);
#26920=AXIS2_PLACEMENT_3D('',#254005,#31429,#31430);
#26921=AXIS2_PLACEMENT_3D('',#254006,#31431,#31432);
#26922=AXIS2_PLACEMENT_3D('',#254007,#31433,#31434);
#26923=AXIS2_PLACEMENT_3D('',#254008,#31435,#31436);
#26924=AXIS2_PLACEMENT_3D('',#254009,#31437,#31438);
#26925=AXIS2_PLACEMENT_3D('',#254010,#31439,#31440);
#26926=AXIS2_PLACEMENT_3D('',#254011,#31441,#31442);
#26927=AXIS2_PLACEMENT_3D('',#254012,#31443,#31444);
#26928=AXIS2_PLACEMENT_3D('',#254013,#31445,#31446);
#26929=AXIS2_PLACEMENT_3D('',#254014,#31447,#31448);
#26930=AXIS2_PLACEMENT_3D('',#254015,#31449,#31450);
#26931=AXIS2_PLACEMENT_3D('',#254016,#31451,#31452);
#26932=AXIS2_PLACEMENT_3D('',#254017,#31453,#31454);
#26933=AXIS2_PLACEMENT_3D('',#254018,#31455,#31456);
#26934=AXIS2_PLACEMENT_3D('',#254019,#31457,#31458);
#26935=AXIS2_PLACEMENT_3D('',#254020,#31459,#31460);
#26936=AXIS2_PLACEMENT_3D('',#254022,#31461,#31462);
#26937=AXIS2_PLACEMENT_3D('',#254232,#31464,#31465);
#26938=AXIS2_PLACEMENT_3D('',#254234,#31466,#31467);
#26939=AXIS2_PLACEMENT_3D('',#254236,#31468,#31469);
#26940=AXIS2_PLACEMENT_3D('',#254445,#31471,#31472);
#26941=AXIS2_PLACEMENT_3D('',#254447,#31473,#31474);
#26942=AXIS2_PLACEMENT_3D('',#254448,#31475,#31476);
#26943=AXIS2_PLACEMENT_3D('',#254450,#31477,#31478);
#26944=AXIS2_PLACEMENT_3D('',#254660,#31480,#31481);
#26945=AXIS2_PLACEMENT_3D('',#254662,#31482,#31483);
#26946=AXIS2_PLACEMENT_3D('',#254664,#31484,#31485);
#26947=AXIS2_PLACEMENT_3D('',#254873,#31487,#31488);
#26948=AXIS2_PLACEMENT_3D('',#254874,#31489,#31490);
#26949=AXIS2_PLACEMENT_3D('',#254875,#31491,#31492);
#26950=AXIS2_PLACEMENT_3D('',#254876,#31493,#31494);
#26951=AXIS2_PLACEMENT_3D('',#254877,#31495,#31496);
#26952=AXIS2_PLACEMENT_3D('',#254878,#31497,#31498);
#26953=AXIS2_PLACEMENT_3D('',#254879,#31499,#31500);
#26954=AXIS2_PLACEMENT_3D('',#254880,#31501,#31502);
#26955=AXIS2_PLACEMENT_3D('',#254881,#31503,#31504);
#26956=AXIS2_PLACEMENT_3D('',#254882,#31505,#31506);
#26957=AXIS2_PLACEMENT_3D('',#254883,#31507,#31508);
#26958=AXIS2_PLACEMENT_3D('',#254884,#31509,#31510);
#26959=AXIS2_PLACEMENT_3D('',#254885,#31511,#31512);
#26960=AXIS2_PLACEMENT_3D('',#254886,#31513,#31514);
#26961=AXIS2_PLACEMENT_3D('',#254887,#31515,#31516);
#26962=AXIS2_PLACEMENT_3D('',#254888,#31517,#31518);
#26963=AXIS2_PLACEMENT_3D('',#254889,#31519,#31520);
#26964=AXIS2_PLACEMENT_3D('',#254890,#31521,#31522);
#26965=AXIS2_PLACEMENT_3D('',#254891,#31523,#31524);
#26966=AXIS2_PLACEMENT_3D('',#254892,#31525,#31526);
#26967=AXIS2_PLACEMENT_3D('',#254893,#31527,#31528);
#26968=AXIS2_PLACEMENT_3D('',#254894,#31529,#31530);
#26969=AXIS2_PLACEMENT_3D('',#254895,#31531,#31532);
#26970=AXIS2_PLACEMENT_3D('',#254897,#31533,#31534);
#26971=AXIS2_PLACEMENT_3D('',#254898,#31535,#31536);
#26972=AXIS2_PLACEMENT_3D('',#254900,#31538,#31539);
#26973=AXIS2_PLACEMENT_3D('',#254901,#31540,#31541);
#26974=AXIS2_PLACEMENT_3D('',#254902,#31542,#31543);
#26975=AXIS2_PLACEMENT_3D('',#254903,#31544,#31545);
#26976=AXIS2_PLACEMENT_3D('',#254904,#31546,#31547);
#26977=AXIS2_PLACEMENT_3D('',#254905,#31548,#31549);
#26978=AXIS2_PLACEMENT_3D('',#254906,#31550,#31551);
#26979=AXIS2_PLACEMENT_3D('',#254907,#31552,#31553);
#26980=AXIS2_PLACEMENT_3D('',#254908,#31554,#31555);
#26981=AXIS2_PLACEMENT_3D('',#254909,#31556,#31557);
#26982=AXIS2_PLACEMENT_3D('',#254910,#31558,#31559);
#26983=AXIS2_PLACEMENT_3D('',#254911,#31560,#31561);
#26984=AXIS2_PLACEMENT_3D('',#254912,#31562,#31563);
#26985=AXIS2_PLACEMENT_3D('',#254913,#31564,#31565);
#26986=AXIS2_PLACEMENT_3D('',#254914,#31566,#31567);
#26987=AXIS2_PLACEMENT_3D('',#254915,#31568,#31569);
#26988=AXIS2_PLACEMENT_3D('',#254916,#31570,#31571);
#26989=AXIS2_PLACEMENT_3D('',#254917,#31572,#31573);
#26990=AXIS2_PLACEMENT_3D('',#254918,#31574,#31575);
#26991=AXIS2_PLACEMENT_3D('',#254919,#31576,#31577);
#26992=AXIS2_PLACEMENT_3D('',#254920,#31578,#31579);
#26993=AXIS2_PLACEMENT_3D('',#254921,#31580,#31581);
#26994=AXIS2_PLACEMENT_3D('',#254922,#31582,#31583);
#26995=AXIS2_PLACEMENT_3D('',#254925,#31586,#31587);
#26996=AXIS2_PLACEMENT_3D('',#254927,#31589,#31590);
#26997=AXIS2_PLACEMENT_3D('',#254930,#31593,#31594);
#26998=AXIS2_PLACEMENT_3D('',#254931,#31595,#31596);
#26999=AXIS2_PLACEMENT_3D('',#255754,#31599,#31600);
#27000=AXIS2_PLACEMENT_3D('',#255756,#31602,#31603);
#27001=AXIS2_PLACEMENT_3D('',#255757,#31604,#31605);
#27002=AXIS2_PLACEMENT_3D('',#255758,#31606,#31607);
#27003=AXIS2_PLACEMENT_3D('',#255760,#31608,#31609);
#27004=AXIS2_PLACEMENT_3D('',#255763,#31611,#31612);
#27005=AXIS2_PLACEMENT_3D('',#255764,#31613,#31614);
#27006=AXIS2_PLACEMENT_3D('',#255766,#31615,#31616);
#27007=AXIS2_PLACEMENT_3D('',#255769,#31618,#31619);
#27008=AXIS2_PLACEMENT_3D('',#255770,#31620,#31621);
#27009=AXIS2_PLACEMENT_3D('',#255771,#31622,#31623);
#27010=AXIS2_PLACEMENT_3D('',#255772,#31624,#31625);
#27011=AXIS2_PLACEMENT_3D('',#255773,#31626,#31627);
#27012=AXIS2_PLACEMENT_3D('',#255782,#31632,#31633);
#27013=AXIS2_PLACEMENT_3D('',#255784,#31634,#31635);
#27014=AXIS2_PLACEMENT_3D('',#255788,#31638,#31639);
#27015=AXIS2_PLACEMENT_3D('',#255794,#31643,#31644);
#27016=AXIS2_PLACEMENT_3D('',#255796,#31646,#31647);
#27017=AXIS2_PLACEMENT_3D('',#255797,#31648,#31649);
#27018=AXIS2_PLACEMENT_3D('',#255798,#31650,#31651);
#27019=AXIS2_PLACEMENT_3D('',#255800,#31652,#31653);
#27020=AXIS2_PLACEMENT_3D('',#255803,#31655,#31656);
#27021=AXIS2_PLACEMENT_3D('',#255804,#31657,#31658);
#27022=AXIS2_PLACEMENT_3D('',#255806,#31659,#31660);
#27023=AXIS2_PLACEMENT_3D('',#255807,#31661,#31662);
#27024=AXIS2_PLACEMENT_3D('',#255809,#31663,#31664);
#27025=AXIS2_PLACEMENT_3D('',#255810,#31665,#31666);
#27026=AXIS2_PLACEMENT_3D('',#255812,#31667,#31668);
#27027=AXIS2_PLACEMENT_3D('',#255814,#31670,#31671);
#27028=AXIS2_PLACEMENT_3D('',#255816,#31672,#31673);
#27029=AXIS2_PLACEMENT_3D('',#255819,#31675,#31676);
#27030=AXIS2_PLACEMENT_3D('',#255820,#31677,#31678);
#27031=AXIS2_PLACEMENT_3D('',#255822,#31679,#31680);
#27032=AXIS2_PLACEMENT_3D('',#255823,#31681,#31682);
#27033=AXIS2_PLACEMENT_3D('',#255825,#31683,#31684);
#27034=AXIS2_PLACEMENT_3D('',#255826,#31685,#31686);
#27035=AXIS2_PLACEMENT_3D('',#255828,#31687,#31688);
#27036=AXIS2_PLACEMENT_3D('',#255830,#31690,#31691);
#27037=AXIS2_PLACEMENT_3D('',#255832,#31692,#31693);
#27038=AXIS2_PLACEMENT_3D('',#255835,#31695,#31696);
#27039=AXIS2_PLACEMENT_3D('',#255836,#31697,#31698);
#27040=AXIS2_PLACEMENT_3D('',#255838,#31699,#31700);
#27041=AXIS2_PLACEMENT_3D('',#255841,#31702,#31703);
#27042=AXIS2_PLACEMENT_3D('',#255842,#31704,#31705);
#27043=AXIS2_PLACEMENT_3D('',#255844,#31706,#31707);
#27044=AXIS2_PLACEMENT_3D('',#255847,#31709,#31710);
#27045=AXIS2_PLACEMENT_3D('',#255848,#31711,#31712);
#27046=AXIS2_PLACEMENT_3D('',#255850,#31713,#31714);
#27047=AXIS2_PLACEMENT_3D('',#255852,#31715,#31716);
#27048=AXIS2_PLACEMENT_3D('',#255853,#31717,#31718);
#27049=AXIS2_PLACEMENT_3D('',#255855,#31719,#31720);
#27050=AXIS2_PLACEMENT_3D('',#255857,#31721,#31722);
#27051=AXIS2_PLACEMENT_3D('',#255858,#31723,#31724);
#27052=AXIS2_PLACEMENT_3D('',#255860,#31726,#31727);
#27053=AXIS2_PLACEMENT_3D('',#255863,#31729,#31730);
#27054=AXIS2_PLACEMENT_3D('',#255864,#31731,#31732);
#27055=AXIS2_PLACEMENT_3D('',#255866,#31734,#31735);
#27056=AXIS2_PLACEMENT_3D('',#255867,#31736,#31737);
#27057=AXIS2_PLACEMENT_3D('',#255869,#31738,#31739);
#27058=AXIS2_PLACEMENT_3D('',#255871,#31740,#31741);
#27059=AXIS2_PLACEMENT_3D('',#255872,#31742,#31743);
#27060=AXIS2_PLACEMENT_3D('',#255874,#31744,#31745);
#27061=AXIS2_PLACEMENT_3D('',#255876,#31746,#31747);
#27062=AXIS2_PLACEMENT_3D('',#255877,#31748,#31749);
#27063=AXIS2_PLACEMENT_3D('',#255879,#31751,#31752);
#27064=AXIS2_PLACEMENT_3D('',#255882,#31754,#31755);
#27065=AXIS2_PLACEMENT_3D('',#255883,#31756,#31757);
#27066=AXIS2_PLACEMENT_3D('',#255885,#31758,#31759);
#27067=AXIS2_PLACEMENT_3D('',#255886,#31760,#31761);
#27068=AXIS2_PLACEMENT_3D('',#255888,#31763,#31764);
#27069=AXIS2_PLACEMENT_3D('',#255889,#31765,#31766);
#27070=AXIS2_PLACEMENT_3D('',#255892,#31768,#31769);
#27071=AXIS2_PLACEMENT_3D('',#255893,#31770,#31771);
#27072=AXIS2_PLACEMENT_3D('',#255895,#31772,#31773);
#27073=AXIS2_PLACEMENT_3D('',#255898,#31775,#31776);
#27074=AXIS2_PLACEMENT_3D('',#255899,#31777,#31778);
#27075=AXIS2_PLACEMENT_3D('',#255900,#31779,#31780);
#27076=AXIS2_PLACEMENT_3D('',#255901,#31781,#31782);
#27077=AXIS2_PLACEMENT_3D('',#255902,#31783,#31784);
#27078=AXIS2_PLACEMENT_3D('',#255911,#31789,#31790);
#27079=AXIS2_PLACEMENT_3D('',#255917,#31794,#31795);
#27080=AXIS2_PLACEMENT_3D('',#255923,#31799,#31800);
#27081=AXIS2_PLACEMENT_3D('',#255926,#31803,#31804);
#27082=AXIS2_PLACEMENT_3D('',#255927,#31805,#31806);
#27083=AXIS2_PLACEMENT_3D('',#255928,#31807,#31808);
#27084=AXIS2_PLACEMENT_3D('',#255929,#31809,#31810);
#27085=AXIS2_PLACEMENT_3D('',#255931,#31811,#31812);
#27086=AXIS2_PLACEMENT_3D('',#255934,#31814,#31815);
#27087=AXIS2_PLACEMENT_3D('',#255935,#31816,#31817);
#27088=AXIS2_PLACEMENT_3D('',#255937,#31818,#31819);
#27089=AXIS2_PLACEMENT_3D('',#255940,#31821,#31822);
#27090=AXIS2_PLACEMENT_3D('',#255941,#31823,#31824);
#27091=AXIS2_PLACEMENT_3D('',#255942,#31825,#31826);
#27092=AXIS2_PLACEMENT_3D('',#255943,#31827,#31828);
#27093=AXIS2_PLACEMENT_3D('',#255944,#31829,#31830);
#27094=AXIS2_PLACEMENT_3D('',#255946,#31831,#31832);
#27095=AXIS2_PLACEMENT_3D('',#255949,#31834,#31835);
#27096=AXIS2_PLACEMENT_3D('',#255950,#31836,#31837);
#27097=AXIS2_PLACEMENT_3D('',#255952,#31838,#31839);
#27098=AXIS2_PLACEMENT_3D('',#255953,#31840,#31841);
#27099=AXIS2_PLACEMENT_3D('',#255955,#31842,#31843);
#27100=AXIS2_PLACEMENT_3D('',#255956,#31844,#31845);
#27101=AXIS2_PLACEMENT_3D('',#255958,#31846,#31847);
#27102=AXIS2_PLACEMENT_3D('',#255960,#31849,#31850);
#27103=AXIS2_PLACEMENT_3D('',#255962,#31851,#31852);
#27104=AXIS2_PLACEMENT_3D('',#255964,#31853,#31854);
#27105=AXIS2_PLACEMENT_3D('',#255965,#31855,#31856);
#27106=AXIS2_PLACEMENT_3D('',#255968,#31858,#31859);
#27107=AXIS2_PLACEMENT_3D('',#255969,#31860,#31861);
#27108=AXIS2_PLACEMENT_3D('',#255970,#31862,#31863);
#27109=AXIS2_PLACEMENT_3D('',#255972,#31865,#31866);
#27110=AXIS2_PLACEMENT_3D('',#255973,#31867,#31868);
#27111=AXIS2_PLACEMENT_3D('',#255974,#31869,#31870);
#27112=AXIS2_PLACEMENT_3D('',#255983,#31875,#31876);
#27113=AXIS2_PLACEMENT_3D('',#255992,#31881,#31882);
#27114=AXIS2_PLACEMENT_3D('',#255993,#31883,#31884);
#27115=AXIS2_PLACEMENT_3D('',#255994,#31885,#31886);
#27116=AXIS2_PLACEMENT_3D('',#255995,#31887,#31888);
#27117=AXIS2_PLACEMENT_3D('',#255996,#31889,#31890);
#27118=AXIS2_PLACEMENT_3D('',#255997,#31891,#31892);
#27119=AXIS2_PLACEMENT_3D('',#255998,#31893,#31894);
#27120=AXIS2_PLACEMENT_3D('',#255999,#31895,#31896);
#27121=AXIS2_PLACEMENT_3D('',#256000,#31897,#31898);
#27122=AXIS2_PLACEMENT_3D('',#256001,#31899,#31900);
#27123=AXIS2_PLACEMENT_3D('',#256003,#31901,#31902);
#27124=AXIS2_PLACEMENT_3D('',#256006,#31904,#31905);
#27125=AXIS2_PLACEMENT_3D('',#256007,#31906,#31907);
#27126=AXIS2_PLACEMENT_3D('',#256009,#31908,#31909);
#27127=AXIS2_PLACEMENT_3D('',#256012,#31911,#31912);
#27128=AXIS2_PLACEMENT_3D('',#256013,#31913,#31914);
#27129=AXIS2_PLACEMENT_3D('',#256014,#31915,#31916);
#27130=AXIS2_PLACEMENT_3D('',#256015,#31917,#31918);
#27131=AXIS2_PLACEMENT_3D('',#256016,#31919,#31920);
#27132=AXIS2_PLACEMENT_3D('',#256018,#31921,#31922);
#27133=AXIS2_PLACEMENT_3D('',#256021,#31924,#31925);
#27134=AXIS2_PLACEMENT_3D('',#256022,#31926,#31927);
#27135=AXIS2_PLACEMENT_3D('',#256024,#31928,#31929);
#27136=AXIS2_PLACEMENT_3D('',#256027,#31931,#31932);
#27137=AXIS2_PLACEMENT_3D('',#256028,#31933,#31934);
#27138=AXIS2_PLACEMENT_3D('',#256029,#31935,#31936);
#27139=AXIS2_PLACEMENT_3D('',#256030,#31937,#31938);
#27140=AXIS2_PLACEMENT_3D('',#256031,#31939,#31940);
#27141=AXIS2_PLACEMENT_3D('',#256033,#31941,#31942);
#27142=AXIS2_PLACEMENT_3D('',#256036,#31944,#31945);
#27143=AXIS2_PLACEMENT_3D('',#256037,#31946,#31947);
#27144=AXIS2_PLACEMENT_3D('',#256039,#31948,#31949);
#27145=AXIS2_PLACEMENT_3D('',#256042,#31951,#31952);
#27146=AXIS2_PLACEMENT_3D('',#256043,#31953,#31954);
#27147=AXIS2_PLACEMENT_3D('',#256044,#31955,#31956);
#27148=AXIS2_PLACEMENT_3D('',#256045,#31957,#31958);
#27149=AXIS2_PLACEMENT_3D('',#256046,#31959,#31960);
#27150=AXIS2_PLACEMENT_3D('',#256055,#31965,#31966);
#27151=AXIS2_PLACEMENT_3D('',#256064,#31971,#31972);
#27152=AXIS2_PLACEMENT_3D('',#256065,#31973,#31974);
#27153=AXIS2_PLACEMENT_3D('',#256066,#31975,#31976);
#27154=AXIS2_PLACEMENT_3D('',#256067,#31977,#31978);
#27155=AXIS2_PLACEMENT_3D('',#256068,#31979,#31980);
#27156=AXIS2_PLACEMENT_3D('',#256069,#31981,#31982);
#27157=AXIS2_PLACEMENT_3D('',#256070,#31983,#31984);
#27158=AXIS2_PLACEMENT_3D('',#256071,#31985,#31986);
#27159=AXIS2_PLACEMENT_3D('',#256072,#31987,#31988);
#27160=AXIS2_PLACEMENT_3D('',#256073,#31989,#31990);
#27161=AXIS2_PLACEMENT_3D('',#256082,#31995,#31996);
#27162=AXIS2_PLACEMENT_3D('',#256091,#32001,#32002);
#27163=AXIS2_PLACEMENT_3D('',#256092,#32003,#32004);
#27164=AXIS2_PLACEMENT_3D('',#256093,#32005,#32006);
#27165=AXIS2_PLACEMENT_3D('',#256094,#32007,#32008);
#27166=AXIS2_PLACEMENT_3D('',#256095,#32009,#32010);
#27167=AXIS2_PLACEMENT_3D('',#256096,#32011,#32012);
#27168=AXIS2_PLACEMENT_3D('',#256097,#32013,#32014);
#27169=AXIS2_PLACEMENT_3D('',#256098,#32015,#32016);
#27170=AXIS2_PLACEMENT_3D('',#256099,#32017,#32018);
#27171=AXIS2_PLACEMENT_3D('',#256100,#32019,#32020);
#27172=AXIS2_PLACEMENT_3D('',#256102,#32021,#32022);
#27173=AXIS2_PLACEMENT_3D('',#256105,#32024,#32025);
#27174=AXIS2_PLACEMENT_3D('',#256106,#32026,#32027);
#27175=AXIS2_PLACEMENT_3D('',#256107,#32028,#32029);
#27176=AXIS2_PLACEMENT_3D('',#256108,#32030,#32031);
#27177=AXIS2_PLACEMENT_3D('',#256109,#32032,#32033);
#27178=AXIS2_PLACEMENT_3D('',#256125,#32035,#32036);
#27179=AXIS2_PLACEMENT_3D('',#256133,#32037,#32038);
#27180=AXIS2_PLACEMENT_3D('',#256181,#32040,#32041);
#27181=AXIS2_PLACEMENT_3D('',#256229,#32043,#32044);
#27182=AXIS2_PLACEMENT_3D('',#256280,#32046,#32047);
#27183=AXIS2_PLACEMENT_3D('',#256331,#32049,#32050);
#27184=AXIS2_PLACEMENT_3D('',#256379,#32052,#32053);
#27185=AXIS2_PLACEMENT_3D('',#256427,#32055,#32056);
#27186=AXIS2_PLACEMENT_3D('',#256481,#32058,#32059);
#27187=AXIS2_PLACEMENT_3D('',#256529,#32061,#32062);
#27188=AXIS2_PLACEMENT_3D('',#256577,#32064,#32065);
#27189=AXIS2_PLACEMENT_3D('',#256631,#32067,#32068);
#27190=AXIS2_PLACEMENT_3D('',#256679,#32070,#32071);
#27191=AXIS2_PLACEMENT_3D('',#256727,#32073,#32074);
#27192=AXIS2_PLACEMENT_3D('',#256775,#32076,#32077);
#27193=AXIS2_PLACEMENT_3D('',#256829,#32079,#32080);
#27194=AXIS2_PLACEMENT_3D('',#256877,#32082,#32083);
#27195=AXIS2_PLACEMENT_3D('',#256925,#32085,#32086);
#27196=AXIS2_PLACEMENT_3D('',#256979,#32088,#32089);
#27197=AXIS2_PLACEMENT_3D('',#257027,#32091,#32092);
#27198=AXIS2_PLACEMENT_3D('',#257075,#32094,#32095);
#27199=AXIS2_PLACEMENT_3D('',#257087,#32097,#32098);
#27200=AXIS2_PLACEMENT_3D('',#257092,#32099,#32100);
#27201=AXIS2_PLACEMENT_3D('',#257117,#32102,#32103);
#27202=AXIS2_PLACEMENT_3D('',#257141,#32105,#32106);
#27203=AXIS2_PLACEMENT_3D('',#257166,#32108,#32109);
#27204=AXIS2_PLACEMENT_3D('',#257191,#32111,#32112);
#27205=AXIS2_PLACEMENT_3D('',#257215,#32114,#32115);
#27206=AXIS2_PLACEMENT_3D('',#257240,#32117,#32118);
#27207=AXIS2_PLACEMENT_3D('',#257265,#32120,#32121);
#27208=AXIS2_PLACEMENT_3D('',#257289,#32123,#32124);
#27209=AXIS2_PLACEMENT_3D('',#257313,#32126,#32127);
#27210=AXIS2_PLACEMENT_3D('',#257338,#32129,#32130);
#27211=AXIS2_PLACEMENT_3D('',#257363,#32132,#32133);
#27212=AXIS2_PLACEMENT_3D('',#257387,#32135,#32136);
#27213=AXIS2_PLACEMENT_3D('',#257412,#32138,#32139);
#27214=AXIS2_PLACEMENT_3D('',#257437,#32141,#32142);
#27215=AXIS2_PLACEMENT_3D('',#257461,#32144,#32145);
#27216=AXIS2_PLACEMENT_3D('',#257486,#32147,#32148);
#27217=AXIS2_PLACEMENT_3D('',#257510,#32150,#32151);
#27218=AXIS2_PLACEMENT_3D('',#257535,#32153,#32154);
#27219=AXIS2_PLACEMENT_3D('',#258298,#32156,#32157);
#27220=AXIS2_PLACEMENT_3D('',#258300,#32158,#32159);
#27221=AXIS2_PLACEMENT_3D('',#259035,#32160,#32161);
#27222=AXIS2_PLACEMENT_3D('',#259036,#32162,#32163);
#27223=AXIS2_PLACEMENT_3D('',#259037,#32164,#32165);
#27224=AXIS2_PLACEMENT_3D('',#259046,#32170,#32171);
#27225=AXIS2_PLACEMENT_3D('',#259052,#32175,#32176);
#27226=AXIS2_PLACEMENT_3D('',#259058,#32180,#32181);
#27227=AXIS2_PLACEMENT_3D('',#259064,#32185,#32186);
#27228=AXIS2_PLACEMENT_3D('',#259070,#32190,#32191);
#27229=AXIS2_PLACEMENT_3D('',#259073,#32194,#32195);
#27230=AXIS2_PLACEMENT_3D('',#259074,#32196,#32197);
#27231=AXIS2_PLACEMENT_3D('',#259076,#32198,#32199);
#27232=AXIS2_PLACEMENT_3D('',#259077,#32200,#32201);
#27233=AXIS2_PLACEMENT_3D('',#259080,#32203,#32204);
#27234=AXIS2_PLACEMENT_3D('',#259081,#32205,#32206);
#27235=AXIS2_PLACEMENT_3D('',#259082,#32207,#32208);
#27236=AXIS2_PLACEMENT_3D('',#259083,#32209,#32210);
#27237=AXIS2_PLACEMENT_3D('',#259084,#32211,#32212);
#27238=AXIS2_PLACEMENT_3D('',#259085,#32213,#32214);
#27239=AXIS2_PLACEMENT_3D('',#259086,#32215,#32216);
#27240=AXIS2_PLACEMENT_3D('',#259087,#32217,#32218);
#27241=AXIS2_PLACEMENT_3D('',#259088,#32219,#32220);
#27242=AXIS2_PLACEMENT_3D('',#259089,#32221,#32222);
#27243=AXIS2_PLACEMENT_3D('',#259090,#32223,#32224);
#27244=AXIS2_PLACEMENT_3D('',#259091,#32225,#32226);
#27245=AXIS2_PLACEMENT_3D('',#259092,#32227,#32228);
#27246=AXIS2_PLACEMENT_3D('',#259093,#32229,#32230);
#27247=AXIS2_PLACEMENT_3D('',#259094,#32231,#32232);
#27248=AXIS2_PLACEMENT_3D('',#259095,#32233,#32234);
#27249=AXIS2_PLACEMENT_3D('',#259096,#32235,#32236);
#27250=AXIS2_PLACEMENT_3D('',#259097,#32237,#32238);
#27251=AXIS2_PLACEMENT_3D('',#259098,#32239,#32240);
#27252=AXIS2_PLACEMENT_3D('',#259099,#32241,#32242);
#27253=AXIS2_PLACEMENT_3D('',#259100,#32243,#32244);
#27254=AXIS2_PLACEMENT_3D('',#259101,#32245,#32246);
#27255=AXIS2_PLACEMENT_3D('',#259102,#32247,#32248);
#27256=AXIS2_PLACEMENT_3D('',#259103,#32249,#32250);
#27257=AXIS2_PLACEMENT_3D('',#259104,#32251,#32252);
#27258=AXIS2_PLACEMENT_3D('',#259105,#32253,#32254);
#27259=AXIS2_PLACEMENT_3D('',#259106,#32255,#32256);
#27260=AXIS2_PLACEMENT_3D('',#259107,#32257,#32258);
#27261=AXIS2_PLACEMENT_3D('',#259108,#32259,#32260);
#27262=AXIS2_PLACEMENT_3D('',#259109,#32261,#32262);
#27263=AXIS2_PLACEMENT_3D('',#259110,#32263,#32264);
#27264=AXIS2_PLACEMENT_3D('',#259111,#32265,#32266);
#27265=AXIS2_PLACEMENT_3D('',#259112,#32267,#32268);
#27266=AXIS2_PLACEMENT_3D('',#259113,#32269,#32270);
#27267=AXIS2_PLACEMENT_3D('',#259114,#32271,#32272);
#27268=AXIS2_PLACEMENT_3D('',#259115,#32273,#32274);
#27269=AXIS2_PLACEMENT_3D('',#259116,#32275,#32276);
#27270=AXIS2_PLACEMENT_3D('',#259117,#32277,#32278);
#27271=AXIS2_PLACEMENT_3D('',#259118,#32279,#32280);
#27272=AXIS2_PLACEMENT_3D('',#259119,#32281,#32282);
#27273=AXIS2_PLACEMENT_3D('',#259120,#32283,#32284);
#27274=AXIS2_PLACEMENT_3D('',#259121,#32285,#32286);
#27275=AXIS2_PLACEMENT_3D('',#259122,#32287,#32288);
#27276=AXIS2_PLACEMENT_3D('',#259123,#32289,#32290);
#27277=AXIS2_PLACEMENT_3D('',#259124,#32291,#32292);
#27278=AXIS2_PLACEMENT_3D('',#259125,#32293,#32294);
#27279=AXIS2_PLACEMENT_3D('',#259126,#32295,#32296);
#27280=AXIS2_PLACEMENT_3D('',#259127,#32297,#32298);
#27281=AXIS2_PLACEMENT_3D('',#259128,#32299,#32300);
#27282=AXIS2_PLACEMENT_3D('',#259129,#32301,#32302);
#27283=AXIS2_PLACEMENT_3D('',#259130,#32303,#32304);
#27284=AXIS2_PLACEMENT_3D('',#259131,#32305,#32306);
#27285=AXIS2_PLACEMENT_3D('',#259132,#32307,#32308);
#27286=AXIS2_PLACEMENT_3D('',#259133,#32309,#32310);
#27287=AXIS2_PLACEMENT_3D('',#259134,#32311,#32312);
#27288=AXIS2_PLACEMENT_3D('',#259135,#32313,#32314);
#27289=AXIS2_PLACEMENT_3D('',#259136,#32315,#32316);
#27290=AXIS2_PLACEMENT_3D('',#259137,#32317,#32318);
#27291=AXIS2_PLACEMENT_3D('',#259138,#32319,#32320);
#27292=AXIS2_PLACEMENT_3D('',#259139,#32321,#32322);
#27293=AXIS2_PLACEMENT_3D('',#259140,#32323,#32324);
#27294=AXIS2_PLACEMENT_3D('',#259141,#32325,#32326);
#27295=AXIS2_PLACEMENT_3D('',#259142,#32327,#32328);
#27296=AXIS2_PLACEMENT_3D('',#259143,#32329,#32330);
#27297=AXIS2_PLACEMENT_3D('',#259144,#32331,#32332);
#27298=AXIS2_PLACEMENT_3D('',#259145,#32333,#32334);
#27299=AXIS2_PLACEMENT_3D('',#259146,#32335,#32336);
#27300=AXIS2_PLACEMENT_3D('',#259147,#32337,#32338);
#27301=AXIS2_PLACEMENT_3D('',#259148,#32339,#32340);
#27302=AXIS2_PLACEMENT_3D('',#259149,#32341,#32342);
#27303=AXIS2_PLACEMENT_3D('',#259150,#32343,#32344);
#27304=AXIS2_PLACEMENT_3D('',#259151,#32345,#32346);
#27305=AXIS2_PLACEMENT_3D('',#259152,#32347,#32348);
#27306=AXIS2_PLACEMENT_3D('',#259153,#32349,#32350);
#27307=AXIS2_PLACEMENT_3D('',#259154,#32351,#32352);
#27308=AXIS2_PLACEMENT_3D('',#259155,#32353,#32354);
#27309=AXIS2_PLACEMENT_3D('',#259156,#32355,#32356);
#27310=AXIS2_PLACEMENT_3D('',#259157,#32357,#32358);
#27311=AXIS2_PLACEMENT_3D('',#259158,#32359,#32360);
#27312=AXIS2_PLACEMENT_3D('',#259159,#32361,#32362);
#27313=AXIS2_PLACEMENT_3D('',#259160,#32363,#32364);
#27314=AXIS2_PLACEMENT_3D('',#259161,#32365,#32366);
#27315=AXIS2_PLACEMENT_3D('',#259162,#32367,#32368);
#27316=AXIS2_PLACEMENT_3D('',#259163,#32369,#32370);
#27317=AXIS2_PLACEMENT_3D('',#259164,#32371,#32372);
#27318=AXIS2_PLACEMENT_3D('',#259165,#32373,#32374);
#27319=AXIS2_PLACEMENT_3D('',#259166,#32375,#32376);
#27320=AXIS2_PLACEMENT_3D('',#259167,#32377,#32378);
#27321=AXIS2_PLACEMENT_3D('',#259168,#32379,#32380);
#27322=AXIS2_PLACEMENT_3D('',#259169,#32381,#32382);
#27323=AXIS2_PLACEMENT_3D('',#259170,#32383,#32384);
#27324=AXIS2_PLACEMENT_3D('',#259171,#32385,#32386);
#27325=AXIS2_PLACEMENT_3D('',#259172,#32387,#32388);
#27326=AXIS2_PLACEMENT_3D('',#259173,#32389,#32390);
#27327=AXIS2_PLACEMENT_3D('',#259174,#32391,#32392);
#27328=AXIS2_PLACEMENT_3D('',#259175,#32393,#32394);
#27329=AXIS2_PLACEMENT_3D('',#259176,#32395,#32396);
#27330=AXIS2_PLACEMENT_3D('',#259177,#32397,#32398);
#27331=AXIS2_PLACEMENT_3D('',#259178,#32399,#32400);
#27332=AXIS2_PLACEMENT_3D('',#259179,#32401,#32402);
#27333=AXIS2_PLACEMENT_3D('',#259180,#32403,#32404);
#27334=DIRECTION('axis',(0.,0.,1.));
#27335=DIRECTION('refdir',(1.,0.,0.));
#27336=DIRECTION('axis',(0.,0.,1.));
#27337=DIRECTION('refdir',(1.,0.,0.));
#27338=DIRECTION('center_axis',(0.,0.,-1.));
#27339=DIRECTION('ref_axis',(1.,0.,0.));
#27340=DIRECTION('',(0.,0.,-1.));
#27341=DIRECTION('center_axis',(0.,0.,1.));
#27342=DIRECTION('ref_axis',(1.,0.,0.));
#27343=DIRECTION('',(0.,0.,-1.));
#27344=DIRECTION('center_axis',(0.,0.,1.));
#27345=DIRECTION('ref_axis',(1.,0.,0.));
#27346=DIRECTION('center_axis',(0.,0.,1.));
#27347=DIRECTION('ref_axis',(1.,0.,0.));
#27348=DIRECTION('center_axis',(0.,0.,-1.));
#27349=DIRECTION('ref_axis',(1.,0.,0.));
#27350=DIRECTION('',(0.,0.,-1.));
#27351=DIRECTION('center_axis',(0.,0.,-1.));
#27352=DIRECTION('ref_axis',(1.,0.,0.));
#27353=DIRECTION('',(0.,0.,-1.));
#27354=DIRECTION('center_axis',(0.,0.,-1.));
#27355=DIRECTION('ref_axis',(1.,0.,0.));
#27356=DIRECTION('',(0.,0.,-1.));
#27357=DIRECTION('center_axis',(0.,0.,-1.));
#27358=DIRECTION('ref_axis',(1.,0.,0.));
#27359=DIRECTION('',(0.,0.,-1.));
#27360=DIRECTION('center_axis',(0.,0.,-1.));
#27361=DIRECTION('ref_axis',(1.,0.,0.));
#27362=DIRECTION('',(0.,0.,-1.));
#27363=DIRECTION('center_axis',(0.,0.,-1.));
#27364=DIRECTION('ref_axis',(1.,0.,0.));
#27365=DIRECTION('',(0.,0.,-1.));
#27366=DIRECTION('center_axis',(0.,0.,-1.));
#27367=DIRECTION('ref_axis',(1.,0.,0.));
#27368=DIRECTION('',(0.,0.,-1.));
#27369=DIRECTION('center_axis',(0.,0.,-1.));
#27370=DIRECTION('ref_axis',(1.,0.,0.));
#27371=DIRECTION('',(0.,0.,-1.));
#27372=DIRECTION('center_axis',(0.,0.,-1.));
#27373=DIRECTION('ref_axis',(1.,0.,0.));
#27374=DIRECTION('',(0.,0.,-1.));
#27375=DIRECTION('center_axis',(0.,0.,-1.));
#27376=DIRECTION('ref_axis',(1.,0.,0.));
#27377=DIRECTION('',(0.,0.,-1.));
#27378=DIRECTION('center_axis',(0.,0.,-1.));
#27379=DIRECTION('ref_axis',(1.,0.,0.));
#27380=DIRECTION('',(0.,0.,-1.));
#27381=DIRECTION('center_axis',(0.,0.,-1.));
#27382=DIRECTION('ref_axis',(1.,0.,0.));
#27383=DIRECTION('',(0.,0.,-1.));
#27384=DIRECTION('center_axis',(0.,0.,-1.));
#27385=DIRECTION('ref_axis',(1.,0.,0.));
#27386=DIRECTION('',(0.,0.,-1.));
#27387=DIRECTION('center_axis',(0.,0.,-1.));
#27388=DIRECTION('ref_axis',(0.938009462242609,-0.346609648947243,0.));
#27389=DIRECTION('',(0.,0.,-1.));
#27390=DIRECTION('center_axis',(0.,0.,-1.));
#27391=DIRECTION('ref_axis',(1.,0.,0.));
#27392=DIRECTION('center_axis',(0.,0.,-1.));
#27393=DIRECTION('ref_axis',(1.,-9.39183297226423E-14,0.));
#27394=DIRECTION('',(1.22464679914735E-16,-1.15166757854366E-29,-1.));
#27395=DIRECTION('center_axis',(0.,0.,1.));
#27396=DIRECTION('ref_axis',(1.,-9.39183297226423E-14,0.));
#27397=DIRECTION('center_axis',(0.,0.,-1.));
#27398=DIRECTION('ref_axis',(1.,-9.39183297226423E-14,0.));
#27399=DIRECTION('',(1.22464679914735E-16,-1.15166757854366E-29,-1.));
#27400=DIRECTION('center_axis',(0.,0.,-1.));
#27401=DIRECTION('ref_axis',(1.,-9.39183297226423E-14,0.));
#27402=DIRECTION('',(1.22464679914735E-16,-1.15166757854366E-29,-1.));
#27403=DIRECTION('center_axis',(0.,0.,-1.));
#27404=DIRECTION('ref_axis',(1.,-9.39183297226423E-14,0.));
#27405=DIRECTION('',(1.22464679914735E-16,-1.15166757854366E-29,-1.));
#27406=DIRECTION('center_axis',(0.,0.,-1.));
#27407=DIRECTION('ref_axis',(1.,-9.39183297226423E-14,0.));
#27408=DIRECTION('',(1.22464679914735E-16,-1.15166757854366E-29,-1.));
#27409=DIRECTION('center_axis',(0.,0.,-1.));
#27410=DIRECTION('ref_axis',(1.,-9.39183297226423E-14,0.));
#27411=DIRECTION('',(1.22464679914735E-16,-1.15166757854366E-29,-1.));
#27412=DIRECTION('center_axis',(0.,0.,-1.));
#27413=DIRECTION('ref_axis',(1.,-9.39183297226423E-14,0.));
#27414=DIRECTION('',(1.22464679914735E-16,-1.15166757854366E-29,-1.));
#27415=DIRECTION('center_axis',(0.,0.,-1.));
#27416=DIRECTION('ref_axis',(1.,-9.39183297226423E-14,0.));
#27417=DIRECTION('',(1.22464679914735E-16,-1.15166757854366E-29,-1.));
#27418=DIRECTION('center_axis',(0.,0.,-1.));
#27419=DIRECTION('ref_axis',(1.,-9.39183297226423E-14,0.));
#27420=DIRECTION('',(1.22464679914735E-16,-1.15166757854366E-29,-1.));
#27421=DIRECTION('center_axis',(0.,0.,-1.));
#27422=DIRECTION('ref_axis',(1.,-9.39183297226423E-14,0.));
#27423=DIRECTION('',(1.22464679914735E-16,-1.15166757854366E-29,-1.));
#27424=DIRECTION('center_axis',(0.,0.,-1.));
#27425=DIRECTION('ref_axis',(1.,-9.39183297226423E-14,0.));
#27426=DIRECTION('',(1.22464679914735E-16,-1.15166757854366E-29,-1.));
#27427=DIRECTION('center_axis',(0.,0.,-1.));
#27428=DIRECTION('ref_axis',(1.,-9.39183297226423E-14,0.));
#27429=DIRECTION('',(1.22464679914735E-16,-1.15166757854366E-29,-1.));
#27430=DIRECTION('center_axis',(0.,0.,-1.));
#27431=DIRECTION('ref_axis',(1.,-9.39183297226423E-14,0.));
#27432=DIRECTION('',(1.22464679914735E-16,-1.15166757854366E-29,-1.));
#27433=DIRECTION('center_axis',(0.,0.,-1.));
#27434=DIRECTION('ref_axis',(1.,-9.39183297226423E-14,0.));
#27435=DIRECTION('',(1.22464679914735E-16,-1.15166757854366E-29,-1.));
#27436=DIRECTION('center_axis',(0.,0.,-1.));
#27437=DIRECTION('ref_axis',(-0.609165547211943,-0.793043085897591,0.));
#27438=DIRECTION('',(1.22464679914735E-16,-1.15166757854366E-29,-1.));
#27439=DIRECTION('center_axis',(0.,0.,-1.));
#27440=DIRECTION('ref_axis',(1.,-9.39183297226423E-14,0.));
#27441=DIRECTION('center_axis',(0.,0.,-1.));
#27442=DIRECTION('ref_axis',(1.,0.,0.));
#27443=DIRECTION('',(0.,0.,-1.));
#27444=DIRECTION('center_axis',(0.,0.,1.));
#27445=DIRECTION('ref_axis',(1.,0.,0.));
#27446=DIRECTION('',(0.,0.,-1.));
#27447=DIRECTION('center_axis',(0.,0.,1.));
#27448=DIRECTION('ref_axis',(1.,0.,0.));
#27449=DIRECTION('center_axis',(0.,0.,1.));
#27450=DIRECTION('ref_axis',(1.,0.,0.));
#27451=DIRECTION('center_axis',(0.,0.,-1.));
#27452=DIRECTION('ref_axis',(1.,0.,0.));
#27453=DIRECTION('',(0.,0.,-1.));
#27454=DIRECTION('center_axis',(0.,0.,-1.));
#27455=DIRECTION('ref_axis',(1.,0.,0.));
#27456=DIRECTION('',(0.,0.,-1.));
#27457=DIRECTION('center_axis',(0.,0.,-1.));
#27458=DIRECTION('ref_axis',(1.,0.,0.));
#27459=DIRECTION('',(0.,0.,-1.));
#27460=DIRECTION('center_axis',(0.,0.,-1.));
#27461=DIRECTION('ref_axis',(1.,0.,0.));
#27462=DIRECTION('',(0.,0.,-1.));
#27463=DIRECTION('center_axis',(0.,0.,-1.));
#27464=DIRECTION('ref_axis',(1.,0.,0.));
#27465=DIRECTION('',(0.,0.,-1.));
#27466=DIRECTION('center_axis',(0.,0.,-1.));
#27467=DIRECTION('ref_axis',(1.,0.,0.));
#27468=DIRECTION('',(0.,0.,-1.));
#27469=DIRECTION('center_axis',(0.,0.,-1.));
#27470=DIRECTION('ref_axis',(1.,0.,0.));
#27471=DIRECTION('',(0.,0.,-1.));
#27472=DIRECTION('center_axis',(0.,0.,-1.));
#27473=DIRECTION('ref_axis',(1.,0.,0.));
#27474=DIRECTION('',(0.,0.,-1.));
#27475=DIRECTION('center_axis',(0.,0.,-1.));
#27476=DIRECTION('ref_axis',(1.,0.,0.));
#27477=DIRECTION('',(0.,0.,-1.));
#27478=DIRECTION('center_axis',(0.,0.,-1.));
#27479=DIRECTION('ref_axis',(1.,0.,0.));
#27480=DIRECTION('',(0.,0.,-1.));
#27481=DIRECTION('center_axis',(0.,0.,-1.));
#27482=DIRECTION('ref_axis',(1.,0.,0.));
#27483=DIRECTION('',(0.,0.,-1.));
#27484=DIRECTION('center_axis',(0.,0.,-1.));
#27485=DIRECTION('ref_axis',(1.,0.,0.));
#27486=DIRECTION('',(0.,0.,-1.));
#27487=DIRECTION('center_axis',(0.,0.,-1.));
#27488=DIRECTION('ref_axis',(1.,0.,0.));
#27489=DIRECTION('',(0.,0.,-1.));
#27490=DIRECTION('center_axis',(0.,0.,-1.));
#27491=DIRECTION('ref_axis',(0.93800946033191,-0.346609654118057,0.));
#27492=DIRECTION('',(0.,0.,-1.));
#27493=DIRECTION('center_axis',(0.,0.,-1.));
#27494=DIRECTION('ref_axis',(1.,0.,0.));
#27495=DIRECTION('center_axis',(0.,0.,-1.));
#27496=DIRECTION('ref_axis',(1.,-9.10285349619456E-14,0.));
#27497=DIRECTION('',(1.22464679914735E-16,-1.11627779950486E-29,-1.));
#27498=DIRECTION('center_axis',(0.,0.,1.));
#27499=DIRECTION('ref_axis',(1.,-9.10285349619456E-14,0.));
#27500=DIRECTION('center_axis',(0.,0.,-1.));
#27501=DIRECTION('ref_axis',(1.,-9.10285349619456E-14,0.));
#27502=DIRECTION('',(1.22464679914735E-16,-1.11627779950486E-29,-1.));
#27503=DIRECTION('center_axis',(0.,0.,-1.));
#27504=DIRECTION('ref_axis',(1.,-9.10285349619456E-14,0.));
#27505=DIRECTION('',(1.22464679914735E-16,-1.11627779950486E-29,-1.));
#27506=DIRECTION('center_axis',(0.,0.,-1.));
#27507=DIRECTION('ref_axis',(1.,-9.10285349619456E-14,0.));
#27508=DIRECTION('',(1.22464679914735E-16,-1.11627779950486E-29,-1.));
#27509=DIRECTION('center_axis',(0.,0.,-1.));
#27510=DIRECTION('ref_axis',(1.,-9.10285349619456E-14,0.));
#27511=DIRECTION('',(1.22464679914735E-16,-1.11627779950486E-29,-1.));
#27512=DIRECTION('center_axis',(0.,0.,-1.));
#27513=DIRECTION('ref_axis',(1.,-9.10285349619456E-14,0.));
#27514=DIRECTION('',(1.22464679914735E-16,-1.11627779950486E-29,-1.));
#27515=DIRECTION('center_axis',(0.,0.,-1.));
#27516=DIRECTION('ref_axis',(1.,-9.10285349619456E-14,0.));
#27517=DIRECTION('',(1.22464679914735E-16,-1.11627779950486E-29,-1.));
#27518=DIRECTION('center_axis',(0.,0.,-1.));
#27519=DIRECTION('ref_axis',(1.,-9.10285349619456E-14,0.));
#27520=DIRECTION('',(1.22464679914735E-16,-1.11627779950486E-29,-1.));
#27521=DIRECTION('center_axis',(0.,0.,-1.));
#27522=DIRECTION('ref_axis',(1.,-9.10285349619456E-14,0.));
#27523=DIRECTION('',(1.22464679914735E-16,-1.11627779950486E-29,-1.));
#27524=DIRECTION('center_axis',(0.,0.,-1.));
#27525=DIRECTION('ref_axis',(1.,-9.10285349619456E-14,0.));
#27526=DIRECTION('',(1.22464679914735E-16,-1.11627779950486E-29,-1.));
#27527=DIRECTION('center_axis',(0.,0.,-1.));
#27528=DIRECTION('ref_axis',(1.,-9.10285349619456E-14,0.));
#27529=DIRECTION('',(1.22464679914735E-16,-1.11627779950486E-29,-1.));
#27530=DIRECTION('center_axis',(0.,0.,-1.));
#27531=DIRECTION('ref_axis',(1.,-9.10285349619456E-14,0.));
#27532=DIRECTION('',(1.22464679914735E-16,-1.11627779950486E-29,-1.));
#27533=DIRECTION('center_axis',(0.,0.,-1.));
#27534=DIRECTION('ref_axis',(1.,-9.10285349619456E-14,0.));
#27535=DIRECTION('',(1.22464679914735E-16,-1.11627779950486E-29,-1.));
#27536=DIRECTION('center_axis',(0.,0.,-1.));
#27537=DIRECTION('ref_axis',(1.,-9.10285349619456E-14,0.));
#27538=DIRECTION('',(1.22464679914735E-16,-1.11627779950486E-29,-1.));
#27539=DIRECTION('center_axis',(0.,0.,-1.));
#27540=DIRECTION('ref_axis',(-0.609165548712575,-0.793043084744901,0.));
#27541=DIRECTION('',(1.22464679914735E-16,-1.11627779950486E-29,-1.));
#27542=DIRECTION('center_axis',(0.,0.,-1.));
#27543=DIRECTION('ref_axis',(1.,-9.10285349619456E-14,0.));
#27544=DIRECTION('center_axis',(0.,0.,-1.));
#27545=DIRECTION('ref_axis',(1.,0.,0.));
#27546=DIRECTION('',(0.,0.,-1.));
#27547=DIRECTION('center_axis',(0.,0.,1.));
#27548=DIRECTION('ref_axis',(1.,0.,0.));
#27549=DIRECTION('',(0.,0.,-1.));
#27550=DIRECTION('center_axis',(0.,0.,1.));
#27551=DIRECTION('ref_axis',(1.,0.,0.));
#27552=DIRECTION('center_axis',(0.,0.,1.));
#27553=DIRECTION('ref_axis',(1.,0.,0.));
#27554=DIRECTION('center_axis',(0.,0.,-1.));
#27555=DIRECTION('ref_axis',(1.,0.,0.));
#27556=DIRECTION('',(0.,0.,-1.));
#27557=DIRECTION('center_axis',(0.,0.,-1.));
#27558=DIRECTION('ref_axis',(1.,0.,0.));
#27559=DIRECTION('',(0.,0.,-1.));
#27560=DIRECTION('center_axis',(0.,0.,-1.));
#27561=DIRECTION('ref_axis',(1.,0.,0.));
#27562=DIRECTION('',(0.,0.,-1.));
#27563=DIRECTION('center_axis',(0.,0.,-1.));
#27564=DIRECTION('ref_axis',(1.,0.,0.));
#27565=DIRECTION('',(0.,0.,-1.));
#27566=DIRECTION('center_axis',(0.,0.,-1.));
#27567=DIRECTION('ref_axis',(1.,0.,0.));
#27568=DIRECTION('',(0.,0.,-1.));
#27569=DIRECTION('center_axis',(0.,0.,-1.));
#27570=DIRECTION('ref_axis',(1.,0.,0.));
#27571=DIRECTION('',(0.,0.,-1.));
#27572=DIRECTION('center_axis',(0.,0.,-1.));
#27573=DIRECTION('ref_axis',(1.,0.,0.));
#27574=DIRECTION('',(0.,0.,-1.));
#27575=DIRECTION('center_axis',(0.,0.,-1.));
#27576=DIRECTION('ref_axis',(1.,0.,0.));
#27577=DIRECTION('',(0.,0.,-1.));
#27578=DIRECTION('center_axis',(0.,0.,-1.));
#27579=DIRECTION('ref_axis',(1.,0.,0.));
#27580=DIRECTION('',(0.,0.,-1.));
#27581=DIRECTION('center_axis',(0.,0.,-1.));
#27582=DIRECTION('ref_axis',(1.,0.,0.));
#27583=DIRECTION('',(0.,0.,-1.));
#27584=DIRECTION('center_axis',(0.,0.,-1.));
#27585=DIRECTION('ref_axis',(1.,0.,0.));
#27586=DIRECTION('',(0.,0.,-1.));
#27587=DIRECTION('center_axis',(0.,0.,-1.));
#27588=DIRECTION('ref_axis',(1.,0.,0.));
#27589=DIRECTION('',(0.,0.,-1.));
#27590=DIRECTION('center_axis',(0.,0.,-1.));
#27591=DIRECTION('ref_axis',(1.,0.,0.));
#27592=DIRECTION('',(0.,0.,-1.));
#27593=DIRECTION('center_axis',(0.,0.,-1.));
#27594=DIRECTION('ref_axis',(0.938009461339291,-0.34660965139184,0.));
#27595=DIRECTION('',(0.,0.,-1.));
#27596=DIRECTION('center_axis',(0.,0.,-1.));
#27597=DIRECTION('ref_axis',(1.,0.,0.));
#27598=DIRECTION('center_axis',(0.,0.,-1.));
#27599=DIRECTION('ref_axis',(1.,-1.09812200906474E-13,0.));
#27600=DIRECTION('',(1.22464679914735E-16,-1.34631136325705E-29,-1.));
#27601=DIRECTION('center_axis',(0.,0.,1.));
#27602=DIRECTION('ref_axis',(1.,-1.09812200906474E-13,0.));
#27603=DIRECTION('center_axis',(0.,0.,-1.));
#27604=DIRECTION('ref_axis',(1.,-1.09812200906474E-13,0.));
#27605=DIRECTION('',(1.22464679914735E-16,-1.34631136325705E-29,-1.));
#27606=DIRECTION('center_axis',(0.,0.,-1.));
#27607=DIRECTION('ref_axis',(1.,-1.09812200906474E-13,0.));
#27608=DIRECTION('',(1.22464679914735E-16,-1.34631136325705E-29,-1.));
#27609=DIRECTION('center_axis',(0.,0.,-1.));
#27610=DIRECTION('ref_axis',(1.,-1.09812200906474E-13,0.));
#27611=DIRECTION('',(1.22464679914735E-16,-1.34631136325705E-29,-1.));
#27612=DIRECTION('center_axis',(0.,0.,-1.));
#27613=DIRECTION('ref_axis',(1.,-1.09812200906474E-13,0.));
#27614=DIRECTION('',(1.22464679914735E-16,-1.34631136325705E-29,-1.));
#27615=DIRECTION('center_axis',(0.,0.,-1.));
#27616=DIRECTION('ref_axis',(1.,-1.09812200906474E-13,0.));
#27617=DIRECTION('',(1.22464679914735E-16,-1.34631136325705E-29,-1.));
#27618=DIRECTION('center_axis',(0.,0.,-1.));
#27619=DIRECTION('ref_axis',(1.,-1.09812200906474E-13,0.));
#27620=DIRECTION('',(1.22464679914735E-16,-1.34631136325705E-29,-1.));
#27621=DIRECTION('center_axis',(0.,0.,-1.));
#27622=DIRECTION('ref_axis',(1.,-1.09812200906474E-13,0.));
#27623=DIRECTION('',(1.22464679914735E-16,-1.34631136325705E-29,-1.));
#27624=DIRECTION('center_axis',(0.,0.,-1.));
#27625=DIRECTION('ref_axis',(1.,-1.09812200906474E-13,0.));
#27626=DIRECTION('',(1.22464679914735E-16,-1.34631136325705E-29,-1.));
#27627=DIRECTION('center_axis',(0.,0.,-1.));
#27628=DIRECTION('ref_axis',(1.,-1.09812200906474E-13,0.));
#27629=DIRECTION('',(1.22464679914735E-16,-1.34631136325705E-29,-1.));
#27630=DIRECTION('center_axis',(0.,0.,-1.));
#27631=DIRECTION('ref_axis',(1.,-1.09812200906474E-13,0.));
#27632=DIRECTION('',(1.22464679914735E-16,-1.34631136325705E-29,-1.));
#27633=DIRECTION('center_axis',(0.,0.,-1.));
#27634=DIRECTION('ref_axis',(1.,-1.09812200906474E-13,0.));
#27635=DIRECTION('',(1.22464679914735E-16,-1.34631136325705E-29,-1.));
#27636=DIRECTION('center_axis',(0.,0.,-1.));
#27637=DIRECTION('ref_axis',(1.,-1.09812200906474E-13,0.));
#27638=DIRECTION('',(1.22464679914735E-16,-1.34631136325705E-29,-1.));
#27639=DIRECTION('center_axis',(0.,0.,-1.));
#27640=DIRECTION('ref_axis',(1.,-1.09812200906474E-13,0.));
#27641=DIRECTION('',(1.22464679914735E-16,-1.34631136325705E-29,-1.));
#27642=DIRECTION('center_axis',(0.,0.,-1.));
#27643=DIRECTION('ref_axis',(-0.609165549363982,-0.793043084244531,0.));
#27644=DIRECTION('',(1.22464679914735E-16,-1.34631136325705E-29,-1.));
#27645=DIRECTION('center_axis',(0.,0.,-1.));
#27646=DIRECTION('ref_axis',(1.,-1.09812200906474E-13,0.));
#27647=DIRECTION('center_axis',(0.,0.,-1.));
#27648=DIRECTION('ref_axis',(1.,0.,0.));
#27649=DIRECTION('',(0.,0.,-1.));
#27650=DIRECTION('center_axis',(0.,0.,1.));
#27651=DIRECTION('ref_axis',(1.,0.,0.));
#27652=DIRECTION('',(0.,0.,-1.));
#27653=DIRECTION('center_axis',(0.,0.,1.));
#27654=DIRECTION('ref_axis',(1.,0.,0.));
#27655=DIRECTION('center_axis',(0.,0.,1.));
#27656=DIRECTION('ref_axis',(1.,0.,0.));
#27657=DIRECTION('center_axis',(0.,0.,-1.));
#27658=DIRECTION('ref_axis',(1.,0.,0.));
#27659=DIRECTION('',(0.,0.,-1.));
#27660=DIRECTION('center_axis',(0.,0.,-1.));
#27661=DIRECTION('ref_axis',(1.,0.,0.));
#27662=DIRECTION('',(0.,0.,-1.));
#27663=DIRECTION('center_axis',(0.,0.,-1.));
#27664=DIRECTION('ref_axis',(1.,0.,0.));
#27665=DIRECTION('',(0.,0.,-1.));
#27666=DIRECTION('center_axis',(0.,0.,-1.));
#27667=DIRECTION('ref_axis',(1.,0.,0.));
#27668=DIRECTION('',(0.,0.,-1.));
#27669=DIRECTION('center_axis',(0.,0.,-1.));
#27670=DIRECTION('ref_axis',(1.,0.,0.));
#27671=DIRECTION('',(0.,0.,-1.));
#27672=DIRECTION('center_axis',(0.,0.,-1.));
#27673=DIRECTION('ref_axis',(1.,0.,0.));
#27674=DIRECTION('',(0.,0.,-1.));
#27675=DIRECTION('center_axis',(0.,0.,-1.));
#27676=DIRECTION('ref_axis',(1.,0.,0.));
#27677=DIRECTION('',(0.,0.,-1.));
#27678=DIRECTION('center_axis',(0.,0.,-1.));
#27679=DIRECTION('ref_axis',(1.,0.,0.));
#27680=DIRECTION('',(0.,0.,-1.));
#27681=DIRECTION('center_axis',(0.,0.,-1.));
#27682=DIRECTION('ref_axis',(1.,0.,0.));
#27683=DIRECTION('',(0.,0.,-1.));
#27684=DIRECTION('center_axis',(0.,0.,-1.));
#27685=DIRECTION('ref_axis',(1.,0.,0.));
#27686=DIRECTION('',(0.,0.,-1.));
#27687=DIRECTION('center_axis',(0.,0.,-1.));
#27688=DIRECTION('ref_axis',(1.,0.,0.));
#27689=DIRECTION('',(0.,0.,-1.));
#27690=DIRECTION('center_axis',(0.,0.,-1.));
#27691=DIRECTION('ref_axis',(1.,0.,0.));
#27692=DIRECTION('',(0.,0.,-1.));
#27693=DIRECTION('center_axis',(0.,0.,-1.));
#27694=DIRECTION('ref_axis',(1.,0.,0.));
#27695=DIRECTION('',(0.,0.,-1.));
#27696=DIRECTION('center_axis',(0.,0.,-1.));
#27697=DIRECTION('ref_axis',(0.938009461339277,-0.346609651391878,0.));
#27698=DIRECTION('',(0.,0.,-1.));
#27699=DIRECTION('center_axis',(0.,0.,-1.));
#27700=DIRECTION('ref_axis',(1.,0.,0.));
#27701=DIRECTION('center_axis',(0.,0.,-1.));
#27702=DIRECTION('ref_axis',(1.,-9.39183297226423E-14,0.));
#27703=DIRECTION('',(1.22464679914735E-16,-1.15166757854366E-29,-1.));
#27704=DIRECTION('center_axis',(0.,0.,1.));
#27705=DIRECTION('ref_axis',(1.,-9.39183297226423E-14,0.));
#27706=DIRECTION('center_axis',(0.,0.,-1.));
#27707=DIRECTION('ref_axis',(1.,-9.39183297226423E-14,0.));
#27708=DIRECTION('',(1.22464679914735E-16,-1.15166757854366E-29,-1.));
#27709=DIRECTION('center_axis',(0.,0.,-1.));
#27710=DIRECTION('ref_axis',(1.,-9.39183297226423E-14,0.));
#27711=DIRECTION('',(1.22464679914735E-16,-1.15166757854366E-29,-1.));
#27712=DIRECTION('center_axis',(0.,0.,-1.));
#27713=DIRECTION('ref_axis',(1.,-9.39183297226423E-14,0.));
#27714=DIRECTION('',(1.22464679914735E-16,-1.15166757854366E-29,-1.));
#27715=DIRECTION('center_axis',(0.,0.,-1.));
#27716=DIRECTION('ref_axis',(1.,-9.39183297226423E-14,0.));
#27717=DIRECTION('',(1.22464679914735E-16,-1.15166757854366E-29,-1.));
#27718=DIRECTION('center_axis',(0.,0.,-1.));
#27719=DIRECTION('ref_axis',(1.,-9.39183297226423E-14,0.));
#27720=DIRECTION('',(1.22464679914735E-16,-1.15166757854366E-29,-1.));
#27721=DIRECTION('center_axis',(0.,0.,-1.));
#27722=DIRECTION('ref_axis',(1.,-9.39183297226423E-14,0.));
#27723=DIRECTION('',(1.22464679914735E-16,-1.15166757854366E-29,-1.));
#27724=DIRECTION('center_axis',(0.,0.,-1.));
#27725=DIRECTION('ref_axis',(1.,-9.39183297226423E-14,0.));
#27726=DIRECTION('',(1.22464679914735E-16,-1.15166757854366E-29,-1.));
#27727=DIRECTION('center_axis',(0.,0.,-1.));
#27728=DIRECTION('ref_axis',(1.,-9.39183297226423E-14,0.));
#27729=DIRECTION('',(1.22464679914735E-16,-1.15166757854366E-29,-1.));
#27730=DIRECTION('center_axis',(0.,0.,-1.));
#27731=DIRECTION('ref_axis',(1.,-9.39183297226423E-14,0.));
#27732=DIRECTION('',(1.22464679914735E-16,-1.15166757854366E-29,-1.));
#27733=DIRECTION('center_axis',(0.,0.,-1.));
#27734=DIRECTION('ref_axis',(1.,-9.39183297226423E-14,0.));
#27735=DIRECTION('',(1.22464679914735E-16,-1.15166757854366E-29,-1.));
#27736=DIRECTION('center_axis',(0.,0.,-1.));
#27737=DIRECTION('ref_axis',(1.,-9.39183297226423E-14,0.));
#27738=DIRECTION('',(1.22464679914735E-16,-1.15166757854366E-29,-1.));
#27739=DIRECTION('center_axis',(0.,0.,-1.));
#27740=DIRECTION('ref_axis',(1.,-9.39183297226423E-14,0.));
#27741=DIRECTION('',(1.22464679914735E-16,-1.15166757854366E-29,-1.));
#27742=DIRECTION('center_axis',(0.,0.,-1.));
#27743=DIRECTION('ref_axis',(1.,-9.39183297226423E-14,0.));
#27744=DIRECTION('',(1.22464679914735E-16,-1.15166757854366E-29,-1.));
#27745=DIRECTION('center_axis',(0.,0.,-1.));
#27746=DIRECTION('ref_axis',(-0.609165549364011,-0.793043084244508,0.));
#27747=DIRECTION('',(1.22464679914735E-16,-1.15166757854366E-29,-1.));
#27748=DIRECTION('center_axis',(0.,0.,-1.));
#27749=DIRECTION('ref_axis',(1.,-9.39183297226423E-14,0.));
#27750=DIRECTION('center_axis',(0.,0.,-1.));
#27751=DIRECTION('ref_axis',(1.,0.,0.));
#27752=DIRECTION('',(0.,0.,-1.));
#27753=DIRECTION('center_axis',(0.,0.,1.));
#27754=DIRECTION('ref_axis',(1.,0.,0.));
#27755=DIRECTION('',(0.,0.,-1.));
#27756=DIRECTION('center_axis',(0.,0.,1.));
#27757=DIRECTION('ref_axis',(1.,0.,0.));
#27758=DIRECTION('center_axis',(0.,0.,1.));
#27759=DIRECTION('ref_axis',(1.,0.,0.));
#27760=DIRECTION('center_axis',(0.,0.,-1.));
#27761=DIRECTION('ref_axis',(1.,0.,0.));
#27762=DIRECTION('',(0.,0.,-1.));
#27763=DIRECTION('center_axis',(0.,0.,-1.));
#27764=DIRECTION('ref_axis',(1.,0.,0.));
#27765=DIRECTION('',(0.,0.,-1.));
#27766=DIRECTION('center_axis',(0.,0.,-1.));
#27767=DIRECTION('ref_axis',(1.,0.,0.));
#27768=DIRECTION('',(0.,0.,-1.));
#27769=DIRECTION('center_axis',(0.,0.,-1.));
#27770=DIRECTION('ref_axis',(1.,0.,0.));
#27771=DIRECTION('',(0.,0.,-1.));
#27772=DIRECTION('center_axis',(0.,0.,-1.));
#27773=DIRECTION('ref_axis',(1.,0.,0.));
#27774=DIRECTION('',(0.,0.,-1.));
#27775=DIRECTION('center_axis',(0.,0.,-1.));
#27776=DIRECTION('ref_axis',(1.,0.,0.));
#27777=DIRECTION('',(0.,0.,-1.));
#27778=DIRECTION('center_axis',(0.,0.,-1.));
#27779=DIRECTION('ref_axis',(1.,0.,0.));
#27780=DIRECTION('',(0.,0.,-1.));
#27781=DIRECTION('center_axis',(0.,0.,-1.));
#27782=DIRECTION('ref_axis',(1.,0.,0.));
#27783=DIRECTION('',(0.,0.,-1.));
#27784=DIRECTION('center_axis',(0.,0.,-1.));
#27785=DIRECTION('ref_axis',(1.,0.,0.));
#27786=DIRECTION('',(0.,0.,-1.));
#27787=DIRECTION('center_axis',(0.,0.,-1.));
#27788=DIRECTION('ref_axis',(1.,0.,0.));
#27789=DIRECTION('',(0.,0.,-1.));
#27790=DIRECTION('center_axis',(0.,0.,-1.));
#27791=DIRECTION('ref_axis',(1.,0.,0.));
#27792=DIRECTION('',(0.,0.,-1.));
#27793=DIRECTION('center_axis',(0.,0.,-1.));
#27794=DIRECTION('ref_axis',(1.,0.,0.));
#27795=DIRECTION('',(0.,0.,-1.));
#27796=DIRECTION('center_axis',(0.,0.,-1.));
#27797=DIRECTION('ref_axis',(1.,0.,0.));
#27798=DIRECTION('',(0.,0.,-1.));
#27799=DIRECTION('center_axis',(0.,0.,-1.));
#27800=DIRECTION('ref_axis',(0.938009463044599,-0.346609646776865,0.));
#27801=DIRECTION('',(0.,0.,-1.));
#27802=DIRECTION('center_axis',(0.,0.,-1.));
#27803=DIRECTION('ref_axis',(1.,0.,0.));
#27804=DIRECTION('center_axis',(0.,0.,-1.));
#27805=DIRECTION('ref_axis',(1.,-7.51346637781136E-14,0.));
#27806=DIRECTION('',(1.22464679914735E-16,-9.21634014791456E-30,-1.));
#27807=DIRECTION('center_axis',(0.,0.,1.));
#27808=DIRECTION('ref_axis',(1.,-7.51346637781136E-14,0.));
#27809=DIRECTION('center_axis',(0.,0.,-1.));
#27810=DIRECTION('ref_axis',(1.,-7.51346637781136E-14,0.));
#27811=DIRECTION('',(1.22464679914735E-16,-9.21634014791456E-30,-1.));
#27812=DIRECTION('center_axis',(0.,0.,-1.));
#27813=DIRECTION('ref_axis',(1.,-7.51346637781136E-14,0.));
#27814=DIRECTION('',(1.22464679914735E-16,-9.21634014791456E-30,-1.));
#27815=DIRECTION('center_axis',(0.,0.,-1.));
#27816=DIRECTION('ref_axis',(1.,-7.51346637781136E-14,0.));
#27817=DIRECTION('',(1.22464679914735E-16,-9.21634014791456E-30,-1.));
#27818=DIRECTION('center_axis',(0.,0.,-1.));
#27819=DIRECTION('ref_axis',(1.,-7.51346637781136E-14,0.));
#27820=DIRECTION('',(1.22464679914735E-16,-9.21634014791456E-30,-1.));
#27821=DIRECTION('center_axis',(0.,0.,-1.));
#27822=DIRECTION('ref_axis',(1.,-7.51346637781136E-14,0.));
#27823=DIRECTION('',(1.22464679914735E-16,-9.21634014791456E-30,-1.));
#27824=DIRECTION('center_axis',(0.,0.,-1.));
#27825=DIRECTION('ref_axis',(1.,-7.51346637781136E-14,0.));
#27826=DIRECTION('',(1.22464679914735E-16,-9.21634014791456E-30,-1.));
#27827=DIRECTION('center_axis',(0.,0.,-1.));
#27828=DIRECTION('ref_axis',(1.,-7.51346637781136E-14,0.));
#27829=DIRECTION('',(1.22464679914735E-16,-9.21634014791456E-30,-1.));
#27830=DIRECTION('center_axis',(0.,0.,-1.));
#27831=DIRECTION('ref_axis',(1.,-7.51346637781136E-14,0.));
#27832=DIRECTION('',(1.22464679914735E-16,-9.21634014791456E-30,-1.));
#27833=DIRECTION('center_axis',(0.,0.,-1.));
#27834=DIRECTION('ref_axis',(1.,-7.51346637781136E-14,0.));
#27835=DIRECTION('',(1.22464679914735E-16,-9.21634014791456E-30,-1.));
#27836=DIRECTION('center_axis',(0.,0.,-1.));
#27837=DIRECTION('ref_axis',(1.,-7.51346637781136E-14,0.));
#27838=DIRECTION('',(1.22464679914735E-16,-9.21634014791456E-30,-1.));
#27839=DIRECTION('center_axis',(0.,0.,-1.));
#27840=DIRECTION('ref_axis',(1.,-7.51346637781136E-14,0.));
#27841=DIRECTION('',(1.22464679914735E-16,-9.21634014791456E-30,-1.));
#27842=DIRECTION('center_axis',(0.,0.,-1.));
#27843=DIRECTION('ref_axis',(1.,-7.51346637781136E-14,0.));
#27844=DIRECTION('',(1.22464679914735E-16,-9.21634014791456E-30,-1.));
#27845=DIRECTION('center_axis',(0.,0.,-1.));
#27846=DIRECTION('ref_axis',(1.,-7.51346637781136E-14,0.));
#27847=DIRECTION('',(1.22464679914735E-16,-9.21634014791456E-30,-1.));
#27848=DIRECTION('center_axis',(0.,0.,-1.));
#27849=DIRECTION('ref_axis',(-0.609165547992927,-0.793043085297689,0.));
#27850=DIRECTION('',(1.22464679914735E-16,-9.21634014791456E-30,-1.));
#27851=DIRECTION('center_axis',(0.,0.,-1.));
#27852=DIRECTION('ref_axis',(1.,-7.51346637781136E-14,0.));
#27853=DIRECTION('center_axis',(0.,0.,-1.));
#27854=DIRECTION('ref_axis',(1.,0.,0.));
#27855=DIRECTION('',(0.,0.,-1.));
#27856=DIRECTION('center_axis',(0.,0.,1.));
#27857=DIRECTION('ref_axis',(1.,0.,0.));
#27858=DIRECTION('',(0.,0.,-1.));
#27859=DIRECTION('center_axis',(0.,0.,1.));
#27860=DIRECTION('ref_axis',(1.,0.,0.));
#27861=DIRECTION('center_axis',(0.,0.,1.));
#27862=DIRECTION('ref_axis',(1.,0.,0.));
#27863=DIRECTION('center_axis',(0.,0.,-1.));
#27864=DIRECTION('ref_axis',(1.,0.,0.));
#27865=DIRECTION('',(0.,0.,-1.));
#27866=DIRECTION('center_axis',(0.,0.,-1.));
#27867=DIRECTION('ref_axis',(1.,0.,0.));
#27868=DIRECTION('',(0.,0.,-1.));
#27869=DIRECTION('center_axis',(0.,0.,-1.));
#27870=DIRECTION('ref_axis',(1.,0.,0.));
#27871=DIRECTION('',(0.,0.,-1.));
#27872=DIRECTION('center_axis',(0.,0.,-1.));
#27873=DIRECTION('ref_axis',(1.,0.,0.));
#27874=DIRECTION('',(0.,0.,-1.));
#27875=DIRECTION('center_axis',(0.,0.,-1.));
#27876=DIRECTION('ref_axis',(1.,0.,0.));
#27877=DIRECTION('',(0.,0.,-1.));
#27878=DIRECTION('center_axis',(0.,0.,-1.));
#27879=DIRECTION('ref_axis',(1.,0.,0.));
#27880=DIRECTION('',(0.,0.,-1.));
#27881=DIRECTION('center_axis',(0.,0.,-1.));
#27882=DIRECTION('ref_axis',(1.,0.,0.));
#27883=DIRECTION('',(0.,0.,-1.));
#27884=DIRECTION('center_axis',(0.,0.,-1.));
#27885=DIRECTION('ref_axis',(1.,0.,0.));
#27886=DIRECTION('',(0.,0.,-1.));
#27887=DIRECTION('center_axis',(0.,0.,-1.));
#27888=DIRECTION('ref_axis',(1.,0.,0.));
#27889=DIRECTION('',(0.,0.,-1.));
#27890=DIRECTION('center_axis',(0.,0.,-1.));
#27891=DIRECTION('ref_axis',(1.,0.,0.));
#27892=DIRECTION('',(0.,0.,-1.));
#27893=DIRECTION('center_axis',(0.,0.,-1.));
#27894=DIRECTION('ref_axis',(1.,0.,0.));
#27895=DIRECTION('',(0.,0.,-1.));
#27896=DIRECTION('center_axis',(0.,0.,-1.));
#27897=DIRECTION('ref_axis',(1.,0.,0.));
#27898=DIRECTION('',(0.,0.,-1.));
#27899=DIRECTION('center_axis',(0.,0.,-1.));
#27900=DIRECTION('ref_axis',(1.,0.,0.));
#27901=DIRECTION('',(0.,0.,-1.));
#27902=DIRECTION('center_axis',(0.,0.,-1.));
#27903=DIRECTION('ref_axis',(0.938009463044576,-0.346609646776926,0.));
#27904=DIRECTION('',(0.,0.,-1.));
#27905=DIRECTION('center_axis',(0.,0.,-1.));
#27906=DIRECTION('ref_axis',(1.,0.,0.));
#27907=DIRECTION('center_axis',(0.,0.,-1.));
#27908=DIRECTION('ref_axis',(1.,-9.39183297226423E-14,0.));
#27909=DIRECTION('',(1.22464679914735E-16,-1.15166757854366E-29,-1.));
#27910=DIRECTION('center_axis',(0.,0.,1.));
#27911=DIRECTION('ref_axis',(1.,-9.39183297226423E-14,0.));
#27912=DIRECTION('center_axis',(0.,0.,-1.));
#27913=DIRECTION('ref_axis',(1.,-9.39183297226423E-14,0.));
#27914=DIRECTION('',(1.22464679914735E-16,-1.15166757854366E-29,-1.));
#27915=DIRECTION('center_axis',(0.,0.,-1.));
#27916=DIRECTION('ref_axis',(1.,-9.39183297226423E-14,0.));
#27917=DIRECTION('',(1.22464679914735E-16,-1.15166757854366E-29,-1.));
#27918=DIRECTION('center_axis',(0.,0.,-1.));
#27919=DIRECTION('ref_axis',(1.,-9.39183297226423E-14,0.));
#27920=DIRECTION('',(1.22464679914735E-16,-1.15166757854366E-29,-1.));
#27921=DIRECTION('center_axis',(0.,0.,-1.));
#27922=DIRECTION('ref_axis',(1.,-9.39183297226423E-14,0.));
#27923=DIRECTION('',(1.22464679914735E-16,-1.15166757854366E-29,-1.));
#27924=DIRECTION('center_axis',(0.,0.,-1.));
#27925=DIRECTION('ref_axis',(1.,-9.39183297226423E-14,0.));
#27926=DIRECTION('',(1.22464679914735E-16,-1.15166757854366E-29,-1.));
#27927=DIRECTION('center_axis',(0.,0.,-1.));
#27928=DIRECTION('ref_axis',(1.,-9.39183297226423E-14,0.));
#27929=DIRECTION('',(1.22464679914735E-16,-1.15166757854366E-29,-1.));
#27930=DIRECTION('center_axis',(0.,0.,-1.));
#27931=DIRECTION('ref_axis',(1.,-9.39183297226423E-14,0.));
#27932=DIRECTION('',(1.22464679914735E-16,-1.15166757854366E-29,-1.));
#27933=DIRECTION('center_axis',(0.,0.,-1.));
#27934=DIRECTION('ref_axis',(1.,-9.39183297226423E-14,0.));
#27935=DIRECTION('',(1.22464679914735E-16,-1.15166757854366E-29,-1.));
#27936=DIRECTION('center_axis',(0.,0.,-1.));
#27937=DIRECTION('ref_axis',(1.,-9.39183297226423E-14,0.));
#27938=DIRECTION('',(1.22464679914735E-16,-1.15166757854366E-29,-1.));
#27939=DIRECTION('center_axis',(0.,0.,-1.));
#27940=DIRECTION('ref_axis',(1.,-9.39183297226423E-14,0.));
#27941=DIRECTION('',(1.22464679914735E-16,-1.15166757854366E-29,-1.));
#27942=DIRECTION('center_axis',(0.,0.,-1.));
#27943=DIRECTION('ref_axis',(1.,-9.39183297226423E-14,0.));
#27944=DIRECTION('',(1.22464679914735E-16,-1.15166757854366E-29,-1.));
#27945=DIRECTION('center_axis',(0.,0.,-1.));
#27946=DIRECTION('ref_axis',(1.,-9.39183297226423E-14,0.));
#27947=DIRECTION('',(1.22464679914735E-16,-1.15166757854366E-29,-1.));
#27948=DIRECTION('center_axis',(0.,0.,-1.));
#27949=DIRECTION('ref_axis',(1.,-9.39183297226423E-14,0.));
#27950=DIRECTION('',(1.22464679914735E-16,-1.15166757854366E-29,-1.));
#27951=DIRECTION('center_axis',(0.,0.,-1.));
#27952=DIRECTION('ref_axis',(-0.609165547992994,-0.793043085297637,0.));
#27953=DIRECTION('',(1.22464679914735E-16,-1.15166757854366E-29,-1.));
#27954=DIRECTION('center_axis',(0.,0.,-1.));
#27955=DIRECTION('ref_axis',(1.,-9.39183297226423E-14,0.));
#27956=DIRECTION('center_axis',(0.,0.,-1.));
#27957=DIRECTION('ref_axis',(1.,0.,0.));
#27958=DIRECTION('',(0.,0.,-1.));
#27959=DIRECTION('center_axis',(0.,0.,1.));
#27960=DIRECTION('ref_axis',(1.,0.,0.));
#27961=DIRECTION('',(0.,0.,-1.));
#27962=DIRECTION('center_axis',(0.,0.,1.));
#27963=DIRECTION('ref_axis',(1.,0.,0.));
#27964=DIRECTION('center_axis',(0.,0.,1.));
#27965=DIRECTION('ref_axis',(1.,0.,0.));
#27966=DIRECTION('center_axis',(0.,0.,-1.));
#27967=DIRECTION('ref_axis',(1.,0.,0.));
#27968=DIRECTION('',(0.,0.,-1.));
#27969=DIRECTION('center_axis',(0.,0.,-1.));
#27970=DIRECTION('ref_axis',(1.,0.,0.));
#27971=DIRECTION('',(0.,0.,-1.));
#27972=DIRECTION('center_axis',(0.,0.,-1.));
#27973=DIRECTION('ref_axis',(1.,0.,0.));
#27974=DIRECTION('',(0.,0.,-1.));
#27975=DIRECTION('center_axis',(0.,0.,-1.));
#27976=DIRECTION('ref_axis',(1.,0.,0.));
#27977=DIRECTION('',(0.,0.,-1.));
#27978=DIRECTION('center_axis',(0.,0.,-1.));
#27979=DIRECTION('ref_axis',(1.,0.,0.));
#27980=DIRECTION('',(0.,0.,-1.));
#27981=DIRECTION('center_axis',(0.,0.,-1.));
#27982=DIRECTION('ref_axis',(1.,0.,0.));
#27983=DIRECTION('',(0.,0.,-1.));
#27984=DIRECTION('center_axis',(0.,0.,-1.));
#27985=DIRECTION('ref_axis',(1.,0.,0.));
#27986=DIRECTION('',(0.,0.,-1.));
#27987=DIRECTION('center_axis',(0.,0.,-1.));
#27988=DIRECTION('ref_axis',(1.,0.,0.));
#27989=DIRECTION('',(0.,0.,-1.));
#27990=DIRECTION('center_axis',(0.,0.,-1.));
#27991=DIRECTION('ref_axis',(1.,0.,0.));
#27992=DIRECTION('',(0.,0.,-1.));
#27993=DIRECTION('center_axis',(0.,0.,-1.));
#27994=DIRECTION('ref_axis',(1.,0.,0.));
#27995=DIRECTION('',(0.,0.,-1.));
#27996=DIRECTION('center_axis',(0.,0.,-1.));
#27997=DIRECTION('ref_axis',(1.,0.,0.));
#27998=DIRECTION('',(0.,0.,-1.));
#27999=DIRECTION('center_axis',(0.,0.,-1.));
#28000=DIRECTION('ref_axis',(1.,0.,0.));
#28001=DIRECTION('',(0.,0.,-1.));
#28002=DIRECTION('center_axis',(0.,0.,-1.));
#28003=DIRECTION('ref_axis',(1.,0.,0.));
#28004=DIRECTION('',(0.,0.,-1.));
#28005=DIRECTION('center_axis',(0.,0.,-1.));
#28006=DIRECTION('ref_axis',(0.938009460331926,-0.346609654118015,0.));
#28007=DIRECTION('',(0.,0.,-1.));
#28008=DIRECTION('center_axis',(0.,0.,-1.));
#28009=DIRECTION('ref_axis',(1.,0.,0.));
#28010=DIRECTION('center_axis',(0.,0.,-1.));
#28011=DIRECTION('ref_axis',(1.,-8.66938428209003E-14,0.));
#28012=DIRECTION('',(1.22464679914735E-16,-1.06319313094666E-29,-1.));
#28013=DIRECTION('center_axis',(0.,0.,1.));
#28014=DIRECTION('ref_axis',(1.,-8.66938428209003E-14,0.));
#28015=DIRECTION('center_axis',(0.,0.,-1.));
#28016=DIRECTION('ref_axis',(1.,-8.66938428209003E-14,0.));
#28017=DIRECTION('',(1.22464679914735E-16,-1.06319313094666E-29,-1.));
#28018=DIRECTION('center_axis',(0.,0.,-1.));
#28019=DIRECTION('ref_axis',(1.,-8.66938428209003E-14,0.));
#28020=DIRECTION('',(1.22464679914735E-16,-1.06319313094666E-29,-1.));
#28021=DIRECTION('center_axis',(0.,0.,-1.));
#28022=DIRECTION('ref_axis',(1.,-8.66938428209003E-14,0.));
#28023=DIRECTION('',(1.22464679914735E-16,-1.06319313094666E-29,-1.));
#28024=DIRECTION('center_axis',(0.,0.,-1.));
#28025=DIRECTION('ref_axis',(1.,-8.66938428209003E-14,0.));
#28026=DIRECTION('',(1.22464679914735E-16,-1.06319313094666E-29,-1.));
#28027=DIRECTION('center_axis',(0.,0.,-1.));
#28028=DIRECTION('ref_axis',(1.,-8.66938428209003E-14,0.));
#28029=DIRECTION('',(1.22464679914735E-16,-1.06319313094666E-29,-1.));
#28030=DIRECTION('center_axis',(0.,0.,-1.));
#28031=DIRECTION('ref_axis',(1.,-8.66938428209003E-14,0.));
#28032=DIRECTION('',(1.22464679914735E-16,-1.06319313094666E-29,-1.));
#28033=DIRECTION('center_axis',(0.,0.,-1.));
#28034=DIRECTION('ref_axis',(1.,-8.66938428209003E-14,0.));
#28035=DIRECTION('',(1.22464679914735E-16,-1.06319313094666E-29,-1.));
#28036=DIRECTION('center_axis',(0.,0.,-1.));
#28037=DIRECTION('ref_axis',(1.,-8.66938428209003E-14,0.));
#28038=DIRECTION('',(1.22464679914735E-16,-1.06319313094666E-29,-1.));
#28039=DIRECTION('center_axis',(0.,0.,-1.));
#28040=DIRECTION('ref_axis',(1.,-8.66938428209003E-14,0.));
#28041=DIRECTION('',(1.22464679914735E-16,-1.06319313094666E-29,-1.));
#28042=DIRECTION('center_axis',(0.,0.,-1.));
#28043=DIRECTION('ref_axis',(1.,-8.66938428209003E-14,0.));
#28044=DIRECTION('',(1.22464679914735E-16,-1.06319313094666E-29,-1.));
#28045=DIRECTION('center_axis',(0.,0.,-1.));
#28046=DIRECTION('ref_axis',(1.,-8.66938428209003E-14,0.));
#28047=DIRECTION('',(1.22464679914735E-16,-1.06319313094666E-29,-1.));
#28048=DIRECTION('center_axis',(0.,0.,-1.));
#28049=DIRECTION('ref_axis',(1.,-8.66938428209003E-14,0.));
#28050=DIRECTION('',(1.22464679914735E-16,-1.06319313094666E-29,-1.));
#28051=DIRECTION('center_axis',(0.,0.,-1.));
#28052=DIRECTION('ref_axis',(1.,-8.66938428209003E-14,0.));
#28053=DIRECTION('',(1.22464679914735E-16,-1.06319313094666E-29,-1.));
#28054=DIRECTION('center_axis',(0.,0.,-1.));
#28055=DIRECTION('ref_axis',(-0.60916554871253,-0.793043084744935,0.));
#28056=DIRECTION('',(1.22464679914735E-16,-1.06319313094666E-29,-1.));
#28057=DIRECTION('center_axis',(0.,0.,-1.));
#28058=DIRECTION('ref_axis',(1.,-8.66938428209003E-14,0.));
#28059=DIRECTION('center_axis',(0.,0.,-1.));
#28060=DIRECTION('ref_axis',(1.,0.,0.));
#28061=DIRECTION('',(0.,0.,-1.));
#28062=DIRECTION('center_axis',(0.,0.,1.));
#28063=DIRECTION('ref_axis',(1.,0.,0.));
#28064=DIRECTION('',(0.,0.,-1.));
#28065=DIRECTION('center_axis',(0.,0.,1.));
#28066=DIRECTION('ref_axis',(1.,0.,0.));
#28067=DIRECTION('center_axis',(0.,0.,1.));
#28068=DIRECTION('ref_axis',(1.,0.,0.));
#28069=DIRECTION('center_axis',(0.,0.,-1.));
#28070=DIRECTION('ref_axis',(1.,0.,0.));
#28071=DIRECTION('',(0.,0.,-1.));
#28072=DIRECTION('center_axis',(0.,0.,-1.));
#28073=DIRECTION('ref_axis',(1.,0.,0.));
#28074=DIRECTION('',(0.,0.,-1.));
#28075=DIRECTION('center_axis',(0.,0.,-1.));
#28076=DIRECTION('ref_axis',(1.,0.,0.));
#28077=DIRECTION('',(0.,0.,-1.));
#28078=DIRECTION('center_axis',(0.,0.,-1.));
#28079=DIRECTION('ref_axis',(1.,0.,0.));
#28080=DIRECTION('',(0.,0.,-1.));
#28081=DIRECTION('center_axis',(0.,0.,-1.));
#28082=DIRECTION('ref_axis',(1.,0.,0.));
#28083=DIRECTION('',(0.,0.,-1.));
#28084=DIRECTION('center_axis',(0.,0.,-1.));
#28085=DIRECTION('ref_axis',(1.,0.,0.));
#28086=DIRECTION('',(0.,0.,-1.));
#28087=DIRECTION('center_axis',(0.,0.,-1.));
#28088=DIRECTION('ref_axis',(1.,0.,0.));
#28089=DIRECTION('',(0.,0.,-1.));
#28090=DIRECTION('center_axis',(0.,0.,-1.));
#28091=DIRECTION('ref_axis',(1.,0.,0.));
#28092=DIRECTION('',(0.,0.,-1.));
#28093=DIRECTION('center_axis',(0.,0.,-1.));
#28094=DIRECTION('ref_axis',(1.,0.,0.));
#28095=DIRECTION('',(0.,0.,-1.));
#28096=DIRECTION('center_axis',(0.,0.,-1.));
#28097=DIRECTION('ref_axis',(1.,0.,0.));
#28098=DIRECTION('',(0.,0.,-1.));
#28099=DIRECTION('center_axis',(0.,0.,-1.));
#28100=DIRECTION('ref_axis',(1.,0.,0.));
#28101=DIRECTION('',(0.,0.,-1.));
#28102=DIRECTION('center_axis',(0.,0.,-1.));
#28103=DIRECTION('ref_axis',(1.,0.,0.));
#28104=DIRECTION('',(0.,0.,-1.));
#28105=DIRECTION('center_axis',(0.,0.,-1.));
#28106=DIRECTION('ref_axis',(1.,0.,0.));
#28107=DIRECTION('',(0.,0.,-1.));
#28108=DIRECTION('center_axis',(0.,0.,-1.));
#28109=DIRECTION('ref_axis',(0.938009462242626,-0.346609648947198,0.));
#28110=DIRECTION('',(0.,0.,-1.));
#28111=DIRECTION('center_axis',(0.,0.,-1.));
#28112=DIRECTION('ref_axis',(1.,0.,0.));
#28113=DIRECTION('center_axis',(0.,0.,-1.));
#28114=DIRECTION('ref_axis',(1.,-9.82530218636872E-14,0.));
#28115=DIRECTION('',(1.22464679914735E-16,-1.20475224710186E-29,-1.));
#28116=DIRECTION('center_axis',(0.,0.,1.));
#28117=DIRECTION('ref_axis',(1.,-9.82530218636872E-14,0.));
#28118=DIRECTION('center_axis',(0.,0.,-1.));
#28119=DIRECTION('ref_axis',(1.,-9.82530218636872E-14,0.));
#28120=DIRECTION('',(1.22464679914735E-16,-1.20475224710186E-29,-1.));
#28121=DIRECTION('center_axis',(0.,0.,-1.));
#28122=DIRECTION('ref_axis',(1.,-9.82530218636872E-14,0.));
#28123=DIRECTION('',(1.22464679914735E-16,-1.20475224710186E-29,-1.));
#28124=DIRECTION('center_axis',(0.,0.,-1.));
#28125=DIRECTION('ref_axis',(1.,-9.82530218636872E-14,0.));
#28126=DIRECTION('',(1.22464679914735E-16,-1.20475224710186E-29,-1.));
#28127=DIRECTION('center_axis',(0.,0.,-1.));
#28128=DIRECTION('ref_axis',(1.,-9.82530218636872E-14,0.));
#28129=DIRECTION('',(1.22464679914735E-16,-1.20475224710186E-29,-1.));
#28130=DIRECTION('center_axis',(0.,0.,-1.));
#28131=DIRECTION('ref_axis',(1.,-9.82530218636872E-14,0.));
#28132=DIRECTION('',(1.22464679914735E-16,-1.20475224710186E-29,-1.));
#28133=DIRECTION('center_axis',(0.,0.,-1.));
#28134=DIRECTION('ref_axis',(1.,-9.82530218636872E-14,0.));
#28135=DIRECTION('',(1.22464679914735E-16,-1.20475224710186E-29,-1.));
#28136=DIRECTION('center_axis',(0.,0.,-1.));
#28137=DIRECTION('ref_axis',(1.,-9.82530218636872E-14,0.));
#28138=DIRECTION('',(1.22464679914735E-16,-1.20475224710186E-29,-1.));
#28139=DIRECTION('center_axis',(0.,0.,-1.));
#28140=DIRECTION('ref_axis',(1.,-9.82530218636872E-14,0.));
#28141=DIRECTION('',(1.22464679914735E-16,-1.20475224710186E-29,-1.));
#28142=DIRECTION('center_axis',(0.,0.,-1.));
#28143=DIRECTION('ref_axis',(1.,-9.82530218636872E-14,0.));
#28144=DIRECTION('',(1.22464679914735E-16,-1.20475224710186E-29,-1.));
#28145=DIRECTION('center_axis',(0.,0.,-1.));
#28146=DIRECTION('ref_axis',(1.,-9.82530218636872E-14,0.));
#28147=DIRECTION('',(1.22464679914735E-16,-1.20475224710186E-29,-1.));
#28148=DIRECTION('center_axis',(0.,0.,-1.));
#28149=DIRECTION('ref_axis',(1.,-9.82530218636872E-14,0.));
#28150=DIRECTION('',(1.22464679914735E-16,-1.20475224710186E-29,-1.));
#28151=DIRECTION('center_axis',(0.,0.,-1.));
#28152=DIRECTION('ref_axis',(1.,-9.82530218636872E-14,0.));
#28153=DIRECTION('',(1.22464679914735E-16,-1.20475224710186E-29,-1.));
#28154=DIRECTION('center_axis',(0.,0.,-1.));
#28155=DIRECTION('ref_axis',(1.,-9.82530218636872E-14,0.));
#28156=DIRECTION('',(1.22464679914735E-16,-1.20475224710186E-29,-1.));
#28157=DIRECTION('center_axis',(0.,0.,-1.));
#28158=DIRECTION('ref_axis',(-0.609165547211898,-0.793043085897626,0.));
#28159=DIRECTION('',(1.22464679914735E-16,-1.20475224710186E-29,-1.));
#28160=DIRECTION('center_axis',(0.,0.,-1.));
#28161=DIRECTION('ref_axis',(1.,-9.82530218636872E-14,0.));
#28162=DIRECTION('center_axis',(0.,1.,0.));
#28163=DIRECTION('ref_axis',(0.,0.,-1.));
#28164=DIRECTION('',(0.,1.,0.));
#28165=DIRECTION('center_axis',(0.,-1.,0.));
#28166=DIRECTION('ref_axis',(0.,0.,1.));
#28167=DIRECTION('',(0.,-1.,0.));
#28168=DIRECTION('center_axis',(1.,0.,0.));
#28169=DIRECTION('ref_axis',(0.,-1.,0.));
#28170=DIRECTION('',(1.,0.,0.));
#28171=DIRECTION('center_axis',(-1.,0.,0.));
#28172=DIRECTION('ref_axis',(0.,1.,0.));
#28173=DIRECTION('',(-1.,0.,0.));
#28174=DIRECTION('center_axis',(0.,1.,0.));
#28175=DIRECTION('ref_axis',(0.,0.,-1.));
#28176=DIRECTION('',(0.,1.,0.));
#28177=DIRECTION('center_axis',(0.,-1.,0.));
#28178=DIRECTION('ref_axis',(0.,0.,1.));
#28179=DIRECTION('',(0.,-1.,0.));
#28180=DIRECTION('center_axis',(1.,0.,0.));
#28181=DIRECTION('ref_axis',(0.,-1.,0.));
#28182=DIRECTION('',(1.,0.,0.));
#28183=DIRECTION('center_axis',(-1.,0.,0.));
#28184=DIRECTION('ref_axis',(0.,1.,0.));
#28185=DIRECTION('',(-1.,0.,0.));
#28186=DIRECTION('center_axis',(0.,1.,0.));
#28187=DIRECTION('ref_axis',(0.,0.,-1.));
#28188=DIRECTION('',(0.,1.,0.));
#28189=DIRECTION('center_axis',(0.,-1.,0.));
#28190=DIRECTION('ref_axis',(0.,0.,1.));
#28191=DIRECTION('',(0.,-1.,0.));
#28192=DIRECTION('center_axis',(1.,0.,0.));
#28193=DIRECTION('ref_axis',(0.,-1.,0.));
#28194=DIRECTION('',(1.,0.,0.));
#28195=DIRECTION('center_axis',(-1.,0.,0.));
#28196=DIRECTION('ref_axis',(0.,1.,0.));
#28197=DIRECTION('',(-1.,0.,0.));
#28198=DIRECTION('center_axis',(0.,0.,1.));
#28199=DIRECTION('ref_axis',(1.,0.,0.));
#28200=DIRECTION('center_axis',(0.,0.,-1.));
#28201=DIRECTION('ref_axis',(1.,-9.82530218636872E-14,0.));
#28202=DIRECTION('center_axis',(0.,0.,-1.));
#28203=DIRECTION('ref_axis',(1.,0.,0.));
#28204=DIRECTION('center_axis',(0.,0.,1.));
#28205=DIRECTION('ref_axis',(1.,0.,0.));
#28206=DIRECTION('center_axis',(0.,0.,-1.));
#28207=DIRECTION('ref_axis',(1.,-8.66938428209003E-14,0.));
#28208=DIRECTION('center_axis',(0.,0.,-1.));
#28209=DIRECTION('ref_axis',(1.,0.,0.));
#28210=DIRECTION('center_axis',(0.,0.,1.));
#28211=DIRECTION('ref_axis',(1.,0.,0.));
#28212=DIRECTION('center_axis',(0.,0.,-1.));
#28213=DIRECTION('ref_axis',(1.,-9.39183297226423E-14,0.));
#28214=DIRECTION('center_axis',(0.,0.,-1.));
#28215=DIRECTION('ref_axis',(1.,0.,0.));
#28216=DIRECTION('center_axis',(0.,0.,1.));
#28217=DIRECTION('ref_axis',(1.,0.,0.));
#28218=DIRECTION('center_axis',(0.,0.,-1.));
#28219=DIRECTION('ref_axis',(1.,-7.51346637781136E-14,0.));
#28220=DIRECTION('center_axis',(0.,0.,-1.));
#28221=DIRECTION('ref_axis',(1.,0.,0.));
#28222=DIRECTION('center_axis',(0.,0.,1.));
#28223=DIRECTION('ref_axis',(1.,0.,0.));
#28224=DIRECTION('center_axis',(0.,0.,-1.));
#28225=DIRECTION('ref_axis',(1.,-9.39183297226423E-14,0.));
#28226=DIRECTION('center_axis',(0.,0.,-1.));
#28227=DIRECTION('ref_axis',(1.,0.,0.));
#28228=DIRECTION('center_axis',(0.,0.,1.));
#28229=DIRECTION('ref_axis',(1.,0.,0.));
#28230=DIRECTION('center_axis',(0.,0.,-1.));
#28231=DIRECTION('ref_axis',(1.,-1.09812200906474E-13,0.));
#28232=DIRECTION('center_axis',(0.,0.,-1.));
#28233=DIRECTION('ref_axis',(1.,0.,0.));
#28234=DIRECTION('center_axis',(0.,0.,1.));
#28235=DIRECTION('ref_axis',(1.,0.,0.));
#28236=DIRECTION('center_axis',(0.,0.,-1.));
#28237=DIRECTION('ref_axis',(1.,-9.10285349619456E-14,0.));
#28238=DIRECTION('center_axis',(0.,0.,-1.));
#28239=DIRECTION('ref_axis',(1.,0.,0.));
#28240=DIRECTION('center_axis',(0.,0.,1.));
#28241=DIRECTION('ref_axis',(1.,0.,0.));
#28242=DIRECTION('center_axis',(0.,0.,-1.));
#28243=DIRECTION('ref_axis',(1.,-9.39183297226423E-14,0.));
#28244=DIRECTION('center_axis',(0.,0.,-1.));
#28245=DIRECTION('ref_axis',(1.,0.,0.));
#28246=DIRECTION('center_axis',(0.,0.,-1.));
#28247=DIRECTION('ref_axis',(1.,0.,0.));
#28248=DIRECTION('center_axis',(0.,0.,-1.));
#28249=DIRECTION('ref_axis',(1.,0.,0.));
#28250=DIRECTION('center_axis',(0.,0.,-1.));
#28251=DIRECTION('ref_axis',(1.,0.,0.));
#28252=DIRECTION('center_axis',(0.,0.,-1.));
#28253=DIRECTION('ref_axis',(1.,0.,0.));
#28254=DIRECTION('center_axis',(0.,0.,-1.));
#28255=DIRECTION('ref_axis',(1.,0.,0.));
#28256=DIRECTION('center_axis',(0.,0.,-1.));
#28257=DIRECTION('ref_axis',(1.,0.,0.));
#28258=DIRECTION('center_axis',(0.,0.,-1.));
#28259=DIRECTION('ref_axis',(1.,0.,0.));
#28260=DIRECTION('center_axis',(0.,0.,-1.));
#28261=DIRECTION('ref_axis',(1.,0.,0.));
#28262=DIRECTION('center_axis',(0.,0.,-1.));
#28263=DIRECTION('ref_axis',(1.,0.,0.));
#28264=DIRECTION('center_axis',(0.,0.,-1.));
#28265=DIRECTION('ref_axis',(1.,0.,0.));
#28266=DIRECTION('',(0.,0.,-1.));
#28267=DIRECTION('center_axis',(0.,0.,1.));
#28268=DIRECTION('ref_axis',(1.,0.,0.));
#28269=DIRECTION('center_axis',(0.,0.,-1.));
#28270=DIRECTION('ref_axis',(1.,0.,0.));
#28271=DIRECTION('center_axis',(0.,0.,-1.));
#28272=DIRECTION('ref_axis',(1.,0.,0.));
#28273=DIRECTION('',(0.,0.,-1.));
#28274=DIRECTION('center_axis',(0.,0.,1.));
#28275=DIRECTION('ref_axis',(1.,0.,0.));
#28276=DIRECTION('center_axis',(0.,0.,-1.));
#28277=DIRECTION('ref_axis',(1.,0.,0.));
#28278=DIRECTION('center_axis',(0.,0.,-1.));
#28279=DIRECTION('ref_axis',(1.,0.,0.));
#28280=DIRECTION('',(0.,0.,-1.));
#28281=DIRECTION('center_axis',(0.,0.,1.));
#28282=DIRECTION('ref_axis',(1.,0.,0.));
#28283=DIRECTION('center_axis',(0.,0.,-1.));
#28284=DIRECTION('ref_axis',(1.,0.,0.));
#28285=DIRECTION('center_axis',(0.,0.,-1.));
#28286=DIRECTION('ref_axis',(1.,0.,0.));
#28287=DIRECTION('',(0.,0.,-1.));
#28288=DIRECTION('center_axis',(0.,0.,1.));
#28289=DIRECTION('ref_axis',(1.,0.,0.));
#28290=DIRECTION('center_axis',(0.,0.,-1.));
#28291=DIRECTION('ref_axis',(1.,0.,0.));
#28292=DIRECTION('center_axis',(0.,0.,-1.));
#28293=DIRECTION('ref_axis',(1.,0.,0.));
#28294=DIRECTION('',(0.,0.,-1.));
#28295=DIRECTION('center_axis',(0.,0.,-1.));
#28296=DIRECTION('ref_axis',(1.,0.,0.));
#28297=DIRECTION('center_axis',(0.,0.,-1.));
#28298=DIRECTION('ref_axis',(1.,0.,0.));
#28299=DIRECTION('center_axis',(0.,0.,1.));
#28300=DIRECTION('ref_axis',(1.,0.,0.));
#28301=DIRECTION('center_axis',(0.,0.,1.));
#28302=DIRECTION('ref_axis',(1.,0.,0.));
#28303=DIRECTION('center_axis',(0.,0.,-1.));
#28304=DIRECTION('ref_axis',(1.,0.,0.));
#28305=DIRECTION('',(0.,0.,-1.));
#28306=DIRECTION('',(0.,0.,-1.));
#28307=DIRECTION('',(0.,0.,-1.));
#28308=DIRECTION('',(0.,0.,-1.));
#28309=DIRECTION('center_axis',(0.,0.,1.));
#28310=DIRECTION('ref_axis',(1.,0.,0.));
#28311=DIRECTION('center_axis',(0.,0.,1.));
#28312=DIRECTION('ref_axis',(1.,0.,0.));
#28313=DIRECTION('center_axis',(0.,0.,1.));
#28314=DIRECTION('ref_axis',(1.,0.,0.));
#28315=DIRECTION('',(0.,0.,-1.));
#28316=DIRECTION('',(0.,0.,-1.));
#28317=DIRECTION('',(0.,0.,-1.));
#28318=DIRECTION('',(0.,0.,-1.));
#28319=DIRECTION('center_axis',(0.,0.,-1.));
#28320=DIRECTION('ref_axis',(1.,0.,0.));
#28321=DIRECTION('center_axis',(0.,0.,1.));
#28322=DIRECTION('ref_axis',(1.,0.,0.));
#28323=DIRECTION('center_axis',(0.,0.,1.));
#28324=DIRECTION('ref_axis',(1.,0.,0.));
#28325=DIRECTION('center_axis',(0.,0.,-1.));
#28326=DIRECTION('ref_axis',(1.,0.,0.));
#28327=DIRECTION('center_axis',(0.,0.,1.));
#28328=DIRECTION('ref_axis',(1.,0.,0.));
#28329=DIRECTION('',(0.,0.,-1.));
#28330=DIRECTION('center_axis',(0.,0.,-1.));
#28331=DIRECTION('ref_axis',(1.,0.,0.));
#28332=DIRECTION('center_axis',(0.,0.,1.));
#28333=DIRECTION('ref_axis',(1.,0.,0.));
#28334=DIRECTION('',(0.,0.,-1.));
#28335=DIRECTION('center_axis',(0.,0.,-1.));
#28336=DIRECTION('ref_axis',(1.,0.,0.));
#28337=DIRECTION('center_axis',(0.,0.,1.));
#28338=DIRECTION('ref_axis',(1.,0.,0.));
#28339=DIRECTION('center_axis',(0.,0.,1.));
#28340=DIRECTION('ref_axis',(1.,0.,0.));
#28341=DIRECTION('axis',(0.,0.,1.));
#28342=DIRECTION('refdir',(1.,0.,0.));
#28343=DIRECTION('center_axis',(0.,1.,0.));
#28344=DIRECTION('ref_axis',(0.,0.,-1.));
#28345=DIRECTION('',(0.,1.,0.));
#28346=DIRECTION('center_axis',(0.,1.,0.));
#28347=DIRECTION('ref_axis',(0.,0.,-1.));
#28348=DIRECTION('center_axis',(0.,1.,0.));
#28349=DIRECTION('ref_axis',(0.,0.,-1.));
#28350=DIRECTION('center_axis',(0.,-1.,0.));
#28351=DIRECTION('ref_axis',(0.,0.,1.));
#28352=DIRECTION('',(0.,-1.,0.));
#28353=DIRECTION('center_axis',(0.,-1.,0.));
#28354=DIRECTION('ref_axis',(0.,0.,1.));
#28355=DIRECTION('center_axis',(0.,-1.,0.));
#28356=DIRECTION('ref_axis',(0.,0.,1.));
#28357=DIRECTION('center_axis',(1.,0.,0.));
#28358=DIRECTION('ref_axis',(0.,-1.,0.));
#28359=DIRECTION('',(1.,0.,0.));
#28360=DIRECTION('center_axis',(1.,0.,0.));
#28361=DIRECTION('ref_axis',(0.,-1.,0.));
#28362=DIRECTION('center_axis',(1.,0.,0.));
#28363=DIRECTION('ref_axis',(0.,-1.,0.));
#28364=DIRECTION('center_axis',(-1.,0.,0.));
#28365=DIRECTION('ref_axis',(0.,1.,0.));
#28366=DIRECTION('',(-1.,0.,0.));
#28367=DIRECTION('center_axis',(-1.,0.,0.));
#28368=DIRECTION('ref_axis',(0.,1.,0.));
#28369=DIRECTION('center_axis',(-1.,0.,0.));
#28370=DIRECTION('ref_axis',(0.,1.,0.));
#28371=DIRECTION('center_axis',(0.,0.,1.));
#28372=DIRECTION('ref_axis',(1.,0.,0.));
#28373=DIRECTION('center_axis',(0.,0.,-1.));
#28374=DIRECTION('ref_axis',(1.,0.,0.));
#28375=DIRECTION('',(0.,0.,-1.));
#28376=DIRECTION('center_axis',(0.,0.,-1.));
#28377=DIRECTION('ref_axis',(1.,0.,0.));
#28378=DIRECTION('center_axis',(0.,0.,1.));
#28379=DIRECTION('ref_axis',(1.,0.,0.));
#28380=DIRECTION('center_axis',(0.,0.,1.));
#28381=DIRECTION('ref_axis',(1.,0.,0.));
#28382=DIRECTION('',(0.,0.,-1.));
#28383=DIRECTION('',(0.,0.,-1.));
#28384=DIRECTION('center_axis',(0.,0.,1.));
#28385=DIRECTION('ref_axis',(1.,0.,0.));
#28386=DIRECTION('center_axis',(0.,0.,1.));
#28387=DIRECTION('ref_axis',(1.,0.,0.));
#28388=DIRECTION('center_axis',(0.,0.,1.));
#28389=DIRECTION('ref_axis',(1.,0.,0.));
#28390=DIRECTION('axis',(0.,0.,1.));
#28391=DIRECTION('refdir',(1.,0.,0.));
#28392=DIRECTION('center_axis',(0.,0.,-1.));
#28393=DIRECTION('ref_axis',(1.,0.,0.));
#28394=DIRECTION('center_axis',(0.,0.,-1.));
#28395=DIRECTION('ref_axis',(1.,0.,0.));
#28396=DIRECTION('',(0.,0.,-1.));
#28397=DIRECTION('center_axis',(0.,0.,1.));
#28398=DIRECTION('ref_axis',(1.,0.,0.));
#28399=DIRECTION('center_axis',(0.,0.,-1.));
#28400=DIRECTION('ref_axis',(1.,0.,0.));
#28401=DIRECTION('center_axis',(0.,0.,-1.));
#28402=DIRECTION('ref_axis',(1.,0.,0.));
#28403=DIRECTION('',(0.,0.,-1.));
#28404=DIRECTION('center_axis',(0.,0.,1.));
#28405=DIRECTION('ref_axis',(1.,0.,0.));
#28406=DIRECTION('center_axis',(0.,0.,-1.));
#28407=DIRECTION('ref_axis',(1.,0.,0.));
#28408=DIRECTION('center_axis',(0.,0.,-1.));
#28409=DIRECTION('ref_axis',(1.,0.,0.));
#28410=DIRECTION('',(0.,0.,-1.));
#28411=DIRECTION('center_axis',(0.,0.,1.));
#28412=DIRECTION('ref_axis',(1.,0.,0.));
#28413=DIRECTION('center_axis',(0.,0.,-1.));
#28414=DIRECTION('ref_axis',(1.,0.,0.));
#28415=DIRECTION('center_axis',(0.,0.,-1.));
#28416=DIRECTION('ref_axis',(1.,0.,0.));
#28417=DIRECTION('',(0.,0.,-1.));
#28418=DIRECTION('center_axis',(0.,0.,1.));
#28419=DIRECTION('ref_axis',(1.,0.,0.));
#28420=DIRECTION('center_axis',(0.,0.,-1.));
#28421=DIRECTION('ref_axis',(1.,0.,0.));
#28422=DIRECTION('center_axis',(0.,0.,-1.));
#28423=DIRECTION('ref_axis',(1.,0.,0.));
#28424=DIRECTION('',(0.,0.,-1.));
#28425=DIRECTION('center_axis',(0.,0.,1.));
#28426=DIRECTION('ref_axis',(1.,0.,0.));
#28427=DIRECTION('center_axis',(0.,0.,-1.));
#28428=DIRECTION('ref_axis',(1.,0.,0.));
#28429=DIRECTION('center_axis',(0.,0.,-1.));
#28430=DIRECTION('ref_axis',(1.,0.,0.));
#28431=DIRECTION('',(0.,0.,-1.));
#28432=DIRECTION('center_axis',(0.,0.,1.));
#28433=DIRECTION('ref_axis',(1.,0.,0.));
#28434=DIRECTION('center_axis',(0.,0.,-1.));
#28435=DIRECTION('ref_axis',(1.,0.,0.));
#28436=DIRECTION('center_axis',(0.,0.,-1.));
#28437=DIRECTION('ref_axis',(1.,0.,0.));
#28438=DIRECTION('',(0.,0.,-1.));
#28439=DIRECTION('center_axis',(0.,0.,1.));
#28440=DIRECTION('ref_axis',(1.,0.,0.));
#28441=DIRECTION('center_axis',(0.,0.,-1.));
#28442=DIRECTION('ref_axis',(1.,0.,0.));
#28443=DIRECTION('center_axis',(0.,0.,-1.));
#28444=DIRECTION('ref_axis',(1.,0.,0.));
#28445=DIRECTION('',(0.,0.,-1.));
#28446=DIRECTION('center_axis',(0.,0.,1.));
#28447=DIRECTION('ref_axis',(1.,0.,0.));
#28448=DIRECTION('center_axis',(0.,0.,1.));
#28449=DIRECTION('ref_axis',(1.,0.,0.));
#28450=DIRECTION('center_axis',(0.,0.,-1.));
#28451=DIRECTION('ref_axis',(1.,0.,0.));
#28452=DIRECTION('',(0.,0.,-1.));
#28453=DIRECTION('center_axis',(0.,0.,-1.));
#28454=DIRECTION('ref_axis',(1.,0.,0.));
#28455=DIRECTION('center_axis',(0.,0.,1.));
#28456=DIRECTION('ref_axis',(1.,0.,0.));
#28457=DIRECTION('center_axis',(0.,0.,1.));
#28458=DIRECTION('ref_axis',(1.,0.,0.));
#28459=DIRECTION('',(0.,0.,-1.));
#28460=DIRECTION('center_axis',(0.,0.,1.));
#28461=DIRECTION('ref_axis',(1.,0.,0.));
#28462=DIRECTION('center_axis',(0.,0.,1.));
#28463=DIRECTION('ref_axis',(1.,0.,0.));
#28464=DIRECTION('center_axis',(0.,0.,1.));
#28465=DIRECTION('ref_axis',(1.,0.,0.));
#28466=DIRECTION('axis',(0.,0.,1.));
#28467=DIRECTION('refdir',(1.,0.,0.));
#28468=DIRECTION('center_axis',(0.,-1.,0.));
#28469=DIRECTION('ref_axis',(-1.,0.,0.));
#28470=DIRECTION('',(0.,0.,1.));
#28471=DIRECTION('',(-1.,0.,0.));
#28472=DIRECTION('',(0.,0.,-1.));
#28473=DIRECTION('',(1.,0.,0.));
#28474=DIRECTION('center_axis',(0.,0.,1.));
#28475=DIRECTION('ref_axis',(1.,0.,0.));
#28476=DIRECTION('center_axis',(0.,0.,1.));
#28477=DIRECTION('ref_axis',(1.,0.,0.));
#28478=DIRECTION('',(0.,-1.,0.));
#28479=DIRECTION('',(-1.,0.,0.));
#28480=DIRECTION('center_axis',(0.,1.,0.));
#28481=DIRECTION('ref_axis',(1.,0.,0.));
#28482=DIRECTION('',(0.,0.,-1.));
#28483=DIRECTION('',(0.,0.,-1.));
#28484=DIRECTION('',(1.,0.,0.));
#28485=DIRECTION('center_axis',(-1.,0.,0.));
#28486=DIRECTION('ref_axis',(0.,1.,0.));
#28487=DIRECTION('',(0.,1.,0.));
#28488=DIRECTION('center_axis',(0.,0.,-1.));
#28489=DIRECTION('ref_axis',(-1.,0.,0.));
#28490=DIRECTION('center_axis',(0.,0.,-1.));
#28491=DIRECTION('ref_axis',(1.,0.,0.));
#28492=DIRECTION('center_axis',(0.,0.,1.));
#28493=DIRECTION('ref_axis',(1.,0.,0.));
#28494=DIRECTION('center_axis',(0.,0.,1.));
#28495=DIRECTION('ref_axis',(1.,0.,0.));
#28496=DIRECTION('',(0.,0.,1.));
#28497=DIRECTION('center_axis',(0.,0.,1.));
#28498=DIRECTION('ref_axis',(1.,0.,0.));
#28499=DIRECTION('center_axis',(0.,0.,-1.));
#28500=DIRECTION('ref_axis',(-1.,0.,0.));
#28501=DIRECTION('center_axis',(0.,0.,-1.));
#28502=DIRECTION('ref_axis',(1.,0.,0.));
#28503=DIRECTION('center_axis',(0.,0.,1.));
#28504=DIRECTION('ref_axis',(1.,0.,0.));
#28505=DIRECTION('center_axis',(0.,0.,1.));
#28506=DIRECTION('ref_axis',(1.,0.,0.));
#28507=DIRECTION('center_axis',(0.,0.,1.));
#28508=DIRECTION('ref_axis',(1.,0.,0.));
#28509=DIRECTION('center_axis',(0.,0.,1.));
#28510=DIRECTION('ref_axis',(1.,0.,0.));
#28511=DIRECTION('',(0.,0.,-1.));
#28512=DIRECTION('center_axis',(0.,0.,1.));
#28513=DIRECTION('ref_axis',(1.,0.,0.));
#28514=DIRECTION('center_axis',(0.,0.,1.));
#28515=DIRECTION('ref_axis',(1.,0.,0.));
#28516=DIRECTION('',(0.,0.,1.));
#28517=DIRECTION('center_axis',(0.,0.,1.));
#28518=DIRECTION('ref_axis',(1.,0.,0.));
#28519=DIRECTION('center_axis',(0.,0.,-1.));
#28520=DIRECTION('ref_axis',(-1.,0.,0.));
#28521=DIRECTION('center_axis',(0.,0.,-1.));
#28522=DIRECTION('ref_axis',(1.,0.,0.));
#28523=DIRECTION('center_axis',(0.,0.,1.));
#28524=DIRECTION('ref_axis',(1.,0.,0.));
#28525=DIRECTION('center_axis',(0.,0.,1.));
#28526=DIRECTION('ref_axis',(1.,0.,0.));
#28527=DIRECTION('center_axis',(0.,0.,1.));
#28528=DIRECTION('ref_axis',(1.,0.,0.));
#28529=DIRECTION('center_axis',(0.,0.,-1.));
#28530=DIRECTION('ref_axis',(1.,0.,0.));
#28531=DIRECTION('',(0.,0.,-1.));
#28532=DIRECTION('center_axis',(0.,0.,1.));
#28533=DIRECTION('ref_axis',(1.,0.,0.));
#28534=DIRECTION('center_axis',(0.,0.,1.));
#28535=DIRECTION('ref_axis',(1.,0.,0.));
#28536=DIRECTION('center_axis',(0.,0.,1.));
#28537=DIRECTION('ref_axis',(1.,0.,0.));
#28538=DIRECTION('center_axis',(0.,0.,1.));
#28539=DIRECTION('ref_axis',(1.,0.,0.));
#28540=DIRECTION('center_axis',(0.,0.,1.));
#28541=DIRECTION('ref_axis',(1.,0.,0.));
#28542=DIRECTION('center_axis',(0.,0.,-1.));
#28543=DIRECTION('ref_axis',(1.,0.,0.));
#28544=DIRECTION('center_axis',(0.,0.,1.));
#28545=DIRECTION('ref_axis',(1.,0.,0.));
#28546=DIRECTION('',(0.,0.,-1.));
#28547=DIRECTION('center_axis',(0.,0.,1.));
#28548=DIRECTION('ref_axis',(1.,0.,0.));
#28549=DIRECTION('',(0.,0.,-1.));
#28550=DIRECTION('center_axis',(0.,0.,-1.));
#28551=DIRECTION('ref_axis',(1.,0.,0.));
#28552=DIRECTION('center_axis',(0.,0.,1.));
#28553=DIRECTION('ref_axis',(1.,0.,0.));
#28554=DIRECTION('center_axis',(0.,0.,1.));
#28555=DIRECTION('ref_axis',(1.,0.,0.));
#28556=DIRECTION('center_axis',(0.,0.,1.));
#28557=DIRECTION('ref_axis',(1.,0.,0.));
#28558=DIRECTION('center_axis',(0.,0.,1.));
#28559=DIRECTION('ref_axis',(1.,0.,0.));
#28560=DIRECTION('center_axis',(0.,0.,1.));
#28561=DIRECTION('ref_axis',(1.,0.,0.));
#28562=DIRECTION('center_axis',(0.,0.,1.));
#28563=DIRECTION('ref_axis',(1.,0.,0.));
#28564=DIRECTION('',(0.,0.,-1.));
#28565=DIRECTION('center_axis',(0.,0.,1.));
#28566=DIRECTION('ref_axis',(1.,0.,0.));
#28567=DIRECTION('',(0.,0.,-1.));
#28568=DIRECTION('center_axis',(0.,0.,1.));
#28569=DIRECTION('ref_axis',(1.,0.,0.));
#28570=DIRECTION('center_axis',(0.,0.,1.));
#28571=DIRECTION('ref_axis',(1.,0.,0.));
#28572=DIRECTION('',(0.,0.,-1.));
#28573=DIRECTION('center_axis',(0.,0.,1.));
#28574=DIRECTION('ref_axis',(1.,0.,0.));
#28575=DIRECTION('center_axis',(0.,0.,1.));
#28576=DIRECTION('ref_axis',(1.,0.,0.));
#28577=DIRECTION('center_axis',(0.,0.,1.));
#28578=DIRECTION('ref_axis',(1.,0.,0.));
#28579=DIRECTION('',(0.,0.,-1.));
#28580=DIRECTION('center_axis',(0.,0.,1.));
#28581=DIRECTION('ref_axis',(1.,0.,0.));
#28582=DIRECTION('center_axis',(0.,0.,1.));
#28583=DIRECTION('ref_axis',(1.,0.,0.));
#28584=DIRECTION('center_axis',(0.,0.,1.));
#28585=DIRECTION('ref_axis',(1.,0.,0.));
#28586=DIRECTION('center_axis',(0.,0.,1.));
#28587=DIRECTION('ref_axis',(1.,0.,0.));
#28588=DIRECTION('',(0.,0.,-1.));
#28589=DIRECTION('center_axis',(0.,0.,1.));
#28590=DIRECTION('ref_axis',(1.,0.,0.));
#28591=DIRECTION('center_axis',(0.,0.,1.));
#28592=DIRECTION('ref_axis',(1.,0.,0.));
#28593=DIRECTION('axis',(0.,0.,1.));
#28594=DIRECTION('refdir',(1.,0.,0.));
#28595=DIRECTION('center_axis',(0.,1.,0.));
#28596=DIRECTION('ref_axis',(0.,0.,-1.));
#28597=DIRECTION('',(0.,1.,0.));
#28598=DIRECTION('center_axis',(0.,1.,0.));
#28599=DIRECTION('ref_axis',(0.,0.,-1.));
#28600=DIRECTION('center_axis',(0.,1.,0.));
#28601=DIRECTION('ref_axis',(0.,0.,-1.));
#28602=DIRECTION('center_axis',(0.,-1.,0.));
#28603=DIRECTION('ref_axis',(0.,0.,1.));
#28604=DIRECTION('',(0.,-1.,0.));
#28605=DIRECTION('center_axis',(0.,-1.,0.));
#28606=DIRECTION('ref_axis',(0.,0.,1.));
#28607=DIRECTION('center_axis',(0.,-1.,0.));
#28608=DIRECTION('ref_axis',(0.,0.,1.));
#28609=DIRECTION('center_axis',(1.,0.,0.));
#28610=DIRECTION('ref_axis',(0.,-1.,0.));
#28611=DIRECTION('',(1.,0.,0.));
#28612=DIRECTION('center_axis',(1.,0.,0.));
#28613=DIRECTION('ref_axis',(0.,-1.,0.));
#28614=DIRECTION('center_axis',(1.,0.,0.));
#28615=DIRECTION('ref_axis',(0.,-1.,0.));
#28616=DIRECTION('center_axis',(-1.,0.,0.));
#28617=DIRECTION('ref_axis',(0.,1.,0.));
#28618=DIRECTION('',(-1.,0.,0.));
#28619=DIRECTION('center_axis',(-1.,0.,0.));
#28620=DIRECTION('ref_axis',(0.,1.,0.));
#28621=DIRECTION('center_axis',(-1.,0.,0.));
#28622=DIRECTION('ref_axis',(0.,1.,0.));
#28623=DIRECTION('',(0.,0.,-1.));
#28624=DIRECTION('center_axis',(0.,0.,1.));
#28625=DIRECTION('ref_axis',(0.998647288695349,-0.0519960842893784,0.));
#28626=DIRECTION('center_axis',(0.,0.,-1.));
#28627=DIRECTION('ref_axis',(0.998647288695349,-0.0519960842893784,0.));
#28628=DIRECTION('center_axis',(0.,0.,1.));
#28629=DIRECTION('ref_axis',(0.998647288695349,-0.0519960842893784,0.));
#28630=DIRECTION('',(0.,0.,-1.));
#28631=DIRECTION('center_axis',(0.,0.,1.));
#28632=DIRECTION('ref_axis',(0.990315376915793,-0.138836069679788,0.));
#28633=DIRECTION('center_axis',(0.,0.,-1.));
#28634=DIRECTION('ref_axis',(0.990315376915793,-0.138836069679788,0.));
#28635=DIRECTION('center_axis',(0.,0.,1.));
#28636=DIRECTION('ref_axis',(0.990315376915793,-0.138836069679788,0.));
#28637=DIRECTION('',(0.,0.,-1.));
#28638=DIRECTION('center_axis',(0.,0.,1.));
#28639=DIRECTION('ref_axis',(0.974446567149134,-0.224619428748424,0.));
#28640=DIRECTION('center_axis',(0.,0.,-1.));
#28641=DIRECTION('ref_axis',(0.974446567149134,-0.224619428748424,0.));
#28642=DIRECTION('center_axis',(0.,0.,1.));
#28643=DIRECTION('ref_axis',(0.974446567149134,-0.224619428748424,0.));
#28644=DIRECTION('',(0.,0.,-1.));
#28645=DIRECTION('center_axis',(0.,0.,1.));
#28646=DIRECTION('ref_axis',(0.951161630619545,-0.308693298335366,0.));
#28647=DIRECTION('center_axis',(0.,0.,-1.));
#28648=DIRECTION('ref_axis',(0.951161630619545,-0.308693298335366,0.));
#28649=DIRECTION('center_axis',(0.,0.,1.));
#28650=DIRECTION('ref_axis',(0.951161630619545,-0.308693298335366,0.));
#28651=DIRECTION('',(0.,0.,-1.));
#28652=DIRECTION('center_axis',(0.,0.,1.));
#28653=DIRECTION('ref_axis',(0.920637779753847,-0.390417825527865,0.));
#28654=DIRECTION('center_axis',(0.,0.,-1.));
#28655=DIRECTION('ref_axis',(0.920637779753847,-0.390417825527865,0.));
#28656=DIRECTION('center_axis',(0.,0.,1.));
#28657=DIRECTION('ref_axis',(0.920637779753847,-0.390417825527865,0.));
#28658=DIRECTION('',(0.,0.,-1.));
#28659=DIRECTION('center_axis',(0.,0.,1.));
#28660=DIRECTION('ref_axis',(0.883107319487932,-0.469171037327369,0.));
#28661=DIRECTION('center_axis',(0.,0.,-1.));
#28662=DIRECTION('ref_axis',(0.883107319487932,-0.469171037327369,0.));
#28663=DIRECTION('center_axis',(0.,0.,1.));
#28664=DIRECTION('ref_axis',(0.883107319487932,-0.469171037327369,0.));
#28665=DIRECTION('',(0.,0.,-1.));
#28666=DIRECTION('center_axis',(0.,0.,1.));
#28667=DIRECTION('ref_axis',(0.838855879285935,-0.544353574239594,0.));
#28668=DIRECTION('center_axis',(0.,0.,-1.));
#28669=DIRECTION('ref_axis',(0.838855879285935,-0.544353574239594,0.));
#28670=DIRECTION('center_axis',(0.,0.,1.));
#28671=DIRECTION('ref_axis',(0.838855879285935,-0.544353574239594,0.));
#28672=DIRECTION('',(0.,0.,-1.));
#28673=DIRECTION('center_axis',(0.,0.,1.));
#28674=DIRECTION('ref_axis',(0.788220239327544,-0.61539325176218,0.));
#28675=DIRECTION('center_axis',(0.,0.,-1.));
#28676=DIRECTION('ref_axis',(0.788220239327544,-0.61539325176218,0.));
#28677=DIRECTION('center_axis',(0.,0.,1.));
#28678=DIRECTION('ref_axis',(0.788220239327544,-0.61539325176218,0.));
#28679=DIRECTION('',(0.,0.,-1.));
#28680=DIRECTION('center_axis',(0.,0.,1.));
#28681=DIRECTION('ref_axis',(0.731585767407476,-0.681749415054251,0.));
#28682=DIRECTION('center_axis',(0.,0.,-1.));
#28683=DIRECTION('ref_axis',(0.731585767407476,-0.681749415054251,0.));
#28684=DIRECTION('center_axis',(0.,0.,1.));
#28685=DIRECTION('ref_axis',(0.731585767407476,-0.681749415054251,0.));
#28686=DIRECTION('',(0.,0.,-1.));
#28687=DIRECTION('center_axis',(0.,0.,1.));
#28688=DIRECTION('ref_axis',(0.669383486053874,-0.742917053646208,0.));
#28689=DIRECTION('center_axis',(0.,0.,-1.));
#28690=DIRECTION('ref_axis',(0.669383486053874,-0.742917053646208,0.));
#28691=DIRECTION('center_axis',(0.,0.,1.));
#28692=DIRECTION('ref_axis',(0.669383486053874,-0.742917053646208,0.));
#28693=DIRECTION('',(0.,0.,-1.));
#28694=DIRECTION('center_axis',(0.,0.,1.));
#28695=DIRECTION('ref_axis',(0.602086792186603,-0.798430644874335,0.));
#28696=DIRECTION('center_axis',(0.,0.,-1.));
#28697=DIRECTION('ref_axis',(0.602086792186603,-0.798430644874335,0.));
#28698=DIRECTION('center_axis',(0.,0.,1.));
#28699=DIRECTION('ref_axis',(0.602086792186603,-0.798430644874335,0.));
#28700=DIRECTION('',(0.,0.,-1.));
#28701=DIRECTION('center_axis',(0.,0.,1.));
#28702=DIRECTION('ref_axis',(0.530207854280846,-0.847867696789364,0.));
#28703=DIRECTION('center_axis',(0.,0.,-1.));
#28704=DIRECTION('ref_axis',(0.530207854280846,-0.847867696789364,0.));
#28705=DIRECTION('center_axis',(0.,0.,1.));
#28706=DIRECTION('ref_axis',(0.530207854280846,-0.847867696789364,0.));
#28707=DIRECTION('',(0.,0.,-1.));
#28708=DIRECTION('center_axis',(0.,0.,1.));
#28709=DIRECTION('ref_axis',(0.454293714455755,-0.890851963575314,0.));
#28710=DIRECTION('center_axis',(0.,0.,-1.));
#28711=DIRECTION('ref_axis',(0.454293714455755,-0.890851963575314,0.));
#28712=DIRECTION('center_axis',(0.,0.,1.));
#28713=DIRECTION('ref_axis',(0.454293714455755,-0.890851963575314,0.));
#28714=DIRECTION('',(0.,0.,-1.));
#28715=DIRECTION('center_axis',(0.,0.,1.));
#28716=DIRECTION('ref_axis',(0.374922125153613,-0.927056309007332,0.));
#28717=DIRECTION('center_axis',(0.,0.,-1.));
#28718=DIRECTION('ref_axis',(0.374922125153613,-0.927056309007332,0.));
#28719=DIRECTION('center_axis',(0.,0.,1.));
#28720=DIRECTION('ref_axis',(0.374922125153613,-0.927056309007332,0.));
#28721=DIRECTION('',(0.,0.,-1.));
#28722=DIRECTION('center_axis',(0.,0.,1.));
#28723=DIRECTION('ref_axis',(0.292697152094883,-0.956205196155901,0.));
#28724=DIRECTION('center_axis',(0.,0.,-1.));
#28725=DIRECTION('ref_axis',(0.292697152094883,-0.956205196155901,0.));
#28726=DIRECTION('center_axis',(0.,0.,1.));
#28727=DIRECTION('ref_axis',(0.292697152094883,-0.956205196155901,0.));
#28728=DIRECTION('',(0.,0.,-1.));
#28729=DIRECTION('center_axis',(0.,0.,1.));
#28730=DIRECTION('ref_axis',(0.208244576973338,-0.97807678438924,0.));
#28731=DIRECTION('center_axis',(0.,0.,-1.));
#28732=DIRECTION('ref_axis',(0.208244576973338,-0.97807678438924,0.));
#28733=DIRECTION('center_axis',(0.,0.,1.));
#28734=DIRECTION('ref_axis',(0.208244576973338,-0.97807678438924,0.));
#28735=DIRECTION('',(0.,0.,-1.));
#28736=DIRECTION('center_axis',(0.,0.,1.));
#28737=DIRECTION('ref_axis',(0.122207134879512,-0.992504617714467,0.));
#28738=DIRECTION('center_axis',(0.,0.,-1.));
#28739=DIRECTION('ref_axis',(0.122207134879512,-0.992504617714467,0.));
#28740=DIRECTION('center_axis',(0.,0.,1.));
#28741=DIRECTION('ref_axis',(0.122207134879512,-0.992504617714467,0.));
#28742=DIRECTION('',(0.,0.,-1.));
#28743=DIRECTION('center_axis',(0.,0.,1.));
#28744=DIRECTION('ref_axis',(0.0352396226985678,-0.999378891608214,0.));
#28745=DIRECTION('center_axis',(0.,0.,-1.));
#28746=DIRECTION('ref_axis',(0.0352396226985678,-0.999378891608214,0.));
#28747=DIRECTION('center_axis',(0.,0.,1.));
#28748=DIRECTION('ref_axis',(0.0352396226985678,-0.999378891608214,0.));
#28749=DIRECTION('',(0.,0.,-1.));
#28750=DIRECTION('center_axis',(0.,0.,1.));
#28751=DIRECTION('ref_axis',(-0.0519960842893783,-0.998647288695349,0.));
#28752=DIRECTION('center_axis',(0.,0.,-1.));
#28753=DIRECTION('ref_axis',(-0.0519960842893783,-0.998647288695349,0.));
#28754=DIRECTION('center_axis',(0.,0.,1.));
#28755=DIRECTION('ref_axis',(-0.0519960842893783,-0.998647288695349,0.));
#28756=DIRECTION('',(0.,0.,-1.));
#28757=DIRECTION('center_axis',(0.,0.,1.));
#28758=DIRECTION('ref_axis',(-0.138836069679788,-0.990315376915793,0.));
#28759=DIRECTION('center_axis',(0.,0.,-1.));
#28760=DIRECTION('ref_axis',(-0.138836069679788,-0.990315376915793,0.));
#28761=DIRECTION('center_axis',(0.,0.,1.));
#28762=DIRECTION('ref_axis',(-0.138836069679788,-0.990315376915793,0.));
#28763=DIRECTION('',(0.,0.,-1.));
#28764=DIRECTION('center_axis',(0.,0.,1.));
#28765=DIRECTION('ref_axis',(-0.224619428748424,-0.974446567149134,0.));
#28766=DIRECTION('center_axis',(0.,0.,-1.));
#28767=DIRECTION('ref_axis',(-0.224619428748424,-0.974446567149134,0.));
#28768=DIRECTION('center_axis',(0.,0.,1.));
#28769=DIRECTION('ref_axis',(-0.224619428748424,-0.974446567149134,0.));
#28770=DIRECTION('',(0.,0.,-1.));
#28771=DIRECTION('center_axis',(0.,0.,1.));
#28772=DIRECTION('ref_axis',(-0.308693298335366,-0.951161630619545,0.));
#28773=DIRECTION('center_axis',(0.,0.,-1.));
#28774=DIRECTION('ref_axis',(-0.308693298335366,-0.951161630619545,0.));
#28775=DIRECTION('center_axis',(0.,0.,1.));
#28776=DIRECTION('ref_axis',(-0.308693298335366,-0.951161630619545,0.));
#28777=DIRECTION('',(0.,0.,-1.));
#28778=DIRECTION('center_axis',(0.,0.,1.));
#28779=DIRECTION('ref_axis',(-0.390417825527865,-0.920637779753847,0.));
#28780=DIRECTION('center_axis',(0.,0.,-1.));
#28781=DIRECTION('ref_axis',(-0.390417825527865,-0.920637779753847,0.));
#28782=DIRECTION('center_axis',(0.,0.,1.));
#28783=DIRECTION('ref_axis',(-0.390417825527865,-0.920637779753847,0.));
#28784=DIRECTION('',(0.,0.,-1.));
#28785=DIRECTION('center_axis',(0.,0.,1.));
#28786=DIRECTION('ref_axis',(-0.469171037327369,-0.883107319487932,0.));
#28787=DIRECTION('center_axis',(0.,0.,-1.));
#28788=DIRECTION('ref_axis',(-0.469171037327369,-0.883107319487932,0.));
#28789=DIRECTION('center_axis',(0.,0.,1.));
#28790=DIRECTION('ref_axis',(-0.469171037327369,-0.883107319487932,0.));
#28791=DIRECTION('',(0.,0.,-1.));
#28792=DIRECTION('center_axis',(0.,0.,1.));
#28793=DIRECTION('ref_axis',(-0.544353574239594,-0.838855879285935,0.));
#28794=DIRECTION('center_axis',(0.,0.,-1.));
#28795=DIRECTION('ref_axis',(-0.544353574239594,-0.838855879285935,0.));
#28796=DIRECTION('center_axis',(0.,0.,1.));
#28797=DIRECTION('ref_axis',(-0.544353574239594,-0.838855879285935,0.));
#28798=DIRECTION('',(0.,0.,-1.));
#28799=DIRECTION('center_axis',(0.,0.,1.));
#28800=DIRECTION('ref_axis',(-0.61539325176218,-0.788220239327544,0.));
#28801=DIRECTION('center_axis',(0.,0.,-1.));
#28802=DIRECTION('ref_axis',(-0.61539325176218,-0.788220239327544,0.));
#28803=DIRECTION('center_axis',(0.,0.,1.));
#28804=DIRECTION('ref_axis',(-0.61539325176218,-0.788220239327544,0.));
#28805=DIRECTION('',(0.,0.,-1.));
#28806=DIRECTION('center_axis',(0.,0.,1.));
#28807=DIRECTION('ref_axis',(-0.681749415054251,-0.731585767407477,0.));
#28808=DIRECTION('center_axis',(0.,0.,-1.));
#28809=DIRECTION('ref_axis',(-0.681749415054251,-0.731585767407477,0.));
#28810=DIRECTION('center_axis',(0.,0.,1.));
#28811=DIRECTION('ref_axis',(-0.681749415054251,-0.731585767407477,0.));
#28812=DIRECTION('',(0.,0.,-1.));
#28813=DIRECTION('center_axis',(0.,0.,1.));
#28814=DIRECTION('ref_axis',(-0.742917053646208,-0.669383486053874,0.));
#28815=DIRECTION('center_axis',(0.,0.,-1.));
#28816=DIRECTION('ref_axis',(-0.742917053646208,-0.669383486053874,0.));
#28817=DIRECTION('center_axis',(0.,0.,1.));
#28818=DIRECTION('ref_axis',(-0.742917053646208,-0.669383486053874,0.));
#28819=DIRECTION('',(0.,0.,-1.));
#28820=DIRECTION('center_axis',(0.,0.,1.));
#28821=DIRECTION('ref_axis',(-0.798430644874335,-0.602086792186602,0.));
#28822=DIRECTION('center_axis',(0.,0.,-1.));
#28823=DIRECTION('ref_axis',(-0.798430644874335,-0.602086792186602,0.));
#28824=DIRECTION('center_axis',(0.,0.,1.));
#28825=DIRECTION('ref_axis',(-0.798430644874335,-0.602086792186602,0.));
#28826=DIRECTION('',(0.,0.,-1.));
#28827=DIRECTION('center_axis',(0.,0.,1.));
#28828=DIRECTION('ref_axis',(-0.847867696789364,-0.530207854280845,0.));
#28829=DIRECTION('center_axis',(0.,0.,-1.));
#28830=DIRECTION('ref_axis',(-0.847867696789364,-0.530207854280845,0.));
#28831=DIRECTION('center_axis',(0.,0.,1.));
#28832=DIRECTION('ref_axis',(-0.847867696789364,-0.530207854280845,0.));
#28833=DIRECTION('',(0.,0.,-1.));
#28834=DIRECTION('center_axis',(0.,0.,1.));
#28835=DIRECTION('ref_axis',(-0.890851963575314,-0.454293714455756,0.));
#28836=DIRECTION('center_axis',(0.,0.,-1.));
#28837=DIRECTION('ref_axis',(-0.890851963575314,-0.454293714455756,0.));
#28838=DIRECTION('center_axis',(0.,0.,1.));
#28839=DIRECTION('ref_axis',(-0.890851963575314,-0.454293714455756,0.));
#28840=DIRECTION('',(0.,0.,-1.));
#28841=DIRECTION('center_axis',(0.,0.,1.));
#28842=DIRECTION('ref_axis',(-0.927056309007332,-0.374922125153613,0.));
#28843=DIRECTION('center_axis',(0.,0.,-1.));
#28844=DIRECTION('ref_axis',(-0.927056309007332,-0.374922125153613,0.));
#28845=DIRECTION('center_axis',(0.,0.,1.));
#28846=DIRECTION('ref_axis',(-0.927056309007332,-0.374922125153613,0.));
#28847=DIRECTION('',(0.,0.,-1.));
#28848=DIRECTION('center_axis',(0.,0.,1.));
#28849=DIRECTION('ref_axis',(-0.956205196155901,-0.292697152094883,0.));
#28850=DIRECTION('center_axis',(0.,0.,-1.));
#28851=DIRECTION('ref_axis',(-0.956205196155901,-0.292697152094883,0.));
#28852=DIRECTION('center_axis',(0.,0.,1.));
#28853=DIRECTION('ref_axis',(-0.956205196155901,-0.292697152094883,0.));
#28854=DIRECTION('',(0.,0.,-1.));
#28855=DIRECTION('center_axis',(0.,0.,1.));
#28856=DIRECTION('ref_axis',(-0.97807678438924,-0.208244576973338,0.));
#28857=DIRECTION('center_axis',(0.,0.,-1.));
#28858=DIRECTION('ref_axis',(-0.97807678438924,-0.208244576973338,0.));
#28859=DIRECTION('center_axis',(0.,0.,1.));
#28860=DIRECTION('ref_axis',(-0.97807678438924,-0.208244576973338,0.));
#28861=DIRECTION('',(0.,0.,-1.));
#28862=DIRECTION('center_axis',(0.,0.,1.));
#28863=DIRECTION('ref_axis',(-0.992504617714467,-0.122207134879512,0.));
#28864=DIRECTION('center_axis',(0.,0.,-1.));
#28865=DIRECTION('ref_axis',(-0.992504617714467,-0.122207134879512,0.));
#28866=DIRECTION('center_axis',(0.,0.,1.));
#28867=DIRECTION('ref_axis',(-0.992504617714467,-0.122207134879512,0.));
#28868=DIRECTION('',(0.,0.,-1.));
#28869=DIRECTION('center_axis',(0.,0.,1.));
#28870=DIRECTION('ref_axis',(-0.999378891608214,-0.0352396226985679,0.));
#28871=DIRECTION('center_axis',(0.,0.,-1.));
#28872=DIRECTION('ref_axis',(-0.999378891608214,-0.0352396226985679,0.));
#28873=DIRECTION('center_axis',(0.,0.,1.));
#28874=DIRECTION('ref_axis',(-0.999378891608214,-0.0352396226985679,0.));
#28875=DIRECTION('',(0.,0.,-1.));
#28876=DIRECTION('center_axis',(0.,0.,1.));
#28877=DIRECTION('ref_axis',(-0.998647288695349,0.0519960842893783,0.));
#28878=DIRECTION('center_axis',(0.,0.,-1.));
#28879=DIRECTION('ref_axis',(-0.998647288695349,0.0519960842893783,0.));
#28880=DIRECTION('center_axis',(0.,0.,1.));
#28881=DIRECTION('ref_axis',(-0.998647288695349,0.0519960842893783,0.));
#28882=DIRECTION('',(0.,0.,-1.));
#28883=DIRECTION('center_axis',(0.,0.,1.));
#28884=DIRECTION('ref_axis',(-0.990315376915793,0.138836069679789,0.));
#28885=DIRECTION('center_axis',(0.,0.,-1.));
#28886=DIRECTION('ref_axis',(-0.990315376915793,0.138836069679789,0.));
#28887=DIRECTION('center_axis',(0.,0.,1.));
#28888=DIRECTION('ref_axis',(-0.990315376915793,0.138836069679789,0.));
#28889=DIRECTION('',(0.,0.,-1.));
#28890=DIRECTION('center_axis',(0.,0.,1.));
#28891=DIRECTION('ref_axis',(-0.974446567149134,0.224619428748424,0.));
#28892=DIRECTION('center_axis',(0.,0.,-1.));
#28893=DIRECTION('ref_axis',(-0.974446567149134,0.224619428748424,0.));
#28894=DIRECTION('center_axis',(0.,0.,1.));
#28895=DIRECTION('ref_axis',(-0.974446567149134,0.224619428748424,0.));
#28896=DIRECTION('',(0.,0.,-1.));
#28897=DIRECTION('center_axis',(0.,0.,1.));
#28898=DIRECTION('ref_axis',(-0.951161630619546,0.308693298335365,0.));
#28899=DIRECTION('center_axis',(0.,0.,-1.));
#28900=DIRECTION('ref_axis',(-0.951161630619546,0.308693298335365,0.));
#28901=DIRECTION('center_axis',(0.,0.,1.));
#28902=DIRECTION('ref_axis',(-0.951161630619546,0.308693298335365,0.));
#28903=DIRECTION('',(0.,0.,-1.));
#28904=DIRECTION('center_axis',(0.,0.,1.));
#28905=DIRECTION('ref_axis',(-0.920637779753848,0.390417825527865,0.));
#28906=DIRECTION('center_axis',(0.,0.,-1.));
#28907=DIRECTION('ref_axis',(-0.920637779753848,0.390417825527865,0.));
#28908=DIRECTION('center_axis',(0.,0.,1.));
#28909=DIRECTION('ref_axis',(-0.920637779753848,0.390417825527865,0.));
#28910=DIRECTION('',(0.,0.,-1.));
#28911=DIRECTION('center_axis',(0.,0.,1.));
#28912=DIRECTION('ref_axis',(-0.883107319487933,0.469171037327368,0.));
#28913=DIRECTION('center_axis',(0.,0.,-1.));
#28914=DIRECTION('ref_axis',(-0.883107319487933,0.469171037327368,0.));
#28915=DIRECTION('center_axis',(0.,0.,1.));
#28916=DIRECTION('ref_axis',(-0.883107319487933,0.469171037327368,0.));
#28917=DIRECTION('',(0.,0.,-1.));
#28918=DIRECTION('center_axis',(0.,0.,1.));
#28919=DIRECTION('ref_axis',(-0.838855879285935,0.544353574239593,0.));
#28920=DIRECTION('center_axis',(0.,0.,-1.));
#28921=DIRECTION('ref_axis',(-0.838855879285935,0.544353574239593,0.));
#28922=DIRECTION('center_axis',(0.,0.,1.));
#28923=DIRECTION('ref_axis',(-0.838855879285935,0.544353574239593,0.));
#28924=DIRECTION('',(0.,0.,-1.));
#28925=DIRECTION('center_axis',(0.,0.,1.));
#28926=DIRECTION('ref_axis',(-0.788220239327544,0.61539325176218,0.));
#28927=DIRECTION('center_axis',(0.,0.,-1.));
#28928=DIRECTION('ref_axis',(-0.788220239327544,0.61539325176218,0.));
#28929=DIRECTION('center_axis',(0.,0.,1.));
#28930=DIRECTION('ref_axis',(-0.788220239327544,0.61539325176218,0.));
#28931=DIRECTION('',(0.,0.,-1.));
#28932=DIRECTION('center_axis',(0.,0.,1.));
#28933=DIRECTION('ref_axis',(-0.731585767407477,0.681749415054251,0.));
#28934=DIRECTION('center_axis',(0.,0.,-1.));
#28935=DIRECTION('ref_axis',(-0.731585767407477,0.681749415054251,0.));
#28936=DIRECTION('center_axis',(0.,0.,1.));
#28937=DIRECTION('ref_axis',(-0.731585767407477,0.681749415054251,0.));
#28938=DIRECTION('',(0.,0.,-1.));
#28939=DIRECTION('center_axis',(0.,0.,1.));
#28940=DIRECTION('ref_axis',(-0.669383486053874,0.742917053646208,0.));
#28941=DIRECTION('center_axis',(0.,0.,-1.));
#28942=DIRECTION('ref_axis',(-0.669383486053874,0.742917053646208,0.));
#28943=DIRECTION('center_axis',(0.,0.,1.));
#28944=DIRECTION('ref_axis',(-0.669383486053874,0.742917053646208,0.));
#28945=DIRECTION('',(0.,0.,-1.));
#28946=DIRECTION('center_axis',(0.,0.,1.));
#28947=DIRECTION('ref_axis',(-0.602086792186602,0.798430644874335,0.));
#28948=DIRECTION('center_axis',(0.,0.,-1.));
#28949=DIRECTION('ref_axis',(-0.602086792186602,0.798430644874335,0.));
#28950=DIRECTION('center_axis',(0.,0.,1.));
#28951=DIRECTION('ref_axis',(-0.602086792186602,0.798430644874335,0.));
#28952=DIRECTION('',(0.,0.,-1.));
#28953=DIRECTION('center_axis',(0.,0.,1.));
#28954=DIRECTION('ref_axis',(-0.530207854280846,0.847867696789364,0.));
#28955=DIRECTION('center_axis',(0.,0.,-1.));
#28956=DIRECTION('ref_axis',(-0.530207854280846,0.847867696789364,0.));
#28957=DIRECTION('center_axis',(0.,0.,1.));
#28958=DIRECTION('ref_axis',(-0.530207854280846,0.847867696789364,0.));
#28959=DIRECTION('',(0.,0.,-1.));
#28960=DIRECTION('center_axis',(0.,0.,1.));
#28961=DIRECTION('ref_axis',(-0.454293714455756,0.890851963575314,0.));
#28962=DIRECTION('center_axis',(0.,0.,-1.));
#28963=DIRECTION('ref_axis',(-0.454293714455756,0.890851963575314,0.));
#28964=DIRECTION('center_axis',(0.,0.,1.));
#28965=DIRECTION('ref_axis',(-0.454293714455756,0.890851963575314,0.));
#28966=DIRECTION('',(0.,0.,-1.));
#28967=DIRECTION('center_axis',(0.,0.,1.));
#28968=DIRECTION('ref_axis',(-0.374922125153613,0.927056309007332,0.));
#28969=DIRECTION('center_axis',(0.,0.,-1.));
#28970=DIRECTION('ref_axis',(-0.374922125153613,0.927056309007332,0.));
#28971=DIRECTION('center_axis',(0.,0.,1.));
#28972=DIRECTION('ref_axis',(-0.374922125153613,0.927056309007332,0.));
#28973=DIRECTION('',(0.,0.,-1.));
#28974=DIRECTION('center_axis',(0.,0.,1.));
#28975=DIRECTION('ref_axis',(-0.292697152094883,0.956205196155901,0.));
#28976=DIRECTION('center_axis',(0.,0.,-1.));
#28977=DIRECTION('ref_axis',(-0.292697152094883,0.956205196155901,0.));
#28978=DIRECTION('center_axis',(0.,0.,1.));
#28979=DIRECTION('ref_axis',(-0.292697152094883,0.956205196155901,0.));
#28980=DIRECTION('',(0.,0.,-1.));
#28981=DIRECTION('center_axis',(0.,0.,1.));
#28982=DIRECTION('ref_axis',(-0.208244576973338,0.97807678438924,0.));
#28983=DIRECTION('center_axis',(0.,0.,-1.));
#28984=DIRECTION('ref_axis',(-0.208244576973338,0.97807678438924,0.));
#28985=DIRECTION('center_axis',(0.,0.,1.));
#28986=DIRECTION('ref_axis',(-0.208244576973338,0.97807678438924,0.));
#28987=DIRECTION('',(0.,0.,-1.));
#28988=DIRECTION('center_axis',(0.,0.,1.));
#28989=DIRECTION('ref_axis',(-0.122207134879512,0.992504617714467,0.));
#28990=DIRECTION('center_axis',(0.,0.,-1.));
#28991=DIRECTION('ref_axis',(-0.122207134879512,0.992504617714467,0.));
#28992=DIRECTION('center_axis',(0.,0.,1.));
#28993=DIRECTION('ref_axis',(-0.122207134879512,0.992504617714467,0.));
#28994=DIRECTION('',(0.,0.,-1.));
#28995=DIRECTION('center_axis',(0.,0.,1.));
#28996=DIRECTION('ref_axis',(-0.035239622698568,0.999378891608214,0.));
#28997=DIRECTION('center_axis',(0.,0.,-1.));
#28998=DIRECTION('ref_axis',(-0.035239622698568,0.999378891608214,0.));
#28999=DIRECTION('center_axis',(0.,0.,1.));
#29000=DIRECTION('ref_axis',(-0.035239622698568,0.999378891608214,0.));
#29001=DIRECTION('',(0.,0.,-1.));
#29002=DIRECTION('center_axis',(0.,0.,1.));
#29003=DIRECTION('ref_axis',(0.0519960842893784,0.998647288695349,0.));
#29004=DIRECTION('center_axis',(0.,0.,-1.));
#29005=DIRECTION('ref_axis',(0.0519960842893784,0.998647288695349,0.));
#29006=DIRECTION('center_axis',(0.,0.,1.));
#29007=DIRECTION('ref_axis',(0.0519960842893784,0.998647288695349,0.));
#29008=DIRECTION('',(0.,0.,-1.));
#29009=DIRECTION('center_axis',(0.,0.,1.));
#29010=DIRECTION('ref_axis',(0.138836069679788,0.990315376915793,0.));
#29011=DIRECTION('center_axis',(0.,0.,-1.));
#29012=DIRECTION('ref_axis',(0.138836069679788,0.990315376915793,0.));
#29013=DIRECTION('center_axis',(0.,0.,1.));
#29014=DIRECTION('ref_axis',(0.138836069679788,0.990315376915793,0.));
#29015=DIRECTION('',(0.,0.,-1.));
#29016=DIRECTION('center_axis',(0.,0.,1.));
#29017=DIRECTION('ref_axis',(0.224619428748424,0.974446567149134,0.));
#29018=DIRECTION('center_axis',(0.,0.,-1.));
#29019=DIRECTION('ref_axis',(0.224619428748424,0.974446567149134,0.));
#29020=DIRECTION('center_axis',(0.,0.,1.));
#29021=DIRECTION('ref_axis',(0.224619428748424,0.974446567149134,0.));
#29022=DIRECTION('',(0.,0.,-1.));
#29023=DIRECTION('center_axis',(0.,0.,1.));
#29024=DIRECTION('ref_axis',(0.308693298335365,0.951161630619546,0.));
#29025=DIRECTION('center_axis',(0.,0.,-1.));
#29026=DIRECTION('ref_axis',(0.308693298335365,0.951161630619546,0.));
#29027=DIRECTION('center_axis',(0.,0.,1.));
#29028=DIRECTION('ref_axis',(0.308693298335365,0.951161630619546,0.));
#29029=DIRECTION('',(0.,0.,-1.));
#29030=DIRECTION('center_axis',(0.,0.,1.));
#29031=DIRECTION('ref_axis',(0.390417825527865,0.920637779753848,0.));
#29032=DIRECTION('center_axis',(0.,0.,-1.));
#29033=DIRECTION('ref_axis',(0.390417825527865,0.920637779753848,0.));
#29034=DIRECTION('center_axis',(0.,0.,1.));
#29035=DIRECTION('ref_axis',(0.390417825527865,0.920637779753848,0.));
#29036=DIRECTION('',(0.,0.,-1.));
#29037=DIRECTION('center_axis',(0.,0.,1.));
#29038=DIRECTION('ref_axis',(0.469171037327368,0.883107319487932,0.));
#29039=DIRECTION('center_axis',(0.,0.,-1.));
#29040=DIRECTION('ref_axis',(0.469171037327368,0.883107319487932,0.));
#29041=DIRECTION('center_axis',(0.,0.,1.));
#29042=DIRECTION('ref_axis',(0.469171037327368,0.883107319487932,0.));
#29043=DIRECTION('',(0.,0.,-1.));
#29044=DIRECTION('center_axis',(0.,0.,1.));
#29045=DIRECTION('ref_axis',(0.544353574239593,0.838855879285935,0.));
#29046=DIRECTION('center_axis',(0.,0.,-1.));
#29047=DIRECTION('ref_axis',(0.544353574239593,0.838855879285935,0.));
#29048=DIRECTION('center_axis',(0.,0.,1.));
#29049=DIRECTION('ref_axis',(0.544353574239593,0.838855879285935,0.));
#29050=DIRECTION('',(0.,0.,-1.));
#29051=DIRECTION('center_axis',(0.,0.,1.));
#29052=DIRECTION('ref_axis',(0.61539325176218,0.788220239327544,0.));
#29053=DIRECTION('center_axis',(0.,0.,-1.));
#29054=DIRECTION('ref_axis',(0.61539325176218,0.788220239327544,0.));
#29055=DIRECTION('center_axis',(0.,0.,1.));
#29056=DIRECTION('ref_axis',(0.61539325176218,0.788220239327544,0.));
#29057=DIRECTION('',(0.,0.,-1.));
#29058=DIRECTION('center_axis',(0.,0.,1.));
#29059=DIRECTION('ref_axis',(0.681749415054251,0.731585767407477,0.));
#29060=DIRECTION('center_axis',(0.,0.,-1.));
#29061=DIRECTION('ref_axis',(0.681749415054251,0.731585767407477,0.));
#29062=DIRECTION('center_axis',(0.,0.,1.));
#29063=DIRECTION('ref_axis',(0.681749415054251,0.731585767407477,0.));
#29064=DIRECTION('',(0.,0.,-1.));
#29065=DIRECTION('center_axis',(0.,0.,1.));
#29066=DIRECTION('ref_axis',(0.742917053646208,0.669383486053874,0.));
#29067=DIRECTION('center_axis',(0.,0.,-1.));
#29068=DIRECTION('ref_axis',(0.742917053646208,0.669383486053874,0.));
#29069=DIRECTION('center_axis',(0.,0.,1.));
#29070=DIRECTION('ref_axis',(0.742917053646208,0.669383486053874,0.));
#29071=DIRECTION('',(0.,0.,-1.));
#29072=DIRECTION('center_axis',(0.,0.,1.));
#29073=DIRECTION('ref_axis',(0.798430644874335,0.602086792186603,0.));
#29074=DIRECTION('center_axis',(0.,0.,-1.));
#29075=DIRECTION('ref_axis',(0.798430644874335,0.602086792186603,0.));
#29076=DIRECTION('center_axis',(0.,0.,1.));
#29077=DIRECTION('ref_axis',(0.798430644874335,0.602086792186603,0.));
#29078=DIRECTION('',(0.,0.,-1.));
#29079=DIRECTION('center_axis',(0.,0.,1.));
#29080=DIRECTION('ref_axis',(0.847867696789364,0.530207854280846,0.));
#29081=DIRECTION('center_axis',(0.,0.,-1.));
#29082=DIRECTION('ref_axis',(0.847867696789364,0.530207854280846,0.));
#29083=DIRECTION('center_axis',(0.,0.,1.));
#29084=DIRECTION('ref_axis',(0.847867696789364,0.530207854280846,0.));
#29085=DIRECTION('',(0.,0.,-1.));
#29086=DIRECTION('center_axis',(0.,0.,1.));
#29087=DIRECTION('ref_axis',(0.890851963575314,0.454293714455756,0.));
#29088=DIRECTION('center_axis',(0.,0.,-1.));
#29089=DIRECTION('ref_axis',(0.890851963575314,0.454293714455756,0.));
#29090=DIRECTION('center_axis',(0.,0.,1.));
#29091=DIRECTION('ref_axis',(0.890851963575314,0.454293714455756,0.));
#29092=DIRECTION('',(0.,0.,-1.));
#29093=DIRECTION('center_axis',(0.,0.,1.));
#29094=DIRECTION('ref_axis',(0.927056309007332,0.374922125153613,0.));
#29095=DIRECTION('center_axis',(0.,0.,-1.));
#29096=DIRECTION('ref_axis',(0.927056309007332,0.374922125153613,0.));
#29097=DIRECTION('center_axis',(0.,0.,1.));
#29098=DIRECTION('ref_axis',(0.927056309007332,0.374922125153613,0.));
#29099=DIRECTION('',(0.,0.,-1.));
#29100=DIRECTION('center_axis',(0.,0.,1.));
#29101=DIRECTION('ref_axis',(0.956205196155901,0.292697152094883,0.));
#29102=DIRECTION('center_axis',(0.,0.,-1.));
#29103=DIRECTION('ref_axis',(0.956205196155901,0.292697152094883,0.));
#29104=DIRECTION('center_axis',(0.,0.,1.));
#29105=DIRECTION('ref_axis',(0.956205196155901,0.292697152094883,0.));
#29106=DIRECTION('',(0.,0.,-1.));
#29107=DIRECTION('center_axis',(0.,0.,1.));
#29108=DIRECTION('ref_axis',(0.97807678438924,0.208244576973338,0.));
#29109=DIRECTION('center_axis',(0.,0.,-1.));
#29110=DIRECTION('ref_axis',(0.97807678438924,0.208244576973338,0.));
#29111=DIRECTION('center_axis',(0.,0.,1.));
#29112=DIRECTION('ref_axis',(0.97807678438924,0.208244576973338,0.));
#29113=DIRECTION('',(0.,0.,-1.));
#29114=DIRECTION('center_axis',(0.,0.,1.));
#29115=DIRECTION('ref_axis',(0.992504617714467,0.122207134879512,0.));
#29116=DIRECTION('center_axis',(0.,0.,-1.));
#29117=DIRECTION('ref_axis',(0.992504617714467,0.122207134879512,0.));
#29118=DIRECTION('center_axis',(0.,0.,1.));
#29119=DIRECTION('ref_axis',(0.992504617714467,0.122207134879512,0.));
#29120=DIRECTION('',(0.,0.,1.));
#29121=DIRECTION('',(0.,0.,1.));
#29122=DIRECTION('',(0.,0.,1.));
#29123=DIRECTION('',(0.,0.,1.));
#29124=DIRECTION('',(0.,0.,1.));
#29125=DIRECTION('',(0.,0.,1.));
#29126=DIRECTION('',(0.,0.,1.));
#29127=DIRECTION('',(0.,0.,1.));
#29128=DIRECTION('',(0.,0.,1.));
#29129=DIRECTION('',(0.,0.,1.));
#29130=DIRECTION('',(0.,0.,1.));
#29131=DIRECTION('',(0.,0.,1.));
#29132=DIRECTION('',(0.,0.,1.));
#29133=DIRECTION('',(0.,0.,1.));
#29134=DIRECTION('',(0.,0.,1.));
#29135=DIRECTION('',(0.,0.,1.));
#29136=DIRECTION('',(0.,0.,1.));
#29137=DIRECTION('',(0.,0.,1.));
#29138=DIRECTION('',(0.,0.,1.));
#29139=DIRECTION('',(0.,0.,1.));
#29140=DIRECTION('',(0.,0.,1.));
#29141=DIRECTION('',(0.,0.,1.));
#29142=DIRECTION('',(0.,0.,1.));
#29143=DIRECTION('',(0.,0.,1.));
#29144=DIRECTION('',(0.,0.,1.));
#29145=DIRECTION('',(0.,0.,1.));
#29146=DIRECTION('',(0.,0.,1.));
#29147=DIRECTION('',(0.,0.,1.));
#29148=DIRECTION('',(0.,0.,1.));
#29149=DIRECTION('',(0.,0.,1.));
#29150=DIRECTION('',(0.,0.,1.));
#29151=DIRECTION('',(0.,0.,1.));
#29152=DIRECTION('',(0.,0.,1.));
#29153=DIRECTION('',(0.,0.,1.));
#29154=DIRECTION('',(0.,0.,1.));
#29155=DIRECTION('',(0.,0.,1.));
#29156=DIRECTION('',(0.,0.,1.));
#29157=DIRECTION('',(0.,0.,1.));
#29158=DIRECTION('',(0.,0.,1.));
#29159=DIRECTION('',(0.,0.,1.));
#29160=DIRECTION('',(0.,0.,1.));
#29161=DIRECTION('',(0.,0.,1.));
#29162=DIRECTION('',(0.,0.,1.));
#29163=DIRECTION('',(0.,0.,1.));
#29164=DIRECTION('',(0.,0.,1.));
#29165=DIRECTION('',(0.,0.,1.));
#29166=DIRECTION('',(0.,0.,1.));
#29167=DIRECTION('',(0.,0.,1.));
#29168=DIRECTION('',(0.,0.,1.));
#29169=DIRECTION('',(0.,0.,1.));
#29170=DIRECTION('',(0.,0.,1.));
#29171=DIRECTION('',(0.,0.,1.));
#29172=DIRECTION('',(0.,0.,1.));
#29173=DIRECTION('',(0.,0.,1.));
#29174=DIRECTION('',(0.,0.,1.));
#29175=DIRECTION('',(0.,0.,1.));
#29176=DIRECTION('',(0.,0.,1.));
#29177=DIRECTION('',(0.,0.,1.));
#29178=DIRECTION('',(0.,0.,1.));
#29179=DIRECTION('',(0.,0.,1.));
#29180=DIRECTION('',(0.,0.,1.));
#29181=DIRECTION('',(0.,0.,1.));
#29182=DIRECTION('',(0.,0.,1.));
#29183=DIRECTION('',(0.,0.,1.));
#29184=DIRECTION('',(0.,0.,1.));
#29185=DIRECTION('',(0.,0.,1.));
#29186=DIRECTION('',(0.,0.,1.));
#29187=DIRECTION('',(0.,0.,1.));
#29188=DIRECTION('',(0.,0.,1.));
#29189=DIRECTION('',(0.,0.,1.));
#29190=DIRECTION('',(0.,0.,1.));
#29191=DIRECTION('center_axis',(0.,0.,1.));
#29192=DIRECTION('ref_axis',(1.,0.,0.));
#29193=DIRECTION('center_axis',(0.,0.,-1.));
#29194=DIRECTION('ref_axis',(1.,0.,0.));
#29195=DIRECTION('',(0.,0.,1.));
#29196=DIRECTION('center_axis',(0.,0.,-1.));
#29197=DIRECTION('ref_axis',(1.,0.,0.));
#29198=DIRECTION('center_axis',(0.,0.,1.));
#29199=DIRECTION('ref_axis',(1.,0.,0.));
#29200=DIRECTION('center_axis',(0.,0.,-1.));
#29201=DIRECTION('ref_axis',(1.,0.,0.));
#29202=DIRECTION('center_axis',(0.,0.,-1.));
#29203=DIRECTION('ref_axis',(1.,0.,0.));
#29204=DIRECTION('center_axis',(0.,0.,1.));
#29205=DIRECTION('ref_axis',(1.,0.,0.));
#29206=DIRECTION('center_axis',(0.,0.,-1.));
#29207=DIRECTION('ref_axis',(1.,0.,0.));
#29208=DIRECTION('center_axis',(0.,0.,-1.));
#29209=DIRECTION('ref_axis',(1.,0.,0.));
#29210=DIRECTION('center_axis',(0.,0.,1.));
#29211=DIRECTION('ref_axis',(1.,0.,0.));
#29212=DIRECTION('center_axis',(0.,0.,-1.));
#29213=DIRECTION('ref_axis',(1.,0.,0.));
#29214=DIRECTION('center_axis',(0.,0.,-1.));
#29215=DIRECTION('ref_axis',(1.,0.,0.));
#29216=DIRECTION('center_axis',(0.,0.,1.));
#29217=DIRECTION('ref_axis',(1.,0.,0.));
#29218=DIRECTION('center_axis',(0.,0.,-1.));
#29219=DIRECTION('ref_axis',(1.,0.,0.));
#29220=DIRECTION('center_axis',(0.,0.,-1.));
#29221=DIRECTION('ref_axis',(1.,0.,0.));
#29222=DIRECTION('center_axis',(0.,0.,1.));
#29223=DIRECTION('ref_axis',(1.,0.,0.));
#29224=DIRECTION('center_axis',(0.,0.,-1.));
#29225=DIRECTION('ref_axis',(1.,0.,0.));
#29226=DIRECTION('center_axis',(0.,0.,-1.));
#29227=DIRECTION('ref_axis',(1.,0.,0.));
#29228=DIRECTION('center_axis',(0.,0.,1.));
#29229=DIRECTION('ref_axis',(1.,0.,0.));
#29230=DIRECTION('center_axis',(0.,0.,-1.));
#29231=DIRECTION('ref_axis',(1.,0.,0.));
#29232=DIRECTION('center_axis',(0.,0.,-1.));
#29233=DIRECTION('ref_axis',(1.,0.,0.));
#29234=DIRECTION('center_axis',(0.,0.,1.));
#29235=DIRECTION('ref_axis',(1.,0.,0.));
#29236=DIRECTION('center_axis',(0.,0.,-1.));
#29237=DIRECTION('ref_axis',(1.,0.,0.));
#29238=DIRECTION('center_axis',(0.,0.,-1.));
#29239=DIRECTION('ref_axis',(1.,0.,0.));
#29240=DIRECTION('center_axis',(0.,0.,1.));
#29241=DIRECTION('ref_axis',(1.,0.,0.));
#29242=DIRECTION('center_axis',(0.,0.,-1.));
#29243=DIRECTION('ref_axis',(1.,0.,0.));
#29244=DIRECTION('center_axis',(0.,0.,-1.));
#29245=DIRECTION('ref_axis',(1.,0.,0.));
#29246=DIRECTION('center_axis',(0.,0.,1.));
#29247=DIRECTION('ref_axis',(1.,0.,0.));
#29248=DIRECTION('center_axis',(0.,0.,-1.));
#29249=DIRECTION('ref_axis',(1.,0.,0.));
#29250=DIRECTION('center_axis',(0.,0.,-1.));
#29251=DIRECTION('ref_axis',(1.,0.,0.));
#29252=DIRECTION('center_axis',(0.,0.,1.));
#29253=DIRECTION('ref_axis',(1.,0.,0.));
#29254=DIRECTION('center_axis',(0.,0.,-1.));
#29255=DIRECTION('ref_axis',(1.,0.,0.));
#29256=DIRECTION('center_axis',(0.,0.,-1.));
#29257=DIRECTION('ref_axis',(1.,0.,0.));
#29258=DIRECTION('center_axis',(0.,0.,1.));
#29259=DIRECTION('ref_axis',(1.,0.,0.));
#29260=DIRECTION('center_axis',(0.,0.,-1.));
#29261=DIRECTION('ref_axis',(1.,0.,0.));
#29262=DIRECTION('center_axis',(0.,0.,-1.));
#29263=DIRECTION('ref_axis',(1.,0.,0.));
#29264=DIRECTION('center_axis',(0.,0.,1.));
#29265=DIRECTION('ref_axis',(1.,0.,0.));
#29266=DIRECTION('center_axis',(0.,0.,-1.));
#29267=DIRECTION('ref_axis',(1.,0.,0.));
#29268=DIRECTION('center_axis',(0.,0.,-1.));
#29269=DIRECTION('ref_axis',(1.,0.,0.));
#29270=DIRECTION('center_axis',(0.,0.,1.));
#29271=DIRECTION('ref_axis',(1.,0.,0.));
#29272=DIRECTION('center_axis',(0.,0.,-1.));
#29273=DIRECTION('ref_axis',(1.,0.,0.));
#29274=DIRECTION('center_axis',(0.,0.,-1.));
#29275=DIRECTION('ref_axis',(1.,0.,0.));
#29276=DIRECTION('center_axis',(0.,0.,1.));
#29277=DIRECTION('ref_axis',(1.,0.,0.));
#29278=DIRECTION('center_axis',(0.,0.,-1.));
#29279=DIRECTION('ref_axis',(1.,0.,0.));
#29280=DIRECTION('center_axis',(0.,0.,-1.));
#29281=DIRECTION('ref_axis',(1.,0.,0.));
#29282=DIRECTION('center_axis',(0.,0.,1.));
#29283=DIRECTION('ref_axis',(1.,0.,0.));
#29284=DIRECTION('center_axis',(0.,0.,-1.));
#29285=DIRECTION('ref_axis',(1.,0.,0.));
#29286=DIRECTION('center_axis',(0.,0.,-1.));
#29287=DIRECTION('ref_axis',(1.,0.,0.));
#29288=DIRECTION('center_axis',(0.,0.,1.));
#29289=DIRECTION('ref_axis',(1.,0.,0.));
#29290=DIRECTION('center_axis',(0.,0.,-1.));
#29291=DIRECTION('ref_axis',(1.,0.,0.));
#29292=DIRECTION('center_axis',(0.,0.,-1.));
#29293=DIRECTION('ref_axis',(1.,0.,0.));
#29294=DIRECTION('center_axis',(0.,0.,1.));
#29295=DIRECTION('ref_axis',(1.,0.,0.));
#29296=DIRECTION('center_axis',(0.,0.,-1.));
#29297=DIRECTION('ref_axis',(1.,0.,0.));
#29298=DIRECTION('center_axis',(0.,0.,-1.));
#29299=DIRECTION('ref_axis',(1.,0.,0.));
#29300=DIRECTION('center_axis',(0.,0.,1.));
#29301=DIRECTION('ref_axis',(1.,0.,0.));
#29302=DIRECTION('center_axis',(0.,0.,-1.));
#29303=DIRECTION('ref_axis',(1.,0.,0.));
#29304=DIRECTION('center_axis',(0.,0.,-1.));
#29305=DIRECTION('ref_axis',(1.,0.,0.));
#29306=DIRECTION('center_axis',(0.,0.,1.));
#29307=DIRECTION('ref_axis',(1.,0.,0.));
#29308=DIRECTION('center_axis',(0.,0.,-1.));
#29309=DIRECTION('ref_axis',(1.,0.,0.));
#29310=DIRECTION('center_axis',(0.,0.,-1.));
#29311=DIRECTION('ref_axis',(1.,0.,0.));
#29312=DIRECTION('center_axis',(0.,0.,1.));
#29313=DIRECTION('ref_axis',(1.,0.,0.));
#29314=DIRECTION('center_axis',(0.,0.,-1.));
#29315=DIRECTION('ref_axis',(1.,0.,0.));
#29316=DIRECTION('center_axis',(0.,0.,-1.));
#29317=DIRECTION('ref_axis',(1.,0.,0.));
#29318=DIRECTION('center_axis',(0.,0.,1.));
#29319=DIRECTION('ref_axis',(1.,0.,0.));
#29320=DIRECTION('center_axis',(0.,0.,-1.));
#29321=DIRECTION('ref_axis',(1.,0.,0.));
#29322=DIRECTION('center_axis',(0.,0.,-1.));
#29323=DIRECTION('ref_axis',(1.,0.,0.));
#29324=DIRECTION('center_axis',(0.,0.,1.));
#29325=DIRECTION('ref_axis',(1.,0.,0.));
#29326=DIRECTION('center_axis',(0.,0.,-1.));
#29327=DIRECTION('ref_axis',(1.,0.,0.));
#29328=DIRECTION('center_axis',(0.,0.,-1.));
#29329=DIRECTION('ref_axis',(1.,0.,0.));
#29330=DIRECTION('center_axis',(0.,0.,1.));
#29331=DIRECTION('ref_axis',(1.,0.,0.));
#29332=DIRECTION('center_axis',(0.,0.,-1.));
#29333=DIRECTION('ref_axis',(1.,0.,0.));
#29334=DIRECTION('center_axis',(0.,0.,-1.));
#29335=DIRECTION('ref_axis',(1.,0.,0.));
#29336=DIRECTION('center_axis',(0.,0.,1.));
#29337=DIRECTION('ref_axis',(1.,0.,0.));
#29338=DIRECTION('center_axis',(0.,0.,-1.));
#29339=DIRECTION('ref_axis',(1.,0.,0.));
#29340=DIRECTION('center_axis',(0.,0.,-1.));
#29341=DIRECTION('ref_axis',(1.,0.,0.));
#29342=DIRECTION('center_axis',(0.,0.,1.));
#29343=DIRECTION('ref_axis',(1.,0.,0.));
#29344=DIRECTION('center_axis',(0.,0.,-1.));
#29345=DIRECTION('ref_axis',(1.,0.,0.));
#29346=DIRECTION('center_axis',(0.,0.,-1.));
#29347=DIRECTION('ref_axis',(1.,0.,0.));
#29348=DIRECTION('center_axis',(0.,0.,1.));
#29349=DIRECTION('ref_axis',(1.,0.,0.));
#29350=DIRECTION('center_axis',(0.,0.,-1.));
#29351=DIRECTION('ref_axis',(1.,0.,0.));
#29352=DIRECTION('center_axis',(0.,0.,-1.));
#29353=DIRECTION('ref_axis',(1.,0.,0.));
#29354=DIRECTION('center_axis',(0.,0.,1.));
#29355=DIRECTION('ref_axis',(1.,0.,0.));
#29356=DIRECTION('center_axis',(0.,0.,-1.));
#29357=DIRECTION('ref_axis',(1.,0.,0.));
#29358=DIRECTION('center_axis',(0.,0.,-1.));
#29359=DIRECTION('ref_axis',(1.,0.,0.));
#29360=DIRECTION('center_axis',(0.,0.,1.));
#29361=DIRECTION('ref_axis',(1.,0.,0.));
#29362=DIRECTION('center_axis',(0.,0.,-1.));
#29363=DIRECTION('ref_axis',(1.,0.,0.));
#29364=DIRECTION('center_axis',(0.,0.,-1.));
#29365=DIRECTION('ref_axis',(1.,0.,0.));
#29366=DIRECTION('center_axis',(0.,0.,1.));
#29367=DIRECTION('ref_axis',(1.,0.,0.));
#29368=DIRECTION('center_axis',(0.,0.,-1.));
#29369=DIRECTION('ref_axis',(1.,0.,0.));
#29370=DIRECTION('center_axis',(0.,0.,-1.));
#29371=DIRECTION('ref_axis',(1.,0.,0.));
#29372=DIRECTION('center_axis',(0.,0.,1.));
#29373=DIRECTION('ref_axis',(1.,0.,0.));
#29374=DIRECTION('center_axis',(0.,0.,-1.));
#29375=DIRECTION('ref_axis',(1.,0.,0.));
#29376=DIRECTION('center_axis',(0.,0.,-1.));
#29377=DIRECTION('ref_axis',(1.,0.,0.));
#29378=DIRECTION('center_axis',(0.,0.,1.));
#29379=DIRECTION('ref_axis',(1.,0.,0.));
#29380=DIRECTION('center_axis',(0.,0.,-1.));
#29381=DIRECTION('ref_axis',(1.,0.,0.));
#29382=DIRECTION('center_axis',(0.,0.,-1.));
#29383=DIRECTION('ref_axis',(1.,0.,0.));
#29384=DIRECTION('center_axis',(0.,0.,1.));
#29385=DIRECTION('ref_axis',(1.,0.,0.));
#29386=DIRECTION('center_axis',(0.,0.,-1.));
#29387=DIRECTION('ref_axis',(1.,0.,0.));
#29388=DIRECTION('center_axis',(0.,0.,-1.));
#29389=DIRECTION('ref_axis',(1.,0.,0.));
#29390=DIRECTION('center_axis',(0.,0.,1.));
#29391=DIRECTION('ref_axis',(1.,0.,0.));
#29392=DIRECTION('center_axis',(0.,0.,-1.));
#29393=DIRECTION('ref_axis',(1.,0.,0.));
#29394=DIRECTION('center_axis',(0.,0.,-1.));
#29395=DIRECTION('ref_axis',(1.,0.,0.));
#29396=DIRECTION('center_axis',(0.,0.,1.));
#29397=DIRECTION('ref_axis',(1.,0.,0.));
#29398=DIRECTION('center_axis',(0.,0.,-1.));
#29399=DIRECTION('ref_axis',(1.,0.,0.));
#29400=DIRECTION('center_axis',(0.,0.,-1.));
#29401=DIRECTION('ref_axis',(1.,0.,0.));
#29402=DIRECTION('center_axis',(0.,0.,1.));
#29403=DIRECTION('ref_axis',(-1.,-1.22464679914735E-16,0.));
#29404=DIRECTION('center_axis',(0.,0.,-1.));
#29405=DIRECTION('ref_axis',(1.,0.,0.));
#29406=DIRECTION('center_axis',(0.,0.,-1.));
#29407=DIRECTION('ref_axis',(1.,0.,0.));
#29408=DIRECTION('center_axis',(0.,0.,1.));
#29409=DIRECTION('ref_axis',(1.,0.,0.));
#29410=DIRECTION('center_axis',(0.,0.,-1.));
#29411=DIRECTION('ref_axis',(1.,0.,0.));
#29412=DIRECTION('center_axis',(0.,0.,-1.));
#29413=DIRECTION('ref_axis',(1.,0.,0.));
#29414=DIRECTION('center_axis',(0.,0.,1.));
#29415=DIRECTION('ref_axis',(1.,0.,0.));
#29416=DIRECTION('center_axis',(0.,0.,-1.));
#29417=DIRECTION('ref_axis',(1.,0.,0.));
#29418=DIRECTION('center_axis',(0.,0.,-1.));
#29419=DIRECTION('ref_axis',(1.,0.,0.));
#29420=DIRECTION('center_axis',(0.,0.,1.));
#29421=DIRECTION('ref_axis',(1.,0.,0.));
#29422=DIRECTION('center_axis',(0.,0.,-1.));
#29423=DIRECTION('ref_axis',(1.,0.,0.));
#29424=DIRECTION('center_axis',(0.,0.,-1.));
#29425=DIRECTION('ref_axis',(1.,0.,0.));
#29426=DIRECTION('center_axis',(0.,0.,1.));
#29427=DIRECTION('ref_axis',(1.,0.,0.));
#29428=DIRECTION('center_axis',(0.,0.,-1.));
#29429=DIRECTION('ref_axis',(1.,0.,0.));
#29430=DIRECTION('center_axis',(0.,0.,-1.));
#29431=DIRECTION('ref_axis',(1.,0.,0.));
#29432=DIRECTION('center_axis',(0.,0.,1.));
#29433=DIRECTION('ref_axis',(1.,0.,0.));
#29434=DIRECTION('center_axis',(0.,0.,-1.));
#29435=DIRECTION('ref_axis',(1.,0.,0.));
#29436=DIRECTION('center_axis',(0.,0.,-1.));
#29437=DIRECTION('ref_axis',(1.,0.,0.));
#29438=DIRECTION('center_axis',(0.,0.,1.));
#29439=DIRECTION('ref_axis',(1.,0.,0.));
#29440=DIRECTION('center_axis',(0.,0.,-1.));
#29441=DIRECTION('ref_axis',(1.,0.,0.));
#29442=DIRECTION('center_axis',(0.,0.,-1.));
#29443=DIRECTION('ref_axis',(1.,0.,0.));
#29444=DIRECTION('center_axis',(0.,0.,1.));
#29445=DIRECTION('ref_axis',(1.,0.,0.));
#29446=DIRECTION('center_axis',(0.,0.,-1.));
#29447=DIRECTION('ref_axis',(1.,0.,0.));
#29448=DIRECTION('center_axis',(0.,0.,-1.));
#29449=DIRECTION('ref_axis',(1.,0.,0.));
#29450=DIRECTION('center_axis',(0.,0.,1.));
#29451=DIRECTION('ref_axis',(1.,0.,0.));
#29452=DIRECTION('center_axis',(0.,0.,-1.));
#29453=DIRECTION('ref_axis',(1.,0.,0.));
#29454=DIRECTION('center_axis',(0.,0.,-1.));
#29455=DIRECTION('ref_axis',(1.,0.,0.));
#29456=DIRECTION('center_axis',(0.,0.,1.));
#29457=DIRECTION('ref_axis',(1.,0.,0.));
#29458=DIRECTION('center_axis',(0.,0.,-1.));
#29459=DIRECTION('ref_axis',(1.,0.,0.));
#29460=DIRECTION('center_axis',(0.,0.,-1.));
#29461=DIRECTION('ref_axis',(1.,0.,0.));
#29462=DIRECTION('center_axis',(0.,0.,1.));
#29463=DIRECTION('ref_axis',(1.,0.,0.));
#29464=DIRECTION('center_axis',(0.,0.,-1.));
#29465=DIRECTION('ref_axis',(1.,0.,0.));
#29466=DIRECTION('center_axis',(0.,0.,-1.));
#29467=DIRECTION('ref_axis',(1.,0.,0.));
#29468=DIRECTION('center_axis',(0.,0.,1.));
#29469=DIRECTION('ref_axis',(1.,0.,0.));
#29470=DIRECTION('center_axis',(0.,0.,-1.));
#29471=DIRECTION('ref_axis',(1.,0.,0.));
#29472=DIRECTION('center_axis',(0.,0.,-1.));
#29473=DIRECTION('ref_axis',(1.,0.,0.));
#29474=DIRECTION('center_axis',(0.,0.,1.));
#29475=DIRECTION('ref_axis',(1.,0.,0.));
#29476=DIRECTION('center_axis',(0.,0.,-1.));
#29477=DIRECTION('ref_axis',(1.,0.,0.));
#29478=DIRECTION('center_axis',(0.,0.,-1.));
#29479=DIRECTION('ref_axis',(1.,0.,0.));
#29480=DIRECTION('center_axis',(0.,0.,1.));
#29481=DIRECTION('ref_axis',(1.,0.,0.));
#29482=DIRECTION('center_axis',(0.,0.,-1.));
#29483=DIRECTION('ref_axis',(1.,0.,0.));
#29484=DIRECTION('center_axis',(0.,0.,-1.));
#29485=DIRECTION('ref_axis',(1.,0.,0.));
#29486=DIRECTION('center_axis',(0.,0.,1.));
#29487=DIRECTION('ref_axis',(1.,0.,0.));
#29488=DIRECTION('center_axis',(0.,0.,-1.));
#29489=DIRECTION('ref_axis',(1.,0.,0.));
#29490=DIRECTION('center_axis',(0.,0.,-1.));
#29491=DIRECTION('ref_axis',(1.,0.,0.));
#29492=DIRECTION('center_axis',(0.,0.,1.));
#29493=DIRECTION('ref_axis',(1.,0.,0.));
#29494=DIRECTION('center_axis',(0.,0.,-1.));
#29495=DIRECTION('ref_axis',(1.,0.,0.));
#29496=DIRECTION('center_axis',(0.,0.,-1.));
#29497=DIRECTION('ref_axis',(1.,0.,0.));
#29498=DIRECTION('center_axis',(0.,0.,1.));
#29499=DIRECTION('ref_axis',(1.,0.,0.));
#29500=DIRECTION('center_axis',(0.,0.,-1.));
#29501=DIRECTION('ref_axis',(1.,0.,0.));
#29502=DIRECTION('center_axis',(0.,0.,-1.));
#29503=DIRECTION('ref_axis',(1.,0.,0.));
#29504=DIRECTION('center_axis',(0.,0.,1.));
#29505=DIRECTION('ref_axis',(1.,0.,0.));
#29506=DIRECTION('center_axis',(0.,0.,-1.));
#29507=DIRECTION('ref_axis',(1.,0.,0.));
#29508=DIRECTION('center_axis',(0.,0.,-1.));
#29509=DIRECTION('ref_axis',(1.,0.,0.));
#29510=DIRECTION('center_axis',(0.,0.,1.));
#29511=DIRECTION('ref_axis',(1.,0.,0.));
#29512=DIRECTION('center_axis',(0.,0.,-1.));
#29513=DIRECTION('ref_axis',(1.,0.,0.));
#29514=DIRECTION('center_axis',(0.,0.,-1.));
#29515=DIRECTION('ref_axis',(1.,0.,0.));
#29516=DIRECTION('center_axis',(0.,0.,1.));
#29517=DIRECTION('ref_axis',(1.,0.,0.));
#29518=DIRECTION('center_axis',(0.,0.,-1.));
#29519=DIRECTION('ref_axis',(1.,0.,0.));
#29520=DIRECTION('center_axis',(0.,0.,-1.));
#29521=DIRECTION('ref_axis',(1.,0.,0.));
#29522=DIRECTION('center_axis',(0.,0.,1.));
#29523=DIRECTION('ref_axis',(1.,0.,0.));
#29524=DIRECTION('center_axis',(0.,0.,-1.));
#29525=DIRECTION('ref_axis',(1.,0.,0.));
#29526=DIRECTION('center_axis',(0.,0.,-1.));
#29527=DIRECTION('ref_axis',(1.,0.,0.));
#29528=DIRECTION('center_axis',(0.,0.,1.));
#29529=DIRECTION('ref_axis',(1.,0.,0.));
#29530=DIRECTION('center_axis',(0.,0.,-1.));
#29531=DIRECTION('ref_axis',(1.,0.,0.));
#29532=DIRECTION('center_axis',(0.,0.,-1.));
#29533=DIRECTION('ref_axis',(1.,0.,0.));
#29534=DIRECTION('center_axis',(0.,0.,1.));
#29535=DIRECTION('ref_axis',(1.,0.,0.));
#29536=DIRECTION('center_axis',(0.,0.,-1.));
#29537=DIRECTION('ref_axis',(1.,0.,0.));
#29538=DIRECTION('center_axis',(0.,0.,-1.));
#29539=DIRECTION('ref_axis',(1.,0.,0.));
#29540=DIRECTION('center_axis',(0.,0.,1.));
#29541=DIRECTION('ref_axis',(1.,0.,0.));
#29542=DIRECTION('center_axis',(0.,0.,-1.));
#29543=DIRECTION('ref_axis',(1.,0.,0.));
#29544=DIRECTION('center_axis',(0.,0.,-1.));
#29545=DIRECTION('ref_axis',(1.,0.,0.));
#29546=DIRECTION('center_axis',(0.,0.,1.));
#29547=DIRECTION('ref_axis',(1.,0.,0.));
#29548=DIRECTION('center_axis',(0.,0.,-1.));
#29549=DIRECTION('ref_axis',(1.,0.,0.));
#29550=DIRECTION('center_axis',(0.,0.,-1.));
#29551=DIRECTION('ref_axis',(1.,0.,0.));
#29552=DIRECTION('center_axis',(0.,0.,1.));
#29553=DIRECTION('ref_axis',(1.,0.,0.));
#29554=DIRECTION('center_axis',(0.,0.,-1.));
#29555=DIRECTION('ref_axis',(1.,0.,0.));
#29556=DIRECTION('center_axis',(0.,0.,-1.));
#29557=DIRECTION('ref_axis',(1.,0.,0.));
#29558=DIRECTION('center_axis',(0.,0.,1.));
#29559=DIRECTION('ref_axis',(1.,0.,0.));
#29560=DIRECTION('center_axis',(0.,0.,-1.));
#29561=DIRECTION('ref_axis',(1.,0.,0.));
#29562=DIRECTION('center_axis',(0.,0.,-1.));
#29563=DIRECTION('ref_axis',(1.,0.,0.));
#29564=DIRECTION('center_axis',(0.,0.,1.));
#29565=DIRECTION('ref_axis',(1.,0.,0.));
#29566=DIRECTION('center_axis',(0.,0.,-1.));
#29567=DIRECTION('ref_axis',(1.,0.,0.));
#29568=DIRECTION('center_axis',(0.,0.,-1.));
#29569=DIRECTION('ref_axis',(1.,0.,0.));
#29570=DIRECTION('center_axis',(0.,0.,1.));
#29571=DIRECTION('ref_axis',(1.,0.,0.));
#29572=DIRECTION('center_axis',(0.,0.,-1.));
#29573=DIRECTION('ref_axis',(1.,0.,0.));
#29574=DIRECTION('center_axis',(0.,0.,-1.));
#29575=DIRECTION('ref_axis',(1.,0.,0.));
#29576=DIRECTION('center_axis',(0.,0.,1.));
#29577=DIRECTION('ref_axis',(1.,0.,0.));
#29578=DIRECTION('center_axis',(0.,0.,-1.));
#29579=DIRECTION('ref_axis',(1.,0.,0.));
#29580=DIRECTION('center_axis',(0.,0.,-1.));
#29581=DIRECTION('ref_axis',(1.,0.,0.));
#29582=DIRECTION('center_axis',(0.,0.,1.));
#29583=DIRECTION('ref_axis',(1.,0.,0.));
#29584=DIRECTION('center_axis',(0.,0.,-1.));
#29585=DIRECTION('ref_axis',(1.,0.,0.));
#29586=DIRECTION('center_axis',(0.,0.,-1.));
#29587=DIRECTION('ref_axis',(1.,0.,0.));
#29588=DIRECTION('center_axis',(0.,0.,1.));
#29589=DIRECTION('ref_axis',(1.,0.,0.));
#29590=DIRECTION('center_axis',(0.,0.,-1.));
#29591=DIRECTION('ref_axis',(1.,0.,0.));
#29592=DIRECTION('center_axis',(0.,0.,-1.));
#29593=DIRECTION('ref_axis',(1.,0.,0.));
#29594=DIRECTION('center_axis',(0.,0.,1.));
#29595=DIRECTION('ref_axis',(1.,0.,0.));
#29596=DIRECTION('center_axis',(0.,0.,-1.));
#29597=DIRECTION('ref_axis',(1.,0.,0.));
#29598=DIRECTION('center_axis',(0.,0.,-1.));
#29599=DIRECTION('ref_axis',(1.,0.,0.));
#29600=DIRECTION('center_axis',(0.,0.,1.));
#29601=DIRECTION('ref_axis',(1.,0.,0.));
#29602=DIRECTION('center_axis',(0.,0.,-1.));
#29603=DIRECTION('ref_axis',(1.,0.,0.));
#29604=DIRECTION('center_axis',(0.,0.,-1.));
#29605=DIRECTION('ref_axis',(1.,0.,0.));
#29606=DIRECTION('center_axis',(0.,0.,1.));
#29607=DIRECTION('ref_axis',(1.,0.,0.));
#29608=DIRECTION('center_axis',(0.,0.,-1.));
#29609=DIRECTION('ref_axis',(1.,0.,0.));
#29610=DIRECTION('center_axis',(0.,0.,-1.));
#29611=DIRECTION('ref_axis',(1.,0.,0.));
#29612=DIRECTION('center_axis',(0.,0.,1.));
#29613=DIRECTION('ref_axis',(1.,0.,0.));
#29614=DIRECTION('center_axis',(0.,0.,-1.));
#29615=DIRECTION('ref_axis',(1.,0.,0.));
#29616=DIRECTION('',(0.,0.,-1.));
#29617=DIRECTION('center_axis',(0.,0.,-1.));
#29618=DIRECTION('ref_axis',(1.,0.,0.));
#29619=DIRECTION('center_axis',(0.,0.,1.));
#29620=DIRECTION('ref_axis',(0.999378891608214,0.035239622698568,0.));
#29621=DIRECTION('center_axis',(0.,0.,-1.));
#29622=DIRECTION('ref_axis',(0.999378891608214,0.035239622698568,0.));
#29623=DIRECTION('center_axis',(0.,0.,1.));
#29624=DIRECTION('ref_axis',(0.999378891608214,0.035239622698568,0.));
#29625=DIRECTION('center_axis',(0.,0.,1.));
#29626=DIRECTION('ref_axis',(1.,0.,0.));
#29627=DIRECTION('center_axis',(0.,0.,1.));
#29628=DIRECTION('ref_axis',(1.,0.,0.));
#29629=DIRECTION('center_axis',(0.,0.,-1.));
#29630=DIRECTION('ref_axis',(1.,0.,0.));
#29631=DIRECTION('center_axis',(0.,0.,1.));
#29632=DIRECTION('ref_axis',(1.,0.,0.));
#29633=DIRECTION('center_axis',(0.,0.,-1.));
#29634=DIRECTION('ref_axis',(1.,0.,0.));
#29635=DIRECTION('center_axis',(0.,0.,1.));
#29636=DIRECTION('ref_axis',(1.,0.,0.));
#29637=DIRECTION('',(0.,0.,-1.));
#29638=DIRECTION('',(0.,0.,-1.));
#29639=DIRECTION('center_axis',(0.,0.,1.));
#29640=DIRECTION('ref_axis',(1.,0.,0.));
#29641=DIRECTION('center_axis',(0.,0.,1.));
#29642=DIRECTION('ref_axis',(1.,0.,0.));
#29643=DIRECTION('axis',(0.,0.,1.));
#29644=DIRECTION('refdir',(1.,0.,0.));
#29645=DIRECTION('center_axis',(0.,1.,0.));
#29646=DIRECTION('ref_axis',(1.,0.,0.));
#29647=DIRECTION('',(0.,0.,1.));
#29648=DIRECTION('',(-1.,0.,0.));
#29649=DIRECTION('',(0.,0.,-1.));
#29650=DIRECTION('',(1.,0.,0.));
#29651=DIRECTION('center_axis',(0.,-1.,0.));
#29652=DIRECTION('ref_axis',(-1.,0.,0.));
#29653=DIRECTION('',(0.,0.,-1.));
#29654=DIRECTION('',(-1.,0.,0.));
#29655=DIRECTION('',(0.,0.,-1.));
#29656=DIRECTION('',(1.,0.,0.));
#29657=DIRECTION('center_axis',(1.,0.,0.));
#29658=DIRECTION('ref_axis',(0.,-1.,0.));
#29659=DIRECTION('',(0.,-1.,0.));
#29660=DIRECTION('',(0.,1.,0.));
#29661=DIRECTION('center_axis',(0.,0.,1.));
#29662=DIRECTION('ref_axis',(-1.,1.22464679914735E-16,0.));
#29663=DIRECTION('center_axis',(0.,0.,-1.));
#29664=DIRECTION('ref_axis',(1.,0.,0.));
#29665=DIRECTION('center_axis',(0.,0.,-1.));
#29666=DIRECTION('ref_axis',(1.,0.,0.));
#29667=DIRECTION('center_axis',(0.,0.,1.));
#29668=DIRECTION('ref_axis',(1.,0.,0.));
#29669=DIRECTION('center_axis',(0.,0.,1.));
#29670=DIRECTION('ref_axis',(1.,0.,0.));
#29671=DIRECTION('',(-0.996938396815926,-0.0781910030252308,0.));
#29672=DIRECTION('center_axis',(0.,0.,1.));
#29673=DIRECTION('ref_axis',(-0.640971010199219,-0.767565087848707,0.));
#29674=DIRECTION('center_axis',(0.,0.,1.));
#29675=DIRECTION('ref_axis',(0.996938396815926,0.0781910030252301,0.));
#29676=DIRECTION('center_axis',(0.,0.,1.));
#29677=DIRECTION('ref_axis',(-0.817790915745051,0.575515436912748,0.));
#29678=DIRECTION('',(0.983205865442321,0.182499934684418,0.));
#29679=DIRECTION('center_axis',(0.,0.,1.));
#29680=DIRECTION('ref_axis',(1.,0.,0.));
#29681=DIRECTION('',(-0.942731223965124,-0.333553353095453,0.));
#29682=DIRECTION('center_axis',(0.,0.,1.));
#29683=DIRECTION('ref_axis',(-0.420469989562974,-0.907306446509068,0.));
#29684=DIRECTION('center_axis',(0.,0.,1.));
#29685=DIRECTION('ref_axis',(0.942731223965124,0.333553353095452,0.));
#29686=DIRECTION('center_axis',(0.,0.,1.));
#29687=DIRECTION('ref_axis',(-0.93887972184625,0.34424536003541,0.));
#29688=DIRECTION('',(0.902469479163339,0.430753803440726,0.));
#29689=DIRECTION('center_axis',(0.,0.,1.));
#29690=DIRECTION('ref_axis',(1.,0.,0.));
#29691=DIRECTION('',(-0.824278476138108,-0.566184593375199,0.));
#29692=DIRECTION('center_axis',(0.,0.,1.));
#29693=DIRECTION('ref_axis',(-0.171314633997547,-0.985216370234623,0.));
#29694=DIRECTION('center_axis',(0.,0.,1.));
#29695=DIRECTION('ref_axis',(0.824278476138108,0.566184593375198,0.));
#29696=DIRECTION('center_axis',(0.,0.,1.));
#29697=DIRECTION('ref_axis',(-0.995985426475728,0.0895155307640127,0.));
#29698=DIRECTION('',(0.760231289280706,0.649652512346867,0.));
#29699=DIRECTION('center_axis',(0.,0.,1.));
#29700=DIRECTION('ref_axis',(1.,0.,0.));
#29701=DIRECTION('',(-0.649652512346868,-0.760231289280705,0.));
#29702=DIRECTION('center_axis',(0.,0.,1.));
#29703=DIRECTION('ref_axis',(0.0895155307640121,-0.995985426475728,0.));
#29704=DIRECTION('center_axis',(0.,0.,1.));
#29705=DIRECTION('ref_axis',(0.649652512346868,0.760231289280704,0.));
#29706=DIRECTION('center_axis',(0.,0.,1.));
#29707=DIRECTION('ref_axis',(-0.985216370234624,-0.171314633997546,0.));
#29708=DIRECTION('',(0.5661845933752,0.824278476138107,0.));
#29709=DIRECTION('center_axis',(0.,0.,1.));
#29710=DIRECTION('ref_axis',(1.,0.,0.));
#29711=DIRECTION('',(-0.430753803440727,-0.902469479163338,0.));
#29712=DIRECTION('center_axis',(0.,0.,1.));
#29713=DIRECTION('ref_axis',(0.344245360035413,-0.938879721846248,0.));
#29714=DIRECTION('center_axis',(0.,0.,1.));
#29715=DIRECTION('ref_axis',(0.430753803440728,0.902469479163338,0.));
#29716=DIRECTION('center_axis',(0.,0.,1.));
#29717=DIRECTION('ref_axis',(-0.907306446509064,-0.420469989562983,0.));
#29718=DIRECTION('',(0.333553353095454,0.942731223965123,0.));
#29719=DIRECTION('center_axis',(0.,0.,1.));
#29720=DIRECTION('ref_axis',(1.,0.,0.));
#29721=DIRECTION('',(-0.182499934684419,-0.983205865442321,0.));
#29722=DIRECTION('center_axis',(0.,0.,1.));
#29723=DIRECTION('ref_axis',(0.57551543691275,-0.817790915745049,0.));
#29724=DIRECTION('center_axis',(0.,0.,1.));
#29725=DIRECTION('ref_axis',(0.18249993468442,0.983205865442321,0.));
#29726=DIRECTION('center_axis',(0.,0.,1.));
#29727=DIRECTION('ref_axis',(-0.767565087848706,-0.640971010199219,0.));
#29728=DIRECTION('',(0.0781910030252323,0.996938396815926,0.));
#29729=DIRECTION('center_axis',(0.,0.,1.));
#29730=DIRECTION('ref_axis',(1.,0.,0.));
#29731=DIRECTION('',(0.0781910030252308,-0.996938396815926,0.));
#29732=DIRECTION('center_axis',(0.,0.,1.));
#29733=DIRECTION('ref_axis',(0.767565087848708,-0.640971010199218,0.));
#29734=DIRECTION('center_axis',(0.,0.,1.));
#29735=DIRECTION('ref_axis',(-0.0781910030252301,0.996938396815926,0.));
#29736=DIRECTION('center_axis',(0.,0.,1.));
#29737=DIRECTION('ref_axis',(-0.575515436912748,-0.817790915745051,0.));
#29738=DIRECTION('',(-0.182499934684418,0.983205865442321,0.));
#29739=DIRECTION('center_axis',(0.,0.,1.));
#29740=DIRECTION('ref_axis',(1.,0.,0.));
#29741=DIRECTION('',(0.333553353095453,-0.942731223965124,0.));
#29742=DIRECTION('center_axis',(0.,0.,1.));
#29743=DIRECTION('ref_axis',(0.907306446509069,-0.420469989562973,0.));
#29744=DIRECTION('center_axis',(0.,0.,1.));
#29745=DIRECTION('ref_axis',(-0.333553353095452,0.942731223965124,0.));
#29746=DIRECTION('center_axis',(0.,0.,1.));
#29747=DIRECTION('ref_axis',(-0.34424536003541,-0.93887972184625,0.));
#29748=DIRECTION('',(-0.430753803440726,0.902469479163339,0.));
#29749=DIRECTION('center_axis',(0.,0.,1.));
#29750=DIRECTION('ref_axis',(1.,0.,0.));
#29751=DIRECTION('',(0.566184593375199,-0.824278476138108,0.));
#29752=DIRECTION('center_axis',(0.,0.,1.));
#29753=DIRECTION('ref_axis',(0.985216370234623,-0.171314633997547,0.));
#29754=DIRECTION('center_axis',(0.,0.,1.));
#29755=DIRECTION('ref_axis',(-0.566184593375198,0.824278476138108,0.));
#29756=DIRECTION('center_axis',(0.,0.,1.));
#29757=DIRECTION('ref_axis',(-0.0895155307640188,-0.995985426475727,0.));
#29758=DIRECTION('',(-0.649652512346867,0.760231289280706,0.));
#29759=DIRECTION('center_axis',(0.,0.,1.));
#29760=DIRECTION('ref_axis',(1.,0.,0.));
#29761=DIRECTION('',(0.760231289280705,-0.649652512346868,0.));
#29762=DIRECTION('center_axis',(0.,0.,1.));
#29763=DIRECTION('ref_axis',(0.995985426475728,0.0895155307640127,0.));
#29764=DIRECTION('center_axis',(0.,0.,1.));
#29765=DIRECTION('ref_axis',(-0.760231289280704,0.649652512346868,0.));
#29766=DIRECTION('center_axis',(0.,0.,1.));
#29767=DIRECTION('ref_axis',(0.171314633997546,-0.985216370234624,0.));
#29768=DIRECTION('',(-0.824278476138107,0.5661845933752,0.));
#29769=DIRECTION('center_axis',(0.,0.,1.));
#29770=DIRECTION('ref_axis',(1.,0.,0.));
#29771=DIRECTION('',(0.902469479163338,-0.430753803440727,0.));
#29772=DIRECTION('center_axis',(0.,0.,1.));
#29773=DIRECTION('ref_axis',(0.93887972184625,0.344245360035408,0.));
#29774=DIRECTION('center_axis',(0.,0.,1.));
#29775=DIRECTION('ref_axis',(-0.902469479163338,0.430753803440728,0.));
#29776=DIRECTION('center_axis',(0.,0.,1.));
#29777=DIRECTION('ref_axis',(0.420469989562984,-0.907306446509064,0.));
#29778=DIRECTION('',(-0.942731223965123,0.333553353095454,0.));
#29779=DIRECTION('center_axis',(0.,0.,1.));
#29780=DIRECTION('ref_axis',(1.,0.,0.));
#29781=DIRECTION('',(0.983205865442321,-0.182499934684419,0.));
#29782=DIRECTION('center_axis',(0.,0.,1.));
#29783=DIRECTION('ref_axis',(0.817790915745049,0.57551543691275,0.));
#29784=DIRECTION('center_axis',(0.,0.,1.));
#29785=DIRECTION('ref_axis',(-0.983205865442321,0.18249993468442,0.));
#29786=DIRECTION('center_axis',(0.,0.,1.));
#29787=DIRECTION('ref_axis',(0.640971010199219,-0.767565087848706,0.));
#29788=DIRECTION('',(-0.996938396815926,0.0781910030252323,0.));
#29789=DIRECTION('center_axis',(0.,0.,1.));
#29790=DIRECTION('ref_axis',(1.,0.,0.));
#29791=DIRECTION('',(0.996938396815926,0.0781910030252307,0.));
#29792=DIRECTION('center_axis',(0.,0.,1.));
#29793=DIRECTION('ref_axis',(0.64097101019921,0.767565087848714,0.));
#29794=DIRECTION('center_axis',(0.,0.,1.));
#29795=DIRECTION('ref_axis',(-0.996938396815926,-0.07819100302523,0.));
#29796=DIRECTION('center_axis',(0.,0.,1.));
#29797=DIRECTION('ref_axis',(0.817790915745051,-0.575515436912747,0.));
#29798=DIRECTION('',(-0.983205865442321,-0.182499934684417,0.));
#29799=DIRECTION('center_axis',(0.,0.,1.));
#29800=DIRECTION('ref_axis',(1.,0.,0.));
#29801=DIRECTION('',(0.942731223965124,0.333553353095453,0.));
#29802=DIRECTION('center_axis',(0.,0.,1.));
#29803=DIRECTION('ref_axis',(0.420469989562982,0.907306446509065,0.));
#29804=DIRECTION('center_axis',(0.,0.,1.));
#29805=DIRECTION('ref_axis',(-0.942731223965124,-0.333553353095452,0.));
#29806=DIRECTION('center_axis',(0.,0.,1.));
#29807=DIRECTION('ref_axis',(0.93887972184625,-0.344245360035407,0.));
#29808=DIRECTION('',(-0.902469479163339,-0.430753803440726,0.));
#29809=DIRECTION('center_axis',(0.,0.,1.));
#29810=DIRECTION('ref_axis',(1.,0.,0.));
#29811=DIRECTION('',(0.824278476138108,0.566184593375198,0.));
#29812=DIRECTION('center_axis',(0.,0.,1.));
#29813=DIRECTION('ref_axis',(0.17131463399754,0.985216370234625,0.));
#29814=DIRECTION('center_axis',(0.,0.,1.));
#29815=DIRECTION('ref_axis',(-0.824278476138108,-0.566184593375198,0.));
#29816=DIRECTION('center_axis',(0.,0.,1.));
#29817=DIRECTION('ref_axis',(0.995985426475728,-0.0895155307640127,0.));
#29818=DIRECTION('',(-0.760231289280706,-0.649652512346867,0.));
#29819=DIRECTION('center_axis',(0.,0.,1.));
#29820=DIRECTION('ref_axis',(1.,0.,0.));
#29821=DIRECTION('',(0.649652512346868,0.760231289280705,0.));
#29822=DIRECTION('center_axis',(0.,0.,1.));
#29823=DIRECTION('ref_axis',(-0.0895155307640188,0.995985426475727,0.));
#29824=DIRECTION('center_axis',(0.,0.,1.));
#29825=DIRECTION('ref_axis',(-0.649652512346869,-0.760231289280704,0.));
#29826=DIRECTION('center_axis',(0.,0.,1.));
#29827=DIRECTION('ref_axis',(0.985216370234623,0.171314633997547,0.));
#29828=DIRECTION('',(-0.5661845933752,-0.824278476138107,0.));
#29829=DIRECTION('center_axis',(0.,0.,1.));
#29830=DIRECTION('ref_axis',(1.,0.,0.));
#29831=DIRECTION('',(0.430753803440728,0.902469479163338,0.));
#29832=DIRECTION('center_axis',(0.,0.,1.));
#29833=DIRECTION('ref_axis',(-0.344245360035407,0.93887972184625,0.));
#29834=DIRECTION('center_axis',(0.,0.,1.));
#29835=DIRECTION('ref_axis',(-0.430753803440728,-0.902469479163338,0.));
#29836=DIRECTION('center_axis',(0.,0.,1.));
#29837=DIRECTION('ref_axis',(0.907306446509064,0.420469989562984,0.));
#29838=DIRECTION('',(-0.333553353095455,-0.942731223965123,0.));
#29839=DIRECTION('center_axis',(0.,0.,1.));
#29840=DIRECTION('ref_axis',(1.,0.,0.));
#29841=DIRECTION('',(0.182499934684419,0.983205865442321,0.));
#29842=DIRECTION('center_axis',(0.,0.,1.));
#29843=DIRECTION('ref_axis',(-0.575515436912756,0.817790915745045,0.));
#29844=DIRECTION('center_axis',(0.,0.,1.));
#29845=DIRECTION('ref_axis',(-0.18249993468442,-0.983205865442321,0.));
#29846=DIRECTION('center_axis',(0.,0.,1.));
#29847=DIRECTION('ref_axis',(0.767565087848712,0.640971010199212,0.));
#29848=DIRECTION('',(-0.0781910030252327,-0.996938396815926,0.));
#29849=DIRECTION('center_axis',(0.,0.,1.));
#29850=DIRECTION('ref_axis',(1.,0.,0.));
#29851=DIRECTION('',(-0.0781910030252307,0.996938396815926,0.));
#29852=DIRECTION('center_axis',(0.,0.,1.));
#29853=DIRECTION('ref_axis',(-0.767565087848714,0.64097101019921,0.));
#29854=DIRECTION('center_axis',(0.,0.,1.));
#29855=DIRECTION('ref_axis',(0.07819100302523,-0.996938396815926,0.));
#29856=DIRECTION('center_axis',(0.,0.,1.));
#29857=DIRECTION('ref_axis',(0.575515436912747,0.817790915745051,0.));
#29858=DIRECTION('',(0.182499934684417,-0.983205865442321,0.));
#29859=DIRECTION('center_axis',(0.,0.,1.));
#29860=DIRECTION('ref_axis',(1.,0.,0.));
#29861=DIRECTION('',(-0.333553353095453,0.942731223965124,0.));
#29862=DIRECTION('center_axis',(0.,0.,1.));
#29863=DIRECTION('ref_axis',(-0.907306446509064,0.420469989562983,0.));
#29864=DIRECTION('center_axis',(0.,0.,1.));
#29865=DIRECTION('ref_axis',(0.333553353095452,-0.942731223965124,0.));
#29866=DIRECTION('center_axis',(0.,0.,1.));
#29867=DIRECTION('ref_axis',(0.344245360035407,0.938879721846251,0.));
#29868=DIRECTION('',(0.430753803440726,-0.902469479163339,0.));
#29869=DIRECTION('center_axis',(0.,0.,1.));
#29870=DIRECTION('ref_axis',(1.,0.,0.));
#29871=DIRECTION('',(-0.566184593375198,0.824278476138108,0.));
#29872=DIRECTION('center_axis',(0.,0.,1.));
#29873=DIRECTION('ref_axis',(-0.985216370234624,0.171314633997541,0.));
#29874=DIRECTION('center_axis',(0.,0.,1.));
#29875=DIRECTION('ref_axis',(0.566184593375197,-0.824278476138108,0.));
#29876=DIRECTION('center_axis',(0.,0.,1.));
#29877=DIRECTION('ref_axis',(0.0895155307640188,0.995985426475727,0.));
#29878=DIRECTION('',(0.649652512346866,-0.760231289280706,0.));
#29879=DIRECTION('center_axis',(0.,0.,1.));
#29880=DIRECTION('ref_axis',(1.,0.,0.));
#29881=DIRECTION('',(-0.760231289280705,0.649652512346868,0.));
#29882=DIRECTION('center_axis',(0.,0.,1.));
#29883=DIRECTION('ref_axis',(-0.995985426475728,-0.0895155307640121,0.));
#29884=DIRECTION('center_axis',(0.,0.,1.));
#29885=DIRECTION('ref_axis',(0.760231289280704,-0.649652512346868,0.));
#29886=DIRECTION('center_axis',(0.,0.,1.));
#29887=DIRECTION('ref_axis',(-0.171314633997541,0.985216370234624,0.));
#29888=DIRECTION('',(0.824278476138107,-0.5661845933752,0.));
#29889=DIRECTION('center_axis',(0.,0.,1.));
#29890=DIRECTION('ref_axis',(1.,0.,0.));
#29891=DIRECTION('',(-0.902469479163338,0.430753803440728,0.));
#29892=DIRECTION('center_axis',(0.,0.,1.));
#29893=DIRECTION('ref_axis',(-0.93887972184625,-0.344245360035407,0.));
#29894=DIRECTION('center_axis',(0.,0.,1.));
#29895=DIRECTION('ref_axis',(0.902469479163338,-0.430753803440728,0.));
#29896=DIRECTION('center_axis',(0.,0.,1.));
#29897=DIRECTION('ref_axis',(-0.420469989562984,0.907306446509064,0.));
#29898=DIRECTION('',(0.942731223965123,-0.333553353095455,0.));
#29899=DIRECTION('center_axis',(0.,0.,1.));
#29900=DIRECTION('ref_axis',(1.,0.,0.));
#29901=DIRECTION('',(-0.983205865442321,0.182499934684419,0.));
#29902=DIRECTION('center_axis',(0.,0.,1.));
#29903=DIRECTION('ref_axis',(-0.817790915745045,-0.575515436912756,0.));
#29904=DIRECTION('center_axis',(0.,0.,1.));
#29905=DIRECTION('ref_axis',(0.983205865442321,-0.18249993468442,0.));
#29906=DIRECTION('center_axis',(0.,0.,1.));
#29907=DIRECTION('ref_axis',(-0.640971010199212,0.767565087848712,0.));
#29908=DIRECTION('',(0.996938396815926,-0.0781910030252328,0.));
#29909=DIRECTION('center_axis',(0.,0.,1.));
#29910=DIRECTION('ref_axis',(-0.640971010199212,0.767565087848712,0.));
#29911=DIRECTION('center_axis',(0.,0.,-1.));
#29912=DIRECTION('ref_axis',(-0.640971010199212,0.767565087848712,0.));
#29913=DIRECTION('',(0.,0.,1.));
#29914=DIRECTION('',(0.,0.,-1.));
#29915=DIRECTION('center_axis',(0.0781910030252328,0.996938396815926,0.));
#29916=DIRECTION('ref_axis',(-0.996938396815926,0.0781910030252328,0.));
#29917=DIRECTION('',(-0.996938396815926,0.0781910030252328,0.));
#29918=DIRECTION('',(0.,0.,1.));
#29919=DIRECTION('center_axis',(0.,0.,1.));
#29920=DIRECTION('ref_axis',(-0.817790915745045,-0.575515436912756,0.));
#29921=DIRECTION('center_axis',(0.,0.,-1.));
#29922=DIRECTION('ref_axis',(-0.817790915745045,-0.575515436912756,0.));
#29923=DIRECTION('',(0.,0.,1.));
#29924=DIRECTION('',(0.,0.,-1.));
#29925=DIRECTION('center_axis',(0.,0.,1.));
#29926=DIRECTION('ref_axis',(0.983205865442321,-0.18249993468442,0.));
#29927=DIRECTION('center_axis',(0.,0.,-1.));
#29928=DIRECTION('ref_axis',(0.983205865442321,-0.18249993468442,0.));
#29929=DIRECTION('center_axis',(0.,0.,1.));
#29930=DIRECTION('ref_axis',(-0.420469989562984,0.907306446509064,0.));
#29931=DIRECTION('center_axis',(0.,0.,-1.));
#29932=DIRECTION('ref_axis',(-0.420469989562984,0.907306446509064,0.));
#29933=DIRECTION('',(0.,0.,1.));
#29934=DIRECTION('',(0.,0.,-1.));
#29935=DIRECTION('center_axis',(0.333553353095455,0.942731223965123,0.));
#29936=DIRECTION('ref_axis',(-0.942731223965123,0.333553353095455,0.));
#29937=DIRECTION('',(-0.942731223965123,0.333553353095455,0.));
#29938=DIRECTION('',(0.,0.,1.));
#29939=DIRECTION('center_axis',(0.,0.,1.));
#29940=DIRECTION('ref_axis',(-0.93887972184625,-0.344245360035407,0.));
#29941=DIRECTION('center_axis',(0.,0.,-1.));
#29942=DIRECTION('ref_axis',(-0.93887972184625,-0.344245360035407,0.));
#29943=DIRECTION('',(0.,0.,1.));
#29944=DIRECTION('',(0.,0.,-1.));
#29945=DIRECTION('center_axis',(0.,0.,1.));
#29946=DIRECTION('ref_axis',(0.902469479163338,-0.430753803440728,0.));
#29947=DIRECTION('center_axis',(0.,0.,-1.));
#29948=DIRECTION('ref_axis',(0.902469479163338,-0.430753803440728,0.));
#29949=DIRECTION('center_axis',(0.,0.,1.));
#29950=DIRECTION('ref_axis',(-0.171314633997541,0.985216370234624,0.));
#29951=DIRECTION('center_axis',(0.,0.,-1.));
#29952=DIRECTION('ref_axis',(-0.171314633997541,0.985216370234624,0.));
#29953=DIRECTION('',(0.,0.,1.));
#29954=DIRECTION('',(0.,0.,-1.));
#29955=DIRECTION('center_axis',(0.5661845933752,0.824278476138107,0.));
#29956=DIRECTION('ref_axis',(-0.824278476138107,0.5661845933752,0.));
#29957=DIRECTION('',(-0.824278476138107,0.5661845933752,0.));
#29958=DIRECTION('',(0.,0.,1.));
#29959=DIRECTION('center_axis',(0.,0.,1.));
#29960=DIRECTION('ref_axis',(-0.995985426475728,-0.0895155307640121,0.));
#29961=DIRECTION('center_axis',(0.,0.,-1.));
#29962=DIRECTION('ref_axis',(-0.995985426475728,-0.0895155307640121,0.));
#29963=DIRECTION('',(0.,0.,1.));
#29964=DIRECTION('',(0.,0.,-1.));
#29965=DIRECTION('center_axis',(0.,0.,1.));
#29966=DIRECTION('ref_axis',(0.760231289280704,-0.649652512346868,0.));
#29967=DIRECTION('center_axis',(0.,0.,-1.));
#29968=DIRECTION('ref_axis',(0.760231289280704,-0.649652512346868,0.));
#29969=DIRECTION('center_axis',(0.,0.,1.));
#29970=DIRECTION('ref_axis',(0.0895155307640188,0.995985426475727,0.));
#29971=DIRECTION('center_axis',(0.,0.,-1.));
#29972=DIRECTION('ref_axis',(0.0895155307640188,0.995985426475727,0.));
#29973=DIRECTION('',(0.,0.,1.));
#29974=DIRECTION('',(0.,0.,-1.));
#29975=DIRECTION('center_axis',(0.760231289280706,0.649652512346866,0.));
#29976=DIRECTION('ref_axis',(-0.649652512346866,0.760231289280706,0.));
#29977=DIRECTION('',(-0.649652512346866,0.760231289280706,0.));
#29978=DIRECTION('',(0.,0.,1.));
#29979=DIRECTION('center_axis',(0.,0.,1.));
#29980=DIRECTION('ref_axis',(-0.985216370234624,0.171314633997541,0.));
#29981=DIRECTION('center_axis',(0.,0.,-1.));
#29982=DIRECTION('ref_axis',(-0.985216370234624,0.171314633997541,0.));
#29983=DIRECTION('',(0.,0.,1.));
#29984=DIRECTION('',(0.,0.,-1.));
#29985=DIRECTION('center_axis',(0.,0.,1.));
#29986=DIRECTION('ref_axis',(0.566184593375197,-0.824278476138108,0.));
#29987=DIRECTION('center_axis',(0.,0.,-1.));
#29988=DIRECTION('ref_axis',(0.566184593375197,-0.824278476138108,0.));
#29989=DIRECTION('center_axis',(0.,0.,1.));
#29990=DIRECTION('ref_axis',(0.344245360035407,0.938879721846251,0.));
#29991=DIRECTION('center_axis',(0.,0.,-1.));
#29992=DIRECTION('ref_axis',(0.344245360035407,0.938879721846251,0.));
#29993=DIRECTION('',(0.,0.,1.));
#29994=DIRECTION('',(0.,0.,-1.));
#29995=DIRECTION('center_axis',(0.902469479163339,0.430753803440726,0.));
#29996=DIRECTION('ref_axis',(-0.430753803440726,0.902469479163339,0.));
#29997=DIRECTION('',(-0.430753803440726,0.902469479163339,0.));
#29998=DIRECTION('',(0.,0.,1.));
#29999=DIRECTION('center_axis',(0.,0.,1.));
#30000=DIRECTION('ref_axis',(-0.907306446509064,0.420469989562983,0.));
#30001=DIRECTION('center_axis',(0.,0.,-1.));
#30002=DIRECTION('ref_axis',(-0.907306446509064,0.420469989562983,0.));
#30003=DIRECTION('',(0.,0.,1.));
#30004=DIRECTION('',(0.,0.,-1.));
#30005=DIRECTION('center_axis',(0.,0.,1.));
#30006=DIRECTION('ref_axis',(0.333553353095452,-0.942731223965124,0.));
#30007=DIRECTION('center_axis',(0.,0.,-1.));
#30008=DIRECTION('ref_axis',(0.333553353095452,-0.942731223965124,0.));
#30009=DIRECTION('center_axis',(0.,0.,1.));
#30010=DIRECTION('ref_axis',(0.575515436912747,0.817790915745051,0.));
#30011=DIRECTION('center_axis',(0.,0.,-1.));
#30012=DIRECTION('ref_axis',(0.575515436912747,0.817790915745051,0.));
#30013=DIRECTION('',(0.,0.,1.));
#30014=DIRECTION('',(0.,0.,-1.));
#30015=DIRECTION('center_axis',(0.983205865442321,0.182499934684417,0.));
#30016=DIRECTION('ref_axis',(-0.182499934684417,0.983205865442321,0.));
#30017=DIRECTION('',(-0.182499934684417,0.983205865442321,0.));
#30018=DIRECTION('',(0.,0.,1.));
#30019=DIRECTION('center_axis',(0.,0.,1.));
#30020=DIRECTION('ref_axis',(-0.767565087848714,0.64097101019921,0.));
#30021=DIRECTION('center_axis',(0.,0.,-1.));
#30022=DIRECTION('ref_axis',(-0.767565087848714,0.64097101019921,0.));
#30023=DIRECTION('',(0.,0.,1.));
#30024=DIRECTION('',(0.,0.,-1.));
#30025=DIRECTION('center_axis',(0.,0.,1.));
#30026=DIRECTION('ref_axis',(0.07819100302523,-0.996938396815926,0.));
#30027=DIRECTION('center_axis',(0.,0.,-1.));
#30028=DIRECTION('ref_axis',(0.07819100302523,-0.996938396815926,0.));
#30029=DIRECTION('center_axis',(0.,0.,1.));
#30030=DIRECTION('ref_axis',(0.767565087848712,0.640971010199212,0.));
#30031=DIRECTION('center_axis',(0.,0.,-1.));
#30032=DIRECTION('ref_axis',(0.767565087848712,0.640971010199212,0.));
#30033=DIRECTION('',(0.,0.,1.));
#30034=DIRECTION('',(0.,0.,-1.));
#30035=DIRECTION('center_axis',(0.996938396815926,-0.0781910030252327,0.));
#30036=DIRECTION('ref_axis',(0.0781910030252327,0.996938396815926,0.));
#30037=DIRECTION('',(0.0781910030252327,0.996938396815926,0.));
#30038=DIRECTION('',(0.,0.,1.));
#30039=DIRECTION('center_axis',(0.,0.,1.));
#30040=DIRECTION('ref_axis',(-0.575515436912756,0.817790915745045,0.));
#30041=DIRECTION('center_axis',(0.,0.,-1.));
#30042=DIRECTION('ref_axis',(-0.575515436912756,0.817790915745045,0.));
#30043=DIRECTION('',(0.,0.,1.));
#30044=DIRECTION('',(0.,0.,-1.));
#30045=DIRECTION('center_axis',(0.,0.,1.));
#30046=DIRECTION('ref_axis',(-0.18249993468442,-0.983205865442321,0.));
#30047=DIRECTION('center_axis',(0.,0.,-1.));
#30048=DIRECTION('ref_axis',(-0.18249993468442,-0.983205865442321,0.));
#30049=DIRECTION('center_axis',(0.,0.,1.));
#30050=DIRECTION('ref_axis',(0.907306446509064,0.420469989562984,0.));
#30051=DIRECTION('center_axis',(0.,0.,-1.));
#30052=DIRECTION('ref_axis',(0.907306446509064,0.420469989562984,0.));
#30053=DIRECTION('',(0.,0.,1.));
#30054=DIRECTION('',(0.,0.,-1.));
#30055=DIRECTION('center_axis',(0.942731223965123,-0.333553353095455,0.));
#30056=DIRECTION('ref_axis',(0.333553353095455,0.942731223965123,0.));
#30057=DIRECTION('',(0.333553353095455,0.942731223965123,0.));
#30058=DIRECTION('',(0.,0.,1.));
#30059=DIRECTION('center_axis',(0.,0.,1.));
#30060=DIRECTION('ref_axis',(-0.344245360035407,0.93887972184625,0.));
#30061=DIRECTION('center_axis',(0.,0.,-1.));
#30062=DIRECTION('ref_axis',(-0.344245360035407,0.93887972184625,0.));
#30063=DIRECTION('',(0.,0.,1.));
#30064=DIRECTION('',(0.,0.,-1.));
#30065=DIRECTION('center_axis',(0.,0.,1.));
#30066=DIRECTION('ref_axis',(-0.430753803440728,-0.902469479163338,0.));
#30067=DIRECTION('center_axis',(0.,0.,-1.));
#30068=DIRECTION('ref_axis',(-0.430753803440728,-0.902469479163338,0.));
#30069=DIRECTION('center_axis',(0.,0.,1.));
#30070=DIRECTION('ref_axis',(0.985216370234623,0.171314633997547,0.));
#30071=DIRECTION('center_axis',(0.,0.,-1.));
#30072=DIRECTION('ref_axis',(0.985216370234623,0.171314633997547,0.));
#30073=DIRECTION('',(0.,0.,1.));
#30074=DIRECTION('',(0.,0.,-1.));
#30075=DIRECTION('center_axis',(0.824278476138107,-0.5661845933752,0.));
#30076=DIRECTION('ref_axis',(0.5661845933752,0.824278476138107,0.));
#30077=DIRECTION('',(0.5661845933752,0.824278476138107,0.));
#30078=DIRECTION('',(0.,0.,1.));
#30079=DIRECTION('center_axis',(0.,0.,1.));
#30080=DIRECTION('ref_axis',(-0.0895155307640188,0.995985426475727,0.));
#30081=DIRECTION('center_axis',(0.,0.,-1.));
#30082=DIRECTION('ref_axis',(-0.0895155307640188,0.995985426475727,0.));
#30083=DIRECTION('',(0.,0.,1.));
#30084=DIRECTION('',(0.,0.,-1.));
#30085=DIRECTION('center_axis',(0.,0.,1.));
#30086=DIRECTION('ref_axis',(-0.649652512346869,-0.760231289280704,0.));
#30087=DIRECTION('center_axis',(0.,0.,-1.));
#30088=DIRECTION('ref_axis',(-0.649652512346869,-0.760231289280704,0.));
#30089=DIRECTION('center_axis',(0.,0.,1.));
#30090=DIRECTION('ref_axis',(0.995985426475728,-0.0895155307640127,0.));
#30091=DIRECTION('center_axis',(0.,0.,-1.));
#30092=DIRECTION('ref_axis',(0.995985426475728,-0.0895155307640127,0.));
#30093=DIRECTION('',(0.,0.,1.));
#30094=DIRECTION('',(0.,0.,-1.));
#30095=DIRECTION('center_axis',(0.649652512346867,-0.760231289280706,0.));
#30096=DIRECTION('ref_axis',(0.760231289280706,0.649652512346867,0.));
#30097=DIRECTION('',(0.760231289280706,0.649652512346867,0.));
#30098=DIRECTION('',(0.,0.,1.));
#30099=DIRECTION('center_axis',(0.,0.,1.));
#30100=DIRECTION('ref_axis',(0.17131463399754,0.985216370234625,0.));
#30101=DIRECTION('center_axis',(0.,0.,-1.));
#30102=DIRECTION('ref_axis',(0.17131463399754,0.985216370234625,0.));
#30103=DIRECTION('',(0.,0.,1.));
#30104=DIRECTION('',(0.,0.,-1.));
#30105=DIRECTION('center_axis',(0.,0.,1.));
#30106=DIRECTION('ref_axis',(-0.824278476138108,-0.566184593375198,0.));
#30107=DIRECTION('center_axis',(0.,0.,-1.));
#30108=DIRECTION('ref_axis',(-0.824278476138108,-0.566184593375198,0.));
#30109=DIRECTION('center_axis',(0.,0.,1.));
#30110=DIRECTION('ref_axis',(0.93887972184625,-0.344245360035407,0.));
#30111=DIRECTION('center_axis',(0.,0.,-1.));
#30112=DIRECTION('ref_axis',(0.93887972184625,-0.344245360035407,0.));
#30113=DIRECTION('',(0.,0.,1.));
#30114=DIRECTION('',(0.,0.,-1.));
#30115=DIRECTION('center_axis',(0.430753803440726,-0.902469479163339,0.));
#30116=DIRECTION('ref_axis',(0.902469479163339,0.430753803440726,0.));
#30117=DIRECTION('',(0.902469479163339,0.430753803440726,0.));
#30118=DIRECTION('',(0.,0.,1.));
#30119=DIRECTION('center_axis',(0.,0.,1.));
#30120=DIRECTION('ref_axis',(0.420469989562982,0.907306446509065,0.));
#30121=DIRECTION('center_axis',(0.,0.,-1.));
#30122=DIRECTION('ref_axis',(0.420469989562982,0.907306446509065,0.));
#30123=DIRECTION('',(0.,0.,1.));
#30124=DIRECTION('',(0.,0.,-1.));
#30125=DIRECTION('center_axis',(0.,0.,1.));
#30126=DIRECTION('ref_axis',(-0.942731223965124,-0.333553353095452,0.));
#30127=DIRECTION('center_axis',(0.,0.,-1.));
#30128=DIRECTION('ref_axis',(-0.942731223965124,-0.333553353095452,0.));
#30129=DIRECTION('center_axis',(0.,0.,1.));
#30130=DIRECTION('ref_axis',(0.817790915745051,-0.575515436912747,0.));
#30131=DIRECTION('center_axis',(0.,0.,-1.));
#30132=DIRECTION('ref_axis',(0.817790915745051,-0.575515436912747,0.));
#30133=DIRECTION('',(0.,0.,1.));
#30134=DIRECTION('',(0.,0.,-1.));
#30135=DIRECTION('center_axis',(0.182499934684417,-0.983205865442321,0.));
#30136=DIRECTION('ref_axis',(0.983205865442321,0.182499934684417,0.));
#30137=DIRECTION('',(0.983205865442321,0.182499934684417,0.));
#30138=DIRECTION('',(0.,0.,1.));
#30139=DIRECTION('center_axis',(0.,0.,1.));
#30140=DIRECTION('ref_axis',(0.64097101019921,0.767565087848714,0.));
#30141=DIRECTION('center_axis',(0.,0.,-1.));
#30142=DIRECTION('ref_axis',(0.64097101019921,0.767565087848714,0.));
#30143=DIRECTION('',(0.,0.,1.));
#30144=DIRECTION('',(0.,0.,-1.));
#30145=DIRECTION('center_axis',(0.,0.,1.));
#30146=DIRECTION('ref_axis',(-0.996938396815926,-0.07819100302523,0.));
#30147=DIRECTION('center_axis',(0.,0.,-1.));
#30148=DIRECTION('ref_axis',(-0.996938396815926,-0.07819100302523,0.));
#30149=DIRECTION('center_axis',(0.,0.,1.));
#30150=DIRECTION('ref_axis',(0.640971010199219,-0.767565087848706,0.));
#30151=DIRECTION('center_axis',(0.,0.,-1.));
#30152=DIRECTION('ref_axis',(0.640971010199219,-0.767565087848706,0.));
#30153=DIRECTION('',(0.,0.,1.));
#30154=DIRECTION('',(0.,0.,-1.));
#30155=DIRECTION('center_axis',(-0.0781910030252323,-0.996938396815926,
0.));
#30156=DIRECTION('ref_axis',(0.996938396815926,-0.0781910030252323,0.));
#30157=DIRECTION('',(0.996938396815926,-0.0781910030252323,0.));
#30158=DIRECTION('',(0.,0.,1.));
#30159=DIRECTION('center_axis',(0.,0.,1.));
#30160=DIRECTION('ref_axis',(0.817790915745049,0.57551543691275,0.));
#30161=DIRECTION('center_axis',(0.,0.,-1.));
#30162=DIRECTION('ref_axis',(0.817790915745049,0.57551543691275,0.));
#30163=DIRECTION('',(0.,0.,1.));
#30164=DIRECTION('',(0.,0.,-1.));
#30165=DIRECTION('center_axis',(0.,0.,1.));
#30166=DIRECTION('ref_axis',(-0.983205865442321,0.18249993468442,0.));
#30167=DIRECTION('center_axis',(0.,0.,-1.));
#30168=DIRECTION('ref_axis',(-0.983205865442321,0.18249993468442,0.));
#30169=DIRECTION('center_axis',(0.,0.,1.));
#30170=DIRECTION('ref_axis',(0.420469989562984,-0.907306446509064,0.));
#30171=DIRECTION('center_axis',(0.,0.,-1.));
#30172=DIRECTION('ref_axis',(0.420469989562984,-0.907306446509064,0.));
#30173=DIRECTION('',(0.,0.,1.));
#30174=DIRECTION('',(0.,0.,-1.));
#30175=DIRECTION('center_axis',(-0.333553353095454,-0.942731223965123,0.));
#30176=DIRECTION('ref_axis',(0.942731223965123,-0.333553353095454,0.));
#30177=DIRECTION('',(0.942731223965123,-0.333553353095454,0.));
#30178=DIRECTION('',(0.,0.,1.));
#30179=DIRECTION('center_axis',(0.,0.,1.));
#30180=DIRECTION('ref_axis',(0.93887972184625,0.344245360035408,0.));
#30181=DIRECTION('center_axis',(0.,0.,-1.));
#30182=DIRECTION('ref_axis',(0.93887972184625,0.344245360035408,0.));
#30183=DIRECTION('',(0.,0.,1.));
#30184=DIRECTION('',(0.,0.,-1.));
#30185=DIRECTION('center_axis',(0.,0.,1.));
#30186=DIRECTION('ref_axis',(-0.902469479163338,0.430753803440728,0.));
#30187=DIRECTION('center_axis',(0.,0.,-1.));
#30188=DIRECTION('ref_axis',(-0.902469479163338,0.430753803440728,0.));
#30189=DIRECTION('center_axis',(0.,0.,1.));
#30190=DIRECTION('ref_axis',(0.171314633997546,-0.985216370234624,0.));
#30191=DIRECTION('center_axis',(0.,0.,-1.));
#30192=DIRECTION('ref_axis',(0.171314633997546,-0.985216370234624,0.));
#30193=DIRECTION('',(0.,0.,1.));
#30194=DIRECTION('',(0.,0.,-1.));
#30195=DIRECTION('center_axis',(-0.5661845933752,-0.824278476138107,0.));
#30196=DIRECTION('ref_axis',(0.824278476138107,-0.5661845933752,0.));
#30197=DIRECTION('',(0.824278476138107,-0.5661845933752,0.));
#30198=DIRECTION('',(0.,0.,1.));
#30199=DIRECTION('center_axis',(0.,0.,1.));
#30200=DIRECTION('ref_axis',(0.995985426475728,0.0895155307640127,0.));
#30201=DIRECTION('center_axis',(0.,0.,-1.));
#30202=DIRECTION('ref_axis',(0.995985426475728,0.0895155307640127,0.));
#30203=DIRECTION('',(0.,0.,1.));
#30204=DIRECTION('',(0.,0.,-1.));
#30205=DIRECTION('center_axis',(0.,0.,1.));
#30206=DIRECTION('ref_axis',(-0.760231289280704,0.649652512346868,0.));
#30207=DIRECTION('center_axis',(0.,0.,-1.));
#30208=DIRECTION('ref_axis',(-0.760231289280704,0.649652512346868,0.));
#30209=DIRECTION('center_axis',(0.,0.,1.));
#30210=DIRECTION('ref_axis',(-0.0895155307640188,-0.995985426475727,0.));
#30211=DIRECTION('center_axis',(0.,0.,-1.));
#30212=DIRECTION('ref_axis',(-0.0895155307640188,-0.995985426475727,0.));
#30213=DIRECTION('',(0.,0.,1.));
#30214=DIRECTION('',(0.,0.,-1.));
#30215=DIRECTION('center_axis',(-0.760231289280706,-0.649652512346867,0.));
#30216=DIRECTION('ref_axis',(0.649652512346867,-0.760231289280706,0.));
#30217=DIRECTION('',(0.649652512346867,-0.760231289280706,0.));
#30218=DIRECTION('',(0.,0.,1.));
#30219=DIRECTION('center_axis',(0.,0.,1.));
#30220=DIRECTION('ref_axis',(0.985216370234623,-0.171314633997547,0.));
#30221=DIRECTION('center_axis',(0.,0.,-1.));
#30222=DIRECTION('ref_axis',(0.985216370234623,-0.171314633997547,0.));
#30223=DIRECTION('',(0.,0.,1.));
#30224=DIRECTION('',(0.,0.,-1.));
#30225=DIRECTION('center_axis',(0.,0.,1.));
#30226=DIRECTION('ref_axis',(-0.566184593375198,0.824278476138108,0.));
#30227=DIRECTION('center_axis',(0.,0.,-1.));
#30228=DIRECTION('ref_axis',(-0.566184593375198,0.824278476138108,0.));
#30229=DIRECTION('center_axis',(0.,0.,1.));
#30230=DIRECTION('ref_axis',(-0.34424536003541,-0.93887972184625,0.));
#30231=DIRECTION('center_axis',(0.,0.,-1.));
#30232=DIRECTION('ref_axis',(-0.34424536003541,-0.93887972184625,0.));
#30233=DIRECTION('',(0.,0.,1.));
#30234=DIRECTION('',(0.,0.,-1.));
#30235=DIRECTION('center_axis',(-0.902469479163339,-0.430753803440726,0.));
#30236=DIRECTION('ref_axis',(0.430753803440726,-0.902469479163339,0.));
#30237=DIRECTION('',(0.430753803440726,-0.902469479163339,0.));
#30238=DIRECTION('',(0.,0.,1.));
#30239=DIRECTION('center_axis',(0.,0.,1.));
#30240=DIRECTION('ref_axis',(0.907306446509069,-0.420469989562973,0.));
#30241=DIRECTION('center_axis',(0.,0.,-1.));
#30242=DIRECTION('ref_axis',(0.907306446509069,-0.420469989562973,0.));
#30243=DIRECTION('',(0.,0.,1.));
#30244=DIRECTION('',(0.,0.,-1.));
#30245=DIRECTION('center_axis',(0.,0.,1.));
#30246=DIRECTION('ref_axis',(-0.333553353095452,0.942731223965124,0.));
#30247=DIRECTION('center_axis',(0.,0.,-1.));
#30248=DIRECTION('ref_axis',(-0.333553353095452,0.942731223965124,0.));
#30249=DIRECTION('center_axis',(0.,0.,1.));
#30250=DIRECTION('ref_axis',(-0.575515436912748,-0.817790915745051,0.));
#30251=DIRECTION('center_axis',(0.,0.,-1.));
#30252=DIRECTION('ref_axis',(-0.575515436912748,-0.817790915745051,0.));
#30253=DIRECTION('',(0.,0.,1.));
#30254=DIRECTION('',(0.,0.,-1.));
#30255=DIRECTION('center_axis',(-0.983205865442321,-0.182499934684418,0.));
#30256=DIRECTION('ref_axis',(0.182499934684418,-0.983205865442321,0.));
#30257=DIRECTION('',(0.182499934684418,-0.983205865442321,0.));
#30258=DIRECTION('',(0.,0.,1.));
#30259=DIRECTION('center_axis',(0.,0.,1.));
#30260=DIRECTION('ref_axis',(0.767565087848708,-0.640971010199218,0.));
#30261=DIRECTION('center_axis',(0.,0.,-1.));
#30262=DIRECTION('ref_axis',(0.767565087848708,-0.640971010199218,0.));
#30263=DIRECTION('',(0.,0.,1.));
#30264=DIRECTION('',(0.,0.,-1.));
#30265=DIRECTION('center_axis',(0.,0.,1.));
#30266=DIRECTION('ref_axis',(-0.0781910030252301,0.996938396815926,0.));
#30267=DIRECTION('center_axis',(0.,0.,-1.));
#30268=DIRECTION('ref_axis',(-0.0781910030252301,0.996938396815926,0.));
#30269=DIRECTION('center_axis',(0.,0.,1.));
#30270=DIRECTION('ref_axis',(-0.767565087848706,-0.640971010199219,0.));
#30271=DIRECTION('center_axis',(0.,0.,-1.));
#30272=DIRECTION('ref_axis',(-0.767565087848706,-0.640971010199219,0.));
#30273=DIRECTION('',(0.,0.,1.));
#30274=DIRECTION('',(0.,0.,-1.));
#30275=DIRECTION('center_axis',(-0.996938396815926,0.0781910030252323,0.));
#30276=DIRECTION('ref_axis',(-0.0781910030252323,-0.996938396815926,0.));
#30277=DIRECTION('',(-0.0781910030252323,-0.996938396815926,0.));
#30278=DIRECTION('',(0.,0.,1.));
#30279=DIRECTION('center_axis',(0.,0.,1.));
#30280=DIRECTION('ref_axis',(0.57551543691275,-0.817790915745049,0.));
#30281=DIRECTION('center_axis',(0.,0.,-1.));
#30282=DIRECTION('ref_axis',(0.57551543691275,-0.817790915745049,0.));
#30283=DIRECTION('',(0.,0.,1.));
#30284=DIRECTION('',(0.,0.,-1.));
#30285=DIRECTION('center_axis',(0.,0.,1.));
#30286=DIRECTION('ref_axis',(0.18249993468442,0.983205865442321,0.));
#30287=DIRECTION('center_axis',(0.,0.,-1.));
#30288=DIRECTION('ref_axis',(0.18249993468442,0.983205865442321,0.));
#30289=DIRECTION('center_axis',(0.,0.,1.));
#30290=DIRECTION('ref_axis',(-0.907306446509064,-0.420469989562983,0.));
#30291=DIRECTION('center_axis',(0.,0.,-1.));
#30292=DIRECTION('ref_axis',(-0.907306446509064,-0.420469989562983,0.));
#30293=DIRECTION('',(0.,0.,1.));
#30294=DIRECTION('',(0.,0.,-1.));
#30295=DIRECTION('center_axis',(-0.942731223965123,0.333553353095454,0.));
#30296=DIRECTION('ref_axis',(-0.333553353095454,-0.942731223965123,0.));
#30297=DIRECTION('',(-0.333553353095454,-0.942731223965123,0.));
#30298=DIRECTION('',(0.,0.,1.));
#30299=DIRECTION('center_axis',(0.,0.,1.));
#30300=DIRECTION('ref_axis',(0.344245360035413,-0.938879721846248,0.));
#30301=DIRECTION('center_axis',(0.,0.,-1.));
#30302=DIRECTION('ref_axis',(0.344245360035413,-0.938879721846248,0.));
#30303=DIRECTION('',(0.,0.,1.));
#30304=DIRECTION('',(0.,0.,-1.));
#30305=DIRECTION('center_axis',(0.,0.,1.));
#30306=DIRECTION('ref_axis',(0.430753803440728,0.902469479163338,0.));
#30307=DIRECTION('center_axis',(0.,0.,-1.));
#30308=DIRECTION('ref_axis',(0.430753803440728,0.902469479163338,0.));
#30309=DIRECTION('center_axis',(0.,0.,1.));
#30310=DIRECTION('ref_axis',(-0.985216370234624,-0.171314633997546,0.));
#30311=DIRECTION('center_axis',(0.,0.,-1.));
#30312=DIRECTION('ref_axis',(-0.985216370234624,-0.171314633997546,0.));
#30313=DIRECTION('',(0.,0.,1.));
#30314=DIRECTION('',(0.,0.,-1.));
#30315=DIRECTION('center_axis',(-0.824278476138107,0.5661845933752,0.));
#30316=DIRECTION('ref_axis',(-0.5661845933752,-0.824278476138107,0.));
#30317=DIRECTION('',(-0.5661845933752,-0.824278476138107,0.));
#30318=DIRECTION('',(0.,0.,1.));
#30319=DIRECTION('center_axis',(0.,0.,1.));
#30320=DIRECTION('ref_axis',(0.0895155307640121,-0.995985426475728,0.));
#30321=DIRECTION('center_axis',(0.,0.,-1.));
#30322=DIRECTION('ref_axis',(0.0895155307640121,-0.995985426475728,0.));
#30323=DIRECTION('',(0.,0.,1.));
#30324=DIRECTION('',(0.,0.,-1.));
#30325=DIRECTION('center_axis',(0.,0.,1.));
#30326=DIRECTION('ref_axis',(0.649652512346868,0.760231289280704,0.));
#30327=DIRECTION('center_axis',(0.,0.,-1.));
#30328=DIRECTION('ref_axis',(0.649652512346868,0.760231289280704,0.));
#30329=DIRECTION('center_axis',(0.,0.,1.));
#30330=DIRECTION('ref_axis',(-0.995985426475728,0.0895155307640127,0.));
#30331=DIRECTION('center_axis',(0.,0.,-1.));
#30332=DIRECTION('ref_axis',(-0.995985426475728,0.0895155307640127,0.));
#30333=DIRECTION('',(0.,0.,1.));
#30334=DIRECTION('',(0.,0.,-1.));
#30335=DIRECTION('center_axis',(-0.649652512346867,0.760231289280706,0.));
#30336=DIRECTION('ref_axis',(-0.760231289280706,-0.649652512346867,0.));
#30337=DIRECTION('',(-0.760231289280706,-0.649652512346867,0.));
#30338=DIRECTION('',(0.,0.,1.));
#30339=DIRECTION('center_axis',(0.,0.,1.));
#30340=DIRECTION('ref_axis',(-0.171314633997547,-0.985216370234623,0.));
#30341=DIRECTION('center_axis',(0.,0.,-1.));
#30342=DIRECTION('ref_axis',(-0.171314633997547,-0.985216370234623,0.));
#30343=DIRECTION('',(0.,0.,1.));
#30344=DIRECTION('',(0.,0.,-1.));
#30345=DIRECTION('center_axis',(0.,0.,1.));
#30346=DIRECTION('ref_axis',(0.824278476138108,0.566184593375198,0.));
#30347=DIRECTION('center_axis',(0.,0.,-1.));
#30348=DIRECTION('ref_axis',(0.824278476138108,0.566184593375198,0.));
#30349=DIRECTION('center_axis',(0.,0.,1.));
#30350=DIRECTION('ref_axis',(-0.93887972184625,0.34424536003541,0.));
#30351=DIRECTION('center_axis',(0.,0.,-1.));
#30352=DIRECTION('ref_axis',(-0.93887972184625,0.34424536003541,0.));
#30353=DIRECTION('',(0.,0.,1.));
#30354=DIRECTION('',(0.,0.,-1.));
#30355=DIRECTION('center_axis',(-0.430753803440726,0.902469479163339,0.));
#30356=DIRECTION('ref_axis',(-0.902469479163339,-0.430753803440726,0.));
#30357=DIRECTION('',(-0.902469479163339,-0.430753803440726,0.));
#30358=DIRECTION('',(0.,0.,1.));
#30359=DIRECTION('center_axis',(0.,0.,1.));
#30360=DIRECTION('ref_axis',(-0.420469989562974,-0.907306446509068,0.));
#30361=DIRECTION('center_axis',(0.,0.,-1.));
#30362=DIRECTION('ref_axis',(-0.420469989562974,-0.907306446509068,0.));
#30363=DIRECTION('',(0.,0.,1.));
#30364=DIRECTION('',(0.,0.,-1.));
#30365=DIRECTION('center_axis',(0.,0.,1.));
#30366=DIRECTION('ref_axis',(0.942731223965124,0.333553353095452,0.));
#30367=DIRECTION('center_axis',(0.,0.,-1.));
#30368=DIRECTION('ref_axis',(0.942731223965124,0.333553353095452,0.));
#30369=DIRECTION('center_axis',(-0.18249993468442,-0.983205865442321,0.));
#30370=DIRECTION('ref_axis',(0.983205865442321,-0.182499934684419,0.));
#30371=DIRECTION('',(0.,0.,1.));
#30372=DIRECTION('',(0.983205865442321,-0.182499934684419,0.));
#30373=DIRECTION('',(0.,0.,-1.));
#30374=DIRECTION('',(0.,0.,1.));
#30375=DIRECTION('center_axis',(-0.430753803440728,-0.902469479163338,0.));
#30376=DIRECTION('ref_axis',(0.902469479163338,-0.430753803440728,0.));
#30377=DIRECTION('',(0.,0.,1.));
#30378=DIRECTION('',(0.902469479163338,-0.430753803440728,0.));
#30379=DIRECTION('',(0.,0.,-1.));
#30380=DIRECTION('',(0.,0.,1.));
#30381=DIRECTION('center_axis',(-0.649652512346868,-0.760231289280705,0.));
#30382=DIRECTION('ref_axis',(0.760231289280705,-0.649652512346868,0.));
#30383=DIRECTION('',(0.,0.,1.));
#30384=DIRECTION('',(0.760231289280705,-0.649652512346868,0.));
#30385=DIRECTION('',(0.,0.,-1.));
#30386=DIRECTION('',(0.,0.,1.));
#30387=DIRECTION('center_axis',(-0.824278476138108,-0.566184593375198,0.));
#30388=DIRECTION('ref_axis',(0.566184593375198,-0.824278476138108,0.));
#30389=DIRECTION('',(0.,0.,1.));
#30390=DIRECTION('',(0.566184593375198,-0.824278476138108,0.));
#30391=DIRECTION('',(0.,0.,-1.));
#30392=DIRECTION('',(0.,0.,1.));
#30393=DIRECTION('center_axis',(-0.942731223965124,-0.333553353095453,0.));
#30394=DIRECTION('ref_axis',(0.333553353095453,-0.942731223965124,0.));
#30395=DIRECTION('',(0.,0.,1.));
#30396=DIRECTION('',(0.333553353095453,-0.942731223965124,0.));
#30397=DIRECTION('',(0.,0.,-1.));
#30398=DIRECTION('',(0.,0.,1.));
#30399=DIRECTION('center_axis',(-0.996938396815926,-0.0781910030252307,
0.));
#30400=DIRECTION('ref_axis',(0.0781910030252307,-0.996938396815926,0.));
#30401=DIRECTION('',(0.,0.,1.));
#30402=DIRECTION('',(0.0781910030252307,-0.996938396815926,0.));
#30403=DIRECTION('',(0.,0.,-1.));
#30404=DIRECTION('',(0.,0.,1.));
#30405=DIRECTION('center_axis',(-0.983205865442321,0.182499934684419,0.));
#30406=DIRECTION('ref_axis',(-0.182499934684419,-0.983205865442321,0.));
#30407=DIRECTION('',(0.,0.,1.));
#30408=DIRECTION('',(-0.182499934684419,-0.983205865442321,0.));
#30409=DIRECTION('',(0.,0.,-1.));
#30410=DIRECTION('',(0.,0.,1.));
#30411=DIRECTION('center_axis',(-0.902469479163338,0.430753803440728,0.));
#30412=DIRECTION('ref_axis',(-0.430753803440728,-0.902469479163338,0.));
#30413=DIRECTION('',(0.,0.,1.));
#30414=DIRECTION('',(-0.430753803440728,-0.902469479163338,0.));
#30415=DIRECTION('',(0.,0.,-1.));
#30416=DIRECTION('',(0.,0.,1.));
#30417=DIRECTION('center_axis',(-0.760231289280705,0.649652512346868,0.));
#30418=DIRECTION('ref_axis',(-0.649652512346868,-0.760231289280705,0.));
#30419=DIRECTION('',(0.,0.,1.));
#30420=DIRECTION('',(-0.649652512346868,-0.760231289280705,0.));
#30421=DIRECTION('',(0.,0.,-1.));
#30422=DIRECTION('',(0.,0.,1.));
#30423=DIRECTION('center_axis',(-0.566184593375199,0.824278476138108,0.));
#30424=DIRECTION('ref_axis',(-0.824278476138108,-0.566184593375198,0.));
#30425=DIRECTION('',(0.,0.,1.));
#30426=DIRECTION('',(-0.824278476138108,-0.566184593375198,0.));
#30427=DIRECTION('',(0.,0.,-1.));
#30428=DIRECTION('',(0.,0.,1.));
#30429=DIRECTION('center_axis',(-0.333553353095453,0.942731223965124,0.));
#30430=DIRECTION('ref_axis',(-0.942731223965124,-0.333553353095453,0.));
#30431=DIRECTION('',(0.,0.,1.));
#30432=DIRECTION('',(-0.942731223965124,-0.333553353095453,0.));
#30433=DIRECTION('',(0.,0.,-1.));
#30434=DIRECTION('',(0.,0.,1.));
#30435=DIRECTION('center_axis',(-0.0781910030252307,0.996938396815926,0.));
#30436=DIRECTION('ref_axis',(-0.996938396815926,-0.0781910030252307,0.));
#30437=DIRECTION('',(0.,0.,1.));
#30438=DIRECTION('',(-0.996938396815926,-0.0781910030252307,0.));
#30439=DIRECTION('',(0.,0.,-1.));
#30440=DIRECTION('',(0.,0.,1.));
#30441=DIRECTION('center_axis',(0.182499934684419,0.983205865442321,0.));
#30442=DIRECTION('ref_axis',(-0.983205865442321,0.182499934684419,0.));
#30443=DIRECTION('',(0.,0.,1.));
#30444=DIRECTION('',(-0.983205865442321,0.182499934684419,0.));
#30445=DIRECTION('',(0.,0.,-1.));
#30446=DIRECTION('',(0.,0.,1.));
#30447=DIRECTION('center_axis',(0.430753803440728,0.902469479163338,0.));
#30448=DIRECTION('ref_axis',(-0.902469479163338,0.430753803440727,0.));
#30449=DIRECTION('',(0.,0.,1.));
#30450=DIRECTION('',(-0.902469479163338,0.430753803440727,0.));
#30451=DIRECTION('',(0.,0.,-1.));
#30452=DIRECTION('',(0.,0.,1.));
#30453=DIRECTION('center_axis',(0.649652512346868,0.760231289280705,0.));
#30454=DIRECTION('ref_axis',(-0.760231289280705,0.649652512346868,0.));
#30455=DIRECTION('',(0.,0.,1.));
#30456=DIRECTION('',(-0.760231289280705,0.649652512346868,0.));
#30457=DIRECTION('',(0.,0.,-1.));
#30458=DIRECTION('',(0.,0.,1.));
#30459=DIRECTION('center_axis',(0.824278476138108,0.566184593375199,0.));
#30460=DIRECTION('ref_axis',(-0.566184593375199,0.824278476138108,0.));
#30461=DIRECTION('',(0.,0.,1.));
#30462=DIRECTION('',(-0.566184593375199,0.824278476138108,0.));
#30463=DIRECTION('',(0.,0.,-1.));
#30464=DIRECTION('',(0.,0.,1.));
#30465=DIRECTION('center_axis',(0.942731223965124,0.333553353095453,0.));
#30466=DIRECTION('ref_axis',(-0.333553353095453,0.942731223965124,0.));
#30467=DIRECTION('',(0.,0.,1.));
#30468=DIRECTION('',(-0.333553353095453,0.942731223965124,0.));
#30469=DIRECTION('',(0.,0.,-1.));
#30470=DIRECTION('',(0.,0.,1.));
#30471=DIRECTION('center_axis',(0.996938396815926,0.0781910030252308,0.));
#30472=DIRECTION('ref_axis',(-0.0781910030252308,0.996938396815926,0.));
#30473=DIRECTION('',(0.,0.,1.));
#30474=DIRECTION('',(-0.0781910030252308,0.996938396815926,0.));
#30475=DIRECTION('',(0.,0.,-1.));
#30476=DIRECTION('',(0.,0.,1.));
#30477=DIRECTION('center_axis',(0.983205865442321,-0.182499934684419,0.));
#30478=DIRECTION('ref_axis',(0.182499934684419,0.983205865442321,0.));
#30479=DIRECTION('',(0.,0.,1.));
#30480=DIRECTION('',(0.182499934684419,0.983205865442321,0.));
#30481=DIRECTION('',(0.,0.,-1.));
#30482=DIRECTION('',(0.,0.,1.));
#30483=DIRECTION('center_axis',(0.902469479163338,-0.430753803440727,0.));
#30484=DIRECTION('ref_axis',(0.430753803440727,0.902469479163338,0.));
#30485=DIRECTION('',(0.,0.,1.));
#30486=DIRECTION('',(0.430753803440727,0.902469479163338,0.));
#30487=DIRECTION('',(0.,0.,-1.));
#30488=DIRECTION('',(0.,0.,1.));
#30489=DIRECTION('center_axis',(0.760231289280705,-0.649652512346868,0.));
#30490=DIRECTION('ref_axis',(0.649652512346868,0.760231289280705,0.));
#30491=DIRECTION('',(0.,0.,1.));
#30492=DIRECTION('',(0.649652512346868,0.760231289280705,0.));
#30493=DIRECTION('',(0.,0.,-1.));
#30494=DIRECTION('',(0.,0.,1.));
#30495=DIRECTION('center_axis',(0.566184593375199,-0.824278476138108,0.));
#30496=DIRECTION('ref_axis',(0.824278476138108,0.566184593375199,0.));
#30497=DIRECTION('',(0.,0.,1.));
#30498=DIRECTION('',(0.824278476138108,0.566184593375199,0.));
#30499=DIRECTION('',(0.,0.,-1.));
#30500=DIRECTION('',(0.,0.,1.));
#30501=DIRECTION('center_axis',(0.333553353095453,-0.942731223965124,0.));
#30502=DIRECTION('ref_axis',(0.942731223965124,0.333553353095453,0.));
#30503=DIRECTION('',(0.,0.,1.));
#30504=DIRECTION('',(0.942731223965124,0.333553353095453,0.));
#30505=DIRECTION('',(0.,0.,-1.));
#30506=DIRECTION('',(0.,0.,1.));
#30507=DIRECTION('center_axis',(0.,0.,1.));
#30508=DIRECTION('ref_axis',(1.,0.,0.));
#30509=DIRECTION('center_axis',(0.,0.,1.));
#30510=DIRECTION('ref_axis',(1.,0.,0.));
#30511=DIRECTION('center_axis',(0.,0.,1.));
#30512=DIRECTION('ref_axis',(1.,0.,0.));
#30513=DIRECTION('center_axis',(0.,0.,1.));
#30514=DIRECTION('ref_axis',(1.,0.,0.));
#30515=DIRECTION('center_axis',(0.,0.,1.));
#30516=DIRECTION('ref_axis',(1.,0.,0.));
#30517=DIRECTION('center_axis',(0.,0.,1.));
#30518=DIRECTION('ref_axis',(1.,0.,0.));
#30519=DIRECTION('center_axis',(0.,0.,1.));
#30520=DIRECTION('ref_axis',(1.,0.,0.));
#30521=DIRECTION('center_axis',(0.,0.,1.));
#30522=DIRECTION('ref_axis',(1.,0.,0.));
#30523=DIRECTION('center_axis',(0.,0.,1.));
#30524=DIRECTION('ref_axis',(1.,0.,0.));
#30525=DIRECTION('center_axis',(0.,0.,1.));
#30526=DIRECTION('ref_axis',(1.,0.,0.));
#30527=DIRECTION('center_axis',(0.,0.,1.));
#30528=DIRECTION('ref_axis',(1.,0.,0.));
#30529=DIRECTION('center_axis',(0.,0.,1.));
#30530=DIRECTION('ref_axis',(1.,0.,0.));
#30531=DIRECTION('center_axis',(0.,0.,1.));
#30532=DIRECTION('ref_axis',(1.,0.,0.));
#30533=DIRECTION('center_axis',(0.,0.,1.));
#30534=DIRECTION('ref_axis',(1.,0.,0.));
#30535=DIRECTION('center_axis',(0.,0.,1.));
#30536=DIRECTION('ref_axis',(1.,0.,0.));
#30537=DIRECTION('center_axis',(0.,0.,1.));
#30538=DIRECTION('ref_axis',(1.,0.,0.));
#30539=DIRECTION('center_axis',(0.,0.,1.));
#30540=DIRECTION('ref_axis',(1.,0.,0.));
#30541=DIRECTION('center_axis',(0.,0.,1.));
#30542=DIRECTION('ref_axis',(1.,0.,0.));
#30543=DIRECTION('center_axis',(0.,0.,1.));
#30544=DIRECTION('ref_axis',(1.,0.,0.));
#30545=DIRECTION('center_axis',(0.,0.,1.));
#30546=DIRECTION('ref_axis',(1.,0.,0.));
#30547=DIRECTION('center_axis',(0.,0.,1.));
#30548=DIRECTION('ref_axis',(1.,0.,0.));
#30549=DIRECTION('center_axis',(0.,0.,1.));
#30550=DIRECTION('ref_axis',(1.,0.,0.));
#30551=DIRECTION('center_axis',(0.,0.,1.));
#30552=DIRECTION('ref_axis',(1.,0.,0.));
#30553=DIRECTION('center_axis',(0.,0.,1.));
#30554=DIRECTION('ref_axis',(1.,0.,0.));
#30555=DIRECTION('',(-0.983205865442321,-0.182499934684418,0.));
#30556=DIRECTION('center_axis',(0.,0.,-1.));
#30557=DIRECTION('ref_axis',(-0.817790915745051,0.575515436912748,0.));
#30558=DIRECTION('center_axis',(0.,0.,-1.));
#30559=DIRECTION('ref_axis',(0.996938396815926,0.0781910030252301,0.));
#30560=DIRECTION('center_axis',(0.,0.,-1.));
#30561=DIRECTION('ref_axis',(-0.640971010199219,-0.767565087848707,0.));
#30562=DIRECTION('',(0.996938396815926,0.0781910030252308,0.));
#30563=DIRECTION('center_axis',(0.,0.,1.));
#30564=DIRECTION('ref_axis',(1.,0.,0.));
#30565=DIRECTION('center_axis',(0.,0.,1.));
#30566=DIRECTION('ref_axis',(1.,0.,0.));
#30567=DIRECTION('',(0.,0.,-1.));
#30568=DIRECTION('center_axis',(0.,0.,1.));
#30569=DIRECTION('ref_axis',(1.,0.,0.));
#30570=DIRECTION('center_axis',(0.,0.,1.));
#30571=DIRECTION('ref_axis',(1.,0.,0.));
#30572=DIRECTION('center_axis',(0.,0.,1.));
#30573=DIRECTION('ref_axis',(1.,0.,0.));
#30574=DIRECTION('center_axis',(0.,0.,1.));
#30575=DIRECTION('ref_axis',(1.,0.,0.));
#30576=DIRECTION('center_axis',(0.,0.,1.));
#30577=DIRECTION('ref_axis',(1.,0.,0.));
#30578=DIRECTION('center_axis',(0.,0.,1.));
#30579=DIRECTION('ref_axis',(1.,0.,0.));
#30580=DIRECTION('center_axis',(0.,0.,1.));
#30581=DIRECTION('ref_axis',(1.,0.,0.));
#30582=DIRECTION('center_axis',(0.,0.,1.));
#30583=DIRECTION('ref_axis',(1.,0.,0.));
#30584=DIRECTION('center_axis',(0.,0.,1.));
#30585=DIRECTION('ref_axis',(1.,0.,0.));
#30586=DIRECTION('center_axis',(0.,0.,1.));
#30587=DIRECTION('ref_axis',(1.,0.,0.));
#30588=DIRECTION('center_axis',(0.,0.,1.));
#30589=DIRECTION('ref_axis',(-1.,-1.22464679914735E-16,0.));
#30590=DIRECTION('center_axis',(0.,0.,1.));
#30591=DIRECTION('ref_axis',(1.,0.,0.));
#30592=DIRECTION('center_axis',(0.,0.,1.));
#30593=DIRECTION('ref_axis',(1.,0.,0.));
#30594=DIRECTION('center_axis',(0.,0.,1.));
#30595=DIRECTION('ref_axis',(1.,0.,0.));
#30596=DIRECTION('center_axis',(0.,0.,1.));
#30597=DIRECTION('ref_axis',(1.,0.,0.));
#30598=DIRECTION('center_axis',(0.,0.,1.));
#30599=DIRECTION('ref_axis',(1.,0.,0.));
#30600=DIRECTION('center_axis',(0.,0.,1.));
#30601=DIRECTION('ref_axis',(1.,0.,0.));
#30602=DIRECTION('center_axis',(0.,0.,1.));
#30603=DIRECTION('ref_axis',(1.,0.,0.));
#30604=DIRECTION('center_axis',(0.,0.,1.));
#30605=DIRECTION('ref_axis',(1.,0.,0.));
#30606=DIRECTION('center_axis',(0.,0.,1.));
#30607=DIRECTION('ref_axis',(1.,0.,0.));
#30608=DIRECTION('center_axis',(0.,0.,1.));
#30609=DIRECTION('ref_axis',(1.,0.,0.));
#30610=DIRECTION('center_axis',(0.,0.,1.));
#30611=DIRECTION('ref_axis',(1.,0.,0.));
#30612=DIRECTION('center_axis',(0.,0.,1.));
#30613=DIRECTION('ref_axis',(-0.817790915745051,0.575515436912748,0.));
#30614=DIRECTION('',(0.,0.,1.));
#30615=DIRECTION('',(0.,0.,-1.));
#30616=DIRECTION('center_axis',(-0.182499934684418,0.983205865442321,0.));
#30617=DIRECTION('ref_axis',(-0.983205865442321,-0.182499934684418,0.));
#30618=DIRECTION('',(0.,0.,1.));
#30619=DIRECTION('center_axis',(0.,0.,1.));
#30620=DIRECTION('ref_axis',(-0.640971010199219,-0.767565087848707,0.));
#30621=DIRECTION('',(0.,0.,1.));
#30622=DIRECTION('',(0.,0.,-1.));
#30623=DIRECTION('center_axis',(0.,0.,1.));
#30624=DIRECTION('ref_axis',(0.996938396815926,0.0781910030252301,0.));
#30625=DIRECTION('center_axis',(0.0781910030252308,-0.996938396815926,0.));
#30626=DIRECTION('ref_axis',(0.996938396815926,0.0781910030252308,0.));
#30627=DIRECTION('',(0.,0.,1.));
#30628=DIRECTION('',(0.,0.,1.));
#30629=DIRECTION('center_axis',(0.,0.,1.));
#30630=DIRECTION('ref_axis',(1.,0.,0.));
#30631=DIRECTION('axis',(0.,0.,1.));
#30632=DIRECTION('refdir',(1.,0.,0.));
#30633=DIRECTION('center_axis',(0.,0.,1.));
#30634=DIRECTION('ref_axis',(-0.640971010199212,0.767565087848712,0.));
#30635=DIRECTION('center_axis',(0.,0.,-1.));
#30636=DIRECTION('ref_axis',(-0.640971010199212,0.767565087848712,0.));
#30637=DIRECTION('',(0.,0.,1.));
#30638=DIRECTION('center_axis',(0.,0.,1.));
#30639=DIRECTION('ref_axis',(-0.640971010199212,0.767565087848712,0.));
#30640=DIRECTION('',(0.,0.,-1.));
#30641=DIRECTION('center_axis',(0.0781910030252328,0.996938396815926,0.));
#30642=DIRECTION('ref_axis',(-0.996938396815926,0.0781910030252328,0.));
#30643=DIRECTION('',(-0.996938396815926,0.0781910030252328,0.));
#30644=DIRECTION('',(0.,0.,1.));
#30645=DIRECTION('',(0.996938396815926,-0.0781910030252328,0.));
#30646=DIRECTION('center_axis',(0.,0.,1.));
#30647=DIRECTION('ref_axis',(-0.817790915745045,-0.575515436912756,0.));
#30648=DIRECTION('center_axis',(0.,0.,-1.));
#30649=DIRECTION('ref_axis',(-0.817790915745045,-0.575515436912756,0.));
#30650=DIRECTION('',(0.,0.,1.));
#30651=DIRECTION('center_axis',(0.,0.,1.));
#30652=DIRECTION('ref_axis',(-0.817790915745045,-0.575515436912756,0.));
#30653=DIRECTION('',(0.,0.,-1.));
#30654=DIRECTION('center_axis',(0.,0.,1.));
#30655=DIRECTION('ref_axis',(0.983205865442321,-0.18249993468442,0.));
#30656=DIRECTION('center_axis',(0.,0.,1.));
#30657=DIRECTION('ref_axis',(0.983205865442321,-0.18249993468442,0.));
#30658=DIRECTION('center_axis',(0.,0.,-1.));
#30659=DIRECTION('ref_axis',(0.983205865442321,-0.18249993468442,0.));
#30660=DIRECTION('center_axis',(0.,0.,1.));
#30661=DIRECTION('ref_axis',(-0.420469989562984,0.907306446509064,0.));
#30662=DIRECTION('center_axis',(0.,0.,-1.));
#30663=DIRECTION('ref_axis',(-0.420469989562984,0.907306446509064,0.));
#30664=DIRECTION('',(0.,0.,1.));
#30665=DIRECTION('center_axis',(0.,0.,1.));
#30666=DIRECTION('ref_axis',(-0.420469989562984,0.907306446509064,0.));
#30667=DIRECTION('',(0.,0.,-1.));
#30668=DIRECTION('center_axis',(0.333553353095455,0.942731223965123,0.));
#30669=DIRECTION('ref_axis',(-0.942731223965123,0.333553353095455,0.));
#30670=DIRECTION('',(-0.942731223965123,0.333553353095455,0.));
#30671=DIRECTION('',(0.,0.,1.));
#30672=DIRECTION('',(0.942731223965123,-0.333553353095455,0.));
#30673=DIRECTION('center_axis',(0.,0.,1.));
#30674=DIRECTION('ref_axis',(-0.93887972184625,-0.344245360035407,0.));
#30675=DIRECTION('center_axis',(0.,0.,-1.));
#30676=DIRECTION('ref_axis',(-0.93887972184625,-0.344245360035407,0.));
#30677=DIRECTION('',(0.,0.,1.));
#30678=DIRECTION('center_axis',(0.,0.,1.));
#30679=DIRECTION('ref_axis',(-0.93887972184625,-0.344245360035407,0.));
#30680=DIRECTION('',(0.,0.,-1.));
#30681=DIRECTION('center_axis',(0.,0.,1.));
#30682=DIRECTION('ref_axis',(0.902469479163338,-0.430753803440728,0.));
#30683=DIRECTION('center_axis',(0.,0.,1.));
#30684=DIRECTION('ref_axis',(0.902469479163338,-0.430753803440728,0.));
#30685=DIRECTION('center_axis',(0.,0.,-1.));
#30686=DIRECTION('ref_axis',(0.902469479163338,-0.430753803440728,0.));
#30687=DIRECTION('center_axis',(0.,0.,1.));
#30688=DIRECTION('ref_axis',(-0.171314633997541,0.985216370234624,0.));
#30689=DIRECTION('center_axis',(0.,0.,-1.));
#30690=DIRECTION('ref_axis',(-0.171314633997541,0.985216370234624,0.));
#30691=DIRECTION('',(0.,0.,1.));
#30692=DIRECTION('center_axis',(0.,0.,1.));
#30693=DIRECTION('ref_axis',(-0.171314633997541,0.985216370234624,0.));
#30694=DIRECTION('',(0.,0.,-1.));
#30695=DIRECTION('center_axis',(0.5661845933752,0.824278476138107,0.));
#30696=DIRECTION('ref_axis',(-0.824278476138107,0.5661845933752,0.));
#30697=DIRECTION('',(-0.824278476138107,0.5661845933752,0.));
#30698=DIRECTION('',(0.,0.,1.));
#30699=DIRECTION('',(0.824278476138107,-0.5661845933752,0.));
#30700=DIRECTION('center_axis',(0.,0.,1.));
#30701=DIRECTION('ref_axis',(-0.995985426475728,-0.0895155307640121,0.));
#30702=DIRECTION('center_axis',(0.,0.,-1.));
#30703=DIRECTION('ref_axis',(-0.995985426475728,-0.0895155307640121,0.));
#30704=DIRECTION('',(0.,0.,1.));
#30705=DIRECTION('center_axis',(0.,0.,1.));
#30706=DIRECTION('ref_axis',(-0.995985426475728,-0.0895155307640121,0.));
#30707=DIRECTION('',(0.,0.,-1.));
#30708=DIRECTION('center_axis',(0.,0.,1.));
#30709=DIRECTION('ref_axis',(0.760231289280704,-0.649652512346868,0.));
#30710=DIRECTION('center_axis',(0.,0.,1.));
#30711=DIRECTION('ref_axis',(0.760231289280704,-0.649652512346868,0.));
#30712=DIRECTION('center_axis',(0.,0.,-1.));
#30713=DIRECTION('ref_axis',(0.760231289280704,-0.649652512346868,0.));
#30714=DIRECTION('center_axis',(0.,0.,1.));
#30715=DIRECTION('ref_axis',(0.0895155307640188,0.995985426475727,0.));
#30716=DIRECTION('center_axis',(0.,0.,-1.));
#30717=DIRECTION('ref_axis',(0.0895155307640188,0.995985426475727,0.));
#30718=DIRECTION('',(0.,0.,1.));
#30719=DIRECTION('center_axis',(0.,0.,1.));
#30720=DIRECTION('ref_axis',(0.0895155307640188,0.995985426475727,0.));
#30721=DIRECTION('',(0.,0.,-1.));
#30722=DIRECTION('center_axis',(0.760231289280706,0.649652512346866,0.));
#30723=DIRECTION('ref_axis',(-0.649652512346866,0.760231289280706,0.));
#30724=DIRECTION('',(-0.649652512346866,0.760231289280706,0.));
#30725=DIRECTION('',(0.,0.,1.));
#30726=DIRECTION('',(0.649652512346866,-0.760231289280706,0.));
#30727=DIRECTION('center_axis',(0.,0.,1.));
#30728=DIRECTION('ref_axis',(-0.985216370234624,0.171314633997541,0.));
#30729=DIRECTION('center_axis',(0.,0.,-1.));
#30730=DIRECTION('ref_axis',(-0.985216370234624,0.171314633997541,0.));
#30731=DIRECTION('',(0.,0.,1.));
#30732=DIRECTION('center_axis',(0.,0.,1.));
#30733=DIRECTION('ref_axis',(-0.985216370234624,0.171314633997541,0.));
#30734=DIRECTION('',(0.,0.,-1.));
#30735=DIRECTION('center_axis',(0.,0.,1.));
#30736=DIRECTION('ref_axis',(0.566184593375197,-0.824278476138108,0.));
#30737=DIRECTION('center_axis',(0.,0.,1.));
#30738=DIRECTION('ref_axis',(0.566184593375197,-0.824278476138108,0.));
#30739=DIRECTION('center_axis',(0.,0.,-1.));
#30740=DIRECTION('ref_axis',(0.566184593375197,-0.824278476138108,0.));
#30741=DIRECTION('center_axis',(0.,0.,1.));
#30742=DIRECTION('ref_axis',(0.344245360035407,0.938879721846251,0.));
#30743=DIRECTION('center_axis',(0.,0.,-1.));
#30744=DIRECTION('ref_axis',(0.344245360035407,0.938879721846251,0.));
#30745=DIRECTION('',(0.,0.,1.));
#30746=DIRECTION('center_axis',(0.,0.,1.));
#30747=DIRECTION('ref_axis',(0.344245360035407,0.938879721846251,0.));
#30748=DIRECTION('',(0.,0.,-1.));
#30749=DIRECTION('center_axis',(0.902469479163339,0.430753803440726,0.));
#30750=DIRECTION('ref_axis',(-0.430753803440726,0.902469479163339,0.));
#30751=DIRECTION('',(-0.430753803440726,0.902469479163339,0.));
#30752=DIRECTION('',(0.,0.,1.));
#30753=DIRECTION('',(0.430753803440726,-0.902469479163339,0.));
#30754=DIRECTION('center_axis',(0.,0.,1.));
#30755=DIRECTION('ref_axis',(-0.907306446509064,0.420469989562983,0.));
#30756=DIRECTION('center_axis',(0.,0.,-1.));
#30757=DIRECTION('ref_axis',(-0.907306446509064,0.420469989562983,0.));
#30758=DIRECTION('',(0.,0.,1.));
#30759=DIRECTION('center_axis',(0.,0.,1.));
#30760=DIRECTION('ref_axis',(-0.907306446509064,0.420469989562983,0.));
#30761=DIRECTION('',(0.,0.,-1.));
#30762=DIRECTION('center_axis',(0.,0.,1.));
#30763=DIRECTION('ref_axis',(0.333553353095452,-0.942731223965124,0.));
#30764=DIRECTION('center_axis',(0.,0.,1.));
#30765=DIRECTION('ref_axis',(0.333553353095452,-0.942731223965124,0.));
#30766=DIRECTION('center_axis',(0.,0.,-1.));
#30767=DIRECTION('ref_axis',(0.333553353095452,-0.942731223965124,0.));
#30768=DIRECTION('center_axis',(0.,0.,1.));
#30769=DIRECTION('ref_axis',(0.575515436912747,0.817790915745051,0.));
#30770=DIRECTION('center_axis',(0.,0.,-1.));
#30771=DIRECTION('ref_axis',(0.575515436912747,0.817790915745051,0.));
#30772=DIRECTION('',(0.,0.,1.));
#30773=DIRECTION('center_axis',(0.,0.,1.));
#30774=DIRECTION('ref_axis',(0.575515436912747,0.817790915745051,0.));
#30775=DIRECTION('',(0.,0.,-1.));
#30776=DIRECTION('center_axis',(0.983205865442321,0.182499934684417,0.));
#30777=DIRECTION('ref_axis',(-0.182499934684417,0.983205865442321,0.));
#30778=DIRECTION('',(-0.182499934684417,0.983205865442321,0.));
#30779=DIRECTION('',(0.,0.,1.));
#30780=DIRECTION('',(0.182499934684417,-0.983205865442321,0.));
#30781=DIRECTION('center_axis',(0.,0.,1.));
#30782=DIRECTION('ref_axis',(-0.767565087848714,0.64097101019921,0.));
#30783=DIRECTION('center_axis',(0.,0.,-1.));
#30784=DIRECTION('ref_axis',(-0.767565087848714,0.64097101019921,0.));
#30785=DIRECTION('',(0.,0.,1.));
#30786=DIRECTION('center_axis',(0.,0.,1.));
#30787=DIRECTION('ref_axis',(-0.767565087848714,0.64097101019921,0.));
#30788=DIRECTION('',(0.,0.,-1.));
#30789=DIRECTION('center_axis',(0.,0.,1.));
#30790=DIRECTION('ref_axis',(0.07819100302523,-0.996938396815926,0.));
#30791=DIRECTION('center_axis',(0.,0.,1.));
#30792=DIRECTION('ref_axis',(0.07819100302523,-0.996938396815926,0.));
#30793=DIRECTION('center_axis',(0.,0.,-1.));
#30794=DIRECTION('ref_axis',(0.07819100302523,-0.996938396815926,0.));
#30795=DIRECTION('center_axis',(0.,0.,1.));
#30796=DIRECTION('ref_axis',(0.767565087848712,0.640971010199212,0.));
#30797=DIRECTION('center_axis',(0.,0.,-1.));
#30798=DIRECTION('ref_axis',(0.767565087848712,0.640971010199212,0.));
#30799=DIRECTION('',(0.,0.,1.));
#30800=DIRECTION('center_axis',(0.,0.,1.));
#30801=DIRECTION('ref_axis',(0.767565087848712,0.640971010199212,0.));
#30802=DIRECTION('',(0.,0.,-1.));
#30803=DIRECTION('center_axis',(0.996938396815926,-0.0781910030252327,0.));
#30804=DIRECTION('ref_axis',(0.0781910030252327,0.996938396815926,0.));
#30805=DIRECTION('',(0.0781910030252327,0.996938396815926,0.));
#30806=DIRECTION('',(0.,0.,1.));
#30807=DIRECTION('',(-0.0781910030252327,-0.996938396815926,0.));
#30808=DIRECTION('center_axis',(0.,0.,1.));
#30809=DIRECTION('ref_axis',(-0.575515436912756,0.817790915745045,0.));
#30810=DIRECTION('center_axis',(0.,0.,-1.));
#30811=DIRECTION('ref_axis',(-0.575515436912756,0.817790915745045,0.));
#30812=DIRECTION('',(0.,0.,1.));
#30813=DIRECTION('center_axis',(0.,0.,1.));
#30814=DIRECTION('ref_axis',(-0.575515436912756,0.817790915745045,0.));
#30815=DIRECTION('',(0.,0.,-1.));
#30816=DIRECTION('center_axis',(0.,0.,1.));
#30817=DIRECTION('ref_axis',(-0.18249993468442,-0.983205865442321,0.));
#30818=DIRECTION('center_axis',(0.,0.,1.));
#30819=DIRECTION('ref_axis',(-0.18249993468442,-0.983205865442321,0.));
#30820=DIRECTION('center_axis',(0.,0.,-1.));
#30821=DIRECTION('ref_axis',(-0.18249993468442,-0.983205865442321,0.));
#30822=DIRECTION('center_axis',(0.,0.,1.));
#30823=DIRECTION('ref_axis',(0.907306446509064,0.420469989562984,0.));
#30824=DIRECTION('center_axis',(0.,0.,-1.));
#30825=DIRECTION('ref_axis',(0.907306446509064,0.420469989562984,0.));
#30826=DIRECTION('',(0.,0.,1.));
#30827=DIRECTION('center_axis',(0.,0.,1.));
#30828=DIRECTION('ref_axis',(0.907306446509064,0.420469989562984,0.));
#30829=DIRECTION('',(0.,0.,-1.));
#30830=DIRECTION('center_axis',(0.942731223965123,-0.333553353095455,0.));
#30831=DIRECTION('ref_axis',(0.333553353095455,0.942731223965123,0.));
#30832=DIRECTION('',(0.333553353095455,0.942731223965123,0.));
#30833=DIRECTION('',(0.,0.,1.));
#30834=DIRECTION('',(-0.333553353095455,-0.942731223965123,0.));
#30835=DIRECTION('center_axis',(0.,0.,1.));
#30836=DIRECTION('ref_axis',(-0.344245360035407,0.93887972184625,0.));
#30837=DIRECTION('center_axis',(0.,0.,-1.));
#30838=DIRECTION('ref_axis',(-0.344245360035407,0.93887972184625,0.));
#30839=DIRECTION('',(0.,0.,1.));
#30840=DIRECTION('center_axis',(0.,0.,1.));
#30841=DIRECTION('ref_axis',(-0.344245360035407,0.93887972184625,0.));
#30842=DIRECTION('',(0.,0.,-1.));
#30843=DIRECTION('center_axis',(0.,0.,1.));
#30844=DIRECTION('ref_axis',(-0.430753803440728,-0.902469479163338,0.));
#30845=DIRECTION('center_axis',(0.,0.,1.));
#30846=DIRECTION('ref_axis',(-0.430753803440728,-0.902469479163338,0.));
#30847=DIRECTION('center_axis',(0.,0.,-1.));
#30848=DIRECTION('ref_axis',(-0.430753803440728,-0.902469479163338,0.));
#30849=DIRECTION('center_axis',(0.,0.,1.));
#30850=DIRECTION('ref_axis',(0.985216370234623,0.171314633997547,0.));
#30851=DIRECTION('center_axis',(0.,0.,-1.));
#30852=DIRECTION('ref_axis',(0.985216370234623,0.171314633997547,0.));
#30853=DIRECTION('',(0.,0.,1.));
#30854=DIRECTION('center_axis',(0.,0.,1.));
#30855=DIRECTION('ref_axis',(0.985216370234623,0.171314633997547,0.));
#30856=DIRECTION('',(0.,0.,-1.));
#30857=DIRECTION('center_axis',(0.824278476138107,-0.5661845933752,0.));
#30858=DIRECTION('ref_axis',(0.5661845933752,0.824278476138107,0.));
#30859=DIRECTION('',(0.5661845933752,0.824278476138107,0.));
#30860=DIRECTION('',(0.,0.,1.));
#30861=DIRECTION('',(-0.5661845933752,-0.824278476138107,0.));
#30862=DIRECTION('center_axis',(0.,0.,1.));
#30863=DIRECTION('ref_axis',(-0.0895155307640188,0.995985426475727,0.));
#30864=DIRECTION('center_axis',(0.,0.,-1.));
#30865=DIRECTION('ref_axis',(-0.0895155307640188,0.995985426475727,0.));
#30866=DIRECTION('',(0.,0.,1.));
#30867=DIRECTION('center_axis',(0.,0.,1.));
#30868=DIRECTION('ref_axis',(-0.0895155307640188,0.995985426475727,0.));
#30869=DIRECTION('',(0.,0.,-1.));
#30870=DIRECTION('center_axis',(0.,0.,1.));
#30871=DIRECTION('ref_axis',(-0.649652512346869,-0.760231289280704,0.));
#30872=DIRECTION('center_axis',(0.,0.,1.));
#30873=DIRECTION('ref_axis',(-0.649652512346869,-0.760231289280704,0.));
#30874=DIRECTION('center_axis',(0.,0.,-1.));
#30875=DIRECTION('ref_axis',(-0.649652512346869,-0.760231289280704,0.));
#30876=DIRECTION('center_axis',(0.,0.,1.));
#30877=DIRECTION('ref_axis',(0.995985426475728,-0.0895155307640127,0.));
#30878=DIRECTION('center_axis',(0.,0.,-1.));
#30879=DIRECTION('ref_axis',(0.995985426475728,-0.0895155307640127,0.));
#30880=DIRECTION('',(0.,0.,1.));
#30881=DIRECTION('center_axis',(0.,0.,1.));
#30882=DIRECTION('ref_axis',(0.995985426475728,-0.0895155307640127,0.));
#30883=DIRECTION('',(0.,0.,-1.));
#30884=DIRECTION('center_axis',(0.649652512346867,-0.760231289280706,0.));
#30885=DIRECTION('ref_axis',(0.760231289280706,0.649652512346867,0.));
#30886=DIRECTION('',(0.760231289280706,0.649652512346867,0.));
#30887=DIRECTION('',(0.,0.,1.));
#30888=DIRECTION('',(-0.760231289280706,-0.649652512346867,0.));
#30889=DIRECTION('center_axis',(0.,0.,1.));
#30890=DIRECTION('ref_axis',(0.17131463399754,0.985216370234625,0.));
#30891=DIRECTION('center_axis',(0.,0.,-1.));
#30892=DIRECTION('ref_axis',(0.17131463399754,0.985216370234625,0.));
#30893=DIRECTION('',(0.,0.,1.));
#30894=DIRECTION('center_axis',(0.,0.,1.));
#30895=DIRECTION('ref_axis',(0.17131463399754,0.985216370234625,0.));
#30896=DIRECTION('',(0.,0.,-1.));
#30897=DIRECTION('center_axis',(0.,0.,1.));
#30898=DIRECTION('ref_axis',(-0.824278476138108,-0.566184593375198,0.));
#30899=DIRECTION('center_axis',(0.,0.,1.));
#30900=DIRECTION('ref_axis',(-0.824278476138108,-0.566184593375198,0.));
#30901=DIRECTION('center_axis',(0.,0.,-1.));
#30902=DIRECTION('ref_axis',(-0.824278476138108,-0.566184593375198,0.));
#30903=DIRECTION('center_axis',(0.,0.,1.));
#30904=DIRECTION('ref_axis',(0.93887972184625,-0.344245360035407,0.));
#30905=DIRECTION('center_axis',(0.,0.,-1.));
#30906=DIRECTION('ref_axis',(0.93887972184625,-0.344245360035407,0.));
#30907=DIRECTION('',(0.,0.,1.));
#30908=DIRECTION('center_axis',(0.,0.,1.));
#30909=DIRECTION('ref_axis',(0.93887972184625,-0.344245360035407,0.));
#30910=DIRECTION('',(0.,0.,-1.));
#30911=DIRECTION('center_axis',(0.430753803440726,-0.902469479163339,0.));
#30912=DIRECTION('ref_axis',(0.902469479163339,0.430753803440726,0.));
#30913=DIRECTION('',(0.902469479163339,0.430753803440726,0.));
#30914=DIRECTION('',(0.,0.,1.));
#30915=DIRECTION('',(-0.902469479163339,-0.430753803440726,0.));
#30916=DIRECTION('center_axis',(0.,0.,1.));
#30917=DIRECTION('ref_axis',(0.420469989562982,0.907306446509065,0.));
#30918=DIRECTION('center_axis',(0.,0.,-1.));
#30919=DIRECTION('ref_axis',(0.420469989562982,0.907306446509065,0.));
#30920=DIRECTION('',(0.,0.,1.));
#30921=DIRECTION('center_axis',(0.,0.,1.));
#30922=DIRECTION('ref_axis',(0.420469989562982,0.907306446509065,0.));
#30923=DIRECTION('',(0.,0.,-1.));
#30924=DIRECTION('center_axis',(0.,0.,1.));
#30925=DIRECTION('ref_axis',(-0.942731223965124,-0.333553353095452,0.));
#30926=DIRECTION('center_axis',(0.,0.,1.));
#30927=DIRECTION('ref_axis',(-0.942731223965124,-0.333553353095452,0.));
#30928=DIRECTION('center_axis',(0.,0.,-1.));
#30929=DIRECTION('ref_axis',(-0.942731223965124,-0.333553353095452,0.));
#30930=DIRECTION('center_axis',(0.,0.,1.));
#30931=DIRECTION('ref_axis',(0.817790915745051,-0.575515436912747,0.));
#30932=DIRECTION('center_axis',(0.,0.,-1.));
#30933=DIRECTION('ref_axis',(0.817790915745051,-0.575515436912747,0.));
#30934=DIRECTION('',(0.,0.,1.));
#30935=DIRECTION('center_axis',(0.,0.,1.));
#30936=DIRECTION('ref_axis',(0.817790915745051,-0.575515436912747,0.));
#30937=DIRECTION('',(0.,0.,-1.));
#30938=DIRECTION('center_axis',(0.182499934684417,-0.983205865442321,0.));
#30939=DIRECTION('ref_axis',(0.983205865442321,0.182499934684417,0.));
#30940=DIRECTION('',(0.983205865442321,0.182499934684417,0.));
#30941=DIRECTION('',(0.,0.,1.));
#30942=DIRECTION('',(-0.983205865442321,-0.182499934684417,0.));
#30943=DIRECTION('center_axis',(0.,0.,1.));
#30944=DIRECTION('ref_axis',(0.64097101019921,0.767565087848714,0.));
#30945=DIRECTION('center_axis',(0.,0.,-1.));
#30946=DIRECTION('ref_axis',(0.64097101019921,0.767565087848714,0.));
#30947=DIRECTION('',(0.,0.,1.));
#30948=DIRECTION('center_axis',(0.,0.,1.));
#30949=DIRECTION('ref_axis',(0.64097101019921,0.767565087848714,0.));
#30950=DIRECTION('',(0.,0.,-1.));
#30951=DIRECTION('center_axis',(0.,0.,1.));
#30952=DIRECTION('ref_axis',(-0.996938396815926,-0.07819100302523,0.));
#30953=DIRECTION('center_axis',(0.,0.,1.));
#30954=DIRECTION('ref_axis',(-0.996938396815926,-0.07819100302523,0.));
#30955=DIRECTION('center_axis',(0.,0.,-1.));
#30956=DIRECTION('ref_axis',(-0.996938396815926,-0.07819100302523,0.));
#30957=DIRECTION('center_axis',(0.,0.,1.));
#30958=DIRECTION('ref_axis',(0.640971010199219,-0.767565087848706,0.));
#30959=DIRECTION('center_axis',(0.,0.,-1.));
#30960=DIRECTION('ref_axis',(0.640971010199219,-0.767565087848706,0.));
#30961=DIRECTION('',(0.,0.,1.));
#30962=DIRECTION('center_axis',(0.,0.,1.));
#30963=DIRECTION('ref_axis',(0.640971010199219,-0.767565087848706,0.));
#30964=DIRECTION('',(0.,0.,-1.));
#30965=DIRECTION('center_axis',(-0.0781910030252323,-0.996938396815926,
0.));
#30966=DIRECTION('ref_axis',(0.996938396815926,-0.0781910030252323,0.));
#30967=DIRECTION('',(0.996938396815926,-0.0781910030252323,0.));
#30968=DIRECTION('',(0.,0.,1.));
#30969=DIRECTION('',(-0.996938396815926,0.0781910030252323,0.));
#30970=DIRECTION('center_axis',(0.,0.,1.));
#30971=DIRECTION('ref_axis',(0.817790915745049,0.57551543691275,0.));
#30972=DIRECTION('center_axis',(0.,0.,-1.));
#30973=DIRECTION('ref_axis',(0.817790915745049,0.57551543691275,0.));
#30974=DIRECTION('',(0.,0.,1.));
#30975=DIRECTION('center_axis',(0.,0.,1.));
#30976=DIRECTION('ref_axis',(0.817790915745049,0.57551543691275,0.));
#30977=DIRECTION('',(0.,0.,-1.));
#30978=DIRECTION('center_axis',(0.,0.,1.));
#30979=DIRECTION('ref_axis',(-0.983205865442321,0.18249993468442,0.));
#30980=DIRECTION('center_axis',(0.,0.,1.));
#30981=DIRECTION('ref_axis',(-0.983205865442321,0.18249993468442,0.));
#30982=DIRECTION('center_axis',(0.,0.,-1.));
#30983=DIRECTION('ref_axis',(-0.983205865442321,0.18249993468442,0.));
#30984=DIRECTION('center_axis',(0.,0.,1.));
#30985=DIRECTION('ref_axis',(0.420469989562984,-0.907306446509064,0.));
#30986=DIRECTION('center_axis',(0.,0.,-1.));
#30987=DIRECTION('ref_axis',(0.420469989562984,-0.907306446509064,0.));
#30988=DIRECTION('',(0.,0.,1.));
#30989=DIRECTION('center_axis',(0.,0.,1.));
#30990=DIRECTION('ref_axis',(0.420469989562984,-0.907306446509064,0.));
#30991=DIRECTION('',(0.,0.,-1.));
#30992=DIRECTION('center_axis',(-0.333553353095454,-0.942731223965123,0.));
#30993=DIRECTION('ref_axis',(0.942731223965123,-0.333553353095454,0.));
#30994=DIRECTION('',(0.942731223965123,-0.333553353095454,0.));
#30995=DIRECTION('',(0.,0.,1.));
#30996=DIRECTION('',(-0.942731223965123,0.333553353095454,0.));
#30997=DIRECTION('center_axis',(0.,0.,1.));
#30998=DIRECTION('ref_axis',(0.93887972184625,0.344245360035408,0.));
#30999=DIRECTION('center_axis',(0.,0.,-1.));
#31000=DIRECTION('ref_axis',(0.93887972184625,0.344245360035408,0.));
#31001=DIRECTION('',(0.,0.,1.));
#31002=DIRECTION('center_axis',(0.,0.,1.));
#31003=DIRECTION('ref_axis',(0.93887972184625,0.344245360035408,0.));
#31004=DIRECTION('',(0.,0.,-1.));
#31005=DIRECTION('center_axis',(0.,0.,1.));
#31006=DIRECTION('ref_axis',(-0.902469479163338,0.430753803440728,0.));
#31007=DIRECTION('center_axis',(0.,0.,1.));
#31008=DIRECTION('ref_axis',(-0.902469479163338,0.430753803440728,0.));
#31009=DIRECTION('center_axis',(0.,0.,-1.));
#31010=DIRECTION('ref_axis',(-0.902469479163338,0.430753803440728,0.));
#31011=DIRECTION('center_axis',(0.,0.,1.));
#31012=DIRECTION('ref_axis',(0.171314633997546,-0.985216370234624,0.));
#31013=DIRECTION('center_axis',(0.,0.,-1.));
#31014=DIRECTION('ref_axis',(0.171314633997546,-0.985216370234624,0.));
#31015=DIRECTION('',(0.,0.,1.));
#31016=DIRECTION('center_axis',(0.,0.,1.));
#31017=DIRECTION('ref_axis',(0.171314633997546,-0.985216370234624,0.));
#31018=DIRECTION('',(0.,0.,-1.));
#31019=DIRECTION('center_axis',(-0.5661845933752,-0.824278476138107,0.));
#31020=DIRECTION('ref_axis',(0.824278476138107,-0.5661845933752,0.));
#31021=DIRECTION('',(0.824278476138107,-0.5661845933752,0.));
#31022=DIRECTION('',(0.,0.,1.));
#31023=DIRECTION('',(-0.824278476138107,0.5661845933752,0.));
#31024=DIRECTION('center_axis',(0.,0.,1.));
#31025=DIRECTION('ref_axis',(0.995985426475728,0.0895155307640127,0.));
#31026=DIRECTION('center_axis',(0.,0.,-1.));
#31027=DIRECTION('ref_axis',(0.995985426475728,0.0895155307640127,0.));
#31028=DIRECTION('',(0.,0.,1.));
#31029=DIRECTION('center_axis',(0.,0.,1.));
#31030=DIRECTION('ref_axis',(0.995985426475728,0.0895155307640127,0.));
#31031=DIRECTION('',(0.,0.,-1.));
#31032=DIRECTION('center_axis',(0.,0.,1.));
#31033=DIRECTION('ref_axis',(-0.760231289280704,0.649652512346868,0.));
#31034=DIRECTION('center_axis',(0.,0.,1.));
#31035=DIRECTION('ref_axis',(-0.760231289280704,0.649652512346868,0.));
#31036=DIRECTION('center_axis',(0.,0.,-1.));
#31037=DIRECTION('ref_axis',(-0.760231289280704,0.649652512346868,0.));
#31038=DIRECTION('center_axis',(0.,0.,1.));
#31039=DIRECTION('ref_axis',(-0.0895155307640188,-0.995985426475727,0.));
#31040=DIRECTION('center_axis',(0.,0.,-1.));
#31041=DIRECTION('ref_axis',(-0.0895155307640188,-0.995985426475727,0.));
#31042=DIRECTION('',(0.,0.,1.));
#31043=DIRECTION('center_axis',(0.,0.,1.));
#31044=DIRECTION('ref_axis',(-0.0895155307640188,-0.995985426475727,0.));
#31045=DIRECTION('',(0.,0.,-1.));
#31046=DIRECTION('center_axis',(-0.760231289280706,-0.649652512346867,0.));
#31047=DIRECTION('ref_axis',(0.649652512346867,-0.760231289280706,0.));
#31048=DIRECTION('',(0.649652512346867,-0.760231289280706,0.));
#31049=DIRECTION('',(0.,0.,1.));
#31050=DIRECTION('',(-0.649652512346867,0.760231289280706,0.));
#31051=DIRECTION('center_axis',(0.,0.,1.));
#31052=DIRECTION('ref_axis',(0.985216370234623,-0.171314633997547,0.));
#31053=DIRECTION('center_axis',(0.,0.,-1.));
#31054=DIRECTION('ref_axis',(0.985216370234623,-0.171314633997547,0.));
#31055=DIRECTION('',(0.,0.,1.));
#31056=DIRECTION('center_axis',(0.,0.,1.));
#31057=DIRECTION('ref_axis',(0.985216370234623,-0.171314633997547,0.));
#31058=DIRECTION('',(0.,0.,-1.));
#31059=DIRECTION('center_axis',(0.,0.,1.));
#31060=DIRECTION('ref_axis',(-0.566184593375198,0.824278476138108,0.));
#31061=DIRECTION('center_axis',(0.,0.,1.));
#31062=DIRECTION('ref_axis',(-0.566184593375198,0.824278476138108,0.));
#31063=DIRECTION('center_axis',(0.,0.,-1.));
#31064=DIRECTION('ref_axis',(-0.566184593375198,0.824278476138108,0.));
#31065=DIRECTION('center_axis',(0.,0.,1.));
#31066=DIRECTION('ref_axis',(-0.34424536003541,-0.93887972184625,0.));
#31067=DIRECTION('center_axis',(0.,0.,-1.));
#31068=DIRECTION('ref_axis',(-0.34424536003541,-0.93887972184625,0.));
#31069=DIRECTION('',(0.,0.,1.));
#31070=DIRECTION('center_axis',(0.,0.,1.));
#31071=DIRECTION('ref_axis',(-0.34424536003541,-0.93887972184625,0.));
#31072=DIRECTION('',(0.,0.,-1.));
#31073=DIRECTION('center_axis',(-0.902469479163339,-0.430753803440726,0.));
#31074=DIRECTION('ref_axis',(0.430753803440726,-0.902469479163339,0.));
#31075=DIRECTION('',(0.430753803440726,-0.902469479163339,0.));
#31076=DIRECTION('',(0.,0.,1.));
#31077=DIRECTION('',(-0.430753803440726,0.902469479163339,0.));
#31078=DIRECTION('center_axis',(0.,0.,1.));
#31079=DIRECTION('ref_axis',(0.907306446509069,-0.420469989562973,0.));
#31080=DIRECTION('center_axis',(0.,0.,-1.));
#31081=DIRECTION('ref_axis',(0.907306446509069,-0.420469989562973,0.));
#31082=DIRECTION('',(0.,0.,1.));
#31083=DIRECTION('center_axis',(0.,0.,1.));
#31084=DIRECTION('ref_axis',(0.907306446509069,-0.420469989562973,0.));
#31085=DIRECTION('',(0.,0.,-1.));
#31086=DIRECTION('center_axis',(0.,0.,1.));
#31087=DIRECTION('ref_axis',(-0.333553353095452,0.942731223965124,0.));
#31088=DIRECTION('center_axis',(0.,0.,1.));
#31089=DIRECTION('ref_axis',(-0.333553353095452,0.942731223965124,0.));
#31090=DIRECTION('center_axis',(0.,0.,-1.));
#31091=DIRECTION('ref_axis',(-0.333553353095452,0.942731223965124,0.));
#31092=DIRECTION('center_axis',(0.,0.,1.));
#31093=DIRECTION('ref_axis',(-0.575515436912748,-0.817790915745051,0.));
#31094=DIRECTION('center_axis',(0.,0.,-1.));
#31095=DIRECTION('ref_axis',(-0.575515436912748,-0.817790915745051,0.));
#31096=DIRECTION('',(0.,0.,1.));
#31097=DIRECTION('center_axis',(0.,0.,1.));
#31098=DIRECTION('ref_axis',(-0.575515436912748,-0.817790915745051,0.));
#31099=DIRECTION('',(0.,0.,-1.));
#31100=DIRECTION('center_axis',(-0.983205865442321,-0.182499934684418,0.));
#31101=DIRECTION('ref_axis',(0.182499934684418,-0.983205865442321,0.));
#31102=DIRECTION('',(0.182499934684418,-0.983205865442321,0.));
#31103=DIRECTION('',(0.,0.,1.));
#31104=DIRECTION('',(-0.182499934684418,0.983205865442321,0.));
#31105=DIRECTION('center_axis',(0.,0.,1.));
#31106=DIRECTION('ref_axis',(0.767565087848708,-0.640971010199218,0.));
#31107=DIRECTION('center_axis',(0.,0.,-1.));
#31108=DIRECTION('ref_axis',(0.767565087848708,-0.640971010199218,0.));
#31109=DIRECTION('',(0.,0.,1.));
#31110=DIRECTION('center_axis',(0.,0.,1.));
#31111=DIRECTION('ref_axis',(0.767565087848708,-0.640971010199218,0.));
#31112=DIRECTION('',(0.,0.,-1.));
#31113=DIRECTION('center_axis',(0.,0.,1.));
#31114=DIRECTION('ref_axis',(-0.0781910030252301,0.996938396815926,0.));
#31115=DIRECTION('center_axis',(0.,0.,1.));
#31116=DIRECTION('ref_axis',(-0.0781910030252301,0.996938396815926,0.));
#31117=DIRECTION('center_axis',(0.,0.,-1.));
#31118=DIRECTION('ref_axis',(-0.0781910030252301,0.996938396815926,0.));
#31119=DIRECTION('center_axis',(0.,0.,1.));
#31120=DIRECTION('ref_axis',(-0.767565087848706,-0.640971010199219,0.));
#31121=DIRECTION('center_axis',(0.,0.,-1.));
#31122=DIRECTION('ref_axis',(-0.767565087848706,-0.640971010199219,0.));
#31123=DIRECTION('',(0.,0.,1.));
#31124=DIRECTION('center_axis',(0.,0.,1.));
#31125=DIRECTION('ref_axis',(-0.767565087848706,-0.640971010199219,0.));
#31126=DIRECTION('',(0.,0.,-1.));
#31127=DIRECTION('center_axis',(-0.996938396815926,0.0781910030252323,0.));
#31128=DIRECTION('ref_axis',(-0.0781910030252323,-0.996938396815926,0.));
#31129=DIRECTION('',(-0.0781910030252323,-0.996938396815926,0.));
#31130=DIRECTION('',(0.,0.,1.));
#31131=DIRECTION('',(0.0781910030252323,0.996938396815926,0.));
#31132=DIRECTION('center_axis',(0.,0.,1.));
#31133=DIRECTION('ref_axis',(0.57551543691275,-0.817790915745049,0.));
#31134=DIRECTION('center_axis',(0.,0.,-1.));
#31135=DIRECTION('ref_axis',(0.57551543691275,-0.817790915745049,0.));
#31136=DIRECTION('',(0.,0.,1.));
#31137=DIRECTION('center_axis',(0.,0.,1.));
#31138=DIRECTION('ref_axis',(0.57551543691275,-0.817790915745049,0.));
#31139=DIRECTION('',(0.,0.,-1.));
#31140=DIRECTION('center_axis',(0.,0.,1.));
#31141=DIRECTION('ref_axis',(0.18249993468442,0.983205865442321,0.));
#31142=DIRECTION('center_axis',(0.,0.,1.));
#31143=DIRECTION('ref_axis',(0.18249993468442,0.983205865442321,0.));
#31144=DIRECTION('center_axis',(0.,0.,-1.));
#31145=DIRECTION('ref_axis',(0.18249993468442,0.983205865442321,0.));
#31146=DIRECTION('center_axis',(0.,0.,1.));
#31147=DIRECTION('ref_axis',(-0.907306446509064,-0.420469989562983,0.));
#31148=DIRECTION('center_axis',(0.,0.,-1.));
#31149=DIRECTION('ref_axis',(-0.907306446509064,-0.420469989562983,0.));
#31150=DIRECTION('',(0.,0.,1.));
#31151=DIRECTION('center_axis',(0.,0.,1.));
#31152=DIRECTION('ref_axis',(-0.907306446509064,-0.420469989562983,0.));
#31153=DIRECTION('',(0.,0.,-1.));
#31154=DIRECTION('center_axis',(-0.942731223965123,0.333553353095454,0.));
#31155=DIRECTION('ref_axis',(-0.333553353095454,-0.942731223965123,0.));
#31156=DIRECTION('',(-0.333553353095454,-0.942731223965123,0.));
#31157=DIRECTION('',(0.,0.,1.));
#31158=DIRECTION('',(0.333553353095454,0.942731223965123,0.));
#31159=DIRECTION('center_axis',(0.,0.,1.));
#31160=DIRECTION('ref_axis',(0.344245360035413,-0.938879721846248,0.));
#31161=DIRECTION('center_axis',(0.,0.,-1.));
#31162=DIRECTION('ref_axis',(0.344245360035413,-0.938879721846248,0.));
#31163=DIRECTION('',(0.,0.,1.));
#31164=DIRECTION('center_axis',(0.,0.,1.));
#31165=DIRECTION('ref_axis',(0.344245360035413,-0.938879721846248,0.));
#31166=DIRECTION('',(0.,0.,-1.));
#31167=DIRECTION('center_axis',(0.,0.,1.));
#31168=DIRECTION('ref_axis',(0.430753803440728,0.902469479163338,0.));
#31169=DIRECTION('center_axis',(0.,0.,1.));
#31170=DIRECTION('ref_axis',(0.430753803440728,0.902469479163338,0.));
#31171=DIRECTION('center_axis',(0.,0.,-1.));
#31172=DIRECTION('ref_axis',(0.430753803440728,0.902469479163338,0.));
#31173=DIRECTION('center_axis',(0.,0.,1.));
#31174=DIRECTION('ref_axis',(-0.985216370234624,-0.171314633997546,0.));
#31175=DIRECTION('center_axis',(0.,0.,-1.));
#31176=DIRECTION('ref_axis',(-0.985216370234624,-0.171314633997546,0.));
#31177=DIRECTION('',(0.,0.,1.));
#31178=DIRECTION('center_axis',(0.,0.,1.));
#31179=DIRECTION('ref_axis',(-0.985216370234624,-0.171314633997546,0.));
#31180=DIRECTION('',(0.,0.,-1.));
#31181=DIRECTION('center_axis',(-0.824278476138107,0.5661845933752,0.));
#31182=DIRECTION('ref_axis',(-0.5661845933752,-0.824278476138107,0.));
#31183=DIRECTION('',(-0.5661845933752,-0.824278476138107,0.));
#31184=DIRECTION('',(0.,0.,1.));
#31185=DIRECTION('',(0.5661845933752,0.824278476138107,0.));
#31186=DIRECTION('center_axis',(0.,0.,1.));
#31187=DIRECTION('ref_axis',(0.0895155307640121,-0.995985426475728,0.));
#31188=DIRECTION('center_axis',(0.,0.,-1.));
#31189=DIRECTION('ref_axis',(0.0895155307640121,-0.995985426475728,0.));
#31190=DIRECTION('',(0.,0.,1.));
#31191=DIRECTION('center_axis',(0.,0.,1.));
#31192=DIRECTION('ref_axis',(0.0895155307640121,-0.995985426475728,0.));
#31193=DIRECTION('',(0.,0.,-1.));
#31194=DIRECTION('center_axis',(0.,0.,1.));
#31195=DIRECTION('ref_axis',(0.649652512346868,0.760231289280704,0.));
#31196=DIRECTION('center_axis',(0.,0.,1.));
#31197=DIRECTION('ref_axis',(0.649652512346868,0.760231289280704,0.));
#31198=DIRECTION('center_axis',(0.,0.,-1.));
#31199=DIRECTION('ref_axis',(0.649652512346868,0.760231289280704,0.));
#31200=DIRECTION('center_axis',(0.,0.,1.));
#31201=DIRECTION('ref_axis',(-0.995985426475728,0.0895155307640127,0.));
#31202=DIRECTION('center_axis',(0.,0.,-1.));
#31203=DIRECTION('ref_axis',(-0.995985426475728,0.0895155307640127,0.));
#31204=DIRECTION('',(0.,0.,1.));
#31205=DIRECTION('center_axis',(0.,0.,1.));
#31206=DIRECTION('ref_axis',(-0.995985426475728,0.0895155307640127,0.));
#31207=DIRECTION('',(0.,0.,-1.));
#31208=DIRECTION('center_axis',(-0.649652512346867,0.760231289280706,0.));
#31209=DIRECTION('ref_axis',(-0.760231289280706,-0.649652512346867,0.));
#31210=DIRECTION('',(-0.760231289280706,-0.649652512346867,0.));
#31211=DIRECTION('',(0.,0.,1.));
#31212=DIRECTION('',(0.760231289280706,0.649652512346867,0.));
#31213=DIRECTION('center_axis',(0.,0.,1.));
#31214=DIRECTION('ref_axis',(-0.171314633997547,-0.985216370234623,0.));
#31215=DIRECTION('center_axis',(0.,0.,-1.));
#31216=DIRECTION('ref_axis',(-0.171314633997547,-0.985216370234623,0.));
#31217=DIRECTION('',(0.,0.,1.));
#31218=DIRECTION('center_axis',(0.,0.,1.));
#31219=DIRECTION('ref_axis',(-0.171314633997547,-0.985216370234623,0.));
#31220=DIRECTION('',(0.,0.,-1.));
#31221=DIRECTION('center_axis',(0.,0.,1.));
#31222=DIRECTION('ref_axis',(0.824278476138108,0.566184593375198,0.));
#31223=DIRECTION('center_axis',(0.,0.,1.));
#31224=DIRECTION('ref_axis',(0.824278476138108,0.566184593375198,0.));
#31225=DIRECTION('center_axis',(0.,0.,-1.));
#31226=DIRECTION('ref_axis',(0.824278476138108,0.566184593375198,0.));
#31227=DIRECTION('center_axis',(0.,0.,1.));
#31228=DIRECTION('ref_axis',(-0.93887972184625,0.34424536003541,0.));
#31229=DIRECTION('center_axis',(0.,0.,-1.));
#31230=DIRECTION('ref_axis',(-0.93887972184625,0.34424536003541,0.));
#31231=DIRECTION('',(0.,0.,1.));
#31232=DIRECTION('center_axis',(0.,0.,1.));
#31233=DIRECTION('ref_axis',(-0.93887972184625,0.34424536003541,0.));
#31234=DIRECTION('',(0.,0.,-1.));
#31235=DIRECTION('center_axis',(-0.430753803440726,0.902469479163339,0.));
#31236=DIRECTION('ref_axis',(-0.902469479163339,-0.430753803440726,0.));
#31237=DIRECTION('',(-0.902469479163339,-0.430753803440726,0.));
#31238=DIRECTION('',(0.,0.,1.));
#31239=DIRECTION('',(0.902469479163339,0.430753803440726,0.));
#31240=DIRECTION('center_axis',(0.,0.,1.));
#31241=DIRECTION('ref_axis',(-0.420469989562974,-0.907306446509068,0.));
#31242=DIRECTION('center_axis',(0.,0.,-1.));
#31243=DIRECTION('ref_axis',(-0.420469989562974,-0.907306446509068,0.));
#31244=DIRECTION('',(0.,0.,1.));
#31245=DIRECTION('center_axis',(0.,0.,1.));
#31246=DIRECTION('ref_axis',(-0.420469989562974,-0.907306446509068,0.));
#31247=DIRECTION('',(0.,0.,-1.));
#31248=DIRECTION('center_axis',(0.,0.,1.));
#31249=DIRECTION('ref_axis',(0.942731223965124,0.333553353095452,0.));
#31250=DIRECTION('center_axis',(0.,0.,1.));
#31251=DIRECTION('ref_axis',(0.942731223965124,0.333553353095452,0.));
#31252=DIRECTION('center_axis',(0.,0.,-1.));
#31253=DIRECTION('ref_axis',(0.942731223965124,0.333553353095452,0.));
#31254=DIRECTION('center_axis',(-0.18249993468442,-0.983205865442321,0.));
#31255=DIRECTION('ref_axis',(0.983205865442321,-0.182499934684419,0.));
#31256=DIRECTION('',(-0.983205865442321,0.182499934684419,0.));
#31257=DIRECTION('',(0.,0.,1.));
#31258=DIRECTION('',(0.983205865442321,-0.182499934684419,0.));
#31259=DIRECTION('',(0.,0.,-1.));
#31260=DIRECTION('',(0.,0.,1.));
#31261=DIRECTION('center_axis',(-0.430753803440728,-0.902469479163338,0.));
#31262=DIRECTION('ref_axis',(0.902469479163338,-0.430753803440728,0.));
#31263=DIRECTION('',(-0.902469479163338,0.430753803440728,0.));
#31264=DIRECTION('',(0.,0.,1.));
#31265=DIRECTION('',(0.902469479163338,-0.430753803440728,0.));
#31266=DIRECTION('',(0.,0.,-1.));
#31267=DIRECTION('',(0.,0.,1.));
#31268=DIRECTION('center_axis',(-0.649652512346868,-0.760231289280705,0.));
#31269=DIRECTION('ref_axis',(0.760231289280705,-0.649652512346868,0.));
#31270=DIRECTION('',(-0.760231289280705,0.649652512346868,0.));
#31271=DIRECTION('',(0.,0.,1.));
#31272=DIRECTION('',(0.760231289280705,-0.649652512346868,0.));
#31273=DIRECTION('',(0.,0.,-1.));
#31274=DIRECTION('',(0.,0.,1.));
#31275=DIRECTION('center_axis',(-0.824278476138108,-0.566184593375198,0.));
#31276=DIRECTION('ref_axis',(0.566184593375198,-0.824278476138108,0.));
#31277=DIRECTION('',(-0.566184593375198,0.824278476138108,0.));
#31278=DIRECTION('',(0.,0.,1.));
#31279=DIRECTION('',(0.566184593375198,-0.824278476138108,0.));
#31280=DIRECTION('',(0.,0.,-1.));
#31281=DIRECTION('',(0.,0.,1.));
#31282=DIRECTION('center_axis',(-0.942731223965124,-0.333553353095453,0.));
#31283=DIRECTION('ref_axis',(0.333553353095453,-0.942731223965124,0.));
#31284=DIRECTION('',(-0.333553353095453,0.942731223965124,0.));
#31285=DIRECTION('',(0.,0.,1.));
#31286=DIRECTION('',(0.333553353095453,-0.942731223965124,0.));
#31287=DIRECTION('',(0.,0.,-1.));
#31288=DIRECTION('',(0.,0.,1.));
#31289=DIRECTION('center_axis',(-0.996938396815926,-0.0781910030252307,
0.));
#31290=DIRECTION('ref_axis',(0.0781910030252307,-0.996938396815926,0.));
#31291=DIRECTION('',(-0.0781910030252307,0.996938396815926,0.));
#31292=DIRECTION('',(0.,0.,1.));
#31293=DIRECTION('',(0.0781910030252307,-0.996938396815926,0.));
#31294=DIRECTION('',(0.,0.,-1.));
#31295=DIRECTION('',(0.,0.,1.));
#31296=DIRECTION('center_axis',(-0.983205865442321,0.182499934684419,0.));
#31297=DIRECTION('ref_axis',(-0.182499934684419,-0.983205865442321,0.));
#31298=DIRECTION('',(0.182499934684419,0.983205865442321,0.));
#31299=DIRECTION('',(0.,0.,1.));
#31300=DIRECTION('',(-0.182499934684419,-0.983205865442321,0.));
#31301=DIRECTION('',(0.,0.,-1.));
#31302=DIRECTION('',(0.,0.,1.));
#31303=DIRECTION('center_axis',(-0.902469479163338,0.430753803440728,0.));
#31304=DIRECTION('ref_axis',(-0.430753803440728,-0.902469479163338,0.));
#31305=DIRECTION('',(0.430753803440728,0.902469479163338,0.));
#31306=DIRECTION('',(0.,0.,1.));
#31307=DIRECTION('',(-0.430753803440728,-0.902469479163338,0.));
#31308=DIRECTION('',(0.,0.,-1.));
#31309=DIRECTION('',(0.,0.,1.));
#31310=DIRECTION('center_axis',(-0.760231289280705,0.649652512346868,0.));
#31311=DIRECTION('ref_axis',(-0.649652512346868,-0.760231289280705,0.));
#31312=DIRECTION('',(0.649652512346868,0.760231289280705,0.));
#31313=DIRECTION('',(0.,0.,1.));
#31314=DIRECTION('',(-0.649652512346868,-0.760231289280705,0.));
#31315=DIRECTION('',(0.,0.,-1.));
#31316=DIRECTION('',(0.,0.,1.));
#31317=DIRECTION('center_axis',(-0.566184593375199,0.824278476138108,0.));
#31318=DIRECTION('ref_axis',(-0.824278476138108,-0.566184593375198,0.));
#31319=DIRECTION('',(0.824278476138108,0.566184593375198,0.));
#31320=DIRECTION('',(0.,0.,1.));
#31321=DIRECTION('',(-0.824278476138108,-0.566184593375198,0.));
#31322=DIRECTION('',(0.,0.,-1.));
#31323=DIRECTION('',(0.,0.,1.));
#31324=DIRECTION('center_axis',(-0.333553353095453,0.942731223965124,0.));
#31325=DIRECTION('ref_axis',(-0.942731223965124,-0.333553353095453,0.));
#31326=DIRECTION('',(0.942731223965124,0.333553353095453,0.));
#31327=DIRECTION('',(0.,0.,1.));
#31328=DIRECTION('',(-0.942731223965124,-0.333553353095453,0.));
#31329=DIRECTION('',(0.,0.,-1.));
#31330=DIRECTION('',(0.,0.,1.));
#31331=DIRECTION('center_axis',(-0.0781910030252307,0.996938396815926,0.));
#31332=DIRECTION('ref_axis',(-0.996938396815926,-0.0781910030252307,0.));
#31333=DIRECTION('',(0.996938396815926,0.0781910030252307,0.));
#31334=DIRECTION('',(0.,0.,1.));
#31335=DIRECTION('',(-0.996938396815926,-0.0781910030252307,0.));
#31336=DIRECTION('',(0.,0.,-1.));
#31337=DIRECTION('',(0.,0.,1.));
#31338=DIRECTION('center_axis',(0.182499934684419,0.983205865442321,0.));
#31339=DIRECTION('ref_axis',(-0.983205865442321,0.182499934684419,0.));
#31340=DIRECTION('',(0.983205865442321,-0.182499934684419,0.));
#31341=DIRECTION('',(0.,0.,1.));
#31342=DIRECTION('',(-0.983205865442321,0.182499934684419,0.));
#31343=DIRECTION('',(0.,0.,-1.));
#31344=DIRECTION('',(0.,0.,1.));
#31345=DIRECTION('center_axis',(0.430753803440728,0.902469479163338,0.));
#31346=DIRECTION('ref_axis',(-0.902469479163338,0.430753803440727,0.));
#31347=DIRECTION('',(0.902469479163338,-0.430753803440727,0.));
#31348=DIRECTION('',(0.,0.,1.));
#31349=DIRECTION('',(-0.902469479163338,0.430753803440727,0.));
#31350=DIRECTION('',(0.,0.,-1.));
#31351=DIRECTION('',(0.,0.,1.));
#31352=DIRECTION('center_axis',(0.649652512346868,0.760231289280705,0.));
#31353=DIRECTION('ref_axis',(-0.760231289280705,0.649652512346868,0.));
#31354=DIRECTION('',(0.760231289280705,-0.649652512346868,0.));
#31355=DIRECTION('',(0.,0.,1.));
#31356=DIRECTION('',(-0.760231289280705,0.649652512346868,0.));
#31357=DIRECTION('',(0.,0.,-1.));
#31358=DIRECTION('',(0.,0.,1.));
#31359=DIRECTION('center_axis',(0.824278476138108,0.566184593375199,0.));
#31360=DIRECTION('ref_axis',(-0.566184593375199,0.824278476138108,0.));
#31361=DIRECTION('',(0.566184593375199,-0.824278476138108,0.));
#31362=DIRECTION('',(0.,0.,1.));
#31363=DIRECTION('',(-0.566184593375199,0.824278476138108,0.));
#31364=DIRECTION('',(0.,0.,-1.));
#31365=DIRECTION('',(0.,0.,1.));
#31366=DIRECTION('center_axis',(0.942731223965124,0.333553353095453,0.));
#31367=DIRECTION('ref_axis',(-0.333553353095453,0.942731223965124,0.));
#31368=DIRECTION('',(0.333553353095453,-0.942731223965124,0.));
#31369=DIRECTION('',(0.,0.,1.));
#31370=DIRECTION('',(-0.333553353095453,0.942731223965124,0.));
#31371=DIRECTION('',(0.,0.,-1.));
#31372=DIRECTION('',(0.,0.,1.));
#31373=DIRECTION('center_axis',(0.996938396815926,0.0781910030252308,0.));
#31374=DIRECTION('ref_axis',(-0.0781910030252308,0.996938396815926,0.));
#31375=DIRECTION('',(0.0781910030252308,-0.996938396815926,0.));
#31376=DIRECTION('',(0.,0.,1.));
#31377=DIRECTION('',(-0.0781910030252308,0.996938396815926,0.));
#31378=DIRECTION('',(0.,0.,-1.));
#31379=DIRECTION('',(0.,0.,1.));
#31380=DIRECTION('center_axis',(0.983205865442321,-0.182499934684419,0.));
#31381=DIRECTION('ref_axis',(0.182499934684419,0.983205865442321,0.));
#31382=DIRECTION('',(-0.182499934684419,-0.983205865442321,0.));
#31383=DIRECTION('',(0.,0.,1.));
#31384=DIRECTION('',(0.182499934684419,0.983205865442321,0.));
#31385=DIRECTION('',(0.,0.,-1.));
#31386=DIRECTION('',(0.,0.,1.));
#31387=DIRECTION('center_axis',(0.902469479163338,-0.430753803440727,0.));
#31388=DIRECTION('ref_axis',(0.430753803440727,0.902469479163338,0.));
#31389=DIRECTION('',(-0.430753803440727,-0.902469479163338,0.));
#31390=DIRECTION('',(0.,0.,1.));
#31391=DIRECTION('',(0.430753803440727,0.902469479163338,0.));
#31392=DIRECTION('',(0.,0.,-1.));
#31393=DIRECTION('',(0.,0.,1.));
#31394=DIRECTION('center_axis',(0.760231289280705,-0.649652512346868,0.));
#31395=DIRECTION('ref_axis',(0.649652512346868,0.760231289280705,0.));
#31396=DIRECTION('',(-0.649652512346868,-0.760231289280705,0.));
#31397=DIRECTION('',(0.,0.,1.));
#31398=DIRECTION('',(0.649652512346868,0.760231289280705,0.));
#31399=DIRECTION('',(0.,0.,-1.));
#31400=DIRECTION('',(0.,0.,1.));
#31401=DIRECTION('center_axis',(0.566184593375199,-0.824278476138108,0.));
#31402=DIRECTION('ref_axis',(0.824278476138108,0.566184593375199,0.));
#31403=DIRECTION('',(-0.824278476138108,-0.566184593375199,0.));
#31404=DIRECTION('',(0.,0.,1.));
#31405=DIRECTION('',(0.824278476138108,0.566184593375199,0.));
#31406=DIRECTION('',(0.,0.,-1.));
#31407=DIRECTION('',(0.,0.,1.));
#31408=DIRECTION('center_axis',(0.333553353095453,-0.942731223965124,0.));
#31409=DIRECTION('ref_axis',(0.942731223965124,0.333553353095453,0.));
#31410=DIRECTION('',(-0.942731223965124,-0.333553353095453,0.));
#31411=DIRECTION('',(0.,0.,1.));
#31412=DIRECTION('',(0.942731223965124,0.333553353095453,0.));
#31413=DIRECTION('',(0.,0.,-1.));
#31414=DIRECTION('',(0.,0.,1.));
#31415=DIRECTION('center_axis',(0.,0.,1.));
#31416=DIRECTION('ref_axis',(1.,0.,0.));
#31417=DIRECTION('center_axis',(0.,0.,1.));
#31418=DIRECTION('ref_axis',(1.,0.,0.));
#31419=DIRECTION('center_axis',(0.,0.,1.));
#31420=DIRECTION('ref_axis',(1.,0.,0.));
#31421=DIRECTION('center_axis',(0.,0.,1.));
#31422=DIRECTION('ref_axis',(1.,0.,0.));
#31423=DIRECTION('center_axis',(0.,0.,1.));
#31424=DIRECTION('ref_axis',(1.,0.,0.));
#31425=DIRECTION('center_axis',(0.,0.,1.));
#31426=DIRECTION('ref_axis',(1.,0.,0.));
#31427=DIRECTION('center_axis',(0.,0.,1.));
#31428=DIRECTION('ref_axis',(1.,0.,0.));
#31429=DIRECTION('center_axis',(0.,0.,1.));
#31430=DIRECTION('ref_axis',(1.,0.,0.));
#31431=DIRECTION('center_axis',(0.,0.,1.));
#31432=DIRECTION('ref_axis',(1.,0.,0.));
#31433=DIRECTION('center_axis',(0.,0.,1.));
#31434=DIRECTION('ref_axis',(1.,0.,0.));
#31435=DIRECTION('center_axis',(0.,0.,1.));
#31436=DIRECTION('ref_axis',(1.,0.,0.));
#31437=DIRECTION('center_axis',(0.,0.,1.));
#31438=DIRECTION('ref_axis',(1.,0.,0.));
#31439=DIRECTION('center_axis',(0.,0.,1.));
#31440=DIRECTION('ref_axis',(1.,0.,0.));
#31441=DIRECTION('center_axis',(0.,0.,1.));
#31442=DIRECTION('ref_axis',(1.,0.,0.));
#31443=DIRECTION('center_axis',(0.,0.,1.));
#31444=DIRECTION('ref_axis',(1.,0.,0.));
#31445=DIRECTION('center_axis',(0.,0.,1.));
#31446=DIRECTION('ref_axis',(1.,0.,0.));
#31447=DIRECTION('center_axis',(0.,0.,1.));
#31448=DIRECTION('ref_axis',(1.,0.,0.));
#31449=DIRECTION('center_axis',(0.,0.,1.));
#31450=DIRECTION('ref_axis',(1.,0.,0.));
#31451=DIRECTION('center_axis',(0.,0.,1.));
#31452=DIRECTION('ref_axis',(1.,0.,0.));
#31453=DIRECTION('center_axis',(0.,0.,1.));
#31454=DIRECTION('ref_axis',(1.,0.,0.));
#31455=DIRECTION('center_axis',(0.,0.,1.));
#31456=DIRECTION('ref_axis',(1.,0.,0.));
#31457=DIRECTION('center_axis',(0.,0.,1.));
#31458=DIRECTION('ref_axis',(1.,0.,0.));
#31459=DIRECTION('center_axis',(0.,0.,1.));
#31460=DIRECTION('ref_axis',(1.,0.,0.));
#31461=DIRECTION('center_axis',(0.,0.,1.));
#31462=DIRECTION('ref_axis',(1.,0.,0.));
#31463=DIRECTION('',(-0.983205865442321,-0.182499934684418,0.));
#31464=DIRECTION('center_axis',(0.,0.,-1.));
#31465=DIRECTION('ref_axis',(-0.817790915745051,0.575515436912748,0.));
#31466=DIRECTION('center_axis',(0.,0.,-1.));
#31467=DIRECTION('ref_axis',(0.996938396815926,0.0781910030252301,0.));
#31468=DIRECTION('center_axis',(0.,0.,-1.));
#31469=DIRECTION('ref_axis',(-0.640971010199219,-0.767565087848707,0.));
#31470=DIRECTION('',(0.996938396815926,0.0781910030252308,0.));
#31471=DIRECTION('center_axis',(0.,0.,1.));
#31472=DIRECTION('ref_axis',(1.,0.,0.));
#31473=DIRECTION('center_axis',(0.,0.,-1.));
#31474=DIRECTION('ref_axis',(1.,0.,0.));
#31475=DIRECTION('center_axis',(0.,0.,1.));
#31476=DIRECTION('ref_axis',(1.,0.,0.));
#31477=DIRECTION('center_axis',(0.,0.,1.));
#31478=DIRECTION('ref_axis',(1.,0.,0.));
#31479=DIRECTION('',(-0.996938396815926,-0.0781910030252308,0.));
#31480=DIRECTION('center_axis',(0.,0.,1.));
#31481=DIRECTION('ref_axis',(-0.640971010199219,-0.767565087848707,0.));
#31482=DIRECTION('center_axis',(0.,0.,1.));
#31483=DIRECTION('ref_axis',(0.996938396815926,0.0781910030252301,0.));
#31484=DIRECTION('center_axis',(0.,0.,1.));
#31485=DIRECTION('ref_axis',(-0.817790915745051,0.575515436912748,0.));
#31486=DIRECTION('',(0.983205865442321,0.182499934684418,0.));
#31487=DIRECTION('center_axis',(0.,0.,1.));
#31488=DIRECTION('ref_axis',(1.,0.,0.));
#31489=DIRECTION('center_axis',(0.,0.,1.));
#31490=DIRECTION('ref_axis',(1.,0.,0.));
#31491=DIRECTION('center_axis',(0.,0.,1.));
#31492=DIRECTION('ref_axis',(1.,0.,0.));
#31493=DIRECTION('center_axis',(0.,0.,1.));
#31494=DIRECTION('ref_axis',(1.,0.,0.));
#31495=DIRECTION('center_axis',(0.,0.,1.));
#31496=DIRECTION('ref_axis',(1.,0.,0.));
#31497=DIRECTION('center_axis',(0.,0.,1.));
#31498=DIRECTION('ref_axis',(1.,0.,0.));
#31499=DIRECTION('center_axis',(0.,0.,1.));
#31500=DIRECTION('ref_axis',(1.,0.,0.));
#31501=DIRECTION('center_axis',(0.,0.,1.));
#31502=DIRECTION('ref_axis',(1.,0.,0.));
#31503=DIRECTION('center_axis',(0.,0.,1.));
#31504=DIRECTION('ref_axis',(1.,0.,0.));
#31505=DIRECTION('center_axis',(0.,0.,1.));
#31506=DIRECTION('ref_axis',(1.,0.,0.));
#31507=DIRECTION('center_axis',(0.,0.,1.));
#31508=DIRECTION('ref_axis',(1.,0.,0.));
#31509=DIRECTION('center_axis',(0.,0.,1.));
#31510=DIRECTION('ref_axis',(1.,0.,0.));
#31511=DIRECTION('center_axis',(0.,0.,1.));
#31512=DIRECTION('ref_axis',(1.,0.,0.));
#31513=DIRECTION('center_axis',(0.,0.,1.));
#31514=DIRECTION('ref_axis',(1.,0.,0.));
#31515=DIRECTION('center_axis',(0.,0.,1.));
#31516=DIRECTION('ref_axis',(1.,0.,0.));
#31517=DIRECTION('center_axis',(0.,0.,1.));
#31518=DIRECTION('ref_axis',(1.,0.,0.));
#31519=DIRECTION('center_axis',(0.,0.,1.));
#31520=DIRECTION('ref_axis',(1.,0.,0.));
#31521=DIRECTION('center_axis',(0.,0.,1.));
#31522=DIRECTION('ref_axis',(1.,0.,0.));
#31523=DIRECTION('center_axis',(0.,0.,1.));
#31524=DIRECTION('ref_axis',(1.,0.,0.));
#31525=DIRECTION('center_axis',(0.,0.,1.));
#31526=DIRECTION('ref_axis',(1.,0.,0.));
#31527=DIRECTION('center_axis',(0.,0.,1.));
#31528=DIRECTION('ref_axis',(1.,0.,0.));
#31529=DIRECTION('center_axis',(0.,0.,1.));
#31530=DIRECTION('ref_axis',(1.,0.,0.));
#31531=DIRECTION('center_axis',(0.,0.,1.));
#31532=DIRECTION('ref_axis',(1.,0.,0.));
#31533=DIRECTION('center_axis',(0.,0.,-1.));
#31534=DIRECTION('ref_axis',(1.,0.,0.));
#31535=DIRECTION('center_axis',(0.,0.,1.));
#31536=DIRECTION('ref_axis',(1.,0.,0.));
#31537=DIRECTION('',(0.,0.,-1.));
#31538=DIRECTION('center_axis',(0.,0.,1.));
#31539=DIRECTION('ref_axis',(1.,0.,0.));
#31540=DIRECTION('center_axis',(0.,0.,1.));
#31541=DIRECTION('ref_axis',(1.,0.,0.));
#31542=DIRECTION('center_axis',(0.,0.,1.));
#31543=DIRECTION('ref_axis',(1.,0.,0.));
#31544=DIRECTION('center_axis',(0.,0.,1.));
#31545=DIRECTION('ref_axis',(1.,0.,0.));
#31546=DIRECTION('center_axis',(0.,0.,1.));
#31547=DIRECTION('ref_axis',(1.,0.,0.));
#31548=DIRECTION('center_axis',(0.,0.,1.));
#31549=DIRECTION('ref_axis',(1.,0.,0.));
#31550=DIRECTION('center_axis',(0.,0.,1.));
#31551=DIRECTION('ref_axis',(1.,0.,0.));
#31552=DIRECTION('center_axis',(0.,0.,1.));
#31553=DIRECTION('ref_axis',(1.,0.,0.));
#31554=DIRECTION('center_axis',(0.,0.,1.));
#31555=DIRECTION('ref_axis',(1.,0.,0.));
#31556=DIRECTION('center_axis',(0.,0.,1.));
#31557=DIRECTION('ref_axis',(1.,0.,0.));
#31558=DIRECTION('center_axis',(0.,0.,1.));
#31559=DIRECTION('ref_axis',(-1.,-1.22464679914735E-16,0.));
#31560=DIRECTION('center_axis',(0.,0.,1.));
#31561=DIRECTION('ref_axis',(1.,0.,0.));
#31562=DIRECTION('center_axis',(0.,0.,1.));
#31563=DIRECTION('ref_axis',(1.,0.,0.));
#31564=DIRECTION('center_axis',(0.,0.,1.));
#31565=DIRECTION('ref_axis',(1.,0.,0.));
#31566=DIRECTION('center_axis',(0.,0.,1.));
#31567=DIRECTION('ref_axis',(1.,0.,0.));
#31568=DIRECTION('center_axis',(0.,0.,1.));
#31569=DIRECTION('ref_axis',(1.,0.,0.));
#31570=DIRECTION('center_axis',(0.,0.,1.));
#31571=DIRECTION('ref_axis',(1.,0.,0.));
#31572=DIRECTION('center_axis',(0.,0.,1.));
#31573=DIRECTION('ref_axis',(1.,0.,0.));
#31574=DIRECTION('center_axis',(0.,0.,1.));
#31575=DIRECTION('ref_axis',(1.,0.,0.));
#31576=DIRECTION('center_axis',(0.,0.,1.));
#31577=DIRECTION('ref_axis',(1.,0.,0.));
#31578=DIRECTION('center_axis',(0.,0.,1.));
#31579=DIRECTION('ref_axis',(1.,0.,0.));
#31580=DIRECTION('center_axis',(0.,0.,1.));
#31581=DIRECTION('ref_axis',(1.,0.,0.));
#31582=DIRECTION('center_axis',(0.,0.,1.));
#31583=DIRECTION('ref_axis',(-0.817790915745051,0.575515436912748,0.));
#31584=DIRECTION('',(0.,0.,1.));
#31585=DIRECTION('',(0.,0.,-1.));
#31586=DIRECTION('center_axis',(-0.182499934684418,0.983205865442321,0.));
#31587=DIRECTION('ref_axis',(-0.983205865442321,-0.182499934684418,0.));
#31588=DIRECTION('',(0.,0.,1.));
#31589=DIRECTION('center_axis',(0.,0.,1.));
#31590=DIRECTION('ref_axis',(-0.640971010199219,-0.767565087848707,0.));
#31591=DIRECTION('',(0.,0.,1.));
#31592=DIRECTION('',(0.,0.,-1.));
#31593=DIRECTION('center_axis',(0.,0.,1.));
#31594=DIRECTION('ref_axis',(0.996938396815926,0.0781910030252301,0.));
#31595=DIRECTION('center_axis',(0.0781910030252308,-0.996938396815926,0.));
#31596=DIRECTION('ref_axis',(0.996938396815926,0.0781910030252308,0.));
#31597=DIRECTION('',(0.,0.,1.));
#31598=DIRECTION('',(0.,0.,1.));
#31599=DIRECTION('center_axis',(0.,0.,1.));
#31600=DIRECTION('ref_axis',(1.,0.,0.));
#31601=DIRECTION('',(0.,0.,-1.));
#31602=DIRECTION('center_axis',(0.,0.,1.));
#31603=DIRECTION('ref_axis',(1.,0.,0.));
#31604=DIRECTION('axis',(0.,0.,1.));
#31605=DIRECTION('refdir',(1.,0.,0.));
#31606=DIRECTION('center_axis',(0.,0.,1.));
#31607=DIRECTION('ref_axis',(1.,0.,0.));
#31608=DIRECTION('center_axis',(0.,0.,-1.));
#31609=DIRECTION('ref_axis',(1.,0.,0.));
#31610=DIRECTION('',(0.,0.,-1.));
#31611=DIRECTION('center_axis',(0.,0.,-1.));
#31612=DIRECTION('ref_axis',(1.,0.,0.));
#31613=DIRECTION('center_axis',(0.,0.,1.));
#31614=DIRECTION('ref_axis',(1.,0.,0.));
#31615=DIRECTION('center_axis',(0.,0.,1.));
#31616=DIRECTION('ref_axis',(1.,0.,0.));
#31617=DIRECTION('',(0.,0.,-1.));
#31618=DIRECTION('center_axis',(0.,0.,1.));
#31619=DIRECTION('ref_axis',(1.,0.,0.));
#31620=DIRECTION('center_axis',(0.,0.,1.));
#31621=DIRECTION('ref_axis',(1.,0.,0.));
#31622=DIRECTION('center_axis',(0.,0.,1.));
#31623=DIRECTION('ref_axis',(1.,0.,0.));
#31624=DIRECTION('axis',(0.,0.,1.));
#31625=DIRECTION('refdir',(1.,0.,0.));
#31626=DIRECTION('center_axis',(0.,-1.,0.));
#31627=DIRECTION('ref_axis',(-1.,0.,0.));
#31628=DIRECTION('',(0.,0.,1.));
#31629=DIRECTION('',(-1.,0.,0.));
#31630=DIRECTION('',(0.,0.,-1.));
#31631=DIRECTION('',(1.,0.,0.));
#31632=DIRECTION('center_axis',(0.,0.,1.));
#31633=DIRECTION('ref_axis',(1.,0.,0.));
#31634=DIRECTION('center_axis',(0.,0.,1.));
#31635=DIRECTION('ref_axis',(1.,0.,0.));
#31636=DIRECTION('',(0.,-1.,0.));
#31637=DIRECTION('',(-1.,0.,0.));
#31638=DIRECTION('center_axis',(0.,1.,0.));
#31639=DIRECTION('ref_axis',(1.,0.,0.));
#31640=DIRECTION('',(0.,0.,-1.));
#31641=DIRECTION('',(0.,0.,-1.));
#31642=DIRECTION('',(1.,0.,0.));
#31643=DIRECTION('center_axis',(-1.,0.,0.));
#31644=DIRECTION('ref_axis',(0.,1.,0.));
#31645=DIRECTION('',(0.,1.,0.));
#31646=DIRECTION('center_axis',(0.,0.,-1.));
#31647=DIRECTION('ref_axis',(-1.,0.,0.));
#31648=DIRECTION('center_axis',(0.,0.,-1.));
#31649=DIRECTION('ref_axis',(1.,0.,0.));
#31650=DIRECTION('center_axis',(0.,0.,1.));
#31651=DIRECTION('ref_axis',(1.,0.,0.));
#31652=DIRECTION('center_axis',(0.,0.,1.));
#31653=DIRECTION('ref_axis',(1.,0.,0.));
#31654=DIRECTION('',(0.,0.,1.));
#31655=DIRECTION('center_axis',(0.,0.,1.));
#31656=DIRECTION('ref_axis',(1.,0.,0.));
#31657=DIRECTION('center_axis',(0.,0.,-1.));
#31658=DIRECTION('ref_axis',(-1.,0.,0.));
#31659=DIRECTION('center_axis',(0.,0.,-1.));
#31660=DIRECTION('ref_axis',(1.,0.,0.));
#31661=DIRECTION('center_axis',(0.,0.,1.));
#31662=DIRECTION('ref_axis',(1.,0.,0.));
#31663=DIRECTION('center_axis',(0.,0.,1.));
#31664=DIRECTION('ref_axis',(1.,0.,0.));
#31665=DIRECTION('center_axis',(0.,0.,1.));
#31666=DIRECTION('ref_axis',(1.,0.,0.));
#31667=DIRECTION('center_axis',(0.,0.,1.));
#31668=DIRECTION('ref_axis',(1.,0.,0.));
#31669=DIRECTION('',(0.,0.,-1.));
#31670=DIRECTION('center_axis',(0.,0.,1.));
#31671=DIRECTION('ref_axis',(1.,0.,0.));
#31672=DIRECTION('center_axis',(0.,0.,1.));
#31673=DIRECTION('ref_axis',(1.,0.,0.));
#31674=DIRECTION('',(0.,0.,1.));
#31675=DIRECTION('center_axis',(0.,0.,1.));
#31676=DIRECTION('ref_axis',(1.,0.,0.));
#31677=DIRECTION('center_axis',(0.,0.,-1.));
#31678=DIRECTION('ref_axis',(-1.,0.,0.));
#31679=DIRECTION('center_axis',(0.,0.,-1.));
#31680=DIRECTION('ref_axis',(1.,0.,0.));
#31681=DIRECTION('center_axis',(0.,0.,1.));
#31682=DIRECTION('ref_axis',(1.,0.,0.));
#31683=DIRECTION('center_axis',(0.,0.,1.));
#31684=DIRECTION('ref_axis',(1.,0.,0.));
#31685=DIRECTION('center_axis',(0.,0.,1.));
#31686=DIRECTION('ref_axis',(1.,0.,0.));
#31687=DIRECTION('center_axis',(0.,0.,1.));
#31688=DIRECTION('ref_axis',(1.,0.,0.));
#31689=DIRECTION('',(0.,0.,-1.));
#31690=DIRECTION('center_axis',(0.,0.,-1.));
#31691=DIRECTION('ref_axis',(1.,0.,0.));
#31692=DIRECTION('center_axis',(0.,0.,-1.));
#31693=DIRECTION('ref_axis',(1.,0.,0.));
#31694=DIRECTION('',(0.,0.,-1.));
#31695=DIRECTION('center_axis',(0.,0.,1.));
#31696=DIRECTION('ref_axis',(1.,0.,0.));
#31697=DIRECTION('center_axis',(0.,0.,-1.));
#31698=DIRECTION('ref_axis',(1.,0.,0.));
#31699=DIRECTION('center_axis',(0.,0.,-1.));
#31700=DIRECTION('ref_axis',(1.,0.,0.));
#31701=DIRECTION('',(0.,0.,-1.));
#31702=DIRECTION('center_axis',(0.,0.,1.));
#31703=DIRECTION('ref_axis',(1.,0.,0.));
#31704=DIRECTION('center_axis',(0.,0.,-1.));
#31705=DIRECTION('ref_axis',(1.,0.,0.));
#31706=DIRECTION('center_axis',(0.,0.,-1.));
#31707=DIRECTION('ref_axis',(1.,0.,0.));
#31708=DIRECTION('',(0.,0.,-1.));
#31709=DIRECTION('center_axis',(0.,0.,1.));
#31710=DIRECTION('ref_axis',(1.,0.,0.));
#31711=DIRECTION('center_axis',(0.,0.,1.));
#31712=DIRECTION('ref_axis',(1.,0.,0.));
#31713=DIRECTION('center_axis',(0.,0.,1.));
#31714=DIRECTION('ref_axis',(1.,0.,0.));
#31715=DIRECTION('center_axis',(0.,0.,1.));
#31716=DIRECTION('ref_axis',(1.,0.,0.));
#31717=DIRECTION('center_axis',(0.,0.,1.));
#31718=DIRECTION('ref_axis',(1.,0.,0.));
#31719=DIRECTION('center_axis',(0.,0.,1.));
#31720=DIRECTION('ref_axis',(1.,0.,0.));
#31721=DIRECTION('center_axis',(0.,0.,-1.));
#31722=DIRECTION('ref_axis',(1.,0.,0.));
#31723=DIRECTION('center_axis',(0.,0.,1.));
#31724=DIRECTION('ref_axis',(1.,0.,0.));
#31725=DIRECTION('',(0.,0.,-1.));
#31726=DIRECTION('center_axis',(0.,0.,1.));
#31727=DIRECTION('ref_axis',(1.,0.,0.));
#31728=DIRECTION('',(0.,0.,-1.));
#31729=DIRECTION('center_axis',(0.,0.,-1.));
#31730=DIRECTION('ref_axis',(1.,0.,0.));
#31731=DIRECTION('center_axis',(0.,0.,1.));
#31732=DIRECTION('ref_axis',(1.,0.,0.));
#31733=DIRECTION('',(0.,0.,-1.));
#31734=DIRECTION('center_axis',(0.,0.,1.));
#31735=DIRECTION('ref_axis',(1.,0.,0.));
#31736=DIRECTION('center_axis',(0.,0.,1.));
#31737=DIRECTION('ref_axis',(1.,0.,0.));
#31738=DIRECTION('center_axis',(0.,0.,1.));
#31739=DIRECTION('ref_axis',(1.,0.,0.));
#31740=DIRECTION('center_axis',(0.,0.,1.));
#31741=DIRECTION('ref_axis',(1.,0.,0.));
#31742=DIRECTION('center_axis',(0.,0.,1.));
#31743=DIRECTION('ref_axis',(1.,0.,0.));
#31744=DIRECTION('center_axis',(0.,0.,1.));
#31745=DIRECTION('ref_axis',(1.,0.,0.));
#31746=DIRECTION('center_axis',(0.,0.,-1.));
#31747=DIRECTION('ref_axis',(1.,0.,0.));
#31748=DIRECTION('center_axis',(0.,0.,1.));
#31749=DIRECTION('ref_axis',(1.,0.,0.));
#31750=DIRECTION('',(0.,0.,-1.));
#31751=DIRECTION('center_axis',(0.,0.,1.));
#31752=DIRECTION('ref_axis',(1.,0.,0.));
#31753=DIRECTION('',(0.,0.,-1.));
#31754=DIRECTION('center_axis',(0.,0.,-1.));
#31755=DIRECTION('ref_axis',(1.,0.,0.));
#31756=DIRECTION('center_axis',(0.,0.,1.));
#31757=DIRECTION('ref_axis',(1.,0.,0.));
#31758=DIRECTION('center_axis',(0.,0.,-1.));
#31759=DIRECTION('ref_axis',(1.,0.,0.));
#31760=DIRECTION('center_axis',(0.,0.,1.));
#31761=DIRECTION('ref_axis',(1.,0.,0.));
#31762=DIRECTION('',(0.,0.,-1.));
#31763=DIRECTION('center_axis',(0.,0.,1.));
#31764=DIRECTION('ref_axis',(1.,0.,0.));
#31765=DIRECTION('center_axis',(0.,0.,1.));
#31766=DIRECTION('ref_axis',(1.,0.,0.));
#31767=DIRECTION('',(0.,0.,-1.));
#31768=DIRECTION('center_axis',(0.,0.,-1.));
#31769=DIRECTION('ref_axis',(1.,0.,0.));
#31770=DIRECTION('center_axis',(0.,0.,1.));
#31771=DIRECTION('ref_axis',(1.,0.,0.));
#31772=DIRECTION('center_axis',(0.,0.,1.));
#31773=DIRECTION('ref_axis',(1.,0.,0.));
#31774=DIRECTION('',(0.,0.,-1.));
#31775=DIRECTION('center_axis',(0.,0.,1.));
#31776=DIRECTION('ref_axis',(1.,0.,0.));
#31777=DIRECTION('center_axis',(0.,0.,1.));
#31778=DIRECTION('ref_axis',(1.,0.,0.));
#31779=DIRECTION('center_axis',(0.,0.,1.));
#31780=DIRECTION('ref_axis',(1.,0.,0.));
#31781=DIRECTION('axis',(0.,0.,1.));
#31782=DIRECTION('refdir',(1.,0.,0.));
#31783=DIRECTION('center_axis',(0.,1.,0.));
#31784=DIRECTION('ref_axis',(-1.,0.,0.));
#31785=DIRECTION('',(-1.,0.,0.));
#31786=DIRECTION('',(0.,0.,1.));
#31787=DIRECTION('',(-1.,0.,0.));
#31788=DIRECTION('',(0.,0.,1.));
#31789=DIRECTION('center_axis',(1.,0.,0.));
#31790=DIRECTION('ref_axis',(0.,1.,0.));
#31791=DIRECTION('',(0.,1.,0.));
#31792=DIRECTION('',(0.,1.,0.));
#31793=DIRECTION('',(0.,0.,1.));
#31794=DIRECTION('center_axis',(0.,-1.,0.));
#31795=DIRECTION('ref_axis',(1.,0.,0.));
#31796=DIRECTION('',(1.,0.,0.));
#31797=DIRECTION('',(1.,0.,0.));
#31798=DIRECTION('',(0.,0.,1.));
#31799=DIRECTION('center_axis',(-1.,0.,0.));
#31800=DIRECTION('ref_axis',(0.,-1.,0.));
#31801=DIRECTION('',(0.,-1.,0.));
#31802=DIRECTION('',(0.,-1.,0.));
#31803=DIRECTION('center_axis',(0.,0.,1.));
#31804=DIRECTION('ref_axis',(1.,0.,0.));
#31805=DIRECTION('center_axis',(0.,0.,1.));
#31806=DIRECTION('ref_axis',(1.,0.,0.));
#31807=DIRECTION('axis',(0.,0.,1.));
#31808=DIRECTION('refdir',(1.,0.,0.));
#31809=DIRECTION('center_axis',(0.,0.,1.));
#31810=DIRECTION('ref_axis',(1.,0.,0.));
#31811=DIRECTION('center_axis',(0.,0.,-1.));
#31812=DIRECTION('ref_axis',(1.,0.,0.));
#31813=DIRECTION('',(0.,0.,-1.));
#31814=DIRECTION('center_axis',(0.,0.,-1.));
#31815=DIRECTION('ref_axis',(1.,0.,0.));
#31816=DIRECTION('center_axis',(0.,0.,1.));
#31817=DIRECTION('ref_axis',(1.,0.,0.));
#31818=DIRECTION('center_axis',(0.,0.,1.));
#31819=DIRECTION('ref_axis',(1.,0.,0.));
#31820=DIRECTION('',(0.,0.,-1.));
#31821=DIRECTION('center_axis',(0.,0.,1.));
#31822=DIRECTION('ref_axis',(1.,0.,0.));
#31823=DIRECTION('center_axis',(0.,0.,1.));
#31824=DIRECTION('ref_axis',(1.,0.,0.));
#31825=DIRECTION('center_axis',(0.,0.,1.));
#31826=DIRECTION('ref_axis',(1.,0.,0.));
#31827=DIRECTION('axis',(0.,0.,1.));
#31828=DIRECTION('refdir',(1.,0.,0.));
#31829=DIRECTION('center_axis',(0.,0.,1.));
#31830=DIRECTION('ref_axis',(1.,0.,0.));
#31831=DIRECTION('center_axis',(0.,0.,1.));
#31832=DIRECTION('ref_axis',(1.,0.,0.));
#31833=DIRECTION('',(0.,0.,1.));
#31834=DIRECTION('center_axis',(0.,0.,1.));
#31835=DIRECTION('ref_axis',(1.,0.,0.));
#31836=DIRECTION('center_axis',(0.,0.,-1.));
#31837=DIRECTION('ref_axis',(-1.,0.,0.));
#31838=DIRECTION('center_axis',(0.,0.,-1.));
#31839=DIRECTION('ref_axis',(1.,0.,0.));
#31840=DIRECTION('center_axis',(0.,0.,1.));
#31841=DIRECTION('ref_axis',(1.,0.,0.));
#31842=DIRECTION('center_axis',(0.,0.,1.));
#31843=DIRECTION('ref_axis',(1.,0.,0.));
#31844=DIRECTION('center_axis',(0.,0.,1.));
#31845=DIRECTION('ref_axis',(1.,0.,0.));
#31846=DIRECTION('center_axis',(0.,0.,1.));
#31847=DIRECTION('ref_axis',(1.,0.,0.));
#31848=DIRECTION('',(0.,0.,-1.));
#31849=DIRECTION('center_axis',(0.,0.,1.));
#31850=DIRECTION('ref_axis',(1.,0.,0.));
#31851=DIRECTION('center_axis',(0.,0.,1.));
#31852=DIRECTION('ref_axis',(1.,0.,0.));
#31853=DIRECTION('center_axis',(0.,0.,1.));
#31854=DIRECTION('ref_axis',(1.,0.,0.));
#31855=DIRECTION('center_axis',(0.,0.,1.));
#31856=DIRECTION('ref_axis',(1.,0.,0.));
#31857=DIRECTION('',(0.,0.,-1.));
#31858=DIRECTION('center_axis',(0.,0.,1.));
#31859=DIRECTION('ref_axis',(1.,0.,0.));
#31860=DIRECTION('center_axis',(0.,0.,1.));
#31861=DIRECTION('ref_axis',(1.,0.,0.));
#31862=DIRECTION('center_axis',(0.,0.,1.));
#31863=DIRECTION('ref_axis',(1.,0.,0.));
#31864=DIRECTION('',(0.,0.,-1.));
#31865=DIRECTION('center_axis',(0.,0.,1.));
#31866=DIRECTION('ref_axis',(1.,0.,0.));
#31867=DIRECTION('axis',(0.,0.,1.));
#31868=DIRECTION('refdir',(1.,0.,0.));
#31869=DIRECTION('center_axis',(-1.,0.,0.));
#31870=DIRECTION('ref_axis',(0.,1.,0.));
#31871=DIRECTION('',(0.,0.,1.));
#31872=DIRECTION('',(0.,-1.,0.));
#31873=DIRECTION('',(0.,0.,-1.));
#31874=DIRECTION('',(0.,1.,0.));
#31875=DIRECTION('center_axis',(1.,0.,0.));
#31876=DIRECTION('ref_axis',(0.,-1.,0.));
#31877=DIRECTION('',(0.,0.,-1.));
#31878=DIRECTION('',(0.,-1.,0.));
#31879=DIRECTION('',(0.,0.,1.));
#31880=DIRECTION('',(0.,1.,0.));
#31881=DIRECTION('center_axis',(0.,0.,1.));
#31882=DIRECTION('ref_axis',(1.,0.,0.));
#31883=DIRECTION('center_axis',(0.,0.,1.));
#31884=DIRECTION('ref_axis',(1.,0.,0.));
#31885=DIRECTION('center_axis',(0.,0.,-1.));
#31886=DIRECTION('ref_axis',(1.,0.,0.));
#31887=DIRECTION('center_axis',(0.,0.,1.));
#31888=DIRECTION('ref_axis',(6.12323399573677E-17,-1.,0.));
#31889=DIRECTION('center_axis',(0.,0.,-1.));
#31890=DIRECTION('ref_axis',(1.,0.,0.));
#31891=DIRECTION('center_axis',(0.,0.,1.));
#31892=DIRECTION('ref_axis',(6.12323399573677E-17,-1.,0.));
#31893=DIRECTION('center_axis',(0.,0.,1.));
#31894=DIRECTION('ref_axis',(1.,0.,0.));
#31895=DIRECTION('center_axis',(0.,0.,1.));
#31896=DIRECTION('ref_axis',(1.,0.,0.));
#31897=DIRECTION('axis',(0.,0.,1.));
#31898=DIRECTION('refdir',(1.,0.,0.));
#31899=DIRECTION('center_axis',(0.,0.,1.));
#31900=DIRECTION('ref_axis',(1.,0.,0.));
#31901=DIRECTION('center_axis',(0.,0.,-1.));
#31902=DIRECTION('ref_axis',(1.,0.,0.));
#31903=DIRECTION('',(0.,0.,-1.));
#31904=DIRECTION('center_axis',(0.,0.,-1.));
#31905=DIRECTION('ref_axis',(1.,0.,0.));
#31906=DIRECTION('center_axis',(0.,0.,1.));
#31907=DIRECTION('ref_axis',(1.,0.,0.));
#31908=DIRECTION('center_axis',(0.,0.,1.));
#31909=DIRECTION('ref_axis',(1.,0.,0.));
#31910=DIRECTION('',(0.,0.,-1.));
#31911=DIRECTION('center_axis',(0.,0.,1.));
#31912=DIRECTION('ref_axis',(1.,0.,0.));
#31913=DIRECTION('center_axis',(0.,0.,1.));
#31914=DIRECTION('ref_axis',(1.,0.,0.));
#31915=DIRECTION('center_axis',(0.,0.,1.));
#31916=DIRECTION('ref_axis',(1.,0.,0.));
#31917=DIRECTION('axis',(0.,0.,1.));
#31918=DIRECTION('refdir',(1.,0.,0.));
#31919=DIRECTION('center_axis',(0.,0.,1.));
#31920=DIRECTION('ref_axis',(1.,0.,0.));
#31921=DIRECTION('center_axis',(0.,0.,-1.));
#31922=DIRECTION('ref_axis',(1.,0.,0.));
#31923=DIRECTION('',(0.,0.,-1.));
#31924=DIRECTION('center_axis',(0.,0.,-1.));
#31925=DIRECTION('ref_axis',(1.,0.,0.));
#31926=DIRECTION('center_axis',(0.,0.,1.));
#31927=DIRECTION('ref_axis',(1.,0.,0.));
#31928=DIRECTION('center_axis',(0.,0.,1.));
#31929=DIRECTION('ref_axis',(1.,0.,0.));
#31930=DIRECTION('',(0.,0.,-1.));
#31931=DIRECTION('center_axis',(0.,0.,1.));
#31932=DIRECTION('ref_axis',(1.,0.,0.));
#31933=DIRECTION('center_axis',(0.,0.,1.));
#31934=DIRECTION('ref_axis',(1.,0.,0.));
#31935=DIRECTION('center_axis',(0.,0.,1.));
#31936=DIRECTION('ref_axis',(1.,0.,0.));
#31937=DIRECTION('axis',(0.,0.,1.));
#31938=DIRECTION('refdir',(1.,0.,0.));
#31939=DIRECTION('center_axis',(0.,0.,1.));
#31940=DIRECTION('ref_axis',(1.,0.,0.));
#31941=DIRECTION('center_axis',(0.,0.,-1.));
#31942=DIRECTION('ref_axis',(1.,0.,0.));
#31943=DIRECTION('',(0.,0.,-1.));
#31944=DIRECTION('center_axis',(0.,0.,-1.));
#31945=DIRECTION('ref_axis',(1.,0.,0.));
#31946=DIRECTION('center_axis',(0.,0.,1.));
#31947=DIRECTION('ref_axis',(1.,0.,0.));
#31948=DIRECTION('center_axis',(0.,0.,1.));
#31949=DIRECTION('ref_axis',(1.,0.,0.));
#31950=DIRECTION('',(0.,0.,-1.));
#31951=DIRECTION('center_axis',(0.,0.,1.));
#31952=DIRECTION('ref_axis',(1.,0.,0.));
#31953=DIRECTION('center_axis',(0.,0.,1.));
#31954=DIRECTION('ref_axis',(1.,0.,0.));
#31955=DIRECTION('center_axis',(0.,0.,1.));
#31956=DIRECTION('ref_axis',(1.,0.,0.));
#31957=DIRECTION('axis',(0.,0.,1.));
#31958=DIRECTION('refdir',(1.,0.,0.));
#31959=DIRECTION('center_axis',(-1.,0.,0.));
#31960=DIRECTION('ref_axis',(0.,1.,0.));
#31961=DIRECTION('',(0.,0.,1.));
#31962=DIRECTION('',(0.,-1.,0.));
#31963=DIRECTION('',(0.,0.,-1.));
#31964=DIRECTION('',(0.,1.,0.));
#31965=DIRECTION('center_axis',(1.,0.,0.));
#31966=DIRECTION('ref_axis',(0.,-1.,0.));
#31967=DIRECTION('',(0.,0.,-1.));
#31968=DIRECTION('',(0.,-1.,0.));
#31969=DIRECTION('',(0.,0.,1.));
#31970=DIRECTION('',(0.,1.,0.));
#31971=DIRECTION('center_axis',(0.,0.,1.));
#31972=DIRECTION('ref_axis',(1.,0.,0.));
#31973=DIRECTION('center_axis',(0.,0.,1.));
#31974=DIRECTION('ref_axis',(1.,0.,0.));
#31975=DIRECTION('center_axis',(0.,0.,-1.));
#31976=DIRECTION('ref_axis',(1.,0.,0.));
#31977=DIRECTION('center_axis',(0.,0.,1.));
#31978=DIRECTION('ref_axis',(6.12323399573677E-17,-1.,0.));
#31979=DIRECTION('center_axis',(0.,0.,-1.));
#31980=DIRECTION('ref_axis',(1.,0.,0.));
#31981=DIRECTION('center_axis',(0.,0.,1.));
#31982=DIRECTION('ref_axis',(6.12323399573677E-17,-1.,0.));
#31983=DIRECTION('center_axis',(0.,0.,1.));
#31984=DIRECTION('ref_axis',(1.,0.,0.));
#31985=DIRECTION('center_axis',(0.,0.,1.));
#31986=DIRECTION('ref_axis',(1.,0.,0.));
#31987=DIRECTION('axis',(0.,0.,1.));
#31988=DIRECTION('refdir',(1.,0.,0.));
#31989=DIRECTION('center_axis',(-1.,0.,0.));
#31990=DIRECTION('ref_axis',(0.,1.,0.));
#31991=DIRECTION('',(0.,0.,1.));
#31992=DIRECTION('',(0.,-1.,0.));
#31993=DIRECTION('',(0.,0.,-1.));
#31994=DIRECTION('',(0.,1.,0.));
#31995=DIRECTION('center_axis',(1.,0.,0.));
#31996=DIRECTION('ref_axis',(0.,-1.,0.));
#31997=DIRECTION('',(0.,0.,-1.));
#31998=DIRECTION('',(0.,-1.,0.));
#31999=DIRECTION('',(0.,0.,1.));
#32000=DIRECTION('',(0.,1.,0.));
#32001=DIRECTION('center_axis',(0.,0.,1.));
#32002=DIRECTION('ref_axis',(1.,0.,0.));
#32003=DIRECTION('center_axis',(0.,0.,1.));
#32004=DIRECTION('ref_axis',(1.,0.,0.));
#32005=DIRECTION('center_axis',(0.,0.,-1.));
#32006=DIRECTION('ref_axis',(1.,0.,0.));
#32007=DIRECTION('center_axis',(0.,0.,1.));
#32008=DIRECTION('ref_axis',(6.12323399573676E-17,-1.,0.));
#32009=DIRECTION('center_axis',(0.,0.,-1.));
#32010=DIRECTION('ref_axis',(1.,0.,0.));
#32011=DIRECTION('center_axis',(0.,0.,1.));
#32012=DIRECTION('ref_axis',(6.12323399573677E-17,-1.,0.));
#32013=DIRECTION('center_axis',(0.,0.,1.));
#32014=DIRECTION('ref_axis',(1.,0.,0.));
#32015=DIRECTION('center_axis',(0.,0.,1.));
#32016=DIRECTION('ref_axis',(1.,0.,0.));
#32017=DIRECTION('axis',(0.,0.,1.));
#32018=DIRECTION('refdir',(1.,0.,0.));
#32019=DIRECTION('center_axis',(0.,0.,1.));
#32020=DIRECTION('ref_axis',(1.,0.,0.));
#32021=DIRECTION('center_axis',(0.,0.,1.));
#32022=DIRECTION('ref_axis',(1.,0.,0.));
#32023=DIRECTION('',(0.,0.,-1.));
#32024=DIRECTION('center_axis',(0.,0.,1.));
#32025=DIRECTION('ref_axis',(1.,0.,0.));
#32026=DIRECTION('center_axis',(0.,0.,1.));
#32027=DIRECTION('ref_axis',(1.,0.,0.));
#32028=DIRECTION('center_axis',(0.,0.,1.));
#32029=DIRECTION('ref_axis',(1.,0.,0.));
#32030=DIRECTION('axis',(0.,0.,1.));
#32031=DIRECTION('refdir',(1.,0.,0.));
#32032=DIRECTION('center_axis',(0.,0.,1.));
#32033=DIRECTION('ref_axis',(1.,0.,0.));
#32034=DIRECTION('',(0.,0.,-1.));
#32035=DIRECTION('center_axis',(0.,0.,-1.));
#32036=DIRECTION('ref_axis',(1.,0.,0.));
#32037=DIRECTION('center_axis',(0.,0.,1.));
#32038=DIRECTION('ref_axis',(1.,0.,0.));
#32039=DIRECTION('',(0.,0.,-1.));
#32040=DIRECTION('center_axis',(0.,0.,1.));
#32041=DIRECTION('ref_axis',(1.,0.,0.));
#32042=DIRECTION('',(0.,0.,-1.));
#32043=DIRECTION('center_axis',(0.,0.,1.));
#32044=DIRECTION('ref_axis',(1.,0.,0.));
#32045=DIRECTION('',(0.,0.,-1.));
#32046=DIRECTION('center_axis',(0.,0.,1.));
#32047=DIRECTION('ref_axis',(1.,0.,0.));
#32048=DIRECTION('',(0.,0.,-1.));
#32049=DIRECTION('center_axis',(0.,0.,1.));
#32050=DIRECTION('ref_axis',(1.,0.,0.));
#32051=DIRECTION('',(0.,0.,-1.));
#32052=DIRECTION('center_axis',(0.,0.,1.));
#32053=DIRECTION('ref_axis',(1.,0.,0.));
#32054=DIRECTION('',(0.,0.,-1.));
#32055=DIRECTION('center_axis',(0.,0.,1.));
#32056=DIRECTION('ref_axis',(1.,0.,0.));
#32057=DIRECTION('',(0.,0.,-1.));
#32058=DIRECTION('center_axis',(0.,0.,1.));
#32059=DIRECTION('ref_axis',(1.,0.,0.));
#32060=DIRECTION('',(0.,0.,-1.));
#32061=DIRECTION('center_axis',(0.,0.,1.));
#32062=DIRECTION('ref_axis',(1.,0.,0.));
#32063=DIRECTION('',(0.,0.,-1.));
#32064=DIRECTION('center_axis',(0.,0.,1.));
#32065=DIRECTION('ref_axis',(1.,0.,0.));
#32066=DIRECTION('',(0.,0.,-1.));
#32067=DIRECTION('center_axis',(0.,0.,1.));
#32068=DIRECTION('ref_axis',(1.,0.,0.));
#32069=DIRECTION('',(0.,0.,-1.));
#32070=DIRECTION('center_axis',(0.,0.,1.));
#32071=DIRECTION('ref_axis',(1.,0.,0.));
#32072=DIRECTION('',(0.,0.,-1.));
#32073=DIRECTION('center_axis',(0.,0.,1.));
#32074=DIRECTION('ref_axis',(1.,0.,0.));
#32075=DIRECTION('',(0.,0.,-1.));
#32076=DIRECTION('center_axis',(0.,0.,1.));
#32077=DIRECTION('ref_axis',(1.,0.,0.));
#32078=DIRECTION('',(0.,0.,-1.));
#32079=DIRECTION('center_axis',(0.,0.,1.));
#32080=DIRECTION('ref_axis',(1.,0.,0.));
#32081=DIRECTION('',(0.,0.,-1.));
#32082=DIRECTION('center_axis',(0.,0.,1.));
#32083=DIRECTION('ref_axis',(1.,0.,0.));
#32084=DIRECTION('',(0.,0.,-1.));
#32085=DIRECTION('center_axis',(0.,0.,1.));
#32086=DIRECTION('ref_axis',(1.,0.,0.));
#32087=DIRECTION('',(0.,0.,-1.));
#32088=DIRECTION('center_axis',(0.,0.,1.));
#32089=DIRECTION('ref_axis',(1.,0.,0.));
#32090=DIRECTION('',(0.,0.,-1.));
#32091=DIRECTION('center_axis',(0.,0.,1.));
#32092=DIRECTION('ref_axis',(1.,0.,0.));
#32093=DIRECTION('',(0.,0.,-1.));
#32094=DIRECTION('center_axis',(0.,0.,1.));
#32095=DIRECTION('ref_axis',(-0.45780573334585,-0.889052254097401,0.));
#32096=DIRECTION('',(0.,0.,1.));
#32097=DIRECTION('center_axis',(0.,0.,1.));
#32098=DIRECTION('ref_axis',(1.,7.52212518638754E-14,0.));
#32099=DIRECTION('center_axis',(0.,0.,1.));
#32100=DIRECTION('ref_axis',(1.,7.52212518638754E-14,0.));
#32101=DIRECTION('',(0.,0.,1.));
#32102=DIRECTION('center_axis',(0.,0.,1.));
#32103=DIRECTION('ref_axis',(1.,7.52212518638754E-14,0.));
#32104=DIRECTION('',(0.,0.,1.));
#32105=DIRECTION('center_axis',(0.,0.,1.));
#32106=DIRECTION('ref_axis',(1.,7.52212518638754E-14,0.));
#32107=DIRECTION('',(0.,0.,1.));
#32108=DIRECTION('center_axis',(0.,0.,1.));
#32109=DIRECTION('ref_axis',(1.,7.52212518638754E-14,0.));
#32110=DIRECTION('',(0.,0.,1.));
#32111=DIRECTION('center_axis',(0.,0.,1.));
#32112=DIRECTION('ref_axis',(1.,7.52212518638754E-14,0.));
#32113=DIRECTION('',(0.,0.,1.));
#32114=DIRECTION('center_axis',(0.,0.,1.));
#32115=DIRECTION('ref_axis',(1.,7.52212518638754E-14,0.));
#32116=DIRECTION('',(0.,0.,1.));
#32117=DIRECTION('center_axis',(0.,0.,1.));
#32118=DIRECTION('ref_axis',(1.,7.52212518638754E-14,0.));
#32119=DIRECTION('',(0.,0.,1.));
#32120=DIRECTION('center_axis',(0.,0.,1.));
#32121=DIRECTION('ref_axis',(1.,7.52212518638754E-14,0.));
#32122=DIRECTION('',(0.,0.,1.));
#32123=DIRECTION('center_axis',(0.,0.,1.));
#32124=DIRECTION('ref_axis',(1.,7.52212518638754E-14,0.));
#32125=DIRECTION('',(0.,0.,1.));
#32126=DIRECTION('center_axis',(0.,0.,1.));
#32127=DIRECTION('ref_axis',(1.,7.52212518638754E-14,0.));
#32128=DIRECTION('',(0.,0.,1.));
#32129=DIRECTION('center_axis',(0.,0.,1.));
#32130=DIRECTION('ref_axis',(1.,7.52212518638754E-14,0.));
#32131=DIRECTION('',(0.,0.,1.));
#32132=DIRECTION('center_axis',(0.,0.,1.));
#32133=DIRECTION('ref_axis',(1.,7.52212518638754E-14,0.));
#32134=DIRECTION('',(0.,0.,1.));
#32135=DIRECTION('center_axis',(0.,0.,1.));
#32136=DIRECTION('ref_axis',(1.,7.52212518638754E-14,0.));
#32137=DIRECTION('',(0.,0.,1.));
#32138=DIRECTION('center_axis',(0.,0.,1.));
#32139=DIRECTION('ref_axis',(1.,7.52212518638754E-14,0.));
#32140=DIRECTION('',(0.,0.,1.));
#32141=DIRECTION('center_axis',(0.,0.,1.));
#32142=DIRECTION('ref_axis',(1.,7.52212518638754E-14,0.));
#32143=DIRECTION('',(0.,0.,1.));
#32144=DIRECTION('center_axis',(0.,0.,1.));
#32145=DIRECTION('ref_axis',(1.,7.52212518638754E-14,0.));
#32146=DIRECTION('',(0.,0.,1.));
#32147=DIRECTION('center_axis',(0.,0.,1.));
#32148=DIRECTION('ref_axis',(1.,7.52212518638754E-14,0.));
#32149=DIRECTION('',(0.,0.,1.));
#32150=DIRECTION('center_axis',(0.,0.,1.));
#32151=DIRECTION('ref_axis',(1.,7.52212518638754E-14,0.));
#32152=DIRECTION('',(0.,0.,1.));
#32153=DIRECTION('center_axis',(0.,0.,1.));
#32154=DIRECTION('ref_axis',(1.,7.52212518638754E-14,0.));
#32155=DIRECTION('',(0.,0.,1.));
#32156=DIRECTION('center_axis',(0.,0.,1.));
#32157=DIRECTION('ref_axis',(1.,7.52212518638754E-14,0.));
#32158=DIRECTION('center_axis',(0.,0.,-1.));
#32159=DIRECTION('ref_axis',(1.,7.52212518638754E-14,0.));
#32160=DIRECTION('center_axis',(0.,0.,1.));
#32161=DIRECTION('ref_axis',(1.,0.,0.));
#32162=DIRECTION('center_axis',(0.,0.,-1.));
#32163=DIRECTION('ref_axis',(1.,0.,0.));
#32164=DIRECTION('center_axis',(-1.92296268638356E-16,-1.,0.));
#32165=DIRECTION('ref_axis',(1.,-1.92296268638356E-16,0.));
#32166=DIRECTION('',(1.,-1.92296268638356E-16,0.));
#32167=DIRECTION('',(0.,0.,1.));
#32168=DIRECTION('',(1.,-1.92296268638356E-16,0.));
#32169=DIRECTION('',(0.,0.,1.));
#32170=DIRECTION('center_axis',(-0.866025403784439,-0.5,0.));
#32171=DIRECTION('ref_axis',(0.5,-0.866025403784439,0.));
#32172=DIRECTION('',(0.5,-0.866025403784439,0.));
#32173=DIRECTION('',(0.,0.,1.));
#32174=DIRECTION('',(0.5,-0.866025403784439,0.));
#32175=DIRECTION('center_axis',(-0.866025403784439,0.5,0.));
#32176=DIRECTION('ref_axis',(-0.5,-0.866025403784438,0.));
#32177=DIRECTION('',(-0.5,-0.866025403784438,0.));
#32178=DIRECTION('',(0.,0.,1.));
#32179=DIRECTION('',(-0.5,-0.866025403784439,0.));
#32180=DIRECTION('center_axis',(1.92296268638356E-16,1.,0.));
#32181=DIRECTION('ref_axis',(-1.,1.92296268638356E-16,0.));
#32182=DIRECTION('',(-1.,1.92296268638356E-16,0.));
#32183=DIRECTION('',(0.,0.,1.));
#32184=DIRECTION('',(-1.,1.92296268638356E-16,0.));
#32185=DIRECTION('center_axis',(0.866025403784439,0.5,0.));
#32186=DIRECTION('ref_axis',(-0.5,0.866025403784439,0.));
#32187=DIRECTION('',(-0.5,0.866025403784439,0.));
#32188=DIRECTION('',(0.,0.,1.));
#32189=DIRECTION('',(-0.5,0.866025403784439,0.));
#32190=DIRECTION('center_axis',(0.866025403784439,-0.5,0.));
#32191=DIRECTION('ref_axis',(0.5,0.866025403784439,0.));
#32192=DIRECTION('',(0.5,0.866025403784439,0.));
#32193=DIRECTION('',(0.5,0.866025403784439,0.));
#32194=DIRECTION('center_axis',(0.,0.,1.));
#32195=DIRECTION('ref_axis',(1.,0.,0.));
#32196=DIRECTION('center_axis',(0.,0.,1.));
#32197=DIRECTION('ref_axis',(1.,0.,0.));
#32198=DIRECTION('center_axis',(0.,0.,1.));
#32199=DIRECTION('ref_axis',(1.,0.,0.));
#32200=DIRECTION('center_axis',(0.,0.,1.));
#32201=DIRECTION('ref_axis',(1.,0.,0.));
#32202=DIRECTION('',(0.,0.,-1.));
#32203=DIRECTION('center_axis',(0.,0.,1.));
#32204=DIRECTION('ref_axis',(1.,0.,0.));
#32205=DIRECTION('center_axis',(0.,0.,1.));
#32206=DIRECTION('ref_axis',(1.,0.,0.));
#32207=DIRECTION('center_axis',(0.,0.,1.));
#32208=DIRECTION('ref_axis',(1.,0.,0.));
#32209=DIRECTION('',(0.,0.,1.));
#32210=DIRECTION('',(1.,0.,0.));
#32211=DIRECTION('',(0.,0.,1.));
#32212=DIRECTION('',(0.99144486137381,0.130526192220052,0.));
#32213=DIRECTION('',(0.,0.,1.));
#32214=DIRECTION('',(1.,0.,0.));
#32215=DIRECTION('',(0.,0.,1.));
#32216=DIRECTION('',(0.99144486137381,0.130526192220052,0.));
#32217=DIRECTION('',(0.,0.,1.));
#32218=DIRECTION('',(0.99144486137381,0.130526192220052,0.));
#32219=DIRECTION('',(0.,0.,1.));
#32220=DIRECTION('',(1.,0.,0.));
#32221=DIRECTION('',(0.,0.,1.));
#32222=DIRECTION('',(1.,0.,0.));
#32223=DIRECTION('',(0.,0.,1.));
#32224=DIRECTION('',(1.,0.,0.));
#32225=DIRECTION('',(0.,0.,1.));
#32226=DIRECTION('',(1.,0.,0.));
#32227=DIRECTION('',(0.,0.,1.));
#32228=DIRECTION('',(1.,0.,0.));
#32229=DIRECTION('',(0.,0.,1.));
#32230=DIRECTION('',(1.,0.,0.));
#32231=DIRECTION('',(0.,0.,1.));
#32232=DIRECTION('',(1.,0.,0.));
#32233=DIRECTION('',(0.,0.,1.));
#32234=DIRECTION('',(1.,0.,0.));
#32235=DIRECTION('',(0.,0.,1.));
#32236=DIRECTION('',(1.,0.,0.));
#32237=DIRECTION('',(0.,0.,1.));
#32238=DIRECTION('',(1.,0.,0.));
#32239=DIRECTION('',(0.,0.,1.));
#32240=DIRECTION('',(0.99144486137381,0.130526192220052,0.));
#32241=DIRECTION('',(0.,0.,1.));
#32242=DIRECTION('',(0.99144486137381,0.130526192220052,0.));
#32243=DIRECTION('',(0.,0.,1.));
#32244=DIRECTION('',(0.99144486137381,0.130526192220052,0.));
#32245=DIRECTION('',(0.,0.,1.));
#32246=DIRECTION('',(1.,0.,0.));
#32247=DIRECTION('',(0.,0.,1.));
#32248=DIRECTION('',(1.,0.,0.));
#32249=DIRECTION('',(0.,0.,1.));
#32250=DIRECTION('',(1.,0.,0.));
#32251=DIRECTION('',(0.,0.,1.));
#32252=DIRECTION('',(1.,0.,0.));
#32253=DIRECTION('',(0.,0.,1.));
#32254=DIRECTION('',(1.,0.,0.));
#32255=DIRECTION('',(0.,0.,1.));
#32256=DIRECTION('',(1.,0.,0.));
#32257=DIRECTION('',(0.,0.,1.));
#32258=DIRECTION('',(1.,0.,0.));
#32259=DIRECTION('',(0.,0.,1.));
#32260=DIRECTION('',(1.,0.,0.));
#32261=DIRECTION('',(0.,0.,1.));
#32262=DIRECTION('',(1.,0.,0.));
#32263=DIRECTION('',(0.,0.,1.));
#32264=DIRECTION('',(1.,0.,0.));
#32265=DIRECTION('',(0.,0.,1.));
#32266=DIRECTION('',(1.,0.,0.));
#32267=DIRECTION('',(0.,0.,1.));
#32268=DIRECTION('',(1.,0.,0.));
#32269=DIRECTION('',(0.,0.,1.));
#32270=DIRECTION('',(1.,0.,0.));
#32271=DIRECTION('',(0.,0.,1.));
#32272=DIRECTION('',(1.,0.,0.));
#32273=DIRECTION('',(0.,0.,1.));
#32274=DIRECTION('',(1.,0.,0.));
#32275=DIRECTION('',(0.,0.,1.));
#32276=DIRECTION('',(1.,0.,0.));
#32277=DIRECTION('',(-1.,0.,-1.22464679914735E-16));
#32278=DIRECTION('',(0.,1.,0.));
#32279=DIRECTION('',(0.,-1.22464679914735E-16,-1.));
#32280=DIRECTION('',(1.,0.,0.));
#32281=DIRECTION('',(0.,0.,1.));
#32282=DIRECTION('',(1.,0.,0.));
#32283=DIRECTION('',(0.,0.,1.));
#32284=DIRECTION('',(1.,0.,0.));
#32285=DIRECTION('',(0.,0.,1.));
#32286=DIRECTION('',(1.,0.,0.));
#32287=DIRECTION('',(0.,0.,1.));
#32288=DIRECTION('',(1.,0.,0.));
#32289=DIRECTION('',(0.,0.,1.));
#32290=DIRECTION('',(1.,0.,0.));
#32291=DIRECTION('',(0.,0.,1.));
#32292=DIRECTION('',(1.,0.,0.));
#32293=DIRECTION('',(0.,0.,1.));
#32294=DIRECTION('',(1.,0.,0.));
#32295=DIRECTION('',(0.,0.,1.));
#32296=DIRECTION('',(1.,0.,0.));
#32297=DIRECTION('',(0.,0.,1.));
#32298=DIRECTION('',(1.,0.,0.));
#32299=DIRECTION('',(0.,0.,1.));
#32300=DIRECTION('',(1.,0.,0.));
#32301=DIRECTION('',(0.,0.,1.));
#32302=DIRECTION('',(1.,0.,0.));
#32303=DIRECTION('',(0.,0.,1.));
#32304=DIRECTION('',(1.,0.,0.));
#32305=DIRECTION('',(0.,0.,1.));
#32306=DIRECTION('',(1.,0.,0.));
#32307=DIRECTION('',(0.,0.,1.));
#32308=DIRECTION('',(1.,0.,0.));
#32309=DIRECTION('',(0.,0.,1.));
#32310=DIRECTION('',(1.,0.,0.));
#32311=DIRECTION('',(0.,0.,1.));
#32312=DIRECTION('',(1.,0.,0.));
#32313=DIRECTION('',(0.,0.,1.));
#32314=DIRECTION('',(1.,0.,0.));
#32315=DIRECTION('',(0.,0.,1.));
#32316=DIRECTION('',(1.,0.,0.));
#32317=DIRECTION('',(0.,0.,1.));
#32318=DIRECTION('',(1.,0.,0.));
#32319=DIRECTION('',(0.,0.,1.));
#32320=DIRECTION('',(1.,0.,0.));
#32321=DIRECTION('',(0.,0.,1.));
#32322=DIRECTION('',(1.,0.,0.));
#32323=DIRECTION('',(0.,0.,1.));
#32324=DIRECTION('',(1.,0.,0.));
#32325=DIRECTION('',(0.,0.,1.));
#32326=DIRECTION('',(1.,0.,0.));
#32327=DIRECTION('',(0.,0.,1.));
#32328=DIRECTION('',(1.,0.,0.));
#32329=DIRECTION('',(0.,0.,1.));
#32330=DIRECTION('',(1.,0.,0.));
#32331=DIRECTION('',(0.,0.,1.));
#32332=DIRECTION('',(1.,0.,0.));
#32333=DIRECTION('',(0.,0.,1.));
#32334=DIRECTION('',(1.,0.,0.));
#32335=DIRECTION('',(0.,0.,1.));
#32336=DIRECTION('',(1.,0.,0.));
#32337=DIRECTION('',(0.,0.,1.));
#32338=DIRECTION('',(1.,0.,0.));
#32339=DIRECTION('',(0.,0.,1.));
#32340=DIRECTION('',(1.,0.,0.));
#32341=DIRECTION('',(0.,0.,1.));
#32342=DIRECTION('',(1.,0.,0.));
#32343=DIRECTION('',(0.,0.,1.));
#32344=DIRECTION('',(1.,0.,0.));
#32345=DIRECTION('',(0.,0.,1.));
#32346=DIRECTION('',(1.,0.,0.));
#32347=DIRECTION('',(0.,0.,1.));
#32348=DIRECTION('',(1.,0.,0.));
#32349=DIRECTION('',(0.,0.,1.));
#32350=DIRECTION('',(1.,0.,0.));
#32351=DIRECTION('',(0.,0.,1.));
#32352=DIRECTION('',(1.,0.,0.));
#32353=DIRECTION('',(0.,0.,1.));
#32354=DIRECTION('',(1.,0.,0.));
#32355=DIRECTION('',(0.,0.,1.));
#32356=DIRECTION('',(1.,0.,0.));
#32357=DIRECTION('',(0.,0.,1.));
#32358=DIRECTION('',(1.,0.,0.));
#32359=DIRECTION('',(0.,0.,1.));
#32360=DIRECTION('',(1.,0.,0.));
#32361=DIRECTION('',(0.,0.,1.));
#32362=DIRECTION('',(1.,0.,0.));
#32363=DIRECTION('',(0.,0.,1.));
#32364=DIRECTION('',(1.,0.,0.));
#32365=DIRECTION('',(0.,0.,1.));
#32366=DIRECTION('',(1.,0.,0.));
#32367=DIRECTION('',(0.,0.,1.));
#32368=DIRECTION('',(1.,0.,0.));
#32369=DIRECTION('',(1.,0.,0.));
#32370=DIRECTION('',(0.,1.,0.));
#32371=DIRECTION('',(0.,-1.,-9.9579925010296E-17));
#32372=DIRECTION('',(1.,0.,0.));
#32373=DIRECTION('',(0.,1.,2.22044604925031E-16));
#32374=DIRECTION('',(1.,0.,0.));
#32375=DIRECTION('',(-1.,0.,-1.22464679914735E-16));
#32376=DIRECTION('',(0.,1.,0.));
#32377=DIRECTION('',(1.,0.,0.));
#32378=DIRECTION('',(0.,1.,0.));
#32379=DIRECTION('',(0.,-1.,-9.9579925010296E-17));
#32380=DIRECTION('',(1.,0.,0.));
#32381=DIRECTION('',(0.,1.,2.22044604925031E-16));
#32382=DIRECTION('',(1.,0.,0.));
#32383=DIRECTION('',(-1.,0.,-1.22464679914735E-16));
#32384=DIRECTION('',(0.,1.,0.));
#32385=DIRECTION('',(1.,0.,0.));
#32386=DIRECTION('',(0.,1.,0.));
#32387=DIRECTION('',(0.,-1.,-9.9579925010296E-17));
#32388=DIRECTION('',(1.,0.,0.));
#32389=DIRECTION('',(0.,1.,2.22044604925031E-16));
#32390=DIRECTION('',(1.,0.,0.));
#32391=DIRECTION('',(0.,-1.22464679914735E-16,-1.));
#32392=DIRECTION('',(1.,0.,0.));
#32393=DIRECTION('',(0.,-1.22464679914735E-16,-1.));
#32394=DIRECTION('',(1.,0.,0.));
#32395=DIRECTION('',(0.,-1.22464679914735E-16,-1.));
#32396=DIRECTION('',(1.,0.,0.));
#32397=DIRECTION('',(0.,-1.22464679914735E-16,-1.));
#32398=DIRECTION('',(1.,0.,0.));
#32399=DIRECTION('',(0.,-1.22464679914735E-16,-1.));
#32400=DIRECTION('',(1.,0.,0.));
#32401=DIRECTION('',(0.,-1.22464679914735E-16,-1.));
#32402=DIRECTION('',(1.,0.,0.));
#32403=DIRECTION('',(0.,-1.22464679914735E-16,-1.));
#32404=DIRECTION('',(1.,0.,0.));
#32405=CARTESIAN_POINT('',(0.,0.,0.));
#32406=CARTESIAN_POINT('',(0.,0.,0.));
#32407=CARTESIAN_POINT('Origin',(-87.7685555885722,36.3549260746835,114.));
#32408=CARTESIAN_POINT('',(-90.2820657582583,36.3551835591638,107.387416697508));
#32409=CARTESIAN_POINT('',(-90.2841460151391,36.3513531397369,107.112583302492));
#32410=CARTESIAN_POINT('',(-90.2860555885722,36.3549260746835,114.));
#32411=CARTESIAN_POINT('',(-89.6820215852369,37.990913278059,107.));
#32412=CARTESIAN_POINT('Ctrl Pts',(-90.2841460151391,36.3513531397369,107.112583302492));
#32413=CARTESIAN_POINT('Ctrl Pts',(-90.2790007066056,36.9439878981613,107.075055534995));
#32414=CARTESIAN_POINT('Ctrl Pts',(-90.0677774166561,37.5397296349884,107.037527767497));
#32415=CARTESIAN_POINT('Ctrl Pts',(-89.6820215852368,37.9909132780591,107.));
#32416=CARTESIAN_POINT('',(-90.2860555885722,36.3549260746835,107.));
#32417=CARTESIAN_POINT('Origin',(-87.7685555885722,36.3549260746835,107.));
#32418=CARTESIAN_POINT('',(-90.2860555885722,36.3549260746835,106.));
#32419=CARTESIAN_POINT('',(-90.2860555885722,36.3549260746835,114.));
#32420=CARTESIAN_POINT('Origin',(-87.7685555885722,36.3549260746835,106.));
#32421=CARTESIAN_POINT('',(-85.8514453951333,37.9934539829853,107.));
#32422=CARTESIAN_POINT('Origin',(-87.7685555885722,36.3549260746835,107.));
#32423=CARTESIAN_POINT('Ctrl Pts',(-85.8514365495282,37.9934601500707,107.));
#32424=CARTESIAN_POINT('Ctrl Pts',(-86.3742571255242,38.6021753146346,107.050946273303));
#32425=CARTESIAN_POINT('Ctrl Pts',(-87.2139815880401,38.9423514879707,107.101892546605));
#32426=CARTESIAN_POINT('Ctrl Pts',(-88.0126524090168,38.8645886693614,107.152838819908));
#32427=CARTESIAN_POINT('Ctrl Pts',(-88.8380243712328,38.7842260863082,107.205488327639));
#32428=CARTESIAN_POINT('Ctrl Pts',(-89.6195517979231,38.2575123321297,107.25813783537));
#32429=CARTESIAN_POINT('Ctrl Pts',(-90.0034364012539,37.5227256169419,107.3107873431));
#32430=CARTESIAN_POINT('Ctrl Pts',(-90.1896795438024,37.1662409188007,107.336330461236));
#32431=CARTESIAN_POINT('Ctrl Pts',(-90.2823277522487,36.7607811758956,107.361873579372));
#32432=CARTESIAN_POINT('Ctrl Pts',(-90.2820657582583,36.3551835591638,107.387416697508));
#32433=CARTESIAN_POINT('Origin',(-87.7685555885722,36.3549260746835,114.));
#32434=CARTESIAN_POINT('',(-90.2873602755412,36.3528305926337,108.387416697508));
#32435=CARTESIAN_POINT('',(-90.2899626058712,36.3555923892882,108.112583302492));
#32436=CARTESIAN_POINT('',(-90.2860555885722,36.3549260746835,114.));
#32437=CARTESIAN_POINT('Ctrl Pts',(-90.2899626058712,36.3555923892882,108.112583302492));
#32438=CARTESIAN_POINT('Ctrl Pts',(-90.2900904417905,36.392049525674,108.110268755777));
#32439=CARTESIAN_POINT('Ctrl Pts',(-90.2893674908555,36.4285014253324,108.107954209062));
#32440=CARTESIAN_POINT('Ctrl Pts',(-90.2877778743739,36.4649154267611,108.105639662347));
#32441=CARTESIAN_POINT('Ctrl Pts',(-90.2516185155238,37.2932327976625,108.052990154616));
#32442=CARTESIAN_POINT('Ctrl Pts',(-89.7670151124418,38.1019402561809,108.000340646886));
#32443=CARTESIAN_POINT('Ctrl Pts',(-89.053640710259,38.5245019232063,107.947691139155));
#32444=CARTESIAN_POINT('Ctrl Pts',(-88.3402663080762,38.9470635902317,107.895041631424));
#32445=CARTESIAN_POINT('Ctrl Pts',(-87.3981209067927,38.9834794657641,107.842392123693));
#32446=CARTESIAN_POINT('Ctrl Pts',(-86.6543416914832,38.6170777740084,107.789742615962));
#32447=CARTESIAN_POINT('Ctrl Pts',(-85.9105624761737,38.2506760822528,107.737093108232));
#32448=CARTESIAN_POINT('Ctrl Pts',(-85.3651494468382,37.481456823209,107.684443600501));
#32449=CARTESIAN_POINT('Ctrl Pts',(-85.2652957945526,36.6584694678107,107.63179409277));
#32450=CARTESIAN_POINT('Ctrl Pts',(-85.1654421422671,35.8354821124124,107.579144585039));
#32451=CARTESIAN_POINT('Ctrl Pts',(-85.5111478670314,34.9587266606595,107.526495077308));
#32452=CARTESIAN_POINT('Ctrl Pts',(-86.145817826788,34.4249747642233,107.473845569577));
#32453=CARTESIAN_POINT('Ctrl Pts',(-86.7804877865446,33.891222867787,107.421196061847));
#32454=CARTESIAN_POINT('Ctrl Pts',(-87.7041219812935,33.7004745266674,107.368546554116));
#32455=CARTESIAN_POINT('Ctrl Pts',(-88.4977390142088,33.940628476657,107.315897046385));
#32456=CARTESIAN_POINT('Ctrl Pts',(-89.291356047124,34.1807824266467,107.263247538654));
#32457=CARTESIAN_POINT('Ctrl Pts',(-89.9549559182057,34.8518386677455,107.210598030923));
#32458=CARTESIAN_POINT('Ctrl Pts',(-90.1879211493143,35.6461245790433,107.157948523192));
#32459=CARTESIAN_POINT('Ctrl Pts',(-90.2548323106925,35.8742555861396,107.142826782959));
#32460=CARTESIAN_POINT('Ctrl Pts',(-90.2862193071108,36.1125521273703,107.127705042726));
#32461=CARTESIAN_POINT('Ctrl Pts',(-90.2841460151391,36.3513531397369,107.112583302492));
#32462=CARTESIAN_POINT('Ctrl Pts',(-90.2820657582583,36.3551835591638,107.387416697508));
#32463=CARTESIAN_POINT('Ctrl Pts',(-90.2817877299011,35.9247628501715,107.414523087103));
#32464=CARTESIAN_POINT('Ctrl Pts',(-90.1768790488432,35.4941868748242,107.441629476698));
#32465=CARTESIAN_POINT('Ctrl Pts',(-89.968158017258,35.1218194639909,107.468735866293));
#32466=CARTESIAN_POINT('Ctrl Pts',(-89.5627532499601,34.3985597024246,107.521385374024));
#32467=CARTESIAN_POINT('Ctrl Pts',(-88.765701935393,33.8948998554888,107.574034881755));
#32468=CARTESIAN_POINT('Ctrl Pts',(-87.9384522457069,33.8390488807469,107.626684389485));
#32469=CARTESIAN_POINT('Ctrl Pts',(-87.1112025560208,33.7831979060051,107.679333897216));
#32470=CARTESIAN_POINT('Ctrl Pts',(-86.2537544912156,34.1751558034572,107.731983404947));
#32471=CARTESIAN_POINT('Ctrl Pts',(-85.754762161375,34.8372915889621,107.784632912678));
#32472=CARTESIAN_POINT('Ctrl Pts',(-85.2557698315344,35.499427374467,107.837282420409));
#32473=CARTESIAN_POINT('Ctrl Pts',(-85.1152332366584,36.4317410480246,107.889931928139));
#32474=CARTESIAN_POINT('Ctrl Pts',(-85.3968901882336,37.2115545845095,107.94258143587));
#32475=CARTESIAN_POINT('Ctrl Pts',(-85.6785471398087,37.9913681209943,107.995230943601));
#32476=CARTESIAN_POINT('Ctrl Pts',(-86.3823976378351,38.6186815204063,108.047880451332));
#32477=CARTESIAN_POINT('Ctrl Pts',(-87.1893483010309,38.8091253099958,108.100529959063));
#32478=CARTESIAN_POINT('Ctrl Pts',(-87.9962989642267,38.9995690995853,108.153179466794));
#32479=CARTESIAN_POINT('Ctrl Pts',(-88.906349792592,38.7531432793523,108.205828974524));
#32480=CARTESIAN_POINT('Ctrl Pts',(-89.5069496277807,38.1815546745416,108.258478482255));
#32481=CARTESIAN_POINT('Ctrl Pts',(-89.9972376612814,37.7149493966099,108.30145788734));
#32482=CARTESIAN_POINT('Ctrl Pts',(-90.2813088913625,37.0316570454253,108.344437292424));
#32483=CARTESIAN_POINT('Ctrl Pts',(-90.2873602755412,36.3528305926337,108.387416697508));
#32484=CARTESIAN_POINT('Origin',(-87.7685555885722,36.3549260746835,114.));
#32485=CARTESIAN_POINT('',(-90.2882104573874,36.3567838325376,109.387416697508));
#32486=CARTESIAN_POINT('',(-90.2831163782917,36.3564540169858,109.112583302492));
#32487=CARTESIAN_POINT('',(-90.2860555885722,36.3549260746835,114.));
#32488=CARTESIAN_POINT('Ctrl Pts',(-90.2831163782917,36.3564540169858,109.112583302492));
#32489=CARTESIAN_POINT('Ctrl Pts',(-90.2848726336429,36.6697453384204,109.092832468829));
#32490=CARTESIAN_POINT('Ctrl Pts',(-90.2305754403938,36.982449840124,109.073081635165));
#32491=CARTESIAN_POINT('Ctrl Pts',(-90.1174358665212,37.2721760255534,109.053330801502));
#32492=CARTESIAN_POINT('Ctrl Pts',(-89.8158413631797,38.0444948703993,109.000681293771));
#32493=CARTESIAN_POINT('Ctrl Pts',(-89.0961200626589,38.6535325956426,108.94803178604));
#32494=CARTESIAN_POINT('Ctrl Pts',(-88.2845464797145,38.8231922589131,108.89538227831));
#32495=CARTESIAN_POINT('Ctrl Pts',(-87.47297289677,38.9928519221836,108.842732770579));
#32496=CARTESIAN_POINT('Ctrl Pts',(-86.5695470314019,38.7231335234814,108.790083262848));
#32497=CARTESIAN_POINT('Ctrl Pts',(-85.9838236566503,38.1363076402997,108.737433755117));
#32498=CARTESIAN_POINT('Ctrl Pts',(-85.3981002818987,37.549481757118,108.684784247386));
#32499=CARTESIAN_POINT('Ctrl Pts',(-85.1300793977636,36.6455483894568,108.632134739655));
#32500=CARTESIAN_POINT('Ctrl Pts',(-85.3012633835703,35.8342964195734,108.579485231925));
#32501=CARTESIAN_POINT('Ctrl Pts',(-85.472447369377,35.02304444969,108.526835724194));
#32502=CARTESIAN_POINT('Ctrl Pts',(-86.0828362251256,34.3044738775844,108.474186216463));
#32503=CARTESIAN_POINT('Ctrl Pts',(-86.8557211165975,34.0043286221669,108.421536708732));
#32504=CARTESIAN_POINT('Ctrl Pts',(-87.6286060080694,33.7041833667494,108.368887201001));
#32505=CARTESIAN_POINT('Ctrl Pts',(-88.5639869352647,33.8224634280202,108.316237693271));
#32506=CARTESIAN_POINT('Ctrl Pts',(-89.2378197415534,34.3055671002978,108.26358818554));
#32507=CARTESIAN_POINT('Ctrl Pts',(-89.8820299060469,34.7674328528715,108.213253224524));
#32508=CARTESIAN_POINT('Ctrl Pts',(-90.2871825297673,35.5627509543319,108.162918263508));
#32509=CARTESIAN_POINT('Ctrl Pts',(-90.2899626058712,36.3555923892882,108.112583302492));
#32510=CARTESIAN_POINT('Ctrl Pts',(-90.2873602755412,36.3528305926337,108.387416697508));
#32511=CARTESIAN_POINT('Ctrl Pts',(-90.2887217998816,36.2000988024933,108.397086800155));
#32512=CARTESIAN_POINT('Ctrl Pts',(-90.2760093365286,36.0475930861384,108.406756902801));
#32513=CARTESIAN_POINT('Ctrl Pts',(-90.248405070806,35.8978323082241,108.416427005448));
#32514=CARTESIAN_POINT('Ctrl Pts',(-90.0981118366304,35.0824499361056,108.469076513179));
#32515=CARTESIAN_POINT('Ctrl Pts',(-89.506376526267,34.3484365812571,108.521726020909));
#32516=CARTESIAN_POINT('Ctrl Pts',(-88.7414548919972,34.0285444819078,108.57437552864));
#32517=CARTESIAN_POINT('Ctrl Pts',(-87.9765332577274,33.7086523825585,108.627025036371));
#32518=CARTESIAN_POINT('Ctrl Pts',(-87.0384252995513,33.8028815387084,108.679674544102));
#32519=CARTESIAN_POINT('Ctrl Pts',(-86.3524072420719,34.2685153510835,108.732324051833));
#32520=CARTESIAN_POINT('Ctrl Pts',(-85.6663891845924,34.7341491634585,108.784973559563));
#32521=CARTESIAN_POINT('Ctrl Pts',(-85.2324610278097,35.5711876320587,108.837623067294));
#32522=CARTESIAN_POINT('Ctrl Pts',(-85.2473378688992,36.4001717283435,108.890272575025));
#32523=CARTESIAN_POINT('Ctrl Pts',(-85.2622147099887,37.2291558246283,108.942922082756));
#32524=CARTESIAN_POINT('Ctrl Pts',(-85.7258965489504,38.0500855485976,108.995571590487));
#32525=CARTESIAN_POINT('Ctrl Pts',(-86.4281800972607,38.4908050723096,109.048221098218));
#32526=CARTESIAN_POINT('Ctrl Pts',(-87.130463645571,38.9315245960216,109.100870605948));
#32527=CARTESIAN_POINT('Ctrl Pts',(-88.0713489032298,38.9920339194763,109.153520113679));
#32528=CARTESIAN_POINT('Ctrl Pts',(-88.824299933075,38.6449019741468,109.20616962141));
#32529=CARTESIAN_POINT('Ctrl Pts',(-89.5772509629203,38.2977700288173,109.258819129141));
#32530=CARTESIAN_POINT('Ctrl Pts',(-90.142267764952,37.5429968147038,109.311468636872));
#32531=CARTESIAN_POINT('Ctrl Pts',(-90.2632085219966,36.7227473329821,109.364118144603));
#32532=CARTESIAN_POINT('Ctrl Pts',(-90.2810481609466,36.6017545844628,109.371884328904));
#32533=CARTESIAN_POINT('Ctrl Pts',(-90.2892254201477,36.4793371777813,109.379650513206));
#32534=CARTESIAN_POINT('Ctrl Pts',(-90.2882104573874,36.3567838325376,109.387416697508));
#32535=CARTESIAN_POINT('Origin',(-87.7685555885722,36.3549260746835,114.));
#32536=CARTESIAN_POINT('',(-90.2821395661149,36.3552114620833,110.387416697508));
#32537=CARTESIAN_POINT('',(-90.284691711587,36.3528024297121,110.112583302492));
#32538=CARTESIAN_POINT('',(-90.2860555885722,36.3549260746835,114.));
#32539=CARTESIAN_POINT('Ctrl Pts',(-90.284691711587,36.3528024297121,110.112583302492));
#32540=CARTESIAN_POINT('Ctrl Pts',(-90.2798922469406,36.9417394945665,110.07539618188));
#32541=CARTESIAN_POINT('Ctrl Pts',(-90.0733337455156,37.5337101378598,110.038209061269));
#32542=CARTESIAN_POINT('Ctrl Pts',(-89.6956382082861,37.9812527577399,110.001021940657));
#32543=CARTESIAN_POINT('Ctrl Pts',(-89.1608970457506,38.6148833867763,109.948372432926));
#32544=CARTESIAN_POINT('Ctrl Pts',(-88.2831136976804,38.9590097330537,109.895722925195));
#32545=CARTESIAN_POINT('Ctrl Pts',(-87.4602178940962,38.8576273644157,109.843073417464));
#32546=CARTESIAN_POINT('Ctrl Pts',(-86.6373220905121,38.7562449957777,109.790423909734));
#32547=CARTESIAN_POINT('Ctrl Pts',(-85.869313831414,38.2093539122244,109.737774402003));
#32548=CARTESIAN_POINT('Ctrl Pts',(-85.5043579873302,37.4648788415031,109.685124894272));
#32549=CARTESIAN_POINT('Ctrl Pts',(-85.1394021432465,36.7204037707817,109.632475386541));
#32550=CARTESIAN_POINT('Ctrl Pts',(-85.177498714177,35.7783447128923,109.57982587881));
#32551=CARTESIAN_POINT('Ctrl Pts',(-85.6013771882749,35.0657698746485,109.52717637108));
#32552=CARTESIAN_POINT('Ctrl Pts',(-86.0252556623728,34.3531950364047,109.474526863349));
#32553=CARTESIAN_POINT('Ctrl Pts',(-86.8349160396379,33.8701044178065,109.421877355618));
#32554=CARTESIAN_POINT('Ctrl Pts',(-87.6633111224845,33.8354996839412,109.369227847887));
#32555=CARTESIAN_POINT('Ctrl Pts',(-88.491706205331,33.8008949500758,109.316578340156));
#32556=CARTESIAN_POINT('Ctrl Pts',(-89.338835993759,34.2147761009433,109.263928832425));
#32557=CARTESIAN_POINT('Ctrl Pts',(-89.8206670348919,34.8895166586012,109.211279324695));
#32558=CARTESIAN_POINT('Ctrl Pts',(-90.1217449188274,35.3111363592072,109.178380650627));
#32559=CARTESIAN_POINT('Ctrl Pts',(-90.2801910095015,35.8346092560125,109.145481976559));
#32560=CARTESIAN_POINT('Ctrl Pts',(-90.2831163782917,36.3564540169858,109.112583302492));
#32561=CARTESIAN_POINT('Ctrl Pts',(-90.2882104573874,36.3567838325376,109.387416697508));
#32562=CARTESIAN_POINT('Ctrl Pts',(-90.2823446550742,35.6485078995844,109.432300020937));
#32563=CARTESIAN_POINT('Ctrl Pts',(-89.9694528690476,34.935691533327,109.477183344366));
#32564=CARTESIAN_POINT('Ctrl Pts',(-89.4402911475608,34.4671003638404,109.522066667795));
#32565=CARTESIAN_POINT('Ctrl Pts',(-88.8195683040227,33.9174286257501,109.574716175526));
#32566=CARTESIAN_POINT('Ctrl Pts',(-87.9012579048889,33.7038108988991,109.627365683257));
#32567=CARTESIAN_POINT('Ctrl Pts',(-87.1016619950835,33.9230875413012,109.680015190987));
#32568=CARTESIAN_POINT('Ctrl Pts',(-86.3020660852782,34.1423641837033,109.732664698718));
#32569=CARTESIAN_POINT('Ctrl Pts',(-85.6211846648011,34.7945351953585,109.785314206449));
#32570=CARTESIAN_POINT('Ctrl Pts',(-85.3676849764274,35.5839487607172,109.83796371418));
#32571=CARTESIAN_POINT('Ctrl Pts',(-85.1141852880536,36.3733623260759,109.890613221911));
#32572=CARTESIAN_POINT('Ctrl Pts',(-85.2880673317831,37.3000184451381,109.943262729642));
#32573=CARTESIAN_POINT('Ctrl Pts',(-85.8105043249304,37.9438316601752,109.995912237372));
#32574=CARTESIAN_POINT('Ctrl Pts',(-86.3329413180777,38.5876448752124,110.048561745103));
#32575=CARTESIAN_POINT('Ctrl Pts',(-87.2039332606428,38.9486151862244,110.101211252834));
#32576=CARTESIAN_POINT('Ctrl Pts',(-88.0286292016189,38.8631021907732,110.153860760565));
#32577=CARTESIAN_POINT('Ctrl Pts',(-88.8533251425949,38.777589195322,110.206510268296));
#32578=CARTESIAN_POINT('Ctrl Pts',(-89.6317250819818,38.2455928934076,110.259159776027));
#32579=CARTESIAN_POINT('Ctrl Pts',(-90.0109532436846,37.5082857190933,110.311809283757));
#32580=CARTESIAN_POINT('Ctrl Pts',(-90.1924836559242,37.1553486516045,110.337011755008));
#32581=CARTESIAN_POINT('Ctrl Pts',(-90.2825485383685,36.7553670064009,110.362214226258));
#32582=CARTESIAN_POINT('Ctrl Pts',(-90.2821395661149,36.3552114620833,110.387416697508));
#32583=CARTESIAN_POINT('Origin',(-87.7685555885722,36.3549260746835,114.));
#32584=CARTESIAN_POINT('',(-90.2872022523859,36.3527998634328,111.387416697508));
#32585=CARTESIAN_POINT('',(-90.2900214059965,36.35548699916,111.112583302492));
#32586=CARTESIAN_POINT('',(-90.2860555885722,36.3549260746835,114.));
#32587=CARTESIAN_POINT('Ctrl Pts',(-90.2900214059965,36.35548699916,111.112583302492));
#32588=CARTESIAN_POINT('Ctrl Pts',(-90.2901161298337,36.3865769482408,111.110609402663));
#32589=CARTESIAN_POINT('Ctrl Pts',(-90.289590328231,36.4176636198089,111.108635502833));
#32590=CARTESIAN_POINT('Ctrl Pts',(-90.2884340218591,36.4487268212695,111.106661603004));
#32591=CARTESIAN_POINT('Ctrl Pts',(-90.2575920508711,37.2772705199817,111.054012095273));
#32592=CARTESIAN_POINT('Ctrl Pts',(-89.7781836309555,38.089116640287,111.001362587543));
#32593=CARTESIAN_POINT('Ctrl Pts',(-89.0675412790233,38.5162270890477,110.948713079812));
#32594=CARTESIAN_POINT('Ctrl Pts',(-88.3568989270911,38.9433375378084,110.896063572081));
#32595=CARTESIAN_POINT('Ctrl Pts',(-87.4150226431423,38.9857123150244,110.84341406435));
#32596=CARTESIAN_POINT('Ctrl Pts',(-86.6688977175355,38.6241414600135,110.790764556619));
#32597=CARTESIAN_POINT('Ctrl Pts',(-85.9227727919286,38.2625706050026,110.738115048888));
#32598=CARTESIAN_POINT('Ctrl Pts',(-85.3723992246636,37.4970541177647,110.685465541158));
#32599=CARTESIAN_POINT('Ctrl Pts',(-85.2672805031015,36.6746272563465,110.632816033427));
#32600=CARTESIAN_POINT('Ctrl Pts',(-85.1621617815393,35.8522003949283,110.580166525696));
#32601=CARTESIAN_POINT('Ctrl Pts',(-85.50229790568,34.9728631593298,110.527517017965));
#32602=CARTESIAN_POINT('Ctrl Pts',(-86.1334933358886,34.4352497141681,110.474867510234));
#32603=CARTESIAN_POINT('Ctrl Pts',(-86.7646887660972,33.8976362690064,110.422218002503));
#32604=CARTESIAN_POINT('Ctrl Pts',(-87.6869435023737,33.7017466142814,110.369568494773));
#32605=CARTESIAN_POINT('Ctrl Pts',(-88.4821673848742,33.9363843445116,110.316918987042));
#32606=CARTESIAN_POINT('Ctrl Pts',(-89.2773912673748,34.1710220747418,110.264269479311));
#32607=CARTESIAN_POINT('Ctrl Pts',(-89.9455842960992,34.8361871899272,110.21161997158));
#32608=CARTESIAN_POINT('Ctrl Pts',(-90.183831321961,35.6303372034176,110.158970463849));
#32609=CARTESIAN_POINT('Ctrl Pts',(-90.25380097415,35.8635673981236,110.14350807673));
#32610=CARTESIAN_POINT('Ctrl Pts',(-90.2866873267115,36.1079226773738,110.128045689611));
#32611=CARTESIAN_POINT('Ctrl Pts',(-90.284691711587,36.3528024297121,110.112583302492));
#32612=CARTESIAN_POINT('Ctrl Pts',(-90.2821395661149,36.3552114620833,110.387416697508));
#32613=CARTESIAN_POINT('Ctrl Pts',(-90.2816941702547,35.9194175387913,110.414863733989));
#32614=CARTESIAN_POINT('Ctrl Pts',(-90.1739418475738,35.4834173616642,110.442310770469));
#32615=CARTESIAN_POINT('Ctrl Pts',(-89.9601635310367,35.1077531359413,110.46975780695));
#32616=CARTESIAN_POINT('Ctrl Pts',(-89.5500892726676,34.3871457738176,110.522407314681));
#32617=CARTESIAN_POINT('Ctrl Pts',(-88.7498843719111,33.8885490962844,110.575056822411));
#32618=CARTESIAN_POINT('Ctrl Pts',(-87.9223095518277,33.8379943251671,110.627706330142));
#32619=CARTESIAN_POINT('Ctrl Pts',(-87.0947347317443,33.7874395540498,110.680355837873));
#32620=CARTESIAN_POINT('Ctrl Pts',(-86.2397899923339,34.1849266893484,110.733005345604));
#32621=CARTESIAN_POINT('Ctrl Pts',(-85.7450515302878,34.8502609827235,110.785654853335));
#32622=CARTESIAN_POINT('Ctrl Pts',(-85.2503130682416,35.5155952760986,110.838304361066));
#32623=CARTESIAN_POINT('Ctrl Pts',(-85.1157808835598,36.4487767275502,110.890953868796));
#32624=CARTESIAN_POINT('Ctrl Pts',(-85.4024430963309,37.2267617168094,110.943603376527));
#32625=CARTESIAN_POINT('Ctrl Pts',(-85.689105309102,38.0047467060685,110.996252884258));
#32626=CARTESIAN_POINT('Ctrl Pts',(-86.3969619193261,38.6275352331353,111.048902391989));
#32627=CARTESIAN_POINT('Ctrl Pts',(-87.205116897016,38.8127955898771,111.10155189972));
#32628=CARTESIAN_POINT('Ctrl Pts',(-88.0132718747059,38.9980559466188,111.154201407451));
#32629=CARTESIAN_POINT('Ctrl Pts',(-88.9217252198616,38.7457881330357,111.206850915181));
#32630=CARTESIAN_POINT('Ctrl Pts',(-89.5186434231292,38.1703539262337,111.259500422912));
#32631=CARTESIAN_POINT('Ctrl Pts',(-90.0020639151804,37.7043324749317,111.302139181111));
#32632=CARTESIAN_POINT('Ctrl Pts',(-90.2811565836147,37.0263545637827,111.344777939309));
#32633=CARTESIAN_POINT('Ctrl Pts',(-90.2872022523859,36.3527998634328,111.387416697508));
#32634=CARTESIAN_POINT('Origin',(-87.7685555885722,36.3549260746835,114.));
#32635=CARTESIAN_POINT('',(-90.2883544400146,36.356729971742,112.387416697508));
#32636=CARTESIAN_POINT('',(-90.2832192959692,36.3565168099065,112.112583302492));
#32637=CARTESIAN_POINT('',(-90.2860555885722,36.3549260746835,114.));
#32638=CARTESIAN_POINT('Ctrl Pts',(-90.2832192959692,36.3565168099065,112.112583302492));
#32639=CARTESIAN_POINT('Ctrl Pts',(-90.2850210486953,36.6643730370269,112.093173115714));
#32640=CARTESIAN_POINT('Ctrl Pts',(-90.2326348324987,36.9716374824648,112.073762928937));
#32641=CARTESIAN_POINT('Ctrl Pts',(-90.1232771295477,37.2570748224305,112.054352742159));
#32642=CARTESIAN_POINT('Ctrl Pts',(-89.8266478753891,38.0313144322456,112.001703234428));
#32643=CARTESIAN_POINT('Ctrl Pts',(-89.1108519400598,38.6449615091715,111.949053726697));
#32644=CARTESIAN_POINT('Ctrl Pts',(-88.3003845258671,38.8198284824987,111.896404218966));
#32645=CARTESIAN_POINT('Ctrl Pts',(-87.4899171116743,38.9946954558259,111.843754711236));
#32646=CARTESIAN_POINT('Ctrl Pts',(-86.584778218618,38.7307823255544,111.791105203505));
#32647=CARTESIAN_POINT('Ctrl Pts',(-85.9952987995873,38.1477300960177,111.738455695774));
#32648=CARTESIAN_POINT('Ctrl Pts',(-85.4058193805567,37.564677866481,111.685806188043));
#32649=CARTESIAN_POINT('Ctrl Pts',(-85.1319994355516,36.6624865376791,111.633156680312));
#32650=CARTESIAN_POINT('Ctrl Pts',(-85.2979710727125,35.8501508290649,111.580507172582));
#32651=CARTESIAN_POINT('Ctrl Pts',(-85.4639427098734,35.0378151204507,111.527857664851));
#32652=CARTESIAN_POINT('Ctrl Pts',(-86.0697059292002,34.3153350320242,111.47520815712));
#32653=CARTESIAN_POINT('Ctrl Pts',(-86.840647186937,34.0102359252646,111.422558649389));
#32654=CARTESIAN_POINT('Ctrl Pts',(-87.6115884446739,33.7051368185049,111.369909141658));
#32655=CARTESIAN_POINT('Ctrl Pts',(-88.5477077408209,33.8174186934119,111.317259633927));
#32656=CARTESIAN_POINT('Ctrl Pts',(-89.2246296278641,34.2961802694251,111.264610126197));
#32657=CARTESIAN_POINT('Ctrl Pts',(-89.876172816134,34.7569924393774,111.213934518295));
#32658=CARTESIAN_POINT('Ctrl Pts',(-90.2875895763982,35.5573198146224,111.163258910394));
#32659=CARTESIAN_POINT('Ctrl Pts',(-90.2900214059965,36.35548699916,111.112583302492));
#32660=CARTESIAN_POINT('Ctrl Pts',(-90.2872022523859,36.3527998634328,111.387416697508));
#32661=CARTESIAN_POINT('Ctrl Pts',(-90.2886216576026,36.1946623452147,111.39742744704));
#32662=CARTESIAN_POINT('Ctrl Pts',(-90.2749901963085,36.036768642733,111.407438196572));
#32663=CARTESIAN_POINT('Ctrl Pts',(-90.2454185361615,35.8819190433356,111.417448946105));
#32664=CARTESIAN_POINT('Ctrl Pts',(-90.0898923845469,35.0675189672606,111.470098453835));
#32665=CARTESIAN_POINT('Ctrl Pts',(-89.493457019938,34.3373194151317,111.522747961566));
#32666=CARTESIAN_POINT('Ctrl Pts',(-88.7264973449979,34.0223452499004,111.575397469297));
#32667=CARTESIAN_POINT('Ctrl Pts',(-87.9595376700576,33.7073710846691,111.628046977028));
#32668=CARTESIAN_POINT('Ctrl Pts',(-87.0220536847861,33.8076223063356,111.680696484759));
#32669=CARTESIAN_POINT('Ctrl Pts',(-86.3390394977637,34.277651548058,111.733345992489));
#32670=CARTESIAN_POINT('Ctrl Pts',(-85.6560253107413,34.7476807897803,111.78599550022));
#32671=CARTESIAN_POINT('Ctrl Pts',(-85.2274809219679,35.5874880515586,111.838645007951));
#32672=CARTESIAN_POINT('Ctrl Pts',(-85.2476804132995,36.4163594820577,111.891294515682));
#32673=CARTESIAN_POINT('Ctrl Pts',(-85.267879904631,37.2452309125568,111.943944023413));
#32674=CARTESIAN_POINT('Ctrl Pts',(-85.7368232760675,38.0631665117766,111.996593531144));
#32675=CARTESIAN_POINT('Ctrl Pts',(-86.4419221813022,38.4993676140041,112.049243038874));
#32676=CARTESIAN_POINT('Ctrl Pts',(-87.147021086537,38.9355687162316,112.101892546605));
#32677=CARTESIAN_POINT('Ctrl Pts',(-88.08827552557,38.9900353214667,112.154542054336));
#32678=CARTESIAN_POINT('Ctrl Pts',(-88.8389821119455,38.6380758224897,112.207191562067));
#32679=CARTESIAN_POINT('Ctrl Pts',(-89.589688698321,38.2861163235126,112.259841069798));
#32680=CARTESIAN_POINT('Ctrl Pts',(-90.149847432039,37.5277307203235,112.312490577529));
#32681=CARTESIAN_POINT('Ctrl Pts',(-90.2655188693974,36.7067215935002,112.365140085259));
#32682=CARTESIAN_POINT('Ctrl Pts',(-90.2818328412294,36.5909287921421,112.372565622676));
#32683=CARTESIAN_POINT('Ctrl Pts',(-90.2893053017908,36.4738903160605,112.379991160092));
#32684=CARTESIAN_POINT('Ctrl Pts',(-90.2883544400146,36.356729971742,112.387416697508));
#32685=CARTESIAN_POINT('Origin',(-87.7685555885722,36.3549260746835,114.));
#32686=CARTESIAN_POINT('',(-90.282160762018,36.3552974008428,113.387416697508));
#32687=CARTESIAN_POINT('',(-90.2845474745906,36.3528324580843,113.112583302492));
#32688=CARTESIAN_POINT('',(-90.2860555885722,36.3549260746835,114.));
#32689=CARTESIAN_POINT('Ctrl Pts',(-90.2845474745906,36.3528324580843,113.112583302492));
#32690=CARTESIAN_POINT('Ctrl Pts',(-90.2798793876854,36.9364594673067,113.075736828766));
#32691=CARTESIAN_POINT('Ctrl Pts',(-90.0774217774617,37.5230086335642,113.03889035504));
#32692=CARTESIAN_POINT('Ctrl Pts',(-89.7060411231664,37.9688454350711,113.002043881314));
#32693=CARTESIAN_POINT('Ctrl Pts',(-89.1753795251323,38.6058965760332,112.949394373583));
#32694=CARTESIAN_POINT('Ctrl Pts',(-88.29982390578,38.9556520813125,112.896744865852));
#32695=CARTESIAN_POINT('Ctrl Pts',(-87.4762940907326,38.859555611257,112.844095358121));
#32696=CARTESIAN_POINT('Ctrl Pts',(-86.6527642756852,38.7634591412015,112.791445850391));
#32697=CARTESIAN_POINT('Ctrl Pts',(-85.8812602649427,38.2215106958113,112.73879634266));
#32698=CARTESIAN_POINT('Ctrl Pts',(-85.5115316696583,37.4793943614956,112.686146834929));
#32699=CARTESIAN_POINT('Ctrl Pts',(-85.141803074374,36.7372780271799,112.633497327198));
#32700=CARTESIAN_POINT('Ctrl Pts',(-85.1738498945477,35.7949938039387,112.580847819467));
#32701=CARTESIAN_POINT('Ctrl Pts',(-85.5931441915838,35.0797119152388,112.528198311736));
#32702=CARTESIAN_POINT('Ctrl Pts',(-86.0124384886199,34.3644300265389,112.475548804006));
#32703=CARTESIAN_POINT('Ctrl Pts',(-86.8189802625183,33.8761504723801,112.422899296275));
#32704=CARTESIAN_POINT('Ctrl Pts',(-87.6471360650118,33.8362273634649,112.370249788544));
#32705=CARTESIAN_POINT('Ctrl Pts',(-88.4752918675053,33.7963042545498,112.317600280813));
#32706=CARTESIAN_POINT('Ctrl Pts',(-89.325061698594,34.2047375908782,112.264950773082));
#32707=CARTESIAN_POINT('Ctrl Pts',(-89.8112153276443,34.8763703303946,112.212301265351));
#32708=CARTESIAN_POINT('Ctrl Pts',(-90.1181396884788,35.3003935958269,112.179061944398));
#32709=CARTESIAN_POINT('Ctrl Pts',(-90.2801338523397,35.8293229164172,112.145822623445));
#32710=CARTESIAN_POINT('Ctrl Pts',(-90.2832192959692,36.3565168099065,112.112583302492));
#32711=CARTESIAN_POINT('Ctrl Pts',(-90.2883544400146,36.356729971742,112.387416697508));
#32712=CARTESIAN_POINT('Ctrl Pts',(-90.2825633783946,35.6431848589072,112.432640667823));
#32713=CARTESIAN_POINT('Ctrl Pts',(-89.9643334791074,34.925119395463,112.477864638137));
#32714=CARTESIAN_POINT('Ctrl Pts',(-89.4281349618304,34.4564050669767,112.523088608452));
#32715=CARTESIAN_POINT('Ctrl Pts',(-88.8038954759064,33.9107303177339,112.575738116183));
#32716=CARTESIAN_POINT('Ctrl Pts',(-87.88423236306,33.7030134697058,112.628387623914));
#32717=CARTESIAN_POINT('Ctrl Pts',(-87.0860609103553,33.9274197972347,112.681037131644));
#32718=CARTESIAN_POINT('Ctrl Pts',(-86.2878894576506,34.1518261247636,112.733686639375));
#32719=CARTESIAN_POINT('Ctrl Pts',(-85.6112096650878,34.8083556278495,112.786336147106));
#32720=CARTESIAN_POINT('Ctrl Pts',(-85.3627840264822,35.5993806399895,112.838985654837));
#32721=CARTESIAN_POINT('Ctrl Pts',(-85.1143583878767,36.3904056521295,112.891635162568));
#32722=CARTESIAN_POINT('Ctrl Pts',(-85.2941869032285,37.3159261733237,112.944284670298));
#32723=CARTESIAN_POINT('Ctrl Pts',(-85.8207470497215,37.9563715495058,112.996934178029));
#32724=CARTESIAN_POINT('Ctrl Pts',(-86.3473071962145,38.5968169256878,113.04958368576));
#32725=CARTESIAN_POINT('Ctrl Pts',(-87.2205989738487,38.9521871568577,113.102233193491));
#32726=CARTESIAN_POINT('Ctrl Pts',(-88.044728835218,38.8613805527632,113.154882701222));
#32727=CARTESIAN_POINT('Ctrl Pts',(-88.8688586965873,38.7705739486686,113.207532208953));
#32728=CARTESIAN_POINT('Ctrl Pts',(-89.6438266416916,38.2335905093095,113.260181716683));
#32729=CARTESIAN_POINT('Ctrl Pts',(-90.0183127374104,37.4938635111128,113.312831224414));
#32730=CARTESIAN_POINT('Ctrl Pts',(-90.1951502415015,37.1445542108066,113.337693048779));
#32731=CARTESIAN_POINT('Ctrl Pts',(-90.2826859490201,36.7500359601435,113.362554873143));
#32732=CARTESIAN_POINT('Ctrl Pts',(-90.282160762018,36.3552974008428,113.387416697508));
#32733=CARTESIAN_POINT('Origin',(-87.7685555885722,36.3549260746835,114.));
#32734=CARTESIAN_POINT('',(-90.2870431970936,36.3527727133248,114.387416697508));
#32735=CARTESIAN_POINT('',(-90.2900699264125,36.3553920695694,114.112583302492));
#32736=CARTESIAN_POINT('',(-90.2860555885722,36.3549260746835,114.));
#32737=CARTESIAN_POINT('Ctrl Pts',(-90.2900699264125,36.3553920695694,114.112583302492));
#32738=CARTESIAN_POINT('Ctrl Pts',(-90.2901360139808,36.3811153253261,114.110950049548));
#32739=CARTESIAN_POINT('Ctrl Pts',(-90.2897760704703,36.4068366869338,114.109316796605));
#32740=CARTESIAN_POINT('Ctrl Pts',(-90.2889843694534,36.4325447522138,114.107683543661));
#32741=CARTESIAN_POINT('Ctrl Pts',(-90.263463112031,37.2612694068783,114.05503403593));
#32742=CARTESIAN_POINT('Ctrl Pts',(-89.7892774376809,38.0761770717666,114.002384528199));
#32743=CARTESIAN_POINT('Ctrl Pts',(-89.0813922110172,38.5078417491499,113.949735020469));
#32744=CARTESIAN_POINT('Ctrl Pts',(-88.3735069843535,38.9395064265332,113.897085512738));
#32745=CARTESIAN_POINT('Ctrl Pts',(-87.4319222053761,38.9879281164113,113.844436005007));
#32746=CARTESIAN_POINT('Ctrl Pts',(-86.6834910151311,38.6311555820177,113.791786497276));
#32747=CARTESIAN_POINT('Ctrl Pts',(-85.9350598248862,38.274383047624,113.739136989545));
#32748=CARTESIAN_POINT('Ctrl Pts',(-85.3797822233737,37.5124162889586,113.686487481814));
#32749=CARTESIAN_POINT('Ctrl Pts',(-85.2693848672369,36.6906813489767,113.633837974084));
#32750=CARTESIAN_POINT('Ctrl Pts',(-85.1589875111001,35.8689464089947,113.581188466353));
#32751=CARTESIAN_POINT('Ctrl Pts',(-85.493470400339,34.9874432876963,113.528538958622));
#32752=CARTESIAN_POINT('Ctrl Pts',(-86.1212008035358,34.4457880202692,113.475889450891));
#32753=CARTESIAN_POINT('Ctrl Pts',(-86.7489312067326,33.904132752842,113.42323994316));
#32754=CARTESIAN_POINT('Ctrl Pts',(-87.6699091238872,33.7023253392863,113.37059043543));
#32755=CARTESIAN_POINT('Ctrl Pts',(-88.4666232213963,33.9318521016899,113.317940927699));
#32756=CARTESIAN_POINT('Ctrl Pts',(-89.2633373189054,34.1613788640935,113.265291419968));
#32757=CARTESIAN_POINT('Ctrl Pts',(-89.9357875967688,34.8222398024565,113.212641912237));
#32758=CARTESIAN_POINT('Ctrl Pts',(-90.1791289473426,35.6148436599604,113.159992404506));
#32759=CARTESIAN_POINT('Ctrl Pts',(-90.2521691675388,35.8527479871284,113.144189370502));
#32760=CARTESIAN_POINT('Ctrl Pts',(-90.2865495640347,36.1025214638383,113.128386336497));
#32761=CARTESIAN_POINT('Ctrl Pts',(-90.2845474745906,36.3528324580843,113.112583302492));
#32762=CARTESIAN_POINT('Ctrl Pts',(-90.282160762018,36.3552974008428,113.387416697508));
#32763=CARTESIAN_POINT('Ctrl Pts',(-90.2815737684849,35.9141041103816,113.415204380874));
#32764=CARTESIAN_POINT('Ctrl Pts',(-90.1709794034964,35.4726356061123,113.44299206424));
#32765=CARTESIAN_POINT('Ctrl Pts',(-89.9521102560219,35.0937065350684,113.470779747607));
#32766=CARTESIAN_POINT('Ctrl Pts',(-89.5374174325816,34.3757471142548,113.523429255338));
#32767=CARTESIAN_POINT('Ctrl Pts',(-88.7340275393681,33.8822988296621,113.576078763068));
#32768=CARTESIAN_POINT('Ctrl Pts',(-87.9061451674701,33.8370589573346,113.628728270799));
#32769=CARTESIAN_POINT('Ctrl Pts',(-87.078262795572,33.7918190850072,113.68137777853));
#32770=CARTESIAN_POINT('Ctrl Pts',(-86.2258879449895,34.194787624945,113.734027286261));
#32771=CARTESIAN_POINT('Ctrl Pts',(-85.7354317923295,34.8632849174344,113.786676793992));
#32772=CARTESIAN_POINT('Ctrl Pts',(-85.2449756396694,35.5317822099238,113.839326301722));
#32773=CARTESIAN_POINT('Ctrl Pts',(-85.1164381849319,36.4658082549647,113.891975809453));
#32774=CARTESIAN_POINT('Ctrl Pts',(-85.4080899285771,37.2419365485969,113.944625317184));
#32775=CARTESIAN_POINT('Ctrl Pts',(-85.6997416722223,38.0180648422291,113.997274824915));
#32776=CARTESIAN_POINT('Ctrl Pts',(-86.4115826142503,38.6362953844525,114.049924332646));
#32777=CARTESIAN_POINT('Ctrl Pts',(-87.2209104884245,38.8163627602663,114.102573840377));
#32778=CARTESIAN_POINT('Ctrl Pts',(-88.0302383625986,38.99643013608,114.155223348107));
#32779=CARTESIAN_POINT('Ctrl Pts',(-88.937053168919,38.7383343454839,114.207872855838));
#32780=CARTESIAN_POINT('Ctrl Pts',(-89.530264204703,38.1590791903305,114.260522363569));
#32781=CARTESIAN_POINT('Ctrl Pts',(-90.0068442812343,37.6937111349145,114.302820474882));
#32782=CARTESIAN_POINT('Ctrl Pts',(-90.2810131308354,37.0210551986511,114.345118586195));
#32783=CARTESIAN_POINT('Ctrl Pts',(-90.2870431970936,36.3527727133248,114.387416697508));
#32784=CARTESIAN_POINT('Origin',(-87.7685555885722,36.3549260746835,114.));
#32785=CARTESIAN_POINT('',(-90.2884952448755,36.3566728106054,115.387416697508));
#32786=CARTESIAN_POINT('',(-90.283326517746,36.3565773825716,115.112583302492));
#32787=CARTESIAN_POINT('',(-90.2860555885722,36.3549260746835,114.));
#32788=CARTESIAN_POINT('Ctrl Pts',(-90.283326517746,36.3565773825716,115.112583302492));
#32789=CARTESIAN_POINT('Ctrl Pts',(-90.2851690825839,36.6589983336067,115.0935137626));
#32790=CARTESIAN_POINT('Ctrl Pts',(-90.2346569267751,36.9608245377031,115.074444222708));
#32791=CARTESIAN_POINT('Ctrl Pts',(-90.1290212830441,37.2419365615535,115.055374682816));
#32792=CARTESIAN_POINT('Ctrl Pts',(-89.8373695351387,38.0180648665217,115.002725175085));
#32793=CARTESIAN_POINT('Ctrl Pts',(-89.1255285827133,38.6362954177748,114.950075667354));
#32794=CARTESIAN_POINT('Ctrl Pts',(-88.316200696718,38.8163627962183,114.897426159623));
#32795=CARTESIAN_POINT('Ctrl Pts',(-87.5068728107227,38.9964301746617,114.844776651893));
#32796=CARTESIAN_POINT('Ctrl Pts',(-86.6000579911575,38.7383343802956,114.792127144162));
#32797=CARTESIAN_POINT('Ctrl Pts',(-86.0068469467092,38.1590792166814,114.739477636431));
#32798=CARTESIAN_POINT('Ctrl Pts',(-85.413635902261,37.5798240530672,114.6868281287));
#32799=CARTESIAN_POINT('Ctrl Pts',(-85.1340286329297,36.6794095202049,114.634178620969));
#32800=CARTESIAN_POINT('Ctrl Pts',(-85.2947808423313,35.8660248541325,114.581529113238));
#32801=CARTESIAN_POINT('Ctrl Pts',(-85.455533051733,35.0526401880602,114.528879605508));
#32802=CARTESIAN_POINT('Ctrl Pts',(-86.0566447398676,34.3262853887778,114.476230097777));
#32803=CARTESIAN_POINT('Ctrl Pts',(-86.8256110639121,34.0162423589988,114.423580590046));
#32804=CARTESIAN_POINT('Ctrl Pts',(-87.5945773879567,33.7061993292197,114.370931082315));
#32805=CARTESIAN_POINT('Ctrl Pts',(-88.5313983479111,33.812468068944,114.318281574584));
#32806=CARTESIAN_POINT('Ctrl Pts',(-89.2113804076409,34.2868732610265,114.265632066854));
#32807=CARTESIAN_POINT('Ctrl Pts',(-89.8702685816242,34.7465618164327,114.214615812066));
#32808=CARTESIAN_POINT('Ctrl Pts',(-90.2880056165118,35.5519009907723,114.163599557279));
#32809=CARTESIAN_POINT('Ctrl Pts',(-90.2900699264125,36.3553920695694,114.112583302492));
#32810=CARTESIAN_POINT('Ctrl Pts',(-90.2870431970936,36.3527727133248,114.387416697508));
#32811=CARTESIAN_POINT('Ctrl Pts',(-90.2885189037937,36.1892274222949,114.397768093926));
#32812=CARTESIAN_POINT('Ctrl Pts',(-90.2739357189781,36.0259440582166,114.408119490344));
#32813=CARTESIAN_POINT('Ctrl Pts',(-90.2423302986814,35.8660248612744,114.418470886762));
#32814=CARTESIAN_POINT('Ctrl Pts',(-90.081578091628,35.0526402070823,114.471120394492));
#32815=CARTESIAN_POINT('Ctrl Pts',(-89.4804664122735,34.3262854184089,114.523769902223));
#32816=CARTESIAN_POINT('Ctrl Pts',(-88.7115000994606,34.016242393158,114.576419409954));
#32817=CARTESIAN_POINT('Ctrl Pts',(-87.9425337866477,33.7061993679072,114.629068917685));
#32818=CARTESIAN_POINT('Ctrl Pts',(-87.0057128403764,33.8124681060789,114.681718425416));
#32819=CARTESIAN_POINT('Ctrl Pts',(-86.3257307905782,34.2868732912319,114.734367933146));
#32820=CARTESIAN_POINT('Ctrl Pts',(-85.6457487407801,34.7612784763849,114.787017440877));
#32821=CARTESIAN_POINT('Ctrl Pts',(-85.2226055874552,35.6038201085191,114.839666948608));
#32822=CARTESIAN_POINT('Ctrl Pts',(-85.2481268445046,36.4325447510792,114.892316456339));
#32823=CARTESIAN_POINT('Ctrl Pts',(-85.2736481015539,37.2612693936393,114.94496596407));
#32824=CARTESIAN_POINT('Ctrl Pts',(-85.7478337689776,38.0761770466252,114.997615471801));
#32825=CARTESIAN_POINT('Ctrl Pts',(-86.4557189853018,38.5078417177038,115.050264979531));
#32826=CARTESIAN_POINT('Ctrl Pts',(-87.1636042016259,38.9395063887825,115.102914487262));
#32827=CARTESIAN_POINT('Ctrl Pts',(-88.1051889668506,38.9879280779537,115.155563994993));
#32828=CARTESIAN_POINT('Ctrl Pts',(-88.853620146164,38.6311555487714,115.208213502724));
#32829=CARTESIAN_POINT('Ctrl Pts',(-89.6020513254776,38.2743830195891,115.260863010455));
#32830=CARTESIAN_POINT('Ctrl Pts',(-90.1573289188799,37.5124162720532,115.313512518185));
#32831=CARTESIAN_POINT('Ctrl Pts',(-90.2677262734045,36.6906813440736,115.366162025916));
#32832=CARTESIAN_POINT('Ctrl Pts',(-90.2825821230674,36.5801028740972,115.373246916447));
#32833=CARTESIAN_POINT('Ctrl Pts',(-90.2893819483098,36.468442104034,115.380331806977));
#32834=CARTESIAN_POINT('Ctrl Pts',(-90.2884952448755,36.3566728106054,115.387416697508));
#32835=CARTESIAN_POINT('Origin',(-87.7685555885722,36.3549260746835,114.));
#32836=CARTESIAN_POINT('',(-90.2821875011782,36.3553827988861,116.387416697508));
#32837=CARTESIAN_POINT('',(-90.2844059463112,36.3528657341098,116.112583302492));
#32838=CARTESIAN_POINT('',(-90.2860555885722,36.3549260746835,114.));
#32839=CARTESIAN_POINT('Ctrl Pts',(-90.2844059463112,36.3528657341098,116.112583302492));
#32840=CARTESIAN_POINT('Ctrl Pts',(-90.2798733875279,36.9311794857661,116.076077475652));
#32841=CARTESIAN_POINT('Ctrl Pts',(-90.0814675469238,37.5123030648938,116.039571648811));
#32842=CARTESIAN_POINT('Ctrl Pts',(-89.7163641558721,37.9563715728973,116.003065821971));
#32843=CARTESIAN_POINT('Ctrl Pts',(-89.1898040016879,38.5968169584335,115.95041631424));
#32844=CARTESIAN_POINT('Ctrl Pts',(-88.3165122112982,38.9521871947936,115.897766806509));
#32845=CARTESIAN_POINT('Ctrl Pts',(-87.4923823378917,38.8613805893724,115.845117298778));
#32846=CARTESIAN_POINT('Ctrl Pts',(-86.6682524644853,38.7705739839512,115.792467791047));
#32847=CARTESIAN_POINT('Ctrl Pts',(-85.8932845080619,38.2335905367486,115.739818283317));
#32848=CARTESIAN_POINT('Ctrl Pts',(-85.5187984068737,37.4938635277473,115.687168775586));
#32849=CARTESIAN_POINT('Ctrl Pts',(-85.1443123056855,36.754136518746,115.634519267855));
#32850=CARTESIAN_POINT('Ctrl Pts',(-85.1703080597325,35.811665947946,115.581869760124));
#32851=CARTESIAN_POINT('Ctrl Pts',(-85.58500088923,35.0937065166461,115.529220252393));
#32852=CARTESIAN_POINT('Ctrl Pts',(-85.9996937187276,34.3757470853462,115.476570744662));
#32853=CARTESIAN_POINT('Ctrl Pts',(-86.8030836236757,33.8822987935465,115.423921236932));
#32854=CARTESIAN_POINT('Ctrl Pts',(-87.6309660076658,33.8370589205585,115.371271729201));
#32855=CARTESIAN_POINT('Ctrl Pts',(-88.4588483916559,33.7918190475706,115.31862222147));
#32856=CARTESIAN_POINT('Ctrl Pts',(-89.3112232546881,34.1947875933945,115.265972713739));
#32857=CARTESIAN_POINT('Ctrl Pts',(-89.8016794145115,34.8632848956482,115.213323206008));
#32858=CARTESIAN_POINT('Ctrl Pts',(-90.1144933947941,35.2896538946663,115.17974323817));
#32859=CARTESIAN_POINT('Ctrl Pts',(-90.2800819052201,35.8240377477917,115.146163270331));
#32860=CARTESIAN_POINT('Ctrl Pts',(-90.283326517746,36.3565773825716,115.112583302492));
#32861=CARTESIAN_POINT('Ctrl Pts',(-90.2884952448755,36.3566728106054,115.387416697508));
#32862=CARTESIAN_POINT('Ctrl Pts',(-90.2827926440549,35.6378578835658,115.432981314708));
#32863=CARTESIAN_POINT('Ctrl Pts',(-89.9591688972838,34.9145543409096,115.478545931909));
#32864=CARTESIAN_POINT('Ctrl Pts',(-89.4159103495481,34.4457880481547,115.524110549109));
#32865=CARTESIAN_POINT('Ctrl Pts',(-88.7881799555201,33.9041327886388,115.57676005684));
#32866=CARTESIAN_POINT('Ctrl Pts',(-87.8672020518174,33.7023253780303,115.62940956457));
#32867=CARTESIAN_POINT('Ctrl Pts',(-87.0704879659451,33.9318521370812,115.682059072301));
#32868=CARTESIAN_POINT('Ctrl Pts',(-86.2737738800728,34.161378896132,115.734708580032));
#32869=CARTESIAN_POINT('Ctrl Pts',(-85.601323612031,34.8222398248422,115.787358087763));
#32870=CARTESIAN_POINT('Ctrl Pts',(-85.3579822650111,35.6148436707692,115.840007595494));
#32871=CARTESIAN_POINT('Ctrl Pts',(-85.1146409179913,36.4074475166962,115.892657103225));
#32872=CARTESIAN_POINT('Ctrl Pts',(-85.3004084919934,37.33179427984,115.945306610955));
#32873=CARTESIAN_POINT('Ctrl Pts',(-85.8310700822764,37.9688454114975,115.997956118686));
#32874=CARTESIAN_POINT('Ctrl Pts',(-86.3617316725594,38.6058965431549,116.050605626417));
#32875=CARTESIAN_POINT('Ctrl Pts',(-87.2372872791233,38.955652043326,116.103255134148));
#32876=CARTESIAN_POINT('Ctrl Pts',(-88.0608170821422,38.8595555746744,116.155904641879));
#32877=CARTESIAN_POINT('Ctrl Pts',(-88.8843468851612,38.7634591060228,116.20855414961));
#32878=CARTESIAN_POINT('Ctrl Pts',(-89.6558508846352,38.2215106685486,116.26120365734));
#32879=CARTESIAN_POINT('Ctrl Pts',(-90.0255794745196,37.4793943450724,116.313853165071));
#32880=CARTESIAN_POINT('Ctrl Pts',(-90.197778242606,37.1337583294227,116.33837434255));
#32881=CARTESIAN_POINT('Ctrl Pts',(-90.2828250094709,36.7447024542471,116.362895520029));
#32882=CARTESIAN_POINT('Ctrl Pts',(-90.2821875011782,36.3553827988861,116.387416697508));
#32883=CARTESIAN_POINT('Origin',(-87.7685555885722,36.3549260746835,114.));
#32884=CARTESIAN_POINT('',(-90.286883306508,36.3527492243956,117.387416697508));
#32885=CARTESIAN_POINT('',(-90.2901099846489,36.3552960960066,117.112583302492));
#32886=CARTESIAN_POINT('',(-90.2860555885722,36.3549260746835,114.));
#32887=CARTESIAN_POINT('Ctrl Pts',(-90.2901099846489,36.3552960960066,117.112583302492));
#32888=CARTESIAN_POINT('Ctrl Pts',(-90.290152157795,36.3756533940165,117.111290696434));
#32889=CARTESIAN_POINT('Ctrl Pts',(-90.2899267214508,36.3960097343219,117.109998090376));
#32890=CARTESIAN_POINT('Ctrl Pts',(-90.289430800665,36.4163594829559,117.108705484318));
#32891=CARTESIAN_POINT('Ctrl Pts',(-90.269231309038,37.2452309255615,117.056055976587));
#32892=CARTESIAN_POINT('Ctrl Pts',(-89.8002879307519,38.063166536728,117.003406468856));
#32893=CARTESIAN_POINT('Ctrl Pts',(-89.0951890152183,38.4993676453264,116.950756961126));
#32894=CARTESIAN_POINT('Ctrl Pts',(-88.3900900996848,38.9355687539247,116.898107453395));
#32895=CARTESIAN_POINT('Ctrl Pts',(-87.4488356469037,38.9900353599551,116.845457945664));
#32896=CARTESIAN_POINT('Ctrl Pts',(-86.6981290495635,38.638075855837,116.792808437933));
#32897=CARTESIAN_POINT('Ctrl Pts',(-85.9474224522232,38.286116351719,116.740158930202));
#32898=CARTESIAN_POINT('Ctrl Pts',(-85.3872637103238,37.5277307374526,116.687509422471));
#32899=CARTESIAN_POINT('Ctrl Pts',(-85.2715922712763,36.7067215986376,116.634859914741));
#32900=CARTESIAN_POINT('Ctrl Pts',(-85.1559208322288,35.8857124598225,116.58221040701));
#32901=CARTESIAN_POINT('Ctrl Pts',(-85.4847366960332,35.0020797964589,116.529560899279));
#32902=CARTESIAN_POINT('Ctrl Pts',(-86.108976191075,34.4564050392462,116.476911391548));
#32903=CARTESIAN_POINT('Ctrl Pts',(-86.7332156861168,33.9107302820335,116.424261883817));
#32904=CARTESIAN_POINT('Ctrl Pts',(-87.6528788123959,33.7030134309718,116.371612376086));
#32905=CARTESIAN_POINT('Ctrl Pts',(-88.4510502767586,33.9274197617787,116.318962868356));
#32906=CARTESIAN_POINT('Ctrl Pts',(-89.2492217411213,34.1518260925856,116.266313360625));
#32907=CARTESIAN_POINT('Ctrl Pts',(-89.9259015435676,34.808355605261,116.213663852894));
#32908=CARTESIAN_POINT('Ctrl Pts',(-90.1743271858014,35.5993806289549,116.161014345163));
#32909=CARTESIAN_POINT('Ctrl Pts',(-90.2505008190614,35.8419290612044,116.144870664273));
#32910=CARTESIAN_POINT('Ctrl Pts',(-90.2864103436622,36.0971226522707,116.128726983382));
#32911=CARTESIAN_POINT('Ctrl Pts',(-90.2844059463112,36.3528657341098,116.112583302492));
#32912=CARTESIAN_POINT('Ctrl Pts',(-90.2821875011782,36.3553827988861,116.387416697508));
#32913=CARTESIAN_POINT('Ctrl Pts',(-90.2814562131392,35.9087928319514,116.41554502776));
#32914=CARTESIAN_POINT('Ctrl Pts',(-90.1679775627328,35.461855770756,116.443673358012));
#32915=CARTESIAN_POINT('Ctrl Pts',(-89.943966953787,35.0797119338654,116.471801688264));
#32916=CARTESIAN_POINT('Ctrl Pts',(-89.5246726628754,34.3644300556127,116.524451195994));
#32917=CARTESIAN_POINT('Ctrl Pts',(-88.7181309007576,33.8761505085855,116.577100703725));
#32918=CARTESIAN_POINT('Ctrl Pts',(-87.8899751103602,33.8362274002532,116.629750211456));
#32919=CARTESIAN_POINT('Ctrl Pts',(-87.0618193199627,33.7963042919208,116.682399719187));
#32920=CARTESIAN_POINT('Ctrl Pts',(-86.2120495012857,34.2047376222833,116.735049226918));
#32921=CARTESIAN_POINT('Ctrl Pts',(-85.725895879336,34.8763703519896,116.787698734649));
#32922=CARTESIAN_POINT('Ctrl Pts',(-85.2397422573863,35.548003081696,116.840348242379));
#32923=CARTESIAN_POINT('Ctrl Pts',(-85.1172048321637,36.4828352107461,116.89299775011));
#32924=CARTESIAN_POINT('Ctrl Pts',(-85.4138340819895,37.2570748092528,116.945647257841));
#32925=CARTESIAN_POINT('Ctrl Pts',(-85.7104633318153,38.0313144077595,116.998296765572));
#32926=CARTESIAN_POINT('Ctrl Pts',(-86.4262592566894,38.6449614757227,117.050946273303));
#32927=CARTESIAN_POINT('Ctrl Pts',(-87.2367266590444,38.8198284464961,117.103595781033));
#32928=CARTESIAN_POINT('Ctrl Pts',(-88.0471940613994,38.9946954172694,117.156245288764));
#32929=CARTESIAN_POINT('Ctrl Pts',(-88.9523329412353,38.730782290853,117.208894796495));
#32930=CARTESIAN_POINT('Ctrl Pts',(-89.5418123516562,38.1477300698326,117.261544304226));
#32931=CARTESIAN_POINT('Ctrl Pts',(-90.0115804930765,37.6830838864755,117.303501768653));
#32932=CARTESIAN_POINT('Ctrl Pts',(-90.2808789705167,37.0157581916285,117.345459233081));
#32933=CARTESIAN_POINT('Ctrl Pts',(-90.286883306508,36.3527492243956,117.387416697508));
#32934=CARTESIAN_POINT('Origin',(-87.7685555885722,36.3549260746835,114.));
#32935=CARTESIAN_POINT('',(-90.2886325747468,36.3566124302836,118.387416697508));
#32936=CARTESIAN_POINT('',(-90.2834379459911,36.3566354806138,118.112583302492));
#32937=CARTESIAN_POINT('',(-90.2860555885722,36.3549260746835,114.));
#32938=CARTESIAN_POINT('Ctrl Pts',(-90.2834379459911,36.3566354806138,118.112583302492));
#32939=CARTESIAN_POINT('Ctrl Pts',(-90.2853166571071,36.653621048985,118.093854409486));
#32940=CARTESIAN_POINT('Ctrl Pts',(-90.2366418321613,36.9500108449635,118.075125516479));
#32941=CARTESIAN_POINT('Ctrl Pts',(-90.1346681153728,37.2267617295443,118.056396623473));
#32942=CARTESIAN_POINT('Ctrl Pts',(-89.8480058984144,38.0047467301666,118.003747115742));
#32943=CARTESIAN_POINT('Ctrl Pts',(-89.1401492778511,38.6275352663295,117.951097608011));
#32944=CARTESIAN_POINT('Ctrl Pts',(-88.3319942883572,38.812795625777,117.89844810028));
#32945=CARTESIAN_POINT('Ctrl Pts',(-87.5238392988634,38.9980559852244,117.845798592549));
#32946=CARTESIAN_POINT('Ctrl Pts',(-86.6153859404389,38.7457881679563,117.793149084819));
#32947=CARTESIAN_POINT('Ctrl Pts',(-86.0184677284529,38.1703539527493,117.740499577088));
#32948=CARTESIAN_POINT('Ctrl Pts',(-85.4215495164669,37.5949197375422,117.687850069357));
#32949=CARTESIAN_POINT('Ctrl Pts',(-85.1361664509194,36.696319124396,117.635200561626));
#32950=CARTESIAN_POINT('Ctrl Pts',(-85.291692604806,35.8819190364259,117.582551053895));
#32951=CARTESIAN_POINT('Ctrl Pts',(-85.4472187586926,35.0675189484558,117.529901546165));
#32952=CARTESIAN_POINT('Ctrl Pts',(-86.0436541320133,34.3373193856618,117.477252038434));
#32953=CARTESIAN_POINT('Ctrl Pts',(-86.8106138181558,34.0223452158303,117.424602530703));
#32954=CARTESIAN_POINT('Ctrl Pts',(-87.5775735042984,33.7073710459988,117.371953022972));
#32955=CARTESIAN_POINT('Ctrl Pts',(-88.5150575032628,33.8076222691299,117.319303515241));
#32956=CARTESIAN_POINT('Ctrl Pts',(-89.1980717002612,34.2776515177178,117.26665400751));
#32957=CARTESIAN_POINT('Ctrl Pts',(-89.8643171120078,34.7361410068596,117.215297105838));
#32958=CARTESIAN_POINT('Ctrl Pts',(-90.2884343912986,35.5464744556199,117.163940204165));
#32959=CARTESIAN_POINT('Ctrl Pts',(-90.2901099846489,36.3552960960066,117.112583302492));
#32960=CARTESIAN_POINT('Ctrl Pts',(-90.286883306508,36.3527492243956,117.387416697508));
#32961=CARTESIAN_POINT('Ctrl Pts',(-90.288413394689,36.1837942914657,117.398108740811));
#32962=CARTESIAN_POINT('Ctrl Pts',(-90.2728455288958,36.0151196808007,117.408800784115));
#32963=CARTESIAN_POINT('Ctrl Pts',(-90.2391400683468,35.8501508364386,117.419492827418));
#32964=CARTESIAN_POINT('Ctrl Pts',(-90.0731684336104,35.0378151396894,117.472142335149));
#32965=CARTESIAN_POINT('Ctrl Pts',(-89.4674052231316,34.3153350618152,117.52479184288));
#32966=CARTESIAN_POINT('Ctrl Pts',(-88.6964639766552,34.0102359595115,117.577441350611));
#32967=CARTESIAN_POINT('Ctrl Pts',(-87.9255227301789,33.7051368572078,117.630090858342));
#32968=CARTESIAN_POINT('Ctrl Pts',(-86.9894034477049,33.8174187304746,117.682740366072));
#32969=CARTESIAN_POINT('Ctrl Pts',(-86.3124815705486,34.2961802994946,117.735389873803));
#32970=CARTESIAN_POINT('Ctrl Pts',(-85.6355596933923,34.7749418685146,117.788039381534));
#32971=CARTESIAN_POINT('Ctrl Pts',(-85.2178352215536,35.620183133288,117.840688889265));
#32972=CARTESIAN_POINT('Ctrl Pts',(-85.2486771920908,36.4487268198985,117.893338396996));
#32973=CARTESIAN_POINT('Ctrl Pts',(-85.279519162628,37.277270506509,117.945987904727));
#32974=CARTESIAN_POINT('Ctrl Pts',(-85.7589275755411,38.0891166149566,117.998637412457));
#32975=CARTESIAN_POINT('Ctrl Pts',(-86.4695699170935,38.5162270574792,118.051286920188));
#32976=CARTESIAN_POINT('Ctrl Pts',(-87.1802122586458,38.9433375000017,118.103936427919));
#32977=CARTESIAN_POINT('Ctrl Pts',(-88.1220885288374,38.9857122765992,118.15658593565));
#32978=CARTESIAN_POINT('Ctrl Pts',(-88.8682134435465,38.6241414268697,118.209235443381));
#32979=CARTESIAN_POINT('Ctrl Pts',(-89.6143383582556,38.2625705771402,118.261884951112));
#32980=CARTESIAN_POINT('Ctrl Pts',(-90.1647119174822,37.4970541010838,118.314534458842));
#32981=CARTESIAN_POINT('Ctrl Pts',(-90.2698306375093,36.674627251678,118.367183966573));
#32982=CARTESIAN_POINT('Ctrl Pts',(-90.283296029496,36.5692768449678,118.373928210218));
#32983=CARTESIAN_POINT('Ctrl Pts',(-90.2894553061913,36.4629926050629,118.380672453863));
#32984=CARTESIAN_POINT('Ctrl Pts',(-90.2886325747468,36.3566124302836,118.387416697508));
#32985=CARTESIAN_POINT('Origin',(-87.7685555885722,36.3549260746835,114.));
#32986=CARTESIAN_POINT('',(-90.282219751568,36.3554675197253,119.387416697508));
#32987=CARTESIAN_POINT('',(-90.2842673072634,36.3529021929646,119.112583302492));
#32988=CARTESIAN_POINT('',(-90.2860555885722,36.3549260746835,114.));
#32989=CARTESIAN_POINT('Ctrl Pts',(-90.2842673072634,36.3529021929646,119.112583302492));
#32990=CARTESIAN_POINT('Ctrl Pts',(-90.2798740930897,36.9258994299071,119.076418122537));
#32991=CARTESIAN_POINT('Ctrl Pts',(-90.0854711696263,37.5015935291692,119.040252942582));
#32992=CARTESIAN_POINT('Ctrl Pts',(-89.7266068808129,37.9438316833838,119.004087762628));
#32993=CARTESIAN_POINT('Ctrl Pts',(-89.2041698800348,38.5876449078244,118.951438254897));
#32994=CARTESIAN_POINT('Ctrl Pts',(-88.3331779247476,38.9486152241081,118.898788747166));
#32995=CARTESIAN_POINT('Ctrl Pts',(-87.508481971726,38.8631022274075,118.846139239435));
#32996=CARTESIAN_POINT('Ctrl Pts',(-86.6837860187044,38.7775892307069,118.793489731704));
#32997=CARTESIAN_POINT('Ctrl Pts',(-85.9053860679484,38.245592921022,118.740840223974));
#32998=CARTESIAN_POINT('Ctrl Pts',(-85.526157900707,37.5082857359385,118.688190716243));
#32999=CARTESIAN_POINT('Ctrl Pts',(-85.1469297334656,36.770978550855,118.635541208512));
#33000=CARTESIAN_POINT('Ctrl Pts',(-85.1668733497388,35.828360490373,118.582891700781));
#33001=CARTESIAN_POINT('Ctrl Pts',(-85.5769476140976,35.1077531177242,118.53024219305));
#33002=CARTESIAN_POINT('Ctrl Pts',(-85.9870218784565,34.3871457450755,118.477592685319));
#33003=CARTESIAN_POINT('Ctrl Pts',(-86.787226790901,33.8885490602601,118.424943177589));
#33004=CARTESIAN_POINT('Ctrl Pts',(-87.614801623072,33.8379942884047,118.372293669858));
#33005=CARTESIAN_POINT('Ctrl Pts',(-88.4423764552431,33.7874395165493,118.319644162127));
#33006=CARTESIAN_POINT('Ctrl Pts',(-89.2973212071407,34.1849266576539,118.266994654396));
#33007=CARTESIAN_POINT('Ctrl Pts',(-89.7920596764127,34.8502609607471,118.214345146665));
#33008=CARTESIAN_POINT('Ctrl Pts',(-90.1108059236012,35.2789173628837,118.180424531941));
#33009=CARTESIAN_POINT('Ctrl Pts',(-90.2800353404061,35.8187535545449,118.146503917216));
#33010=CARTESIAN_POINT('Ctrl Pts',(-90.2834379459911,36.3566354806138,118.112583302492));
#33011=CARTESIAN_POINT('Ctrl Pts',(-90.2886325747468,36.3566124302836,118.387416697508));
#33012=CARTESIAN_POINT('Ctrl Pts',(-90.2830325836699,35.6325267842361,118.433321961594));
#33013=CARTESIAN_POINT('Ctrl Pts',(-89.9539590026799,34.9039965145798,118.47922722568));
#33014=CARTESIAN_POINT('Ctrl Pts',(-89.4036178173749,34.4352497422075,118.525132489766));
#33015=CARTESIAN_POINT('Ctrl Pts',(-88.7724223963857,33.897636304898,118.577781997497));
#33016=CARTESIAN_POINT('Ctrl Pts',(-87.8501676735797,33.7017466530343,118.630431505227));
#33017=CARTESIAN_POINT('Ctrl Pts',(-87.0549438026942,33.9363843798368,118.683081012958));
#33018=CARTESIAN_POINT('Ctrl Pts',(-86.2597199318087,34.1710221066394,118.735730520689));
#33019=CARTESIAN_POINT('Ctrl Pts',(-85.5915269128436,34.8361872121083,118.78838002842));
#33020=CARTESIAN_POINT('Ctrl Pts',(-85.3532798904614,35.6303372139996,118.841029536151));
#33021=CARTESIAN_POINT('Ctrl Pts',(-85.1150328680792,36.4244872158909,118.893679043881));
#33022=CARTESIAN_POINT('Ctrl Pts',(-85.3067318422799,37.3476221142046,118.946328551612));
#33023=CARTESIAN_POINT('Ctrl Pts',(-85.8414729970048,37.9812527339857,118.998978059343));
#33024=CARTESIAN_POINT('Ctrl Pts',(-86.3762141517297,38.6148833537668,119.051627567074));
#33025=CARTESIAN_POINT('Ctrl Pts',(-87.2539974869788,38.9590096950153,119.104277074805));
#33026=CARTESIAN_POINT('Ctrl Pts',(-88.0768932785437,38.8576273278598,119.156926582536));
#33027=CARTESIAN_POINT('Ctrl Pts',(-88.8997890701086,38.7562449607043,119.209576090266));
#33028=CARTESIAN_POINT('Ctrl Pts',(-89.6677973179892,38.2093538851449,119.262225597997));
#33029=CARTESIAN_POINT('Ctrl Pts',(-90.0327531567428,37.4648788252948,119.314875105728));
#33030=CARTESIAN_POINT('Ctrl Pts',(-90.2003677500134,37.1229610612634,119.339055636321));
#33031=CARTESIAN_POINT('Ctrl Pts',(-90.2829655843985,36.7393664592534,119.363236166915));
#33032=CARTESIAN_POINT('Ctrl Pts',(-90.282219751568,36.3554675197253,119.387416697508));
#33033=CARTESIAN_POINT('Origin',(-87.7685555885722,36.3549260746835,114.));
#33034=CARTESIAN_POINT('',(-90.2867225490468,36.352727843524,120.387416697508));
#33035=CARTESIAN_POINT('',(-90.2901412986672,36.3551993258176,120.112583302492));
#33036=CARTESIAN_POINT('',(-90.2860555885722,36.3549260746835,114.));
#33037=CARTESIAN_POINT('Ctrl Pts',(-90.2901412986672,36.3551993258176,120.112583302492));
#33038=CARTESIAN_POINT('Ctrl Pts',(-90.2901645977928,36.3701912646894,120.11163134332));
#33039=CARTESIAN_POINT('Ctrl Pts',(-90.2900423341944,36.3851828134258,120.110679384147));
#33040=CARTESIAN_POINT('Ctrl Pts',(-90.2897733450593,36.4001717289872,120.109727424975));
#33041=CARTESIAN_POINT('Ctrl Pts',(-90.2748965037429,37.2291558373634,120.057077917244));
#33042=CARTESIAN_POINT('Ctrl Pts',(-89.8112146580294,38.0500855733585,120.004428409513));
#33043=CARTESIAN_POINT('Ctrl Pts',(-89.1089310994663,38.4908051035161,119.951778901782));
#33044=CARTESIAN_POINT('Ctrl Pts',(-88.4066475409033,38.9315246336736,119.899129394052));
#33045=CARTESIAN_POINT('Ctrl Pts',(-87.4657622694907,38.9920339579935,119.846479886321));
#33046=CARTESIAN_POINT('Ctrl Pts',(-86.7128112286454,38.6449020075891,119.79383037859));
#33047=CARTESIAN_POINT('Ctrl Pts',(-85.9598601878,38.2977700571847,119.741180870859));
#33048=CARTESIAN_POINT('Ctrl Pts',(-85.3948433775217,37.542996832056,119.688531363128));
#33049=CARTESIAN_POINT('Ctrl Pts',(-85.2739026187123,36.722747338356,119.635881855397));
#33050=CARTESIAN_POINT('Ctrl Pts',(-85.1529618599029,35.902497844656,119.583232347667));
#33051=CARTESIAN_POINT('Ctrl Pts',(-85.4760971525623,35.0167720823848,119.530582839936));
#33052=CARTESIAN_POINT('Ctrl Pts',(-86.0968200051661,34.467100336265,119.477933332205));
#33053=CARTESIAN_POINT('Ctrl Pts',(-86.71754285777,33.9174285901452,119.425283824474));
#33054=CARTESIAN_POINT('Ctrl Pts',(-87.6358532703183,33.7038108601768,119.372634316743));
#33055=CARTESIAN_POINT('Ctrl Pts',(-88.4354491918029,33.9230875057825,119.319984809013));
#33056=CARTESIAN_POINT('Ctrl Pts',(-89.2350451132875,34.1423641513883,119.267335301282));
#33057=CARTESIAN_POINT('Ctrl Pts',(-89.9159265437086,34.7945351725681,119.214685793551));
#33058=CARTESIAN_POINT('Ctrl Pts',(-90.1694262357844,35.5839487494568,119.16203628582));
#33059=CARTESIAN_POINT('Ctrl Pts',(-90.2487958670574,35.8311106454198,119.145551958044));
#33060=CARTESIAN_POINT('Ctrl Pts',(-90.2862697632866,36.0917262695954,119.129067630268));
#33061=CARTESIAN_POINT('Ctrl Pts',(-90.2842673072634,36.3529021929646,119.112583302492));
#33062=CARTESIAN_POINT('Ctrl Pts',(-90.282219751568,36.3554675197253,119.387416697508));
#33063=CARTESIAN_POINT('Ctrl Pts',(-90.2813416443767,35.9034836358174,119.415885674645));
#33064=CARTESIAN_POINT('Ctrl Pts',(-90.1649362220051,35.4510778926663,119.444354651783));
#33065=CARTESIAN_POINT('Ctrl Pts',(-89.9357339572164,35.0657698934732,119.472823628921));
#33066=CARTESIAN_POINT('Ctrl Pts',(-89.5118554893097,34.3531950656423,119.525473136651));
#33067=CARTESIAN_POINT('Ctrl Pts',(-88.7021951238695,33.8701044541211,119.578122644382));
#33068=CARTESIAN_POINT('Ctrl Pts',(-87.8738000531233,33.8354997207509,119.630772152113));
#33069=CARTESIAN_POINT('Ctrl Pts',(-87.0454049823771,33.8008949873808,119.683421659844));
#33070=CARTESIAN_POINT('Ctrl Pts',(-86.1982752063249,34.2147761321616,119.736071167575));
#33071=CARTESIAN_POINT('Ctrl Pts',(-85.7164441722275,34.8895166799831,119.788720675305));
#33072=CARTESIAN_POINT('Ctrl Pts',(-85.2346131381301,35.5642572278047,119.841370183036));
#33073=CARTESIAN_POINT('Ctrl Pts',(-85.1180808459875,36.499857178667,119.894019690767));
#33074=CARTESIAN_POINT('Ctrl Pts',(-85.419675344928,37.272176012196,119.946669198498));
#33075=CARTESIAN_POINT('Ctrl Pts',(-85.7212698438684,38.044494845725,119.999318706229));
#33076=CARTESIAN_POINT('Ctrl Pts',(-86.4409911338919,38.6535325619209,120.05196821396));
#33077=CARTESIAN_POINT('Ctrl Pts',(-87.2525647049724,38.8231922227827,120.10461772169));
#33078=CARTESIAN_POINT('Ctrl Pts',(-88.0641382760528,38.9928518836446,120.157267229421));
#33079=CARTESIAN_POINT('Ctrl Pts',(-88.9675641281902,38.7231334891725,120.209916737152));
#33080=CARTESIAN_POINT('Ctrl Pts',(-89.5532874944098,38.1363076144321,120.262566244883));
#33081=CARTESIAN_POINT('Ctrl Pts',(-90.0162726867219,37.6724509439633,120.304183062425));
#33082=CARTESIAN_POINT('Ctrl Pts',(-90.2807536717285,37.0104618326376,120.345799879966));
#33083=CARTESIAN_POINT('Ctrl Pts',(-90.2867225490468,36.352727843524,120.387416697508));
#33084=CARTESIAN_POINT('Origin',(-87.7685555885722,36.3549260746835,114.));
#33085=CARTESIAN_POINT('',(-90.2887581529621,36.3565049378502,121.387416697508));
#33086=CARTESIAN_POINT('',(-90.2835503128821,36.3566878611388,121.112583302492));
#33087=CARTESIAN_POINT('',(-90.2860555885722,36.3549260746835,114.));
#33088=CARTESIAN_POINT('',(-85.855089591907,37.9909132780583,122.));
#33089=CARTESIAN_POINT('Ctrl Pts',(-90.2887581529621,36.3565049378502,121.387416697508));
#33090=CARTESIAN_POINT('Ctrl Pts',(-90.2833000777792,35.6272821077594,121.43366260848));
#33091=CARTESIAN_POINT('Ctrl Pts',(-89.9487703120527,34.8938081203929,121.479908519451));
#33092=CARTESIAN_POINT('Ctrl Pts',(-89.3912933146495,34.4249748138373,121.526154430423));
#33093=CARTESIAN_POINT('Ctrl Pts',(-88.7566233758821,33.8912229149252,121.578803938153));
#33094=CARTESIAN_POINT('Ctrl Pts',(-87.8329892401945,33.7004745205997,121.631453445884));
#33095=CARTESIAN_POINT('Ctrl Pts',(-87.0393721722715,33.9406285050808,121.684102953615));
#33096=CARTESIAN_POINT('Ctrl Pts',(-86.2457551043485,34.1807824895619,121.736752461346));
#33097=CARTESIAN_POINT('Ctrl Pts',(-85.5821551041903,34.8518388528496,121.789401969077));
#33098=CARTESIAN_POINT('Ctrl Pts',(-85.3491898794995,35.6461247484183,121.842051476807));
#33099=CARTESIAN_POINT('Ctrl Pts',(-85.1162246548087,36.4404106439871,121.894700984538));
#33100=CARTESIAN_POINT('Ctrl Pts',(-85.3138942055855,37.3579260718368,121.947350492269));
#33101=CARTESIAN_POINT('Ctrl Pts',(-85.855089591907,37.9909132780583,122.));
#33102=CARTESIAN_POINT('',(-89.6856658064524,37.9934539967174,122.));
#33103=CARTESIAN_POINT('Origin',(-87.7685555885722,36.3549260746835,122.));
#33104=CARTESIAN_POINT('Ctrl Pts',(-89.6856746522266,37.9934601639126,122.));
#33105=CARTESIAN_POINT('Ctrl Pts',(-89.1628540835289,38.6021752894523,121.949053726697));
#33106=CARTESIAN_POINT('Ctrl Pts',(-88.3231296031605,38.9423515356051,121.898107453395));
#33107=CARTESIAN_POINT('Ctrl Pts',(-87.5244587668031,38.8645887304742,121.847161180092));
#33108=CARTESIAN_POINT('Ctrl Pts',(-86.6990867886923,38.7842261613498,121.794511672361));
#33109=CARTESIAN_POINT('Ctrl Pts',(-85.9175593487471,38.2575123577278,121.74186216463));
#33110=CARTESIAN_POINT('Ctrl Pts',(-85.5336747406072,37.5227256222368,121.6892126569));
#33111=CARTESIAN_POINT('Ctrl Pts',(-85.1497901324673,36.7879388867457,121.636563149169));
#33112=CARTESIAN_POINT('Ctrl Pts',(-85.1635483561328,35.8450792193857,121.583913641438));
#33113=CARTESIAN_POINT('Ctrl Pts',(-85.5689531296241,35.1218194524428,121.531264133707));
#33114=CARTESIAN_POINT('Ctrl Pts',(-85.9743579031154,34.3985596854999,121.478614625976));
#33115=CARTESIAN_POINT('Ctrl Pts',(-86.7714092264326,33.8948998189741,121.425965118245));
#33116=CARTESIAN_POINT('Ctrl Pts',(-87.5986589277565,33.8390488405726,121.373315610515));
#33117=CARTESIAN_POINT('Ctrl Pts',(-88.4259086290804,33.7831978621711,121.320666102784));
#33118=CARTESIAN_POINT('Ctrl Pts',(-89.2833567084111,34.1751557718939,121.268016595053));
#33119=CARTESIAN_POINT('Ctrl Pts',(-89.7823490459092,34.837291568606,121.215367087322));
#33120=CARTESIAN_POINT('Ctrl Pts',(-90.1070644659248,35.2681713380526,121.181105825712));
#33121=CARTESIAN_POINT('Ctrl Pts',(-90.2799862325785,35.8134621316163,121.146844564102));
#33122=CARTESIAN_POINT('Ctrl Pts',(-90.2835503128821,36.3566878611388,121.112583302492));
#33123=CARTESIAN_POINT('Origin',(-87.7685555885722,36.3549260746835,124.208423447177));
#33124=CARTESIAN_POINT('',(-90.8468254863551,36.3557395475489,107.791576552823));
#33125=CARTESIAN_POINT('',(-90.837184588187,36.355240425647,107.708423447177));
#33126=CARTESIAN_POINT('',(-90.8420555885722,36.3549260746838,124.208423447177));
#33127=CARTESIAN_POINT('',(-86.9747563060399,33.3857031209377,107.));
#33128=CARTESIAN_POINT('Ctrl Pts',(-90.8371845881871,36.355240425647,107.708423447177));
#33129=CARTESIAN_POINT('Ctrl Pts',(-90.8375044446039,36.8504159072854,107.682880329042));
#33130=CARTESIAN_POINT('Ctrl Pts',(-90.4912521582202,38.3657324511424,107.604687703175));
#33131=CARTESIAN_POINT('Ctrl Pts',(-88.1200899510646,39.9637873692998,107.473845569578));
#33132=CARTESIAN_POINT('Ctrl Pts',(-84.9365305796935,38.6233314502058,107.315897046385));
#33133=CARTESIAN_POINT('Ctrl Pts',(-84.3257621873457,35.2211429743639,107.157948523192));
#33134=CARTESIAN_POINT('Ctrl Pts',(-85.9925177162683,33.6482971733151,107.052649507731));
#33135=CARTESIAN_POINT('Ctrl Pts',(-86.97475630604,33.3857031209377,107.));
#33136=CARTESIAN_POINT('',(-88.5623548711056,33.385703120938,107.));
#33137=CARTESIAN_POINT('Origin',(-87.7685555885722,36.3549260746835,107.));
#33138=CARTESIAN_POINT('Ctrl Pts',(-90.8468254863551,36.3557395475489,107.791576552823));
#33139=CARTESIAN_POINT('Ctrl Pts',(-90.8469815553513,36.4002483891304,107.789262006108));
#33140=CARTESIAN_POINT('Ctrl Pts',(-90.826021840379,37.4570579042178,107.734297951662));
#33141=CARTESIAN_POINT('Ctrl Pts',(-89.6167529221334,39.4750891176184,107.626684389485));
#33142=CARTESIAN_POINT('Ctrl Pts',(-86.1660869151683,39.6084645219268,107.468735866293));
#33143=CARTESIAN_POINT('Ctrl Pts',(-84.1684778438722,36.7911512436696,107.310787343101));
#33144=CARTESIAN_POINT('Ctrl Pts',(-85.4209928151755,33.6146075800065,107.154542054336));
#33145=CARTESIAN_POINT('Ctrl Pts',(-87.6173026093478,33.1297337487181,107.050946273303));
#33146=CARTESIAN_POINT('Ctrl Pts',(-88.5642689721409,33.3806144275731,107.));
#33147=CARTESIAN_POINT('Origin',(-87.7685555885722,36.3549260746835,124.208423447177));
#33148=CARTESIAN_POINT('',(-90.8384672418802,36.3567914691884,108.791576552823));
#33149=CARTESIAN_POINT('',(-90.8436484209055,36.3523677969953,108.708423447177));
#33150=CARTESIAN_POINT('',(-90.8420555885722,36.3549260746838,124.208423447177));
#33151=CARTESIAN_POINT('Ctrl Pts',(-90.8436484209055,36.3523677969953,108.708423447177));
#33152=CARTESIAN_POINT('Ctrl Pts',(-90.8362605641932,37.1811158020221,108.665444042093));
#33153=CARTESIAN_POINT('Ctrl Pts',(-90.0646115445956,39.0372061661879,108.569815129278));
#33154=CARTESIAN_POINT('Ctrl Pts',(-86.9355577907939,39.8844991017031,108.421536708732));
#33155=CARTESIAN_POINT('Ctrl Pts',(-84.3576616569105,37.5869248418109,108.26358818554));
#33156=CARTESIAN_POINT('Ctrl Pts',(-84.8723856581236,34.1722681478534,108.105639662347));
#33157=CARTESIAN_POINT('Ctrl Pts',(-88.0128424134507,32.7366980213559,107.947691139155));
#33158=CARTESIAN_POINT('Ctrl Pts',(-90.4599970867152,34.2830646424737,107.815285734098));
#33159=CARTESIAN_POINT('Ctrl Pts',(-90.8368451561489,35.8297595719873,107.735529836772));
#33160=CARTESIAN_POINT('Ctrl Pts',(-90.8371845881871,36.355240425647,107.708423447177));
#33161=CARTESIAN_POINT('Ctrl Pts',(-90.8384672418802,36.3567914691884,108.791576552823));
#33162=CARTESIAN_POINT('Ctrl Pts',(-90.8406113732891,36.7392744389716,108.771825719159));
#33163=CARTESIAN_POINT('Ctrl Pts',(-90.5976169530331,38.1387104789577,108.699425377765));
#33164=CARTESIAN_POINT('Ctrl Pts',(-88.5106433716724,39.9047352467602,108.57437552864));
#33165=CARTESIAN_POINT('Ctrl Pts',(-85.2017900681466,38.9168748712948,108.416427005448));
#33166=CARTESIAN_POINT('Ctrl Pts',(-84.2201469451404,35.6061628091222,108.258478482255));
#33167=CARTESIAN_POINT('Ctrl Pts',(-86.4557340134341,32.9743534903137,108.100529959063));
#33168=CARTESIAN_POINT('Ctrl Pts',(-89.8314223830532,33.4012134097122,107.944895982585));
#33169=CARTESIAN_POINT('Ctrl Pts',(-90.8434314192628,35.3877958929954,107.841911513838));
#33170=CARTESIAN_POINT('Ctrl Pts',(-90.8468254863551,36.3557395475489,107.791576552823));
#33171=CARTESIAN_POINT('Origin',(-87.7685555885722,36.3549260746835,124.208423447177));
#33172=CARTESIAN_POINT('',(-90.8403904938695,36.3523334141797,109.791576552823));
#33173=CARTESIAN_POINT('',(-90.8446863688317,36.3571941258315,109.708423447177));
#33174=CARTESIAN_POINT('',(-90.8420555885722,36.3549260746838,124.208423447177));
#33175=CARTESIAN_POINT('Ctrl Pts',(-90.8446863688317,36.3571941258315,109.708423447177));
#33176=CARTESIAN_POINT('Ctrl Pts',(-90.8459254901998,36.5068138702629,109.700657262876));
#33177=CARTESIAN_POINT('Ctrl Pts',(-90.7682625972272,37.6694638143677,109.640241570843));
#33178=CARTESIAN_POINT('Ctrl Pts',(-89.2869055754696,39.648322843942,109.52717637108));
#33179=CARTESIAN_POINT('Ctrl Pts',(-85.8408549227417,39.4267036912455,109.369227847887));
#33180=CARTESIAN_POINT('Ctrl Pts',(-84.1425914088798,36.4199976257601,109.211279324695));
#33181=CARTESIAN_POINT('Ctrl Pts',(-85.7318802150827,33.3542922832663,109.053330801502));
#33182=CARTESIAN_POINT('Ctrl Pts',(-89.1677588360808,33.0091721504837,108.89538227831));
#33183=CARTESIAN_POINT('Ctrl Pts',(-90.7452905864005,34.9660088512056,108.780413160201));
#33184=CARTESIAN_POINT('Ctrl Pts',(-90.8453106433724,36.1659045767385,108.718093549824));
#33185=CARTESIAN_POINT('Ctrl Pts',(-90.8436484209055,36.3523677969953,108.708423447177));
#33186=CARTESIAN_POINT('Ctrl Pts',(-90.8403904938695,36.3523334141797,109.791576552823));
#33187=CARTESIAN_POINT('Ctrl Pts',(-90.8345310481531,37.0713395984218,109.754389432211));
#33188=CARTESIAN_POINT('Ctrl Pts',(-90.2253200935287,38.8172614473035,109.664552803868));
#33189=CARTESIAN_POINT('Ctrl Pts',(-87.325110594749,39.9542601161072,109.522066667795));
#33190=CARTESIAN_POINT('Ctrl Pts',(-84.512232678954,37.9512375795022,109.364118144602));
#33191=CARTESIAN_POINT('Ctrl Pts',(-84.6517637344715,34.5008878105768,109.20616962141));
#33192=CARTESIAN_POINT('Ctrl Pts',(-87.6171951182148,32.7315384366804,109.048221098217));
#33193=CARTESIAN_POINT('Ctrl Pts',(-90.331884593125,34.0578509090687,108.910023408688));
#33194=CARTESIAN_POINT('Ctrl Pts',(-90.8348957936273,35.7196951939743,108.82447522689));
#33195=CARTESIAN_POINT('Ctrl Pts',(-90.8384672418802,36.3567914691884,108.791576552823));
#33196=CARTESIAN_POINT('Origin',(-87.7685555885722,36.3549260746835,124.208423447177));
#33197=CARTESIAN_POINT('',(-90.8468972727246,36.3556108815869,110.791576552823));
#33198=CARTESIAN_POINT('',(-90.8372746968057,36.3552744910384,110.708423447177));
#33199=CARTESIAN_POINT('',(-90.8420555885722,36.3549260746838,124.208423447177));
#33200=CARTESIAN_POINT('Ctrl Pts',(-90.8372746968057,36.3552744910384,110.708423447177));
#33201=CARTESIAN_POINT('Ctrl Pts',(-90.8377739922262,36.8438059966829,110.683220975927));
#33202=CARTESIAN_POINT('Ctrl Pts',(-90.4981129378111,38.3522539474203,110.605368996946));
#33203=CARTESIAN_POINT('Ctrl Pts',(-88.1425881647719,39.9621339138956,110.474867510234));
#33204=CARTESIAN_POINT('Ctrl Pts',(-84.952526116541,38.6400577459963,110.316918987042));
#33205=CARTESIAN_POINT('Ctrl Pts',(-84.3156723392984,35.2461221965173,110.158970463849));
#33206=CARTESIAN_POINT('Ctrl Pts',(-86.8094428010696,32.8575053889834,110.001021940657));
#33207=CARTESIAN_POINT('Ctrl Pts',(-90.0074378666204,33.6014242611079,109.850839601766));
#33208=CARTESIAN_POINT('Ctrl Pts',(-90.8375250804865,35.4924926045081,109.753306770606));
#33209=CARTESIAN_POINT('Ctrl Pts',(-90.8446863688317,36.3571941258315,109.708423447177));
#33210=CARTESIAN_POINT('Ctrl Pts',(-90.8468972727246,36.3556108815869,110.791576552823));
#33211=CARTESIAN_POINT('Ctrl Pts',(-90.8470129167021,36.3935671709611,110.789602652993));
#33212=CARTESIAN_POINT('Ctrl Pts',(-90.8292489756467,37.4438146379521,110.734979245433));
#33213=CARTESIAN_POINT('Ctrl Pts',(-89.6367303689711,39.4632652024454,110.627706330142));
#33214=CARTESIAN_POINT('Ctrl Pts',(-86.1870500209474,39.6184654540127,110.46975780695));
#33215=CARTESIAN_POINT('Ctrl Pts',(-84.1712726716061,36.8147138073089,110.311809283757));
#33216=CARTESIAN_POINT('Ctrl Pts',(-85.417042337004,33.594086605388,110.153860760565));
#33217=CARTESIAN_POINT('Ctrl Pts',(-88.7948575488562,32.8766285869604,109.995912237372));
#33218=CARTESIAN_POINT('Ctrl Pts',(-90.665968377309,34.7392604855723,109.875150834792));
#33219=CARTESIAN_POINT('Ctrl Pts',(-90.8428268486203,36.0533709836683,109.807038939942));
#33220=CARTESIAN_POINT('Ctrl Pts',(-90.8403904938695,36.3523334141797,109.791576552823));
#33221=CARTESIAN_POINT('Origin',(-87.7685555885722,36.3549260746835,124.208423447177));
#33222=CARTESIAN_POINT('',(-90.8385928893407,36.3568681301786,111.791576552823));
#33223=CARTESIAN_POINT('',(-90.8434554977008,36.3523302811269,111.708423447177));
#33224=CARTESIAN_POINT('',(-90.8420555885722,36.3549260746838,124.208423447177));
#33225=CARTESIAN_POINT('Ctrl Pts',(-90.8434554977008,36.3523302811269,111.708423447177));
#33226=CARTESIAN_POINT('Ctrl Pts',(-90.8360746186667,37.174642245983,111.665784688979));
#33227=CARTESIAN_POINT('Ctrl Pts',(-90.0746147106792,39.0243970272075,111.570496423049));
#33228=CARTESIAN_POINT('Ctrl Pts',(-86.9582295306161,39.8897839838954,111.422558649389));
#33229=CARTESIAN_POINT('Ctrl Pts',(-84.3656607621669,37.6087823498066,111.264610126197));
#33230=CARTESIAN_POINT('Ctrl Pts',(-84.858393238377,34.1909473654533,111.106661603004));
#33231=CARTESIAN_POINT('Ctrl Pts',(-87.9896814090755,32.7351260621679,110.948713079812));
#33232=CARTESIAN_POINT('Ctrl Pts',(-90.4528392552173,34.269885868269,110.815967027869));
#33233=CARTESIAN_POINT('Ctrl Pts',(-90.8367309334783,35.8232337270908,110.735870483658));
#33234=CARTESIAN_POINT('Ctrl Pts',(-90.8372746968057,36.3552744910384,110.708423447177));
#33235=CARTESIAN_POINT('Ctrl Pts',(-90.8385928893406,36.3568681301786,111.791576552823));
#33236=CARTESIAN_POINT('Ctrl Pts',(-90.8407925664026,36.7327156432091,111.772166366045));
#33237=CARTESIAN_POINT('Ctrl Pts',(-90.6033582589985,38.1253552741901,111.700106671536));
#33238=CARTESIAN_POINT('Ctrl Pts',(-88.5334211413281,39.8998985469101,111.575397469297));
#33239=CARTESIAN_POINT('Ctrl Pts',(-85.2182937675741,38.9333003273795,111.417448946105));
#33240=CARTESIAN_POINT('Ctrl Pts',(-84.21541122421,35.6289685906495,111.259500422912));
#33241=CARTESIAN_POINT('Ctrl Pts',(-86.4340566120166,32.9828404256698,111.10155189972));
#33242=CARTESIAN_POINT('Ctrl Pts',(-89.8198041109555,33.3889404587613,110.945577276356));
#33243=CARTESIAN_POINT('Ctrl Pts',(-90.8439283637791,35.3811652642377,110.842252160724));
#33244=CARTESIAN_POINT('Ctrl Pts',(-90.8468972727246,36.3556108815869,110.791576552823));
#33245=CARTESIAN_POINT('Origin',(-87.7685555885722,36.3549260746835,124.208423447177));
#33246=CARTESIAN_POINT('',(-90.8402144015523,36.3523700744382,112.791576552823));
#33247=CARTESIAN_POINT('',(-90.8448621506013,36.3571283696629,112.708423447177));
#33248=CARTESIAN_POINT('',(-90.8420555885722,36.3549260746838,124.208423447177));
#33249=CARTESIAN_POINT('Ctrl Pts',(-90.8448621506013,36.3571283696629,112.708423447177));
#33250=CARTESIAN_POINT('Ctrl Pts',(-90.8460230140249,36.5001640472249,112.700997909761));
#33251=CARTESIAN_POINT('Ctrl Pts',(-90.7722166884106,37.6561661169679,112.640922864614));
#33252=CARTESIAN_POINT('Ctrl Pts',(-89.3080212269955,39.6385055706828,112.528198311736));
#33253=CARTESIAN_POINT('Ctrl Pts',(-85.8606184245708,39.4390182485099,112.370249788544));
#33254=CARTESIAN_POINT('Ctrl Pts',(-84.1430842214608,36.4432783507515,112.212301265351));
#33255=CARTESIAN_POINT('Ctrl Pts',(-85.7126546431824,33.3674321313963,112.054352742159));
#33256=CARTESIAN_POINT('Ctrl Pts',(-89.1462479246903,33.0002558098966,111.896404218967));
#33257=CARTESIAN_POINT('Ctrl Pts',(-90.7410210066454,34.9526930047544,111.781094453973));
#33258=CARTESIAN_POINT('Ctrl Pts',(-90.8451883842683,36.1592674560054,111.71843419671));
#33259=CARTESIAN_POINT('Ctrl Pts',(-90.8434554977008,36.3523302811269,111.708423447177));
#33260=CARTESIAN_POINT('Ctrl Pts',(-90.8402144015524,36.3523700744382,112.791576552823));
#33261=CARTESIAN_POINT('Ctrl Pts',(-90.8345153488798,37.064893455906,112.754730079097));
#33262=CARTESIAN_POINT('Ctrl Pts',(-90.2341640589546,38.8041985290923,112.66523409764));
#33263=CARTESIAN_POINT('Ctrl Pts',(-87.3482310510782,39.957033294882,112.523088608452));
#33264=CARTESIAN_POINT('Ctrl Pts',(-84.5225497279198,37.9721134773169,112.365140085259));
#33265=CARTESIAN_POINT('Ctrl Pts',(-84.6399231958095,34.5209390263157,112.207191562067));
#33266=CARTESIAN_POINT('Ctrl Pts',(-87.5939325011642,32.7325848538746,112.049243038874));
#33267=CARTESIAN_POINT('Ctrl Pts',(-90.3237945448813,34.0446656332115,111.91070470246));
#33268=CARTESIAN_POINT('Ctrl Pts',(-90.8348260130765,35.7132413450188,111.824815873776));
#33269=CARTESIAN_POINT('Ctrl Pts',(-90.8385928893406,36.3568681301786,111.791576552823));
#33270=CARTESIAN_POINT('Origin',(-87.7685555885722,36.3549260746835,124.208423447177));
#33271=CARTESIAN_POINT('',(-90.8469565090695,36.3554949864144,113.791576552823));
#33272=CARTESIAN_POINT('',(-90.8373005739091,36.3553794097185,113.708423447177));
#33273=CARTESIAN_POINT('',(-90.8420555885722,36.3549260746838,124.208423447177));
#33274=CARTESIAN_POINT('Ctrl Pts',(-90.8373005739091,36.3553794097185,113.708423447178));
#33275=CARTESIAN_POINT('Ctrl Pts',(-90.8379417505728,36.8372975674189,113.683561622813));
#33276=CARTESIAN_POINT('Ctrl Pts',(-90.5047600111548,38.338927938775,113.606050290717));
#33277=CARTESIAN_POINT('Ctrl Pts',(-88.16574233066,39.9596578886113,113.475889450891));
#33278=CARTESIAN_POINT('Ctrl Pts',(-84.9672569937481,38.6580923607057,113.317940927699));
#33279=CARTESIAN_POINT('Ctrl Pts',(-84.3086238951178,35.2683160089,113.159992404506));
#33280=CARTESIAN_POINT('Ctrl Pts',(-86.7870056338769,32.863735955989,113.002043881314));
#33281=CARTESIAN_POINT('Ctrl Pts',(-89.99697594205,33.5887459138352,112.851520895538));
#33282=CARTESIAN_POINT('Ctrl Pts',(-90.8377921097319,35.485993948889,112.753647417492));
#33283=CARTESIAN_POINT('Ctrl Pts',(-90.8448621506013,36.3571283696629,112.708423447177));
#33284=CARTESIAN_POINT('Ctrl Pts',(-90.8469565090695,36.3554949864144,113.791576552823));
#33285=CARTESIAN_POINT('Ctrl Pts',(-90.8470371923431,36.38689932666,113.789943299879));
#33286=CARTESIAN_POINT('Ctrl Pts',(-90.8324320241331,37.4305764646951,113.735660539204));
#33287=CARTESIAN_POINT('Ctrl Pts',(-89.6566504974584,39.4512055771937,113.628728270799));
#33288=CARTESIAN_POINT('Ctrl Pts',(-86.2080378044846,39.6285530216908,113.470779747607));
#33289=CARTESIAN_POINT('Ctrl Pts',(-84.1742991253402,36.8378024761994,113.312831224414));
#33290=CARTESIAN_POINT('Ctrl Pts',(-85.3993634670394,33.6092425834755,113.154882701222));
#33291=CARTESIAN_POINT('Ctrl Pts',(-88.7725022496111,32.8701104060413,112.996934178029));
#33292=CARTESIAN_POINT('Ctrl Pts',(-90.6608461669204,34.7259096736242,112.875832128563));
#33293=CARTESIAN_POINT('Ctrl Pts',(-90.8426586605023,36.0467768904004,112.807379586827));
#33294=CARTESIAN_POINT('Ctrl Pts',(-90.8402144015524,36.3523700744382,112.791576552823));
#33295=CARTESIAN_POINT('Origin',(-87.7685555885722,36.3549260746835,124.208423447177));
#33296=CARTESIAN_POINT('',(-90.8387237914782,36.3569420805603,114.791576552823));
#33297=CARTESIAN_POINT('',(-90.8432613144075,36.3522971348084,114.708423447177));
#33298=CARTESIAN_POINT('',(-90.8420555885722,36.3549260746838,124.208423447177));
#33299=CARTESIAN_POINT('Ctrl Pts',(-90.8432613144075,36.3522971348084,114.708423447177));
#33300=CARTESIAN_POINT('Ctrl Pts',(-90.8358994837641,37.1681724947489,114.666125335864));
#33301=CARTESIAN_POINT('Ctrl Pts',(-90.0845448816577,39.0115735013954,114.571177716821));
#33302=CARTESIAN_POINT('Ctrl Pts',(-86.9809435523238,39.8949142157357,114.423580590046));
#33303=CARTESIAN_POINT('Ctrl Pts',(-84.373781921353,37.630606484029,114.265632066854));
#33304=CARTESIAN_POINT('Ctrl Pts',(-84.8445583270759,34.2096781232347,114.107683543661));
#33305=CARTESIAN_POINT('Ctrl Pts',(-87.9664341204409,32.7337808352518,113.949735020469));
#33306=CARTESIAN_POINT('Ctrl Pts',(-90.445741881575,34.256590833291,113.816648321641));
#33307=CARTESIAN_POINT('Ctrl Pts',(-90.8365839404934,35.8167468066471,113.736211130544));
#33308=CARTESIAN_POINT('Ctrl Pts',(-90.8373005739091,36.3553794097185,113.708423447178));
#33309=CARTESIAN_POINT('Ctrl Pts',(-90.8387237914782,36.3569420805603,114.791576552823));
#33310=CARTESIAN_POINT('Ctrl Pts',(-90.8409732941709,36.7261539149222,114.772507012931));
#33311=CARTESIAN_POINT('Ctrl Pts',(-90.6090448889861,38.1119999363053,114.700787965308));
#33312=CARTESIAN_POINT('Ctrl Pts',(-88.5561676363232,39.8949142674411,114.576419409954));
#33313=CARTESIAN_POINT('Ctrl Pts',(-85.2349020777131,38.9496224017201,114.418470886762));
#33314=CARTESIAN_POINT('Ctrl Pts',(-84.2108230998106,35.6517982903965,114.260522363569));
#33315=CARTESIAN_POINT('Ctrl Pts',(-86.412431965926,32.9914787564211,114.102573840377));
#33316=CARTESIAN_POINT('Ctrl Pts',(-89.8081172142279,33.3766699586493,113.946258570128));
#33317=CARTESIAN_POINT('Ctrl Pts',(-90.8444362880251,35.3745496713466,113.84259280761));
#33318=CARTESIAN_POINT('Ctrl Pts',(-90.8469565090695,36.3554949864144,113.791576552823));
#33319=CARTESIAN_POINT('Origin',(-87.7685555885722,36.3549260746835,124.208423447177));
#33320=CARTESIAN_POINT('',(-90.8400416161831,36.3524106996081,115.791576552823));
#33321=CARTESIAN_POINT('',(-90.845034052782,36.3570585842589,115.708423447177));
#33322=CARTESIAN_POINT('',(-90.8420555885722,36.3549260746838,124.208423447177));
#33323=CARTESIAN_POINT('Ctrl Pts',(-90.845034052782,36.3570585842589,115.708423447177));
#33324=CARTESIAN_POINT('Ctrl Pts',(-90.8461165882359,36.4935125756602,115.701338556647));
#33325=CARTESIAN_POINT('Ctrl Pts',(-90.7761238734907,37.6428715883725,115.641604158386));
#33326=CARTESIAN_POINT('Ctrl Pts',(-89.3290733498657,39.6285529738767,115.529220252393));
#33327=CARTESIAN_POINT('Ctrl Pts',(-85.8804607072626,39.4512055319686,115.371271729201));
#33328=CARTESIAN_POINT('Ctrl Pts',(-84.143726269733,36.466555675223,115.213323206008));
#33329=CARTESIAN_POINT('Ctrl Pts',(-85.6935143313946,33.3806946547291,115.055374682816));
#33330=CARTESIAN_POINT('Ctrl Pts',(-89.1246791914122,32.9914788055483,114.897426159624));
#33331=CARTESIAN_POINT('Ctrl Pts',(-90.7367041935985,34.939373215214,114.781775747744));
#33332=CARTESIAN_POINT('Ctrl Pts',(-90.8450629368673,36.1526322085003,114.718774843595));
#33333=CARTESIAN_POINT('Ctrl Pts',(-90.8432613144075,36.3522971348084,114.708423447177));
#33334=CARTESIAN_POINT('Ctrl Pts',(-90.8400416161831,36.3524106996081,115.791576552823));
#33335=CARTESIAN_POINT('Ctrl Pts',(-90.8345080235632,37.058447369207,115.755070725982));
#33336=CARTESIAN_POINT('Ctrl Pts',(-90.242941846011,38.7911234504317,115.665915391411));
#33337=CARTESIAN_POINT('Ctrl Pts',(-87.3713688406819,39.959657941262,115.524110549109));
#33338=CARTESIAN_POINT('Ctrl Pts',(-84.5330006014756,37.9929227377143,115.366162025916));
#33339=CARTESIAN_POINT('Ctrl Pts',(-84.6282116641132,34.5410657772132,115.208213502724));
#33340=CARTESIAN_POINT('Ctrl Pts',(-87.5706770538148,32.7337807823612,115.050264979531));
#33341=CARTESIAN_POINT('Ctrl Pts',(-90.3156406263894,34.0314891348168,114.911385996231));
#33342=CARTESIAN_POINT('Ctrl Pts',(-90.8347625932267,35.7067889256462,114.825156520661));
#33343=CARTESIAN_POINT('Ctrl Pts',(-90.8387237914782,36.3569420805603,114.791576552823));
#33344=CARTESIAN_POINT('Origin',(-87.7685555885722,36.3549260746835,124.208423447177));
#33345=CARTESIAN_POINT('',(-90.8470054143286,36.355377816704,116.791576552823));
#33346=CARTESIAN_POINT('',(-90.8373332185204,36.3554836682631,116.708423447177));
#33347=CARTESIAN_POINT('',(-90.8420555885722,36.3549260746838,124.208423447177));
#33348=CARTESIAN_POINT('Ctrl Pts',(-90.8373332185204,36.3554836682631,116.708423447177));
#33349=CARTESIAN_POINT('Ctrl Pts',(-90.8381115230835,36.8307861352947,116.683902269698));
#33350=CARTESIAN_POINT('Ctrl Pts',(-90.5113487431761,38.3255987424985,116.606731584489));
#33351=CARTESIAN_POINT('Ctrl Pts',(-88.1888801199258,39.9570332422698,116.476911391548));
#33352=CARTESIAN_POINT('Ctrl Pts',(-84.9821033690532,38.6760320151288,116.318962868356));
#33353=CARTESIAN_POINT('Ctrl Pts',(-84.3017180995052,35.2905546250324,116.161014345163));
#33354=CARTESIAN_POINT('Ctrl Pts',(-86.7646089421984,32.8701104569402,116.003065821971));
#33355=CARTESIAN_POINT('Ctrl Pts',(-89.9864431986579,33.5760883377251,115.852202189309));
#33356=CARTESIAN_POINT('Ctrl Pts',(-90.8380720096351,35.4794904896189,115.753988064378));
#33357=CARTESIAN_POINT('Ctrl Pts',(-90.845034052782,36.3570585842589,115.708423447177));
#33358=CARTESIAN_POINT('Ctrl Pts',(-90.8470054143286,36.355377816704,116.791576552823));
#33359=CARTESIAN_POINT('Ctrl Pts',(-90.8470569015836,36.3802311058533,116.790283946765));
#33360=CARTESIAN_POINT('Ctrl Pts',(-90.8355714137741,37.4173420438333,116.736341832976));
#33361=CARTESIAN_POINT('Ctrl Pts',(-89.6764927804399,39.4390182935569,116.629750211456));
#33362=CARTESIAN_POINT('Ctrl Pts',(-86.2290899276622,39.6385056186423,116.471801688264));
#33363=CARTESIAN_POINT('Ctrl Pts',(-84.1774737689002,36.8608712367781,116.313853165071));
#33364=CARTESIAN_POINT('Ctrl Pts',(-85.3817822782182,33.6245117640691,116.155904641879));
#33365=CARTESIAN_POINT('Ctrl Pts',(-88.7501055576055,32.8637359049969,115.997956118686));
#33366=CARTESIAN_POINT('Ctrl Pts',(-90.6556717462417,34.7125578096458,115.876513422334));
#33367=CARTESIAN_POINT('Ctrl Pts',(-90.8424886927505,36.0401857295852,115.807720233713));
#33368=CARTESIAN_POINT('Ctrl Pts',(-90.8400416161831,36.3524106996081,115.791576552823));
#33369=CARTESIAN_POINT('Origin',(-87.7685555885722,36.3549260746835,124.208423447177));
#33370=CARTESIAN_POINT('',(-90.8388598290993,36.3570130097889,117.791576552823));
#33371=CARTESIAN_POINT('',(-90.8430661113431,36.3522684582546,117.708423447177));
#33372=CARTESIAN_POINT('',(-90.8420555885722,36.3549260746838,124.208423447177));
#33373=CARTESIAN_POINT('Ctrl Pts',(-90.8430661113431,36.3522684582546,117.708423447177));
#33374=CARTESIAN_POINT('Ctrl Pts',(-90.8357356935995,37.1617056224215,117.66646598275));
#33375=CARTESIAN_POINT('Ctrl Pts',(-90.0944057462884,38.9987324296382,117.571859010592));
#33376=CARTESIAN_POINT('Ctrl Pts',(-87.0036900469868,39.8998984951319,117.424602530703));
#33377=CARTESIAN_POINT('Ctrl Pts',(-84.3820430458739,37.6523780223793,117.26665400751));
#33378=CARTESIAN_POINT('Ctrl Pts',(-84.8308439711031,34.228497328871,117.108705484318));
#33379=CARTESIAN_POINT('Ctrl Pts',(-87.9431786734311,32.7325849067827,116.950756961125));
#33380=CARTESIAN_POINT('Ctrl Pts',(-90.4385841834224,34.2433008167291,116.817329615412));
#33381=CARTESIAN_POINT('Ctrl Pts',(-90.8364404225768,35.8102625110144,116.736551777429));
#33382=CARTESIAN_POINT('Ctrl Pts',(-90.8373332185204,36.3554836682631,116.708423447177));
#33383=CARTESIAN_POINT('Ctrl Pts',(-90.8388598290993,36.3570130097889,117.791576552823));
#33384=CARTESIAN_POINT('Ctrl Pts',(-90.8411534611211,36.7195890353653,117.772847659816));
#33385=CARTESIAN_POINT('Ctrl Pts',(-90.6146771194904,38.0986443635484,117.701469259079));
#33386=CARTESIAN_POINT('Ctrl Pts',(-88.5788816583627,39.8897840355259,117.577441350611));
#33387=CARTESIAN_POINT('Ctrl Pts',(-85.2516148494836,38.9658374976431,117.419492827418));
#33388=CARTESIAN_POINT('Ctrl Pts',(-84.2063816594615,35.6746569798619,117.261544304226));
#33389=CARTESIAN_POINT('Ctrl Pts',(-86.3908632323328,33.0002557608977,117.103595781033));
#33390=CARTESIAN_POINT('Ctrl Pts',(-89.7963570069237,33.3644272205121,116.946939863899));
#33391=CARTESIAN_POINT('Ctrl Pts',(-90.8449597594478,35.3679246640809,116.842933454495));
#33392=CARTESIAN_POINT('Ctrl Pts',(-90.8470054143286,36.355377816704,116.791576552823));
#33393=CARTESIAN_POINT('Origin',(-87.7685555885722,36.3549260746835,124.208423447177));
#33394=CARTESIAN_POINT('',(-90.8398723581442,36.3524552105476,118.791576552823));
#33395=CARTESIAN_POINT('',(-90.8452017125077,36.3569848687002,118.708423447177));
#33396=CARTESIAN_POINT('',(-90.8420555885722,36.3549260746838,124.208423447177));
#33397=CARTESIAN_POINT('Ctrl Pts',(-90.8452017125077,36.3569848687002,118.708423447177));
#33398=CARTESIAN_POINT('Ctrl Pts',(-90.8462061475006,36.4868595329243,118.701679203533));
#33399=CARTESIAN_POINT('Ctrl Pts',(-90.7799843510519,37.6295802855217,118.642285452157));
#33400=CARTESIAN_POINT('Ctrl Pts',(-89.3500611330962,39.6184654063458,118.53024219305));
#33401=CARTESIAN_POINT('Ctrl Pts',(-85.9003808354589,39.4632651570443,118.372293669858));
#33402=CARTESIAN_POINT('Ctrl Pts',(-84.144517768422,36.4898283971866,118.214345146665));
#33403=CARTESIAN_POINT('Ctrl Pts',(-85.6744595728268,33.3940798045978,118.056396623473));
#33404=CARTESIAN_POINT('Ctrl Pts',(-89.1030545456374,32.9828404749231,117.89844810028));
#33405=CARTESIAN_POINT('Ctrl Pts',(-90.7323386857844,34.9260508120483,117.782457041515));
#33406=CARTESIAN_POINT('Ctrl Pts',(-90.8449341256527,36.1459991488762,117.719115490481));
#33407=CARTESIAN_POINT('Ctrl Pts',(-90.8430661113431,36.3522684582546,117.708423447177));
#33408=CARTESIAN_POINT('Ctrl Pts',(-90.8398723581442,36.3524552105476,118.791576552823));
#33409=CARTESIAN_POINT('Ctrl Pts',(-90.8345088849513,37.052001191776,118.755411372868));
#33410=CARTESIAN_POINT('Ctrl Pts',(-90.2516536622113,38.7780365130427,118.666596685182));
#33411=CARTESIAN_POINT('Ctrl Pts',(-87.394523006908,39.962133966582,118.525132489766));
#33412=CARTESIAN_POINT('Ctrl Pts',(-84.5435848754497,38.0136644637222,118.367183966573));
#33413=CARTESIAN_POINT('Ctrl Pts',(-84.6166296078616,34.5612673131065,118.209235443381));
#33414=CARTESIAN_POINT('Ctrl Pts',(-87.5474297648405,32.7351260092969,118.051286920188));
#33415=CARTESIAN_POINT('Ctrl Pts',(-90.3074225693738,34.0183219665893,117.912067290002));
#33416=CARTESIAN_POINT('Ctrl Pts',(-90.8347057443862,35.7003376970687,117.825497167547));
#33417=CARTESIAN_POINT('Ctrl Pts',(-90.8388598290993,36.3570130097889,117.791576552823));
#33418=CARTESIAN_POINT('Origin',(-87.7685555885722,36.3549260746835,124.208423447177));
#33419=CARTESIAN_POINT('',(-90.8470436441738,36.3552596744299,119.791576552823));
#33420=CARTESIAN_POINT('',(-90.8373725915384,36.3555871000405,119.708423447177));
#33421=CARTESIAN_POINT('',(-90.8420555885722,36.3549260746838,124.208423447177));
#33422=CARTESIAN_POINT('Ctrl Pts',(-90.8373725915384,36.3555871000405,119.708423447177));
#33423=CARTESIAN_POINT('Ctrl Pts',(-90.8382831445492,36.8242716643461,119.684242916584));
#33424=CARTESIAN_POINT('Ctrl Pts',(-90.5178793708824,38.3122665852445,119.60741287826));
#33425=CARTESIAN_POINT('Ctrl Pts',(-88.2120005759172,39.9542600635284,119.477933332205));
#33426=CARTESIAN_POINT('Ctrl Pts',(-84.9970646304694,38.6938759803182,119.319984809012));
#33427=CARTESIAN_POINT('Ctrl Pts',(-84.2949552395589,35.3128371203772,119.16203628582));
#33428=CARTESIAN_POINT('Ctrl Pts',(-86.7422536432798,32.8766286377651,119.004087762628));
#33429=CARTESIAN_POINT('Ctrl Pts',(-89.9758394835887,33.5634519078074,118.85288348308));
#33430=CARTESIAN_POINT('Ctrl Pts',(-90.8383649408792,35.4729819955614,118.754328711263));
#33431=CARTESIAN_POINT('Ctrl Pts',(-90.8452017125077,36.3569848687002,118.708423447177));
#33432=CARTESIAN_POINT('Ctrl Pts',(-90.8470436441738,36.3552596744299,119.791576552823));
#33433=CARTESIAN_POINT('Ctrl Pts',(-90.847072089005,36.3735626432968,119.79062459365));
#33434=CARTESIAN_POINT('Ctrl Pts',(-90.8386674461304,37.4041115135856,119.737023126747));
#33435=CARTESIAN_POINT('Ctrl Pts',(-89.6962562825846,39.4267037361566,119.630772152113));
#33436=CARTESIAN_POINT('Ctrl Pts',(-86.2502055794825,39.6483228920224,119.47282362892));
#33437=CARTESIAN_POINT('Ctrl Pts',(-84.1807964437643,36.8839191095796,119.314875105728));
#33438=CARTESIAN_POINT('Ctrl Pts',(-85.3642995086962,33.6398935322125,119.156926582536));
#33439=CARTESIAN_POINT('Ctrl Pts',(-88.727668390087,32.8575053379033,118.998978059343));
#33440=CARTESIAN_POINT('Ctrl Pts',(-90.650444889663,34.6992050189384,118.877194716105));
#33441=CARTESIAN_POINT('Ctrl Pts',(-90.8423170646337,36.0335975340926,118.808060880599));
#33442=CARTESIAN_POINT('Ctrl Pts',(-90.8398723581442,36.3524552105476,118.791576552823));
#33443=CARTESIAN_POINT('Origin',(-87.7685555885722,36.3549260746835,124.208423447177));
#33444=CARTESIAN_POINT('',(-90.8389970126702,36.3570769587632,120.791576552823));
#33445=CARTESIAN_POINT('',(-90.84286984995,36.3522423553315,120.708423447177));
#33446=CARTESIAN_POINT('',(-90.8420555885722,36.3549260746838,124.208423447177));
#33447=CARTESIAN_POINT('Ctrl Pts',(-90.84286984995,36.3522423553315,120.708423447177));
#33448=CARTESIAN_POINT('Ctrl Pts',(-90.8355827220701,37.1552395412463,120.666806629636));
#33449=CARTESIAN_POINT('Ctrl Pts',(-90.1041979681009,38.9858767921816,120.572540304363));
#33450=CARTESIAN_POINT('Ctrl Pts',(-87.0264678163487,39.9047351945452,120.42562447136));
#33451=CARTESIAN_POINT('Ctrl Pts',(-84.3904439217461,37.6740967587225,120.267675948167));
#33452=CARTESIAN_POINT('Ctrl Pts',(-84.8172506743583,34.2474038701722,120.109727424975));
#33453=CARTESIAN_POINT('Ctrl Pts',(-87.9199160567175,32.7315384896552,119.951778901782));
#33454=CARTESIAN_POINT('Ctrl Pts',(-90.431365923944,34.2300160043642,119.818010909183));
#33455=CARTESIAN_POINT('Ctrl Pts',(-90.8363005508424,35.8037807575614,119.736892424315));
#33456=CARTESIAN_POINT('Ctrl Pts',(-90.8373725915384,36.3555871000405,119.708423447177));
#33457=CARTESIAN_POINT('Ctrl Pts',(-90.8389970126702,36.3570769587632,120.791576552823));
#33458=CARTESIAN_POINT('Ctrl Pts',(-90.8413323422268,36.7130204263635,120.773188306702));
#33459=CARTESIAN_POINT('Ctrl Pts',(-90.6202675433234,38.0853011148081,120.70215055285));
#33460=CARTESIAN_POINT('Ctrl Pts',(-88.601553399534,39.8844991555637,120.578463291268));
#33461=CARTESIAN_POINT('Ctrl Pts',(-85.2684357075705,38.981949277713,120.420514768075));
#33462=CARTESIAN_POINT('Ctrl Pts',(-84.202084988714,35.697541610575,120.262566244883));
#33463=CARTESIAN_POINT('Ctrl Pts',(-86.3693523204529,33.0091721012914,120.10461772169));
#33464=CARTESIAN_POINT('Ctrl Pts',(-89.7845228766894,33.3522121930534,119.94762115767));
#33465=CARTESIAN_POINT('Ctrl Pts',(-90.8454989056133,35.3612899231855,119.843274101381));
#33466=CARTESIAN_POINT('Ctrl Pts',(-90.8470436441738,36.3552596744299,119.791576552823));
#33467=CARTESIAN_POINT('Origin',(-87.7685555885722,36.3549260746835,124.208423447177));
#33468=CARTESIAN_POINT('',(-90.8388342008425,36.3519111454271,121.791576552823));
#33469=CARTESIAN_POINT('',(-90.8453550251769,36.3568536361305,121.708423447177));
#33470=CARTESIAN_POINT('',(-90.8420555885722,36.3549260746838,124.208423447177));
#33471=CARTESIAN_POINT('',(-88.5623548711056,33.385703120938,122.));
#33472=CARTESIAN_POINT('Ctrl Pts',(-88.5623548711056,33.385703120938,122.));
#33473=CARTESIAN_POINT('Ctrl Pts',(-89.5445934608772,33.6482971733158,121.947350492269));
#33474=CARTESIAN_POINT('Ctrl Pts',(-90.6442900920727,34.6860341601982,121.877876009877));
#33475=CARTESIAN_POINT('Ctrl Pts',(-90.8411753710437,36.0264353653473,121.808401527484));
#33476=CARTESIAN_POINT('Ctrl Pts',(-90.8388342008425,36.3519111454271,121.791576552823));
#33477=CARTESIAN_POINT('',(-86.9728468550288,33.380626780384,122.));
#33478=CARTESIAN_POINT('Origin',(-87.7685555885722,36.3549260746835,122.));
#33479=CARTESIAN_POINT('Ctrl Pts',(-86.972842220194,33.3806144585182,122.));
#33480=CARTESIAN_POINT('Ctrl Pts',(-87.9198086173169,33.1297337454483,121.949053726697));
#33481=CARTESIAN_POINT('Ctrl Pts',(-89.9803571320055,33.5846360429098,121.851861542423));
#33482=CARTESIAN_POINT('Ctrl Pts',(-90.8386915121384,35.4665790111915,121.754669358149));
#33483=CARTESIAN_POINT('Ctrl Pts',(-90.8453550251768,36.3568536361305,121.708423447177));
#33484=CARTESIAN_POINT('Origin',(87.7685555885722,-36.3549260746835,114.));
#33485=CARTESIAN_POINT('',(85.2550452373729,-36.354668632511,107.387416697508));
#33486=CARTESIAN_POINT('',(85.2529645136107,-36.3584982898635,107.112583302492));
#33487=CARTESIAN_POINT('',(85.2510555885723,-36.3549260746835,114.));
#33488=CARTESIAN_POINT('',(85.8550895919076,-34.7189388713081,107.));
#33489=CARTESIAN_POINT('Ctrl Pts',(85.2529645136107,-36.3584982898635,107.112583302492));
#33490=CARTESIAN_POINT('Ctrl Pts',(85.2581100669596,-35.7658638142766,107.075055534995));
#33491=CARTESIAN_POINT('Ctrl Pts',(85.4693337604884,-35.1701225143786,107.037527767497));
#33492=CARTESIAN_POINT('Ctrl Pts',(85.8550895919077,-34.718938871308,107.));
#33493=CARTESIAN_POINT('',(85.2510555885723,-36.3549260746835,107.));
#33494=CARTESIAN_POINT('Origin',(87.7685555885722,-36.3549260746835,107.));
#33495=CARTESIAN_POINT('',(85.2510555885723,-36.3549260746835,106.));
#33496=CARTESIAN_POINT('',(85.2510555885723,-36.3549260746835,114.));
#33497=CARTESIAN_POINT('Origin',(87.7685555885722,-36.3549260746835,106.));
#33498=CARTESIAN_POINT('',(89.6856659018966,-34.7163980987228,107.));
#33499=CARTESIAN_POINT('Origin',(87.7685555885722,-36.3549260746835,107.));
#33500=CARTESIAN_POINT('Ctrl Pts',(89.685674748321,-34.7163919311049,107.));
#33501=CARTESIAN_POINT('Ctrl Pts',(89.1628542081215,-34.1076769579869,107.050946273303));
#33502=CARTESIAN_POINT('Ctrl Pts',(88.3231296580498,-33.7675004276397,107.101892546605));
#33503=CARTESIAN_POINT('Ctrl Pts',(87.5244587616235,-33.8452631801865,107.152838819908));
#33504=CARTESIAN_POINT('Ctrl Pts',(86.6990867214356,-33.9256256949687,107.205488327639));
#33505=CARTESIAN_POINT('Ctrl Pts',(85.9175592297027,-34.4523396916042,107.25813783537));
#33506=CARTESIAN_POINT('Ctrl Pts',(85.5336746027685,-35.1871265063861,107.3107873431));
#33507=CARTESIAN_POINT('Ctrl Pts',(85.3474314487688,-35.5436112528458,107.336330461236));
#33508=CARTESIAN_POINT('Ctrl Pts',(85.2547832386249,-35.9490710104433,107.361873579372));
#33509=CARTESIAN_POINT('Ctrl Pts',(85.2550452373729,-36.354668632511,107.387416697508));
#33510=CARTESIAN_POINT('Origin',(87.7685555885722,-36.3549260746835,114.));
#33511=CARTESIAN_POINT('',(85.2497507212102,-36.3570215567107,108.387416697508));
#33512=CARTESIAN_POINT('',(85.2471487745657,-36.3542597485476,108.112583302492));
#33513=CARTESIAN_POINT('',(85.2510555885723,-36.3549260746835,114.));
#33514=CARTESIAN_POINT('Ctrl Pts',(85.2471487745657,-36.3542597485476,108.112583302492));
#33515=CARTESIAN_POINT('Ctrl Pts',(85.2470209387648,-36.3178026153987,108.110268755777));
#33516=CARTESIAN_POINT('Ctrl Pts',(85.2477438897639,-36.2813507190277,108.107954209062));
#33517=CARTESIAN_POINT('Ctrl Pts',(85.2493335062549,-36.2449367209381,108.105639662347));
#33518=CARTESIAN_POINT('Ctrl Pts',(85.2854928653183,-35.4166194259904,108.052990154616));
#33519=CARTESIAN_POINT('Ctrl Pts',(85.7700962403271,-34.6079120701247,108.000340646886));
#33520=CARTESIAN_POINT('Ctrl Pts',(86.483470577241,-34.1853504230939,107.947691139155));
#33521=CARTESIAN_POINT('Ctrl Pts',(87.1968449141549,-33.762788776063,107.895041631424));
#33522=CARTESIAN_POINT('Ctrl Pts',(88.1389902129737,-33.726372837867,107.842392123693));
#33523=CARTESIAN_POINT('Ctrl Pts',(88.882769382702,-34.0927745244804,107.789742615962));
#33524=CARTESIAN_POINT('Ctrl Pts',(89.6265485524304,-34.4591762110938,107.737093108232));
#33525=CARTESIAN_POINT('Ctrl Pts',(90.1719615930681,-35.2283955225168,107.684443600501));
#33526=CARTESIAN_POINT('Ctrl Pts',(90.2718152031542,-36.0513827690257,107.63179409277));
#33527=CARTESIAN_POINT('Ctrl Pts',(90.3716688132402,-36.8743700155345,107.579144585039));
#33528=CARTESIAN_POINT('Ctrl Pts',(90.0259629927746,-37.7511251971291,107.526495077308));
#33529=CARTESIAN_POINT('Ctrl Pts',(89.3912931505371,-38.2848771074855,107.473845569577));
#33530=CARTESIAN_POINT('Ctrl Pts',(88.7566233082995,-38.8186290178419,107.421196061847));
#33531=CARTESIAN_POINT('Ctrl Pts',(87.83298944429,-39.0093776569599,107.368546554116));
#33532=CARTESIAN_POINT('Ctrl Pts',(87.0393722154312,-38.7692235139292,107.315897046385));
#33533=CARTESIAN_POINT('Ctrl Pts',(86.2457549865724,-38.5290693708984,107.263247538654));
#33534=CARTESIAN_POINT('Ctrl Pts',(85.5821543928644,-37.8580124457189,107.210598030923));
#33535=CARTESIAN_POINT('Ctrl Pts',(85.3491891976178,-37.0637266223766,107.157948523192));
#33536=CARTESIAN_POINT('Ctrl Pts',(85.2822780465398,-36.8355956405425,107.142826782959));
#33537=CARTESIAN_POINT('Ctrl Pts',(85.2508911229913,-36.5972991882612,107.127705042726));
#33538=CARTESIAN_POINT('Ctrl Pts',(85.2529645136107,-36.3584982898635,107.112583302492));
#33539=CARTESIAN_POINT('Ctrl Pts',(85.2550452373729,-36.354668632511,107.387416697508));
#33540=CARTESIAN_POINT('Ctrl Pts',(85.2553232707789,-36.7850893471658,107.414523087103));
#33541=CARTESIAN_POINT('Ctrl Pts',(85.360231964155,-37.2156653176389,107.441629476698));
#33542=CARTESIAN_POINT('Ctrl Pts',(85.568953011386,-37.5880327420653,107.468735866293));
#33543=CARTESIAN_POINT('Ctrl Pts',(85.9743578090732,-38.3112925300341,107.521385374024));
#33544=CARTESIAN_POINT('Ctrl Pts',(86.771409166583,-38.8149524730431,107.574034881755));
#33545=CARTESIAN_POINT('Ctrl Pts',(87.5986589133747,-38.8708034657323,107.626684389485));
#33546=CARTESIAN_POINT('Ctrl Pts',(88.4259086601662,-38.9266544584215,107.679333897216));
#33547=CARTESIAN_POINT('Ctrl Pts',(89.2833567962396,-38.534696500791,107.731983404947));
#33548=CARTESIAN_POINT('Ctrl Pts',(89.7823491636544,-37.8725606603013,107.784632912678));
#33549=CARTESIAN_POINT('Ctrl Pts',(90.2813415310692,-37.2104248198116,107.837282420409));
#33550=CARTESIAN_POINT('Ctrl Pts',(90.4218781298253,-36.2781110964627,107.889931928139));
#33551=CARTESIAN_POINT('Ctrl Pts',(90.1402211568184,-35.4982975081166,107.94258143587));
#33552=CARTESIAN_POINT('Ctrl Pts',(89.8585641838115,-34.7184839197706,107.995230943601));
#33553=CARTESIAN_POINT('Ctrl Pts',(89.1547136390417,-34.0911704664274,108.047880451332));
#33554=CARTESIAN_POINT('Ctrl Pts',(88.3477629187951,-33.9007266610526,108.100529959063));
#33555=CARTESIAN_POINT('Ctrl Pts',(87.5408121985486,-33.7102828556778,108.153179466794));
#33556=CARTESIAN_POINT('Ctrl Pts',(86.6307613028254,-33.9567086982715,108.205828974524));
#33557=CARTESIAN_POINT('Ctrl Pts',(86.0301614241252,-34.5282973451729,108.258478482255));
#33558=CARTESIAN_POINT('Ctrl Pts',(85.5398733551047,-34.9949026574645,108.30145788734));
#33559=CARTESIAN_POINT('Ctrl Pts',(85.255802105395,-35.6781950561571,108.344437292424));
#33560=CARTESIAN_POINT('Ctrl Pts',(85.2497507212102,-36.3570215567107,108.387416697508));
#33561=CARTESIAN_POINT('Origin',(87.7685555885722,-36.3549260746835,114.));
#33562=CARTESIAN_POINT('',(85.2489005391845,-36.3530683166817,109.387416697508));
#33563=CARTESIAN_POINT('',(85.2539950043281,-36.3533981322694,109.112583302492));
#33564=CARTESIAN_POINT('',(85.2510555885723,-36.3549260746835,114.));
#33565=CARTESIAN_POINT('Ctrl Pts',(85.2539950043281,-36.3533981322694,109.112583302492));
#33566=CARTESIAN_POINT('Ctrl Pts',(85.2522387491172,-36.0401068363841,109.092832468829));
#33567=CARTESIAN_POINT('Ctrl Pts',(85.3065359379297,-35.7274023602209,109.073081635165));
#33568=CARTESIAN_POINT('Ctrl Pts',(85.4196755025654,-35.4376761985452,109.053330801502));
#33569=CARTESIAN_POINT('Ctrl Pts',(85.7212699812842,-34.6653574170195,109.000681293771));
#33570=CARTESIAN_POINT('Ctrl Pts',(86.4409912230722,-34.056319742401,108.94803178604));
#33571=CARTESIAN_POINT('Ctrl Pts',(87.2525647396359,-33.8866600926086,108.89538227831));
#33572=CARTESIAN_POINT('Ctrl Pts',(88.0641382561996,-33.7170004428162,108.842732770579));
#33573=CARTESIAN_POINT('Ctrl Pts',(88.9675640475391,-33.98671881785,108.790083262848));
#33574=CARTESIAN_POINT('Ctrl Pts',(89.5532873745519,-34.5735446538035,108.737433755117));
#33575=CARTESIAN_POINT('Ctrl Pts',(90.1390107015647,-35.160370489757,108.684784247386));
#33576=CARTESIAN_POINT('Ctrl Pts',(90.4070315642508,-36.0643037866303,108.632134739655));
#33577=CARTESIAN_POINT('Ctrl Pts',(90.2358475921449,-36.8755556888539,108.579485231925));
#33578=CARTESIAN_POINT('Ctrl Pts',(90.0646636200388,-37.6868075910774,108.526835724194));
#33579=CARTESIAN_POINT('Ctrl Pts',(89.4542748131408,-38.4053780986513,108.474186216463));
#33580=CARTESIAN_POINT('Ctrl Pts',(88.6813899854773,-38.7055233320582,108.421536708732));
#33581=CARTESIAN_POINT('Ctrl Pts',(87.9085051578137,-39.0056685654652,108.368887201001));
#33582=CARTESIAN_POINT('Ctrl Pts',(86.9731243093848,-38.8873885247051,108.316237693271));
#33583=CARTESIAN_POINT('Ctrl Pts',(86.2992915567292,-38.4042848873103,108.26358818554));
#33584=CARTESIAN_POINT('Ctrl Pts',(85.655081443511,-37.9424191680858,108.213253224524));
#33585=CARTESIAN_POINT('Ctrl Pts',(85.2499288480938,-37.1471011131107,108.162918263508));
#33586=CARTESIAN_POINT('Ctrl Pts',(85.2471487745657,-36.3542597485476,108.112583302492));
#33587=CARTESIAN_POINT('Ctrl Pts',(85.2497507212102,-36.3570215567107,108.387416697508));
#33588=CARTESIAN_POINT('Ctrl Pts',(85.2483891968683,-36.5097533575973,108.397086800155));
#33589=CARTESIAN_POINT('Ctrl Pts',(85.2611016612133,-36.6622590847112,108.406756902801));
#33590=CARTESIAN_POINT('Ctrl Pts',(85.2887059289636,-36.8120198732506,108.416427005448));
#33591=CARTESIAN_POINT('Ctrl Pts',(85.4389991741796,-37.6274023032177,108.469076513178));
#33592=CARTESIAN_POINT('Ctrl Pts',(86.0307345262888,-38.3614157119429,108.521726020909));
#33593=CARTESIAN_POINT('Ctrl Pts',(86.7956562152289,-38.6813078345256,108.57437552864));
#33594=CARTESIAN_POINT('Ctrl Pts',(87.560577904169,-39.0011999571083,108.627025036371));
#33595=CARTESIAN_POINT('Ctrl Pts',(88.4986859299399,-38.9069707935486,108.679674544102));
#33596=CARTESIAN_POINT('Ctrl Pts',(89.1847040366692,-38.4413369476427,108.732324051833));
#33597=CARTESIAN_POINT('Ctrl Pts',(89.8707221433986,-37.9757031017368,108.784973559563));
#33598=CARTESIAN_POINT('Ctrl Pts',(90.3046503310864,-37.1386645734846,108.837623067294));
#33599=CARTESIAN_POINT('Ctrl Pts',(90.2897734888853,-36.3096804178693,108.890272575025));
#33600=CARTESIAN_POINT('Ctrl Pts',(90.2748966466842,-35.480696262254,108.942922082756));
#33601=CARTESIAN_POINT('Ctrl Pts',(89.8112147745942,-34.6597664792756,108.995571590487));
#33602=CARTESIAN_POINT('Ctrl Pts',(89.1089311759761,-34.2190469239351,109.048221098218));
#33603=CARTESIAN_POINT('Ctrl Pts',(88.406647577358,-33.7783273685947,109.100870605948));
#33604=CARTESIAN_POINT('Ctrl Pts',(87.4657622522118,-33.7178180408923,109.153520113679));
#33605=CARTESIAN_POINT('Ctrl Pts',(86.71281116839,-34.0649500111222,109.20616962141));
#33606=CARTESIAN_POINT('Ctrl Pts',(85.9598600845683,-34.4120819813521,109.258819129141));
#33607=CARTESIAN_POINT('Ctrl Pts',(85.3948432420709,-35.1668552495144,109.311468636872));
#33608=CARTESIAN_POINT('Ctrl Pts',(85.2739024763654,-35.9871047900117,109.364118144602));
#33609=CARTESIAN_POINT('Ctrl Pts',(85.2560628361378,-36.1080975472008,109.371884328904));
#33610=CARTESIAN_POINT('Ctrl Pts',(85.2478855763512,-36.2305149626551,109.379650513206));
#33611=CARTESIAN_POINT('Ctrl Pts',(85.2489005391845,-36.3530683166817,109.387416697508));
#33612=CARTESIAN_POINT('Origin',(87.7685555885722,-36.3549260746835,114.));
#33613=CARTESIAN_POINT('',(85.2549714308827,-36.3546406872631,110.387416697508));
#33614=CARTESIAN_POINT('',(85.2524196711837,-36.3570497194806,110.112583302492));
#33615=CARTESIAN_POINT('',(85.2510555885723,-36.3549260746835,114.));
#33616=CARTESIAN_POINT('Ctrl Pts',(85.2524196711837,-36.3570497194806,110.112583302492));
#33617=CARTESIAN_POINT('Ctrl Pts',(85.2572191354379,-35.768112702753,110.07539618188));
#33618=CARTESIAN_POINT('Ctrl Pts',(85.4637776199823,-35.1761421078341,110.038209061269));
#33619=CARTESIAN_POINT('Ctrl Pts',(85.8414731263454,-34.7285995245313,110.001021940657));
#33620=CARTESIAN_POINT('Ctrl Pts',(86.3762142451804,-34.094968947281,109.948372432926));
#33621=CARTESIAN_POINT('Ctrl Pts',(87.2539975215157,-33.7508426291429,109.895722925195));
#33622=CARTESIAN_POINT('Ctrl Pts',(88.07689325785,-33.8522249894879,109.843073417464));
#33623=CARTESIAN_POINT('Ctrl Pts',(88.8997889941843,-33.9536073498329,109.790423909734));
#33624=CARTESIAN_POINT('Ctrl Pts',(89.6677971905177,-34.500498388661,109.737774402003));
#33625=CARTESIAN_POINT('Ctrl Pts',(90.0327530047769,-35.2449733985566,109.685124894272));
#33626=CARTESIAN_POINT('Ctrl Pts',(90.3977088190361,-35.9894484084521,109.632475386541));
#33627=CARTESIAN_POINT('Ctrl Pts',(90.3596122512212,-36.9315073894151,109.57982587881));
#33628=CARTESIAN_POINT('Ctrl Pts',(89.9357338117621,-37.6440821693962,109.52717637108));
#33629=CARTESIAN_POINT('Ctrl Pts',(89.511855372303,-38.3566569493773,109.474526863349));
#33630=CARTESIAN_POINT('Ctrl Pts',(88.7021950611999,-38.8397475283767,109.421877355618));
#33631=CARTESIAN_POINT('Ctrl Pts',(87.8738000460567,-38.8743522594697,109.369227847887));
#33632=CARTESIAN_POINT('Ctrl Pts',(87.0454050309135,-38.9089569905627,109.316578340156));
#33633=CARTESIAN_POINT('Ctrl Pts',(86.1982753117304,-38.4950758737495,109.263928832425));
#33634=CARTESIAN_POINT('Ctrl Pts',(85.7164443099636,-37.8203353711265,109.211279324695));
#33635=CARTESIAN_POINT('Ctrl Pts',(85.4153664506265,-37.3987157049098,109.178380650627));
#33636=CARTESIAN_POINT('Ctrl Pts',(85.2569203728846,-36.8752428506858,109.14548197656));
#33637=CARTESIAN_POINT('Ctrl Pts',(85.2539950043281,-36.3533981322694,109.112583302492));
#33638=CARTESIAN_POINT('Ctrl Pts',(85.2489005391845,-36.3530683166817,109.387416697508));
#33639=CARTESIAN_POINT('Ctrl Pts',(85.254766341919,-37.0613443003947,109.432300020937));
#33640=CARTESIAN_POINT('Ctrl Pts',(85.567658150359,-37.7741607177567,109.477183344366));
#33641=CARTESIAN_POINT('Ctrl Pts',(86.0968199097674,-38.2427519208318,109.522066667795));
#33642=CARTESIAN_POINT('Ctrl Pts',(86.7175427977887,-38.7924236983225,109.574716175526));
#33643=CARTESIAN_POINT('Ctrl Pts',(87.635853262745,-39.0060414404716,109.627365683257));
#33644=CARTESIAN_POINT('Ctrl Pts',(88.4354492298588,-38.7867647823512,109.680015190987));
#33645=CARTESIAN_POINT('Ctrl Pts',(89.2350451969726,-38.5674881242308,109.732664698718));
#33646=CARTESIAN_POINT('Ctrl Pts',(89.915926666244,-37.9153170658409,109.785314206449));
#33647=CARTESIAN_POINT('Ctrl Pts',(90.169426372785,-37.1259034439069,109.83796371418));
#33648=CARTESIAN_POINT('Ctrl Pts',(90.4229260793259,-36.3364898219729,109.890613221911));
#33649=CARTESIAN_POINT('Ctrl Pts',(90.2490440231364,-35.4098336364947,109.943262729642));
#33650=CARTESIAN_POINT('Ctrl Pts',(89.7266069925469,-34.7660203753152,109.995912237372));
#33651=CARTESIAN_POINT('Ctrl Pts',(89.2041699619573,-34.1222071141356,110.048561745103));
#33652=CARTESIAN_POINT('Ctrl Pts',(88.3331779569678,-33.7612367772546,110.101211252834));
#33653=CARTESIAN_POINT('Ctrl Pts',(87.5084819568861,-33.8467497788348,110.153860760565));
#33654=CARTESIAN_POINT('Ctrl Pts',(86.6837859568044,-33.9322627804151,110.206510268296));
#33655=CARTESIAN_POINT('Ctrl Pts',(85.9053859616305,-34.4642591204566,110.259159776027));
#33656=CARTESIAN_POINT('Ctrl Pts',(85.5261577727488,-35.201566347613,110.311809283757));
#33657=CARTESIAN_POINT('Ctrl Pts',(85.3446273474991,-35.5545034403965,110.337011755008));
#33658=CARTESIAN_POINT('Ctrl Pts',(85.2545624585998,-35.9544851142665,110.362214226258));
#33659=CARTESIAN_POINT('Ctrl Pts',(85.2549714308827,-36.3546406872631,110.387416697508));
#33660=CARTESIAN_POINT('Origin',(87.7685555885722,-36.3549260746835,114.));
#33661=CARTESIAN_POINT('',(85.2499087442488,-36.3570522860866,111.387416697508));
#33662=CARTESIAN_POINT('',(85.2470899772098,-36.354365150253,111.112583302492));
#33663=CARTESIAN_POINT('',(85.2510555885723,-36.3549260746835,114.));
#33664=CARTESIAN_POINT('Ctrl Pts',(85.2470899772098,-36.354365150253,111.112583302492));
#33665=CARTESIAN_POINT('Ctrl Pts',(85.2469952533804,-36.323275203713,111.110609402663));
#33666=CARTESIAN_POINT('Ctrl Pts',(85.2475210549401,-36.2921885346853,111.108635502833));
#33667=CARTESIAN_POINT('Ctrl Pts',(85.2486773612175,-36.2611253357633,111.106661603004));
#33668=CARTESIAN_POINT('Ctrl Pts',(85.279519329685,-35.4325817047621,111.054012095273));
#33669=CARTESIAN_POINT('Ctrl Pts',(85.7589277104219,-34.6207356508032,111.001362587543));
#33670=CARTESIAN_POINT('Ctrl Pts',(86.4695700042782,-34.1936252369474,110.948713079812));
#33671=CARTESIAN_POINT('Ctrl Pts',(87.1802122981346,-33.7665148230915,110.896063572081));
#33672=CARTESIAN_POINT('Ctrl Pts',(88.1220885051104,-33.7241400493387,110.84341406435));
#33673=CARTESIAN_POINT('Ctrl Pts',(88.8682133697417,-34.0857108748008,110.790764556619));
#33674=CARTESIAN_POINT('Ctrl Pts',(89.614338234373,-34.4472817002629,110.738115048888));
#33675=CARTESIAN_POINT('Ctrl Pts',(90.1647117566598,-35.2127981249399,110.685465541158));
#33676=CARTESIAN_POINT('Ctrl Pts',(90.2698304696313,-36.0352249191472,110.632816033427));
#33677=CARTESIAN_POINT('Ctrl Pts',(90.3749491826028,-36.8576517133544,110.580166525696));
#33678=CARTESIAN_POINT('Ctrl Pts',(90.0348130862591,-37.7369888770919,110.527517017965));
#33679=CARTESIAN_POINT('Ctrl Pts',(89.4036177076337,-38.2746022783177,110.474867510234));
#33680=CARTESIAN_POINT('Ctrl Pts',(88.7724223290083,-38.8122156795435,110.422218002503));
#33681=CARTESIAN_POINT('Ctrl Pts',(87.8501676681012,-39.0081053182576,110.369568494773));
#33682=CARTESIAN_POINT('Ctrl Pts',(87.0549438505888,-38.7734676072038,110.316918987042));
#33683=CARTESIAN_POINT('Ctrl Pts',(86.2597200330764,-38.5388298961499,110.264269479311));
#33684=CARTESIAN_POINT('Ctrl Pts',(85.5915270589586,-37.8736648353281,110.21161997158));
#33685=CARTESIAN_POINT('Ctrl Pts',(85.3532800525671,-37.079514886736,110.158970463849));
#33686=CARTESIAN_POINT('Ctrl Pts',(85.2833104060962,-36.8462847110897,110.14350807673));
#33687=CARTESIAN_POINT('Ctrl Pts',(85.2504240562223,-36.6019294518078,110.128045689611));
#33688=CARTESIAN_POINT('Ctrl Pts',(85.2524196711837,-36.3570497194806,110.112583302492));
#33689=CARTESIAN_POINT('Ctrl Pts',(85.2549714308827,-36.3546406872631,110.387416697508));
#33690=CARTESIAN_POINT('Ctrl Pts',(85.2554168267748,-36.7904346417883,110.414863733989));
#33691=CARTESIAN_POINT('Ctrl Pts',(85.3631691571782,-37.2264348501634,110.442310770469));
#33692=CARTESIAN_POINT('Ctrl Pts',(85.5769474890366,-37.60209910281,110.46975780695));
#33693=CARTESIAN_POINT('Ctrl Pts',(85.9870217767954,-38.3227065165792,110.522407314681));
#33694=CARTESIAN_POINT('Ctrl Pts',(86.7872267349022,-38.8213032298464,110.575056822411));
#33695=CARTESIAN_POINT('Ctrl Pts',(87.6148016142974,-38.8718580045868,110.627706330142));
#33696=CARTESIAN_POINT('Ctrl Pts',(88.4423764936926,-38.9224127793273,110.680355837873));
#33697=CARTESIAN_POINT('Ctrl Pts',(89.2973212943763,-38.5249256155411,110.733005345604));
#33698=CARTESIAN_POINT('Ctrl Pts',(89.79205979188,-37.8595912744819,110.785654853335));
#33699=CARTESIAN_POINT('Ctrl Pts',(90.2867982893837,-37.1942569334227,110.838304361066));
#33700=CARTESIAN_POINT('Ctrl Pts',(90.4213304837074,-36.2610754150906,110.890953868796));
#33701=CARTESIAN_POINT('Ctrl Pts',(90.1346682503914,-35.4830903700737,110.943603376527));
#33702=CARTESIAN_POINT('Ctrl Pts',(89.8480060170754,-34.7051053250569,110.996252884258));
#33703=CARTESIAN_POINT('Ctrl Pts',(89.1401493561197,-34.0823167533554,111.048902391989));
#33704=CARTESIAN_POINT('Ctrl Pts',(88.3319943205098,-33.8970563833361,111.10155189972));
#33705=CARTESIAN_POINT('Ctrl Pts',(87.5238392849,-33.7117960133168,111.15420140745));
#33706=CARTESIAN_POINT('Ctrl Pts',(86.615385874636,-33.9640638449797,111.206850915181));
#33707=CARTESIAN_POINT('Ctrl Pts',(86.0184676285876,-34.5394980930228,111.259500422912));
#33708=CARTESIAN_POINT('Ctrl Pts',(85.53504710189,-35.0055195777242,111.302139181111));
#33709=CARTESIAN_POINT('Ctrl Pts',(85.2559544134533,-35.6834975374635,111.344777939309));
#33710=CARTESIAN_POINT('Ctrl Pts',(85.2499087442488,-36.3570522860866,111.387416697508));
#33711=CARTESIAN_POINT('Origin',(87.7685555885722,-36.3549260746835,114.));
#33712=CARTESIAN_POINT('',(85.2487565565375,-36.3531221774957,112.387416697508));
#33713=CARTESIAN_POINT('',(85.2538920866812,-36.3533353395906,112.112583302492));
#33714=CARTESIAN_POINT('',(85.2510555885723,-36.3549260746835,114.));
#33715=CARTESIAN_POINT('Ctrl Pts',(85.2538920866812,-36.3533353395906,112.112583302492));
#33716=CARTESIAN_POINT('Ctrl Pts',(85.2520903341024,-36.0454791376291,112.093173115714));
#33717=CARTESIAN_POINT('Ctrl Pts',(85.3044765460178,-35.7382147173017,112.073762928937));
#33718=CARTESIAN_POINT('Ctrl Pts',(85.4138342400317,-35.4527774006629,112.054352742159));
#33719=CARTESIAN_POINT('Ctrl Pts',(85.7104634699489,-34.6785378541209,112.001703234428));
#33720=CARTESIAN_POINT('Ctrl Pts',(86.4262593467811,-34.0648908273442,111.949053726697));
#33721=CARTESIAN_POINT('Ctrl Pts',(87.2367266947401,-33.8900238683076,111.896404218967));
#33722=CARTESIAN_POINT('Ctrl Pts',(88.047194042699,-33.7151569092711,111.843754711236));
#33723=CARTESIAN_POINT('Ctrl Pts',(88.9523328617846,-33.9790700179748,111.791105203505));
#33724=CARTESIAN_POINT('Ctrl Pts',(89.5418122326413,-34.5621221998627,111.738455695774));
#33725=CARTESIAN_POINT('Ctrl Pts',(90.1312916034979,-35.1451743817506,111.685806188043));
#33726=CARTESIAN_POINT('Ctrl Pts',(90.4051115261256,-36.0473656368227,111.633156680312));
#33727=CARTESIAN_POINT('Ctrl Pts',(90.2391399025284,-36.8597012790504,111.580507172582));
#33728=CARTESIAN_POINT('Ctrl Pts',(90.0731682789312,-37.672036921278,111.527857664851));
#33729=CARTESIAN_POINT('Ctrl Pts',(89.4674051091091,-38.3945169506613,111.47520815712));
#33730=CARTESIAN_POINT('Ctrl Pts',(88.696463914376,-38.6996160324873,111.422558649389));
#33731=CARTESIAN_POINT('Ctrl Pts',(87.9255227196427,-39.0047151143134,111.369909141658));
#33732=CARTESIAN_POINT('Ctrl Pts',(86.9894034999983,-38.8924332485823,111.317259633928));
#33733=CARTESIAN_POINT('Ctrl Pts',(86.3124816682752,-38.4136717116951,111.264610126197));
#33734=CARTESIAN_POINT('Ctrl Pts',(85.6609385332515,-37.9528595794017,111.213934518295));
#33735=CARTESIAN_POINT('Ctrl Pts',(85.2495218066094,-37.152532269562,111.163258910394));
#33736=CARTESIAN_POINT('Ctrl Pts',(85.2470899772098,-36.354365150253,111.112583302492));
#33737=CARTESIAN_POINT('Ctrl Pts',(85.2499087442488,-36.3570522860866,111.387416697508));
#33738=CARTESIAN_POINT('Ctrl Pts',(85.2484893389303,-36.5151898156383,111.39742744704));
#33739=CARTESIAN_POINT('Ctrl Pts',(85.2621208012014,-36.6730835294362,111.407438196572));
#33740=CARTESIAN_POINT('Ctrl Pts',(85.2916924634678,-36.8279331399315,111.417448946105));
#33741=CARTESIAN_POINT('Ctrl Pts',(85.4472186262289,-37.6423332743741,111.470098453835));
#33742=CARTESIAN_POINT('Ctrl Pts',(86.0436540335839,-38.372532878836,111.522747961566));
#33743=CARTESIAN_POINT('Ctrl Pts',(86.8106137634916,-38.6875070666412,111.575397469297));
#33744=CARTESIAN_POINT('Ctrl Pts',(87.5775734933993,-39.0024812544465,111.628046977028));
#33745=CARTESIAN_POINT('Ctrl Pts',(88.5150575458597,-38.9022300255951,111.680696484759));
#33746=CARTESIAN_POINT('Ctrl Pts',(89.1980717818333,-38.432200750186,111.73334599249));
#33747=CARTESIAN_POINT('Ctrl Pts',(89.8810860178069,-37.9621714747769,111.78599550022));
#33748=CARTESIAN_POINT('Ctrl Pts',(90.3096304372937,-37.1223641528102,111.838645007951));
#33749=CARTESIAN_POINT('Ctrl Pts',(90.2894309445145,-36.2934926629065,111.891294515682));
#33750=CARTESIAN_POINT('Ctrl Pts',(90.2692314517352,-35.4646211730027,111.943944023413));
#33751=CARTESIAN_POINT('Ctrl Pts',(89.80028804669,-34.6466855151619,111.996593531144));
#33752=CARTESIAN_POINT('Ctrl Pts',(89.0951890909213,-34.2104843816722,112.049243038874));
#33753=CARTESIAN_POINT('Ctrl Pts',(88.3900901351525,-33.7742832481825,112.101892546605));
#33754=CARTESIAN_POINT('Ctrl Pts',(87.4488356286603,-33.7198166390438,112.154542054336));
#33755=CARTESIAN_POINT('Ctrl Pts',(86.6981289884821,-34.0717761632455,112.207191562067));
#33756=CARTESIAN_POINT('Ctrl Pts',(85.9474223483039,-34.4237356874472,112.259841069798));
#33757=CARTESIAN_POINT('Ctrl Pts',(85.3872635744398,-35.1821213449894,112.312490577529));
#33758=CARTESIAN_POINT('Ctrl Pts',(85.2715921287914,-36.0031305306539,112.365140085259));
#33759=CARTESIAN_POINT('Ctrl Pts',(85.2552781557902,-36.1189233403108,112.372565622676));
#33760=CARTESIAN_POINT('Ctrl Pts',(85.2478056946932,-36.2359618247805,112.379991160092));
#33761=CARTESIAN_POINT('Ctrl Pts',(85.2487565565375,-36.3531221774957,112.387416697508));
#33762=CARTESIAN_POINT('Origin',(87.7685555885722,-36.3549260746835,114.));
#33763=CARTESIAN_POINT('',(85.254950234978,-36.3545547484977,113.387416697508));
#33764=CARTESIAN_POINT('',(85.2525639081684,-36.3570196911117,113.112583302492));
#33765=CARTESIAN_POINT('',(85.2510555885723,-36.3549260746835,114.));
#33766=CARTESIAN_POINT('Ctrl Pts',(85.2525639081684,-36.3570196911117,113.112583302492));
#33767=CARTESIAN_POINT('Ctrl Pts',(85.2572319946921,-35.773392729585,113.075736828766));
#33768=CARTESIAN_POINT('Ctrl Pts',(85.4596895883703,-35.1868436112621,113.03889035504));
#33769=CARTESIAN_POINT('Ctrl Pts',(85.8310702123153,-34.7410068461903,113.002043881314));
#33770=CARTESIAN_POINT('Ctrl Pts',(86.3617317669821,-34.10395575729,112.949394373583));
#33771=CARTESIAN_POINT('Ctrl Pts',(87.2372873147814,-33.7542002805938,112.896744865852));
#33772=CARTESIAN_POINT('Ctrl Pts',(88.0608170625274,-33.850296742796,112.844095358121));
#33773=CARTESIAN_POINT('Ctrl Pts',(88.8843468102735,-33.9463932049982,112.791445850391));
#33774=CARTESIAN_POINT('Ctrl Pts',(89.6558507579663,-34.4883416060987,112.73879634266));
#33775=CARTESIAN_POINT('Ctrl Pts',(90.0255793230353,-35.2304578797664,112.686146834929));
#33776=CARTESIAN_POINT('Ctrl Pts',(90.3953078881044,-35.9725741534341,112.633497327198));
#33777=CARTESIAN_POINT('Ctrl Pts',(90.3632610705496,-36.914858299669,112.580847819467));
#33778=CARTESIAN_POINT('Ctrl Pts',(89.9439668077795,-37.6301401299139,112.528198311736));
#33779=CARTESIAN_POINT('Ctrl Pts',(89.5246725450094,-38.3454219601589,112.475548804006));
#33780=CARTESIAN_POINT('Ctrl Pts',(88.718130837024,-38.8337014744139,112.422899296275));
#33781=CARTESIAN_POINT('Ctrl Pts',(87.8899751022099,-38.8736245800664,112.370249788544));
#33782=CARTESIAN_POINT('Ctrl Pts',(87.0618193673958,-38.9135476857189,112.317600280813));
#33783=CARTESIAN_POINT('Ctrl Pts',(86.212049605753,-38.5051143827689,112.264950773082));
#33784=CARTESIAN_POINT('Ctrl Pts',(85.7258960164326,-37.8334816981404,112.212301265351));
#33785=CARTESIAN_POINT('Ctrl Pts',(85.4189716806808,-37.4094584673606,112.179061944398));
#33786=CARTESIAN_POINT('Ctrl Pts',(85.2569775300586,-36.880529189996,112.145822623445));
#33787=CARTESIAN_POINT('Ctrl Pts',(85.2538920866812,-36.3533353395906,112.112583302492));
#33788=CARTESIAN_POINT('Ctrl Pts',(85.2487565565375,-36.3531221774957,112.387416697508));
#33789=CARTESIAN_POINT('Ctrl Pts',(85.2545476185725,-37.0666673414699,112.432640667823));
#33790=CARTESIAN_POINT('Ctrl Pts',(85.572777540667,-37.7847328563774,112.477864638137));
#33791=CARTESIAN_POINT('Ctrl Pts',(86.1089760963731,-38.2534472184562,112.523088608452));
#33792=CARTESIAN_POINT('Ctrl Pts',(86.7332156270358,-38.7991220068071,112.575738116183));
#33793=CARTESIAN_POINT('Ctrl Pts',(87.652878805794,-39.0068388697222,112.628387623914));
#33794=CARTESIAN_POINT('Ctrl Pts',(88.4510503157032,-38.7824325261102,112.681037131644));
#33795=CARTESIAN_POINT('Ctrl Pts',(89.2492218256123,-38.5580261824983,112.733686639375));
#33796=CARTESIAN_POINT('Ctrl Pts',(89.9259016666724,-37.9014966323593,112.786336147106));
#33797=CARTESIAN_POINT('Ctrl Pts',(90.1743273230824,-37.110471563527,112.838985654837));
#33798=CARTESIAN_POINT('Ctrl Pts',(90.4227529794924,-36.3194464946947,112.891635162568));
#33799=CARTESIAN_POINT('Ctrl Pts',(90.2429244512524,-35.3939259071691,112.944284670298));
#33800=CARTESIAN_POINT('Ctrl Pts',(89.7163642670212,-34.7534804850867,112.996934178029));
#33801=CARTESIAN_POINT('Ctrl Pts',(89.1898040827899,-34.1130350630043,113.04958368576));
#33802=CARTESIAN_POINT('Ctrl Pts',(88.3165122425674,-33.7576648063653,113.102233193491));
#33803=CARTESIAN_POINT('Ctrl Pts',(87.4923823221333,-33.8484714169679,113.154882701222));
#33804=CARTESIAN_POINT('Ctrl Pts',(86.6682524016991,-33.9392780275705,113.207532208953));
#33805=CARTESIAN_POINT('Ctrl Pts',(85.8932844010533,-34.4762615054149,113.260181716683));
#33806=CARTESIAN_POINT('Ctrl Pts',(85.5187982784954,-35.2159885566273,113.312831224414));
#33807=CARTESIAN_POINT('Ctrl Pts',(85.3419607617305,-35.5652978819683,113.337693048779));
#33808=CARTESIAN_POINT('Ctrl Pts',(85.2544250479382,-35.9598161609063,113.362554873143));
#33809=CARTESIAN_POINT('Ctrl Pts',(85.254950234978,-36.3545547484977,113.387416697508));
#33810=CARTESIAN_POINT('Origin',(87.7685555885722,-36.3549260746835,114.));
#33811=CARTESIAN_POINT('',(85.2500677995525,-36.3570794361965,114.387416697508));
#33812=CARTESIAN_POINT('',(85.2470414567978,-36.3544600798358,114.112583302492));
#33813=CARTESIAN_POINT('',(85.2510555885723,-36.3549260746835,114.));
#33814=CARTESIAN_POINT('Ctrl Pts',(85.2470414567978,-36.3544600798358,114.112583302492));
#33815=CARTESIAN_POINT('Ctrl Pts',(85.2469753692349,-36.3287368261812,114.110950049548));
#33816=CARTESIAN_POINT('Ctrl Pts',(85.2473353127159,-36.3030154666756,114.109316796605));
#33817=CARTESIAN_POINT('Ctrl Pts',(85.2481270136682,-36.2773074034965,114.107683543661));
#33818=CARTESIAN_POINT('Ctrl Pts',(85.2736482690049,-35.4485828165579,114.05503403593));
#33819=CARTESIAN_POINT('Ctrl Pts',(85.7478339046031,-34.6336752182663,114.002384528199));
#33820=CARTESIAN_POINT('Ctrl Pts',(86.4557190734163,-34.2020105761599,113.949735020469));
#33821=CARTESIAN_POINT('Ctrl Pts',(87.1636042422294,-33.7703459340536,113.897085512738));
#33822=CARTESIAN_POINT('Ctrl Pts',(88.1051889442577,-33.7219242481326,113.844436005007));
#33823=CARTESIAN_POINT('Ctrl Pts',(88.8536200733386,-34.0786967533697,113.791786497276));
#33824=CARTESIAN_POINT('Ctrl Pts',(89.6020512024195,-34.4354692586068,113.739136989545));
#33825=CARTESIAN_POINT('Ctrl Pts',(90.157328758553,-35.197435955002,113.686487481814));
#33826=CARTESIAN_POINT('Ctrl Pts',(90.2677261056678,-36.0191708278293,113.633837974084));
#33827=CARTESIAN_POINT('Ctrl Pts',(90.3781234527826,-36.8409057006566,113.581188466353));
#33828=CARTESIAN_POINT('Ctrl Pts',(90.0436405908786,-37.7224087499159,113.528538958622));
#33829=CARTESIAN_POINT('Ctrl Pts',(89.4159102389819,-38.2640639730773,113.475889450891));
#33830=CARTESIAN_POINT('Ctrl Pts',(88.7881798870852,-38.8057191962387,113.42323994316));
#33831=CARTESIAN_POINT('Ctrl Pts',(87.8672020451956,-39.0075265933022,113.37059043543));
#33832=CARTESIAN_POINT('Ctrl Pts',(87.0704880127964,-38.7779998496562,113.317940927699));
#33833=CARTESIAN_POINT('Ctrl Pts',(86.2737739803972,-38.5484731060102,113.265291419968));
#33834=CARTESIAN_POINT('Ctrl Pts',(85.6013237574885,-37.8876122216548,113.212641912237));
#33835=CARTESIAN_POINT('Ctrl Pts',(85.3579824268013,-37.0950084289249,113.159992404506));
#33836=CARTESIAN_POINT('Ctrl Pts',(85.2849422125742,-36.8571041211991,113.144189370502));
#33837=CARTESIAN_POINT('Ctrl Pts',(85.2505618188879,-36.6073306649015,113.128386336497));
#33838=CARTESIAN_POINT('Ctrl Pts',(85.2525639081684,-36.3570196911117,113.112583302492));
#33839=CARTESIAN_POINT('Ctrl Pts',(85.254950234978,-36.3545547484977,113.387416697508));
#33840=CARTESIAN_POINT('Ctrl Pts',(85.2555372285531,-36.7957480705789,113.415204380874));
#33841=CARTESIAN_POINT('Ctrl Pts',(85.3661316014678,-37.237216606488,113.44299206424));
#33842=CARTESIAN_POINT('Ctrl Pts',(85.5850007646286,-37.6161457046895,113.470779747607));
#33843=CARTESIAN_POINT('Ctrl Pts',(85.9996936177896,-38.3341051769587,113.523429255337));
#33844=CARTESIAN_POINT('Ctrl Pts',(86.8030835685816,-38.8275534969166,113.576078763068));
#33845=CARTESIAN_POINT('Ctrl Pts',(87.6309659998135,-38.8727933724864,113.628728270799));
#33846=CARTESIAN_POINT('Ctrl Pts',(88.4588484310453,-38.9180332480561,113.68137777853));
#33847=CARTESIAN_POINT('Ctrl Pts',(89.311223342717,-38.5150646792378,113.734027286261));
#33848=CARTESIAN_POINT('Ctrl Pts',(89.8016795305277,-37.8465673388377,113.786676793992));
#33849=CARTESIAN_POINT('Ctrl Pts',(90.2921357183384,-37.1780699984375,113.839326301722));
#33850=CARTESIAN_POINT('Ctrl Pts',(90.4206731822881,-36.2440438864555,113.891975809453));
#33851=CARTESIAN_POINT('Ctrl Pts',(90.1290214177404,-35.4679155371987,113.944625317184));
#33852=CARTESIAN_POINT('Ctrl Pts',(89.8373696531927,-34.6917871879419,113.997274824915));
#33853=CARTESIAN_POINT('Ctrl Pts',(89.1255286601476,-34.0735566014102,114.049924332646));
#33854=CARTESIAN_POINT('Ctrl Pts',(88.3162007279694,-33.8934892126912,114.102573840377));
#33855=CARTESIAN_POINT('Ctrl Pts',(87.5068727957913,-33.7134218239722,114.155223348107));
#33856=CARTESIAN_POINT('Ctrl Pts',(86.60005792448,-33.9715176330658,114.207872855838));
#33857=CARTESIAN_POINT('Ctrl Pts',(86.0068468461809,-34.550772829734,114.260522363569));
#33858=CARTESIAN_POINT('Ctrl Pts',(85.5302667354934,-35.0161409185027,114.302820474882));
#33859=CARTESIAN_POINT('Ctrl Pts',(85.2560978662429,-35.6887969029749,114.345118586195));
#33860=CARTESIAN_POINT('Ctrl Pts',(85.2500677995525,-36.3570794361965,114.387416697508));
#33861=CARTESIAN_POINT('Origin',(87.7685555885722,-36.3549260746835,114.));
#33862=CARTESIAN_POINT('',(85.2486157516665,-36.3531793386365,115.387416697508));
#33863=CARTESIAN_POINT('',(85.2537848649131,-36.3532747669305,115.112583302492));
#33864=CARTESIAN_POINT('',(85.2510555885723,-36.3549260746835,114.));
#33865=CARTESIAN_POINT('Ctrl Pts',(85.2537848649131,-36.3532747669305,115.112583302492));
#33866=CARTESIAN_POINT('Ctrl Pts',(85.2519423002258,-36.0508538406101,115.0935137626));
#33867=CARTESIAN_POINT('Ctrl Pts',(85.3024544519066,-35.7490276611798,115.074444222708));
#33868=CARTESIAN_POINT('Ctrl Pts',(85.4080900870048,-35.4679156603028,115.055374682816));
#33869=CARTESIAN_POINT('Ctrl Pts',(85.6997418110755,-34.6917874187621,115.002725175085));
#33870=CARTESIAN_POINT('Ctrl Pts',(86.4115827053271,-34.0735569180327,114.950075667354));
#33871=CARTESIAN_POINT('Ctrl Pts',(87.2209105251817,-33.8934895543048,114.897426159623));
#33872=CARTESIAN_POINT('Ctrl Pts',(88.0302383450363,-33.713422190577,114.844776651893));
#33873=CARTESIAN_POINT('Ctrl Pts',(88.9370530904939,-33.9715179638508,114.792127144162));
#33874=CARTESIAN_POINT('Ctrl Pts',(89.5302640864631,-34.5507730801265,114.739477636431));
#33875=CARTESIAN_POINT('Ctrl Pts',(90.1234750824323,-35.1300281964022,114.6868281287));
#33876=CARTESIAN_POINT('Ctrl Pts',(90.4030823289133,-36.0304426556799,114.634178620969));
#33877=CARTESIAN_POINT('Ctrl Pts',(90.2423301326488,-36.84382725528,114.581529113239));
#33878=CARTESIAN_POINT('Ctrl Pts',(90.0815779363843,-37.6572118548801,114.528879605508));
#33879=CARTESIAN_POINT('Ctrl Pts',(89.4804662973744,-38.3835665948026,114.476230097777));
#33880=CARTESIAN_POINT('Ctrl Pts',(88.7115000361721,-38.693609599244,114.423580590046));
#33881=CARTESIAN_POINT('Ctrl Pts',(87.9425337749698,-39.0036526036854,114.370931082315));
#33882=CARTESIAN_POINT('Ctrl Pts',(87.0057128915752,-38.8973838726457,114.318281574584));
#33883=CARTESIAN_POINT('Ctrl Pts',(86.3257308874156,-38.4229787193331,114.265632066854));
#33884=CARTESIAN_POINT('Ctrl Pts',(85.6668427672787,-37.9632902014939,114.214615812066));
#33885=CARTESIAN_POINT('Ctrl Pts',(85.2491057665298,-37.1579510929692,114.163599557279));
#33886=CARTESIAN_POINT('Ctrl Pts',(85.2470414567978,-36.3544600798358,114.112583302492));
#33887=CARTESIAN_POINT('Ctrl Pts',(85.2500677995525,-36.3570794361965,114.387416697508));
#33888=CARTESIAN_POINT('Ctrl Pts',(85.2485920927467,-36.5206247389477,114.397768093926));
#33889=CARTESIAN_POINT('Ctrl Pts',(85.2631752786074,-36.6839081147284,114.408119490344));
#33890=CARTESIAN_POINT('Ctrl Pts',(85.2947807011693,-36.8438273231319,114.418470886761));
#33891=CARTESIAN_POINT('Ctrl Pts',(85.4555329197437,-37.6572120356188,114.471120394492));
#33892=CARTESIAN_POINT('Ctrl Pts',(86.0566446421795,-38.3835668763496,114.523769902223));
#33893=CARTESIAN_POINT('Ctrl Pts',(86.8256110101037,-38.693609923821,114.576419409954));
#33894=CARTESIAN_POINT('Ctrl Pts',(87.5945773780279,-39.0036529712925,114.629068917685));
#33895=CARTESIAN_POINT('Ctrl Pts',(88.5313983914405,-38.8973842255045,114.681718425416));
#33896=CARTESIAN_POINT('Ctrl Pts',(89.2113804899725,-38.4229790063511,114.734367933146));
#33897=CARTESIAN_POINT('Ctrl Pts',(89.8913625885046,-37.9485737871978,114.787017440877));
#33898=CARTESIAN_POINT('Ctrl Pts',(90.314505772156,-37.1060320946792,114.839666948608));
#33899=CARTESIAN_POINT('Ctrl Pts',(90.2889845132775,-36.2773073927249,114.892316456339));
#33900=CARTESIAN_POINT('Ctrl Pts',(90.263463254399,-35.4485826907707,114.94496596407));
#33901=CARTESIAN_POINT('Ctrl Pts',(89.7892775529907,-34.6336749793808,114.997615471801));
#33902=CARTESIAN_POINT('Ctrl Pts',(89.0813922859328,-34.2020102773651,115.050264979531));
#33903=CARTESIAN_POINT('Ctrl Pts',(88.373507018875,-33.7703455753493,115.102914487262));
#33904=CARTESIAN_POINT('Ctrl Pts',(87.4319221861676,-33.7219238827077,115.155563994993));
#33905=CARTESIAN_POINT('Ctrl Pts',(86.6834909532146,-34.0786964374597,115.208213502724));
#33906=CARTESIAN_POINT('Ctrl Pts',(85.9350597202615,-34.4354689922117,115.260863010455));
#33907=CARTESIAN_POINT('Ctrl Pts',(85.3797820870628,-35.1974357943573,115.313512518185));
#33908=CARTESIAN_POINT('Ctrl Pts',(85.269384724626,-36.0191707812301,115.366162025916));
#33909=CARTESIAN_POINT('Ctrl Pts',(85.2545288738985,-36.1297492591316,115.373246916447));
#33910=CARTESIAN_POINT('Ctrl Pts',(85.2477290481687,-36.2414100371975,115.380331806977));
#33911=CARTESIAN_POINT('Ctrl Pts',(85.2486157516665,-36.3531793386365,115.387416697508));
#33912=CARTESIAN_POINT('Origin',(87.7685555885722,-36.3549260746835,114.));
#33913=CARTESIAN_POINT('',(85.2549234958158,-36.3544693504482,116.387416697508));
#33914=CARTESIAN_POINT('',(85.2527054364363,-36.3569864150889,116.112583302492));
#33915=CARTESIAN_POINT('',(85.2510555885723,-36.3549260746835,114.));
#33916=CARTESIAN_POINT('Ctrl Pts',(85.2527054364363,-36.3569864150889,116.112583302492));
#33917=CARTESIAN_POINT('Ctrl Pts',(85.2572379948492,-35.7786727106942,116.076077475652));
#33918=CARTESIAN_POINT('Ctrl Pts',(85.4556438192389,-35.1975491790577,116.039571648811));
#33919=CARTESIAN_POINT('Ctrl Pts',(85.8207471804533,-34.7534807073448,116.003065821971));
#33920=CARTESIAN_POINT('Ctrl Pts',(86.3473072916053,-34.1130353741477,115.95041631424));
#33921=CARTESIAN_POINT('Ctrl Pts',(87.2205990106268,-33.7576651668295,115.897766806509));
#33922=CARTESIAN_POINT('Ctrl Pts',(88.0447288166829,-33.8484717648297,115.845117298778));
#33923=CARTESIAN_POINT('Ctrl Pts',(88.8688586227391,-33.9392783628299,115.792467791047));
#33924=CARTESIAN_POINT('Ctrl Pts',(89.6438265158298,-34.4762617661486,115.739818283317));
#33925=CARTESIAN_POINT('Ctrl Pts',(90.0183125864139,-35.2159887146971,115.687168775586));
#33926=CARTESIAN_POINT('Ctrl Pts',(90.3927986569979,-35.9557156632457,115.634519267855));
#33927=CARTESIAN_POINT('Ctrl Pts',(90.3668029050753,-36.8981861570242,115.581869760124));
#33928=CARTESIAN_POINT('Ctrl Pts',(89.9521101094678,-37.6161455296502,115.529220252393));
#33929=CARTESIAN_POINT('Ctrl Pts',(89.5374173138602,-38.3341049022763,115.476570744662));
#33930=CARTESIAN_POINT('Ctrl Pts',(88.7340274745676,-38.82755315375,115.423921236932));
#33931=CARTESIAN_POINT('Ctrl Pts',(87.9061451582346,-38.8727930230408,115.371271729201));
#33932=CARTESIAN_POINT('Ctrl Pts',(87.0782628419015,-38.9180328923316,115.31862222147));
#33933=CARTESIAN_POINT('Ctrl Pts',(86.225888048528,-38.5150643794395,115.265972713739));
#33934=CARTESIAN_POINT('Ctrl Pts',(85.7354319287861,-37.8465671318175,115.213323206008));
#33935=CARTESIAN_POINT('Ctrl Pts',(85.4226179740676,-37.4201981676435,115.17974323817));
#33936=CARTESIAN_POINT('Ctrl Pts',(85.2570294771738,-36.8858143581896,115.146163270331));
#33937=CARTESIAN_POINT('Ctrl Pts',(85.2537848649131,-36.3532747669305,115.112583302492));
#33938=CARTESIAN_POINT('Ctrl Pts',(85.2486157516665,-36.3531793386365,115.387416697508));
#33939=CARTESIAN_POINT('Ctrl Pts',(85.2543183528958,-37.0719943171931,115.432981314708));
#33940=CARTESIAN_POINT('Ctrl Pts',(85.5779421228608,-37.795297911688,115.478545931909));
#33941=CARTESIAN_POINT('Ctrl Pts',(86.1212007095315,-38.2640642380391,115.524110549109));
#33942=CARTESIAN_POINT('Ctrl Pts',(86.7489311485485,-38.8057195363751,115.57676005684));
#33943=CARTESIAN_POINT('Ctrl Pts',(87.6699091182572,-39.0075269614469,115.62940956457));
#33944=CARTESIAN_POINT('Ctrl Pts',(88.4666232612295,-38.7780001859461,115.682059072301));
#33945=CARTESIAN_POINT('Ctrl Pts',(89.2633374042018,-38.5484734104452,115.734708580032));
#33946=CARTESIAN_POINT('Ctrl Pts',(89.9357877204377,-37.8876124343716,115.787358087763));
#33947=CARTESIAN_POINT('Ctrl Pts',(90.1791290848976,-37.0950085316391,115.840007595494));
#33948=CARTESIAN_POINT('Ctrl Pts',(90.4224704493576,-36.3024046289067,115.892657103225));
#33949=CARTESIAN_POINT('Ctrl Pts',(90.2367028620415,-35.3780577995155,115.945306610955));
#33950=CARTESIAN_POINT('Ctrl Pts',(89.7060412337264,-34.741006622201,115.997956118686));
#33951=CARTESIAN_POINT('Ctrl Pts',(89.1753796054112,-34.1039554448865,116.050605626417));
#33952=CARTESIAN_POINT('Ctrl Pts',(88.2998239360969,-33.7541999196487,116.103255134148));
#33953=CARTESIAN_POINT('Ctrl Pts',(87.4762940740561,-33.8502963951874,116.155904641879));
#33954=CARTESIAN_POINT('Ctrl Pts',(86.6527642120154,-33.9463928707262,116.20855414961));
#33955=CARTESIAN_POINT('Ctrl Pts',(85.881260157248,-34.4883413470415,116.26120365734));
#33956=CARTESIAN_POINT('Ctrl Pts',(85.5115315408654,-35.2304577237047,116.313853165071));
#33957=CARTESIAN_POINT('Ctrl Pts',(85.3393327604376,-35.5760937641259,116.33837434255));
#33958=CARTESIAN_POINT('Ctrl Pts',(85.2542859874774,-35.9651496671849,116.362895520029));
#33959=CARTESIAN_POINT('Ctrl Pts',(85.2549234958158,-36.3544693504482,116.387416697508));
#33960=CARTESIAN_POINT('Origin',(87.7685555885722,-36.3549260746835,114.));
#33961=CARTESIAN_POINT('',(85.2502276901495,-36.3571029251275,117.387416697508));
#33962=CARTESIAN_POINT('',(85.2470013985646,-36.3545560533907,117.112583302492));
#33963=CARTESIAN_POINT('',(85.2510555885723,-36.3549260746835,114.));
#33964=CARTESIAN_POINT('Ctrl Pts',(85.2470013985646,-36.3545560533907,117.112583302492));
#33965=CARTESIAN_POINT('Ctrl Pts',(85.246959225422,-36.3341987570445,117.111290696434));
#33966=CARTESIAN_POINT('Ctrl Pts',(85.2471846617478,-36.3138424184026,117.109998090376));
#33967=CARTESIAN_POINT('Ctrl Pts',(85.2476805824931,-36.2934926714317,117.108705484318));
#33968=CARTESIAN_POINT('Ctrl Pts',(85.2678800724692,-35.464621296564,117.056055976587));
#33969=CARTESIAN_POINT('Ctrl Pts',(85.7368234124319,-34.6466857522417,117.003406468856));
#33970=CARTESIAN_POINT('Ctrl Pts',(86.4419222703427,-34.2104846792909,116.950756961126));
#33971=CARTESIAN_POINT('Ctrl Pts',(87.1470211282534,-33.7742836063402,116.898107453395));
#33972=CARTESIAN_POINT('Ctrl Pts',(88.0882755041123,-33.7198170047611,116.845457945664));
#33973=CARTESIAN_POINT('Ctrl Pts',(88.8389820401025,-34.0717764801159,116.792808437933));
#33974=CARTESIAN_POINT('Ctrl Pts',(89.5896885760928,-34.4237359554708,116.740158930202));
#33975=CARTESIAN_POINT('Ctrl Pts',(90.1498472722143,-35.1821215077596,116.687509422471));
#33976=CARTESIAN_POINT('Ctrl Pts',(90.2655187018088,-36.0031305794793,116.634859914741));
#33977=CARTESIAN_POINT('Ctrl Pts',(90.3811901314033,-36.824139651199,116.58221040701));
#33978=CARTESIAN_POINT('Ctrl Pts',(90.0523742944708,-37.7077722423495,116.529560899279));
#33979=CARTESIAN_POINT('Ctrl Pts',(89.4281348504437,-38.253446954968,116.476911391548));
#33980=CARTESIAN_POINT('Ctrl Pts',(88.8038954064167,-38.7991216675865,116.424261883817));
#33981=CARTESIAN_POINT('Ctrl Pts',(87.8842323552952,-39.0068385016729,116.371612376086));
#33982=CARTESIAN_POINT('Ctrl Pts',(87.0860609561614,-38.7824321892052,116.318962868356));
#33983=CARTESIAN_POINT('Ctrl Pts',(86.2878895570277,-38.5580258767375,116.266313360625));
#33984=CARTESIAN_POINT('Ctrl Pts',(85.6112098098817,-37.9014964177156,116.213663852894));
#33985=CARTESIAN_POINT('Ctrl Pts',(85.3627841879501,-37.1104714586667,116.161014345163));
#33986=CARTESIAN_POINT('Ctrl Pts',(85.2866105609152,-36.867923046239,116.144870664273));
#33987=CARTESIAN_POINT('Ctrl Pts',(85.2507010392491,-36.6127294760279,116.128726983382));
#33988=CARTESIAN_POINT('Ctrl Pts',(85.2527054364363,-36.3569864150889,116.112583302492));
#33989=CARTESIAN_POINT('Ctrl Pts',(85.2549234958158,-36.3544693504482,116.387416697508));
#33990=CARTESIAN_POINT('Ctrl Pts',(85.2556547839073,-36.8010593493897,116.41554502776));
#33991=CARTESIAN_POINT('Ctrl Pts',(85.3691334424466,-37.2479964426169,116.443673358012));
#33992=CARTESIAN_POINT('Ctrl Pts',(85.5931440674471,-37.6301403068955,116.471801688264));
#33993=CARTESIAN_POINT('Ctrl Pts',(86.0124383884093,-38.3454222364119,116.524451195994));
#33994=CARTESIAN_POINT('Ctrl Pts',(86.8189802083315,-38.8337018184338,116.577100703725));
#33995=CARTESIAN_POINT('Ctrl Pts',(87.6471360580823,-38.8736249296274,116.629750211456));
#33996=CARTESIAN_POINT('Ctrl Pts',(88.4752919078331,-38.913548040821,116.682399719187));
#33997=CARTESIAN_POINT('Ctrl Pts',(89.3250617874126,-38.5051146811863,116.735049226918));
#33998=CARTESIAN_POINT('Ctrl Pts',(89.8112154442046,-37.8334819033445,116.787698734649));
#33999=CARTESIAN_POINT('Ctrl Pts',(90.2973691009967,-37.1618491255027,116.840348242379));
#34000=CARTESIAN_POINT('Ctrl Pts',(90.4199065350014,-36.2270169294537,116.89299775011));
#34001=CARTESIAN_POINT('Ctrl Pts',(90.1232772639163,-35.4527772754578,116.945647257841));
#34002=CARTESIAN_POINT('Ctrl Pts',(89.8266479928313,-34.6785376214619,116.998296765572));
#34003=CARTESIAN_POINT('Ctrl Pts',(89.1108520166566,-34.064890509519,117.050946273303));
#34004=CARTESIAN_POINT('Ctrl Pts',(88.3003845562159,-33.890023526213,117.103595781033));
#34005=CARTESIAN_POINT('Ctrl Pts',(87.4899170957753,-33.715156542907,117.156245288764));
#34006=CARTESIAN_POINT('Ctrl Pts',(86.5847781510686,-33.979069688238,117.208894796495));
#34007=CARTESIAN_POINT('Ctrl Pts',(85.9952986984001,-34.5621219510453,117.261544304226));
#34008=CARTESIAN_POINT('Ctrl Pts',(85.5255305233118,-35.0267681677034,117.303501768653));
#34009=CARTESIAN_POINT('Ctrl Pts',(85.2562320265711,-35.6940939103772,117.345459233081));
#34010=CARTESIAN_POINT('Ctrl Pts',(85.2502276901495,-36.3571029251275,117.387416697508));
#34011=CARTESIAN_POINT('Origin',(87.7685555885722,-36.3549260746835,114.));
#34012=CARTESIAN_POINT('',(85.2484784217854,-36.3532397189627,118.387416697508));
#34013=CARTESIAN_POINT('',(85.2536734366772,-36.353216668893,118.112583302492));
#34014=CARTESIAN_POINT('',(85.2510555885723,-36.3549260746835,114.));
#34015=CARTESIAN_POINT('Ctrl Pts',(85.2536734366772,-36.353216668893,118.112583302492));
#34016=CARTESIAN_POINT('Ctrl Pts',(85.2517947257147,-36.0562311247923,118.093854409486));
#34017=CARTESIAN_POINT('Ctrl Pts',(85.3004695466827,-35.7598413530357,118.075125516479));
#34018=CARTESIAN_POINT('Ctrl Pts',(85.4024432551376,-35.4830904910718,118.056396623473));
#34019=CARTESIAN_POINT('Ctrl Pts',(85.689105448669,-34.7051055540288,118.003747115742));
#34020=CARTESIAN_POINT('Ctrl Pts',(86.3969620113841,-34.082317068762,117.951097608011));
#34021=CARTESIAN_POINT('Ctrl Pts',(87.2051169348331,-33.8970567244546,117.89844810028));
#34022=CARTESIAN_POINT('Ctrl Pts',(88.0132718582821,-33.7117963801472,117.845798592549));
#34023=CARTESIAN_POINT('Ctrl Pts',(88.9217251424651,-33.9640641767992,117.793149084819));
#34024=CARTESIAN_POINT('Ctrl Pts',(89.5186433056692,-34.5394983449801,117.740499577088));
#34025=CARTESIAN_POINT('Ctrl Pts',(90.1155614688732,-35.1149325131609,117.687850069357));
#34026=CARTESIAN_POINT('Ctrl Pts',(90.4009445110984,-36.0135330528707,117.635200561626));
#34027=CARTESIAN_POINT('Ctrl Pts',(90.2454183699218,-36.8279330742855,117.582551053895));
#34028=CARTESIAN_POINT('Ctrl Pts',(90.0898922287453,-37.6423330957004,117.529901546165));
#34029=CARTESIAN_POINT('Ctrl Pts',(89.493456904167,-38.3725325988204,117.477252038434));
#34030=CARTESIAN_POINT('Ctrl Pts',(88.7264972807027,-38.6875067429112,117.424602530703));
#34031=CARTESIAN_POINT('Ctrl Pts',(87.9595376572385,-39.0024808870021,117.371953022972));
#34032=CARTESIAN_POINT('Ctrl Pts',(87.0220537348881,-38.9022296720638,117.319303515241));
#34033=CARTESIAN_POINT('Ctrl Pts',(86.3390395937077,-38.4322004618881,117.26665400751));
#34034=CARTESIAN_POINT('Ctrl Pts',(85.6727942364087,-37.9737110102155,117.215297105838));
#34035=CARTESIAN_POINT('Ctrl Pts',(85.2486769917781,-37.1633776276781,117.163940204165));
#34036=CARTESIAN_POINT('Ctrl Pts',(85.2470013985646,-36.3545560533907,117.112583302492));
#34037=CARTESIAN_POINT('Ctrl Pts',(85.2502276901495,-36.3571029251275,117.387416697508));
#34038=CARTESIAN_POINT('Ctrl Pts',(85.2486976018588,-36.5260578701663,117.398108740812));
#34039=CARTESIAN_POINT('Ctrl Pts',(85.2642654687678,-36.6947324929201,117.408800784115));
#34040=CARTESIAN_POINT('Ctrl Pts',(85.2979709317325,-36.8597013491054,117.419492827418));
#34041=CARTESIAN_POINT('Ctrl Pts',(85.463942578364,-37.6720371040742,117.472142335149));
#34042=CARTESIAN_POINT('Ctrl Pts',(86.0697058322574,-38.394517233728,117.52479184288));
#34043=CARTESIAN_POINT('Ctrl Pts',(86.8406471339867,-38.699616357898,117.577441350611));
#34044=CARTESIAN_POINT('Ctrl Pts',(87.6115884357159,-39.004715482068,117.630090858342));
#34045=CARTESIAN_POINT('Ctrl Pts',(88.5477077852809,-38.8924336007541,117.682740366073));
#34046=CARTESIAN_POINT('Ctrl Pts',(89.2246297109517,-38.4136719974215,117.735389873803));
#34047=CARTESIAN_POINT('Ctrl Pts',(89.9015516366226,-37.9349103940889,117.788039381534));
#34048=CARTESIAN_POINT('Ctrl Pts',(90.3192761383994,-37.0896690687376,117.840688889265));
#34049=CARTESIAN_POINT('Ctrl Pts',(90.2884341656518,-36.2611253227459,117.893338396996));
#34050=CARTESIAN_POINT('Ctrl Pts',(90.2575921929042,-35.4325815767542,117.945987904727));
#34051=CARTESIAN_POINT('Ctrl Pts',(89.7781837456322,-34.6207354101222,117.998637412457));
#34052=CARTESIAN_POINT('Ctrl Pts',(89.0675413531486,-34.1936249369889,118.051286920188));
#34053=CARTESIAN_POINT('Ctrl Pts',(88.3568989606649,-33.7665144638555,118.103936427919));
#34054=CARTESIAN_POINT('Ctrl Pts',(87.4150226229695,-33.7241396842209,118.15658593565));
#34055=CARTESIAN_POINT('Ctrl Pts',(86.6688976547862,-34.085710559864,118.209235443381));
#34056=CARTESIAN_POINT('Ctrl Pts',(85.9227726866028,-34.4472814355072,118.261884951112));
#34057=CARTESIAN_POINT('Ctrl Pts',(85.3723990879314,-35.2127979664282,118.314534458842));
#34058=CARTESIAN_POINT('Ctrl Pts',(85.2672803603705,-36.0352248747766,118.367183966573));
#34059=CARTESIAN_POINT('Ctrl Pts',(85.2538149674186,-36.1405752890371,118.373928210218));
#34060=CARTESIAN_POINT('Ctrl Pts',(85.2476556902819,-36.2468595365593,118.380672453863));
#34061=CARTESIAN_POINT('Ctrl Pts',(85.2484784217854,-36.3532397189627,118.387416697508));
#34062=CARTESIAN_POINT('Origin',(87.7685555885722,-36.3549260746835,114.));
#34063=CARTESIAN_POINT('',(85.2548912454248,-36.3543846295848,119.387416697508));
#34064=CARTESIAN_POINT('',(85.2528440754712,-36.356949956235,119.112583302492));
#34065=CARTESIAN_POINT('',(85.2510555885723,-36.3549260746835,114.));
#34066=CARTESIAN_POINT('Ctrl Pts',(85.2528440754712,-36.356949956235,119.112583302492));
#34067=CARTESIAN_POINT('Ctrl Pts',(85.2572372892863,-35.7839527661201,119.076418122537));
#34068=CARTESIAN_POINT('Ctrl Pts',(85.4516401968638,-35.2082587139073,119.040252942582));
#34069=CARTESIAN_POINT('Ctrl Pts',(85.8105044563501,-34.7660205958344,119.004087762628));
#34070=CARTESIAN_POINT('Ctrl Pts',(86.3329414144337,-34.1222074240089,118.951438254897));
#34071=CARTESIAN_POINT('Ctrl Pts',(87.2039332985395,-33.761237137223,118.898788747166));
#34072=CARTESIAN_POINT('Ctrl Pts',(88.0286291841641,-33.8467501269348,118.846139239435));
#34073=CARTESIAN_POINT('Ctrl Pts',(88.8533250697887,-33.9322631166466,118.793489731704));
#34074=CARTESIAN_POINT('Ctrl Pts',(89.6317249569322,-34.4642593828561,118.740840223974));
#34075=CARTESIAN_POINT('Ctrl Pts',(90.0109530931821,-35.2015665076848,118.688190716243));
#34076=CARTESIAN_POINT('Ctrl Pts',(90.390181229432,-35.9388736325135,118.635541208512));
#34077=CARTESIAN_POINT('Ctrl Pts',(90.3702376147884,-36.8814916159616,118.582891700781));
#34078=CARTESIAN_POINT('Ctrl Pts',(89.960163383942,-37.60209892972,118.53024219305));
#34079=CARTESIAN_POINT('Ctrl Pts',(89.5500891530956,-38.3227062434784,118.477592685319));
#34080=CARTESIAN_POINT('Ctrl Pts',(88.7498843060464,-38.8213028875472,118.424943177589));
#34081=CARTESIAN_POINT('Ctrl Pts',(87.9223095415073,-38.8718576552712,118.372293669858));
#34082=CARTESIAN_POINT('Ctrl Pts',(87.0947347769682,-38.9224124229951,118.319644162127));
#34083=CARTESIAN_POINT('Ctrl Pts',(86.2397900949392,-38.5249253143742,118.266994654396));
#34084=CARTESIAN_POINT('Ctrl Pts',(85.7450516660987,-37.8595910656541,118.214345146665));
#34085=CARTESIAN_POINT('Ctrl Pts',(85.4263054449591,-37.4309346985486,118.180424531941));
#34086=CARTESIAN_POINT('Ctrl Pts',(85.2570760419841,-36.8910985510045,118.146503917216));
#34087=CARTESIAN_POINT('Ctrl Pts',(85.2536734366772,-36.353216668893,118.112583302492));
#34088=CARTESIAN_POINT('Ctrl Pts',(85.2484784217854,-36.3532397189627,118.387416697508));
#34089=CARTESIAN_POINT('Ctrl Pts',(85.2540784132636,-37.0773254169046,118.433321961594));
#34090=CARTESIAN_POINT('Ctrl Pts',(85.583152017838,-37.8058557387736,118.47922722568));
#34091=CARTESIAN_POINT('Ctrl Pts',(86.1334932425857,-38.2746025447411,118.525132489766));
#34092=CARTESIAN_POINT('Ctrl Pts',(86.7646887088122,-38.8122160205814,118.577781997496));
#34093=CARTESIAN_POINT('Ctrl Pts',(87.6869434977158,-39.0081056864863,118.630431505227));
#34094=CARTESIAN_POINT('Ctrl Pts',(88.4821674255945,-38.7734679428665,118.683081012958));
#34095=CARTESIAN_POINT('Ctrl Pts',(89.2773913534732,-38.5388301992467,118.735730520689));
#34096=CARTESIAN_POINT('Ctrl Pts',(89.9455844203271,-37.8736650461022,118.78838002842));
#34097=CARTESIAN_POINT('Ctrl Pts',(90.1838314597843,-37.0795149872964,118.841029536151));
#34098=CARTESIAN_POINT('Ctrl Pts',(90.4220784992415,-36.2853649284906,118.893679043881));
#34099=CARTESIAN_POINT('Ctrl Pts',(90.2303795113019,-35.3622299640236,118.946328551612));
#34100=CARTESIAN_POINT('Ctrl Pts',(89.6956383182525,-34.7285992988272,118.998978059343));
#34101=CARTESIAN_POINT('Ctrl Pts',(89.1608971252032,-34.0949686336307,119.051627567074));
#34102=CARTESIAN_POINT('Ctrl Pts',(88.283113727044,-33.7508422677048,119.104277074805));
#34103=CARTESIAN_POINT('Ctrl Pts',(87.4602178765024,-33.852224642133,119.156926582536));
#34104=CARTESIAN_POINT('Ctrl Pts',(86.6373220259608,-33.9536070165613,119.209576090266));
#34105=CARTESIAN_POINT('Ctrl Pts',(85.8693137230369,-34.5004981313436,119.262225597997));
#34106=CARTESIAN_POINT('Ctrl Pts',(85.5043578581278,-35.2449732445367,119.314875105728));
#34107=CARTESIAN_POINT('Ctrl Pts',(85.3367432528447,-35.5868910330671,119.339055636321));
#34108=CARTESIAN_POINT('Ctrl Pts',(85.2541454125404,-35.9704856625546,119.363236166915));
#34109=CARTESIAN_POINT('Ctrl Pts',(85.2548912454248,-36.3543846295848,119.387416697508));
#34110=CARTESIAN_POINT('Origin',(87.7685555885722,-36.3549260746835,114.));
#34111=CARTESIAN_POINT('',(85.2503884478834,-36.3571243043025,120.387416697508));
#34112=CARTESIAN_POINT('',(85.2469700844899,-36.3546528234761,120.112583302492));
#34113=CARTESIAN_POINT('',(85.2510555885723,-36.3549260746835,114.));
#34114=CARTESIAN_POINT('Ctrl Pts',(85.2469700844899,-36.3546528234761,120.112583302492));
#34115=CARTESIAN_POINT('Ctrl Pts',(85.2469467853652,-36.3396608858275,120.11163134332));
#34116=CARTESIAN_POINT('Ctrl Pts',(85.2470690489527,-36.3246693383145,120.110679384147));
#34117=CARTESIAN_POINT('Ctrl Pts',(85.2473380380648,-36.3096804239763,120.109727424975));
#34118=CARTESIAN_POINT('Ctrl Pts',(85.2622148781136,-35.4806963832532,120.057077917244));
#34119=CARTESIAN_POINT('Ctrl Pts',(85.7258966860521,-34.6597667145453,120.004428409513));
#34120=CARTESIAN_POINT('Ctrl Pts',(86.4281801872503,-34.2190472204532,119.951778901782));
#34121=CARTESIAN_POINT('Ctrl Pts',(87.1304636884485,-33.778327726361,119.899129394052));
#34122=CARTESIAN_POINT('Ctrl Pts',(88.0713488829063,-33.7178184068845,119.846479886321));
#34123=CARTESIAN_POINT('Ctrl Pts',(88.8242998622034,-34.0649503288953,119.79383037859));
#34124=CARTESIAN_POINT('Ctrl Pts',(89.5772508415005,-34.4120822509062,119.741180870859));
#34125=CARTESIAN_POINT('Ctrl Pts',(90.1422676056369,-35.1668554144045,119.688531363128));
#34126=CARTESIAN_POINT('Ctrl Pts',(90.2632083545705,-35.9871048410839,119.635881855397));
#34127=CARTESIAN_POINT('Ctrl Pts',(90.3841491035041,-36.8073542677633,119.583232347667));
#34128=CARTESIAN_POINT('Ctrl Pts',(90.0610138372351,-37.6930799576239,119.530582839936));
#34129=CARTESIAN_POINT('Ctrl Pts',(89.4402910353544,-38.2427516588164,119.477933332205));
#34130=CARTESIAN_POINT('Ctrl Pts',(88.8195682334738,-38.7924233600089,119.425283824474));
#34131=CARTESIAN_POINT('Ctrl Pts',(87.9012578959816,-39.0060410725332,119.372634316743));
#34132=CARTESIAN_POINT('Ctrl Pts',(87.1016620398446,-38.7867644448508,119.319984809013));
#34133=CARTESIAN_POINT('Ctrl Pts',(86.3020661837075,-38.5674878171683,119.267335301282));
#34134=CARTESIAN_POINT('Ctrl Pts',(85.6211848089255,-37.915316849279,119.214685793551));
#34135=CARTESIAN_POINT('Ctrl Pts',(85.3676851375653,-37.1259033369019,119.16203628582));
#34136=CARTESIAN_POINT('Ctrl Pts',(85.2883155127783,-36.8787414611372,119.145551958044));
#34137=CARTESIAN_POINT('Ctrl Pts',(85.2508416196115,-36.6181258582599,119.129067630268));
#34138=CARTESIAN_POINT('Ctrl Pts',(85.2528440754712,-36.356949956235,119.112583302492));
#34139=CARTESIAN_POINT('Ctrl Pts',(85.2548912454248,-36.3543846295848,119.387416697508));
#34140=CARTESIAN_POINT('Ctrl Pts',(85.2557693526794,-36.8063685458726,119.415885674645));
#34141=CARTESIAN_POINT('Ctrl Pts',(85.372174783394,-37.2587743214379,119.444354651783));
#34142=CARTESIAN_POINT('Ctrl Pts',(85.6013770646085,-37.6440823482595,119.47282362892));
#34143=CARTESIAN_POINT('Ctrl Pts',(86.0252555628928,-38.3566572271855,119.525473136651));
#34144=CARTESIAN_POINT('Ctrl Pts',(86.8349159863556,-38.8397478734336,119.578122644382));
#34145=CARTESIAN_POINT('Ctrl Pts',(87.6633111164763,-38.8743526092352,119.630772152113));
#34146=CARTESIAN_POINT('Ctrl Pts',(88.4917062465969,-38.9089573450367,119.683421659844));
#34147=CARTESIAN_POINT('Ctrl Pts',(89.3388360833753,-38.4950761703916,119.736071167575));
#34148=CARTESIAN_POINT('Ctrl Pts',(89.820667151996,-37.8203355743053,119.788720675305));
#34149=CARTESIAN_POINT('Ctrl Pts',(90.3024982206167,-37.1455949782191,119.841370183036));
#34150=CARTESIAN_POINT('Ctrl Pts',(90.4190305210798,-36.2099949606916,119.894019690767));
#34151=CARTESIAN_POINT('Ctrl Pts',(90.1174360005457,-35.4376760716325,119.946669198498));
#34152=CARTESIAN_POINT('Ctrl Pts',(89.8158414800116,-34.6653571825733,119.999318706229));
#34153=CARTESIAN_POINT('Ctrl Pts',(89.0961201384803,-34.0563194219826,120.051968213959));
#34154=CARTESIAN_POINT('Ctrl Pts',(88.2845465091856,-33.8866597493,120.10461772169));
#34155=CARTESIAN_POINT('Ctrl Pts',(87.4729728798908,-33.7170000766173,120.157267229421));
#34156=CARTESIAN_POINT('Ctrl Pts',(86.5695469628327,-33.9867184918427,120.209916737152));
#34157=CARTESIAN_POINT('Ctrl Pts',(85.9838235547468,-34.5735444080027,120.262566244883));
#34158=CARTESIAN_POINT('Ctrl Pts',(85.5208383293416,-35.0374011112114,120.304183062425));
#34159=CARTESIAN_POINT('Ctrl Pts',(85.2563573256464,-35.6993902681898,120.345799879966));
#34160=CARTESIAN_POINT('Ctrl Pts',(85.2503884478834,-36.3571243043025,120.387416697508));
#34161=CARTESIAN_POINT('Origin',(87.7685555885722,-36.3549260746835,114.));
#34162=CARTESIAN_POINT('',(85.2483528516199,-36.3533471753035,121.387416697508));
#34163=CARTESIAN_POINT('',(85.2535610703604,-36.3531642914838,121.112583302492));
#34164=CARTESIAN_POINT('',(85.2510555885723,-36.3549260746835,114.));
#34165=CARTESIAN_POINT('',(89.6820215852375,-34.7189388713088,122.));
#34166=CARTESIAN_POINT('Ctrl Pts',(85.2483528516199,-36.3533471753035,121.387416697508));
#34167=CARTESIAN_POINT('Ctrl Pts',(85.253810887375,-37.0825701143354,121.43366260848));
#34168=CARTESIAN_POINT('Ctrl Pts',(85.5883405994922,-37.816044282996,121.479908519451));
#34169=CARTESIAN_POINT('Ctrl Pts',(86.1458176873049,-38.2848775789271,121.526154430423));
#34170=CARTESIAN_POINT('Ctrl Pts',(86.7804877290006,-38.8186294657434,121.578803938153));
#34171=CARTESIAN_POINT('Ctrl Pts',(87.7041221542809,-39.0093775992254,121.631453445884));
#34172=CARTESIAN_POINT('Ctrl Pts',(88.4977390504798,-38.7692237839494,121.684102953615));
#34173=CARTESIAN_POINT('Ctrl Pts',(89.2913559466788,-38.5290699686735,121.736752461346));
#34174=CARTESIAN_POINT('Ctrl Pts',(89.9549553137964,-37.8580142046394,121.789401969077));
#34175=CARTESIAN_POINT('Ctrl Pts',(90.1879205700165,-37.0637282318536,121.842051476808));
#34176=CARTESIAN_POINT('Ctrl Pts',(90.4208858262365,-36.2694422590678,121.894700984538));
#34177=CARTESIAN_POINT('Ctrl Pts',(90.223216971559,-35.3519260775303,121.947350492269));
#34178=CARTESIAN_POINT('Ctrl Pts',(89.6820215852375,-34.7189388713087,122.));
#34179=CARTESIAN_POINT('',(85.8514455075092,-34.7163982291022,122.));
#34180=CARTESIAN_POINT('Origin',(87.7685555885722,-36.3549260746835,122.));
#34181=CARTESIAN_POINT('Ctrl Pts',(85.8514366626952,-34.7163920625306,122.));
#34182=CARTESIAN_POINT('Ctrl Pts',(86.3742572722501,-34.1076767185939,121.949053726697));
#34183=CARTESIAN_POINT('Ctrl Pts',(87.2139816526743,-33.767500880252,121.898107453395));
#34184=CARTESIAN_POINT('Ctrl Pts',(88.012652402947,-33.8452637608976,121.847161180092));
#34185=CARTESIAN_POINT('Ctrl Pts',(88.838024292095,-33.9256264080613,121.794511672361));
#34186=CARTESIAN_POINT('Ctrl Pts',(89.619551657879,-34.4523399348362,121.74186216463));
#34187=CARTESIAN_POINT('Ctrl Pts',(90.003436239116,-35.1871265566876,121.6892126569));
#34188=CARTESIAN_POINT('Ctrl Pts',(90.3873208203531,-35.9219131785391,121.636563149169));
#34189=CARTESIAN_POINT('Ctrl Pts',(90.3735626170432,-36.864772895467,121.583913641438));
#34190=CARTESIAN_POINT('Ctrl Pts',(89.9681578782027,-37.5880326323531,121.531264133707));
#34191=CARTESIAN_POINT('Ctrl Pts',(89.5627531393622,-38.3112923692392,121.478614625976));
#34192=CARTESIAN_POINT('Ctrl Pts',(88.765701864991,-38.8149521260835,121.425965118245));
#34193=CARTESIAN_POINT('Ctrl Pts',(87.9384522287811,-38.8708030839915,121.373315610515));
#34194=CARTESIAN_POINT('Ctrl Pts',(87.1112025925711,-38.9266540418996,121.320666102784));
#34195=CARTESIAN_POINT('Ctrl Pts',(86.2537545945224,-38.5346962008713,121.268016595053));
#34196=CARTESIAN_POINT('Ctrl Pts',(85.7547622998719,-37.8725604668736,121.215367087322));
#34197=CARTESIAN_POINT('Ctrl Pts',(85.430046907739,-37.4416807382379,121.181105825712));
#34198=CARTESIAN_POINT('Ctrl Pts',(85.2571251526924,-36.8963899829528,121.146844564102));
#34199=CARTESIAN_POINT('Ctrl Pts',(85.2535610703604,-36.3531642914838,121.112583302492));
#34200=CARTESIAN_POINT('Origin',(87.7685555885722,-36.3549260746835,124.208423447177));
#34201=CARTESIAN_POINT('',(84.6902859389797,-36.3541125877401,107.791576552823));
#34202=CARTESIAN_POINT('',(84.6999263673563,-36.3546117753717,107.708423447177));
#34203=CARTESIAN_POINT('',(84.6950555885722,-36.3549260746832,124.208423447177));
#34204=CARTESIAN_POINT('',(88.5623548711046,-39.3241490284293,107.));
#34205=CARTESIAN_POINT('Ctrl Pts',(84.6999263673563,-36.3546117753717,107.708423447177));
#34206=CARTESIAN_POINT('Ctrl Pts',(84.6996065051311,-35.8594362872189,107.682880329042));
#34207=CARTESIAN_POINT('Ctrl Pts',(85.0458587978589,-34.3441196884525,107.604687703175));
#34208=CARTESIAN_POINT('Ctrl Pts',(87.4170212023543,-32.7460640346786,107.473845569577));
#34209=CARTESIAN_POINT('Ctrl Pts',(90.6005809066571,-34.0865213418793,107.315897046385));
#34210=CARTESIAN_POINT('Ctrl Pts',(91.2113486315107,-37.4887066956559,107.157948523193));
#34211=CARTESIAN_POINT('Ctrl Pts',(89.5445934608762,-39.0615549760519,107.052649507731));
#34212=CARTESIAN_POINT('Ctrl Pts',(88.5623548711045,-39.3241490284294,107.));
#34213=CARTESIAN_POINT('',(86.9747563060389,-39.3241490284291,107.));
#34214=CARTESIAN_POINT('Origin',(87.7685555885722,-36.3549260746835,107.));
#34215=CARTESIAN_POINT('Ctrl Pts',(84.6902859389797,-36.3541125877401,107.791576552823));
#34216=CARTESIAN_POINT('Ctrl Pts',(84.6901298701282,-36.3096037501105,107.789262006108));
#34217=CARTESIAN_POINT('Ctrl Pts',(84.7110895869572,-35.252794330332,107.734297951662));
#34218=CARTESIAN_POINT('Ctrl Pts',(85.9203584351496,-33.2347633730889,107.626684389485));
#34219=CARTESIAN_POINT('Ctrl Pts',(89.3710240668315,-33.1013877392709,107.468735866293));
#34220=CARTESIAN_POINT('Ctrl Pts',(91.3686331795228,-35.9187012093704,107.3107873431));
#34221=CARTESIAN_POINT('Ctrl Pts',(90.1161178614875,-39.0952438942321,107.154542054336));
#34222=CARTESIAN_POINT('Ctrl Pts',(87.9198088452516,-39.5801184192997,107.050946273303));
#34223=CARTESIAN_POINT('Ctrl Pts',(86.9728422903211,-39.3292375489681,107.));
#34224=CARTESIAN_POINT('Origin',(87.7685555885722,-36.3549260746835,124.208423447177));
#34225=CARTESIAN_POINT('',(84.6986441861196,-36.3530606800421,108.791576552823));
#34226=CARTESIAN_POINT('',(84.6934625360053,-36.357484352344,108.708423447177));
#34227=CARTESIAN_POINT('',(84.6950555885722,-36.3549260746832,124.208423447177));
#34228=CARTESIAN_POINT('Ctrl Pts',(84.6934625360053,-36.357484352344,108.708423447177));
#34229=CARTESIAN_POINT('Ctrl Pts',(84.7008503927251,-35.5287362890068,108.665444042093));
#34230=CARTESIAN_POINT('Ctrl Pts',(85.4724994656418,-33.6726457957907,108.569815129278));
#34231=CARTESIAN_POINT('Ctrl Pts',(88.6015534510421,-32.8253527833924,108.421536708732));
#34232=CARTESIAN_POINT('Ctrl Pts',(91.1794497561267,-35.1229272408109,108.26358818554));
#34233=CARTESIAN_POINT('Ctrl Pts',(90.6647257407023,-38.5375841171318,108.105639662347));
#34234=CARTESIAN_POINT('Ctrl Pts',(87.5242687243508,-39.9731544640366,107.947691139155));
#34235=CARTESIAN_POINT('Ctrl Pts',(85.0771139192411,-38.4267875479491,107.815285734098));
#34236=CARTESIAN_POINT('Ctrl Pts',(84.7002658055582,-36.8800926359444,107.735529836772));
#34237=CARTESIAN_POINT('Ctrl Pts',(84.6999263673563,-36.3546117753717,107.708423447177));
#34238=CARTESIAN_POINT('Ctrl Pts',(84.6986441861196,-36.3530606800421,108.791576552823));
#34239=CARTESIAN_POINT('Ctrl Pts',(84.6965000548819,-35.9705777414508,108.771825719159));
#34240=CARTESIAN_POINT('Ctrl Pts',(84.9394944552829,-34.5711418157649,108.699425377765));
#34241=CARTESIAN_POINT('Ctrl Pts',(87.0264678663363,-32.8051171947587,108.57437552864));
#34242=CARTESIAN_POINT('Ctrl Pts',(90.3353208987278,-33.792977483537,108.416427005448));
#34243=CARTESIAN_POINT('Ctrl Pts',(91.3169639431757,-37.1036892864445,108.258478482255));
#34244=CARTESIAN_POINT('Ctrl Pts',(89.0813770537997,-39.7354983689013,108.100529959063));
#34245=CARTESIAN_POINT('Ctrl Pts',(85.70568896844,-39.3086385235238,107.944895982585));
#34246=CARTESIAN_POINT('Ctrl Pts',(84.6936800029274,-37.3220561563539,107.841911513838));
#34247=CARTESIAN_POINT('Ctrl Pts',(84.6902859389797,-36.3541125877401,107.791576552823));
#34248=CARTESIAN_POINT('Origin',(87.7685555885722,-36.3549260746835,124.208423447177));
#34249=CARTESIAN_POINT('',(84.6967209343146,-36.3575187349746,109.791576552823));
#34250=CARTESIAN_POINT('',(84.6924245878599,-36.3526580233552,109.708423447177));
#34251=CARTESIAN_POINT('',(84.6950555885722,-36.3549260746832,124.208423447177));
#34252=CARTESIAN_POINT('Ctrl Pts',(84.6924245878599,-36.3526580233552,109.708423447177));
#34253=CARTESIAN_POINT('Ctrl Pts',(84.6911854664029,-36.203038268201,109.700657262876));
#34254=CARTESIAN_POINT('Ctrl Pts',(84.7688483649364,-35.0403882407784,109.640241570843));
#34255=CARTESIAN_POINT('Ctrl Pts',(86.2502054927865,-33.0615290694994,109.527176371079));
#34256=CARTESIAN_POINT('Ctrl Pts',(89.6962563926914,-33.2831482377538,109.369227847887));
#34257=CARTESIAN_POINT('Ctrl Pts',(91.3945200278872,-36.2898545193635,109.211279324695));
#34258=CARTESIAN_POINT('Ctrl Pts',(89.805231108493,-39.3555600803365,109.053330801502));
#34259=CARTESIAN_POINT('Ctrl Pts',(86.3693522399246,-39.7006802402578,108.89538227831));
#34260=CARTESIAN_POINT('Ctrl Pts',(84.7918203783131,-37.7438433959039,108.780413160201));
#34261=CARTESIAN_POINT('Ctrl Pts',(84.6918003135367,-36.5439475857204,108.718093549824));
#34262=CARTESIAN_POINT('Ctrl Pts',(84.6934625360053,-36.357484352344,108.708423447177));
#34263=CARTESIAN_POINT('Ctrl Pts',(84.6967209343146,-36.3575187349745,109.791576552823));
#34264=CARTESIAN_POINT('Ctrl Pts',(84.7025803795521,-35.6385126094882,109.754389432211));
#34265=CARTESIAN_POINT('Ctrl Pts',(85.3117912843899,-33.8925909032789,109.664552803868));
#34266=CARTESIAN_POINT('Ctrl Pts',(88.2120005461565,-32.7555923274475,109.522066667795));
#34267=CARTESIAN_POINT('Ctrl Pts',(91.0248782320717,-34.7586147002439,109.364118144602));
#34268=CARTESIAN_POINT('Ctrl Pts',(90.8853471879654,-38.2089641874212,109.20616962141));
#34269=CARTESIAN_POINT('Ctrl Pts',(87.9199160465446,-39.9783134162844,109.048221098218));
#34270=CARTESIAN_POINT('Ctrl Pts',(85.2052267935342,-38.6520010530253,108.910023408688));
#34271=CARTESIAN_POINT('Ctrl Pts',(84.7022156340872,-36.9901569033004,108.82447522689));
#34272=CARTESIAN_POINT('Ctrl Pts',(84.6986441861196,-36.3530606800421,108.791576552823));
#34273=CARTESIAN_POINT('Origin',(87.7685555885722,-36.3549260746835,124.208423447177));
#34274=CARTESIAN_POINT('',(84.6902141559912,-36.3542412678362,110.791576552823));
#34275=CARTESIAN_POINT('',(84.6998362604058,-36.3545776583035,110.708423447177));
#34276=CARTESIAN_POINT('',(84.6950555885722,-36.3549260746832,124.208423447177));
#34277=CARTESIAN_POINT('Ctrl Pts',(84.6998362604058,-36.3545776583035,110.708423447177));
#34278=CARTESIAN_POINT('Ctrl Pts',(84.6993369649495,-35.8660461176461,110.683220975927));
#34279=CARTESIAN_POINT('Ctrl Pts',(85.0389980437079,-34.3575980587991,110.605368996946));
#34280=CARTESIAN_POINT('Ctrl Pts',(87.3945229855647,-32.747717976947,110.474867510234));
#34281=CARTESIAN_POINT('Ctrl Pts',(90.584585262429,-34.069794239593,110.316918987042));
#34282=CARTESIAN_POINT('Ctrl Pts',(91.221439085307,-37.4637300323244,110.158970463849));
#34283=CARTESIAN_POINT('Ctrl Pts',(88.7276684448237,-39.8523470110271,110.001021940657));
#34284=CARTESIAN_POINT('Ctrl Pts',(85.5296731500474,-39.1084280856274,109.850839601766));
#34285=CARTESIAN_POINT('Ctrl Pts',(84.6995858767197,-37.217359606649,109.753306770606));
#34286=CARTESIAN_POINT('Ctrl Pts',(84.6924245878599,-36.3526580233552,109.708423447177));
#34287=CARTESIAN_POINT('Ctrl Pts',(84.6902141559913,-36.3542412678362,110.791576552823));
#34288=CARTESIAN_POINT('Ctrl Pts',(84.6900985120232,-36.3162849815638,110.789602652993));
#34289=CARTESIAN_POINT('Ctrl Pts',(84.7078624516269,-35.2660376004022,110.734979245433));
#34290=CARTESIAN_POINT('Ctrl Pts',(85.9003809608462,-33.2465872009442,110.627706330142));
#34291=CARTESIAN_POINT('Ctrl Pts',(89.3500610269517,-33.0913869620613,110.46975780695));
#34292=CARTESIAN_POINT('Ctrl Pts',(91.3658382115574,-35.895138379632,110.311809283757));
#34293=CARTESIAN_POINT('Ctrl Pts',(90.1200686479678,-39.1157653183575,110.153860760565));
#34294=CARTESIAN_POINT('Ctrl Pts',(86.7422537121608,-39.8332232781445,109.995912237372));
#34295=CARTESIAN_POINT('Ctrl Pts',(84.8711430366209,-37.9705915317642,109.875150834792));
#34296=CARTESIAN_POINT('Ctrl Pts',(84.6942845797629,-36.6564811410552,109.807038939942));
#34297=CARTESIAN_POINT('Ctrl Pts',(84.6967209343146,-36.3575187349745,109.791576552823));
#34298=CARTESIAN_POINT('Origin',(87.7685555885722,-36.3549260746835,124.208423447177));
#34299=CARTESIAN_POINT('',(84.6985185386966,-36.3529840193472,111.791576552823));
#34300=CARTESIAN_POINT('',(84.6936554590675,-36.3575218684262,111.708423447177));
#34301=CARTESIAN_POINT('',(84.6950555885722,-36.3549260746832,124.208423447177));
#34302=CARTESIAN_POINT('Ctrl Pts',(84.6936554590675,-36.3575218684262,111.708423447177));
#34303=CARTESIAN_POINT('Ctrl Pts',(84.7010363386306,-35.5352098446355,111.665784688979));
#34304=CARTESIAN_POINT('Ctrl Pts',(85.4624963011915,-33.6854549308403,111.570496423049));
#34305=CARTESIAN_POINT('Ctrl Pts',(88.5788817046039,-32.8200679121307,111.422558649389));
#34306=CARTESIAN_POINT('Ctrl Pts',(91.1714506588609,-35.1010697096973,111.264610126197));
#34307=CARTESIAN_POINT('Ctrl Pts',(90.6787181473369,-38.5189049390048,111.106661603004));
#34308=CARTESIAN_POINT('Ctrl Pts',(87.5474297522212,-39.9747263466277,110.948713079812));
#34309=CARTESIAN_POINT('Ctrl Pts',(85.0842717295461,-38.4399664305319,110.815967027869));
#34310=CARTESIAN_POINT('Ctrl Pts',(84.700380023772,-36.8866184603822,110.735870483658));
#34311=CARTESIAN_POINT('Ctrl Pts',(84.6998362604058,-36.3545776583035,110.708423447177));
#34312=CARTESIAN_POINT('Ctrl Pts',(84.6985185386966,-36.3529840193472,111.791576552823));
#34313=CARTESIAN_POINT('Ctrl Pts',(84.6963188618144,-35.9771365370321,111.772166366045));
#34314=CARTESIAN_POINT('Ctrl Pts',(84.9337531498146,-34.5844970198617,111.700106671536));
#34315=CARTESIAN_POINT('Ctrl Pts',(87.0036900983236,-32.8099538921628,111.575397469297));
#34316=CARTESIAN_POINT('Ctrl Pts',(90.3188172011552,-33.7765520327001,111.417448946105));
#34317=CARTESIAN_POINT('Ctrl Pts',(91.3216996625609,-37.0808834993901,111.259500422912));
#34318=CARTESIAN_POINT('Ctrl Pts',(89.1030544560686,-39.7270114481203,111.10155189972));
#34319=CARTESIAN_POINT('Ctrl Pts',(85.7173072338234,-39.3209114482164,110.945577276356));
#34320=CARTESIAN_POINT('Ctrl Pts',(84.6931830646942,-37.3286868055508,110.842252160724));
#34321=CARTESIAN_POINT('Ctrl Pts',(84.6902141559913,-36.3542412678362,110.791576552823));
#34322=CARTESIAN_POINT('Origin',(87.7685555885722,-36.3549260746835,124.208423447177));
#34323=CARTESIAN_POINT('',(84.6968970266175,-36.35748207472,112.791576552823));
#34324=CARTESIAN_POINT('',(84.6922488060663,-36.3527237795464,112.708423447177));
#34325=CARTESIAN_POINT('',(84.6950555885722,-36.3549260746832,124.208423447177));
#34326=CARTESIAN_POINT('Ctrl Pts',(84.6922488060663,-36.3527237795464,112.708423447177));
#34327=CARTESIAN_POINT('Ctrl Pts',(84.6910879425595,-36.2096880917331,112.700997909761));
#34328=CARTESIAN_POINT('Ctrl Pts',(84.7648942734634,-35.0536859391401,112.640922864614));
#34329=CARTESIAN_POINT('Ctrl Pts',(86.2290898398163,-33.0713463433522,112.528198311736));
#34330=CARTESIAN_POINT('Ctrl Pts',(89.6764928893144,-33.2708336798222,112.370249788544));
#34331=CARTESIAN_POINT('Ctrl Pts',(91.3940272155189,-36.2665737922834,112.212301265351));
#34332=CARTESIAN_POINT('Ctrl Pts',(89.8244566813072,-39.3424202320825,112.054352742159));
#34333=CARTESIAN_POINT('Ctrl Pts',(86.3908631537158,-39.7095965798975,111.896404218966));
#34334=CARTESIAN_POINT('Ctrl Pts',(84.7960899574643,-37.7571592451098,111.781094453973));
#34335=CARTESIAN_POINT('Ctrl Pts',(84.6919225723758,-36.5505847073844,111.71843419671));
#34336=CARTESIAN_POINT('Ctrl Pts',(84.6936554590675,-36.3575218684262,111.708423447177));
#34337=CARTESIAN_POINT('Ctrl Pts',(84.6968970266175,-36.35748207472,112.791576552823));
#34338=CARTESIAN_POINT('Ctrl Pts',(84.7025960788243,-35.6449587514818,112.754730079097));
#34339=CARTESIAN_POINT('Ctrl Pts',(85.3029473196868,-33.9056538204367,112.66523409764));
#34340=CARTESIAN_POINT('Ctrl Pts',(88.1888800917162,-32.7528191488601,112.523088608452));
#34341=CARTESIAN_POINT('Ctrl Pts',(91.0145611839512,-34.7377388042116,112.365140085259));
#34342=CARTESIAN_POINT('Ctrl Pts',(90.8971877256538,-38.1889129731724,112.207191562067));
#34343=CARTESIAN_POINT('Ctrl Pts',(87.9431786617096,-39.9772669994637,112.049243038874));
#34344=CARTESIAN_POINT('Ctrl Pts',(85.2133168410851,-38.6651863273541,111.91070470246));
#34345=CARTESIAN_POINT('Ctrl Pts',(84.702285414653,-36.9966107519078,111.824815873776));
#34346=CARTESIAN_POINT('Ctrl Pts',(84.6985185386966,-36.3529840193472,111.791576552823));
#34347=CARTESIAN_POINT('Origin',(87.7685555885722,-36.3549260746835,124.208423447177));
#34348=CARTESIAN_POINT('',(84.6901549196512,-36.3543571629991,113.791576552823));
#34349=CARTESIAN_POINT('',(84.6998103833004,-36.354472739616,113.708423447177));
#34350=CARTESIAN_POINT('',(84.6950555885722,-36.3549260746832,124.208423447177));
#34351=CARTESIAN_POINT('Ctrl Pts',(84.6998103833004,-36.354472739616,113.708423447177));
#34352=CARTESIAN_POINT('Ctrl Pts',(84.6991692065907,-35.8725545473769,113.683561622813));
#34353=CARTESIAN_POINT('Ctrl Pts',(85.0323509698878,-34.3709240683999,113.606050290717));
#34354=CARTESIAN_POINT('Ctrl Pts',(87.3713688180184,-32.7501940024069,113.475889450891));
#34355=CARTESIAN_POINT('Ctrl Pts',(90.5698543841637,-34.0517596235948,113.317940927699));
#34356=CARTESIAN_POINT('Ctrl Pts',(91.2284875299979,-37.4415362183437,113.159992404506));
#34357=CARTESIAN_POINT('Ctrl Pts',(88.7501056136147,-39.8461164435895,113.002043881314));
#34358=CARTESIAN_POINT('Ctrl Pts',(85.5401350753849,-39.1211064337822,112.851520895538));
#34359=CARTESIAN_POINT('Ctrl Pts',(84.6993188474424,-37.2238582627538,112.753647417492));
#34360=CARTESIAN_POINT('Ctrl Pts',(84.6922488060663,-36.3527237795464,112.708423447177));
#34361=CARTESIAN_POINT('Ctrl Pts',(84.6901549196511,-36.3543571629991,113.791576552823));
#34362=CARTESIAN_POINT('Ctrl Pts',(84.6900742363842,-36.32295282532,113.789943299879));
#34363=CARTESIAN_POINT('Ctrl Pts',(84.7046794034006,-35.2792757725774,113.735660539204));
#34364=CARTESIAN_POINT('Ctrl Pts',(85.8804608339871,-33.2586468252107,113.628728270799));
#34365=CARTESIAN_POINT('Ctrl Pts',(89.3290732451296,-33.0812993952069,113.470779747607));
#34366=CARTESIAN_POINT('Ctrl Pts',(91.3628117580707,-35.8720497126298,113.312831224414));
#34367=CARTESIAN_POINT('Ctrl Pts',(90.1377475164876,-39.100609341506,113.154882701222));
#34368=CARTESIAN_POINT('Ctrl Pts',(86.7646090095788,-39.8397414585361,112.996934178029));
#34369=CARTESIAN_POINT('Ctrl Pts',(84.876265246591,-37.9839423426147,112.875832128563));
#34370=CARTESIAN_POINT('Ctrl Pts',(84.6944527678673,-36.6630752337838,112.807379586827));
#34371=CARTESIAN_POINT('Ctrl Pts',(84.6968970266175,-36.35748207472,112.791576552823));
#34372=CARTESIAN_POINT('Origin',(87.7685555885722,-36.3549260746835,124.208423447177));
#34373=CARTESIAN_POINT('',(84.6983876365698,-36.3529100689715,114.791576552823));
#34374=CARTESIAN_POINT('',(84.6938496423748,-36.3575550147471,114.708423447177));
#34375=CARTESIAN_POINT('',(84.6950555885722,-36.3549260746832,124.208423447177));
#34376=CARTESIAN_POINT('Ctrl Pts',(84.6938496423747,-36.3575550147471,114.708423447177));
#34377=CARTESIAN_POINT('Ctrl Pts',(84.7012114735458,-35.5416795963333,114.666125335864));
#34378=CARTESIAN_POINT('Ctrl Pts',(85.4525661295013,-33.6982784575714,114.571177716821));
#34379=CARTESIAN_POINT('Ctrl Pts',(88.5561676812683,-32.8149376799226,114.423580590046));
#34380=CARTESIAN_POINT('Ctrl Pts',(91.1633294990928,-35.0792455739108,114.265632066854));
#34381=CARTESIAN_POINT('Ctrl Pts',(90.6925530596296,-38.5001741798809,114.107683543661));
#34382=CARTESIAN_POINT('Ctrl Pts',(87.5706770425218,-39.9760715736404,113.949735020469));
#34383=CARTESIAN_POINT('Ctrl Pts',(85.0913691036972,-38.4532614664624,113.816648321641));
#34384=CARTESIAN_POINT('Ctrl Pts',(84.7005270167674,-36.8931053812909,113.736211130544));
#34385=CARTESIAN_POINT('Ctrl Pts',(84.6998103833004,-36.354472739616,113.708423447177));
#34386=CARTESIAN_POINT('Ctrl Pts',(84.6983876365698,-36.3529100689715,114.791576552823));
#34387=CARTESIAN_POINT('Ctrl Pts',(84.6961381340608,-35.9836982647827,114.77250701293));
#34388=CARTESIAN_POINT('Ctrl Pts',(84.9280665202918,-34.5978523566551,114.700787965308));
#34389=CARTESIAN_POINT('Ctrl Pts',(86.9809436051873,-32.8149381712244,114.576419409954));
#34390=CARTESIAN_POINT('Ctrl Pts',(90.3022088923736,-33.7602299596934,114.418470886762));
#34391=CARTESIAN_POINT('Ctrl Pts',(91.3262877865851,-37.0580538015087,114.260522363569));
#34392=CARTESIAN_POINT('Ctrl Pts',(89.124679100392,-39.7183731180749,114.102573840377));
#34393=CARTESIAN_POINT('Ctrl Pts',(85.7289941295958,-39.3331819473256,113.946258570128));
#34394=CARTESIAN_POINT('Ctrl Pts',(84.6926751404897,-37.3353023979011,113.84259280761));
#34395=CARTESIAN_POINT('Ctrl Pts',(84.6901549196511,-36.3543571629991,113.791576552823));
#34396=CARTESIAN_POINT('Origin',(87.7685555885722,-36.3549260746835,124.208423447177));
#34397=CARTESIAN_POINT('',(84.6970698119725,-36.3574414495534,115.791576552823));
#34398=CARTESIAN_POINT('',(84.6920769038732,-36.3527935649553,115.708423447177));
#34399=CARTESIAN_POINT('',(84.6950555885722,-36.3549260746832,124.208423447177));
#34400=CARTESIAN_POINT('Ctrl Pts',(84.6920769038732,-36.3527935649552,115.708423447177));
#34401=CARTESIAN_POINT('Ctrl Pts',(84.6909943683417,-36.2163395637745,115.701338556647));
#34402=CARTESIAN_POINT('Ctrl Pts',(84.7609870881033,-35.0669804686883,115.641604158386));
#34403=CARTESIAN_POINT('Ctrl Pts',(86.2080377154374,-33.0812989408716,115.529220252393));
#34404=CARTESIAN_POINT('Ctrl Pts',(89.6566506052006,-33.2586463954901,115.371271729201));
#34405=CARTESIAN_POINT('Ctrl Pts',(91.3933851672007,-36.2432964661436,115.213323206008));
#34406=CARTESIAN_POINT('Ctrl Pts',(89.8435969944667,-39.3291577077992,115.055374682816));
#34407=CARTESIAN_POINT('Ctrl Pts',(86.4124318885398,-39.718373584875,114.897426159624));
#34408=CARTESIAN_POINT('Ctrl Pts',(84.8004067708206,-37.7704790356049,114.781775747744));
#34409=CARTESIAN_POINT('Ctrl Pts',(84.6920480197858,-36.557219955365,114.718774843595));
#34410=CARTESIAN_POINT('Ctrl Pts',(84.6938496423747,-36.3575550147471,114.708423447177));
#34411=CARTESIAN_POINT('Ctrl Pts',(84.6970698119725,-36.3574414495534,115.791576552823));
#34412=CARTESIAN_POINT('Ctrl Pts',(84.7026034041402,-35.6514048376539,115.755070725982));
#34413=CARTESIAN_POINT('Ctrl Pts',(85.2941695333478,-33.9187288980288,115.665915391411));
#34414=CARTESIAN_POINT('Ctrl Pts',(88.1657423040033,-32.7501945026947,115.524110549109));
#34415=CARTESIAN_POINT('Ctrl Pts',(91.0041103112496,-34.7169295455148,115.366162025916));
#34416=CARTESIAN_POINT('Ctrl Pts',(90.9088992563929,-38.1687862239197,115.208213502724));
#34417=CARTESIAN_POINT('Ctrl Pts',(87.9664341071585,-39.9760710710749,115.050264979531));
#34418=CARTESIAN_POINT('Ctrl Pts',(85.2214707589106,-38.678362824672,114.911385996231));
#34419=CARTESIAN_POINT('Ctrl Pts',(84.7023488344975,-37.0030631707532,114.825156520661));
#34420=CARTESIAN_POINT('Ctrl Pts',(84.6983876365698,-36.3529100689715,114.791576552823));
#34421=CARTESIAN_POINT('Origin',(87.7685555885722,-36.3549260746835,124.208423447177));
#34422=CARTESIAN_POINT('',(84.6901060143961,-36.3544743326999,116.791576552823));
#34423=CARTESIAN_POINT('',(84.6997777386867,-36.354368481064,116.708423447177));
#34424=CARTESIAN_POINT('',(84.6950555885722,-36.3549260746832,124.208423447177));
#34425=CARTESIAN_POINT('Ctrl Pts',(84.6997777386867,-36.354368481064,116.708423447177));
#34426=CARTESIAN_POINT('Ctrl Pts',(84.6989994340679,-35.8790659799677,116.683902269698));
#34427=CARTESIAN_POINT('Ctrl Pts',(85.025762237394,-34.3842532656316,116.606731584489));
#34428=CARTESIAN_POINT('Ctrl Pts',(87.3482310270943,-32.7528186489366,116.476911391548));
#34429=CARTESIAN_POINT('Ctrl Pts',(90.5550080077946,-34.0338199678859,116.318962868355));
#34430=CARTESIAN_POINT('Ctrl Pts',(91.2353933261053,-37.4192976006176,116.161014345163));
#34431=CARTESIAN_POINT('Ctrl Pts',(88.7725023068986,-39.8397419421814,116.003065821971));
#34432=CARTESIAN_POINT('Ctrl Pts',(85.5506678195318,-39.1337640107994,115.852202189309));
#34433=CARTESIAN_POINT('Ctrl Pts',(84.699038947519,-37.2303617224901,115.753988064378));
#34434=CARTESIAN_POINT('Ctrl Pts',(84.6920769038732,-36.3527935649552,115.708423447177));
#34435=CARTESIAN_POINT('Ctrl Pts',(84.6901060143962,-36.3544743326999,116.791576552823));
#34436=CARTESIAN_POINT('Ctrl Pts',(84.6900545271454,-36.3296210455818,116.790283946765));
#34437=CARTESIAN_POINT('Ctrl Pts',(84.7015400140162,-35.2925101923577,116.736341832976));
#34438=CARTESIAN_POINT('Ctrl Pts',(85.860618552627,-33.2708341078515,116.629750211456));
#34439=CARTESIAN_POINT('Ctrl Pts',(89.3080211236725,-33.0713467990688,116.471801688264));
#34440=CARTESIAN_POINT('Ctrl Pts',(91.3596371147702,-35.8489809539364,116.313853165071));
#34441=CARTESIAN_POINT('Ctrl Pts',(90.1553287038718,-39.0853401621602,116.155904641879));
#34442=CARTESIAN_POINT('Ctrl Pts',(86.7870056997543,-39.8461159590596,115.997956118686));
#34443=CARTESIAN_POINT('Ctrl Pts',(84.8814396668467,-37.997294205502,115.876513422334));
#34444=CARTESIAN_POINT('Ctrl Pts',(84.6946227356051,-36.6696663940604,115.807720233713));
#34445=CARTESIAN_POINT('Ctrl Pts',(84.6970698119725,-36.3574414495534,115.791576552823));
#34446=CARTESIAN_POINT('Origin',(87.7685555885722,-36.3549260746835,124.208423447177));
#34447=CARTESIAN_POINT('',(84.6982515989598,-36.3528391397487,117.791576552823));
#34448=CARTESIAN_POINT('',(84.6940448454532,-36.3575836913029,117.708423447177));
#34449=CARTESIAN_POINT('',(84.6950555885722,-36.3549260746832,124.208423447177));
#34450=CARTESIAN_POINT('Ctrl Pts',(84.6940448454532,-36.3575836913029,117.708423447177));
#34451=CARTESIAN_POINT('Ctrl Pts',(84.7013752637221,-35.5481464691242,117.66646598275));
#34452=CARTESIAN_POINT('Ctrl Pts',(85.4427052641639,-33.7111195302489,117.571859010592));
#34453=CARTESIAN_POINT('Ctrl Pts',(88.5334211849751,-32.8099534001692,117.424602530703));
#34454=CARTESIAN_POINT('Ctrl Pts',(91.1550683739797,-35.0574740340002,117.26665400751));
#34455=CARTESIAN_POINT('Ctrl Pts',(90.7062674165854,-38.4813549728958,117.108705484318));
#34456=CARTESIAN_POINT('Ctrl Pts',(87.5939324911983,-39.9772675021952,116.950756961125));
#34457=CARTESIAN_POINT('Ctrl Pts',(85.0985268023629,-38.4665514839768,116.817329615412));
#34458=CARTESIAN_POINT('Ctrl Pts',(84.7006705346943,-36.8995896773883,116.736551777429));
#34459=CARTESIAN_POINT('Ctrl Pts',(84.6997777386867,-36.354368481064,116.708423447177));
#34460=CARTESIAN_POINT('Ctrl Pts',(84.6982515989598,-36.3528391397487,117.791576552823));
#34461=CARTESIAN_POINT('Ctrl Pts',(84.6959579671254,-35.9902631438032,117.772847659816));
#34462=CARTESIAN_POINT('Ctrl Pts',(84.9224342902478,-34.6112079283206,117.701469259079));
#34463=CARTESIAN_POINT('Ctrl Pts',(86.9582295850041,-32.8200684027204,117.577441350611));
#34464=CARTESIAN_POINT('Ctrl Pts',(90.2854961219689,-33.7440148650956,117.419492827418));
#34465=CARTESIAN_POINT('Ctrl Pts',(91.3307292265714,-37.0351951139114,117.261544304226));
#34466=CARTESIAN_POINT('Ctrl Pts',(89.1462478322224,-39.7095961143156,117.103595781033));
#34467=CARTESIAN_POINT('Ctrl Pts',(85.740754335939,-39.3454246844624,116.946939863899));
#34468=CARTESIAN_POINT('Ctrl Pts',(84.6921516691098,-37.3419274046254,116.842933454495));
#34469=CARTESIAN_POINT('Ctrl Pts',(84.6901060143962,-36.3544743326999,116.791576552823));
#34470=CARTESIAN_POINT('Origin',(87.7685555885722,-36.3549260746835,124.208423447177));
#34471=CARTESIAN_POINT('',(84.6972390699959,-36.357396938615,118.791576552823));
#34472=CARTESIAN_POINT('',(84.6919092441355,-36.3528672805194,118.708423447177));
#34473=CARTESIAN_POINT('',(84.6950555885722,-36.3549260746832,124.208423447177));
#34474=CARTESIAN_POINT('Ctrl Pts',(84.6919092441355,-36.3528672805194,118.708423447177));
#34475=CARTESIAN_POINT('Ctrl Pts',(84.6909048090706,-36.2229926069874,118.701679203533));
#34476=CARTESIAN_POINT('Ctrl Pts',(84.7571266102654,-35.0802717724924,118.642285452157));
#34477=CARTESIAN_POINT('Ctrl Pts',(86.1870499307028,-33.0913865091248,118.53024219305));
#34478=CARTESIAN_POINT('Ctrl Pts',(89.6367304755765,-33.2465867695503,118.372293669858));
#34479=CARTESIAN_POINT('Ctrl Pts',(91.3925936684549,-36.2200237425119,118.214345146665));
#34480=CARTESIAN_POINT('Ctrl Pts',(89.8626517544002,-39.3157725569713,118.056396623473));
#34481=CARTESIAN_POINT('Ctrl Pts',(86.4340565358644,-39.7270119161192,117.89844810028));
#34482=CARTESIAN_POINT('Ctrl Pts',(84.8047722789476,-37.7838014397254,117.782457041515));
#34483=CARTESIAN_POINT('Ctrl Pts',(84.6921768310097,-36.5638530154645,117.719115490481));
#34484=CARTESIAN_POINT('Ctrl Pts',(84.6940448454532,-36.3575836913029,117.708423447177));
#34485=CARTESIAN_POINT('Ctrl Pts',(84.6972390699959,-36.357396938615,118.791576552823));
#34486=CARTESIAN_POINT('Ctrl Pts',(84.702602542751,-35.6578510145562,118.755411372868));
#34487=CARTESIAN_POINT('Ctrl Pts',(85.2854577178621,-33.9318158343519,118.666596685182));
#34488=CARTESIAN_POINT('Ctrl Pts',(88.1425881396678,-32.7477184775748,118.525132489766));
#34489=CARTESIAN_POINT('Ctrl Pts',(90.9935260381413,-34.6961878212031,118.367183966573));
#34490=CARTESIAN_POINT('Ctrl Pts',(90.9204813116975,-38.1485846896768,118.209235443381));
#34491=CARTESIAN_POINT('Ctrl Pts',(87.9896813942331,-39.9747258442494,118.051286920188));
#34492=CARTESIAN_POINT('Ctrl Pts',(85.2296888152546,-38.6915299918233,117.912067290002));
#34493=CARTESIAN_POINT('Ctrl Pts',(84.7024056833334,-37.0095143988034,117.825497167547));
#34494=CARTESIAN_POINT('Ctrl Pts',(84.6982515989598,-36.3528391397487,117.791576552823));
#34495=CARTESIAN_POINT('Origin',(87.7685555885722,-36.3549260746835,124.208423447177));
#34496=CARTESIAN_POINT('',(84.6900677844821,-36.3545924748475,119.791576552823));
#34497=CARTESIAN_POINT('',(84.6997383656671,-36.3542650492571,119.708423447177));
#34498=CARTESIAN_POINT('',(84.6950555885722,-36.3549260746832,124.208423447177));
#34499=CARTESIAN_POINT('Ctrl Pts',(84.6997383656671,-36.3542650492571,119.708423447177));
#34500=CARTESIAN_POINT('Ctrl Pts',(84.6988278125906,-35.8855804513753,119.684242916584));
#34501=CARTESIAN_POINT('Ctrl Pts',(85.0192316092183,-34.3975854238898,119.60741287826));
#34502=CARTESIAN_POINT('Ctrl Pts',(87.3251105694465,-32.7555918278425,119.477933332205));
#34503=CARTESIAN_POINT('Ctrl Pts',(90.540046745306,-34.0159760014353,119.319984809013));
#34504=CARTESIAN_POINT('Ctrl Pts',(91.2421561865363,-37.3970151036668,119.16203628582));
#34505=CARTESIAN_POINT('Ctrl Pts',(88.7948576074191,-39.8332237608939,119.004087762628));
#34506=CARTESIAN_POINT('Ctrl Pts',(85.5612715353611,-39.1464004416207,118.85288348308));
#34507=CARTESIAN_POINT('Ctrl Pts',(84.698746016254,-37.2368702170138,118.754328711263));
#34508=CARTESIAN_POINT('Ctrl Pts',(84.6919092441355,-36.3528672805194,118.708423447177));
#34509=CARTESIAN_POINT('Ctrl Pts',(84.6900677844821,-36.3545924748475,119.791576552823));
#34510=CARTESIAN_POINT('Ctrl Pts',(84.690039339652,-36.3362895074741,119.79062459365));
#34511=CARTESIAN_POINT('Ctrl Pts',(84.6984439817714,-35.3057407212815,119.737023126747));
#34512=CARTESIAN_POINT('Ctrl Pts',(85.8408550522478,-33.2831486644916,119.630772152113));
#34513=CARTESIAN_POINT('Ctrl Pts',(89.2869054734986,-33.0615295263651,119.472823628921));
#34514=CARTESIAN_POINT('Ctrl Pts',(91.3563144402191,-35.8259330830824,119.314875105728));
#34515=CARTESIAN_POINT('Ctrl Pts',(90.1728114719436,-39.0699583952412,119.156926582536));
#34516=CARTESIAN_POINT('Ctrl Pts',(86.8094428654503,-39.8523465256606,118.998978059343));
#34517=CARTESIAN_POINT('Ctrl Pts',(84.8866665229963,-38.0106469951155,118.877194716105));
#34518=CARTESIAN_POINT('Ctrl Pts',(84.694794363706,-36.6762545890117,118.808060880599));
#34519=CARTESIAN_POINT('Ctrl Pts',(84.6972390699959,-36.357396938615,118.791576552823));
#34520=CARTESIAN_POINT('Origin',(87.7685555885722,-36.3549260746835,124.208423447177));
#34521=CARTESIAN_POINT('',(84.69811441609,-36.3527751945784,120.791576552823));
#34522=CARTESIAN_POINT('',(84.6942411071791,-36.3576097921547,120.708423447177));
#34523=CARTESIAN_POINT('',(84.6950555885722,-36.3549260746832,124.208423447177));
#34524=CARTESIAN_POINT('Ctrl Pts',(84.6942411071791,-36.3576097921547,120.708423447177));
#34525=CARTESIAN_POINT('Ctrl Pts',(84.701528235602,-35.5546125488608,120.666806629636));
#34526=CARTESIAN_POINT('Ctrl Pts',(85.4329130412516,-33.7239751716799,120.572540304363));
#34527=CARTESIAN_POINT('Ctrl Pts',(88.5106434141715,-32.8051166986153,120.42562447136));
#34528=CARTESIAN_POINT('Ctrl Pts',(91.1466674974244,-35.0357552970371,120.267675948167));
#34529=CARTESIAN_POINT('Ctrl Pts',(90.7198607143381,-38.4624484297529,120.109727424975));
#34530=CARTESIAN_POINT('Ctrl Pts',(87.6171951095654,-39.9783139196497,119.951778901782));
#34531=CARTESIAN_POINT('Ctrl Pts',(85.105745062361,-38.4798362972224,119.818010909183));
#34532=CARTESIAN_POINT('Ctrl Pts',(84.7008104064405,-36.9060714312672,119.736892424315));
#34533=CARTESIAN_POINT('Ctrl Pts',(84.6997383656671,-36.3542650492571,119.708423447177));
#34534=CARTESIAN_POINT('Ctrl Pts',(84.69811441609,-36.3527751945784,120.791576552823));
#34535=CARTESIAN_POINT('Ctrl Pts',(84.6957790852043,-35.9968317519122,120.773188306702));
#34536=CARTESIAN_POINT('Ctrl Pts',(84.9168438604484,-34.6245511594877,120.70215055285));
#34537=CARTESIAN_POINT('Ctrl Pts',(86.935557851387,-32.8253532951761,120.578463291268));
#34538=CARTESIAN_POINT('Ctrl Pts',(90.2686752620247,-33.7279030795955,120.420514768075));
#34539=CARTESIAN_POINT('Ctrl Pts',(91.3350258987628,-37.0123104885738,120.262566244883));
#34540=CARTESIAN_POINT('Ctrl Pts',(89.167758741363,-39.7006797728369,120.10461772169));
#34541=CARTESIAN_POINT('Ctrl Pts',(85.7525884657271,-39.3576397118412,119.94762115767));
#34542=CARTESIAN_POINT('Ctrl Pts',(84.6916125229857,-37.3485621449868,119.843274101381));
#34543=CARTESIAN_POINT('Ctrl Pts',(84.6900677844821,-36.3545924748475,119.791576552823));
#34544=CARTESIAN_POINT('Origin',(87.7685555885722,-36.3549260746835,124.208423447177));
#34545=CARTESIAN_POINT('',(84.6982768768212,-36.3579423122256,121.791576552823));
#34546=CARTESIAN_POINT('',(84.691755941294,-36.3529984690253,121.708423447177));
#34547=CARTESIAN_POINT('',(84.6950555885722,-36.3549260746832,124.208423447177));
#34548=CARTESIAN_POINT('',(86.9747563060389,-39.3241490284291,122.));
#34549=CARTESIAN_POINT('Ctrl Pts',(86.9747563060389,-39.3241490284291,122.));
#34550=CARTESIAN_POINT('Ctrl Pts',(85.9925177162673,-39.0615549760513,121.947350492269));
#34551=CARTESIAN_POINT('Ctrl Pts',(84.8928208152446,-38.023819855789,121.877876009877));
#34552=CARTESIAN_POINT('Ctrl Pts',(84.6959356655866,-36.6834182514038,121.808401527484));
#34553=CARTESIAN_POINT('Ctrl Pts',(84.6982768768212,-36.3579423122256,121.791576552823));
#34554=CARTESIAN_POINT('',(88.5642643959444,-39.3292255199611,122.));
#34555=CARTESIAN_POINT('Origin',(87.7685555885722,-36.3549260746835,122.));
#34556=CARTESIAN_POINT('Ctrl Pts',(88.5642690312351,-39.3292378429293,122.));
#34557=CARTESIAN_POINT('Ctrl Pts',(87.6173028025204,-39.5801183881388,121.949053726697));
#34558=CARTESIAN_POINT('Ctrl Pts',(85.5567536487794,-39.1252166604105,121.851861542423));
#34559=CARTESIAN_POINT('Ctrl Pts',(84.698419406197,-37.2432732269655,121.754669358149));
#34560=CARTESIAN_POINT('Ctrl Pts',(84.691755941294,-36.3529984690253,121.708423447177));
#34561=CARTESIAN_POINT('Origin',(36.3549260746835,87.7685555885722,114.));
#34562=CARTESIAN_POINT('',(33.8414156476497,87.7688130130942,107.387416697508));
#34563=CARTESIAN_POINT('',(33.8393353393333,87.7649829964101,107.112583302492));
#34564=CARTESIAN_POINT('',(33.8374260746835,87.7685555885722,114.));
#34565=CARTESIAN_POINT('',(34.4414600780189,89.4045427919477,107.));
#34566=CARTESIAN_POINT('Ctrl Pts',(33.8393353393333,87.7649829964101,107.112583302492));
#34567=CARTESIAN_POINT('Ctrl Pts',(33.844480764459,88.3576176201294,107.075055534995));
#34568=CARTESIAN_POINT('Ctrl Pts',(34.0557042465997,88.9533591488772,107.037527767497));
#34569=CARTESIAN_POINT('Ctrl Pts',(34.441460078019,89.4045427919478,107.));
#34570=CARTESIAN_POINT('',(33.8374260746835,87.7685555885722,107.));
#34571=CARTESIAN_POINT('Origin',(36.3549260746835,87.7685555885722,107.));
#34572=CARTESIAN_POINT('',(33.8374260746835,87.7685555885722,106.));
#34573=CARTESIAN_POINT('',(33.8374260746835,87.7685555885722,114.));
#34574=CARTESIAN_POINT('Origin',(36.3549260746835,87.7685555885722,106.));
#34575=CARTESIAN_POINT('',(38.2720364380598,89.4070835930084,107.));
#34576=CARTESIAN_POINT('Origin',(36.3549260746835,87.7685555885722,107.));
#34577=CARTESIAN_POINT('Ctrl Pts',(38.2720452848186,89.4070897608439,107.));
#34578=CARTESIAN_POINT('Ctrl Pts',(37.7492247595626,90.0158046540078,107.050946273303));
#34579=CARTESIAN_POINT('Ctrl Pts',(36.9095001729433,90.355981333293,107.101892546605));
#34580=CARTESIAN_POINT('Ctrl Pts',(36.1108292450109,90.2782186082904,107.152838819908));
#34581=CARTESIAN_POINT('Ctrl Pts',(35.2854571722635,90.1978561219734,107.205488327639));
#34582=CARTESIAN_POINT('Ctrl Pts',(34.5039296533554,89.6711420241569,107.25813783537));
#34583=CARTESIAN_POINT('Ctrl Pts',(34.1200450165566,88.9363551677885,107.3107873431));
#34584=CARTESIAN_POINT('Ctrl Pts',(33.933801857771,88.5798704011529,107.336330461236));
#34585=CARTESIAN_POINT('Ctrl Pts',(33.8411536469158,88.1744106374066,107.361873579372));
#34586=CARTESIAN_POINT('Ctrl Pts',(33.8414156476497,87.7688130130942,107.387416697508));
#34587=CARTESIAN_POINT('Origin',(36.3549260746835,87.7685555885722,114.));
#34588=CARTESIAN_POINT('',(33.8361211319563,87.7664601065544,108.387416697508));
#34589=CARTESIAN_POINT('',(33.8335191542225,87.7692219086659,108.112583302492));
#34590=CARTESIAN_POINT('',(33.8374260746835,87.7685555885722,114.));
#34591=CARTESIAN_POINT('Ctrl Pts',(33.8335191542225,87.7692219086659,108.112583302492));
#34592=CARTESIAN_POINT('Ctrl Pts',(33.8333913183595,87.8056790435099,108.110268755777));
#34593=CARTESIAN_POINT('Ctrl Pts',(33.834114269325,87.8421309416024,108.107954209062));
#34594=CARTESIAN_POINT('Ctrl Pts',(33.8357038858111,87.8785449414407,108.105639662347));
#34595=CARTESIAN_POINT('Ctrl Pts',(33.8718632447615,88.7068622761646,108.052990154616));
#34596=CARTESIAN_POINT('Ctrl Pts',(34.3564666344665,89.5155696857969,108.000340646886));
#34597=CARTESIAN_POINT('Ctrl Pts',(35.0698410055614,89.938131343294,107.947691139155));
#34598=CARTESIAN_POINT('Ctrl Pts',(35.7832153766562,90.3606930007911,107.895041631424));
#34599=CARTESIAN_POINT('Ctrl Pts',(36.725360729141,90.3971089061531,107.842392123693));
#34600=CARTESIAN_POINT('Ctrl Pts',(37.4691399227335,90.0307072168534,107.789742615962));
#34601=CARTESIAN_POINT('Ctrl Pts',(38.212919116326,89.6643055275537,107.737093108231));
#34602=CARTESIAN_POINT('Ctrl Pts',(38.7583321510263,88.8950862435923,107.684443600501));
#34603=CARTESIAN_POINT('Ctrl Pts',(38.8581857832189,88.0720989400536,107.63179409277));
#34604=CARTESIAN_POINT('Ctrl Pts',(38.9580394154116,87.2491116365149,107.579144585039));
#34605=CARTESIAN_POINT('Ctrl Pts',(38.6123336450968,86.3723563133988,107.526495077308));
#34606=CARTESIAN_POINT('Ctrl Pts',(37.9776637412943,85.8386044103528,107.473845569577));
#34607=CARTESIAN_POINT('Ctrl Pts',(37.3429938374919,85.3048525073067,107.421196061847));
#34608=CARTESIAN_POINT('Ctrl Pts',(36.4193598002019,85.1141040243308,107.368546554116));
#34609=CARTESIAN_POINT('Ctrl Pts',(35.625742673972,85.3542580662575,107.315897046385));
#34610=CARTESIAN_POINT('Ctrl Pts',(34.8321255477422,85.5944121081842,107.263247538654));
#34611=CARTESIAN_POINT('Ctrl Pts',(34.1685253325724,86.2654686750135,107.210598030923));
#34612=CARTESIAN_POINT('Ctrl Pts',(33.9355601185611,87.0597545443991,107.157948523192));
#34613=CARTESIAN_POINT('Ctrl Pts',(33.8686489620936,87.2878855394576,107.142826782959));
#34614=CARTESIAN_POINT('Ctrl Pts',(33.8372620003811,87.5261820383226,107.127705042725));
#34615=CARTESIAN_POINT('Ctrl Pts',(33.8393353393333,87.7649829964101,107.112583302492));
#34616=CARTESIAN_POINT('Ctrl Pts',(33.8414156476497,87.7688130130942,107.387416697508));
#34617=CARTESIAN_POINT('Ctrl Pts',(33.8416936831633,87.3383922960573,107.414523087103));
#34618=CARTESIAN_POINT('Ctrl Pts',(33.9466023816844,86.9078163275987,107.441629476698));
#34619=CARTESIAN_POINT('Ctrl Pts',(34.1553234354522,86.5354488974857,107.468735866293));
#34620=CARTESIAN_POINT('Ctrl Pts',(34.5607282458358,85.8121890984717,107.521385374024));
#34621=CARTESIAN_POINT('Ctrl Pts',(35.3577796212926,85.3085291153642,107.574034881755));
#34622=CARTESIAN_POINT('Ctrl Pts',(36.1850293919425,85.2526781151853,107.626684389485));
#34623=CARTESIAN_POINT('Ctrl Pts',(37.0122791625924,85.1968271150065,107.679333897216));
#34624=CARTESIAN_POINT('Ctrl Pts',(37.8697273284356,85.5887850977564,107.731983404947));
#34625=CARTESIAN_POINT('Ctrl Pts',(38.3687197115474,86.2509209612129,107.784632912678));
#34626=CARTESIAN_POINT('Ctrl Pts',(38.8677120946593,86.9130568246694,107.837282420409));
#34627=CARTESIAN_POINT('Ctrl Pts',(39.0082486950399,87.8453705688325,107.889931928139));
#34628=CARTESIAN_POINT('Ctrl Pts',(38.7265917130798,88.625184178848,107.94258143587));
#34629=CARTESIAN_POINT('Ctrl Pts',(38.4449347311198,89.4049977888636,107.995230943601));
#34630=CARTESIAN_POINT('Ctrl Pts',(37.7410841668192,90.0323112647315,108.047880451332));
#34631=CARTESIAN_POINT('Ctrl Pts',(36.9341334227374,90.2227550766996,108.100529959063));
#34632=CARTESIAN_POINT('Ctrl Pts',(36.1271826786556,90.4131988886677,108.153179466794));
#34633=CARTESIAN_POINT('Ctrl Pts',(35.2171317547927,90.1667730367359,108.205828974524));
#34634=CARTESIAN_POINT('Ctrl Pts',(34.6165318579143,89.5951843722506,108.258478482255));
#34635=CARTESIAN_POINT('Ctrl Pts',(34.1262437740546,89.1285790456046,108.301457887339));
#34636=CARTESIAN_POINT('Ctrl Pts',(33.842172516144,88.4452866270629,108.344437292424));
#34637=CARTESIAN_POINT('Ctrl Pts',(33.8361211319563,87.7664601065544,108.387416697508));
#34638=CARTESIAN_POINT('Origin',(36.3549260746835,87.7685555885722,114.));
#34639=CARTESIAN_POINT('',(33.8352709498557,87.7704133466358,109.387416697508));
#34640=CARTESIAN_POINT('',(33.8403653828405,87.7700835309277,109.112583302492));
#34641=CARTESIAN_POINT('',(33.8374260746835,87.7685555885722,114.));
#34642=CARTESIAN_POINT('Ctrl Pts',(33.8403653828405,87.7700835309277,109.112583302492));
#34643=CARTESIAN_POINT('Ctrl Pts',(33.8386091275561,88.0833748401921,109.092832468829));
#34644=CARTESIAN_POINT('Ctrl Pts',(33.8929063186919,88.3960793297297,109.073081635165));
#34645=CARTESIAN_POINT('Ctrl Pts',(34.0060458881645,88.6858055038443,109.053330801502));
#34646=CARTESIAN_POINT('Ctrl Pts',(34.3076403797772,89.4581243185282,109.000681293771));
#34647=CARTESIAN_POINT('Ctrl Pts',(35.0273616523211,90.0671620196572,108.94803178604));
#34648=CARTESIAN_POINT('Ctrl Pts',(35.8389352036457,90.2368216765074,108.89538227831));
#34649=CARTESIAN_POINT('Ctrl Pts',(36.6505087549703,90.4064813333576,108.842732770579));
#34650=CARTESIAN_POINT('Ctrl Pts',(37.5539345850756,90.136762945929,108.790083262848));
#34651=CARTESIAN_POINT('Ctrl Pts',(38.1396579370872,89.5499370852442,108.737433755117));
#34652=CARTESIAN_POINT('Ctrl Pts',(38.7253812890987,88.9631112245596,108.684784247386));
#34653=CARTESIAN_POINT('Ctrl Pts',(38.9934021630165,88.0591778906187,108.632134739655));
#34654=CARTESIAN_POINT('Ctrl Pts',(38.8222181837362,87.247925952964,108.579485231925));
#34655=CARTESIAN_POINT('Ctrl Pts',(38.6510342044558,86.4366740153094,108.526835724194));
#34656=CARTESIAN_POINT('Ctrl Pts',(38.0406453719773,85.7181034739408,108.474186216463));
#34657=CARTESIAN_POINT('Ctrl Pts',(37.2677605108997,85.4179582290087,108.421536708732));
#34658=CARTESIAN_POINT('Ctrl Pts',(36.4948756498221,85.1178129840766,108.368887201001));
#34659=CARTESIAN_POINT('Ctrl Pts',(35.5594947601453,85.236093035581,108.316237693271));
#34660=CARTESIAN_POINT('Ctrl Pts',(34.8856619794049,85.7191966912411,108.26358818554));
#34661=CARTESIAN_POINT('Ctrl Pts',(34.2414518393365,86.1810624279278,108.213253224524));
#34662=CARTESIAN_POINT('Ctrl Pts',(33.8362992291002,86.9763805072392,108.162918263508));
#34663=CARTESIAN_POINT('Ctrl Pts',(33.8335191542225,87.7692219086659,108.112583302492));
#34664=CARTESIAN_POINT('Ctrl Pts',(33.8361211319563,87.7664601065544,108.387416697508));
#34665=CARTESIAN_POINT('Ctrl Pts',(33.8347596076138,87.6137283011781,108.397086800155));
#34666=CARTESIAN_POINT('Ctrl Pts',(33.8474720723731,87.4612225695691,108.406756902801));
#34667=CARTESIAN_POINT('Ctrl Pts',(33.8750763409706,87.3114617765907,108.416427005448));
#34668=CARTESIAN_POINT('Ctrl Pts',(34.0253695907989,86.4960793224549,108.469076513179));
#34669=CARTESIAN_POINT('Ctrl Pts',(34.6171049603491,85.7620658912221,108.521726020909));
#34670=CARTESIAN_POINT('Ctrl Pts',(35.3820266721296,85.4421737589331,108.57437552864));
#34671=CARTESIAN_POINT('Ctrl Pts',(36.1469483839101,85.1222816266441,108.627025036371));
#34672=CARTESIAN_POINT('Ctrl Pts',(37.0850564379207,85.2165107932989,108.679674544102));
#34673=CARTESIAN_POINT('Ctrl Pts',(37.7710745652258,85.6821446532133,108.732324051833));
#34674=CARTESIAN_POINT('Ctrl Pts',(38.4570926925308,86.1477785131277,108.784973559563));
#34675=CARTESIAN_POINT('Ctrl Pts',(38.8910208931303,86.9848170663018,108.837623067294));
#34676=CARTESIAN_POINT('Ctrl Pts',(38.8761440504648,87.8138012467044,108.890272575025));
#34677=CARTESIAN_POINT('Ctrl Pts',(38.8612672077993,88.642785427107,108.942922082756));
#34678=CARTESIAN_POINT('Ctrl Pts',(38.397585321869,89.4637152347382,108.995571590487));
#34679=CARTESIAN_POINT('Ctrl Pts',(37.6953017022331,89.9044348032924,109.048221098218));
#34680=CARTESIAN_POINT('Ctrl Pts',(36.9930180825973,90.3451543718466,109.100870605948));
#34681=CARTESIAN_POINT('Ctrl Pts',(36.052132729256,90.4056637013238,109.153520113679));
#34682=CARTESIAN_POINT('Ctrl Pts',(35.2991816228838,90.0585317206909,109.20616962141));
#34683=CARTESIAN_POINT('Ctrl Pts',(34.5462305165115,89.711399740058,109.258819129141));
#34684=CARTESIAN_POINT('Ctrl Pts',(33.9812136571084,88.9566264493151,109.311468636872));
#34685=CARTESIAN_POINT('Ctrl Pts',(33.8602728877845,88.1363768842624,109.364118144603));
#34686=CARTESIAN_POINT('Ctrl Pts',(33.8424332470232,88.0153841234512,109.371884328904));
#34687=CARTESIAN_POINT('Ctrl Pts',(33.834255986992,87.8929667043318,109.379650513206));
#34688=CARTESIAN_POINT('Ctrl Pts',(33.8352709498557,87.7704133466358,109.387416697508));
#34689=CARTESIAN_POINT('Origin',(36.3549260746835,87.7685555885722,114.));
#34690=CARTESIAN_POINT('',(33.8413418417317,87.7688409760013,110.387416697508));
#34691=CARTESIAN_POINT('',(33.8387900496171,87.766431943684,110.112583302492));
#34692=CARTESIAN_POINT('',(33.8374260746835,87.7685555885722,114.));
#34693=CARTESIAN_POINT('Ctrl Pts',(33.8387900496171,87.766431943684,110.112583302492));
#34694=CARTESIAN_POINT('Ctrl Pts',(33.8435895140767,88.3553689856135,110.07539618188));
#34695=CARTESIAN_POINT('Ctrl Pts',(34.0501480074608,88.947339605864,110.038209061269));
#34696=CARTESIAN_POINT('Ctrl Pts',(34.4278435299873,89.3948822083208,110.001021940657));
#34697=CARTESIAN_POINT('Ctrl Pts',(34.9625846717064,90.0285128126893,109.948372432926));
#34698=CARTESIAN_POINT('Ctrl Pts',(35.8403679856063,90.3726391455629,109.895722925195));
#34699=CARTESIAN_POINT('Ctrl Pts',(36.6632637571565,90.2712567808753,109.843073417464));
#34700=CARTESIAN_POINT('Ctrl Pts',(37.4861595287068,90.1698744161876,109.790423909734));
#34701=CARTESIAN_POINT('Ctrl Pts',(38.2541677579075,89.6229833539386,109.737774402003));
#34702=CARTESIAN_POINT('Ctrl Pts',(38.6191235877846,88.8785083121911,109.685124894272));
#34703=CARTESIAN_POINT('Ctrl Pts',(38.9840794176617,88.1340332704436,109.632475386541));
#34704=CARTESIAN_POINT('Ctrl Pts',(38.9459828482152,87.1919742491975,109.57982587881));
#34705=CARTESIAN_POINT('Ctrl Pts',(38.5221043906172,86.4793994387067,109.527176371079));
#34706=CARTESIAN_POINT('Ctrl Pts',(38.0982259330193,85.7668246282158,109.474526863349));
#34707=CARTESIAN_POINT('Ctrl Pts',(37.2885655872697,85.2837340284801,109.421877355618));
#34708=CARTESIAN_POINT('Ctrl Pts',(36.4601705366731,85.2491292959353,109.369227847887));
#34709=CARTESIAN_POINT('Ctrl Pts',(35.6317754860765,85.2145245633906,109.316578340156));
#34710=CARTESIAN_POINT('Ctrl Pts',(34.7846457306328,85.6284056980367,109.263928832425));
#34711=CARTESIAN_POINT('Ctrl Pts',(34.3028147082516,86.3031462294792,109.211279324695));
#34712=CARTESIAN_POINT('Ctrl Pts',(34.0017368360334,86.724765913704,109.178380650627));
#34713=CARTESIAN_POINT('Ctrl Pts',(33.8432907515194,87.2482387902261,109.14548197656));
#34714=CARTESIAN_POINT('Ctrl Pts',(33.8403653828405,87.7700835309277,109.112583302492));
#34715=CARTESIAN_POINT('Ctrl Pts',(33.8352709498557,87.7704133466358,109.387416697508));
#34716=CARTESIAN_POINT('Ctrl Pts',(33.8411367527663,87.0621373417162,109.432300020937));
#34717=CARTESIAN_POINT('Ctrl Pts',(34.1540285705701,86.3493209030035,109.477183344366));
#34718=CARTESIAN_POINT('Ctrl Pts',(34.6831903458215,85.8807296858958,109.522066667795));
#34719=CARTESIAN_POINT('Ctrl Pts',(35.3039132524271,85.3310578919444,109.574716175526));
#34720=CARTESIAN_POINT('Ctrl Pts',(36.2222237448829,85.1174401434039,109.627365683257));
#34721=CARTESIAN_POINT('Ctrl Pts',(37.0218197359392,85.3367168080912,109.680015190987));
#34722=CARTESIAN_POINT('Ctrl Pts',(37.8214157269956,85.5559934727784,109.732664698718));
#34723=CARTESIAN_POINT('Ctrl Pts',(38.5022972166524,86.2081645506933,109.785314206449));
#34724=CARTESIAN_POINT('Ctrl Pts',(38.7557969307832,86.9975781962635,109.83796371418));
#34725=CARTESIAN_POINT('Ctrl Pts',(39.0092966449141,87.7869918418337,109.890613221911));
#34726=CARTESIAN_POINT('Ctrl Pts',(38.835414583519,88.7136480550593,109.943262729642));
#34727=CARTESIAN_POINT('Ctrl Pts',(38.3129775372868,89.3574613355163,109.995912237372));
#34728=CARTESIAN_POINT('Ctrl Pts',(37.7905404910545,90.0012746159734,110.048561745103));
#34729=CARTESIAN_POINT('Ctrl Pts',(36.9195484599851,90.362244963662,110.101211252834));
#34730=CARTESIAN_POINT('Ctrl Pts',(36.0948524352101,90.2767319595211,110.153860760565));
#34731=CARTESIAN_POINT('Ctrl Pts',(35.270156410435,90.1912189553803,110.206510268296));
#34732=CARTESIAN_POINT('Ctrl Pts',(34.4917563919543,89.6592225994099,110.259159776027));
#34733=CARTESIAN_POINT('Ctrl Pts',(34.1125281917178,88.921915350177,110.311809283757));
#34734=CARTESIAN_POINT('Ctrl Pts',(33.9309977610326,88.5689782468258,110.337011755008));
#34735=CARTESIAN_POINT('Ctrl Pts',(33.8409328694367,88.1689965609794,110.362214226258));
#34736=CARTESIAN_POINT('Ctrl Pts',(33.8413418417317,87.7688409760013,110.387416697508));
#34737=CARTESIAN_POINT('Origin',(36.3549260746835,87.7685555885722,114.));
#34738=CARTESIAN_POINT('',(33.8362791549462,87.7664293771055,111.387416697508));
#34739=CARTESIAN_POINT('',(33.833460355415,87.7691165130268,111.112583302492));
#34740=CARTESIAN_POINT('',(33.8374260746835,87.7685555885722,114.));
#34741=CARTESIAN_POINT('Ctrl Pts',(33.833460355415,87.7691165130268,111.112583302492));
#34742=CARTESIAN_POINT('Ctrl Pts',(33.8333656315816,87.8002064608974,111.110609402663));
#34743=CARTESIAN_POINT('Ctrl Pts',(33.8338914331638,87.8312931312554,111.108635502833));
#34744=CARTESIAN_POINT('Ctrl Pts',(33.8350477394907,87.8623563315067,111.106661603004));
#34745=CARTESIAN_POINT('Ctrl Pts',(33.8658897092781,88.6908999979653,111.054012095273));
#34746=CARTESIAN_POINT('Ctrl Pts',(34.3452981105313,89.5027460866671,111.001362587543));
#34747=CARTESIAN_POINT('Ctrl Pts',(35.0559404347995,89.9298565188012,110.948713079812));
#34748=CARTESIAN_POINT('Ctrl Pts',(35.7665827590678,90.3569669509352,110.896063572081));
#34749=CARTESIAN_POINT('Ctrl Pts',(36.7084590063511,90.3993417265016,110.84341406435));
#34750=CARTESIAN_POINT('Ctrl Pts',(37.4545839029127,90.037770885566,110.790764556619));
#34751=CARTESIAN_POINT('Ctrl Pts',(38.2007087994744,89.6762000446304,110.738115048888));
#34752=CARTESIAN_POINT('Ctrl Pts',(38.7510823453145,88.9106835871929,110.685465541158));
#34753=CARTESIAN_POINT('Ctrl Pts',(38.8562010627845,88.08825675779,110.632816033427));
#34754=CARTESIAN_POINT('Ctrl Pts',(38.9613197802546,87.2658299283872,110.580166525696));
#34755=CARTESIAN_POINT('Ctrl Pts',(38.6211836693548,86.3864927270191,110.527517017965));
#34756=CARTESIAN_POINT('Ctrl Pts',(37.9899882637174,85.8488793027858,110.474867510234));
#34757=CARTESIAN_POINT('Ctrl Pts',(37.35879285808,85.3112658785526,110.422218002503));
#34758=CARTESIAN_POINT('Ctrl Pts',(36.4365381577051,85.1153762314543,110.369568494773));
#34759=CARTESIAN_POINT('Ctrl Pts',(35.6413143061611,85.35001395255,110.316918987042));
#34760=CARTESIAN_POINT('Ctrl Pts',(34.8460904546171,85.5846516736457,110.264269479311));
#34761=CARTESIAN_POINT('Ctrl Pts',(34.1778974519041,86.2498167629355,110.21161997158));
#34762=CARTESIAN_POINT('Ctrl Pts',(33.9396504353168,87.0439667455121,110.158970463849));
#34763=CARTESIAN_POINT('Ctrl Pts',(33.8696807858515,87.2771969311392,110.14350807673));
#34764=CARTESIAN_POINT('Ctrl Pts',(33.8367944345703,87.5215522008777,110.128045689611));
#34765=CARTESIAN_POINT('Ctrl Pts',(33.8387900496171,87.766431943684,110.112583302492));
#34766=CARTESIAN_POINT('Ctrl Pts',(33.8413418417317,87.7688409760013,110.387416697508));
#34767=CARTESIAN_POINT('Ctrl Pts',(33.8417872376371,87.3330470084274,110.414863733989));
#34768=CARTESIAN_POINT('Ctrl Pts',(33.9495395712668,86.8970467869974,110.442310770469));
#34769=CARTESIAN_POINT('Ctrl Pts',(34.1633179095263,86.5213825231027,110.46975780695));
#34770=CARTESIAN_POINT('Ctrl Pts',(34.5733922095635,85.8007750877568,110.522407314681));
#34771=CARTESIAN_POINT('Ctrl Pts',(35.3735971916303,85.3021783595606,110.575056822411));
#34772=CARTESIAN_POINT('Ctrl Pts',(36.201172095805,85.2516235833065,110.627706330142));
#34773=CARTESIAN_POINT('Ctrl Pts',(37.0287469999796,85.2010688070523,110.680355837873));
#34774=CARTESIAN_POINT('Ctrl Pts',(37.8836918262622,85.5985559827401,110.733005345604));
#34775=CARTESIAN_POINT('Ctrl Pts',(38.3784303385795,86.2638903437209,110.785654853335));
#34776=CARTESIAN_POINT('Ctrl Pts',(38.8731688508967,86.9292247047016,110.838304361066));
#34777=CARTESIAN_POINT('Ctrl Pts',(39.0077010492487,87.8624062509753,110.890953868796));
#34778=CARTESIAN_POINT('Ctrl Pts',(38.7210388073494,88.6403913192867,110.943603376527));
#34779=CARTESIAN_POINT('Ctrl Pts',(38.4343765654501,89.4183763875982,110.996252884258));
#34780=CARTESIAN_POINT('Ctrl Pts',(37.7265198832995,90.0411649779474,111.048902391989));
#34781=CARTESIAN_POINT('Ctrl Pts',(36.9183648234917,90.2264253535138,111.10155189972));
#34782=CARTESIAN_POINT('Ctrl Pts',(36.1102097636839,90.4116857290801,111.15420140745));
#34783=CARTESIAN_POINT('Ctrl Pts',(35.2017563262188,90.1594178898637,111.206850915181));
#34784=CARTESIAN_POINT('Ctrl Pts',(34.6048380622974,89.5839836245909,111.259500422912));
#34785=CARTESIAN_POINT('Ctrl Pts',(34.1214175211251,89.1179621259357,111.302139181111));
#34786=CARTESIAN_POINT('Ctrl Pts',(33.8423248243317,88.4399841458963,111.344777939309));
#34787=CARTESIAN_POINT('Ctrl Pts',(33.8362791549462,87.7664293771055,111.387416697508));
#34788=CARTESIAN_POINT('Origin',(36.3549260746835,87.7685555885722,114.));
#34789=CARTESIAN_POINT('',(33.8351269672004,87.770359485814,112.387416697508));
#34790=CARTESIAN_POINT('',(33.8402624651776,87.7701463237333,112.112583302492));
#34791=CARTESIAN_POINT('',(33.8374260746835,87.7685555885722,114.));
#34792=CARTESIAN_POINT('Ctrl Pts',(33.8402624651776,87.7701463237333,112.112583302492));
#34793=CARTESIAN_POINT('Ctrl Pts',(33.8384607125217,88.0780025388695,112.093173115714));
#34794=CARTESIAN_POINT('Ctrl Pts',(33.8908469266789,88.3852669723462,112.073762928937));
#34795=CARTESIAN_POINT('Ctrl Pts',(34.0002046253728,88.6707043012003,112.054352742159));
#34796=CARTESIAN_POINT('Ctrl Pts',(34.2968338679842,89.4449438808758,112.001703234428));
#34797=CARTESIAN_POINT('Ctrl Pts',(35.0126297754489,90.0585909339135,111.949053726697));
#34798=CARTESIAN_POINT('Ctrl Pts',(35.8230971580917,90.2334579004335,111.896404218967));
#34799=CARTESIAN_POINT('Ctrl Pts',(36.6335645407346,90.4083248669535,111.843754711236));
#34800=CARTESIAN_POINT('Ctrl Pts',(37.5387033985555,90.1444117469556,111.791105203505));
#34801=CARTESIAN_POINT('Ctrl Pts',(38.1281827946389,89.561359540116,111.738455695774));
#34802=CARTESIAN_POINT('Ctrl Pts',(38.7176621907223,88.9783073332764,111.685806188043));
#34803=CARTESIAN_POINT('Ctrl Pts',(38.9914821250682,88.0761160395951,111.633156680312));
#34804=CARTESIAN_POINT('Ctrl Pts',(38.8255104943682,87.2637803626035,111.580507172582));
#34805=CARTESIAN_POINT('Ctrl Pts',(38.6595388636683,86.451444685612,111.527857664851));
#34806=CARTESIAN_POINT('Ctrl Pts',(38.0537756679227,85.7289646253103,111.47520815712));
#34807=CARTESIAN_POINT('Ctrl Pts',(37.2828344401971,85.4238655304275,111.422558649389));
#34808=CARTESIAN_POINT('Ctrl Pts',(36.5118932124715,85.1187664355448,111.369909141658));
#34809=CARTESIAN_POINT('Ctrl Pts',(35.5757739527659,85.2310483060809,111.317259633927));
#34810=CARTESIAN_POINT('Ctrl Pts',(34.8988520920738,85.7098098634567,111.264610126197));
#34811=CARTESIAN_POINT('Ctrl Pts',(34.2473089291673,86.1706220154706,111.213934518295));
#34812=CARTESIAN_POINT('Ctrl Pts',(33.8358921849187,86.9709493595603,111.163258910394));
#34813=CARTESIAN_POINT('Ctrl Pts',(33.833460355415,87.7691165130268,111.112583302492));
#34814=CARTESIAN_POINT('Ctrl Pts',(33.8362791549462,87.7664293771055,111.387416697508));
#34815=CARTESIAN_POINT('Ctrl Pts',(33.8348597495852,87.6082918428188,111.39742744704));
#34816=CARTESIAN_POINT('Ctrl Pts',(33.8484912122645,87.4503981242932,111.407438196572));
#34817=CARTESIAN_POINT('Ctrl Pts',(33.8780628754162,87.2955485091613,111.417448946105));
#34818=CARTESIAN_POINT('Ctrl Pts',(34.0335890428342,86.4811483503338,111.470098453835));
#34819=CARTESIAN_POINT('Ctrl Pts',(34.6300244680478,85.7509487240081,111.522747961566));
#34820=CARTESIAN_POINT('Ctrl Pts',(35.39698422092,85.4359745267719,111.575397469297));
#34821=CARTESIAN_POINT('Ctrl Pts',(36.1639439737922,85.1210003295356,111.628046977028));
#34822=CARTESIAN_POINT('Ctrl Pts',(37.101428054323,85.2212515613887,111.680696484759));
#34823=CARTESIAN_POINT('Ctrl Pts',(37.7844423107475,85.6912808508716,111.73334599249));
#34824=CARTESIAN_POINT('Ctrl Pts',(38.4674565671721,86.1613101403543,111.78599550022));
#34825=CARTESIAN_POINT('Ctrl Pts',(38.8960009994905,87.0011174874669,111.838645007951));
#34826=CARTESIAN_POINT('Ctrl Pts',(38.8758015061064,87.8299890021889,111.891294515682));
#34827=CARTESIAN_POINT('Ctrl Pts',(38.8556020127223,88.6588605169108,111.943944023413));
#34828=CARTESIAN_POINT('Ctrl Pts',(38.3866585936358,89.4767961992423,111.996593531144));
#34829=CARTESIAN_POINT('Ctrl Pts',(37.6815596167549,89.9129973457929,112.049243038874));
#34830=CARTESIAN_POINT('Ctrl Pts',(36.9764606398739,90.3491984923434,112.101892546605));
#34831=CARTESIAN_POINT('Ctrl Pts',(36.0352061051984,90.4036651031131,112.154542054336));
#34832=CARTESIAN_POINT('Ctrl Pts',(35.2844994425424,90.0517055683729,112.207191562067));
#34833=CARTESIAN_POINT('Ctrl Pts',(34.5337927798864,89.6997460336326,112.259841069798));
#34834=CARTESIAN_POINT('Ctrl Pts',(33.9736339892499,88.9413603533826,112.312490577529));
#34835=CARTESIAN_POINT('Ctrl Pts',(33.857962540138,88.1203511431353,112.365140085259));
#34836=CARTESIAN_POINT('Ctrl Pts',(33.8416485666483,88.0045583300114,112.372565622676));
#34837=CARTESIAN_POINT('Ctrl Pts',(33.8341761053276,87.8875198420373,112.379991160092));
#34838=CARTESIAN_POINT('Ctrl Pts',(33.8351269672004,87.770359485814,112.387416697508));
#34839=CARTESIAN_POINT('Origin',(36.3549260746835,87.7685555885722,114.));
#34840=CARTESIAN_POINT('',(33.8413206458264,87.7689269147693,113.387416697508));
#34841=CARTESIAN_POINT('',(33.8389342866079,87.7664619720545,113.112583302492));
#34842=CARTESIAN_POINT('',(33.8374260746835,87.7685555885722,114.));
#34843=CARTESIAN_POINT('Ctrl Pts',(33.8389342866079,87.7664619720545,113.112583302492));
#34844=CARTESIAN_POINT('Ctrl Pts',(33.8436023733314,88.3500889585574,113.075736828766));
#34845=CARTESIAN_POINT('Ctrl Pts',(34.0460599756738,88.9366381019817,113.03889035504));
#34846=CARTESIAN_POINT('Ctrl Pts',(34.4174406155119,89.3824748861331,113.002043881314));
#34847=CARTESIAN_POINT('Ctrl Pts',(34.9481021928884,90.019526002296,112.949394373583));
#34848=CARTESIAN_POINT('Ctrl Pts',(35.823657778157,90.36928149396,112.896744865852));
#34849=CARTESIAN_POINT('Ctrl Pts',(36.6471875611459,90.2731850276454,112.844095358121));
#34850=CARTESIAN_POINT('Ctrl Pts',(37.4707173441349,90.1770885613307,112.791445850391));
#34851=CARTESIAN_POINT('Ctrl Pts',(38.2422213248443,89.6351401370375,112.73879634266));
#34852=CARTESIAN_POINT('Ctrl Pts',(38.6119499057358,88.8930238316109,112.686146834929));
#34853=CARTESIAN_POINT('Ctrl Pts',(38.9816784866274,88.1509075261844,112.633497327198));
#34854=CARTESIAN_POINT('Ctrl Pts',(38.9496316677012,87.2086233396246,112.580847819467));
#34855=CARTESIAN_POINT('Ctrl Pts',(38.5303373869874,86.4933414787692,112.528198311736));
#34856=CARTESIAN_POINT('Ctrl Pts',(38.1110431062737,85.7780596179138,112.475548804006));
#34857=CARTESIAN_POINT('Ctrl Pts',(37.3045013637724,85.2897800827628,112.422899296275));
#34858=CARTESIAN_POINT('Ctrl Pts',(36.4763455935174,85.2498569754018,112.370249788544));
#34859=CARTESIAN_POINT('Ctrl Pts',(35.6481898232623,85.2099338680407,112.317600280813));
#34860=CARTESIAN_POINT('Ctrl Pts',(34.7984200252536,85.6183671884695,112.264950773082));
#34861=CARTESIAN_POINT('Ctrl Pts',(34.3122664151284,86.2899999018406,112.212301265351));
#34862=CARTESIAN_POINT('Ctrl Pts',(34.0053420662418,86.7140231507665,112.179061944398));
#34863=CARTESIAN_POINT('Ctrl Pts',(33.843347908687,87.2429524507666,112.145822623445));
#34864=CARTESIAN_POINT('Ctrl Pts',(33.8402624651776,87.7701463237333,112.112583302492));
#34865=CARTESIAN_POINT('Ctrl Pts',(33.8351269672004,87.770359485814,112.387416697508));
#34866=CARTESIAN_POINT('Ctrl Pts',(33.8409180294089,87.0568143004748,112.432640667823));
#34867=CARTESIAN_POINT('Ctrl Pts',(34.1591479610319,86.3387487640668,112.477864638137));
#34868=CARTESIAN_POINT('Ctrl Pts',(34.6953465327929,85.8700343879536,112.523088608452));
#34869=CARTESIAN_POINT('Ctrl Pts',(35.3195860821468,85.324359583264,112.575738116183));
#34870=CARTESIAN_POINT('Ctrl Pts',(36.2392492884418,85.1166427141294,112.628387623914));
#34871=CARTESIAN_POINT('Ctrl Pts',(37.0374208222499,85.3410490644606,112.681037131644));
#34872=CARTESIAN_POINT('Ctrl Pts',(37.8355923560581,85.5654554147918,112.733686639375));
#34873=CARTESIAN_POINT('Ctrl Pts',(38.5122722173794,86.2219849845887,112.786336147106));
#34874=CARTESIAN_POINT('Ctrl Pts',(38.7606978812279,87.0130100771061,112.838985654837));
#34875=CARTESIAN_POINT('Ctrl Pts',(39.0091235450763,87.8040351696234,112.891635162568));
#34876=CARTESIAN_POINT('Ctrl Pts',(38.8292950114517,88.7295557848613,112.944284670298));
#34877=CARTESIAN_POINT('Ctrl Pts',(38.3027348114541,89.37000122612,112.996934178029));
#34878=CARTESIAN_POINT('Ctrl Pts',(37.7761746114565,90.0104466673787,113.04958368576));
#34879=CARTESIAN_POINT('Ctrl Pts',(36.9028827450857,90.3658169346583,113.102233193491));
#34880=CARTESIAN_POINT('Ctrl Pts',(36.0787527999753,90.2750103213367,113.154882701222));
#34881=CARTESIAN_POINT('Ctrl Pts',(35.2546228548649,90.184203708015,113.207532208953));
#34882=CARTESIAN_POINT('Ctrl Pts',(34.4796548310148,89.6472202140922,113.260181716683));
#34883=CARTESIAN_POINT('Ctrl Pts',(34.105168697244,88.9074931407307,113.312831224414));
#34884=CARTESIAN_POINT('Ctrl Pts',(33.9283311751842,88.5581838049307,113.337693048779));
#34885=CARTESIAN_POINT('Ctrl Pts',(33.8407954587709,88.16366551418,113.362554873143));
#34886=CARTESIAN_POINT('Ctrl Pts',(33.8413206458264,87.7689269147693,113.387416697508));
#34887=CARTESIAN_POINT('Origin',(36.3549260746835,87.7685555885722,114.));
#34888=CARTESIAN_POINT('',(33.8364382102547,87.7664022269947,114.387416697508));
#34889=CARTESIAN_POINT('',(33.8334118350009,87.76902158344,114.112583302492));
#34890=CARTESIAN_POINT('',(33.8374260746835,87.7685555885722,114.));
#34891=CARTESIAN_POINT('Ctrl Pts',(33.8334118350009,87.76902158344,114.112583302492));
#34892=CARTESIAN_POINT('Ctrl Pts',(33.8333457474352,87.7947448381954,114.110950049548));
#34893=CARTESIAN_POINT('Ctrl Pts',(33.8337056909317,87.8204661988017,114.109316796605));
#34894=CARTESIAN_POINT('Ctrl Pts',(33.8344973919178,87.846174263081,114.107683543661));
#34895=CARTESIAN_POINT('Ctrl Pts',(33.8600186483467,88.6748988854847,114.05503403593));
#34896=CARTESIAN_POINT('Ctrl Pts',(34.3342043042376,89.4898065186503,114.002384528199));
#34897=CARTESIAN_POINT('Ctrl Pts',(35.0420895033447,89.9214711792297,113.949735020469));
#34898=CARTESIAN_POINT('Ctrl Pts',(35.7499747024518,90.3531358398091,113.897085512738));
#34899=CARTESIAN_POINT('Ctrl Pts',(36.6915594447751,90.4015575278024,113.844436005007));
#34900=CARTESIAN_POINT('Ctrl Pts',(37.4399906058851,90.0447850072972,113.791786497276));
#34901=CARTESIAN_POINT('Ctrl Pts',(38.1884217669951,89.6880124867921,113.739136989545));
#34902=CARTESIAN_POINT('Ctrl Pts',(38.7436993468918,88.9260457577886,113.686487481814));
#34903=CARTESIAN_POINT('Ctrl Pts',(38.854096698731,88.1043108497952,113.633837974084));
#34904=CARTESIAN_POINT('Ctrl Pts',(38.9644940505703,87.2825759418018,113.581188466353));
#34905=CARTESIAN_POINT('Ctrl Pts',(38.6300111743521,86.4010728548185,113.528538958622));
#34906=CARTESIAN_POINT('Ctrl Pts',(38.0022807955917,85.8594176084769,113.475889450891));
#34907=CARTESIAN_POINT('Ctrl Pts',(37.3745504168312,85.3177623621354,113.42323994316));
#34908=CARTESIAN_POINT('Ctrl Pts',(36.4535725355285,85.1159549564357,113.37059043543));
#34909=CARTESIAN_POINT('Ctrl Pts',(35.656858469034,85.3454817099042,113.317940927699));
#34910=CARTESIAN_POINT('Ctrl Pts',(34.8601444025395,85.5750084633728,113.265291419968));
#34911=CARTESIAN_POINT('Ctrl Pts',(34.1876941508532,86.2358693760097,113.212641912237));
#34912=CARTESIAN_POINT('Ctrl Pts',(33.9443528097522,87.028473202659,113.159992404506));
#34913=CARTESIAN_POINT('Ctrl Pts',(33.8713125923993,87.2663775205659,113.144189370502));
#34914=CARTESIAN_POINT('Ctrl Pts',(33.8369321972417,87.5161509875526,113.128386336497));
#34915=CARTESIAN_POINT('Ctrl Pts',(33.8389342866079,87.7664619720545,113.112583302492));
#34916=CARTESIAN_POINT('Ctrl Pts',(33.8413206458264,87.7689269147693,113.387416697508));
#34917=CARTESIAN_POINT('Ctrl Pts',(33.8419076394191,87.3277335794778,113.415204380874));
#34918=CARTESIAN_POINT('Ctrl Pts',(33.9525020156452,86.88626503035,113.44299206424));
#34919=CARTESIAN_POINT('Ctrl Pts',(34.1713711853595,86.5073359208025,113.470779747607));
#34920=CARTESIAN_POINT('Ctrl Pts',(34.5860640509373,85.7893764270359,113.523429255337));
#34921=CARTESIAN_POINT('Ctrl Pts',(35.3894540257846,85.2959280923031,113.576078763068));
#34922=CARTESIAN_POINT('Ctrl Pts',(36.2173364818051,85.2506882153788,113.628728270799));
#34923=CARTESIAN_POINT('Ctrl Pts',(37.0452189378256,85.2054483384545,113.68137777853));
#34924=CARTESIAN_POINT('Ctrl Pts',(37.8975938750193,85.6084169193387,113.734027286261));
#34925=CARTESIAN_POINT('Ctrl Pts',(38.3880500775153,86.2769142797552,113.786676793992));
#34926=CARTESIAN_POINT('Ctrl Pts',(38.8785062800113,86.9454116401717,113.839326301723));
#34927=CARTESIAN_POINT('Ctrl Pts',(39.0070437478097,87.8794377801204,113.891975809453));
#34928=CARTESIAN_POINT('Ctrl Pts',(38.7153919745293,88.6555661526162,113.944625317184));
#34929=CARTESIAN_POINT('Ctrl Pts',(38.4237402012488,89.431694525112,113.997274824915));
#34930=CARTESIAN_POINT('Ctrl Pts',(37.7118991868896,90.0499251301549,114.049924332646));
#34931=CARTESIAN_POINT('Ctrl Pts',(36.9025712304783,90.2299925242655,114.102573840377));
#34932=CARTESIAN_POINT('Ctrl Pts',(36.093243274067,90.4100599183761,114.155223348107));
#34933=CARTESIAN_POINT('Ctrl Pts',(35.1864283756038,90.1519641015545,114.207872855838));
#34934=CARTESIAN_POINT('Ctrl Pts',(34.5932172795427,89.5727088875421,114.260522363569));
#34935=CARTESIAN_POINT('Ctrl Pts',(34.1166371545854,89.1073407848392,114.302820474882));
#34936=CARTESIAN_POINT('Ctrl Pts',(33.8424682771257,88.4346847802262,114.345118586195));
#34937=CARTESIAN_POINT('Ctrl Pts',(33.8364382102547,87.7664022269947,114.387416697508));
#34938=CARTESIAN_POINT('Origin',(36.3549260746835,87.7685555885722,114.));
#34939=CARTESIAN_POINT('',(33.8349861623252,87.7703023246717,115.387416697508));
#34940=CARTESIAN_POINT('',(33.8401552434049,87.770206896396,115.112583302492));
#34941=CARTESIAN_POINT('',(33.8374260746835,87.7685555885722,114.));
#34942=CARTESIAN_POINT('Ctrl Pts',(33.8401552434049,87.770206896396,115.112583302492));
#34943=CARTESIAN_POINT('Ctrl Pts',(33.8383126786388,88.0726278356584,115.0935137626));
#34944=CARTESIAN_POINT('Ctrl Pts',(33.8888248324812,88.3744540280053,115.074444222708));
#34945=CARTESIAN_POINT('Ctrl Pts',(33.9944604721,88.6555660409125,115.055374682816));
#34946=CARTESIAN_POINT('Ctrl Pts',(34.2861122086519,89.4316943156675,115.002725175085));
#34947=CARTESIAN_POINT('Ctrl Pts',(34.9979531333667,90.0499248428541,114.950075667354));
#34948=CARTESIAN_POINT('Ctrl Pts',(35.8072809878564,90.229992214288,114.897426159623));
#34949=CARTESIAN_POINT('Ctrl Pts',(36.6166088423462,90.4100595857218,114.844776651893));
#34950=CARTESIAN_POINT('Ctrl Pts',(37.5234236266108,90.1519638014029,114.792127144162));
#34951=CARTESIAN_POINT('Ctrl Pts',(38.1166346479666,89.572708660338,114.739477636431));
#34952=CARTESIAN_POINT('Ctrl Pts',(38.7098456693223,88.993453519273,114.6868281287));
#34953=CARTESIAN_POINT('Ctrl Pts',(38.9894529277691,88.0930390214621,114.634178620969));
#34954=CARTESIAN_POINT('Ctrl Pts',(38.8287007246252,87.2796543870533,114.581529113239));
#34955=CARTESIAN_POINT('Ctrl Pts',(38.6679485214813,86.4662697526444,114.528879605508));
#34956=CARTESIAN_POINT('Ctrl Pts',(38.0668368567469,85.7399149816376,114.476230097777));
#34957=CARTESIAN_POINT('Ctrl Pts',(37.2978705626367,85.429871963928,114.423580590046));
#34958=CARTESIAN_POINT('Ctrl Pts',(36.5289042685266,85.1198289462183,114.370931082315));
#34959=CARTESIAN_POINT('Ctrl Pts',(35.5920833450407,85.2260976818057,114.318281574584));
#34960=CARTESIAN_POINT('Ctrl Pts',(34.9121013117813,85.7005028554204,114.265632066854));
#34961=CARTESIAN_POINT('Ctrl Pts',(34.2532131634472,86.1601913929319,114.214615812066));
#34962=CARTESIAN_POINT('Ctrl Pts',(33.8354761448212,86.9655305359212,114.163599557279));
#34963=CARTESIAN_POINT('Ctrl Pts',(33.8334118350009,87.76902158344,114.112583302492));
#34964=CARTESIAN_POINT('Ctrl Pts',(33.8364382102547,87.7664022269947,114.387416697508));
#34965=CARTESIAN_POINT('Ctrl Pts',(33.8349625034047,87.6028569193466,114.397768093926));
#34966=CARTESIAN_POINT('Ctrl Pts',(33.8495456897021,87.4395735386768,114.408119490344));
#34967=CARTESIAN_POINT('Ctrl Pts',(33.8811511132103,87.2796543254849,114.418470886762));
#34968=CARTESIAN_POINT('Ctrl Pts',(34.041903336598,86.4662695886435,114.471120394492));
#34969=CARTESIAN_POINT('Ctrl Pts',(34.6430150770324,85.739914726164,114.523769902223));
#34970=CARTESIAN_POINT('Ctrl Pts',(35.4119814679812,85.4298716694093,114.576419409954));
#34971=CARTESIAN_POINT('Ctrl Pts',(36.18094785893,85.1198286126545,114.629068917685));
#34972=CARTESIAN_POINT('Ctrl Pts',(37.1177689003931,85.2260973616245,114.681718425416));
#34973=CARTESIAN_POINT('Ctrl Pts',(37.7977510192853,85.7005025949826,114.734367933146));
#34974=CARTESIAN_POINT('Ctrl Pts',(38.4777331381775,86.1749078283407,114.787017440877));
#34975=CARTESIAN_POINT('Ctrl Pts',(38.9008763344987,87.0174495460869,114.839666948608));
#34976=CARTESIAN_POINT('Ctrl Pts',(38.875355074856,87.846174272855,114.892316456339));
#34977=CARTESIAN_POINT('Ctrl Pts',(38.8498338152134,88.6748989996231,114.94496596407));
#34978=CARTESIAN_POINT('Ctrl Pts',(38.3756480996068,89.4898067354131,114.997615471801));
#34979=CARTESIAN_POINT('Ctrl Pts',(37.6677628113533,89.9214714503538,115.050264979531));
#34980=CARTESIAN_POINT('Ctrl Pts',(36.9598775230998,90.3531361652945,115.102914487262));
#34981=CARTESIAN_POINT('Ctrl Pts',(36.0182926621993,90.4015578593859,115.155563994993));
#34982=CARTESIAN_POINT('Ctrl Pts',(35.2698614068365,90.0447852939514,115.208213502724));
#34983=CARTESIAN_POINT('Ctrl Pts',(34.5214301514738,89.6880127285168,115.260863010455));
#34984=CARTESIAN_POINT('Ctrl Pts',(33.9661525016488,88.9260459035562,115.313512518185));
#34985=CARTESIAN_POINT('Ctrl Pts',(33.8557551359065,88.1043108920788,115.366162025916));
#34986=CARTESIAN_POINT('Ctrl Pts',(33.8408992847342,87.9937324108665,115.373246916447));
#34987=CARTESIAN_POINT('Ctrl Pts',(33.8340994588008,87.8820716294572,115.380331806977));
#34988=CARTESIAN_POINT('Ctrl Pts',(33.8349861623252,87.7703023246717,115.387416697508));
#34989=CARTESIAN_POINT('Origin',(36.3549260746835,87.7685555885722,114.));
#34990=CARTESIAN_POINT('',(33.8412939066634,87.7690123128212,116.387416697508));
#34991=CARTESIAN_POINT('',(33.8390758148819,87.7664952480788,116.112583302492));
#34992=CARTESIAN_POINT('',(33.8374260746835,87.7685555885722,114.));
#34993=CARTESIAN_POINT('Ctrl Pts',(33.8390758148819,87.7664952480788,116.112583302492));
#34994=CARTESIAN_POINT('Ctrl Pts',(33.8436083734887,88.3448089772224,116.076077475652));
#34995=CARTESIAN_POINT('Ctrl Pts',(34.0420142063692,88.925932533728,116.039571648811));
#34996=CARTESIAN_POINT('Ctrl Pts',(34.407117583208,89.3700010244447,116.003065821971));
#34997=CARTESIAN_POINT('Ctrl Pts',(34.9336777168943,90.0104463850497,115.95041631424));
#34998=CARTESIAN_POINT('Ctrl Pts',(35.8069694732883,90.3658166075759,115.897766806509));
#34999=CARTESIAN_POINT('Ctrl Pts',(36.631099314613,90.2750100056896,115.845117298778));
#35000=CARTESIAN_POINT('Ctrl Pts',(37.4552291559377,90.1842034038034,115.792467791047));
#35001=CARTESIAN_POINT('Ctrl Pts',(38.2301970821931,89.6472199775046,115.739818283317));
#35002=CARTESIAN_POINT('Ctrl Pts',(38.6046831688033,88.9074929972995,115.687168775586));
#35003=CARTESIAN_POINT('Ctrl Pts',(38.9791692554135,88.1677660170944,115.634519267855));
#35004=CARTESIAN_POINT('Ctrl Pts',(38.9531735023785,87.225295482983,115.581869760124));
#35005=CARTESIAN_POINT('Ctrl Pts',(38.5384806890242,86.5073360796318,115.529220252393));
#35006=CARTESIAN_POINT('Ctrl Pts',(38.1237878756699,85.7893766762806,115.476570744662));
#35007=CARTESIAN_POINT('Ctrl Pts',(37.3203980019963,85.2959284036898,115.423921236932));
#35008=CARTESIAN_POINT('Ctrl Pts',(36.492515650234,85.2506885324629,115.371271729201));
#35009=CARTESIAN_POINT('Ctrl Pts',(35.6646332984718,85.2054486612361,115.31862222147));
#35010=CARTESIAN_POINT('Ctrl Pts',(34.8122584686209,85.6084171913732,115.265972713739));
#35011=CARTESIAN_POINT('Ctrl Pts',(34.32180232789,86.2769144676035,115.213323206008));
#35012=CARTESIAN_POINT('Ctrl Pts',(34.0089883597845,86.703283450024,115.17974323817));
#35013=CARTESIAN_POINT('Ctrl Pts',(33.8433998558045,87.2376672823468,115.146163270331));
#35014=CARTESIAN_POINT('Ctrl Pts',(33.8401552434049,87.770206896396,115.112583302492));
#35015=CARTESIAN_POINT('Ctrl Pts',(33.8349861623252,87.7703023246717,115.387416697508));
#35016=CARTESIAN_POINT('Ctrl Pts',(33.8406887637253,87.051487324592,115.432981314708));
#35017=CARTESIAN_POINT('Ctrl Pts',(34.1643125433803,86.3281837084398,115.478545931909));
#35018=CARTESIAN_POINT('Ctrl Pts',(34.7075711463174,85.8594173680528,115.524110549109));
#35019=CARTESIAN_POINT('Ctrl Pts',(35.3353016041301,85.3177620534985,115.57676005684));
#35020=CARTESIAN_POINT('Ctrl Pts',(36.2562796014149,85.115954622384,115.62940956457));
#35021=CARTESIAN_POINT('Ctrl Pts',(37.0529937682425,85.3454814047575,115.682059072301));
#35022=CARTESIAN_POINT('Ctrl Pts',(37.8497079350702,85.5750081871309,115.734708580032));
#35023=CARTESIAN_POINT('Ctrl Pts',(38.5221582714408,86.2358691829923,115.787358087763));
#35024=CARTESIAN_POINT('Ctrl Pts',(38.7654996431869,87.028473109457,115.840007595494));
#35025=CARTESIAN_POINT('Ctrl Pts',(39.008841014933,87.8210770359218,115.892657103225));
#35026=CARTESIAN_POINT('Ctrl Pts',(38.8230734220546,88.74542389299,115.945306610955));
#35027=CARTESIAN_POINT('Ctrl Pts',(38.2924117778502,89.3824750893792,115.997956118686));
#35028=CARTESIAN_POINT('Ctrl Pts',(37.7617501336458,90.0195262857684,116.050605626417));
#35029=CARTESIAN_POINT('Ctrl Pts',(36.8861944381154,90.3692818214786,116.103255134148));
#35030=CARTESIAN_POINT('Ctrl Pts',(36.0626645514163,90.2731853430625,116.155904641879));
#35031=CARTESIAN_POINT('Ctrl Pts',(35.2391346647172,90.1770888646463,116.20855414961));
#35032=CARTESIAN_POINT('Ctrl Pts',(34.4676305868494,89.6351403721039,116.26120365734));
#35033=CARTESIAN_POINT('Ctrl Pts',(34.0979019593964,88.8930239732201,116.313853165071));
#35034=CARTESIAN_POINT('Ctrl Pts',(33.9257031738126,88.5473879224497,116.33837434255));
#35035=CARTESIAN_POINT('Ctrl Pts',(33.8406563983059,88.1583320077416,116.362895520029));
#35036=CARTESIAN_POINT('Ctrl Pts',(33.8412939066634,87.7690123128212,116.387416697508));
#35037=CARTESIAN_POINT('Origin',(36.3549260746835,87.7685555885722,114.));
#35038=CARTESIAN_POINT('',(33.8365981008565,87.7663787380631,117.387416697508));
#35039=CARTESIAN_POINT('',(33.8333717767661,87.768925609881,117.112583302492));
#35040=CARTESIAN_POINT('',(33.8374260746835,87.7685555885722,114.));
#35041=CARTESIAN_POINT('Ctrl Pts',(33.8333717767661,87.768925609881,117.112583302492));
#35042=CARTESIAN_POINT('Ctrl Pts',(33.8333296036217,87.7892829070983,117.111290696434));
#35043=CARTESIAN_POINT('Ctrl Pts',(33.8335550399572,87.8096392466113,117.109998090376));
#35044=CARTESIAN_POINT('Ctrl Pts',(33.8340509607236,87.829988994453,117.108705484318));
#35045=CARTESIAN_POINT('Ctrl Pts',(33.8542504515642,88.6588604047923,117.056055976587));
#35046=CARTESIAN_POINT('Ctrl Pts',(34.3231938115952,89.4767959841181,117.003406468856));
#35047=CARTESIAN_POINT('Ctrl Pts',(35.0282926996806,89.912997075736,116.950756961126));
#35048=CARTESIAN_POINT('Ctrl Pts',(35.733391587766,90.349198167354,116.898107453395));
#35049=CARTESIAN_POINT('Ctrl Pts',(36.6746460039059,90.4036647712641,116.845457945664));
#35050=CARTESIAN_POINT('Ctrl Pts',(37.4253525720226,90.0517052808472,116.792808437933));
#35051=CARTESIAN_POINT('Ctrl Pts',(38.1760591401393,89.6997457904303,116.740158930202));
#35052=CARTESIAN_POINT('Ctrl Pts',(38.7362178602328,88.9413602056864,116.687509422471));
#35053=CARTESIAN_POINT('Ctrl Pts',(38.8518892947775,88.1203510988316,116.634859914741));
#35054=CARTESIAN_POINT('Ctrl Pts',(38.9675607293222,87.2993419919769,116.58221040701));
#35055=CARTESIAN_POINT('Ctrl Pts',(38.638744878318,86.4157093630114,116.529560899279));
#35056=CARTESIAN_POINT('Ctrl Pts',(38.0145054075767,85.8700346270407,116.476911391548));
#35057=CARTESIAN_POINT('Ctrl Pts',(37.3902659368354,85.3243598910701,116.424261883817));
#35058=CARTESIAN_POINT('Ctrl Pts',(36.4706028463569,85.1166430480943,116.371612376086));
#35059=CARTESIAN_POINT('Ctrl Pts',(35.6724314130655,85.3410493701655,116.318962868356));
#35060=CARTESIAN_POINT('Ctrl Pts',(34.874259979774,85.5654556922366,116.266313360625));
#35061=CARTESIAN_POINT('Ctrl Pts',(34.1975802036695,86.2219851793546,116.213663852894));
#35062=CARTESIAN_POINT('Ctrl Pts',(33.9491545711065,87.0130101722554,116.161014345163));
#35063=CARTESIAN_POINT('Ctrl Pts',(33.8729809408117,87.255558595063,116.144870664273));
#35064=CARTESIAN_POINT('Ctrl Pts',(33.8370714176089,87.5107521761952,116.128726983382));
#35065=CARTESIAN_POINT('Ctrl Pts',(33.8390758148819,87.7664952480788,116.112583302492));
#35066=CARTESIAN_POINT('Ctrl Pts',(33.8412939066634,87.7690123128212,116.387416697508));
#35067=CARTESIAN_POINT('Ctrl Pts',(33.8420251947768,87.3224223005078,116.41554502776));
#35068=CARTESIAN_POINT('Ctrl Pts',(33.9555038567139,86.8754851938983,116.443673358012));
#35069=CARTESIAN_POINT('Ctrl Pts',(34.1795144884218,86.4933413181774,116.471801688264));
#35070=CARTESIAN_POINT('Ctrl Pts',(34.5988088219386,85.7780593672439,116.524451195994));
#35071=CARTESIAN_POINT('Ctrl Pts',(35.4053506660105,85.2897797706019,116.577100703725));
#35072=CARTESIAN_POINT('Ctrl Pts',(36.2335065405582,85.2498566582129,116.629750211456));
#35073=CARTESIAN_POINT('Ctrl Pts',(37.0616624151058,85.2099335458239,116.682399719187));
#35074=CARTESIAN_POINT('Ctrl Pts',(37.9114323201292,85.618366917688,116.735049226918));
#35075=CARTESIAN_POINT('Ctrl Pts',(38.3975859914778,86.2899997156401,116.787698734649));
#35076=CARTESIAN_POINT('Ctrl Pts',(38.8837396628263,86.9616325135921,116.840348242379));
#35077=CARTESIAN_POINT('Ctrl Pts',(39.0062771005,87.8964647376321,116.89299775011));
#35078=CARTESIAN_POINT('Ctrl Pts',(38.7096478205332,88.6707044148104,116.945647257841));
#35079=CARTESIAN_POINT('Ctrl Pts',(38.4130185405664,89.4449440919888,116.998296765572));
#35080=CARTESIAN_POINT('Ctrl Pts',(37.6972225429591,90.0585912223056,117.050946273303));
#35081=CARTESIAN_POINT('Ctrl Pts',(36.8867550582512,90.2334582108475,117.103595781034));
#35082=CARTESIAN_POINT('Ctrl Pts',(36.0762875735433,90.4083251993893,117.156245288764));
#35083=CARTESIAN_POINT('Ctrl Pts',(35.1711486017349,90.1444120461562,117.208894796495));
#35084=CARTESIAN_POINT('Ctrl Pts',(34.581669131416,89.5613597658909,117.261544304226));
#35085=CARTESIAN_POINT('Ctrl Pts',(34.1119009422619,89.0967135353203,117.303501768653));
#35086=CARTESIAN_POINT('Ctrl Pts',(33.8426024374579,88.4293877726653,117.345459233081));
#35087=CARTESIAN_POINT('Ctrl Pts',(33.8365981008565,87.7663787380631,117.387416697508));
#35088=CARTESIAN_POINT('Origin',(36.3549260746835,87.7685555885722,114.));
#35089=CARTESIAN_POINT('',(33.83484883244,87.7702419443436,118.387416697508));
#35090=CARTESIAN_POINT('',(33.8400438151642,87.770264994436,118.112583302492));
#35091=CARTESIAN_POINT('',(33.8374260746835,87.7685555885722,114.));
#35092=CARTESIAN_POINT('Ctrl Pts',(33.8400438151642,87.770264994436,118.112583302492));
#35093=CARTESIAN_POINT('Ctrl Pts',(33.8381651041214,88.0672505512461,118.093854409486));
#35094=CARTESIAN_POINT('Ctrl Pts',(33.8868399271723,88.3636403356866,118.075125516479));
#35095=CARTESIAN_POINT('Ctrl Pts',(33.9888136399911,88.640391209494,118.056396623473));
#35096=CARTESIAN_POINT('Ctrl Pts',(34.2754758457902,89.4183761798309,118.003747115742));
#35097=CARTESIAN_POINT('Ctrl Pts',(34.983332438798,90.0411646917499,117.951097608011));
#35098=CARTESIAN_POINT('Ctrl Pts',(35.791487396832,90.2264250439855,117.89844810028));
#35099=CARTESIAN_POINT('Ctrl Pts',(36.5996423548659,90.4116853962211,117.845798592549));
#35100=CARTESIAN_POINT('Ctrl Pts',(37.5080956779261,90.1594175887735,117.793149084819));
#35101=CARTESIAN_POINT('Ctrl Pts',(38.1050138666753,89.583983395967,117.740499577088));
#35102=CARTESIAN_POINT('Ctrl Pts',(38.7019320554245,89.0085492031604,117.687850069357));
#35103=CARTESIAN_POINT('Ctrl Pts',(38.9873151098626,88.109948624995,117.635200561626));
#35104=CARTESIAN_POINT('Ctrl Pts',(38.8317889620303,87.295548568728,117.582551053895));
#35105=CARTESIAN_POINT('Ctrl Pts',(38.6762628141981,86.4811485124609,117.529901546165));
#35106=CARTESIAN_POINT('Ctrl Pts',(38.0798274640955,85.7509489780921,117.477252038434));
#35107=CARTESIAN_POINT('Ctrl Pts',(37.3128678078092,85.4359748205219,117.424602530703));
#35108=CARTESIAN_POINT('Ctrl Pts',(36.545908151523,85.1210006629517,117.371953022972));
#35109=CARTESIAN_POINT('Ctrl Pts',(35.608424189053,85.2212518821802,117.319303515241));
#35110=CARTESIAN_POINT('Ctrl Pts',(34.925410018643,85.6912811124707,117.26665400751));
#35111=CARTESIAN_POINT('Ctrl Pts',(34.259164632832,86.1497705837644,117.215297105838));
#35112=CARTESIAN_POINT('Ctrl Pts',(33.8350473700513,86.96010400098,117.163940204165));
#35113=CARTESIAN_POINT('Ctrl Pts',(33.8333717767661,87.768925609881,117.112583302492));
#35114=CARTESIAN_POINT('Ctrl Pts',(33.8365981008565,87.7663787380631,117.387416697508));
#35115=CARTESIAN_POINT('Ctrl Pts',(33.83506801252,87.5974237879654,117.398108740811));
#35116=CARTESIAN_POINT('Ctrl Pts',(33.8506358798951,87.428749160161,117.408800784115));
#35117=CARTESIAN_POINT('Ctrl Pts',(33.884341343869,87.2637802990361,117.419492827418));
#35118=CARTESIAN_POINT('Ctrl Pts',(34.0503129954701,86.4514445197442,117.472142335149));
#35119=CARTESIAN_POINT('Ctrl Pts',(34.6560762675015,85.7289643684577,117.52479184288));
#35120=CARTESIAN_POINT('Ctrl Pts',(35.4270175923144,85.4238652351525,117.577441350611));
#35121=CARTESIAN_POINT('Ctrl Pts',(36.1979589171274,85.1187661018472,117.630090858342));
#35122=CARTESIAN_POINT('Ctrl Pts',(37.1340782947219,85.2310479865231,117.682740366073));
#35123=CARTESIAN_POINT('Ctrl Pts',(37.8110002406613,85.709809604191,117.735389873803));
#35124=CARTESIAN_POINT('Ctrl Pts',(38.4879221866007,86.1885712218588,117.788039381534));
#35125=CARTESIAN_POINT('Ctrl Pts',(38.905646700885,87.0338125725185,117.840688889265));
#35126=CARTESIAN_POINT('Ctrl Pts',(38.8748047272138,87.8623563433186,117.893338396996));
#35127=CARTESIAN_POINT('Ctrl Pts',(38.8439627535427,88.6909001141187,117.945987904727));
#35128=CARTESIAN_POINT('Ctrl Pts',(38.3645542919161,89.5027463050592,117.998637412458));
#35129=CARTESIAN_POINT('Ctrl Pts',(37.6539118781542,89.9298567909811,118.051286920188));
#35130=CARTESIAN_POINT('Ctrl Pts',(36.9432694643923,90.3569672769031,118.103936427919));
#35131=CARTESIAN_POINT('Ctrl Pts',(36.0013930984951,90.3993420578065,118.15658593565));
#35132=CARTESIAN_POINT('Ctrl Pts',(35.2552681079711,90.0377711713371,118.209235443381));
#35133=CARTESIAN_POINT('Ctrl Pts',(34.5091431174471,89.6762002848676,118.261884951112));
#35134=CARTESIAN_POINT('Ctrl Pts',(33.9587695022963,88.9106837310251,118.314534458842));
#35135=CARTESIAN_POINT('Ctrl Pts',(33.853650771588,88.0882567980515,118.367183966573));
#35136=CARTESIAN_POINT('Ctrl Pts',(33.840185378233,87.9829063806367,118.373928210218));
#35137=CARTESIAN_POINT('Ctrl Pts',(33.8340261009119,87.8766221299322,118.380672453863));
#35138=CARTESIAN_POINT('Ctrl Pts',(33.83484883244,87.7702419443436,118.387416697508));
#35139=CARTESIAN_POINT('Origin',(36.3549260746835,87.7685555885722,114.));
#35140=CARTESIAN_POINT('',(33.8412616562718,87.7690970336947,119.387416697508));
#35141=CARTESIAN_POINT('',(33.8392144539235,87.7665317069332,119.112583302492));
#35142=CARTESIAN_POINT('',(33.8374260746835,87.7685555885722,114.));
#35143=CARTESIAN_POINT('Ctrl Pts',(33.8392144539235,87.7665317069332,119.112583302492));
#35144=CARTESIAN_POINT('Ctrl Pts',(33.8436076679264,88.3395289215697,119.076418122537));
#35145=CARTESIAN_POINT('Ctrl Pts',(34.0380105838227,88.9152229984202,119.040252942582));
#35146=CARTESIAN_POINT('Ctrl Pts',(34.3968748586662,89.3574611354189,119.004087762628));
#35147=CARTESIAN_POINT('Ctrl Pts',(34.9193118391072,90.0012743347968,118.951438254897));
#35148=CARTESIAN_POINT('Ctrl Pts',(35.7903037604876,90.3622446370295,118.898788747166));
#35149=CARTESIAN_POINT('Ctrl Pts',(36.6149996814052,90.276731643658,118.846139239435));
#35150=CARTESIAN_POINT('Ctrl Pts',(37.4396956023229,90.1912186502865,118.793489731704));
#35151=CARTESIAN_POINT('Ctrl Pts',(38.2180955227777,89.6592223613109,118.740840223974));
#35152=CARTESIAN_POINT('Ctrl Pts',(38.5973236752566,88.9219152049292,118.688190716243));
#35153=CARTESIAN_POINT('Ctrl Pts',(38.9765518277355,88.1846080485476,118.635541208512));
#35154=CARTESIAN_POINT('Ctrl Pts',(38.9566082122386,87.24199002476,118.582891700781));
#35155=CARTESIAN_POINT('Ctrl Pts',(38.5465339638431,86.5213826801631,118.53024219305));
#35156=CARTESIAN_POINT('Ctrl Pts',(38.1364597154477,85.8007753355662,118.477592685319));
#35157=CARTESIAN_POINT('Ctrl Pts',(37.3362548341537,85.3021786701601,118.424943177589));
#35158=CARTESIAN_POINT('Ctrl Pts',(36.5086800341986,85.2516239002727,118.372293669858));
#35159=CARTESIAN_POINT('Ctrl Pts',(35.6811052342435,85.2010691303852,118.319644162127));
#35160=CARTESIAN_POINT('Ctrl Pts',(34.8261605156272,85.5985562560164,118.266994654396));
#35161=CARTESIAN_POINT('Ctrl Pts',(34.3314220656143,86.2638905332094,118.214345146665));
#35162=CARTESIAN_POINT('Ctrl Pts',(34.0126758308339,86.6925469186593,118.180424531941));
#35163=CARTESIAN_POINT('Ctrl Pts',(33.8434464206167,87.2323830893058,118.146503917216));
#35164=CARTESIAN_POINT('Ctrl Pts',(33.8400438151642,87.770264994436,118.112583302492));
#35165=CARTESIAN_POINT('Ctrl Pts',(33.83484883244,87.7702419443436,118.387416697508));
#35166=CARTESIAN_POINT('Ctrl Pts',(33.8404488240859,87.046156224721,118.433321961594));
#35167=CARTESIAN_POINT('Ctrl Pts',(34.1695224385136,86.3176258810383,118.47922722568));
#35168=CARTESIAN_POINT('Ctrl Pts',(34.7198636797397,85.8488790610354,118.525132489766));
#35169=CARTESIAN_POINT('Ctrl Pts',(35.3510591648657,85.3112655690975,118.577781997496));
#35170=CARTESIAN_POINT('Ctrl Pts',(36.2733139813835,85.1153758973266,118.630431505227));
#35171=CARTESIAN_POINT('Ctrl Pts',(37.068537933073,85.3500136479724,118.683081012958));
#35172=CARTESIAN_POINT('Ctrl Pts',(37.8637618847625,85.5846513986182,118.735730520689));
#35173=CARTESIAN_POINT('Ctrl Pts',(38.5319549716236,86.2498165716809,118.78838002842));
#35174=CARTESIAN_POINT('Ctrl Pts',(38.7702020182144,87.0439666542645,118.841029536151));
#35175=CARTESIAN_POINT('Ctrl Pts',(39.0084490648051,87.8381167368482,118.893679043881));
#35176=CARTESIAN_POINT('Ctrl Pts',(38.8167500711256,88.7612517289529,118.946328551612));
#35177=CARTESIAN_POINT('Ctrl Pts',(38.2820088620648,89.394882413123,118.998978059343));
#35178=CARTESIAN_POINT('Ctrl Pts',(37.7472676530041,90.0285130972932,119.051627567074));
#35179=CARTESIAN_POINT('Ctrl Pts',(36.8694842285622,90.3726394735288,119.104277074805));
#35180=CARTESIAN_POINT('Ctrl Pts',(36.0465883533813,90.2712570960621,119.156926582536));
#35181=CARTESIAN_POINT('Ctrl Pts',(35.2236924782003,90.1698747185954,119.209576090266));
#35182=CARTESIAN_POINT('Ctrl Pts',(34.4556841522802,89.6229835874264,119.262225597997));
#35183=CARTESIAN_POINT('Ctrl Pts',(34.0907282764438,88.8785084519475,119.314875105728));
#35184=CARTESIAN_POINT('Ctrl Pts',(33.9231136661421,88.5365906531818,119.339055636321));
#35185=CARTESIAN_POINT('Ctrl Pts',(33.840515823365,88.1529960122149,119.363236166915));
#35186=CARTESIAN_POINT('Ctrl Pts',(33.8412616562718,87.7690970336947,119.387416697508));
#35187=CARTESIAN_POINT('Origin',(36.3549260746835,87.7685555885722,114.));
#35188=CARTESIAN_POINT('',(33.836758858704,87.7663573595953,120.387416697508));
#35189=CARTESIAN_POINT('',(33.833340462721,87.7688288397412,120.112583302492));
#35190=CARTESIAN_POINT('',(33.8374260746835,87.7685555885722,114.));
#35191=CARTESIAN_POINT('Ctrl Pts',(33.833340462721,87.7688288397412,120.112583302492));
#35192=CARTESIAN_POINT('Ctrl Pts',(33.8333171635958,87.7838207780303,120.11163134332));
#35193=CARTESIAN_POINT('Ctrl Pts',(33.833439427189,87.7988123261839,120.110679384147));
#35194=CARTESIAN_POINT('Ctrl Pts',(33.8337084163132,87.8138012411625,120.109727424975));
#35195=CARTESIAN_POINT('Ctrl Pts',(33.8485852570257,88.6427853173127,120.057077917244));
#35196=CARTESIAN_POINT('Ctrl Pts',(34.3122670847453,89.4637150212562,120.004428409513));
#35197=CARTESIAN_POINT('Ctrl Pts',(35.014550615983,89.9044345342344,119.951778901782));
#35198=CARTESIAN_POINT('Ctrl Pts',(35.7168341472208,90.3451540472126,119.899129394052));
#35199=CARTESIAN_POINT('Ctrl Pts',(36.6577193819767,90.4056633692255,119.846479886321));
#35200=CARTESIAN_POINT('Ctrl Pts',(37.4106703935041,90.0585314323461,119.79383037859));
#35201=CARTESIAN_POINT('Ctrl Pts',(38.1636214050315,89.7113994954668,119.741180870859));
#35202=CARTESIAN_POINT('Ctrl Pts',(38.7286381933304,88.9566262996952,119.688531363128));
#35203=CARTESIAN_POINT('Ctrl Pts',(38.8495789474356,88.13637683792,119.635881855397));
#35204=CARTESIAN_POINT('Ctrl Pts',(38.9705197015409,87.3161273761447,119.583232347667));
#35205=CARTESIAN_POINT('Ctrl Pts',(38.6473844214524,86.4304016483656,119.530582839936));
#35206=CARTESIAN_POINT('Ctrl Pts',(38.0266615930102,85.8807299236465,119.477933332205));
#35207=CARTESIAN_POINT('Ctrl Pts',(37.4059387645679,85.3310581989274,119.425283824474));
#35208=CARTESIAN_POINT('Ctrl Pts',(36.487628387772,85.1174404772682,119.372634316743));
#35209=CARTESIAN_POINT('Ctrl Pts',(35.6880324974151,85.3367171143363,119.319984809013));
#35210=CARTESIAN_POINT('Ctrl Pts',(34.8884366070581,85.5559937514044,119.267335301282));
#35211=CARTESIAN_POINT('Ctrl Pts',(34.2075552031403,86.2081647471997,119.214685793551));
#35212=CARTESIAN_POINT('Ctrl Pts',(33.9540555209321,86.9975782933589,119.16203628582));
#35213=CARTESIAN_POINT('Ctrl Pts',(33.8746858927486,87.2447401797007,119.145551958044));
#35214=CARTESIAN_POINT('Ctrl Pts',(33.8372119979782,87.5053557937311,119.129067630268));
#35215=CARTESIAN_POINT('Ctrl Pts',(33.8392144539235,87.7665317069332,119.112583302492));
#35216=CARTESIAN_POINT('Ctrl Pts',(33.8412616562718,87.7690970336947,119.387416697508));
#35217=CARTESIAN_POINT('Ctrl Pts',(33.8421397635529,87.3171131038791,119.415885674646));
#35218=CARTESIAN_POINT('Ctrl Pts',(33.958545197753,86.8647073147717,119.444354651783));
#35219=CARTESIAN_POINT('Ctrl Pts',(34.1877474858301,86.4793992764073,119.472823628921));
#35220=CARTESIAN_POINT('Ctrl Pts',(34.6116259968056,85.7668243761348,119.525473136651));
#35221=CARTESIAN_POINT('Ctrl Pts',(35.4212864445094,85.2837337153784,119.578122644382));
#35222=CARTESIAN_POINT('Ctrl Pts',(36.2496815994356,85.2491289785611,119.630772152113));
#35223=CARTESIAN_POINT('Ctrl Pts',(37.0780767543618,85.2145242417438,119.683421659844));
#35224=CARTESIAN_POINT('Ctrl Pts',(37.9252066165105,85.6284054288655,119.736071167575));
#35225=CARTESIAN_POINT('Ctrl Pts',(38.4070376995544,86.3031460451161,119.788720675305));
#35226=CARTESIAN_POINT('Ctrl Pts',(38.8888687825984,86.9778866613667,119.841370183036));
#35227=CARTESIAN_POINT('Ctrl Pts',(39.0054010865376,87.9134867067461,119.894019690767));
#35228=CARTESIAN_POINT('Ctrl Pts',(38.703806556982,88.6858056190045,119.946669198498));
#35229=CARTESIAN_POINT('Ctrl Pts',(38.4022120274264,89.458124531263,119.999318706229));
#35230=CARTESIAN_POINT('Ctrl Pts',(37.6824906643758,90.0671623104004,120.05196821396));
#35231=CARTESIAN_POINT('Ctrl Pts',(36.8709170107602,90.2368219880218,120.10461772169));
#35232=CARTESIAN_POINT('Ctrl Pts',(36.0593433571446,90.4064816656432,120.157267229421));
#35233=CARTESIAN_POINT('Ctrl Pts',(35.1559174129639,90.1367632417485,120.209916737152));
#35234=CARTESIAN_POINT('Ctrl Pts',(34.570193987387,89.5499373082837,120.262566244883));
#35235=CARTESIAN_POINT('Ctrl Pts',(34.1072087481559,89.0860805913963,120.304183062425));
#35236=CARTESIAN_POINT('Ctrl Pts',(33.8427277366527,88.4240914153437,120.345799879966));
#35237=CARTESIAN_POINT('Ctrl Pts',(33.836758858704,87.7663573595953,120.387416697508));
#35238=CARTESIAN_POINT('Origin',(36.3549260746835,87.7685555885722,114.));
#35239=CARTESIAN_POINT('',(33.8347232656258,87.7701345030551,121.387416697508));
#35240=CARTESIAN_POINT('',(33.8399314485466,87.7703173734778,121.112583302492));
#35241=CARTESIAN_POINT('',(33.8374260746835,87.7685555885722,114.));
#35242=CARTESIAN_POINT('',(38.2683920713486,89.4045427919472,122.));
#35243=CARTESIAN_POINT('Ctrl Pts',(33.8347232656258,87.7701345030551,121.387416697508));
#35244=CARTESIAN_POINT('Ctrl Pts',(33.8401812849309,87.0409115185374,121.43366260848));
#35245=CARTESIAN_POINT('Ctrl Pts',(34.1747109746967,86.3074372742024,121.479908519451));
#35246=CARTESIAN_POINT('Ctrl Pts',(34.732188100241,85.8386039826766,121.526154430423));
#35247=CARTESIAN_POINT('Ctrl Pts',(35.366858184893,85.3048521008755,121.578803938153));
#35248=CARTESIAN_POINT('Ctrl Pts',(36.2904927310035,85.1141040762004,121.631453445884));
#35249=CARTESIAN_POINT('Ctrl Pts',(37.0841095554981,85.3542578208156,121.684102953615));
#35250=CARTESIAN_POINT('Ctrl Pts',(37.8777263799928,85.5944115654307,121.736752461346));
#35251=CARTESIAN_POINT('Ctrl Pts',(38.5413254828716,86.265467079336,121.789401969077));
#35252=CARTESIAN_POINT('Ctrl Pts',(38.774290752291,87.0597530844097,121.842051476808));
#35253=CARTESIAN_POINT('Ctrl Pts',(39.0072560217103,87.8540390894835,121.894700984538));
#35254=CARTESIAN_POINT('Ctrl Pts',(38.8095874576702,88.7715555857257,121.947350492269));
#35255=CARTESIAN_POINT('Ctrl Pts',(38.2683920713486,89.4045427919472,122.));
#35256=CARTESIAN_POINT('',(34.4378159219561,89.4070834740737,122.));
#35257=CARTESIAN_POINT('Origin',(36.3549260746835,87.7685555885722,122.));
#35258=CARTESIAN_POINT('Ctrl Pts',(34.437807076635,89.4070896409746,122.));
#35259=CARTESIAN_POINT('Ctrl Pts',(34.9606276647882,90.0158048705303,121.949053726697));
#35260=CARTESIAN_POINT('Ctrl Pts',(35.8003520975665,90.3559809225441,121.898107453395));
#35261=CARTESIAN_POINT('Ctrl Pts',(36.5990228929266,90.2782180814728,121.847161180092));
#35262=CARTESIAN_POINT('Ctrl Pts',(37.4243948286695,90.1978554752066,121.794511672361));
#35263=CARTESIAN_POINT('Ctrl Pts',(38.2059222332878,89.6711418033962,121.74186216463));
#35264=CARTESIAN_POINT('Ctrl Pts',(38.5898068286109,88.9363551220242,121.6892126569));
#35265=CARTESIAN_POINT('Ctrl Pts',(38.973691423934,88.2015684406522,121.636563149169));
#35266=CARTESIAN_POINT('Ctrl Pts',(38.9599332099619,87.2587087497187,121.583913641438));
#35267=CARTESIAN_POINT('Ctrl Pts',(38.5545284529765,86.5354489971012,121.531264133707));
#35268=CARTESIAN_POINT('Ctrl Pts',(38.1491236959911,85.8121892444836,121.478614625976));
#35269=CARTESIAN_POINT('Ctrl Pts',(37.3520723959923,85.3085294301821,121.425965118245));
#35270=CARTESIAN_POINT('Ctrl Pts',(36.5248227256852,85.2526784615377,121.373315610515));
#35271=CARTESIAN_POINT('Ctrl Pts',(35.6975730553781,85.1968274928934,121.320666102784));
#35272=CARTESIAN_POINT('Ctrl Pts',(34.8401250147627,85.5887853699062,121.268016595053));
#35273=CARTESIAN_POINT('Ctrl Pts',(34.3411326976743,86.2509211367476,121.215367087322));
#35274=CARTESIAN_POINT('Ctrl Pts',(34.01641729094,86.681800886756,121.181105825712));
#35275=CARTESIAN_POINT('Ctrl Pts',(33.8434955298159,87.2270916620838,121.146844564102));
#35276=CARTESIAN_POINT('Ctrl Pts',(33.8399314485466,87.7703173734778,121.112583302492));
#35277=CARTESIAN_POINT('Origin',(36.3549260746835,87.7685555885722,124.208423447177));
#35278=CARTESIAN_POINT('',(33.2766562951256,87.7693690681389,107.791576552823));
#35279=CARTESIAN_POINT('',(33.2862967608848,87.7688698663354,107.708423447177));
#35280=CARTESIAN_POINT('',(33.2814260746835,87.7685555885726,124.208423447177));
#35281=CARTESIAN_POINT('',(37.1487253572158,84.7993326348264,107.));
#35282=CARTESIAN_POINT('Ctrl Pts',(33.2862967608848,87.7688698663354,107.708423447177));
#35283=CARTESIAN_POINT('Ctrl Pts',(33.285976896235,88.2640453572287,107.682880329042));
#35284=CARTESIAN_POINT('Ctrl Pts',(33.6322291916214,89.7793619789749,107.604687703175));
#35285=CARTESIAN_POINT('Ctrl Pts',(36.0033916785668,91.377417939733,107.473845569577));
#35286=CARTESIAN_POINT('Ctrl Pts',(39.1869515218405,90.0369600534397,107.315897046385));
#35287=CARTESIAN_POINT('Ctrl Pts',(39.7977189680597,86.63477600283,107.157948523192));
#35288=CARTESIAN_POINT('Ctrl Pts',(38.1309639469874,85.0619266872038,107.052649507731));
#35289=CARTESIAN_POINT('Ctrl Pts',(37.1487253572157,84.7993326348264,107.));
#35290=CARTESIAN_POINT('',(35.5611267921501,84.7993326348267,107.));
#35291=CARTESIAN_POINT('Origin',(36.3549260746835,87.7685555885722,107.));
#35292=CARTESIAN_POINT('Ctrl Pts',(33.2766562951256,87.7693690681389,107.791576552822));
#35293=CARTESIAN_POINT('Ctrl Pts',(33.2765002261982,87.813877907838,107.789262006108));
#35294=CARTESIAN_POINT('Ctrl Pts',(33.2974599420536,88.8706873775284,107.734297951662));
#35295=CARTESIAN_POINT('Ctrl Pts',(34.5067288269183,90.8887184689395,107.626684389486));
#35296=CARTESIAN_POINT('Ctrl Pts',(37.957394655155,91.0220939825006,107.468735866293));
#35297=CARTESIAN_POINT('Ctrl Pts',(39.9550037460998,88.2047806129811,107.310787343101));
#35298=CARTESIAN_POINT('Ctrl Pts',(38.702488609764,85.0282374153775,107.154542054336));
#35299=CARTESIAN_POINT('Ctrl Pts',(36.5061791859533,84.5433632538305,107.050946273303));
#35300=CARTESIAN_POINT('Ctrl Pts',(35.5592127316546,84.7942440238826,107.));
#35301=CARTESIAN_POINT('Origin',(36.3549260746835,87.7685555885722,124.208423447177));
#35302=CARTESIAN_POINT('',(33.2850145408684,87.7704209831421,108.791576552823));
#35303=CARTESIAN_POINT('',(33.2798329301067,87.7659973109231,108.708423447177));
#35304=CARTESIAN_POINT('',(33.2814260746835,87.7685555885726,124.208423447177));
#35305=CARTESIAN_POINT('Ctrl Pts',(33.2798329301067,87.7659973109231,108.708423447178));
#35306=CARTESIAN_POINT('Ctrl Pts',(33.28722078683,88.5947453986223,108.665444042093));
#35307=CARTESIAN_POINT('Ctrl Pts',(34.0588698820238,90.4508359457567,108.569815129278));
#35308=CARTESIAN_POINT('Ctrl Pts',(37.1879239641774,91.2981289902626,108.421536708732));
#35309=CARTESIAN_POINT('Ctrl Pts',(39.7658203407947,89.0005544503459,108.26358818554));
#35310=CARTESIAN_POINT('Ctrl Pts',(39.2510963194207,85.5858974977915,108.105639662347));
#35311=CARTESIAN_POINT('Ctrl Pts',(36.1106391940357,84.1503270588856,107.947691139155));
#35312=CARTESIAN_POINT('Ctrl Pts',(33.6634843338243,85.6966940980861,107.815285734098));
#35313=CARTESIAN_POINT('Ctrl Pts',(33.2866362016597,87.2433890028545,107.735529836772));
#35314=CARTESIAN_POINT('Ctrl Pts',(33.2862967608848,87.7688698663354,107.708423447177));
#35315=CARTESIAN_POINT('Ctrl Pts',(33.2850145408684,87.7704209831421,108.791576552823));
#35316=CARTESIAN_POINT('Ctrl Pts',(33.2828704095411,88.1529039380672,108.771825719159));
#35317=CARTESIAN_POINT('Ctrl Pts',(33.5258648203393,89.5523399236073,108.699425377765));
#35318=CARTESIAN_POINT('Ctrl Pts',(35.6128383205754,91.3183646214857,108.57437552864));
#35319=CARTESIAN_POINT('Ctrl Pts',(38.9216914949492,90.3305042873106,108.416427005448));
#35320=CARTESIAN_POINT('Ctrl Pts',(39.9033345805337,87.019792348641,108.258478482255));
#35321=CARTESIAN_POINT('Ctrl Pts',(37.667747597468,84.3879831424088,108.100529959063));
#35322=CARTESIAN_POINT('Ctrl Pts',(34.2920593632494,84.8148430265618,107.944895982585));
#35323=CARTESIAN_POINT('Ctrl Pts',(33.280050360721,86.80142545452,107.841911513838));
#35324=CARTESIAN_POINT('Ctrl Pts',(33.2766562951256,87.7693690681389,107.791576552822));
#35325=CARTESIAN_POINT('Origin',(36.3549260746835,87.7685555885722,124.208423447177));
#35326=CARTESIAN_POINT('',(33.2830912889668,87.7659629281698,109.791576552823));
#35327=CARTESIAN_POINT('',(33.2787949818699,87.7708236399759,109.708423447177));
#35328=CARTESIAN_POINT('',(33.2814260746835,87.7685555885726,124.208423447177));
#35329=CARTESIAN_POINT('Ctrl Pts',(33.2787949818699,87.7708236399759,109.708423447177));
#35330=CARTESIAN_POINT('Ctrl Pts',(33.2775558603757,87.9204433996099,109.700657262876));
#35331=CARTESIAN_POINT('Ctrl Pts',(33.3552187612325,89.0830934618413,109.640241570843));
#35332=CARTESIAN_POINT('Ctrl Pts',(34.836575933406,91.0619526923221,109.527176371079));
#35333=CARTESIAN_POINT('Ctrl Pts',(38.2826269365773,90.8403335175675,109.369227847887));
#35334=CARTESIAN_POINT('Ctrl Pts',(39.9808906224645,87.8336271456654,109.211279324694));
#35335=CARTESIAN_POINT('Ctrl Pts',(38.3916016557803,84.7679214934147,109.053330801502));
#35336=CARTESIAN_POINT('Ctrl Pts',(34.9557226837823,84.4228013221572,108.89538227831));
#35337=CARTESIAN_POINT('Ctrl Pts',(33.3781907756738,86.3796382265152,108.780413160201));
#35338=CARTESIAN_POINT('Ctrl Pts',(33.2781707076373,87.5795340720654,108.718093549824));
#35339=CARTESIAN_POINT('Ctrl Pts',(33.2798329301067,87.7659973109231,108.708423447178));
#35340=CARTESIAN_POINT('Ctrl Pts',(33.2830912889669,87.7659629281698,109.791576552823));
#35341=CARTESIAN_POINT('Ctrl Pts',(33.2889507344551,88.4849690844241,109.754389432211));
#35342=CARTESIAN_POINT('Ctrl Pts',(33.8981616653641,90.2308908653449,109.664552803868));
#35343=CARTESIAN_POINT('Ctrl Pts',(36.7983710512446,91.3678894898621,109.522066667795));
#35344=CARTESIAN_POINT('Ctrl Pts',(39.6112488575384,89.3648670312859,109.364118144603));
#35345=CARTESIAN_POINT('Ctrl Pts',(39.4717178074565,85.914517396569,109.20616962141));
#35346=CARTESIAN_POINT('Ctrl Pts',(36.5062865391415,84.1451680917577,109.048221098218));
#35347=CARTESIAN_POINT('Ctrl Pts',(33.7915971699313,85.4714805121635,108.910023408688));
#35348=CARTESIAN_POINT('Ctrl Pts',(33.2885859889854,87.1333247326767,108.82447522689));
#35349=CARTESIAN_POINT('Ctrl Pts',(33.2850145408684,87.7704209831421,108.791576552823));
#35350=CARTESIAN_POINT('Origin',(36.3549260746835,87.7685555885722,124.208423447177));
#35351=CARTESIAN_POINT('',(33.276584510365,87.769240395449,110.791576552823));
#35352=CARTESIAN_POINT('',(33.2862066546329,87.7689040049629,110.708423447177));
#35353=CARTESIAN_POINT('',(33.2814260746835,87.7685555885726,124.208423447177));
#35354=CARTESIAN_POINT('Ctrl Pts',(33.2862066546329,87.7689040049629,110.708423447177));
#35355=CARTESIAN_POINT('Ctrl Pts',(33.2857073591617,88.2574355602479,110.683220975927));
#35356=CARTESIAN_POINT('Ctrl Pts',(33.6253684480904,89.7658836642612,110.605368996946));
#35357=CARTESIAN_POINT('Ctrl Pts',(35.980893460476,91.3757637943158,110.474867510234));
#35358=CARTESIAN_POINT('Ctrl Pts',(39.1709558328596,90.0536874920861,110.316918987042));
#35359=CARTESIAN_POINT('Ctrl Pts',(39.8078096748032,86.6597515977284,110.158970463849));
#35360=CARTESIAN_POINT('Ctrl Pts',(37.3140389596571,84.2711345475141,110.001021940657));
#35361=CARTESIAN_POINT('Ctrl Pts',(34.1160435691142,85.0150534951715,109.850839601766));
#35362=CARTESIAN_POINT('Ctrl Pts',(33.2859562709446,86.906122030792,109.753306770606));
#35363=CARTESIAN_POINT('Ctrl Pts',(33.2787949818699,87.7708236399759,109.708423447177));
#35364=CARTESIAN_POINT('Ctrl Pts',(33.276584510365,87.769240395449,110.791576552823));
#35365=CARTESIAN_POINT('Ctrl Pts',(33.276468866392,87.8071966833456,110.789602652993));
#35366=CARTESIAN_POINT('Ctrl Pts',(33.2942328067559,88.8574441094525,110.734979245433));
#35367=CARTESIAN_POINT('Ctrl Pts',(34.4867513670091,90.8768945953326,110.627706330142));
#35368=CARTESIAN_POINT('Ctrl Pts',(37.9364315807433,91.0320948408579,110.46975780695));
#35369=CARTESIAN_POINT('Ctrl Pts',(39.9522088516144,88.2283433032996,110.311809283757));
#35370=CARTESIAN_POINT('Ctrl Pts',(38.7064392347119,85.0077162267496,110.153860760565));
#35371=CARTESIAN_POINT('Ctrl Pts',(35.3286241543516,84.290258236255,109.995912237372));
#35372=CARTESIAN_POINT('Ctrl Pts',(33.4575133987375,86.1528900623526,109.875150834792));
#35373=CARTESIAN_POINT('Ctrl Pts',(33.2806549343109,87.4670005092958,109.807038939942));
#35374=CARTESIAN_POINT('Ctrl Pts',(33.2830912889669,87.7659629281698,109.791576552823));
#35375=CARTESIAN_POINT('Origin',(36.3549260746835,87.7685555885722,124.208423447177));
#35376=CARTESIAN_POINT('',(33.2848888934257,87.7704976439917,111.791576552823));
#35377=CARTESIAN_POINT('',(33.2800258531095,87.7659597947519,111.708423447178));
#35378=CARTESIAN_POINT('',(33.2814260746835,87.7685555885726,124.208423447177));
#35379=CARTESIAN_POINT('Ctrl Pts',(33.2800258531095,87.7659597947519,111.708423447177));
#35380=CARTESIAN_POINT('Ctrl Pts',(33.2874067328936,88.5882718431644,111.665784688979));
#35381=CARTESIAN_POINT('Ctrl Pts',(34.0488667182543,90.4380268123453,111.570496423049));
#35382=CARTESIAN_POINT('Ctrl Pts',(37.1652522149781,91.3034138569667,111.422558649389));
#35383=CARTESIAN_POINT('Ctrl Pts',(39.7578212468625,89.0224119911016,111.264610126197));
#35384=CARTESIAN_POINT('Ctrl Pts',(39.2650887205849,85.6045766594567,111.106661603004));
#35385=CARTESIAN_POINT('Ctrl Pts',(36.1338002317116,84.1487552082432,110.948713079812));
#35386=CARTESIAN_POINT('Ctrl Pts',(33.6706421352838,85.6835151702931,110.81596702787));
#35387=CARTESIAN_POINT('Ctrl Pts',(33.2867504180154,87.2368631869536,110.735870483658));
#35388=CARTESIAN_POINT('Ctrl Pts',(33.2862066546329,87.7689040049629,110.708423447177));
#35389=CARTESIAN_POINT('Ctrl Pts',(33.2848888934257,87.7704976439917,111.791576552823));
#35390=CARTESIAN_POINT('Ctrl Pts',(33.2826892164494,88.1463451423912,111.772166366045));
#35391=CARTESIAN_POINT('Ctrl Pts',(33.5201235146107,89.5389847191594,111.700106671536));
#35392=CARTESIAN_POINT('Ctrl Pts',(35.5900605517025,91.3135279228,111.575397469297));
#35393=CARTESIAN_POINT('Ctrl Pts',(38.9051877964048,90.346929740897,111.417448946105));
#35394=CARTESIAN_POINT('Ctrl Pts',(39.9080703007288,87.0425981327984,111.259500422912));
#35395=CARTESIAN_POINT('Ctrl Pts',(37.6894249992898,84.3964700708273,111.10155189972));
#35396=CARTESIAN_POINT('Ctrl Pts',(34.3036776321515,84.8025700881101,110.945577276356));
#35397=CARTESIAN_POINT('Ctrl Pts',(33.279553419195,86.794794816033,110.842252160724));
#35398=CARTESIAN_POINT('Ctrl Pts',(33.276584510365,87.769240395449,110.791576552823));
#35399=CARTESIAN_POINT('Origin',(36.3549260746835,87.7685555885722,124.208423447177));
#35400=CARTESIAN_POINT('',(33.2832673812772,87.7659995884264,112.791576552823));
#35401=CARTESIAN_POINT('',(33.2786192000661,87.7707578837754,112.708423447177));
#35402=CARTESIAN_POINT('',(33.2814260746835,87.7685555885726,124.208423447177));
#35403=CARTESIAN_POINT('Ctrl Pts',(33.2786192000661,87.7707578837754,112.708423447177));
#35404=CARTESIAN_POINT('Ctrl Pts',(33.2774583365245,87.9137935758715,112.700997909761));
#35405=CARTESIAN_POINT('Ctrl Pts',(33.3512646696384,89.0697957630776,112.640922864614));
#35406=CARTESIAN_POINT('Ctrl Pts',(34.8154602798326,91.0521354182212,112.528198311736));
#35407=CARTESIAN_POINT('Ctrl Pts',(38.2628634325534,90.8526480757781,112.370249788544));
#35408=CARTESIAN_POINT('Ctrl Pts',(39.9803978101849,87.856907873618,112.212301265351));
#35409=CARTESIAN_POINT('Ctrl Pts',(38.4108272289767,84.7810613417211,112.054352742159));
#35410=CARTESIAN_POINT('Ctrl Pts',(34.977233598576,84.4138849829118,111.896404218966));
#35411=CARTESIAN_POINT('Ctrl Pts',(33.3824603545734,86.36632237616,111.781094453973));
#35412=CARTESIAN_POINT('Ctrl Pts',(33.2782929663659,87.5728969500129,111.71843419671));
#35413=CARTESIAN_POINT('Ctrl Pts',(33.2800258531095,87.7659597947519,111.708423447177));
#35414=CARTESIAN_POINT('Ctrl Pts',(33.2832673812772,87.7659995884264,112.791576552823));
#35415=CARTESIAN_POINT('Ctrl Pts',(33.2889664337279,88.478522942157,112.754730079096));
#35416=CARTESIAN_POINT('Ctrl Pts',(33.8893177002825,90.2178279476355,112.66523409764));
#35417=CARTESIAN_POINT('Ctrl Pts',(36.7752505958151,91.3706626685477,112.523088608452));
#35418=CARTESIAN_POINT('Ctrl Pts',(39.6009318089752,89.3857429282516,112.365140085259));
#35419=CARTESIAN_POINT('Ctrl Pts',(39.4835583456547,85.9345686115981,112.207191562067));
#35420=CARTESIAN_POINT('Ctrl Pts',(36.5295491552939,84.1462145087741,112.049243038874));
#35421=CARTESIAN_POINT('Ctrl Pts',(33.799687217845,85.4582952370342,111.91070470246));
#35422=CARTESIAN_POINT('Ctrl Pts',(33.2886557695433,87.1268708838871,111.824815873776));
#35423=CARTESIAN_POINT('Ctrl Pts',(33.2848888934257,87.7704976439917,111.791576552823));
#35424=CARTESIAN_POINT('Origin',(36.3549260746835,87.7685555885722,124.208423447177));
#35425=CARTESIAN_POINT('',(33.2765252740224,87.769124500281,113.791576552823));
#35426=CARTESIAN_POINT('',(33.2861807775267,87.7690089236533,113.708423447177));
#35427=CARTESIAN_POINT('',(33.2814260746835,87.7685555885726,124.208423447177));
#35428=CARTESIAN_POINT('Ctrl Pts',(33.2861807775267,87.7690089236533,113.708423447177));
#35429=CARTESIAN_POINT('Ctrl Pts',(33.2855396007978,88.2509271303222,113.683561622813));
#35430=CARTESIAN_POINT('Ctrl Pts',(33.618721374071,89.7525576542612,113.606050290718));
#35431=CARTESIAN_POINT('Ctrl Pts',(35.9577392922369,91.3732877687825,113.475889450891));
#35432=CARTESIAN_POINT('Ctrl Pts',(39.1562249541521,90.071722108623,113.317940927699));
#35433=CARTESIAN_POINT('Ctrl Pts',(39.8148581197072,86.6819454123766,113.159992404506));
#35434=CARTESIAN_POINT('Ctrl Pts',(37.3364761291159,84.2773651151324,113.002043881314));
#35435=CARTESIAN_POINT('Ctrl Pts',(34.1265054947725,85.0023751466479,112.851520895538));
#35436=CARTESIAN_POINT('Ctrl Pts',(33.2856892416539,86.8996233744842,112.753647417492));
#35437=CARTESIAN_POINT('Ctrl Pts',(33.2786192000661,87.7707578837754,112.708423447177));
#35438=CARTESIAN_POINT('Ctrl Pts',(33.2765252740224,87.769124500281,113.791576552822));
#35439=CARTESIAN_POINT('Ctrl Pts',(33.276444590752,87.800528839304,113.789943299879));
#35440=CARTESIAN_POINT('Ctrl Pts',(33.2910497583934,88.8442059367107,113.735660539204));
#35441=CARTESIAN_POINT('Ctrl Pts',(34.4668312392973,90.8648349705502,113.628728270799));
#35442=CARTESIAN_POINT('Ctrl Pts',(37.915443798023,91.0421824081436,113.470779747607));
#35443=CARTESIAN_POINT('Ctrl Pts',(39.9491823979981,88.2514319712908,113.312831224414));
#35444=CARTESIAN_POINT('Ctrl Pts',(38.7241181039884,85.0228722042484,113.154882701222));
#35445=CARTESIAN_POINT('Ctrl Pts',(35.3509794527264,84.2837400555871,112.996934178029));
#35446=CARTESIAN_POINT('Ctrl Pts',(33.4626356089268,86.1395392509273,112.875832128563));
#35447=CARTESIAN_POINT('Ctrl Pts',(33.2808231224224,87.4604064162848,112.807379586827));
#35448=CARTESIAN_POINT('Ctrl Pts',(33.2832673812772,87.7659995884264,112.791576552823));
#35449=CARTESIAN_POINT('Origin',(36.3549260746835,87.7685555885722,124.208423447177));
#35450=CARTESIAN_POINT('',(33.2847579912934,87.7705715943706,114.791576552823));
#35451=CARTESIAN_POINT('',(33.2802200364225,87.76592664843,114.708423447178));
#35452=CARTESIAN_POINT('',(33.2814260746835,87.7685555885726,124.208423447177));
#35453=CARTESIAN_POINT('Ctrl Pts',(33.2802200364225,87.76592664843,114.708423447177));
#35454=CARTESIAN_POINT('Ctrl Pts',(33.287581867814,88.5818020912728,114.666125335864));
#35455=CARTESIAN_POINT('Ctrl Pts',(34.0389365462666,90.4252032852303,114.571177716821));
#35456=CARTESIAN_POINT('Ctrl Pts',(37.1425381909624,91.3085440893281,114.423580590046));
#35457=CARTESIAN_POINT('Ctrl Pts',(39.749700086851,89.0442361275419,114.265632066853));
#35458=CARTESIAN_POINT('Ctrl Pts',(39.2789236332919,85.6233074191414,114.107683543661));
#35459=CARTESIAN_POINT('Ctrl Pts',(36.1570475227083,84.1474099811903,113.949735020469));
#35460=CARTESIAN_POINT('Ctrl Pts',(33.6777395096476,85.6702201339644,113.816648321641));
#35461=CARTESIAN_POINT('Ctrl Pts',(33.2868974110151,87.2303762658505,113.736211130544));
#35462=CARTESIAN_POINT('Ctrl Pts',(33.2861807775267,87.7690089236533,113.708423447177));
#35463=CARTESIAN_POINT('Ctrl Pts',(33.2847579912934,87.7705715943706,114.791576552823));
#35464=CARTESIAN_POINT('Ctrl Pts',(33.2825084886882,88.1397834143597,114.772507012931));
#35465=CARTESIAN_POINT('Ctrl Pts',(33.5144368848445,89.5256293817944,114.700787965308));
#35466=CARTESIAN_POINT('Ctrl Pts',(35.5673140575926,91.308543643525,114.576419409954));
#35467=CARTESIAN_POINT('Ctrl Pts',(38.8885794869123,90.3632518146024,114.418470886761));
#35468=CARTESIAN_POINT('Ctrl Pts',(39.9126584249495,87.0654278316568,114.260522363569));
#35469=CARTESIAN_POINT('Ctrl Pts',(37.7110496445387,84.4051084012425,114.102573840377));
#35470=CARTESIAN_POINT('Ctrl Pts',(34.3153645284242,84.7902995884757,113.946258570128));
#35471=CARTESIAN_POINT('Ctrl Pts',(33.2790454949687,86.7881792233995,113.84259280761));
#35472=CARTESIAN_POINT('Ctrl Pts',(33.2765252740224,87.769124500281,113.791576552822));
#35473=CARTESIAN_POINT('Origin',(36.3549260746835,87.7685555885722,124.208423447177));
#35474=CARTESIAN_POINT('',(33.2834401666397,87.7660402135948,115.791576552823));
#35475=CARTESIAN_POINT('',(33.2784472978679,87.7706880983643,115.708423447177));
#35476=CARTESIAN_POINT('',(33.2814260746835,87.7685555885726,124.208423447177));
#35477=CARTESIAN_POINT('Ctrl Pts',(33.2784472978679,87.7706880983643,115.708423447178));
#35478=CARTESIAN_POINT('Ctrl Pts',(33.277364762304,87.9071421036308,115.701338556647));
#35479=CARTESIAN_POINT('Ctrl Pts',(33.3473574841613,89.0565012331312,115.641604158386));
#35480=CARTESIAN_POINT('Ctrl Pts',(34.7944081548233,91.0421828204038,115.529220252393));
#35481=CARTESIAN_POINT('Ctrl Pts',(38.2430211478453,90.8648353604754,115.371271729201));
#35482=CARTESIAN_POINT('Ctrl Pts',(39.9797557618474,87.8801852004548,115.213323206008));
#35483=CARTESIAN_POINT('Ctrl Pts',(38.4299675427095,84.7943238664015,115.055374682816));
#35484=CARTESIAN_POINT('Ctrl Pts',(34.9988023340458,84.4051079776717,114.897426159623));
#35485=CARTESIAN_POINT('Ctrl Pts',(33.386777168059,86.353002585266,114.781775747744));
#35486=CARTESIAN_POINT('Ctrl Pts',(33.2784184137796,87.5662617018335,114.718774843595));
#35487=CARTESIAN_POINT('Ctrl Pts',(33.2802200364225,87.76592664843,114.708423447177));
#35488=CARTESIAN_POINT('Ctrl Pts',(33.2834401666397,87.7660402135947,115.791576552823));
#35489=CARTESIAN_POINT('Ctrl Pts',(33.2889737590442,88.472076855709,115.755070725982));
#35490=CARTESIAN_POINT('Ctrl Pts',(33.8805399135678,90.2047528694839,115.665915391411));
#35491=CARTESIAN_POINT('Ctrl Pts',(36.752112807112,91.3732873148253,115.524110549109));
#35492=CARTESIAN_POINT('Ctrl Pts',(39.5904809358262,89.4065521878392,115.366162025916));
#35493=CARTESIAN_POINT('Ctrl Pts',(39.4952698768951,85.954695361712,115.208213502724));
#35494=CARTESIAN_POINT('Ctrl Pts',(36.5528046017381,84.1474104372141,115.050264979531));
#35495=CARTESIAN_POINT('Ctrl Pts',(33.8078411360195,85.4451187391524,114.911385996231));
#35496=CARTESIAN_POINT('Ctrl Pts',(33.2887191893906,87.1204184647656,114.825156520661));
#35497=CARTESIAN_POINT('Ctrl Pts',(33.2847579912934,87.7705715943706,114.791576552823));
#35498=CARTESIAN_POINT('Origin',(36.3549260746835,87.7685555885722,124.208423447177));
#35499=CARTESIAN_POINT('',(33.2764763687653,87.7690073305752,116.791576552823));
#35500=CARTESIAN_POINT('',(33.286148132912,87.7691131822086,116.708423447177));
#35501=CARTESIAN_POINT('',(33.2814260746835,87.7685555885726,124.208423447177));
#35502=CARTESIAN_POINT('Ctrl Pts',(33.286148132912,87.7691131822085,116.708423447177));
#35503=CARTESIAN_POINT('Ctrl Pts',(33.2853698282698,88.2444156975363,116.683902269699));
#35504=CARTESIAN_POINT('Ctrl Pts',(33.6121326413799,89.7392284566303,116.606731584489));
#35505=CARTESIAN_POINT('Ctrl Pts',(35.93460150062,91.3706631221744,116.476911391548));
#35506=CARTESIAN_POINT('Ctrl Pts',(39.1413785773383,90.0896617648689,116.318962868356));
#35507=CARTESIAN_POINT('Ctrl Pts',(39.8217639160215,86.7041840307689,116.161014345163));
#35508=CARTESIAN_POINT('Ctrl Pts',(37.3588728230703,84.2837396167312,116.003065821971));
#35509=CARTESIAN_POINT('Ctrl Pts',(34.1370382392348,84.9897175692517,115.852202189309));
#35510=CARTESIAN_POINT('Ctrl Pts',(33.2854093417222,86.8931199145531,115.753988064378));
#35511=CARTESIAN_POINT('Ctrl Pts',(33.2784472978679,87.7706880983643,115.708423447178));
#35512=CARTESIAN_POINT('Ctrl Pts',(33.2764763687653,87.7690073305752,116.791576552823));
#35513=CARTESIAN_POINT('Ctrl Pts',(33.2764248815123,87.7938606187569,116.790283946765));
#35514=CARTESIAN_POINT('Ctrl Pts',(33.2879103688746,88.830971516364,116.736341832976));
#35515=CARTESIAN_POINT('Ctrl Pts',(34.446988957088,90.8526476873878,116.629750211456));
#35516=CARTESIAN_POINT('Ctrl Pts',(37.894391675665,91.0521350047077,116.471801688264));
#35517=CARTESIAN_POINT('Ctrl Pts',(39.9460077545616,88.2745007309714,116.313853165071));
#35518=CARTESIAN_POINT('Ctrl Pts',(38.7416992921252,85.0381413842478,116.155904641879));
#35519=CARTESIAN_POINT('Ctrl Pts',(35.3733761438603,84.2773655547908,115.997956118686));
#35520=CARTESIAN_POINT('Ctrl Pts',(33.467810029404,86.1261873874685,115.876513422334));
#35521=CARTESIAN_POINT('Ctrl Pts',(33.2809930901675,87.453815255726,115.807720233713));
#35522=CARTESIAN_POINT('Ctrl Pts',(33.2834401666397,87.7660402135947,115.791576552823));
#35523=CARTESIAN_POINT('Origin',(36.3549260746835,87.7685555885722,124.208423447177));
#35524=CARTESIAN_POINT('',(33.2846219536775,87.7706425235964,117.791576552823));
#35525=CARTESIAN_POINT('',(33.2804152395068,87.7658979718733,117.708423447177));
#35526=CARTESIAN_POINT('',(33.2814260746835,87.7685555885726,124.208423447177));
#35527=CARTESIAN_POINT('Ctrl Pts',(33.2804152395068,87.7658979718733,117.708423447177));
#35528=CARTESIAN_POINT('Ctrl Pts',(33.2877456579952,88.5753352182883,117.66646598275));
#35529=CARTESIAN_POINT('Ctrl Pts',(34.029075680634,90.4123622121681,117.571859010592));
#35530=CARTESIAN_POINT('Ctrl Pts',(37.1197916939879,91.3135283692309,117.424602530703));
#35531=CARTESIAN_POINT('Ctrl Pts',(39.7414389614906,89.0660076681044,117.26665400751));
#35532=CARTESIAN_POINT('Ctrl Pts',(39.2926379906584,85.6421266266902,117.108705484318));
#35533=CARTESIAN_POINT('Ctrl Pts',(36.1803029720811,84.1462140525996,116.950756961126));
#35534=CARTESIAN_POINT('Ctrl Pts',(33.6848972085276,85.6569301160522,116.817329615412));
#35535=CARTESIAN_POINT('Ctrl Pts',(33.2870409289463,87.223891969559,116.736551777429));
#35536=CARTESIAN_POINT('Ctrl Pts',(33.286148132912,87.7691131822085,116.708423447177));
#35537=CARTESIAN_POINT('Ctrl Pts',(33.2846219536775,87.7706425235964,117.791576552823));
#35538=CARTESIAN_POINT('Ctrl Pts',(33.282328321745,88.1332185350583,117.772847659816));
#35539=CARTESIAN_POINT('Ctrl Pts',(33.5088046545594,89.5122738095575,117.701469259079));
#35540=CARTESIAN_POINT('Ctrl Pts',(35.5446000364372,91.3034134118094,117.577441350611));
#35541=CARTESIAN_POINT('Ctrl Pts',(38.8718667157924,90.3794669098942,117.419492827418));
#35542=CARTESIAN_POINT('Ctrl Pts',(39.9170998651258,87.0882865202323,117.261544304226));
#35543=CARTESIAN_POINT('Ctrl Pts',(37.7326183772922,84.4138854053773,117.103595781033));
#35544=CARTESIAN_POINT('Ctrl Pts',(34.3271247352706,84.778056850815,116.946939863899));
#35545=CARTESIAN_POINT('Ctrl Pts',(33.2785220235664,86.7815542163916,116.842933454495));
#35546=CARTESIAN_POINT('Ctrl Pts',(33.2764763687653,87.7690073305752,116.791576552823));
#35547=CARTESIAN_POINT('Origin',(36.3549260746835,87.7685555885722,124.208423447177));
#35548=CARTESIAN_POINT('',(33.2836094246712,87.7660847245338,118.791576552823));
#35549=CARTESIAN_POINT('',(33.2782796381252,87.770614382798,118.708423447178));
#35550=CARTESIAN_POINT('',(33.2814260746835,87.7685555885726,124.208423447177));
#35551=CARTESIAN_POINT('Ctrl Pts',(33.2782796381252,87.770614382798,118.708423447178));
#35552=CARTESIAN_POINT('Ctrl Pts',(33.2772752030302,87.9004890602186,118.701679203533));
#35553=CARTESIAN_POINT('Ctrl Pts',(33.3434970062078,89.0432099289289,118.642285452157));
#35554=CARTESIAN_POINT('Ctrl Pts',(34.7734203694599,91.0320952518487,118.53024219305));
#35555=CARTESIAN_POINT('Ctrl Pts',(38.223101017625,90.876894986776,118.372293669858));
#35556=CARTESIAN_POINT('Ctrl Pts',(39.9789642630779,87.9034579247835,118.214345146665));
#35557=CARTESIAN_POINT('Ctrl Pts',(38.4490223032137,84.8077090176302,118.056396623473));
#35558=CARTESIAN_POINT('Ctrl Pts',(35.020426982018,84.3964696461687,117.89844810028));
#35559=CARTESIAN_POINT('Ctrl Pts',(33.3911426763166,86.3396801807466,117.782457041515));
#35560=CARTESIAN_POINT('Ctrl Pts',(33.2785472250074,87.5596286415355,117.719115490481));
#35561=CARTESIAN_POINT('Ctrl Pts',(33.2804152395068,87.7658979718733,117.708423447177));
#35562=CARTESIAN_POINT('Ctrl Pts',(33.2836094246713,87.7660847245338,118.791576552823));
#35563=CARTESIAN_POINT('Ctrl Pts',(33.2889728976556,88.4656306785298,118.755411372868));
#35564=CARTESIAN_POINT('Ctrl Pts',(33.8718280977078,90.1916659326025,118.666596685182));
#35565=CARTESIAN_POINT('Ctrl Pts',(36.7289586417865,91.3757633400502,118.525132489766));
#35566=CARTESIAN_POINT('Ctrl Pts',(39.5798966622645,89.4272939130391,118.367183966573));
#35567=CARTESIAN_POINT('Ctrl Pts',(39.5068519326957,85.9748968968193,118.209235443381));
#35568=CARTESIAN_POINT('Ctrl Pts',(36.5760518898075,84.1487556640973,118.051286920188));
#35569=CARTESIAN_POINT('Ctrl Pts',(33.8160591927152,85.4319515714374,117.912067290002));
#35570=CARTESIAN_POINT('Ctrl Pts',(33.2887760382289,87.1139672364392,117.825497167547));
#35571=CARTESIAN_POINT('Ctrl Pts',(33.2846219536775,87.7706425235964,117.791576552823));
#35572=CARTESIAN_POINT('Origin',(36.3549260746835,87.7685555885722,124.208423447177));
#35573=CARTESIAN_POINT('',(33.2764381388873,87.7688891883613,119.791576552823));
#35574=CARTESIAN_POINT('',(33.2861087598917,87.7692166140277,119.708423447178));
#35575=CARTESIAN_POINT('',(33.2814260746835,87.7685555885726,124.208423447177));
#35576=CARTESIAN_POINT('Ctrl Pts',(33.2861087598917,87.7692166140277,119.708423447178));
#35577=CARTESIAN_POINT('Ctrl Pts',(33.2851982067878,88.237901225937,119.684242916584));
#35578=CARTESIAN_POINT('Ctrl Pts',(33.6056020130081,89.7258962979527,119.60741287826));
#35579=CARTESIAN_POINT('Ctrl Pts',(35.91148104228,91.3678899431996,119.477933332205));
#35580=CARTESIAN_POINT('Ctrl Pts',(39.1264173144016,90.1075057318468,119.319984809013));
#35581=CARTESIAN_POINT('Ctrl Pts',(39.8285267766549,86.7264665283904,119.16203628582));
#35582=CARTESIAN_POINT('Ctrl Pts',(37.3812281242605,84.2902577982121,119.004087762628));
#35583=CARTESIAN_POINT('Ctrl Pts',(34.1476419553814,84.9770811380528,118.85288348308));
#35584=CARTESIAN_POINT('Ctrl Pts',(33.2851164104484,86.8866114198347,118.754328711263));
#35585=CARTESIAN_POINT('Ctrl Pts',(33.2782796381252,87.770614382798,118.708423447178));
#35586=CARTESIAN_POINT('Ctrl Pts',(33.2764381388873,87.7688891883613,119.791576552823));
#35587=CARTESIAN_POINT('Ctrl Pts',(33.2764096940567,87.7871921565167,119.79062459365));
#35588=CARTESIAN_POINT('Ctrl Pts',(33.2848143365715,88.8177409867468,119.737023126747));
#35589=CARTESIAN_POINT('Ctrl Pts',(34.4272254557842,90.8403331303497,119.630772152113));
#35590=CARTESIAN_POINT('Ctrl Pts',(37.873276024629,91.0619522777656,119.47282362892));
#35591=CARTESIAN_POINT('Ctrl Pts',(39.9426850798466,88.2975486028455,119.314875105728));
#35592=CARTESIAN_POINT('Ctrl Pts',(38.7591820609565,85.0535231518079,119.156926582535));
#35593=CARTESIAN_POINT('Ctrl Pts',(35.3958133105107,84.2711349879319,118.998978059343));
#35594=CARTESIAN_POINT('Ctrl Pts',(33.4730368857783,86.1128345972822,118.877194716105));
#35595=CARTESIAN_POINT('Ctrl Pts',(33.2811647182768,87.4472270604913,118.808060880599));
#35596=CARTESIAN_POINT('Ctrl Pts',(33.2836094246713,87.7660847245338,118.791576552823));
#35597=CARTESIAN_POINT('Origin',(36.3549260746835,87.7685555885722,124.208423447177));
#35598=CARTESIAN_POINT('',(33.2844847704405,87.7707064707598,120.791576552823));
#35599=CARTESIAN_POINT('',(33.2806115013714,87.7658718718852,120.708423447177));
#35600=CARTESIAN_POINT('',(33.2814260746835,87.7685555885726,124.208423447177));
#35601=CARTESIAN_POINT('Ctrl Pts',(33.2806115013714,87.7658718718852,120.708423447177));
#35602=CARTESIAN_POINT('Ctrl Pts',(33.2878986300211,88.5688691391512,120.666806629636));
#35603=CARTESIAN_POINT('Ctrl Pts',(34.0192834572627,90.3995065690792,120.572540304363));
#35604=CARTESIAN_POINT('Ctrl Pts',(37.0970139225816,91.3183650716777,120.42562447136));
#35605=CARTESIAN_POINT('Ctrl Pts',(39.7330380846501,89.0877264053273,120.267675948167));
#35606=CARTESIAN_POINT('Ctrl Pts',(39.3062312888321,85.6610331706022,120.109727424975));
#35607=CARTESIAN_POINT('Ctrl Pts',(36.2035655911394,84.1451676350087,119.951778901782));
#35608=CARTESIAN_POINT('Ctrl Pts',(33.6921154687428,85.6436453024385,119.818010909183));
#35609=CARTESIAN_POINT('Ctrl Pts',(33.2871808006975,87.2174102155021,119.736892424315));
#35610=CARTESIAN_POINT('Ctrl Pts',(33.2861087598917,87.7692166140277,119.708423447178));
#35611=CARTESIAN_POINT('Ctrl Pts',(33.2844847704405,87.7707064707598,120.791576552823));
#35612=CARTESIAN_POINT('Ctrl Pts',(33.2821494402512,88.1266499264814,120.773188306702));
#35613=CARTESIAN_POINT('Ctrl Pts',(33.503214227886,89.498930569182,120.70215055285));
#35614=CARTESIAN_POINT('Ctrl Pts',(35.5219282988626,91.2981285259009,120.578463291268));
#35615=CARTESIAN_POINT('Ctrl Pts',(38.8550458568218,90.3955786925481,120.420514768075));
#35616=CARTESIAN_POINT('Ctrl Pts',(39.9213965365604,87.1111711483864,120.262566244883));
#35617=CARTESIAN_POINT('Ctrl Pts',(37.7541292878677,84.4228017462871,120.10461772169));
#35618=CARTESIAN_POINT('Ctrl Pts',(34.3389588652922,84.7658418233948,119.94762115767));
#35619=CARTESIAN_POINT('Ctrl Pts',(33.2779828774206,86.7749194757506,119.843274101381));
#35620=CARTESIAN_POINT('Ctrl Pts',(33.2764381388873,87.7688891883613,119.791576552823));
#35621=CARTESIAN_POINT('Origin',(36.3549260746835,87.7685555885722,124.208423447177));
#35622=CARTESIAN_POINT('',(33.2846474150427,87.7655400361929,121.791576552823));
#35623=CARTESIAN_POINT('',(33.2781263393751,87.7704832126689,121.708423447178));
#35624=CARTESIAN_POINT('',(33.2814260746835,87.7685555885726,124.208423447177));
#35625=CARTESIAN_POINT('',(35.5611267921504,84.7993326348266,122.));
#35626=CARTESIAN_POINT('Ctrl Pts',(35.5611267921505,84.7993326348266,122.));
#35627=CARTESIAN_POINT('Ctrl Pts',(34.5788882023788,85.0619266872043,121.947350492269));
#35628=CARTESIAN_POINT('Ctrl Pts',(33.4791914426982,86.0996627851545,121.877876009877));
#35629=CARTESIAN_POINT('Ctrl Pts',(33.2823062253025,87.4400641803626,121.808401527484));
#35630=CARTESIAN_POINT('Ctrl Pts',(33.2846474150427,87.7655400361928,121.791576552823));
#35631=CARTESIAN_POINT('',(37.1506349127216,84.7942560800323,122.));
#35632=CARTESIAN_POINT('Origin',(36.3549260746835,87.7685555885722,122.));
#35633=CARTESIAN_POINT('Ctrl Pts',(37.1506395481982,84.7942437566139,122.));
#35634=CARTESIAN_POINT('Ctrl Pts',(36.2036733898099,84.5433632815128,121.949053726697));
#35635=CARTESIAN_POINT('Ctrl Pts',(34.1431239694285,84.9982647715874,121.851861542423));
#35636=CARTESIAN_POINT('Ctrl Pts',(33.284789784195,86.880208399197,121.754669358149));
#35637=CARTESIAN_POINT('Ctrl Pts',(33.2781263393751,87.7704832126688,121.708423447178));
#35638=CARTESIAN_POINT('Origin',(87.7685555885722,36.3549260746835,114.));
#35639=CARTESIAN_POINT('',(85.2550451615384,36.3551834992055,107.387416697508));
#35640=CARTESIAN_POINT('',(85.252964853222,36.3513534825213,107.112583302492));
#35641=CARTESIAN_POINT('',(85.2510555885723,36.3549260746835,114.));
#35642=CARTESIAN_POINT('',(85.8550895919076,37.9909132780589,107.));
#35643=CARTESIAN_POINT('Ctrl Pts',(85.252964853222,36.3513534825213,107.112583302492));
#35644=CARTESIAN_POINT('Ctrl Pts',(85.2581102783477,36.9439881062406,107.075055534995));
#35645=CARTESIAN_POINT('Ctrl Pts',(85.4693337604884,37.5397296349884,107.037527767497));
#35646=CARTESIAN_POINT('Ctrl Pts',(85.8550895919077,37.9909132780591,107.));
#35647=CARTESIAN_POINT('',(85.2510555885723,36.3549260746835,107.));
#35648=CARTESIAN_POINT('Origin',(87.7685555885722,36.3549260746835,107.));
#35649=CARTESIAN_POINT('',(85.2510555885723,36.3549260746835,106.));
#35650=CARTESIAN_POINT('',(85.2510555885723,36.3549260746835,114.));
#35651=CARTESIAN_POINT('Origin',(87.7685555885722,36.3549260746835,106.));
#35652=CARTESIAN_POINT('',(89.6856659519484,37.9934540791198,107.));
#35653=CARTESIAN_POINT('Origin',(87.7685555885722,36.3549260746835,107.));
#35654=CARTESIAN_POINT('Ctrl Pts',(89.6856747987073,37.9934602469553,107.));
#35655=CARTESIAN_POINT('Ctrl Pts',(89.1628542734512,38.6021751401191,107.050946273303));
#35656=CARTESIAN_POINT('Ctrl Pts',(88.3231296868319,38.9423518194042,107.101892546605));
#35657=CARTESIAN_POINT('Ctrl Pts',(87.5244587588995,38.8645890944017,107.152838819908));
#35658=CARTESIAN_POINT('Ctrl Pts',(86.6990866861522,38.7842266080846,107.205488327639));
#35659=CARTESIAN_POINT('Ctrl Pts',(85.9175591672441,38.2575125102682,107.25813783537));
#35660=CARTESIAN_POINT('Ctrl Pts',(85.5336745304453,37.5227256538998,107.3107873431));
#35661=CARTESIAN_POINT('Ctrl Pts',(85.3474313716597,37.1662408872642,107.336330461236));
#35662=CARTESIAN_POINT('Ctrl Pts',(85.2547831608045,36.7607811235179,107.361873579372));
#35663=CARTESIAN_POINT('Ctrl Pts',(85.2550451615384,36.3551834992055,107.387416697508));
#35664=CARTESIAN_POINT('Origin',(87.7685555885722,36.3549260746835,114.));
#35665=CARTESIAN_POINT('',(85.249750645845,36.3528305926657,108.387416697508));
#35666=CARTESIAN_POINT('',(85.2471486681112,36.3555923947772,108.112583302492));
#35667=CARTESIAN_POINT('',(85.2510555885723,36.3549260746835,114.));
#35668=CARTESIAN_POINT('Ctrl Pts',(85.2471486681112,36.3555923947772,108.112583302492));
#35669=CARTESIAN_POINT('Ctrl Pts',(85.2470208322483,36.3920495296211,108.110268755777));
#35670=CARTESIAN_POINT('Ctrl Pts',(85.2477437832137,36.4285014277137,108.107954209062));
#35671=CARTESIAN_POINT('Ctrl Pts',(85.2493333996998,36.464915427552,108.105639662347));
#35672=CARTESIAN_POINT('Ctrl Pts',(85.2854927586503,37.2932327622759,108.052990154616));
#35673=CARTESIAN_POINT('Ctrl Pts',(85.7700961483552,38.1019401719081,108.000340646886));
#35674=CARTESIAN_POINT('Ctrl Pts',(86.48347051945,38.5245018294053,107.947691139155));
#35675=CARTESIAN_POINT('Ctrl Pts',(87.1968448905449,38.9470634869024,107.895041631424));
#35676=CARTESIAN_POINT('Ctrl Pts',(88.1389902430297,38.9834793922643,107.842392123693));
#35677=CARTESIAN_POINT('Ctrl Pts',(88.8827694366222,38.6170777029647,107.789742615962));
#35678=CARTESIAN_POINT('Ctrl Pts',(89.6265486302147,38.250676013665,107.737093108232));
#35679=CARTESIAN_POINT('Ctrl Pts',(90.1719616649149,37.4814567297037,107.684443600501));
#35680=CARTESIAN_POINT('Ctrl Pts',(90.2718152971076,36.6584694261649,107.63179409277));
#35681=CARTESIAN_POINT('Ctrl Pts',(90.3716689293003,35.8354821226262,107.579144585039));
#35682=CARTESIAN_POINT('Ctrl Pts',(90.0259631589855,34.9587267995101,107.526495077308));
#35683=CARTESIAN_POINT('Ctrl Pts',(89.3912932551831,34.4249748964641,107.473845569577));
#35684=CARTESIAN_POINT('Ctrl Pts',(88.7566233513807,33.8912229934181,107.421196061847));
#35685=CARTESIAN_POINT('Ctrl Pts',(87.8329893140907,33.7004745104421,107.368546554116));
#35686=CARTESIAN_POINT('Ctrl Pts',(87.0393721878608,33.9406285523688,107.315897046385));
#35687=CARTESIAN_POINT('Ctrl Pts',(86.2457550616309,34.1807825942955,107.263247538654));
#35688=CARTESIAN_POINT('Ctrl Pts',(85.5821548464612,34.8518391611248,107.210598030923));
#35689=CARTESIAN_POINT('Ctrl Pts',(85.3491896324499,35.6461250305103,107.157948523192));
#35690=CARTESIAN_POINT('Ctrl Pts',(85.2822784759824,35.8742560255688,107.142826782959));
#35691=CARTESIAN_POINT('Ctrl Pts',(85.2508915142698,36.1125525244339,107.127705042726));
#35692=CARTESIAN_POINT('Ctrl Pts',(85.252964853222,36.3513534825213,107.112583302492));
#35693=CARTESIAN_POINT('Ctrl Pts',(85.2550451615384,36.3551834992055,107.387416697508));
#35694=CARTESIAN_POINT('Ctrl Pts',(85.2553231970519,35.9247627821685,107.414523087103));
#35695=CARTESIAN_POINT('Ctrl Pts',(85.3602318955731,35.49418681371,107.441629476698));
#35696=CARTESIAN_POINT('Ctrl Pts',(85.5689529493409,35.1218193835969,107.468735866293));
#35697=CARTESIAN_POINT('Ctrl Pts',(85.9743577597246,34.398559584583,107.521385374024));
#35698=CARTESIAN_POINT('Ctrl Pts',(86.7714091351813,33.8948996014755,107.574034881755));
#35699=CARTESIAN_POINT('Ctrl Pts',(87.5986589058312,33.8390486012967,107.626684389485));
#35700=CARTESIAN_POINT('Ctrl Pts',(88.4259086764811,33.7831976011178,107.679333897216));
#35701=CARTESIAN_POINT('Ctrl Pts',(89.2833568423243,34.1751555838677,107.731983404947));
#35702=CARTESIAN_POINT('Ctrl Pts',(89.7823492254361,34.8372914473242,107.784632912678));
#35703=CARTESIAN_POINT('Ctrl Pts',(90.281341608548,35.4994273107807,107.837282420409));
#35704=CARTESIAN_POINT('Ctrl Pts',(90.4218782089285,36.4317410549438,107.889931928139));
#35705=CARTESIAN_POINT('Ctrl Pts',(90.1402212269685,37.2115546649594,107.94258143587));
#35706=CARTESIAN_POINT('Ctrl Pts',(89.8585642450085,37.9913682749749,107.995230943601));
#35707=CARTESIAN_POINT('Ctrl Pts',(89.1547136807079,38.6186817508428,108.047880451332));
#35708=CARTESIAN_POINT('Ctrl Pts',(88.3477629366261,38.8091255628108,108.100529959063));
#35709=CARTESIAN_POINT('Ctrl Pts',(87.5408121925443,38.9995693747789,108.153179466794));
#35710=CARTESIAN_POINT('Ctrl Pts',(86.6307612686814,38.7531435228472,108.205828974524));
#35711=CARTESIAN_POINT('Ctrl Pts',(86.030161371803,38.1815548583619,108.258478482255));
#35712=CARTESIAN_POINT('Ctrl Pts',(85.5398732879433,37.7149495317159,108.301457887339));
#35713=CARTESIAN_POINT('Ctrl Pts',(85.2558020300327,37.0316571131741,108.344437292424));
#35714=CARTESIAN_POINT('Ctrl Pts',(85.249750645845,36.3528305926657,108.387416697508));
#35715=CARTESIAN_POINT('Origin',(87.7685555885722,36.3549260746835,114.));
#35716=CARTESIAN_POINT('',(85.2489004637444,36.356783832747,109.387416697508));
#35717=CARTESIAN_POINT('',(85.2539948967292,36.356454017039,109.112583302492));
#35718=CARTESIAN_POINT('',(85.2510555885723,36.3549260746835,114.));
#35719=CARTESIAN_POINT('Ctrl Pts',(85.2539948967292,36.356454017039,109.112583302492));
#35720=CARTESIAN_POINT('Ctrl Pts',(85.2522386414448,36.6697453263034,109.092832468829));
#35721=CARTESIAN_POINT('Ctrl Pts',(85.3065358325806,36.982449815841,109.073081635165));
#35722=CARTESIAN_POINT('Ctrl Pts',(85.4196754020532,37.2721759899556,109.053330801502));
#35723=CARTESIAN_POINT('Ctrl Pts',(85.7212698936659,38.0444948046395,109.000681293771));
#35724=CARTESIAN_POINT('Ctrl Pts',(86.4409911662098,38.6535325057685,108.94803178604));
#35725=CARTESIAN_POINT('Ctrl Pts',(87.2525647175344,38.8231921626186,108.89538227831));
#35726=CARTESIAN_POINT('Ctrl Pts',(88.064138268859,38.9928518194688,108.842732770579));
#35727=CARTESIAN_POINT('Ctrl Pts',(88.9675640989643,38.7231334320402,108.790083262848));
#35728=CARTESIAN_POINT('Ctrl Pts',(89.5532874509759,38.1363075713555,108.737433755117));
#35729=CARTESIAN_POINT('Ctrl Pts',(90.1390108029874,37.5494817106708,108.684784247386));
#35730=CARTESIAN_POINT('Ctrl Pts',(90.4070316769052,36.64554837673,108.632134739655));
#35731=CARTESIAN_POINT('Ctrl Pts',(90.2358476976249,35.8342964390754,108.579485231925));
#35732=CARTESIAN_POINT('Ctrl Pts',(90.0646637183446,35.0230445014207,108.526835724194));
#35733=CARTESIAN_POINT('Ctrl Pts',(89.4542748858661,34.3044739600521,108.474186216463));
#35734=CARTESIAN_POINT('Ctrl Pts',(88.6813900247885,34.00432871512,108.421536708732));
#35735=CARTESIAN_POINT('Ctrl Pts',(87.9085051637108,33.7041834701879,108.368887201001));
#35736=CARTESIAN_POINT('Ctrl Pts',(86.973124274034,33.8224635216923,108.316237693271));
#35737=CARTESIAN_POINT('Ctrl Pts',(86.2992914932937,34.3055671773523,108.26358818554));
#35738=CARTESIAN_POINT('Ctrl Pts',(85.6550813532253,34.767432914039,108.213253224524));
#35739=CARTESIAN_POINT('Ctrl Pts',(85.249928742989,35.5627509933504,108.162918263508));
#35740=CARTESIAN_POINT('Ctrl Pts',(85.2471486681112,36.3555923947772,108.112583302492));
#35741=CARTESIAN_POINT('Ctrl Pts',(85.249750645845,36.3528305926657,108.387416697508));
#35742=CARTESIAN_POINT('Ctrl Pts',(85.2483891215025,36.2000987872894,108.397086800155));
#35743=CARTESIAN_POINT('Ctrl Pts',(85.2611015862619,36.0475930556804,108.406756902801));
#35744=CARTESIAN_POINT('Ctrl Pts',(85.2887058548593,35.897832262702,108.416427005448));
#35745=CARTESIAN_POINT('Ctrl Pts',(85.4389991046876,35.0824498085661,108.469076513179));
#35746=CARTESIAN_POINT('Ctrl Pts',(86.0307344742379,34.3484363773334,108.521726020909));
#35747=CARTESIAN_POINT('Ctrl Pts',(86.7956561860184,34.0285442450444,108.57437552864));
#35748=CARTESIAN_POINT('Ctrl Pts',(87.5605778977989,33.7086521127554,108.627025036371));
#35749=CARTESIAN_POINT('Ctrl Pts',(88.4986859518095,33.8028812794101,108.679674544102));
#35750=CARTESIAN_POINT('Ctrl Pts',(89.1847040791145,34.2685151393245,108.732324051833));
#35751=CARTESIAN_POINT('Ctrl Pts',(89.8707222064195,34.734148999239,108.784973559563));
#35752=CARTESIAN_POINT('Ctrl Pts',(90.304650407019,35.5711875524131,108.837623067294));
#35753=CARTESIAN_POINT('Ctrl Pts',(90.2897735643535,36.4001717328157,108.890272575025));
#35754=CARTESIAN_POINT('Ctrl Pts',(90.2748967216881,37.2291559132183,108.942922082756));
#35755=CARTESIAN_POINT('Ctrl Pts',(89.8112148357577,38.0500857208495,108.995571590487));
#35756=CARTESIAN_POINT('Ctrl Pts',(89.1089312161219,38.4908052894037,109.048221098218));
#35757=CARTESIAN_POINT('Ctrl Pts',(88.406647596486,38.9315248579579,109.100870605948));
#35758=CARTESIAN_POINT('Ctrl Pts',(87.4657622431447,38.9920341874351,109.153520113679));
#35759=CARTESIAN_POINT('Ctrl Pts',(86.7128111367725,38.6449022068022,109.20616962141));
#35760=CARTESIAN_POINT('Ctrl Pts',(85.9598600304002,38.2977702261693,109.258819129141));
#35761=CARTESIAN_POINT('Ctrl Pts',(85.3948431709971,37.5429969354263,109.311468636872));
#35762=CARTESIAN_POINT('Ctrl Pts',(85.2739024016732,36.7227473703736,109.364118144603));
#35763=CARTESIAN_POINT('Ctrl Pts',(85.2560627609119,36.6017546095624,109.371884328904));
#35764=CARTESIAN_POINT('Ctrl Pts',(85.2478855008807,36.479337190443,109.379650513206));
#35765=CARTESIAN_POINT('Ctrl Pts',(85.2489004637444,36.356783832747,109.387416697508));
#35766=CARTESIAN_POINT('Origin',(87.7685555885722,36.3549260746835,114.));
#35767=CARTESIAN_POINT('',(85.2549713556205,36.3552114621125,110.387416697508));
#35768=CARTESIAN_POINT('',(85.2524195635058,36.3528024297952,110.112583302492));
#35769=CARTESIAN_POINT('',(85.2510555885723,36.3549260746835,114.));
#35770=CARTESIAN_POINT('Ctrl Pts',(85.2524195635058,36.3528024297952,110.112583302492));
#35771=CARTESIAN_POINT('Ctrl Pts',(85.2572190279654,36.9417394717248,110.07539618188));
#35772=CARTESIAN_POINT('Ctrl Pts',(85.4637775213495,37.5337100919753,110.038209061269));
#35773=CARTESIAN_POINT('Ctrl Pts',(85.841473043876,37.9812526944321,110.001021940657));
#35774=CARTESIAN_POINT('Ctrl Pts',(86.3762141855952,38.6148832988006,109.948372432926));
#35775=CARTESIAN_POINT('Ctrl Pts',(87.253997499495,38.9590096316741,109.895722925195));
#35776=CARTESIAN_POINT('Ctrl Pts',(88.0768932710453,38.8576272669864,109.843073417464));
#35777=CARTESIAN_POINT('Ctrl Pts',(88.8997890425955,38.7562449022988,109.790423909734));
#35778=CARTESIAN_POINT('Ctrl Pts',(89.6677972717962,38.2093538400499,109.737774402003));
#35779=CARTESIAN_POINT('Ctrl Pts',(90.0327531016733,37.4648787983024,109.685124894272));
#35780=CARTESIAN_POINT('Ctrl Pts',(90.3977089315504,36.7204037565549,109.632475386541));
#35781=CARTESIAN_POINT('Ctrl Pts',(90.359612362104,35.7783447353088,109.57982587881));
#35782=CARTESIAN_POINT('Ctrl Pts',(89.935733904506,35.0657699248179,109.52717637108));
#35783=CARTESIAN_POINT('Ctrl Pts',(89.511855446908,34.353195114327,109.474526863349));
#35784=CARTESIAN_POINT('Ctrl Pts',(88.7021951011585,33.8701045145914,109.421877355618));
#35785=CARTESIAN_POINT('Ctrl Pts',(87.8738000505619,33.8354997820466,109.369227847887));
#35786=CARTESIAN_POINT('Ctrl Pts',(87.0454049999653,33.8008950495019,109.316578340156));
#35787=CARTESIAN_POINT('Ctrl Pts',(86.1982752445215,34.214776184148,109.263928832425));
#35788=CARTESIAN_POINT('Ctrl Pts',(85.7164442221403,34.8895167155904,109.211279324695));
#35789=CARTESIAN_POINT('Ctrl Pts',(85.4153663499221,35.3111363998153,109.178380650627));
#35790=CARTESIAN_POINT('Ctrl Pts',(85.2569202654081,35.8346092763373,109.14548197656));
#35791=CARTESIAN_POINT('Ctrl Pts',(85.2539948967292,36.356454017039,109.112583302492));
#35792=CARTESIAN_POINT('Ctrl Pts',(85.2489004637444,36.356783832747,109.387416697508));
#35793=CARTESIAN_POINT('Ctrl Pts',(85.254766266655,35.6485078278274,109.432300020937));
#35794=CARTESIAN_POINT('Ctrl Pts',(85.5676580844589,34.9356913891148,109.477183344366));
#35795=CARTESIAN_POINT('Ctrl Pts',(86.0968198597103,34.467100172007,109.522066667795));
#35796=CARTESIAN_POINT('Ctrl Pts',(86.7175427663159,33.9174283780556,109.574716175526));
#35797=CARTESIAN_POINT('Ctrl Pts',(87.6358532587717,33.7038106295153,109.627365683257));
#35798=CARTESIAN_POINT('Ctrl Pts',(88.435449249828,33.9230872942025,109.680015190987));
#35799=CARTESIAN_POINT('Ctrl Pts',(89.2350452408843,34.1423639588897,109.732664698718));
#35800=CARTESIAN_POINT('Ctrl Pts',(89.915926730541,34.7945350368046,109.785314206449));
#35801=CARTESIAN_POINT('Ctrl Pts',(90.1694264446719,35.5839486823747,109.83796371418));
#35802=CARTESIAN_POINT('Ctrl Pts',(90.4229261588028,36.3733623279449,109.890613221911));
#35803=CARTESIAN_POINT('Ctrl Pts',(90.2490440974077,37.3000185411705,109.943262729642));
#35804=CARTESIAN_POINT('Ctrl Pts',(89.7266070511755,37.9438318216275,109.995912237372));
#35805=CARTESIAN_POINT('Ctrl Pts',(89.2041700049433,38.5876451020846,110.048561745103));
#35806=CARTESIAN_POINT('Ctrl Pts',(88.3331779738739,38.9486154497732,110.101211252834));
#35807=CARTESIAN_POINT('Ctrl Pts',(87.5084819490988,38.8631024456324,110.153860760565));
#35808=CARTESIAN_POINT('Ctrl Pts',(86.6837859243238,38.7775894414915,110.206510268296));
#35809=CARTESIAN_POINT('Ctrl Pts',(85.905385905843,38.2455930855212,110.259159776026));
#35810=CARTESIAN_POINT('Ctrl Pts',(85.5261577056066,37.5082858362883,110.311809283757));
#35811=CARTESIAN_POINT('Ctrl Pts',(85.3446272749214,37.1553487329371,110.337011755008));
#35812=CARTESIAN_POINT('Ctrl Pts',(85.2545623833254,36.7553670470907,110.362214226258));
#35813=CARTESIAN_POINT('Ctrl Pts',(85.2549713556205,36.3552114621125,110.387416697508));
#35814=CARTESIAN_POINT('Origin',(87.7685555885722,36.3549260746835,114.));
#35815=CARTESIAN_POINT('',(85.2499086688349,36.3527998632167,111.387416697508));
#35816=CARTESIAN_POINT('',(85.2470898693037,36.3554869991381,111.112583302492));
#35817=CARTESIAN_POINT('',(85.2510555885723,36.3549260746835,114.));
#35818=CARTESIAN_POINT('Ctrl Pts',(85.2470898693037,36.3554869991381,111.112583302492));
#35819=CARTESIAN_POINT('Ctrl Pts',(85.2469951454703,36.3865769470086,111.110609402663));
#35820=CARTESIAN_POINT('Ctrl Pts',(85.2475209470525,36.4176636173667,111.108635502833));
#35821=CARTESIAN_POINT('Ctrl Pts',(85.2486772533794,36.448726817618,111.106661603004));
#35822=CARTESIAN_POINT('Ctrl Pts',(85.2795192231668,37.2772704840766,111.054012095273));
#35823=CARTESIAN_POINT('Ctrl Pts',(85.75892762442,38.0891165727784,111.001362587543));
#35824=CARTESIAN_POINT('Ctrl Pts',(86.4695699486882,38.5162270049124,110.948713079812));
#35825=CARTESIAN_POINT('Ctrl Pts',(87.1802122729565,38.9433374370465,110.896063572081));
#35826=CARTESIAN_POINT('Ctrl Pts',(88.1220885202398,38.9857122126128,110.84341406435));
#35827=CARTESIAN_POINT('Ctrl Pts',(88.8682134168015,38.6241413716773,110.790764556619));
#35828=CARTESIAN_POINT('Ctrl Pts',(89.6143383133631,38.2625705307417,110.738115048888));
#35829=CARTESIAN_POINT('Ctrl Pts',(90.1647118592032,37.4970540733041,110.685465541158));
#35830=CARTESIAN_POINT('Ctrl Pts',(90.2698305766733,36.6746272439013,110.632816033427));
#35831=CARTESIAN_POINT('Ctrl Pts',(90.3749492941434,35.8522004144985,110.580166525696));
#35832=CARTESIAN_POINT('Ctrl Pts',(90.0348131832435,34.9728632131304,110.527517017965));
#35833=CARTESIAN_POINT('Ctrl Pts',(89.4036177776061,34.4352497888972,110.474867510234));
#35834=CARTESIAN_POINT('Ctrl Pts',(88.7724223719687,33.8976363646639,110.422218002503));
#35835=CARTESIAN_POINT('Ctrl Pts',(87.8501676715938,33.7017467175656,110.369568494773));
#35836=CARTESIAN_POINT('Ctrl Pts',(87.0549438200498,33.9363844386613,110.316918987042));
#35837=CARTESIAN_POINT('Ctrl Pts',(86.2597199685058,34.171022159757,110.264269479311));
#35838=CARTESIAN_POINT('Ctrl Pts',(85.5915269657928,34.8361872490467,110.21161997158));
#35839=CARTESIAN_POINT('Ctrl Pts',(85.3532799492055,35.6303372316234,110.158970463849));
#35840=CARTESIAN_POINT('Ctrl Pts',(85.2833102997403,35.8635674172505,110.14350807673));
#35841=CARTESIAN_POINT('Ctrl Pts',(85.250423948459,36.107922686989,110.128045689611));
#35842=CARTESIAN_POINT('Ctrl Pts',(85.2524195635058,36.3528024297952,110.112583302492));
#35843=CARTESIAN_POINT('Ctrl Pts',(85.2549713556205,36.3552114621125,110.387416697508));
#35844=CARTESIAN_POINT('Ctrl Pts',(85.2554167515259,35.9194174945387,110.414863733989));
#35845=CARTESIAN_POINT('Ctrl Pts',(85.3631690851555,35.4834172731087,110.442310770469));
#35846=CARTESIAN_POINT('Ctrl Pts',(85.576947423415,35.107753009214,110.46975780695));
#35847=CARTESIAN_POINT('Ctrl Pts',(85.9870217234522,34.3871455738681,110.522407314681));
#35848=CARTESIAN_POINT('Ctrl Pts',(86.787226705519,33.8885488456719,110.575056822411));
#35849=CARTESIAN_POINT('Ctrl Pts',(87.6148016096937,33.8379940694177,110.627706330142));
#35850=CARTESIAN_POINT('Ctrl Pts',(88.4423765138683,33.7874392931636,110.680355837873));
#35851=CARTESIAN_POINT('Ctrl Pts',(89.2973213401509,34.1849264688513,110.733005345604));
#35852=CARTESIAN_POINT('Ctrl Pts',(89.7920598524681,34.8502608298321,110.785654853335));
#35853=CARTESIAN_POINT('Ctrl Pts',(90.2867983647854,35.5155951908128,110.838304361066));
#35854=CARTESIAN_POINT('Ctrl Pts',(90.4213305631374,36.4487767370866,110.890953868796));
#35855=CARTESIAN_POINT('Ctrl Pts',(90.1346683212381,37.226761805398,110.943603376527));
#35856=CARTESIAN_POINT('Ctrl Pts',(89.8480060793388,38.0047468737095,110.996252884258));
#35857=CARTESIAN_POINT('Ctrl Pts',(89.1401493971882,38.6275354640587,111.048902391989));
#35858=CARTESIAN_POINT('Ctrl Pts',(88.3319943373804,38.812795839625,111.10155189972));
#35859=CARTESIAN_POINT('Ctrl Pts',(87.5238392775726,38.9980562151914,111.15420140745));
#35860=CARTESIAN_POINT('Ctrl Pts',(86.6153858401076,38.745788375975,111.206850915181));
#35861=CARTESIAN_POINT('Ctrl Pts',(86.0184675761862,38.1703541107022,111.259500422912));
#35862=CARTESIAN_POINT('Ctrl Pts',(85.5350470350138,37.704332612047,111.302139181111));
#35863=CARTESIAN_POINT('Ctrl Pts',(85.2559543382204,37.0263546320076,111.344777939309));
#35864=CARTESIAN_POINT('Ctrl Pts',(85.2499086688349,36.3527998632167,111.387416697508));
#35865=CARTESIAN_POINT('Origin',(87.7685555885722,36.3549260746835,114.));
#35866=CARTESIAN_POINT('',(85.2487564810892,36.3567299719253,112.387416697508));
#35867=CARTESIAN_POINT('',(85.2538919790663,36.3565168098445,112.112583302492));
#35868=CARTESIAN_POINT('',(85.2510555885723,36.3549260746835,114.));
#35869=CARTESIAN_POINT('Ctrl Pts',(85.2538919790663,36.3565168098445,112.112583302492));
#35870=CARTESIAN_POINT('Ctrl Pts',(85.2520902264104,36.6643730249807,112.093173115714));
#35871=CARTESIAN_POINT('Ctrl Pts',(85.3044764405676,36.9716374584574,112.073762928937));
#35872=CARTESIAN_POINT('Ctrl Pts',(85.4138341392615,37.2570747873116,112.054352742159));
#35873=CARTESIAN_POINT('Ctrl Pts',(85.710463381873,38.0313143669871,112.001703234428));
#35874=CARTESIAN_POINT('Ctrl Pts',(86.4262592893377,38.6449614200248,111.949053726697));
#35875=CARTESIAN_POINT('Ctrl Pts',(87.2367266719805,38.8198283865448,111.896404218967));
#35876=CARTESIAN_POINT('Ctrl Pts',(88.0471940546233,38.9946953530647,111.843754711236));
#35877=CARTESIAN_POINT('Ctrl Pts',(88.9523329124443,38.7307822330669,111.791105203505));
#35878=CARTESIAN_POINT('Ctrl Pts',(89.5418123085277,38.1477300262273,111.738455695774));
#35879=CARTESIAN_POINT('Ctrl Pts',(90.1312917046111,37.5646778193877,111.685806188043));
#35880=CARTESIAN_POINT('Ctrl Pts',(90.4051116389569,36.6624865257063,111.633156680312));
#35881=CARTESIAN_POINT('Ctrl Pts',(90.239140008257,35.8501508487148,111.580507172582));
#35882=CARTESIAN_POINT('Ctrl Pts',(90.073168377557,35.0378151717233,111.527857664851));
#35883=CARTESIAN_POINT('Ctrl Pts',(89.4674051818114,34.3153351114216,111.47520815712));
#35884=CARTESIAN_POINT('Ctrl Pts',(88.6964639540858,34.0102360165388,111.422558649389));
#35885=CARTESIAN_POINT('Ctrl Pts',(87.9255227263601,33.705136921656,111.369909141658));
#35886=CARTESIAN_POINT('Ctrl Pts',(86.9894034666545,33.8174187921922,111.317259633927));
#35887=CARTESIAN_POINT('Ctrl Pts',(86.3124816059625,34.296180349568,111.264610126197));
#35888=CARTESIAN_POINT('Ctrl Pts',(85.660938443056,34.7569925015818,111.213934518295));
#35889=CARTESIAN_POINT('Ctrl Pts',(85.2495216988075,35.5573198456716,111.163258910394));
#35890=CARTESIAN_POINT('Ctrl Pts',(85.2470898693037,36.3554869991381,111.112583302492));
#35891=CARTESIAN_POINT('Ctrl Pts',(85.2499086688349,36.3527998632167,111.387416697508));
#35892=CARTESIAN_POINT('Ctrl Pts',(85.248489263474,36.19466232893,111.39742744704));
#35893=CARTESIAN_POINT('Ctrl Pts',(85.2621207261532,36.0367686104045,111.407438196572));
#35894=CARTESIAN_POINT('Ctrl Pts',(85.291692389305,35.8819189952726,111.417448946105));
#35895=CARTESIAN_POINT('Ctrl Pts',(85.4472185567229,35.0675188364451,111.470098453835));
#35896=CARTESIAN_POINT('Ctrl Pts',(86.0436539819365,34.3373192101194,111.522747961566));
#35897=CARTESIAN_POINT('Ctrl Pts',(86.8106137348087,34.0223450128831,111.575397469297));
#35898=CARTESIAN_POINT('Ctrl Pts',(87.5775734876809,33.7073708156469,111.628046977028));
#35899=CARTESIAN_POINT('Ctrl Pts',(88.5150575682117,33.8076220475,111.680696484759));
#35900=CARTESIAN_POINT('Ctrl Pts',(89.1980718246363,34.2776513369828,111.73334599249));
#35901=CARTESIAN_POINT('Ctrl Pts',(89.8810860810608,34.7476806264656,111.78599550022));
#35902=CARTESIAN_POINT('Ctrl Pts',(90.3096305133791,35.587487973578,111.838645007951));
#35903=CARTESIAN_POINT('Ctrl Pts',(90.2894310199951,36.4163594883,111.891294515682));
#35904=CARTESIAN_POINT('Ctrl Pts',(90.2692315266111,37.245231003022,111.943944023413));
#35905=CARTESIAN_POINT('Ctrl Pts',(89.8002881075246,38.0631666853536,111.996593531144));
#35906=CARTESIAN_POINT('Ctrl Pts',(89.0951891306436,38.4993678319042,112.049243038874));
#35907=CARTESIAN_POINT('Ctrl Pts',(88.3900901537627,38.9355689784547,112.101892546605));
#35908=CARTESIAN_POINT('Ctrl Pts',(87.4488356190872,38.9900355892243,112.154542054336));
#35909=CARTESIAN_POINT('Ctrl Pts',(86.6981289564312,38.6380760544841,112.207191562067));
#35910=CARTESIAN_POINT('Ctrl Pts',(85.9474222937752,38.2861165197439,112.259841069798));
#35911=CARTESIAN_POINT('Ctrl Pts',(85.3872635031387,37.527730839494,112.312490577529));
#35912=CARTESIAN_POINT('Ctrl Pts',(85.2715920540268,36.7067216292466,112.365140085259));
#35913=CARTESIAN_POINT('Ctrl Pts',(85.2552780805371,36.5909288161227,112.372565622676));
#35914=CARTESIAN_POINT('Ctrl Pts',(85.2478056192164,36.4738903281486,112.379991160092));
#35915=CARTESIAN_POINT('Ctrl Pts',(85.2487564810892,36.3567299719253,112.387416697508));
#35916=CARTESIAN_POINT('Origin',(87.7685555885722,36.3549260746835,114.));
#35917=CARTESIAN_POINT('',(85.2549501597152,36.3552974008805,113.387416697508));
#35918=CARTESIAN_POINT('',(85.2525638004967,36.3528324581658,113.112583302492));
#35919=CARTESIAN_POINT('',(85.2510555885723,36.3549260746835,114.));
#35920=CARTESIAN_POINT('Ctrl Pts',(85.2525638004967,36.3528324581658,113.112583302492));
#35921=CARTESIAN_POINT('Ctrl Pts',(85.2572318872201,36.9364594446687,113.075736828766));
#35922=CARTESIAN_POINT('Ctrl Pts',(85.4596894895625,37.523008588093,113.03889035504));
#35923=CARTESIAN_POINT('Ctrl Pts',(85.8310701294007,37.9688453722444,113.002043881314));
#35924=CARTESIAN_POINT('Ctrl Pts',(86.3617317067771,38.6058964884073,112.949394373583));
#35925=CARTESIAN_POINT('Ctrl Pts',(87.2372872920457,38.9556519800712,112.896744865852));
#35926=CARTESIAN_POINT('Ctrl Pts',(88.0608170750347,38.8595555137566,112.844095358121));
#35927=CARTESIAN_POINT('Ctrl Pts',(88.8843468580237,38.7634590474419,112.79144585039));
#35928=CARTESIAN_POINT('Ctrl Pts',(89.655850838733,38.2215106231487,112.73879634266));
#35929=CARTESIAN_POINT('Ctrl Pts',(90.0255794196246,37.4793943177222,112.686146834929));
#35930=CARTESIAN_POINT('Ctrl Pts',(90.3953080005161,36.7372780122957,112.633497327198));
#35931=CARTESIAN_POINT('Ctrl Pts',(90.3632611815899,35.7949938257358,112.580847819467));
#35932=CARTESIAN_POINT('Ctrl Pts',(89.9439669008761,35.0797119648804,112.528198311736));
#35933=CARTESIAN_POINT('Ctrl Pts',(89.5246726201623,34.364430104025,112.475548804006));
#35934=CARTESIAN_POINT('Ctrl Pts',(88.7181308776611,33.8761505688741,112.422899296275));
#35935=CARTESIAN_POINT('Ctrl Pts',(87.8899751074061,33.836227461513,112.370249788544));
#35936=CARTESIAN_POINT('Ctrl Pts',(87.061819337151,33.796304354152,112.317600280813));
#35937=CARTESIAN_POINT('Ctrl Pts',(86.2120495391423,34.2047376745809,112.264950773082));
#35938=CARTESIAN_POINT('Ctrl Pts',(85.7258959290171,34.8763703879519,112.212301265351));
#35939=CARTESIAN_POINT('Ctrl Pts',(85.4189715801305,35.3003936368778,112.179061944398));
#35940=CARTESIAN_POINT('Ctrl Pts',(85.2569774225757,35.8293229368779,112.145822623445));
#35941=CARTESIAN_POINT('Ctrl Pts',(85.2538919790663,36.3565168098445,112.112583302492));
#35942=CARTESIAN_POINT('Ctrl Pts',(85.2487564810892,36.3567299719253,112.387416697508));
#35943=CARTESIAN_POINT('Ctrl Pts',(85.2545475432976,35.6431847865861,112.432640667823));
#35944=CARTESIAN_POINT('Ctrl Pts',(85.5727774749206,34.9251192501781,112.477864638137));
#35945=CARTESIAN_POINT('Ctrl Pts',(86.1089760466816,34.4564048740649,112.523088608452));
#35946=CARTESIAN_POINT('Ctrl Pts',(86.7332155960355,33.9107300693753,112.575738116183));
#35947=CARTESIAN_POINT('Ctrl Pts',(87.6528788023304,33.7030132002407,112.628387623914));
#35948=CARTESIAN_POINT('Ctrl Pts',(88.4510503361386,33.9274195505719,112.681037131644));
#35949=CARTESIAN_POINT('Ctrl Pts',(89.2492218699467,34.1518259009031,112.733686639375));
#35950=CARTESIAN_POINT('Ctrl Pts',(89.9259017312681,34.8083554706999,112.786336147106));
#35951=CARTESIAN_POINT('Ctrl Pts',(90.1743273951165,35.5993805632173,112.838985654837));
#35952=CARTESIAN_POINT('Ctrl Pts',(90.422753058965,36.3904056557346,112.891635162568));
#35953=CARTESIAN_POINT('Ctrl Pts',(90.2429245253405,37.3159262709724,112.944284670298));
#35954=CARTESIAN_POINT('Ctrl Pts',(89.7163643253429,37.9563717122312,112.996934178029));
#35955=CARTESIAN_POINT('Ctrl Pts',(89.1898041253453,38.5968171534899,113.04958368576));
#35956=CARTESIAN_POINT('Ctrl Pts',(88.3165122589745,38.9521874207695,113.102233193491));
#35957=CARTESIAN_POINT('Ctrl Pts',(87.4923823138641,38.8613808074479,113.154882701222));
#35958=CARTESIAN_POINT('Ctrl Pts',(86.6682523687537,38.7705741941264,113.207532208953));
#35959=CARTESIAN_POINT('Ctrl Pts',(85.8932843449036,38.2335907002035,113.260181716683));
#35960=CARTESIAN_POINT('Ctrl Pts',(85.5187982111328,37.493863626842,113.312831224414));
#35961=CARTESIAN_POINT('Ctrl Pts',(85.3419606890729,37.1445542910419,113.337693048779));
#35962=CARTESIAN_POINT('Ctrl Pts',(85.2544249726597,36.7500360002912,113.362554873143));
#35963=CARTESIAN_POINT('Ctrl Pts',(85.2549501597152,36.3552974008805,113.387416697508));
#35964=CARTESIAN_POINT('Origin',(87.7685555885722,36.3549260746835,114.));
#35965=CARTESIAN_POINT('',(85.2500677241434,36.352772713106,114.387416697508));
#35966=CARTESIAN_POINT('',(85.2470413488897,36.3553920695512,114.112583302492));
#35967=CARTESIAN_POINT('',(85.2510555885723,36.3549260746835,114.));
#35968=CARTESIAN_POINT('Ctrl Pts',(85.2470413488897,36.3553920695512,114.112583302492));
#35969=CARTESIAN_POINT('Ctrl Pts',(85.246975261324,36.3811153243067,114.110950049548));
#35970=CARTESIAN_POINT('Ctrl Pts',(85.2473352048204,36.406836684913,114.109316796605));
#35971=CARTESIAN_POINT('Ctrl Pts',(85.2481269058065,36.4325447491923,114.107683543661));
#35972=CARTESIAN_POINT('Ctrl Pts',(85.2736481622355,37.2612693715961,114.05503403593));
#35973=CARTESIAN_POINT('Ctrl Pts',(85.7478338181264,38.0761770047617,114.002384528199));
#35974=CARTESIAN_POINT('Ctrl Pts',(86.4557190172335,38.507841665341,113.949735020469));
#35975=CARTESIAN_POINT('Ctrl Pts',(87.1636042163406,38.9395063259204,113.897085512738));
#35976=CARTESIAN_POINT('Ctrl Pts',(88.105188958664,38.9879280139136,113.844436005007));
#35977=CARTESIAN_POINT('Ctrl Pts',(88.853620119774,38.6311554934084,113.791786497276));
#35978=CARTESIAN_POINT('Ctrl Pts',(89.6020512808839,38.2743829729033,113.739136989545));
#35979=CARTESIAN_POINT('Ctrl Pts',(90.1573288607805,37.5124162438998,113.686487481815));
#35980=CARTESIAN_POINT('Ctrl Pts',(90.2677262126197,36.6906813359064,113.633837974084));
#35981=CARTESIAN_POINT('Ctrl Pts',(90.3781235644589,35.868946427913,113.581188466353));
#35982=CARTESIAN_POINT('Ctrl Pts',(90.0436406882408,34.9874433409297,113.528538958622));
#35983=CARTESIAN_POINT('Ctrl Pts',(89.4159103094804,34.4457880945882,113.475889450891));
#35984=CARTESIAN_POINT('Ctrl Pts',(88.7881799307199,33.9041328482467,113.42323994316));
#35985=CARTESIAN_POINT('Ctrl Pts',(87.867202049417,33.7023254425469,113.37059043543));
#35986=CARTESIAN_POINT('Ctrl Pts',(87.0704879829226,33.9318521960155,113.317940927699));
#35987=CARTESIAN_POINT('Ctrl Pts',(86.2737739164281,34.1613789494841,113.265291419968));
#35988=CARTESIAN_POINT('Ctrl Pts',(85.6013236647419,34.822239862121,113.212641912237));
#35989=CARTESIAN_POINT('Ctrl Pts',(85.357982323641,35.6148436887704,113.159992404506));
#35990=CARTESIAN_POINT('Ctrl Pts',(85.2849421062881,35.8527480066772,113.144189370502));
#35991=CARTESIAN_POINT('Ctrl Pts',(85.2505617111305,36.1025214736639,113.128386336497));
#35992=CARTESIAN_POINT('Ctrl Pts',(85.2525638004967,36.3528324581658,113.112583302492));
#35993=CARTESIAN_POINT('Ctrl Pts',(85.2549501597152,36.3552974008805,113.387416697508));
#35994=CARTESIAN_POINT('Ctrl Pts',(85.2555371533079,35.914104065589,113.415204380874));
#35995=CARTESIAN_POINT('Ctrl Pts',(85.366131529534,35.4726355164613,113.44299206424));
#35996=CARTESIAN_POINT('Ctrl Pts',(85.5850006992482,35.0937064069138,113.470779747607));
#35997=CARTESIAN_POINT('Ctrl Pts',(85.999693564826,34.3757469131473,113.523429255337));
#35998=CARTESIAN_POINT('Ctrl Pts',(86.8030835396733,33.8822985784145,113.576078763068));
#35999=CARTESIAN_POINT('Ctrl Pts',(87.6309659956938,33.8370587014901,113.628728270799));
#36000=CARTESIAN_POINT('Ctrl Pts',(88.4588484517142,33.7918188245658,113.68137777853));
#36001=CARTESIAN_POINT('Ctrl Pts',(89.3112233889079,34.1947874054499,113.734027286261));
#36002=CARTESIAN_POINT('Ctrl Pts',(89.801679591404,34.8632847658664,113.786676793992));
#36003=CARTESIAN_POINT('Ctrl Pts',(90.2921357939,35.5317821262828,113.839326301722));
#36004=CARTESIAN_POINT('Ctrl Pts',(90.4206732616985,36.4658082662316,113.891975809453));
#36005=CARTESIAN_POINT('Ctrl Pts',(90.129021488418,37.2419366387274,113.944625317184));
#36006=CARTESIAN_POINT('Ctrl Pts',(89.8373697151376,38.0180650112232,113.997274824915));
#36007=CARTESIAN_POINT('Ctrl Pts',(89.1255287007783,38.6362956162661,114.049924332646));
#36008=CARTESIAN_POINT('Ctrl Pts',(88.3162007443671,38.8163630103767,114.102573840377));
#36009=CARTESIAN_POINT('Ctrl Pts',(87.5068727879558,38.9964304044874,114.155223348107));
#36010=CARTESIAN_POINT('Ctrl Pts',(86.6000578894926,38.7383345876658,114.207872855838));
#36011=CARTESIAN_POINT('Ctrl Pts',(86.0068467934315,38.1590793736534,114.260522363569));
#36012=CARTESIAN_POINT('Ctrl Pts',(85.5302666684741,37.6937112709506,114.302820474882));
#36013=CARTESIAN_POINT('Ctrl Pts',(85.2560977910143,37.0210552663375,114.345118586195));
#36014=CARTESIAN_POINT('Ctrl Pts',(85.2500677241434,36.352772713106,114.387416697508));
#36015=CARTESIAN_POINT('Origin',(87.7685555885722,36.3549260746835,114.));
#36016=CARTESIAN_POINT('',(85.2486156762139,36.3566728107829,115.387416697508));
#36017=CARTESIAN_POINT('',(85.2537847572937,36.3565773825072,115.112583302492));
#36018=CARTESIAN_POINT('',(85.2510555885723,36.3549260746835,114.));
#36019=CARTESIAN_POINT('Ctrl Pts',(85.2537847572937,36.3565773825072,115.112583302492));
#36020=CARTESIAN_POINT('Ctrl Pts',(85.2519421925275,36.6589983217697,115.0935137626));
#36021=CARTESIAN_POINT('Ctrl Pts',(85.30245434637,36.9608245141166,115.074444222708));
#36022=CARTESIAN_POINT('Ctrl Pts',(85.4080899859888,37.2419365270239,115.055374682816));
#36023=CARTESIAN_POINT('Ctrl Pts',(85.6997417225407,38.0180648017789,115.002725175085));
#36024=CARTESIAN_POINT('Ctrl Pts',(86.4115826472556,38.6362953289655,114.950075667354));
#36025=CARTESIAN_POINT('Ctrl Pts',(87.2209105017453,38.8163627003993,114.897426159623));
#36026=CARTESIAN_POINT('Ctrl Pts',(88.030238356235,38.9964300718331,114.844776651893));
#36027=CARTESIAN_POINT('Ctrl Pts',(88.9370531404997,38.7383342875141,114.792127144162));
#36028=CARTESIAN_POINT('Ctrl Pts',(89.5302641618553,38.1590791464492,114.739477636431));
#36029=CARTESIAN_POINT('Ctrl Pts',(90.123475183211,37.5798240053843,114.6868281287));
#36030=CARTESIAN_POINT('Ctrl Pts',(90.4030824416578,36.6794095075733,114.634178620969));
#36031=CARTESIAN_POINT('Ctrl Pts',(90.2423302385139,35.8660248731645,114.581529113238));
#36032=CARTESIAN_POINT('Ctrl Pts',(90.0815780353701,35.0526402387556,114.528879605508));
#36033=CARTESIAN_POINT('Ctrl Pts',(89.4804663706356,34.3262854677489,114.476230097777));
#36034=CARTESIAN_POINT('Ctrl Pts',(88.7115000765254,34.0162424500392,114.423580590046));
#36035=CARTESIAN_POINT('Ctrl Pts',(87.9425337824152,33.7061994323295,114.370931082315));
#36036=CARTESIAN_POINT('Ctrl Pts',(87.0057128589294,33.812468167917,114.318281574584));
#36037=CARTESIAN_POINT('Ctrl Pts',(86.3257308256699,34.2868733415318,114.265632066854));
#36038=CARTESIAN_POINT('Ctrl Pts',(85.6668426773359,34.7465618790433,114.214615812066));
#36039=CARTESIAN_POINT('Ctrl Pts',(85.24910565871,35.5519010220325,114.163599557279));
#36040=CARTESIAN_POINT('Ctrl Pts',(85.2470413488897,36.3553920695512,114.112583302492));
#36041=CARTESIAN_POINT('Ctrl Pts',(85.2500677241434,36.352772713106,114.387416697508));
#36042=CARTESIAN_POINT('Ctrl Pts',(85.2485920172934,36.189227405458,114.397768093926));
#36043=CARTESIAN_POINT('Ctrl Pts',(85.2631752035907,36.0259440247882,114.408119490344));
#36044=CARTESIAN_POINT('Ctrl Pts',(85.294780627099,35.8660248115963,114.418470886761));
#36045=CARTESIAN_POINT('Ctrl Pts',(85.4555328504867,35.0526400747549,114.471120394492));
#36046=CARTESIAN_POINT('Ctrl Pts',(86.0566445909211,34.3262852122755,114.523769902223));
#36047=CARTESIAN_POINT('Ctrl Pts',(86.8256109818699,34.0162421555207,114.576419409954));
#36048=CARTESIAN_POINT('Ctrl Pts',(87.5945773728186,33.7061990987659,114.629068917685));
#36049=CARTESIAN_POINT('Ctrl Pts',(88.5313984142817,33.8124678477358,114.681718425416));
#36050=CARTESIAN_POINT('Ctrl Pts',(89.2113805331739,34.2868730810938,114.734367933146));
#36051=CARTESIAN_POINT('Ctrl Pts',(89.8913626520661,34.7612783144519,114.787017440877));
#36052=CARTESIAN_POINT('Ctrl Pts',(90.3145058483874,35.6038200321981,114.839666948608));
#36053=CARTESIAN_POINT('Ctrl Pts',(90.2889845887447,36.4325447589662,114.892316456339));
#36054=CARTESIAN_POINT('Ctrl Pts',(90.2634633291021,37.2612694857343,114.94496596407));
#36055=CARTESIAN_POINT('Ctrl Pts',(89.7892776134956,38.0761772215243,114.997615471801));
#36056=CARTESIAN_POINT('Ctrl Pts',(89.0813923252421,38.507841936465,115.050264979531));
#36057=CARTESIAN_POINT('Ctrl Pts',(88.3735070369886,38.9395066514057,115.102914487262));
#36058=CARTESIAN_POINT('Ctrl Pts',(87.4319221760881,38.9879283454972,115.155563994993));
#36059=CARTESIAN_POINT('Ctrl Pts',(86.6834909207253,38.6311557800627,115.208213502724));
#36060=CARTESIAN_POINT('Ctrl Pts',(85.9350596653626,38.2743832146282,115.260863010455));
#36061=CARTESIAN_POINT('Ctrl Pts',(85.3797820155375,37.5124163896676,115.313512518185));
#36062=CARTESIAN_POINT('Ctrl Pts',(85.2693846497952,36.6906813781902,115.366162025916));
#36063=CARTESIAN_POINT('Ctrl Pts',(85.2545287986229,36.5801028969778,115.373246916447));
#36064=CARTESIAN_POINT('Ctrl Pts',(85.2477289726895,36.4684421155685,115.380331806977));
#36065=CARTESIAN_POINT('Ctrl Pts',(85.2486156762139,36.3566728107829,115.387416697508));
#36066=CARTESIAN_POINT('Origin',(87.7685555885722,36.3549260746835,114.));
#36067=CARTESIAN_POINT('',(85.2549234205521,36.3553827989325,116.387416697508));
#36068=CARTESIAN_POINT('',(85.2527053287706,36.35286573419,116.112583302492));
#36069=CARTESIAN_POINT('',(85.2510555885723,36.3549260746835,114.));
#36070=CARTESIAN_POINT('Ctrl Pts',(85.2527053287706,36.35286573419,116.112583302492));
#36071=CARTESIAN_POINT('Ctrl Pts',(85.2572378873775,36.9311794633336,116.076077475652));
#36072=CARTESIAN_POINT('Ctrl Pts',(85.455643720258,37.5123030198393,116.039571648811));
#36073=CARTESIAN_POINT('Ctrl Pts',(85.8207470970968,37.9563715105561,116.003065821971));
#36074=CARTESIAN_POINT('Ctrl Pts',(86.3473072307831,38.596816871161,115.95041631424));
#36075=CARTESIAN_POINT('Ctrl Pts',(87.2205989871771,38.9521870936872,115.897766806509));
#36076=CARTESIAN_POINT('Ctrl Pts',(88.0447288285018,38.861380491801,115.845117298778));
#36077=CARTESIAN_POINT('Ctrl Pts',(88.8688586698266,38.7705738899147,115.792467791047));
#36078=CARTESIAN_POINT('Ctrl Pts',(89.6438265960819,38.2335904636158,115.739818283317));
#36079=CARTESIAN_POINT('Ctrl Pts',(90.0183126826921,37.4938634834107,115.687168775586));
#36080=CARTESIAN_POINT('Ctrl Pts',(90.3927987693023,36.7541365032055,115.634519267855));
#36081=CARTESIAN_POINT('Ctrl Pts',(90.3668030162672,35.8116659690941,115.581869760124));
#36082=CARTESIAN_POINT('Ctrl Pts',(89.9521102029129,35.093706565743,115.529220252393));
#36083=CARTESIAN_POINT('Ctrl Pts',(89.5374173895586,34.3757471623918,115.476570744662));
#36084=CARTESIAN_POINT('Ctrl Pts',(88.7340275158849,33.8822988898011,115.423921236932));
#36085=CARTESIAN_POINT('Ctrl Pts',(87.9061451641227,33.8370590185742,115.371271729201));
#36086=CARTESIAN_POINT('Ctrl Pts',(87.0782628123604,33.7918191473474,115.31862222147));
#36087=CARTESIAN_POINT('Ctrl Pts',(86.2258879825096,34.1947876774846,115.265972713739));
#36088=CARTESIAN_POINT('Ctrl Pts',(85.7354318417787,34.8632849537149,115.213323206008));
#36089=CARTESIAN_POINT('Ctrl Pts',(85.4226178736733,35.2896539361353,115.17974323817));
#36090=CARTESIAN_POINT('Ctrl Pts',(85.2570293696933,35.8240377684581,115.146163270331));
#36091=CARTESIAN_POINT('Ctrl Pts',(85.2537847572937,36.3565773825072,115.112583302492));
#36092=CARTESIAN_POINT('Ctrl Pts',(85.2486156762139,36.3566728107829,115.387416697508));
#36093=CARTESIAN_POINT('Ctrl Pts',(85.254318277614,35.6378578107033,115.432981314708));
#36094=CARTESIAN_POINT('Ctrl Pts',(85.577942057269,34.9145541945511,115.478545931909));
#36095=CARTESIAN_POINT('Ctrl Pts',(86.1212006602061,34.4457878541641,115.524110549109));
#36096=CARTESIAN_POINT('Ctrl Pts',(86.7489311180187,33.9041325396098,115.57676005684));
#36097=CARTESIAN_POINT('Ctrl Pts',(87.6699091153034,33.7023251084953,115.62940956457));
#36098=CARTESIAN_POINT('Ctrl Pts',(88.4666232821311,33.9318518908688,115.682059072301));
#36099=CARTESIAN_POINT('Ctrl Pts',(89.2633374489588,34.1613786732422,115.734708580032));
#36100=CARTESIAN_POINT('Ctrl Pts',(89.9357877853295,34.8222396691035,115.787358087763));
#36101=CARTESIAN_POINT('Ctrl Pts',(90.1791291570756,35.6148435955682,115.840007595494));
#36102=CARTESIAN_POINT('Ctrl Pts',(90.4224705288217,36.407447522033,115.892657103225));
#36103=CARTESIAN_POINT('Ctrl Pts',(90.2367029359434,37.3317943791011,115.945306610955));
#36104=CARTESIAN_POINT('Ctrl Pts',(89.706041291739,37.9688455754904,115.997956118686));
#36105=CARTESIAN_POINT('Ctrl Pts',(89.1753796475346,38.6058967718796,116.050605626417));
#36106=CARTESIAN_POINT('Ctrl Pts',(88.2998239520043,38.9556523075899,116.103255134148));
#36107=CARTESIAN_POINT('Ctrl Pts',(87.4762940653052,38.8595558291738,116.155904641879));
#36108=CARTESIAN_POINT('Ctrl Pts',(86.6527641786061,38.7634593507577,116.20855414961));
#36109=CARTESIAN_POINT('Ctrl Pts',(85.8812601007382,38.2215108582152,116.26120365734));
#36110=CARTESIAN_POINT('Ctrl Pts',(85.5115314732851,37.4793944593314,116.313853165071));
#36111=CARTESIAN_POINT('Ctrl Pts',(85.3393326877013,37.1337584085611,116.33837434255));
#36112=CARTESIAN_POINT('Ctrl Pts',(85.2542859121947,36.7447024938529,116.362895520029));
#36113=CARTESIAN_POINT('Ctrl Pts',(85.2549234205521,36.3553827989325,116.387416697508));
#36114=CARTESIAN_POINT('Origin',(87.7685555885722,36.3549260746835,114.));
#36115=CARTESIAN_POINT('',(85.2502276147452,36.3527492241744,117.387416697508));
#36116=CARTESIAN_POINT('',(85.2470012906549,36.3552960959922,117.112583302492));
#36117=CARTESIAN_POINT('',(85.2510555885723,36.3549260746835,114.));
#36118=CARTESIAN_POINT('Ctrl Pts',(85.2470012906549,36.3552960959922,117.112583302492));
#36119=CARTESIAN_POINT('Ctrl Pts',(85.2469591175104,36.3756533932096,117.111290696434));
#36120=CARTESIAN_POINT('Ctrl Pts',(85.2471845538459,36.3960097327226,117.109998090376));
#36121=CARTESIAN_POINT('Ctrl Pts',(85.2476804746124,36.4163594805645,117.108705484318));
#36122=CARTESIAN_POINT('Ctrl Pts',(85.2678799654529,37.2452308909037,117.056055976587));
#36123=CARTESIAN_POINT('Ctrl Pts',(85.736823325484,38.0631664702294,117.003406468856));
#36124=CARTESIAN_POINT('Ctrl Pts',(86.4419222135695,38.4993675618474,116.950756961125));
#36125=CARTESIAN_POINT('Ctrl Pts',(87.1470211016549,38.9355686534653,116.898107453395));
#36126=CARTESIAN_POINT('Ctrl Pts',(88.0882755177948,38.9900352573753,116.845457945664));
#36127=CARTESIAN_POINT('Ctrl Pts',(88.8389820859114,38.6380757669584,116.792808437933));
#36128=CARTESIAN_POINT('Ctrl Pts',(89.5896886540281,38.2861162765415,116.740158930202));
#36129=CARTESIAN_POINT('Ctrl Pts',(90.1498473741216,37.5277306917976,116.687509422471));
#36130=CARTESIAN_POINT('Ctrl Pts',(90.2655188086662,36.7067215849428,116.634859914741));
#36131=CARTESIAN_POINT('Ctrl Pts',(90.3811902432109,35.8857124780881,116.58221040701));
#36132=CARTESIAN_POINT('Ctrl Pts',(90.0523743922067,35.0020798491225,116.529560899279));
#36133=CARTESIAN_POINT('Ctrl Pts',(89.4281349214653,34.4564051131519,116.476911391548));
#36134=CARTESIAN_POINT('Ctrl Pts',(88.803895450724,33.9107303771813,116.424261883817));
#36135=CARTESIAN_POINT('Ctrl Pts',(87.8842323602454,33.7030135342056,116.371612376086));
#36136=CARTESIAN_POINT('Ctrl Pts',(87.086060926954,33.9274198562768,116.318962868356));
#36137=CARTESIAN_POINT('Ctrl Pts',(86.2878894936626,34.151826178348,116.266313360625));
#36138=CARTESIAN_POINT('Ctrl Pts',(85.6112097175582,34.808355665466,116.213663852894));
#36139=CARTESIAN_POINT('Ctrl Pts',(85.3627840849953,35.5993806583668,116.161014345163));
#36140=CARTESIAN_POINT('Ctrl Pts',(85.2866104547005,35.8419290811744,116.144870664273));
#36141=CARTESIAN_POINT('Ctrl Pts',(85.2507009314977,36.0971226623065,116.128726983382));
#36142=CARTESIAN_POINT('Ctrl Pts',(85.2527053287706,36.35286573419,116.112583302492));
#36143=CARTESIAN_POINT('Ctrl Pts',(85.2549234205521,36.3553827989325,116.387416697508));
#36144=CARTESIAN_POINT('Ctrl Pts',(85.2556547086655,35.9087927866191,116.41554502776));
#36145=CARTESIAN_POINT('Ctrl Pts',(85.3691333706026,35.4618556800097,116.443673358012));
#36146=CARTESIAN_POINT('Ctrl Pts',(85.5931440023105,35.0797118042889,116.471801688264));
#36147=CARTESIAN_POINT('Ctrl Pts',(86.0124383358272,34.3644298533553,116.524451195994));
#36148=CARTESIAN_POINT('Ctrl Pts',(86.8189801798991,33.8761502567132,116.577100703725));
#36149=CARTESIAN_POINT('Ctrl Pts',(87.6471360544467,33.8362271443242,116.629750211456));
#36150=CARTESIAN_POINT('Ctrl Pts',(88.4752919289944,33.7963040319352,116.682399719187));
#36151=CARTESIAN_POINT('Ctrl Pts',(89.3250618340178,34.2047374037992,116.735049226918));
#36152=CARTESIAN_POINT('Ctrl Pts',(89.8112155053664,34.8763702017512,116.787698734649));
#36153=CARTESIAN_POINT('Ctrl Pts',(90.297369176715,35.5480029997032,116.840348242379));
#36154=CARTESIAN_POINT('Ctrl Pts',(90.4199066143887,36.4828352237432,116.89299775011));
#36155=CARTESIAN_POINT('Ctrl Pts',(90.1232773344219,37.2570749009216,116.945647257841));
#36156=CARTESIAN_POINT('Ctrl Pts',(89.8266480544551,38.0313145781,116.998296765572));
#36157=CARTESIAN_POINT('Ctrl Pts',(89.1108520568479,38.6449617084168,117.050946273303));
#36158=CARTESIAN_POINT('Ctrl Pts',(88.30038457214,38.8198286969587,117.103595781033));
#36159=CARTESIAN_POINT('Ctrl Pts',(87.4899170874322,38.9946956855005,117.156245288764));
#36160=CARTESIAN_POINT('Ctrl Pts',(86.5847781156238,38.7307825322675,117.208894796495));
#36161=CARTESIAN_POINT('Ctrl Pts',(85.995298645305,38.1477302520023,117.261544304226));
#36162=CARTESIAN_POINT('Ctrl Pts',(85.5255304561508,37.6830840214317,117.303501768653));
#36163=CARTESIAN_POINT('Ctrl Pts',(85.2562319513466,37.0157582587766,117.345459233081));
#36164=CARTESIAN_POINT('Ctrl Pts',(85.2502276147452,36.3527492241744,117.387416697508));
#36165=CARTESIAN_POINT('Origin',(87.7685555885722,36.3549260746835,114.));
#36166=CARTESIAN_POINT('',(85.2484783463287,36.3566124304548,118.387416697508));
#36167=CARTESIAN_POINT('',(85.2536733290529,36.3566354805472,118.112583302492));
#36168=CARTESIAN_POINT('',(85.2510555885723,36.3549260746835,114.));
#36169=CARTESIAN_POINT('Ctrl Pts',(85.2536733290529,36.3566354805472,118.112583302492));
#36170=CARTESIAN_POINT('Ctrl Pts',(85.25179461801,36.6536210373574,118.093854409486));
#36171=CARTESIAN_POINT('Ctrl Pts',(85.300469441061,36.950010821798,118.075125516479));
#36172=CARTESIAN_POINT('Ctrl Pts',(85.4024431538798,37.2267616956054,118.056396623473));
#36173=CARTESIAN_POINT('Ctrl Pts',(85.689105359679,38.0047466659423,118.003747115742));
#36174=CARTESIAN_POINT('Ctrl Pts',(86.3969619526868,38.6275351778612,117.951097608011));
#36175=CARTESIAN_POINT('Ctrl Pts',(87.2051169107208,38.8127955300968,117.89844810028));
#36176=CARTESIAN_POINT('Ctrl Pts',(88.0132718687548,38.9980558823324,117.845798592549));
#36177=CARTESIAN_POINT('Ctrl Pts',(88.921725191815,38.7457880748847,117.793149084819));
#36178=CARTESIAN_POINT('Ctrl Pts',(89.5186433805641,38.1703538820781,117.740499577088));
#36179=CARTESIAN_POINT('Ctrl Pts',(90.1155615693133,37.5949196892716,117.687850069357));
#36180=CARTESIAN_POINT('Ctrl Pts',(90.4009446237513,36.6963191111062,117.635200561626));
#36181=CARTESIAN_POINT('Ctrl Pts',(90.245418475919,35.8819190548391,117.582551053895));
#36182=CARTESIAN_POINT('Ctrl Pts',(90.0898923280867,35.0675189985721,117.529901546165));
#36183=CARTESIAN_POINT('Ctrl Pts',(89.4934569779841,34.3373194642033,117.477252038434));
#36184=CARTESIAN_POINT('Ctrl Pts',(88.7264973216978,34.0223453066331,117.424602530703));
#36185=CARTESIAN_POINT('Ctrl Pts',(87.9595376654115,33.707371149063,117.371953022972));
#36186=CARTESIAN_POINT('Ctrl Pts',(87.0220537029416,33.8076223682915,117.319303515241));
#36187=CARTESIAN_POINT('Ctrl Pts',(86.3390395325317,34.277651598582,117.266654007511));
#36188=CARTESIAN_POINT('Ctrl Pts',(85.6727941467207,34.7361410698757,117.215297105838));
#36189=CARTESIAN_POINT('Ctrl Pts',(85.24867688394,35.5464744870913,117.163940204165));
#36190=CARTESIAN_POINT('Ctrl Pts',(85.2470012906549,36.3552960959922,117.112583302492));
#36191=CARTESIAN_POINT('Ctrl Pts',(85.2502276147452,36.3527492241744,117.387416697508));
#36192=CARTESIAN_POINT('Ctrl Pts',(85.2486975264086,36.1837942740767,117.398108740812));
#36193=CARTESIAN_POINT('Ctrl Pts',(85.2642653937837,36.0151196462724,117.408800784115));
#36194=CARTESIAN_POINT('Ctrl Pts',(85.2979708577576,35.8501507851476,117.419492827418));
#36195=CARTESIAN_POINT('Ctrl Pts',(85.4639425093587,35.0378150058556,117.472142335149));
#36196=CARTESIAN_POINT('Ctrl Pts',(86.0697057813901,34.3153348545691,117.52479184288));
#36197=CARTESIAN_POINT('Ctrl Pts',(86.8406471062031,34.0102357212638,117.577441350611));
#36198=CARTESIAN_POINT('Ctrl Pts',(87.611588431016,33.7051365879585,117.630090858342));
#36199=CARTESIAN_POINT('Ctrl Pts',(88.5477078086104,33.8174184726344,117.682740366072));
#36200=CARTESIAN_POINT('Ctrl Pts',(89.2246297545498,34.2961800903021,117.735389873803));
#36201=CARTESIAN_POINT('Ctrl Pts',(89.9015517004892,34.7749417079699,117.788039381534));
#36202=CARTESIAN_POINT('Ctrl Pts',(90.3192762147736,35.6201830586296,117.840688889265));
#36203=CARTESIAN_POINT('Ctrl Pts',(90.2884342411026,36.4487268294297,117.893338396996));
#36204=CARTESIAN_POINT('Ctrl Pts',(90.2575922674315,37.2772706002298,117.945987904727));
#36205=CARTESIAN_POINT('Ctrl Pts',(89.778183805805,38.0891167911703,117.998637412457));
#36206=CARTESIAN_POINT('Ctrl Pts',(89.0675413920431,38.5162272770923,118.051286920188));
#36207=CARTESIAN_POINT('Ctrl Pts',(88.3568989782812,38.9433377630143,118.103936427919));
#36208=CARTESIAN_POINT('Ctrl Pts',(87.415022612384,38.9857125439178,118.15658593565));
#36209=CARTESIAN_POINT('Ctrl Pts',(86.66889762186,38.6241416574484,118.209235443381));
#36210=CARTESIAN_POINT('Ctrl Pts',(85.922772631336,38.262570770979,118.261884951112));
#36211=CARTESIAN_POINT('Ctrl Pts',(85.3723990161852,37.4970542171365,118.314534458842));
#36212=CARTESIAN_POINT('Ctrl Pts',(85.2672802854768,36.674627284163,118.367183966573));
#36213=CARTESIAN_POINT('Ctrl Pts',(85.2538148921218,36.569276866748,118.373928210218));
#36214=CARTESIAN_POINT('Ctrl Pts',(85.2476556148006,36.4629926160435,118.380672453863));
#36215=CARTESIAN_POINT('Ctrl Pts',(85.2484783463287,36.3566124304548,118.387416697508));
#36216=CARTESIAN_POINT('Origin',(87.7685555885722,36.3549260746835,114.));
#36217=CARTESIAN_POINT('',(85.2548911701606,36.3554675198059,119.387416697508));
#36218=CARTESIAN_POINT('',(85.2528439678122,36.3529021930443,119.112583302492));
#36219=CARTESIAN_POINT('',(85.2510555885723,36.3549260746835,114.));
#36220=CARTESIAN_POINT('Ctrl Pts',(85.2528439678122,36.3529021930443,119.112583302492));
#36221=CARTESIAN_POINT('Ctrl Pts',(85.2572371818151,36.925899407681,119.076418122537));
#36222=CARTESIAN_POINT('Ctrl Pts',(85.4516400977114,37.5015934845315,119.040252942582));
#36223=CARTESIAN_POINT('Ctrl Pts',(85.8105043725551,37.9438316215303,119.004087762628));
#36224=CARTESIAN_POINT('Ctrl Pts',(86.332941352996,38.5876448209081,118.951438254897));
#36225=CARTESIAN_POINT('Ctrl Pts',(87.2039332743765,38.9486151231408,118.898788747166));
#36226=CARTESIAN_POINT('Ctrl Pts',(88.0286291952941,38.8631021297693,118.846139239435));
#36227=CARTESIAN_POINT('Ctrl Pts',(88.8533251162117,38.7775891363977,118.793489731704));
#36228=CARTESIAN_POINT('Ctrl Pts',(89.6317250366665,38.245592847422,118.740840223974));
#36229=CARTESIAN_POINT('Ctrl Pts',(90.0109531891454,37.5082856910403,118.688190716243));
#36230=CARTESIAN_POINT('Ctrl Pts',(90.3901813416243,36.7709785346587,118.635541208512));
#36231=CARTESIAN_POINT('Ctrl Pts',(90.3702377261273,35.8283605108711,118.582891700781));
#36232=CARTESIAN_POINT('Ctrl Pts',(89.9601634777318,35.1077531662743,118.53024219305));
#36233=CARTESIAN_POINT('Ctrl Pts',(89.5500892293363,34.3871458216774,118.477592685319));
#36234=CARTESIAN_POINT('Ctrl Pts',(88.7498843480423,33.8885491562713,118.424943177589));
#36235=CARTESIAN_POINT('Ctrl Pts',(87.9223095480872,33.8379943863839,118.372293669858));
#36236=CARTESIAN_POINT('Ctrl Pts',(87.094734748132,33.7874396164965,118.319644162127));
#36237=CARTESIAN_POINT('Ctrl Pts',(86.2397900295158,34.1849267421278,118.266994654396));
#36238=CARTESIAN_POINT('Ctrl Pts',(85.745051579503,34.8502610193208,118.214345146665));
#36239=CARTESIAN_POINT('Ctrl Pts',(85.4263053447227,35.2789174047707,118.180424531941));
#36240=CARTESIAN_POINT('Ctrl Pts',(85.2570759345055,35.818753575417,118.146503917216));
#36241=CARTESIAN_POINT('Ctrl Pts',(85.2536733290529,36.3566354805472,118.112583302492));
#36242=CARTESIAN_POINT('Ctrl Pts',(85.2484783463287,36.3566124304548,118.387416697508));
#36243=CARTESIAN_POINT('Ctrl Pts',(85.2540783379746,35.6325267108323,118.433321961594));
#36244=CARTESIAN_POINT('Ctrl Pts',(85.5831519524022,34.9039963671497,118.47922722568));
#36245=CARTESIAN_POINT('Ctrl Pts',(86.1334931936283,34.4352495471468,118.525132489766));
#36246=CARTESIAN_POINT('Ctrl Pts',(86.7646886787542,33.8976360552089,118.577781997497));
#36247=CARTESIAN_POINT('Ctrl Pts',(87.686943495272,33.7017463834379,118.630431505227));
#36248=CARTESIAN_POINT('Ctrl Pts',(88.4821674469615,33.9363841340836,118.683081012958));
#36249=CARTESIAN_POINT('Ctrl Pts',(89.277391398651,34.1710218847294,118.735730520689));
#36250=CARTESIAN_POINT('Ctrl Pts',(89.9455844855122,34.836187057792,118.78838002842));
#36251=CARTESIAN_POINT('Ctrl Pts',(90.183831532103,35.6303371403756,118.841029536151));
#36252=CARTESIAN_POINT('Ctrl Pts',(90.4220785786939,36.4244872229593,118.893679043881));
#36253=CARTESIAN_POINT('Ctrl Pts',(90.2303795850143,37.347622215064,118.946328551612));
#36254=CARTESIAN_POINT('Ctrl Pts',(89.6956383759536,37.9812528992341,118.998978059343));
#36255=CARTESIAN_POINT('Ctrl Pts',(89.160897166893,38.6148835834043,119.051627567074));
#36256=CARTESIAN_POINT('Ctrl Pts',(88.2831137424512,38.9590099596401,119.104277074805));
#36257=CARTESIAN_POINT('Ctrl Pts',(87.4602178672702,38.8576275821734,119.156926582536));
#36258=CARTESIAN_POINT('Ctrl Pts',(86.6373219920892,38.7562452047068,119.209576090266));
#36259=CARTESIAN_POINT('Ctrl Pts',(85.8693136661691,38.2093540735378,119.262225597997));
#36260=CARTESIAN_POINT('Ctrl Pts',(85.5043577903326,37.4648789380589,119.314875105728));
#36261=CARTESIAN_POINT('Ctrl Pts',(85.3367431800309,37.1229611392932,119.339055636321));
#36262=CARTESIAN_POINT('Ctrl Pts',(85.2541453372537,36.7393664983262,119.363236166915));
#36263=CARTESIAN_POINT('Ctrl Pts',(85.2548911701606,36.3554675198059,119.387416697508));
#36264=CARTESIAN_POINT('Origin',(87.7685555885722,36.3549260746835,114.));
#36265=CARTESIAN_POINT('',(85.2503883725927,36.3527278457068,120.387416697508));
#36266=CARTESIAN_POINT('',(85.2469699766098,36.3551993258525,120.112583302492));
#36267=CARTESIAN_POINT('',(85.2510555885723,36.3549260746835,114.));
#36268=CARTESIAN_POINT('Ctrl Pts',(85.2469699766098,36.3551993258525,120.112583302492));
#36269=CARTESIAN_POINT('Ctrl Pts',(85.2469466774846,36.3701912641417,120.11163134332));
#36270=CARTESIAN_POINT('Ctrl Pts',(85.2470689410778,36.3851828122953,120.110679384147));
#36271=CARTESIAN_POINT('Ctrl Pts',(85.247337930202,36.400171727274,120.109727424975));
#36272=CARTESIAN_POINT('Ctrl Pts',(85.2622147709145,37.2291558034242,120.057077917244));
#36273=CARTESIAN_POINT('Ctrl Pts',(85.7258965986341,38.0500855073677,120.004428409513));
#36274=CARTESIAN_POINT('Ctrl Pts',(86.4281801298719,38.4908050203458,119.951778901782));
#36275=CARTESIAN_POINT('Ctrl Pts',(87.1304636611096,38.9315245333239,119.899129394052));
#36276=CARTESIAN_POINT('Ctrl Pts',(88.0713488958655,38.9920338553367,119.846479886321));
#36277=CARTESIAN_POINT('Ctrl Pts',(88.8242999073929,38.6449019184573,119.79383037859));
#36278=CARTESIAN_POINT('Ctrl Pts',(89.5772509189203,38.2977699815779,119.741180870859));
#36279=CARTESIAN_POINT('Ctrl Pts',(90.1422677072192,37.5429967858063,119.688531363128));
#36280=CARTESIAN_POINT('Ctrl Pts',(90.2632084613244,36.722747324031,119.635881855397));
#36281=CARTESIAN_POINT('Ctrl Pts',(90.3841492154295,35.9024978622557,119.583232347667));
#36282=CARTESIAN_POINT('Ctrl Pts',(90.061013935341,35.0167721344767,119.530582839936));
#36283=CARTESIAN_POINT('Ctrl Pts',(89.4402911068987,34.4671004097576,119.477933332205));
#36284=CARTESIAN_POINT('Ctrl Pts',(88.8195682784564,33.9174286850386,119.425283824474));
#36285=CARTESIAN_POINT('Ctrl Pts',(87.9012579016605,33.7038109633795,119.372634316743));
#36286=CARTESIAN_POINT('Ctrl Pts',(87.1016620113036,33.9230876004477,119.319984809013));
#36287=CARTESIAN_POINT('Ctrl Pts',(86.3020661209467,34.1423642375158,119.267335301282));
#36288=CARTESIAN_POINT('Ctrl Pts',(85.6211847170289,34.7945352333111,119.214685793551));
#36289=CARTESIAN_POINT('Ctrl Pts',(85.3676850348207,35.5839487794703,119.16203628582));
#36290=CARTESIAN_POINT('Ctrl Pts',(85.2883154066373,35.831110665812,119.145551958044));
#36291=CARTESIAN_POINT('Ctrl Pts',(85.2508415118669,36.0917262798423,119.129067630268));
#36292=CARTESIAN_POINT('Ctrl Pts',(85.2528439678122,36.3529021930443,119.112583302492));
#36293=CARTESIAN_POINT('Ctrl Pts',(85.2548911701606,36.3554675198059,119.387416697508));
#36294=CARTESIAN_POINT('Ctrl Pts',(85.2557692774417,35.9034835899905,119.415885674646));
#36295=CARTESIAN_POINT('Ctrl Pts',(85.3721747116417,35.4510778008831,119.444354651783));
#36296=CARTESIAN_POINT('Ctrl Pts',(85.6013769997188,35.0657697625188,119.472823628921));
#36297=CARTESIAN_POINT('Ctrl Pts',(86.0252555106942,34.3531948622462,119.525473136651));
#36298=CARTESIAN_POINT('Ctrl Pts',(86.8349159583979,33.8701042014898,119.578122644382));
#36299=CARTESIAN_POINT('Ctrl Pts',(87.6633111133241,33.8354994646724,119.630772152113));
#36300=CARTESIAN_POINT('Ctrl Pts',(88.4917062682503,33.800894727855,119.683421659844));
#36301=CARTESIAN_POINT('Ctrl Pts',(89.338836130399,34.2147759149767,119.736071167575));
#36302=CARTESIAN_POINT('Ctrl Pts',(89.820667213443,34.8895165312273,119.788720675305));
#36303=CARTESIAN_POINT('Ctrl Pts',(90.302498296487,35.5642571474778,119.841370183036));
#36304=CARTESIAN_POINT('Ctrl Pts',(90.4190306004264,36.4998571928572,119.894019690767));
#36305=CARTESIAN_POINT('Ctrl Pts',(90.1174360708708,37.2721761051156,119.946669198498));
#36306=CARTESIAN_POINT('Ctrl Pts',(89.8158415413152,38.0444950173741,119.999318706229));
#36307=CARTESIAN_POINT('Ctrl Pts',(89.0961201782648,38.6535327965116,120.05196821396));
#36308=CARTESIAN_POINT('Ctrl Pts',(88.2845465246492,38.823192474133,120.10461772169));
#36309=CARTESIAN_POINT('Ctrl Pts',(87.4729728710336,38.9928521517545,120.157267229421));
#36310=CARTESIAN_POINT('Ctrl Pts',(86.5695469268528,38.7231337278599,120.209916737152));
#36311=CARTESIAN_POINT('Ctrl Pts',(85.9838235012758,38.1363077943951,120.262566244883));
#36312=CARTESIAN_POINT('Ctrl Pts',(85.5208382620447,37.6724510775078,120.304183062425));
#36313=CARTESIAN_POINT('Ctrl Pts',(85.2563572505414,37.0104619014552,120.345799879966));
#36314=CARTESIAN_POINT('Ctrl Pts',(85.2503883725927,36.3527278457068,120.387416697508));
#36315=CARTESIAN_POINT('Origin',(87.7685555885722,36.3549260746835,114.));
#36316=CARTESIAN_POINT('',(85.2483527795145,36.3565049891663,121.387416697508));
#36317=CARTESIAN_POINT('',(85.2535609624353,36.356687859589,121.112583302492));
#36318=CARTESIAN_POINT('',(85.2510555885723,36.3549260746835,114.));
#36319=CARTESIAN_POINT('',(89.6820215852375,37.9909132780583,122.));
#36320=CARTESIAN_POINT('Ctrl Pts',(85.2483527795145,36.3565049891663,121.387416697508));
#36321=CARTESIAN_POINT('Ctrl Pts',(85.2538107988196,35.6272820046487,121.43366260848));
#36322=CARTESIAN_POINT('Ctrl Pts',(85.5883404885854,34.8938077603138,121.479908519451));
#36323=CARTESIAN_POINT('Ctrl Pts',(86.1458176141296,34.424974468788,121.526154430423));
#36324=CARTESIAN_POINT('Ctrl Pts',(86.7804876987815,33.8912225869868,121.578803938153));
#36325=CARTESIAN_POINT('Ctrl Pts',(87.7041222448919,33.7004745623117,121.631453445884));
#36326=CARTESIAN_POINT('Ctrl Pts',(88.4977390693866,33.9406283069268,121.684102953615));
#36327=CARTESIAN_POINT('Ctrl Pts',(89.2913558938813,34.1807820515418,121.736752461346));
#36328=CARTESIAN_POINT('Ctrl Pts',(89.9549549967602,34.8518375654471,121.789401969077));
#36329=CARTESIAN_POINT('Ctrl Pts',(90.1879202661796,35.6461235705208,121.842051476808));
#36330=CARTESIAN_POINT('Ctrl Pts',(90.420885535599,36.4404095755945,121.894700984538));
#36331=CARTESIAN_POINT('Ctrl Pts',(90.223216971559,37.3579260718367,121.947350492269));
#36332=CARTESIAN_POINT('Ctrl Pts',(89.6820215852375,37.9909132780583,122.));
#36333=CARTESIAN_POINT('',(85.851445435845,37.9934539601853,122.));
#36334=CARTESIAN_POINT('Origin',(87.7685555885722,36.3549260746835,122.));
#36335=CARTESIAN_POINT('Ctrl Pts',(85.8514365905238,37.9934601270861,122.));
#36336=CARTESIAN_POINT('Ctrl Pts',(86.3742571786771,38.6021753566418,121.949053726697));
#36337=CARTESIAN_POINT('Ctrl Pts',(87.2139816114554,38.9423514086554,121.898107453395));
#36338=CARTESIAN_POINT('Ctrl Pts',(88.0126524068155,38.8645885675841,121.847161180092));
#36339=CARTESIAN_POINT('Ctrl Pts',(88.8380243425583,38.7842259613178,121.794511672361));
#36340=CARTESIAN_POINT('Ctrl Pts',(89.6195517471766,38.2575122895073,121.74186216463));
#36341=CARTESIAN_POINT('Ctrl Pts',(90.0034363424997,37.5227256081353,121.6892126569));
#36342=CARTESIAN_POINT('Ctrl Pts',(90.3873209378227,36.7879389267633,121.636563149169));
#36343=CARTESIAN_POINT('Ctrl Pts',(90.3735627238505,35.8450792358298,121.583913641438));
#36344=CARTESIAN_POINT('Ctrl Pts',(89.968157966865,35.1218194832123,121.531264133707));
#36345=CARTESIAN_POINT('Ctrl Pts',(89.5627532098795,34.3985597305948,121.478614625976));
#36346=CARTESIAN_POINT('Ctrl Pts',(88.7657019098808,33.8948999162933,121.425965118245));
#36347=CARTESIAN_POINT('Ctrl Pts',(87.9384522395737,33.839048947649,121.373315610515));
#36348=CARTESIAN_POINT('Ctrl Pts',(87.1112025692666,33.7831979790047,121.320666102784));
#36349=CARTESIAN_POINT('Ctrl Pts',(86.2537545286512,34.1751558560176,121.268016595053));
#36350=CARTESIAN_POINT('Ctrl Pts',(85.7547622115628,34.837291622859,121.215367087322));
#36351=CARTESIAN_POINT('Ctrl Pts',(85.4300468048286,35.2681713728674,121.181105825712));
#36352=CARTESIAN_POINT('Ctrl Pts',(85.2571250437046,35.8134621481951,121.146844564102));
#36353=CARTESIAN_POINT('Ctrl Pts',(85.2535609624353,36.356687859589,121.112583302492));
#36354=CARTESIAN_POINT('Origin',(87.7685555885722,36.3549260746835,124.208423447177));
#36355=CARTESIAN_POINT('',(84.6902858090144,36.3557395542501,107.791576552823));
#36356=CARTESIAN_POINT('',(84.6999262747735,36.3552403524466,107.708423447177));
#36357=CARTESIAN_POINT('',(84.6950555885722,36.3549260746838,124.208423447177));
#36358=CARTESIAN_POINT('',(88.5623548711046,33.3857031209377,107.));
#36359=CARTESIAN_POINT('Ctrl Pts',(84.6999262747735,36.3552403524466,107.708423447177));
#36360=CARTESIAN_POINT('Ctrl Pts',(84.6996064101237,36.85041584334,107.682880329042));
#36361=CARTESIAN_POINT('Ctrl Pts',(85.0458587055101,38.3657324650862,107.604687703175));
#36362=CARTESIAN_POINT('Ctrl Pts',(87.4170211924556,39.9637884258442,107.473845569577));
#36363=CARTESIAN_POINT('Ctrl Pts',(90.6005810357291,38.6233305395511,107.315897046385));
#36364=CARTESIAN_POINT('Ctrl Pts',(91.2113484819485,35.2211464889414,107.157948523192));
#36365=CARTESIAN_POINT('Ctrl Pts',(89.5445934608762,33.6482971733151,107.052649507731));
#36366=CARTESIAN_POINT('Ctrl Pts',(88.5623548711045,33.3857031209377,107.));
#36367=CARTESIAN_POINT('',(86.9747563060389,33.385703120938,107.));
#36368=CARTESIAN_POINT('Origin',(87.7685555885722,36.3549260746835,107.));
#36369=CARTESIAN_POINT('Ctrl Pts',(84.6902858090144,36.3557395542501,107.791576552823));
#36370=CARTESIAN_POINT('Ctrl Pts',(84.690129740087,36.4002483939492,107.789262006108));
#36371=CARTESIAN_POINT('Ctrl Pts',(84.7110894559424,37.4570578636397,107.734297951662));
#36372=CARTESIAN_POINT('Ctrl Pts',(85.920358340807,39.4750889550508,107.626684389485));
#36373=CARTESIAN_POINT('Ctrl Pts',(89.3710241690437,39.6084644686119,107.468735866293));
#36374=CARTESIAN_POINT('Ctrl Pts',(91.3686332599885,36.7911510990924,107.3107873431));
#36375=CARTESIAN_POINT('Ctrl Pts',(90.1161181236528,33.6146079014889,107.154542054336));
#36376=CARTESIAN_POINT('Ctrl Pts',(87.9198086998421,33.1297337399419,107.050946273303));
#36377=CARTESIAN_POINT('Ctrl Pts',(86.9728422455434,33.3806145099939,107.));
#36378=CARTESIAN_POINT('Origin',(87.7685555885722,36.3549260746835,124.208423447177));
#36379=CARTESIAN_POINT('',(84.6986440547572,36.3567914692534,108.791576552823));
#36380=CARTESIAN_POINT('',(84.6934624439954,36.3523677970343,108.708423447177));
#36381=CARTESIAN_POINT('',(84.6950555885722,36.3549260746838,124.208423447177));
#36382=CARTESIAN_POINT('Ctrl Pts',(84.6934624439954,36.3523677970344,108.708423447177));
#36383=CARTESIAN_POINT('Ctrl Pts',(84.7008503007187,37.1811158847336,108.665444042093));
#36384=CARTESIAN_POINT('Ctrl Pts',(85.4724993959125,39.0372064318679,108.569815129278));
#36385=CARTESIAN_POINT('Ctrl Pts',(88.6015534780661,39.8844994763739,108.421536708732));
#36386=CARTESIAN_POINT('Ctrl Pts',(91.1794498546833,37.5869249364573,108.26358818554));
#36387=CARTESIAN_POINT('Ctrl Pts',(90.6647258333095,34.1722679839027,108.105639662347));
#36388=CARTESIAN_POINT('Ctrl Pts',(87.5242687079243,32.736697544997,107.947691139155));
#36389=CARTESIAN_POINT('Ctrl Pts',(85.0771138477131,34.2830645841973,107.815285734098));
#36390=CARTESIAN_POINT('Ctrl Pts',(84.7002657155484,35.8297594889657,107.735529836772));
#36391=CARTESIAN_POINT('Ctrl Pts',(84.6999262747735,36.3552403524466,107.708423447177));
#36392=CARTESIAN_POINT('Ctrl Pts',(84.6986440547572,36.3567914692533,108.791576552823));
#36393=CARTESIAN_POINT('Ctrl Pts',(84.6964999234298,36.7392744241785,108.771825719159));
#36394=CARTESIAN_POINT('Ctrl Pts',(84.939494334228,38.1387104097186,108.699425377765));
#36395=CARTESIAN_POINT('Ctrl Pts',(87.0264678344641,39.9047351075969,108.57437552864));
#36396=CARTESIAN_POINT('Ctrl Pts',(90.3353210088379,38.9168747734219,108.416427005448));
#36397=CARTESIAN_POINT('Ctrl Pts',(91.3169640944224,35.6061628347523,108.258478482255));
#36398=CARTESIAN_POINT('Ctrl Pts',(89.0813771113567,32.9743536285202,108.100529959063));
#36399=CARTESIAN_POINT('Ctrl Pts',(85.7056888771381,33.401213512673,107.944895982585));
#36400=CARTESIAN_POINT('Ctrl Pts',(84.6936798746098,35.3877959406313,107.841911513838));
#36401=CARTESIAN_POINT('Ctrl Pts',(84.6902858090144,36.3557395542501,107.791576552823));
#36402=CARTESIAN_POINT('Origin',(87.7685555885722,36.3549260746835,124.208423447177));
#36403=CARTESIAN_POINT('',(84.6967208028556,36.352333414281,109.791576552823));
#36404=CARTESIAN_POINT('',(84.6924244957587,36.3571941260871,109.708423447177));
#36405=CARTESIAN_POINT('',(84.6950555885722,36.3549260746838,124.208423447177));
#36406=CARTESIAN_POINT('Ctrl Pts',(84.6924244957587,36.3571941260872,109.708423447177));
#36407=CARTESIAN_POINT('Ctrl Pts',(84.6911853742644,36.5068138857211,109.700657262876));
#36408=CARTESIAN_POINT('Ctrl Pts',(84.7688482751212,37.6694639479526,109.640241570843));
#36409=CARTESIAN_POINT('Ctrl Pts',(86.2502054472947,39.6483231784334,109.527176371079));
#36410=CARTESIAN_POINT('Ctrl Pts',(89.696256450466,39.4267040036787,109.369227847887));
#36411=CARTESIAN_POINT('Ctrl Pts',(91.3945201363532,36.4199976317768,109.211279324695));
#36412=CARTESIAN_POINT('Ctrl Pts',(89.805231169669,33.3542919795258,109.053330801502));
#36413=CARTESIAN_POINT('Ctrl Pts',(86.3693521976711,33.0091718082685,108.89538227831));
#36414=CARTESIAN_POINT('Ctrl Pts',(84.7918202895625,34.9660087126265,108.780413160201));
#36415=CARTESIAN_POINT('Ctrl Pts',(84.691800221526,36.1659045581767,108.718093549824));
#36416=CARTESIAN_POINT('Ctrl Pts',(84.6934624439954,36.3523677970344,108.708423447177));
#36417=CARTESIAN_POINT('Ctrl Pts',(84.6967208028556,36.352333414281,109.791576552823));
#36418=CARTESIAN_POINT('Ctrl Pts',(84.7025802483439,37.0713395705354,109.754389432211));
#36419=CARTESIAN_POINT('Ctrl Pts',(85.3117911792528,38.8172613514562,109.664552803868));
#36420=CARTESIAN_POINT('Ctrl Pts',(88.2120005651333,39.9542599759734,109.522066667795));
#36421=CARTESIAN_POINT('Ctrl Pts',(91.0248783714271,37.9512375173972,109.364118144602));
#36422=CARTESIAN_POINT('Ctrl Pts',(90.8853473213453,34.5008878826802,109.20616962141));
#36423=CARTESIAN_POINT('Ctrl Pts',(87.9199160530301,32.731538577869,109.048221098218));
#36424=CARTESIAN_POINT('Ctrl Pts',(85.2052266838201,34.0578509982748,108.910023408688));
#36425=CARTESIAN_POINT('Ctrl Pts',(84.7022155028742,35.719695218788,108.82447522689));
#36426=CARTESIAN_POINT('Ctrl Pts',(84.6986440547572,36.3567914692533,108.791576552823));
#36427=CARTESIAN_POINT('Origin',(87.7685555885722,36.3549260746835,124.208423447177));
#36428=CARTESIAN_POINT('',(84.6902140242538,36.3556108815602,110.791576552823));
#36429=CARTESIAN_POINT('',(84.6998361685216,36.3552744910741,110.708423447177));
#36430=CARTESIAN_POINT('',(84.6950555885722,36.3549260746838,124.208423447177));
#36431=CARTESIAN_POINT('Ctrl Pts',(84.6998361685216,36.3552744910741,110.708423447177));
#36432=CARTESIAN_POINT('Ctrl Pts',(84.6993368730504,36.8438060463592,110.683220975927));
#36433=CARTESIAN_POINT('Ctrl Pts',(85.0389979619791,38.3522541503725,110.605368996946));
#36434=CARTESIAN_POINT('Ctrl Pts',(87.3945229743647,39.962134280427,110.474867510234));
#36435=CARTESIAN_POINT('Ctrl Pts',(90.5845853467483,38.6400579781975,110.316918987042));
#36436=CARTESIAN_POINT('Ctrl Pts',(91.2214391886919,35.2461220838395,110.158970463849));
#36437=CARTESIAN_POINT('Ctrl Pts',(88.7276684735458,32.8575050336255,110.001021940657));
#36438=CARTESIAN_POINT('Ctrl Pts',(85.529673083003,33.6014239812827,109.850839601766));
#36439=CARTESIAN_POINT('Ctrl Pts',(84.6995857848333,35.4924925169032,109.753306770606));
#36440=CARTESIAN_POINT('Ctrl Pts',(84.6924244957587,36.3571941260872,109.708423447177));
#36441=CARTESIAN_POINT('Ctrl Pts',(84.6902140242538,36.3556108815602,110.791576552823));
#36442=CARTESIAN_POINT('Ctrl Pts',(84.6900983802807,36.3935671694569,110.789602652993));
#36443=CARTESIAN_POINT('Ctrl Pts',(84.7078623206447,37.4438145955638,110.734979245433));
#36444=CARTESIAN_POINT('Ctrl Pts',(85.9003808808979,39.463265081444,110.627706330142));
#36445=CARTESIAN_POINT('Ctrl Pts',(89.3500610946321,39.6184653269691,110.46975780695));
#36446=CARTESIAN_POINT('Ctrl Pts',(91.365838365503,36.8147137894109,110.311809283757));
#36447=CARTESIAN_POINT('Ctrl Pts',(90.1200687486007,33.5940867128609,110.153860760565));
#36448=CARTESIAN_POINT('Ctrl Pts',(86.7422536682402,32.8766287223663,109.995912237372));
#36449=CARTESIAN_POINT('Ctrl Pts',(84.8711429126263,34.7392605484639,109.875150834792));
#36450=CARTESIAN_POINT('Ctrl Pts',(84.6942844481997,36.0533709954071,109.807038939942));
#36451=CARTESIAN_POINT('Ctrl Pts',(84.6967208028556,36.352333414281,109.791576552823));
#36452=CARTESIAN_POINT('Origin',(87.7685555885722,36.3549260746835,124.208423447177));
#36453=CARTESIAN_POINT('',(84.6985184073145,36.356868130103,111.791576552823));
#36454=CARTESIAN_POINT('',(84.6936553669982,36.3523302808631,111.708423447177));
#36455=CARTESIAN_POINT('',(84.6950555885722,36.3549260746838,124.208423447177));
#36456=CARTESIAN_POINT('Ctrl Pts',(84.6936553669982,36.3523302808631,111.708423447177));
#36457=CARTESIAN_POINT('Ctrl Pts',(84.7010362467823,37.1746423292757,111.665784688979));
#36458=CARTESIAN_POINT('Ctrl Pts',(85.4624962321431,39.0243972984566,111.570496423049));
#36459=CARTESIAN_POINT('Ctrl Pts',(88.5788817288668,39.8897843430778,111.422558649389));
#36460=CARTESIAN_POINT('Ctrl Pts',(91.1714507607514,37.608782477213,111.264610126197));
#36461=CARTESIAN_POINT('Ctrl Pts',(90.6787182344735,34.1909471455679,111.106661603004));
#36462=CARTESIAN_POINT('Ctrl Pts',(87.5474297456003,32.7351256943546,110.948713079812));
#36463=CARTESIAN_POINT('Ctrl Pts',(85.0842716491725,34.2698856564043,110.81596702787));
#36464=CARTESIAN_POINT('Ctrl Pts',(84.7003799319041,35.8232336730648,110.735870483658));
#36465=CARTESIAN_POINT('Ctrl Pts',(84.6998361685216,36.3552744910741,110.708423447177));
#36466=CARTESIAN_POINT('Ctrl Pts',(84.6985184073145,36.356868130103,111.791576552823));
#36467=CARTESIAN_POINT('Ctrl Pts',(84.6963187303381,36.7327156285024,111.772166366045));
#36468=CARTESIAN_POINT('Ctrl Pts',(84.9337530284994,38.1253552052707,111.700106671536));
#36469=CARTESIAN_POINT('Ctrl Pts',(87.0036900655912,39.8998984089112,111.575397469297));
#36470=CARTESIAN_POINT('Ctrl Pts',(90.3188173102936,38.9333002270083,111.417448946105));
#36471=CARTESIAN_POINT('Ctrl Pts',(91.3216998146175,35.6289686189096,111.259500422912));
#36472=CARTESIAN_POINT('Ctrl Pts',(89.1030545131784,32.9828405569386,111.10155189972));
#36473=CARTESIAN_POINT('Ctrl Pts',(85.7173071460403,33.3889405742214,110.945577276356));
#36474=CARTESIAN_POINT('Ctrl Pts',(84.6931829330837,35.3811653021443,110.842252160724));
#36475=CARTESIAN_POINT('Ctrl Pts',(84.6902140242538,36.3556108815602,110.791576552823));
#36476=CARTESIAN_POINT('Origin',(87.7685555885722,36.3549260746835,124.208423447177));
#36477=CARTESIAN_POINT('',(84.6968968951659,36.3523700745377,112.791576552823));
#36478=CARTESIAN_POINT('',(84.6922487139548,36.3571283698866,112.708423447177));
#36479=CARTESIAN_POINT('',(84.6950555885722,36.3549260746838,124.208423447177));
#36480=CARTESIAN_POINT('Ctrl Pts',(84.6922487139549,36.3571283698866,112.708423447177));
#36481=CARTESIAN_POINT('Ctrl Pts',(84.6910878504133,36.5001640619827,112.700997909761));
#36482=CARTESIAN_POINT('Ctrl Pts',(84.7648941835271,37.6561662491889,112.640922864614));
#36483=CARTESIAN_POINT('Ctrl Pts',(86.2290897937213,39.6385059043325,112.528198311736));
#36484=CARTESIAN_POINT('Ctrl Pts',(89.6764929464422,39.4390185618894,112.370249788544));
#36485=CARTESIAN_POINT('Ctrl Pts',(91.3940273240736,36.4432783597291,112.212301265351));
#36486=CARTESIAN_POINT('Ctrl Pts',(89.8244567428654,33.3674318278324,112.054352742159));
#36487=CARTESIAN_POINT('Ctrl Pts',(86.3908631124647,33.0002554690232,111.896404218966));
#36488=CARTESIAN_POINT('Ctrl Pts',(84.7960898684621,34.9526928622712,111.781094453973));
#36489=CARTESIAN_POINT('Ctrl Pts',(84.6919224802546,36.1592674361242,111.71843419671));
#36490=CARTESIAN_POINT('Ctrl Pts',(84.6936553669982,36.3523302808631,111.708423447177));
#36491=CARTESIAN_POINT('Ctrl Pts',(84.696896895166,36.3523700745377,112.791576552823));
#36492=CARTESIAN_POINT('Ctrl Pts',(84.7025959476166,37.0648934282683,112.754730079097));
#36493=CARTESIAN_POINT('Ctrl Pts',(85.3029472141711,38.8041984337469,112.66523409764));
#36494=CARTESIAN_POINT('Ctrl Pts',(88.188880109704,39.957033154659,112.523088608452));
#36495=CARTESIAN_POINT('Ctrl Pts',(91.0145613228638,37.9721134143629,112.365140085259));
#36496=CARTESIAN_POINT('Ctrl Pts',(90.8971878595435,34.5209390977093,112.207191562067));
#36497=CARTESIAN_POINT('Ctrl Pts',(87.9431786691826,32.7325849948854,112.049243038874));
#36498=CARTESIAN_POINT('Ctrl Pts',(85.2133167317337,34.0446657231455,111.91070470246));
#36499=CARTESIAN_POINT('Ctrl Pts',(84.702285283432,35.7132413699984,111.824815873776));
#36500=CARTESIAN_POINT('Ctrl Pts',(84.6985184073145,36.356868130103,111.791576552823));
#36501=CARTESIAN_POINT('Origin',(87.7685555885722,36.3549260746835,124.208423447177));
#36502=CARTESIAN_POINT('',(84.6901547879111,36.3554949863923,113.791576552823));
#36503=CARTESIAN_POINT('',(84.6998102914154,36.3553794097646,113.708423447177));
#36504=CARTESIAN_POINT('',(84.6950555885722,36.3549260746838,124.208423447177));
#36505=CARTESIAN_POINT('Ctrl Pts',(84.6998102914154,36.3553794097646,113.708423447177));
#36506=CARTESIAN_POINT('Ctrl Pts',(84.6991691146865,36.8372976164334,113.683561622813));
#36507=CARTESIAN_POINT('Ctrl Pts',(85.0323508879597,38.3389281403725,113.606050290717));
#36508=CARTESIAN_POINT('Ctrl Pts',(87.3713688061258,39.9596582548938,113.475889450891));
#36509=CARTESIAN_POINT('Ctrl Pts',(90.5698544680408,38.6580925947341,113.317940927699));
#36510=CARTESIAN_POINT('Ctrl Pts',(91.2284876335959,35.2683158984878,113.159992404506));
#36511=CARTESIAN_POINT('Ctrl Pts',(88.7501056430045,32.8637356012436,113.002043881314));
#36512=CARTESIAN_POINT('Ctrl Pts',(85.5401350086611,33.5887456327592,112.851520895538));
#36513=CARTESIAN_POINT('Ctrl Pts',(84.6993187555426,35.4859938605954,112.753647417492));
#36514=CARTESIAN_POINT('Ctrl Pts',(84.6922487139549,36.3571283698866,112.708423447177));
#36515=CARTESIAN_POINT('Ctrl Pts',(84.6901547879111,36.3554949863923,113.791576552823));
#36516=CARTESIAN_POINT('Ctrl Pts',(84.6900741046407,36.3868993254153,113.789943299879));
#36517=CARTESIAN_POINT('Ctrl Pts',(84.7046792722822,37.4305764228221,113.735660539204));
#36518=CARTESIAN_POINT('Ctrl Pts',(85.880460753186,39.4512054566615,113.628728270799));
#36519=CARTESIAN_POINT('Ctrl Pts',(89.3290733119119,39.6285528942548,113.470779747607));
#36520=CARTESIAN_POINT('Ctrl Pts',(91.3628119118867,36.837802457402,113.312831224414));
#36521=CARTESIAN_POINT('Ctrl Pts',(90.1377476178771,33.6092426903596,113.154882701222));
#36522=CARTESIAN_POINT('Ctrl Pts',(86.7646089666149,32.8701105416984,112.996934178029));
#36523=CARTESIAN_POINT('Ctrl Pts',(84.8762651228155,34.7259097370386,112.875832128563));
#36524=CARTESIAN_POINT('Ctrl Pts',(84.6944526363112,36.046776902396,112.807379586827));
#36525=CARTESIAN_POINT('Ctrl Pts',(84.696896895166,36.3523700745377,112.791576552823));
#36526=CARTESIAN_POINT('Origin',(87.7685555885722,36.3549260746835,124.208423447177));
#36527=CARTESIAN_POINT('',(84.6983875051821,36.3569420804818,114.791576552823));
#36528=CARTESIAN_POINT('',(84.6938495503113,36.3522971345412,114.708423447178));
#36529=CARTESIAN_POINT('',(84.6950555885722,36.3549260746838,124.208423447177));
#36530=CARTESIAN_POINT('Ctrl Pts',(84.6938495503113,36.3522971345412,114.708423447177));
#36531=CARTESIAN_POINT('Ctrl Pts',(84.7012113817027,37.1681725773841,114.666125335864));
#36532=CARTESIAN_POINT('Ctrl Pts',(85.4525660601554,39.0115737713416,114.571177716821));
#36533=CARTESIAN_POINT('Ctrl Pts',(88.5561677048511,39.8949145754395,114.423580590046));
#36534=CARTESIAN_POINT('Ctrl Pts',(91.1633296007399,37.630606613653,114.265632066854));
#36535=CARTESIAN_POINT('Ctrl Pts',(90.6925531471805,34.2096779052527,114.107683543661));
#36536=CARTESIAN_POINT('Ctrl Pts',(87.5706770365969,32.7337804673015,113.949735020469));
#36537=CARTESIAN_POINT('Ctrl Pts',(85.0913690235364,34.2565906200758,113.816648321641));
#36538=CARTESIAN_POINT('Ctrl Pts',(84.7005269249039,35.8167467519618,113.736211130544));
#36539=CARTESIAN_POINT('Ctrl Pts',(84.6998102914154,36.3553794097646,113.708423447177));
#36540=CARTESIAN_POINT('Ctrl Pts',(84.6983875051821,36.3569420804818,114.791576552823));
#36541=CARTESIAN_POINT('Ctrl Pts',(84.6961380025769,36.726153900471,114.772507012931));
#36542=CARTESIAN_POINT('Ctrl Pts',(84.9280663987333,38.1119998679058,114.700787965308));
#36543=CARTESIAN_POINT('Ctrl Pts',(86.9809435714815,39.8949141296362,114.576419409954));
#36544=CARTESIAN_POINT('Ctrl Pts',(90.3022090008012,38.9496223007136,114.418470886762));
#36545=CARTESIAN_POINT('Ctrl Pts',(91.3262879388381,35.6517983177679,114.260522363569));
#36546=CARTESIAN_POINT('Ctrl Pts',(89.1246791584273,32.9914788873536,114.102573840377));
#36547=CARTESIAN_POINT('Ctrl Pts',(85.7289940423128,33.376670074587,113.946258570128));
#36548=CARTESIAN_POINT('Ctrl Pts',(84.6926750088575,35.3745497095108,113.84259280761));
#36549=CARTESIAN_POINT('Ctrl Pts',(84.6901547879111,36.3554949863923,113.791576552823));
#36550=CARTESIAN_POINT('Origin',(87.7685555885722,36.3549260746835,124.208423447177));
#36551=CARTESIAN_POINT('',(84.6970696805284,36.352410699706,115.791576552823));
#36552=CARTESIAN_POINT('',(84.6920768117566,36.3570585844756,115.708423447177));
#36553=CARTESIAN_POINT('',(84.6950555885722,36.3549260746838,124.208423447177));
#36554=CARTESIAN_POINT('Ctrl Pts',(84.6920768117566,36.3570585844756,115.708423447177));
#36555=CARTESIAN_POINT('Ctrl Pts',(84.6909942761927,36.4935125897422,115.701338556647));
#36556=CARTESIAN_POINT('Ctrl Pts',(84.76098699805,37.6428717192427,115.641604158385));
#36557=CARTESIAN_POINT('Ctrl Pts',(86.2080376687123,39.6285533065152,115.529220252393));
#36558=CARTESIAN_POINT('Ctrl Pts',(89.6566506617342,39.4512058465864,115.371271729201));
#36559=CARTESIAN_POINT('Ctrl Pts',(91.3933852757362,36.4665556865659,115.213323206008));
#36560=CARTESIAN_POINT('Ctrl Pts',(89.843597056598,33.3806943525127,115.055374682816));
#36561=CARTESIAN_POINT('Ctrl Pts',(86.4124318479345,32.9914784637831,114.897426159623));
#36562=CARTESIAN_POINT('Ctrl Pts',(84.8004066819477,34.9393730713774,114.781775747744));
#36563=CARTESIAN_POINT('Ctrl Pts',(84.6920479276683,36.1526321879448,114.718774843595));
#36564=CARTESIAN_POINT('Ctrl Pts',(84.6938495503113,36.3522971345412,114.708423447177));
#36565=CARTESIAN_POINT('Ctrl Pts',(84.6970696805284,36.352410699706,115.791576552823));
#36566=CARTESIAN_POINT('Ctrl Pts',(84.7026032729329,37.0584473418203,115.755070725982));
#36567=CARTESIAN_POINT('Ctrl Pts',(85.2941694274566,38.7911233555952,115.665915391411));
#36568=CARTESIAN_POINT('Ctrl Pts',(88.1657423210009,39.9596578009367,115.524110549109));
#36569=CARTESIAN_POINT('Ctrl Pts',(91.0041104497151,37.9929226739502,115.366162025916));
#36570=CARTESIAN_POINT('Ctrl Pts',(90.9088993907837,34.5410658478232,115.208213502724));
#36571=CARTESIAN_POINT('Ctrl Pts',(87.9664341156267,32.7337809233254,115.050264979531));
#36572=CARTESIAN_POINT('Ctrl Pts',(85.2214706499081,34.0314892252637,114.911385996231));
#36573=CARTESIAN_POINT('Ctrl Pts',(84.7023487032794,35.7067889508769,114.825156520661));
#36574=CARTESIAN_POINT('Ctrl Pts',(84.6983875051821,36.3569420804818,114.791576552823));
#36575=CARTESIAN_POINT('Origin',(87.7685555885722,36.3549260746835,124.208423447177));
#36576=CARTESIAN_POINT('',(84.690105882654,36.3553778166865,116.791576552823));
#36577=CARTESIAN_POINT('',(84.6997776468007,36.3554836683198,116.708423447177));
#36578=CARTESIAN_POINT('',(84.6950555885722,36.3549260746838,124.208423447177));
#36579=CARTESIAN_POINT('Ctrl Pts',(84.6997776468007,36.3554836683198,116.708423447177));
#36580=CARTESIAN_POINT('Ctrl Pts',(84.6989993421585,36.8307861836476,116.683902269698));
#36581=CARTESIAN_POINT('Ctrl Pts',(85.0257621552687,38.3255989427417,116.606731584489));
#36582=CARTESIAN_POINT('Ctrl Pts',(87.3482310145089,39.9570336082856,116.476911391548));
#36583=CARTESIAN_POINT('Ctrl Pts',(90.5550080912271,38.6760322509801,116.318962868356));
#36584=CARTESIAN_POINT('Ctrl Pts',(91.2353934299102,35.2905545168799,116.161014345163));
#36585=CARTESIAN_POINT('Ctrl Pts',(88.7725023369588,32.8701101028426,116.003065821971));
#36586=CARTESIAN_POINT('Ctrl Pts',(85.5506677531235,33.576088055363,115.852202189309));
#36587=CARTESIAN_POINT('Ctrl Pts',(84.6990388556109,35.4794904006645,115.753988064378));
#36588=CARTESIAN_POINT('Ctrl Pts',(84.6920768117566,36.3570585844756,115.708423447177));
#36589=CARTESIAN_POINT('Ctrl Pts',(84.690105882654,36.3553778166865,116.791576552823));
#36590=CARTESIAN_POINT('Ctrl Pts',(84.690054395401,36.3802311048682,116.790283946765));
#36591=CARTESIAN_POINT('Ctrl Pts',(84.7015398827634,37.4173420024755,116.736341832976));
#36592=CARTESIAN_POINT('Ctrl Pts',(85.8606184709768,39.4390181734991,116.629750211456));
#36593=CARTESIAN_POINT('Ctrl Pts',(89.3080211895539,39.6385054908189,116.471801688264));
#36594=CARTESIAN_POINT('Ctrl Pts',(91.3596372684504,36.8608712170826,116.313853165071));
#36595=CARTESIAN_POINT('Ctrl Pts',(90.1553288060137,33.6245118703589,116.155904641879));
#36596=CARTESIAN_POINT('Ctrl Pts',(86.7870056577489,32.8637360409022,115.997956118686));
#36597=CARTESIAN_POINT('Ctrl Pts',(84.8814395432927,34.71255787358,115.876513422334));
#36598=CARTESIAN_POINT('Ctrl Pts',(84.6946226040563,36.0401857418374,115.807720233713));
#36599=CARTESIAN_POINT('Ctrl Pts',(84.6970696805284,36.352410699706,115.791576552823));
#36600=CARTESIAN_POINT('Origin',(87.7685555885722,36.3549260746835,124.208423447177));
#36601=CARTESIAN_POINT('',(84.6982514675662,36.3570130097076,117.791576552823));
#36602=CARTESIAN_POINT('',(84.6940447533955,36.3522684579846,117.708423447177));
#36603=CARTESIAN_POINT('',(84.6950555885722,36.3549260746838,124.208423447177));
#36604=CARTESIAN_POINT('Ctrl Pts',(84.6940447533956,36.3522684579846,117.708423447177));
#36605=CARTESIAN_POINT('Ctrl Pts',(84.7013751718839,37.1617057043996,117.66646598275));
#36606=CARTESIAN_POINT('Ctrl Pts',(85.4427051945229,38.9987326982796,117.571859010592));
#36607=CARTESIAN_POINT('Ctrl Pts',(88.5334212078769,39.8998988553421,117.424602530703));
#36608=CARTESIAN_POINT('Ctrl Pts',(91.1550684753794,37.6523781542154,117.266654007511));
#36609=CARTESIAN_POINT('Ctrl Pts',(90.7062675045469,34.2284971128012,117.108705484318));
#36610=CARTESIAN_POINT('Ctrl Pts',(87.5939324859696,32.7325845387109,116.950756961126));
#36611=CARTESIAN_POINT('Ctrl Pts',(85.0985267224163,34.2433006021635,116.817329615412));
#36612=CARTESIAN_POINT('Ctrl Pts',(84.700670442835,35.8102624556703,116.736551777429));
#36613=CARTESIAN_POINT('Ctrl Pts',(84.6997776468007,36.3554836683198,116.708423447177));
#36614=CARTESIAN_POINT('Ctrl Pts',(84.6982514675662,36.3570130097076,117.791576552823));
#36615=CARTESIAN_POINT('Ctrl Pts',(84.6959578356337,36.7195890211696,117.772847659816));
#36616=CARTESIAN_POINT('Ctrl Pts',(84.9224341684481,38.0986442956688,117.701469259079));
#36617=CARTESIAN_POINT('Ctrl Pts',(86.9582295503262,39.8897838979207,117.577441350611));
#36618=CARTESIAN_POINT('Ctrl Pts',(90.2854962296813,38.9658373960053,117.419492827418));
#36619=CARTESIAN_POINT('Ctrl Pts',(91.3307293790144,35.6746570063435,117.261544304226));
#36620=CARTESIAN_POINT('Ctrl Pts',(89.1462478911809,33.0002558914885,117.103595781033));
#36621=CARTESIAN_POINT('Ctrl Pts',(85.7407542491592,33.3644273369264,116.946939863899));
#36622=CARTESIAN_POINT('Ctrl Pts',(84.6921515374552,35.367924702503,116.842933454495));
#36623=CARTESIAN_POINT('Ctrl Pts',(84.690105882654,36.3553778166865,116.791576552823));
#36624=CARTESIAN_POINT('Origin',(87.7685555885722,36.3549260746835,124.208423447177));
#36625=CARTESIAN_POINT('',(84.69723893856,36.352455210645,118.791576552823));
#36626=CARTESIAN_POINT('',(84.6919091520139,36.3569848689092,118.708423447178));
#36627=CARTESIAN_POINT('',(84.6950555885722,36.3549260746838,124.208423447177));
#36628=CARTESIAN_POINT('Ctrl Pts',(84.6919091520139,36.3569848689092,118.708423447178));
#36629=CARTESIAN_POINT('Ctrl Pts',(84.690904716919,36.48685954633,118.701679203533));
#36630=CARTESIAN_POINT('Ctrl Pts',(84.7571265200965,37.6295804150404,118.642285452157));
#36631=CARTESIAN_POINT('Ctrl Pts',(86.1870498833489,39.6184657379601,118.53024219305));
#36632=CARTESIAN_POINT('Ctrl Pts',(89.6367305315139,39.4632654728871,118.372293669858));
#36633=CARTESIAN_POINT('Ctrl Pts',(91.3925937769666,36.4898284108945,118.214345146665));
#36634=CARTESIAN_POINT('Ctrl Pts',(89.8626518171021,33.3940795037413,118.056396623473));
#36635=CARTESIAN_POINT('Ctrl Pts',(86.4340564959065,32.9828401322801,117.89844810028));
#36636=CARTESIAN_POINT('Ctrl Pts',(84.8047721902053,34.926050666858,117.782457041515));
#36637=CARTESIAN_POINT('Ctrl Pts',(84.6921767388961,36.1459991276468,117.719115490481));
#36638=CARTESIAN_POINT('Ctrl Pts',(84.6940447533956,36.3522684579846,117.708423447177));
#36639=CARTESIAN_POINT('Ctrl Pts',(84.69723893856,36.352455210645,118.791576552823));
#36640=CARTESIAN_POINT('Ctrl Pts',(84.7026024115443,37.0520011646411,118.755411372868));
#36641=CARTESIAN_POINT('Ctrl Pts',(85.2854576115966,38.7780364187139,118.666596685182));
#36642=CARTESIAN_POINT('Ctrl Pts',(88.1425881556754,39.9621338261614,118.525132489766));
#36643=CARTESIAN_POINT('Ctrl Pts',(90.9935261761534,38.0136643991501,118.367183966573));
#36644=CARTESIAN_POINT('Ctrl Pts',(90.9204814465843,34.5612673829304,118.209235443381));
#36645=CARTESIAN_POINT('Ctrl Pts',(87.989681403696,32.7351261502086,118.051286920188));
#36646=CARTESIAN_POINT('Ctrl Pts',(85.2296887066039,34.0183220575488,117.912067290002));
#36647=CARTESIAN_POINT('Ctrl Pts',(84.7024055521176,35.7003377225505,117.825497167547));
#36648=CARTESIAN_POINT('Ctrl Pts',(84.6982514675662,36.3570130097076,117.791576552823));
#36649=CARTESIAN_POINT('Origin',(87.7685555885722,36.3549260746835,124.208423447177));
#36650=CARTESIAN_POINT('',(84.6900676527761,36.3552596744725,119.791576552823));
#36651=CARTESIAN_POINT('',(84.6997382737804,36.3555871001389,119.708423447177));
#36652=CARTESIAN_POINT('',(84.6950555885722,36.3549260746838,124.208423447177));
#36653=CARTESIAN_POINT('Ctrl Pts',(84.6997382737804,36.3555871001389,119.708423447177));
#36654=CARTESIAN_POINT('Ctrl Pts',(84.6988277206765,36.8242717120483,119.684242916584));
#36655=CARTESIAN_POINT('Ctrl Pts',(85.0192315268969,38.3122667840641,119.60741287826));
#36656=CARTESIAN_POINT('Ctrl Pts',(87.325110556169,39.9542604293109,119.477933332205));
#36657=CARTESIAN_POINT('Ctrl Pts',(90.5400468282905,38.6938762179578,119.319984809012));
#36658=CARTESIAN_POINT('Ctrl Pts',(91.2421562905436,35.3128370145015,119.16203628582));
#36659=CARTESIAN_POINT('Ctrl Pts',(88.7948576381488,32.8766282843233,119.004087762628));
#36660=CARTESIAN_POINT('Ctrl Pts',(85.5612714692701,33.5634516241642,118.85288348308));
#36661=CARTESIAN_POINT('Ctrl Pts',(84.6987459243371,35.472981905946,118.754328711263));
#36662=CARTESIAN_POINT('Ctrl Pts',(84.6919091520139,36.3569848689092,118.708423447178));
#36663=CARTESIAN_POINT('Ctrl Pts',(84.6900676527761,36.3552596744725,119.791576552823));
#36664=CARTESIAN_POINT('Ctrl Pts',(84.6900392079454,36.373562642628,119.79062459365));
#36665=CARTESIAN_POINT('Ctrl Pts',(84.6984438504603,37.4041114728583,119.737023126747));
#36666=CARTESIAN_POINT('Ctrl Pts',(85.8408549696731,39.426703616461,119.630772152113));
#36667=CARTESIAN_POINT('Ctrl Pts',(89.286905538518,39.6483227638767,119.472823628921));
#36668=CARTESIAN_POINT('Ctrl Pts',(91.3563145937352,36.8839190889564,119.314875105728));
#36669=CARTESIAN_POINT('Ctrl Pts',(90.1728115748451,33.639893637919,119.156926582536));
#36670=CARTESIAN_POINT('Ctrl Pts',(86.8094428243991,32.8575054740432,118.998978059343));
#36671=CARTESIAN_POINT('Ctrl Pts',(84.886666399667,34.6992050833937,118.877194716105));
#36672=CARTESIAN_POINT('Ctrl Pts',(84.6947942321655,36.0335975466026,118.808060880599));
#36673=CARTESIAN_POINT('Ctrl Pts',(84.69723893856,36.352455210645,118.791576552823));
#36674=CARTESIAN_POINT('Origin',(87.7685555885722,36.3549260746835,124.208423447177));
#36675=CARTESIAN_POINT('',(84.6981142843292,36.357076956871,120.791576552823));
#36676=CARTESIAN_POINT('',(84.6942410152602,36.3522423579964,120.708423447177));
#36677=CARTESIAN_POINT('',(84.6950555885722,36.3549260746838,124.208423447177));
#36678=CARTESIAN_POINT('Ctrl Pts',(84.6942410152602,36.3522423579965,120.708423447177));
#36679=CARTESIAN_POINT('Ctrl Pts',(84.7015281439098,37.1552396252626,120.666806629636));
#36680=CARTESIAN_POINT('Ctrl Pts',(85.4329129711515,38.9858770551906,120.572540304363));
#36681=CARTESIAN_POINT('Ctrl Pts',(88.5106434364707,39.9047355577889,120.42562447136));
#36682=CARTESIAN_POINT('Ctrl Pts',(91.146667598539,37.6740968914383,120.267675948167));
#36683=CARTESIAN_POINT('Ctrl Pts',(90.7198608027206,34.2474036567132,120.109727424975));
#36684=CARTESIAN_POINT('Ctrl Pts',(87.6171951050278,32.7315381211201,119.951778901782));
#36685=CARTESIAN_POINT('Ctrl Pts',(85.1057449826314,34.2300157885499,119.818010909183));
#36686=CARTESIAN_POINT('Ctrl Pts',(84.7008103145862,35.8037807016134,119.736892424315));
#36687=CARTESIAN_POINT('Ctrl Pts',(84.6997382737804,36.3555871001389,119.708423447177));
#36688=CARTESIAN_POINT('Ctrl Pts',(84.6981142843292,36.357076956871,120.791576552823));
#36689=CARTESIAN_POINT('Ctrl Pts',(84.6957789541399,36.7130204125928,120.773188306702));
#36690=CARTESIAN_POINT('Ctrl Pts',(84.9168437417748,38.0853010552934,120.70215055285));
#36691=CARTESIAN_POINT('Ctrl Pts',(86.9355578127517,39.8844990120122,120.578463291268));
#36692=CARTESIAN_POINT('Ctrl Pts',(90.2686753707106,38.9819491786592,120.420514768075));
#36693=CARTESIAN_POINT('Ctrl Pts',(91.3350260504491,35.6975416344974,120.262566244883));
#36694=CARTESIAN_POINT('Ctrl Pts',(89.1677588017562,33.0091722323982,120.10461772169));
#36695=CARTESIAN_POINT('Ctrl Pts',(85.7525883791808,33.3522123095062,119.94762115767));
#36696=CARTESIAN_POINT('Ctrl Pts',(84.6916123913094,35.361289961862,119.843274101381));
#36697=CARTESIAN_POINT('Ctrl Pts',(84.6900676527761,36.3552596744725,119.791576552823));
#36698=CARTESIAN_POINT('Origin',(87.7685555885722,36.3549260746835,124.208423447177));
#36699=CARTESIAN_POINT('',(84.6982769289314,36.3519105223041,121.791576552823));
#36700=CARTESIAN_POINT('',(84.6917558532639,36.3568536987801,121.708423447177));
#36701=CARTESIAN_POINT('',(84.6950555885722,36.3549260746838,124.208423447177));
#36702=CARTESIAN_POINT('',(86.9747563060389,33.385703120938,122.));
#36703=CARTESIAN_POINT('Ctrl Pts',(86.9747563060389,33.385703120938,122.));
#36704=CARTESIAN_POINT('Ctrl Pts',(85.9925177162673,33.6482971733158,121.947350492269));
#36705=CARTESIAN_POINT('Ctrl Pts',(84.8928209565869,34.686033271266,121.877876009877));
#36706=CARTESIAN_POINT('Ctrl Pts',(84.6959357391912,36.0264346664739,121.808401527484));
#36707=CARTESIAN_POINT('Ctrl Pts',(84.6982769289315,36.3519105223041,121.791576552823));
#36708=CARTESIAN_POINT('',(88.5642644266099,33.3806265661435,122.));
#36709=CARTESIAN_POINT('Origin',(87.7685555885722,36.3549260746835,122.));
#36710=CARTESIAN_POINT('Ctrl Pts',(88.5642690620867,33.3806142427251,122.));
#36711=CARTESIAN_POINT('Ctrl Pts',(87.6173029036983,33.1297337676241,121.949053726697));
#36712=CARTESIAN_POINT('Ctrl Pts',(85.556753483317,33.5846352576989,121.851861542423));
#36713=CARTESIAN_POINT('Ctrl Pts',(84.6984192980838,35.4665788853084,121.754669358149));
#36714=CARTESIAN_POINT('Ctrl Pts',(84.6917558532639,36.3568536987801,121.708423447177));
#36715=CARTESIAN_POINT('Origin',(-36.3549260746835,-87.7685555885722,114.));
#36716=CARTESIAN_POINT('',(-38.8684363400902,-87.7682981264136,107.387416697508));
#36717=CARTESIAN_POINT('',(-38.8705162236156,-87.7721288317432,107.112583302492));
#36718=CARTESIAN_POINT('',(-38.8724260746835,-87.7685555885722,114.));
#36719=CARTESIAN_POINT('',(-38.2683920713482,-86.1325683851969,107.));
#36720=CARTESIAN_POINT('Ctrl Pts',(-38.8705162236156,-87.7721288317432,
107.112583302492));
#36721=CARTESIAN_POINT('Ctrl Pts',(-38.8653710199197,-87.1794939521863,
107.075055534995));
#36722=CARTESIAN_POINT('Ctrl Pts',(-38.6541479027674,-86.5837520282675,
107.037527767497));
#36723=CARTESIAN_POINT('Ctrl Pts',(-38.2683920713482,-86.1325683851969,
107.));
#36724=CARTESIAN_POINT('',(-38.8724260746835,-87.7685555885722,107.));
#36725=CARTESIAN_POINT('Origin',(-36.3549260746835,-87.7685555885722,107.));
#36726=CARTESIAN_POINT('',(-38.8724260746835,-87.7685555885722,106.));
#36727=CARTESIAN_POINT('',(-38.8724260746835,-87.7685555885722,114.));
#36728=CARTESIAN_POINT('Origin',(-36.3549260746835,-87.7685555885722,106.));
#36729=CARTESIAN_POINT('',(-34.4378158180085,-86.1300276446784,107.));
#36730=CARTESIAN_POINT('Origin',(-36.3549260746835,-87.7685555885722,107.));
#36731=CARTESIAN_POINT('Ctrl Pts',(-34.4378069719681,-86.1300214773102,
107.));
#36732=CARTESIAN_POINT('Ctrl Pts',(-34.9606275290818,-85.5213064137174,
107.050946273303));
#36733=CARTESIAN_POINT('Ctrl Pts',(-35.8003520377837,-85.1811300520207,
107.101892546605));
#36734=CARTESIAN_POINT('Ctrl Pts',(-36.5990228985553,-85.2588928357685,
107.152838819908));
#36735=CARTESIAN_POINT('Ctrl Pts',(-37.4243949018965,-85.3392553827949,
107.205488327639));
#36736=CARTESIAN_POINT('Ctrl Pts',(-38.2059223628864,-85.865969264881,107.25813783537));
#36737=CARTESIAN_POINT('Ctrl Pts',(-38.589806978663,-86.6007560325992,107.3107873431));
#36738=CARTESIAN_POINT('Ctrl Pts',(-38.7760501272496,-86.9572407562258,
107.336330461236));
#36739=CARTESIAN_POINT('Ctrl Pts',(-38.8686983365902,-87.3627005068745,
107.361873579372));
#36740=CARTESIAN_POINT('Ctrl Pts',(-38.8684363400902,-87.7682981264136,
107.387416697508));
#36741=CARTESIAN_POINT('Origin',(-36.3549260746835,-87.7685555885722,114.));
#36742=CARTESIAN_POINT('',(-38.8737308567828,-87.7706510706098,108.387416697508));
#36743=CARTESIAN_POINT('',(-38.8763331790899,-87.7678892788988,108.112583302492));
#36744=CARTESIAN_POINT('',(-38.8724260746835,-87.7685555885722,114.));
#36745=CARTESIAN_POINT('Ctrl Pts',(-38.8763331790899,-87.7678892788988,
108.112583302492));
#36746=CARTESIAN_POINT('Ctrl Pts',(-38.8764610150598,-87.7314321411263,
108.110268755777));
#36747=CARTESIAN_POINT('Ctrl Pts',(-38.8757380641522,-87.6949802400596,
108.107954209062));
#36748=CARTESIAN_POINT('Ctrl Pts',(-38.8741484476744,-87.6585662372005,
108.105639662347));
#36749=CARTESIAN_POINT('Ctrl Pts',(-38.8379890889129,-86.8302488337614,
108.052990154616));
#36750=CARTESIAN_POINT('Ctrl Pts',(-38.3533856737909,-86.021541331288,108.000340646886));
#36751=CARTESIAN_POINT('Ctrl Pts',(-37.6400112436482,-85.5989796556856,
107.947691139155));
#36752=CARTESIAN_POINT('Ctrl Pts',(-36.9266368135056,-85.1764179800833,
107.895041631424));
#36753=CARTESIAN_POINT('Ctrl Pts',(-35.9844913683424,-85.140002131352,107.842392123693));
#36754=CARTESIAN_POINT('Ctrl Pts',(-35.2407121334911,-85.5064038253269,
107.789742615962));
#36755=CARTESIAN_POINT('Ctrl Pts',(-34.4969328986398,-85.8728055193019,
107.737093108232));
#36756=CARTESIAN_POINT('Ctrl Pts',(-33.9515198741004,-86.6420247559832,
107.684443600501));
#36757=CARTESIAN_POINT('Ctrl Pts',(-33.8516662037545,-87.465012158015,107.63179409277));
#36758=CARTESIAN_POINT('Ctrl Pts',(-33.7518125334087,-88.2879995600469,
107.579144585039));
#36759=CARTESIAN_POINT('Ctrl Pts',(-34.0975182172564,-89.1647551274293,
107.526495077308));
#36760=CARTESIAN_POINT('Ctrl Pts',(-34.7321882273048,-89.6985070179526,
107.473845569577));
#36761=CARTESIAN_POINT('Ctrl Pts',(-35.3668582373533,-90.232258908476,107.421196061847));
#36762=CARTESIAN_POINT('Ctrl Pts',(-36.2904925736025,-90.4230071221403,
107.368546554116));
#36763=CARTESIAN_POINT('Ctrl Pts',(-37.0841095226148,-90.1828532548222,
107.315897046385));
#36764=CARTESIAN_POINT('Ctrl Pts',(-37.8777264716271,-89.9426993875041,
107.263247538654));
#36765=CARTESIAN_POINT('Ctrl Pts',(-38.5413260334026,-89.2716434392036,
107.210598030923));
#36766=CARTESIAN_POINT('Ctrl Pts',(-38.7742912799133,-88.4773574901821,
107.157948523192));
#36767=CARTESIAN_POINT('Ctrl Pts',(-38.8412024457151,-88.249226472251,107.142826782959));
#36768=CARTESIAN_POINT('Ctrl Pts',(-38.8725894733431,-88.0109298929199,
107.127705042726));
#36769=CARTESIAN_POINT('Ctrl Pts',(-38.8705162236156,-87.7721288317432,
107.112583302492));
#36770=CARTESIAN_POINT('Ctrl Pts',(-38.8684363400902,-87.7682981264136,
107.387416697508));
#36771=CARTESIAN_POINT('Ctrl Pts',(-38.8681583090697,-88.1987188383852,
107.414523087103));
#36772=CARTESIAN_POINT('Ctrl Pts',(-38.7632496215152,-88.6292948111527,
107.441629476698));
#36773=CARTESIAN_POINT('Ctrl Pts',(-38.5545285816793,-89.0016622291512,
107.468735866293));
#36774=CARTESIAN_POINT('Ctrl Pts',(-38.1491237983557,-89.7249220046346,
107.521385374024));
#36775=CARTESIAN_POINT('Ctrl Pts',(-37.3520724611453,-90.2285819022512,
107.574034881755));
#36776=CARTESIAN_POINT('Ctrl Pts',(-36.5248227413449,-90.2844328864611,
107.626684389485));
#36777=CARTESIAN_POINT('Ctrl Pts',(-35.6975730215444,-90.3402838706711,
107.679333897216));
#36778=CARTESIAN_POINT('Ctrl Pts',(-34.8401249191538,-89.9483259414745,
107.731983404947));
#36779=CARTESIAN_POINT('Ctrl Pts',(-34.3411325694982,-89.2861901269712,
107.784632912678));
#36780=CARTESIAN_POINT('Ctrl Pts',(-33.8421402198425,-88.624054312468,107.837282420409));
#36781=CARTESIAN_POINT('Ctrl Pts',(-33.7016036229218,-87.6917406126582,
107.889931928139));
#36782=CARTESIAN_POINT('Ctrl Pts',(-33.9832605857992,-86.9119270488255,
107.94258143587));
#36783=CARTESIAN_POINT('Ctrl Pts',(-34.2649175486767,-86.1321134849928,
107.995230943601));
#36784=CARTESIAN_POINT('Ctrl Pts',(-34.9687680713523,-85.5048000571372,
108.047880451332));
#36785=CARTESIAN_POINT('Ctrl Pts',(-35.7757187646338,-85.3143562592227,
108.100529959063));
#36786=CARTESIAN_POINT('Ctrl Pts',(-36.5826694579152,-85.1239124613082,
108.153179466794));
#36787=CARTESIAN_POINT('Ctrl Pts',(-37.4927203218023,-85.3703382933347,
108.205828974524));
#36788=CARTESIAN_POINT('Ctrl Pts',(-38.093320179937,-85.9419269203423,108.258478482255));
#36789=CARTESIAN_POINT('Ctrl Pts',(-38.583608232169,-86.4085322163941,108.30145788734));
#36790=CARTESIAN_POINT('Ctrl Pts',(-38.8676794726009,-87.0918245926314,
108.344437292424));
#36791=CARTESIAN_POINT('Ctrl Pts',(-38.8737308567828,-87.7706510706098,
108.387416697508));
#36792=CARTESIAN_POINT('Origin',(-36.3549260746835,-87.7685555885722,114.));
#36793=CARTESIAN_POINT('',(-38.8745810387237,-87.7666978306399,109.387416697508));
#36794=CARTESIAN_POINT('',(-38.8694869524425,-87.7670276463177,109.112583302492));
#36795=CARTESIAN_POINT('',(-38.8724260746835,-87.7685555885722,114.));
#36796=CARTESIAN_POINT('Ctrl Pts',(-38.8694869524425,-87.7670276463177,
109.112583302492));
#36797=CARTESIAN_POINT('Ctrl Pts',(-38.8712432078539,-87.4537363139361,
109.092832468829));
#36798=CARTESIAN_POINT('Ctrl Pts',(-38.8169460127038,-87.1410318012893,
109.073081635165));
#36799=CARTESIAN_POINT('Ctrl Pts',(-38.7038064348735,-86.8513056056821,
109.053330801502));
#36800=CARTESIAN_POINT('Ctrl Pts',(-38.402211920982,-86.0789867337058,109.000681293771));
#36801=CARTESIAN_POINT('Ctrl Pts',(-37.6824905952959,-85.4699489867722,
108.94803178604));
#36802=CARTESIAN_POINT('Ctrl Pts',(-36.8709169839095,-85.3002893177264,
108.89538227831));
#36803=CARTESIAN_POINT('Ctrl Pts',(-36.0593433725232,-85.1306296486805,
108.842732770579));
#36804=CARTESIAN_POINT('Ctrl Pts',(-35.1559174754367,-85.4003480575224,
108.790083262848));
#36805=CARTESIAN_POINT('Ctrl Pts',(-34.5701940802303,-85.9871739609405,
108.737433755117));
#36806=CARTESIAN_POINT('Ctrl Pts',(-33.984470685024,-86.5739998643585,108.684784247386));
#36807=CARTESIAN_POINT('Ctrl Pts',(-33.716449791698,-87.4779332623528,108.632134739655));
#36808=CARTESIAN_POINT('Ctrl Pts',(-33.8876337833753,-88.2891852612251,
108.579485231925));
#36809=CARTESIAN_POINT('Ctrl Pts',(-34.0588177750527,-89.1004372600974,
108.526835724194));
#36810=CARTESIAN_POINT('Ctrl Pts',(-34.6692066517334,-89.8190078598478,
108.474186216463));
#36811=CARTESIAN_POINT('Ctrl Pts',(-35.4420915705444,-90.1191531246981,
108.421536708732));
#36812=CARTESIAN_POINT('Ctrl Pts',(-36.2149764893555,-90.4192983895484,
108.368887201001));
#36813=CARTESIAN_POINT('Ctrl Pts',(-37.1503574502968,-90.3010183194988,
108.316237693271));
#36814=CARTESIAN_POINT('Ctrl Pts',(-37.8241902795669,-89.8179146322715,
108.26358818554));
#36815=CARTESIAN_POINT('Ctrl Pts',(-38.4684004660316,-89.3560488654054,
108.213253224524));
#36816=CARTESIAN_POINT('Ctrl Pts',(-38.8735531018844,-88.5607307440123,
108.162918263508));
#36817=CARTESIAN_POINT('Ctrl Pts',(-38.8763331790899,-87.7678892788988,
108.112583302492));
#36818=CARTESIAN_POINT('Ctrl Pts',(-38.8737308567828,-87.7706510706098,
108.387416697508));
#36819=CARTESIAN_POINT('Ctrl Pts',(-38.875092381124,-87.9233828664173,108.397086800155));
#36820=CARTESIAN_POINT('Ctrl Pts',(-38.8623799172478,-88.0758885884459,
108.406756902801));
#36821=CARTESIAN_POINT('Ctrl Pts',(-38.8347756504559,-88.2256493719635,
108.416427005448));
#36822=CARTESIAN_POINT('Ctrl Pts',(-38.684482410458,-89.0410317745883,108.469076513179));
#36823=CARTESIAN_POINT('Ctrl Pts',(-38.0927470780801,-89.7750451578491,
108.521726020909));
#36824=CARTESIAN_POINT('Ctrl Pts',(-37.32782541498,-90.0949372694507,108.57437552864));
#36825=CARTESIAN_POINT('Ctrl Pts',(-36.5629037518798,-90.4148293810522,
108.627025036371));
#36826=CARTESIAN_POINT('Ctrl Pts',(-35.6247957580574,-90.3206002209945,
108.679674544102));
#36827=CARTESIAN_POINT('Ctrl Pts',(-34.938777674606,-89.8549663909368,108.732324051833));
#36828=CARTESIAN_POINT('Ctrl Pts',(-34.2527595911546,-89.3893325608792,
108.784973559563));
#36829=CARTESIAN_POINT('Ctrl Pts',(-33.8188314180741,-88.5522940608215,
108.837623067294));
#36830=CARTESIAN_POINT('Ctrl Pts',(-33.8337082597499,-87.7233099332487,
108.890272575025));
#36831=CARTESIAN_POINT('Ctrl Pts',(-33.8485851014256,-86.894325805676,108.942922082756));
#36832=CARTESIAN_POINT('Ctrl Pts',(-34.3122669578576,-86.0733960505882,
108.995571590487));
#36833=CARTESIAN_POINT('Ctrl Pts',(-35.0145505326977,-85.632676510197,109.048221098218));
#36834=CARTESIAN_POINT('Ctrl Pts',(-35.7168341075378,-85.1919569698057,
109.100870605948));
#36835=CARTESIAN_POINT('Ctrl Pts',(-36.6577194007862,-85.1314476441111,
109.153520113679));
#36836=CARTESIAN_POINT('Ctrl Pts',(-37.410670459096,-85.4785796025718,109.20616962141));
#36837=CARTESIAN_POINT('Ctrl Pts',(-38.1636215174058,-85.8257115610326,
109.258819129141));
#36838=CARTESIAN_POINT('Ctrl Pts',(-38.728638340777,-86.5804848036488,109.311468636872));
#36839=CARTESIAN_POINT('Ctrl Pts',(-38.8495791023889,-87.4007343163658,
109.364118144603));
#36840=CARTESIAN_POINT('Ctrl Pts',(-38.8674187420126,-87.521727069457,109.371884328904));
#36841=CARTESIAN_POINT('Ctrl Pts',(-38.8755960015225,-87.6441444807647,
109.379650513206));
#36842=CARTESIAN_POINT('Ctrl Pts',(-38.8745810387237,-87.7666978306399,
109.387416697508));
#36843=CARTESIAN_POINT('Origin',(-36.3549260746835,-87.7685555885722,114.));
#36844=CARTESIAN_POINT('',(-38.8685101472268,-87.7682702011617,110.387416697508));
#36845=CARTESIAN_POINT('',(-38.8710622858024,-87.7706792336182,110.112583302492));
#36846=CARTESIAN_POINT('',(-38.8724260746835,-87.7685555885722,114.));
#36847=CARTESIAN_POINT('Ctrl Pts',(-38.8710622858024,-87.7706792336182,
110.112583302492));
#36848=CARTESIAN_POINT('Ctrl Pts',(-38.8662628209879,-87.1817421481431,
110.07539618188));
#36849=CARTESIAN_POINT('Ctrl Pts',(-38.6597043123301,-86.5897714841231,
110.038209061269));
#36850=CARTESIAN_POINT('Ctrl Pts',(-38.2820087618755,-86.1422288485708,
110.001021940657));
#36851=CARTESIAN_POINT('Ctrl Pts',(-37.7472675806157,-85.5085981973457,
109.948372432926));
#36852=CARTESIAN_POINT('Ctrl Pts',(-36.8694842018095,-85.1644718390116,
109.895722925195));
#36853=CARTESIAN_POINT('Ctrl Pts',(-36.046588369411,-85.2658542112028,109.843073417464));
#36854=CARTESIAN_POINT('Ctrl Pts',(-35.2236925370125,-85.367236583394,109.790423909734));
#36855=CARTESIAN_POINT('Ctrl Pts',(-34.4556842510217,-85.9141276861104,
109.737774402003));
#36856=CARTESIAN_POINT('Ctrl Pts',(-34.090728394159,-86.6586027828937,109.685124894272));
#36857=CARTESIAN_POINT('Ctrl Pts',(-33.7257725372963,-87.403077879677,109.632475386541));
#36858=CARTESIAN_POINT('Ctrl Pts',(-33.7638691095618,-88.345136970527,109.57982587881));
#36859=CARTESIAN_POINT('Ctrl Pts',(-34.1877475985013,-89.0577118337345,
109.527176371079));
#36860=CARTESIAN_POINT('Ctrl Pts',(-34.6116260874407,-89.770286696942,109.474526863349));
#36861=CARTESIAN_POINT('Ctrl Pts',(-35.4212864930542,-90.2533773325069,
109.421877355618));
#36862=CARTESIAN_POINT('Ctrl Pts',(-36.2496816049095,-90.2879820675602,
109.369227847887));
#36863=CARTESIAN_POINT('Ctrl Pts',(-37.0780767167647,-90.3225868026134,
109.316578340156));
#36864=CARTESIAN_POINT('Ctrl Pts',(-37.9252065348617,-89.908705637155,109.263928832425));
#36865=CARTESIAN_POINT('Ctrl Pts',(-38.4070375928618,-89.2339650559163,
109.211279324695));
#36866=CARTESIAN_POINT('Ctrl Pts',(-38.708115487337,-88.8123453405756,109.178380650627));
#36867=CARTESIAN_POINT('Ctrl Pts',(-38.8665615835522,-88.2888724255255,
109.145481976559));
#36868=CARTESIAN_POINT('Ctrl Pts',(-38.8694869524425,-87.7670276463177,
109.112583302492));
#36869=CARTESIAN_POINT('Ctrl Pts',(-38.8745810387237,-87.7666978306399,
109.387416697508));
#36870=CARTESIAN_POINT('Ctrl Pts',(-38.8687152361884,-88.4749737903615,
109.432300020937));
#36871=CARTESIAN_POINT('Ctrl Pts',(-38.5558234383421,-89.1877901835691,
109.477183344366));
#36872=CARTESIAN_POINT('Ctrl Pts',(-38.0266616968572,-89.6563813707687,
109.522066667795));
#36873=CARTESIAN_POINT('Ctrl Pts',(-37.4059388298609,-90.2060531296368,
109.574716175526));
#36874=CARTESIAN_POINT('Ctrl Pts',(-36.4876283960155,-90.4196708645552,
109.627365683257));
#36875=CARTESIAN_POINT('Ctrl Pts',(-35.6880324559884,-90.200394213864,109.680015190987));
#36876=CARTESIAN_POINT('Ctrl Pts',(-34.8884365159614,-89.9811175631728,
109.732664698718));
#36877=CARTESIAN_POINT('Ctrl Pts',(-34.2075550697527,-89.3289465268721,
109.785314206449));
#36878=CARTESIAN_POINT('Ctrl Pts',(-33.9540553717985,-88.5395329316783,
109.83796371418));
#36879=CARTESIAN_POINT('Ctrl Pts',(-33.7005556738443,-87.7501193364846,
109.890613221911));
#36880=CARTESIAN_POINT('Ctrl Pts',(-33.8744377241447,-86.8234631823979,
109.943262729642));
#36881=CARTESIAN_POINT('Ctrl Pts',(-34.3968747370372,-86.1796499430275,
109.995912237372));
#36882=CARTESIAN_POINT('Ctrl Pts',(-34.9193117499297,-85.5358367036571,
110.048561745103));
#36883=CARTESIAN_POINT('Ctrl Pts',(-35.7903037254143,-85.1748663790032,
110.101211252834));
#36884=CARTESIAN_POINT('Ctrl Pts',(-36.6149996975598,-85.2603793776866,
110.153860760565));
#36885=CARTESIAN_POINT('Ctrl Pts',(-37.4396956697052,-85.34589237637,110.206510268296));
#36886=CARTESIAN_POINT('Ctrl Pts',(-38.2180956385115,-85.8778886983908,
110.259159776027));
#36887=CARTESIAN_POINT('Ctrl Pts',(-38.597323814547,-86.6151959005714,110.311809283757));
#36888=CARTESIAN_POINT('Ctrl Pts',(-38.7788542336475,-86.9681329813994,
110.337011755008));
#36889=CARTESIAN_POINT('Ctrl Pts',(-38.8689191194958,-87.3681146417202,
110.362214226258));
#36890=CARTESIAN_POINT('Ctrl Pts',(-38.8685101472268,-87.7682702011617,
110.387416697508));
#36891=CARTESIAN_POINT('Origin',(-36.3549260746835,-87.7685555885722,114.));
#36892=CARTESIAN_POINT('',(-38.8735728336891,-87.7706817999035,111.387416697508));
#36893=CARTESIAN_POINT('',(-38.8763919803986,-87.7679946640762,111.112583302492));
#36894=CARTESIAN_POINT('',(-38.8724260746835,-87.7685555885722,114.));
#36895=CARTESIAN_POINT('Ctrl Pts',(-38.8763919803986,-87.7679946640762,
111.112583302492));
#36896=CARTESIAN_POINT('Ctrl Pts',(-38.8764867042391,-87.7369047139068,
111.110609402663));
#36897=CARTESIAN_POINT('Ctrl Pts',(-38.875960902618,-87.7058180412501,111.108635502833));
#36898=CARTESIAN_POINT('Ctrl Pts',(-38.8748045962056,-87.6747548387019,
111.106661603004));
#36899=CARTESIAN_POINT('Ctrl Pts',(-38.8439626241377,-86.8462111109777,
111.054012095273));
#36900=CARTESIAN_POINT('Ctrl Pts',(-38.3645541874353,-86.034364962245,111.001362587542));
#36901=CARTESIAN_POINT('Ctrl Pts',(-37.6539118106195,-85.6072544985287,
110.948713079812));
#36902=CARTESIAN_POINT('Ctrl Pts',(-36.9432694338037,-85.1801440348125,
110.896063572081));
#36903=CARTESIAN_POINT('Ctrl Pts',(-36.0013931168745,-85.1377692561125,
110.84341406435));
#36904=CARTESIAN_POINT('Ctrl Pts',(-35.2552681651416,-85.499340123784,110.790764556619));
#36905=CARTESIAN_POINT('Ctrl Pts',(-34.5091432134086,-85.8609109914556,
110.738115048888));
#36906=CARTESIAN_POINT('Ctrl Pts',(-33.9587696268719,-86.6264275054988,
110.685465541158));
#36907=CARTESIAN_POINT('Ctrl Pts',(-33.8536509016289,-87.4488543957147,
110.632816033427));
#36908=CARTESIAN_POINT('Ctrl Pts',(-33.7485321763859,-88.2712812859306,
110.580166525696));
#36909=CARTESIAN_POINT('Ctrl Pts',(-34.0886683124366,-89.1506185523193,
110.527517017965));
#36910=CARTESIAN_POINT('Ctrl Pts',(-34.719863764747,-89.6882320163061,110.474867510234));
#36911=CARTESIAN_POINT('Ctrl Pts',(-35.3510592170573,-90.225845480293,110.422218002503));
#36912=CARTESIAN_POINT('Ctrl Pts',(-36.2733139856272,-90.4217351418781,
110.369568494773));
#36913=CARTESIAN_POINT('Ctrl Pts',(-37.068537895973,-90.1870974034315,110.316918987042));
#36914=CARTESIAN_POINT('Ctrl Pts',(-37.8637618063188,-89.9524596649849,
110.264269479311));
#36915=CARTESIAN_POINT('Ctrl Pts',(-38.5319548584405,-89.2872945265066,
110.21161997158));
#36916=CARTESIAN_POINT('Ctrl Pts',(-38.7702018926446,-88.4931444852094,
110.158970463849));
#36917=CARTESIAN_POINT('Ctrl Pts',(-38.8401715472838,-88.2599142823368,
110.14350807673));
#36918=CARTESIAN_POINT('Ctrl Pts',(-38.8730579009968,-88.0155589945307,
110.128045689611));
#36919=CARTESIAN_POINT('Ctrl Pts',(-38.8710622858024,-87.7706792336182,
110.112583302492));
#36920=CARTESIAN_POINT('Ctrl Pts',(-38.8685101472268,-87.7682702011617,
110.387416697508));
#36921=CARTESIAN_POINT('Ctrl Pts',(-38.8680647513497,-88.2040641409246,
110.414863733989));
#36922=CARTESIAN_POINT('Ctrl Pts',(-38.7603124245963,-88.6400643345304,
110.442310770469));
#36923=CARTESIAN_POINT('Ctrl Pts',(-38.5465340999794,-89.0157285744514,
110.46975780695));
#36924=CARTESIAN_POINT('Ctrl Pts',(-38.1364598261117,-89.7363359638104,
110.522407314681));
#36925=CARTESIAN_POINT('Ctrl Pts',(-37.3362548951114,-90.2349326601879,
110.575056822411));
#36926=CARTESIAN_POINT('Ctrl Pts',(-36.5086800437499,-90.2854874332158,
110.627706330142));
#36927=CARTESIAN_POINT('Ctrl Pts',(-35.6811051923884,-90.3360422062437,
110.680355837873));
#36928=CARTESIAN_POINT('Ctrl Pts',(-34.8261604206655,-89.9385550559221,
110.733005345604));
#36929=CARTESIAN_POINT('Ctrl Pts',(-34.3314219399208,-89.2732207374008,
110.785654853335));
#36930=CARTESIAN_POINT('Ctrl Pts',(-33.8366834591761,-88.6078864188794,
110.838304361066));
#36931=CARTESIAN_POINT('Ctrl Pts',(-33.7021512694097,-87.6747049321583,
110.890953868796));
#36932=CARTESIAN_POINT('Ctrl Pts',(-33.9888134930152,-86.8967199134953,
110.943603376527));
#36933=CARTESIAN_POINT('Ctrl Pts',(-34.2754757166207,-86.1187348948324,
110.996252884258));
#36934=CARTESIAN_POINT('Ctrl Pts',(-34.9833323535982,-85.4959463442275,
111.048902391989));
#36935=CARTESIAN_POINT('Ctrl Pts',(-35.7914873618322,-85.3106859804839,
111.10155189972));
#36936=CARTESIAN_POINT('Ctrl Pts',(-36.5996423700663,-85.1254256167402,
111.154201407451));
#36937=CARTESIAN_POINT('Ctrl Pts',(-37.5080957495568,-85.3776934398577,
111.206850915181));
#36938=CARTESIAN_POINT('Ctrl Pts',(-38.1050139753849,-85.9531276684082,
111.259500422912));
#36939=CARTESIAN_POINT('Ctrl Pts',(-38.5884344857069,-86.4191491373235,
111.302139181111));
#36940=CARTESIAN_POINT('Ctrl Pts',(-38.8675271646894,-87.0971270740966,
111.344777939309));
#36941=CARTESIAN_POINT('Ctrl Pts',(-38.8735728336891,-87.7706817999035,
111.387416697508));
#36942=CARTESIAN_POINT('Origin',(-36.3549260746835,-87.7685555885722,114.));
#36943=CARTESIAN_POINT('',(-38.8747250213613,-87.7667516914454,112.387416697508));
#36944=CARTESIAN_POINT('',(-38.869589870133,-87.7669648532936,112.112583302492));
#36945=CARTESIAN_POINT('',(-38.8724260746835,-87.7685555885722,114.));
#36946=CARTESIAN_POINT('Ctrl Pts',(-38.869589870133,-87.7669648532936,112.112583302492));
#36947=CARTESIAN_POINT('Ctrl Pts',(-38.8713916229222,-87.4591086153934,
112.093173115714));
#36948=CARTESIAN_POINT('Ctrl Pts',(-38.8190054048914,-87.1518441591964,
112.073762928937));
#36949=CARTESIAN_POINT('Ctrl Pts',(-38.7096476981112,-86.866406809236,112.054352742159));
#36950=CARTESIAN_POINT('Ctrl Pts',(-38.4130184335659,-86.0921671723103,
112.001703234428));
#36951=CARTESIAN_POINT('Ctrl Pts',(-37.6972224731726,-85.4785200738972,
111.949053726697));
#36952=CARTESIAN_POINT('Ctrl Pts',(-36.8867550306008,-85.3036530944469,
111.896404218966));
#36953=CARTESIAN_POINT('Ctrl Pts',(-36.076287588029,-85.1287861149966,111.843754711236));
#36954=CARTESIAN_POINT('Ctrl Pts',(-35.1711486632787,-85.3926992545092,
111.791105203505));
#36955=CARTESIAN_POINT('Ctrl Pts',(-34.5816692236069,-85.9757515044618,
111.738455695774));
#36956=CARTESIAN_POINT('Ctrl Pts',(-33.9921897839352,-86.5588037544144,
111.685806188043));
#36957=CARTESIAN_POINT('Ctrl Pts',(-33.7183698293421,-87.4609951148072,
111.633156680312));
#36958=CARTESIAN_POINT('Ctrl Pts',(-33.8843414723145,-88.2733308518658,
111.580507172582));
#36959=CARTESIAN_POINT('Ctrl Pts',(-34.050313115287,-89.0856665889245,111.527857664851));
#36960=CARTESIAN_POINT('Ctrl Pts',(-34.656076355825,-89.808146702649,111.47520815712));
#36961=CARTESIAN_POINT('Ctrl Pts',(-35.4270176405568,-90.113245820092,111.422558649389));
#36962=CARTESIAN_POINT('Ctrl Pts',(-36.1979589252887,-90.418344937535,111.369909141658));
#36963=CARTESIAN_POINT('Ctrl Pts',(-37.1340782542145,-90.3060630586964,
111.317259633927));
#36964=CARTESIAN_POINT('Ctrl Pts',(-37.8110001649606,-89.8273014659192,
111.264610126197));
#36965=CARTESIAN_POINT('Ctrl Pts',(-38.4625433760447,-89.3664892798312,
111.213934518295));
#36966=CARTESIAN_POINT('Ctrl Pts',(-38.8739601507151,-88.5661618765622,
111.163258910394));
#36967=CARTESIAN_POINT('Ctrl Pts',(-38.8763919803986,-87.7679946640762,
111.112583302492));
#36968=CARTESIAN_POINT('Ctrl Pts',(-38.8735728336891,-87.7706817999035,
111.387416697508));
#36969=CARTESIAN_POINT('Ctrl Pts',(-38.8749922389595,-87.9288193240984,
111.39742744704));
#36970=CARTESIAN_POINT('Ctrl Pts',(-38.8613607771502,-88.0867130325477,
111.407438196572));
#36971=CARTESIAN_POINT('Ctrl Pts',(-38.8317891158855,-88.2415626377976,
111.417448946105));
#36972=CARTESIAN_POINT('Ctrl Pts',(-38.6762629583927,-89.0559627446527,
111.470098453835));
#36973=CARTESIAN_POINT('Ctrl Pts',(-38.0798275712416,-89.7861623243795,
111.522747961566));
#36974=CARTESIAN_POINT('Ctrl Pts',(-37.3128678673142,-90.1011365015151,
111.575397469297));
#36975=CARTESIAN_POINT('Ctrl Pts',(-36.5459081633868,-90.4161106786507,
111.628046977028));
#36976=CARTESIAN_POINT('Ctrl Pts',(-35.6084241426832,-90.3158594531952,
111.680696484759));
#36977=CARTESIAN_POINT('Ctrl Pts',(-34.9254099298464,-89.8458301937081,
111.733345992489));
#36978=CARTESIAN_POINT('Ctrl Pts',(-34.2423957170096,-89.3758009342209,
111.78599550022));
#36979=CARTESIAN_POINT('Ctrl Pts',(-33.8138513120396,-88.5359936407022,
111.838645007951));
#36980=CARTESIAN_POINT('Ctrl Pts',(-33.8340508041346,-87.7071221788761,
111.891294515682));
#36981=CARTESIAN_POINT('Ctrl Pts',(-33.8542502962297,-86.8782507170499,
111.943944023413));
#36982=CARTESIAN_POINT('Ctrl Pts',(-34.3231936853898,-86.0603150869163,
111.996593531144));
#36983=CARTESIAN_POINT('Ctrl Pts',(-35.0282926172737,-85.6241139682027,
112.049243038875));
#36984=CARTESIAN_POINT('Ctrl Pts',(-35.7333915491576,-85.1879128494891,
112.101892546605));
#36985=CARTESIAN_POINT('Ctrl Pts',(-36.6746460237652,-85.1334462421954,
112.154542054336));
#36986=CARTESIAN_POINT('Ctrl Pts',(-37.4253526385136,-85.4854057544748,
112.207191562067));
#36987=CARTESIAN_POINT('Ctrl Pts',(-38.1760592532619,-85.8373652667541,
112.259841069798));
#36988=CARTESIAN_POINT('Ctrl Pts',(-38.736218008151,-86.5957508986065,112.312490577529));
#36989=CARTESIAN_POINT('Ctrl Pts',(-38.851889449881,-87.4167600564597,112.365140085259));
#36990=CARTESIAN_POINT('Ctrl Pts',(-38.8682034223296,-87.5325528621941,
112.372565622676));
#36991=CARTESIAN_POINT('Ctrl Pts',(-38.8756758831734,-87.649591342699,112.379991160092));
#36992=CARTESIAN_POINT('Ctrl Pts',(-38.8747250213613,-87.7667516914454,
112.387416697508));
#36993=CARTESIAN_POINT('Origin',(-36.3549260746835,-87.7685555885722,114.));
#36994=CARTESIAN_POINT('',(-38.8685313431306,-87.768184262399,113.387416697508));
#36995=CARTESIAN_POINT('',(-38.8709180488009,-87.7706492052449,113.112583302492));
#36996=CARTESIAN_POINT('',(-38.8724260746835,-87.7685555885722,114.));
#36997=CARTESIAN_POINT('Ctrl Pts',(-38.8709180488009,-87.7706492052449,
113.112583302492));
#36998=CARTESIAN_POINT('Ctrl Pts',(-38.8662499617323,-87.1870221755863,
113.075736828766));
#36999=CARTESIAN_POINT('Ctrl Pts',(-38.6637923444195,-86.6004729887904,
113.03889035504));
#37000=CARTESIAN_POINT('Ctrl Pts',(-38.2924116771201,-86.1546361716722,
113.002043881314));
#37001=CARTESIAN_POINT('Ctrl Pts',(-37.7617500605046,-85.5175850084034,
112.949394373583));
#37002=CARTESIAN_POINT('Ctrl Pts',(-36.8861944104941,-85.1678294908771,
112.896744865852));
#37003=CARTESIAN_POINT('Ctrl Pts',(-36.0626645666103,-85.2639259642975,
112.844095358121));
#37004=CARTESIAN_POINT('Ctrl Pts',(-35.2391347227264,-85.3600224377178,
112.791445850391));
#37005=CARTESIAN_POINT('Ctrl Pts',(-34.4676306849692,-85.9019709020846,
112.73879634266));
#37006=CARTESIAN_POINT('Ctrl Pts',(-34.0979020767385,-86.644087262386,112.686146834929));
#37007=CARTESIAN_POINT('Ctrl Pts',(-33.7281734685077,-87.3862036226874,
112.633497327198));
#37008=CARTESIAN_POINT('Ctrl Pts',(-33.7602202898036,-88.3284878789233,
112.580847819467));
#37009=CARTESIAN_POINT('Ctrl Pts',(-34.1795146015215,-89.0437697926693,
112.528198311736));
#37010=CARTESIAN_POINT('Ctrl Pts',(-34.5988089132394,-89.7590517064154,
112.475548804006));
#37011=CARTESIAN_POINT('Ctrl Pts',(-35.4053507153794,-90.2473312776716,
112.422899296275));
#37012=CARTESIAN_POINT('Ctrl Pts',(-36.2335065468714,-90.2872543879847,
112.370249788544));
#37013=CARTESIAN_POINT('Ctrl Pts',(-37.0616623783633,-90.3271774982979,
112.317600280813));
#37014=CARTESIAN_POINT('Ctrl Pts',(-37.9114322392072,-89.918744147668,112.264950773082));
#37015=CARTESIAN_POINT('Ctrl Pts',(-38.3975858852805,-89.2471113846339,
112.212301265351));
#37016=CARTESIAN_POINT('Ctrl Pts',(-38.7045102568622,-88.8230881043542,
112.179061944398));
#37017=CARTESIAN_POINT('Ctrl Pts',(-38.8665044263955,-88.294158765243,112.145822623445));
#37018=CARTESIAN_POINT('Ctrl Pts',(-38.869589870133,-87.7669648532936,112.112583302492));
#37019=CARTESIAN_POINT('Ctrl Pts',(-38.8747250213613,-87.7667516914454,
112.387416697508));
#37020=CARTESIAN_POINT('Ctrl Pts',(-38.8689339595225,-88.4802968312487,
112.432640667823));
#37021=CARTESIAN_POINT('Ctrl Pts',(-38.5507040482079,-89.1983623218322,
112.477864638137));
#37022=CARTESIAN_POINT('Ctrl Pts',(-38.0145055106651,-89.6670766680336,
112.523088608452));
#37023=CARTESIAN_POINT('Ctrl Pts',(-37.3902660011481,-90.2127514379001,
112.575738116183));
#37024=CARTESIAN_POINT('Ctrl Pts',(-36.4706028535431,-90.4204682937787,
112.628387623914));
#37025=CARTESIAN_POINT('Ctrl Pts',(-35.6724313706716,-90.1960619577684,
112.681037131644));
#37026=CARTESIAN_POINT('Ctrl Pts',(-34.8742598878001,-89.971655621758,112.733686639375));
#37027=CARTESIAN_POINT('Ctrl Pts',(-34.1975800696622,-89.3151260938587,
112.786336147106));
#37028=CARTESIAN_POINT('Ctrl Pts',(-33.9491544216676,-88.5241010518219,
112.838985654837));
#37029=CARTESIAN_POINT('Ctrl Pts',(-33.7007287736729,-87.7330760097852,
112.891635162568));
#37030=CARTESIAN_POINT('Ctrl Pts',(-33.8805572958214,-86.8075554536111,
112.944284670298));
#37031=CARTESIAN_POINT('Ctrl Pts',(-34.4071174622157,-86.1671100532235,
112.996934178029));
#37032=CARTESIAN_POINT('Ctrl Pts',(-34.9336776286101,-85.5266646528359,
113.04958368576));
#37033=CARTESIAN_POINT('Ctrl Pts',(-35.8069694392502,-85.1712944082348,
113.102233193491));
#37034=CARTESIAN_POINT('Ctrl Pts',(-36.6310993317674,-85.2621010157615,
113.154882701222));
#37035=CARTESIAN_POINT('Ctrl Pts',(-37.4552292242845,-85.3529076232882,
113.207532208953));
#37036=CARTESIAN_POINT('Ctrl Pts',(-38.2301971986787,-85.8898910829425,
113.260181716683));
#37037=CARTESIAN_POINT('Ctrl Pts',(-38.604683308551,-86.6296181090971,113.312831224414));
#37038=CARTESIAN_POINT('Ctrl Pts',(-38.7815208193256,-86.9789274226054,
113.337693048779));
#37039=CARTESIAN_POINT('Ctrl Pts',(-38.8690565301526,-87.3734456881792,
113.362554873143));
#37040=CARTESIAN_POINT('Ctrl Pts',(-38.8685313431306,-87.768184262399,113.387416697508));
#37041=CARTESIAN_POINT('Origin',(-36.3549260746835,-87.7685555885722,114.));
#37042=CARTESIAN_POINT('',(-38.8734137783908,-87.7707089500124,114.387416697508));
#37043=CARTESIAN_POINT('',(-38.8764405008163,-87.7680895936699,114.112583302492));
#37044=CARTESIAN_POINT('',(-38.8724260746835,-87.7685555885722,114.));
#37045=CARTESIAN_POINT('Ctrl Pts',(-38.8764405008163,-87.7680895936699,
114.112583302492));
#37046=CARTESIAN_POINT('Ctrl Pts',(-38.8765065883869,-87.7423663370125,
114.110950049548));
#37047=CARTESIAN_POINT('Ctrl Pts',(-38.8761466448638,-87.7166449745044,
114.109316796605));
#37048=CARTESIAN_POINT('Ctrl Pts',(-38.8753549438192,-87.6909369083243,
114.107683543661));
#37049=CARTESIAN_POINT('Ctrl Pts',(-38.8498336855031,-86.8622122246415,
114.05503403593));
#37050=CARTESIAN_POINT('Ctrl Pts',(-38.3756479945492,-86.0473045312185,
114.002384528199));
#37051=CARTESIAN_POINT('Ctrl Pts',(-37.6677627430985,-85.6156398387202,
113.949735020469));
#37052=CARTESIAN_POINT('Ctrl Pts',(-36.9598774916477,-85.1839751462218,
113.897085512738));
#37053=CARTESIAN_POINT('Ctrl Pts',(-36.0182926797001,-85.1355534546481,
113.844436005007));
#37054=CARTESIAN_POINT('Ctrl Pts',(-35.2698614632483,-85.4923260015343,
113.791786497276));
#37055=CARTESIAN_POINT('Ctrl Pts',(-34.5214302467965,-85.8490985484205,
113.739136989545));
#37056=CARTESIAN_POINT('Ctrl Pts',(-33.9661526258405,-86.6110653337667,
113.686487481815));
#37057=CARTESIAN_POINT('Ctrl Pts',(-33.855755265838,-87.4328003025223,113.633837974084));
#37058=CARTESIAN_POINT('Ctrl Pts',(-33.7453579058355,-88.2545352712778,
113.581188466353));
#37059=CARTESIAN_POINT('Ctrl Pts',(-34.0798408067865,-89.1360384234427,
113.528538958622));
#37060=CARTESIAN_POINT('Ctrl Pts',(-34.7075712319637,-89.6776937098362,
113.475889450891));
#37061=CARTESIAN_POINT('Ctrl Pts',(-35.3353016571408,-90.2193489962298,
113.42323994316));
#37062=CARTESIAN_POINT('Ctrl Pts',(-36.2562796065442,-90.421156416852,113.37059043543));
#37063=CARTESIAN_POINT('Ctrl Pts',(-37.0529937319507,-90.1916296464115,
113.317940927699));
#37064=CARTESIAN_POINT('Ctrl Pts',(-37.8497078573572,-89.9621028759709,
113.265291419968));
#37065=CARTESIAN_POINT('Ctrl Pts',(-38.522158158767,-89.3012419144675,113.212641912237));
#37066=CARTESIAN_POINT('Ctrl Pts',(-38.7654995178616,-88.50863802921,113.159992404506));
#37067=CARTESIAN_POINT('Ctrl Pts',(-38.8385397406153,-88.2707336937116,
113.144189370502));
#37068=CARTESIAN_POINT('Ctrl Pts',(-38.8729201383152,-88.0209602082557,
113.128386336497));
#37069=CARTESIAN_POINT('Ctrl Pts',(-38.8709180488009,-87.7706492052449,
113.112583302492));
#37070=CARTESIAN_POINT('Ctrl Pts',(-38.8685313431306,-87.768184262399,113.387416697508));
#37071=CARTESIAN_POINT('Ctrl Pts',(-38.8679443495754,-88.2093775695351,
113.415204380874));
#37072=CARTESIAN_POINT('Ctrl Pts',(-38.757349980407,-88.6508460904898,113.442992064241));
#37073=CARTESIAN_POINT('Ctrl Pts',(-38.5384808246602,-89.0297751758553,
113.470779747607));
#37074=CARTESIAN_POINT('Ctrl Pts',(-38.1237879855467,-89.747734623804,113.523429255338));
#37075=CARTESIAN_POINT('Ctrl Pts',(-37.3203980619691,-90.2411829270465,
113.576078763068));
#37076=CARTESIAN_POINT('Ctrl Pts',(-36.4925156587813,-90.2864228010837,
113.628728270799));
#37077=CARTESIAN_POINT('Ctrl Pts',(-35.6646332555936,-90.3316626751209,
113.68137777853));
#37078=CARTESIAN_POINT('Ctrl Pts',(-34.8122583727957,-89.9286941199529,
113.734027286261));
#37079=CARTESIAN_POINT('Ctrl Pts',(-34.321802201599,-89.2601968021977,113.786676793992));
#37080=CARTESIAN_POINT('Ctrl Pts',(-33.8313460304022,-88.5916994844425,
113.839326301723));
#37081=CARTESIAN_POINT('Ctrl Pts',(-33.7028085708067,-87.6576734041001,
113.891975809453));
#37082=CARTESIAN_POINT('Ctrl Pts',(-33.9944603254749,-86.8815450811342,
113.944625317184));
#37083=CARTESIAN_POINT('Ctrl Pts',(-34.2861120801431,-86.1054167581684,
113.997274824915));
#37084=CARTESIAN_POINT('Ctrl Pts',(-34.9979530490751,-85.4871861925791,
114.049924332646));
#37085=CARTESIAN_POINT('Ctrl Pts',(-35.8072809538378,-85.3071188099598,
114.102573840377));
#37086=CARTESIAN_POINT('Ctrl Pts',(-36.6166088586004,-85.1270514273405,
114.155223348107));
#37087=CARTESIAN_POINT('Ctrl Pts',(-37.5234236991937,-85.3851472276913,
114.207872855838));
#37088=CARTESIAN_POINT('Ctrl Pts',(-38.116634757398,-85.9644024047377,114.260522363569));
#37089=CARTESIAN_POINT('Ctrl Pts',(-38.5932148519415,-86.4297704777422,
114.302820474882));
#37090=CARTESIAN_POINT('Ctrl Pts',(-38.8673837119047,-87.1024264394285,
114.345118586195));
#37091=CARTESIAN_POINT('Ctrl Pts',(-38.8734137783908,-87.7707089500124,
114.387416697508));
#37092=CARTESIAN_POINT('Origin',(-36.3549260746835,-87.7685555885722,114.));
#37093=CARTESIAN_POINT('',(-38.8748658262276,-87.7668088525845,115.387416697508));
#37094=CARTESIAN_POINT('',(-38.8696970919136,-87.7669042806264,115.112583302492));
#37095=CARTESIAN_POINT('',(-38.8724260746835,-87.7685555885722,114.));
#37096=CARTESIAN_POINT('Ctrl Pts',(-38.8696970919136,-87.7669042806264,
115.112583302492));
#37097=CARTESIAN_POINT('Ctrl Pts',(-38.871539656816,-87.4644833190019,115.0935137626));
#37098=CARTESIAN_POINT('Ctrl Pts',(-38.8210274992386,-87.1626571043369,
115.074444222708));
#37099=CARTESIAN_POINT('Ctrl Pts',(-38.7153918518087,-86.8815450706432,
115.055374682816));
#37100=CARTESIAN_POINT('Ctrl Pts',(-38.423740093691,-86.1054167384983,115.002725175085));
#37101=CARTESIAN_POINT('Ctrl Pts',(-37.7118991163401,-85.4871861655974,
114.950075667354));
#37102=CARTESIAN_POINT('Ctrl Pts',(-36.9025712020056,-85.3071187808487,
114.897426159623));
#37103=CARTESIAN_POINT('Ctrl Pts',(-36.0932432876712,-85.1270513961,114.844776651893));
#37104=CARTESIAN_POINT('Ctrl Pts',(-35.1864284363532,-85.3851471995034,
114.792127144162));
#37105=CARTESIAN_POINT('Ctrl Pts',(-34.5932173711332,-85.9644023834006,
114.739477636431));
#37106=CARTESIAN_POINT('Ctrl Pts',(-34.0000063059132,-86.5436575672978,
114.6868281287));
#37107=CARTESIAN_POINT('Ctrl Pts',(-33.7203990267912,-87.4440721316887,
114.634178620969));
#37108=CARTESIAN_POINT('Ctrl Pts',(-33.8811512418217,-88.2574568262423,
114.581529113239));
#37109=CARTESIAN_POINT('Ctrl Pts',(-34.0419034568521,-89.0708415207959,
114.528879605508));
#37110=CARTESIAN_POINT('Ctrl Pts',(-34.643015166035,-89.797196345512,114.476230097777));
#37111=CARTESIAN_POINT('Ctrl Pts',(-35.4119815170054,-90.1072393861475,
114.423580590046));
#37112=CARTESIAN_POINT('Ctrl Pts',(-36.1809478679757,-90.417282426783,114.370931082315));
#37113=CARTESIAN_POINT('Ctrl Pts',(-37.1177688607336,-90.3110136833377,
114.318281574584));
#37114=CARTESIAN_POINT('Ctrl Pts',(-37.7977509442735,-89.8366084746437,
114.265632066854));
#37115=CARTESIAN_POINT('Ctrl Pts',(-38.4566391413284,-89.3769199031411,
114.214615812066));
#37116=CARTESIAN_POINT('Ctrl Pts',(-38.8743761908434,-88.5715807006019,
114.163599557279));
#37117=CARTESIAN_POINT('Ctrl Pts',(-38.8764405008163,-87.7680895936699,
114.112583302492));
#37118=CARTESIAN_POINT('Ctrl Pts',(-38.8734137783908,-87.7707089500124,
114.387416697508));
#37119=CARTESIAN_POINT('Ctrl Pts',(-38.8748894851466,-87.9342542472236,
114.397768093926));
#37120=CARTESIAN_POINT('Ctrl Pts',(-38.8603062997799,-88.0975376174732,
114.408119490344));
#37121=CARTESIAN_POINT('Ctrl Pts',(-38.8287008782886,-88.2574568204596,
114.418470886762));
#37122=CARTESIAN_POINT('Ctrl Pts',(-38.6679486651595,-89.0708415053934,
114.471120394492));
#37123=CARTESIAN_POINT('Ctrl Pts',(-38.066836963086,-89.7971963215193,114.523769902223));
#37124=CARTESIAN_POINT('Ctrl Pts',(-37.2978706212101,-90.1072393584882,
114.576419409954));
#37125=CARTESIAN_POINT('Ctrl Pts',(-36.5289042793342,-90.417282395457,114.629068917685));
#37126=CARTESIAN_POINT('Ctrl Pts',(-35.5920832976559,-90.3110136532687,
114.681718425416));
#37127=CARTESIAN_POINT('Ctrl Pts',(-34.912101222158,-89.8366084501855,114.734367933147));
#37128=CARTESIAN_POINT('Ctrl Pts',(-34.2321191466601,-89.3622032471024,
114.787017440877));
#37129=CARTESIAN_POINT('Ctrl Pts',(-33.8089759773425,-88.5196615831244,
114.839666948608));
#37130=CARTESIAN_POINT('Ctrl Pts',(-33.8344972353565,-87.6909369092428,
114.892316456339));
#37131=CARTESIAN_POINT('Ctrl Pts',(-33.8600184933705,-86.8622122353612,
114.94496596407));
#37132=CARTESIAN_POINT('Ctrl Pts',(-34.3342041787161,-86.0473045515759,
114.997615471801));
#37133=CARTESIAN_POINT('Ctrl Pts',(-35.0420894217948,-85.6156398641826,
115.050264979531));
#37134=CARTESIAN_POINT('Ctrl Pts',(-35.7499746648734,-85.1839751767894,
115.102914487262));
#37135=CARTESIAN_POINT('Ctrl Pts',(-36.6915594656851,-85.1355534857881,
115.155563994993));
#37136=CARTESIAN_POINT('Ctrl Pts',(-37.4399906732854,-85.4923260284547,
115.208213502724));
#37137=CARTESIAN_POINT('Ctrl Pts',(-38.1884218808857,-85.8490985711212,
115.260863010455));
#37138=CARTESIAN_POINT('Ctrl Pts',(-38.7436994952747,-86.6110653474556,
115.313512518185));
#37139=CARTESIAN_POINT('Ctrl Pts',(-38.8540968539717,-87.4328003064926,
115.366162025916));
#37140=CARTESIAN_POINT('Ctrl Pts',(-38.868952704196,-87.5433787806482,115.373246916447));
#37141=CARTESIAN_POINT('Ctrl Pts',(-38.8757525296954,-87.6550395549316,
115.380331806977));
#37142=CARTESIAN_POINT('Ctrl Pts',(-38.8748658262276,-87.7668088525845,
115.387416697508));
#37143=CARTESIAN_POINT('Origin',(-36.3549260746835,-87.7685555885722,114.));
#37144=CARTESIAN_POINT('',(-38.868558082292,-87.7680988643522,116.387416697508));
#37145=CARTESIAN_POINT('',(-38.8707765205166,-87.7706159292182,116.112583302492));
#37146=CARTESIAN_POINT('',(-38.8724260746835,-87.7685555885722,114.));
#37147=CARTESIAN_POINT('Ctrl Pts',(-38.8707765205166,-87.7706159292182,
116.112583302492));
#37148=CARTESIAN_POINT('Ctrl Pts',(-38.8662439615746,-87.1923021573119,
116.076077475652));
#37149=CARTESIAN_POINT('Ctrl Pts',(-38.6678381140232,-86.6111785578358,
116.039571648811));
#37150=CARTESIAN_POINT('Ctrl Pts',(-38.3027347101873,-86.167110034283,116.003065821971));
#37151=CARTESIAN_POINT('Ctrl Pts',(-37.7761745375653,-85.5266646263211,
115.95041631424));
#37152=CARTESIAN_POINT('Ctrl Pts',(-36.9028827165968,-85.1712943775174,
115.897766806509));
#37153=CARTESIAN_POINT('Ctrl Pts',(-36.0787528143328,-85.2621009861182,
115.845117298778));
#37154=CARTESIAN_POINT('Ctrl Pts',(-35.2546229120689,-85.352907594719,115.792467791047));
#37155=CARTESIAN_POINT('Ctrl Pts',(-34.4796549285094,-85.8898910607243,
115.739818283317));
#37156=CARTESIAN_POINT('Ctrl Pts',(-34.1051688142083,-86.6296180956276,
115.687168775586));
#37157=CARTESIAN_POINT('Ctrl Pts',(-33.7306826999072,-87.3693451305309,
115.634519267855));
#37158=CARTESIAN_POINT('Ctrl Pts',(-33.7566784548643,-88.3118157343321,
115.581869760124));
#37159=CARTESIAN_POINT('Ctrl Pts',(-34.1713712988825,-89.0297751907719,
115.529220252393));
#37160=CARTESIAN_POINT('Ctrl Pts',(-34.5860641429007,-89.7477346472117,
115.476570744662));
#37161=CARTESIAN_POINT('Ctrl Pts',(-35.38945407598,-90.2411829562899,115.423921236932));
#37162=CARTESIAN_POINT('Ctrl Pts',(-36.217336488959,-90.2864228308621,115.371271729201));
#37163=CARTESIAN_POINT('Ctrl Pts',(-37.045218901938,-90.3316627054341,115.31862222147));
#37164=CARTESIAN_POINT('Ctrl Pts',(-37.8975937948167,-89.9286941455001,
115.265972713739));
#37165=CARTESIAN_POINT('Ctrl Pts',(-38.3880499718138,-89.2601968198386,
115.213323206008));
#37166=CARTESIAN_POINT('Ctrl Pts',(-38.7008639630498,-88.8338278058908,
115.17974323817));
#37167=CARTESIAN_POINT('Ctrl Pts',(-38.8664524792742,-88.2994439340536,
115.146163270331));
#37168=CARTESIAN_POINT('Ctrl Pts',(-38.8696970919136,-87.7669042806264,
115.112583302492));
#37169=CARTESIAN_POINT('Ctrl Pts',(-38.8748658262276,-87.7668088525845,
115.387416697508));
#37170=CARTESIAN_POINT('Ctrl Pts',(-38.8691632251914,-88.4856238067917,
115.432981314708));
#37171=CARTESIAN_POINT('Ctrl Pts',(-38.5455394661889,-89.2089273767851,
115.478545931909));
#37172=CARTESIAN_POINT('Ctrl Pts',(-38.0022808979207,-89.6776936872569,
115.524110549109));
#37173=CARTESIAN_POINT('Ctrl Pts',(-37.3745504801678,-90.2193489672445,
115.57676005684));
#37174=CARTESIAN_POINT('Ctrl Pts',(-36.4535725416567,-90.4211563854802,
115.62940956457));
#37175=CARTESIAN_POINT('Ctrl Pts',(-35.6568584256728,-90.1916296177544,
115.682059072301));
#37176=CARTESIAN_POINT('Ctrl Pts',(-34.8601443096888,-89.9621028500285,
115.734708580032));
#37177=CARTESIAN_POINT('Ctrl Pts',(-34.1876940162318,-89.3012418963412,
115.787358087763));
#37178=CARTESIAN_POINT('Ctrl Pts',(-33.944352660015,-88.5086380204578,115.840007595494));
#37179=CARTESIAN_POINT('Ctrl Pts',(-33.7010113037982,-87.7160341445744,
115.892657103225));
#37180=CARTESIAN_POINT('Ctrl Pts',(-33.8867788848215,-86.7916873464949,
115.945306610955));
#37181=CARTESIAN_POINT('Ctrl Pts',(-34.4174404951608,-86.1546361907602,
115.997956118686));
#37182=CARTESIAN_POINT('Ctrl Pts',(-34.9481021055002,-85.5175850350255,
116.050605626417));
#37183=CARTESIAN_POINT('Ctrl Pts',(-35.8236577451555,-85.1678295216356,
116.103255134148));
#37184=CARTESIAN_POINT('Ctrl Pts',(-36.6471875792997,-85.2639259939193,
116.155904641879));
#37185=CARTESIAN_POINT('Ctrl Pts',(-37.4707174134438,-85.3600224662028,
116.208554149609));
#37186=CARTESIAN_POINT('Ctrl Pts',(-38.2422214420767,-85.90197092416,116.26120365734));
#37187=CARTESIAN_POINT('Ctrl Pts',(-38.6119500459349,-86.6440872756844,
116.313853165071));
#37188=CARTESIAN_POINT('Ctrl Pts',(-38.7841488205295,-86.9897233043973,
116.33837434255));
#37189=CARTESIAN_POINT('Ctrl Pts',(-38.8691955906087,-87.3787791942771,
116.362895520029));
#37190=CARTESIAN_POINT('Ctrl Pts',(-38.868558082292,-87.7680988643522,116.387416697508));
#37191=CARTESIAN_POINT('Origin',(-36.3549260746835,-87.7685555885722,114.));
#37192=CARTESIAN_POINT('',(-38.8732538877992,-87.7707324389422,117.387416697508));
#37193=CARTESIAN_POINT('',(-38.8764805590541,-87.7681855672363,117.112583302492));
#37194=CARTESIAN_POINT('',(-38.8724260746835,-87.7685555885722,114.));
#37195=CARTESIAN_POINT('Ctrl Pts',(-38.8764805590541,-87.7681855672363,
117.112583302492));
#37196=CARTESIAN_POINT('Ctrl Pts',(-38.8765227322016,-87.7478282685136,
117.111290696434));
#37197=CARTESIAN_POINT('Ctrl Pts',(-38.8762972958495,-87.7274719274955,
117.109998090376));
#37198=CARTESIAN_POINT('Ctrl Pts',(-38.8758013750463,-87.707122178149,117.108705484318));
#37199=CARTESIAN_POINT('Ctrl Pts',(-38.8556018827122,-86.8782507065199,
117.056055976587));
#37200=CARTESIAN_POINT('Ctrl Pts',(-38.3866584880058,-86.0603150667128,
117.003406468856));
#37201=CARTESIAN_POINT('Ctrl Pts',(-37.6815595477827,-85.6241139428405,
116.950756961126));
#37202=CARTESIAN_POINT('Ctrl Pts',(-36.9764606075597,-85.1879128189682,
116.898107453395));
#37203=CARTESIAN_POINT('Ctrl Pts',(-36.0352061218199,-85.1334462110306,
116.845457945664));
#37204=CARTESIAN_POINT('Ctrl Pts',(-35.2844994981932,-85.4854057274726,
116.792808437933));
#37205=CARTESIAN_POINT('Ctrl Pts',(-34.5337928745664,-85.8373652439147,
116.740158930202));
#37206=CARTESIAN_POINT('Ctrl Pts',(-33.9736341130527,-86.5957508847365,
116.687509422471));
#37207=CARTESIAN_POINT('Ctrl Pts',(-33.8579626699548,-87.4167600522997,
116.634859914741));
#37208=CARTESIAN_POINT('Ctrl Pts',(-33.7422912268569,-88.2377692198629,
116.58221040701));
#37209=CARTESIAN_POINT('Ctrl Pts',(-34.0711071021749,-89.1214019141675,
116.529560899279));
#37210=CARTESIAN_POINT('Ctrl Pts',(-34.6953466190748,-89.6670766904874,
116.476911391548));
#37211=CARTESIAN_POINT('Ctrl Pts',(-35.3195861359746,-90.2127514668073,
116.424261883817));
#37212=CARTESIAN_POINT('Ctrl Pts',(-36.2392492944564,-90.4204683251425,
116.371612376086));
#37213=CARTESIAN_POINT('Ctrl Pts',(-37.0374207867677,-90.1960619864779,
116.318962868356));
#37214=CARTESIAN_POINT('Ctrl Pts',(-37.8355922790789,-89.9716556478134,
116.266313360625));
#37215=CARTESIAN_POINT('Ctrl Pts',(-38.5122721052197,-89.3151261121492,
116.213663852894));
#37216=CARTESIAN_POINT('Ctrl Pts',(-38.7606977561522,-88.5241010607571,
116.161014345163));
#37217=CARTESIAN_POINT('Ctrl Pts',(-38.8368713920796,-88.2815526200145,
116.144870664273));
#37218=CARTESIAN_POINT('Ctrl Pts',(-38.8727809179377,-88.0263590200123,
116.128726983382));
#37219=CARTESIAN_POINT('Ctrl Pts',(-38.8707765205166,-87.7706159292182,
116.112583302492));
#37220=CARTESIAN_POINT('Ctrl Pts',(-38.868558082292,-87.7680988643522,116.387416697508));
#37221=CARTESIAN_POINT('Ctrl Pts',(-38.8678267942253,-88.2146888481658,
116.41554502776));
#37222=CARTESIAN_POINT('Ctrl Pts',(-38.7543481395299,-88.6616259262534,
116.443673358012));
#37223=CARTESIAN_POINT('Ctrl Pts',(-38.5303375221176,-89.0437697775872,
116.471801688264));
#37224=CARTESIAN_POINT('Ctrl Pts',(-38.1110432153587,-89.7590516828738,
116.524451195994));
#37225=CARTESIAN_POINT('Ctrl Pts',(-37.3045014227577,-90.2473312483554,
116.577100703725));
#37226=CARTESIAN_POINT('Ctrl Pts',(-36.4763456010602,-90.2872543581965,
116.629750211456));
#37227=CARTESIAN_POINT('Ctrl Pts',(-35.6481897793627,-90.3271774680377,
116.682399719187));
#37228=CARTESIAN_POINT('Ctrl Pts',(-34.7984199285688,-89.9187441222385,
116.735049226918));
#37229=CARTESIAN_POINT('Ctrl Pts',(-34.312266288245,-89.2471113671478,116.787698734649));
#37230=CARTESIAN_POINT('Ctrl Pts',(-33.8261126479212,-88.5754786120571,
116.840348242379));
#37231=CARTESIAN_POINT('Ctrl Pts',(-33.7035752180675,-87.640646447675,116.89299775011));
#37232=CARTESIAN_POINT('Ctrl Pts',(-34.0002044791045,-86.8664068199061,
116.945647257841));
#37233=CARTESIAN_POINT('Ctrl Pts',(-34.2968337401414,-86.0921671921372,
116.998296765572));
#37234=CARTESIAN_POINT('Ctrl Pts',(-35.012629692069,-85.4785201009814,117.050946273303));
#37235=CARTESIAN_POINT('Ctrl Pts',(-35.8230971250555,-85.303653123599,117.103595781034));
#37236=CARTESIAN_POINT('Ctrl Pts',(-36.633564558042,-85.1287861462166,117.156245288764));
#37237=CARTESIAN_POINT('Ctrl Pts',(-37.5387034720875,-85.3926992826077,
117.208894796495));
#37238=CARTESIAN_POINT('Ctrl Pts',(-38.1281829047877,-85.9757515256646,
117.261544304226));
#37239=CARTESIAN_POINT('Ctrl Pts',(-38.5979510639627,-86.4403977265829,
117.303501768653));
#37240=CARTESIAN_POINT('Ctrl Pts',(-38.8672495515809,-87.1077234466512,
117.345459233081));
#37241=CARTESIAN_POINT('Ctrl Pts',(-38.8732538877992,-87.7707324389422,
117.387416697508));
#37242=CARTESIAN_POINT('Origin',(-36.3549260746835,-87.7685555885722,114.));
#37243=CARTESIAN_POINT('',(-38.8750031561041,-87.7668692329086,118.387416697508));
#37244=CARTESIAN_POINT('',(-38.8698085201626,-87.7668461825819,118.112583302492));
#37245=CARTESIAN_POINT('',(-38.8724260746835,-87.7685555885722,114.));
#37246=CARTESIAN_POINT('Ctrl Pts',(-38.8698085201626,-87.7668461825819,
118.112583302492));
#37247=CARTESIAN_POINT('Ctrl Pts',(-38.8716872313444,-87.4698606038117,
118.093854409486));
#37248=CARTESIAN_POINT('Ctrl Pts',(-38.8230124046943,-87.1734707974551,
118.075125516479));
#37249=CARTESIAN_POINT('Ctrl Pts',(-38.7210386843352,-86.8967199031838,
118.056396623473));
#37250=CARTESIAN_POINT('Ctrl Pts',(-38.4343764573392,-86.1187348753197,
118.003747115742));
#37251=CARTESIAN_POINT('Ctrl Pts',(-37.7265198119899,-85.4959463173494,
117.951097608011));
#37252=CARTESIAN_POINT('Ctrl Pts',(-36.9183647941979,-85.3106859514149,
117.89844810028));
#37253=CARTESIAN_POINT('Ctrl Pts',(-36.110209776406,-85.1254255854804,117.845798592549));
#37254=CARTESIAN_POINT('Ctrl Pts',(-35.2017563861714,-85.3776934115817,
117.793149084819));
#37255=CARTESIAN_POINT('Ctrl Pts',(-34.6048381532838,-85.9531276469379,
117.740499577088));
#37256=CARTESIAN_POINT('Ctrl Pts',(-34.0079199203962,-86.5285618822942,
117.687850069357));
#37257=CARTESIAN_POINT('Ctrl Pts',(-33.7225368448558,-87.4271625269054,
117.635200561626));
#37258=CARTESIAN_POINT('Ctrl Pts',(-33.8780630041881,-88.2415626433923,
117.582551053895));
#37259=CARTESIAN_POINT('Ctrl Pts',(-34.0335891635205,-89.0559627598792,
117.529901546165));
#37260=CARTESIAN_POINT('Ctrl Pts',(-34.6300245577258,-89.7861623482417,
117.477252038434));
#37261=CARTESIAN_POINT('Ctrl Pts',(-35.3969842707239,-90.1011365291023,
117.424602530703));
#37262=CARTESIAN_POINT('Ctrl Pts',(-36.163943983722,-90.4161107099629,117.371953022972));
#37263=CARTESIAN_POINT('Ctrl Pts',(-37.1014280155131,-90.3158594833215,
117.319303515241));
#37264=CARTESIAN_POINT('Ctrl Pts',(-37.7844422364276,-89.8458302182753,
117.26665400751));
#37265=CARTESIAN_POINT('Ctrl Pts',(-38.4506876715034,-89.3873407130792,
117.215297105838));
#37266=CARTESIAN_POINT('Ctrl Pts',(-38.874804965645,-88.5770072359445,117.163940204165));
#37267=CARTESIAN_POINT('Ctrl Pts',(-38.8764805590541,-87.7681855672363,
117.112583302492));
#37268=CARTESIAN_POINT('Ctrl Pts',(-38.8732538877992,-87.7707324389422,
117.387416697508));
#37269=CARTESIAN_POINT('Ctrl Pts',(-38.8747839760381,-87.9396873782579,
117.398108740812));
#37270=CARTESIAN_POINT('Ctrl Pts',(-38.8592161096564,-88.1083619952982,
117.408800784115));
#37271=CARTESIAN_POINT('Ctrl Pts',(-38.8255106478334,-88.2733308458954,
117.419492827418));
#37272=CARTESIAN_POINT('Ctrl Pts',(-38.6595390068241,-89.0856665733467,
117.472142335149));
#37273=CARTESIAN_POINT('Ctrl Pts',(-38.0537757734505,-89.8081466785269,
117.52479184288));
#37274=CARTESIAN_POINT('Ctrl Pts',(-37.2828344978364,-90.1132457923617,
117.577441350611));
#37275=CARTESIAN_POINT('Ctrl Pts',(-36.5118932222224,-90.4183449061965,
117.630090858342));
#37276=CARTESIAN_POINT('Ctrl Pts',(-35.5757739043679,-90.3060630286859,
117.682740366073));
#37277=CARTESIAN_POINT('Ctrl Pts',(-34.8988520016275,-89.8273014415711,
117.735389873803));
#37278=CARTESIAN_POINT('Ctrl Pts',(-34.2219300988871,-89.3485398544562,
117.788039381534));
#37279=CARTESIAN_POINT('Ctrl Pts',(-33.8042056112606,-88.5032985577371,
117.840688889265));
#37280=CARTESIAN_POINT('Ctrl Pts',(-33.8350475829636,-87.6747548398119,
117.893338396996));
#37281=CARTESIAN_POINT('Ctrl Pts',(-33.8658895546665,-86.8462111218867,
117.945987904727));
#37282=CARTESIAN_POINT('Ctrl Pts',(-34.3452979856988,-86.0343649827555,
117.998637412457));
#37283=CARTESIAN_POINT('Ctrl Pts',(-35.0559403541099,-85.6072545240904,
118.051286920188));
#37284=CARTESIAN_POINT('Ctrl Pts',(-35.766582722521,-85.1801440654253,118.103936427919));
#37285=CARTESIAN_POINT('Ctrl Pts',(-36.7084590283107,-85.1377692872263,
118.15658593565));
#37286=CARTESIAN_POINT('Ctrl Pts',(-37.4545839712195,-85.4993401506215,
118.209235443381));
#37287=CARTESIAN_POINT('Ctrl Pts',(-38.2007089141282,-85.8609110140166,
118.261884951112));
#37288=CARTESIAN_POINT('Ctrl Pts',(-38.751082494156,-86.626427519006,118.314534458842));
#37289=CARTESIAN_POINT('Ctrl Pts',(-38.8562012181559,-87.4488543994952,
118.367183966573));
#37290=CARTESIAN_POINT('Ctrl Pts',(-38.8696666106516,-87.554204810187,118.373928210218));
#37291=CARTESIAN_POINT('Ctrl Pts',(-38.8758258875797,-87.6604890541088,
118.380672453863));
#37292=CARTESIAN_POINT('Ctrl Pts',(-38.8750031561041,-87.7668692329086,
118.387416697508));
#37293=CARTESIAN_POINT('Origin',(-36.3549260746835,-87.7685555885722,114.));
#37294=CARTESIAN_POINT('',(-38.8685903326823,-87.7680141435005,119.387416697508));
#37295=CARTESIAN_POINT('',(-38.8706378814634,-87.770579470363,119.112583302492));
#37296=CARTESIAN_POINT('',(-38.8724260746835,-87.7685555885722,114.));
#37297=CARTESIAN_POINT('Ctrl Pts',(-38.8706378814634,-87.770579470363,119.112583302492));
#37298=CARTESIAN_POINT('Ctrl Pts',(-38.866244667136,-87.1975822133564,119.076418122537));
#37299=CARTESIAN_POINT('Ctrl Pts',(-38.671841736866,-86.6218880939353,119.040252942582));
#37300=CARTESIAN_POINT('Ctrl Pts',(-38.3129774354871,-86.1796499242353,
119.004087762628));
#37301=CARTESIAN_POINT('Ctrl Pts',(-37.7905404164158,-85.5358366772506,
118.951438254897));
#37302=CARTESIAN_POINT('Ctrl Pts',(-36.9195484306298,-85.174866348328,118.898788747166));
#37303=CARTESIAN_POINT('Ctrl Pts',(-36.0948524487308,-85.260379348023,118.846139239435));
#37304=CARTESIAN_POINT('Ctrl Pts',(-35.2701564668318,-85.345892347718,118.793489731704));
#37305=CARTESIAN_POINT('Ctrl Pts',(-34.4917564888197,-85.8778886760306,
118.740840223973));
#37306=CARTESIAN_POINT('Ctrl Pts',(-34.1125283082994,-86.6151958869313,
118.688190716243));
#37307=CARTESIAN_POINT('Ctrl Pts',(-33.733300127779,-87.352503097832,118.635541208512));
#37308=CARTESIAN_POINT('Ctrl Pts',(-33.7532437447503,-88.2951211913206,
118.582891700781));
#37309=CARTESIAN_POINT('Ctrl Pts',(-34.1633180234681,-89.015728589202,118.53024219305));
#37310=CARTESIAN_POINT('Ctrl Pts',(-34.5733923021859,-89.7363359870834,
118.477592685319));
#37311=CARTESIAN_POINT('Ctrl Pts',(-35.3735972426501,-90.2349326893574,
118.424943177588));
#37312=CARTESIAN_POINT('Ctrl Pts',(-36.2011721037992,-90.2854874629831,
118.372293669858));
#37313=CARTESIAN_POINT('Ctrl Pts',(-37.0287469649484,-90.3360422366088,
118.319644162127));
#37314=CARTESIAN_POINT('Ctrl Pts',(-37.8836917467824,-89.938555081586,118.266994654396));
#37315=CARTESIAN_POINT('Ctrl Pts',(-38.3784302333781,-89.2732207551958,
118.214345146665));
#37316=CARTESIAN_POINT('Ctrl Pts',(-38.6971764917278,-88.8445643380494,
118.180424531941));
#37317=CARTESIAN_POINT('Ctrl Pts',(-38.8664059144585,-88.3047281274853,
118.146503917216));
#37318=CARTESIAN_POINT('Ctrl Pts',(-38.8698085201626,-87.7668461825819,
118.112583302492));
#37319=CARTESIAN_POINT('Ctrl Pts',(-38.8750031561041,-87.7668692329086,
118.387416697508));
#37320=CARTESIAN_POINT('Ctrl Pts',(-38.8694031648155,-88.4909549063227,
118.433321961594));
#37321=CARTESIAN_POINT('Ctrl Pts',(-38.5403295713882,-89.2194852035135,
118.47922722568));
#37322=CARTESIAN_POINT('Ctrl Pts',(-37.9899883652829,-89.6882319936022,
118.525132489766));
#37323=CARTESIAN_POINT('Ctrl Pts',(-37.3587929204378,-90.2258454512309,
118.577781997497));
#37324=CARTESIAN_POINT('Ctrl Pts',(-36.4365381627752,-90.4217351104991,
118.630431505227));
#37325=CARTESIAN_POINT('Ctrl Pts',(-35.6413142618343,-90.1870973748279,
118.683081012958));
#37326=CARTESIAN_POINT('Ctrl Pts',(-34.8460903608934,-89.9524596391566,
118.735730520689));
#37327=CARTESIAN_POINT('Ctrl Pts',(-34.1778973166741,-89.2872945085458,
118.78838002842));
#37328=CARTESIAN_POINT('Ctrl Pts',(-33.9396502852875,-88.4931444766406,
118.841029536151));
#37329=CARTESIAN_POINT('Ctrl Pts',(-33.7014032539009,-87.6989944447354,
118.893679043881));
#37330=CARTESIAN_POINT('Ctrl Pts',(-33.8931022353469,-86.7758595115357,
118.946328551612));
#37331=CARTESIAN_POINT('Ctrl Pts',(-34.4278434102823,-86.1422288678049,
118.998978059343));
#37332=CARTESIAN_POINT('Ctrl Pts',(-34.9625845852178,-85.5085982240741,
119.051627567074));
#37333=CARTESIAN_POINT('Ctrl Pts',(-35.8403679536426,-85.164471869812,119.104277074805));
#37334=CARTESIAN_POINT('Ctrl Pts',(-36.6632637763088,-85.2658542408029,
119.156926582536));
#37335=CARTESIAN_POINT('Ctrl Pts',(-37.4861595989751,-85.3672366117938,
119.209576090266));
#37336=CARTESIAN_POINT('Ctrl Pts',(-38.2541678758828,-85.9141277080375,
119.262225597997));
#37337=CARTESIAN_POINT('Ctrl Pts',(-38.6191237284295,-86.6586027960181,
119.314875105728));
#37338=CARTESIAN_POINT('Ctrl Pts',(-38.7867383280348,-87.000520572969,119.339055636321));
#37339=CARTESIAN_POINT('Ctrl Pts',(-38.8693361655413,-87.3841151894692,
119.363236166915));
#37340=CARTESIAN_POINT('Ctrl Pts',(-38.8685903326823,-87.7680141435005,
119.387416697508));
#37341=CARTESIAN_POINT('Origin',(-36.3549260746835,-87.7685555885722,114.));
#37342=CARTESIAN_POINT('',(-38.873093130194,-87.7707538189189,120.387416697508));
#37343=CARTESIAN_POINT('',(-38.8765118730483,-87.7682823374696,120.112583302492));
#37344=CARTESIAN_POINT('',(-38.8724260746835,-87.7685555885722,114.));
#37345=CARTESIAN_POINT('Ctrl Pts',(-38.8765118730483,-87.7682823374696,
120.112583302492));
#37346=CARTESIAN_POINT('Ctrl Pts',(-38.8765351721742,-87.7532903980737,
120.11163134332));
#37347=CARTESIAN_POINT('Ctrl Pts',(-38.8764129085711,-87.7382988488132,
120.110679384147));
#37348=CARTESIAN_POINT('Ctrl Pts',(-38.8761439194262,-87.7233099327277,
120.109727424975));
#37349=CARTESIAN_POINT('Ctrl Pts',(-38.8612670775668,-86.8943257953643,
120.057077917244));
#37350=CARTESIAN_POINT('Ctrl Pts',(-38.3975852156679,-86.0733960305389,
120.004428409513));
#37351=CARTESIAN_POINT('Ctrl Pts',(-37.6953016325259,-85.6326764849286,
119.951778901782));
#37352=CARTESIAN_POINT('Ctrl Pts',(-36.9930180493839,-85.1919569393182,
119.899129394052));
#37353=CARTESIAN_POINT('Ctrl Pts',(-36.0521327449989,-85.1314476129227,
119.846479886321));
#37354=CARTESIAN_POINT('Ctrl Pts',(-35.299181677782,-85.4785795754927,119.79383037859));
#37355=CARTESIAN_POINT('Ctrl Pts',(-34.5462306105651,-85.8257115380627,
119.741180870859));
#37356=CARTESIAN_POINT('Ctrl Pts',(-33.9812137805165,-86.5804847895982,
119.688531363128));
#37357=CARTESIAN_POINT('Ctrl Pts',(-33.8602730174755,-87.4007343120143,
119.635881855397));
#37358=CARTESIAN_POINT('Ctrl Pts',(-33.7393322544345,-88.2209838344304,
119.583232347667));
#37359=CARTESIAN_POINT('Ctrl Pts',(-34.0624675584012,-89.1067096277273,
119.530582839936));
#37360=CARTESIAN_POINT('Ctrl Pts',(-34.6831904327383,-89.656381393097,119.477933332205));
#37361=CARTESIAN_POINT('Ctrl Pts',(-35.3039133070753,-90.2060531584668,
119.425283824474));
#37362=CARTESIAN_POINT('Ctrl Pts',(-36.2222237517827,-90.4196708959094,
119.372634316743));
#37363=CARTESIAN_POINT('Ctrl Pts',(-37.0218197012666,-90.2003942426243,
119.319984809013));
#37364=CARTESIAN_POINT('Ctrl Pts',(-37.8214156507506,-89.9811175893391,
119.267335301282));
#37365=CARTESIAN_POINT('Ctrl Pts',(-38.5022971050112,-89.328946545326,119.214685793551));
#37366=CARTESIAN_POINT('Ctrl Pts',(-38.7557968059632,-88.5395329407962,
119.16203628582));
#37367=CARTESIAN_POINT('Ctrl Pts',(-38.8351664400152,-88.2923710361789,
119.145551958044));
#37368=CARTESIAN_POINT('Ctrl Pts',(-38.8726403375566,-88.0317554028776,
119.129067630268));
#37369=CARTESIAN_POINT('Ctrl Pts',(-38.8706378814634,-87.770579470363,119.112583302492));
#37370=CARTESIAN_POINT('Ctrl Pts',(-38.8685903326823,-87.7680141435005,
119.387416697508));
#37371=CARTESIAN_POINT('Ctrl Pts',(-38.8677122254576,-88.219998044484,119.415885674646));
#37372=CARTESIAN_POINT('Ctrl Pts',(-38.7513067986863,-88.6724038047288,
119.444354651783));
#37373=CARTESIAN_POINT('Ctrl Pts',(-38.5221045252354,-89.0577118184919,
119.472823628921));
#37374=CARTESIAN_POINT('Ctrl Pts',(-38.0982260413089,-89.7702866732678,
119.525473136651));
#37375=CARTESIAN_POINT('Ctrl Pts',(-37.2885656452704,-90.2533773031023,
119.578122644382));
#37376=CARTESIAN_POINT('Ctrl Pts',(-36.4601705432131,-90.2879820377545,
119.630772152113));
#37377=CARTESIAN_POINT('Ctrl Pts',(-35.6317754411557,-90.3225867724067,
119.683421659844));
#37378=CARTESIAN_POINT('Ctrl Pts',(-34.7846456330796,-89.9087056118767,
119.736071167575));
#37379=CARTESIAN_POINT('Ctrl Pts',(-34.3028145807763,-89.2339650386027,
119.788720675305));
#37380=CARTESIAN_POINT('Ctrl Pts',(-33.8209835284731,-88.5592244653287,
119.841370183036));
#37381=CARTESIAN_POINT('Ctrl Pts',(-33.7044512319429,-87.6236244793106,
119.894019690767));
#37382=CARTESIAN_POINT('Ctrl Pts',(-34.0060457422708,-86.8513056164977,
119.946669198498));
#37383=CARTESIAN_POINT('Ctrl Pts',(-34.3076402525988,-86.0789867536849,
119.999318706229));
#37384=CARTESIAN_POINT('Ctrl Pts',(-35.027361569785,-85.4699490140772,120.05196821396));
#37385=CARTESIAN_POINT('Ctrl Pts',(-35.8389351715648,-85.3002893469818,
120.10461772169));
#37386=CARTESIAN_POINT('Ctrl Pts',(-36.6505087733447,-85.1306296798865,
120.157267229421));
#37387=CARTESIAN_POINT('Ctrl Pts',(-37.5539346597181,-85.4003480853034,
120.209916737152));
#37388=CARTESIAN_POINT('Ctrl Pts',(-38.1396580480158,-85.9871739818863,
120.262566244883));
#37389=CARTESIAN_POINT('Ctrl Pts',(-38.6026432577794,-86.4510306696204,
120.304183062425));
#37390=CARTESIAN_POINT('Ctrl Pts',(-38.8671242526413,-87.1130198050204,
120.345799879966));
#37391=CARTESIAN_POINT('Ctrl Pts',(-38.873093130194,-87.7707538189189,120.387416697508));
#37392=CARTESIAN_POINT('Origin',(-36.3549260746835,-87.7685555885722,114.));
#37393=CARTESIAN_POINT('',(-38.8751287300693,-87.7669767062971,121.387416697508));
#37394=CARTESIAN_POINT('',(-38.8699208872996,-87.7667938007243,121.112583302492));
#37395=CARTESIAN_POINT('',(-38.8724260746835,-87.7685555885722,114.));
#37396=CARTESIAN_POINT('',(-34.4414600780185,-86.1325683851973,122.));
#37397=CARTESIAN_POINT('Ctrl Pts',(-38.8751287300693,-87.7669767062971,
121.387416697508));
#37398=CARTESIAN_POINT('Ctrl Pts',(-38.8696706756881,-88.49619959385,121.43366260848));
#37399=CARTESIAN_POINT('Ctrl Pts',(-38.5351409382516,-89.2296736768507,
121.479908519451));
#37400=CARTESIAN_POINT('Ctrl Pts',(-37.9776638931539,-89.6985069777893,
121.526154430423));
#37401=CARTESIAN_POINT('Ctrl Pts',(-37.3429939000879,-90.2322588703065,
121.578803938153));
#37402=CARTESIAN_POINT('Ctrl Pts',(-36.4193596116175,-90.4230071270047,
121.631453445884));
#37403=CARTESIAN_POINT('Ctrl Pts',(-35.6257426342697,-90.1828532317666,
121.684102953615));
#37404=CARTESIAN_POINT('Ctrl Pts',(-34.832125656922,-89.9426993365284,121.736752461346));
#37405=CARTESIAN_POINT('Ctrl Pts',(-34.168525990697,-89.2716432893538,121.789401969077));
#37406=CARTESIAN_POINT('Ctrl Pts',(-33.9355607493907,-88.4773573530763,
121.842051476808));
#37407=CARTESIAN_POINT('Ctrl Pts',(-33.7025955080844,-87.6830714167989,
121.894700984538));
#37408=CARTESIAN_POINT('Ctrl Pts',(-33.9002646916969,-86.7655555914187,
121.947350492269));
#37409=CARTESIAN_POINT('Ctrl Pts',(-34.4414600780185,-86.1325683851972,
122.));
#37410=CARTESIAN_POINT('',(-38.2720363511395,-86.1300276335002,122.));
#37411=CARTESIAN_POINT('Origin',(-36.3549260746835,-87.7685555885722,122.));
#37412=CARTESIAN_POINT('Ctrl Pts',(-38.2720451973147,-86.1300214660444,
122.));
#37413=CARTESIAN_POINT('Ctrl Pts',(-37.7492246461072,-85.5213064340422,
121.949053726697));
#37414=CARTESIAN_POINT('Ctrl Pts',(-36.9095001229587,-85.1811300134451,
121.898107453395));
#37415=CARTESIAN_POINT('Ctrl Pts',(-36.1108292497374,-85.258892786295,121.847161180092));
#37416=CARTESIAN_POINT('Ctrl Pts',(-35.2854572335304,-85.3392553220591,
121.794511672361));
#37417=CARTESIAN_POINT('Ctrl Pts',(-34.5039297618072,-85.8659692441484,
121.74186216463));
#37418=CARTESIAN_POINT('Ctrl Pts',(-34.1200451421356,-86.6007560283003,
121.6892126569));
#37419=CARTESIAN_POINT('Ctrl Pts',(-33.7361605224639,-87.3355428124522,
121.636563149169));
#37420=CARTESIAN_POINT('Ctrl Pts',(-33.7499187548438,-88.2784024586666,
121.583913641438));
#37421=CARTESIAN_POINT('Ctrl Pts',(-34.1553235431823,-89.0016622385077,
121.531264133707));
#37422=CARTESIAN_POINT('Ctrl Pts',(-34.5607283315209,-89.7249220183489,
121.478614625976));
#37423=CARTESIAN_POINT('Ctrl Pts',(-35.3577796758181,-90.2285819318168,
121.425965118245));
#37424=CARTESIAN_POINT('Ctrl Pts',(-36.1850294050421,-90.2844329189877,
121.373315610515));
#37425=CARTESIAN_POINT('Ctrl Pts',(-37.0122791342662,-90.3402839061586,
121.320666102784));
#37426=CARTESIAN_POINT('Ctrl Pts',(-37.8697272484169,-89.9483259670326,
121.268016595053));
#37427=CARTESIAN_POINT('Ctrl Pts',(-38.3687196042729,-89.286190143456,121.215367087322));
#37428=CARTESIAN_POINT('Ctrl Pts',(-38.6934350362348,-88.8553103565275,
121.181105825712));
#37429=CARTESIAN_POINT('Ctrl Pts',(-38.8663568078635,-88.310019546557,121.146844564102));
#37430=CARTESIAN_POINT('Ctrl Pts',(-38.8699208872996,-87.7667938007243,
121.112583302492));
#37431=CARTESIAN_POINT('Origin',(-36.3549260746835,-87.7685555885722,124.208423447177));
#37432=CARTESIAN_POINT('',(-39.4331960788118,-87.7677421217272,107.791576552823));
#37433=CARTESIAN_POINT('',(-39.4235551911591,-87.7682412648602,107.708423447177));
#37434=CARTESIAN_POINT('',(-39.4284260746835,-87.768555588572,124.208423447177));
#37435=CARTESIAN_POINT('',(-35.5611267921511,-90.7377785423181,107.));
#37436=CARTESIAN_POINT('Ctrl Pts',(-39.4235551911591,-87.7682412648602,
107.708423447177));
#37437=CARTESIAN_POINT('Ctrl Pts',(-39.4238750506399,-87.2730657797943,
107.682880329042));
#37438=CARTESIAN_POINT('Ctrl Pts',(-39.077622760914,-85.7577492069975,107.604687703175));
#37439=CARTESIAN_POINT('Ctrl Pts',(-36.7064604496932,-84.1596939007676,
107.473845569577));
#37440=CARTESIAN_POINT('Ctrl Pts',(-33.5229009026989,-85.5001505522318,
107.315897046385));
#37441=CARTESIAN_POINT('Ctrl Pts',(-32.9121328624527,-88.9023373811549,
107.157948523192));
#37442=CARTESIAN_POINT('Ctrl Pts',(-34.5788882023795,-90.4751844899406,
107.052649507731));
#37443=CARTESIAN_POINT('Ctrl Pts',(-35.5611267921512,-90.7377785423181,
107.));
#37444=CARTESIAN_POINT('',(-37.1487253572168,-90.7377785423178,107.));
#37445=CARTESIAN_POINT('Origin',(-36.3549260746835,-87.7685555885722,107.));
#37446=CARTESIAN_POINT('Ctrl Pts',(-39.4331960788118,-87.7677421217272,
107.791576552823));
#37447=CARTESIAN_POINT('Ctrl Pts',(-39.4333521478699,-87.7232332784528,
107.789262006108));
#37448=CARTESIAN_POINT('Ctrl Pts',(-39.4123924336899,-86.666423722535,107.734297951662));
#37449=CARTESIAN_POINT('Ctrl Pts',(-38.2031234854001,-84.6483923994501,
107.626684389485));
#37450=CARTESIAN_POINT('Ctrl Pts',(-34.7524573177229,-84.5150170933021,
107.468735866293));
#37451=CARTESIAN_POINT('Ctrl Pts',(-32.7548482639927,-87.3323302896557,
107.3107873431));
#37452=CARTESIAN_POINT('Ctrl Pts',(-34.0073630870521,-90.5088743722522,
107.154542054336));
#37453=CARTESIAN_POINT('Ctrl Pts',(-36.2036732140504,-90.9937479068112,
107.050946273303));
#37454=CARTESIAN_POINT('Ctrl Pts',(-37.1506394945612,-90.7428673099699,
107.));
#37455=CARTESIAN_POINT('Origin',(-36.3549260746835,-87.7685555885722,124.208423447177));
#37456=CARTESIAN_POINT('',(-39.4248378354749,-87.7666901941256,108.791576552823));
#37457=CARTESIAN_POINT('',(-39.4300190231571,-87.7711138662458,108.708423447177));
#37458=CARTESIAN_POINT('',(-39.4284260746835,-87.768555588572,124.208423447177));
#37459=CARTESIAN_POINT('Ctrl Pts',(-39.4300190231571,-87.7711138662458,
108.708423447177));
#37460=CARTESIAN_POINT('Ctrl Pts',(-39.422631166441,-86.9423658304694,108.665444042093));
#37461=CARTESIAN_POINT('Ctrl Pts',(-38.6509821187261,-85.0862753982503,
108.569815129278));
#37462=CARTESIAN_POINT('Ctrl Pts',(-35.5219282427889,-84.238982422185,108.421536708732));
#37463=CARTESIAN_POINT('Ctrl Pts',(-32.9440320186257,-86.5365567862535,
108.26358818554));
#37464=CARTESIAN_POINT('Ctrl Pts',(-33.4587560273279,-89.9512135763613,
108.105639662347));
#37465=CARTESIAN_POINT('Ctrl Pts',(-36.5992129203138,-91.3867838191251,
107.947691139155));
#37466=CARTESIAN_POINT('Ctrl Pts',(-39.0463676630991,-89.8404170424041,
107.815285734098));
#37467=CARTESIAN_POINT('Ctrl Pts',(-39.4232157558696,-88.293722122157,107.735529836772));
#37468=CARTESIAN_POINT('Ctrl Pts',(-39.4235551911591,-87.7682412648602,
107.708423447177));
#37469=CARTESIAN_POINT('Ctrl Pts',(-39.4248378354749,-87.7666901941256,
108.791576552823));
#37470=CARTESIAN_POINT('Ctrl Pts',(-39.4269819669572,-87.3842072109777,
108.771825719159));
#37471=CARTESIAN_POINT('Ctrl Pts',(-39.183987538194,-85.9847711220175,108.699425377765));
#37472=CARTESIAN_POINT('Ctrl Pts',(-37.0970138838616,-84.2187462913202,
108.57437552864));
#37473=CARTESIAN_POINT('Ctrl Pts',(-33.7881604641648,-85.2066067039222,
108.416427005448));
#37474=CARTESIAN_POINT('Ctrl Pts',(-32.8065173074963,-88.517318877192,108.258478482255));
#37475=CARTESIAN_POINT('Ctrl Pts',(-35.0421044524555,-91.1491282972506,
108.100529959063));
#37476=CARTESIAN_POINT('Ctrl Pts',(-38.4177929438602,-90.72226834617,107.944895982585));
#37477=CARTESIAN_POINT('Ctrl Pts',(-39.4298020103746,-88.7356858130984,
107.841911513838));
#37478=CARTESIAN_POINT('Ctrl Pts',(-39.4331960788118,-87.7677421217272,
107.791576552823));
#37479=CARTESIAN_POINT('Origin',(-36.3549260746835,-87.7685555885722,124.208423447177));
#37480=CARTESIAN_POINT('',(-39.4267610875431,-87.7711482491674,109.791576552823));
#37481=CARTESIAN_POINT('',(-39.4310569711989,-87.7662875373292,109.708423447177));
#37482=CARTESIAN_POINT('',(-39.4284260746835,-87.768555588572,124.208423447177));
#37483=CARTESIAN_POINT('Ctrl Pts',(-39.4310569711989,-87.7662875373292,
109.708423447177));
#37484=CARTESIAN_POINT('Ctrl Pts',(-39.4322960926139,-87.6166677872432,
109.700657262876));
#37485=CARTESIAN_POINT('Ctrl Pts',(-39.3546331967087,-86.4540177992007,
109.640241570843));
#37486=CARTESIAN_POINT('Ctrl Pts',(-37.8732761190034,-84.4751586948984,
109.52717637108));
#37487=CARTESIAN_POINT('Ctrl Pts',(-34.4272253359264,-84.6967778557991,
109.369227847887));
#37488=CARTESIAN_POINT('Ctrl Pts',(-32.728961758079,-87.7034840352579,109.211279324695));
#37489=CARTESIAN_POINT('Ctrl Pts',(-34.3182506239731,-90.7691894929664,
109.053330801502));
#37490=CARTESIAN_POINT('Ctrl Pts',(-37.754129375528,-91.1143096400617,108.89538227831));
#37491=CARTESIAN_POINT('Ctrl Pts',(-39.3316611845371,-89.1574728635941,
108.780413160201));
#37492=CARTESIAN_POINT('Ctrl Pts',(-39.4316812456249,-87.9575770934212,
108.718093549824));
#37493=CARTESIAN_POINT('Ctrl Pts',(-39.4300190231571,-87.7711138662458,
108.708423447177));
#37494=CARTESIAN_POINT('Ctrl Pts',(-39.4267610875431,-87.7711482491674,
109.791576552823));
#37495=CARTESIAN_POINT('Ctrl Pts',(-39.4209016416215,-87.0521420397502,
109.754389432211));
#37496=CARTESIAN_POINT('Ctrl Pts',(-38.8116906656652,-85.3062201297381,
109.664552803868));
#37497=CARTESIAN_POINT('Ctrl Pts',(-35.9114810653333,-84.1692214210988,
109.522066667795));
#37498=CARTESIAN_POINT('Ctrl Pts',(-33.098603051042,-86.1722440278901,109.364118144602));
#37499=CARTESIAN_POINT('Ctrl Pts',(-33.2381341114487,-89.6225939175359,
109.20616962141));
#37500=CARTESIAN_POINT('Ctrl Pts',(-36.2035655990193,-91.3919433535738,
109.048221098218));
#37501=CARTESIAN_POINT('Ctrl Pts',(-38.9182551690064,-90.0656308344281,
108.910023408688));
#37502=CARTESIAN_POINT('Ctrl Pts',(-39.4212663870998,-88.4037864916013,
108.82447522689));
#37503=CARTESIAN_POINT('Ctrl Pts',(-39.4248378354749,-87.7666901941256,
108.791576552823));
#37504=CARTESIAN_POINT('Origin',(-36.3549260746835,-87.7685555885722,124.208423447177));
#37505=CARTESIAN_POINT('',(-39.4332678666261,-87.7678707816449,110.791576552823));
#37506=CARTESIAN_POINT('',(-39.4236452988987,-87.7682071722042,110.708423447177));
#37507=CARTESIAN_POINT('',(-39.4284260746835,-87.768555588572,124.208423447177));
#37508=CARTESIAN_POINT('Ctrl Pts',(-39.4236452988987,-87.7682071722042,
110.708423447177));
#37509=CARTESIAN_POINT('Ctrl Pts',(-39.4241445943381,-87.2796756480956,
110.683220975927));
#37510=CARTESIAN_POINT('Ctrl Pts',(-39.0844835270856,-85.7712276403467,
110.605368996946));
#37511=CARTESIAN_POINT('Ctrl Pts',(-36.7289586650204,-84.1613476130271,
110.474867510234));
#37512=CARTESIAN_POINT('Ctrl Pts',(-33.5388964962196,-85.4834238308911,
110.316918987042));
#37513=CARTESIAN_POINT('Ctrl Pts',(-32.9020426949109,-88.8773595086493,
110.158970463849));
#37514=CARTESIAN_POINT('Ctrl Pts',(-35.3958132509259,-91.2659764064493,
110.001021940657));
#37515=CARTESIAN_POINT('Ctrl Pts',(-38.5938084373591,-90.5220575062303,
109.850839601766));
#37516=CARTESIAN_POINT('Ctrl Pts',(-39.4238956825823,-88.6309890913328,
109.753306770606));
#37517=CARTESIAN_POINT('Ctrl Pts',(-39.4310569711989,-87.7662875373292,
109.708423447177));
#37518=CARTESIAN_POINT('Ctrl Pts',(-39.4332678666261,-87.7678707816449,
110.791576552823));
#37519=CARTESIAN_POINT('Ctrl Pts',(-39.4333835106076,-87.7299144909416,
110.789602652993));
#37520=CARTESIAN_POINT('Ctrl Pts',(-39.4156195689302,-86.6796669871756,
110.734979245433));
#37521=CARTESIAN_POINT('Ctrl Pts',(-38.2231009204979,-84.66021635197,110.627706330142));
#37522=CARTESIAN_POINT('Ctrl Pts',(-34.7734204516813,-84.5050160949677,
110.46975780695));
#37523=CARTESIAN_POINT('Ctrl Pts',(-32.7576430317562,-87.3087678398475,
110.311809283757));
#37524=CARTESIAN_POINT('Ctrl Pts',(-34.0034127407753,-90.5293951545392,
110.153860760565));
#37525=CARTESIAN_POINT('Ctrl Pts',(-37.381228070904,-91.2468531980925,109.995912237372));
#37526=CARTESIAN_POINT('Ctrl Pts',(-39.252338964875,-89.3842212342544,109.875150834792));
#37527=CARTESIAN_POINT('Ctrl Pts',(-39.4291974423792,-88.0701106901465,
109.807038939942));
#37528=CARTESIAN_POINT('Ctrl Pts',(-39.4267610875431,-87.7711482491674,
109.791576552823));
#37529=CARTESIAN_POINT('Origin',(-36.3549260746835,-87.7685555885722,124.208423447177));
#37530=CARTESIAN_POINT('',(-39.4249634829513,-87.7666135330092,111.791576552823));
#37531=CARTESIAN_POINT('',(-39.4298261000276,-87.7711513822271,111.708423447177));
#37532=CARTESIAN_POINT('',(-39.4284260746835,-87.768555588572,124.208423447177));
#37533=CARTESIAN_POINT('Ctrl Pts',(-39.4298261000276,-87.7711513822271,
111.708423447177));
#37534=CARTESIAN_POINT('Ctrl Pts',(-39.4224452207145,-86.9488393862918,
111.665784688979));
#37535=CARTESIAN_POINT('Ctrl Pts',(-38.6609852839478,-85.0990845351561,
111.570496423049));
#37536=CARTESIAN_POINT('Ctrl Pts',(-35.5445999861014,-84.2336975457609,
111.422558649389));
#37537=CARTESIAN_POINT('Ctrl Pts',(-32.9520311196661,-86.5146992660596,
111.264610126197));
#37538=CARTESIAN_POINT('Ctrl Pts',(-33.444763614499,-89.9325343795896,111.106661603004));
#37539=CARTESIAN_POINT('Ctrl Pts',(-36.5760519035439,-91.3883557378978,
110.948713079812));
#37540=CARTESIAN_POINT('Ctrl Pts',(-39.0392098427808,-89.8535958737908,
110.815967027869));
#37541=CARTESIAN_POINT('Ctrl Pts',(-39.4231015355509,-88.3002479562603,
110.735870483658));
#37542=CARTESIAN_POINT('Ctrl Pts',(-39.4236452988987,-87.7682071722042,
110.708423447177));
#37543=CARTESIAN_POINT('Ctrl Pts',(-39.4249634829513,-87.7666135330092,
111.791576552823));
#37544=CARTESIAN_POINT('Ctrl Pts',(-39.4271631600903,-87.3907660068182,
111.772166366045));
#37545=CARTESIAN_POINT('Ctrl Pts',(-39.1897288443723,-85.998126327073,111.700106671536));
#37546=CARTESIAN_POINT('Ctrl Pts',(-37.1197916542217,-84.2235829922162,
111.575397469297));
#37547=CARTESIAN_POINT('Ctrl Pts',(-33.8046641643864,-85.1901812455926,
111.417448946105));
#37548=CARTESIAN_POINT('Ctrl Pts',(-32.8017815859054,-88.494513098026,111.259500422912));
#37549=CARTESIAN_POINT('Ctrl Pts',(-35.0204270513993,-91.1406413556617,
111.10155189972));
#37550=CARTESIAN_POINT('Ctrl Pts',(-38.4061746688924,-90.7345413083506,
110.945577276357));
#37551=CARTESIAN_POINT('Ctrl Pts',(-39.4302989575766,-88.742316433115,110.842252160724));
#37552=CARTESIAN_POINT('Ctrl Pts',(-39.4332678666261,-87.7678707816449,
110.791576552823));
#37553=CARTESIAN_POINT('Origin',(-36.3549260746835,-87.7685555885722,124.208423447177));
#37554=CARTESIAN_POINT('',(-39.4265849952197,-87.7711115889072,112.791576552823));
#37555=CARTESIAN_POINT('',(-39.4312327529812,-87.7663532935098,112.708423447177));
#37556=CARTESIAN_POINT('',(-39.4284260746835,-87.768555588572,124.208423447177));
#37557=CARTESIAN_POINT('Ctrl Pts',(-39.4312327529812,-87.7663532935098,
112.708423447177));
#37558=CARTESIAN_POINT('Ctrl Pts',(-39.4323936164487,-87.6233176105418,
112.700997909761));
#37559=CARTESIAN_POINT('Ctrl Pts',(-39.358587288045,-86.4673154971078,112.640922864614));
#37560=CARTESIAN_POINT('Ctrl Pts',(-37.8943917712909,-84.4849759684705,
112.528198311736));
#37561=CARTESIAN_POINT('Ctrl Pts',(-34.446988838572,-84.684463298183,112.370249788544));
#37562=CARTESIAN_POINT('Ctrl Pts',(-32.7294545705478,-87.6802033091648,
112.212301265352));
#37563=CARTESIAN_POINT('Ctrl Pts',(-34.299025051591,-90.7560496447713,112.054352742159));
#37564=CARTESIAN_POINT('Ctrl Pts',(-37.7326184628711,-91.1232259801486,
111.896404218966));
#37565=CARTESIAN_POINT('Ctrl Pts',(-39.3273916051006,-89.1707887114988,
111.781094453973));
#37566=CARTESIAN_POINT('Ctrl Pts',(-39.4315589866606,-87.9642142146455,
111.71843419671));
#37567=CARTESIAN_POINT('Ctrl Pts',(-39.4298261000276,-87.7711513822271,
111.708423447177));
#37568=CARTESIAN_POINT('Ctrl Pts',(-39.4265849952197,-87.7711115889072,
112.791576552823));
#37569=CARTESIAN_POINT('Ctrl Pts',(-39.4208859423477,-87.05858818249,112.754730079096));
#37570=CARTESIAN_POINT('Ctrl Pts',(-38.820534631401,-85.3192830484007,112.66523409764));
#37571=CARTESIAN_POINT('Ctrl Pts',(-35.9346015224717,-84.1664482422435,
112.523088608452));
#37572=CARTESIAN_POINT('Ctrl Pts',(-33.1089201003701,-86.1513681293118,
112.365140085259));
#37573=CARTESIAN_POINT('Ctrl Pts',(-33.2262935723694,-89.6025427011582,
112.207191562067));
#37574=CARTESIAN_POINT('Ctrl Pts',(-36.1803029811607,-91.3908969362198,
112.049243038874));
#37575=CARTESIAN_POINT('Ctrl Pts',(-38.9101651204659,-90.0788161109398,
111.91070470246));
#37576=CARTESIAN_POINT('Ctrl Pts',(-39.4211966065552,-88.4102403407061,
111.824815873776));
#37577=CARTESIAN_POINT('Ctrl Pts',(-39.4249634829513,-87.7666135330092,
111.791576552823));
#37578=CARTESIAN_POINT('Origin',(-36.3549260746835,-87.7685555885722,124.208423447177));
#37579=CARTESIAN_POINT('',(-39.4333271029731,-87.7679866768215,113.791576552823));
#37580=CARTESIAN_POINT('',(-39.4236711760032,-87.7681022535202,113.708423447177));
#37581=CARTESIAN_POINT('',(-39.4284260746835,-87.768555588572,124.208423447177));
#37582=CARTESIAN_POINT('Ctrl Pts',(-39.4236711760032,-87.7681022535202,
113.708423447178));
#37583=CARTESIAN_POINT('Ctrl Pts',(-39.4243123526912,-87.2861840776058,
113.683561622813));
#37584=CARTESIAN_POINT('Ctrl Pts',(-39.0911306006805,-85.7845536494958,
113.606050290717));
#37585=CARTESIAN_POINT('Ctrl Pts',(-36.7521128317831,-84.1638236384041,
113.475889450891));
#37586=CARTESIAN_POINT('Ctrl Pts',(-33.5536273739847,-85.4653892155019,
113.317940927699));
#37587=CARTESIAN_POINT('Ctrl Pts',(-32.8949942504612,-88.8551656954239,
113.159992404506));
#37588=CARTESIAN_POINT('Ctrl Pts',(-35.3733760828904,-91.2597458392159,
113.002043881314));
#37589=CARTESIAN_POINT('Ctrl Pts',(-38.5833465123841,-90.5347358539682,
112.851520895538));
#37590=CARTESIAN_POINT('Ctrl Pts',(-39.4241627118446,-88.6374877472081,
112.753647417492));
#37591=CARTESIAN_POINT('Ctrl Pts',(-39.4312327529812,-87.7663532935098,
112.708423447177));
#37592=CARTESIAN_POINT('Ctrl Pts',(-39.4333271029731,-87.7679866768215,
113.791576552823));
#37593=CARTESIAN_POINT('Ctrl Pts',(-39.4334077862495,-87.7365823354763,
113.789943299879));
#37594=CARTESIAN_POINT('Ctrl Pts',(-39.4188026175281,-86.6929051608962,
113.735660539204));
#37595=CARTESIAN_POINT('Ctrl Pts',(-38.2430210496827,-84.672275977644,113.628728270799));
#37596=CARTESIAN_POINT('Ctrl Pts',(-34.7944082359535,-84.4949285269366,
113.470779747607));
#37597=CARTESIAN_POINT('Ctrl Pts',(-32.7606694855963,-87.2856791701479,
113.312831224414));
#37598=CARTESIAN_POINT('Ctrl Pts',(-33.9857338701916,-90.514239175922,113.154882701222));
#37599=CARTESIAN_POINT('Ctrl Pts',(-37.3588727708761,-91.2533713792378,
112.996934178029));
#37600=CARTESIAN_POINT('Ctrl Pts',(-39.247216754307,-89.3975720466728,112.875832128563));
#37601=CARTESIAN_POINT('Ctrl Pts',(-39.4290292542553,-88.0767047836455,
112.807379586827));
#37602=CARTESIAN_POINT('Ctrl Pts',(-39.4265849952197,-87.7711115889072,
112.791576552823));
#37603=CARTESIAN_POINT('Origin',(-36.3549260746835,-87.7685555885722,124.208423447177));
#37604=CARTESIAN_POINT('',(-39.4250943850934,-87.7665395826249,114.791576552823));
#37605=CARTESIAN_POINT('',(-39.4296319167269,-87.7711845285468,114.708423447178));
#37606=CARTESIAN_POINT('',(-39.4284260746835,-87.768555588572,124.208423447177));
#37607=CARTESIAN_POINT('Ctrl Pts',(-39.4296319167269,-87.7711845285468,
114.708423447177));
#37608=CARTESIAN_POINT('Ctrl Pts',(-39.4222700858053,-86.9553091377705,
114.666125335865));
#37609=CARTESIAN_POINT('Ctrl Pts',(-38.6709154553017,-85.1119080614529,
114.571177716821));
#37610=CARTESIAN_POINT('Ctrl Pts',(-35.5673140086676,-84.2285673137265,
114.423580590046));
#37611=CARTESIAN_POINT('Ctrl Pts',(-32.9601522791593,-86.4928751310124,
114.265632066854));
#37612=CARTESIAN_POINT('Ctrl Pts',(-33.4309287026749,-89.9138036211001,
114.107683543661));
#37613=CARTESIAN_POINT('Ctrl Pts',(-36.5528046140307,-91.3897009648648,
113.949735020469));
#37614=CARTESIAN_POINT('Ctrl Pts',(-39.0321124688702,-89.8668909092713,
113.816648321641));
#37615=CARTESIAN_POINT('Ctrl Pts',(-39.4229545425604,-88.3067348769492,
113.736211130544));
#37616=CARTESIAN_POINT('Ctrl Pts',(-39.4236711760032,-87.7681022535202,
113.708423447178));
#37617=CARTESIAN_POINT('Ctrl Pts',(-39.4250943850934,-87.7665395826249,
114.791576552823));
#37618=CARTESIAN_POINT('Ctrl Pts',(-39.4273438878649,-87.3973277353349,
114.772507012931));
#37619=CARTESIAN_POINT('Ctrl Pts',(-39.195415474559,-86.0114816654255,114.700787965308));
#37620=CARTESIAN_POINT('Ctrl Pts',(-37.1425381500136,-84.2285672718597,
114.576419409954));
#37621=CARTESIAN_POINT('Ctrl Pts',(-33.821272475107,-85.1738591706804,114.418470886761));
#37622=CARTESIAN_POINT('Ctrl Pts',(-32.7971934613455,-88.4716833974796,
114.260522363569));
#37623=CARTESIAN_POINT('Ctrl Pts',(-34.9988024045514,-91.1320030246078,
114.102573840377));
#37624=CARTESIAN_POINT('Ctrl Pts',(-38.3944877717556,-90.7468118088923,
113.946258570128));
#37625=CARTESIAN_POINT('Ctrl Pts',(-39.4308068818404,-88.7489320262378,
113.84259280761));
#37626=CARTESIAN_POINT('Ctrl Pts',(-39.4333271029731,-87.7679866768215,
113.791576552823));
#37627=CARTESIAN_POINT('Origin',(-36.3549260746835,-87.7685555885722,124.208423447177));
#37628=CARTESIAN_POINT('',(-39.4264122098445,-87.7710709637358,115.791576552823));
#37629=CARTESIAN_POINT('',(-39.4314046551684,-87.7664230789163,115.708423447177));
#37630=CARTESIAN_POINT('',(-39.4284260746835,-87.768555588572,124.208423447177));
#37631=CARTESIAN_POINT('Ctrl Pts',(-39.4314046551684,-87.7664230789163,
115.708423447177));
#37632=CARTESIAN_POINT('Ctrl Pts',(-39.4324871906633,-87.6299690823578,
115.701338556647));
#37633=CARTESIAN_POINT('Ctrl Pts',(-39.3624944732727,-86.4806100262057,
115.641604158386));
#37634=CARTESIAN_POINT('Ctrl Pts',(-37.9154438949567,-84.494928565653,115.529220252393));
#37635=CARTESIAN_POINT('Ctrl Pts',(-34.4668311220138,-84.6722760142634,
115.371271729201));
#37636=CARTESIAN_POINT('Ctrl Pts',(-32.7300966188443,-87.6569259838135,
115.213323206008));
#37637=CARTESIAN_POINT('Ctrl Pts',(-34.2798847390797,-90.7427871209372,
115.055374682816));
#37638=CARTESIAN_POINT('Ctrl Pts',(-37.7110497287778,-91.1320029848287,
114.897426159623));
#37639=CARTESIAN_POINT('Ctrl Pts',(-39.3230747918906,-89.1841085015426,
114.781775747744));
#37640=CARTESIAN_POINT('Ctrl Pts',(-39.4314335392548,-87.9708494624013,
114.718774843595));
#37641=CARTESIAN_POINT('Ctrl Pts',(-39.4296319167269,-87.7711845285468,
114.708423447177));
#37642=CARTESIAN_POINT('Ctrl Pts',(-39.4264122098445,-87.7710709637358,
115.791576552823));
#37643=CARTESIAN_POINT('Ctrl Pts',(-39.4208786170309,-87.0650342694146,
115.755070725982));
#37644=CARTESIAN_POINT('Ctrl Pts',(-38.8293124187647,-85.3323581275192,
115.665915391411));
#37645=CARTESIAN_POINT('Ctrl Pts',(-35.9577393128856,-84.1638235957717,
115.524110549109));
#37646=CARTESIAN_POINT('Ctrl Pts',(-33.1193709742919,-86.1305588681857,
115.366162025916));
#37647=CARTESIAN_POINT('Ctrl Pts',(-33.2145820402631,-89.5824159495559,
115.208213502724));
#37648=CARTESIAN_POINT('Ctrl Pts',(-36.1570475329969,-91.3897010076914,
115.050264979531));
#37649=CARTESIAN_POINT('Ctrl Pts',(-38.9020112016885,-90.0919926097959,
114.911385996231));
#37650=CARTESIAN_POINT('Ctrl Pts',(-39.4211331867032,-88.4166927603047,
114.825156520661));
#37651=CARTESIAN_POINT('Ctrl Pts',(-39.4250943850934,-87.7665395826249,
114.791576552823));
#37652=CARTESIAN_POINT('Origin',(-36.3549260746835,-87.7685555885722,124.208423447177));
#37653=CARTESIAN_POINT('',(-39.4333760082338,-87.768103846536,116.791576552823));
#37654=CARTESIAN_POINT('',(-39.4237038206158,-87.7679979949716,116.708423447177));
#37655=CARTESIAN_POINT('',(-39.4284260746835,-87.768555588572,124.208423447177));
#37656=CARTESIAN_POINT('Ctrl Pts',(-39.4237038206158,-87.7679979949716,
116.708423447177));
#37657=CARTESIAN_POINT('Ctrl Pts',(-39.4244821252083,-87.2926955099761,
116.683902269698));
#37658=CARTESIAN_POINT('Ctrl Pts',(-39.0977193329511,-85.7978828462761,
116.606731584489));
#37659=CARTESIAN_POINT('Ctrl Pts',(-36.7752506219235,-84.1664482848449,
116.476911391548));
#37660=CARTESIAN_POINT('Ctrl Pts',(-33.568473749851,-85.4474495604007,116.318962868356));
#37661=CARTESIAN_POINT('Ctrl Pts',(-32.8880884545876,-88.8329270784509,
116.161014345163));
#37662=CARTESIAN_POINT('Ctrl Pts',(-35.3509793903652,-91.2533713380237,
116.003065821971));
#37663=CARTESIAN_POINT('Ctrl Pts',(-38.5728137685938,-90.5473934305567,
115.852202189309));
#37664=CARTESIAN_POINT('Ctrl Pts',(-39.4244426117584,-88.643991206724,115.753988064378));
#37665=CARTESIAN_POINT('Ctrl Pts',(-39.4314046551684,-87.7664230789163,
115.708423447177));
#37666=CARTESIAN_POINT('Ctrl Pts',(-39.4333760082338,-87.768103846536,116.791576552823));
#37667=CARTESIAN_POINT('Ctrl Pts',(-39.4334274954906,-87.7432505565165,
116.790283946765));
#37668=CARTESIAN_POINT('Ctrl Pts',(-39.421942007279,-86.7061395822215,116.736341832976));
#37669=CARTESIAN_POINT('Ctrl Pts',(-38.2628633333592,-84.6844632617075,
116.629750211456));
#37670=CARTESIAN_POINT('Ctrl Pts',(-34.8154603598683,-84.4849759296366,
116.471801688264));
#37671=CARTESIAN_POINT('Ctrl Pts',(-32.7638441292674,-87.2626104087614,
116.313853165071));
#37672=CARTESIAN_POINT('Ctrl Pts',(-33.9681526807548,-90.4989699947938,
116.155904641879));
#37673=CARTESIAN_POINT('Ctrl Pts',(-37.336476078086,-91.2597458805054,115.997956118686));
#37674=CARTESIAN_POINT('Ctrl Pts',(-39.2420423334472,-89.4109239111188,
115.876513422334));
#37675=CARTESIAN_POINT('Ctrl Pts',(-39.4288592864976,-88.0832959446915,
115.807720233713));
#37676=CARTESIAN_POINT('Ctrl Pts',(-39.4264122098445,-87.7710709637358,
115.791576552823));
#37677=CARTESIAN_POINT('Origin',(-36.3549260746835,-87.7685555885722,124.208423447177));
#37678=CARTESIAN_POINT('',(-39.4252304227193,-87.7664686533939,117.791576552823));
#37679=CARTESIAN_POINT('',(-39.4294367136551,-87.7712132051017,117.708423447177));
#37680=CARTESIAN_POINT('',(-39.4284260746835,-87.768555588572,124.208423447177));
#37681=CARTESIAN_POINT('Ctrl Pts',(-39.4294367136551,-87.7712132051017,
117.708423447177));
#37682=CARTESIAN_POINT('Ctrl Pts',(-39.4221062956345,-86.9617760103423,
117.66646598275));
#37683=CARTESIAN_POINT('Ctrl Pts',(-38.680776320305,-85.1247491336954,117.571859010592));
#37684=CARTESIAN_POINT('Ctrl Pts',(-35.5900605041904,-84.2235830341421,
117.424602530703));
#37685=CARTESIAN_POINT('Ctrl Pts',(-32.9684134039925,-86.4711035918391,
117.26665400751));
#37686=CARTESIAN_POINT('Ctrl Pts',(-33.4172143461837,-89.8949844147526,
117.108705484318));
#37687=CARTESIAN_POINT('Ctrl Pts',(-36.5295491661419,-91.390896893379,116.950756961125));
#37688=CARTESIAN_POINT('Ctrl Pts',(-39.0249547704469,-89.8801809263355,
116.817329615412));
#37689=CARTESIAN_POINT('Ctrl Pts',(-39.4228110246384,-88.313219172827,116.736551777429));
#37690=CARTESIAN_POINT('Ctrl Pts',(-39.4237038206158,-87.7679979949716,
116.708423447177));
#37691=CARTESIAN_POINT('Ctrl Pts',(-39.4252304227193,-87.7664686533939,
117.791576552823));
#37692=CARTESIAN_POINT('Ctrl Pts',(-39.4275240548214,-87.4038926151218,
117.772847659816));
#37693=CARTESIAN_POINT('Ctrl Pts',(-39.2010477052606,-86.0248372386501,
117.701469259079));
#37694=CARTESIAN_POINT('Ctrl Pts',(-37.1652521728484,-84.2336975039545,
117.577441350611));
#37695=CARTESIAN_POINT('Ctrl Pts',(-33.8379852474627,-85.1576440741897,
117.419492827418));
#37696=CARTESIAN_POINT('Ctrl Pts',(-32.7927520208408,-88.4488247072137,
117.261544304226));
#37697=CARTESIAN_POINT('Ctrl Pts',(-34.9772336702029,-91.123226019824,117.103595781034));
#37698=CARTESIAN_POINT('Ctrl Pts',(-38.3827275640396,-90.7590545474582,
116.946939863899));
#37699=CARTESIAN_POINT('Ctrl Pts',(-39.4313303532814,-88.7555570337355,
116.842933454495));
#37700=CARTESIAN_POINT('Ctrl Pts',(-39.4333760082338,-87.768103846536,116.791576552823));
#37701=CARTESIAN_POINT('Origin',(-36.3549260746835,-87.7685555885722,124.208423447177));
#37702=CARTESIAN_POINT('',(-39.4262429517989,-87.7710264527958,118.791576552823));
#37703=CARTESIAN_POINT('',(-39.4315723149004,-87.7664967944779,118.708423447177));
#37704=CARTESIAN_POINT('',(-39.4284260746835,-87.768555588572,124.208423447177));
#37705=CARTESIAN_POINT('Ctrl Pts',(-39.4315723149004,-87.7664967944779,
118.708423447177));
#37706=CARTESIAN_POINT('Ctrl Pts',(-39.4325767499313,-87.6366221253453,
118.701679203533));
#37707=CARTESIAN_POINT('Ctrl Pts',(-39.3663549509798,-86.4939013295593,
118.642285452157));
#37708=CARTESIAN_POINT('Ctrl Pts',(-37.9364316789807,-84.5050161335647,
118.53024219305));
#37709=CARTESIAN_POINT('Ctrl Pts',(-34.4867512509629,-84.6602163887321,
118.372293669858));
#37710=CARTESIAN_POINT('Ctrl Pts',(-32.7308881175633,-87.6336532609701,
118.214345146665));
#37711=CARTESIAN_POINT('Ctrl Pts',(-34.2608299797916,-90.7294019705626,
118.056396623473));
#37712=CARTESIAN_POINT('Ctrl Pts',(-37.6894250821856,-91.1406413157804,
117.89844810028));
#37713=CARTESIAN_POINT('Ctrl Pts',(-39.3187092839115,-89.197430905212,117.782457041515));
#37714=CARTESIAN_POINT('Ctrl Pts',(-39.4313047280353,-87.9774825222761,
117.719115490481));
#37715=CARTESIAN_POINT('Ctrl Pts',(-39.4294367136551,-87.7712132051017,
117.708423447177));
#37716=CARTESIAN_POINT('Ctrl Pts',(-39.4262429517989,-87.7710264527958,
118.791576552823));
#37717=CARTESIAN_POINT('Ctrl Pts',(-39.4208794784184,-87.0714804470721,
118.755411372868));
#37718=CARTESIAN_POINT('Ctrl Pts',(-38.8380242352711,-85.345445065365,118.666596685182));
#37719=CARTESIAN_POINT('Ctrl Pts',(-35.980893479922,-84.1613475703659,118.525132489766));
#37720=CARTESIAN_POINT('Ctrl Pts',(-33.1299552486368,-86.109817141451,118.367183966573));
#37721=CARTESIAN_POINT('Ctrl Pts',(-33.2029999836058,-89.5622144129554,
118.209235443381));
#37722=CARTESIAN_POINT('Ctrl Pts',(-36.1338002432087,-91.3883557807084,
118.051286920188));
#37723=CARTESIAN_POINT('Ctrl Pts',(-38.893793144385,-90.1051597784844,117.912067290002));
#37724=CARTESIAN_POINT('Ctrl Pts',(-39.4210763378607,-88.4231439891081,
117.825497167547));
#37725=CARTESIAN_POINT('Ctrl Pts',(-39.4252304227193,-87.7664686533939,
117.791576552823));
#37726=CARTESIAN_POINT('Origin',(-36.3549260746835,-87.7685555885722,124.208423447177));
#37727=CARTESIAN_POINT('',(-39.4334142380496,-87.7682219888642,119.791576552823));
#37728=CARTESIAN_POINT('',(-39.4237431936346,-87.7678945631787,119.708423447177));
#37729=CARTESIAN_POINT('',(-39.4284260746835,-87.768555588572,124.208423447177));
#37730=CARTESIAN_POINT('Ctrl Pts',(-39.4237431936346,-87.7678945631786,
119.708423447177));
#37731=CARTESIAN_POINT('Ctrl Pts',(-39.4246537466801,-87.2992099811667,
119.684242916584));
#37732=CARTESIAN_POINT('Ctrl Pts',(-39.1042499609049,-85.8112150040598,
119.60741287826));
#37733=CARTESIAN_POINT('Ctrl Pts',(-36.7983710787885,-84.169221463673,119.477933332205));
#37734=CARTESIAN_POINT('Ctrl Pts',(-33.5834350118328,-85.4296055945461,
119.319984809013));
#37735=CARTESIAN_POINT('Ctrl Pts',(-32.8813255943857,-88.8106445822591,
119.16203628582));
#37736=CARTESIAN_POINT('Ctrl Pts',(-35.3286240906017,-91.2468531569549,
119.004087762628));
#37737=CARTESIAN_POINT('Ctrl Pts',(-38.5622100531239,-90.5600298609509,
118.85288348308));
#37738=CARTESIAN_POINT('Ctrl Pts',(-39.4247355430135,-88.6504997010273,
118.754328711263));
#37739=CARTESIAN_POINT('Ctrl Pts',(-39.4315723149004,-87.7664967944779,
118.708423447177));
#37740=CARTESIAN_POINT('Ctrl Pts',(-39.4334142380496,-87.7682219888642,
119.791576552823));
#37741=CARTESIAN_POINT('Ctrl Pts',(-39.4334426828812,-87.7499190193576,
119.79062459365));
#37742=CARTESIAN_POINT('Ctrl Pts',(-39.4250380396833,-86.7193701130363,
119.737023126747));
#37743=CARTESIAN_POINT('Ctrl Pts',(-38.2826268362602,-84.6967778194338,
119.630772152113));
#37744=CARTESIAN_POINT('Ctrl Pts',(-34.8365760123942,-84.4751586559665,
119.472823628921));
#37745=CARTESIAN_POINT('Ctrl Pts',(-32.7671668042656,-87.2395625351253,
119.314875105728));
#37746=CARTESIAN_POINT('Ctrl Pts',(-33.9506699106112,-90.4835882261257,
119.156926582536));
#37747=CARTESIAN_POINT('Ctrl Pts',(-37.3140389097867,-91.26597644781,118.998978059343));
#37748=CARTESIAN_POINT('Ctrl Pts',(-39.2368154766846,-89.424276702295,118.877194716105));
#37749=CARTESIAN_POINT('Ctrl Pts',(-39.4286876583739,-88.0898841404161,
118.808060880599));
#37750=CARTESIAN_POINT('Ctrl Pts',(-39.4262429517989,-87.7710264527958,
118.791576552823));
#37751=CARTESIAN_POINT('Origin',(-36.3549260746835,-87.7685555885722,124.208423447177));
#37752=CARTESIAN_POINT('',(-39.4253676065904,-87.7664047027925,120.791576552823));
#37753=CARTESIAN_POINT('',(-39.4292404520863,-87.7712393069318,120.708423447177));
#37754=CARTESIAN_POINT('',(-39.4284260746835,-87.768555588572,124.208423447177));
#37755=CARTESIAN_POINT('Ctrl Pts',(-39.4292404520863,-87.7712393069318,
120.708423447177));
#37756=CARTESIAN_POINT('Ctrl Pts',(-39.4219533239201,-86.9682420907583,
120.666806629636));
#37757=CARTESIAN_POINT('Ctrl Pts',(-38.6905685426978,-85.137604773249,120.572540304363));
#37758=CARTESIAN_POINT('Ctrl Pts',(-35.6128382743126,-84.2187463335991,
120.42562447136));
#37759=CARTESIAN_POINT('Ctrl Pts',(-32.976814280225,-86.4493848551693,120.267675948167));
#37760=CARTESIAN_POINT('Ctrl Pts',(-33.4036210489072,-89.8760778724798,
120.109727424975));
#37761=CARTESIAN_POINT('Ctrl Pts',(-36.5062865485562,-91.3919433106791,
119.951778901783));
#37762=CARTESIAN_POINT('Ctrl Pts',(-39.0177365106944,-89.8934657391649,
119.818010909183));
#37763=CARTESIAN_POINT('Ctrl Pts',(-39.4226711528978,-88.3197009265046,
119.736892424315));
#37764=CARTESIAN_POINT('Ctrl Pts',(-39.4237431936346,-87.7678945631786,
119.708423447177));
#37765=CARTESIAN_POINT('Ctrl Pts',(-39.4253676065904,-87.7664047027925,
120.791576552823));
#37766=CARTESIAN_POINT('Ctrl Pts',(-39.4277029355786,-87.4104612245052,
120.773188306702));
#37767=CARTESIAN_POINT('Ctrl Pts',(-39.2066381265416,-86.0381804949055,
120.70215055285));
#37768=CARTESIAN_POINT('Ctrl Pts',(-37.1879239172525,-84.2389823785756,
120.578463291268));
#37769=CARTESIAN_POINT('Ctrl Pts',(-33.8548061047563,-85.1415322964398,
120.420514768075));
#37770=CARTESIAN_POINT('Ctrl Pts',(-32.7884553507106,-88.4259400742007,
120.262566244883));
#37771=CARTESIAN_POINT('Ctrl Pts',(-34.9557227571499,-91.1143096798933,
120.10461772169));
#37772=CARTESIAN_POINT('Ctrl Pts',(-38.3708934336136,-90.771269574952,119.94762115767));
#37773=CARTESIAN_POINT('Ctrl Pts',(-39.4318694994647,-88.7621917748598,
119.843274101381));
#37774=CARTESIAN_POINT('Ctrl Pts',(-39.4334142380496,-87.7682219888642,
119.791576552823));
#37775=CARTESIAN_POINT('Origin',(-36.3549260746835,-87.7685555885722,124.208423447177));
#37776=CARTESIAN_POINT('',(-39.4252046443693,-87.771569957437,121.791576552823));
#37777=CARTESIAN_POINT('',(-39.4317256223809,-87.7666280037969,121.708423447177));
#37778=CARTESIAN_POINT('',(-39.4284260746835,-87.768555588572,124.208423447177));
#37779=CARTESIAN_POINT('',(-37.1487253572165,-90.7377785423179,122.));
#37780=CARTESIAN_POINT('Ctrl Pts',(-37.1487253572165,-90.7377785423179,
122.));
#37781=CARTESIAN_POINT('Ctrl Pts',(-38.1309639469881,-90.4751844899402,
121.947350492269));
#37782=CARTESIAN_POINT('Ctrl Pts',(-39.2306604626821,-89.4374467038025,
121.877876009877));
#37783=CARTESIAN_POINT('Ctrl Pts',(-39.427545797006,-88.0970456694337,121.808401527484));
#37784=CARTESIAN_POINT('Ctrl Pts',(-39.4252046443693,-87.771569957437,121.791576552823));
#37785=CARTESIAN_POINT('',(-35.5592173021306,-90.7428549624115,122.));
#37786=CARTESIAN_POINT('Origin',(-36.3549260746835,-87.7685555885722,122.));
#37787=CARTESIAN_POINT('Ctrl Pts',(-35.5592126670536,-90.7428672848631,
122.));
#37788=CARTESIAN_POINT('Ctrl Pts',(-36.5061789753531,-90.9937479094032,
121.949053726697));
#37789=CARTESIAN_POINT('Ctrl Pts',(-38.5667278271917,-90.5388459125472,
121.851861542423));
#37790=CARTESIAN_POINT('Ctrl Pts',(-39.4250621347381,-88.6569026988886,
121.754669358149));
#37791=CARTESIAN_POINT('Ctrl Pts',(-39.4317256223809,-87.7666280037969,
121.708423447177));
#37792=CARTESIAN_POINT('Origin',(-87.7685555885722,-36.3549260746835,114.));
#37793=CARTESIAN_POINT('',(-90.2820658539789,-36.3546686125247,107.387416697508));
#37794=CARTESIAN_POINT('',(-90.2841457375043,-36.3584993178544,107.112583302492));
#37795=CARTESIAN_POINT('',(-90.2860555885722,-36.3549260746835,114.));
#37796=CARTESIAN_POINT('',(-89.6820215852369,-34.7189388713081,107.));
#37797=CARTESIAN_POINT('Ctrl Pts',(-90.2841457375043,-36.3584993178544,
107.112583302492));
#37798=CARTESIAN_POINT('Ctrl Pts',(-90.2790005338084,-35.7658644382975,
107.075055534995));
#37799=CARTESIAN_POINT('Ctrl Pts',(-90.0677774166561,-35.1701225143786,
107.037527767497));
#37800=CARTESIAN_POINT('Ctrl Pts',(-89.6820215852368,-34.718938871308,107.));
#37801=CARTESIAN_POINT('',(-90.2860555885722,-36.3549260746835,107.));
#37802=CARTESIAN_POINT('Origin',(-87.7685555885722,-36.3549260746835,107.));
#37803=CARTESIAN_POINT('',(-90.2860555885722,-36.3549260746835,106.));
#37804=CARTESIAN_POINT('',(-90.2860555885722,-36.3549260746835,114.));
#37805=CARTESIAN_POINT('Origin',(-87.7685555885722,-36.3549260746835,106.));
#37806=CARTESIAN_POINT('',(-85.8514453318972,-34.7163981307897,107.));
#37807=CARTESIAN_POINT('Origin',(-87.7685555885722,-36.3549260746835,107.));
#37808=CARTESIAN_POINT('Ctrl Pts',(-85.8514364858568,-34.7163919634214,
107.));
#37809=CARTESIAN_POINT('Ctrl Pts',(-86.3742570429706,-34.1076768998287,
107.050946273303));
#37810=CARTESIAN_POINT('Ctrl Pts',(-87.2139815516724,-33.767500538132,107.101892546605));
#37811=CARTESIAN_POINT('Ctrl Pts',(-88.012652412444,-33.8452633218798,107.152838819908));
#37812=CARTESIAN_POINT('Ctrl Pts',(-88.8380244157852,-33.9256258689062,
107.205488327639));
#37813=CARTESIAN_POINT('Ctrl Pts',(-89.6195518767751,-34.4523397509922,
107.25813783537));
#37814=CARTESIAN_POINT('Ctrl Pts',(-90.0034364925517,-35.1871265187104,
107.3107873431));
#37815=CARTESIAN_POINT('Ctrl Pts',(-90.1896796411383,-35.543611242337,107.336330461236));
#37816=CARTESIAN_POINT('Ctrl Pts',(-90.2823278504789,-35.9490709929857,
107.361873579372));
#37817=CARTESIAN_POINT('Ctrl Pts',(-90.2820658539789,-36.3546686125247,
107.387416697508));
#37818=CARTESIAN_POINT('Origin',(-87.7685555885722,-36.3549260746835,114.));
#37819=CARTESIAN_POINT('',(-90.2873603706715,-36.3570215567213,108.387416697508));
#37820=CARTESIAN_POINT('',(-90.2899626929787,-36.35425976501,108.112583302492));
#37821=CARTESIAN_POINT('',(-90.2860555885722,-36.3549260746835,114.));
#37822=CARTESIAN_POINT('Ctrl Pts',(-90.2899626929787,-36.35425976501,108.112583302492));
#37823=CARTESIAN_POINT('Ctrl Pts',(-90.2900905289486,-36.3178026272376,
108.110268755777));
#37824=CARTESIAN_POINT('Ctrl Pts',(-90.289367578041,-36.2813507261708,108.107954209062));
#37825=CARTESIAN_POINT('Ctrl Pts',(-90.2877779615632,-36.2449367233117,
108.105639662347));
#37826=CARTESIAN_POINT('Ctrl Pts',(-90.2516186028016,-35.4166193198727,
108.052990154616));
#37827=CARTESIAN_POINT('Ctrl Pts',(-89.7670151876795,-34.6079118173993,
108.000340646886));
#37828=CARTESIAN_POINT('Ctrl Pts',(-89.0536407575369,-34.1853501417969,
107.947691139155));
#37829=CARTESIAN_POINT('Ctrl Pts',(-88.3402663273943,-33.7627884661946,
107.895041631424));
#37830=CARTESIAN_POINT('Ctrl Pts',(-87.3981208822312,-33.7263726174632,
107.842392123693));
#37831=CARTESIAN_POINT('Ctrl Pts',(-86.6543416473799,-34.0927743114382,
107.789742615962));
#37832=CARTESIAN_POINT('Ctrl Pts',(-85.9105624125286,-34.4591760054132,
107.737093108232));
#37833=CARTESIAN_POINT('Ctrl Pts',(-85.3651493879892,-35.2283952420945,
107.684443600501));
#37834=CARTESIAN_POINT('Ctrl Pts',(-85.2652957176433,-36.0513826441264,
107.63179409277));
#37835=CARTESIAN_POINT('Ctrl Pts',(-85.1654420472974,-36.8743700461582,
107.579144585039));
#37836=CARTESIAN_POINT('Ctrl Pts',(-85.5111477311451,-37.7511256135406,
107.526495077308));
#37837=CARTESIAN_POINT('Ctrl Pts',(-86.1458177411936,-38.284877504064,107.473845569577));
#37838=CARTESIAN_POINT('Ctrl Pts',(-86.7804877512421,-38.8186293945873,
107.421196061847));
#37839=CARTESIAN_POINT('Ctrl Pts',(-87.7041220874913,-39.0093776082516,
107.368546554116));
#37840=CARTESIAN_POINT('Ctrl Pts',(-88.4977390365037,-38.7692237409335,
107.315897046385));
#37841=CARTESIAN_POINT('Ctrl Pts',(-89.291355985516,-38.5290698736153,107.263247538654));
#37842=CARTESIAN_POINT('Ctrl Pts',(-89.9549555472913,-37.8580139253148,
107.210598030923));
#37843=CARTESIAN_POINT('Ctrl Pts',(-90.187920793802,-37.0637279762933,107.157948523192));
#37844=CARTESIAN_POINT('Ctrl Pts',(-90.2548319596038,-36.8355969583622,
107.142826782959));
#37845=CARTESIAN_POINT('Ctrl Pts',(-90.2862189872318,-36.597300379031,107.127705042726));
#37846=CARTESIAN_POINT('Ctrl Pts',(-90.2841457375043,-36.3584993178544,
107.112583302492));
#37847=CARTESIAN_POINT('Ctrl Pts',(-90.2820658539789,-36.3546686125247,
107.387416697508));
#37848=CARTESIAN_POINT('Ctrl Pts',(-90.2817878229584,-36.7850893244963,
107.414523087103));
#37849=CARTESIAN_POINT('Ctrl Pts',(-90.1768791354039,-37.2156652972639,
107.441629476698));
#37850=CARTESIAN_POINT('Ctrl Pts',(-89.968158095568,-37.5880327152623,107.468735866293));
#37851=CARTESIAN_POINT('Ctrl Pts',(-89.5627533122445,-38.3112924907458,
107.521385374024));
#37852=CARTESIAN_POINT('Ctrl Pts',(-88.7657019750341,-38.8149523883624,
107.574034881755));
#37853=CARTESIAN_POINT('Ctrl Pts',(-87.9384522552337,-38.8708033725724,
107.626684389485));
#37854=CARTESIAN_POINT('Ctrl Pts',(-87.1112025354333,-38.9266543567824,
107.679333897216));
#37855=CARTESIAN_POINT('Ctrl Pts',(-86.2537544330426,-38.5346964275858,
107.731983404947));
#37856=CARTESIAN_POINT('Ctrl Pts',(-85.754762083387,-37.8725606130825,107.784632912678));
#37857=CARTESIAN_POINT('Ctrl Pts',(-85.2557697337313,-37.2104247985793,
107.837282420409));
#37858=CARTESIAN_POINT('Ctrl Pts',(-85.1152331368106,-36.2781110987695,
107.889931928139));
#37859=CARTESIAN_POINT('Ctrl Pts',(-85.396890099688,-35.4982975349368,107.94258143587));
#37860=CARTESIAN_POINT('Ctrl Pts',(-85.6785470625655,-34.7184839711041,
107.995230943601));
#37861=CARTESIAN_POINT('Ctrl Pts',(-86.3823975852411,-34.0911705432485,
108.047880451332));
#37862=CARTESIAN_POINT('Ctrl Pts',(-87.1893482785224,-33.900726745334,108.100529959063));
#37863=CARTESIAN_POINT('Ctrl Pts',(-87.9962989718038,-33.7102829474194,
108.153179466794));
#37864=CARTESIAN_POINT('Ctrl Pts',(-88.9063498356909,-33.9567087794459,
108.205828974524));
#37865=CARTESIAN_POINT('Ctrl Pts',(-89.5069496938256,-34.5282974064535,
108.258478482255));
#37866=CARTESIAN_POINT('Ctrl Pts',(-89.9972377460577,-34.9949027025053,
108.301457887339));
#37867=CARTESIAN_POINT('Ctrl Pts',(-90.2813089864897,-35.6781950787427,
108.344437292424));
#37868=CARTESIAN_POINT('Ctrl Pts',(-90.2873603706715,-36.3570215567213,
108.387416697508));
#37869=CARTESIAN_POINT('Origin',(-87.7685555885722,-36.3549260746835,114.));
#37870=CARTESIAN_POINT('',(-90.2882105526124,-36.3530683167515,109.387416697508));
#37871=CARTESIAN_POINT('',(-90.2831164663313,-36.3533981324289,109.112583302492));
#37872=CARTESIAN_POINT('',(-90.2860555885722,-36.3549260746835,114.));
#37873=CARTESIAN_POINT('Ctrl Pts',(-90.2831164663313,-36.3533981324289,
109.112583302492));
#37874=CARTESIAN_POINT('Ctrl Pts',(-90.2848727217426,-36.0401068000473,
109.092832468829));
#37875=CARTESIAN_POINT('Ctrl Pts',(-90.2305755265925,-35.7274022874004,
109.073081635165));
#37876=CARTESIAN_POINT('Ctrl Pts',(-90.1174359487622,-35.4376760917933,
109.053330801502));
#37877=CARTESIAN_POINT('Ctrl Pts',(-89.8158414348707,-34.665357219817,109.000681293771));
#37878=CARTESIAN_POINT('Ctrl Pts',(-89.0961201091845,-34.0563194728835,
108.94803178604));
#37879=CARTESIAN_POINT('Ctrl Pts',(-88.2845464977982,-33.8866598038377,
108.89538227831));
#37880=CARTESIAN_POINT('Ctrl Pts',(-87.4729728864118,-33.7170001347919,
108.842732770579));
#37881=CARTESIAN_POINT('Ctrl Pts',(-86.5695469893253,-33.9867185436337,
108.790083262848));
#37882=CARTESIAN_POINT('Ctrl Pts',(-85.983823594119,-34.5735444470518,108.737433755117));
#37883=CARTESIAN_POINT('Ctrl Pts',(-85.3981001989128,-35.1603703504699,
108.684784247386));
#37884=CARTESIAN_POINT('Ctrl Pts',(-85.1300793055867,-36.0643037484642,
108.632134739655));
#37885=CARTESIAN_POINT('Ctrl Pts',(-85.301263297264,-36.8755557473365,108.579485231925));
#37886=CARTESIAN_POINT('Ctrl Pts',(-85.4724472889414,-37.6868077462088,
108.526835724194));
#37887=CARTESIAN_POINT('Ctrl Pts',(-86.0828361656222,-38.4053783459591,
108.474186216463));
#37888=CARTESIAN_POINT('Ctrl Pts',(-86.8557210844333,-38.7055236108094,
108.421536708732));
#37889=CARTESIAN_POINT('Ctrl Pts',(-87.6286060032443,-39.0056688756597,
108.368887201001));
#37890=CARTESIAN_POINT('Ctrl Pts',(-88.5639869641856,-38.88738880561,108.316237693271));
#37891=CARTESIAN_POINT('Ctrl Pts',(-89.2378197934557,-38.4042851183828,
108.26358818554));
#37892=CARTESIAN_POINT('Ctrl Pts',(-89.8820299799204,-37.9424193515166,
108.213253224524));
#37893=CARTESIAN_POINT('Ctrl Pts',(-90.2871826157732,-37.1471012301236,
108.162918263508));
#37894=CARTESIAN_POINT('Ctrl Pts',(-90.2899626929787,-36.35425976501,108.112583302492));
#37895=CARTESIAN_POINT('Ctrl Pts',(-90.2873603706715,-36.3570215567213,
108.387416697508));
#37896=CARTESIAN_POINT('Ctrl Pts',(-90.2887218950127,-36.5097533525287,
108.397086800155));
#37897=CARTESIAN_POINT('Ctrl Pts',(-90.2760094311365,-36.6622590745572,
108.406756902801));
#37898=CARTESIAN_POINT('Ctrl Pts',(-90.2484051643446,-36.8120198580747,
108.416427005448));
#37899=CARTESIAN_POINT('Ctrl Pts',(-90.0981119243468,-37.6274022606995,
108.469076513179));
#37900=CARTESIAN_POINT('Ctrl Pts',(-89.5063765919689,-38.3614156439603,
108.521726020909));
#37901=CARTESIAN_POINT('Ctrl Pts',(-88.7414549288688,-38.6813077555619,
108.57437552864));
#37902=CARTESIAN_POINT('Ctrl Pts',(-87.9765332657687,-39.0011998671635,
108.627025036371));
#37903=CARTESIAN_POINT('Ctrl Pts',(-87.0384252719463,-38.9069707071058,
108.679674544102));
#37904=CARTESIAN_POINT('Ctrl Pts',(-86.3524071884949,-38.4413368770482,
108.732324051833));
#37905=CARTESIAN_POINT('Ctrl Pts',(-85.6663891050434,-37.9757030469905,
108.784973559563));
#37906=CARTESIAN_POINT('Ctrl Pts',(-85.2324609319629,-37.1386645469329,
108.837623067294));
#37907=CARTESIAN_POINT('Ctrl Pts',(-85.2473377736386,-36.3096804193602,
108.890272575025));
#37908=CARTESIAN_POINT('Ctrl Pts',(-85.2622146153143,-35.4806962917874,
108.942922082756));
#37909=CARTESIAN_POINT('Ctrl Pts',(-85.7258964717462,-34.6597665366996,
108.995571590487));
#37910=CARTESIAN_POINT('Ctrl Pts',(-86.4281800465863,-34.2190469963083,
109.048221098218));
#37911=CARTESIAN_POINT('Ctrl Pts',(-87.1304636214265,-33.778327455917,109.100870605948));
#37912=CARTESIAN_POINT('Ctrl Pts',(-88.0713489146749,-33.7178181302223,
109.153520113679));
#37913=CARTESIAN_POINT('Ctrl Pts',(-88.8242999729847,-34.0649500886831,
109.20616962141));
#37914=CARTESIAN_POINT('Ctrl Pts',(-89.5772510312945,-34.4120820471438,
109.258819129141));
#37915=CARTESIAN_POINT('Ctrl Pts',(-90.1422678546657,-35.16685528976,109.311468636872));
#37916=CARTESIAN_POINT('Ctrl Pts',(-90.2632086162776,-35.987104802477,109.364118144603));
#37917=CARTESIAN_POINT('Ctrl Pts',(-90.2810482559013,-36.1080975555683,
109.371884328904));
#37918=CARTESIAN_POINT('Ctrl Pts',(-90.2892255154112,-36.2305149668762,
109.379650513206));
#37919=CARTESIAN_POINT('Ctrl Pts',(-90.2882105526124,-36.3530683167515,
109.387416697508));
#37920=CARTESIAN_POINT('Origin',(-87.7685555885722,-36.3549260746835,114.));
#37921=CARTESIAN_POINT('',(-90.2821396611156,-36.3546406872729,110.387416697508));
#37922=CARTESIAN_POINT('',(-90.2846917996912,-36.3570497197296,110.112583302492));
#37923=CARTESIAN_POINT('',(-90.2860555885722,-36.3549260746835,114.));
#37924=CARTESIAN_POINT('Ctrl Pts',(-90.2846917996912,-36.3570497197296,
110.112583302492));
#37925=CARTESIAN_POINT('Ctrl Pts',(-90.2798923348767,-35.7681126342544,
110.07539618188));
#37926=CARTESIAN_POINT('Ctrl Pts',(-90.0733338262189,-35.1761419702344,
110.038209061269));
#37927=CARTESIAN_POINT('Ctrl Pts',(-89.6956382757642,-34.728599334682,110.001021940657));
#37928=CARTESIAN_POINT('Ctrl Pts',(-89.1608970945044,-34.0949686834569,
109.948372432926));
#37929=CARTESIAN_POINT('Ctrl Pts',(-88.2831137156981,-33.7508423251229,
109.895722925195));
#37930=CARTESIAN_POINT('Ctrl Pts',(-87.4602178832996,-33.8522246973141,
109.843073417464));
#37931=CARTESIAN_POINT('Ctrl Pts',(-86.6373220509011,-33.9536070695053,
109.790423909734));
#37932=CARTESIAN_POINT('Ctrl Pts',(-85.8693137649103,-34.5004981722218,
109.737774402003));
#37933=CARTESIAN_POINT('Ctrl Pts',(-85.5043579080477,-35.2449732690051,
109.685124894272));
#37934=CARTESIAN_POINT('Ctrl Pts',(-85.139402051185,-35.9894483657884,109.632475386541));
#37935=CARTESIAN_POINT('Ctrl Pts',(-85.1774986234505,-36.9315074566384,
109.57982587881));
#37936=CARTESIAN_POINT('Ctrl Pts',(-85.60137711239,-37.6440823198458,109.52717637108));
#37937=CARTESIAN_POINT('Ctrl Pts',(-86.0252556013295,-38.3566571830533,
109.474526863349));
#37938=CARTESIAN_POINT('Ctrl Pts',(-86.834916006943,-38.8397478186181,109.421877355618));
#37939=CARTESIAN_POINT('Ctrl Pts',(-87.6633111187983,-38.8743525536714,
109.369227847887));
#37940=CARTESIAN_POINT('Ctrl Pts',(-88.4917062306535,-38.9089572887246,
109.316578340156));
#37941=CARTESIAN_POINT('Ctrl Pts',(-89.3388360487506,-38.4950761232663,
109.263928832425));
#37942=CARTESIAN_POINT('Ctrl Pts',(-89.8206671067506,-37.8203355420275,
109.211279324695));
#37943=CARTESIAN_POINT('Ctrl Pts',(-90.1217450012257,-37.3987158266868,
109.178380650627));
#37944=CARTESIAN_POINT('Ctrl Pts',(-90.280191097441,-36.8752429116366,109.14548197656));
#37945=CARTESIAN_POINT('Ctrl Pts',(-90.2831164663313,-36.3533981324289,
109.112583302492));
#37946=CARTESIAN_POINT('Ctrl Pts',(-90.2882105526124,-36.3530683167515,
109.387416697508));
#37947=CARTESIAN_POINT('Ctrl Pts',(-90.2823447500771,-37.061344276473,109.432300020937));
#37948=CARTESIAN_POINT('Ctrl Pts',(-89.9694529522308,-37.7741606696804,
109.477183344366));
#37949=CARTESIAN_POINT('Ctrl Pts',(-89.440291210746,-38.2427518568799,109.522066667795));
#37950=CARTESIAN_POINT('Ctrl Pts',(-88.8195683437496,-38.792423615748,109.574716175526));
#37951=CARTESIAN_POINT('Ctrl Pts',(-87.9012579099043,-39.0060413506665,
109.627365683257));
#37952=CARTESIAN_POINT('Ctrl Pts',(-87.1016619698773,-38.7867646999753,
109.680015190987));
#37953=CARTESIAN_POINT('Ctrl Pts',(-86.3020660298503,-38.5674880492842,
109.732664698718));
#37954=CARTESIAN_POINT('Ctrl Pts',(-85.6211845836416,-37.9153170129834,
109.785314206449));
#37955=CARTESIAN_POINT('Ctrl Pts',(-85.3676848856873,-37.1259034177897,
109.83796371418));
#37956=CARTESIAN_POINT('Ctrl Pts',(-85.1141851877331,-36.336489822596,109.890613221911));
#37957=CARTESIAN_POINT('Ctrl Pts',(-85.2880672380334,-35.4098336685093,
109.943262729642));
#37958=CARTESIAN_POINT('Ctrl Pts',(-85.8105042509258,-34.7660204291389,
109.995912237372));
#37959=CARTESIAN_POINT('Ctrl Pts',(-86.3329412638183,-34.1222071897685,
110.048561745103));
#37960=CARTESIAN_POINT('Ctrl Pts',(-87.203933239303,-33.7612368651145,110.101211252834));
#37961=CARTESIAN_POINT('Ctrl Pts',(-88.0286292114484,-33.8467498637978,
110.153860760565));
#37962=CARTESIAN_POINT('Ctrl Pts',(-88.8533251835939,-33.9322628624812,
110.206510268296));
#37963=CARTESIAN_POINT('Ctrl Pts',(-89.6317251524002,-34.464259184502,110.259159776027));
#37964=CARTESIAN_POINT('Ctrl Pts',(-90.0109533284357,-35.2015663866826,
110.311809283757));
#37965=CARTESIAN_POINT('Ctrl Pts',(-90.1924837475362,-35.5545034675106,
110.337011755008));
#37966=CARTESIAN_POINT('Ctrl Pts',(-90.2825486333846,-35.9544851278314,
110.362214226258));
#37967=CARTESIAN_POINT('Ctrl Pts',(-90.2821396611156,-36.3546406872729,
110.387416697508));
#37968=CARTESIAN_POINT('Origin',(-87.7685555885722,-36.3549260746835,114.));
#37969=CARTESIAN_POINT('',(-90.2872023475779,-36.3570522860146,111.387416697508));
#37970=CARTESIAN_POINT('',(-90.2900214942874,-36.3543651501874,111.112583302492));
#37971=CARTESIAN_POINT('',(-90.2860555885722,-36.3549260746835,114.));
#37972=CARTESIAN_POINT('Ctrl Pts',(-90.2900214942874,-36.3543651501874,
111.112583302492));
#37973=CARTESIAN_POINT('Ctrl Pts',(-90.2901162181278,-36.323275200018,111.110609402663));
#37974=CARTESIAN_POINT('Ctrl Pts',(-90.2895904165067,-36.2921885273613,
111.108635502833));
#37975=CARTESIAN_POINT('Ctrl Pts',(-90.2884341100943,-36.261125324813,111.106661603004));
#37976=CARTESIAN_POINT('Ctrl Pts',(-90.2575921380264,-35.4325815970888,
111.054012095273));
#37977=CARTESIAN_POINT('Ctrl Pts',(-89.7781837013239,-34.6207354483563,
111.001362587542));
#37978=CARTESIAN_POINT('Ctrl Pts',(-89.0675413245081,-34.19362498464,110.948713079812));
#37979=CARTESIAN_POINT('Ctrl Pts',(-88.3568989476923,-33.7665145209237,
110.896063572081));
#37980=CARTESIAN_POINT('Ctrl Pts',(-87.4150226307631,-33.7241397422238,
110.84341406435));
#37981=CARTESIAN_POINT('Ctrl Pts',(-86.6688976790302,-34.0857106098954,
110.790764556619));
#37982=CARTESIAN_POINT('Ctrl Pts',(-85.9227727272973,-34.447281477567,110.738115048888));
#37983=CARTESIAN_POINT('Ctrl Pts',(-85.3723991407606,-35.2127979916102,
110.685465541158));
#37984=CARTESIAN_POINT('Ctrl Pts',(-85.2672804155176,-36.0352248818261,
110.632816033427));
#37985=CARTESIAN_POINT('Ctrl Pts',(-85.1621616902746,-36.857651772042,110.580166525696));
#37986=CARTESIAN_POINT('Ctrl Pts',(-85.5022978263254,-37.7369890384306,
110.527517017965));
#37987=CARTESIAN_POINT('Ctrl Pts',(-86.1334932786358,-38.2746025024174,
110.474867510234));
#37988=CARTESIAN_POINT('Ctrl Pts',(-86.7646887309461,-38.8122159664043,
110.422218002503));
#37989=CARTESIAN_POINT('Ctrl Pts',(-87.686943499516,-39.0081056279894,110.369568494773));
#37990=CARTESIAN_POINT('Ctrl Pts',(-88.4821674098618,-38.7734678895427,
110.316918987042));
#37991=CARTESIAN_POINT('Ctrl Pts',(-89.2773913202076,-38.5388301510961,
110.264269479311));
#37992=CARTESIAN_POINT('Ctrl Pts',(-89.9455843723293,-37.8736650126178,
110.21161997158));
#37993=CARTESIAN_POINT('Ctrl Pts',(-90.1838314065334,-37.0795149713205,
110.158970463849));
#37994=CARTESIAN_POINT('Ctrl Pts',(-90.2538010611725,-36.8462847684481,
110.14350807673));
#37995=CARTESIAN_POINT('Ctrl Pts',(-90.2866874148855,-36.6019294806421,
110.128045689611));
#37996=CARTESIAN_POINT('Ctrl Pts',(-90.2846917996912,-36.3570497197296,
110.112583302492));
#37997=CARTESIAN_POINT('Ctrl Pts',(-90.2821396611156,-36.3546406872729,
110.387416697508));
#37998=CARTESIAN_POINT('Ctrl Pts',(-90.2816942652385,-36.7904346270357,
110.414863733989));
#37999=CARTESIAN_POINT('Ctrl Pts',(-90.1739419384852,-37.2264348206415,
110.442310770469));
#38000=CARTESIAN_POINT('Ctrl Pts',(-89.9601636138683,-37.6020990605625,
110.46975780695));
#38001=CARTESIAN_POINT('Ctrl Pts',(-89.5500893400006,-38.3227064499215,
110.522407314681));
#38002=CARTESIAN_POINT('Ctrl Pts',(-88.7498844090003,-38.8213031462991,
110.575056822411));
#38003=CARTESIAN_POINT('Ctrl Pts',(-87.9223095576387,-38.8718579193271,
110.627706330142));
#38004=CARTESIAN_POINT('Ctrl Pts',(-87.0947347062772,-38.9224126923551,
110.680355837873));
#38005=CARTESIAN_POINT('Ctrl Pts',(-86.2397899345544,-38.5249255420335,
110.733005345604));
#38006=CARTESIAN_POINT('Ctrl Pts',(-85.7450514538097,-37.8595912235122,
110.785654853335));
#38007=CARTESIAN_POINT('Ctrl Pts',(-85.250312973065,-37.1942569049909,110.838304361066));
#38008=CARTESIAN_POINT('Ctrl Pts',(-85.1157807832985,-36.2610754182697,
110.890953868796));
#38009=CARTESIAN_POINT('Ctrl Pts',(-85.402443006904,-35.4830903996067,110.943603376527));
#38010=CARTESIAN_POINT('Ctrl Pts',(-85.6891052305094,-34.7051053809437,
110.996252884258));
#38011=CARTESIAN_POINT('Ctrl Pts',(-86.3969618674869,-34.0823168303388,
111.048902391989));
#38012=CARTESIAN_POINT('Ctrl Pts',(-87.2051168757209,-33.8970564665951,
111.10155189972));
#38013=CARTESIAN_POINT('Ctrl Pts',(-88.0132718839549,-33.7117961028514,
111.154201407451));
#38014=CARTESIAN_POINT('Ctrl Pts',(-88.9217252634454,-33.964063925969,111.206850915181));
#38015=CARTESIAN_POINT('Ctrl Pts',(-89.5186434892735,-34.5394981545195,
111.259500422912));
#38016=CARTESIAN_POINT('Ctrl Pts',(-90.0020639995955,-35.0055196234347,
111.302139181111));
#38017=CARTESIAN_POINT('Ctrl Pts',(-90.2811566785782,-35.6834975602078,
111.344777939309));
#38018=CARTESIAN_POINT('Ctrl Pts',(-90.2872023475779,-36.3570522860146,
111.387416697508));
#38019=CARTESIAN_POINT('Origin',(-87.7685555885722,-36.3549260746835,114.));
#38020=CARTESIAN_POINT('',(-90.2883545352501,-36.3531221775569,112.387416697508));
#38021=CARTESIAN_POINT('',(-90.2832193840218,-36.3533353394049,112.112583302492));
#38022=CARTESIAN_POINT('',(-90.2860555885722,-36.3549260746835,114.));
#38023=CARTESIAN_POINT('Ctrl Pts',(-90.2832193840218,-36.3533353394049,
112.112583302492));
#38024=CARTESIAN_POINT('Ctrl Pts',(-90.285021136811,-36.0454791015047,112.093173115714));
#38025=CARTESIAN_POINT('Ctrl Pts',(-90.2326349187801,-35.7382146453077,
112.073762928937));
#38026=CARTESIAN_POINT('Ctrl Pts',(-90.1232772119999,-35.4527772953472,
112.054352742159));
#38027=CARTESIAN_POINT('Ctrl Pts',(-89.8266479474545,-34.6785376584215,
112.001703234428));
#38028=CARTESIAN_POINT('Ctrl Pts',(-89.1108519870612,-34.0648905600084,
111.949053726697));
#38029=CARTESIAN_POINT('Ctrl Pts',(-88.3003845444894,-33.8900235805582,
111.896404218967));
#38030=CARTESIAN_POINT('Ctrl Pts',(-87.4899171019176,-33.7151566011079,
111.843754711236));
#38031=CARTESIAN_POINT('Ctrl Pts',(-86.5847781771673,-33.9790697406205,
111.791105203505));
#38032=CARTESIAN_POINT('Ctrl Pts',(-85.9952987374956,-34.5621219905731,
111.738455695774));
#38033=CARTESIAN_POINT('Ctrl Pts',(-85.4058192978239,-35.1451742405258,
111.685806188043));
#38034=CARTESIAN_POINT('Ctrl Pts',(-85.1319993432308,-36.0473656009185,
111.633156680312));
#38035=CARTESIAN_POINT('Ctrl Pts',(-85.2979709862033,-36.8597013379772,
111.580507172582));
#38036=CARTESIAN_POINT('Ctrl Pts',(-85.4639426291757,-37.6720370750359,
111.527857664851));
#38037=CARTESIAN_POINT('Ctrl Pts',(-86.0697058697138,-38.3945171887604,
111.47520815712));
#38038=CARTESIAN_POINT('Ctrl Pts',(-86.8406471544457,-38.6996163062034,
111.422558649389));
#38039=CARTESIAN_POINT('Ctrl Pts',(-87.6115884391776,-39.0047154236463,
111.369909141658));
#38040=CARTESIAN_POINT('Ctrl Pts',(-88.5477077681033,-38.8924335448076,
111.317259633927));
#38041=CARTESIAN_POINT('Ctrl Pts',(-89.2246296788495,-38.4136719520304,
111.264610126197));
#38042=CARTESIAN_POINT('Ctrl Pts',(-89.8761728899335,-37.9528597659424,
111.213934518295));
#38043=CARTESIAN_POINT('Ctrl Pts',(-90.2875896646038,-37.1525323626734,
111.163258910394));
#38044=CARTESIAN_POINT('Ctrl Pts',(-90.2900214942874,-36.3543651501874,
111.112583302492));
#38045=CARTESIAN_POINT('Ctrl Pts',(-90.2872023475779,-36.3570522860146,
111.387416697508));
#38046=CARTESIAN_POINT('Ctrl Pts',(-90.2886217528483,-36.5151898102095,
111.39742744704));
#38047=CARTESIAN_POINT('Ctrl Pts',(-90.274990291039,-36.6730835186588,111.407438196572));
#38048=CARTESIAN_POINT('Ctrl Pts',(-90.2454186297744,-36.8279331239087,
111.417448946105));
#38049=CARTESIAN_POINT('Ctrl Pts',(-90.0898924722816,-37.6423332307638,
111.470098453835));
#38050=CARTESIAN_POINT('Ctrl Pts',(-89.4934570851304,-38.3725328104906,
111.522747961566));
#38051=CARTESIAN_POINT('Ctrl Pts',(-88.7264973812031,-38.6875069876263,
111.575397469297));
#38052=CARTESIAN_POINT('Ctrl Pts',(-87.9595376772757,-39.0024811647619,
111.628046977028));
#38053=CARTESIAN_POINT('Ctrl Pts',(-87.0220536565721,-38.9022299393065,
111.680696484759));
#38054=CARTESIAN_POINT('Ctrl Pts',(-86.3390394437353,-38.4322006798194,
111.73334599249));
#38055=CARTESIAN_POINT('Ctrl Pts',(-85.6560252308984,-37.9621714203324,
111.78599550022));
#38056=CARTESIAN_POINT('Ctrl Pts',(-85.2274808259284,-37.1223641268137,
111.838645007951));
#38057=CARTESIAN_POINT('Ctrl Pts',(-85.2476803180234,-36.2934926649875,
111.891294515682));
#38058=CARTESIAN_POINT('Ctrl Pts',(-85.2678798101183,-35.4646212031613,
111.943944023413));
#38059=CARTESIAN_POINT('Ctrl Pts',(-85.7368231992784,-34.6466855730277,
111.996593531144));
#38060=CARTESIAN_POINT('Ctrl Pts',(-86.4419221311623,-34.210484454314,112.049243038874));
#38061=CARTESIAN_POINT('Ctrl Pts',(-87.1470210630461,-33.7742833356004,
112.101892546605));
#38062=CARTESIAN_POINT('Ctrl Pts',(-88.0882755376538,-33.7198167283067,
112.154542054336));
#38063=CARTESIAN_POINT('Ctrl Pts',(-88.8389821524022,-34.071776240586,112.207191562067));
#38064=CARTESIAN_POINT('Ctrl Pts',(-89.5896887671506,-34.4237357528653,
112.259841069798));
#38065=CARTESIAN_POINT('Ctrl Pts',(-90.1498475220396,-35.1821213847176,
112.312490577529));
#38066=CARTESIAN_POINT('Ctrl Pts',(-90.2655189637697,-36.0031305425708,
112.365140085259));
#38067=CARTESIAN_POINT('Ctrl Pts',(-90.2818329362183,-36.1189233483053,
112.372565622676));
#38068=CARTESIAN_POINT('Ctrl Pts',(-90.2893053970622,-36.2359618288104,
112.379991160092));
#38069=CARTESIAN_POINT('Ctrl Pts',(-90.2883545352501,-36.3531221775569,
112.387416697508));
#38070=CARTESIAN_POINT('Origin',(-87.7685555885722,-36.3549260746835,114.));
#38071=CARTESIAN_POINT('',(-90.2821608570194,-36.3545547485103,113.387416697508));
#38072=CARTESIAN_POINT('',(-90.2845475626897,-36.3570196913561,113.112583302492));
#38073=CARTESIAN_POINT('',(-90.2860555885722,-36.3549260746835,114.));
#38074=CARTESIAN_POINT('Ctrl Pts',(-90.2845475626897,-36.3570196913561,
113.112583302492));
#38075=CARTESIAN_POINT('Ctrl Pts',(-90.279879475621,-35.7733926616976,113.075736828766));
#38076=CARTESIAN_POINT('Ctrl Pts',(-90.0774218583082,-35.1868434749016,
113.03889035504));
#38077=CARTESIAN_POINT('Ctrl Pts',(-89.7060411910088,-34.7410066577834,
113.002043881314));
#38078=CARTESIAN_POINT('Ctrl Pts',(-89.1753795743932,-34.1039554945146,
112.949394373583));
#38079=CARTESIAN_POINT('Ctrl Pts',(-88.2998239243827,-33.7541999769884,
112.896744865852));
#38080=CARTESIAN_POINT('Ctrl Pts',(-87.4762940804989,-33.8502964504088,
112.844095358121));
#38081=CARTESIAN_POINT('Ctrl Pts',(-86.652764236615,-33.9463929238291,112.791445850391));
#38082=CARTESIAN_POINT('Ctrl Pts',(-85.8812601988578,-34.4883413881961,
112.73879634266));
#38083=CARTESIAN_POINT('Ctrl Pts',(-85.5115315906271,-35.2304577484975,
112.686146834929));
#38084=CARTESIAN_POINT('Ctrl Pts',(-85.1418029823965,-35.9725741087989,
112.633497327198));
#38085=CARTESIAN_POINT('Ctrl Pts',(-85.1738498036924,-36.9148583650348,
112.580847819467));
#38086=CARTESIAN_POINT('Ctrl Pts',(-85.5931441154104,-37.6301402787808,
112.528198311736));
#38087=CARTESIAN_POINT('Ctrl Pts',(-86.0124384271283,-38.3454221925268,
112.475548804006));
#38088=CARTESIAN_POINT('Ctrl Pts',(-86.8189802292683,-38.8337017637829,
112.422899296275));
#38089=CARTESIAN_POINT('Ctrl Pts',(-87.6471360607603,-38.873624874096,112.370249788544));
#38090=CARTESIAN_POINT('Ctrl Pts',(-88.4752918922522,-38.9135479844091,
112.317600280813));
#38091=CARTESIAN_POINT('Ctrl Pts',(-89.325061753096,-38.5051146337791,112.264950773082));
#38092=CARTESIAN_POINT('Ctrl Pts',(-89.8112153991693,-37.833481870745,112.212301265351));
#38093=CARTESIAN_POINT('Ctrl Pts',(-90.118139770751,-37.4094585904653,112.179061944398));
#38094=CARTESIAN_POINT('Ctrl Pts',(-90.2801339402842,-36.8805292513542,
112.145822623445));
#38095=CARTESIAN_POINT('Ctrl Pts',(-90.2832193840218,-36.3533353394049,
112.112583302492));
#38096=CARTESIAN_POINT('Ctrl Pts',(-90.2883545352501,-36.3531221775569,
112.387416697508));
#38097=CARTESIAN_POINT('Ctrl Pts',(-90.2825634734112,-37.06666731736,112.432640667823));
#38098=CARTESIAN_POINT('Ctrl Pts',(-89.9643335620966,-37.7847328079434,
112.477864638137));
#38099=CARTESIAN_POINT('Ctrl Pts',(-89.4281350245541,-38.2534471541448,
112.523088608452));
#38100=CARTESIAN_POINT('Ctrl Pts',(-88.8038955150371,-38.7991219240113,
112.575738116183));
#38101=CARTESIAN_POINT('Ctrl Pts',(-87.884232367432,-39.00683877989,112.628387623914));
#38102=CARTESIAN_POINT('Ctrl Pts',(-87.0860608845605,-38.7824324438797,
112.681037131644));
#38103=CARTESIAN_POINT('Ctrl Pts',(-86.287889401689,-38.5580261078694,112.733686639375));
#38104=CARTESIAN_POINT('Ctrl Pts',(-85.6112095835511,-37.9014965799701,
112.786336147106));
#38105=CARTESIAN_POINT('Ctrl Pts',(-85.3627839355564,-37.1104715379333,
112.838985654837));
#38106=CARTESIAN_POINT('Ctrl Pts',(-85.1143582875617,-36.3194464958966,
112.891635162568));
#38107=CARTESIAN_POINT('Ctrl Pts',(-85.2941868097101,-35.3939259397225,
112.944284670298));
#38108=CARTESIAN_POINT('Ctrl Pts',(-85.8207469761043,-34.7534805393349,
112.996934178029));
#38109=CARTESIAN_POINT('Ctrl Pts',(-86.3473071424986,-34.1130351389473,
113.04958368576));
#38110=CARTESIAN_POINT('Ctrl Pts',(-87.2205989531388,-33.7576648943461,
113.102233193491));
#38111=CARTESIAN_POINT('Ctrl Pts',(-88.044728845656,-33.8484715018728,113.154882701222));
#38112=CARTESIAN_POINT('Ctrl Pts',(-88.8688587381731,-33.9392781093994,
113.207532208953));
#38113=CARTESIAN_POINT('Ctrl Pts',(-89.6438267125673,-34.4762615690537,
113.260181716683));
#38114=CARTESIAN_POINT('Ctrl Pts',(-90.0183128224397,-35.2159885952083,
113.312831224414));
#38115=CARTESIAN_POINT('Ctrl Pts',(-90.1951503332143,-35.5652979087166,
113.337693048779));
#38116=CARTESIAN_POINT('Ctrl Pts',(-90.2826860440414,-35.9598161742905,
113.362554873143));
#38117=CARTESIAN_POINT('Ctrl Pts',(-90.2821608570194,-36.3545547485103,
113.387416697508));
#38118=CARTESIAN_POINT('Origin',(-87.7685555885722,-36.3549260746835,114.));
#38119=CARTESIAN_POINT('',(-90.2870432922795,-36.3570794361236,114.387416697508));
#38120=CARTESIAN_POINT('',(-90.290070014705,-36.3544600797813,114.112583302492));
#38121=CARTESIAN_POINT('',(-90.2860555885722,-36.3549260746835,114.));
#38122=CARTESIAN_POINT('Ctrl Pts',(-90.290070014705,-36.3544600797813,114.112583302492));
#38123=CARTESIAN_POINT('Ctrl Pts',(-90.2901361022756,-36.3287368231238,
114.110950049548));
#38124=CARTESIAN_POINT('Ctrl Pts',(-90.2897761587525,-36.3030154606156,
114.109316796605));
#38125=CARTESIAN_POINT('Ctrl Pts',(-90.2889844577079,-36.2773073944353,
114.107683543661));
#38126=CARTESIAN_POINT('Ctrl Pts',(-90.2634631993918,-35.4485827107525,
114.05503403593));
#38127=CARTESIAN_POINT('Ctrl Pts',(-89.7892775084378,-34.6336750173297,
114.002384528199));
#38128=CARTESIAN_POINT('Ctrl Pts',(-89.081392256987,-34.2020103248314,113.949735020469));
#38129=CARTESIAN_POINT('Ctrl Pts',(-88.3735070055363,-33.7703456323331,
113.897085512738));
#38130=CARTESIAN_POINT('Ctrl Pts',(-87.4319221935886,-33.7219239407594,
113.844436005007));
#38131=CARTESIAN_POINT('Ctrl Pts',(-86.6834909771368,-34.0786964876457,
113.791786497276));
#38132=CARTESIAN_POINT('Ctrl Pts',(-85.9350597606851,-34.4354690345319,
113.739136989545));
#38133=CARTESIAN_POINT('Ctrl Pts',(-85.3797821397292,-35.1974358198782,
113.686487481814));
#38134=CARTESIAN_POINT('Ctrl Pts',(-85.2693847797268,-36.0191707886337,
113.633837974084));
#38135=CARTESIAN_POINT('Ctrl Pts',(-85.1589874197243,-36.8409057573892,
113.581188466353));
#38136=CARTESIAN_POINT('Ctrl Pts',(-85.4934703206754,-37.7224089095541,
113.528538958622));
#38137=CARTESIAN_POINT('Ctrl Pts',(-86.1212007458526,-38.2640641959476,
113.475889450891));
#38138=CARTESIAN_POINT('Ctrl Pts',(-86.7489311710298,-38.8057194823412,
113.42323994316));
#38139=CARTESIAN_POINT('Ctrl Pts',(-87.6699091204331,-39.0075269029633,
113.37059043543));
#38140=CARTESIAN_POINT('Ctrl Pts',(-88.4666232458397,-38.7780001325227,
113.317940927699));
#38141=CARTESIAN_POINT('Ctrl Pts',(-89.2633373712462,-38.548473362082,113.265291419968));
#38142=CARTESIAN_POINT('Ctrl Pts',(-89.9357876726559,-37.8876124005786,
113.212641912237));
#38143=CARTESIAN_POINT('Ctrl Pts',(-90.1791290317504,-37.0950085153211,
113.159992404506));
#38144=CARTESIAN_POINT('Ctrl Pts',(-90.2521692545041,-36.8571041798227,
113.144189370502));
#38145=CARTESIAN_POINT('Ctrl Pts',(-90.2865496522039,-36.6073306943669,
113.128386336497));
#38146=CARTESIAN_POINT('Ctrl Pts',(-90.2845475626897,-36.3570196913561,
113.112583302492));
#38147=CARTESIAN_POINT('Ctrl Pts',(-90.2821608570194,-36.3545547485103,
113.387416697508));
#38148=CARTESIAN_POINT('Ctrl Pts',(-90.2815738634642,-36.7957480556462,
113.415204380874));
#38149=CARTESIAN_POINT('Ctrl Pts',(-90.1709794942958,-37.2372165766009,
113.442992064241));
#38150=CARTESIAN_POINT('Ctrl Pts',(-89.9521103385491,-37.6161456619663,
113.470779747607));
#38151=CARTESIAN_POINT('Ctrl Pts',(-89.5374174994356,-38.3341051099151,
113.523429255338));
#38152=CARTESIAN_POINT('Ctrl Pts',(-88.7340275758579,-38.8275534131576,
113.576078763068));
#38153=CARTESIAN_POINT('Ctrl Pts',(-87.9061451726702,-38.8727932871949,
113.628728270799));
#38154=CARTESIAN_POINT('Ctrl Pts',(-87.0782627694825,-38.9180331612322,
113.68137777853));
#38155=CARTESIAN_POINT('Ctrl Pts',(-86.2258878866846,-38.5150646060642,
113.734027286261));
#38156=CARTESIAN_POINT('Ctrl Pts',(-85.7354317154879,-37.8465672883091,
113.786676793992));
#38157=CARTESIAN_POINT('Ctrl Pts',(-85.2449755442911,-37.1780699705539,
113.839326301722));
#38158=CARTESIAN_POINT('Ctrl Pts',(-85.1164380846954,-36.2440438902116,
113.891975809453));
#38159=CARTESIAN_POINT('Ctrl Pts',(-85.4080898393636,-35.4679155672457,
113.944625317184));
#38160=CARTESIAN_POINT('Ctrl Pts',(-85.6997415940317,-34.6917872442799,
113.997274824915));
#38161=CARTESIAN_POINT('Ctrl Pts',(-86.4115825629637,-34.0735566786905,
114.049924332646));
#38162=CARTESIAN_POINT('Ctrl Pts',(-87.2209104677263,-33.8934892960711,
114.102573840377));
#38163=CARTESIAN_POINT('Ctrl Pts',(-88.0302383724889,-33.7134219134518,
114.155223348107));
#38164=CARTESIAN_POINT('Ctrl Pts',(-88.9370532130822,-33.9715177138025,
114.207872855838));
#38165=CARTESIAN_POINT('Ctrl Pts',(-89.5302642712866,-34.5507728908488,
114.260522363569));
#38166=CARTESIAN_POINT('Ctrl Pts',(-90.0068443658301,-35.0161409638533,
114.302820474882));
#38167=CARTESIAN_POINT('Ctrl Pts',(-90.2810132257934,-35.6887969255397,
114.345118586195));
#38168=CARTESIAN_POINT('Ctrl Pts',(-90.2870432922795,-36.3570794361236,
114.387416697508));
#38169=CARTESIAN_POINT('Origin',(-87.7685555885722,-36.3549260746835,114.));
#38170=CARTESIAN_POINT('',(-90.2884953401163,-36.3531793386956,115.387416697508));
#38171=CARTESIAN_POINT('',(-90.2833266058024,-36.3532747667377,115.112583302492));
#38172=CARTESIAN_POINT('',(-90.2860555885722,-36.3549260746835,114.));
#38173=CARTESIAN_POINT('Ctrl Pts',(-90.2833266058024,-36.3532747667377,
115.112583302492));
#38174=CARTESIAN_POINT('Ctrl Pts',(-90.2851691707048,-36.0508538051131,
115.0935137626));
#38175=CARTESIAN_POINT('Ctrl Pts',(-90.2346570131273,-35.749027590448,115.074444222708));
#38176=CARTESIAN_POINT('Ctrl Pts',(-90.1290213656974,-35.4679155567543,
115.055374682816));
#38177=CARTESIAN_POINT('Ctrl Pts',(-89.8373696075796,-34.6917872246094,
115.002725175085));
#38178=CARTESIAN_POINT('Ctrl Pts',(-89.1255286302286,-34.0735566517086,
114.950075667354));
#38179=CARTESIAN_POINT('Ctrl Pts',(-88.3162007158942,-33.89348926696,114.897426159623));
#38180=CARTESIAN_POINT('Ctrl Pts',(-87.5068728015597,-33.7134218822113,
114.844776651893));
#38181=CARTESIAN_POINT('Ctrl Pts',(-86.6000579502418,-33.9715176856148,
114.792127144162));
#38182=CARTESIAN_POINT('Ctrl Pts',(-86.0068468850218,-34.550772869512,114.739477636431));
#38183=CARTESIAN_POINT('Ctrl Pts',(-85.4136358198019,-35.1300280534093,
114.6868281287));
#38184=CARTESIAN_POINT('Ctrl Pts',(-85.13402854068,-36.0304426178002,114.634178620969));
#38185=CARTESIAN_POINT('Ctrl Pts',(-85.2947807557105,-36.8438273123537,
114.581529113239));
#38186=CARTESIAN_POINT('Ctrl Pts',(-85.4555329707409,-37.6572120069073,
114.528879605508));
#38187=CARTESIAN_POINT('Ctrl Pts',(-86.0566446799239,-38.3835668316234,
114.476230097777));
#38188=CARTESIAN_POINT('Ctrl Pts',(-86.8256110308943,-38.6936098722588,
114.423580590046));
#38189=CARTESIAN_POINT('Ctrl Pts',(-87.5945773818647,-39.0036529128942,
114.370931082315));
#38190=CARTESIAN_POINT('Ctrl Pts',(-88.5313983746226,-38.8973841694489,
114.318281574584));
#38191=CARTESIAN_POINT('Ctrl Pts',(-89.2113804581624,-38.4229789607549,
114.265632066854));
#38192=CARTESIAN_POINT('Ctrl Pts',(-89.8702686552171,-37.9632903892523,
114.214615812066));
#38193=CARTESIAN_POINT('Ctrl Pts',(-90.288005704732,-37.1579511867132,114.163599557279));
#38194=CARTESIAN_POINT('Ctrl Pts',(-90.290070014705,-36.3544600797813,114.112583302492));
#38195=CARTESIAN_POINT('Ctrl Pts',(-90.2870432922795,-36.3570794361236,
114.387416697508));
#38196=CARTESIAN_POINT('Ctrl Pts',(-90.2885189990354,-36.5206247333347,
114.397768093926));
#38197=CARTESIAN_POINT('Ctrl Pts',(-90.2739358136687,-36.6839081035843,
114.408119490344));
#38198=CARTESIAN_POINT('Ctrl Pts',(-90.2423303921774,-36.8438273065707,
114.418470886762));
#38199=CARTESIAN_POINT('Ctrl Pts',(-90.0815781790484,-37.6572119915045,
114.471120394492));
#38200=CARTESIAN_POINT('Ctrl Pts',(-89.4804664769749,-38.3835668076304,
114.523769902223));
#38201=CARTESIAN_POINT('Ctrl Pts',(-88.711500135099,-38.6936098445993,114.576419409954));
#38202=CARTESIAN_POINT('Ctrl Pts',(-87.9425337932232,-39.0036528815682,
114.629068917685));
#38203=CARTESIAN_POINT('Ctrl Pts',(-87.0057128115448,-38.89738413938,114.681718425416));
#38204=CARTESIAN_POINT('Ctrl Pts',(-86.3257307360469,-38.4229789362969,
114.734367933146));
#38205=CARTESIAN_POINT('Ctrl Pts',(-85.6457486605489,-37.9485737332138,
114.787017440877));
#38206=CARTESIAN_POINT('Ctrl Pts',(-85.2226054912313,-37.1060320692359,
114.839666948608));
#38207=CARTESIAN_POINT('Ctrl Pts',(-85.2481267492453,-36.2773073953543,
114.892316456339));
#38208=CARTESIAN_POINT('Ctrl Pts',(-85.2736480072592,-35.4485827214727,
114.94496596407));
#38209=CARTESIAN_POINT('Ctrl Pts',(-85.7478336926047,-34.6336750376873,
114.997615471801));
#38210=CARTESIAN_POINT('Ctrl Pts',(-86.4557189356833,-34.202010350294,115.050264979531));
#38211=CARTESIAN_POINT('Ctrl Pts',(-87.1636041787619,-33.7703456629007,
115.102914487262));
#38212=CARTESIAN_POINT('Ctrl Pts',(-88.1051889795735,-33.7219239718993,
115.155563994993));
#38213=CARTESIAN_POINT('Ctrl Pts',(-88.8536201871739,-34.0786965145658,
115.208213502724));
#38214=CARTESIAN_POINT('Ctrl Pts',(-89.6020513947743,-34.4354690572323,
115.260863010455));
#38215=CARTESIAN_POINT('Ctrl Pts',(-90.1573290091633,-35.1974358335667,
115.313512518185));
#38216=CARTESIAN_POINT('Ctrl Pts',(-90.2677263678604,-36.0191707926036,
115.366162025916));
#38217=CARTESIAN_POINT('Ctrl Pts',(-90.2825822180847,-36.1297492667593,
115.373246916447));
#38218=CARTESIAN_POINT('Ctrl Pts',(-90.2893820435841,-36.2414100410428,
115.380331806977));
#38219=CARTESIAN_POINT('Ctrl Pts',(-90.2884953401163,-36.3531793386956,
115.387416697508));
#38220=CARTESIAN_POINT('Origin',(-87.7685555885722,-36.3549260746835,114.));
#38221=CARTESIAN_POINT('',(-90.2821875961807,-36.3544693504637,116.387416697508));
#38222=CARTESIAN_POINT('',(-90.2844060344053,-36.3569864153294,116.112583302492));
#38223=CARTESIAN_POINT('',(-90.2860555885722,-36.3549260746835,114.));
#38224=CARTESIAN_POINT('Ctrl Pts',(-90.2844060344053,-36.3569864153294,
116.112583302492));
#38225=CARTESIAN_POINT('Ctrl Pts',(-90.2798734754633,-35.7786726434231,
116.076077475652));
#38226=CARTESIAN_POINT('Ctrl Pts',(-90.0814676279119,-35.197549043947,116.039571648811));
#38227=CARTESIAN_POINT('Ctrl Pts',(-89.7163642240759,-34.7534805203941,
116.003065821971));
#38228=CARTESIAN_POINT('Ctrl Pts',(-89.1898040514538,-34.1130351124323,
115.95041631424));
#38229=CARTESIAN_POINT('Ctrl Pts',(-88.3165122304853,-33.7576648636286,
115.897766806509));
#38230=CARTESIAN_POINT('Ctrl Pts',(-87.4923823282214,-33.8484714722295,
115.845117298778));
#38231=CARTESIAN_POINT('Ctrl Pts',(-86.6682524259574,-33.9392780808303,
115.792467791047));
#38232=CARTESIAN_POINT('Ctrl Pts',(-85.893284442398,-34.4762615468358,115.739818283317));
#38233=CARTESIAN_POINT('Ctrl Pts',(-85.5187983280969,-35.2159885817391,
115.687168775586));
#38234=CARTESIAN_POINT('Ctrl Pts',(-85.1443122137959,-35.9557156166424,
115.634519267855));
#38235=CARTESIAN_POINT('Ctrl Pts',(-85.1703079687531,-36.8981862204437,
115.581869760124));
#38236=CARTESIAN_POINT('Ctrl Pts',(-85.5850008127714,-37.6161456768834,
115.529220252393));
#38237=CARTESIAN_POINT('Ctrl Pts',(-85.9996936567897,-38.3341051333231,
115.476570744662));
#38238=CARTESIAN_POINT('Ctrl Pts',(-86.8030835898689,-38.8275534424013,
115.423921236932));
#38239=CARTESIAN_POINT('Ctrl Pts',(-87.6309660028479,-38.8727933169733,
115.371271729201));
#38240=CARTESIAN_POINT('Ctrl Pts',(-88.4588484158269,-38.9180331915453,
115.31862222147));
#38241=CARTESIAN_POINT('Ctrl Pts',(-89.3112233087056,-38.5150646316112,
115.265972713739));
#38242=CARTESIAN_POINT('Ctrl Pts',(-89.8016794857027,-37.8465673059497,
115.213323206008));
#38243=CARTESIAN_POINT('Ctrl Pts',(-90.1144934769387,-37.420198292002,115.17974323817));
#38244=CARTESIAN_POINT('Ctrl Pts',(-90.2800819931629,-36.8858144201648,
115.146163270331));
#38245=CARTESIAN_POINT('Ctrl Pts',(-90.2833266058024,-36.3532747667377,
115.112583302492));
#38246=CARTESIAN_POINT('Ctrl Pts',(-90.2884953401163,-36.3531793386956,
115.387416697508));
#38247=CARTESIAN_POINT('Ctrl Pts',(-90.2827927390801,-37.0719942929028,
115.432981314708));
#38248=CARTESIAN_POINT('Ctrl Pts',(-89.9591689800778,-37.7952978628962,
115.478545931909));
#38249=CARTESIAN_POINT('Ctrl Pts',(-89.4159104118097,-38.264064173368,115.524110549109));
#38250=CARTESIAN_POINT('Ctrl Pts',(-88.7881799940568,-38.8057194533557,
115.57676005684));
#38251=CARTESIAN_POINT('Ctrl Pts',(-87.8672020555458,-39.0075268715915,
115.62940956457));
#38252=CARTESIAN_POINT('Ctrl Pts',(-87.0704879395618,-38.7780001038657,
115.682059072301));
#38253=CARTESIAN_POINT('Ctrl Pts',(-86.2737738235778,-38.5484733361399,
115.734708580032));
#38254=CARTESIAN_POINT('Ctrl Pts',(-85.6013235301207,-37.8876123824526,
115.787358087763));
#38255=CARTESIAN_POINT('Ctrl Pts',(-85.3579821739038,-37.0950085065692,
115.840007595494));
#38256=CARTESIAN_POINT('Ctrl Pts',(-85.1146408176869,-36.3024046306858,
115.892657103225));
#38257=CARTESIAN_POINT('Ctrl Pts',(-85.3004083987102,-35.3780578326064,
115.945306610955));
#38258=CARTESIAN_POINT('Ctrl Pts',(-85.8310700090495,-34.7410066768717,
115.997956118686));
#38259=CARTESIAN_POINT('Ctrl Pts',(-86.3617316193887,-34.103955521137,116.050605626417));
#38260=CARTESIAN_POINT('Ctrl Pts',(-87.237287259044,-33.754200007747,116.103255134148));
#38261=CARTESIAN_POINT('Ctrl Pts',(-88.0608170931881,-33.8502964800305,
116.155904641879));
#38262=CARTESIAN_POINT('Ctrl Pts',(-88.8843469273323,-33.946392952314,116.208554149609));
#38263=CARTESIAN_POINT('Ctrl Pts',(-89.6558509559653,-34.4883414102711,
116.26120365734));
#38264=CARTESIAN_POINT('Ctrl Pts',(-90.0255795598235,-35.2304577617955,
116.313853165071));
#38265=CARTESIAN_POINT('Ctrl Pts',(-90.1977783344182,-35.5760937905085,
116.33837434255));
#38266=CARTESIAN_POINT('Ctrl Pts',(-90.2828251044975,-35.9651496803884,
116.362895520029));
#38267=CARTESIAN_POINT('Ctrl Pts',(-90.2821875961807,-36.3544693504637,
116.387416697508));
#38268=CARTESIAN_POINT('Origin',(-87.7685555885722,-36.3549260746835,114.));
#38269=CARTESIAN_POINT('',(-90.2868834016879,-36.3571029250538,117.387416697508));
#38270=CARTESIAN_POINT('',(-90.2901100729428,-36.3545560533475,117.112583302492));
#38271=CARTESIAN_POINT('',(-90.2860555885722,-36.3549260746835,114.));
#38272=CARTESIAN_POINT('Ctrl Pts',(-90.2901100729428,-36.3545560533475,
117.112583302492));
#38273=CARTESIAN_POINT('Ctrl Pts',(-90.2901522460903,-36.3341987546248,
117.111290696434));
#38274=CARTESIAN_POINT('Ctrl Pts',(-90.2899268097382,-36.3138424136066,
117.109998090376));
#38275=CARTESIAN_POINT('Ctrl Pts',(-90.2894308889351,-36.29349266426,117.108705484318));
#38276=CARTESIAN_POINT('Ctrl Pts',(-90.2692313966009,-35.4646211926309,
117.056055976587));
#38277=CARTESIAN_POINT('Ctrl Pts',(-89.8002880018944,-34.6466855528239,
117.003406468856));
#38278=CARTESIAN_POINT('Ctrl Pts',(-89.0951890616713,-34.2104844289517,
116.950756961126));
#38279=CARTESIAN_POINT('Ctrl Pts',(-88.3900901214482,-33.7742833050794,
116.898107453395));
#38280=CARTESIAN_POINT('Ctrl Pts',(-87.4488356357085,-33.7198166971419,
116.845457945664));
#38281=CARTESIAN_POINT('Ctrl Pts',(-86.6981290120818,-34.071776213584,116.792808437933));
#38282=CARTESIAN_POINT('Ctrl Pts',(-85.947422388455,-34.4237357300261,116.740158930202));
#38283=CARTESIAN_POINT('Ctrl Pts',(-85.3872636269413,-35.1821213708479,
116.687509422471));
#38284=CARTESIAN_POINT('Ctrl Pts',(-85.2715921838434,-36.0031305384112,
116.634859914741));
#38285=CARTESIAN_POINT('Ctrl Pts',(-85.1559207407456,-36.8241397059744,
116.58221040701));
#38286=CARTESIAN_POINT('Ctrl Pts',(-85.4847366160637,-37.707772400279,116.529560899279));
#38287=CARTESIAN_POINT('Ctrl Pts',(-86.1089761329637,-38.2534471765989,
116.476911391548));
#38288=CARTESIAN_POINT('Ctrl Pts',(-86.7332156498636,-38.7991219529187,
116.424261883817));
#38289=CARTESIAN_POINT('Ctrl Pts',(-87.6528788083454,-39.0068388112537,
116.371612376086));
#38290=CARTESIAN_POINT('Ctrl Pts',(-88.4510503006566,-38.7824324725891,
116.318962868356));
#38291=CARTESIAN_POINT('Ctrl Pts',(-89.2492217929678,-38.5580261339245,
116.266313360625));
#38292=CARTESIAN_POINT('Ctrl Pts',(-89.9259016191085,-37.9014965982603,
116.213663852894));
#38293=CARTESIAN_POINT('Ctrl Pts',(-90.174327270041,-37.1104715468681,116.161014345163));
#38294=CARTESIAN_POINT('Ctrl Pts',(-90.2505009059684,-36.8679231061256,
116.144870664273));
#38295=CARTESIAN_POINT('Ctrl Pts',(-90.2864104318265,-36.6127295061235,
116.128726983382));
#38296=CARTESIAN_POINT('Ctrl Pts',(-90.2844060344053,-36.3569864153294,
116.112583302492));
#38297=CARTESIAN_POINT('Ctrl Pts',(-90.2821875961807,-36.3544693504637,
116.387416697508));
#38298=CARTESIAN_POINT('Ctrl Pts',(-90.281456308114,-36.8010593342772,116.41554502776));
#38299=CARTESIAN_POINT('Ctrl Pts',(-90.1679776534187,-37.2479964123646,
116.443673358012));
#38300=CARTESIAN_POINT('Ctrl Pts',(-89.9439670360065,-37.6301402636982,
116.471801688264));
#38301=CARTESIAN_POINT('Ctrl Pts',(-89.5246727292477,-38.3454221689849,
116.524451195994));
#38302=CARTESIAN_POINT('Ctrl Pts',(-88.7181309366466,-38.8337017344665,
116.577100703725));
#38303=CARTESIAN_POINT('Ctrl Pts',(-87.8899751149491,-38.8736248443078,
116.629750211456));
#38304=CARTESIAN_POINT('Ctrl Pts',(-87.0618192932517,-38.913547954149,116.682399719187));
#38305=CARTESIAN_POINT('Ctrl Pts',(-86.2120494424578,-38.5051146083499,
116.735049226918));
#38306=CARTESIAN_POINT('Ctrl Pts',(-85.7258958021339,-37.8334818532593,
116.787698734649));
#38307=CARTESIAN_POINT('Ctrl Pts',(-85.2397421618101,-37.1618490981687,
116.840348242379));
#38308=CARTESIAN_POINT('Ctrl Pts',(-85.1172047319563,-36.2270169337866,
116.89299775011));
#38309=CARTESIAN_POINT('Ctrl Pts',(-85.4138339929931,-35.4527773060176,
116.945647257841));
#38310=CARTESIAN_POINT('Ctrl Pts',(-85.71046325403,-34.6785376782487,116.998296765572));
#38311=CARTESIAN_POINT('Ctrl Pts',(-86.4262592059575,-34.0648905870928,
117.050946273303));
#38312=CARTESIAN_POINT('Ctrl Pts',(-87.236726638944,-33.8900236097103,117.103595781033));
#38313=CARTESIAN_POINT('Ctrl Pts',(-88.0471940719305,-33.7151566323279,
117.156245288764));
#38314=CARTESIAN_POINT('Ctrl Pts',(-88.952332985976,-33.9790697687189,117.208894796495));
#38315=CARTESIAN_POINT('Ctrl Pts',(-89.5418124186763,-34.5621220117756,
117.261544304226));
#38316=CARTESIAN_POINT('Ctrl Pts',(-90.0115805778514,-35.026768212694,117.303501768653));
#38317=CARTESIAN_POINT('Ctrl Pts',(-90.2808790654697,-35.6940939327625,
117.345459233081));
#38318=CARTESIAN_POINT('Ctrl Pts',(-90.2868834016879,-36.3571029250538,
117.387416697508));
#38319=CARTESIAN_POINT('Origin',(-87.7685555885722,-36.3549260746835,114.));
#38320=CARTESIAN_POINT('',(-90.2886326699929,-36.3532397190198,118.387416697508));
#38321=CARTESIAN_POINT('',(-90.2834380340513,-36.3532166686934,118.112583302492));
#38322=CARTESIAN_POINT('',(-90.2860555885722,-36.3549260746835,114.));
#38323=CARTESIAN_POINT('Ctrl Pts',(-90.2834380340513,-36.3532166686934,
118.112583302492));
#38324=CARTESIAN_POINT('Ctrl Pts',(-90.2853167452331,-36.0562310899231,
118.093854409486));
#38325=CARTESIAN_POINT('Ctrl Pts',(-90.236641918583,-35.7598412835663,118.075125516479));
#38326=CARTESIAN_POINT('Ctrl Pts',(-90.1346681982238,-35.4830903892948,
118.056396623473));
#38327=CARTESIAN_POINT('Ctrl Pts',(-89.8480059712278,-34.7051053614309,
118.003747115742));
#38328=CARTESIAN_POINT('Ctrl Pts',(-89.1401493258784,-34.0823168034606,
117.951097608011));
#38329=CARTESIAN_POINT('Ctrl Pts',(-88.3319943080865,-33.8970564375262,
117.89844810028));
#38330=CARTESIAN_POINT('Ctrl Pts',(-87.5238392902945,-33.7117960715917,
117.845798592549));
#38331=CARTESIAN_POINT('Ctrl Pts',(-86.6153859000598,-33.9640638976931,
117.793149084819));
#38332=CARTESIAN_POINT('Ctrl Pts',(-86.0184676671723,-34.5394981330494,
117.740499577088));
#38333=CARTESIAN_POINT('Ctrl Pts',(-85.4215494342849,-35.1149323684057,
117.687850069357));
#38334=CARTESIAN_POINT('Ctrl Pts',(-85.1361663587445,-36.013533013017,117.635200561626));
#38335=CARTESIAN_POINT('Ctrl Pts',(-85.291692518077,-36.8279331295038,117.582551053895));
#38336=CARTESIAN_POINT('Ctrl Pts',(-85.4472186774094,-37.6423332459907,
117.529901546165));
#38337=CARTESIAN_POINT('Ctrl Pts',(-86.0436540716147,-38.3725328343531,
117.477252038434));
#38338=CARTESIAN_POINT('Ctrl Pts',(-86.8106137846128,-38.6875070152136,
117.424602530703));
#38339=CARTESIAN_POINT('Ctrl Pts',(-87.577573497611,-39.0024811960742,117.371953022972));
#38340=CARTESIAN_POINT('Ctrl Pts',(-88.515057529402,-38.9022299694327,117.319303515241));
#38341=CARTESIAN_POINT('Ctrl Pts',(-89.1980717503166,-38.4322007043864,
117.26665400751));
#38342=CARTESIAN_POINT('Ctrl Pts',(-89.8643171853922,-37.9737111991903,
117.215297105838));
#38343=CARTESIAN_POINT('Ctrl Pts',(-90.2884344795338,-37.1633777220556,
117.163940204165));
#38344=CARTESIAN_POINT('Ctrl Pts',(-90.2901100729428,-36.3545560533475,
117.112583302492));
#38345=CARTESIAN_POINT('Ctrl Pts',(-90.2868834016879,-36.3571029250538,
117.387416697508));
#38346=CARTESIAN_POINT('Ctrl Pts',(-90.2884134899268,-36.5260578643693,
117.398108740811));
#38347=CARTESIAN_POINT('Ctrl Pts',(-90.2728456235452,-36.6947324814093,
117.408800784115));
#38348=CARTESIAN_POINT('Ctrl Pts',(-90.2391401617222,-36.8597013320064,
117.419492827418));
#38349=CARTESIAN_POINT('Ctrl Pts',(-90.073168520713,-37.6720370594578,117.472142335149));
#38350=CARTESIAN_POINT('Ctrl Pts',(-89.4674052873395,-38.394517164638,117.52479184288));
#38351=CARTESIAN_POINT('Ctrl Pts',(-88.6964640117255,-38.6996162784728,
117.577441350611));
#38352=CARTESIAN_POINT('Ctrl Pts',(-87.9255227361115,-39.0047153923077,
117.630090858342));
#38353=CARTESIAN_POINT('Ctrl Pts',(-86.989403418257,-38.8924335147973,117.682740366073));
#38354=CARTESIAN_POINT('Ctrl Pts',(-86.3124815155165,-38.4136719276825,
117.735389873803));
#38355=CARTESIAN_POINT('Ctrl Pts',(-85.6355596127759,-37.9349103405677,
117.788039381534));
#38356=CARTESIAN_POINT('Ctrl Pts',(-85.2178351251494,-37.0896690438486,
117.840688889265));
#38357=CARTESIAN_POINT('Ctrl Pts',(-85.2486770968523,-36.2611253259234,
117.893338396996));
#38358=CARTESIAN_POINT('Ctrl Pts',(-85.2795190685552,-35.4325816079982,
117.945987904727));
#38359=CARTESIAN_POINT('Ctrl Pts',(-85.7589274995874,-34.620735468867,117.998637412457));
#38360=CARTESIAN_POINT('Ctrl Pts',(-86.4695698679984,-34.1936250102018,
118.051286920188));
#38361=CARTESIAN_POINT('Ctrl Pts',(-87.1802122364094,-33.7665145515366,
118.103936427919));
#38362=CARTESIAN_POINT('Ctrl Pts',(-88.1220885421992,-33.7241397733375,
118.15658593565));
#38363=CARTESIAN_POINT('Ctrl Pts',(-88.868213485108,-34.0857106367326,118.209235443381));
#38364=CARTESIAN_POINT('Ctrl Pts',(-89.6143384280168,-34.4472815001277,
118.261884951112));
#38365=CARTESIAN_POINT('Ctrl Pts',(-90.1647120080446,-35.212798005117,118.314534458842));
#38366=CARTESIAN_POINT('Ctrl Pts',(-90.2698307320447,-36.0352248856062,
118.367183966573));
#38367=CARTESIAN_POINT('Ctrl Pts',(-90.2832961245404,-36.140575296298,118.373928210218));
#38368=CARTESIAN_POINT('Ctrl Pts',(-90.2894554014685,-36.2468595402199,
118.380672453863));
#38369=CARTESIAN_POINT('Ctrl Pts',(-90.2886326699929,-36.3532397190198,
118.387416697508));
#38370=CARTESIAN_POINT('Origin',(-87.7685555885722,-36.3549260746835,114.));
#38371=CARTESIAN_POINT('',(-90.2822198465711,-36.3543846296117,119.387416697508));
#38372=CARTESIAN_POINT('',(-90.2842673953521,-36.3569499564742,119.112583302492));
#38373=CARTESIAN_POINT('',(-90.2860555885722,-36.3549260746835,114.));
#38374=CARTESIAN_POINT('Ctrl Pts',(-90.2842673953521,-36.3569499564742,
119.112583302492));
#38375=CARTESIAN_POINT('Ctrl Pts',(-90.2798741810248,-35.7839526994676,
119.076418122537));
#38376=CARTESIAN_POINT('Ctrl Pts',(-90.0854712507547,-35.2082585800464,
119.040252942582));
#38377=CARTESIAN_POINT('Ctrl Pts',(-89.7266069493757,-34.7660204103463,
119.004087762628));
#38378=CARTESIAN_POINT('Ctrl Pts',(-89.2041699303043,-34.1222071633618,
118.951438254897));
#38379=CARTESIAN_POINT('Ctrl Pts',(-88.3331779445183,-33.7612368344392,
118.898788747166));
#38380=CARTESIAN_POINT('Ctrl Pts',(-87.5084819626193,-33.8467498341343,
118.846139239435));
#38381=CARTESIAN_POINT('Ctrl Pts',(-86.6837859807203,-33.9322628338293,
118.793489731704));
#38382=CARTESIAN_POINT('Ctrl Pts',(-85.9053860027083,-34.4642591621421,
118.740840223973));
#38383=CARTESIAN_POINT('Ctrl Pts',(-85.526157822188,-35.2015663730428,118.688190716243));
#38384=CARTESIAN_POINT('Ctrl Pts',(-85.1469296416677,-35.9388735839435,
118.635541208512));
#38385=CARTESIAN_POINT('Ctrl Pts',(-85.1668732586391,-36.8814916774321,
118.582891700781));
#38386=CARTESIAN_POINT('Ctrl Pts',(-85.576947537357,-37.6020990753135,118.53024219305));
#38387=CARTESIAN_POINT('Ctrl Pts',(-85.9870218160749,-38.3227064731948,
118.477592685319));
#38388=CARTESIAN_POINT('Ctrl Pts',(-86.7872267565391,-38.8213031754689,
118.424943177589));
#38389=CARTESIAN_POINT('Ctrl Pts',(-87.6148016176882,-38.8718579490944,
118.372293669858));
#38390=CARTESIAN_POINT('Ctrl Pts',(-88.4423764788374,-38.92241272272,118.319644162127));
#38391=CARTESIAN_POINT('Ctrl Pts',(-89.2973212606714,-38.5249255676971,
118.266994654396));
#38392=CARTESIAN_POINT('Ctrl Pts',(-89.792059747267,-37.8595912413068,118.214345146665));
#38393=CARTESIAN_POINT('Ctrl Pts',(-90.1108060056166,-37.4309348241605,
118.180424531941));
#38394=CARTESIAN_POINT('Ctrl Pts',(-90.2800354283472,-36.8910986135966,
118.146503917216));
#38395=CARTESIAN_POINT('Ctrl Pts',(-90.2834380340513,-36.3532166686934,
118.112583302492));
#38396=CARTESIAN_POINT('Ctrl Pts',(-90.2886326699929,-36.3532397190198,
118.387416697508));
#38397=CARTESIAN_POINT('Ctrl Pts',(-90.2830326787043,-37.0773253924338,
118.433321961594));
#38398=CARTESIAN_POINT('Ctrl Pts',(-89.953959085277,-37.8058556896245,118.47922722568));
#38399=CARTESIAN_POINT('Ctrl Pts',(-89.4036178791718,-38.2746024797132,
118.525132489766));
#38400=CARTESIAN_POINT('Ctrl Pts',(-88.7724224343267,-38.812215937342,118.577781997496));
#38401=CARTESIAN_POINT('Ctrl Pts',(-87.8501676766643,-39.0081055966104,
118.630431505227));
#38402=CARTESIAN_POINT('Ctrl Pts',(-87.0549437757234,-38.7734678609392,
118.683081012958));
#38403=CARTESIAN_POINT('Ctrl Pts',(-86.2597198747824,-38.538830125268,118.735730520689));
#38404=CARTESIAN_POINT('Ctrl Pts',(-85.5915268305631,-37.8736649946574,
118.78838002842));
#38405=CARTESIAN_POINT('Ctrl Pts',(-85.3532797991764,-37.0795149627522,
118.841029536151));
#38406=CARTESIAN_POINT('Ctrl Pts',(-85.1150327677896,-36.285364930847,118.893679043881));
#38407=CARTESIAN_POINT('Ctrl Pts',(-85.3067317492356,-35.3622299976473,
118.946328551612));
#38408=CARTESIAN_POINT('Ctrl Pts',(-85.8414729241709,-34.7285993539164,
118.998978059343));
#38409=CARTESIAN_POINT('Ctrl Pts',(-86.3762140991062,-34.0949687101855,
119.051627567074));
#38410=CARTESIAN_POINT('Ctrl Pts',(-87.253997467531,-33.7508423559234,119.104277074805));
#38411=CARTESIAN_POINT('Ctrl Pts',(-88.0768932901973,-33.8522247269142,
119.156926582536));
#38412=CARTESIAN_POINT('Ctrl Pts',(-88.8997891128635,-33.9536070979049,
119.209576090266));
#38413=CARTESIAN_POINT('Ctrl Pts',(-89.6677973897713,-34.5004981941486,
119.262225597997));
#38414=CARTESIAN_POINT('Ctrl Pts',(-90.0327532423181,-35.2449732821291,
119.314875105728));
#38415=CARTESIAN_POINT('Ctrl Pts',(-90.2003678419235,-35.5868910590801,
119.339055636321));
#38416=CARTESIAN_POINT('Ctrl Pts',(-90.28296567943,-35.9704856755803,119.363236166915));
#38417=CARTESIAN_POINT('Ctrl Pts',(-90.2822198465711,-36.3543846296117,
119.387416697508));
#38418=CARTESIAN_POINT('Origin',(-87.7685555885722,-36.3549260746835,114.));
#38419=CARTESIAN_POINT('',(-90.2867226440827,-36.3571243050301,120.387416697508));
#38420=CARTESIAN_POINT('',(-90.290141386937,-36.3546528235808,120.112583302492));
#38421=CARTESIAN_POINT('',(-90.2860555885722,-36.3549260746835,114.));
#38422=CARTESIAN_POINT('Ctrl Pts',(-90.290141386937,-36.3546528235808,120.112583302492));
#38423=CARTESIAN_POINT('Ctrl Pts',(-90.290164686063,-36.3396608841848,120.11163134332));
#38424=CARTESIAN_POINT('Ctrl Pts',(-90.2900424224598,-36.3246693349243,
120.110679384147));
#38425=CARTESIAN_POINT('Ctrl Pts',(-90.2897734333149,-36.3096804188387,
120.109727424975));
#38426=CARTESIAN_POINT('Ctrl Pts',(-90.2748965914554,-35.4806962814753,
120.057077917244));
#38427=CARTESIAN_POINT('Ctrl Pts',(-89.8112147295564,-34.65976651665,120.004428409513));
#38428=CARTESIAN_POINT('Ctrl Pts',(-89.1089311464144,-34.2190469710397,
119.951778901782));
#38429=CARTESIAN_POINT('Ctrl Pts',(-88.4066475632724,-33.7783274254294,
119.899129394052));
#38430=CARTESIAN_POINT('Ctrl Pts',(-87.4657622588873,-33.7178180990341,
119.846479886321));
#38431=CARTESIAN_POINT('Ctrl Pts',(-86.7128111916705,-34.0649500616042,
119.79383037859));
#38432=CARTESIAN_POINT('Ctrl Pts',(-85.9598601244536,-34.4120820241742,
119.741180870859));
#38433=CARTESIAN_POINT('Ctrl Pts',(-85.394843294405,-35.1668552757097,119.688531363128));
#38434=CARTESIAN_POINT('Ctrl Pts',(-85.2739025313641,-35.9871047981258,
119.635881855397));
#38435=CARTESIAN_POINT('Ctrl Pts',(-85.1529617683233,-36.8073543205419,
119.583232347667));
#38436=CARTESIAN_POINT('Ctrl Pts',(-85.4760970722901,-37.6930801138387,
119.530582839936));
#38437=CARTESIAN_POINT('Ctrl Pts',(-86.0968199466272,-38.2427518792084,
119.477933332205));
#38438=CARTESIAN_POINT('Ctrl Pts',(-86.7175428209643,-38.7924236445782,
119.425283824474));
#38439=CARTESIAN_POINT('Ctrl Pts',(-87.6358532656717,-39.0060413820208,
119.372634316743));
#38440=CARTESIAN_POINT('Ctrl Pts',(-88.4354492151556,-38.7867647287355,
119.319984809013));
#38441=CARTESIAN_POINT('Ctrl Pts',(-89.2350451646396,-38.5674880754502,
119.267335301282));
#38442=CARTESIAN_POINT('Ctrl Pts',(-89.9159266189002,-37.9153170314371,
119.214685793551));
#38443=CARTESIAN_POINT('Ctrl Pts',(-90.169426319852,-37.1259034269073,119.16203628582));
#38444=CARTESIAN_POINT('Ctrl Pts',(-90.248795953904,-36.87874152229,119.145551958044));
#38445=CARTESIAN_POINT('Ctrl Pts',(-90.2862698514454,-36.6181258889888,
119.129067630268));
#38446=CARTESIAN_POINT('Ctrl Pts',(-90.2842673953521,-36.3569499564742,
119.112583302492));
#38447=CARTESIAN_POINT('Ctrl Pts',(-90.2822198465711,-36.3543846296117,
119.387416697508));
#38448=CARTESIAN_POINT('Ctrl Pts',(-90.2813417393464,-36.8063685305952,
119.415885674646));
#38449=CARTESIAN_POINT('Ctrl Pts',(-90.1649363125751,-37.2587742908399,
119.444354651783));
#38450=CARTESIAN_POINT('Ctrl Pts',(-89.9357340391242,-37.6440823046029,
119.472823628921));
#38451=CARTESIAN_POINT('Ctrl Pts',(-89.5118555551979,-38.3566571593789,
119.525473136651));
#38452=CARTESIAN_POINT('Ctrl Pts',(-88.7021951591595,-38.8397477892134,
119.578122644382));
#38453=CARTESIAN_POINT('Ctrl Pts',(-87.8738000571021,-38.8743525238657,
119.630772152113));
#38454=CARTESIAN_POINT('Ctrl Pts',(-87.0454049550448,-38.9089572585181,
119.683421659844));
#38455=CARTESIAN_POINT('Ctrl Pts',(-86.1982751469685,-38.4950760979882,
119.736071167575));
#38456=CARTESIAN_POINT('Ctrl Pts',(-85.7164440946653,-37.8203355247142,
119.788720675305));
#38457=CARTESIAN_POINT('Ctrl Pts',(-85.234613042362,-37.1455949514403,119.841370183036));
#38458=CARTESIAN_POINT('Ctrl Pts',(-85.1180807458316,-36.2099949654222,
119.894019690767));
#38459=CARTESIAN_POINT('Ctrl Pts',(-85.4196752561595,-35.4376761026093,
119.946669198498));
#38460=CARTESIAN_POINT('Ctrl Pts',(-85.7212697664874,-34.6653572397964,
119.999318706229));
#38461=CARTESIAN_POINT('Ctrl Pts',(-86.4409910836734,-34.0563195001886,
120.05196821396));
#38462=CARTESIAN_POINT('Ctrl Pts',(-87.2525646854532,-33.8866598330932,
120.10461772169));
#38463=CARTESIAN_POINT('Ctrl Pts',(-88.064138287233,-33.7170001659977,120.157267229421));
#38464=CARTESIAN_POINT('Ctrl Pts',(-88.9675641736066,-33.9867185714146,
120.209916737152));
#38465=CARTESIAN_POINT('Ctrl Pts',(-89.5532875619044,-34.5735444679974,
120.262566244883));
#38466=CARTESIAN_POINT('Ctrl Pts',(-90.0162727716681,-35.0374011557315,
120.304183062425));
#38467=CARTESIAN_POINT('Ctrl Pts',(-90.28075376653,-35.6993902911316,120.345799879966));
#38468=CARTESIAN_POINT('Ctrl Pts',(-90.2867226440827,-36.3571243050301,
120.387416697508));
#38469=CARTESIAN_POINT('Origin',(-87.7685555885722,-36.3549260746835,114.));
#38470=CARTESIAN_POINT('',(-90.2887582439581,-36.3533471924086,121.387416697508));
#38471=CARTESIAN_POINT('',(-90.2835504011883,-36.3531642868356,121.112583302492));
#38472=CARTESIAN_POINT('',(-90.2860555885722,-36.3549260746835,114.));
#38473=CARTESIAN_POINT('',(-85.855089591907,-34.7189388713088,122.));
#38474=CARTESIAN_POINT('Ctrl Pts',(-90.2887582439581,-36.3533471924086,
121.387416697508));
#38475=CARTESIAN_POINT('Ctrl Pts',(-90.2833001895768,-37.0825700799613,
121.43366260848));
#38476=CARTESIAN_POINT('Ctrl Pts',(-89.9487704521404,-37.8160441629617,
121.479908519451));
#38477=CARTESIAN_POINT('Ctrl Pts',(-89.3912934070429,-38.2848774639003,
121.526154430423));
#38478=CARTESIAN_POINT('Ctrl Pts',(-88.756623413977,-38.8186293564175,121.578803938153));
#38479=CARTESIAN_POINT('Ctrl Pts',(-87.8329891255066,-39.009377613116,121.631453445884));
#38480=CARTESIAN_POINT('Ctrl Pts',(-87.0393721481588,-38.769223717878,121.684102953615));
#38481=CARTESIAN_POINT('Ctrl Pts',(-86.2457551708111,-38.5290698226399,
121.736752461346));
#38482=CARTESIAN_POINT('Ctrl Pts',(-85.5821555045859,-37.8580137754653,
121.789401969077));
#38483=CARTESIAN_POINT('Ctrl Pts',(-85.3491902632795,-37.0637278391879,
121.842051476807));
#38484=CARTESIAN_POINT('Ctrl Pts',(-85.1162250219731,-36.2694419029105,
121.894700984538));
#38485=CARTESIAN_POINT('Ctrl Pts',(-85.3138942055855,-35.3519260775303,
121.947350492269));
#38486=CARTESIAN_POINT('Ctrl Pts',(-85.855089591907,-34.7189388713087,122.));
#38487=CARTESIAN_POINT('',(-89.685665865028,-34.7163981196112,122.));
#38488=CARTESIAN_POINT('Origin',(-87.7685555885722,-36.3549260746835,122.));
#38489=CARTESIAN_POINT('Ctrl Pts',(-89.6856747112032,-34.7163919521555,
122.));
#38490=CARTESIAN_POINT('Ctrl Pts',(-89.1628541599957,-34.1076769201533,
121.949053726697));
#38491=CARTESIAN_POINT('Ctrl Pts',(-88.3231296368472,-33.7675004995563,
121.898107453395));
#38492=CARTESIAN_POINT('Ctrl Pts',(-87.5244587636259,-33.8452632724063,
121.847161180092));
#38493=CARTESIAN_POINT('Ctrl Pts',(-86.6990867474188,-33.9256258081705,
121.794511672361));
#38494=CARTESIAN_POINT('Ctrl Pts',(-85.9175592756957,-34.4523397302599,
121.74186216463));
#38495=CARTESIAN_POINT('Ctrl Pts',(-85.5336746560242,-35.1871265144118,
121.689212656899));
#38496=CARTESIAN_POINT('Ctrl Pts',(-85.1497900363526,-35.9219132985637,
121.636563149169));
#38497=CARTESIAN_POINT('Ctrl Pts',(-85.1635482687327,-36.8647729447781,
121.583913641438));
#38498=CARTESIAN_POINT('Ctrl Pts',(-85.5689530570713,-37.5880327246192,
121.531264133707));
#38499=CARTESIAN_POINT('Ctrl Pts',(-85.9743578454099,-38.3112925044604,
121.478614625976));
#38500=CARTESIAN_POINT('Ctrl Pts',(-86.7714091897071,-38.8149524179282,
121.425965118245));
#38501=CARTESIAN_POINT('Ctrl Pts',(-87.5986589189311,-38.870803405099,121.373315610515));
#38502=CARTESIAN_POINT('Ctrl Pts',(-88.4259086481551,-38.9266543922699,
121.320666102784));
#38503=CARTESIAN_POINT('Ctrl Pts',(-89.2833567623059,-38.5346964531437,
121.268016595053));
#38504=CARTESIAN_POINT('Ctrl Pts',(-89.7823491181618,-37.872560629567,121.215367087322));
#38505=CARTESIAN_POINT('Ctrl Pts',(-90.1070645501236,-37.4416808426386,
121.181105825712));
#38506=CARTESIAN_POINT('Ctrl Pts',(-90.2799863217522,-36.8963900326682,
121.146844564102));
#38507=CARTESIAN_POINT('Ctrl Pts',(-90.2835504011883,-36.3531642868356,
121.112583302492));
#38508=CARTESIAN_POINT('Origin',(-87.7685555885722,-36.3549260746835,124.208423447177));
#38509=CARTESIAN_POINT('',(-90.8468255927006,-36.3541126078384,107.791576552823));
#38510=CARTESIAN_POINT('',(-90.8371847050479,-36.3546117509714,107.708423447177));
#38511=CARTESIAN_POINT('',(-90.8420555885722,-36.3549260746832,124.208423447177));
#38512=CARTESIAN_POINT('',(-86.9747563060399,-39.3241490284294,107.));
#38513=CARTESIAN_POINT('Ctrl Pts',(-90.8371847050479,-36.3546117509714,
107.708423447177));
#38514=CARTESIAN_POINT('Ctrl Pts',(-90.8375045645286,-35.8594362659055,
107.682880329042));
#38515=CARTESIAN_POINT('Ctrl Pts',(-90.4912522748027,-34.3441196931088,
107.604687703175));
#38516=CARTESIAN_POINT('Ctrl Pts',(-88.1200899635817,-32.7460643868788,
107.473845569577));
#38517=CARTESIAN_POINT('Ctrl Pts',(-84.9365304165877,-34.0865210383432,
107.315897046385));
#38518=CARTESIAN_POINT('Ctrl Pts',(-84.3257623763415,-37.4887078672662,
107.157948523192));
#38519=CARTESIAN_POINT('Ctrl Pts',(-85.9925177162683,-39.0615549760519,
107.052649507731));
#38520=CARTESIAN_POINT('Ctrl Pts',(-86.97475630604,-39.3241490284294,107.));
#38521=CARTESIAN_POINT('',(-88.5623548711056,-39.3241490284291,107.));
#38522=CARTESIAN_POINT('Origin',(-87.7685555885722,-36.3549260746835,107.));
#38523=CARTESIAN_POINT('Ctrl Pts',(-90.8468255927006,-36.3541126078384,
107.791576552823));
#38524=CARTESIAN_POINT('Ctrl Pts',(-90.8469816617586,-36.309603764564,107.789262006108));
#38525=CARTESIAN_POINT('Ctrl Pts',(-90.8260219475787,-35.2527942086462,
107.734297951662));
#38526=CARTESIAN_POINT('Ctrl Pts',(-89.6167529992886,-33.2347628855613,
107.626684389485));
#38527=CARTESIAN_POINT('Ctrl Pts',(-86.1660868316116,-33.1013875794135,
107.468735866293));
#38528=CARTESIAN_POINT('Ctrl Pts',(-84.1684777778814,-35.918700775767,107.3107873431));
#38529=CARTESIAN_POINT('Ctrl Pts',(-85.4209926009409,-39.0952448583635,
107.154542054336));
#38530=CARTESIAN_POINT('Ctrl Pts',(-87.6173027279392,-39.5801183929225,
107.050946273303));
#38531=CARTESIAN_POINT('Ctrl Pts',(-88.56426900845,-39.3292377960811,107.));
#38532=CARTESIAN_POINT('Origin',(-87.7685555885722,-36.3549260746835,124.208423447177));
#38533=CARTESIAN_POINT('',(-90.8384673493636,-36.3530606802369,108.791576552823));
#38534=CARTESIAN_POINT('',(-90.8436485370458,-36.357484352357,108.708423447177));
#38535=CARTESIAN_POINT('',(-90.8420555885722,-36.3549260746832,124.208423447177));
#38536=CARTESIAN_POINT('Ctrl Pts',(-90.8436485370458,-36.357484352357,108.708423447177));
#38537=CARTESIAN_POINT('Ctrl Pts',(-90.8362606803297,-35.5287363165806,
108.665444042093));
#38538=CARTESIAN_POINT('Ctrl Pts',(-90.0646116326147,-33.6726458843614,
108.569815129278));
#38539=CARTESIAN_POINT('Ctrl Pts',(-86.9355577566776,-32.8253529082965,
108.421536708732));
#38540=CARTESIAN_POINT('Ctrl Pts',(-84.3576615325144,-35.1229272723648,
108.26358818554));
#38541=CARTESIAN_POINT('Ctrl Pts',(-84.8723855412168,-38.5375840624727,
108.105639662347));
#38542=CARTESIAN_POINT('Ctrl Pts',(-88.0128424342027,-39.9731543052364,
107.947691139155));
#38543=CARTESIAN_POINT('Ctrl Pts',(-90.4599971769878,-38.4267875285153,
107.815285734098));
#38544=CARTESIAN_POINT('Ctrl Pts',(-90.8368452697583,-36.8800926082682,
107.735529836772));
#38545=CARTESIAN_POINT('Ctrl Pts',(-90.8371847050479,-36.3546117509714,
107.708423447177));
#38546=CARTESIAN_POINT('Ctrl Pts',(-90.8384673493637,-36.3530606802369,
108.791576552823));
#38547=CARTESIAN_POINT('Ctrl Pts',(-90.8406114808459,-35.9705776970889,
108.771825719159));
#38548=CARTESIAN_POINT('Ctrl Pts',(-90.5976170520827,-34.5711416081288,
108.699425377765));
#38549=CARTESIAN_POINT('Ctrl Pts',(-88.5106433977503,-32.8051167774314,
108.57437552864));
#38550=CARTESIAN_POINT('Ctrl Pts',(-85.2017899780534,-33.7929771900336,
108.416427005448));
#38551=CARTESIAN_POINT('Ctrl Pts',(-84.2201468213852,-37.1036893633033,
108.258478482255));
#38552=CARTESIAN_POINT('Ctrl Pts',(-86.4557339663443,-39.7354987833619,
108.100529959063));
#38553=CARTESIAN_POINT('Ctrl Pts',(-89.8314224577491,-39.3086388322812,
107.944895982585));
#38554=CARTESIAN_POINT('Ctrl Pts',(-90.8434315242634,-37.3220562992096,
107.841911513839));
#38555=CARTESIAN_POINT('Ctrl Pts',(-90.8468255927006,-36.3541126078384,
107.791576552823));
#38556=CARTESIAN_POINT('Origin',(-87.7685555885722,-36.3549260746835,124.208423447177));
#38557=CARTESIAN_POINT('',(-90.8403906014318,-36.3575187352786,109.791576552823));
#38558=CARTESIAN_POINT('',(-90.8446864850876,-36.3526580234404,109.708423447177));
#38559=CARTESIAN_POINT('',(-90.8420555885722,-36.3549260746832,124.208423447177));
#38560=CARTESIAN_POINT('Ctrl Pts',(-90.8446864850876,-36.3526580234404,
109.708423447177));
#38561=CARTESIAN_POINT('Ctrl Pts',(-90.8459256065026,-36.2030382733544,
109.700657262876));
#38562=CARTESIAN_POINT('Ctrl Pts',(-90.7682627105974,-35.0403882853119,
109.640241570843));
#38563=CARTESIAN_POINT('Ctrl Pts',(-89.2869056328921,-33.0615291810096,
109.52717637108));
#38564=CARTESIAN_POINT('Ctrl Pts',(-85.840854849815,-33.2831483419104,109.369227847887));
#38565=CARTESIAN_POINT('Ctrl Pts',(-84.1425912719677,-36.2898545213693,
109.211279324695));
#38566=CARTESIAN_POINT('Ctrl Pts',(-85.731880137862,-39.3555599790778,109.053330801502));
#38567=CARTESIAN_POINT('Ctrl Pts',(-89.1677588894168,-39.7006801261729,
108.89538227831));
#38568=CARTESIAN_POINT('Ctrl Pts',(-90.7452906984258,-37.7438433497054,
108.780413160201));
#38569=CARTESIAN_POINT('Ctrl Pts',(-90.8453107595136,-36.5439475795324,
108.718093549824));
#38570=CARTESIAN_POINT('Ctrl Pts',(-90.8436485370458,-36.357484352357,108.708423447177));
#38571=CARTESIAN_POINT('Ctrl Pts',(-90.8403906014318,-36.3575187352786,
109.791576552823));
#38572=CARTESIAN_POINT('Ctrl Pts',(-90.8345311555102,-35.6385125258615,
109.754389432211));
#38573=CARTESIAN_POINT('Ctrl Pts',(-90.225320179554,-33.8925906158493,109.664552803868));
#38574=CARTESIAN_POINT('Ctrl Pts',(-87.3251105792218,-32.7555919072101,
109.522066667795));
#38575=CARTESIAN_POINT('Ctrl Pts',(-84.5122325649308,-34.7586145140015,
109.364118144603));
#38576=CARTESIAN_POINT('Ctrl Pts',(-84.6517636253375,-38.2089644036472,
109.20616962141));
#38577=CARTESIAN_POINT('Ctrl Pts',(-87.6171951129081,-39.9783138396851,
109.048221098218));
#38578=CARTESIAN_POINT('Ctrl Pts',(-90.3318846828953,-38.6520013205392,
108.910023408688));
#38579=CARTESIAN_POINT('Ctrl Pts',(-90.8348959009886,-36.9901569777125,
108.82447522689));
#38580=CARTESIAN_POINT('Ctrl Pts',(-90.8384673493637,-36.3530606802369,
108.791576552823));
#38581=CARTESIAN_POINT('Origin',(-87.7685555885722,-36.3549260746835,124.208423447177));
#38582=CARTESIAN_POINT('',(-90.8468973805148,-36.3542412677562,110.791576552823));
#38583=CARTESIAN_POINT('',(-90.8372748127875,-36.3545776583154,110.708423447177));
#38584=CARTESIAN_POINT('',(-90.8420555885722,-36.3549260746832,124.208423447177));
#38585=CARTESIAN_POINT('Ctrl Pts',(-90.8372748127875,-36.3545776583154,
110.708423447177));
#38586=CARTESIAN_POINT('Ctrl Pts',(-90.8377741082269,-35.8660461342068,
110.683220975927));
#38587=CARTESIAN_POINT('Ctrl Pts',(-90.4981130409743,-34.3575981264578,
110.605368996946));
#38588=CARTESIAN_POINT('Ctrl Pts',(-88.142588178909,-32.7477180991385,110.474867510234));
#38589=CARTESIAN_POINT('Ctrl Pts',(-84.9525260101083,-34.0697943170025,
110.316918987042));
#38590=CARTESIAN_POINT('Ctrl Pts',(-84.3156722087998,-37.4637299947607,
110.158970463849));
#38591=CARTESIAN_POINT('Ctrl Pts',(-86.8094427648148,-39.8523468925606,
110.001021940657));
#38592=CARTESIAN_POINT('Ctrl Pts',(-90.0074379512479,-39.1084279923414,
109.850839601766));
#38593=CARTESIAN_POINT('Ctrl Pts',(-90.837525196471,-37.217359577444,109.753306770606));
#38594=CARTESIAN_POINT('Ctrl Pts',(-90.8446864850876,-36.3526580234404,
109.708423447177));
#38595=CARTESIAN_POINT('Ctrl Pts',(-90.8468973805148,-36.3542412677562,
110.791576552823));
#38596=CARTESIAN_POINT('Ctrl Pts',(-90.8470130244964,-36.3162849770529,
110.789602652993));
#38597=CARTESIAN_POINT('Ctrl Pts',(-90.8292490828189,-35.2660374732868,
110.734979245433));
#38598=CARTESIAN_POINT('Ctrl Pts',(-89.6367304343865,-33.2465868380812,
110.627706330142));
#38599=CARTESIAN_POINT('Ctrl Pts',(-86.18704996557,-33.091386581079,110.46975780695));
#38600=CARTESIAN_POINT('Ctrl Pts',(-84.1712725456449,-35.8951383259589,
110.311809283757));
#38601=CARTESIAN_POINT('Ctrl Pts',(-85.4170422546641,-39.1157656406506,
110.153860760565));
#38602=CARTESIAN_POINT('Ctrl Pts',(-88.794857584793,-39.8332236842038,109.995912237372));
#38603=CARTESIAN_POINT('Ctrl Pts',(-90.6659684787637,-37.9705917203656,
109.875150834792));
#38604=CARTESIAN_POINT('Ctrl Pts',(-90.8428269562679,-36.6564811762577,
109.807038939942));
#38605=CARTESIAN_POINT('Ctrl Pts',(-90.8403906014318,-36.3575187352786,
109.791576552823));
#38606=CARTESIAN_POINT('Origin',(-87.7685555885722,-36.3549260746835,124.208423447177));
#38607=CARTESIAN_POINT('',(-90.83859299684,-36.3529840191205,111.791576552823));
#38608=CARTESIAN_POINT('',(-90.8434556139163,-36.3575218683383,111.708423447177));
#38609=CARTESIAN_POINT('',(-90.8420555885722,-36.3549260746832,124.208423447177));
#38610=CARTESIAN_POINT('Ctrl Pts',(-90.8434556139163,-36.3575218683383,
111.708423447177));
#38611=CARTESIAN_POINT('Ctrl Pts',(-90.8360747346033,-35.535209872403,111.665784688979));
#38612=CARTESIAN_POINT('Ctrl Pts',(-90.0746147978365,-33.6854550212672,
111.570496423049));
#38613=CARTESIAN_POINT('Ctrl Pts',(-86.9582294999899,-32.8200680318722,
111.422558649389));
#38614=CARTESIAN_POINT('Ctrl Pts',(-84.3656606335548,-35.1010697521711,
111.264610126197));
#38615=CARTESIAN_POINT('Ctrl Pts',(-84.8583931283879,-38.5189048657011,
111.106661603004));
#38616=CARTESIAN_POINT('Ctrl Pts',(-87.9896814174328,-39.974726224009,110.948713079812));
#38617=CARTESIAN_POINT('Ctrl Pts',(-90.4528393566696,-38.4399663599021,
110.81596702787));
#38618=CARTESIAN_POINT('Ctrl Pts',(-90.8367310494397,-36.8866184423715,
110.735870483658));
#38619=CARTESIAN_POINT('Ctrl Pts',(-90.8372748127875,-36.3545776583154,
110.708423447177));
#38620=CARTESIAN_POINT('Ctrl Pts',(-90.8385929968401,-36.3529840191205,
111.791576552823));
#38621=CARTESIAN_POINT('Ctrl Pts',(-90.8407926739791,-35.9771364929294,
111.772166366045));
#38622=CARTESIAN_POINT('Ctrl Pts',(-90.603358358261,-34.5844968131842,111.700106671536));
#38623=CARTESIAN_POINT('Ctrl Pts',(-88.5334211681103,-32.8099534783274,
111.575397469297));
#38624=CARTESIAN_POINT('Ctrl Pts',(-85.218293678275,-33.7765517317041,111.417448946105));
#38625=CARTESIAN_POINT('Ctrl Pts',(-84.2154110997942,-37.0808835841375,
111.259500422912));
#38626=CARTESIAN_POINT('Ctrl Pts',(-86.4340565652882,-39.7270118417731,
111.10155189972));
#38627=CARTESIAN_POINT('Ctrl Pts',(-89.8198041827813,-39.3209117944618,
110.945577276356));
#38628=CARTESIAN_POINT('Ctrl Pts',(-90.8439284714653,-37.3286869192262,
110.842252160724));
#38629=CARTESIAN_POINT('Ctrl Pts',(-90.8468973805148,-36.3542412677562,
110.791576552823));
#38630=CARTESIAN_POINT('Origin',(-87.7685555885722,-36.3549260746835,124.208423447177));
#38631=CARTESIAN_POINT('',(-90.8402145091085,-36.3574820750184,112.791576552823));
#38632=CARTESIAN_POINT('',(-90.8448622668699,-36.352723779621,112.708423447177));
#38633=CARTESIAN_POINT('',(-90.8420555885722,-36.3549260746832,124.208423447177));
#38634=CARTESIAN_POINT('Ctrl Pts',(-90.8448622668699,-36.352723779621,112.708423447177));
#38635=CARTESIAN_POINT('Ctrl Pts',(-90.8460231303374,-36.2096880966529,
112.700997909761));
#38636=CARTESIAN_POINT('Ctrl Pts',(-90.7722168019337,-35.0536859832189,
112.640922864614));
#38637=CARTESIAN_POINT('Ctrl Pts',(-89.3080212851796,-33.0713464545818,
112.528198311736));
#38638=CARTESIAN_POINT('Ctrl Pts',(-85.8606183524605,-33.2708337842943,
112.370249788544));
#38639=CARTESIAN_POINT('Ctrl Pts',(-84.1430840844366,-36.2665737952763,
112.212301265351));
#38640=CARTESIAN_POINT('Ctrl Pts',(-85.7126545654799,-39.3424201308827,
112.054352742159));
#38641=CARTESIAN_POINT('Ctrl Pts',(-89.1462479767601,-39.7095964662598,
111.896404218967));
#38642=CARTESIAN_POINT('Ctrl Pts',(-90.7410211189894,-37.7571591976099,
111.781094453973));
#38643=CARTESIAN_POINT('Ctrl Pts',(-90.8451885005493,-36.5505847007566,
111.71843419671));
#38644=CARTESIAN_POINT('Ctrl Pts',(-90.8434556139163,-36.3575218683383,
111.708423447177));
#38645=CARTESIAN_POINT('Ctrl Pts',(-90.8402145091085,-36.3574820750184,
112.791576552823));
#38646=CARTESIAN_POINT('Ctrl Pts',(-90.8345154562364,-35.6449586686011,
112.754730079097));
#38647=CARTESIAN_POINT('Ctrl Pts',(-90.2341641452897,-33.9056535345118,
112.66523409764));
#38648=CARTESIAN_POINT('Ctrl Pts',(-87.3482310363601,-32.7528187283548,
112.523088608452));
#38649=CARTESIAN_POINT('Ctrl Pts',(-84.5225496142588,-34.7377386154233,
112.365140085259));
#38650=CARTESIAN_POINT('Ctrl Pts',(-84.6399230862583,-38.1889131872696,
112.207191562067));
#38651=CARTESIAN_POINT('Ctrl Pts',(-87.5939324950497,-39.9772674223311,
112.049243038875));
#38652=CARTESIAN_POINT('Ctrl Pts',(-90.3237946343547,-38.6651865970509,
111.91070470246));
#38653=CARTESIAN_POINT('Ctrl Pts',(-90.8348261204439,-36.9966108268173,
111.824815873776));
#38654=CARTESIAN_POINT('Ctrl Pts',(-90.8385929968401,-36.3529840191205,
111.791576552823));
#38655=CARTESIAN_POINT('Origin',(-87.7685555885722,-36.3549260746835,124.208423447177));
#38656=CARTESIAN_POINT('',(-90.8469566168618,-36.3543571629327,113.791576552823));
#38657=CARTESIAN_POINT('',(-90.837300689892,-36.3544727396314,113.708423447177));
#38658=CARTESIAN_POINT('',(-90.8420555885722,-36.3549260746832,124.208423447177));
#38659=CARTESIAN_POINT('Ctrl Pts',(-90.837300689892,-36.3544727396314,113.708423447178));
#38660=CARTESIAN_POINT('Ctrl Pts',(-90.8379418665799,-35.872554563717,113.683561622813));
#38661=CARTESIAN_POINT('Ctrl Pts',(-90.5047601145692,-34.370924135607,113.606050290717));
#38662=CARTESIAN_POINT('Ctrl Pts',(-88.1657423456717,-32.7501941245154,
113.475889450891));
#38663=CARTESIAN_POINT('Ctrl Pts',(-84.9672568878733,-34.0517597016134,
113.317940927699));
#38664=CARTESIAN_POINT('Ctrl Pts',(-84.3086237643501,-37.4415361815354,
113.159992404506));
#38665=CARTESIAN_POINT('Ctrl Pts',(-86.7870055967793,-39.8461163253272,
113.002043881314));
#38666=CARTESIAN_POINT('Ctrl Pts',(-89.9969760262728,-39.1211063400793,
112.851520895538));
#38667=CARTESIAN_POINT('Ctrl Pts',(-90.8377922257333,-37.2238582333192,
112.753647417492));
#38668=CARTESIAN_POINT('Ctrl Pts',(-90.8448622668699,-36.352723779621,112.708423447177));
#38669=CARTESIAN_POINT('Ctrl Pts',(-90.8469566168618,-36.3543571629327,
113.791576552823));
#38670=CARTESIAN_POINT('Ctrl Pts',(-90.8470373001381,-36.3229528215875,
113.789943299879));
#38671=CARTESIAN_POINT('Ctrl Pts',(-90.8324321314168,-35.2792756470073,
113.735660539204));
#38672=CARTESIAN_POINT('Ctrl Pts',(-89.6566505635712,-33.2586464637551,
113.628728270799));
#38673=CARTESIAN_POINT('Ctrl Pts',(-86.2080377498421,-33.081299013048,113.470779747607));
#38674=CARTESIAN_POINT('Ctrl Pts',(-84.1742989994849,-35.8720496562593,
113.312831224414));
#38675=CARTESIAN_POINT('Ctrl Pts',(-85.3993633840806,-39.1006096620336,
113.154882701222));
#38676=CARTESIAN_POINT('Ctrl Pts',(-88.7725022847651,-39.8397418653489,
112.996934178029));
#38677=CARTESIAN_POINT('Ctrl Pts',(-90.6608462681957,-37.983942532784,112.875832128563));
#38678=CARTESIAN_POINT('Ctrl Pts',(-90.842658768144,-36.6630752697567,112.807379586827));
#38679=CARTESIAN_POINT('Ctrl Pts',(-90.8402145091085,-36.3574820750184,
112.791576552823));
#38680=CARTESIAN_POINT('Origin',(-87.7685555885722,-36.3549260746835,124.208423447177));
#38681=CARTESIAN_POINT('',(-90.8387238989822,-36.3529100687362,114.791576552823));
#38682=CARTESIAN_POINT('',(-90.8432614306157,-36.357555014658,114.708423447177));
#38683=CARTESIAN_POINT('',(-90.8420555885722,-36.3549260746832,124.208423447177));
#38684=CARTESIAN_POINT('Ctrl Pts',(-90.8432614306156,-36.357555014658,114.708423447177));
#38685=CARTESIAN_POINT('Ctrl Pts',(-90.835899599694,-35.5416796238816,114.666125335864));
#38686=CARTESIAN_POINT('Ctrl Pts',(-90.0845449691903,-33.6982785475639,
114.571177716821));
#38687=CARTESIAN_POINT('Ctrl Pts',(-86.9809435225561,-32.814937799838,114.423580590046));
#38688=CARTESIAN_POINT('Ctrl Pts',(-84.3737817930479,-35.0792456171238,
114.265632066854));
#38689=CARTESIAN_POINT('Ctrl Pts',(-84.8445582165638,-38.5001741072118,
114.107683543661));
#38690=CARTESIAN_POINT('Ctrl Pts',(-87.9664341279196,-39.9760714509759,
113.949735020469));
#38691=CARTESIAN_POINT('Ctrl Pts',(-90.445741982759,-38.4532613953824,113.816648321641));
#38692=CARTESIAN_POINT('Ctrl Pts',(-90.8365840564492,-36.8931053630604,
113.736211130544));
#38693=CARTESIAN_POINT('Ctrl Pts',(-90.837300689892,-36.3544727396314,113.708423447178));
#38694=CARTESIAN_POINT('Ctrl Pts',(-90.8387238989822,-36.3529100687362,
114.791576552823));
#38695=CARTESIAN_POINT('Ctrl Pts',(-90.8409734017537,-35.9836982214461,
114.772507012931));
#38696=CARTESIAN_POINT('Ctrl Pts',(-90.6090449884476,-34.5978521515366,
114.700787965308));
#38697=CARTESIAN_POINT('Ctrl Pts',(-88.556167663902,-32.8149377579708,114.576419409954));
#38698=CARTESIAN_POINT('Ctrl Pts',(-85.2349019889955,-33.760229656792,114.418470886761));
#38699=CARTESIAN_POINT('Ctrl Pts',(-84.2108229752343,-37.058053883591,114.260522363569));
#38700=CARTESIAN_POINT('Ctrl Pts',(-86.4124319184404,-39.7183735107193,
114.102573840377));
#38701=CARTESIAN_POINT('Ctrl Pts',(-89.8081172856445,-39.3331822950034,
113.946258570128));
#38702=CARTESIAN_POINT('Ctrl Pts',(-90.8444363957291,-37.335302512349,113.84259280761));
#38703=CARTESIAN_POINT('Ctrl Pts',(-90.8469566168618,-36.3543571629327,
113.791576552823));
#38704=CARTESIAN_POINT('Origin',(-87.7685555885722,-36.3549260746835,124.208423447177));
#38705=CARTESIAN_POINT('',(-90.8400417237333,-36.357441449847,115.791576552823));
#38706=CARTESIAN_POINT('',(-90.8450341690572,-36.3527935650275,115.708423447177));
#38707=CARTESIAN_POINT('',(-90.8420555885722,-36.3549260746832,124.208423447177));
#38708=CARTESIAN_POINT('Ctrl Pts',(-90.8450341690572,-36.3527935650275,
115.708423447177));
#38709=CARTESIAN_POINT('Ctrl Pts',(-90.846116704552,-36.216339568469,115.701338556647));
#38710=CARTESIAN_POINT('Ctrl Pts',(-90.7761239871613,-35.0669805123168,
115.641604158385));
#38711=CARTESIAN_POINT('Ctrl Pts',(-89.3290734088453,-33.081299051764,115.529220252393));
#38712=CARTESIAN_POINT('Ctrl Pts',(-85.8804606359022,-33.2586465003749,
115.371271729201));
#38713=CARTESIAN_POINT('Ctrl Pts',(-84.1437261327331,-36.243296469925,115.213323206008));
#38714=CARTESIAN_POINT('Ctrl Pts',(-85.6935142529687,-39.3291576070487,
115.055374682816));
#38715=CARTESIAN_POINT('Ctrl Pts',(-89.1246792426668,-39.7183734709399,
114.897426159623));
#38716=CARTESIAN_POINT('Ctrl Pts',(-90.7367043057794,-37.7704789876537,
114.781775747744));
#38717=CARTESIAN_POINT('Ctrl Pts',(-90.8450630531436,-36.5572199485125,
114.718774843595));
#38718=CARTESIAN_POINT('Ctrl Pts',(-90.8432614306156,-36.357555014658,114.708423447177));
#38719=CARTESIAN_POINT('Ctrl Pts',(-90.8400417237333,-36.357441449847,115.791576552823));
#38720=CARTESIAN_POINT('Ctrl Pts',(-90.8345081309196,-35.6514047555258,
115.755070725982));
#38721=CARTESIAN_POINT('Ctrl Pts',(-90.2429419326533,-33.9187286136303,
115.665915391411));
#38722=CARTESIAN_POINT('Ctrl Pts',(-87.3713688267741,-32.750194081883,115.524110549109));
#38723=CARTESIAN_POINT('Ctrl Pts',(-84.5330004881805,-34.7169293542972,
115.366162025916));
#38724=CARTESIAN_POINT('Ctrl Pts',(-84.628211554152,-38.1687864356674,115.208213502724));
#38725=CARTESIAN_POINT('Ctrl Pts',(-87.5706770468859,-39.9760714938026,
115.050264979531));
#38726=CARTESIAN_POINT('Ctrl Pts',(-90.3156407155774,-38.6783630959069,
114.911385996231));
#38727=CARTESIAN_POINT('Ctrl Pts',(-90.834762700592,-37.0030632464158,114.825156520661));
#38728=CARTESIAN_POINT('Ctrl Pts',(-90.8387238989822,-36.3529100687362,
114.791576552823));
#38729=CARTESIAN_POINT('Origin',(-87.7685555885722,-36.3549260746835,124.208423447177));
#38730=CARTESIAN_POINT('',(-90.8470055221225,-36.3544743326472,116.791576552823));
#38731=CARTESIAN_POINT('',(-90.8373333345046,-36.3543684810828,116.708423447177));
#38732=CARTESIAN_POINT('',(-90.8420555885722,-36.3549260746832,124.208423447177));
#38733=CARTESIAN_POINT('Ctrl Pts',(-90.8373333345046,-36.3543684810828,
116.708423447177));
#38734=CARTESIAN_POINT('Ctrl Pts',(-90.838111639097,-35.8790659960872,116.683902269699));
#38735=CARTESIAN_POINT('Ctrl Pts',(-90.5113488468397,-34.3842533323872,
116.606731584489));
#38736=CARTESIAN_POINT('Ctrl Pts',(-88.1888801358119,-32.7528187709561,
116.476911391548));
#38737=CARTESIAN_POINT('Ctrl Pts',(-84.9821032637396,-34.0338200465123,
116.318962868356));
#38738=CARTESIAN_POINT('Ctrl Pts',(-84.3017179684765,-37.4192975645625,
116.161014345163));
#38739=CARTESIAN_POINT('Ctrl Pts',(-86.7646089042542,-39.839741824135,116.003065821971));
#38740=CARTESIAN_POINT('Ctrl Pts',(-89.9864432824828,-39.1337639166678,
115.852202189309));
#38741=CARTESIAN_POINT('Ctrl Pts',(-90.8380721256472,-37.2303616928352,
115.753988064378));
#38742=CARTESIAN_POINT('Ctrl Pts',(-90.8450341690572,-36.3527935650275,
115.708423447177));
#38743=CARTESIAN_POINT('Ctrl Pts',(-90.8470055221225,-36.3544743326472,
116.791576552823));
#38744=CARTESIAN_POINT('Ctrl Pts',(-90.8470570093793,-36.3296210426277,
116.790283946765));
#38745=CARTESIAN_POINT('Ctrl Pts',(-90.8355715211677,-35.2925100683326,
116.736341832976));
#38746=CARTESIAN_POINT('Ctrl Pts',(-89.6764928472477,-33.2708337478186,
116.629750211456));
#38747=CARTESIAN_POINT('Ctrl Pts',(-86.2290898737567,-33.071346415748,116.471801688264));
#38748=CARTESIAN_POINT('Ctrl Pts',(-84.1774736431561,-35.848980894873,116.313853165071));
#38749=CARTESIAN_POINT('Ctrl Pts',(-85.3817821946438,-39.0853404809052,
116.155904641879));
#38750=CARTESIAN_POINT('Ctrl Pts',(-88.7501055919751,-39.8461163666165,
115.997956118686));
#38751=CARTESIAN_POINT('Ctrl Pts',(-90.655671847336,-37.9972943972299,115.876513422334));
#38752=CARTESIAN_POINT('Ctrl Pts',(-90.8424888003863,-36.6696664308027,
115.807720233713));
#38753=CARTESIAN_POINT('Ctrl Pts',(-90.8400417237333,-36.357441449847,115.791576552823));
#38754=CARTESIAN_POINT('Origin',(-87.7685555885722,-36.3549260746835,124.208423447177));
#38755=CARTESIAN_POINT('',(-90.838859936608,-36.3528391395051,117.791576552823));
#38756=CARTESIAN_POINT('',(-90.8430662275438,-36.3575836912129,117.708423447178));
#38757=CARTESIAN_POINT('',(-90.8420555885722,-36.3549260746832,124.208423447177));
#38758=CARTESIAN_POINT('Ctrl Pts',(-90.8430662275438,-36.3575836912129,
117.708423447178));
#38759=CARTESIAN_POINT('Ctrl Pts',(-90.8357358095233,-35.5481464964534,
117.66646598275));
#38760=CARTESIAN_POINT('Ctrl Pts',(-90.0944058341935,-33.7111196198065,
117.571859010592));
#38761=CARTESIAN_POINT('Ctrl Pts',(-87.0036900180789,-32.8099535202534,
117.424602530703));
#38762=CARTESIAN_POINT('Ctrl Pts',(-84.382042917881,-35.0574740779507,117.26665400751));
#38763=CARTESIAN_POINT('Ctrl Pts',(-84.8308438600728,-38.4813549008641,
117.108705484318));
#38764=CARTESIAN_POINT('Ctrl Pts',(-87.9431786800308,-39.9772673794902,
116.950756961126));
#38765=CARTESIAN_POINT('Ctrl Pts',(-90.4385842843359,-38.4665514124466,
116.817329615412));
#38766=CARTESIAN_POINT('Ctrl Pts',(-90.8364405385272,-36.8995896589381,
116.736551777429));
#38767=CARTESIAN_POINT('Ctrl Pts',(-90.8373333345046,-36.3543684810828,
116.708423447177));
#38768=CARTESIAN_POINT('Ctrl Pts',(-90.838859936608,-36.3528391395051,117.791576552823));
#38769=CARTESIAN_POINT('Ctrl Pts',(-90.8411535687101,-35.9902631012329,
117.772847659816));
#38770=CARTESIAN_POINT('Ctrl Pts',(-90.6146772191493,-34.6112077247612,
117.701469259079));
#38771=CARTESIAN_POINT('Ctrl Pts',(-88.5788816867368,-32.8200679900657,
117.577441350611));
#38772=CARTESIAN_POINT('Ctrl Pts',(-85.2516147613512,-33.7440145603012,
117.419492827418));
#38773=CARTESIAN_POINT('Ctrl Pts',(-84.2063815347296,-37.0351951933252,
117.261544304226));
#38774=CARTESIAN_POINT('Ctrl Pts',(-86.390863184092,-39.7095965059354,117.103595781033));
#38775=CARTESIAN_POINT('Ctrl Pts',(-89.7963570779285,-39.3454250335693,
116.946939863899));
#38776=CARTESIAN_POINT('Ctrl Pts',(-90.8449598671701,-37.3419275198467,
116.842933454495));
#38777=CARTESIAN_POINT('Ctrl Pts',(-90.8470055221225,-36.3544743326472,
116.791576552823));
#38778=CARTESIAN_POINT('Origin',(-87.7685555885722,-36.3549260746835,124.208423447177));
#38779=CARTESIAN_POINT('',(-90.8398724656877,-36.357396938907,118.791576552823));
#38780=CARTESIAN_POINT('',(-90.8452018287892,-36.3528672805891,118.708423447178));
#38781=CARTESIAN_POINT('',(-90.8420555885722,-36.3549260746832,124.208423447177));
#38782=CARTESIAN_POINT('Ctrl Pts',(-90.8452018287892,-36.3528672805891,
118.708423447178));
#38783=CARTESIAN_POINT('Ctrl Pts',(-90.8462062638201,-36.2229926114565,
118.701679203533));
#38784=CARTESIAN_POINT('Ctrl Pts',(-90.7799844648685,-35.0802718156704,
118.642285452157));
#38785=CARTESIAN_POINT('Ctrl Pts',(-89.350061192869,-33.0913866196758,118.53024219305));
#38786=CARTESIAN_POINT('Ctrl Pts',(-85.9003807648513,-33.2465868748436,
118.372293669858));
#38787=CARTESIAN_POINT('Ctrl Pts',(-84.1445176314521,-36.2200237470817,
118.214345146665));
#38788=CARTESIAN_POINT('Ctrl Pts',(-85.6744594936806,-39.3157724566742,
118.056396623473));
#38789=CARTESIAN_POINT('Ctrl Pts',(-89.1030545960746,-39.7270118018916,
117.89844810028));
#38790=CARTESIAN_POINT('Ctrl Pts',(-90.7323387978003,-37.783801391323,117.782457041515));
#38791=CARTESIAN_POINT('Ctrl Pts',(-90.8449342419241,-36.5638530083872,
117.719115490481));
#38792=CARTESIAN_POINT('Ctrl Pts',(-90.8430662275438,-36.3575836912129,
117.708423447178));
#38793=CARTESIAN_POINT('Ctrl Pts',(-90.8398724656877,-36.357396938907,118.791576552823));
#38794=CARTESIAN_POINT('Ctrl Pts',(-90.8345089923071,-35.6578509331832,
118.755411372868));
#38795=CARTESIAN_POINT('Ctrl Pts',(-90.2516537491596,-33.931815551476,118.666596685182));
#38796=CARTESIAN_POINT('Ctrl Pts',(-87.3945229938104,-32.7477180564772,
118.525132489766));
#38797=CARTESIAN_POINT('Ctrl Pts',(-84.5435847625254,-34.6961876275626,
118.367183966573));
#38798=CARTESIAN_POINT('Ctrl Pts',(-84.6166294974947,-38.1485848990669,
118.209235443381));
#38799=CARTESIAN_POINT('Ctrl Pts',(-87.5474297570977,-39.9747262668198,
118.051286920188));
#38800=CARTESIAN_POINT('Ctrl Pts',(-90.3074226582739,-38.6915302645955,
117.912067290002));
#38801=CARTESIAN_POINT('Ctrl Pts',(-90.8347058517495,-37.0095144752193,
117.825497167547));
#38802=CARTESIAN_POINT('Ctrl Pts',(-90.838859936608,-36.3528391395051,117.791576552823));
#38803=CARTESIAN_POINT('Origin',(-87.7685555885722,-36.3549260746835,124.208423447177));
#38804=CARTESIAN_POINT('',(-90.8470437519384,-36.3545924749754,119.791576552823));
#38805=CARTESIAN_POINT('',(-90.8373727075233,-36.3542650492899,119.708423447177));
#38806=CARTESIAN_POINT('',(-90.8420555885722,-36.3549260746832,124.208423447177));
#38807=CARTESIAN_POINT('Ctrl Pts',(-90.8373727075233,-36.3542650492899,
119.708423447177));
#38808=CARTESIAN_POINT('Ctrl Pts',(-90.8382832605688,-35.8855804672779,
119.684242916584));
#38809=CARTESIAN_POINT('Ctrl Pts',(-90.5178794747935,-34.3975854901708,
119.60741287826));
#38810=CARTESIAN_POINT('Ctrl Pts',(-88.2120005926768,-32.7555919497842,
119.477933332205));
#38811=CARTESIAN_POINT('Ctrl Pts',(-84.9970645257212,-34.0159760806577,
119.319984809012));
#38812=CARTESIAN_POINT('Ctrl Pts',(-84.2949551082748,-37.3970150683708,
119.16203628582));
#38813=CARTESIAN_POINT('Ctrl Pts',(-86.7422536044908,-39.8332236430662,
119.004087762628));
#38814=CARTESIAN_POINT('Ctrl Pts',(-89.9758395670128,-39.1464003470619,
118.85288348308));
#38815=CARTESIAN_POINT('Ctrl Pts',(-90.8383650569023,-37.2368701871385,
118.754328711263));
#38816=CARTESIAN_POINT('Ctrl Pts',(-90.8452018287892,-36.3528672805891,
118.708423447178));
#38817=CARTESIAN_POINT('Ctrl Pts',(-90.8470437519384,-36.3545924749754,
119.791576552823));
#38818=CARTESIAN_POINT('Ctrl Pts',(-90.84707219677,-36.3362895054686,119.79062459365));
#38819=CARTESIAN_POINT('Ctrl Pts',(-90.838667553572,-35.3057405991472,119.737023126747));
#38820=CARTESIAN_POINT('Ctrl Pts',(-89.6962563501485,-33.2831483055448,
119.630772152113));
#38821=CARTESIAN_POINT('Ctrl Pts',(-86.2502055262826,-33.0615291420779,
119.47282362892));
#38822=CARTESIAN_POINT('Ctrl Pts',(-84.1807963181542,-35.8259330212369,
119.314875105728));
#38823=CARTESIAN_POINT('Ctrl Pts',(-85.3642994245004,-39.0699587122372,
119.156926582536));
#38824=CARTESIAN_POINT('Ctrl Pts',(-88.7276684236758,-39.8523469339212,
118.998978059343));
#38825=CARTESIAN_POINT('Ctrl Pts',(-90.6504449905735,-38.010647188406,118.877194716105));
#38826=CARTESIAN_POINT('Ctrl Pts',(-90.8423171722627,-36.6762546265272,
118.808060880599));
#38827=CARTESIAN_POINT('Ctrl Pts',(-90.8398724656877,-36.357396938907,118.791576552823));
#38828=CARTESIAN_POINT('Origin',(-87.7685555885722,-36.3549260746835,124.208423447177));
#38829=CARTESIAN_POINT('',(-90.8389971204791,-36.3527751889037,120.791576552823));
#38830=CARTESIAN_POINT('',(-90.8428699659751,-36.357609793043,120.708423447177));
#38831=CARTESIAN_POINT('',(-90.8420555885722,-36.3549260746832,124.208423447177));
#38832=CARTESIAN_POINT('Ctrl Pts',(-90.8428699659751,-36.357609793043,120.708423447177));
#38833=CARTESIAN_POINT('Ctrl Pts',(-90.8355828378088,-35.5546125768694,
120.666806629636));
#38834=CARTESIAN_POINT('Ctrl Pts',(-90.1041980565863,-33.72397525936,120.572540304363));
#38835=CARTESIAN_POINT('Ctrl Pts',(-87.0264677882008,-32.8051168197105,
120.42562447136));
#38836=CARTESIAN_POINT('Ctrl Pts',(-84.3904437941137,-35.0357553412809,
120.267675948167));
#38837=CARTESIAN_POINT('Ctrl Pts',(-84.8172505627962,-38.4624483585915,
120.109727424975));
#38838=CARTESIAN_POINT('Ctrl Pts',(-87.9199160624454,-39.9783137967903,
119.951778901782));
#38839=CARTESIAN_POINT('Ctrl Pts',(-90.4313660245834,-38.4798362252759,
119.818010909183));
#38840=CARTESIAN_POINT('Ctrl Pts',(-90.8363006667865,-36.9060714126157,
119.736892424315));
#38841=CARTESIAN_POINT('Ctrl Pts',(-90.8373727075233,-36.3542650492899,
119.708423447177));
#38842=CARTESIAN_POINT('Ctrl Pts',(-90.8389971204791,-36.3527751889037,
120.791576552823));
#38843=CARTESIAN_POINT('Ctrl Pts',(-90.8413324494673,-35.9968317106162,
120.773188306702));
#38844=CARTESIAN_POINT('Ctrl Pts',(-90.6202676404303,-34.6245509810165,
120.70215055285));
#38845=CARTESIAN_POINT('Ctrl Pts',(-88.6015534311407,-32.8253528646868,
120.578463291268));
#38846=CARTESIAN_POINT('Ctrl Pts',(-85.2684356186448,-33.7279027825514,
120.420514768075));
#38847=CARTESIAN_POINT('Ctrl Pts',(-84.2020848645994,-37.0123105603124,
120.262566244883));
#38848=CARTESIAN_POINT('Ctrl Pts',(-86.3693522710391,-39.7006801660047,
120.10461772169));
#38849=CARTESIAN_POINT('Ctrl Pts',(-89.7845229475026,-39.3576400610631,
119.94762115767));
#38850=CARTESIAN_POINT('Ctrl Pts',(-90.8454990133535,-37.3485622609709,
119.843274101381));
#38851=CARTESIAN_POINT('Ctrl Pts',(-90.8470437519384,-36.3545924749754,
119.791576552823));
#38852=CARTESIAN_POINT('Origin',(-87.7685555885722,-36.3549260746835,124.208423447177));
#38853=CARTESIAN_POINT('',(-90.8388341582581,-36.3579404435482,121.791576552823));
#38854=CARTESIAN_POINT('',(-90.8453551362697,-36.3529984899081,121.708423447177));
#38855=CARTESIAN_POINT('',(-90.8420555885722,-36.3549260746832,124.208423447177));
#38856=CARTESIAN_POINT('',(-88.5623548711056,-39.3241490284291,122.));
#38857=CARTESIAN_POINT('Ctrl Pts',(-88.5623548711056,-39.3241490284291,
122.));
#38858=CARTESIAN_POINT('Ctrl Pts',(-89.5445934608772,-39.0615549760513,
121.947350492269));
#38859=CARTESIAN_POINT('Ctrl Pts',(-90.644289976571,-38.0238171899135,121.877876009877));
#38860=CARTESIAN_POINT('Ctrl Pts',(-90.8411753108947,-36.6834161555448,
121.808401527484));
#38861=CARTESIAN_POINT('Ctrl Pts',(-90.8388341582581,-36.3579404435482,
121.791576552823));
#38862=CARTESIAN_POINT('',(-86.9728468160199,-39.3292254485229,122.));
#38863=CARTESIAN_POINT('Origin',(-87.7685555885722,-36.3549260746835,122.));
#38864=CARTESIAN_POINT('Ctrl Pts',(-86.9728421809427,-39.3292377709744,
122.));
#38865=CARTESIAN_POINT('Ctrl Pts',(-87.9198084892423,-39.5801183955144,
121.949053726697));
#38866=CARTESIAN_POINT('Ctrl Pts',(-89.9803573410806,-39.1252163986582,
121.851861542423));
#38867=CARTESIAN_POINT('Ctrl Pts',(-90.8386916486268,-37.2432731849997,
121.754669358149));
#38868=CARTESIAN_POINT('Ctrl Pts',(-90.8453551362697,-36.3529984899081,
121.708423447177));
#38869=CARTESIAN_POINT('Origin',(36.3549260746835,-87.7685555885722,114.));
#38870=CARTESIAN_POINT('',(33.8414157234842,-87.7682981463998,107.387416697508));
#38871=CARTESIAN_POINT('',(33.839334999722,-87.7721278037521,107.112583302492));
#38872=CARTESIAN_POINT('',(33.8374260746835,-87.7685555885722,114.));
#38873=CARTESIAN_POINT('',(34.4414600780189,-86.1325683851968,107.));
#38874=CARTESIAN_POINT('Ctrl Pts',(33.839334999722,-87.7721278037521,107.112583302492));
#38875=CARTESIAN_POINT('Ctrl Pts',(33.8444805530708,-87.1794933281653,107.075055534995));
#38876=CARTESIAN_POINT('Ctrl Pts',(34.0557042465997,-86.5837520282674,107.037527767497));
#38877=CARTESIAN_POINT('Ctrl Pts',(34.441460078019,-86.1325683851967,107.));
#38878=CARTESIAN_POINT('',(33.8374260746835,-87.7685555885722,107.));
#38879=CARTESIAN_POINT('Origin',(36.3549260746835,-87.7685555885722,107.));
#38880=CARTESIAN_POINT('',(33.8374260746835,-87.7685555885722,106.));
#38881=CARTESIAN_POINT('',(33.8374260746835,-87.7685555885722,114.));
#38882=CARTESIAN_POINT('Origin',(36.3549260746835,-87.7685555885722,106.));
#38883=CARTESIAN_POINT('',(38.2720363880079,-86.1300276126115,107.));
#38884=CARTESIAN_POINT('Origin',(36.3549260746835,-87.7685555885722,107.));
#38885=CARTESIAN_POINT('Ctrl Pts',(38.2720452344323,-86.1300214449936,107.));
#38886=CARTESIAN_POINT('Ctrl Pts',(37.7492246942328,-85.5213064718756,107.050946273303));
#38887=CARTESIAN_POINT('Ctrl Pts',(36.9095001441611,-85.1811299415284,107.101892546605));
#38888=CARTESIAN_POINT('Ctrl Pts',(36.1108292477348,-85.2588926940752,107.152838819908));
#38889=CARTESIAN_POINT('Ctrl Pts',(35.2854572075469,-85.3392552088574,107.205488327639));
#38890=CARTESIAN_POINT('Ctrl Pts',(34.503929715814,-85.8659692054928,107.25813783537));
#38891=CARTESIAN_POINT('Ctrl Pts',(34.1200450888798,-86.6007560202748,107.3107873431));
#38892=CARTESIAN_POINT('Ctrl Pts',(33.9338019348801,-86.9572407667346,107.336330461236));
#38893=CARTESIAN_POINT('Ctrl Pts',(33.8411537247362,-87.3627005243321,107.361873579372));
#38894=CARTESIAN_POINT('Ctrl Pts',(33.8414157234842,-87.7682981463998,107.387416697508));
#38895=CARTESIAN_POINT('Origin',(36.3549260746835,-87.7685555885722,114.));
#38896=CARTESIAN_POINT('',(33.8361212073215,-87.7706510705991,108.387416697508));
#38897=CARTESIAN_POINT('',(33.833519260677,-87.7678892624363,108.112583302492));
#38898=CARTESIAN_POINT('',(33.8374260746835,-87.7685555885722,114.));
#38899=CARTESIAN_POINT('Ctrl Pts',(33.833519260677,-87.7678892624363,108.112583302492));
#38900=CARTESIAN_POINT('Ctrl Pts',(33.8333914248761,-87.7314321292875,108.110268755777));
#38901=CARTESIAN_POINT('Ctrl Pts',(33.8341143758752,-87.6949802329165,108.107954209062));
#38902=CARTESIAN_POINT('Ctrl Pts',(33.8357039923662,-87.6585662348268,108.105639662347));
#38903=CARTESIAN_POINT('Ctrl Pts',(33.8718633514296,-86.8302489398792,108.052990154616));
#38904=CARTESIAN_POINT('Ctrl Pts',(34.3564667264384,-86.0215415840135,108.000340646886));
#38905=CARTESIAN_POINT('Ctrl Pts',(35.0698410633522,-85.5989799369826,107.947691139155));
#38906=CARTESIAN_POINT('Ctrl Pts',(35.7832154002661,-85.1764182899517,107.895041631424));
#38907=CARTESIAN_POINT('Ctrl Pts',(36.725360699085,-85.1400023517557,107.842392123693));
#38908=CARTESIAN_POINT('Ctrl Pts',(37.4691398688133,-85.5064040383691,107.789742615962));
#38909=CARTESIAN_POINT('Ctrl Pts',(38.2129190385417,-85.8728057249826,107.737093108232));
#38910=CARTESIAN_POINT('Ctrl Pts',(38.7583320791794,-86.6420250364055,107.684443600501));
#38911=CARTESIAN_POINT('Ctrl Pts',(38.8581856892655,-87.4650122829143,107.63179409277));
#38912=CARTESIAN_POINT('Ctrl Pts',(38.9580392993515,-88.2879995294231,107.579144585039));
#38913=CARTESIAN_POINT('Ctrl Pts',(38.612333478886,-89.1647547110178,107.526495077308));
#38914=CARTESIAN_POINT('Ctrl Pts',(37.9776636366484,-89.6985066213742,107.473845569577));
#38915=CARTESIAN_POINT('Ctrl Pts',(37.3429937944108,-90.2322585317306,107.421196061847));
#38916=CARTESIAN_POINT('Ctrl Pts',(36.4193599304013,-90.4230071708486,107.368546554116));
#38917=CARTESIAN_POINT('Ctrl Pts',(35.6257427015425,-90.1828530278179,107.315897046385));
#38918=CARTESIAN_POINT('Ctrl Pts',(34.8321254726837,-89.9426988847871,107.263247538654));
#38919=CARTESIAN_POINT('Ctrl Pts',(34.1685248789757,-89.2716419596076,107.210598030923));
#38920=CARTESIAN_POINT('Ctrl Pts',(33.9355596837291,-88.4773561362653,107.157948523192));
#38921=CARTESIAN_POINT('Ctrl Pts',(33.868648532651,-88.2492251544312,107.142826782959));
#38922=CARTESIAN_POINT('Ctrl Pts',(33.8372616091025,-88.0109287021499,107.127705042725));
#38923=CARTESIAN_POINT('Ctrl Pts',(33.839334999722,-87.7721278037521,107.112583302492));
#38924=CARTESIAN_POINT('Ctrl Pts',(33.8414157234842,-87.7682981463998,107.387416697508));
#38925=CARTESIAN_POINT('Ctrl Pts',(33.8416937568902,-88.1987188610546,107.414523087103));
#38926=CARTESIAN_POINT('Ctrl Pts',(33.9466024502664,-88.6292948315277,107.441629476698));
#38927=CARTESIAN_POINT('Ctrl Pts',(34.1553234974974,-89.0016622559541,107.468735866293));
#38928=CARTESIAN_POINT('Ctrl Pts',(34.5607282951845,-89.7249220439228,107.521385374024));
#38929=CARTESIAN_POINT('Ctrl Pts',(35.3577796526943,-90.2285819869318,107.574034881754));
#38930=CARTESIAN_POINT('Ctrl Pts',(36.1850293994859,-90.284432979621,107.626684389485));
#38931=CARTESIAN_POINT('Ctrl Pts',(37.0122791462776,-90.3402839723102,107.679333897216));
#38932=CARTESIAN_POINT('Ctrl Pts',(37.869727282351,-89.9483260146797,107.731983404947));
#38933=CARTESIAN_POINT('Ctrl Pts',(38.3687196497657,-89.28619017419,107.784632912678));
#38934=CARTESIAN_POINT('Ctrl Pts',(38.8677120171805,-88.6240543337003,107.837282420409));
#38935=CARTESIAN_POINT('Ctrl Pts',(39.0082486159366,-87.6917406103514,107.889931928139));
#38936=CARTESIAN_POINT('Ctrl Pts',(38.7265916429298,-86.9119270220054,107.94258143587));
#38937=CARTESIAN_POINT('Ctrl Pts',(38.4449346699229,-86.1321134336593,107.995230943601));
#38938=CARTESIAN_POINT('Ctrl Pts',(37.741084125153,-85.5047999803161,108.047880451332));
#38939=CARTESIAN_POINT('Ctrl Pts',(36.9341334049065,-85.3143561749413,108.100529959063));
#38940=CARTESIAN_POINT('Ctrl Pts',(36.1271826846599,-85.1239123695665,108.153179466794));
#38941=CARTESIAN_POINT('Ctrl Pts',(35.2171317889366,-85.3703382121602,108.205828974524));
#38942=CARTESIAN_POINT('Ctrl Pts',(34.6165319102364,-85.9419268590616,108.258478482255));
#38943=CARTESIAN_POINT('Ctrl Pts',(34.126243841216,-86.4085321713532,108.301457887339));
#38944=CARTESIAN_POINT('Ctrl Pts',(33.8421725915064,-87.0918245700457,108.344437292424));
#38945=CARTESIAN_POINT('Ctrl Pts',(33.8361212073215,-87.7706510705991,108.387416697508));
#38946=CARTESIAN_POINT('Origin',(36.3549260746835,-87.7685555885722,114.));
#38947=CARTESIAN_POINT('',(33.8352710252958,-87.7666978305704,109.387416697508));
#38948=CARTESIAN_POINT('',(33.8403654904393,-87.7670276461582,109.112583302492));
#38949=CARTESIAN_POINT('',(33.8374260746835,-87.7685555885722,114.));
#38950=CARTESIAN_POINT('Ctrl Pts',(33.8403654904393,-87.7670276461582,109.112583302492));
#38951=CARTESIAN_POINT('Ctrl Pts',(33.8386092352284,-87.4537363502728,109.092832468829));
#38952=CARTESIAN_POINT('Ctrl Pts',(33.8929064240409,-87.1410318741097,109.073081635165));
#38953=CARTESIAN_POINT('Ctrl Pts',(34.0060459886766,-86.851305712434,109.053330801502));
#38954=CARTESIAN_POINT('Ctrl Pts',(34.3076404673954,-86.0789869309084,109.000681293771));
#38955=CARTESIAN_POINT('Ctrl Pts',(35.0273617091834,-85.4699492562897,108.94803178604));
#38956=CARTESIAN_POINT('Ctrl Pts',(35.8389352257471,-85.3002896064973,108.89538227831));
#38957=CARTESIAN_POINT('Ctrl Pts',(36.6505087423109,-85.1306299567049,108.842732770579));
#38958=CARTESIAN_POINT('Ctrl Pts',(37.5539345336504,-85.4003483317387,108.790083262848));
#38959=CARTESIAN_POINT('Ctrl Pts',(38.1396578606632,-85.9871741676922,108.737433755117));
#38960=CARTESIAN_POINT('Ctrl Pts',(38.7253811876761,-86.5740000036457,108.684784247386));
#38961=CARTESIAN_POINT('Ctrl Pts',(38.9934020503622,-87.4779333005189,108.632134739655));
#38962=CARTESIAN_POINT('Ctrl Pts',(38.8222180782562,-88.2891852027425,108.579485231925));
#38963=CARTESIAN_POINT('Ctrl Pts',(38.6510341061502,-89.1004371049661,108.526835724194));
#38964=CARTESIAN_POINT('Ctrl Pts',(38.0406452992521,-89.81900761254,108.474186216463));
#38965=CARTESIAN_POINT('Ctrl Pts',(37.2677604715886,-90.1191528459469,108.421536708732));
#38966=CARTESIAN_POINT('Ctrl Pts',(36.4948756439251,-90.4192980793539,108.368887201001));
#38967=CARTESIAN_POINT('Ctrl Pts',(35.5594947954961,-90.3010180385939,108.316237693271));
#38968=CARTESIAN_POINT('Ctrl Pts',(34.8856620428406,-89.817914401199,108.26358818554));
#38969=CARTESIAN_POINT('Ctrl Pts',(34.2414519296223,-89.3560486819745,108.213253224524));
#38970=CARTESIAN_POINT('Ctrl Pts',(33.8362993342051,-88.5607306269994,108.162918263508));
#38971=CARTESIAN_POINT('Ctrl Pts',(33.833519260677,-87.7678892624363,108.112583302492));
#38972=CARTESIAN_POINT('Ctrl Pts',(33.8361212073215,-87.7706510705991,108.387416697508));
#38973=CARTESIAN_POINT('Ctrl Pts',(33.8347596829796,-87.9233828714858,108.397086800155));
#38974=CARTESIAN_POINT('Ctrl Pts',(33.8474721473246,-88.0758885985998,108.406756902801));
#38975=CARTESIAN_POINT('Ctrl Pts',(33.8750764150749,-88.2256493871394,108.416427005448));
#38976=CARTESIAN_POINT('Ctrl Pts',(34.0253696602909,-89.0410318171065,108.469076513179));
#38977=CARTESIAN_POINT('Ctrl Pts',(34.6171050124002,-89.7750452258316,108.521726020909));
#38978=CARTESIAN_POINT('Ctrl Pts',(35.3820267013402,-90.0949373484143,108.57437552864));
#38979=CARTESIAN_POINT('Ctrl Pts',(36.1469483902803,-90.4148294709971,108.627025036371));
#38980=CARTESIAN_POINT('Ctrl Pts',(37.0850564160513,-90.3206003074374,108.679674544102));
#38981=CARTESIAN_POINT('Ctrl Pts',(37.7710745227806,-89.8549664615314,108.732324051833));
#38982=CARTESIAN_POINT('Ctrl Pts',(38.4570926295099,-89.3893326156255,108.784973559563));
#38983=CARTESIAN_POINT('Ctrl Pts',(38.8910208171977,-88.5522940873732,108.837623067294));
#38984=CARTESIAN_POINT('Ctrl Pts',(38.8761439749966,-87.7233099317579,108.890272575025));
#38985=CARTESIAN_POINT('Ctrl Pts',(38.8612671327955,-86.8943257761426,108.942922082756));
#38986=CARTESIAN_POINT('Ctrl Pts',(38.3975852607055,-86.0733959931642,108.995571590487));
#38987=CARTESIAN_POINT('Ctrl Pts',(37.6953016620874,-85.6326764378238,109.048221098218));
#38988=CARTESIAN_POINT('Ctrl Pts',(36.9930180634693,-85.1919568824835,109.100870605948));
#38989=CARTESIAN_POINT('Ctrl Pts',(36.052132738323,-85.131447554781,109.153520113679));
#38990=CARTESIAN_POINT('Ctrl Pts',(35.2991816545013,-85.4785795250109,109.20616962141));
#38991=CARTESIAN_POINT('Ctrl Pts',(34.5462305706795,-85.8257114952409,109.258819129141));
#38992=CARTESIAN_POINT('Ctrl Pts',(33.9812137281822,-86.5804847634032,109.311468636872));
#38993=CARTESIAN_POINT('Ctrl Pts',(33.8602729624767,-87.4007343039005,109.364118144603));
#38994=CARTESIAN_POINT('Ctrl Pts',(33.8424333222492,-87.5217270610896,109.371884328904));
#38995=CARTESIAN_POINT('Ctrl Pts',(33.8342560624626,-87.6441444765438,109.379650513206));
#38996=CARTESIAN_POINT('Ctrl Pts',(33.8352710252958,-87.7666978305704,109.387416697508));
#38997=CARTESIAN_POINT('Origin',(36.3549260746835,-87.7685555885722,114.));
#38998=CARTESIAN_POINT('',(33.8413419169939,-87.7682702011519,110.387416697508));
#38999=CARTESIAN_POINT('',(33.838790157295,-87.7706792333693,110.112583302492));
#39000=CARTESIAN_POINT('',(33.8374260746835,-87.7685555885722,114.));
#39001=CARTESIAN_POINT('Ctrl Pts',(33.838790157295,-87.7706792333693,110.112583302492));
#39002=CARTESIAN_POINT('Ctrl Pts',(33.8435896215492,-87.1817422166418,110.07539618188));
#39003=CARTESIAN_POINT('Ctrl Pts',(34.0501481060936,-86.5897716217229,110.038209061269));
#39004=CARTESIAN_POINT('Ctrl Pts',(34.4278436124566,-86.1422290384201,110.001021940657));
#39005=CARTESIAN_POINT('Ctrl Pts',(34.9625847312916,-85.5085984611698,109.948372432926));
#39006=CARTESIAN_POINT('Ctrl Pts',(35.8403680076269,-85.1644721430316,109.895722925195));
#39007=CARTESIAN_POINT('Ctrl Pts',(36.6632637439612,-85.2658545033766,109.843073417464));
#39008=CARTESIAN_POINT('Ctrl Pts',(37.4861594802956,-85.3672368637215,109.790423909734));
#39009=CARTESIAN_POINT('Ctrl Pts',(38.254167676629,-85.9141279025497,109.737774402003));
#39010=CARTESIAN_POINT('Ctrl Pts',(38.6191234908882,-86.6586029124452,109.685124894272));
#39011=CARTESIAN_POINT('Ctrl Pts',(38.9840793051474,-87.4030779223408,109.632475386541));
#39012=CARTESIAN_POINT('Ctrl Pts',(38.9459827373325,-88.3451369033038,109.57982587881));
#39013=CARTESIAN_POINT('Ctrl Pts',(38.5221042978734,-89.0577116832849,109.527176371079));
#39014=CARTESIAN_POINT('Ctrl Pts',(38.0982258584144,-89.770286463266,109.474526863349));
#39015=CARTESIAN_POINT('Ctrl Pts',(37.2885655473112,-90.2533770422654,109.421877355618));
#39016=CARTESIAN_POINT('Ctrl Pts',(36.460170532168,-90.2879817733584,109.369227847887));
#39017=CARTESIAN_POINT('Ctrl Pts',(35.6317755170249,-90.3225865044515,109.316578340156));
#39018=CARTESIAN_POINT('Ctrl Pts',(34.7846457978417,-89.9087053876382,109.263928832425));
#39019=CARTESIAN_POINT('Ctrl Pts',(34.3028147960749,-89.2339648850153,109.211279324695));
#39020=CARTESIAN_POINT('Ctrl Pts',(34.0017369367378,-88.8123452187986,109.178380650627));
#39021=CARTESIAN_POINT('Ctrl Pts',(33.8432908589959,-88.2888723645746,109.14548197656));
#39022=CARTESIAN_POINT('Ctrl Pts',(33.8403654904393,-87.7670276461582,109.112583302492));
#39023=CARTESIAN_POINT('Ctrl Pts',(33.8352710252958,-87.7666978305704,109.387416697508));
#39024=CARTESIAN_POINT('Ctrl Pts',(33.8411368280303,-88.4749738142835,109.432300020937));
#39025=CARTESIAN_POINT('Ctrl Pts',(34.1540286364703,-89.1877902316456,109.477183344366));
#39026=CARTESIAN_POINT('Ctrl Pts',(34.6831903958788,-89.6563814347206,109.522066667795));
#39027=CARTESIAN_POINT('Ctrl Pts',(35.3039132839001,-90.2060532122112,109.574716175526));
#39028=CARTESIAN_POINT('Ctrl Pts',(36.2222237488564,-90.4196709543603,109.627365683257));
#39029=CARTESIAN_POINT('Ctrl Pts',(37.0218197159702,-90.2003942962398,109.680015190987));
#39030=CARTESIAN_POINT('Ctrl Pts',(37.821415683084,-89.9811176381194,109.732664698718));
#39031=CARTESIAN_POINT('Ctrl Pts',(38.5022971523554,-89.3289465797295,109.785314206449));
#39032=CARTESIAN_POINT('Ctrl Pts',(38.7557968588963,-88.5395329577955,109.83796371418));
#39033=CARTESIAN_POINT('Ctrl Pts',(39.0092965654372,-87.7501193358615,109.890613221911));
#39034=CARTESIAN_POINT('Ctrl Pts',(38.8354145092477,-86.8234631503834,109.943262729642));
#39035=CARTESIAN_POINT('Ctrl Pts',(38.3129774786581,-86.1796498892039,109.995912237372));
#39036=CARTESIAN_POINT('Ctrl Pts',(37.7905404480686,-85.5358366280243,110.048561745103));
#39037=CARTESIAN_POINT('Ctrl Pts',(36.9195484430791,-85.1748662911433,110.101211252834));
#39038=CARTESIAN_POINT('Ctrl Pts',(36.0948524429973,-85.2603792927236,110.153860760565));
#39039=CARTESIAN_POINT('Ctrl Pts',(35.2701564429156,-85.3458922943038,110.206510268296));
#39040=CARTESIAN_POINT('Ctrl Pts',(34.4917564477417,-85.8778886343454,110.259159776027));
#39041=CARTESIAN_POINT('Ctrl Pts',(34.1125282588601,-86.6151958615018,110.311809283757));
#39042=CARTESIAN_POINT('Ctrl Pts',(33.9309978336103,-86.9681329542853,110.337011755008));
#39043=CARTESIAN_POINT('Ctrl Pts',(33.8409329447111,-87.3681146281553,110.362214226258));
#39044=CARTESIAN_POINT('Ctrl Pts',(33.8413419169939,-87.7682702011519,110.387416697508));
#39045=CARTESIAN_POINT('Origin',(36.3549260746835,-87.7685555885722,114.));
#39046=CARTESIAN_POINT('',(33.8362792303601,-87.7706817999754,111.387416697508));
#39047=CARTESIAN_POINT('',(33.833460463321,-87.7679946641417,111.112583302492));
#39048=CARTESIAN_POINT('',(33.8374260746835,-87.7685555885722,114.));
#39049=CARTESIAN_POINT('Ctrl Pts',(33.833460463321,-87.7679946641417,111.112583302492));
#39050=CARTESIAN_POINT('Ctrl Pts',(33.8333657394917,-87.7369047176017,111.110609402663));
#39051=CARTESIAN_POINT('Ctrl Pts',(33.8338915410514,-87.7058180485741,111.108635502833));
#39052=CARTESIAN_POINT('Ctrl Pts',(33.8350478473288,-87.6747548496521,111.106661603004));
#39053=CARTESIAN_POINT('Ctrl Pts',(33.8658898157962,-86.846211218651,111.054012095273));
#39054=CARTESIAN_POINT('Ctrl Pts',(34.3452981965331,-86.034365164692,111.001362587543));
#39055=CARTESIAN_POINT('Ctrl Pts',(35.0559404903895,-85.6072547508361,110.948713079812));
#39056=CARTESIAN_POINT('Ctrl Pts',(35.7665827842458,-85.1801443369802,110.896063572081));
#39057=CARTESIAN_POINT('Ctrl Pts',(36.7084589912216,-85.1377695632274,110.84341406435));
#39058=CARTESIAN_POINT('Ctrl Pts',(37.4545838558529,-85.4993403886895,110.790764556619));
#39059=CARTESIAN_POINT('Ctrl Pts',(38.2007087204842,-85.8609112141515,110.738115048888));
#39060=CARTESIAN_POINT('Ctrl Pts',(38.7510822427711,-86.6264276388286,110.685465541158));
#39061=CARTESIAN_POINT('Ctrl Pts',(38.8562009557426,-87.4488544330359,110.632816033427));
#39062=CARTESIAN_POINT('Ctrl Pts',(38.9613196687142,-88.2712812272431,110.580166525696));
#39063=CARTESIAN_POINT('Ctrl Pts',(38.6211835723705,-89.1506183909805,110.527517017965));
#39064=CARTESIAN_POINT('Ctrl Pts',(37.9899881937451,-89.6882317922063,110.474867510234));
#39065=CARTESIAN_POINT('Ctrl Pts',(37.3587928151197,-90.2258451934322,110.422218002503));
#39066=CARTESIAN_POINT('Ctrl Pts',(36.4365381542126,-90.4217348321464,110.369568494773));
#39067=CARTESIAN_POINT('Ctrl Pts',(35.6413143367002,-90.1870971210926,110.316918987042));
#39068=CARTESIAN_POINT('Ctrl Pts',(34.8460905191878,-89.9524594100387,110.264269479311));
#39069=CARTESIAN_POINT('Ctrl Pts',(34.17789754507,-89.2872943492169,110.21161997158));
#39070=CARTESIAN_POINT('Ctrl Pts',(33.9396505386785,-88.4931444006248,110.158970463849));
#39071=CARTESIAN_POINT('Ctrl Pts',(33.8696808922075,-88.2599142249784,110.14350807673));
#39072=CARTESIAN_POINT('Ctrl Pts',(33.8367945423336,-88.0155589656965,110.128045689611));
#39073=CARTESIAN_POINT('Ctrl Pts',(33.838790157295,-87.7706792333693,110.112583302492));
#39074=CARTESIAN_POINT('Ctrl Pts',(33.8413419169939,-87.7682702011519,110.387416697508));
#39075=CARTESIAN_POINT('Ctrl Pts',(33.8417873128861,-88.2040641556771,110.414863733989));
#39076=CARTESIAN_POINT('Ctrl Pts',(33.9495396432895,-88.6400643640522,110.442310770469));
#39077=CARTESIAN_POINT('Ctrl Pts',(34.1633179751479,-89.0157286166987,110.46975780695));
#39078=CARTESIAN_POINT('Ctrl Pts',(34.5733922629067,-89.7363360304679,110.522407314681));
#39079=CARTESIAN_POINT('Ctrl Pts',(35.3735972210135,-90.2349327437351,110.575056822411));
#39080=CARTESIAN_POINT('Ctrl Pts',(36.2011721004088,-90.2854875184755,110.627706330142));
#39081=CARTESIAN_POINT('Ctrl Pts',(37.028746979804,-90.336042293216,110.680355837873));
#39082=CARTESIAN_POINT('Ctrl Pts',(37.8836917804877,-89.9385551294297,110.733005345604));
#39083=CARTESIAN_POINT('Ctrl Pts',(38.3784302779913,-89.2732207883705,110.785654853335));
#39084=CARTESIAN_POINT('Ctrl Pts',(38.873168775495,-88.6078864473114,110.838304361066));
#39085=CARTESIAN_POINT('Ctrl Pts',(39.0077009698187,-87.6747049289793,110.890953868796));
#39086=CARTESIAN_POINT('Ctrl Pts',(38.7210387365027,-86.8967198839624,110.943603376527));
#39087=CARTESIAN_POINT('Ctrl Pts',(38.4343765031867,-86.1187348389456,110.996252884258));
#39088=CARTESIAN_POINT('Ctrl Pts',(37.7265198422309,-85.495946267244,111.048902391989));
#39089=CARTESIAN_POINT('Ctrl Pts',(36.9183648066211,-85.3106858972247,111.10155189972));
#39090=CARTESIAN_POINT('Ctrl Pts',(36.1102097710112,-85.1254255272055,111.154201407451));
#39091=CARTESIAN_POINT('Ctrl Pts',(35.2017563607472,-85.3776933588685,111.206850915181));
#39092=CARTESIAN_POINT('Ctrl Pts',(34.6048381146989,-85.9531276069116,111.259500422912));
#39093=CARTESIAN_POINT('Ctrl Pts',(34.1214175880013,-86.419149091613,111.302139181111));
#39094=CARTESIAN_POINT('Ctrl Pts',(33.8423248995646,-87.0971270513523,111.344777939309));
#39095=CARTESIAN_POINT('Ctrl Pts',(33.8362792303601,-87.7706817999754,111.387416697508));
#39096=CARTESIAN_POINT('Origin',(36.3549260746835,-87.7685555885722,114.));
#39097=CARTESIAN_POINT('',(33.8351270426488,-87.7667516913842,112.387416697508));
#39098=CARTESIAN_POINT('',(33.8402625727925,-87.7669648534793,112.112583302492));
#39099=CARTESIAN_POINT('',(33.8374260746835,-87.7685555885722,114.));
#39100=CARTESIAN_POINT('Ctrl Pts',(33.8402625727925,-87.7669648534793,112.112583302492));
#39101=CARTESIAN_POINT('Ctrl Pts',(33.8384608202137,-87.4591086515179,112.093173115714));
#39102=CARTESIAN_POINT('Ctrl Pts',(33.8908470321291,-87.1518442311906,112.073762928937));
#39103=CARTESIAN_POINT('Ctrl Pts',(34.000204726143,-86.8664069145517,112.054352742159));
#39104=CARTESIAN_POINT('Ctrl Pts',(34.2968339560602,-86.0921673680098,112.001703234428));
#39105=CARTESIAN_POINT('Ctrl Pts',(35.0126298328924,-85.478520341233,111.949053726697));
#39106=CARTESIAN_POINT('Ctrl Pts',(35.8230971808513,-85.3036533821964,111.896404218967));
#39107=CARTESIAN_POINT('Ctrl Pts',(36.6335645288102,-85.1287864231598,111.843754711236));
#39108=CARTESIAN_POINT('Ctrl Pts',(37.5387033478958,-85.3926995318635,111.791105203505));
#39109=CARTESIAN_POINT('Ctrl Pts',(38.1281827187525,-85.9757517137513,111.738455695774));
#39110=CARTESIAN_POINT('Ctrl Pts',(38.7176620896091,-86.5588038956392,111.685806188043));
#39111=CARTESIAN_POINT('Ctrl Pts',(38.9914820122369,-87.4609951507114,111.633156680312));
#39112=CARTESIAN_POINT('Ctrl Pts',(38.8255103886397,-88.2733307929391,111.580507172582));
#39113=CARTESIAN_POINT('Ctrl Pts',(38.6595387650426,-89.0856664351667,111.527857664851));
#39114=CARTESIAN_POINT('Ctrl Pts',(38.0537755952206,-89.8081464645499,111.47520815712));
#39115=CARTESIAN_POINT('Ctrl Pts',(37.2828344004873,-90.113245546376,111.422558649389));
#39116=CARTESIAN_POINT('Ctrl Pts',(36.5118932057541,-90.4183446282021,111.369909141658));
#39117=CARTESIAN_POINT('Ctrl Pts',(35.5757739861097,-90.306062762471,111.317259633927));
#39118=CARTESIAN_POINT('Ctrl Pts',(34.8988521543865,-89.8273012255838,111.264610126197));
#39119=CARTESIAN_POINT('Ctrl Pts',(34.2473090193628,-89.3664890932904,111.213934518295));
#39120=CARTESIAN_POINT('Ctrl Pts',(33.8358922927207,-88.5661617834507,111.163258910394));
#39121=CARTESIAN_POINT('Ctrl Pts',(33.833460463321,-87.7679946641417,111.112583302492));
#39122=CARTESIAN_POINT('Ctrl Pts',(33.8362792303601,-87.7706817999754,111.387416697508));
#39123=CARTESIAN_POINT('Ctrl Pts',(33.8348598250416,-87.9288193295271,111.39742744704));
#39124=CARTESIAN_POINT('Ctrl Pts',(33.8484912873127,-88.086713043325,111.407438196572));
#39125=CARTESIAN_POINT('Ctrl Pts',(33.878062949579,-88.2415626538203,111.417448946105));
#39126=CARTESIAN_POINT('Ctrl Pts',(34.0335891123402,-89.0559627882629,111.470098453835));
#39127=CARTESIAN_POINT('Ctrl Pts',(34.6300245196953,-89.7861623927248,111.522747961566));
#39128=CARTESIAN_POINT('Ctrl Pts',(35.396984249603,-90.10113658053,111.575397469297));
#39129=CARTESIAN_POINT('Ctrl Pts',(36.1639439795107,-90.4161107683353,111.628046977028));
#39130=CARTESIAN_POINT('Ctrl Pts',(37.1014280319711,-90.3158595394838,111.680696484759));
#39131=CARTESIAN_POINT('Ctrl Pts',(37.7844422679447,-89.8458302640747,111.733345992489));
#39132=CARTESIAN_POINT('Ctrl Pts',(38.4674565039183,-89.3758009886656,111.78599550022));
#39133=CARTESIAN_POINT('Ctrl Pts',(38.8960009234051,-88.5359936666988,111.838645007951));
#39134=CARTESIAN_POINT('Ctrl Pts',(38.8758014306258,-87.7071221767951,111.891294515682));
#39135=CARTESIAN_POINT('Ctrl Pts',(38.8556019378465,-86.8782506868913,111.943944023413));
#39136=CARTESIAN_POINT('Ctrl Pts',(38.3866585328012,-86.0603150290506,111.996593531144));
#39137=CARTESIAN_POINT('Ctrl Pts',(37.6815595770325,-85.6241138955609,112.049243038874));
#39138=CARTESIAN_POINT('Ctrl Pts',(36.9764606212637,-85.1879127620711,112.101892546605));
#39139=CARTESIAN_POINT('Ctrl Pts',(36.0352061147715,-85.1334461529325,112.154542054336));
#39140=CARTESIAN_POINT('Ctrl Pts',(35.2844994745933,-85.4854056771343,112.207191562067));
#39141=CARTESIAN_POINT('Ctrl Pts',(34.5337928344152,-85.8373652013361,112.259841069798));
#39142=CARTESIAN_POINT('Ctrl Pts',(33.973634060551,-86.5957508588782,112.312490577529));
#39143=CARTESIAN_POINT('Ctrl Pts',(33.8579626149027,-87.4167600445428,112.365140085259));
#39144=CARTESIAN_POINT('Ctrl Pts',(33.8416486419014,-87.5325528541995,112.372565622676));
#39145=CARTESIAN_POINT('Ctrl Pts',(33.8341761808045,-87.6495913386691,112.379991160092));
#39146=CARTESIAN_POINT('Ctrl Pts',(33.8351270426488,-87.7667516913842,112.387416697508));
#39147=CARTESIAN_POINT('Origin',(36.3549260746835,-87.7685555885722,114.));
#39148=CARTESIAN_POINT('',(33.8413207210893,-87.7681842623864,113.387416697508));
#39149=CARTESIAN_POINT('',(33.8389343942797,-87.7706492050004,113.112583302492));
#39150=CARTESIAN_POINT('',(33.8374260746835,-87.7685555885722,114.));
#39151=CARTESIAN_POINT('Ctrl Pts',(33.8389343942797,-87.7706492050004,113.112583302492));
#39152=CARTESIAN_POINT('Ctrl Pts',(33.8436024808034,-87.1870222434737,113.075736828766));
#39153=CARTESIAN_POINT('Ctrl Pts',(34.0460600744816,-86.6004731251508,113.03889035504));
#39154=CARTESIAN_POINT('Ctrl Pts',(34.4174406984265,-86.1546363600791,113.002043881314));
#39155=CARTESIAN_POINT('Ctrl Pts',(34.9481022530933,-85.5175852711787,112.949394373583));
#39156=CARTESIAN_POINT('Ctrl Pts',(35.8236578008925,-85.1678297944825,112.896744865852));
#39157=CARTESIAN_POINT('Ctrl Pts',(36.6471875486386,-85.2639262566846,112.844095358121));
#39158=CARTESIAN_POINT('Ctrl Pts',(37.4707172963847,-85.3600227188868,112.791445850391));
#39159=CARTESIAN_POINT('Ctrl Pts',(38.2422212440775,-85.9019711199873,112.73879634266));
#39160=CARTESIAN_POINT('Ctrl Pts',(38.6119498091466,-86.644087393655,112.686146834929));
#39161=CARTESIAN_POINT('Ctrl Pts',(38.9816783742156,-87.3862036673227,112.633497327198));
#39162=CARTESIAN_POINT('Ctrl Pts',(38.9496315566609,-88.3284878135576,112.580847819467));
#39163=CARTESIAN_POINT('Ctrl Pts',(38.5303372938909,-89.0437696438026,112.528198311736));
#39164=CARTESIAN_POINT('Ctrl Pts',(38.1110430311208,-89.7590514740476,112.475548804006));
#39165=CARTESIAN_POINT('Ctrl Pts',(37.3045013231354,-90.2473309883026,112.422899296275));
#39166=CARTESIAN_POINT('Ctrl Pts',(36.4763455883213,-90.2872540939552,112.370249788544));
#39167=CARTESIAN_POINT('Ctrl Pts',(35.6481898535072,-90.3271771996077,112.317600280813));
#39168=CARTESIAN_POINT('Ctrl Pts',(34.7984200918643,-89.9187438966577,112.264950773082));
#39169=CARTESIAN_POINT('Ctrl Pts',(34.312266502544,-89.2471112120292,112.212301265351));
#39170=CARTESIAN_POINT('Ctrl Pts',(34.0053421667922,-88.8230879812494,112.179061944398));
#39171=CARTESIAN_POINT('Ctrl Pts',(33.8433480161699,-88.2941587038847,112.145822623445));
#39172=CARTESIAN_POINT('Ctrl Pts',(33.8402625727925,-87.7669648534793,112.112583302492));
#39173=CARTESIAN_POINT('Ctrl Pts',(33.8351270426488,-87.7667516913842,112.387416697508));
#39174=CARTESIAN_POINT('Ctrl Pts',(33.8409181046838,-88.4802968553584,112.432640667823));
#39175=CARTESIAN_POINT('Ctrl Pts',(34.1591480267783,-89.1983623702661,112.477864638137));
#39176=CARTESIAN_POINT('Ctrl Pts',(34.6953465824845,-89.667076732345,112.523088608452));
#39177=CARTESIAN_POINT('Ctrl Pts',(35.3195861131473,-90.2127515206959,112.575738116183));
#39178=CARTESIAN_POINT('Ctrl Pts',(36.2392492919054,-90.4204683836109,112.628387623914));
#39179=CARTESIAN_POINT('Ctrl Pts',(37.0374208018146,-90.1960620399989,112.681037131644));
#39180=CARTESIAN_POINT('Ctrl Pts',(37.8355923117237,-89.9716556963869,112.733686639375));
#39181=CARTESIAN_POINT('Ctrl Pts',(38.5122721527838,-89.315126146248,112.786336147106));
#39182=CARTESIAN_POINT('Ctrl Pts',(38.7606978091938,-88.5241010774157,112.838985654837));
#39183=CARTESIAN_POINT('Ctrl Pts',(39.0091234656037,-87.7330760085833,112.891635162568));
#39184=CARTESIAN_POINT('Ctrl Pts',(38.8292949373637,-86.8075554210577,112.944284670298));
#39185=CARTESIAN_POINT('Ctrl Pts',(38.3027347531324,-86.1671099989753,112.996934178029));
#39186=CARTESIAN_POINT('Ctrl Pts',(37.7761745689011,-85.526664576893,113.04958368576));
#39187=CARTESIAN_POINT('Ctrl Pts',(36.9028827286787,-85.171294320254,113.102233193491));
#39188=CARTESIAN_POINT('Ctrl Pts',(36.0787528082445,-85.2621009308566,113.154882701222));
#39189=CARTESIAN_POINT('Ctrl Pts',(35.2546228878104,-85.3529075414593,113.207532208953));
#39190=CARTESIAN_POINT('Ctrl Pts',(34.4796548871646,-85.8898910193036,113.260181716683));
#39191=CARTESIAN_POINT('Ctrl Pts',(34.1051687646067,-86.6296180705161,113.312831224414));
#39192=CARTESIAN_POINT('Ctrl Pts',(33.9283312478418,-86.9789273958571,113.337693048779));
#39193=CARTESIAN_POINT('Ctrl Pts',(33.8407955340496,-87.373445674795,113.362554873143));
#39194=CARTESIAN_POINT('Ctrl Pts',(33.8413207210893,-87.7681842623864,113.387416697508));
#39195=CARTESIAN_POINT('Origin',(36.3549260746835,-87.7685555885722,114.));
#39196=CARTESIAN_POINT('',(33.8364382856638,-87.7707089500853,114.387416697508));
#39197=CARTESIAN_POINT('',(33.8334119429091,-87.7680895937245,114.112583302492));
#39198=CARTESIAN_POINT('',(33.8374260746835,-87.7685555885722,114.));
#39199=CARTESIAN_POINT('Ctrl Pts',(33.8334119429091,-87.7680895937245,114.112583302492));
#39200=CARTESIAN_POINT('Ctrl Pts',(33.8333458553462,-87.7423663400699,114.110950049548));
#39201=CARTESIAN_POINT('Ctrl Pts',(33.8337057988272,-87.7166449805644,114.109316796605));
#39202=CARTESIAN_POINT('Ctrl Pts',(33.8344974997795,-87.6909369173853,114.107683543661));
#39203=CARTESIAN_POINT('Ctrl Pts',(33.8600187551162,-86.8622123304467,114.05503403593));
#39204=CARTESIAN_POINT('Ctrl Pts',(34.3342043907143,-86.0473047321551,114.002384528199));
#39205=CARTESIAN_POINT('Ctrl Pts',(35.0420895595274,-85.6156400900488,113.949735020469));
#39206=CARTESIAN_POINT('Ctrl Pts',(35.7499747283406,-85.1839754479424,113.897085512738));
#39207=CARTESIAN_POINT('Ctrl Pts',(36.6915594303689,-85.1355537620213,113.844436005007));
#39208=CARTESIAN_POINT('Ctrl Pts',(37.4399905594498,-85.4923262672584,113.791786497276));
#39209=CARTESIAN_POINT('Ctrl Pts',(38.1884216885307,-85.8490987724954,113.739136989545));
#39210=CARTESIAN_POINT('Ctrl Pts',(38.7436992446643,-86.6110654688906,113.686487481814));
#39211=CARTESIAN_POINT('Ctrl Pts',(38.8540965917791,-87.4328003417179,113.633837974084));
#39212=CARTESIAN_POINT('Ctrl Pts',(38.964493938894,-88.2545352145452,113.581188466353));
#39213=CARTESIAN_POINT('Ctrl Pts',(38.63001107699,-89.1360382638046,113.528538958622));
#39214=CARTESIAN_POINT('Ctrl Pts',(38.0022807250933,-89.677693486966,113.475889450891));
#39215=CARTESIAN_POINT('Ctrl Pts',(37.3745503731965,-90.2193487101274,113.42323994316));
#39216=CARTESIAN_POINT('Ctrl Pts',(36.453572531307,-90.4211561071909,113.37059043543));
#39217=CARTESIAN_POINT('Ctrl Pts',(35.6568584989078,-90.191629363545,113.317940927699));
#39218=CARTESIAN_POINT('Ctrl Pts',(34.8601444665087,-89.962102619899,113.265291419968));
#39219=CARTESIAN_POINT('Ctrl Pts',(34.1876942435999,-89.3012417355436,113.212641912237));
#39220=CARTESIAN_POINT('Ctrl Pts',(33.9443529129126,-88.5086379428137,113.159992404506));
#39221=CARTESIAN_POINT('Ctrl Pts',(33.8713126986855,-88.2707336350879,113.144189370502));
#39222=CARTESIAN_POINT('Ctrl Pts',(33.8369323049992,-88.0209601787902,113.128386336497));
#39223=CARTESIAN_POINT('Ctrl Pts',(33.8389343942797,-87.7706492050004,113.112583302492));
#39224=CARTESIAN_POINT('Ctrl Pts',(33.8413207210893,-87.7681842623864,113.387416697508));
#39225=CARTESIAN_POINT('Ctrl Pts',(33.8419077146645,-88.2093775844676,113.415204380874));
#39226=CARTESIAN_POINT('Ctrl Pts',(33.9525020875792,-88.6508461203768,113.442992064241));
#39227=CARTESIAN_POINT('Ctrl Pts',(34.17137125074,-89.0297752185784,113.470779747607));
#39228=CARTESIAN_POINT('Ctrl Pts',(34.5860641039011,-89.7477346908476,113.523429255338));
#39229=CARTESIAN_POINT('Ctrl Pts',(35.3894540546931,-90.2411830108054,113.576078763068));
#39230=CARTESIAN_POINT('Ctrl Pts',(36.2173364859249,-90.2864228863751,113.628728270799));
#39231=CARTESIAN_POINT('Ctrl Pts',(37.0452189171568,-90.3316627619448,113.68137777853));
#39232=CARTESIAN_POINT('Ctrl Pts',(37.8975938288284,-89.9286941931264,113.734027286261));
#39233=CARTESIAN_POINT('Ctrl Pts',(38.3880500166391,-89.2601968527262,113.786676793992));
#39234=CARTESIAN_POINT('Ctrl Pts',(38.8785062044498,-88.591699512326,113.839326301722));
#39235=CARTESIAN_POINT('Ctrl Pts',(39.0070436683995,-87.6576734003441,113.891975809453));
#39236=CARTESIAN_POINT('Ctrl Pts',(38.7153919038517,-86.8815450510873,113.944625317184));
#39237=CARTESIAN_POINT('Ctrl Pts',(38.423740139304,-86.1054167018305,113.997274824915));
#39238=CARTESIAN_POINT('Ctrl Pts',(37.7118991462587,-85.4871861152989,114.049924332646));
#39239=CARTESIAN_POINT('Ctrl Pts',(36.9025712140805,-85.3071187265799,114.102573840377));
#39240=CARTESIAN_POINT('Ctrl Pts',(36.0932432819023,-85.1270513378609,114.155223348107));
#39241=CARTESIAN_POINT('Ctrl Pts',(35.1864284105912,-85.3851471469545,114.207872855838));
#39242=CARTESIAN_POINT('Ctrl Pts',(34.5932173322921,-85.9644023436228,114.260522363569));
#39243=CARTESIAN_POINT('Ctrl Pts',(34.1166372216047,-86.4297704323915,114.302820474882));
#39244=CARTESIAN_POINT('Ctrl Pts',(33.8424683523542,-87.1024264168637,114.345118586195));
#39245=CARTESIAN_POINT('Ctrl Pts',(33.8364382856638,-87.7707089500853,114.387416697508));
#39246=CARTESIAN_POINT('Origin',(36.3549260746835,-87.7685555885722,114.));
#39247=CARTESIAN_POINT('',(33.8349862377778,-87.7668088525252,115.387416697508));
#39248=CARTESIAN_POINT('',(33.8401553510245,-87.7669042808192,115.112583302492));
#39249=CARTESIAN_POINT('',(33.8374260746835,-87.7685555885722,114.));
#39250=CARTESIAN_POINT('Ctrl Pts',(33.8401553510245,-87.7669042808192,115.112583302492));
#39251=CARTESIAN_POINT('Ctrl Pts',(33.8383127863372,-87.4644833544989,115.0935137626));
#39252=CARTESIAN_POINT('Ctrl Pts',(33.8888249380179,-87.1626571750687,115.074444222708));
#39253=CARTESIAN_POINT('Ctrl Pts',(33.9944605731161,-86.8815451741916,115.055374682816));
#39254=CARTESIAN_POINT('Ctrl Pts',(34.2861122971867,-86.1054169326509,115.002725175085));
#39255=CARTESIAN_POINT('Ctrl Pts',(34.9979531914383,-85.4871864319215,114.950075667354));
#39256=CARTESIAN_POINT('Ctrl Pts',(35.8072810112928,-85.3071190681936,114.897426159623));
#39257=CARTESIAN_POINT('Ctrl Pts',(36.6166088311474,-85.1270517044657,114.844776651893));
#39258=CARTESIAN_POINT('Ctrl Pts',(37.523423576605,-85.3851474777394,114.792127144162));
#39259=CARTESIAN_POINT('Ctrl Pts',(38.1166345725743,-85.9644025940151,114.739477636431));
#39260=CARTESIAN_POINT('Ctrl Pts',(38.7098455685436,-86.5436577102908,114.6868281287));
#39261=CARTESIAN_POINT('Ctrl Pts',(38.9894528150246,-87.4440721695685,114.634178620969));
#39262=CARTESIAN_POINT('Ctrl Pts',(38.8287006187602,-88.2574567691686,114.581529113239));
#39263=CARTESIAN_POINT('Ctrl Pts',(38.6679484224957,-89.0708413687687,114.528879605508));
#39264=CARTESIAN_POINT('Ctrl Pts',(38.0668367834858,-89.7971961086912,114.476230097777));
#39265=CARTESIAN_POINT('Ctrl Pts',(37.2978705222835,-90.1072391131326,114.423580590046));
#39266=CARTESIAN_POINT('Ctrl Pts',(36.5289042610813,-90.4172821175741,114.370931082315));
#39267=CARTESIAN_POINT('Ctrl Pts',(35.5920833776866,-90.3110133865345,114.318281574584));
#39268=CARTESIAN_POINT('Ctrl Pts',(34.912101373527,-89.8366082332219,114.265632066854));
#39269=CARTESIAN_POINT('Ctrl Pts',(34.25321325339,-89.3769197153828,114.214615812066));
#39270=CARTESIAN_POINT('Ctrl Pts',(33.835476252641,-88.5715806068579,114.163599557279));
#39271=CARTESIAN_POINT('Ctrl Pts',(33.8334119429091,-87.7680895937245,114.112583302492));
#39272=CARTESIAN_POINT('Ctrl Pts',(33.8364382856638,-87.7707089500853,114.387416697508));
#39273=CARTESIAN_POINT('Ctrl Pts',(33.834962578858,-87.9342542528365,114.397768093926));
#39274=CARTESIAN_POINT('Ctrl Pts',(33.8495457647187,-88.0975376286172,114.408119490344));
#39275=CARTESIAN_POINT('Ctrl Pts',(33.8811511872807,-88.2574568370208,114.418470886762));
#39276=CARTESIAN_POINT('Ctrl Pts',(34.0419034058551,-89.0708415495077,114.471120394492));
#39277=CARTESIAN_POINT('Ctrl Pts',(34.6430151282909,-89.7971963902384,114.523769902223));
#39278=CARTESIAN_POINT('Ctrl Pts',(35.4119814962151,-90.1072394377098,114.576419409954));
#39279=CARTESIAN_POINT('Ctrl Pts',(36.1809478641394,-90.4172824851811,114.629068917685));
#39280=CARTESIAN_POINT('Ctrl Pts',(37.117768877552,-90.3110137393931,114.681718425416));
#39281=CARTESIAN_POINT('Ctrl Pts',(37.797750976084,-89.8366085202398,114.734367933147));
#39282=CARTESIAN_POINT('Ctrl Pts',(38.477733074616,-89.3622033010865,114.787017440877));
#39283=CARTESIAN_POINT('Ctrl Pts',(38.9008762582673,-88.5196616085678,114.839666948608));
#39284=CARTESIAN_POINT('Ctrl Pts',(38.8753549993888,-87.6909369066135,114.892316456339));
#39285=CARTESIAN_POINT('Ctrl Pts',(38.8498337405103,-86.8622122046593,114.94496596407));
#39286=CARTESIAN_POINT('Ctrl Pts',(38.3756480391019,-86.0473044932694,114.997615471801));
#39287=CARTESIAN_POINT('Ctrl Pts',(37.667762772044,-85.6156397912537,115.050264979531));
#39288=CARTESIAN_POINT('Ctrl Pts',(36.9598775049861,-85.183975089238,115.102914487262));
#39289=CARTESIAN_POINT('Ctrl Pts',(36.0182926722788,-85.1355533965965,115.155563994993));
#39290=CARTESIAN_POINT('Ctrl Pts',(35.2698614393257,-85.4923259513485,115.208213502724));
#39291=CARTESIAN_POINT('Ctrl Pts',(34.5214302063727,-85.8490985061005,115.260863010455));
#39292=CARTESIAN_POINT('Ctrl Pts',(33.9661525731739,-86.6110653082461,115.313512518185));
#39293=CARTESIAN_POINT('Ctrl Pts',(33.8557552107373,-87.432800295119,115.366162025916));
#39294=CARTESIAN_POINT('Ctrl Pts',(33.8408993600097,-87.5433787730203,115.373246916447));
#39295=CARTESIAN_POINT('Ctrl Pts',(33.8340995342799,-87.6550395510862,115.380331806977));
#39296=CARTESIAN_POINT('Ctrl Pts',(33.8349862377778,-87.7668088525252,115.387416697508));
#39297=CARTESIAN_POINT('Origin',(36.3549260746835,-87.7685555885722,114.));
#39298=CARTESIAN_POINT('',(33.8412939819271,-87.7680988643367,116.387416697508));
#39299=CARTESIAN_POINT('',(33.8390759225476,-87.7706159289776,116.112583302492));
#39300=CARTESIAN_POINT('',(33.8374260746835,-87.7685555885722,114.));
#39301=CARTESIAN_POINT('Ctrl Pts',(33.8390759225476,-87.7706159289776,116.112583302492));
#39302=CARTESIAN_POINT('Ctrl Pts',(33.8436084809604,-87.1923022245829,116.076077475652));
#39303=CARTESIAN_POINT('Ctrl Pts',(34.0420143053501,-86.6111786929465,116.039571648811));
#39304=CARTESIAN_POINT('Ctrl Pts',(34.4071176665644,-86.1671102212336,116.003065821971));
#39305=CARTESIAN_POINT('Ctrl Pts',(34.9336777777165,-85.5266648880365,115.95041631424));
#39306=CARTESIAN_POINT('Ctrl Pts',(35.8069694967381,-85.1712946807182,115.897766806509));
#39307=CARTESIAN_POINT('Ctrl Pts',(36.6310993027942,-85.2621012787183,115.845117298778));
#39308=CARTESIAN_POINT('Ctrl Pts',(37.4552291088503,-85.3529078767185,115.792467791047));
#39309=CARTESIAN_POINT('Ctrl Pts',(38.2301970019409,-85.8898912800372,115.739818283317));
#39310=CARTESIAN_POINT('Ctrl Pts',(38.6046830725251,-86.6296182285857,115.687168775586));
#39311=CARTESIAN_POINT('Ctrl Pts',(38.9791691431092,-87.3693451771342,115.634519267855));
#39312=CARTESIAN_POINT('Ctrl Pts',(38.9531733911867,-88.3118156709127,115.581869760124));
#39313=CARTESIAN_POINT('Ctrl Pts',(38.5384805955792,-89.0297750435388,115.529220252393));
#39314=CARTESIAN_POINT('Ctrl Pts',(38.1237877999717,-89.7477344161649,115.476570744663));
#39315=CARTESIAN_POINT('Ctrl Pts',(37.3203979606791,-90.2411826676387,115.423921236932));
#39316=CARTESIAN_POINT('Ctrl Pts',(36.492515644346,-90.2864225369295,115.371271729201));
#39317=CARTESIAN_POINT('Ctrl Pts',(35.6646333280129,-90.3316624062204,115.31862222147));
#39318=CARTESIAN_POINT('Ctrl Pts',(34.8122585346393,-89.9286938933283,115.265972713739));
#39319=CARTESIAN_POINT('Ctrl Pts',(34.3218024148975,-89.2601966457063,115.213323206008));
#39320=CARTESIAN_POINT('Ctrl Pts',(34.0089884601789,-88.8338276815323,115.17974323817));
#39321=CARTESIAN_POINT('Ctrl Pts',(33.8433999632852,-88.2994438720784,115.146163270331));
#39322=CARTESIAN_POINT('Ctrl Pts',(33.8401553510245,-87.7669042808192,115.112583302492));
#39323=CARTESIAN_POINT('Ctrl Pts',(33.8349862377778,-87.7668088525252,115.387416697508));
#39324=CARTESIAN_POINT('Ctrl Pts',(33.8406888390072,-88.4856238310819,115.432981314708));
#39325=CARTESIAN_POINT('Ctrl Pts',(34.1643126089722,-89.2089274255769,115.478545931909));
#39326=CARTESIAN_POINT('Ctrl Pts',(34.707571195643,-89.6776937519279,115.524110549109));
#39327=CARTESIAN_POINT('Ctrl Pts',(35.33530163466,-90.2193490502639,115.57676005684));
#39328=CARTESIAN_POINT('Ctrl Pts',(36.2562796043687,-90.4211564753357,115.62940956457));
#39329=CARTESIAN_POINT('Ctrl Pts',(37.0529937473409,-90.1916296998348,115.682059072301));
#39330=CARTESIAN_POINT('Ctrl Pts',(37.8497078903132,-89.9621029243338,115.734708580032));
#39331=CARTESIAN_POINT('Ctrl Pts',(38.5221582065491,-89.3012419482601,115.787358087763));
#39332=CARTESIAN_POINT('Ctrl Pts',(38.765499571009,-88.5086380455277,115.840007595494));
#39333=CARTESIAN_POINT('Ctrl Pts',(39.0088409354689,-87.7160341427952,115.892657103225));
#39334=CARTESIAN_POINT('Ctrl Pts',(38.8230733481528,-86.791687313404,115.945306610955));
#39335=CARTESIAN_POINT('Ctrl Pts',(38.2924117198376,-86.1546361360895,115.997956118686));
#39336=CARTESIAN_POINT('Ctrl Pts',(37.7617500915224,-85.5175849587751,116.050605626417));
#39337=CARTESIAN_POINT('Ctrl Pts',(36.886194422208,-85.1678294335373,116.103255134148));
#39338=CARTESIAN_POINT('Ctrl Pts',(36.0626645601672,-85.2639259090762,116.155904641879));
#39339=CARTESIAN_POINT('Ctrl Pts',(35.2391346981264,-85.360022384615,116.208554149609));
#39340=CARTESIAN_POINT('Ctrl Pts',(34.4676306433592,-85.9019708609303,116.26120365734));
#39341=CARTESIAN_POINT('Ctrl Pts',(34.0979020269767,-86.6440872375935,116.313853165071));
#39342=CARTESIAN_POINT('Ctrl Pts',(33.9257032465489,-86.9897232780147,116.33837434255));
#39343=CARTESIAN_POINT('Ctrl Pts',(33.8406564735888,-87.3787791810735,116.362895520029));
#39344=CARTESIAN_POINT('Ctrl Pts',(33.8412939819271,-87.7680988643367,116.387416697508));
#39345=CARTESIAN_POINT('Origin',(36.3549260746835,-87.7685555885722,114.));
#39346=CARTESIAN_POINT('',(33.8365981762608,-87.7707324390162,117.387416697508));
#39347=CARTESIAN_POINT('',(33.8333718846759,-87.7681855672794,117.112583302492));
#39348=CARTESIAN_POINT('',(33.8374260746835,-87.7685555885722,114.));
#39349=CARTESIAN_POINT('Ctrl Pts',(33.8333718846759,-87.7681855672794,117.112583302492));
#39350=CARTESIAN_POINT('Ctrl Pts',(33.8333297115333,-87.7478282709333,117.111290696434));
#39351=CARTESIAN_POINT('Ctrl Pts',(33.8335551478591,-87.7274719322915,117.109998090376));
#39352=CARTESIAN_POINT('Ctrl Pts',(33.8340510686044,-87.7071221853206,117.108705484318));
#39353=CARTESIAN_POINT('Ctrl Pts',(33.8542505585804,-86.8782508104529,117.056055976587));
#39354=CARTESIAN_POINT('Ctrl Pts',(34.323193898543,-86.0603152661305,117.003406468856));
#39355=CARTESIAN_POINT('Ctrl Pts',(35.0282927564538,-85.6241141931798,116.950756961126));
#39356=CARTESIAN_POINT('Ctrl Pts',(35.7333916143645,-85.187913120229,116.898107453395));
#39357=CARTESIAN_POINT('Ctrl Pts',(36.6746459902234,-85.1334465186498,116.845457945664));
#39358=CARTESIAN_POINT('Ctrl Pts',(37.4253525262137,-85.4854059940045,116.792808437933));
#39359=CARTESIAN_POINT('Ctrl Pts',(38.1760590622039,-85.8373654693593,116.740158930202));
#39360=CARTESIAN_POINT('Ctrl Pts',(38.7362177583255,-86.5957510216481,116.687509422471));
#39361=CARTESIAN_POINT('Ctrl Pts',(38.8518891879201,-87.4167600933678,116.634859914741));
#39362=CARTESIAN_POINT('Ctrl Pts',(38.9675606175146,-88.2377691650875,116.58221040701));
#39363=CARTESIAN_POINT('Ctrl Pts',(38.6387447805821,-89.121401756238,116.529560899279));
#39364=CARTESIAN_POINT('Ctrl Pts',(38.0145053365551,-89.6670764688566,116.476911391548));
#39365=CARTESIAN_POINT('Ctrl Pts',(37.3902658925281,-90.2127511814751,116.424261883817));
#39366=CARTESIAN_POINT('Ctrl Pts',(36.4706028414066,-90.4204680155617,116.371612376086));
#39367=CARTESIAN_POINT('Ctrl Pts',(35.6724314422729,-90.196061703094,116.318962868356));
#39368=CARTESIAN_POINT('Ctrl Pts',(34.8742600431391,-89.9716553906263,116.266313360625));
#39369=CARTESIAN_POINT('Ctrl Pts',(34.1975802959931,-89.3151259316045,116.213663852894));
#39370=CARTESIAN_POINT('Ctrl Pts',(33.9491546740614,-88.5241009725556,116.161014345163));
#39371=CARTESIAN_POINT('Ctrl Pts',(33.8729810470265,-88.2815525601278,116.144870664273));
#39372=CARTESIAN_POINT('Ctrl Pts',(33.8370715253604,-88.0263589899167,116.128726983382));
#39373=CARTESIAN_POINT('Ctrl Pts',(33.8390759225476,-87.7706159289776,116.112583302492));
#39374=CARTESIAN_POINT('Ctrl Pts',(33.8412939819271,-87.7680988643367,116.387416697508));
#39375=CARTESIAN_POINT('Ctrl Pts',(33.8420252700186,-88.2146888632784,116.41554502776));
#39376=CARTESIAN_POINT('Ctrl Pts',(33.9555039285579,-88.6616259565057,116.443673358012));
#39377=CARTESIAN_POINT('Ctrl Pts',(34.1795145535585,-89.0437698207844,116.471801688264));
#39378=CARTESIAN_POINT('Ctrl Pts',(34.5988088745207,-89.7590517503008,116.524451195994));
#39379=CARTESIAN_POINT('Ctrl Pts',(35.405350694443,-90.2473313323226,116.577100703725));
#39380=CARTESIAN_POINT('Ctrl Pts',(36.2335065441938,-90.2872544435161,116.629750211456));
#39381=CARTESIAN_POINT('Ctrl Pts',(37.0616623939446,-90.3271775547097,116.682399719187));
#39382=CARTESIAN_POINT('Ctrl Pts',(37.9114322735241,-89.918744195075,116.735049226918));
#39383=CARTESIAN_POINT('Ctrl Pts',(38.3975859303161,-89.2471114172331,116.787698734649));
#39384=CARTESIAN_POINT('Ctrl Pts',(38.8837395871081,-88.5754786393912,116.840348242379));
#39385=CARTESIAN_POINT('Ctrl Pts',(39.0062770211127,-87.6406464433422,116.89299775011));
#39386=CARTESIAN_POINT('Ctrl Pts',(38.7096477500276,-86.8664067893463,116.945647257841));
#39387=CARTESIAN_POINT('Ctrl Pts',(38.4130184789425,-86.0921671353504,116.998296765572));
#39388=CARTESIAN_POINT('Ctrl Pts',(37.6972225027677,-85.4785200234076,117.050946273303));
#39389=CARTESIAN_POINT('Ctrl Pts',(36.886755042327,-85.3036530401017,117.103595781034));
#39390=CARTESIAN_POINT('Ctrl Pts',(36.0762875818863,-85.1287860567958,117.156245288764));
#39391=CARTESIAN_POINT('Ctrl Pts',(35.1711486371797,-85.3926992021267,117.208894796495));
#39392=CARTESIAN_POINT('Ctrl Pts',(34.5816691845112,-85.9757514649342,117.261544304226));
#39393=CARTESIAN_POINT('Ctrl Pts',(34.111901009423,-86.4403976815922,117.303501768653));
#39394=CARTESIAN_POINT('Ctrl Pts',(33.8426025126824,-87.107723424266,117.345459233081));
#39395=CARTESIAN_POINT('Ctrl Pts',(33.8365981762608,-87.7707324390162,117.387416697508));
#39396=CARTESIAN_POINT('Origin',(36.3549260746835,-87.7685555885722,114.));
#39397=CARTESIAN_POINT('',(33.8348489078967,-87.7668692328515,118.387416697508));
#39398=CARTESIAN_POINT('',(33.8400439227885,-87.7668461827817,118.112583302492));
#39399=CARTESIAN_POINT('',(33.8374260746835,-87.7685555885722,114.));
#39400=CARTESIAN_POINT('Ctrl Pts',(33.8400439227885,-87.7668461827817,118.112583302492));
#39401=CARTESIAN_POINT('Ctrl Pts',(33.8381652118261,-87.4698606386811,118.093854409486));
#39402=CARTESIAN_POINT('Ctrl Pts',(33.8868400327939,-87.1734708669246,118.075125516479));
#39403=CARTESIAN_POINT('Ctrl Pts',(33.9888137412488,-86.8967200049607,118.056396623473));
#39404=CARTESIAN_POINT('Ctrl Pts',(34.2754759347802,-86.1187350679177,118.003747115742));
#39405=CARTESIAN_POINT('Ctrl Pts',(34.9833324974952,-85.4959465826508,117.951097608011));
#39406=CARTESIAN_POINT('Ctrl Pts',(35.7914874209442,-85.3106862383434,117.89844810028));
#39407=CARTESIAN_POINT('Ctrl Pts',(36.5996423443932,-85.1254258940359,117.845798592549));
#39408=CARTESIAN_POINT('Ctrl Pts',(37.5080956285762,-85.3776936906878,117.793149084819));
#39409=CARTESIAN_POINT('Ctrl Pts',(38.1050137917803,-85.9531278588686,117.740499577088));
#39410=CARTESIAN_POINT('Ctrl Pts',(38.7019319549844,-86.5285620270495,117.687850069357));
#39411=CARTESIAN_POINT('Ctrl Pts',(38.9873149972096,-87.4271625667592,117.635200561626));
#39412=CARTESIAN_POINT('Ctrl Pts',(38.8317888560331,-88.241562588174,117.582551053895));
#39413=CARTESIAN_POINT('Ctrl Pts',(38.6762627148567,-89.0559626095889,117.529901546165));
#39414=CARTESIAN_POINT('Ctrl Pts',(38.0798273902785,-89.7861621127089,117.477252038434));
#39415=CARTESIAN_POINT('Ctrl Pts',(37.3128677668143,-90.1011362567998,117.424602530703));
#39416=CARTESIAN_POINT('Ctrl Pts',(36.54590814335,-90.4161104008908,117.371953022972));
#39417=CARTESIAN_POINT('Ctrl Pts',(35.6084242209996,-90.3158591859526,117.319303515241));
#39418=CARTESIAN_POINT('Ctrl Pts',(34.9254100798192,-89.845829975777,117.26665400751));
#39419=CARTESIAN_POINT('Ctrl Pts',(34.2591647225201,-89.3873405241043,117.215297105838));
#39420=CARTESIAN_POINT('Ctrl Pts',(33.8350474778894,-88.5770071415669,117.163940204165));
#39421=CARTESIAN_POINT('Ctrl Pts',(33.8333718846759,-87.7681855672794,117.112583302492));
#39422=CARTESIAN_POINT('Ctrl Pts',(33.8365981762608,-87.7707324390162,117.387416697508));
#39423=CARTESIAN_POINT('Ctrl Pts',(33.8350680879701,-87.9396873840551,117.398108740812));
#39424=CARTESIAN_POINT('Ctrl Pts',(33.8506359548791,-88.108362006809,117.408800784115));
#39425=CARTESIAN_POINT('Ctrl Pts',(33.8843414178438,-88.2733308629943,117.419492827418));
#39426=CARTESIAN_POINT('Ctrl Pts',(34.0503130644754,-89.0856666179632,117.472142335149));
#39427=CARTESIAN_POINT('Ctrl Pts',(34.6560763183689,-89.8081467476169,117.52479184288));
#39428=CARTESIAN_POINT('Ctrl Pts',(35.4270176200981,-90.1132458717868,117.577441350611));
#39429=CARTESIAN_POINT('Ctrl Pts',(36.1979589218274,-90.4183449959567,117.630090858342));
#39430=CARTESIAN_POINT('Ctrl Pts',(37.1340782713924,-90.3060631146427,117.682740366073));
#39431=CARTESIAN_POINT('Ctrl Pts',(37.8110001970633,-89.8273015113101,117.735389873803));
#39432=CARTESIAN_POINT('Ctrl Pts',(38.4879221227341,-89.3485399079774,117.788039381534));
#39433=CARTESIAN_POINT('Ctrl Pts',(38.9056466245108,-88.5032985826261,117.840688889265));
#39434=CARTESIAN_POINT('Ctrl Pts',(38.8748046517631,-87.6747548366344,117.893338396996));
#39435=CARTESIAN_POINT('Ctrl Pts',(38.8439626790154,-86.8462110906427,117.945987904727));
#39436=CARTESIAN_POINT('Ctrl Pts',(38.3645542317434,-86.0343649240108,117.998637412458));
#39437=CARTESIAN_POINT('Ctrl Pts',(37.6539118392597,-85.6072544508775,118.051286920188));
#39438=CARTESIAN_POINT('Ctrl Pts',(36.943269446776,-85.1801439777442,118.103936427919));
#39439=CARTESIAN_POINT('Ctrl Pts',(36.0013931090806,-85.1377691981096,118.15658593565));
#39440=CARTESIAN_POINT('Ctrl Pts',(35.2552681408972,-85.4993400737528,118.209235443381));
#39441=CARTESIAN_POINT('Ctrl Pts',(34.5091431727139,-85.8609109493961,118.261884951112));
#39442=CARTESIAN_POINT('Ctrl Pts',(33.9587695740425,-86.6264274803171,118.314534458842));
#39443=CARTESIAN_POINT('Ctrl Pts',(33.8536508464817,-87.4488543886655,118.367183966573));
#39444=CARTESIAN_POINT('Ctrl Pts',(33.8401854535299,-87.554204802926,118.373928210218));
#39445=CARTESIAN_POINT('Ctrl Pts',(33.8340261763932,-87.6604890504481,118.380672453863));
#39446=CARTESIAN_POINT('Ctrl Pts',(33.8348489078967,-87.7668692328515,118.387416697508));
#39447=CARTESIAN_POINT('Origin',(36.3549260746835,-87.7685555885722,114.));
#39448=CARTESIAN_POINT('',(33.8412617315361,-87.7680141434736,119.387416697508));
#39449=CARTESIAN_POINT('',(33.8392145615825,-87.7705794701237,119.112583302492));
#39450=CARTESIAN_POINT('',(33.8374260746835,-87.7685555885722,114.));
#39451=CARTESIAN_POINT('Ctrl Pts',(33.8392145615825,-87.7705794701237,119.112583302492));
#39452=CARTESIAN_POINT('Ctrl Pts',(33.8436077753976,-87.1975822800088,119.076418122537));
#39453=CARTESIAN_POINT('Ctrl Pts',(34.0380106829751,-86.6218882277961,119.040252942582));
#39454=CARTESIAN_POINT('Ctrl Pts',(34.3968749424612,-86.1796501097232,119.004087762628));
#39455=CARTESIAN_POINT('Ctrl Pts',(34.9193119005448,-85.5358369378978,118.951438254897));
#39456=CARTESIAN_POINT('Ctrl Pts',(35.7903037846505,-85.1748666511118,118.898788747166));
#39457=CARTESIAN_POINT('Ctrl Pts',(36.6149996702752,-85.2603796408235,118.846139239435));
#39458=CARTESIAN_POINT('Ctrl Pts',(37.4396955558998,-85.3458926305352,118.793489731704));
#39459=CARTESIAN_POINT('Ctrl Pts',(38.2180954430434,-85.8778888967446,118.740840223974));
#39460=CARTESIAN_POINT('Ctrl Pts',(38.5973235792934,-86.6151960215733,118.688190716243));
#39461=CARTESIAN_POINT('Ctrl Pts',(38.9765517155434,-87.352503146402,118.635541208512));
#39462=CARTESIAN_POINT('Ctrl Pts',(38.9566081008998,-88.2951211298501,118.582891700781));
#39463=CARTESIAN_POINT('Ctrl Pts',(38.5465338700534,-89.0157284436085,118.53024219305));
#39464=CARTESIAN_POINT('Ctrl Pts',(38.136459639207,-89.736335757367,118.477592685319));
#39465=CARTESIAN_POINT('Ctrl Pts',(37.3362547921579,-90.2349324014359,118.424943177589));
#39466=CARTESIAN_POINT('Ctrl Pts',(36.5086800276188,-90.2854871691599,118.372293669858));
#39467=CARTESIAN_POINT('Ctrl Pts',(35.6811052630797,-90.3360419368839,118.319644162127));
#39468=CARTESIAN_POINT('Ctrl Pts',(34.8261605810507,-89.938554828263,118.266994654396));
#39469=CARTESIAN_POINT('Ctrl Pts',(34.3314221522101,-89.273220579543,118.214345146665));
#39470=CARTESIAN_POINT('Ctrl Pts',(34.0126759310704,-88.8445642124375,118.180424531941));
#39471=CARTESIAN_POINT('Ctrl Pts',(33.8434465280954,-88.3047280648933,118.146503917216));
#39472=CARTESIAN_POINT('Ctrl Pts',(33.8400439227885,-87.7668461827817,118.112583302492));
#39473=CARTESIAN_POINT('Ctrl Pts',(33.8348489078967,-87.7668692328515,118.387416697508));
#39474=CARTESIAN_POINT('Ctrl Pts',(33.8404488993749,-88.4909549307934,118.433321961594));
#39475=CARTESIAN_POINT('Ctrl Pts',(34.1695225039494,-89.2194852526625,118.47922722568));
#39476=CARTESIAN_POINT('Ctrl Pts',(34.7198637286972,-89.6882320586299,118.525132489766));
#39477=CARTESIAN_POINT('Ctrl Pts',(35.3510591949238,-90.2258455344702,118.577781997497));
#39478=CARTESIAN_POINT('Ctrl Pts',(36.2733139838272,-90.4217352003751,118.630431505227));
#39479=CARTESIAN_POINT('Ctrl Pts',(37.0685379117059,-90.1870974567552,118.683081012958));
#39480=CARTESIAN_POINT('Ctrl Pts',(37.8637618395846,-89.9524597131353,118.735730520689));
#39481=CARTESIAN_POINT('Ctrl Pts',(38.5319549064386,-89.2872945599906,118.78838002842));
#39482=CARTESIAN_POINT('Ctrl Pts',(38.7702019458957,-88.4931445011848,118.841029536151));
#39483=CARTESIAN_POINT('Ctrl Pts',(39.0084489853528,-87.698994442379,118.893679043881));
#39484=CARTESIAN_POINT('Ctrl Pts',(38.8167499974131,-86.7758594779121,118.946328551612));
#39485=CARTESIAN_POINT('Ctrl Pts',(38.2820088043637,-86.1422288127157,118.998978059343));
#39486=CARTESIAN_POINT('Ctrl Pts',(37.7472676113142,-85.5085981475193,119.051627567074));
#39487=CARTESIAN_POINT('Ctrl Pts',(36.8694842131551,-85.1644717815935,119.104277074805));
#39488=CARTESIAN_POINT('Ctrl Pts',(36.0465883626135,-85.2658541560218,119.156926582536));
#39489=CARTESIAN_POINT('Ctrl Pts',(35.223692512072,-85.3672365304501,119.209576090266));
#39490=CARTESIAN_POINT('Ctrl Pts',(34.455684209148,-85.9141276452325,119.262225597997));
#39491=CARTESIAN_POINT('Ctrl Pts',(34.090728344239,-86.6586027584256,119.314875105728));
#39492=CARTESIAN_POINT('Ctrl Pts',(33.9231137389559,-87.000520546956,119.339055636321));
#39493=CARTESIAN_POINT('Ctrl Pts',(33.8405158986517,-87.3841151764434,119.363236166915));
#39494=CARTESIAN_POINT('Ctrl Pts',(33.8412617315361,-87.7680141434736,119.387416697508));
#39495=CARTESIAN_POINT('Origin',(36.3549260746835,-87.7685555885722,114.));
#39496=CARTESIAN_POINT('',(33.8367589339947,-87.7707538181913,120.387416697508));
#39497=CARTESIAN_POINT('',(33.8333405706013,-87.7682823373648,120.112583302492));
#39498=CARTESIAN_POINT('',(33.8374260746835,-87.7685555885722,114.));
#39499=CARTESIAN_POINT('Ctrl Pts',(33.8333405706013,-87.7682823373648,120.112583302492));
#39500=CARTESIAN_POINT('Ctrl Pts',(33.8333172714765,-87.7532903997163,120.11163134332));
#39501=CARTESIAN_POINT('Ctrl Pts',(33.833439535064,-87.7382988522033,120.110679384147));
#39502=CARTESIAN_POINT('Ctrl Pts',(33.8337085241762,-87.7233099378653,120.109727424975));
#39503=CARTESIAN_POINT('Ctrl Pts',(33.8485853642248,-86.8943258971421,120.057077917244));
#39504=CARTESIAN_POINT('Ctrl Pts',(34.3122671721632,-86.0733962284342,120.004428409513));
#39505=CARTESIAN_POINT('Ctrl Pts',(35.0145506733614,-85.632676734342,119.951778901782));
#39506=CARTESIAN_POINT('Ctrl Pts',(35.7168341745595,-85.1919572402497,119.899129394052));
#39507=CARTESIAN_POINT('Ctrl Pts',(36.6577193690174,-85.1314479207731,119.846479886321));
#39508=CARTESIAN_POINT('Ctrl Pts',(37.4106703483145,-85.4785798427839,119.79383037859));
#39509=CARTESIAN_POINT('Ctrl Pts',(38.1636213276117,-85.8257117647948,119.741180870859));
#39510=CARTESIAN_POINT('Ctrl Pts',(38.728638091748,-86.580484928293,119.688531363128));
#39511=CARTESIAN_POINT('Ctrl Pts',(38.8495788406817,-87.4007343549724,119.635881855397));
#39512=CARTESIAN_POINT('Ctrl Pts',(38.9705195896155,-88.2209837816518,119.583232347667));
#39513=CARTESIAN_POINT('Ctrl Pts',(38.6473843233466,-89.1067094715124,119.530582839936));
#39514=CARTESIAN_POINT('Ctrl Pts',(38.026661521466,-89.656381172705,119.477933332205));
#39515=CARTESIAN_POINT('Ctrl Pts',(37.4059387195854,-90.2060528738975,119.425283824474));
#39516=CARTESIAN_POINT('Ctrl Pts',(36.4876283820932,-90.4196705864219,119.372634316743));
#39517=CARTESIAN_POINT('Ctrl Pts',(35.6880325259561,-90.2003939587395,119.319984809013));
#39518=CARTESIAN_POINT('Ctrl Pts',(34.888436669819,-89.9811173310572,119.267335301282));
#39519=CARTESIAN_POINT('Ctrl Pts',(34.2075552950369,-89.3289463631679,119.214685793551));
#39520=CARTESIAN_POINT('Ctrl Pts',(33.9540556236766,-88.5395328507908,119.16203628582));
#39521=CARTESIAN_POINT('Ctrl Pts',(33.8746859988896,-88.2923709750261,119.145551958044));
#39522=CARTESIAN_POINT('Ctrl Pts',(33.8372121057229,-88.0317553721487,119.129067630268));
#39523=CARTESIAN_POINT('Ctrl Pts',(33.8392145615825,-87.7705794701237,119.112583302492));
#39524=CARTESIAN_POINT('Ctrl Pts',(33.8412617315361,-87.7680141434736,119.387416697508));
#39525=CARTESIAN_POINT('Ctrl Pts',(33.8421398387907,-88.2199980597614,119.415885674646));
#39526=CARTESIAN_POINT('Ctrl Pts',(33.9585452695053,-88.6724038353267,119.444354651783));
#39527=CARTESIAN_POINT('Ctrl Pts',(34.18774755072,-89.0577118621484,119.472823628921));
#39528=CARTESIAN_POINT('Ctrl Pts',(34.6116260490043,-89.7702867410744,119.525473136651));
#39529=CARTESIAN_POINT('Ctrl Pts',(35.4212864724672,-90.2533773873225,119.578122644382));
#39530=CARTESIAN_POINT('Ctrl Pts',(36.2496816025878,-90.2879821231239,119.630772152113));
#39531=CARTESIAN_POINT('Ctrl Pts',(37.0780767327084,-90.3225868589254,119.683421659844));
#39532=CARTESIAN_POINT('Ctrl Pts',(37.9252065694868,-89.9087056842802,119.736071167575));
#39533=CARTESIAN_POINT('Ctrl Pts',(38.4070376381075,-89.2339650881938,119.788720675305));
#39534=CARTESIAN_POINT('Ctrl Pts',(38.8888687067281,-88.5592244921074,119.841370183036));
#39535=CARTESIAN_POINT('Ctrl Pts',(39.0054010071911,-87.62362447458,119.894019690767));
#39536=CARTESIAN_POINT('Ctrl Pts',(38.703806486657,-86.8513055855209,119.946669198498));
#39537=CARTESIAN_POINT('Ctrl Pts',(38.4022119661228,-86.0789866964619,119.999318706229));
#39538=CARTESIAN_POINT('Ctrl Pts',(37.6824906245914,-85.4699489358712,120.05196821396));
#39539=CARTESIAN_POINT('Ctrl Pts',(36.8709169952967,-85.3002892631886,120.10461772169));
#39540=CARTESIAN_POINT('Ctrl Pts',(36.0593433660019,-85.130629590506,120.157267229421));
#39541=CARTESIAN_POINT('Ctrl Pts',(35.1559174489438,-85.4003480057315,120.209916737152));
#39542=CARTESIAN_POINT('Ctrl Pts',(34.5701940408579,-85.9871739218915,120.262566244883));
#39543=CARTESIAN_POINT('Ctrl Pts',(34.1072088154528,-86.4510306251003,120.304183062425));
#39544=CARTESIAN_POINT('Ctrl Pts',(33.8427278117577,-87.1130197820786,120.345799879966));
#39545=CARTESIAN_POINT('Ctrl Pts',(33.8367589339947,-87.7707538181913,120.387416697508));
#39546=CARTESIAN_POINT('Origin',(36.3549260746835,-87.7685555885722,114.));
#39547=CARTESIAN_POINT('',(33.8347233377312,-87.7669766891919,121.387416697508));
#39548=CARTESIAN_POINT('',(33.8399315564717,-87.7667938053724,121.112583302492));
#39549=CARTESIAN_POINT('',(33.8374260746835,-87.7685555885722,114.));
#39550=CARTESIAN_POINT('',(38.2683920713486,-86.1325683851973,122.));
#39551=CARTESIAN_POINT('Ctrl Pts',(33.8347233377312,-87.7669766891919,121.387416697508));
#39552=CARTESIAN_POINT('Ctrl Pts',(33.8401813734862,-88.496199628224,121.43366260848));
#39553=CARTESIAN_POINT('Ctrl Pts',(34.1747110856035,-89.2296737968849,121.479908519451));
#39554=CARTESIAN_POINT('Ctrl Pts',(34.7321881734164,-89.698507092816,121.526154430423));
#39555=CARTESIAN_POINT('Ctrl Pts',(35.3668582151122,-90.2322589796322,121.578803938153));
#39556=CARTESIAN_POINT('Ctrl Pts',(36.2904926403925,-90.4230071131142,121.631453445884));
#39557=CARTESIAN_POINT('Ctrl Pts',(37.0841095365915,-90.1828532978381,121.684102953615));
#39558=CARTESIAN_POINT('Ctrl Pts',(37.8777264327904,-89.942699482562,121.736752461346));
#39559=CARTESIAN_POINT('Ctrl Pts',(38.5413257999079,-89.2716437185279,121.789401969077));
#39560=CARTESIAN_POINT('Ctrl Pts',(38.7742910561279,-88.477357745742,121.842051476808));
#39561=CARTESIAN_POINT('Ctrl Pts',(39.0072563123478,-87.6830717729562,121.894700984538));
#39562=CARTESIAN_POINT('Ctrl Pts',(38.8095874576702,-86.7655555914187,121.947350492269));
#39563=CARTESIAN_POINT('Ctrl Pts',(38.2683920713486,-86.1325683851972,122.));
#39564=CARTESIAN_POINT('',(34.4378159936203,-86.1300277429912,122.));
#39565=CARTESIAN_POINT('Origin',(36.3549260746835,-87.7685555885722,122.));
#39566=CARTESIAN_POINT('Ctrl Pts',(34.4378071488063,-86.1300215764196,122.));
#39567=CARTESIAN_POINT('Ctrl Pts',(34.9606277583611,-85.5213062324827,121.949053726697));
#39568=CARTESIAN_POINT('Ctrl Pts',(35.8003521387853,-85.1811303941408,121.898107453395));
#39569=CARTESIAN_POINT('Ctrl Pts',(36.599022889058,-85.2588932747863,121.847161180092));
#39570=CARTESIAN_POINT('Ctrl Pts',(37.4243947782061,-85.3392559219499,121.794511672361));
#39571=CARTESIAN_POINT('Ctrl Pts',(38.2059221439901,-85.8659694487247,121.74186216463));
#39572=CARTESIAN_POINT('Ctrl Pts',(38.5898067252272,-86.6007560705761,121.6892126569));
#39573=CARTESIAN_POINT('Ctrl Pts',(38.9736913064644,-87.3355426924275,121.636563149169));
#39574=CARTESIAN_POINT('Ctrl Pts',(38.9599331031547,-88.2784024093554,121.583913641438));
#39575=CARTESIAN_POINT('Ctrl Pts',(38.5545283643142,-89.0016621462416,121.531264133707));
#39576=CARTESIAN_POINT('Ctrl Pts',(38.1491236254738,-89.7249218831277,121.478614625976));
#39577=CARTESIAN_POINT('Ctrl Pts',(37.3520723511026,-90.2285816399721,121.425965118245));
#39578=CARTESIAN_POINT('Ctrl Pts',(36.5248227148927,-90.2844325978802,121.373315610515));
#39579=CARTESIAN_POINT('Ctrl Pts',(35.6975730786827,-90.3402835557883,121.320666102784));
#39580=CARTESIAN_POINT('Ctrl Pts',(34.840125080634,-89.9483257147602,121.268016595053));
#39581=CARTESIAN_POINT('Ctrl Pts',(34.3411327859834,-89.2861899807625,121.215367087322));
#39582=CARTESIAN_POINT('Ctrl Pts',(34.0164173938504,-88.8553102521269,121.181105825712));
#39583=CARTESIAN_POINT('Ctrl Pts',(33.8434956388037,-88.3100194968416,121.146844564102));
#39584=CARTESIAN_POINT('Ctrl Pts',(33.8399315564717,-87.7667938053724,121.112583302492));
#39585=CARTESIAN_POINT('Origin',(36.3549260746835,-87.7685555885722,124.208423447177));
#39586=CARTESIAN_POINT('',(33.276656425091,-87.7677421016288,107.791576552823));
#39587=CARTESIAN_POINT('',(33.2862968534675,-87.7682412892605,107.708423447177));
#39588=CARTESIAN_POINT('',(33.2814260746835,-87.768555588572,124.208423447177));
#39589=CARTESIAN_POINT('',(37.1487253572159,-90.7377785423181,107.));
#39590=CARTESIAN_POINT('Ctrl Pts',(33.2862968534675,-87.7682412892604,107.708423447177));
#39591=CARTESIAN_POINT('Ctrl Pts',(33.2859769912424,-87.2730658011076,107.682880329042));
#39592=CARTESIAN_POINT('Ctrl Pts',(33.6322292839702,-85.7577492023412,107.604687703175));
#39593=CARTESIAN_POINT('Ctrl Pts',(36.0033916884657,-84.1596935485673,107.473845569577));
#39594=CARTESIAN_POINT('Ctrl Pts',(39.1869513927685,-85.500150855768,107.315897046385));
#39595=CARTESIAN_POINT('Ctrl Pts',(39.797719117622,-88.9023362095446,107.157948523192));
#39596=CARTESIAN_POINT('Ctrl Pts',(38.1309639469875,-90.4751844899406,107.052649507731));
#39597=CARTESIAN_POINT('Ctrl Pts',(37.1487253572158,-90.7377785423181,107.));
#39598=CARTESIAN_POINT('',(35.5611267921502,-90.7377785423178,107.));
#39599=CARTESIAN_POINT('Origin',(36.3549260746835,-87.7685555885722,107.));
#39600=CARTESIAN_POINT('Ctrl Pts',(33.276656425091,-87.7677421016288,107.791576552823));
#39601=CARTESIAN_POINT('Ctrl Pts',(33.2765003562394,-87.7232332639992,107.789262006108));
#39602=CARTESIAN_POINT('Ctrl Pts',(33.2974600730684,-86.6664238442207,107.734297951662));
#39603=CARTESIAN_POINT('Ctrl Pts',(34.5067289212608,-84.6483928869776,107.626684389485));
#39604=CARTESIAN_POINT('Ctrl Pts',(37.9573945529429,-84.5150172531596,107.468735866293));
#39605=CARTESIAN_POINT('Ctrl Pts',(39.9550036656341,-87.3323307232591,107.3107873431));
#39606=CARTESIAN_POINT('Ctrl Pts',(38.7024883475988,-90.5088734081208,107.154542054336));
#39607=CARTESIAN_POINT('Ctrl Pts',(36.5061793313629,-90.9937479331884,107.050946273303));
#39608=CARTESIAN_POINT('Ctrl Pts',(35.5592127764325,-90.7428670628568,107.));
#39609=CARTESIAN_POINT('Origin',(36.3549260746835,-87.7685555885722,124.208423447177));
#39610=CARTESIAN_POINT('',(33.2850146722309,-87.7666901939308,108.791576552823));
#39611=CARTESIAN_POINT('',(33.2798330221166,-87.7711138662328,108.708423447177));
#39612=CARTESIAN_POINT('',(33.2814260746835,-87.768555588572,124.208423447177));
#39613=CARTESIAN_POINT('Ctrl Pts',(33.2798330221166,-87.7711138662328,108.708423447178));
#39614=CARTESIAN_POINT('Ctrl Pts',(33.2872208788364,-86.9423658028956,108.665444042093));
#39615=CARTESIAN_POINT('Ctrl Pts',(34.0588699517531,-85.0862753096796,108.569815129278));
#39616=CARTESIAN_POINT('Ctrl Pts',(37.1879239371534,-84.238982297281,108.421536708732));
#39617=CARTESIAN_POINT('Ctrl Pts',(39.7658202422379,-86.5365567546996,108.26358818554));
#39618=CARTESIAN_POINT('Ctrl Pts',(39.2510962268136,-89.9512136310206,108.105639662347));
#39619=CARTESIAN_POINT('Ctrl Pts',(36.1106392104622,-91.3867839779253,107.947691139155));
#39620=CARTESIAN_POINT('Ctrl Pts',(33.6634844053523,-89.8404170618379,107.815285734098));
#39621=CARTESIAN_POINT('Ctrl Pts',(33.2866362916695,-88.2937221498332,107.735529836772));
#39622=CARTESIAN_POINT('Ctrl Pts',(33.2862968534675,-87.7682412892604,107.708423447177));
#39623=CARTESIAN_POINT('Ctrl Pts',(33.2850146722309,-87.7666901939308,108.791576552823));
#39624=CARTESIAN_POINT('Ctrl Pts',(33.2828705409932,-87.3842072553396,108.771825719159));
#39625=CARTESIAN_POINT('Ctrl Pts',(33.5258649413941,-85.9847713296537,108.699425377765));
#39626=CARTESIAN_POINT('Ctrl Pts',(35.6128383524474,-84.2187467086474,108.57437552864));
#39627=CARTESIAN_POINT('Ctrl Pts',(38.9216913848391,-85.2066069974257,108.416427005448));
#39628=CARTESIAN_POINT('Ctrl Pts',(39.9033344292869,-88.5173188003331,108.258478482255));
#39629=CARTESIAN_POINT('Ctrl Pts',(37.6677475399111,-91.14912788279,108.100529959063));
#39630=CARTESIAN_POINT('Ctrl Pts',(34.2920594545513,-90.7222680374125,107.944895982585));
#39631=CARTESIAN_POINT('Ctrl Pts',(33.2800504890387,-88.7356856702426,107.841911513839));
#39632=CARTESIAN_POINT('Ctrl Pts',(33.276656425091,-87.7677421016288,107.791576552823));
#39633=CARTESIAN_POINT('Origin',(36.3549260746835,-87.7685555885722,124.208423447177));
#39634=CARTESIAN_POINT('',(33.2830914204259,-87.7711482488633,109.791576552823));
#39635=CARTESIAN_POINT('',(33.2787950739713,-87.766287537244,109.708423447178));
#39636=CARTESIAN_POINT('',(33.2814260746835,-87.768555588572,124.208423447177));
#39637=CARTESIAN_POINT('Ctrl Pts',(33.2787950739713,-87.766287537244,109.708423447178));
#39638=CARTESIAN_POINT('Ctrl Pts',(33.2775559525143,-87.6166677820898,109.700657262876));
#39639=CARTESIAN_POINT('Ctrl Pts',(33.3552188510478,-86.4540177546672,109.640241570843));
#39640=CARTESIAN_POINT('Ctrl Pts',(34.8365759788977,-84.4751585833882,109.527176371079));
#39641=CARTESIAN_POINT('Ctrl Pts',(38.2826268788027,-84.6967777516425,109.369227847887));
#39642=CARTESIAN_POINT('Ctrl Pts',(39.9808905139985,-87.7034840332521,109.211279324694));
#39643=CARTESIAN_POINT('Ctrl Pts',(38.3916015946044,-90.7691895942252,109.053330801502));
#39644=CARTESIAN_POINT('Ctrl Pts',(34.9557227260359,-91.1143097541466,108.89538227831));
#39645=CARTESIAN_POINT('Ctrl Pts',(33.3781908644244,-89.1574729097927,108.780413160201));
#39646=CARTESIAN_POINT('Ctrl Pts',(33.278170799648,-87.9575770996091,108.718093549824));
#39647=CARTESIAN_POINT('Ctrl Pts',(33.2798330221166,-87.7711138662328,108.708423447178));
#39648=CARTESIAN_POINT('Ctrl Pts',(33.2830914204259,-87.7711482488633,109.791576552823));
#39649=CARTESIAN_POINT('Ctrl Pts',(33.2889508656634,-87.052142123377,109.754389432211));
#39650=CARTESIAN_POINT('Ctrl Pts',(33.8981617705012,-85.3062204171677,109.664552803868));
#39651=CARTESIAN_POINT('Ctrl Pts',(36.7983710322676,-84.1692218413362,109.522066667795));
#39652=CARTESIAN_POINT('Ctrl Pts',(39.611248718183,-86.1722442141325,109.364118144603));
#39653=CARTESIAN_POINT('Ctrl Pts',(39.4717176740767,-89.6225937013098,109.20616962141));
#39654=CARTESIAN_POINT('Ctrl Pts',(36.506286532656,-91.3919429301732,109.048221098218));
#39655=CARTESIAN_POINT('Ctrl Pts',(33.7915972796456,-90.0656305669141,108.910023408688));
#39656=CARTESIAN_POINT('Ctrl Pts',(33.2885861201985,-88.4037864171892,108.82447522689));
#39657=CARTESIAN_POINT('Ctrl Pts',(33.2850146722309,-87.7666901939308,108.791576552823));
#39658=CARTESIAN_POINT('Origin',(36.3549260746835,-87.7685555885722,124.208423447177));
#39659=CARTESIAN_POINT('',(33.2765846421026,-87.7678707817249,110.791576552823));
#39660=CARTESIAN_POINT('',(33.2862067465171,-87.7682071721922,110.708423447177));
#39661=CARTESIAN_POINT('',(33.2814260746835,-87.768555588572,124.208423447177));
#39662=CARTESIAN_POINT('Ctrl Pts',(33.2862067465171,-87.7682071721922,110.708423447177));
#39663=CARTESIAN_POINT('Ctrl Pts',(33.2857074510608,-87.2796756315349,110.683220975927));
#39664=CARTESIAN_POINT('Ctrl Pts',(33.6253685298192,-85.7712275726879,110.605368996946));
#39665=CARTESIAN_POINT('Ctrl Pts',(35.9808934716759,-84.1613474908357,110.474867510234));
#39666=CARTESIAN_POINT('Ctrl Pts',(39.1709557485403,-85.4834237534817,110.316918987042));
#39667=CARTESIAN_POINT('Ctrl Pts',(39.8078095714184,-88.8773595462129,110.158970463849));
#39668=CARTESIAN_POINT('Ctrl Pts',(37.3140389309351,-91.2659765249159,110.001021940657));
#39669=CARTESIAN_POINT('Ctrl Pts',(34.1160436361588,-90.5220575995161,109.850839601766));
#39670=CARTESIAN_POINT('Ctrl Pts',(33.285956362831,-88.6309891205378,109.753306770607));
#39671=CARTESIAN_POINT('Ctrl Pts',(33.2787950739713,-87.766287537244,109.708423447178));
#39672=CARTESIAN_POINT('Ctrl Pts',(33.2765846421026,-87.7678707817249,110.791576552823));
#39673=CARTESIAN_POINT('Ctrl Pts',(33.2764689981345,-87.7299144954526,110.789602652993));
#39674=CARTESIAN_POINT('Ctrl Pts',(33.2942329377382,-86.679667114291,110.734979245433));
#39675=CARTESIAN_POINT('Ctrl Pts',(34.4867514469574,-84.660216714833,110.627706330142));
#39676=CARTESIAN_POINT('Ctrl Pts',(37.9364315130628,-84.5050164759499,110.46975780695));
#39677=CARTESIAN_POINT('Ctrl Pts',(39.9522086976689,-87.3087678935207,110.311809283757));
#39678=CARTESIAN_POINT('Ctrl Pts',(38.7064391340791,-90.5293948322461,110.153860760565));
#39679=CARTESIAN_POINT('Ctrl Pts',(35.3286241982722,-91.2468527920333,109.995912237372));
#39680=CARTESIAN_POINT('Ctrl Pts',(33.4575135227322,-89.3842210456531,109.875150834792));
#39681=CARTESIAN_POINT('Ctrl Pts',(33.2806550658742,-88.070110654944,109.807038939942));
#39682=CARTESIAN_POINT('Ctrl Pts',(33.2830914204259,-87.7711482488633,109.791576552823));
#39683=CARTESIAN_POINT('Origin',(36.3549260746835,-87.7685555885722,124.208423447177));
#39684=CARTESIAN_POINT('',(33.2848890248079,-87.7666135332359,111.791576552823));
#39685=CARTESIAN_POINT('',(33.2800259451788,-87.7711513823149,111.708423447177));
#39686=CARTESIAN_POINT('',(33.2814260746835,-87.768555588572,124.208423447177));
#39687=CARTESIAN_POINT('Ctrl Pts',(33.2800259451788,-87.7711513823149,111.708423447177));
#39688=CARTESIAN_POINT('Ctrl Pts',(33.2874068247419,-86.9488393585243,111.665784688979));
#39689=CARTESIAN_POINT('Ctrl Pts',(34.0488667873028,-85.0990844447291,111.570496423049));
#39690=CARTESIAN_POINT('Ctrl Pts',(37.1652521907151,-84.2336974260193,111.422558649389));
#39691=CARTESIAN_POINT('Ctrl Pts',(39.7578211449723,-86.5146992235859,111.264610126197));
#39692=CARTESIAN_POINT('Ctrl Pts',(39.2650886334483,-89.9325344528934,111.106661603004));
#39693=CARTESIAN_POINT('Ctrl Pts',(36.1338002383326,-91.3883558605165,110.948713079812));
#39694=CARTESIAN_POINT('Ctrl Pts',(33.6706422156574,-89.8535959444207,110.815967027869));
#39695=CARTESIAN_POINT('Ctrl Pts',(33.2867505098833,-88.300247974271,110.735870483658));
#39696=CARTESIAN_POINT('Ctrl Pts',(33.2862067465171,-87.7682071721922,110.708423447177));
#39697=CARTESIAN_POINT('Ctrl Pts',(33.2848890248079,-87.7666135332359,111.791576552823));
#39698=CARTESIAN_POINT('Ctrl Pts',(33.2826893479257,-87.3907660509209,111.772166366045));
#39699=CARTESIAN_POINT('Ctrl Pts',(33.5201236359259,-85.9981265337506,111.700106671536));
#39700=CARTESIAN_POINT('Ctrl Pts',(35.5900605844347,-84.2235834060515,111.575397469297));
#39701=CARTESIAN_POINT('Ctrl Pts',(38.9051876872665,-85.1901815465887,111.417448946105));
#39702=CARTESIAN_POINT('Ctrl Pts',(39.9080701486722,-88.4945130132787,111.259500422912));
#39703=CARTESIAN_POINT('Ctrl Pts',(37.6894249421801,-91.1406409620089,111.10155189972));
#39704=CARTESIAN_POINT('Ctrl Pts',(34.3036777199347,-90.7345409621052,110.945577276356));
#39705=CARTESIAN_POINT('Ctrl Pts',(33.2795535508054,-88.7423163194395,110.842252160724));
#39706=CARTESIAN_POINT('Ctrl Pts',(33.2765846421026,-87.7678707817249,110.791576552823));
#39707=CARTESIAN_POINT('Origin',(36.3549260746835,-87.7685555885722,124.208423447177));
#39708=CARTESIAN_POINT('',(33.2832675127287,-87.7711115886087,112.791576552823));
#39709=CARTESIAN_POINT('',(33.2786192921776,-87.7663532934355,112.708423447177));
#39710=CARTESIAN_POINT('',(33.2814260746835,-87.768555588572,124.208423447177));
#39711=CARTESIAN_POINT('Ctrl Pts',(33.2786192921776,-87.7663532934355,112.708423447177));
#39712=CARTESIAN_POINT('Ctrl Pts',(33.2774584286707,-87.6233176056221,112.700997909761));
#39713=CARTESIAN_POINT('Ctrl Pts',(33.3512647595745,-86.467315453029,112.640922864614));
#39714=CARTESIAN_POINT('Ctrl Pts',(34.8154603259275,-84.484975857241,112.528198311736));
#39715=CARTESIAN_POINT('Ctrl Pts',(38.2628633754255,-84.6844631937108,112.370249788544));
#39716=CARTESIAN_POINT('Ctrl Pts',(39.9803977016302,-87.6802033061719,112.212301265351));
#39717=CARTESIAN_POINT('Ctrl Pts',(38.4108271674185,-90.7560497459711,112.054352742159));
#39718=CARTESIAN_POINT('Ctrl Pts',(34.9772336398273,-91.1232260937864,111.896404218966));
#39719=CARTESIAN_POINT('Ctrl Pts',(33.3824604435757,-89.1707887589986,111.781094453973));
#39720=CARTESIAN_POINT('Ctrl Pts',(33.2782930584871,-87.9642142212732,111.71843419671));
#39721=CARTESIAN_POINT('Ctrl Pts',(33.2800259451788,-87.7711513823149,111.708423447177));
#39722=CARTESIAN_POINT('Ctrl Pts',(33.2832675127287,-87.7711115886087,112.791576552823));
#39723=CARTESIAN_POINT('Ctrl Pts',(33.2889665649355,-87.0585882653705,112.754730079097));
#39724=CARTESIAN_POINT('Ctrl Pts',(33.889317805798,-85.3192833343254,112.66523409764));
#39725=CARTESIAN_POINT('Ctrl Pts',(36.7752505778273,-84.1664486627489,112.523088608452));
#39726=CARTESIAN_POINT('Ctrl Pts',(39.6009316700625,-86.1513683181001,112.365140085259));
#39727=CARTESIAN_POINT('Ctrl Pts',(39.4835582117651,-89.6025424870611,112.207191562067));
#39728=CARTESIAN_POINT('Ctrl Pts',(36.5295491478211,-91.3908965133523,112.049243038874));
#39729=CARTESIAN_POINT('Ctrl Pts',(33.7996873271964,-90.0788158412429,111.91070470246));
#39730=CARTESIAN_POINT('Ctrl Pts',(33.2886559007642,-88.4102402657966,111.824815873776));
#39731=CARTESIAN_POINT('Ctrl Pts',(33.2848890248079,-87.7666135332359,111.791576552823));
#39732=CARTESIAN_POINT('Origin',(36.3549260746835,-87.7685555885722,124.208423447177));
#39733=CARTESIAN_POINT('',(33.2765254057624,-87.7679866768878,113.791576552823));
#39734=CARTESIAN_POINT('',(33.2861808694117,-87.7681022535048,113.708423447177));
#39735=CARTESIAN_POINT('',(33.2814260746835,-87.768555588572,124.208423447177));
#39736=CARTESIAN_POINT('Ctrl Pts',(33.2861808694117,-87.7681022535048,113.708423447177));
#39737=CARTESIAN_POINT('Ctrl Pts',(33.285539692702,-87.2861840612657,113.683561622813));
#39738=CARTESIAN_POINT('Ctrl Pts',(33.618721455999,-85.7845535822887,113.606050290717));
#39739=CARTESIAN_POINT('Ctrl Pts',(35.9577393041295,-84.1638235162957,113.475889450891));
#39740=CARTESIAN_POINT('Ctrl Pts',(39.1562248702749,-85.4653891374834,113.317940927699));
#39741=CARTESIAN_POINT('Ctrl Pts',(39.8148580161093,-88.8551657322322,113.159992404506));
#39742=CARTESIAN_POINT('Ctrl Pts',(37.3364760997262,-91.2597459574781,113.002043881314));
#39743=CARTESIAN_POINT('Ctrl Pts',(34.1265055614965,-90.5347359476712,112.851520895538));
#39744=CARTESIAN_POINT('Ctrl Pts',(33.2856893335538,-88.6374877766429,112.753647417492));
#39745=CARTESIAN_POINT('Ctrl Pts',(33.2786192921776,-87.7663532934355,112.708423447177));
#39746=CARTESIAN_POINT('Ctrl Pts',(33.2765254057624,-87.7679866768878,113.791576552823));
#39747=CARTESIAN_POINT('Ctrl Pts',(33.2764447224955,-87.7365823392088,113.789943299879));
#39748=CARTESIAN_POINT('Ctrl Pts',(33.2910498895119,-86.6929052864662,113.735660539204));
#39749=CARTESIAN_POINT('Ctrl Pts',(34.4668313200981,-84.6722763390996,113.628728270799));
#39750=CARTESIAN_POINT('Ctrl Pts',(37.9154437312407,-84.4949289090955,113.470779747607));
#39751=CARTESIAN_POINT('Ctrl Pts',(39.949182244182,-87.2856792265183,113.312831224414));
#39752=CARTESIAN_POINT('Ctrl Pts',(38.724118002599,-90.5142388553946,113.154882701222));
#39753=CARTESIAN_POINT('Ctrl Pts',(35.3509794956904,-91.2533709724249,112.996934178029));
#39754=CARTESIAN_POINT('Ctrl Pts',(33.4626357327023,-89.3975718565036,112.875832128563));
#39755=CARTESIAN_POINT('Ctrl Pts',(33.2808232539786,-88.0767047476726,112.807379586827));
#39756=CARTESIAN_POINT('Ctrl Pts',(33.2832675127287,-87.7711115886087,112.791576552823));
#39757=CARTESIAN_POINT('Origin',(36.3549260746835,-87.7685555885722,124.208423447177));
#39758=CARTESIAN_POINT('',(33.2847581226811,-87.7665395828602,114.791576552823));
#39759=CARTESIAN_POINT('',(33.2802201284861,-87.7711845286359,114.708423447177));
#39760=CARTESIAN_POINT('',(33.2814260746835,-87.768555588572,124.208423447177));
#39761=CARTESIAN_POINT('Ctrl Pts',(33.2802201284861,-87.7711845286358,114.708423447177));
#39762=CARTESIAN_POINT('Ctrl Pts',(33.2875819596571,-86.9553091102221,114.666125335864));
#39763=CARTESIAN_POINT('Ctrl Pts',(34.0389366156125,-85.1119079714602,114.571177716821));
#39764=CARTESIAN_POINT('Ctrl Pts',(37.1425381673794,-84.2285671938113,114.423580590046));
#39765=CARTESIAN_POINT('Ctrl Pts',(39.749699985204,-86.4928750877993,114.265632066854));
#39766=CARTESIAN_POINT('Ctrl Pts',(39.278923545741,-89.9138036937695,114.107683543661));
#39767=CARTESIAN_POINT('Ctrl Pts',(36.1570475286333,-91.3897010875291,113.949735020469));
#39768=CARTESIAN_POINT('Ctrl Pts',(33.6777395898086,-89.8668909803513,113.816648321641));
#39769=CARTESIAN_POINT('Ctrl Pts',(33.2868975028787,-88.3067348951798,113.736211130544));
#39770=CARTESIAN_POINT('Ctrl Pts',(33.2861808694117,-87.7681022535048,113.708423447177));
#39771=CARTESIAN_POINT('Ctrl Pts',(33.2847581226811,-87.7665395828602,114.791576552823));
#39772=CARTESIAN_POINT('Ctrl Pts',(33.2825086201721,-87.3973277786715,114.772507012931));
#39773=CARTESIAN_POINT('Ctrl Pts',(33.5144370064031,-86.011481870544,114.700787965308));
#39774=CARTESIAN_POINT('Ctrl Pts',(35.5673140912984,-84.2285676851132,114.576419409954));
#39775=CARTESIAN_POINT('Ctrl Pts',(38.8885793784847,-85.1738594735819,114.418470886761));
#39776=CARTESIAN_POINT('Ctrl Pts',(39.9126582726965,-88.4716833153973,114.260522363569));
#39777=CARTESIAN_POINT('Ctrl Pts',(37.7110495865035,-91.1320026319635,114.102573840377));
#39778=CARTESIAN_POINT('Ctrl Pts',(34.3153646157072,-90.7468114612145,113.946258570128));
#39779=CARTESIAN_POINT('Ctrl Pts',(33.2790456266009,-88.7489319117899,113.84259280761));
#39780=CARTESIAN_POINT('Ctrl Pts',(33.2765254057624,-87.7679866768878,113.791576552823));
#39781=CARTESIAN_POINT('Origin',(36.3549260746835,-87.7685555885722,124.208423447177));
#39782=CARTESIAN_POINT('',(33.2834402980838,-87.7710709634421,115.791576552823));
#39783=CARTESIAN_POINT('',(33.2784473899845,-87.766423078844,115.708423447177));
#39784=CARTESIAN_POINT('',(33.2814260746835,-87.768555588572,124.208423447177));
#39785=CARTESIAN_POINT('Ctrl Pts',(33.2784473899845,-87.766423078844,115.708423447177));
#39786=CARTESIAN_POINT('Ctrl Pts',(33.277364854453,-87.6299690776632,115.701338556647));
#39787=CARTESIAN_POINT('Ctrl Pts',(33.3473575742145,-86.4806099825772,115.641604158385));
#39788=CARTESIAN_POINT('Ctrl Pts',(34.7944082015486,-84.4949284547604,115.529220252393));
#39789=CARTESIAN_POINT('Ctrl Pts',(38.2430210913116,-84.6722759093786,115.371271729201));
#39790=CARTESIAN_POINT('Ctrl Pts',(39.979755653312,-87.6569259800321,115.213323206008));
#39791=CARTESIAN_POINT('Ctrl Pts',(38.4299674805782,-90.7427872216878,115.055374682816));
#39792=CARTESIAN_POINT('Ctrl Pts',(34.9988023746513,-91.1320030987637,114.897426159623));
#39793=CARTESIAN_POINT('Ctrl Pts',(33.3867772569319,-89.1841085494937,114.781775747744));
#39794=CARTESIAN_POINT('Ctrl Pts',(33.2784185058971,-87.9708494692539,114.718774843595));
#39795=CARTESIAN_POINT('Ctrl Pts',(33.2802201284861,-87.7711845286358,114.708423447177));
#39796=CARTESIAN_POINT('Ctrl Pts',(33.2834402980838,-87.7710709634421,115.791576552823));
#39797=CARTESIAN_POINT('Ctrl Pts',(33.2889738902515,-87.0650343515427,115.755070725982));
#39798=CARTESIAN_POINT('Ctrl Pts',(33.880540019459,-85.3323584119177,115.665915391411));
#39799=CARTESIAN_POINT('Ctrl Pts',(36.7521127901144,-84.1638240165833,115.524110549109));
#39800=CARTESIAN_POINT('Ctrl Pts',(39.5904807973608,-86.1305590594033,115.366162025916));
#39801=CARTESIAN_POINT('Ctrl Pts',(39.4952697425043,-89.5824157378083,115.208213502724));
#39802=CARTESIAN_POINT('Ctrl Pts',(36.55280459327,-91.3897005849636,115.050264979531));
#39803=CARTESIAN_POINT('Ctrl Pts',(33.8078412450219,-90.0919923385608,114.911385996231));
#39804=CARTESIAN_POINT('Ctrl Pts',(33.2887193206088,-88.4166926846419,114.825156520661));
#39805=CARTESIAN_POINT('Ctrl Pts',(33.2847581226811,-87.7665395828602,114.791576552823));
#39806=CARTESIAN_POINT('Origin',(36.3549260746835,-87.7685555885722,124.208423447177));
#39807=CARTESIAN_POINT('',(33.2764765005074,-87.7681038465887,116.791576552823));
#39808=CARTESIAN_POINT('',(33.286148224798,-87.7679979949527,116.708423447177));
#39809=CARTESIAN_POINT('',(33.2814260746835,-87.768555588572,124.208423447177));
#39810=CARTESIAN_POINT('Ctrl Pts',(33.286148224798,-87.7679979949527,116.708423447177));
#39811=CARTESIAN_POINT('Ctrl Pts',(33.2853699201791,-87.2926954938565,116.683902269698));
#39812=CARTESIAN_POINT('Ctrl Pts',(33.6121327235052,-85.7978827795205,116.606731584489));
#39813=CARTESIAN_POINT('Ctrl Pts',(35.9346015132054,-84.1664481628253,116.476911391548));
#39814=CARTESIAN_POINT('Ctrl Pts',(39.1413784939057,-85.4474494817745,116.318962868356));
#39815=CARTESIAN_POINT('Ctrl Pts',(39.8217638122167,-88.8329271145059,116.161014345163));
#39816=CARTESIAN_POINT('Ctrl Pts',(37.35887279301,-91.2533714560701,116.003065821971));
#39817=CARTESIAN_POINT('Ctrl Pts',(34.1370383056434,-90.5473935246883,115.852202189309));
#39818=CARTESIAN_POINT('Ctrl Pts',(33.2854094336303,-88.6439912363789,115.753988064378));
#39819=CARTESIAN_POINT('Ctrl Pts',(33.2784473899845,-87.766423078844,115.708423447177));
#39820=CARTESIAN_POINT('Ctrl Pts',(33.2764765005074,-87.7681038465887,116.791576552823));
#39821=CARTESIAN_POINT('Ctrl Pts',(33.2764250132567,-87.7432505594706,116.790283946765));
#39822=CARTESIAN_POINT('Ctrl Pts',(33.2879105001274,-86.7061397062465,116.736341832976));
#39823=CARTESIAN_POINT('Ctrl Pts',(34.446989038738,-84.6844636217403,116.629750211456));
#39824=CARTESIAN_POINT('Ctrl Pts',(37.8943916097836,-84.4849763129574,116.471801688264));
#39825=CARTESIAN_POINT('Ctrl Pts',(39.9460076008814,-87.2626104678248,116.313853165071));
#39826=CARTESIAN_POINT('Ctrl Pts',(38.7416991899834,-90.4989696760488,116.155904641879));
#39827=CARTESIAN_POINT('Ctrl Pts',(35.3733761858658,-91.2597454729484,115.997956118686));
#39828=CARTESIAN_POINT('Ctrl Pts',(33.467810152958,-89.4109237193908,115.876513422334));
#39829=CARTESIAN_POINT('Ctrl Pts',(33.2809932217164,-88.0832959079491,115.807720233713));
#39830=CARTESIAN_POINT('Ctrl Pts',(33.2834402980838,-87.7710709634421,115.791576552823));
#39831=CARTESIAN_POINT('Origin',(36.3549260746835,-87.7685555885722,124.208423447177));
#39832=CARTESIAN_POINT('',(33.2846220850711,-87.7664686536375,117.791576552823));
#39833=CARTESIAN_POINT('',(33.2804153315645,-87.7712132051916,117.708423447177));
#39834=CARTESIAN_POINT('',(33.2814260746835,-87.768555588572,124.208423447177));
#39835=CARTESIAN_POINT('Ctrl Pts',(33.2804153315645,-87.7712132051916,117.708423447177));
#39836=CARTESIAN_POINT('Ctrl Pts',(33.2877457498334,-86.961775983013,117.66646598275));
#39837=CARTESIAN_POINT('Ctrl Pts',(34.029075750275,-85.1247490441378,117.571859010592));
#39838=CARTESIAN_POINT('Ctrl Pts',(37.1197916710861,-84.2235829140579,117.424602530703));
#39839=CARTESIAN_POINT('Ctrl Pts',(39.7414388600909,-86.4711035478885,117.26665400751));
#39840=CARTESIAN_POINT('Ctrl Pts',(39.2926379026969,-89.8949844867843,117.108705484318));
#39841=CARTESIAN_POINT('Ctrl Pts',(36.1803029773098,-91.3908970160839,116.950756961125));
#39842=CARTESIAN_POINT('Ctrl Pts',(33.6848972884743,-89.8801809978657,116.817329615412));
#39843=CARTESIAN_POINT('Ctrl Pts',(33.2870410208056,-88.3132191912772,116.736551777429));
#39844=CARTESIAN_POINT('Ctrl Pts',(33.286148224798,-87.7679979949527,116.708423447177));
#39845=CARTESIAN_POINT('Ctrl Pts',(33.2846220850711,-87.7664686536375,117.791576552823));
#39846=CARTESIAN_POINT('Ctrl Pts',(33.2823284532367,-87.403892657692,117.772847659816));
#39847=CARTESIAN_POINT('Ctrl Pts',(33.508804776359,-86.0248374422096,117.701469259079));
#39848=CARTESIAN_POINT('Ctrl Pts',(35.544600071115,-84.2336979166091,117.577441350611));
#39849=CARTESIAN_POINT('Ctrl Pts',(38.87186660808,-85.1576443789841,117.419492827418));
#39850=CARTESIAN_POINT('Ctrl Pts',(39.9170997126827,-88.4488246277999,117.261544304226));
#39851=CARTESIAN_POINT('Ctrl Pts',(37.7326183183341,-91.1232256282042,117.103595781033));
#39852=CARTESIAN_POINT('Ctrl Pts',(34.3271248220504,-90.7590541983513,116.946939863899));
#39853=CARTESIAN_POINT('Ctrl Pts',(33.2785221552211,-88.7555569185142,116.842933454495));
#39854=CARTESIAN_POINT('Ctrl Pts',(33.2764765005074,-87.7681038465887,116.791576552823));
#39855=CARTESIAN_POINT('Origin',(36.3549260746835,-87.7685555885722,124.208423447177));
#39856=CARTESIAN_POINT('',(33.2836095561072,-87.7710264525037,118.791576552823));
#39857=CARTESIAN_POINT('',(33.2782797302468,-87.7664967944082,118.708423447177));
#39858=CARTESIAN_POINT('',(33.2814260746835,-87.768555588572,124.208423447177));
#39859=CARTESIAN_POINT('Ctrl Pts',(33.2782797302468,-87.7664967944082,118.708423447177));
#39860=CARTESIAN_POINT('Ctrl Pts',(33.2772752951819,-87.6366221208762,118.701679203533));
#39861=CARTESIAN_POINT('Ctrl Pts',(33.3434970963766,-86.4939012863813,118.642285452157));
#39862=CARTESIAN_POINT('Ctrl Pts',(34.7734204168137,-84.5050160230137,118.53024219305));
#39863=CARTESIAN_POINT('Ctrl Pts',(38.2231009616876,-84.6602162834389,118.372293669858));
#39864=CARTESIAN_POINT('Ctrl Pts',(39.9789641545662,-87.6336532564003,118.214345146665));
#39865=CARTESIAN_POINT('Ctrl Pts',(38.4490222405119,-90.7294020708598,118.056396623473));
#39866=CARTESIAN_POINT('Ctrl Pts',(35.0204270219759,-91.1406414300081,117.89844810028));
#39867=CARTESIAN_POINT('Ctrl Pts',(33.3911427650589,-89.1974309536143,117.782457041515));
#39868=CARTESIAN_POINT('Ctrl Pts',(33.278547317121,-87.9774825293533,117.719115490481));
#39869=CARTESIAN_POINT('Ctrl Pts',(33.2804153315645,-87.7712132051916,117.708423447177));
#39870=CARTESIAN_POINT('Ctrl Pts',(33.2836095561072,-87.7710264525037,118.791576552823));
#39871=CARTESIAN_POINT('Ctrl Pts',(33.2889730288622,-87.0714805284451,118.755411372868));
#39872=CARTESIAN_POINT('Ctrl Pts',(33.8718282039732,-85.3454453482408,118.666596685182));
#39873=CARTESIAN_POINT('Ctrl Pts',(36.7289586257789,-84.1613479914634,118.525132489766));
#39874=CARTESIAN_POINT('Ctrl Pts',(39.5798965242524,-86.1098173350916,118.367183966573));
#39875=CARTESIAN_POINT('Ctrl Pts',(39.506851797809,-89.5622142035652,118.209235443381));
#39876=CARTESIAN_POINT('Ctrl Pts',(36.5760518803447,-91.3883553581382,118.051286920188));
#39877=CARTESIAN_POINT('Ctrl Pts',(33.816059301366,-90.1051595057121,117.912067290002));
#39878=CARTESIAN_POINT('Ctrl Pts',(33.2887761694447,-88.4231439126922,117.825497167547));
#39879=CARTESIAN_POINT('Ctrl Pts',(33.2846220850711,-87.7664686536375,117.791576552823));
#39880=CARTESIAN_POINT('Origin',(36.3549260746835,-87.7685555885722,124.208423447177));
#39881=CARTESIAN_POINT('',(33.2764382705934,-87.7682219887363,119.791576552823));
#39882=CARTESIAN_POINT('',(33.2861088517784,-87.7678945631458,119.708423447177));
#39883=CARTESIAN_POINT('',(33.2814260746835,-87.768555588572,124.208423447177));
#39884=CARTESIAN_POINT('Ctrl Pts',(33.2861088517784,-87.7678945631458,119.708423447177));
#39885=CARTESIAN_POINT('Ctrl Pts',(33.2851982987019,-87.2992099652641,119.684242916584));
#39886=CARTESIAN_POINT('Ctrl Pts',(33.6056020953296,-85.8112149377787,119.60741287826));
#39887=CARTESIAN_POINT('Ctrl Pts',(35.9114810555574,-84.1692213417312,119.477933332205));
#39888=CARTESIAN_POINT('Ctrl Pts',(39.1264172314171,-85.4296055153237,119.319984809012));
#39889=CARTESIAN_POINT('Ctrl Pts',(39.8285266726477,-88.8106446175552,119.16203628582));
#39890=CARTESIAN_POINT('Ctrl Pts',(37.3812280935308,-91.2468532747826,119.004087762628));
#39891=CARTESIAN_POINT('Ctrl Pts',(34.1476420214725,-90.5600299555096,118.85288348308));
#39892=CARTESIAN_POINT('Ctrl Pts',(33.2851165023653,-88.6504997309026,118.754328711263));
#39893=CARTESIAN_POINT('Ctrl Pts',(33.2782797302468,-87.7664967944082,118.708423447177));
#39894=CARTESIAN_POINT('Ctrl Pts',(33.2764382705934,-87.7682219887363,119.791576552823));
#39895=CARTESIAN_POINT('Ctrl Pts',(33.2764098257633,-87.749919021363,119.79062459365));
#39896=CARTESIAN_POINT('Ctrl Pts',(33.2848144678827,-86.7193702351704,119.737023126747));
#39897=CARTESIAN_POINT('Ctrl Pts',(34.4272255383588,-84.6967781783805,119.630772152113));
#39898=CARTESIAN_POINT('Ctrl Pts',(37.8732759596097,-84.4751590402537,119.47282362892));
#39899=CARTESIAN_POINT('Ctrl Pts',(39.9426849263303,-87.2395625969708,119.314875105728));
#39900=CARTESIAN_POINT('Ctrl Pts',(38.7591819580553,-90.4835879091297,119.156926582536));
#39901=CARTESIAN_POINT('Ctrl Pts',(35.3958133515618,-91.2659760395494,118.998978059343));
#39902=CARTESIAN_POINT('Ctrl Pts',(33.4730370091077,-89.4242765090044,118.877194716105));
#39903=CARTESIAN_POINT('Ctrl Pts',(33.2811648498173,-88.0898841029006,118.808060880599));
#39904=CARTESIAN_POINT('Ctrl Pts',(33.2836095561072,-87.7710264525037,118.791576552823));
#39905=CARTESIAN_POINT('Origin',(36.3549260746835,-87.7685555885722,124.208423447177));
#39906=CARTESIAN_POINT('',(33.2844849022013,-87.7664047084671,120.791576552823));
#39907=CARTESIAN_POINT('',(33.2806115932904,-87.7712393060438,120.708423447177));
#39908=CARTESIAN_POINT('',(33.2814260746835,-87.768555588572,124.208423447177));
#39909=CARTESIAN_POINT('Ctrl Pts',(33.2806115932904,-87.7712393060438,120.708423447177));
#39910=CARTESIAN_POINT('Ctrl Pts',(33.2878987217132,-86.9682420627499,120.666806629636));
#39911=CARTESIAN_POINT('Ctrl Pts',(34.0192835273626,-85.1376046855688,120.572540304363));
#39912=CARTESIAN_POINT('Ctrl Pts',(37.0970139002824,-84.2187462125039,120.42562447136));
#39913=CARTESIAN_POINT('Ctrl Pts',(39.7330379835356,-86.4493848109254,120.267675948167));
#39914=CARTESIAN_POINT('Ctrl Pts',(39.3062312004495,-89.8760779436413,120.109727424975));
#39915=CARTESIAN_POINT('Ctrl Pts',(36.2035655956772,-91.3919434335384,119.951778901782));
#39916=CARTESIAN_POINT('Ctrl Pts',(33.6921155484724,-89.8934658111114,119.818010909183));
#39917=CARTESIAN_POINT('Ctrl Pts',(33.2871808925518,-88.319700945156,119.736892424315));
#39918=CARTESIAN_POINT('Ctrl Pts',(33.2861088517784,-87.7678945631458,119.708423447177));
#39919=CARTESIAN_POINT('Ctrl Pts',(33.2844849022013,-87.7664047084671,120.791576552823));
#39920=CARTESIAN_POINT('Ctrl Pts',(33.2821495713156,-87.410461265801,120.773188306702));
#39921=CARTESIAN_POINT('Ctrl Pts',(33.5032143465596,-86.0381806733766,120.70215055285));
#39922=CARTESIAN_POINT('Ctrl Pts',(35.5219283374979,-84.238982809065,120.578463291268));
#39923=CARTESIAN_POINT('Ctrl Pts',(38.8550457481358,-85.1415325934838,120.420514768075));
#39924=CARTESIAN_POINT('Ctrl Pts',(39.921396384874,-88.4259400024622,120.262566244883));
#39925=CARTESIAN_POINT('Ctrl Pts',(37.7541292274747,-91.1143092867255,120.10461772169));
#39926=CARTESIAN_POINT('Ctrl Pts',(34.3389589518385,-90.7712692257301,119.94762115767));
#39927=CARTESIAN_POINT('Ctrl Pts',(33.277983009097,-88.7621916588756,119.843274101381));
#39928=CARTESIAN_POINT('Ctrl Pts',(33.2764382705934,-87.7682219887363,119.791576552823));
#39929=CARTESIAN_POINT('Origin',(36.3549260746835,-87.7685555885722,124.208423447177));
#39930=CARTESIAN_POINT('',(33.2846473629325,-87.7715718261143,121.791576552823));
#39931=CARTESIAN_POINT('',(33.2781264274053,-87.766627982914,121.708423447177));
#39932=CARTESIAN_POINT('',(33.2814260746835,-87.768555588572,124.208423447177));
#39933=CARTESIAN_POINT('',(35.5611267921505,-90.7377785423179,122.));
#39934=CARTESIAN_POINT('Ctrl Pts',(35.5611267921506,-90.7377785423179,122.));
#39935=CARTESIAN_POINT('Ctrl Pts',(34.5788882023789,-90.4751844899402,121.947350492269));
#39936=CARTESIAN_POINT('Ctrl Pts',(33.479191301356,-89.437449369678,121.877876009877));
#39937=CARTESIAN_POINT('Ctrl Pts',(33.2823061516979,-88.0970477652926,121.808401527484));
#39938=CARTESIAN_POINT('Ctrl Pts',(33.2846473629325,-87.7715718261144,121.791576552823));
#39939=CARTESIAN_POINT('',(37.1506348820562,-90.7428550338497,122.));
#39940=CARTESIAN_POINT('Origin',(36.3549260746835,-87.7685555885722,122.));
#39941=CARTESIAN_POINT('Ctrl Pts',(37.1506395173468,-90.7428673568179,122.));
#39942=CARTESIAN_POINT('Ctrl Pts',(36.203673288632,-90.9937479020275,121.949053726697));
#39943=CARTESIAN_POINT('Ctrl Pts',(34.1431241348909,-90.5388461742994,121.851861542423));
#39944=CARTESIAN_POINT('Ctrl Pts',(33.2847898923083,-88.6569027408543,121.754669358149));
#39945=CARTESIAN_POINT('Ctrl Pts',(33.2781264274053,-87.766627982914,121.708423447177));
#39946=CARTESIAN_POINT('Origin',(-36.3549260746835,87.7685555885722,114.));
#39947=CARTESIAN_POINT('',(-38.8684362443696,87.7688130730525,107.387416697508));
#39948=CARTESIAN_POINT('',(-38.8705165012504,87.7649826536256,107.112583302492));
#39949=CARTESIAN_POINT('',(-38.8724260746835,87.7685555885722,114.));
#39950=CARTESIAN_POINT('',(-38.2683920713485,89.4045427919473,107.));
#39951=CARTESIAN_POINT('Ctrl Pts',(-38.8705165012504,87.7649826536256,107.112583302492));
#39952=CARTESIAN_POINT('Ctrl Pts',(-38.8653711927169,88.3576174120498,107.075055534995));
#39953=CARTESIAN_POINT('Ctrl Pts',(-38.6541479027676,88.9533591488767,107.037527767497));
#39954=CARTESIAN_POINT('Ctrl Pts',(-38.2683920713485,89.4045427919473,107.));
#39955=CARTESIAN_POINT('',(-38.8724260746835,87.7685555885722,107.));
#39956=CARTESIAN_POINT('Origin',(-36.3549260746835,87.7685555885722,107.));
#39957=CARTESIAN_POINT('',(-38.8724260746835,87.7685555885722,106.));
#39958=CARTESIAN_POINT('',(-38.8724260746835,87.7685555885722,114.));
#39959=CARTESIAN_POINT('Origin',(-36.3549260746835,87.7685555885722,106.));
#39960=CARTESIAN_POINT('',(-34.4378158812449,89.4070834968744,107.));
#39961=CARTESIAN_POINT('Origin',(-36.3549260746835,87.7685555885722,107.));
#39962=CARTESIAN_POINT('Ctrl Pts',(-34.4378070356398,89.4070896639597,107.));
#39963=CARTESIAN_POINT('Ctrl Pts',(-34.960627611636,90.0158048285236,107.050946273303));
#39964=CARTESIAN_POINT('Ctrl Pts',(-35.8003520741518,90.3559810018596,107.101892546605));
#39965=CARTESIAN_POINT('Ctrl Pts',(-36.5990228951286,90.2782181832502,107.152838819908));
#39966=CARTESIAN_POINT('Ctrl Pts',(-37.4243948573446,90.1978556001967,107.205488327639));
#39967=CARTESIAN_POINT('Ctrl Pts',(-38.2059222840348,89.6711418460179,107.25813783537));
#39968=CARTESIAN_POINT('Ctrl Pts',(-38.5898068873655,88.9363551308301,107.3107873431));
#39969=CARTESIAN_POINT('Ctrl Pts',(-38.7760500299138,88.579870432689,107.336330461236));
#39970=CARTESIAN_POINT('Ctrl Pts',(-38.86869823836,88.174410689784,107.361873579372));
#39971=CARTESIAN_POINT('Ctrl Pts',(-38.8684362443696,87.7688130730525,107.387416697508));
#39972=CARTESIAN_POINT('Origin',(-36.3549260746835,87.7685555885722,114.));
#39973=CARTESIAN_POINT('',(-38.8737307616524,87.7664601065225,108.387416697508));
#39974=CARTESIAN_POINT('',(-38.8763330919825,87.769221903177,108.112583302492));
#39975=CARTESIAN_POINT('',(-38.8724260746835,87.7685555885722,114.));
#39976=CARTESIAN_POINT('Ctrl Pts',(-38.8763330919825,87.769221903177,108.112583302492));
#39977=CARTESIAN_POINT('Ctrl Pts',(-38.8764609279018,87.8056790395625,108.110268755777));
#39978=CARTESIAN_POINT('Ctrl Pts',(-38.8757379769668,87.8421309392208,108.107954209062));
#39979=CARTESIAN_POINT('Ctrl Pts',(-38.8741483604852,87.8785449406493,108.105639662347));
#39980=CARTESIAN_POINT('Ctrl Pts',(-38.8379890016353,88.7068623115507,108.052990154616));
#39981=CARTESIAN_POINT('Ctrl Pts',(-38.3533855985534,89.5155697700692,108.000340646886));
#39982=CARTESIAN_POINT('Ctrl Pts',(-37.6400111963707,89.9381314370947,107.947691139155));
#39983=CARTESIAN_POINT('Ctrl Pts',(-36.9266367941881,90.3606931041203,107.895041631424));
#39984=CARTESIAN_POINT('Ctrl Pts',(-35.9844913929046,90.3971089796529,107.842392123693));
#39985=CARTESIAN_POINT('Ctrl Pts',(-35.240712177595,90.0307072878974,107.789742615962));
#39986=CARTESIAN_POINT('Ctrl Pts',(-34.4969329622854,89.6643055961419,107.737093108232));
#39987=CARTESIAN_POINT('Ctrl Pts',(-33.9515199329497,88.8950863370982,107.684443600501));
#39988=CARTESIAN_POINT('Ctrl Pts',(-33.8516662806639,88.0720989817,107.63179409277));
#39989=CARTESIAN_POINT('Ctrl Pts',(-33.7518126283782,87.2491116263017,107.579144585039));
#39990=CARTESIAN_POINT('Ctrl Pts',(-34.0975183531424,86.3723561745487,107.526495077308));
#39991=CARTESIAN_POINT('Ctrl Pts',(-34.7321883128989,85.8386042781123,107.473845569577));
#39992=CARTESIAN_POINT('Ctrl Pts',(-35.3668582726554,85.304852381676,107.421196061847));
#39993=CARTESIAN_POINT('Ctrl Pts',(-36.2904924674042,85.1141040405562,107.368546554116));
#39994=CARTESIAN_POINT('Ctrl Pts',(-37.0841095003195,85.3542579905456,107.315897046385));
#39995=CARTESIAN_POINT('Ctrl Pts',(-37.8777265332349,85.5944119405351,107.263247538654));
#39996=CARTESIAN_POINT('Ctrl Pts',(-38.5413264043166,86.2654681816338,107.210598030923));
#39997=CARTESIAN_POINT('Ctrl Pts',(-38.7742916354254,87.0597540929315,107.157948523192));
#39998=CARTESIAN_POINT('Ctrl Pts',(-38.8412027968037,87.2878851000279,107.142826782959));
#39999=CARTESIAN_POINT('Ctrl Pts',(-38.872589793222,87.5261816412588,107.127705042725));
#40000=CARTESIAN_POINT('Ctrl Pts',(-38.8705165012504,87.7649826536256,107.112583302492));
#40001=CARTESIAN_POINT('Ctrl Pts',(-38.8684362443696,87.7688130730525,107.387416697508));
#40002=CARTESIAN_POINT('Ctrl Pts',(-38.8681582160124,87.33839236406,107.414523087103));
#40003=CARTESIAN_POINT('Ctrl Pts',(-38.7632495349544,86.9078163887126,107.441629476698));
#40004=CARTESIAN_POINT('Ctrl Pts',(-38.5545285033691,86.5354489778792,107.468735866293));
#40005=CARTESIAN_POINT('Ctrl Pts',(-38.149123736071,85.812189216313,107.521385374024));
#40006=CARTESIAN_POINT('Ctrl Pts',(-37.3520724215038,85.3085293693773,107.574034881755));
#40007=CARTESIAN_POINT('Ctrl Pts',(-36.5248227318176,85.2526783946356,107.626684389485));
#40008=CARTESIAN_POINT('Ctrl Pts',(-35.6975730421315,85.1968274198939,107.679333897216));
#40009=CARTESIAN_POINT('Ctrl Pts',(-34.8401249773264,85.5887853173462,107.731983404947));
#40010=CARTESIAN_POINT('Ctrl Pts',(-34.341132647486,86.2509211028512,107.784632912678));
#40011=CARTESIAN_POINT('Ctrl Pts',(-33.8421403176455,86.9130568883562,107.837282420409));
#40012=CARTESIAN_POINT('Ctrl Pts',(-33.7016037227697,87.8453705619139,107.88993192814));
#40013=CARTESIAN_POINT('Ctrl Pts',(-33.983260674345,88.6251840983987,107.94258143587));
#40014=CARTESIAN_POINT('Ctrl Pts',(-34.2649176259204,89.4049976348835,107.995230943601));
#40015=CARTESIAN_POINT('Ctrl Pts',(-34.9687681239468,90.0323110342953,108.047880451332));
#40016=CARTESIAN_POINT('Ctrl Pts',(-35.7757187871427,90.2227548238847,108.100529959063));
#40017=CARTESIAN_POINT('Ctrl Pts',(-36.5826694503386,90.413198613474,108.153179466794));
#40018=CARTESIAN_POINT('Ctrl Pts',(-37.4927202787039,90.1667727932408,108.205828974524));
#40019=CARTESIAN_POINT('Ctrl Pts',(-38.0933201138925,89.59518418843,108.258478482255));
#40020=CARTESIAN_POINT('Ctrl Pts',(-38.5836081473929,89.1285789104982,108.30145788734));
#40021=CARTESIAN_POINT('Ctrl Pts',(-38.8676793774738,88.4452865593138,108.344437292424));
#40022=CARTESIAN_POINT('Ctrl Pts',(-38.8737307616524,87.7664601065225,108.387416697508));
#40023=CARTESIAN_POINT('Origin',(-36.3549260746835,87.7685555885722,114.));
#40024=CARTESIAN_POINT('',(-38.8745809434987,87.7704133464264,109.387416697508));
#40025=CARTESIAN_POINT('',(-38.869486864403,87.7700835308745,109.112583302492));
#40026=CARTESIAN_POINT('',(-38.8724260746835,87.7685555885722,114.));
#40027=CARTESIAN_POINT('Ctrl Pts',(-38.869486864403,87.7700835308745,109.112583302492));
#40028=CARTESIAN_POINT('Ctrl Pts',(-38.8712431197542,88.0833748523089,109.092832468829));
#40029=CARTESIAN_POINT('Ctrl Pts',(-38.8169459265052,88.3960793540123,109.073081635165));
#40030=CARTESIAN_POINT('Ctrl Pts',(-38.7038063526327,88.6858055394416,109.053330801502));
#40031=CARTESIAN_POINT('Ctrl Pts',(-38.4022118492914,89.4581243842876,109.000681293771));
#40032=CARTESIAN_POINT('Ctrl Pts',(-37.6824905487707,90.067162109531,108.94803178604));
#40033=CARTESIAN_POINT('Ctrl Pts',(-36.8709169658262,90.2368217728017,108.89538227831));
#40034=CARTESIAN_POINT('Ctrl Pts',(-36.0593433828818,90.4064814360724,108.842732770579));
#40035=CARTESIAN_POINT('Ctrl Pts',(-35.1559175175137,90.1367630373703,108.790083262848));
#40036=CARTESIAN_POINT('Ctrl Pts',(-34.570194142762,89.5499371541887,108.737433755117));
#40037=CARTESIAN_POINT('Ctrl Pts',(-33.9844707680103,88.9631112710072,108.684784247386));
#40038=CARTESIAN_POINT('Ctrl Pts',(-33.716449883875,88.0591779033461,108.632134739656));
#40039=CARTESIAN_POINT('Ctrl Pts',(-33.8876338696815,87.2479259334627,108.579485231925));
#40040=CARTESIAN_POINT('Ctrl Pts',(-34.058817855488,86.4366739635793,108.526835724194));
#40041=CARTESIAN_POINT('Ctrl Pts',(-34.6692067112364,85.7181033914734,108.474186216463));
#40042=CARTESIAN_POINT('Ctrl Pts',(-35.4420916027083,85.4179581360558,108.421536708732));
#40043=CARTESIAN_POINT('Ctrl Pts',(-36.2149764941802,85.1178128806382,108.368887201001));
#40044=CARTESIAN_POINT('Ctrl Pts',(-37.1503574213755,85.2360929419088,108.316237693271));
#40045=CARTESIAN_POINT('Ctrl Pts',(-37.8241902276642,85.7191966141862,108.26358818554));
#40046=CARTESIAN_POINT('Ctrl Pts',(-38.468400392158,86.1810623667598,108.213253224524));
#40047=CARTESIAN_POINT('Ctrl Pts',(-38.8735530158786,86.9763804682205,108.162918263508));
#40048=CARTESIAN_POINT('Ctrl Pts',(-38.8763330919825,87.769221903177,108.112583302492));
#40049=CARTESIAN_POINT('Ctrl Pts',(-38.8737307616524,87.7664601065225,108.387416697508));
#40050=CARTESIAN_POINT('Ctrl Pts',(-38.8750922859929,87.6137283163819,108.397086800155));
#40051=CARTESIAN_POINT('Ctrl Pts',(-38.8623798226398,87.4612226000268,108.406756902801));
#40052=CARTESIAN_POINT('Ctrl Pts',(-38.8347755569173,87.3114618221123,108.416427005448));
#40053=CARTESIAN_POINT('Ctrl Pts',(-38.6844823227415,86.4960794499939,108.469076513179));
#40054=CARTESIAN_POINT('Ctrl Pts',(-38.0927470123779,85.7620660951455,108.521726020909));
#40055=CARTESIAN_POINT('Ctrl Pts',(-37.3278253781081,85.4421739957963,108.57437552864));
#40056=CARTESIAN_POINT('Ctrl Pts',(-36.5629037438382,85.1222818964472,108.627025036371));
#40057=CARTESIAN_POINT('Ctrl Pts',(-35.6247957856621,85.2165110525973,108.679674544102));
#40058=CARTESIAN_POINT('Ctrl Pts',(-34.9387777281827,85.6821448649725,108.732324051833));
#40059=CARTESIAN_POINT('Ctrl Pts',(-34.2527596707034,86.1477786773477,108.784973559563));
#40060=CARTESIAN_POINT('Ctrl Pts',(-33.8188315139207,86.984817145948,108.837623067294));
#40061=CARTESIAN_POINT('Ctrl Pts',(-33.8337083550104,87.8138012422328,108.890272575025));
#40062=CARTESIAN_POINT('Ctrl Pts',(-33.8485851961001,88.6427853385176,108.942922082756));
#40063=CARTESIAN_POINT('Ctrl Pts',(-34.3122670350621,89.4637150624868,108.995571590487));
#40064=CARTESIAN_POINT('Ctrl Pts',(-35.0145505833724,89.9044345861986,109.048221098218));
#40065=CARTESIAN_POINT('Ctrl Pts',(-35.7168341316828,90.3451541099105,109.100870605948));
#40066=CARTESIAN_POINT('Ctrl Pts',(-36.6577193893416,90.4056634333649,109.153520113679));
#40067=CARTESIAN_POINT('Ctrl Pts',(-37.4106704191868,90.0585314880353,109.20616962141));
#40068=CARTESIAN_POINT('Ctrl Pts',(-38.1636214490319,89.7113995427057,109.258819129141));
#40069=CARTESIAN_POINT('Ctrl Pts',(-38.7286382510635,88.956626328592,109.311468636872));
#40070=CARTESIAN_POINT('Ctrl Pts',(-38.849579008108,88.1363768468704,109.364118144603));
#40071=CARTESIAN_POINT('Ctrl Pts',(-38.867418647058,88.0153840983512,109.371884328904));
#40072=CARTESIAN_POINT('Ctrl Pts',(-38.875595906259,87.8929666916698,109.379650513206));
#40073=CARTESIAN_POINT('Ctrl Pts',(-38.8745809434987,87.7704133464264,109.387416697508));
#40074=CARTESIAN_POINT('Origin',(-36.3549260746835,87.7685555885722,114.));
#40075=CARTESIAN_POINT('',(-38.8685100522263,87.768840975972,110.387416697508));
#40076=CARTESIAN_POINT('',(-38.8710621976983,87.7664319436008,110.112583302492));
#40077=CARTESIAN_POINT('',(-38.8724260746835,87.7685555885722,114.));
#40078=CARTESIAN_POINT('Ctrl Pts',(-38.8710621976983,87.7664319436008,110.112583302492));
#40079=CARTESIAN_POINT('Ctrl Pts',(-38.8662627330518,88.3553690084551,110.07539618188));
#40080=CARTESIAN_POINT('Ctrl Pts',(-38.6597042316269,88.9473396517482,110.038209061269));
#40081=CARTESIAN_POINT('Ctrl Pts',(-38.2820086943977,89.3948822716282,110.001021940657));
#40082=CARTESIAN_POINT('Ctrl Pts',(-37.7472675318623,90.0285129006648,109.948372432926));
#40083=CARTESIAN_POINT('Ctrl Pts',(-36.8694841837922,90.3726392469423,109.895722925195));
#40084=CARTESIAN_POINT('Ctrl Pts',(-36.046588380208,90.2712568783045,109.843073417465));
#40085=CARTESIAN_POINT('Ctrl Pts',(-35.2236925766238,90.1698745096667,109.790423909734));
#40086=CARTESIAN_POINT('Ctrl Pts',(-34.4556843175256,89.6229834261135,109.737774402003));
#40087=CARTESIAN_POINT('Ctrl Pts',(-34.0907284734417,88.8785083553923,109.685124894272));
#40088=CARTESIAN_POINT('Ctrl Pts',(-33.7257726293578,88.134033284671,109.632475386541));
#40089=CARTESIAN_POINT('Ctrl Pts',(-33.7638692002882,87.1919742267815,109.57982587881));
#40090=CARTESIAN_POINT('Ctrl Pts',(-34.1877476743859,86.4793993885376,109.52717637108));
#40091=CARTESIAN_POINT('Ctrl Pts',(-34.6116261484836,85.7668245502937,109.474526863349));
#40092=CARTESIAN_POINT('Ctrl Pts',(-35.4212865257487,85.2837339316954,109.421877355618));
#40093=CARTESIAN_POINT('Ctrl Pts',(-36.2496816085953,85.2491291978299,109.369227847887));
#40094=CARTESIAN_POINT('Ctrl Pts',(-37.0780766914418,85.2145244639644,109.316578340156));
#40095=CARTESIAN_POINT('Ctrl Pts',(-37.9252064798698,85.6284056148317,109.263928832425));
#40096=CARTESIAN_POINT('Ctrl Pts',(-38.4070375210029,86.3031461724895,109.211279324695));
#40097=CARTESIAN_POINT('Ctrl Pts',(-38.7081154049386,86.7247658730955,109.178380650627));
#40098=CARTESIAN_POINT('Ctrl Pts',(-38.8665614956128,87.248238769901,109.14548197656));
#40099=CARTESIAN_POINT('Ctrl Pts',(-38.869486864403,87.7700835308745,109.112583302492));
#40100=CARTESIAN_POINT('Ctrl Pts',(-38.8745809434987,87.7704133464264,109.387416697508));
#40101=CARTESIAN_POINT('Ctrl Pts',(-38.8687151411856,87.062137413473,109.432300020937));
#40102=CARTESIAN_POINT('Ctrl Pts',(-38.5558233551588,86.3493210472154,109.477183344366));
#40103=CARTESIAN_POINT('Ctrl Pts',(-38.0266616336717,85.8807298777288,109.522066667795));
#40104=CARTESIAN_POINT('Ctrl Pts',(-37.4059387901335,85.3310581396386,109.574716175526));
#40105=CARTESIAN_POINT('Ctrl Pts',(-36.4876283909998,85.1174404127878,109.627365683257));
#40106=CARTESIAN_POINT('Ctrl Pts',(-35.6880324811944,85.33671705519,109.680015190988));
#40107=CARTESIAN_POINT('Ctrl Pts',(-34.888436571389,85.5559936975923,109.732664698718));
#40108=CARTESIAN_POINT('Ctrl Pts',(-34.2075551509121,86.2081647092476,109.785314206449));
#40109=CARTESIAN_POINT('Ctrl Pts',(-33.9540554625385,86.9975782746064,109.83796371418));
#40110=CARTESIAN_POINT('Ctrl Pts',(-33.7005557741649,87.7869918399651,109.890613221911));
#40111=CARTESIAN_POINT('Ctrl Pts',(-33.8744378178946,88.7136479590273,109.943262729642));
#40112=CARTESIAN_POINT('Ctrl Pts',(-34.396874811042,89.3574611740643,109.995912237372));
#40113=CARTESIAN_POINT('Ctrl Pts',(-34.9193118041894,90.0012743891014,110.048561745103));
#40114=CARTESIAN_POINT('Ctrl Pts',(-35.7903037467545,90.3622447001133,110.101211252834));
#40115=CARTESIAN_POINT('Ctrl Pts',(-36.6149996877306,90.2767317046619,110.153860760565));
#40116=CARTESIAN_POINT('Ctrl Pts',(-37.4396956287066,90.1912187092105,110.206510268296));
#40117=CARTESIAN_POINT('Ctrl Pts',(-38.2180955680935,89.6592224072959,110.259159776027));
#40118=CARTESIAN_POINT('Ctrl Pts',(-38.5973237297961,88.9219152329815,110.311809283757));
#40119=CARTESIAN_POINT('Ctrl Pts',(-38.7788541420356,88.5689781654928,110.337011755008));
#40120=CARTESIAN_POINT('Ctrl Pts',(-38.8689190244798,88.1689965202894,110.362214226258));
#40121=CARTESIAN_POINT('Ctrl Pts',(-38.8685100522263,87.768840975972,110.387416697508));
#40122=CARTESIAN_POINT('Origin',(-36.3549260746835,87.7685555885722,114.));
#40123=CARTESIAN_POINT('',(-38.8735727384972,87.7664293773215,111.387416697508));
#40124=CARTESIAN_POINT('',(-38.8763918921078,87.7691165130487,111.112583302492));
#40125=CARTESIAN_POINT('',(-38.8724260746835,87.7685555885722,114.));
#40126=CARTESIAN_POINT('Ctrl Pts',(-38.8763918921078,87.7691165130487,111.112583302492));
#40127=CARTESIAN_POINT('Ctrl Pts',(-38.876486615945,87.8002064621293,111.110609402663));
#40128=CARTESIAN_POINT('Ctrl Pts',(-38.8759608143423,87.8312931336973,111.108635502833));
#40129=CARTESIAN_POINT('Ctrl Pts',(-38.8748045079704,87.8623563351577,111.106661603004));
#40130=CARTESIAN_POINT('Ctrl Pts',(-38.8439625369826,88.69090003387,111.054012095273));
#40131=CARTESIAN_POINT('Ctrl Pts',(-38.3645541170671,89.5027461541754,111.001362587543));
#40132=CARTESIAN_POINT('Ctrl Pts',(-37.6539117651349,89.9298566029362,110.948713079812));
#40133=CARTESIAN_POINT('Ctrl Pts',(-36.9432694132028,90.356967051697,110.896063572081));
#40134=CARTESIAN_POINT('Ctrl Pts',(-36.0013931292541,90.3993418289132,110.84341406435));
#40135=CARTESIAN_POINT('Ctrl Pts',(-35.2552682036472,90.0377709739024,110.790764556619));
#40136=CARTESIAN_POINT('Ctrl Pts',(-34.5091432780402,89.6762001188916,110.738115048888));
#40137=CARTESIAN_POINT('Ctrl Pts',(-33.9587697107751,88.9106836316539,110.685465541158));
#40138=CARTESIAN_POINT('Ctrl Pts',(-33.8536509892128,88.0882567702357,110.632816033427));
#40139=CARTESIAN_POINT('Ctrl Pts',(-33.7485322676505,87.2658299088175,110.580166525696));
#40140=CARTESIAN_POINT('Ctrl Pts',(-34.088668391791,86.3864926732189,110.527517017965));
#40141=CARTESIAN_POINT('Ctrl Pts',(-34.7198638219995,85.8488792280571,110.474867510234));
#40142=CARTESIAN_POINT('Ctrl Pts',(-35.351059252208,85.3112657828952,110.422218002503));
#40143=CARTESIAN_POINT('Ctrl Pts',(-36.2733139884845,85.1153761281701,110.369568494773));
#40144=CARTESIAN_POINT('Ctrl Pts',(-37.0685378709851,85.3500138584002,110.316918987042));
#40145=CARTESIAN_POINT('Ctrl Pts',(-37.8637617534856,85.5846515886302,110.264269479311));
#40146=CARTESIAN_POINT('Ctrl Pts',(-38.5319547822102,86.2498167038154,110.21161997158));
#40147=CARTESIAN_POINT('Ctrl Pts',(-38.7702018080721,87.0439667173058,110.158970463849));
#40148=CARTESIAN_POINT('Ctrl Pts',(-38.8401714602612,87.277196912012,110.14350807673));
#40149=CARTESIAN_POINT('Ctrl Pts',(-38.8730578128227,87.5215521912624,110.128045689611));
#40150=CARTESIAN_POINT('Ctrl Pts',(-38.8710621976983,87.7664319436008,110.112583302492));
#40151=CARTESIAN_POINT('Ctrl Pts',(-38.8685100522263,87.768840975972,110.387416697508));
#40152=CARTESIAN_POINT('Ctrl Pts',(-38.868064656366,87.3330470526798,110.414863733989));
#40153=CARTESIAN_POINT('Ctrl Pts',(-38.760312333685,86.8970468755525,110.442310770469));
#40154=CARTESIAN_POINT('Ctrl Pts',(-38.5465340171477,86.5213826498296,110.46975780695));
#40155=CARTESIAN_POINT('Ctrl Pts',(-38.1364597587785,85.800775287706,110.522407314681));
#40156=CARTESIAN_POINT('Ctrl Pts',(-37.336254858022,85.3021786101729,110.575056822411));
#40157=CARTESIAN_POINT('Ctrl Pts',(-36.5086800379385,85.2516238390558,110.627706330142));
#40158=CARTESIAN_POINT('Ctrl Pts',(-35.6811052178551,85.2010690679386,110.680355837873));
#40159=CARTESIAN_POINT('Ctrl Pts',(-34.8261604784448,85.5985562032374,110.733005345604));
#40160=CARTESIAN_POINT('Ctrl Pts',(-34.3314220163987,86.2638904966127,110.785654853335));
#40161=CARTESIAN_POINT('Ctrl Pts',(-33.8366835543527,86.9292247899879,110.838304361066));
#40162=CARTESIAN_POINT('Ctrl Pts',(-33.702151369671,87.8624062414395,110.890953868796));
#40163=CARTESIAN_POINT('Ctrl Pts',(-33.9888135824423,88.6403912306986,110.943603376527));
#40164=CARTESIAN_POINT('Ctrl Pts',(-34.2754757952136,89.4183762199577,110.996252884258));
#40165=CARTESIAN_POINT('Ctrl Pts',(-34.9833324054377,90.0411647470242,111.048902391989));
#40166=CARTESIAN_POINT('Ctrl Pts',(-35.7914873831277,90.2264251037659,111.10155189972));
#40167=CARTESIAN_POINT('Ctrl Pts',(-36.5996423608176,90.4116854605075,111.154201407451));
#40168=CARTESIAN_POINT('Ctrl Pts',(-37.5080957059732,90.1594176469243,111.206850915181));
#40169=CARTESIAN_POINT('Ctrl Pts',(-38.1050139092408,89.5839834401221,111.259500422912));
#40170=CARTESIAN_POINT('Ctrl Pts',(-38.5884344012918,89.1179619888201,111.302139181111));
#40171=CARTESIAN_POINT('Ctrl Pts',(-38.867527069726,88.4399840776712,111.344777939309));
#40172=CARTESIAN_POINT('Ctrl Pts',(-38.8735727384972,87.7664293773215,111.387416697508));
#40173=CARTESIAN_POINT('Origin',(-36.3549260746835,87.7685555885722,114.));
#40174=CARTESIAN_POINT('',(-38.8747249261259,87.7703594856308,112.387416697508));
#40175=CARTESIAN_POINT('',(-38.8695897820805,87.7701463237952,112.112583302492));
#40176=CARTESIAN_POINT('',(-38.8724260746835,87.7685555885722,114.));
#40177=CARTESIAN_POINT('Ctrl Pts',(-38.8695897820805,87.7701463237952,112.112583302492));
#40178=CARTESIAN_POINT('Ctrl Pts',(-38.8713915348065,88.0780025509154,112.093173115714));
#40179=CARTESIAN_POINT('Ctrl Pts',(-38.8190053186101,88.3852669963532,112.073762928937));
#40180=CARTESIAN_POINT('Ctrl Pts',(-38.7096476156592,88.6707043363187,112.054352742159));
#40181=CARTESIAN_POINT('Ctrl Pts',(-38.4130183615007,89.4449439461339,112.001703234428));
#40182=CARTESIAN_POINT('Ctrl Pts',(-37.6972224261715,90.05859102306,111.949053726697));
#40183=CARTESIAN_POINT('Ctrl Pts',(-36.8867550119788,90.2334579963873,111.896404218967));
#40184=CARTESIAN_POINT('Ctrl Pts',(-36.076287597786,90.4083249697147,111.843754711236));
#40185=CARTESIAN_POINT('Ctrl Pts',(-35.1711487047297,90.1444118394433,111.791105203505));
#40186=CARTESIAN_POINT('Ctrl Pts',(-34.5816692856989,89.5613596099067,111.738455695774));
#40187=CARTESIAN_POINT('Ctrl Pts',(-33.9921898666682,88.9783073803701,111.685806188043));
#40188=CARTESIAN_POINT('Ctrl Pts',(-33.7183699216629,88.0761160515683,111.633156680312));
#40189=CARTESIAN_POINT('Ctrl Pts',(-33.8843415588236,87.2637803429541,111.580507172582));
#40190=CARTESIAN_POINT('Ctrl Pts',(-34.0503131959844,86.4514446343399,111.527857664851));
#40191=CARTESIAN_POINT('Ctrl Pts',(-34.6560764153111,85.7289645459133,111.47520815712));
#40192=CARTESIAN_POINT('Ctrl Pts',(-35.4270176730479,85.4238654391534,111.422558649389));
#40193=CARTESIAN_POINT('Ctrl Pts',(-36.1979589307848,85.1187663323936,111.369909141658));
#40194=CARTESIAN_POINT('Ctrl Pts',(-37.1340782269316,85.2310482073005,111.317259633927));
#40195=CARTESIAN_POINT('Ctrl Pts',(-37.811000113975,85.7098097833135,111.264610126197));
#40196=CARTESIAN_POINT('Ctrl Pts',(-38.462543302245,86.1706219532658,111.213934518295));
#40197=CARTESIAN_POINT('Ctrl Pts',(-38.8739600625095,86.9709493285109,111.163258910394));
#40198=CARTESIAN_POINT('Ctrl Pts',(-38.8763918921078,87.7691165130487,111.112583302492));
#40199=CARTESIAN_POINT('Ctrl Pts',(-38.8735727384972,87.7664293773215,111.387416697508));
#40200=CARTESIAN_POINT('Ctrl Pts',(-38.8749921437139,87.6082918591033,111.39742744704));
#40201=CARTESIAN_POINT('Ctrl Pts',(-38.8613606824198,87.4503981566214,111.407438196572));
#40202=CARTESIAN_POINT('Ctrl Pts',(-38.8317890222728,87.2955485572239,111.417448946105));
#40203=CARTESIAN_POINT('Ctrl Pts',(-38.6762628706579,86.4811484811489,111.470098453835));
#40204=CARTESIAN_POINT('Ctrl Pts',(-38.0798275060489,85.75094892902,111.522747961566));
#40205=CARTESIAN_POINT('Ctrl Pts',(-37.3128678311087,85.4359747637889,111.575397469297));
#40206=CARTESIAN_POINT('Ctrl Pts',(-36.5459081561684,85.1210005985578,111.628046977028));
#40207=CARTESIAN_POINT('Ctrl Pts',(-35.6084241708969,85.2212518202244,111.680696484759));
#40208=CARTESIAN_POINT('Ctrl Pts',(-34.9254099838746,85.6912810619469,111.73334599249));
#40209=CARTESIAN_POINT('Ctrl Pts',(-34.2423957968523,86.1613103036694,111.78599550022));
#40210=CARTESIAN_POINT('Ctrl Pts',(-33.8138514080791,87.0011175654478,111.838645007951));
#40211=CARTESIAN_POINT('Ctrl Pts',(-33.8340508994108,87.8299889959469,111.891294515682));
#40212=CARTESIAN_POINT('Ctrl Pts',(-33.8542503907425,88.6588604264459,111.943944023413));
#40213=CARTESIAN_POINT('Ctrl Pts',(-34.3231937621791,89.4767960256657,111.996593531144));
#40214=CARTESIAN_POINT('Ctrl Pts',(-35.0282926674139,89.912997127893,112.049243038875));
#40215=CARTESIAN_POINT('Ctrl Pts',(-35.7333915726487,90.3491982301204,112.101892546605));
#40216=CARTESIAN_POINT('Ctrl Pts',(-36.6746460116818,90.4036648353553,112.154542054336));
#40217=CARTESIAN_POINT('Ctrl Pts',(-37.4253525980572,90.0517053363782,112.207191562067));
#40218=CARTESIAN_POINT('Ctrl Pts',(-38.1760591844327,89.699745837401,112.259841069798));
#40219=CARTESIAN_POINT('Ctrl Pts',(-38.7362179181505,88.9413602342117,112.312490577529));
#40220=CARTESIAN_POINT('Ctrl Pts',(-38.8518893555087,88.1203511073884,112.365140085259));
#40221=CARTESIAN_POINT('Ctrl Pts',(-38.8682033273407,88.0045583060305,112.372565622676));
#40222=CARTESIAN_POINT('Ctrl Pts',(-38.875675787902,87.8875198299491,112.379991160092));
#40223=CARTESIAN_POINT('Ctrl Pts',(-38.8747249261259,87.7703594856308,112.387416697508));
#40224=CARTESIAN_POINT('Origin',(-36.3549260746835,87.7685555885722,114.));
#40225=CARTESIAN_POINT('',(-38.8685312481293,87.7689269147315,113.387416697508));
#40226=CARTESIAN_POINT('',(-38.8709179607018,87.766461971973,113.112583302492));
#40227=CARTESIAN_POINT('',(-38.8724260746835,87.7685555885722,114.));
#40228=CARTESIAN_POINT('Ctrl Pts',(-38.8709179607018,87.766461971973,113.112583302492));
#40229=CARTESIAN_POINT('Ctrl Pts',(-38.8662498737967,88.3500889811953,113.075736828766));
#40230=CARTESIAN_POINT('Ctrl Pts',(-38.6637922635731,88.9366381474527,113.03889035504));
#40231=CARTESIAN_POINT('Ctrl Pts',(-38.2924116092779,89.3824749489596,113.002043881314));
#40232=CARTESIAN_POINT('Ctrl Pts',(-37.761750011244,90.0195260899217,112.949394373583));
#40233=CARTESIAN_POINT('Ctrl Pts',(-36.8861943918917,90.3692815952011,112.896744865852));
#40234=CARTESIAN_POINT('Ctrl Pts',(-36.0626645768443,90.2731851251457,112.844095358121));
#40235=CARTESIAN_POINT('Ctrl Pts',(-35.2391347617969,90.1770886550904,112.791445850391));
#40236=CARTESIAN_POINT('Ctrl Pts',(-34.4676307510543,89.6351402097004,112.73879634266));
#40237=CARTESIAN_POINT('Ctrl Pts',(-34.0979021557698,88.8930238753848,112.686146834929));
#40238=CARTESIAN_POINT('Ctrl Pts',(-33.7281735604853,88.1509075410691,112.633497327198));
#40239=CARTESIAN_POINT('Ctrl Pts',(-33.7602203806589,87.2086233178279,112.580847819467));
#40240=CARTESIAN_POINT('Ctrl Pts',(-34.1795146776949,86.4933414291279,112.528198311736));
#40241=CARTESIAN_POINT('Ctrl Pts',(-34.5988089747308,85.7780595404278,112.475548804006));
#40242=CARTESIAN_POINT('Ctrl Pts',(-35.4053507486292,85.289779986269,112.422899296275));
#40243=CARTESIAN_POINT('Ctrl Pts',(-36.2335065511227,85.2498568773537,112.370249788544));
#40244=CARTESIAN_POINT('Ctrl Pts',(-37.0616623536162,85.2099337684384,112.317600280813));
#40245=CARTESIAN_POINT('Ctrl Pts',(-37.9114321847049,85.6183671047667,112.264950773082));
#40246=CARTESIAN_POINT('Ctrl Pts',(-38.3975858137553,86.289999844283,112.212301265352));
#40247=CARTESIAN_POINT('Ctrl Pts',(-38.70451017459,86.7140231097153,112.179061944398));
#40248=CARTESIAN_POINT('Ctrl Pts',(-38.8665043384509,87.2429524303057,112.145822623445));
#40249=CARTESIAN_POINT('Ctrl Pts',(-38.8695897820805,87.7701463237952,112.112583302492));
#40250=CARTESIAN_POINT('Ctrl Pts',(-38.8747249261259,87.7703594856308,112.387416697508));
#40251=CARTESIAN_POINT('Ctrl Pts',(-38.8689338645059,87.0568143727958,112.432640667823));
#40252=CARTESIAN_POINT('Ctrl Pts',(-38.5507039652186,86.3387489093515,112.477864638137));
#40253=CARTESIAN_POINT('Ctrl Pts',(-38.0145054479413,85.8700345808651,112.523088608452));
#40254=CARTESIAN_POINT('Ctrl Pts',(-37.3902659620173,85.3243598316224,112.575738116183));
#40255=CARTESIAN_POINT('Ctrl Pts',(-36.4706028491709,85.1166429835945,112.628387623914));
#40256=CARTESIAN_POINT('Ctrl Pts',(-35.6724313964662,85.3410493111235,112.681037131644));
#40257=CARTESIAN_POINT('Ctrl Pts',(-34.8742599437615,85.5654556386525,112.733686639375));
#40258=CARTESIAN_POINT('Ctrl Pts',(-34.1975801511987,86.2219851417385,112.786336147106));
#40259=CARTESIAN_POINT('Ctrl Pts',(-33.9491545125933,87.0130101538787,112.838985654837));
#40260=CARTESIAN_POINT('Ctrl Pts',(-33.700728873988,87.8040351660187,112.891635162568));
#40261=CARTESIAN_POINT('Ctrl Pts',(-33.88055738934,88.7295556872129,112.944284670298));
#40262=CARTESIAN_POINT('Ctrl Pts',(-34.4071175358331,89.3700010633948,112.996934178029));
#40263=CARTESIAN_POINT('Ctrl Pts',(-34.9336776823263,90.0104464395768,113.04958368576));
#40264=CARTESIAN_POINT('Ctrl Pts',(-35.8069694599605,90.3658166707465,113.102233193491));
#40265=CARTESIAN_POINT('Ctrl Pts',(-36.6310993213297,90.2750100666518,113.154882701222));
#40266=CARTESIAN_POINT('Ctrl Pts',(-37.455229182699,90.1842034625571,113.207532208953));
#40267=CARTESIAN_POINT('Ctrl Pts',(-38.2301971278032,89.6472200231979,113.260181716683));
#40268=CARTESIAN_POINT('Ctrl Pts',(-38.6046832235218,88.9074930250012,113.312831224414));
#40269=CARTESIAN_POINT('Ctrl Pts',(-38.7815207276128,88.5581837246951,113.337693048779));
#40270=CARTESIAN_POINT('Ctrl Pts',(-38.8690564351314,88.1636654740321,113.362554873143));
#40271=CARTESIAN_POINT('Ctrl Pts',(-38.8685312481293,87.7689269147315,113.387416697508));
#40272=CARTESIAN_POINT('Origin',(-36.3549260746835,87.7685555885722,114.));
#40273=CARTESIAN_POINT('',(-38.8734136832049,87.7664022272136,114.387416697508));
#40274=CARTESIAN_POINT('',(-38.8764404125238,87.769021583458,114.112583302492));
#40275=CARTESIAN_POINT('',(-38.8724260746835,87.7685555885722,114.));
#40276=CARTESIAN_POINT('Ctrl Pts',(-38.8764404125238,87.769021583458,114.112583302492));
#40277=CARTESIAN_POINT('Ctrl Pts',(-38.8765065000921,87.7947448392147,114.110950049548));
#40278=CARTESIAN_POINT('Ctrl Pts',(-38.8761465565816,87.8204662008222,114.109316796605));
#40279=CARTESIAN_POINT('Ctrl Pts',(-38.8753548555647,87.8461742661021,114.107683543661));
#40280=CARTESIAN_POINT('Ctrl Pts',(-38.8498335981424,88.6748989207666,114.05503403593));
#40281=CARTESIAN_POINT('Ctrl Pts',(-38.3756479237925,89.489806585655,114.002384528199));
#40282=CARTESIAN_POINT('Ctrl Pts',(-37.6677626971288,89.9214712630384,113.949735020469));
#40283=CARTESIAN_POINT('Ctrl Pts',(-36.9598774704652,90.3531359404218,113.897085512738));
#40284=CARTESIAN_POINT('Ctrl Pts',(-36.0182926914878,90.4015576303001,113.844436005007));
#40285=CARTESIAN_POINT('Ctrl Pts',(-35.2698615012428,90.0447850959066,113.791786497276));
#40286=CARTESIAN_POINT('Ctrl Pts',(-34.5214303109978,89.6880125615131,113.739136989545));
#40287=CARTESIAN_POINT('Ctrl Pts',(-33.9661527094851,88.9260458028477,113.686487481814));
#40288=CARTESIAN_POINT('Ctrl Pts',(-33.8557553533482,88.1043108628658,113.633837974084));
#40289=CARTESIAN_POINT('Ctrl Pts',(-33.7453579972113,87.2825759228839,113.581188466353));
#40290=CARTESIAN_POINT('Ctrl Pts',(-34.0798408864501,86.4010728015853,113.528538958622));
#40291=CARTESIAN_POINT('Ctrl Pts',(-34.7075712896468,85.8594175341581,113.475889450891));
#40292=CARTESIAN_POINT('Ctrl Pts',(-35.3353016928435,85.3177622667309,113.42323994316));
#40293=CARTESIAN_POINT('Ctrl Pts',(-36.2562796099981,85.1159548531751,113.37059043543));
#40294=CARTESIAN_POINT('Ctrl Pts',(-37.0529937075072,85.3454816155785,113.317940927699));
#40295=CARTESIAN_POINT('Ctrl Pts',(-37.8497078050162,85.575008377982,113.265291419968));
#40296=CARTESIAN_POINT('Ctrl Pts',(-38.5221580828798,86.2358693163448,113.212641912237));
#40297=CARTESIAN_POINT('Ctrl Pts',(-38.7654994334537,87.0284731738487,113.159992404506));
#40298=CARTESIAN_POINT('Ctrl Pts',(-38.83853965365,87.2663775010168,113.144189370502));
#40299=CARTESIAN_POINT('Ctrl Pts',(-38.872920050146,87.5161509777269,113.128386336497));
#40300=CARTESIAN_POINT('Ctrl Pts',(-38.8709179607018,87.766461971973,113.112583302492));
#40301=CARTESIAN_POINT('Ctrl Pts',(-38.8685312481293,87.7689269147315,113.387416697508));
#40302=CARTESIAN_POINT('Ctrl Pts',(-38.8679442545962,87.3277336242702,113.415204380874));
#40303=CARTESIAN_POINT('Ctrl Pts',(-38.7573498896077,86.8862651200007,113.442992064241));
#40304=CARTESIAN_POINT('Ctrl Pts',(-38.538480742133,86.5073360489567,113.470779747607));
#40305=CARTESIAN_POINT('Ctrl Pts',(-38.1237879186926,85.7893766281432,113.523429255338));
#40306=CARTESIAN_POINT('Ctrl Pts',(-37.320398025479,85.2959283435506,113.576078763068));
#40307=CARTESIAN_POINT('Ctrl Pts',(-36.4925156535809,85.2506884712233,113.628728270799));
#40308=CARTESIAN_POINT('Ctrl Pts',(-35.6646332816829,85.205448598896,113.68137777853));
#40309=CARTESIAN_POINT('Ctrl Pts',(-34.8122584311004,85.608417138834,113.734027286261));
#40310=CARTESIAN_POINT('Ctrl Pts',(-34.3218022784405,86.2769144313234,113.786676793992));
#40311=CARTESIAN_POINT('Ctrl Pts',(-33.8313461257806,86.9454117238129,113.839326301722));
#40312=CARTESIAN_POINT('Ctrl Pts',(-33.7028086710432,87.8794377688538,113.891975809453));
#40313=CARTESIAN_POINT('Ctrl Pts',(-33.9944604146885,88.655566062486,113.944625317184));
#40314=CARTESIAN_POINT('Ctrl Pts',(-34.2861121583339,89.4316943561181,113.997274824915));
#40315=CARTESIAN_POINT('Ctrl Pts',(-34.997953100362,90.0499248983415,114.049924332646));
#40316=CARTESIAN_POINT('Ctrl Pts',(-35.8072809745362,90.229992274155,114.102573840377));
#40317=CARTESIAN_POINT('Ctrl Pts',(-36.6166088487104,90.4100596499686,114.155223348107));
#40318=CARTESIAN_POINT('Ctrl Pts',(-37.5234236550307,90.1519638593725,114.207872855838));
#40319=CARTESIAN_POINT('Ctrl Pts',(-38.1166346908146,89.572708704219,114.260522363569));
#40320=CARTESIAN_POINT('Ctrl Pts',(-38.5932147673457,89.1073406488029,114.302820474882));
#40321=CARTESIAN_POINT('Ctrl Pts',(-38.8673836169466,88.4346847125397,114.345118586195));
#40322=CARTESIAN_POINT('Ctrl Pts',(-38.8734136832049,87.7664022272136,114.387416697508));
#40323=CARTESIAN_POINT('Origin',(-36.3549260746835,87.7685555885722,114.));
#40324=CARTESIAN_POINT('',(-38.8748657309868,87.7703023244941,115.387416697508));
#40325=CARTESIAN_POINT('',(-38.8696970038573,87.7702068964603,115.112583302492));
#40326=CARTESIAN_POINT('',(-38.8724260746835,87.7685555885722,114.));
#40327=CARTESIAN_POINT('Ctrl Pts',(-38.8696970038573,87.7702068964603,115.112583302492));
#40328=CARTESIAN_POINT('Ctrl Pts',(-38.8715395686952,88.0726278474952,115.0935137626));
#40329=CARTESIAN_POINT('Ctrl Pts',(-38.8210274128864,88.3744540515915,115.074444222708));
#40330=CARTESIAN_POINT('Ctrl Pts',(-38.7153917691555,88.6555660754418,115.055374682816));
#40331=CARTESIAN_POINT('Ctrl Pts',(-38.4237400212503,89.4316943804101,115.002725175085));
#40332=CARTESIAN_POINT('Ctrl Pts',(-37.7118990688249,90.0499249316633,114.950075667354));
#40333=CARTESIAN_POINT('Ctrl Pts',(-36.9025711828297,90.2299923101069,114.897426159623));
#40334=CARTESIAN_POINT('Ctrl Pts',(-36.0932432968344,90.4100596885505,114.844776651893));
#40335=CARTESIAN_POINT('Ctrl Pts',(-35.1864284772691,90.1519638941845,114.792127144162));
#40336=CARTESIAN_POINT('Ctrl Pts',(-34.5932174328208,89.5727087305704,114.739477636431));
#40337=CARTESIAN_POINT('Ctrl Pts',(-34.0000063883724,88.9934535669563,114.6868281287));
#40338=CARTESIAN_POINT('Ctrl Pts',(-33.720399119041,88.093039034094,114.634178620969));
#40339=CARTESIAN_POINT('Ctrl Pts',(-33.8811513284425,87.2796543680216,114.581529113239));
#40340=CARTESIAN_POINT('Ctrl Pts',(-34.0419035378441,86.4662697019493,114.528879605508));
#40341=CARTESIAN_POINT('Ctrl Pts',(-34.6430152259786,85.7399149026668,114.476230097777));
#40342=CARTESIAN_POINT('Ctrl Pts',(-35.411981550023,85.4298718728877,114.423580590046));
#40343=CARTESIAN_POINT('Ctrl Pts',(-36.1809478740675,85.1198288431085,114.370931082315));
#40344=CARTESIAN_POINT('Ctrl Pts',(-37.117768834022,85.2260975828327,114.318281574584));
#40345=CARTESIAN_POINT('Ctrl Pts',(-37.7977508937519,85.700502774915,114.265632066854));
#40346=CARTESIAN_POINT('Ctrl Pts',(-38.4566390677353,86.1601913303212,114.214615812066));
#40347=CARTESIAN_POINT('Ctrl Pts',(-38.8743761026231,86.9655305046608,114.163599557279));
#40348=CARTESIAN_POINT('Ctrl Pts',(-38.8764404125238,87.769021583458,114.112583302492));
#40349=CARTESIAN_POINT('Ctrl Pts',(-38.8734136832049,87.7664022272136,114.387416697508));
#40350=CARTESIAN_POINT('Ctrl Pts',(-38.8748893899049,87.6028569361835,114.397768093926));
#40351=CARTESIAN_POINT('Ctrl Pts',(-38.8603062050893,87.4395735721051,114.408119490344));
#40352=CARTESIAN_POINT('Ctrl Pts',(-38.8287007847925,87.2796543751627,114.418470886762));
#40353=CARTESIAN_POINT('Ctrl Pts',(-38.667948577739,86.4662697209706,114.471120394492));
#40354=CARTESIAN_POINT('Ctrl Pts',(-38.0668368983844,85.7399149322973,114.523769902223));
#40355=CARTESIAN_POINT('Ctrl Pts',(-37.2978705855715,85.4298719070465,114.576419409954));
#40356=CARTESIAN_POINT('Ctrl Pts',(-36.5289042727585,85.1198288817958,114.629068917685));
#40357=CARTESIAN_POINT('Ctrl Pts',(-35.5920833264873,85.2260976199678,114.681718425416));
#40358=CARTESIAN_POINT('Ctrl Pts',(-34.9121012766892,85.7005028051209,114.734367933147));
#40359=CARTESIAN_POINT('Ctrl Pts',(-34.2321192268912,86.174907990274,114.787017440877));
#40360=CARTESIAN_POINT('Ctrl Pts',(-33.8089760735663,87.0174496224082,114.839666948608));
#40361=CARTESIAN_POINT('Ctrl Pts',(-33.8344973306158,87.8461742649683,114.892316456339));
#40362=CARTESIAN_POINT('Ctrl Pts',(-33.8600185876653,88.6748989075284,114.94496596407));
#40363=CARTESIAN_POINT('Ctrl Pts',(-34.3342042550892,89.4898065605143,114.997615471801));
#40364=CARTESIAN_POINT('Ctrl Pts',(-35.0420894714134,89.9214712315928,115.050264979531));
#40365=CARTESIAN_POINT('Ctrl Pts',(-35.7499746877377,90.3531359026713,115.102914487262));
#40366=CARTESIAN_POINT('Ctrl Pts',(-36.6915594529623,90.4015575918424,115.155563994993));
#40367=CARTESIAN_POINT('Ctrl Pts',(-37.4399906322757,90.04478506266,115.208213502724));
#40368=CARTESIAN_POINT('Ctrl Pts',(-38.1884218115891,89.6880125334775,115.260863010455));
#40369=CARTESIAN_POINT('Ctrl Pts',(-38.7436994049914,88.9260457859415,115.313512518185));
#40370=CARTESIAN_POINT('Ctrl Pts',(-38.8540967595159,88.1043108579619,115.366162025916));
#40371=CARTESIAN_POINT('Ctrl Pts',(-38.8689526091787,87.9937323879857,115.373246916447));
#40372=CARTESIAN_POINT('Ctrl Pts',(-38.8757524344211,87.8820716179226,115.380331806977));
#40373=CARTESIAN_POINT('Ctrl Pts',(-38.8748657309868,87.7703023244941,115.387416697508));
#40374=CARTESIAN_POINT('Origin',(-36.3549260746835,87.7685555885722,114.));
#40375=CARTESIAN_POINT('',(-38.8685579872896,87.7690123127748,116.387416697508));
#40376=CARTESIAN_POINT('',(-38.8707764324224,87.7664952479985,116.112583302492));
#40377=CARTESIAN_POINT('',(-38.8724260746835,87.7685555885722,114.));
#40378=CARTESIAN_POINT('Ctrl Pts',(-38.8707764324224,87.7664952479985,116.112583302492));
#40379=CARTESIAN_POINT('Ctrl Pts',(-38.8662438736391,88.3448089996547,116.076077475652));
#40380=CARTESIAN_POINT('Ctrl Pts',(-38.6678380330352,88.9259325787823,116.039571648811));
#40381=CARTESIAN_POINT('Ctrl Pts',(-38.3027346419836,89.3700010867857,116.003065821971));
#40382=CARTESIAN_POINT('Ctrl Pts',(-37.7761744877995,90.010446472322,115.95041631424));
#40383=CARTESIAN_POINT('Ctrl Pts',(-36.9028826974099,90.3658167086822,115.897766806509));
#40384=CARTESIAN_POINT('Ctrl Pts',(-36.0787528240034,90.2750101032611,115.845117298778));
#40385=CARTESIAN_POINT('Ctrl Pts',(-35.2546229505969,90.18420349784,115.792467791047));
#40386=CARTESIAN_POINT('Ctrl Pts',(-34.4796549941735,89.6472200506376,115.739818283317));
#40387=CARTESIAN_POINT('Ctrl Pts',(-34.1051688929851,88.9074930416363,115.687168775586));
#40388=CARTESIAN_POINT('Ctrl Pts',(-33.7306827917968,88.1677660326351,115.634519267855));
#40389=CARTESIAN_POINT('Ctrl Pts',(-33.7566785458437,87.2252954618351,115.581869760124));
#40390=CARTESIAN_POINT('Ctrl Pts',(-34.1713713753411,86.5073360305352,115.529220252393));
#40391=CARTESIAN_POINT('Ctrl Pts',(-34.5860642048385,85.7893765992352,115.476570744662));
#40392=CARTESIAN_POINT('Ctrl Pts',(-35.3894541097865,85.2959283074353,115.423921236932));
#40393=CARTESIAN_POINT('Ctrl Pts',(-36.2173364937766,85.2506884344473,115.371271729201));
#40394=CARTESIAN_POINT('Ctrl Pts',(-37.0452188777668,85.2054485614592,115.31862222147));
#40395=CARTESIAN_POINT('Ctrl Pts',(-37.897593740799,85.608417107283,115.265972713739));
#40396=CARTESIAN_POINT('Ctrl Pts',(-38.3880499006225,86.2769144095366,115.213323206008));
#40397=CARTESIAN_POINT('Ctrl Pts',(-38.7008638809052,86.7032834085547,115.17974323817));
#40398=CARTESIAN_POINT('Ctrl Pts',(-38.8664523913314,87.2376672616802,115.146163270331));
#40399=CARTESIAN_POINT('Ctrl Pts',(-38.8696970038573,87.7702068964603,115.112583302492));
#40400=CARTESIAN_POINT('Ctrl Pts',(-38.8748657309868,87.7703023244941,115.387416697508));
#40401=CARTESIAN_POINT('Ctrl Pts',(-38.8691631301662,87.0514873974544,115.432981314708));
#40402=CARTESIAN_POINT('Ctrl Pts',(-38.545539383395,86.3281838547981,115.478545931909));
#40403=CARTESIAN_POINT('Ctrl Pts',(-38.0022808356591,85.8594175620432,115.524110549109));
#40404=CARTESIAN_POINT('Ctrl Pts',(-37.3745504416311,85.3177623025274,115.57676005684));
#40405=CARTESIAN_POINT('Ctrl Pts',(-36.4535725379283,85.115954891919,115.62940956457));
#40406=CARTESIAN_POINT('Ctrl Pts',(-35.656858452056,85.34548165097,115.682059072301));
#40407=CARTESIAN_POINT('Ctrl Pts',(-34.8601443661838,85.5750084100209,115.734708580032));
#40408=CARTESIAN_POINT('Ctrl Pts',(-34.187694098142,86.2358693387312,115.787358087763));
#40409=CARTESIAN_POINT('Ctrl Pts',(-33.9443527511223,87.0284731846582,115.840007595494));
#40410=CARTESIAN_POINT('Ctrl Pts',(-33.7010114041026,87.8210770305853,115.892657103225));
#40411=CARTESIAN_POINT('Ctrl Pts',(-33.8867789781049,88.7454237937291,115.945306610955));
#40412=CARTESIAN_POINT('Ctrl Pts',(-34.417440568388,89.3824749253865,115.997956118686));
#40413=CARTESIAN_POINT('Ctrl Pts',(-34.9481021586711,90.0195260570439,116.050605626417));
#40414=CARTESIAN_POINT('Ctrl Pts',(-35.8236577652349,90.3692815572148,116.103255134148));
#40415=CARTESIAN_POINT('Ctrl Pts',(-36.6471875682538,90.2731850885631,116.155904641879));
#40416=CARTESIAN_POINT('Ctrl Pts',(-37.4707173712728,90.1770886199114,116.20855414961));
#40417=CARTESIAN_POINT('Ctrl Pts',(-38.2422213707468,89.6351401824371,116.26120365734));
#40418=CARTESIAN_POINT('Ctrl Pts',(-38.611949960631,88.8930238589608,116.313853165071));
#40419=CARTESIAN_POINT('Ctrl Pts',(-38.7841487287174,88.5473878433112,116.33837434255));
#40420=CARTESIAN_POINT('Ctrl Pts',(-38.8691954955822,88.1583319681357,116.362895520029));
#40421=CARTESIAN_POINT('Ctrl Pts',(-38.8685579872896,87.7690123127748,116.387416697508));
#40422=CARTESIAN_POINT('Origin',(-36.3549260746835,87.7685555885722,114.));
#40423=CARTESIAN_POINT('',(-38.8732537926193,87.7663787382843,117.387416697508));
#40424=CARTESIAN_POINT('',(-38.8764804707602,87.7689256098953,117.112583302492));
#40425=CARTESIAN_POINT('',(-38.8724260746835,87.7685555885722,114.));
#40426=CARTESIAN_POINT('Ctrl Pts',(-38.8764804707602,87.7689256098953,117.112583302492));
#40427=CARTESIAN_POINT('Ctrl Pts',(-38.8765226439062,87.789282907905,117.111290696434));
#40428=CARTESIAN_POINT('Ctrl Pts',(-38.876297207562,87.8096392482103,117.109998090376));
#40429=CARTESIAN_POINT('Ctrl Pts',(-38.8758012867762,87.8299889968442,117.108705484318));
#40430=CARTESIAN_POINT('Ctrl Pts',(-38.8556017951495,88.6588604394498,117.056055976587));
#40431=CARTESIAN_POINT('Ctrl Pts',(-38.3866584168635,89.4767960506164,117.003406468856));
#40432=CARTESIAN_POINT('Ctrl Pts',(-37.6815595013299,89.9129971592149,116.950756961126));
#40433=CARTESIAN_POINT('Ctrl Pts',(-36.9764605857964,90.3491982678134,116.898107453395));
#40434=CARTESIAN_POINT('Ctrl Pts',(-36.0352061330153,90.4036648738438,116.845457945664));
#40435=CARTESIAN_POINT('Ctrl Pts',(-35.2844995356751,90.0517053697259,116.792808437933));
#40436=CARTESIAN_POINT('Ctrl Pts',(-34.5337929383348,89.699745865608,116.740158930202));
#40437=CARTESIAN_POINT('Ctrl Pts',(-33.9736341964353,88.9413602513417,116.687509422471));
#40438=CARTESIAN_POINT('Ctrl Pts',(-33.8579627573876,88.1203511125267,116.634859914741));
#40439=CARTESIAN_POINT('Ctrl Pts',(-33.74229131834,87.2993419737117,116.58221040701));
#40440=CARTESIAN_POINT('Ctrl Pts',(-34.0711071821443,86.4157093103479,116.529560899279));
#40441=CARTESIAN_POINT('Ctrl Pts',(-34.6953466771859,85.8700345531351,116.476911391548));
#40442=CARTESIAN_POINT('Ctrl Pts',(-35.3195861722276,85.3243597959224,116.424261883817));
#40443=CARTESIAN_POINT('Ctrl Pts',(-36.2392492985068,85.1166429448606,116.371612376086));
#40444=CARTESIAN_POINT('Ctrl Pts',(-37.0374207628696,85.3410492756673,116.318962868356));
#40445=CARTESIAN_POINT('Ctrl Pts',(-37.8355922272323,85.5654556064741,116.266313360625));
#40446=CARTESIAN_POINT('Ctrl Pts',(-38.5122720296786,86.2219851191493,116.213663852894));
#40447=CARTESIAN_POINT('Ctrl Pts',(-38.7606976719125,87.0130101428432,116.161014345163));
#40448=CARTESIAN_POINT('Ctrl Pts',(-38.8368713051726,87.2555585750928,116.144870664273));
#40449=CARTESIAN_POINT('Ctrl Pts',(-38.8727808297734,87.5107521661593,116.128726983382));
#40450=CARTESIAN_POINT('Ctrl Pts',(-38.8707764324224,87.7664952479985,116.112583302492));
#40451=CARTESIAN_POINT('Ctrl Pts',(-38.8685579872896,87.7690123127748,116.387416697508));
#40452=CARTESIAN_POINT('Ctrl Pts',(-38.8678266992505,87.32242234584,116.41554502776));
#40453=CARTESIAN_POINT('Ctrl Pts',(-38.754348048844,86.8754852846444,116.443673358012));
#40454=CARTESIAN_POINT('Ctrl Pts',(-38.5303374398981,86.4933414477537,116.471801688264));
#40455=CARTESIAN_POINT('Ctrl Pts',(-38.1110431489864,85.7780595695012,116.524451195994));
#40456=CARTESIAN_POINT('Ctrl Pts',(-37.3045013868685,85.2897800224741,116.577100703725));
#40457=CARTESIAN_POINT('Ctrl Pts',(-36.476345596471,85.2498569141419,116.629750211456));
#40458=CARTESIAN_POINT('Ctrl Pts',(-35.6481898060736,85.2099338058097,116.682399719187));
#40459=CARTESIAN_POINT('Ctrl Pts',(-34.7984199873967,85.6183671361723,116.735049226918));
#40460=CARTESIAN_POINT('Ctrl Pts',(-34.3122663654471,86.2899998658787,116.787698734649));
#40461=CARTESIAN_POINT('Ctrl Pts',(-33.8261127434974,86.961632595585,116.840348242379));
#40462=CARTESIAN_POINT('Ctrl Pts',(-33.703575318275,87.8964647246352,116.89299775011));
#40463=CARTESIAN_POINT('Ctrl Pts',(-34.0002045681009,88.6707043231418,116.945647257841));
#40464=CARTESIAN_POINT('Ctrl Pts',(-34.2968338179268,89.4449439216484,116.998296765572));
#40465=CARTESIAN_POINT('Ctrl Pts',(-35.012629742801,90.0585909896116,117.050946273303));
#40466=CARTESIAN_POINT('Ctrl Pts',(-35.823097145156,90.2334579603849,117.103595781034));
#40467=CARTESIAN_POINT('Ctrl Pts',(-36.6335645475111,90.4083249311581,117.156245288764));
#40468=CARTESIAN_POINT('Ctrl Pts',(-37.5387034273469,90.1444118047415,117.208894796495));
#40469=CARTESIAN_POINT('Ctrl Pts',(-38.1281828377678,89.561359583721,117.261544304226));
#40470=CARTESIAN_POINT('Ctrl Pts',(-38.5979509791879,89.0967134003639,117.303501768653));
#40471=CARTESIAN_POINT('Ctrl Pts',(-38.867249456628,88.429387705517,117.345459233081));
#40472=CARTESIAN_POINT('Ctrl Pts',(-38.8732537926193,87.7663787382843,117.387416697508));
#40473=CARTESIAN_POINT('Origin',(-36.3549260746835,87.7685555885722,114.));
#40474=CARTESIAN_POINT('',(-38.8750030608581,87.7702419441723,118.387416697508));
#40475=CARTESIAN_POINT('',(-38.8698084321024,87.7702649945025,118.112583302492));
#40476=CARTESIAN_POINT('',(-38.8724260746835,87.7685555885722,114.));
#40477=CARTESIAN_POINT('Ctrl Pts',(-38.8698084321024,87.7702649945025,118.112583302492));
#40478=CARTESIAN_POINT('Ctrl Pts',(-38.8716871432184,88.0672505628736,118.093854409486));
#40479=CARTESIAN_POINT('Ctrl Pts',(-38.8230123182726,88.363640358852,118.075125516479));
#40480=CARTESIAN_POINT('Ctrl Pts',(-38.7210386014842,88.6403912434327,118.056396623473));
#40481=CARTESIAN_POINT('Ctrl Pts',(-38.434376384526,89.418376244055,118.003747115742));
#40482=CARTESIAN_POINT('Ctrl Pts',(-37.7265197639628,90.0411647802181,117.951097608011));
#40483=CARTESIAN_POINT('Ctrl Pts',(-36.9183647744689,90.2264251396656,117.89844810028));
#40484=CARTESIAN_POINT('Ctrl Pts',(-36.110209784975,90.4116854991132,117.84579859255));
#40485=CARTESIAN_POINT('Ctrl Pts',(-35.2017564265505,90.1594176818452,117.793149084819));
#40486=CARTESIAN_POINT('Ctrl Pts',(-34.6048382145644,89.5839834666382,117.740499577088));
#40487=CARTESIAN_POINT('Ctrl Pts',(-34.0079200025783,89.0085492514311,117.687850069357));
#40488=CARTESIAN_POINT('Ctrl Pts',(-33.7225369370307,88.1099486382851,117.635200561626));
#40489=CARTESIAN_POINT('Ctrl Pts',(-33.8780630909172,87.295548550315,117.582551053895));
#40490=CARTESIAN_POINT('Ctrl Pts',(-34.0335892448037,86.4811484623449,117.529901546165));
#40491=CARTESIAN_POINT('Ctrl Pts',(-34.6300246181243,85.7509488995507,117.477252038434));
#40492=CARTESIAN_POINT('Ctrl Pts',(-35.3969843042668,85.4359747297191,117.424602530703));
#40493=CARTESIAN_POINT('Ctrl Pts',(-36.1639439904093,85.1210005598875,117.371953022972));
#40494=CARTESIAN_POINT('Ctrl Pts',(-37.1014279893737,85.2212517830186,117.319303515241));
#40495=CARTESIAN_POINT('Ctrl Pts',(-37.7844421863721,85.6912810316064,117.266654007511));
#40496=CARTESIAN_POINT('Ctrl Pts',(-38.4506875981189,86.1497705207481,117.215297105838));
#40497=CARTESIAN_POINT('Ctrl Pts',(-38.8748048774098,86.9601039695085,117.163940204165));
#40498=CARTESIAN_POINT('Ctrl Pts',(-38.8764804707602,87.7689256098953,117.112583302492));
#40499=CARTESIAN_POINT('Ctrl Pts',(-38.8732537926193,87.7663787382843,117.387416697508));
#40500=CARTESIAN_POINT('Ctrl Pts',(-38.8747838808003,87.5974238053543,117.398108740811));
#40501=CARTESIAN_POINT('Ctrl Pts',(-38.8592160150071,87.4287491946892,117.408800784115));
#40502=CARTESIAN_POINT('Ctrl Pts',(-38.825510554458,87.263780350327,117.419492827418));
#40503=CARTESIAN_POINT('Ctrl Pts',(-38.6595389197215,86.4514446535778,117.472142335149));
#40504=CARTESIAN_POINT('Ctrl Pts',(-38.0537757092426,85.7289645757037,117.52479184288));
#40505=CARTESIAN_POINT('Ctrl Pts',(-37.2828344627662,85.4238654734001,117.577441350611));
#40506=CARTESIAN_POINT('Ctrl Pts',(-36.5118932162898,85.1187663710965,117.630090858342));
#40507=CARTESIAN_POINT('Ctrl Pts',(-35.5757739338159,85.2310482443633,117.682740366072));
#40508=CARTESIAN_POINT('Ctrl Pts',(-34.8988520566596,85.7098098133835,117.735389873803));
#40509=CARTESIAN_POINT('Ctrl Pts',(-34.2219301795033,86.1885713824036,117.788039381534));
#40510=CARTESIAN_POINT('Ctrl Pts',(-33.8042057076648,87.033812647177,117.840688889265));
#40511=CARTESIAN_POINT('Ctrl Pts',(-33.8350476782021,87.8623563337875,117.893338396996));
#40512=CARTESIAN_POINT('Ctrl Pts',(-33.8658896487394,88.690900020398,117.945987904727));
#40513=CARTESIAN_POINT('Ctrl Pts',(-34.3452980616525,89.5027461288456,117.998637412457));
#40514=CARTESIAN_POINT('Ctrl Pts',(-35.055940403205,89.929856571368,118.051286920188));
#40515=CARTESIAN_POINT('Ctrl Pts',(-35.7665827447574,90.3569670138905,118.103936427919));
#40516=CARTESIAN_POINT('Ctrl Pts',(-36.7084590149491,90.3993417904879,118.15658593565));
#40517=CARTESIAN_POINT('Ctrl Pts',(-37.4545839296581,90.0377709407583,118.209235443381));
#40518=CARTESIAN_POINT('Ctrl Pts',(-38.2007088443672,89.6762000910287,118.261884951112));
#40519=CARTESIAN_POINT('Ctrl Pts',(-38.7510824035936,88.9106836149721,118.314534458842));
#40520=CARTESIAN_POINT('Ctrl Pts',(-38.8562011236206,88.0882567655663,118.367183966573));
#40521=CARTESIAN_POINT('Ctrl Pts',(-38.8696665156073,87.9829063588563,118.373928210218));
#40522=CARTESIAN_POINT('Ctrl Pts',(-38.8758257923026,87.8766221189515,118.380672453863));
#40523=CARTESIAN_POINT('Ctrl Pts',(-38.8750030608581,87.7702419441723,118.387416697508));
#40524=CARTESIAN_POINT('Origin',(-36.3549260746835,87.7685555885722,114.));
#40525=CARTESIAN_POINT('',(-38.8685902376792,87.769097033614,119.387416697508));
#40526=CARTESIAN_POINT('',(-38.8706377933747,87.7665317068533,119.112583302492));
#40527=CARTESIAN_POINT('',(-38.8724260746835,87.7685555885722,114.));
#40528=CARTESIAN_POINT('Ctrl Pts',(-38.8706377933747,87.7665317068533,119.112583302492));
#40529=CARTESIAN_POINT('Ctrl Pts',(-38.866244579201,88.3395289437958,119.076418122537));
#40530=CARTESIAN_POINT('Ctrl Pts',(-38.6718416557376,88.9152230430577,119.040252942582));
#40531=CARTESIAN_POINT('Ctrl Pts',(-38.3129773669244,89.3574611972722,119.004087762628));
#40532=CARTESIAN_POINT('Ctrl Pts',(-37.7905403661463,90.0012744217129,118.951438254897));
#40533=CARTESIAN_POINT('Ctrl Pts',(-36.9195484108592,90.3622447379968,118.898788747166));
#40534=CARTESIAN_POINT('Ctrl Pts',(-36.0948524578377,90.2767317412963,118.846139239435));
#40535=CARTESIAN_POINT('Ctrl Pts',(-35.2701565048161,90.1912187445957,118.793489731704));
#40536=CARTESIAN_POINT('Ctrl Pts',(-34.4917565540599,89.6592224349109,118.740840223973));
#40537=CARTESIAN_POINT('Ctrl Pts',(-34.1125283868184,88.9219152498275,118.688190716243));
#40538=CARTESIAN_POINT('Ctrl Pts',(-33.7333002195769,88.1846080647441,118.635541208512));
#40539=CARTESIAN_POINT('Ctrl Pts',(-33.75324383585,87.2419900042621,118.582891700781));
#40540=CARTESIAN_POINT('Ctrl Pts',(-34.1633181002087,86.5213826316133,118.53024219305));
#40541=CARTESIAN_POINT('Ctrl Pts',(-34.5733923645675,85.8007752589644,118.477592685319));
#40542=CARTESIAN_POINT('Ctrl Pts',(-35.3735972770119,85.3021785741488,118.424943177589));
#40543=CARTESIAN_POINT('Ctrl Pts',(-36.2011721091829,85.2516238022933,118.372293669858));
#40544=CARTESIAN_POINT('Ctrl Pts',(-37.028746941354,85.2010690304378,118.319644162127));
#40545=CARTESIAN_POINT('Ctrl Pts',(-37.8836916932516,85.5985561715425,118.266994654396));
#40546=CARTESIAN_POINT('Ctrl Pts',(-38.3784301625238,86.2638904746356,118.214345146665));
#40547=CARTESIAN_POINT('Ctrl Pts',(-38.6971764097124,86.6925468767723,118.180424531941));
#40548=CARTESIAN_POINT('Ctrl Pts',(-38.8664058265174,87.2323830684335,118.146503917216));
#40549=CARTESIAN_POINT('Ctrl Pts',(-38.8698084321024,87.7702649945025,118.112583302492));
#40550=CARTESIAN_POINT('Ctrl Pts',(-38.8750030608581,87.7702419441723,118.387416697508));
#40551=CARTESIAN_POINT('Ctrl Pts',(-38.8694030697812,87.0461562981247,118.433321961594));
#40552=CARTESIAN_POINT('Ctrl Pts',(-38.5403294887911,86.3176260284683,118.47922722568));
#40553=CARTESIAN_POINT('Ctrl Pts',(-37.9899883034859,85.848879256096,118.525132489766));
#40554=CARTESIAN_POINT('Ctrl Pts',(-37.3587928824967,85.3112658187866,118.577781997497));
#40555=CARTESIAN_POINT('Ctrl Pts',(-36.4365381596906,85.115376166923,118.630431505227));
#40556=CARTESIAN_POINT('Ctrl Pts',(-35.6413142888051,85.3500138937257,118.683081012958));
#40557=CARTESIAN_POINT('Ctrl Pts',(-34.8460904179196,85.5846516205283,118.735730520689));
#40558=CARTESIAN_POINT('Ctrl Pts',(-34.1778973989547,86.2498167259973,118.78838002842));
#40559=CARTESIAN_POINT('Ctrl Pts',(-33.9396503765726,87.0439667278887,118.841029536151));
#40560=CARTESIAN_POINT('Ctrl Pts',(-33.7014033541905,87.83811672978,118.893679043881));
#40561=CARTESIAN_POINT('Ctrl Pts',(-33.8931023283913,88.7612516280936,118.946328551612));
#40562=CARTESIAN_POINT('Ctrl Pts',(-34.4278434831162,89.3948822478746,118.998978059343));
#40563=CARTESIAN_POINT('Ctrl Pts',(-34.9625846378412,90.0285128676557,119.051627567074));
#40564=CARTESIAN_POINT('Ctrl Pts',(-35.8403679730904,90.3726392089041,119.104277074805));
#40565=CARTESIAN_POINT('Ctrl Pts',(-36.6632637646553,90.2712568417485,119.156926582536));
#40566=CARTESIAN_POINT('Ctrl Pts',(-37.4861595562202,90.1698744745929,119.209576090266));
#40567=CARTESIAN_POINT('Ctrl Pts',(-38.2541678041008,89.6229833990333,119.262225597997));
#40568=CARTESIAN_POINT('Ctrl Pts',(-38.6191236428543,88.8785083391832,119.314875105728));
#40569=CARTESIAN_POINT('Ctrl Pts',(-38.7867382361248,88.5365905751519,119.339055636321));
#40570=CARTESIAN_POINT('Ctrl Pts',(-38.8693360705098,88.152995973142,119.363236166915));
#40571=CARTESIAN_POINT('Ctrl Pts',(-38.8685902376792,87.769097033614,119.387416697508));
#40572=CARTESIAN_POINT('Origin',(-36.3549260746835,87.7685555885722,114.));
#40573=CARTESIAN_POINT('',(-38.8730930351581,87.7663573574127,120.387416697508));
#40574=CARTESIAN_POINT('',(-38.8765117847785,87.7688288397063,120.112583302492));
#40575=CARTESIAN_POINT('',(-38.8724260746835,87.7685555885722,114.));
#40576=CARTESIAN_POINT('Ctrl Pts',(-38.8765117847785,87.7688288397063,120.112583302492));
#40577=CARTESIAN_POINT('Ctrl Pts',(-38.8765350839041,87.783820778578,120.11163134332));
#40578=CARTESIAN_POINT('Ctrl Pts',(-38.8764128203056,87.7988123273143,120.110679384147));
#40579=CARTESIAN_POINT('Ctrl Pts',(-38.8761438311705,87.8138012428756,120.109727424975));
#40580=CARTESIAN_POINT('Ctrl Pts',(-38.8612669898543,88.6427853512518,120.057077917244));
#40581=CARTESIAN_POINT('Ctrl Pts',(-38.3975851441409,89.463715087247,120.004428409513));
#40582=CARTESIAN_POINT('Ctrl Pts',(-37.6953015855779,89.9044346174046,119.951778901782));
#40583=CARTESIAN_POINT('Ctrl Pts',(-36.9930180270149,90.3451541475622,119.899129394052));
#40584=CARTESIAN_POINT('Ctrl Pts',(-36.0521327556023,90.4056634718823,119.846479886321));
#40585=CARTESIAN_POINT('Ctrl Pts',(-35.2991817147569,90.058531521478,119.79383037859));
#40586=CARTESIAN_POINT('Ctrl Pts',(-34.5462306739115,89.7113995710737,119.741180870859));
#40587=CARTESIAN_POINT('Ctrl Pts',(-33.9812138636332,88.956626345945,119.688531363128));
#40588=CARTESIAN_POINT('Ctrl Pts',(-33.8602731048237,88.136376852245,119.635881855397));
#40589=CARTESIAN_POINT('Ctrl Pts',(-33.7393323460141,87.316127358545,119.583232347667));
#40590=CARTESIAN_POINT('Ctrl Pts',(-34.0624676386734,86.4304015962738,119.530582839936));
#40591=CARTESIAN_POINT('Ctrl Pts',(-34.6831904912772,85.8807298501539,119.477933332205));
#40592=CARTESIAN_POINT('Ctrl Pts',(-35.3039133438809,85.3310581040341,119.425283824474));
#40593=CARTESIAN_POINT('Ctrl Pts',(-36.2222237564292,85.1174403740656,119.372634316743));
#40594=CARTESIAN_POINT('Ctrl Pts',(-37.0218196779139,85.3367170196712,119.319984809013));
#40595=CARTESIAN_POINT('Ctrl Pts',(-37.8214155993986,85.5559936652768,119.267335301282));
#40596=CARTESIAN_POINT('Ctrl Pts',(-38.5022970298196,86.2081646864565,119.214685793551));
#40597=CARTESIAN_POINT('Ctrl Pts',(-38.7557967218956,86.9975782633452,119.16203628582));
#40598=CARTESIAN_POINT('Ctrl Pts',(-38.8351663531686,87.2447401593083,119.145551958044));
#40599=CARTESIAN_POINT('Ctrl Pts',(-38.8726402493978,87.505355783484,119.129067630268));
#40600=CARTESIAN_POINT('Ctrl Pts',(-38.8706377933747,87.7665317068533,119.112583302492));
#40601=CARTESIAN_POINT('Ctrl Pts',(-38.8685902376792,87.769097033614,119.387416697508));
#40602=CARTESIAN_POINT('Ctrl Pts',(-38.867712130488,87.317113149706,119.415885674646));
#40603=CARTESIAN_POINT('Ctrl Pts',(-38.7513067081162,86.8647074065548,119.444354651783));
#40604=CARTESIAN_POINT('Ctrl Pts',(-38.5221044433275,86.4793994073616,119.472823628921));
#40605=CARTESIAN_POINT('Ctrl Pts',(-38.0982259754207,85.7668245795307,119.525473136651));
#40606=CARTESIAN_POINT('Ctrl Pts',(-37.2885656099805,85.2837339680096,119.578122644382));
#40607=CARTESIAN_POINT('Ctrl Pts',(-36.4601705392343,85.2491292346396,119.630772152113));
#40608=CARTESIAN_POINT('Ctrl Pts',(-35.6317754684881,85.2145245012696,119.683421659844));
#40609=CARTESIAN_POINT('Ctrl Pts',(-34.7846456924359,85.6284056460505,119.736071167575));
#40610=CARTESIAN_POINT('Ctrl Pts',(-34.3028146583386,86.3031461938721,119.788720675305));
#40611=CARTESIAN_POINT('Ctrl Pts',(-33.8209836242412,86.9778867416937,119.841370183036));
#40612=CARTESIAN_POINT('Ctrl Pts',(-33.7044513320988,87.913486692556,119.894019690767));
#40613=CARTESIAN_POINT('Ctrl Pts',(-34.0060458310393,88.685805526085,119.946669198498));
#40614=CARTESIAN_POINT('Ctrl Pts',(-34.3076403299799,89.458124359614,119.999318706229));
#40615=CARTESIAN_POINT('Ctrl Pts',(-35.0273616200035,90.0671620758098,120.05196821396));
#40616=CARTESIAN_POINT('Ctrl Pts',(-35.8389351910839,90.2368217366715,120.10461772169));
#40617=CARTESIAN_POINT('Ctrl Pts',(-36.6505087621644,90.4064813975333,120.157267229421));
#40618=CARTESIAN_POINT('Ctrl Pts',(-37.5539346143018,90.136763003061,120.209916737152));
#40619=CARTESIAN_POINT('Ctrl Pts',(-38.1396579805213,89.5499371283205,120.262566244883));
#40620=CARTESIAN_POINT('Ctrl Pts',(-38.6026431728332,89.0860804578518,120.304183062425));
#40621=CARTESIAN_POINT('Ctrl Pts',(-38.8671241578398,88.4240913465261,120.345799879966));
#40622=CARTESIAN_POINT('Ctrl Pts',(-38.8730930351581,87.7663573574127,120.387416697508));
#40623=CARTESIAN_POINT('Origin',(-36.3549260746835,87.7685555885722,114.));
#40624=CARTESIAN_POINT('',(-38.8751286390733,87.7701344517389,121.387416697508));
#40625=CARTESIAN_POINT('',(-38.8699207989934,87.7703173750275,121.112583302492));
#40626=CARTESIAN_POINT('',(-38.8724260746835,87.7685555885722,114.));
#40627=CARTESIAN_POINT('',(-34.4414600780185,89.4045427919472,122.));
#40628=CARTESIAN_POINT('Ctrl Pts',(-38.8751286390733,87.7701344517389,121.387416697508));
#40629=CARTESIAN_POINT('Ctrl Pts',(-38.8696705638905,87.0409116216481,121.43366260848));
#40630=CARTESIAN_POINT('Ctrl Pts',(-38.5351407981639,86.3074376342814,121.479908519451));
#40631=CARTESIAN_POINT('Ctrl Pts',(-37.9776638007606,85.8386043277258,121.526154430423));
#40632=CARTESIAN_POINT('Ctrl Pts',(-37.3429938619931,85.3048524288138,121.578803938153));
#40633=CARTESIAN_POINT('Ctrl Pts',(-36.4193597263055,85.1141040344884,121.631453445884));
#40634=CARTESIAN_POINT('Ctrl Pts',(-35.6257426583825,85.3542580189696,121.684102953615));
#40635=CARTESIAN_POINT('Ctrl Pts',(-34.8321255904596,85.5944120034508,121.736752461346));
#40636=CARTESIAN_POINT('Ctrl Pts',(-34.1685255903014,86.2654683667386,121.789401969077));
#40637=CARTESIAN_POINT('Ctrl Pts',(-33.9355603656107,87.0597542623074,121.842051476807));
#40638=CARTESIAN_POINT('Ctrl Pts',(-33.70259514092,87.8540401578761,121.894700984538));
#40639=CARTESIAN_POINT('Ctrl Pts',(-33.9002646916968,88.7715555857257,121.947350492269));
#40640=CARTESIAN_POINT('Ctrl Pts',(-34.4414600780185,89.4045427919472,122.));
#40641=CARTESIAN_POINT('',(-38.2720362925639,89.4070835106059,122.));
#40642=CARTESIAN_POINT('Origin',(-36.3549260746835,87.7685555885722,122.));
#40643=CARTESIAN_POINT('Ctrl Pts',(-38.2720451383381,89.4070896778011,122.));
#40644=CARTESIAN_POINT('Ctrl Pts',(-37.7492245696404,90.0158048033409,121.949053726697));
#40645=CARTESIAN_POINT('Ctrl Pts',(-36.9095000892721,90.3559810494937,121.898107453395));
#40646=CARTESIAN_POINT('Ctrl Pts',(-36.1108292529146,90.2782182443628,121.847161180092));
#40647=CARTESIAN_POINT('Ctrl Pts',(-35.2854572748038,90.1978556752386,121.794511672361));
#40648=CARTESIAN_POINT('Ctrl Pts',(-34.5039298348585,89.6711418716167,121.74186216463));
#40649=CARTESIAN_POINT('Ctrl Pts',(-34.1200452267186,88.9363551361257,121.6892126569));
#40650=CARTESIAN_POINT('Ctrl Pts',(-33.7361606185786,88.2015684006347,121.636563149169));
#40651=CARTESIAN_POINT('Ctrl Pts',(-33.749918842244,87.2587087332746,121.583913641438));
#40652=CARTESIAN_POINT('Ctrl Pts',(-34.1553236157352,86.5354489663317,121.531264133707));
#40653=CARTESIAN_POINT('Ctrl Pts',(-34.5607283892265,85.8121891993888,121.478614625976));
#40654=CARTESIAN_POINT('Ctrl Pts',(-35.3577797125436,85.308529332863,121.425965118246));
#40655=CARTESIAN_POINT('Ctrl Pts',(-36.1850294138675,85.2526783544614,121.373315610515));
#40656=CARTESIAN_POINT('Ctrl Pts',(-37.0122791151915,85.1968273760598,121.320666102784));
#40657=CARTESIAN_POINT('Ctrl Pts',(-37.8697271945221,85.5887852857824,121.268016595053));
#40658=CARTESIAN_POINT('Ctrl Pts',(-38.3687195320203,86.2509210824945,121.215367087322));
#40659=CARTESIAN_POINT('Ctrl Pts',(-38.693434952036,86.6818008519411,121.181105825712));
#40660=CARTESIAN_POINT('Ctrl Pts',(-38.8663567186898,87.2270916455049,121.146844564102));
#40661=CARTESIAN_POINT('Ctrl Pts',(-38.8699207989934,87.7703173750275,121.112583302492));
#40662=CARTESIAN_POINT('Origin',(-36.3549260746835,87.7685555885722,124.208423447177));
#40663=CARTESIAN_POINT('',(-39.4331959724664,87.7693690614377,107.791576552823));
#40664=CARTESIAN_POINT('',(-39.4235550742983,87.7688699395357,107.708423447177));
#40665=CARTESIAN_POINT('',(-39.4284260746835,87.7685555885726,124.208423447177));
#40666=CARTESIAN_POINT('',(-35.5611267921506,84.7993326348266,107.));
#40667=CARTESIAN_POINT('Ctrl Pts',(-39.4235550742983,87.7688699395357,107.708423447177));
#40668=CARTESIAN_POINT('Ctrl Pts',(-39.4238749307152,88.2640454211739,107.682880329042));
#40669=CARTESIAN_POINT('Ctrl Pts',(-39.0776226443318,89.7793619650307,107.604687703175));
#40670=CARTESIAN_POINT('Ctrl Pts',(-36.7064604371766,91.3774168831885,107.473845569577));
#40671=CARTESIAN_POINT('Ctrl Pts',(-33.5229010658053,90.036960964095,107.315897046385));
#40672=CARTESIAN_POINT('Ctrl Pts',(-32.9121326734567,86.6347724882534,107.157948523192));
#40673=CARTESIAN_POINT('Ctrl Pts',(-34.578888202379,85.0619266872042,107.052649507731));
#40674=CARTESIAN_POINT('Ctrl Pts',(-35.5611267921506,84.7993326348266,107.));
#40675=CARTESIAN_POINT('',(-37.1487253572163,84.7993326348265,107.));
#40676=CARTESIAN_POINT('Origin',(-36.3549260746835,87.7685555885722,107.));
#40677=CARTESIAN_POINT('Ctrl Pts',(-39.4331959724664,87.7693690614377,107.791576552823));
#40678=CARTESIAN_POINT('Ctrl Pts',(-39.4333520414626,87.8138779030189,107.789262006108));
#40679=CARTESIAN_POINT('Ctrl Pts',(-39.4123923264904,88.8706874181061,107.734297951662));
#40680=CARTESIAN_POINT('Ctrl Pts',(-38.2031234082454,90.8887186315066,107.626684389485));
#40681=CARTESIAN_POINT('Ctrl Pts',(-34.7524574012803,91.0220940358159,107.468735866293));
#40682=CARTESIAN_POINT('Ctrl Pts',(-32.7548483299835,88.204780757559,107.3107873431));
#40683=CARTESIAN_POINT('Ctrl Pts',(-34.0073633012862,85.0282370938957,107.154542054336));
#40684=CARTESIAN_POINT('Ctrl Pts',(-36.2036730954584,84.5433632626068,107.050946273303));
#40685=CARTESIAN_POINT('Ctrl Pts',(-37.1506394582515,84.7942439414616,107.));
#40686=CARTESIAN_POINT('Origin',(-36.3549260746835,87.7685555885722,124.208423447177));
#40687=CARTESIAN_POINT('',(-39.4248377279915,87.7704209830772,108.791576552823));
#40688=CARTESIAN_POINT('',(-39.4300189070168,87.765997310884,108.708423447177));
#40689=CARTESIAN_POINT('',(-39.4284260746835,87.7685555885726,124.208423447177));
#40690=CARTESIAN_POINT('Ctrl Pts',(-39.4300189070168,87.765997310884,108.708423447177));
#40691=CARTESIAN_POINT('Ctrl Pts',(-39.4226310503045,88.5947453159106,108.665444042093));
#40692=CARTESIAN_POINT('Ctrl Pts',(-38.6509820307071,90.4508356800763,108.569815129278));
#40693=CARTESIAN_POINT('Ctrl Pts',(-35.521928276906,91.298128615592,108.421536708732));
#40694=CARTESIAN_POINT('Ctrl Pts',(-32.944032143022,89.0005543557004,108.26358818554));
#40695=CARTESIAN_POINT('Ctrl Pts',(-33.4587561442345,85.5858976617427,108.105639662347));
#40696=CARTESIAN_POINT('Ctrl Pts',(-36.5992128995613,84.1503275352445,107.947691139155));
#40697=CARTESIAN_POINT('Ctrl Pts',(-39.0463675728263,85.696694156362,107.815285734098));
#40698=CARTESIAN_POINT('Ctrl Pts',(-39.4232156422602,87.2433890858758,107.735529836772));
#40699=CARTESIAN_POINT('Ctrl Pts',(-39.4235550742983,87.7688699395357,107.708423447177));
#40700=CARTESIAN_POINT('Ctrl Pts',(-39.4248377279915,87.7704209830772,108.791576552823));
#40701=CARTESIAN_POINT('Ctrl Pts',(-39.4269818594004,88.1529039528601,108.771825719159));
#40702=CARTESIAN_POINT('Ctrl Pts',(-39.1839874391446,89.552339992846,108.699425377765));
#40703=CARTESIAN_POINT('Ctrl Pts',(-37.0970138577844,91.3183647606488,108.57437552864));
#40704=CARTESIAN_POINT('Ctrl Pts',(-33.7881605542584,90.3305043851839,108.416427005448));
#40705=CARTESIAN_POINT('Ctrl Pts',(-32.8065174312516,87.0197923230117,108.258478482255));
#40706=CARTESIAN_POINT('Ctrl Pts',(-35.0421044995447,84.3879830042027,108.100529959063));
#40707=CARTESIAN_POINT('Ctrl Pts',(-38.4177928691641,84.8148429236005,107.944895982585));
#40708=CARTESIAN_POINT('Ctrl Pts',(-39.4298019053741,86.8014254068839,107.841911513839));
#40709=CARTESIAN_POINT('Ctrl Pts',(-39.4331959724664,87.7693690614377,107.791576552823));
#40710=CARTESIAN_POINT('Origin',(-36.3549260746835,87.7685555885722,124.208423447177));
#40711=CARTESIAN_POINT('',(-39.4267609799808,87.7659629280684,109.791576552823));
#40712=CARTESIAN_POINT('',(-39.4310568549431,87.7708236397202,109.708423447177));
#40713=CARTESIAN_POINT('',(-39.4284260746835,87.7685555885726,124.208423447177));
#40714=CARTESIAN_POINT('Ctrl Pts',(-39.431056854943,87.7708236397202,109.708423447178));
#40715=CARTESIAN_POINT('Ctrl Pts',(-39.4322959763111,87.9204433841515,109.700657262876));
#40716=CARTESIAN_POINT('Ctrl Pts',(-39.3546330833386,89.083093328256,109.640241570843));
#40717=CARTESIAN_POINT('Ctrl Pts',(-37.8732760615816,91.0619523578304,109.527176371079));
#40718=CARTESIAN_POINT('Ctrl Pts',(-34.4272254088536,90.8403332051346,109.369227847887));
#40719=CARTESIAN_POINT('Ctrl Pts',(-32.7289618949911,87.8336271396496,109.211279324695));
#40720=CARTESIAN_POINT('Ctrl Pts',(-34.3182507011933,84.7679217971554,109.053330801502));
#40721=CARTESIAN_POINT('Ctrl Pts',(-37.7541293221915,84.4228016643723,108.89538227831));
#40722=CARTESIAN_POINT('Ctrl Pts',(-39.3316610725117,86.3796383650939,108.780413160201));
#40723=CARTESIAN_POINT('Ctrl Pts',(-39.4316811294837,87.579534090627,108.718093549824));
#40724=CARTESIAN_POINT('Ctrl Pts',(-39.4300189070168,87.765997310884,108.708423447177));
#40725=CARTESIAN_POINT('Ctrl Pts',(-39.4267609799808,87.7659629280684,109.791576552823));
#40726=CARTESIAN_POINT('Ctrl Pts',(-39.4209015342644,88.4849691123104,109.754389432211));
#40727=CARTESIAN_POINT('Ctrl Pts',(-38.8116905796402,90.2308909611916,109.664552803868));
#40728=CARTESIAN_POINT('Ctrl Pts',(-35.9114810808611,91.3678896299961,109.522066667795));
#40729=CARTESIAN_POINT('Ctrl Pts',(-33.0986031650656,89.3648670933915,109.364118144603));
#40730=CARTESIAN_POINT('Ctrl Pts',(-33.2381342205824,85.9145173244662,109.20616962141));
#40731=CARTESIAN_POINT('Ctrl Pts',(-36.2035656043253,84.1451679505691,109.048221098218));
#40732=CARTESIAN_POINT('Ctrl Pts',(-38.918255079236,85.471480422957,108.910023408688));
#40733=CARTESIAN_POINT('Ctrl Pts',(-39.4212662797386,87.1333247078628,108.82447522689));
#40734=CARTESIAN_POINT('Ctrl Pts',(-39.4248377279915,87.7704209830772,108.791576552823));
#40735=CARTESIAN_POINT('Origin',(-36.3549260746835,87.7685555885722,124.208423447177));
#40736=CARTESIAN_POINT('',(-39.4332677588359,87.7692403954757,110.791576552823));
#40737=CARTESIAN_POINT('',(-39.4236451829169,87.7689040049272,110.708423447177));
#40738=CARTESIAN_POINT('',(-39.4284260746835,87.7685555885726,124.208423447177));
#40739=CARTESIAN_POINT('Ctrl Pts',(-39.4236451829169,87.7689040049272,110.708423447177));
#40740=CARTESIAN_POINT('Ctrl Pts',(-39.4241444783375,88.2574355105714,110.683220975927));
#40741=CARTESIAN_POINT('Ctrl Pts',(-39.0844834239227,89.7658834613085,110.605368996946));
#40742=CARTESIAN_POINT('Ctrl Pts',(-36.7289586508838,91.3757634277843,110.474867510234));
#40743=CARTESIAN_POINT('Ctrl Pts',(-33.5388966026528,90.0536872598855,110.316918987042));
#40744=CARTESIAN_POINT('Ctrl Pts',(-32.9020428254094,86.6597517104068,110.158970463849));
#40745=CARTESIAN_POINT('Ctrl Pts',(-35.3958132871802,84.2711349028723,110.001021940657));
#40746=CARTESIAN_POINT('Ctrl Pts',(-38.5938083527313,85.0150537749961,109.850839601766));
#40747=CARTESIAN_POINT('Ctrl Pts',(-39.4238955665977,86.9061221183966,109.753306770606));
#40748=CARTESIAN_POINT('Ctrl Pts',(-39.431056854943,87.7708236397202,109.708423447178));
#40749=CARTESIAN_POINT('Ctrl Pts',(-39.4332677588359,87.7692403954757,110.791576552823));
#40750=CARTESIAN_POINT('Ctrl Pts',(-39.4333834028134,87.8071966848497,110.789602652993));
#40751=CARTESIAN_POINT('Ctrl Pts',(-39.4156194617581,88.8574441518405,110.734979245433));
#40752=CARTESIAN_POINT('Ctrl Pts',(-38.223100855083,90.8768947163338,110.627706330142));
#40753=CARTESIAN_POINT('Ctrl Pts',(-34.7734205070594,91.0320949679017,110.46975780695));
#40754=CARTESIAN_POINT('Ctrl Pts',(-32.7576431577175,88.2283433211983,110.311809283757));
#40755=CARTESIAN_POINT('Ctrl Pts',(-34.0034128231148,85.0077161192772,110.153860760565));
#40756=CARTESIAN_POINT('Ctrl Pts',(-37.3812280349669,84.2902581008489,109.995912237372));
#40757=CARTESIAN_POINT('Ctrl Pts',(-39.2523388634201,86.1528899994607,109.875150834792));
#40758=CARTESIAN_POINT('Ctrl Pts',(-39.4291973347315,87.4670004975569,109.807038939942));
#40759=CARTESIAN_POINT('Ctrl Pts',(-39.4267609799808,87.7659629280684,109.791576552823));
#40760=CARTESIAN_POINT('Origin',(-36.3549260746835,87.7685555885722,124.208423447177));
#40761=CARTESIAN_POINT('',(-39.4249633754519,87.7704976440673,111.791576552823));
#40762=CARTESIAN_POINT('',(-39.4298259838121,87.7659597950156,111.708423447177));
#40763=CARTESIAN_POINT('',(-39.4284260746835,87.7685555885726,124.208423447177));
#40764=CARTESIAN_POINT('Ctrl Pts',(-39.4298259838121,87.7659597950156,111.708423447177));
#40765=CARTESIAN_POINT('Ctrl Pts',(-39.422445104778,88.5882717598716,111.665784688979));
#40766=CARTESIAN_POINT('Ctrl Pts',(-38.6609851967907,90.4380265410958,111.570496423049));
#40767=CARTESIAN_POINT('Ctrl Pts',(-35.544600016728,91.3034134977843,111.422558649389));
#40768=CARTESIAN_POINT('Ctrl Pts',(-32.9520312482784,89.0224118636959,111.264610126197));
#40769=CARTESIAN_POINT('Ctrl Pts',(-33.4447637244879,85.6045768793427,111.106661603004));
#40770=CARTESIAN_POINT('Ctrl Pts',(-36.5760518951862,84.1487555760565,110.948713079812));
#40771=CARTESIAN_POINT('Ctrl Pts',(-39.0392097413283,85.6835153821574,110.81596702787));
#40772=CARTESIAN_POINT('Ctrl Pts',(-39.4231014195896,87.2368632409793,110.735870483658));
#40773=CARTESIAN_POINT('Ctrl Pts',(-39.4236451829169,87.7689040049272,110.708423447177));
#40774=CARTESIAN_POINT('Ctrl Pts',(-39.4249633754519,87.7704976440673,111.791576552823));
#40775=CARTESIAN_POINT('Ctrl Pts',(-39.4271630525139,88.1463451570976,111.772166366045));
#40776=CARTESIAN_POINT('Ctrl Pts',(-39.1897287451099,89.5389847880784,111.700106671536));
#40777=CARTESIAN_POINT('Ctrl Pts',(-37.11979162744,91.3135280607988,111.575397469297));
#40778=CARTESIAN_POINT('Ctrl Pts',(-33.8046642536859,90.3469298412686,111.417448946105));
#40779=CARTESIAN_POINT('Ctrl Pts',(-32.8017817103211,87.0425981045389,111.259500422912));
#40780=CARTESIAN_POINT('Ctrl Pts',(-35.0204270981272,84.3964699395587,111.10155189972));
#40781=CARTESIAN_POINT('Ctrl Pts',(-38.4061745970663,84.8025699726496,110.945577276356));
#40782=CARTESIAN_POINT('Ctrl Pts',(-39.4302988498904,86.7947947781262,110.842252160724));
#40783=CARTESIAN_POINT('Ctrl Pts',(-39.4332677588359,87.7692403954757,110.791576552823));
#40784=CARTESIAN_POINT('Origin',(-36.3549260746835,87.7685555885722,124.208423447177));
#40785=CARTESIAN_POINT('',(-39.4265848876636,87.7659995883269,112.791576552823));
#40786=CARTESIAN_POINT('',(-39.4312326367126,87.7707578835516,112.708423447177));
#40787=CARTESIAN_POINT('',(-39.4284260746835,87.7685555885726,124.208423447177));
#40788=CARTESIAN_POINT('Ctrl Pts',(-39.4312326367126,87.7707578835516,112.708423447177));
#40789=CARTESIAN_POINT('Ctrl Pts',(-39.4323935001362,87.9137935611134,112.700997909761));
#40790=CARTESIAN_POINT('Ctrl Pts',(-39.358587174522,89.0697956308562,112.640922864614));
#40791=CARTESIAN_POINT('Ctrl Pts',(-37.8943917131075,91.0521350845713,112.528198311736));
#40792=CARTESIAN_POINT('Ctrl Pts',(-34.4469889106826,90.8526477623989,112.370249788544));
#40793=CARTESIAN_POINT('Ctrl Pts',(-32.7294547075721,87.8569078646409,112.212301265352));
#40794=CARTESIAN_POINT('Ctrl Pts',(-34.2990251292932,84.7810616452854,112.054352742159));
#40795=CARTESIAN_POINT('Ctrl Pts',(-37.732618410801,84.413885323785,111.896404218967));
#40796=CARTESIAN_POINT('Ctrl Pts',(-39.3273914927566,86.3663225186427,111.781094453973));
#40797=CARTESIAN_POINT('Ctrl Pts',(-39.4315588703796,87.5728969698939,111.71843419671));
#40798=CARTESIAN_POINT('Ctrl Pts',(-39.4298259838121,87.7659597950156,111.708423447177));
#40799=CARTESIAN_POINT('Ctrl Pts',(-39.4265848876636,87.7659995883269,112.791576552823));
#40800=CARTESIAN_POINT('Ctrl Pts',(-39.4208858349911,88.4785229697945,112.754730079097));
#40801=CARTESIAN_POINT('Ctrl Pts',(-38.8205345450662,90.2178280429807,112.66523409764));
#40802=CARTESIAN_POINT('Ctrl Pts',(-35.93460153719,91.3706628087708,112.523088608452));
#40803=CARTESIAN_POINT('Ctrl Pts',(-33.1089202140314,89.3857429912062,112.365140085259));
#40804=CARTESIAN_POINT('Ctrl Pts',(-33.2262936819204,85.934568540205,112.207191562067));
#40805=CARTESIAN_POINT('Ctrl Pts',(-36.1803029872748,84.1462143677634,112.049243038875));
#40806=CARTESIAN_POINT('Ctrl Pts',(-38.9101650309924,85.4582951470999,111.91070470246));
#40807=CARTESIAN_POINT('Ctrl Pts',(-39.4211964991877,87.1268708589074,111.824815873776));
#40808=CARTESIAN_POINT('Ctrl Pts',(-39.4249633754519,87.7704976440673,111.791576552823));
#40809=CARTESIAN_POINT('Origin',(-36.3549260746835,87.7685555885722,124.208423447177));
#40810=CARTESIAN_POINT('',(-39.4333269951809,87.7691245003032,113.791576552823));
#40811=CARTESIAN_POINT('',(-39.4236710600204,87.7690089236073,113.708423447177));
#40812=CARTESIAN_POINT('',(-39.4284260746835,87.7685555885726,124.208423447177));
#40813=CARTESIAN_POINT('Ctrl Pts',(-39.4236710600204,87.7690089236073,113.708423447178));
#40814=CARTESIAN_POINT('Ctrl Pts',(-39.4243122366841,88.2509270813075,113.683561622813));
#40815=CARTESIAN_POINT('Ctrl Pts',(-39.0911304972661,89.7525574526633,113.606050290717));
#40816=CARTESIAN_POINT('Ctrl Pts',(-36.7521128167719,91.3732874025,113.475889450891));
#40817=CARTESIAN_POINT('Ctrl Pts',(-33.5536274798598,90.071721874595,113.317940927699));
#40818=CARTESIAN_POINT('Ctrl Pts',(-32.8949943812288,86.6819455227893,113.159992404506));
#40819=CARTESIAN_POINT('Ctrl Pts',(-35.3733761199876,84.2773654698779,113.002043881314));
#40820=CARTESIAN_POINT('Ctrl Pts',(-38.583346428161,85.0023754277235,112.851520895538));
#40821=CARTESIAN_POINT('Ctrl Pts',(-39.4241625958431,86.8996234627776,112.753647417492));
#40822=CARTESIAN_POINT('Ctrl Pts',(-39.4312326367126,87.7707578835516,112.708423447177));
#40823=CARTESIAN_POINT('Ctrl Pts',(-39.4333269951809,87.7691245003032,113.791576552823));
#40824=CARTESIAN_POINT('Ctrl Pts',(-39.4334076784544,87.8005288405486,113.789943299879));
#40825=CARTESIAN_POINT('Ctrl Pts',(-39.4188025102445,88.8442059785835,113.735660539205));
#40826=CARTESIAN_POINT('Ctrl Pts',(-38.2430209835701,90.864835091082,113.628728270799));
#40827=CARTESIAN_POINT('Ctrl Pts',(-34.7944082905965,91.0421825355799,113.470779747607));
#40828=CARTESIAN_POINT('Ctrl Pts',(-32.7606696114516,88.2514319900887,113.312831224414));
#40829=CARTESIAN_POINT('Ctrl Pts',(-33.9857339531502,85.0228720973646,113.154882701222));
#40830=CARTESIAN_POINT('Ctrl Pts',(-37.3588727357218,84.2837399199298,112.996934178029));
#40831=CARTESIAN_POINT('Ctrl Pts',(-39.2472166530314,86.1395391875126,112.875832128563));
#40832=CARTESIAN_POINT('Ctrl Pts',(-39.4290291466135,87.460406404289,112.807379586827));
#40833=CARTESIAN_POINT('Ctrl Pts',(-39.4265848876636,87.7659995883269,112.791576552823));
#40834=CARTESIAN_POINT('Origin',(-36.3549260746835,87.7685555885722,124.208423447177));
#40835=CARTESIAN_POINT('',(-39.4250942775894,87.770571594449,114.791576552823));
#40836=CARTESIAN_POINT('',(-39.4296318005188,87.7659266486971,114.708423447177));
#40837=CARTESIAN_POINT('',(-39.4284260746835,87.7685555885726,124.208423447177));
#40838=CARTESIAN_POINT('Ctrl Pts',(-39.4296318005188,87.7659266486971,114.708423447177));
#40839=CARTESIAN_POINT('Ctrl Pts',(-39.4222699698754,88.5818020086375,114.666125335864));
#40840=CARTESIAN_POINT('Ctrl Pts',(-38.6709153677693,90.4252030152838,114.571177716821));
#40841=CARTESIAN_POINT('Ctrl Pts',(-35.5673140384357,91.3085437296246,114.423580590046));
#40842=CARTESIAN_POINT('Ctrl Pts',(-32.9601524074645,89.0442359979183,114.265632066854));
#40843=CARTESIAN_POINT('Ctrl Pts',(-33.4309288131869,85.623307637124,114.107683543661));
#40844=CARTESIAN_POINT('Ctrl Pts',(-36.5528046065515,84.1474103491404,113.949735020469));
#40845=CARTESIAN_POINT('Ctrl Pts',(-39.0321123676862,85.6702203471794,113.816648321641));
#40846=CARTESIAN_POINT('Ctrl Pts',(-39.4229544266047,87.2303763205356,113.736211130544));
#40847=CARTESIAN_POINT('Ctrl Pts',(-39.4236710600204,87.7690089236073,113.708423447178));
#40848=CARTESIAN_POINT('Ctrl Pts',(-39.4250942775894,87.770571594449,114.791576552823));
#40849=CARTESIAN_POINT('Ctrl Pts',(-39.4273437802822,88.1397834288107,114.772507012931));
#40850=CARTESIAN_POINT('Ctrl Pts',(-39.1954153750974,89.5256294501937,114.700787965308));
#40851=CARTESIAN_POINT('Ctrl Pts',(-37.1425381224351,91.3085437813298,114.576419409954));
#40852=CARTESIAN_POINT('Ctrl Pts',(-33.8212725638248,90.3632519156092,114.418470886762));
#40853=CARTESIAN_POINT('Ctrl Pts',(-32.7971935859219,87.0654278042858,114.260522363569));
#40854=CARTESIAN_POINT('Ctrl Pts',(-34.9988024520367,84.4051082703102,114.102573840377));
#40855=CARTESIAN_POINT('Ctrl Pts',(-38.3944877003389,84.7902994725376,113.946258570128));
#40856=CARTESIAN_POINT('Ctrl Pts',(-39.4308067741364,86.7881791852352,113.84259280761));
#40857=CARTESIAN_POINT('Ctrl Pts',(-39.4333269951809,87.7691245003032,113.791576552823));
#40858=CARTESIAN_POINT('Origin',(-36.3549260746835,87.7685555885722,124.208423447177));
#40859=CARTESIAN_POINT('',(-39.4264121022944,87.7660402134969,115.791576552823));
#40860=CARTESIAN_POINT('',(-39.4314045388933,87.7706880981477,115.708423447177));
#40861=CARTESIAN_POINT('',(-39.4284260746835,87.7685555885726,124.208423447177));
#40862=CARTESIAN_POINT('Ctrl Pts',(-39.4314045388933,87.7706880981477,115.708423447177));
#40863=CARTESIAN_POINT('Ctrl Pts',(-39.4324870743472,87.9071420895487,115.701338556647));
#40864=CARTESIAN_POINT('Ctrl Pts',(-39.362494359602,89.0565011022609,115.641604158386));
#40865=CARTESIAN_POINT('Ctrl Pts',(-37.9154438359774,91.0421824877652,115.529220252393));
#40866=CARTESIAN_POINT('Ctrl Pts',(-34.4668311933744,90.8648350458576,115.371271729201));
#40867=CARTESIAN_POINT('Ctrl Pts',(-32.7300967558443,87.8801851891123,115.213323206008));
#40868=CARTESIAN_POINT('Ctrl Pts',(-34.2798848175055,84.7943241686182,115.055374682816));
#40869=CARTESIAN_POINT('Ctrl Pts',(-37.7110496775229,84.4051083194366,114.897426159624));
#40870=CARTESIAN_POINT('Ctrl Pts',(-39.3230746797097,86.3530027291024,114.781775747744));
#40871=CARTESIAN_POINT('Ctrl Pts',(-39.4314334229786,87.5662617223888,114.718774843595));
#40872=CARTESIAN_POINT('Ctrl Pts',(-39.4296318005188,87.7659266486971,114.708423447177));
#40873=CARTESIAN_POINT('Ctrl Pts',(-39.4264121022944,87.7660402134969,115.791576552823));
#40874=CARTESIAN_POINT('Ctrl Pts',(-39.4208785096745,88.4720768830956,115.755070725982));
#40875=CARTESIAN_POINT('Ctrl Pts',(-38.8293123321225,90.2047529643201,115.665915391411));
#40876=CARTESIAN_POINT('Ctrl Pts',(-35.9577393267937,91.3732874551507,115.524110549109));
#40877=CARTESIAN_POINT('Ctrl Pts',(-33.1193710875871,89.4065522516036,115.366162025916));
#40878=CARTESIAN_POINT('Ctrl Pts',(-33.2145821502242,85.9546952911023,115.208213502724));
#40879=CARTESIAN_POINT('Ctrl Pts',(-36.1570475399255,84.14741029625,115.050264979531));
#40880=CARTESIAN_POINT('Ctrl Pts',(-38.9020111125005,85.4451186487052,114.911385996231));
#40881=CARTESIAN_POINT('Ctrl Pts',(-39.4211330793379,87.1204184395347,114.825156520661));
#40882=CARTESIAN_POINT('Ctrl Pts',(-39.4250942775894,87.770571594449,114.791576552823));
#40883=CARTESIAN_POINT('Origin',(-36.3549260746835,87.7685555885722,124.208423447177));
#40884=CARTESIAN_POINT('',(-39.4333759004399,87.7690073305927,116.791576552823));
#40885=CARTESIAN_POINT('',(-39.4237037046317,87.7691131821519,116.708423447178));
#40886=CARTESIAN_POINT('',(-39.4284260746835,87.7685555885726,124.208423447177));
#40887=CARTESIAN_POINT('Ctrl Pts',(-39.4237037046317,87.7691131821519,116.708423447178));
#40888=CARTESIAN_POINT('Ctrl Pts',(-39.4244820091948,88.2444156491833,116.683902269699));
#40889=CARTESIAN_POINT('Ctrl Pts',(-39.0977192292877,89.739228256387,116.606731584489));
#40890=CARTESIAN_POINT('Ctrl Pts',(-36.7752506060375,91.3706627561583,116.476911391548));
#40891=CARTESIAN_POINT('Ctrl Pts',(-33.5684738551649,90.0896615290181,116.318962868356));
#40892=CARTESIAN_POINT('Ctrl Pts',(-32.8880885856163,86.7041841389216,116.161014345163));
#40893=CARTESIAN_POINT('Ctrl Pts',(-35.3509794283091,84.2837399708291,116.003065821971));
#40894=CARTESIAN_POINT('Ctrl Pts',(-38.572813684769,84.9897178516136,115.852202189309));
#40895=CARTESIAN_POINT('Ctrl Pts',(-39.4244424957464,86.8931200035074,115.753988064378));
#40896=CARTESIAN_POINT('Ctrl Pts',(-39.4314045388933,87.7706880981477,115.708423447177));
#40897=CARTESIAN_POINT('Ctrl Pts',(-39.4333759004399,87.7690073305927,116.791576552823));
#40898=CARTESIAN_POINT('Ctrl Pts',(-39.4334273876949,87.7938606197418,116.790283946765));
#40899=CARTESIAN_POINT('Ctrl Pts',(-39.4219418998855,88.8309715577217,116.736341832976));
#40900=CARTESIAN_POINT('Ctrl Pts',(-38.2628632665517,90.8526478074454,116.629750211456));
#40901=CARTESIAN_POINT('Ctrl Pts',(-34.8154604137739,91.0521351325312,116.471801688264));
#40902=CARTESIAN_POINT('Ctrl Pts',(-32.7638442550116,88.2745007506674,116.313853165071));
#40903=CARTESIAN_POINT('Ctrl Pts',(-33.9681527643291,85.0381412779581,116.155904641879));
#40904=CARTESIAN_POINT('Ctrl Pts',(-37.3364760437162,84.2773654188855,115.997956118686));
#40905=CARTESIAN_POINT('Ctrl Pts',(-39.2420422323528,86.1261873235342,115.876513422334));
#40906=CARTESIAN_POINT('Ctrl Pts',(-39.4288591788618,87.4538152434738,115.807720233713));
#40907=CARTESIAN_POINT('Ctrl Pts',(-39.4264121022944,87.7660402134969,115.791576552823));
#40908=CARTESIAN_POINT('Origin',(-36.3549260746835,87.7685555885722,124.208423447177));
#40909=CARTESIAN_POINT('',(-39.4252303152106,87.7706425236776,117.791576552823));
#40910=CARTESIAN_POINT('',(-39.4294365974543,87.7658979721433,117.708423447178));
#40911=CARTESIAN_POINT('',(-39.4284260746835,87.7685555885726,124.208423447177));
#40912=CARTESIAN_POINT('Ctrl Pts',(-39.4294365974543,87.7658979721433,117.708423447178));
#40913=CARTESIAN_POINT('Ctrl Pts',(-39.4221061797108,88.57533513631,117.66646598275));
#40914=CARTESIAN_POINT('Ctrl Pts',(-38.6807762323999,90.4123619435266,117.571859010592));
#40915=CARTESIAN_POINT('Ctrl Pts',(-35.5900605330986,91.3135280090206,117.424602530703));
#40916=CARTESIAN_POINT('Ctrl Pts',(-32.9684135319854,89.0660075362686,117.26665400751));
#40917=CARTESIAN_POINT('Ctrl Pts',(-33.417214457214,85.6421268427602,117.108705484318));
#40918=CARTESIAN_POINT('Ctrl Pts',(-36.5295491595418,84.1462144206715,116.950756961126));
#40919=CARTESIAN_POINT('Ctrl Pts',(-39.0249546695335,85.6569303306175,116.817329615412));
#40920=CARTESIAN_POINT('Ctrl Pts',(-39.4228109086881,87.223892024903,116.736551777429));
#40921=CARTESIAN_POINT('Ctrl Pts',(-39.4237037046317,87.7691131821519,116.708423447178));
#40922=CARTESIAN_POINT('Ctrl Pts',(-39.4252303152106,87.7706425236776,117.791576552823));
#40923=CARTESIAN_POINT('Ctrl Pts',(-39.4275239472324,88.1332185492538,117.772847659816));
#40924=CARTESIAN_POINT('Ctrl Pts',(-39.2010476056018,89.5122738774369,117.701469259079));
#40925=CARTESIAN_POINT('Ctrl Pts',(-37.1652521444745,91.3034135494146,117.577441350611));
#40926=CARTESIAN_POINT('Ctrl Pts',(-33.8379853355952,90.3794670115321,117.419492827418));
#40927=CARTESIAN_POINT('Ctrl Pts',(-32.7927521455727,87.0882864937512,117.261544304226));
#40928=CARTESIAN_POINT('Ctrl Pts',(-34.9772337184436,84.4138852747866,117.103595781033));
#40929=CARTESIAN_POINT('Ctrl Pts',(-38.3827274930347,84.7780567344006,116.946939863899));
#40930=CARTESIAN_POINT('Ctrl Pts',(-39.4313302455591,86.7815541779694,116.842933454495));
#40931=CARTESIAN_POINT('Ctrl Pts',(-39.4333759004399,87.7690073305927,116.791576552823));
#40932=CARTESIAN_POINT('Origin',(-36.3549260746835,87.7685555885722,124.208423447177));
#40933=CARTESIAN_POINT('',(-39.4262428442554,87.7660847244363,118.791576552823));
#40934=CARTESIAN_POINT('',(-39.431572198619,87.7706143825889,118.708423447177));
#40935=CARTESIAN_POINT('',(-39.4284260746835,87.7685555885726,124.208423447177));
#40936=CARTESIAN_POINT('Ctrl Pts',(-39.431572198619,87.7706143825889,118.708423447177));
#40937=CARTESIAN_POINT('Ctrl Pts',(-39.4325766336119,87.9004890468128,118.701679203533));
#40938=CARTESIAN_POINT('Ctrl Pts',(-39.3663548371633,89.0432097994101,118.642285452157));
#40939=CARTESIAN_POINT('Ctrl Pts',(-37.936431619208,91.0320949202345,118.53024219305));
#40940=CARTESIAN_POINT('Ctrl Pts',(-34.4867513215705,90.8768946709331,118.372293669858));
#40941=CARTESIAN_POINT('Ctrl Pts',(-32.7308882545334,87.903457911076,118.214345146665));
#40942=CARTESIAN_POINT('Ctrl Pts',(-34.2608300589376,84.8077093184867,118.056396623473));
#40943=CARTESIAN_POINT('Ctrl Pts',(-37.6894250317483,84.3964699888117,117.89844810028));
#40944=CARTESIAN_POINT('Ctrl Pts',(-39.3187091718957,86.3396803259367,117.782457041515));
#40945=CARTESIAN_POINT('Ctrl Pts',(-39.431304611764,87.5596286627648,117.719115490481));
#40946=CARTESIAN_POINT('Ctrl Pts',(-39.4294365974543,87.7658979721433,117.708423447178));
#40947=CARTESIAN_POINT('Ctrl Pts',(-39.4262428442554,87.7660847244363,118.791576552823));
#40948=CARTESIAN_POINT('Ctrl Pts',(-39.4208793710626,88.4656307056646,118.755411372868));
#40949=CARTESIAN_POINT('Ctrl Pts',(-38.8380241483227,90.1916660269312,118.666596685182));
#40950=CARTESIAN_POINT('Ctrl Pts',(-35.9808934930197,91.3757634804708,118.525132489766));
#40951=CARTESIAN_POINT('Ctrl Pts',(-33.1299553615612,89.4272939776113,118.367183966573));
#40952=CARTESIAN_POINT('Ctrl Pts',(-33.2030000939727,85.9748968269957,118.209235443381));
#40953=CARTESIAN_POINT('Ctrl Pts',(-36.1338002509514,84.1487555231856,118.051286920188));
#40954=CARTESIAN_POINT('Ctrl Pts',(-38.8937930554849,85.4319514804777,117.912067290002));
#40955=CARTESIAN_POINT('Ctrl Pts',(-39.4210762304975,87.1139672109572,117.825497167547));
#40956=CARTESIAN_POINT('Ctrl Pts',(-39.4252303152106,87.7706425236776,117.791576552823));
#40957=CARTESIAN_POINT('Origin',(-36.3549260746835,87.7685555885722,124.208423447177));
#40958=CARTESIAN_POINT('',(-39.4334141302851,87.7688891883186,119.791576552823));
#40959=CARTESIAN_POINT('',(-39.4237430776497,87.7692166139293,119.708423447177));
#40960=CARTESIAN_POINT('',(-39.4284260746835,87.7685555885726,124.208423447177));
#40961=CARTESIAN_POINT('Ctrl Pts',(-39.4237430776497,87.7692166139293,119.708423447177));
#40962=CARTESIAN_POINT('Ctrl Pts',(-39.4246536306605,88.2379011782348,119.684242916584));
#40963=CARTESIAN_POINT('Ctrl Pts',(-39.1042498569938,89.725896099133,119.60741287826));
#40964=CARTESIAN_POINT('Ctrl Pts',(-36.7983710620289,91.3678895774169,119.477933332205));
#40965=CARTESIAN_POINT('Ctrl Pts',(-33.583435116581,90.1075054942073,119.319984809013));
#40966=CARTESIAN_POINT('Ctrl Pts',(-32.8813257256701,86.7264666342663,119.16203628582));
#40967=CARTESIAN_POINT('Ctrl Pts',(-35.3286241293906,84.2902581516539,119.004087762628));
#40968=CARTESIAN_POINT('Ctrl Pts',(-38.5622099696999,84.977081421696,118.85288348308));
#40969=CARTESIAN_POINT('Ctrl Pts',(-39.4247354269905,86.8866115094499,118.754328711263));
#40970=CARTESIAN_POINT('Ctrl Pts',(-39.431572198619,87.7706143825889,118.708423447177));
#40971=CARTESIAN_POINT('Ctrl Pts',(-39.4334141302851,87.7688891883186,119.791576552823));
#40972=CARTESIAN_POINT('Ctrl Pts',(-39.4334425751163,87.7871921571854,119.79062459365));
#40973=CARTESIAN_POINT('Ctrl Pts',(-39.4250379322418,88.817741027474,119.737023126747));
#40974=CARTESIAN_POINT('Ctrl Pts',(-38.2826267686962,90.8403332500451,119.630772152113));
#40975=CARTESIAN_POINT('Ctrl Pts',(-34.8365760655942,91.0619524059114,119.47282362892));
#40976=CARTESIAN_POINT('Ctrl Pts',(-32.7671669298757,88.2975486234688,119.314875105728));
#40977=CARTESIAN_POINT('Ctrl Pts',(-33.9506699948071,85.0535230461015,119.156926582536));
#40978=CARTESIAN_POINT('Ctrl Pts',(-37.3140388761979,84.2711348517919,118.998978059343));
#40979=CARTESIAN_POINT('Ctrl Pts',(-39.2368153757742,86.1128345328268,118.877194716105));
#40980=CARTESIAN_POINT('Ctrl Pts',(-39.4286875507449,87.4472270479811,118.808060880599));
#40981=CARTESIAN_POINT('Ctrl Pts',(-39.4262428442554,87.7660847244363,118.791576552823));
#40982=CARTESIAN_POINT('Origin',(-36.3549260746835,87.7685555885722,124.208423447177));
#40983=CARTESIAN_POINT('',(-39.4253674987814,87.7707064726519,120.791576552823));
#40984=CARTESIAN_POINT('',(-39.4292403360613,87.7658718692203,120.708423447177));
#40985=CARTESIAN_POINT('',(-39.4284260746835,87.7685555885726,124.208423447177));
#40986=CARTESIAN_POINT('Ctrl Pts',(-39.4292403360613,87.7658718692203,120.708423447177));
#40987=CARTESIAN_POINT('Ctrl Pts',(-39.4219532081813,88.5688690551349,120.666806629636));
#40988=CARTESIAN_POINT('Ctrl Pts',(-38.6905684542124,90.39950630607,120.572540304363));
#40989=CARTESIAN_POINT('Ctrl Pts',(-35.6128383024604,91.3183647084341,120.42562447136));
#40990=CARTESIAN_POINT('Ctrl Pts',(-32.9768144078577,89.0877262726116,120.267675948167));
#40991=CARTESIAN_POINT('Ctrl Pts',(-33.4036211604692,85.6610333840612,120.109727424975));
#40992=CARTESIAN_POINT('Ctrl Pts',(-36.5062865428284,84.1451680035439,119.951778901782));
#40993=CARTESIAN_POINT('Ctrl Pts',(-39.0177364100551,85.6436455182526,119.818010909183));
#40994=CARTESIAN_POINT('Ctrl Pts',(-39.4226710369536,87.21741027145,119.736892424315));
#40995=CARTESIAN_POINT('Ctrl Pts',(-39.4237430776497,87.7692166139293,119.708423447177));
#40996=CARTESIAN_POINT('Ctrl Pts',(-39.4253674987814,87.7707064726519,120.791576552823));
#40997=CARTESIAN_POINT('Ctrl Pts',(-39.4277028283381,88.1266499402521,120.773188306702));
#40998=CARTESIAN_POINT('Ctrl Pts',(-39.2066380294348,89.4989306286966,120.70215055285));
#40999=CARTESIAN_POINT('Ctrl Pts',(-37.1879238856457,91.2981286694523,120.578463291268));
#41000=CARTESIAN_POINT('Ctrl Pts',(-33.854806193682,90.395578791602,120.420514768075));
#41001=CARTESIAN_POINT('Ctrl Pts',(-32.7884554748253,87.1111711244642,120.262566244883));
#41002=CARTESIAN_POINT('Ctrl Pts',(-34.9557228065637,84.4228016151801,120.10461772169));
#41003=CARTESIAN_POINT('Ctrl Pts',(-38.3708933628005,84.765841706942,119.94762115767));
#41004=CARTESIAN_POINT('Ctrl Pts',(-39.4318693917246,86.7749194370741,119.843274101381));
#41005=CARTESIAN_POINT('Ctrl Pts',(-39.4334141302851,87.7688891883186,119.791576552823));
#41006=CARTESIAN_POINT('Origin',(-36.3549260746835,87.7685555885722,124.208423447177));
#41007=CARTESIAN_POINT('',(-39.4252046869538,87.7655406593158,121.791576552823));
#41008=CARTESIAN_POINT('',(-39.4317255112881,87.7704831500192,121.708423447178));
#41009=CARTESIAN_POINT('',(-39.4284260746835,87.7685555885726,124.208423447177));
#41010=CARTESIAN_POINT('',(-37.1487253572166,84.7993326348266,122.));
#41011=CARTESIAN_POINT('Ctrl Pts',(-37.1487253572165,84.7993326348266,122.));
#41012=CARTESIAN_POINT('Ctrl Pts',(-38.1309639469882,85.0619266872043,121.947350492269));
#41013=CARTESIAN_POINT('Ctrl Pts',(-39.230660578184,86.0996636740867,121.877876009877));
#41014=CARTESIAN_POINT('Ctrl Pts',(-39.427545857155,87.4400648792359,121.808401527484));
#41015=CARTESIAN_POINT('Ctrl Pts',(-39.4252046869538,87.7655406593158,121.791576552823));
#41016=CARTESIAN_POINT('',(-35.5592173411396,84.7942562942729,122.));
#41017=CARTESIAN_POINT('Origin',(-36.3549260746835,87.7685555885722,122.));
#41018=CARTESIAN_POINT('Ctrl Pts',(-35.5592127063049,84.794243972407,122.));
#41019=CARTESIAN_POINT('Ctrl Pts',(-36.5061791034278,84.5433632593369,121.949053726697));
#41020=CARTESIAN_POINT('Ctrl Pts',(-38.5667276181166,84.9982655567983,121.851861542423));
#41021=CARTESIAN_POINT('Ctrl Pts',(-39.4250619982496,86.8802085250801,121.754669358149));
#41022=CARTESIAN_POINT('Ctrl Pts',(-39.4317255112881,87.7704831500192,121.708423447178));
#41023=CARTESIAN_POINT('Origin',(0.,-94.,92.));
#41024=CARTESIAN_POINT('',(0.,-100.,94.));
#41025=CARTESIAN_POINT('',(0.,-100.,90.));
#41026=CARTESIAN_POINT('Ctrl Pts',(8.32667268468867E-16,-100.,94.));
#41027=CARTESIAN_POINT('Ctrl Pts',(0.251131643913751,-100.,94.));
#41028=CARTESIAN_POINT('Ctrl Pts',(0.518997821386429,-99.998956730068,93.9498099158249));
#41029=CARTESIAN_POINT('Ctrl Pts',(1.01175449350969,-99.995185177515,93.7457005158259));
#41030=CARTESIAN_POINT('Ctrl Pts',(1.23664555394558,-99.9925109419644,93.5917815708006));
#41031=CARTESIAN_POINT('Ctrl Pts',(1.591781571759,-99.9874880579221,93.2366455529872));
#41032=CARTESIAN_POINT('Ctrl Pts',(1.74570051630388,-99.9848135889912,93.0117544930956));
#41033=CARTESIAN_POINT('Ctrl Pts',(1.94980991520061,-99.9810415029486,92.5189978221538));
#41034=CARTESIAN_POINT('Ctrl Pts',(2.,-99.9799979995999,92.2511316452692));
#41035=CARTESIAN_POINT('Ctrl Pts',(2.,-99.9799979995999,91.7488683547308));
#41036=CARTESIAN_POINT('Ctrl Pts',(1.94980991520062,-99.9810415029486,91.4810021778462));
#41037=CARTESIAN_POINT('Ctrl Pts',(1.7457005163039,-99.9848135889912,90.9882455069044));
#41038=CARTESIAN_POINT('Ctrl Pts',(1.591781571759,-99.9874880579221,90.7633544470128));
#41039=CARTESIAN_POINT('Ctrl Pts',(1.23664555394558,-99.9925109419644,90.4082184291994));
#41040=CARTESIAN_POINT('Ctrl Pts',(1.01175449350969,-99.995185177515,90.2542994841741));
#41041=CARTESIAN_POINT('Ctrl Pts',(0.518997821386429,-99.998956730068,90.050190084175));
#41042=CARTESIAN_POINT('Ctrl Pts',(0.251131643913753,-100.,90.));
#41043=CARTESIAN_POINT('Ctrl Pts',(2.4980018054066E-15,-100.,90.));
#41044=CARTESIAN_POINT('',(2.00527236333692E-16,-90.,94.));
#41045=CARTESIAN_POINT('',(2.44929359829471E-16,-94.,94.));
#41046=CARTESIAN_POINT('',(-2.,-89.9777750336159,92.));
#41047=CARTESIAN_POINT('Ctrl Pts',(-2.,-89.9777750336159,92.));
#41048=CARTESIAN_POINT('Ctrl Pts',(-2.,-89.9777750336159,91.7488666698803));
#41049=CARTESIAN_POINT('Ctrl Pts',(-1.94980925677131,-89.9789345539658,
91.480999766208));
#41050=CARTESIAN_POINT('Ctrl Pts',(-1.74569936855886,-89.9831259365723,
90.9882435581214));
#41051=CARTESIAN_POINT('Ctrl Pts',(-1.59178067978086,-89.9860976603374,
90.7633535550347));
#41052=CARTESIAN_POINT('Ctrl Pts',(-1.23664644642618,-89.9916787455059,
90.40821932168));
#41053=CARTESIAN_POINT('Ctrl Pts',(-1.01175644254643,-89.9946501491172,
90.2543006320885));
#41054=CARTESIAN_POINT('Ctrl Pts',(-0.519000232590767,-89.9988407998655,
90.0501907423603));
#41055=CARTESIAN_POINT('Ctrl Pts',(-0.251133328053566,-90.,90.));
#41056=CARTESIAN_POINT('Ctrl Pts',(0.251133328053566,-90.,90.));
#41057=CARTESIAN_POINT('Ctrl Pts',(0.519000232590767,-89.9988407998655,
90.0501907423603));
#41058=CARTESIAN_POINT('Ctrl Pts',(1.01175644254643,-89.9946501491172,90.2543006320885));
#41059=CARTESIAN_POINT('Ctrl Pts',(1.23664644642618,-89.9916787455059,90.40821932168));
#41060=CARTESIAN_POINT('Ctrl Pts',(1.59178067978086,-89.9860976603374,90.7633535550347));
#41061=CARTESIAN_POINT('Ctrl Pts',(1.74569936855888,-89.9831259365723,90.9882435581214));
#41062=CARTESIAN_POINT('Ctrl Pts',(1.94980925677131,-89.9789345539658,91.480999766208));
#41063=CARTESIAN_POINT('Ctrl Pts',(2.,-89.9777750336159,91.7488666698804));
#41064=CARTESIAN_POINT('Ctrl Pts',(2.,-89.9777750336159,92.2511333301196));
#41065=CARTESIAN_POINT('Ctrl Pts',(1.94980925677131,-89.9789345539658,92.519000233792));
#41066=CARTESIAN_POINT('Ctrl Pts',(1.74569936855886,-89.9831259365723,93.0117564418786));
#41067=CARTESIAN_POINT('Ctrl Pts',(1.59178067978086,-89.9860976603374,93.2366464449653));
#41068=CARTESIAN_POINT('Ctrl Pts',(1.23664644642618,-89.9916787455059,93.59178067832));
#41069=CARTESIAN_POINT('Ctrl Pts',(1.01175644254643,-89.9946501491172,93.7456993679115));
#41070=CARTESIAN_POINT('Ctrl Pts',(0.519000232590768,-89.9988407998655,
93.9498092576397));
#41071=CARTESIAN_POINT('Ctrl Pts',(0.251133328053567,-90.,94.));
#41072=CARTESIAN_POINT('Ctrl Pts',(3.46944695195361E-16,-90.,94.));
#41073=CARTESIAN_POINT('Ctrl Pts',(1.56125112837913E-16,-90.,94.));
#41074=CARTESIAN_POINT('Ctrl Pts',(-0.251133328053566,-90.,94.));
#41075=CARTESIAN_POINT('Ctrl Pts',(-0.519000232590761,-89.9988407998655,
93.9498092576397));
#41076=CARTESIAN_POINT('Ctrl Pts',(-1.01175644254643,-89.9946501491172,
93.7456993679115));
#41077=CARTESIAN_POINT('Ctrl Pts',(-1.23664644642618,-89.9916787455059,
93.59178067832));
#41078=CARTESIAN_POINT('Ctrl Pts',(-1.59178067978086,-89.9860976603374,
93.2366464449653));
#41079=CARTESIAN_POINT('Ctrl Pts',(-1.74569936855886,-89.9831259365723,
93.0117564418786));
#41080=CARTESIAN_POINT('Ctrl Pts',(-1.94980925677131,-89.9789345539658,
92.519000233792));
#41081=CARTESIAN_POINT('Ctrl Pts',(-2.,-89.9777750336159,92.2511333301196));
#41082=CARTESIAN_POINT('Ctrl Pts',(-2.,-89.9777750336159,92.));
#41083=CARTESIAN_POINT('Ctrl Pts',(-6.93889390390723E-16,-100.,90.));
#41084=CARTESIAN_POINT('Ctrl Pts',(-0.251131643913751,-100.,90.));
#41085=CARTESIAN_POINT('Ctrl Pts',(-0.518997821386429,-99.998956730068,
90.050190084175));
#41086=CARTESIAN_POINT('Ctrl Pts',(-1.01175449350969,-99.995185177515,90.2542994841741));
#41087=CARTESIAN_POINT('Ctrl Pts',(-1.23664555394558,-99.9925109419644,
90.4082184291994));
#41088=CARTESIAN_POINT('Ctrl Pts',(-1.591781571759,-99.9874880579221,90.7633544470128));
#41089=CARTESIAN_POINT('Ctrl Pts',(-1.74570051630388,-99.9848135889912,
90.9882455069044));
#41090=CARTESIAN_POINT('Ctrl Pts',(-1.94980991520061,-99.9810415029486,
91.4810021778462));
#41091=CARTESIAN_POINT('Ctrl Pts',(-2.,-99.9799979995999,91.7488683547308));
#41092=CARTESIAN_POINT('Ctrl Pts',(-2.,-99.9799979995999,92.));
#41093=CARTESIAN_POINT('Ctrl Pts',(-2.,-99.9799979995999,92.2511316452692));
#41094=CARTESIAN_POINT('Ctrl Pts',(-1.94980991520061,-99.9810415029486,
92.5189978221538));
#41095=CARTESIAN_POINT('Ctrl Pts',(-1.74570051630388,-99.9848135889912,
93.0117544930956));
#41096=CARTESIAN_POINT('Ctrl Pts',(-1.591781571759,-99.9874880579221,93.2366455529872));
#41097=CARTESIAN_POINT('Ctrl Pts',(-1.23664555394558,-99.9925109419644,
93.5917815708006));
#41098=CARTESIAN_POINT('Ctrl Pts',(-1.01175449350969,-99.995185177515,93.7457005158259));
#41099=CARTESIAN_POINT('Ctrl Pts',(-0.518997821386429,-99.998956730068,
93.9498099158249));
#41100=CARTESIAN_POINT('Ctrl Pts',(-0.251131643913751,-100.,94.));
#41101=CARTESIAN_POINT('Ctrl Pts',(-7.63278329429795E-16,-100.,94.));
#41102=CARTESIAN_POINT('Origin',(0.,94.,92.));
#41103=CARTESIAN_POINT('',(0.,100.,94.));
#41104=CARTESIAN_POINT('',(0.,100.,90.));
#41105=CARTESIAN_POINT('Ctrl Pts',(2.77555756156289E-16,100.,94.));
#41106=CARTESIAN_POINT('Ctrl Pts',(-0.25113164391375,100.,94.));
#41107=CARTESIAN_POINT('Ctrl Pts',(-0.518997821386429,99.998956730068,93.9498099158249));
#41108=CARTESIAN_POINT('Ctrl Pts',(-1.01175449350969,99.995185177515,93.7457005158259));
#41109=CARTESIAN_POINT('Ctrl Pts',(-1.23664555394558,99.9925109419644,93.5917815708006));
#41110=CARTESIAN_POINT('Ctrl Pts',(-1.591781571759,99.9874880579221,93.2366455529872));
#41111=CARTESIAN_POINT('Ctrl Pts',(-1.74570051630388,99.9848135889912,93.0117544930956));
#41112=CARTESIAN_POINT('Ctrl Pts',(-1.94980991520061,99.9810415029486,92.5189978221538));
#41113=CARTESIAN_POINT('Ctrl Pts',(-2.,99.9799979995999,92.2511316452692));
#41114=CARTESIAN_POINT('Ctrl Pts',(-2.,99.9799979995999,91.7488683547308));
#41115=CARTESIAN_POINT('Ctrl Pts',(-1.94980991520061,99.9810415029486,91.4810021778462));
#41116=CARTESIAN_POINT('Ctrl Pts',(-1.74570051630388,99.9848135889912,90.9882455069044));
#41117=CARTESIAN_POINT('Ctrl Pts',(-1.591781571759,99.9874880579221,90.7633544470128));
#41118=CARTESIAN_POINT('Ctrl Pts',(-1.23664555394558,99.9925109419644,90.4082184291994));
#41119=CARTESIAN_POINT('Ctrl Pts',(-1.01175449350969,99.995185177515,90.2542994841741));
#41120=CARTESIAN_POINT('Ctrl Pts',(-0.518997821386428,99.998956730068,90.050190084175));
#41121=CARTESIAN_POINT('Ctrl Pts',(-0.251131643913752,100.,90.));
#41122=CARTESIAN_POINT('Ctrl Pts',(-2.28983498828939E-15,100.,90.));
#41123=CARTESIAN_POINT('Ctrl Pts',(1.94289029309402E-15,100.,90.));
#41124=CARTESIAN_POINT('Ctrl Pts',(0.251131643913752,100.,90.));
#41125=CARTESIAN_POINT('Ctrl Pts',(0.518997821386421,99.998956730068,90.050190084175));
#41126=CARTESIAN_POINT('Ctrl Pts',(1.01175449350969,99.995185177515,90.2542994841741));
#41127=CARTESIAN_POINT('Ctrl Pts',(1.23664555394558,99.9925109419644,90.4082184291994));
#41128=CARTESIAN_POINT('Ctrl Pts',(1.591781571759,99.9874880579221,90.7633544470128));
#41129=CARTESIAN_POINT('Ctrl Pts',(1.74570051630388,99.9848135889912,90.9882455069044));
#41130=CARTESIAN_POINT('Ctrl Pts',(1.94980991520061,99.9810415029486,91.4810021778462));
#41131=CARTESIAN_POINT('Ctrl Pts',(2.,99.9799979995999,91.7488683547308));
#41132=CARTESIAN_POINT('Ctrl Pts',(2.,99.9799979995999,92.));
#41133=CARTESIAN_POINT('Ctrl Pts',(2.,99.9799979995999,92.2511316452692));
#41134=CARTESIAN_POINT('Ctrl Pts',(1.94980991520061,99.9810415029486,92.5189978221538));
#41135=CARTESIAN_POINT('Ctrl Pts',(1.74570051630388,99.9848135889912,93.0117544930956));
#41136=CARTESIAN_POINT('Ctrl Pts',(1.591781571759,99.9874880579221,93.2366455529872));
#41137=CARTESIAN_POINT('Ctrl Pts',(1.23664555394558,99.9925109419644,93.5917815708006));
#41138=CARTESIAN_POINT('Ctrl Pts',(1.01175449350969,99.995185177515,93.7457005158259));
#41139=CARTESIAN_POINT('Ctrl Pts',(0.518997821386429,99.998956730068,93.9498099158249));
#41140=CARTESIAN_POINT('Ctrl Pts',(0.25113164391375,100.,94.));
#41141=CARTESIAN_POINT('Ctrl Pts',(-3.46944695195361E-17,100.,94.));
#41142=CARTESIAN_POINT('',(7.46965131266386E-16,90.,90.));
#41143=CARTESIAN_POINT('',(2.44929359829471E-16,94.,90.));
#41144=CARTESIAN_POINT('',(2.,89.9777750336159,92.));
#41145=CARTESIAN_POINT('Ctrl Pts',(2.,89.9777750336159,92.));
#41146=CARTESIAN_POINT('Ctrl Pts',(2.,89.9777750336159,91.7488666698804));
#41147=CARTESIAN_POINT('Ctrl Pts',(1.94980925677131,89.9789345539658,91.480999766208));
#41148=CARTESIAN_POINT('Ctrl Pts',(1.74569936855886,89.9831259365723,90.9882435581214));
#41149=CARTESIAN_POINT('Ctrl Pts',(1.59178067978086,89.9860976603374,90.7633535550347));
#41150=CARTESIAN_POINT('Ctrl Pts',(1.23664644642618,89.9916787455059,90.40821932168));
#41151=CARTESIAN_POINT('Ctrl Pts',(1.01175644254643,89.9946501491172,90.2543006320885));
#41152=CARTESIAN_POINT('Ctrl Pts',(0.519000232590768,89.9988407998655,90.0501907423603));
#41153=CARTESIAN_POINT('Ctrl Pts',(0.251133328053566,90.,90.));
#41154=CARTESIAN_POINT('Ctrl Pts',(-2.08166817117217E-16,90.,90.));
#41155=CARTESIAN_POINT('Ctrl Pts',(1.2490009027033E-15,90.,90.));
#41156=CARTESIAN_POINT('Ctrl Pts',(-0.251133328053565,90.,90.));
#41157=CARTESIAN_POINT('Ctrl Pts',(-0.519000232590767,89.9988407998655,
90.0501907423603));
#41158=CARTESIAN_POINT('Ctrl Pts',(-1.01175644254643,89.9946501491172,90.2543006320885));
#41159=CARTESIAN_POINT('Ctrl Pts',(-1.23664644642618,89.9916787455059,90.40821932168));
#41160=CARTESIAN_POINT('Ctrl Pts',(-1.59178067978086,89.9860976603374,90.7633535550347));
#41161=CARTESIAN_POINT('Ctrl Pts',(-1.74569936855888,89.9831259365723,90.9882435581214));
#41162=CARTESIAN_POINT('Ctrl Pts',(-1.94980925677131,89.9789345539658,91.480999766208));
#41163=CARTESIAN_POINT('Ctrl Pts',(-2.,89.9777750336159,91.7488666698804));
#41164=CARTESIAN_POINT('Ctrl Pts',(-2.,89.9777750336159,92.2511333301196));
#41165=CARTESIAN_POINT('Ctrl Pts',(-1.94980925677131,89.9789345539658,92.519000233792));
#41166=CARTESIAN_POINT('Ctrl Pts',(-1.74569936855886,89.9831259365723,93.0117564418786));
#41167=CARTESIAN_POINT('Ctrl Pts',(-1.59178067978086,89.9860976603374,93.2366464449653));
#41168=CARTESIAN_POINT('Ctrl Pts',(-1.23664644642618,89.9916787455059,93.59178067832));
#41169=CARTESIAN_POINT('Ctrl Pts',(-1.01175644254643,89.9946501491172,93.7456993679115));
#41170=CARTESIAN_POINT('Ctrl Pts',(-0.519000232590768,89.9988407998655,
93.9498092576397));
#41171=CARTESIAN_POINT('Ctrl Pts',(-0.251133328053566,90.,94.));
#41172=CARTESIAN_POINT('Ctrl Pts',(0.251133328053566,90.,94.));
#41173=CARTESIAN_POINT('Ctrl Pts',(0.519000232590767,89.9988407998655,93.9498092576397));
#41174=CARTESIAN_POINT('Ctrl Pts',(1.01175644254643,89.9946501491172,93.7456993679115));
#41175=CARTESIAN_POINT('Ctrl Pts',(1.23664644642618,89.9916787455059,93.59178067832));
#41176=CARTESIAN_POINT('Ctrl Pts',(1.59178067978086,89.9860976603374,93.2366464449653));
#41177=CARTESIAN_POINT('Ctrl Pts',(1.74569936855886,89.9831259365723,93.0117564418786));
#41178=CARTESIAN_POINT('Ctrl Pts',(1.94980925677131,89.9789345539658,92.519000233792));
#41179=CARTESIAN_POINT('Ctrl Pts',(2.,89.9777750336159,92.2511333301196));
#41180=CARTESIAN_POINT('Ctrl Pts',(2.,89.9777750336159,92.));
#41181=CARTESIAN_POINT('Origin',(-94.,0.,92.));
#41182=CARTESIAN_POINT('',(-100.,0.,94.));
#41183=CARTESIAN_POINT('',(-100.,0.,90.));
#41184=CARTESIAN_POINT('Ctrl Pts',(-100.,-8.32667268468867E-16,94.));
#41185=CARTESIAN_POINT('Ctrl Pts',(-100.,-0.251131643913751,94.));
#41186=CARTESIAN_POINT('Ctrl Pts',(-99.998956730068,-0.518997821386429,
93.9498099158249));
#41187=CARTESIAN_POINT('Ctrl Pts',(-99.995185177515,-1.01175449350969,93.7457005158259));
#41188=CARTESIAN_POINT('Ctrl Pts',(-99.9925109419644,-1.23664555394558,
93.5917815708006));
#41189=CARTESIAN_POINT('Ctrl Pts',(-99.9874880579221,-1.591781571759,93.2366455529872));
#41190=CARTESIAN_POINT('Ctrl Pts',(-99.9848135889912,-1.74570051630388,
93.0117544930956));
#41191=CARTESIAN_POINT('Ctrl Pts',(-99.9810415029486,-1.94980991520061,
92.5189978221538));
#41192=CARTESIAN_POINT('Ctrl Pts',(-99.9799979995999,-2.,92.2511316452692));
#41193=CARTESIAN_POINT('Ctrl Pts',(-99.9799979995999,-2.,91.7488683547308));
#41194=CARTESIAN_POINT('Ctrl Pts',(-99.9810415029486,-1.94980991520061,
91.4810021778462));
#41195=CARTESIAN_POINT('Ctrl Pts',(-99.9848135889912,-1.74570051630388,
90.9882455069044));
#41196=CARTESIAN_POINT('Ctrl Pts',(-99.9874880579221,-1.591781571759,90.7633544470128));
#41197=CARTESIAN_POINT('Ctrl Pts',(-99.9925109419644,-1.23664555394558,
90.4082184291994));
#41198=CARTESIAN_POINT('Ctrl Pts',(-99.995185177515,-1.01175449350969,90.2542994841741));
#41199=CARTESIAN_POINT('Ctrl Pts',(-99.998956730068,-0.518997821386429,
90.050190084175));
#41200=CARTESIAN_POINT('Ctrl Pts',(-100.,-0.251131643913753,90.));
#41201=CARTESIAN_POINT('Ctrl Pts',(-100.,-2.4980018054066E-15,90.));
#41202=CARTESIAN_POINT('',(-99.9799979995999,2.,92.));
#41203=CARTESIAN_POINT('Ctrl Pts',(-99.9799979995999,2.,92.));
#41204=CARTESIAN_POINT('Ctrl Pts',(-99.9799979995999,2.,92.2511316452692));
#41205=CARTESIAN_POINT('Ctrl Pts',(-99.9810415029486,1.94980991520061,92.5189978221538));
#41206=CARTESIAN_POINT('Ctrl Pts',(-99.9848135889912,1.74570051630388,93.0117544930956));
#41207=CARTESIAN_POINT('Ctrl Pts',(-99.9874880579221,1.591781571759,93.2366455529872));
#41208=CARTESIAN_POINT('Ctrl Pts',(-99.9925109419644,1.23664555394558,93.5917815708006));
#41209=CARTESIAN_POINT('Ctrl Pts',(-99.995185177515,1.01175449350969,93.7457005158259));
#41210=CARTESIAN_POINT('Ctrl Pts',(-99.998956730068,0.518997821386429,93.9498099158249));
#41211=CARTESIAN_POINT('Ctrl Pts',(-100.,0.251131643913751,94.));
#41212=CARTESIAN_POINT('Ctrl Pts',(-100.,2.42861286636753E-16,94.));
#41213=CARTESIAN_POINT('',(-89.9777750336159,2.,92.));
#41214=CARTESIAN_POINT('',(-94.,2.,92.));
#41215=CARTESIAN_POINT('',(-90.,-5.47621612664355E-15,94.));
#41216=CARTESIAN_POINT('Ctrl Pts',(-90.,3.46944695195361E-16,94.));
#41217=CARTESIAN_POINT('Ctrl Pts',(-90.,0.251133328053567,94.));
#41218=CARTESIAN_POINT('Ctrl Pts',(-89.9988407998655,0.519000232590767,
93.9498092576397));
#41219=CARTESIAN_POINT('Ctrl Pts',(-89.9946501491172,1.01175644254643,93.7456993679115));
#41220=CARTESIAN_POINT('Ctrl Pts',(-89.9916787455059,1.23664644642618,93.59178067832));
#41221=CARTESIAN_POINT('Ctrl Pts',(-89.9860976603374,1.59178067978086,93.2366464449653));
#41222=CARTESIAN_POINT('Ctrl Pts',(-89.9831259365723,1.74569936855886,93.0117564418786));
#41223=CARTESIAN_POINT('Ctrl Pts',(-89.9789345539658,1.94980925677131,92.519000233792));
#41224=CARTESIAN_POINT('Ctrl Pts',(-89.9777750336159,2.,92.2511333301196));
#41225=CARTESIAN_POINT('Ctrl Pts',(-89.9777750336159,2.,92.));
#41226=CARTESIAN_POINT('',(-90.,-5.16396590096773E-15,90.));
#41227=CARTESIAN_POINT('Ctrl Pts',(-90.,6.93889390390723E-16,90.));
#41228=CARTESIAN_POINT('Ctrl Pts',(-90.,-0.251133328053566,90.));
#41229=CARTESIAN_POINT('Ctrl Pts',(-89.9988407998655,-0.519000232590767,
90.0501907423603));
#41230=CARTESIAN_POINT('Ctrl Pts',(-89.9946501491172,-1.01175644254643,
90.2543006320885));
#41231=CARTESIAN_POINT('Ctrl Pts',(-89.9916787455059,-1.23664644642618,
90.40821932168));
#41232=CARTESIAN_POINT('Ctrl Pts',(-89.9860976603374,-1.59178067978086,
90.7633535550347));
#41233=CARTESIAN_POINT('Ctrl Pts',(-89.9831259365723,-1.74569936855888,
90.9882435581214));
#41234=CARTESIAN_POINT('Ctrl Pts',(-89.9789345539658,-1.94980925677131,
91.480999766208));
#41235=CARTESIAN_POINT('Ctrl Pts',(-89.9777750336159,-2.,91.7488666698804));
#41236=CARTESIAN_POINT('Ctrl Pts',(-89.9777750336159,-2.,92.2511333301196));
#41237=CARTESIAN_POINT('Ctrl Pts',(-89.9789345539658,-1.94980925677131,
92.519000233792));
#41238=CARTESIAN_POINT('Ctrl Pts',(-89.9831259365723,-1.74569936855886,
93.0117564418786));
#41239=CARTESIAN_POINT('Ctrl Pts',(-89.9860976603374,-1.59178067978086,
93.2366464449653));
#41240=CARTESIAN_POINT('Ctrl Pts',(-89.9916787455059,-1.23664644642618,
93.59178067832));
#41241=CARTESIAN_POINT('Ctrl Pts',(-89.9946501491172,-1.01175644254643,
93.7456993679115));
#41242=CARTESIAN_POINT('Ctrl Pts',(-89.9988407998655,-0.519000232590767,
93.9498092576397));
#41243=CARTESIAN_POINT('Ctrl Pts',(-90.,-0.251133328053567,94.));
#41244=CARTESIAN_POINT('Ctrl Pts',(-90.,-4.16333634234434E-16,94.));
#41245=CARTESIAN_POINT('Ctrl Pts',(-89.9777750336159,2.,92.));
#41246=CARTESIAN_POINT('Ctrl Pts',(-89.9777750336159,2.,91.7488666698804));
#41247=CARTESIAN_POINT('Ctrl Pts',(-89.9789345539658,1.94980925677131,91.480999766208));
#41248=CARTESIAN_POINT('Ctrl Pts',(-89.9831259365723,1.74569936855886,90.9882435581214));
#41249=CARTESIAN_POINT('Ctrl Pts',(-89.9860976603374,1.59178067978086,90.7633535550347));
#41250=CARTESIAN_POINT('Ctrl Pts',(-89.9916787455059,1.23664644642618,90.40821932168));
#41251=CARTESIAN_POINT('Ctrl Pts',(-89.9946501491172,1.01175644254643,90.2543006320885));
#41252=CARTESIAN_POINT('Ctrl Pts',(-89.9988407998655,0.519000232590768,
90.0501907423603));
#41253=CARTESIAN_POINT('Ctrl Pts',(-90.,0.251133328053566,90.));
#41254=CARTESIAN_POINT('Ctrl Pts',(-90.,-4.85722573273506E-16,90.));
#41255=CARTESIAN_POINT('Ctrl Pts',(-100.,3.12250225675825E-16,90.));
#41256=CARTESIAN_POINT('Ctrl Pts',(-100.,0.25113164391375,90.));
#41257=CARTESIAN_POINT('Ctrl Pts',(-99.998956730068,0.518997821386421,90.050190084175));
#41258=CARTESIAN_POINT('Ctrl Pts',(-99.995185177515,1.01175449350969,90.2542994841741));
#41259=CARTESIAN_POINT('Ctrl Pts',(-99.9925109419644,1.23664555394558,90.4082184291994));
#41260=CARTESIAN_POINT('Ctrl Pts',(-99.9874880579221,1.591781571759,90.7633544470128));
#41261=CARTESIAN_POINT('Ctrl Pts',(-99.9848135889912,1.74570051630388,90.9882455069044));
#41262=CARTESIAN_POINT('Ctrl Pts',(-99.9810415029486,1.94980991520061,91.4810021778462));
#41263=CARTESIAN_POINT('Ctrl Pts',(-99.9799979995999,2.,91.7488683547308));
#41264=CARTESIAN_POINT('Ctrl Pts',(-99.9799979995999,2.,92.));
#41265=CARTESIAN_POINT('Origin',(94.,0.,92.));
#41266=CARTESIAN_POINT('',(100.,0.,94.));
#41267=CARTESIAN_POINT('',(100.,0.,90.));
#41268=CARTESIAN_POINT('Ctrl Pts',(100.,8.32667268468867E-16,94.));
#41269=CARTESIAN_POINT('Ctrl Pts',(100.,0.251131643913751,94.));
#41270=CARTESIAN_POINT('Ctrl Pts',(99.998956730068,0.518997821386429,93.9498099158249));
#41271=CARTESIAN_POINT('Ctrl Pts',(99.995185177515,1.01175449350969,93.7457005158259));
#41272=CARTESIAN_POINT('Ctrl Pts',(99.9925109419644,1.23664555394558,93.5917815708006));
#41273=CARTESIAN_POINT('Ctrl Pts',(99.9874880579221,1.591781571759,93.2366455529872));
#41274=CARTESIAN_POINT('Ctrl Pts',(99.9848135889912,1.74570051630388,93.0117544930956));
#41275=CARTESIAN_POINT('Ctrl Pts',(99.9810415029486,1.94980991520061,92.5189978221538));
#41276=CARTESIAN_POINT('Ctrl Pts',(99.9799979995999,2.,92.2511316452692));
#41277=CARTESIAN_POINT('Ctrl Pts',(99.9799979995999,2.,91.7488683547308));
#41278=CARTESIAN_POINT('Ctrl Pts',(99.9810415029486,1.94980991520061,91.4810021778462));
#41279=CARTESIAN_POINT('Ctrl Pts',(99.9848135889912,1.74570051630388,90.9882455069044));
#41280=CARTESIAN_POINT('Ctrl Pts',(99.9874880579221,1.591781571759,90.7633544470128));
#41281=CARTESIAN_POINT('Ctrl Pts',(99.9925109419644,1.23664555394558,90.4082184291994));
#41282=CARTESIAN_POINT('Ctrl Pts',(99.995185177515,1.01175449350969,90.2542994841741));
#41283=CARTESIAN_POINT('Ctrl Pts',(99.998956730068,0.518997821386429,90.050190084175));
#41284=CARTESIAN_POINT('Ctrl Pts',(100.,0.251131643913753,90.));
#41285=CARTESIAN_POINT('Ctrl Pts',(100.,2.4980018054066E-15,90.));
#41286=CARTESIAN_POINT('',(99.9799979995999,-2.,92.));
#41287=CARTESIAN_POINT('Ctrl Pts',(99.9799979995999,-2.,92.));
#41288=CARTESIAN_POINT('Ctrl Pts',(99.9799979995999,-2.,92.2511316452692));
#41289=CARTESIAN_POINT('Ctrl Pts',(99.9810415029486,-1.94980991520061,92.5189978221538));
#41290=CARTESIAN_POINT('Ctrl Pts',(99.9848135889912,-1.74570051630388,93.0117544930956));
#41291=CARTESIAN_POINT('Ctrl Pts',(99.9874880579221,-1.591781571759,93.2366455529872));
#41292=CARTESIAN_POINT('Ctrl Pts',(99.9925109419644,-1.23664555394558,93.5917815708006));
#41293=CARTESIAN_POINT('Ctrl Pts',(99.995185177515,-1.01175449350969,93.7457005158259));
#41294=CARTESIAN_POINT('Ctrl Pts',(99.998956730068,-0.518997821386429,93.9498099158249));
#41295=CARTESIAN_POINT('Ctrl Pts',(100.,-0.251131643913751,94.));
#41296=CARTESIAN_POINT('Ctrl Pts',(100.,-2.42861286636753E-16,94.));
#41297=CARTESIAN_POINT('',(89.9777750336159,-2.,92.));
#41298=CARTESIAN_POINT('',(94.,-2.,92.));
#41299=CARTESIAN_POINT('Ctrl Pts',(89.9777750336159,-2.,92.));
#41300=CARTESIAN_POINT('Ctrl Pts',(89.9777750336159,-2.,91.7488666698804));
#41301=CARTESIAN_POINT('Ctrl Pts',(89.9789345539658,-1.94980925677131,91.480999766208));
#41302=CARTESIAN_POINT('Ctrl Pts',(89.9831259365723,-1.74569936855886,90.9882435581214));
#41303=CARTESIAN_POINT('Ctrl Pts',(89.9860976603374,-1.59178067978086,90.7633535550347));
#41304=CARTESIAN_POINT('Ctrl Pts',(89.9916787455059,-1.23664644642618,90.40821932168));
#41305=CARTESIAN_POINT('Ctrl Pts',(89.9946501491172,-1.01175644254643,90.2543006320885));
#41306=CARTESIAN_POINT('Ctrl Pts',(89.9988407998655,-0.519000232590768,
90.0501907423603));
#41307=CARTESIAN_POINT('Ctrl Pts',(90.,-0.251133328053566,90.));
#41308=CARTESIAN_POINT('Ctrl Pts',(90.,0.251133328053566,90.));
#41309=CARTESIAN_POINT('Ctrl Pts',(89.9988407998655,0.519000232590767,90.0501907423603));
#41310=CARTESIAN_POINT('Ctrl Pts',(89.9946501491172,1.01175644254643,90.2543006320885));
#41311=CARTESIAN_POINT('Ctrl Pts',(89.9916787455059,1.23664644642618,90.40821932168));
#41312=CARTESIAN_POINT('Ctrl Pts',(89.9860976603374,1.59178067978086,90.7633535550347));
#41313=CARTESIAN_POINT('Ctrl Pts',(89.9831259365723,1.74569936855888,90.9882435581214));
#41314=CARTESIAN_POINT('Ctrl Pts',(89.9789345539658,1.94980925677131,91.480999766208));
#41315=CARTESIAN_POINT('Ctrl Pts',(89.9777750336159,2.,91.7488666698804));
#41316=CARTESIAN_POINT('Ctrl Pts',(89.9777750336159,2.,92.2511333301196));
#41317=CARTESIAN_POINT('Ctrl Pts',(89.9789345539658,1.94980925677131,92.519000233792));
#41318=CARTESIAN_POINT('Ctrl Pts',(89.9831259365723,1.74569936855886,93.0117564418786));
#41319=CARTESIAN_POINT('Ctrl Pts',(89.9860976603374,1.59178067978086,93.2366464449653));
#41320=CARTESIAN_POINT('Ctrl Pts',(89.9916787455059,1.23664644642618,93.59178067832));
#41321=CARTESIAN_POINT('Ctrl Pts',(89.9946501491172,1.01175644254643,93.7456993679115));
#41322=CARTESIAN_POINT('Ctrl Pts',(89.9988407998655,0.519000232590767,93.9498092576397));
#41323=CARTESIAN_POINT('Ctrl Pts',(90.,0.251133328053566,94.));
#41324=CARTESIAN_POINT('Ctrl Pts',(90.,-0.251133328053566,94.));
#41325=CARTESIAN_POINT('Ctrl Pts',(89.9988407998655,-0.519000232590767,
93.9498092576397));
#41326=CARTESIAN_POINT('Ctrl Pts',(89.9946501491172,-1.01175644254643,93.7456993679115));
#41327=CARTESIAN_POINT('Ctrl Pts',(89.9916787455059,-1.23664644642618,93.59178067832));
#41328=CARTESIAN_POINT('Ctrl Pts',(89.9860976603374,-1.59178067978086,93.2366464449653));
#41329=CARTESIAN_POINT('Ctrl Pts',(89.9831259365723,-1.74569936855886,93.0117564418786));
#41330=CARTESIAN_POINT('Ctrl Pts',(89.9789345539658,-1.94980925677131,92.519000233792));
#41331=CARTESIAN_POINT('Ctrl Pts',(89.9777750336159,-2.,92.2511333301196));
#41332=CARTESIAN_POINT('Ctrl Pts',(89.9777750336159,-2.,92.));
#41333=CARTESIAN_POINT('Ctrl Pts',(100.,-3.12250225675825E-16,90.));
#41334=CARTESIAN_POINT('Ctrl Pts',(100.,-0.25113164391375,90.));
#41335=CARTESIAN_POINT('Ctrl Pts',(99.998956730068,-0.518997821386421,90.050190084175));
#41336=CARTESIAN_POINT('Ctrl Pts',(99.995185177515,-1.01175449350969,90.2542994841741));
#41337=CARTESIAN_POINT('Ctrl Pts',(99.9925109419644,-1.23664555394558,90.4082184291994));
#41338=CARTESIAN_POINT('Ctrl Pts',(99.9874880579221,-1.591781571759,90.7633544470128));
#41339=CARTESIAN_POINT('Ctrl Pts',(99.9848135889912,-1.74570051630388,90.9882455069044));
#41340=CARTESIAN_POINT('Ctrl Pts',(99.9810415029486,-1.94980991520061,91.4810021778462));
#41341=CARTESIAN_POINT('Ctrl Pts',(99.9799979995999,-2.,91.7488683547308));
#41342=CARTESIAN_POINT('Ctrl Pts',(99.9799979995999,-2.,92.));
#41343=CARTESIAN_POINT('Origin',(0.,-94.,70.));
#41344=CARTESIAN_POINT('',(0.,-100.,72.));
#41345=CARTESIAN_POINT('',(0.,-100.,68.));
#41346=CARTESIAN_POINT('Ctrl Pts',(-1.73472347597681E-15,-100.,72.));
#41347=CARTESIAN_POINT('Ctrl Pts',(0.251131643913749,-100.,72.));
#41348=CARTESIAN_POINT('Ctrl Pts',(0.51899782138642,-99.998956730068,71.949809915825));
#41349=CARTESIAN_POINT('Ctrl Pts',(1.01175449350968,-99.995185177515,71.7457005158259));
#41350=CARTESIAN_POINT('Ctrl Pts',(1.23664555394557,-99.9925109419644,71.5917815708006));
#41351=CARTESIAN_POINT('Ctrl Pts',(1.591781571759,-99.9874880579221,71.2366455529872));
#41352=CARTESIAN_POINT('Ctrl Pts',(1.74570051630387,-99.9848135889912,71.0117544930956));
#41353=CARTESIAN_POINT('Ctrl Pts',(1.94980991520061,-99.9810415029486,70.5189978221538));
#41354=CARTESIAN_POINT('Ctrl Pts',(2.,-99.9799979995999,70.2511316452692));
#41355=CARTESIAN_POINT('Ctrl Pts',(2.,-99.9799979995999,69.7488683547308));
#41356=CARTESIAN_POINT('Ctrl Pts',(1.94980991520061,-99.9810415029486,69.4810021778462));
#41357=CARTESIAN_POINT('Ctrl Pts',(1.74570051630388,-99.9848135889912,68.9882455069044));
#41358=CARTESIAN_POINT('Ctrl Pts',(1.591781571759,-99.9874880579221,68.7633544470128));
#41359=CARTESIAN_POINT('Ctrl Pts',(1.23664555394557,-99.9925109419644,68.4082184291994));
#41360=CARTESIAN_POINT('Ctrl Pts',(1.01175449350969,-99.995185177515,68.2542994841741));
#41361=CARTESIAN_POINT('Ctrl Pts',(0.518997821386427,-99.998956730068,68.0501900841751));
#41362=CARTESIAN_POINT('Ctrl Pts',(0.251131643913751,-100.,68.));
#41363=CARTESIAN_POINT('Ctrl Pts',(2.77555756156289E-16,-100.,68.));
#41364=CARTESIAN_POINT('',(-4.32646832397843E-16,-90.,72.));
#41365=CARTESIAN_POINT('',(2.44929359829471E-16,-94.,72.));
#41366=CARTESIAN_POINT('',(-2.,-89.9777750336159,70.));
#41367=CARTESIAN_POINT('Ctrl Pts',(-2.,-89.9777750336159,70.));
#41368=CARTESIAN_POINT('Ctrl Pts',(-2.,-89.9777750336159,69.7488666698804));
#41369=CARTESIAN_POINT('Ctrl Pts',(-1.9498092567713,-89.9789345539658,69.480999766208));
#41370=CARTESIAN_POINT('Ctrl Pts',(-1.74569936855887,-89.9831259365723,
68.9882435581214));
#41371=CARTESIAN_POINT('Ctrl Pts',(-1.59178067978086,-89.9860976603374,
68.7633535550347));
#41372=CARTESIAN_POINT('Ctrl Pts',(-1.23664644642618,-89.9916787455059,
68.40821932168));
#41373=CARTESIAN_POINT('Ctrl Pts',(-1.01175644254643,-89.9946501491172,
68.2543006320885));
#41374=CARTESIAN_POINT('Ctrl Pts',(-0.519000232590759,-89.9988407998655,
68.0501907423603));
#41375=CARTESIAN_POINT('Ctrl Pts',(-0.251133328053567,-90.,68.));
#41376=CARTESIAN_POINT('Ctrl Pts',(0.251133328053567,-90.,68.));
#41377=CARTESIAN_POINT('Ctrl Pts',(0.519000232590759,-89.9988407998655,
68.0501907423603));
#41378=CARTESIAN_POINT('Ctrl Pts',(1.01175644254643,-89.9946501491172,68.2543006320885));
#41379=CARTESIAN_POINT('Ctrl Pts',(1.23664644642618,-89.9916787455059,68.40821932168));
#41380=CARTESIAN_POINT('Ctrl Pts',(1.59178067978086,-89.9860976603374,68.7633535550347));
#41381=CARTESIAN_POINT('Ctrl Pts',(1.74569936855887,-89.9831259365723,68.9882435581214));
#41382=CARTESIAN_POINT('Ctrl Pts',(1.94980925677131,-89.9789345539658,69.480999766208));
#41383=CARTESIAN_POINT('Ctrl Pts',(2.,-89.9777750336159,69.7488666698804));
#41384=CARTESIAN_POINT('Ctrl Pts',(2.,-89.9777750336159,70.2511333301196));
#41385=CARTESIAN_POINT('Ctrl Pts',(1.9498092567713,-89.9789345539658,70.519000233792));
#41386=CARTESIAN_POINT('Ctrl Pts',(1.74569936855887,-89.9831259365723,71.0117564418786));
#41387=CARTESIAN_POINT('Ctrl Pts',(1.59178067978086,-89.9860976603374,71.2366464449653));
#41388=CARTESIAN_POINT('Ctrl Pts',(1.23664644642618,-89.9916787455059,71.59178067832));
#41389=CARTESIAN_POINT('Ctrl Pts',(1.01175644254643,-89.9946501491172,71.7456993679115));
#41390=CARTESIAN_POINT('Ctrl Pts',(0.519000232590759,-89.9988407998655,
71.9498092576397));
#41391=CARTESIAN_POINT('Ctrl Pts',(0.251133328053568,-90.,72.));
#41392=CARTESIAN_POINT('Ctrl Pts',(1.31838984174237E-15,-90.,72.));
#41393=CARTESIAN_POINT('Ctrl Pts',(-9.71445146547012E-16,-90.,72.));
#41394=CARTESIAN_POINT('Ctrl Pts',(-0.251133328053568,-90.,72.));
#41395=CARTESIAN_POINT('Ctrl Pts',(-0.519000232590759,-89.9988407998655,
71.9498092576397));
#41396=CARTESIAN_POINT('Ctrl Pts',(-1.01175644254643,-89.9946501491172,
71.7456993679115));
#41397=CARTESIAN_POINT('Ctrl Pts',(-1.23664644642618,-89.9916787455059,
71.59178067832));
#41398=CARTESIAN_POINT('Ctrl Pts',(-1.59178067978086,-89.9860976603374,
71.2366464449653));
#41399=CARTESIAN_POINT('Ctrl Pts',(-1.74569936855887,-89.9831259365723,
71.0117564418786));
#41400=CARTESIAN_POINT('Ctrl Pts',(-1.9498092567713,-89.9789345539658,70.519000233792));
#41401=CARTESIAN_POINT('Ctrl Pts',(-2.,-89.9777750336159,70.2511333301196));
#41402=CARTESIAN_POINT('Ctrl Pts',(-2.,-89.9777750336159,70.));
#41403=CARTESIAN_POINT('Ctrl Pts',(6.93889390390723E-16,-100.,68.));
#41404=CARTESIAN_POINT('Ctrl Pts',(-0.25113164391375,-100.,68.));
#41405=CARTESIAN_POINT('Ctrl Pts',(-0.518997821386426,-99.998956730068,
68.0501900841751));
#41406=CARTESIAN_POINT('Ctrl Pts',(-1.01175449350968,-99.995185177515,68.2542994841741));
#41407=CARTESIAN_POINT('Ctrl Pts',(-1.23664555394557,-99.9925109419644,
68.4082184291994));
#41408=CARTESIAN_POINT('Ctrl Pts',(-1.591781571759,-99.9874880579221,68.7633544470128));
#41409=CARTESIAN_POINT('Ctrl Pts',(-1.74570051630388,-99.9848135889912,
68.9882455069044));
#41410=CARTESIAN_POINT('Ctrl Pts',(-1.94980991520061,-99.9810415029486,
69.4810021778462));
#41411=CARTESIAN_POINT('Ctrl Pts',(-2.,-99.9799979995999,69.7488683547308));
#41412=CARTESIAN_POINT('Ctrl Pts',(-2.,-99.9799979995999,70.));
#41413=CARTESIAN_POINT('Ctrl Pts',(-2.,-99.9799979995999,70.2511316452692));
#41414=CARTESIAN_POINT('Ctrl Pts',(-1.94980991520061,-99.9810415029486,
70.5189978221538));
#41415=CARTESIAN_POINT('Ctrl Pts',(-1.74570051630388,-99.9848135889912,
71.0117544930956));
#41416=CARTESIAN_POINT('Ctrl Pts',(-1.591781571759,-99.9874880579221,71.2366455529872));
#41417=CARTESIAN_POINT('Ctrl Pts',(-1.23664555394557,-99.9925109419644,
71.5917815708006));
#41418=CARTESIAN_POINT('Ctrl Pts',(-1.01175449350968,-99.995185177515,71.7457005158259));
#41419=CARTESIAN_POINT('Ctrl Pts',(-0.51899782138642,-99.998956730068,71.949809915825));
#41420=CARTESIAN_POINT('Ctrl Pts',(-0.251131643913751,-100.,72.));
#41421=CARTESIAN_POINT('Ctrl Pts',(-6.93889390390723E-17,-100.,72.));
#41422=CARTESIAN_POINT('Origin',(0.,94.,70.));
#41423=CARTESIAN_POINT('',(0.,100.,72.));
#41424=CARTESIAN_POINT('',(0.,100.,68.));
#41425=CARTESIAN_POINT('Ctrl Pts',(1.45716771982052E-15,100.,72.));
#41426=CARTESIAN_POINT('Ctrl Pts',(-0.25113164391375,100.,72.));
#41427=CARTESIAN_POINT('Ctrl Pts',(-0.51899782138642,99.998956730068,71.949809915825));
#41428=CARTESIAN_POINT('Ctrl Pts',(-1.01175449350968,99.995185177515,71.7457005158259));
#41429=CARTESIAN_POINT('Ctrl Pts',(-1.23664555394557,99.9925109419644,71.5917815708006));
#41430=CARTESIAN_POINT('Ctrl Pts',(-1.591781571759,99.9874880579221,71.2366455529872));
#41431=CARTESIAN_POINT('Ctrl Pts',(-1.74570051630387,99.9848135889912,71.0117544930956));
#41432=CARTESIAN_POINT('Ctrl Pts',(-1.94980991520061,99.9810415029486,70.5189978221538));
#41433=CARTESIAN_POINT('Ctrl Pts',(-2.,99.9799979995999,70.2511316452692));
#41434=CARTESIAN_POINT('Ctrl Pts',(-2.,99.9799979995999,69.7488683547308));
#41435=CARTESIAN_POINT('Ctrl Pts',(-1.94980991520061,99.9810415029486,69.4810021778462));
#41436=CARTESIAN_POINT('Ctrl Pts',(-1.74570051630388,99.9848135889912,68.9882455069044));
#41437=CARTESIAN_POINT('Ctrl Pts',(-1.591781571759,99.9874880579221,68.7633544470128));
#41438=CARTESIAN_POINT('Ctrl Pts',(-1.23664555394558,99.9925109419644,68.4082184291994));
#41439=CARTESIAN_POINT('Ctrl Pts',(-1.01175449350969,99.995185177515,68.2542994841741));
#41440=CARTESIAN_POINT('Ctrl Pts',(-0.518997821386427,99.998956730068,68.0501900841751));
#41441=CARTESIAN_POINT('Ctrl Pts',(-0.251131643913751,100.,68.));
#41442=CARTESIAN_POINT('Ctrl Pts',(1.38777878078145E-16,100.,68.));
#41443=CARTESIAN_POINT('Ctrl Pts',(-8.32667268468867E-16,100.,68.));
#41444=CARTESIAN_POINT('Ctrl Pts',(0.25113164391375,100.,68.));
#41445=CARTESIAN_POINT('Ctrl Pts',(0.518997821386427,99.998956730068,68.0501900841751));
#41446=CARTESIAN_POINT('Ctrl Pts',(1.01175449350969,99.995185177515,68.2542994841741));
#41447=CARTESIAN_POINT('Ctrl Pts',(1.23664555394558,99.9925109419644,68.4082184291994));
#41448=CARTESIAN_POINT('Ctrl Pts',(1.591781571759,99.9874880579221,68.7633544470128));
#41449=CARTESIAN_POINT('Ctrl Pts',(1.74570051630388,99.9848135889912,68.9882455069044));
#41450=CARTESIAN_POINT('Ctrl Pts',(1.94980991520061,99.9810415029486,69.4810021778462));
#41451=CARTESIAN_POINT('Ctrl Pts',(2.,99.9799979995999,69.7488683547308));
#41452=CARTESIAN_POINT('Ctrl Pts',(2.,99.9799979995999,70.));
#41453=CARTESIAN_POINT('Ctrl Pts',(2.,99.9799979995999,70.2511316452692));
#41454=CARTESIAN_POINT('Ctrl Pts',(1.94980991520061,99.9810415029486,70.5189978221538));
#41455=CARTESIAN_POINT('Ctrl Pts',(1.74570051630388,99.9848135889912,71.0117544930956));
#41456=CARTESIAN_POINT('Ctrl Pts',(1.591781571759,99.9874880579221,71.2366455529872));
#41457=CARTESIAN_POINT('Ctrl Pts',(1.23664555394557,99.9925109419644,71.5917815708006));
#41458=CARTESIAN_POINT('Ctrl Pts',(1.01175449350968,99.995185177515,71.7457005158259));
#41459=CARTESIAN_POINT('Ctrl Pts',(0.51899782138642,99.998956730068,71.949809915825));
#41460=CARTESIAN_POINT('Ctrl Pts',(0.251131643913751,100.,72.));
#41461=CARTESIAN_POINT('Ctrl Pts',(-3.46944695195361E-16,100.,72.));
#41462=CARTESIAN_POINT('',(2.09200853713576E-16,90.,68.));
#41463=CARTESIAN_POINT('',(2.44929359829471E-16,94.,68.));
#41464=CARTESIAN_POINT('',(2.,89.9777750336159,70.));
#41465=CARTESIAN_POINT('Ctrl Pts',(2.,89.9777750336159,70.));
#41466=CARTESIAN_POINT('Ctrl Pts',(2.,89.9777750336159,69.7488666698804));
#41467=CARTESIAN_POINT('Ctrl Pts',(1.9498092567713,89.9789345539658,69.480999766208));
#41468=CARTESIAN_POINT('Ctrl Pts',(1.74569936855887,89.9831259365723,68.9882435581214));
#41469=CARTESIAN_POINT('Ctrl Pts',(1.59178067978086,89.9860976603374,68.7633535550347));
#41470=CARTESIAN_POINT('Ctrl Pts',(1.23664644642618,89.9916787455059,68.40821932168));
#41471=CARTESIAN_POINT('Ctrl Pts',(1.01175644254643,89.9946501491172,68.2543006320885));
#41472=CARTESIAN_POINT('Ctrl Pts',(0.519000232590759,89.9988407998655,68.0501907423603));
#41473=CARTESIAN_POINT('Ctrl Pts',(0.251133328053567,90.,68.));
#41474=CARTESIAN_POINT('Ctrl Pts',(4.85722573273506E-16,90.,68.));
#41475=CARTESIAN_POINT('Ctrl Pts',(1.73472347597681E-16,90.,68.));
#41476=CARTESIAN_POINT('Ctrl Pts',(-0.251133328053567,90.,68.));
#41477=CARTESIAN_POINT('Ctrl Pts',(-0.519000232590759,89.9988407998655,
68.0501907423603));
#41478=CARTESIAN_POINT('Ctrl Pts',(-1.01175644254643,89.9946501491172,68.2543006320885));
#41479=CARTESIAN_POINT('Ctrl Pts',(-1.23664644642618,89.9916787455059,68.40821932168));
#41480=CARTESIAN_POINT('Ctrl Pts',(-1.59178067978086,89.9860976603374,68.7633535550347));
#41481=CARTESIAN_POINT('Ctrl Pts',(-1.74569936855887,89.9831259365723,68.9882435581214));
#41482=CARTESIAN_POINT('Ctrl Pts',(-1.9498092567713,89.9789345539658,69.480999766208));
#41483=CARTESIAN_POINT('Ctrl Pts',(-2.,89.9777750336159,69.7488666698804));
#41484=CARTESIAN_POINT('Ctrl Pts',(-2.,89.9777750336159,70.2511333301196));
#41485=CARTESIAN_POINT('Ctrl Pts',(-1.9498092567713,89.9789345539658,70.519000233792));
#41486=CARTESIAN_POINT('Ctrl Pts',(-1.74569936855887,89.9831259365723,71.0117564418786));
#41487=CARTESIAN_POINT('Ctrl Pts',(-1.59178067978086,89.9860976603374,71.2366464449653));
#41488=CARTESIAN_POINT('Ctrl Pts',(-1.23664644642618,89.9916787455059,71.59178067832));
#41489=CARTESIAN_POINT('Ctrl Pts',(-1.01175644254643,89.9946501491172,71.7456993679115));
#41490=CARTESIAN_POINT('Ctrl Pts',(-0.519000232590759,89.9988407998655,
71.9498092576397));
#41491=CARTESIAN_POINT('Ctrl Pts',(-0.251133328053567,90.,72.));
#41492=CARTESIAN_POINT('Ctrl Pts',(0.251133328053566,90.,72.));
#41493=CARTESIAN_POINT('Ctrl Pts',(0.519000232590759,89.9988407998655,71.9498092576397));
#41494=CARTESIAN_POINT('Ctrl Pts',(1.01175644254643,89.9946501491172,71.7456993679115));
#41495=CARTESIAN_POINT('Ctrl Pts',(1.23664644642618,89.9916787455059,71.59178067832));
#41496=CARTESIAN_POINT('Ctrl Pts',(1.59178067978086,89.9860976603374,71.2366464449653));
#41497=CARTESIAN_POINT('Ctrl Pts',(1.74569936855887,89.9831259365723,71.0117564418786));
#41498=CARTESIAN_POINT('Ctrl Pts',(1.9498092567713,89.9789345539658,70.519000233792));
#41499=CARTESIAN_POINT('Ctrl Pts',(2.,89.9777750336159,70.2511333301196));
#41500=CARTESIAN_POINT('Ctrl Pts',(2.,89.9777750336159,70.));
#41501=CARTESIAN_POINT('Origin',(-94.,0.,70.));
#41502=CARTESIAN_POINT('',(-100.,0.,72.));
#41503=CARTESIAN_POINT('',(-100.,0.,68.));
#41504=CARTESIAN_POINT('Ctrl Pts',(-100.,1.73472347597681E-15,72.));
#41505=CARTESIAN_POINT('Ctrl Pts',(-100.,-0.251131643913749,72.));
#41506=CARTESIAN_POINT('Ctrl Pts',(-99.998956730068,-0.51899782138642,71.949809915825));
#41507=CARTESIAN_POINT('Ctrl Pts',(-99.995185177515,-1.01175449350968,71.7457005158259));
#41508=CARTESIAN_POINT('Ctrl Pts',(-99.9925109419644,-1.23664555394557,
71.5917815708006));
#41509=CARTESIAN_POINT('Ctrl Pts',(-99.9874880579221,-1.591781571759,71.2366455529872));
#41510=CARTESIAN_POINT('Ctrl Pts',(-99.9848135889912,-1.74570051630387,
71.0117544930956));
#41511=CARTESIAN_POINT('Ctrl Pts',(-99.9810415029486,-1.94980991520061,
70.5189978221538));
#41512=CARTESIAN_POINT('Ctrl Pts',(-99.9799979995999,-2.,70.2511316452692));
#41513=CARTESIAN_POINT('Ctrl Pts',(-99.9799979995999,-2.,69.7488683547308));
#41514=CARTESIAN_POINT('Ctrl Pts',(-99.9810415029486,-1.94980991520061,
69.4810021778462));
#41515=CARTESIAN_POINT('Ctrl Pts',(-99.9848135889912,-1.74570051630388,
68.9882455069044));
#41516=CARTESIAN_POINT('Ctrl Pts',(-99.9874880579221,-1.591781571759,68.7633544470128));
#41517=CARTESIAN_POINT('Ctrl Pts',(-99.9925109419644,-1.23664555394558,
68.4082184291994));
#41518=CARTESIAN_POINT('Ctrl Pts',(-99.995185177515,-1.01175449350969,68.2542994841741));
#41519=CARTESIAN_POINT('Ctrl Pts',(-99.998956730068,-0.518997821386428,
68.0501900841751));
#41520=CARTESIAN_POINT('Ctrl Pts',(-100.,-0.251131643913751,68.));
#41521=CARTESIAN_POINT('Ctrl Pts',(-100.,-4.85722573273506E-16,68.));
#41522=CARTESIAN_POINT('',(-99.9799979995999,2.,70.));
#41523=CARTESIAN_POINT('Ctrl Pts',(-99.9799979995999,2.,70.));
#41524=CARTESIAN_POINT('Ctrl Pts',(-99.9799979995999,2.,70.2511316452692));
#41525=CARTESIAN_POINT('Ctrl Pts',(-99.9810415029486,1.94980991520061,70.5189978221538));
#41526=CARTESIAN_POINT('Ctrl Pts',(-99.9848135889912,1.74570051630388,71.0117544930956));
#41527=CARTESIAN_POINT('Ctrl Pts',(-99.9874880579221,1.591781571759,71.2366455529872));
#41528=CARTESIAN_POINT('Ctrl Pts',(-99.9925109419644,1.23664555394557,71.5917815708006));
#41529=CARTESIAN_POINT('Ctrl Pts',(-99.995185177515,1.01175449350968,71.7457005158259));
#41530=CARTESIAN_POINT('Ctrl Pts',(-99.998956730068,0.51899782138642,71.949809915825));
#41531=CARTESIAN_POINT('Ctrl Pts',(-100.,0.251131643913751,72.));
#41532=CARTESIAN_POINT('Ctrl Pts',(-100.,-6.93889390390723E-17,72.));
#41533=CARTESIAN_POINT('',(-89.9777750336159,2.,70.));
#41534=CARTESIAN_POINT('',(-94.,2.,70.));
#41535=CARTESIAN_POINT('',(-90.,-4.92110461433098E-15,72.));
#41536=CARTESIAN_POINT('Ctrl Pts',(-90.,1.11022302462516E-15,72.));
#41537=CARTESIAN_POINT('Ctrl Pts',(-90.,0.251133328053568,72.));
#41538=CARTESIAN_POINT('Ctrl Pts',(-89.9988407998655,0.519000232590759,
71.9498092576397));
#41539=CARTESIAN_POINT('Ctrl Pts',(-89.9946501491172,1.01175644254643,71.7456993679115));
#41540=CARTESIAN_POINT('Ctrl Pts',(-89.9916787455059,1.23664644642618,71.59178067832));
#41541=CARTESIAN_POINT('Ctrl Pts',(-89.9860976603374,1.59178067978086,71.2366464449653));
#41542=CARTESIAN_POINT('Ctrl Pts',(-89.9831259365723,1.74569936855887,71.0117564418786));
#41543=CARTESIAN_POINT('Ctrl Pts',(-89.9789345539658,1.9498092567713,70.519000233792));
#41544=CARTESIAN_POINT('Ctrl Pts',(-89.9777750336159,2.,70.2511333301196));
#41545=CARTESIAN_POINT('Ctrl Pts',(-89.9777750336159,2.,70.));
#41546=CARTESIAN_POINT('',(-90.,-5.40682718760448E-15,68.));
#41547=CARTESIAN_POINT('Ctrl Pts',(-90.,2.08166817117217E-16,68.));
#41548=CARTESIAN_POINT('Ctrl Pts',(-90.,-0.251133328053567,68.));
#41549=CARTESIAN_POINT('Ctrl Pts',(-89.9988407998655,-0.519000232590759,
68.0501907423603));
#41550=CARTESIAN_POINT('Ctrl Pts',(-89.9946501491172,-1.01175644254643,
68.2543006320885));
#41551=CARTESIAN_POINT('Ctrl Pts',(-89.9916787455059,-1.23664644642618,
68.40821932168));
#41552=CARTESIAN_POINT('Ctrl Pts',(-89.9860976603374,-1.59178067978086,
68.7633535550347));
#41553=CARTESIAN_POINT('Ctrl Pts',(-89.9831259365723,-1.74569936855887,
68.9882435581214));
#41554=CARTESIAN_POINT('Ctrl Pts',(-89.9789345539658,-1.94980925677131,
69.480999766208));
#41555=CARTESIAN_POINT('Ctrl Pts',(-89.9777750336159,-2.,69.7488666698804));
#41556=CARTESIAN_POINT('Ctrl Pts',(-89.9777750336159,-2.,70.2511333301196));
#41557=CARTESIAN_POINT('Ctrl Pts',(-89.9789345539658,-1.9498092567713,70.519000233792));
#41558=CARTESIAN_POINT('Ctrl Pts',(-89.9831259365723,-1.74569936855886,
71.0117564418786));
#41559=CARTESIAN_POINT('Ctrl Pts',(-89.9860976603374,-1.59178067978086,
71.2366464449653));
#41560=CARTESIAN_POINT('Ctrl Pts',(-89.9916787455059,-1.23664644642618,
71.59178067832));
#41561=CARTESIAN_POINT('Ctrl Pts',(-89.9946501491172,-1.01175644254642,
71.7456993679115));
#41562=CARTESIAN_POINT('Ctrl Pts',(-89.9988407998655,-0.519000232590759,
71.9498092576397));
#41563=CARTESIAN_POINT('Ctrl Pts',(-90.,-0.251133328053567,72.));
#41564=CARTESIAN_POINT('Ctrl Pts',(-90.,-6.93889390390723E-17,72.));
#41565=CARTESIAN_POINT('Ctrl Pts',(-89.9777750336159,2.,70.));
#41566=CARTESIAN_POINT('Ctrl Pts',(-89.9777750336159,2.,69.7488666698804));
#41567=CARTESIAN_POINT('Ctrl Pts',(-89.9789345539658,1.9498092567713,69.480999766208));
#41568=CARTESIAN_POINT('Ctrl Pts',(-89.9831259365723,1.74569936855887,68.9882435581214));
#41569=CARTESIAN_POINT('Ctrl Pts',(-89.9860976603374,1.59178067978086,68.7633535550347));
#41570=CARTESIAN_POINT('Ctrl Pts',(-89.9916787455059,1.23664644642618,68.40821932168));
#41571=CARTESIAN_POINT('Ctrl Pts',(-89.9946501491172,1.01175644254643,68.2543006320885));
#41572=CARTESIAN_POINT('Ctrl Pts',(-89.9988407998655,0.519000232590759,
68.0501907423603));
#41573=CARTESIAN_POINT('Ctrl Pts',(-90.,0.251133328053566,68.));
#41574=CARTESIAN_POINT('Ctrl Pts',(-90.,-5.55111512312578E-16,68.));
#41575=CARTESIAN_POINT('Ctrl Pts',(-100.,-4.16333634234434E-16,68.));
#41576=CARTESIAN_POINT('Ctrl Pts',(-100.,0.25113164391375,68.));
#41577=CARTESIAN_POINT('Ctrl Pts',(-99.998956730068,0.518997821386425,68.0501900841751));
#41578=CARTESIAN_POINT('Ctrl Pts',(-99.995185177515,1.01175449350968,68.2542994841741));
#41579=CARTESIAN_POINT('Ctrl Pts',(-99.9925109419644,1.23664555394557,68.4082184291994));
#41580=CARTESIAN_POINT('Ctrl Pts',(-99.9874880579221,1.591781571759,68.7633544470128));
#41581=CARTESIAN_POINT('Ctrl Pts',(-99.9848135889912,1.74570051630388,68.9882455069044));
#41582=CARTESIAN_POINT('Ctrl Pts',(-99.9810415029486,1.94980991520061,69.4810021778462));
#41583=CARTESIAN_POINT('Ctrl Pts',(-99.9799979995999,2.,69.7488683547308));
#41584=CARTESIAN_POINT('Ctrl Pts',(-99.9799979995999,2.,70.));
#41585=CARTESIAN_POINT('Origin',(94.,0.,70.));
#41586=CARTESIAN_POINT('',(100.,0.,72.));
#41587=CARTESIAN_POINT('',(100.,0.,68.));
#41588=CARTESIAN_POINT('Ctrl Pts',(100.,-1.73472347597681E-15,72.));
#41589=CARTESIAN_POINT('Ctrl Pts',(100.,0.251131643913749,72.));
#41590=CARTESIAN_POINT('Ctrl Pts',(99.998956730068,0.51899782138642,71.949809915825));
#41591=CARTESIAN_POINT('Ctrl Pts',(99.995185177515,1.01175449350968,71.7457005158259));
#41592=CARTESIAN_POINT('Ctrl Pts',(99.9925109419644,1.23664555394557,71.5917815708006));
#41593=CARTESIAN_POINT('Ctrl Pts',(99.9874880579221,1.591781571759,71.2366455529872));
#41594=CARTESIAN_POINT('Ctrl Pts',(99.9848135889912,1.74570051630387,71.0117544930956));
#41595=CARTESIAN_POINT('Ctrl Pts',(99.9810415029486,1.94980991520061,70.5189978221538));
#41596=CARTESIAN_POINT('Ctrl Pts',(99.9799979995999,2.,70.2511316452692));
#41597=CARTESIAN_POINT('Ctrl Pts',(99.9799979995999,2.,69.7488683547308));
#41598=CARTESIAN_POINT('Ctrl Pts',(99.9810415029486,1.94980991520061,69.4810021778462));
#41599=CARTESIAN_POINT('Ctrl Pts',(99.9848135889912,1.74570051630388,68.9882455069044));
#41600=CARTESIAN_POINT('Ctrl Pts',(99.9874880579221,1.591781571759,68.7633544470128));
#41601=CARTESIAN_POINT('Ctrl Pts',(99.9925109419644,1.23664555394558,68.4082184291994));
#41602=CARTESIAN_POINT('Ctrl Pts',(99.995185177515,1.01175449350969,68.2542994841741));
#41603=CARTESIAN_POINT('Ctrl Pts',(99.998956730068,0.518997821386428,68.0501900841751));
#41604=CARTESIAN_POINT('Ctrl Pts',(100.,0.251131643913751,68.));
#41605=CARTESIAN_POINT('Ctrl Pts',(100.,4.85722573273506E-16,68.));
#41606=CARTESIAN_POINT('',(99.9799979995999,-2.,70.));
#41607=CARTESIAN_POINT('Ctrl Pts',(99.9799979995999,-2.,70.));
#41608=CARTESIAN_POINT('Ctrl Pts',(99.9799979995999,-2.,70.2511316452692));
#41609=CARTESIAN_POINT('Ctrl Pts',(99.9810415029486,-1.94980991520061,70.5189978221538));
#41610=CARTESIAN_POINT('Ctrl Pts',(99.9848135889912,-1.74570051630388,71.0117544930956));
#41611=CARTESIAN_POINT('Ctrl Pts',(99.9874880579221,-1.591781571759,71.2366455529872));
#41612=CARTESIAN_POINT('Ctrl Pts',(99.9925109419644,-1.23664555394557,71.5917815708006));
#41613=CARTESIAN_POINT('Ctrl Pts',(99.995185177515,-1.01175449350968,71.7457005158259));
#41614=CARTESIAN_POINT('Ctrl Pts',(99.998956730068,-0.51899782138642,71.949809915825));
#41615=CARTESIAN_POINT('Ctrl Pts',(100.,-0.251131643913751,72.));
#41616=CARTESIAN_POINT('Ctrl Pts',(100.,6.93889390390723E-17,72.));
#41617=CARTESIAN_POINT('',(89.9777750336159,-2.,70.));
#41618=CARTESIAN_POINT('',(94.,-2.,70.));
#41619=CARTESIAN_POINT('Ctrl Pts',(89.9777750336159,-2.,70.));
#41620=CARTESIAN_POINT('Ctrl Pts',(89.9777750336159,-2.,69.7488666698804));
#41621=CARTESIAN_POINT('Ctrl Pts',(89.9789345539658,-1.9498092567713,69.480999766208));
#41622=CARTESIAN_POINT('Ctrl Pts',(89.9831259365723,-1.74569936855887,68.9882435581214));
#41623=CARTESIAN_POINT('Ctrl Pts',(89.9860976603374,-1.59178067978086,68.7633535550347));
#41624=CARTESIAN_POINT('Ctrl Pts',(89.9916787455059,-1.23664644642618,68.40821932168));
#41625=CARTESIAN_POINT('Ctrl Pts',(89.9946501491172,-1.01175644254643,68.2543006320885));
#41626=CARTESIAN_POINT('Ctrl Pts',(89.9988407998655,-0.519000232590759,
68.0501907423603));
#41627=CARTESIAN_POINT('Ctrl Pts',(90.,-0.251133328053567,68.));
#41628=CARTESIAN_POINT('Ctrl Pts',(90.,0.251133328053567,68.));
#41629=CARTESIAN_POINT('Ctrl Pts',(89.9988407998655,0.519000232590759,68.0501907423603));
#41630=CARTESIAN_POINT('Ctrl Pts',(89.9946501491172,1.01175644254643,68.2543006320885));
#41631=CARTESIAN_POINT('Ctrl Pts',(89.9916787455059,1.23664644642618,68.40821932168));
#41632=CARTESIAN_POINT('Ctrl Pts',(89.9860976603374,1.59178067978086,68.7633535550347));
#41633=CARTESIAN_POINT('Ctrl Pts',(89.9831259365723,1.74569936855887,68.9882435581214));
#41634=CARTESIAN_POINT('Ctrl Pts',(89.9789345539658,1.94980925677131,69.480999766208));
#41635=CARTESIAN_POINT('Ctrl Pts',(89.9777750336159,2.,69.7488666698804));
#41636=CARTESIAN_POINT('Ctrl Pts',(89.9777750336159,2.,70.2511333301196));
#41637=CARTESIAN_POINT('Ctrl Pts',(89.9789345539658,1.9498092567713,70.519000233792));
#41638=CARTESIAN_POINT('Ctrl Pts',(89.9831259365723,1.74569936855886,71.0117564418786));
#41639=CARTESIAN_POINT('Ctrl Pts',(89.9860976603374,1.59178067978086,71.2366464449653));
#41640=CARTESIAN_POINT('Ctrl Pts',(89.9916787455059,1.23664644642618,71.59178067832));
#41641=CARTESIAN_POINT('Ctrl Pts',(89.9946501491172,1.01175644254642,71.7456993679115));
#41642=CARTESIAN_POINT('Ctrl Pts',(89.9988407998655,0.519000232590759,71.9498092576397));
#41643=CARTESIAN_POINT('Ctrl Pts',(90.,0.251133328053567,72.));
#41644=CARTESIAN_POINT('Ctrl Pts',(90.,-0.251133328053567,72.));
#41645=CARTESIAN_POINT('Ctrl Pts',(89.9988407998655,-0.519000232590759,
71.9498092576397));
#41646=CARTESIAN_POINT('Ctrl Pts',(89.9946501491172,-1.01175644254643,71.7456993679115));
#41647=CARTESIAN_POINT('Ctrl Pts',(89.9916787455059,-1.23664644642618,71.59178067832));
#41648=CARTESIAN_POINT('Ctrl Pts',(89.9860976603374,-1.59178067978086,71.2366464449653));
#41649=CARTESIAN_POINT('Ctrl Pts',(89.9831259365723,-1.74569936855887,71.0117564418786));
#41650=CARTESIAN_POINT('Ctrl Pts',(89.9789345539658,-1.9498092567713,70.519000233792));
#41651=CARTESIAN_POINT('Ctrl Pts',(89.9777750336159,-2.,70.2511333301196));
#41652=CARTESIAN_POINT('Ctrl Pts',(89.9777750336159,-2.,70.));
#41653=CARTESIAN_POINT('Ctrl Pts',(100.,4.16333634234434E-16,68.));
#41654=CARTESIAN_POINT('Ctrl Pts',(100.,-0.25113164391375,68.));
#41655=CARTESIAN_POINT('Ctrl Pts',(99.998956730068,-0.518997821386425,68.0501900841751));
#41656=CARTESIAN_POINT('Ctrl Pts',(99.995185177515,-1.01175449350968,68.2542994841741));
#41657=CARTESIAN_POINT('Ctrl Pts',(99.9925109419644,-1.23664555394557,68.4082184291994));
#41658=CARTESIAN_POINT('Ctrl Pts',(99.9874880579221,-1.591781571759,68.7633544470128));
#41659=CARTESIAN_POINT('Ctrl Pts',(99.9848135889912,-1.74570051630388,68.9882455069044));
#41660=CARTESIAN_POINT('Ctrl Pts',(99.9810415029486,-1.94980991520061,69.4810021778462));
#41661=CARTESIAN_POINT('Ctrl Pts',(99.9799979995999,-2.,69.7488683547308));
#41662=CARTESIAN_POINT('Ctrl Pts',(99.9799979995999,-2.,70.));
#41663=CARTESIAN_POINT('Origin',(0.,-94.,36.));
#41664=CARTESIAN_POINT('',(0.,-100.,38.));
#41665=CARTESIAN_POINT('',(0.,-100.,34.));
#41666=CARTESIAN_POINT('Ctrl Pts',(-6.24500451351651E-16,-100.,38.));
#41667=CARTESIAN_POINT('Ctrl Pts',(0.251131643913749,-100.,38.));
#41668=CARTESIAN_POINT('Ctrl Pts',(0.518997821386425,-99.998956730068,37.9498099158249));
#41669=CARTESIAN_POINT('Ctrl Pts',(1.01175449350969,-99.995185177515,37.7457005158259));
#41670=CARTESIAN_POINT('Ctrl Pts',(1.23664555394557,-99.9925109419644,37.5917815708006));
#41671=CARTESIAN_POINT('Ctrl Pts',(1.591781571759,-99.9874880579221,37.2366455529872));
#41672=CARTESIAN_POINT('Ctrl Pts',(1.74570051630387,-99.9848135889912,37.0117544930956));
#41673=CARTESIAN_POINT('Ctrl Pts',(1.94980991520061,-99.9810415029486,36.5189978221538));
#41674=CARTESIAN_POINT('Ctrl Pts',(2.,-99.9799979995999,36.2511316452692));
#41675=CARTESIAN_POINT('Ctrl Pts',(2.,-99.9799979995999,35.7488683547308));
#41676=CARTESIAN_POINT('Ctrl Pts',(1.94980991520061,-99.9810415029486,35.4810021778462));
#41677=CARTESIAN_POINT('Ctrl Pts',(1.74570051630388,-99.9848135889912,34.9882455069044));
#41678=CARTESIAN_POINT('Ctrl Pts',(1.591781571759,-99.9874880579221,34.7633544470128));
#41679=CARTESIAN_POINT('Ctrl Pts',(1.23664555394558,-99.9925109419644,34.4082184291994));
#41680=CARTESIAN_POINT('Ctrl Pts',(1.01175449350969,-99.995185177515,34.2542994841741));
#41681=CARTESIAN_POINT('Ctrl Pts',(0.518997821386428,-99.998956730068,34.050190084175));
#41682=CARTESIAN_POINT('Ctrl Pts',(0.251131643913751,-100.,34.));
#41683=CARTESIAN_POINT('Ctrl Pts',(1.38777878078145E-16,-100.,34.));
#41684=CARTESIAN_POINT('',(2.95937027512416E-16,-90.,38.));
#41685=CARTESIAN_POINT('',(2.44929359829471E-16,-94.,38.));
#41686=CARTESIAN_POINT('',(-2.,-89.9777750336159,36.));
#41687=CARTESIAN_POINT('Ctrl Pts',(-2.,-89.9777750336159,36.));
#41688=CARTESIAN_POINT('Ctrl Pts',(-2.,-89.9777750336159,35.7488666698804));
#41689=CARTESIAN_POINT('Ctrl Pts',(-1.94980925677131,-89.9789345539658,
35.480999766208));
#41690=CARTESIAN_POINT('Ctrl Pts',(-1.74569936855887,-89.9831259365723,
34.9882435581214));
#41691=CARTESIAN_POINT('Ctrl Pts',(-1.59178067978086,-89.9860976603374,
34.7633535550347));
#41692=CARTESIAN_POINT('Ctrl Pts',(-1.23664644642618,-89.9916787455059,
34.40821932168));
#41693=CARTESIAN_POINT('Ctrl Pts',(-1.01175644254643,-89.9946501491172,
34.2543006320885));
#41694=CARTESIAN_POINT('Ctrl Pts',(-0.519000232590761,-89.9988407998655,
34.0501907423603));
#41695=CARTESIAN_POINT('Ctrl Pts',(-0.251133328053567,-90.,34.));
#41696=CARTESIAN_POINT('Ctrl Pts',(0.251133328053567,-90.,34.));
#41697=CARTESIAN_POINT('Ctrl Pts',(0.519000232590761,-89.9988407998655,
34.0501907423603));
#41698=CARTESIAN_POINT('Ctrl Pts',(1.01175644254643,-89.9946501491172,34.2543006320885));
#41699=CARTESIAN_POINT('Ctrl Pts',(1.23664644642618,-89.9916787455059,34.40821932168));
#41700=CARTESIAN_POINT('Ctrl Pts',(1.59178067978086,-89.9860976603374,34.7633535550347));
#41701=CARTESIAN_POINT('Ctrl Pts',(1.74569936855887,-89.9831259365723,34.9882435581214));
#41702=CARTESIAN_POINT('Ctrl Pts',(1.94980925677131,-89.9789345539658,35.480999766208));
#41703=CARTESIAN_POINT('Ctrl Pts',(2.,-89.9777750336159,35.7488666698804));
#41704=CARTESIAN_POINT('Ctrl Pts',(2.,-89.9777750336159,36.2511333301197));
#41705=CARTESIAN_POINT('Ctrl Pts',(1.9498092567713,-89.9789345539658,36.519000233792));
#41706=CARTESIAN_POINT('Ctrl Pts',(1.74569936855886,-89.9831259365723,37.0117564418786));
#41707=CARTESIAN_POINT('Ctrl Pts',(1.59178067978086,-89.9860976603374,37.2366464449653));
#41708=CARTESIAN_POINT('Ctrl Pts',(1.23664644642618,-89.9916787455059,37.59178067832));
#41709=CARTESIAN_POINT('Ctrl Pts',(1.01175644254643,-89.9946501491172,37.7456993679115));
#41710=CARTESIAN_POINT('Ctrl Pts',(0.51900023259076,-89.9988407998655,37.9498092576397));
#41711=CARTESIAN_POINT('Ctrl Pts',(0.251133328053566,-90.,38.));
#41712=CARTESIAN_POINT('Ctrl Pts',(6.93889390390723E-17,-90.,38.));
#41713=CARTESIAN_POINT('Ctrl Pts',(0.,-90.,38.));
#41714=CARTESIAN_POINT('Ctrl Pts',(-0.251133328053566,-90.,38.));
#41715=CARTESIAN_POINT('Ctrl Pts',(-0.51900023259076,-89.9988407998655,
37.9498092576397));
#41716=CARTESIAN_POINT('Ctrl Pts',(-1.01175644254643,-89.9946501491172,
37.7456993679115));
#41717=CARTESIAN_POINT('Ctrl Pts',(-1.23664644642618,-89.9916787455059,
37.59178067832));
#41718=CARTESIAN_POINT('Ctrl Pts',(-1.59178067978086,-89.9860976603374,
37.2366464449653));
#41719=CARTESIAN_POINT('Ctrl Pts',(-1.74569936855887,-89.9831259365723,
37.0117564418786));
#41720=CARTESIAN_POINT('Ctrl Pts',(-1.94980925677131,-89.9789345539658,
36.519000233792));
#41721=CARTESIAN_POINT('Ctrl Pts',(-2.,-89.9777750336159,36.2511333301197));
#41722=CARTESIAN_POINT('Ctrl Pts',(-2.,-89.9777750336159,36.));
#41723=CARTESIAN_POINT('Ctrl Pts',(-1.38777878078145E-16,-100.,34.));
#41724=CARTESIAN_POINT('Ctrl Pts',(-0.251131643913752,-100.,34.));
#41725=CARTESIAN_POINT('Ctrl Pts',(-0.518997821386424,-99.998956730068,
34.050190084175));
#41726=CARTESIAN_POINT('Ctrl Pts',(-1.01175449350969,-99.995185177515,34.2542994841741));
#41727=CARTESIAN_POINT('Ctrl Pts',(-1.23664555394558,-99.9925109419644,
34.4082184291994));
#41728=CARTESIAN_POINT('Ctrl Pts',(-1.591781571759,-99.9874880579221,34.7633544470128));
#41729=CARTESIAN_POINT('Ctrl Pts',(-1.74570051630388,-99.9848135889912,
34.9882455069044));
#41730=CARTESIAN_POINT('Ctrl Pts',(-1.94980991520062,-99.9810415029486,
35.4810021778462));
#41731=CARTESIAN_POINT('Ctrl Pts',(-2.,-99.9799979995999,35.7488683547308));
#41732=CARTESIAN_POINT('Ctrl Pts',(-2.,-99.9799979995999,36.));
#41733=CARTESIAN_POINT('Ctrl Pts',(-2.,-99.9799979995999,36.2511316452692));
#41734=CARTESIAN_POINT('Ctrl Pts',(-1.94980991520061,-99.9810415029486,
36.5189978221538));
#41735=CARTESIAN_POINT('Ctrl Pts',(-1.74570051630387,-99.9848135889912,
37.0117544930956));
#41736=CARTESIAN_POINT('Ctrl Pts',(-1.591781571759,-99.9874880579221,37.2366455529872));
#41737=CARTESIAN_POINT('Ctrl Pts',(-1.23664555394557,-99.9925109419644,
37.5917815708006));
#41738=CARTESIAN_POINT('Ctrl Pts',(-1.01175449350969,-99.995185177515,37.7457005158259));
#41739=CARTESIAN_POINT('Ctrl Pts',(-0.518997821386425,-99.998956730068,
37.9498099158249));
#41740=CARTESIAN_POINT('Ctrl Pts',(-0.25113164391375,-100.,38.));
#41741=CARTESIAN_POINT('Ctrl Pts',(-4.16333634234434E-16,-100.,38.));
#41742=CARTESIAN_POINT('Origin',(0.,94.,36.));
#41743=CARTESIAN_POINT('',(0.,100.,38.));
#41744=CARTESIAN_POINT('',(0.,100.,34.));
#41745=CARTESIAN_POINT('Ctrl Pts',(5.55111512312578E-16,100.,38.));
#41746=CARTESIAN_POINT('Ctrl Pts',(-0.251131643913749,100.,38.));
#41747=CARTESIAN_POINT('Ctrl Pts',(-0.518997821386421,99.998956730068,37.9498099158249));
#41748=CARTESIAN_POINT('Ctrl Pts',(-1.01175449350968,99.995185177515,37.7457005158259));
#41749=CARTESIAN_POINT('Ctrl Pts',(-1.23664555394557,99.9925109419644,37.5917815708006));
#41750=CARTESIAN_POINT('Ctrl Pts',(-1.591781571759,99.9874880579221,37.2366455529872));
#41751=CARTESIAN_POINT('Ctrl Pts',(-1.74570051630387,99.9848135889912,37.0117544930956));
#41752=CARTESIAN_POINT('Ctrl Pts',(-1.94980991520061,99.9810415029486,36.5189978221538));
#41753=CARTESIAN_POINT('Ctrl Pts',(-2.,99.9799979995999,36.2511316452692));
#41754=CARTESIAN_POINT('Ctrl Pts',(-2.,99.9799979995999,35.7488683547308));
#41755=CARTESIAN_POINT('Ctrl Pts',(-1.94980991520062,99.9810415029486,35.4810021778462));
#41756=CARTESIAN_POINT('Ctrl Pts',(-1.74570051630388,99.9848135889912,34.9882455069044));
#41757=CARTESIAN_POINT('Ctrl Pts',(-1.591781571759,99.9874880579221,34.7633544470128));
#41758=CARTESIAN_POINT('Ctrl Pts',(-1.23664555394558,99.9925109419644,34.4082184291994));
#41759=CARTESIAN_POINT('Ctrl Pts',(-1.01175449350969,99.995185177515,34.2542994841741));
#41760=CARTESIAN_POINT('Ctrl Pts',(-0.518997821386425,99.998956730068,34.050190084175));
#41761=CARTESIAN_POINT('Ctrl Pts',(-0.251131643913753,100.,34.));
#41762=CARTESIAN_POINT('Ctrl Pts',(-9.71445146547012E-16,100.,34.));
#41763=CARTESIAN_POINT('Ctrl Pts',(2.77555756156289E-16,100.,34.));
#41764=CARTESIAN_POINT('Ctrl Pts',(0.251131643913752,100.,34.));
#41765=CARTESIAN_POINT('Ctrl Pts',(0.518997821386428,99.998956730068,34.050190084175));
#41766=CARTESIAN_POINT('Ctrl Pts',(1.01175449350969,99.995185177515,34.2542994841741));
#41767=CARTESIAN_POINT('Ctrl Pts',(1.23664555394558,99.9925109419644,34.4082184291994));
#41768=CARTESIAN_POINT('Ctrl Pts',(1.591781571759,99.9874880579221,34.7633544470128));
#41769=CARTESIAN_POINT('Ctrl Pts',(1.74570051630388,99.9848135889912,34.9882455069044));
#41770=CARTESIAN_POINT('Ctrl Pts',(1.94980991520061,99.9810415029486,35.4810021778462));
#41771=CARTESIAN_POINT('Ctrl Pts',(2.,99.9799979995999,35.7488683547308));
#41772=CARTESIAN_POINT('Ctrl Pts',(2.,99.9799979995999,36.));
#41773=CARTESIAN_POINT('Ctrl Pts',(2.,99.9799979995999,36.2511316452692));
#41774=CARTESIAN_POINT('Ctrl Pts',(1.94980991520061,99.9810415029486,36.5189978221538));
#41775=CARTESIAN_POINT('Ctrl Pts',(1.74570051630387,99.9848135889912,37.0117544930956));
#41776=CARTESIAN_POINT('Ctrl Pts',(1.591781571759,99.9874880579221,37.2366455529872));
#41777=CARTESIAN_POINT('Ctrl Pts',(1.23664555394557,99.9925109419644,37.5917815708006));
#41778=CARTESIAN_POINT('Ctrl Pts',(1.01175449350968,99.995185177515,37.7457005158259));
#41779=CARTESIAN_POINT('Ctrl Pts',(0.518997821386424,99.998956730068,37.949809915825));
#41780=CARTESIAN_POINT('Ctrl Pts',(0.25113164391375,100.,38.));
#41781=CARTESIAN_POINT('Ctrl Pts',(1.38777878078145E-16,100.,38.));
#41782=CARTESIAN_POINT('',(4.00020436071024E-16,90.,34.));
#41783=CARTESIAN_POINT('',(2.44929359829471E-16,94.,34.));
#41784=CARTESIAN_POINT('',(2.,89.9777750336159,36.));
#41785=CARTESIAN_POINT('Ctrl Pts',(2.,89.9777750336159,36.));
#41786=CARTESIAN_POINT('Ctrl Pts',(2.,89.9777750336159,35.7488666698804));
#41787=CARTESIAN_POINT('Ctrl Pts',(1.94980925677131,89.9789345539658,35.480999766208));
#41788=CARTESIAN_POINT('Ctrl Pts',(1.74569936855887,89.9831259365723,34.9882435581214));
#41789=CARTESIAN_POINT('Ctrl Pts',(1.59178067978086,89.9860976603374,34.7633535550347));
#41790=CARTESIAN_POINT('Ctrl Pts',(1.23664644642618,89.9916787455059,34.40821932168));
#41791=CARTESIAN_POINT('Ctrl Pts',(1.01175644254643,89.9946501491172,34.2543006320885));
#41792=CARTESIAN_POINT('Ctrl Pts',(0.519000232590761,89.9988407998655,34.0501907423603));
#41793=CARTESIAN_POINT('Ctrl Pts',(0.251133328053567,90.,34.));
#41794=CARTESIAN_POINT('Ctrl Pts',(0.,90.,34.));
#41795=CARTESIAN_POINT('Ctrl Pts',(5.55111512312578E-16,90.,34.));
#41796=CARTESIAN_POINT('Ctrl Pts',(-0.251133328053567,90.,34.));
#41797=CARTESIAN_POINT('Ctrl Pts',(-0.519000232590761,89.9988407998655,
34.0501907423603));
#41798=CARTESIAN_POINT('Ctrl Pts',(-1.01175644254643,89.9946501491172,34.2543006320885));
#41799=CARTESIAN_POINT('Ctrl Pts',(-1.23664644642618,89.9916787455059,34.40821932168));
#41800=CARTESIAN_POINT('Ctrl Pts',(-1.59178067978086,89.9860976603374,34.7633535550347));
#41801=CARTESIAN_POINT('Ctrl Pts',(-1.74569936855887,89.9831259365723,34.9882435581214));
#41802=CARTESIAN_POINT('Ctrl Pts',(-1.94980925677131,89.9789345539658,35.480999766208));
#41803=CARTESIAN_POINT('Ctrl Pts',(-2.,89.9777750336159,35.7488666698804));
#41804=CARTESIAN_POINT('Ctrl Pts',(-2.,89.9777750336159,36.2511333301197));
#41805=CARTESIAN_POINT('Ctrl Pts',(-1.9498092567713,89.9789345539658,36.519000233792));
#41806=CARTESIAN_POINT('Ctrl Pts',(-1.74569936855886,89.9831259365723,37.0117564418786));
#41807=CARTESIAN_POINT('Ctrl Pts',(-1.59178067978086,89.9860976603374,37.2366464449653));
#41808=CARTESIAN_POINT('Ctrl Pts',(-1.23664644642618,89.9916787455059,37.59178067832));
#41809=CARTESIAN_POINT('Ctrl Pts',(-1.01175644254643,89.9946501491172,37.7456993679115));
#41810=CARTESIAN_POINT('Ctrl Pts',(-0.519000232590762,89.9988407998655,
37.9498092576397));
#41811=CARTESIAN_POINT('Ctrl Pts',(-0.251133328053566,90.,38.));
#41812=CARTESIAN_POINT('Ctrl Pts',(0.251133328053565,90.,38.));
#41813=CARTESIAN_POINT('Ctrl Pts',(0.519000232590761,89.9988407998655,37.9498092576397));
#41814=CARTESIAN_POINT('Ctrl Pts',(1.01175644254643,89.9946501491172,37.7456993679115));
#41815=CARTESIAN_POINT('Ctrl Pts',(1.23664644642618,89.9916787455059,37.59178067832));
#41816=CARTESIAN_POINT('Ctrl Pts',(1.59178067978086,89.9860976603374,37.2366464449653));
#41817=CARTESIAN_POINT('Ctrl Pts',(1.74569936855886,89.9831259365723,37.0117564418786));
#41818=CARTESIAN_POINT('Ctrl Pts',(1.9498092567713,89.9789345539658,36.519000233792));
#41819=CARTESIAN_POINT('Ctrl Pts',(2.,89.9777750336159,36.2511333301197));
#41820=CARTESIAN_POINT('Ctrl Pts',(2.,89.9777750336159,36.));
#41821=CARTESIAN_POINT('Origin',(-94.,0.,36.));
#41822=CARTESIAN_POINT('',(-100.,0.,38.));
#41823=CARTESIAN_POINT('',(-100.,0.,34.));
#41824=CARTESIAN_POINT('Ctrl Pts',(-100.,-5.55111512312578E-16,38.));
#41825=CARTESIAN_POINT('Ctrl Pts',(-100.,-0.251131643913751,38.));
#41826=CARTESIAN_POINT('Ctrl Pts',(-99.998956730068,-0.518997821386424,
37.949809915825));
#41827=CARTESIAN_POINT('Ctrl Pts',(-99.995185177515,-1.01175449350968,37.7457005158259));
#41828=CARTESIAN_POINT('Ctrl Pts',(-99.9925109419644,-1.23664555394557,
37.5917815708006));
#41829=CARTESIAN_POINT('Ctrl Pts',(-99.9874880579221,-1.591781571759,37.2366455529872));
#41830=CARTESIAN_POINT('Ctrl Pts',(-99.9848135889912,-1.74570051630387,
37.0117544930956));
#41831=CARTESIAN_POINT('Ctrl Pts',(-99.9810415029486,-1.94980991520061,
36.5189978221538));
#41832=CARTESIAN_POINT('Ctrl Pts',(-99.9799979995999,-2.,36.2511316452692));
#41833=CARTESIAN_POINT('Ctrl Pts',(-99.9799979995999,-2.,35.7488683547308));
#41834=CARTESIAN_POINT('Ctrl Pts',(-99.9810415029486,-1.94980991520061,
35.4810021778462));
#41835=CARTESIAN_POINT('Ctrl Pts',(-99.9848135889912,-1.74570051630388,
34.9882455069044));
#41836=CARTESIAN_POINT('Ctrl Pts',(-99.9874880579221,-1.591781571759,34.7633544470128));
#41837=CARTESIAN_POINT('Ctrl Pts',(-99.9925109419644,-1.23664555394558,
34.4082184291994));
#41838=CARTESIAN_POINT('Ctrl Pts',(-99.995185177515,-1.01175449350969,34.2542994841741));
#41839=CARTESIAN_POINT('Ctrl Pts',(-99.998956730068,-0.518997821386425,
34.050190084175));
#41840=CARTESIAN_POINT('Ctrl Pts',(-100.,-0.251131643913752,34.));
#41841=CARTESIAN_POINT('Ctrl Pts',(-100.,-7.63278329429795E-16,34.));
#41842=CARTESIAN_POINT('',(-99.9799979995999,2.,36.));
#41843=CARTESIAN_POINT('Ctrl Pts',(-99.9799979995999,2.,36.));
#41844=CARTESIAN_POINT('Ctrl Pts',(-99.9799979995999,2.,36.2511316452692));
#41845=CARTESIAN_POINT('Ctrl Pts',(-99.9810415029486,1.94980991520061,36.5189978221538));
#41846=CARTESIAN_POINT('Ctrl Pts',(-99.9848135889912,1.74570051630387,37.0117544930956));
#41847=CARTESIAN_POINT('Ctrl Pts',(-99.9874880579221,1.591781571759,37.2366455529872));
#41848=CARTESIAN_POINT('Ctrl Pts',(-99.9925109419644,1.23664555394557,37.5917815708006));
#41849=CARTESIAN_POINT('Ctrl Pts',(-99.995185177515,1.01175449350969,37.7457005158259));
#41850=CARTESIAN_POINT('Ctrl Pts',(-99.998956730068,0.518997821386425,37.9498099158249));
#41851=CARTESIAN_POINT('Ctrl Pts',(-100.,0.25113164391375,38.));
#41852=CARTESIAN_POINT('Ctrl Pts',(-100.,-6.93889390390723E-17,38.));
#41853=CARTESIAN_POINT('',(-89.9777750336159,2.,36.));
#41854=CARTESIAN_POINT('',(-94.,2.,36.));
#41855=CARTESIAN_POINT('',(-90.,-5.78846635231938E-15,38.));
#41856=CARTESIAN_POINT('Ctrl Pts',(-90.,-6.24500451351651E-16,38.));
#41857=CARTESIAN_POINT('Ctrl Pts',(-90.,0.251133328053565,38.));
#41858=CARTESIAN_POINT('Ctrl Pts',(-89.9988407998655,0.519000232590761,
37.9498092576397));
#41859=CARTESIAN_POINT('Ctrl Pts',(-89.9946501491172,1.01175644254643,37.7456993679115));
#41860=CARTESIAN_POINT('Ctrl Pts',(-89.9916787455059,1.23664644642618,37.59178067832));
#41861=CARTESIAN_POINT('Ctrl Pts',(-89.9860976603374,1.59178067978086,37.2366464449653));
#41862=CARTESIAN_POINT('Ctrl Pts',(-89.9831259365723,1.74569936855886,37.0117564418786));
#41863=CARTESIAN_POINT('Ctrl Pts',(-89.9789345539658,1.9498092567713,36.519000233792));
#41864=CARTESIAN_POINT('Ctrl Pts',(-89.9777750336159,2.,36.2511333301197));
#41865=CARTESIAN_POINT('Ctrl Pts',(-89.9777750336159,2.,36.));
#41866=CARTESIAN_POINT('',(-90.,-5.16396590096773E-15,34.));
#41867=CARTESIAN_POINT('Ctrl Pts',(-90.,6.24500451351651E-16,34.));
#41868=CARTESIAN_POINT('Ctrl Pts',(-90.,-0.251133328053567,34.));
#41869=CARTESIAN_POINT('Ctrl Pts',(-89.9988407998655,-0.519000232590761,
34.0501907423603));
#41870=CARTESIAN_POINT('Ctrl Pts',(-89.9946501491172,-1.01175644254643,
34.2543006320885));
#41871=CARTESIAN_POINT('Ctrl Pts',(-89.9916787455059,-1.23664644642618,
34.40821932168));
#41872=CARTESIAN_POINT('Ctrl Pts',(-89.9860976603374,-1.59178067978086,
34.7633535550347));
#41873=CARTESIAN_POINT('Ctrl Pts',(-89.9831259365723,-1.74569936855887,
34.9882435581214));
#41874=CARTESIAN_POINT('Ctrl Pts',(-89.9789345539658,-1.94980925677131,
35.480999766208));
#41875=CARTESIAN_POINT('Ctrl Pts',(-89.9777750336159,-2.,35.7488666698804));
#41876=CARTESIAN_POINT('Ctrl Pts',(-89.9777750336159,-2.,36.2511333301197));
#41877=CARTESIAN_POINT('Ctrl Pts',(-89.9789345539658,-1.9498092567713,36.519000233792));
#41878=CARTESIAN_POINT('Ctrl Pts',(-89.9831259365723,-1.74569936855886,
37.0117564418786));
#41879=CARTESIAN_POINT('Ctrl Pts',(-89.9860976603374,-1.59178067978086,
37.2366464449653));
#41880=CARTESIAN_POINT('Ctrl Pts',(-89.9916787455059,-1.23664644642618,
37.59178067832));
#41881=CARTESIAN_POINT('Ctrl Pts',(-89.9946501491172,-1.01175644254643,
37.7456993679115));
#41882=CARTESIAN_POINT('Ctrl Pts',(-89.9988407998655,-0.519000232590762,
37.9498092576397));
#41883=CARTESIAN_POINT('Ctrl Pts',(-90.,-0.251133328053566,38.));
#41884=CARTESIAN_POINT('Ctrl Pts',(-90.,-4.85722573273506E-16,38.));
#41885=CARTESIAN_POINT('Ctrl Pts',(-89.9777750336159,2.,36.));
#41886=CARTESIAN_POINT('Ctrl Pts',(-89.9777750336159,2.,35.7488666698804));
#41887=CARTESIAN_POINT('Ctrl Pts',(-89.9789345539658,1.94980925677131,35.480999766208));
#41888=CARTESIAN_POINT('Ctrl Pts',(-89.9831259365723,1.74569936855887,34.9882435581214));
#41889=CARTESIAN_POINT('Ctrl Pts',(-89.9860976603374,1.59178067978086,34.7633535550347));
#41890=CARTESIAN_POINT('Ctrl Pts',(-89.9916787455059,1.23664644642618,34.40821932168));
#41891=CARTESIAN_POINT('Ctrl Pts',(-89.9946501491172,1.01175644254643,34.2543006320885));
#41892=CARTESIAN_POINT('Ctrl Pts',(-89.9988407998655,0.519000232590761,
34.0501907423603));
#41893=CARTESIAN_POINT('Ctrl Pts',(-90.,0.251133328053567,34.));
#41894=CARTESIAN_POINT('Ctrl Pts',(-90.,6.93889390390723E-17,34.));
#41895=CARTESIAN_POINT('Ctrl Pts',(-100.,2.77555756156289E-16,34.));
#41896=CARTESIAN_POINT('Ctrl Pts',(-100.,0.251131643913752,34.));
#41897=CARTESIAN_POINT('Ctrl Pts',(-99.998956730068,0.518997821386424,34.050190084175));
#41898=CARTESIAN_POINT('Ctrl Pts',(-99.995185177515,1.01175449350969,34.2542994841741));
#41899=CARTESIAN_POINT('Ctrl Pts',(-99.9925109419644,1.23664555394558,34.4082184291994));
#41900=CARTESIAN_POINT('Ctrl Pts',(-99.9874880579221,1.591781571759,34.7633544470128));
#41901=CARTESIAN_POINT('Ctrl Pts',(-99.9848135889912,1.74570051630388,34.9882455069044));
#41902=CARTESIAN_POINT('Ctrl Pts',(-99.9810415029486,1.94980991520061,35.4810021778462));
#41903=CARTESIAN_POINT('Ctrl Pts',(-99.9799979995999,2.,35.7488683547308));
#41904=CARTESIAN_POINT('Ctrl Pts',(-99.9799979995999,2.,36.));
#41905=CARTESIAN_POINT('Origin',(94.,0.,36.));
#41906=CARTESIAN_POINT('',(100.,0.,38.));
#41907=CARTESIAN_POINT('',(100.,0.,34.));
#41908=CARTESIAN_POINT('Ctrl Pts',(100.,5.55111512312578E-16,38.));
#41909=CARTESIAN_POINT('Ctrl Pts',(100.,0.251131643913751,38.));
#41910=CARTESIAN_POINT('Ctrl Pts',(99.998956730068,0.518997821386424,37.949809915825));
#41911=CARTESIAN_POINT('Ctrl Pts',(99.995185177515,1.01175449350968,37.7457005158259));
#41912=CARTESIAN_POINT('Ctrl Pts',(99.9925109419644,1.23664555394557,37.5917815708006));
#41913=CARTESIAN_POINT('Ctrl Pts',(99.9874880579221,1.591781571759,37.2366455529872));
#41914=CARTESIAN_POINT('Ctrl Pts',(99.9848135889912,1.74570051630387,37.0117544930956));
#41915=CARTESIAN_POINT('Ctrl Pts',(99.9810415029486,1.94980991520061,36.5189978221538));
#41916=CARTESIAN_POINT('Ctrl Pts',(99.9799979995999,2.,36.2511316452692));
#41917=CARTESIAN_POINT('Ctrl Pts',(99.9799979995999,2.,35.7488683547308));
#41918=CARTESIAN_POINT('Ctrl Pts',(99.9810415029486,1.94980991520061,35.4810021778462));
#41919=CARTESIAN_POINT('Ctrl Pts',(99.9848135889912,1.74570051630388,34.9882455069044));
#41920=CARTESIAN_POINT('Ctrl Pts',(99.9874880579221,1.591781571759,34.7633544470128));
#41921=CARTESIAN_POINT('Ctrl Pts',(99.9925109419644,1.23664555394558,34.4082184291994));
#41922=CARTESIAN_POINT('Ctrl Pts',(99.995185177515,1.01175449350969,34.2542994841741));
#41923=CARTESIAN_POINT('Ctrl Pts',(99.998956730068,0.518997821386425,34.050190084175));
#41924=CARTESIAN_POINT('Ctrl Pts',(100.,0.251131643913752,34.));
#41925=CARTESIAN_POINT('Ctrl Pts',(100.,7.63278329429795E-16,34.));
#41926=CARTESIAN_POINT('',(99.9799979995999,-2.,36.));
#41927=CARTESIAN_POINT('Ctrl Pts',(99.9799979995999,-2.,36.));
#41928=CARTESIAN_POINT('Ctrl Pts',(99.9799979995999,-2.,36.2511316452692));
#41929=CARTESIAN_POINT('Ctrl Pts',(99.9810415029486,-1.94980991520061,36.5189978221538));
#41930=CARTESIAN_POINT('Ctrl Pts',(99.9848135889912,-1.74570051630387,37.0117544930956));
#41931=CARTESIAN_POINT('Ctrl Pts',(99.9874880579221,-1.591781571759,37.2366455529872));
#41932=CARTESIAN_POINT('Ctrl Pts',(99.9925109419644,-1.23664555394557,37.5917815708006));
#41933=CARTESIAN_POINT('Ctrl Pts',(99.995185177515,-1.01175449350969,37.7457005158259));
#41934=CARTESIAN_POINT('Ctrl Pts',(99.998956730068,-0.518997821386425,37.9498099158249));
#41935=CARTESIAN_POINT('Ctrl Pts',(100.,-0.25113164391375,38.));
#41936=CARTESIAN_POINT('Ctrl Pts',(100.,6.93889390390723E-17,38.));
#41937=CARTESIAN_POINT('',(89.9777750336159,-2.,36.));
#41938=CARTESIAN_POINT('',(94.,-2.,36.));
#41939=CARTESIAN_POINT('Ctrl Pts',(89.9777750336159,-2.,36.));
#41940=CARTESIAN_POINT('Ctrl Pts',(89.9777750336159,-2.,35.7488666698804));
#41941=CARTESIAN_POINT('Ctrl Pts',(89.9789345539658,-1.94980925677131,35.480999766208));
#41942=CARTESIAN_POINT('Ctrl Pts',(89.9831259365723,-1.74569936855887,34.9882435581214));
#41943=CARTESIAN_POINT('Ctrl Pts',(89.9860976603374,-1.59178067978086,34.7633535550347));
#41944=CARTESIAN_POINT('Ctrl Pts',(89.9916787455059,-1.23664644642618,34.40821932168));
#41945=CARTESIAN_POINT('Ctrl Pts',(89.9946501491172,-1.01175644254643,34.2543006320885));
#41946=CARTESIAN_POINT('Ctrl Pts',(89.9988407998655,-0.519000232590761,
34.0501907423603));
#41947=CARTESIAN_POINT('Ctrl Pts',(90.,-0.251133328053568,34.));
#41948=CARTESIAN_POINT('Ctrl Pts',(90.,0.251133328053567,34.));
#41949=CARTESIAN_POINT('Ctrl Pts',(89.9988407998655,0.519000232590761,34.0501907423603));
#41950=CARTESIAN_POINT('Ctrl Pts',(89.9946501491172,1.01175644254643,34.2543006320885));
#41951=CARTESIAN_POINT('Ctrl Pts',(89.9916787455059,1.23664644642618,34.40821932168));
#41952=CARTESIAN_POINT('Ctrl Pts',(89.9860976603374,1.59178067978086,34.7633535550347));
#41953=CARTESIAN_POINT('Ctrl Pts',(89.9831259365723,1.74569936855887,34.9882435581214));
#41954=CARTESIAN_POINT('Ctrl Pts',(89.9789345539658,1.94980925677131,35.480999766208));
#41955=CARTESIAN_POINT('Ctrl Pts',(89.9777750336159,2.,35.7488666698804));
#41956=CARTESIAN_POINT('Ctrl Pts',(89.9777750336159,2.,36.2511333301197));
#41957=CARTESIAN_POINT('Ctrl Pts',(89.9789345539658,1.9498092567713,36.519000233792));
#41958=CARTESIAN_POINT('Ctrl Pts',(89.9831259365723,1.74569936855886,37.0117564418786));
#41959=CARTESIAN_POINT('Ctrl Pts',(89.9860976603374,1.59178067978086,37.2366464449653));
#41960=CARTESIAN_POINT('Ctrl Pts',(89.9916787455059,1.23664644642618,37.59178067832));
#41961=CARTESIAN_POINT('Ctrl Pts',(89.9946501491172,1.01175644254643,37.7456993679115));
#41962=CARTESIAN_POINT('Ctrl Pts',(89.9988407998655,0.519000232590762,37.9498092576397));
#41963=CARTESIAN_POINT('Ctrl Pts',(90.,0.251133328053566,38.));
#41964=CARTESIAN_POINT('Ctrl Pts',(90.,-0.251133328053565,38.));
#41965=CARTESIAN_POINT('Ctrl Pts',(89.9988407998655,-0.519000232590761,
37.9498092576397));
#41966=CARTESIAN_POINT('Ctrl Pts',(89.9946501491172,-1.01175644254643,37.7456993679115));
#41967=CARTESIAN_POINT('Ctrl Pts',(89.9916787455059,-1.23664644642618,37.59178067832));
#41968=CARTESIAN_POINT('Ctrl Pts',(89.9860976603374,-1.59178067978086,37.2366464449653));
#41969=CARTESIAN_POINT('Ctrl Pts',(89.9831259365723,-1.74569936855886,37.0117564418786));
#41970=CARTESIAN_POINT('Ctrl Pts',(89.9789345539658,-1.9498092567713,36.519000233792));
#41971=CARTESIAN_POINT('Ctrl Pts',(89.9777750336159,-2.,36.2511333301197));
#41972=CARTESIAN_POINT('Ctrl Pts',(89.9777750336159,-2.,36.));
#41973=CARTESIAN_POINT('Ctrl Pts',(100.,-2.77555756156289E-16,34.));
#41974=CARTESIAN_POINT('Ctrl Pts',(100.,-0.251131643913752,34.));
#41975=CARTESIAN_POINT('Ctrl Pts',(99.998956730068,-0.518997821386424,34.050190084175));
#41976=CARTESIAN_POINT('Ctrl Pts',(99.995185177515,-1.01175449350969,34.2542994841741));
#41977=CARTESIAN_POINT('Ctrl Pts',(99.9925109419644,-1.23664555394558,34.4082184291994));
#41978=CARTESIAN_POINT('Ctrl Pts',(99.9874880579221,-1.591781571759,34.7633544470128));
#41979=CARTESIAN_POINT('Ctrl Pts',(99.9848135889912,-1.74570051630388,34.9882455069044));
#41980=CARTESIAN_POINT('Ctrl Pts',(99.9810415029486,-1.94980991520061,35.4810021778462));
#41981=CARTESIAN_POINT('Ctrl Pts',(99.9799979995999,-2.,35.7488683547308));
#41982=CARTESIAN_POINT('Ctrl Pts',(99.9799979995999,-2.,36.));
#41983=CARTESIAN_POINT('Origin',(-36.3549260746835,87.7685555885722,107.));
#41984=CARTESIAN_POINT('Ctrl Pts',(-38.2683920713485,89.4045427919473,107.));
#41985=CARTESIAN_POINT('Ctrl Pts',(-38.3305296090722,89.3461487645065,107.));
#41986=CARTESIAN_POINT('Ctrl Pts',(-38.3892917721933,89.2845008284283,107.));
#41987=CARTESIAN_POINT('Ctrl Pts',(-38.4446665812863,89.2199754596173,107.));
#41988=CARTESIAN_POINT('Ctrl Pts',(-38.501396469585,89.1538710878815,107.));
#41989=CARTESIAN_POINT('Ctrl Pts',(-38.5545716594879,89.0847462416478,107.));
#41990=CARTESIAN_POINT('Ctrl Pts',(-38.6041503825645,89.0129594416844,107.));
#41991=CARTESIAN_POINT('Ctrl Pts',(-38.617088116682,88.9942264353979,107.));
#41992=CARTESIAN_POINT('Ctrl Pts',(-38.6297807726147,88.9753119423136,107.));
#41993=CARTESIAN_POINT('Ctrl Pts',(-38.6422272327037,88.9562219002017,107.));
#41994=CARTESIAN_POINT('Ctrl Pts',(-38.6523972170385,88.9406234547127,107.));
#41995=CARTESIAN_POINT('Ctrl Pts',(-38.662403269216,88.9249068962603,107.));
#41996=CARTESIAN_POINT('Ctrl Pts',(-38.6722359315353,88.9090900594939,107.));
#41997=CARTESIAN_POINT('Ctrl Pts',(-38.7196800505418,88.8327713716876,107.));
#41998=CARTESIAN_POINT('Ctrl Pts',(-38.7631406056323,88.7540453242351,107.));
#41999=CARTESIAN_POINT('Ctrl Pts',(-38.8025829106836,88.67330446842,107.));
#42000=CARTESIAN_POINT('Ctrl Pts',(-38.8344113785719,88.6081496116427,107.));
#42001=CARTESIAN_POINT('Ctrl Pts',(-38.8636227066877,88.5416816457212,107.));
#42002=CARTESIAN_POINT('Ctrl Pts',(-38.8901815095572,88.474089043938,107.));
#42003=CARTESIAN_POINT('Ctrl Pts',(-38.9007829847814,88.4471081104725,107.));
#42004=CARTESIAN_POINT('Ctrl Pts',(-38.9109616320996,88.4199478294018,107.));
#42005=CARTESIAN_POINT('Ctrl Pts',(-38.9207144403471,88.3926196422929,107.));
#42006=CARTESIAN_POINT('Ctrl Pts',(-38.9259553817286,88.3779340847521,107.));
#42007=CARTESIAN_POINT('Ctrl Pts',(-38.9310729716149,88.3632008585835,107.));
#42008=CARTESIAN_POINT('Ctrl Pts',(-38.9360627431239,88.3484342176154,107.));
#42009=CARTESIAN_POINT('Ctrl Pts',(-38.9656015479925,88.2610176043829,107.));
#42010=CARTESIAN_POINT('Ctrl Pts',(-38.9907048899124,88.1723198874215,107.));
#42011=CARTESIAN_POINT('Ctrl Pts',(-39.0113402006962,88.082738876299,107.));
#42012=CARTESIAN_POINT('Ctrl Pts',(-39.0322969781321,87.9917623297253,107.));
#42013=CARTESIAN_POINT('Ctrl Pts',(-39.0486459305825,87.8998739484332,107.));
#42014=CARTESIAN_POINT('Ctrl Pts',(-39.0603111188663,87.8074572392324,107.));
#42015=CARTESIAN_POINT('Ctrl Pts',(-39.0718855922787,87.7157592128064,107.));
#42016=CARTESIAN_POINT('Ctrl Pts',(-39.0788492094664,87.6235401137,107.));
#42017=CARTESIAN_POINT('Ctrl Pts',(-39.0810808446038,87.5311553610101,107.));
#42018=CARTESIAN_POINT('Ctrl Pts',(-39.0821914618531,87.4851782663684,107.));
#42019=CARTESIAN_POINT('Ctrl Pts',(-39.0821293210671,87.4391599303236,107.));
#42020=CARTESIAN_POINT('Ctrl Pts',(-39.0808746940999,87.3931434632704,107.));
#42021=CARTESIAN_POINT('Ctrl Pts',(-39.0805049187082,87.3795810598021,107.));
#42022=CARTESIAN_POINT('Ctrl Pts',(-39.0800315353698,87.3660188180032,107.));
#42023=CARTESIAN_POINT('Ctrl Pts',(-39.0794539826403,87.3524578415654,107.));
#42024=CARTESIAN_POINT('Ctrl Pts',(-39.0788334726149,87.3378882249662,107.));
#42025=CARTESIAN_POINT('Ctrl Pts',(-39.0780931235918,87.3233298551507,107.));
#42026=CARTESIAN_POINT('Ctrl Pts',(-39.0772328870959,87.3087866606173,107.));
#42027=CARTESIAN_POINT('Ctrl Pts',(-39.071581078401,87.2132369441038,107.));
#42028=CARTESIAN_POINT('Ctrl Pts',(-39.0607566330613,87.1183089467729,107.));
#42029=CARTESIAN_POINT('Ctrl Pts',(-39.0446890962994,87.0243983125872,107.));
#42030=CARTESIAN_POINT('Ctrl Pts',(-39.0423087640973,87.0104858809568,107.));
#42031=CARTESIAN_POINT('Ctrl Pts',(-39.039813274356,86.9965957440252,107.));
#42032=CARTESIAN_POINT('Ctrl Pts',(-39.0372023054818,86.9827291574775,107.));
#42033=CARTESIAN_POINT('Ctrl Pts',(-39.020256651193,86.8927325343363,107.));
#42034=CARTESIAN_POINT('Ctrl Pts',(-38.998451114988,86.8037280854647,107.));
#42035=CARTESIAN_POINT('Ctrl Pts',(-38.9720882464109,86.7159480589121,107.));
#42036=CARTESIAN_POINT('Ctrl Pts',(-38.9451294332351,86.626183725055,107.));
#42037=CARTESIAN_POINT('Ctrl Pts',(-38.9134047085586,86.5376990962214,107.));
#42038=CARTESIAN_POINT('Ctrl Pts',(-38.8771833655368,86.4507462170881,107.));
#42039=CARTESIAN_POINT('Ctrl Pts',(-38.8646932387025,86.4207624451355,107.));
#42040=CARTESIAN_POINT('Ctrl Pts',(-38.8516679859885,86.3909608889171,107.));
#42041=CARTESIAN_POINT('Ctrl Pts',(-38.838117277065,86.3613522223643,107.));
#42042=CARTESIAN_POINT('Ctrl Pts',(-38.8314262146987,86.3467320696029,107.));
#42043=CARTESIAN_POINT('Ctrl Pts',(-38.8246070262069,86.3321589503315,107.));
#42044=CARTESIAN_POINT('Ctrl Pts',(-38.8176608165039,86.3176341721329,107.));
#42045=CARTESIAN_POINT('Ctrl Pts',(-38.8121670423093,86.3061464896326,107.));
#42046=CARTESIAN_POINT('Ctrl Pts',(-38.8065942532154,86.2946900708772,107.));
#42047=CARTESIAN_POINT('Ctrl Pts',(-38.8009475899525,86.283274492168,107.));
#42048=CARTESIAN_POINT('Ctrl Pts',(-38.758223644909,86.1969016141157,107.));
#42049=CARTESIAN_POINT('Ctrl Pts',(-38.7112088421257,86.1127270557926,107.));
#42050=CARTESIAN_POINT('Ctrl Pts',(-38.660245836794,86.0310004544778,107.));
#42051=CARTESIAN_POINT('Ctrl Pts',(-38.6082721210866,85.9476530318752,107.));
#42052=CARTESIAN_POINT('Ctrl Pts',(-38.5521917328472,85.8668508545203,107.));
#42053=CARTESIAN_POINT('Ctrl Pts',(-38.4923131112639,85.7888657379894,107.));
#42054=CARTESIAN_POINT('Ctrl Pts',(-38.4319476605325,85.7102465816819,107.));
#42055=CARTESIAN_POINT('Ctrl Pts',(-38.3677215052906,85.6344896425683,107.));
#42056=CARTESIAN_POINT('Ctrl Pts',(-38.299901338034,85.5618926996275,107.));
#42057=CARTESIAN_POINT('Ctrl Pts',(-38.262900667006,85.5222859615134,107.));
#42058=CARTESIAN_POINT('Ctrl Pts',(-38.2248294325612,85.4836201949921,107.));
#42059=CARTESIAN_POINT('Ctrl Pts',(-38.1857255936742,85.4459475341521,107.));
#42060=CARTESIAN_POINT('Ctrl Pts',(-38.1737580085947,85.4344179558138,107.));
#42061=CARTESIAN_POINT('Ctrl Pts',(-38.1616936808026,85.4229814184087,107.));
#42062=CARTESIAN_POINT('Ctrl Pts',(-38.1495336354026,85.4116394784339,107.));
#42063=CARTESIAN_POINT('Ctrl Pts',(-38.1389878579288,85.4018032014168,107.));
#42064=CARTESIAN_POINT('Ctrl Pts',(-38.1283712028283,85.3920391899121,107.));
#42065=CARTESIAN_POINT('Ctrl Pts',(-38.1176934507031,85.3823564375337,107.));
#42066=CARTESIAN_POINT('Ctrl Pts',(-38.0421189670067,85.3138243154934,107.));
#42067=CARTESIAN_POINT('Ctrl Pts',(-37.9633677633205,85.2492485396459,107.));
#42068=CARTESIAN_POINT('Ctrl Pts',(-37.8817671861085,85.1889108818132,107.));
#42069=CARTESIAN_POINT('Ctrl Pts',(-37.8000624207147,85.1284961844413,107.));
#42070=CARTESIAN_POINT('Ctrl Pts',(-37.7155004275651,85.0723295959512,107.));
#42071=CARTESIAN_POINT('Ctrl Pts',(-37.6283645341542,85.0207197688895,107.));
#42072=CARTESIAN_POINT('Ctrl Pts',(-37.5429608768295,84.9701359301014,107.));
#42073=CARTESIAN_POINT('Ctrl Pts',(-37.4550839747521,84.9239288015609,107.));
#42074=CARTESIAN_POINT('Ctrl Pts',(-37.3649665022594,84.8824247956419,107.));
#42075=CARTESIAN_POINT('Ctrl Pts',(-37.3246172470079,84.8638417652653,107.));
#42076=CARTESIAN_POINT('Ctrl Pts',(-37.2838184192053,84.8462021227698,107.));
#42077=CARTESIAN_POINT('Ctrl Pts',(-37.2425891498101,84.8295381139694,107.));
#42078=CARTESIAN_POINT('Ctrl Pts',(-37.2121695076316,84.817243130517,107.));
#42079=CARTESIAN_POINT('Ctrl Pts',(-37.1815155207895,84.8054792999133,107.));
#42080=CARTESIAN_POINT('Ctrl Pts',(-37.1506394582515,84.7942439414617,107.));
#42081=CARTESIAN_POINT('Ctrl Pts',(-35.5611267921506,84.7993326348266,107.));
#42082=CARTESIAN_POINT('Ctrl Pts',(-35.4662928667291,84.8340233083661,107.));
#42083=CARTESIAN_POINT('Ctrl Pts',(-35.373502094942,84.8737048604511,107.));
#42084=CARTESIAN_POINT('Ctrl Pts',(-35.2829954003415,84.9180569417674,107.));
#42085=CARTESIAN_POINT('Ctrl Pts',(-35.1912158404665,84.9630327805242,107.));
#42086=CARTESIAN_POINT('Ctrl Pts',(-35.1017843865515,85.0128121445763,107.));
#42087=CARTESIAN_POINT('Ctrl Pts',(-35.0149862950964,85.0671016605279,107.));
#42088=CARTESIAN_POINT('Ctrl Pts',(-34.9904732710836,85.0824337972818,107.));
#42089=CARTESIAN_POINT('Ctrl Pts',(-34.9661705183484,85.098125863753,107.));
#42090=CARTESIAN_POINT('Ctrl Pts',(-34.9420850585175,85.1141717075186,107.));
#42091=CARTESIAN_POINT('Ctrl Pts',(-34.9227555338565,85.1270491254692,107.));
#42092=CARTESIAN_POINT('Ctrl Pts',(-34.9035638566542,85.1401560264525,107.));
#42093=CARTESIAN_POINT('Ctrl Pts',(-34.8845329423808,85.1534754654736,107.));
#42094=CARTESIAN_POINT('Ctrl Pts',(-34.8018258386928,85.211360872783,107.));
#42095=CARTESIAN_POINT('Ctrl Pts',(-34.7220735941393,85.2733084226108,107.));
#42096=CARTESIAN_POINT('Ctrl Pts',(-34.6455425705562,85.3390207553953,107.));
#42097=CARTESIAN_POINT('Ctrl Pts',(-34.5865493779202,85.3896744658125,107.));
#42098=CARTESIAN_POINT('Ctrl Pts',(-34.5294708526726,85.442566101346,107.));
#42099=CARTESIAN_POINT('Ctrl Pts',(-34.4744465628682,85.4975712321909,107.));
#42100=CARTESIAN_POINT('Ctrl Pts',(-34.4451578114394,85.5268497855414,107.));
#42101=CARTESIAN_POINT('Ctrl Pts',(-34.4164513632894,85.5567273046795,107.));
#42102=CARTESIAN_POINT('Ctrl Pts',(-34.388350288722,85.5871858552371,107.));
#42103=CARTESIAN_POINT('Ctrl Pts',(-34.3787142836071,85.5976302511715,107.));
#42104=CARTESIAN_POINT('Ctrl Pts',(-34.3691501941652,85.6081422590004,107.));
#42105=CARTESIAN_POINT('Ctrl Pts',(-34.3596655870238,85.6187135430261,107.));
#42106=CARTESIAN_POINT('Ctrl Pts',(-34.2938683933846,85.6920492976525,107.));
#42107=CARTESIAN_POINT('Ctrl Pts',(-34.2318033500797,85.7683316754912,107.));
#42108=CARTESIAN_POINT('Ctrl Pts',(-34.1737142259206,85.8472821195271,107.));
#42109=CARTESIAN_POINT('Ctrl Pts',(-34.1161515595356,85.9255170410685,107.));
#42110=CARTESIAN_POINT('Ctrl Pts',(-34.0624926380258,86.0063726715474,107.));
#42111=CARTESIAN_POINT('Ctrl Pts',(-34.0130204055193,86.0896003448039,107.));
#42112=CARTESIAN_POINT('Ctrl Pts',(-33.964962467509,86.170448735092,107.));
#42113=CARTESIAN_POINT('Ctrl Pts',(-33.92085505662,86.2535361835536,107.));
#42114=CARTESIAN_POINT('Ctrl Pts',(-33.8810053242648,86.3386450701133,107.));
#42115=CARTESIAN_POINT('Ctrl Pts',(-33.8602009063501,86.3830780120577,107.));
#42116=CARTESIAN_POINT('Ctrl Pts',(-33.8405577745803,86.4280620243428,107.));
#42117=CARTESIAN_POINT('Ctrl Pts',(-33.8221253291101,86.4735663764393,107.));
#42118=CARTESIAN_POINT('Ctrl Pts',(-33.8150672434759,86.4909907390581,107.));
#42119=CARTESIAN_POINT('Ctrl Pts',(-33.8081867174046,86.5084913952829,107.));
#42120=CARTESIAN_POINT('Ctrl Pts',(-33.8014866864851,86.5260666110052,107.));
#42121=CARTESIAN_POINT('Ctrl Pts',(-33.7962449527397,86.5398164880495,107.));
#42122=CARTESIAN_POINT('Ctrl Pts',(-33.791113595039,86.5536125010622,107.));
#42123=CARTESIAN_POINT('Ctrl Pts',(-33.7860991485526,86.5674391067525,107.));
#42124=CARTESIAN_POINT('Ctrl Pts',(-33.7544154646644,86.6548022494497,107.));
#42125=CARTESIAN_POINT('Ctrl Pts',(-33.7273406062928,86.7435263402015,107.));
#42126=CARTESIAN_POINT('Ctrl Pts',(-33.705125829678,86.8333878288782,107.));
#42127=CARTESIAN_POINT('Ctrl Pts',(-33.7001418550498,86.8535486158801,107.));
#42128=CARTESIAN_POINT('Ctrl Pts',(-33.6954027145293,86.8737666931234,107.));
#42129=CARTESIAN_POINT('Ctrl Pts',(-33.6909116062639,86.8940395916533,107.));
#42130=CARTESIAN_POINT('Ctrl Pts',(-33.6705458557277,86.9859707520051,107.));
#42131=CARTESIAN_POINT('Ctrl Pts',(-33.6552763187112,87.0790295393631,107.));
#42132=CARTESIAN_POINT('Ctrl Pts',(-33.6449931699608,87.1728243655036,107.));
#42133=CARTESIAN_POINT('Ctrl Pts',(-33.6342593131593,87.2707301973596,107.));
#42134=CARTESIAN_POINT('Ctrl Pts',(-33.6289585408132,87.3694392403859,107.));
#42135=CARTESIAN_POINT('Ctrl Pts',(-33.6290234054697,87.4684914760975,107.));
#42136=CARTESIAN_POINT('Ctrl Pts',(-33.6290487774748,87.5072360553908,107.));
#42137=CARTESIAN_POINT('Ctrl Pts',(-33.6298956946779,87.5460328865882,107.));
#42138=CARTESIAN_POINT('Ctrl Pts',(-33.6315623444562,87.5848532118375,107.));
#42139=CARTESIAN_POINT('Ctrl Pts',(-33.6320953845293,87.5972690110524,107.));
#42140=CARTESIAN_POINT('Ctrl Pts',(-33.6327122710738,87.6096859021259,107.));
#42141=CARTESIAN_POINT('Ctrl Pts',(-33.6334122429631,87.6220932757044,107.));
#42142=CARTESIAN_POINT('Ctrl Pts',(-33.638651466045,87.7149612880346,107.));
#42143=CARTESIAN_POINT('Ctrl Pts',(-33.648547110654,87.807446071697,107.));
#42144=CARTESIAN_POINT('Ctrl Pts',(-33.6629757175006,87.8991760479908,107.));
#42145=CARTESIAN_POINT('Ctrl Pts',(-33.6773703353928,87.9906899392528,107.));
#42146=CARTESIAN_POINT('Ctrl Pts',(-33.696276994312,88.0814535204309,107.));
#42147=CARTESIAN_POINT('Ctrl Pts',(-33.7196217814369,88.1710808801793,107.));
#42148=CARTESIAN_POINT('Ctrl Pts',(-33.7425704165735,88.2591872983752,107.));
#42149=CARTESIAN_POINT('Ctrl Pts',(-33.7698082987973,88.3461965157412,107.));
#42150=CARTESIAN_POINT('Ctrl Pts',(-33.8013056556184,88.4317128384291,107.));
#42151=CARTESIAN_POINT('Ctrl Pts',(-33.8171471032868,88.4747228712503,107.));
#42152=CARTESIAN_POINT('Ctrl Pts',(-33.8340666009129,88.5173547357403,107.));
#42153=CARTESIAN_POINT('Ctrl Pts',(-33.8520637782135,88.5595543004123,107.));
#42154=CARTESIAN_POINT('Ctrl Pts',(-33.8576294800274,88.5726046910218,107.));
#42155=CARTESIAN_POINT('Ctrl Pts',(-33.8632982646163,88.5856137165589,107.));
#42156=CARTESIAN_POINT('Ctrl Pts',(-33.8690701619053,88.5985797184015,107.));
#42157=CARTESIAN_POINT('Ctrl Pts',(-33.8747496320563,88.6113380917329,107.));
#42158=CARTESIAN_POINT('Ctrl Pts',(-33.8805254577359,88.6240469437888,107.));
#42159=CARTESIAN_POINT('Ctrl Pts',(-33.886395849193,88.6367017889012,107.));
#42160=CARTESIAN_POINT('Ctrl Pts',(-33.9238756556946,88.7174972775129,107.));
#42161=CARTESIAN_POINT('Ctrl Pts',(-33.9652256181719,88.7961359866757,107.));
#42162=CARTESIAN_POINT('Ctrl Pts',(-34.0103760601782,88.8722703240689,107.));
#42163=CARTESIAN_POINT('Ctrl Pts',(-34.0547690647657,88.9471274426035,107.));
#42164=CARTESIAN_POINT('Ctrl Pts',(-34.1028365599303,89.0195641800131,107.));
#42165=CARTESIAN_POINT('Ctrl Pts',(-34.1545485303629,89.0892159682587,107.));
#42166=CARTESIAN_POINT('Ctrl Pts',(-34.2046829766307,89.1567429606752,107.));
#42167=CARTESIAN_POINT('Ctrl Pts',(-34.2582433760492,89.2216527685488,107.));
#42168=CARTESIAN_POINT('Ctrl Pts',(-34.3152300879658,89.2835728963379,107.));
#42169=CARTESIAN_POINT('Ctrl Pts',(-34.3361977081016,89.3063557113939,107.));
#42170=CARTESIAN_POINT('Ctrl Pts',(-34.3576294231801,89.3287333523195,107.));
#42171=CARTESIAN_POINT('Ctrl Pts',(-34.3795260622952,89.3506856545374,107.));
#42172=CARTESIAN_POINT('Ctrl Pts',(-34.3986034990632,89.3698115877581,107.));
#42173=CARTESIAN_POINT('Ctrl Pts',(-34.4180338691283,89.3886146337316,107.));
#42174=CARTESIAN_POINT('Ctrl Pts',(-34.4378070356397,89.4070896639596,107.));
#42175=CARTESIAN_POINT('Origin',(-36.3549260746835,87.7685555885722,124.208423447177));
#42176=CARTESIAN_POINT('Ctrl Pts',(-39.4317255112881,87.7704831500192,121.708423447178));
#42177=CARTESIAN_POINT('Ctrl Pts',(-39.4326481971992,87.8937580425098,121.702019850418));
#42178=CARTESIAN_POINT('Ctrl Pts',(-39.3701217699364,89.029664773114,121.642966745928));
#42179=CARTESIAN_POINT('Ctrl Pts',(-37.9573947132227,91.0220940158023,121.531264133707));
#42180=CARTESIAN_POINT('Ctrl Pts',(-34.5067287733102,90.8887185705161,121.373315610515));
#42181=CARTESIAN_POINT('Ctrl Pts',(-32.7318387507372,87.9267773779968,121.215367087322));
#42182=CARTESIAN_POINT('Ctrl Pts',(-34.2418569809606,84.8211911081587,121.05741856413));
#42183=CARTESIAN_POINT('Ctrl Pts',(-37.6677476301795,84.3879830560575,120.899470040937));
#42184=CARTESIAN_POINT('Ctrl Pts',(-39.314294541848,86.3263542158685,120.783138335287));
#42185=CARTESIAN_POINT('Ctrl Pts',(-39.4311721662448,87.5529959287177,120.719456137367));
#42186=CARTESIAN_POINT('Ctrl Pts',(-39.4292403360613,87.7658718692203,120.708423447177));
#42187=CARTESIAN_POINT('Ctrl Pts',(-39.4252046869538,87.7655406593158,121.791576552823));
#42188=CARTESIAN_POINT('Ctrl Pts',(-39.4202197564572,88.4585591084465,121.755752019753));
#42189=CARTESIAN_POINT('Ctrl Pts',(-38.8478323893262,90.1797487563936,121.667277978953));
#42190=CARTESIAN_POINT('Ctrl Pts',(-36.0033917073514,91.3774170351665,121.526154430422));
#42191=CARTESIAN_POINT('Ctrl Pts',(-33.1409989526284,89.4482950386239,121.36820590723));
#42192=CARTESIAN_POINT('Ctrl Pts',(-33.1913893007143,85.9950129878222,121.210257384038));
#42193=CARTESIAN_POINT('Ctrl Pts',(-36.1106392417851,84.1503274667491,121.052308860845));
#42194=CARTESIAN_POINT('Ctrl Pts',(-38.8854864734731,85.418769658119,120.912748583773));
#42195=CARTESIAN_POINT('Ctrl Pts',(-39.4210162770085,87.1075071559934,120.825837814433));
#42196=CARTESIAN_POINT('Ctrl Pts',(-39.4253674987814,87.7707064726519,120.791576552823));
#42197=CARTESIAN_POINT('Ctrl Pts',(-34.4414600780185,89.4045427919472,122.));
#42198=CARTESIAN_POINT('Ctrl Pts',(-33.9002646916968,88.7715555857257,121.947350492269));
#42199=CARTESIAN_POINT('Ctrl Pts',(-33.5049255901432,86.9365247300264,121.842051476807));
#42200=CARTESIAN_POINT('Ctrl Pts',(-35.4957255906178,84.923355640163,121.684102953615));
#42201=CARTESIAN_POINT('Ctrl Pts',(-38.2666279976808,85.4956008231392,121.526154430423));
#42202=CARTESIAN_POINT('Ctrl Pts',(-39.3037452232225,88.1258670336349,121.36820590723));
#42203=CARTESIAN_POINT('Ctrl Pts',(-37.6675061291889,90.4335248387924,121.210257384038));
#42204=CARTESIAN_POINT('Ctrl Pts',(-34.841069980261,90.3242771786304,121.052308860845));
#42205=CARTESIAN_POINT('Ctrl Pts',(-33.3872597860761,87.8981548580944,120.894360337653));
#42206=CARTESIAN_POINT('Ctrl Pts',(-34.6241138269375,85.3543730346626,120.73641181446));
#42207=CARTESIAN_POINT('Ctrl Pts',(-37.4302565662928,84.9995328618419,120.578463291268));
#42208=CARTESIAN_POINT('Ctrl Pts',(-39.2614231073442,87.1552445435626,120.420514768075));
#42209=CARTESIAN_POINT('Ctrl Pts',(-38.4573604664392,89.8670446085888,120.262566244883));
#42210=CARTESIAN_POINT('Ctrl Pts',(-35.747082910027,90.6761997920055,120.10461772169));
#42211=CARTESIAN_POINT('Ctrl Pts',(-33.5879190399563,88.8490866434182,119.946669198498));
#42212=CARTESIAN_POINT('Ctrl Pts',(-33.9375159163837,86.0422867908315,119.788720675305));
#42213=CARTESIAN_POINT('Ctrl Pts',(-36.4789052445403,84.8006433564885,119.630772152113));
#42214=CARTESIAN_POINT('Ctrl Pts',(-38.9078863408608,86.2499151910518,119.47282362892));
#42215=CARTESIAN_POINT('Ctrl Pts',(-39.0221760519813,89.0760923234738,119.314875105728));
#42216=CARTESIAN_POINT('Ctrl Pts',(-36.7181513083396,90.7167655501525,119.156926582536));
#42217=CARTESIAN_POINT('Ctrl Pts',(-34.084801302592,89.6843865264073,118.998978059343));
#42218=CARTESIAN_POINT('Ctrl Pts',(-33.5097043799898,86.9149818314663,118.841029536151));
#42219=CARTESIAN_POINT('Ctrl Pts',(-35.5142834368846,84.9194865150593,118.683081012958));
#42220=CARTESIAN_POINT('Ctrl Pts',(-38.2810476053028,85.5071554706503,118.525132489766));
#42221=CARTESIAN_POINT('Ctrl Pts',(-39.3014559628199,88.1451671389155,118.367183966573));
#42222=CARTESIAN_POINT('Ctrl Pts',(-37.6503352851408,90.4417165670853,118.209235443381));
#42223=CARTESIAN_POINT('Ctrl Pts',(-34.8247064745657,90.3145922372931,118.051286920188));
#42224=CARTESIAN_POINT('Ctrl Pts',(-33.3864812358262,87.8790539119505,117.893338396996));
#42225=CARTESIAN_POINT('Ctrl Pts',(-34.6396546513419,85.3433301176302,117.735389873803));
#42226=CARTESIAN_POINT('Ctrl Pts',(-37.4480124987638,85.0064844978296,117.577441350611));
#42227=CARTESIAN_POINT('Ctrl Pts',(-39.2653021302004,87.1739247314519,117.419492827418));
#42228=CARTESIAN_POINT('Ctrl Pts',(-38.4438423071828,89.8804986783248,117.261544304226));
#42229=CARTESIAN_POINT('Ctrl Pts',(-35.7284256676752,90.6722380575748,117.103595781034));
#42230=CARTESIAN_POINT('Ctrl Pts',(-33.5810378930527,88.8312968536853,116.945647257841));
#42231=CARTESIAN_POINT('Ctrl Pts',(-33.9486501687198,86.0268004665349,116.787698734649));
#42232=CARTESIAN_POINT('Ctrl Pts',(-36.4979596247505,84.8015004754471,116.629750211456));
#42233=CARTESIAN_POINT('Ctrl Pts',(-38.9175849111044,86.2663391165282,116.471801688264));
#42234=CARTESIAN_POINT('Ctrl Pts',(-39.0137253702208,89.0931917449628,116.313853165071));
#42235=CARTESIAN_POINT('Ctrl Pts',(-36.6992133717988,90.7190370573856,116.155904641879));
#42236=CARTESIAN_POINT('Ctrl Pts',(-34.0725465521072,89.669770556873,115.997956118686));
#42237=CARTESIAN_POINT('Ctrl Pts',(-33.5152438301002,86.8967302674414,115.840007595494));
#42238=CARTESIAN_POINT('Ctrl Pts',(-35.5325946342255,84.9141474813107,115.682059072301));
#42239=CARTESIAN_POINT('Ctrl Pts',(-38.2955283453338,85.5195697131357,115.524110549109));
#42240=CARTESIAN_POINT('Ctrl Pts',(-39.2989769983936,88.1640790384055,115.366162025916));
#42241=CARTESIAN_POINT('Ctrl Pts',(-37.6331442181869,90.4499792810135,115.208213502724));
#42242=CARTESIAN_POINT('Ctrl Pts',(-34.8083899225131,90.3047142135001,115.050264979531));
#42243=CARTESIAN_POINT('Ctrl Pts',(-33.3858329202414,87.8599912545425,114.892316456339));
#42244=CARTESIAN_POINT('Ctrl Pts',(-34.6552623802161,85.3323663581397,114.734367933147));
#42245=CARTESIAN_POINT('Ctrl Pts',(-37.4657252190298,85.0135601436239,114.576419409954));
#42246=CARTESIAN_POINT('Ctrl Pts',(-39.2690602570936,87.192624509644,114.418470886762));
#42247=CARTESIAN_POINT('Ctrl Pts',(-38.430238461351,89.8938680687762,114.260522363569));
#42248=CARTESIAN_POINT('Ctrl Pts',(-35.7097940423901,90.6681554405648,114.102573840377));
#42249=CARTESIAN_POINT('Ctrl Pts',(-33.5742712163058,88.8134638138948,113.944625317184));
#42250=CARTESIAN_POINT('Ctrl Pts',(-33.959883580518,86.0113856787719,113.786676793992));
#42251=CARTESIAN_POINT('Ctrl Pts',(-36.5170081322653,84.802480058958,113.628728270799));
#42252=CARTESIAN_POINT('Ctrl Pts',(-38.9271778119062,86.2828249127359,113.470779747607));
#42253=CARTESIAN_POINT('Ctrl Pts',(-39.0051650729075,89.1102365838387,113.312831224414));
#42254=CARTESIAN_POINT('Ctrl Pts',(-36.6802612375947,90.7211869019163,113.154882701222));
#42255=CARTESIAN_POINT('Ctrl Pts',(-34.060385904692,89.655076208407,112.996934178029));
#42256=CARTESIAN_POINT('Ctrl Pts',(-33.5209003586359,86.8785146448246,112.838985654837));
#42257=CARTESIAN_POINT('Ctrl Pts',(-35.5509397363243,84.9089261355665,112.681037131644));
#42258=CARTESIAN_POINT('Ctrl Pts',(-38.3099290748638,85.5320766796504,112.523088608452));
#42259=CARTESIAN_POINT('Ctrl Pts',(-39.2963766518683,88.1829746310225,112.365140085259));
#42260=CARTESIAN_POINT('Ctrl Pts',(-37.6159004507148,90.4581314405903,112.207191562067));
#42261=CARTESIAN_POINT('Ctrl Pts',(-34.7921371336156,90.2947316248854,112.049243038875));
#42262=CARTESIAN_POINT('Ctrl Pts',(-33.385307019306,87.8409248272262,111.891294515682));
#42263=CARTESIAN_POINT('Ctrl Pts',(-34.6709401856254,85.321503041891,111.73334599249));
#42264=CARTESIAN_POINT('Ctrl Pts',(-37.4833921414399,85.0207493768912,111.575397469297));
#42265=CARTESIAN_POINT('Ctrl Pts',(-39.272698235267,87.2113480332777,111.417448946105));
#42266=CARTESIAN_POINT('Ctrl Pts',(-38.4165490511289,89.907149833341,111.259500422912));
#42267=CARTESIAN_POINT('Ctrl Pts',(-35.6911890156619,90.6639532740908,111.10155189972));
#42268=CARTESIAN_POINT('Ctrl Pts',(-33.5676191849894,88.795587692891,110.943603376527));
#42269=CARTESIAN_POINT('Ctrl Pts',(-33.9712157390344,85.9960433385363,110.785654853335));
#42270=CARTESIAN_POINT('Ctrl Pts',(-36.5360499572654,84.8035819326398,110.627706330142));
#42271=CARTESIAN_POINT('Ctrl Pts',(-38.9366646595351,86.2993719652391,110.46975780695));
#42272=CARTESIAN_POINT('Ctrl Pts',(-38.9964955074805,89.1272261053812,110.311809283757));
#42273=CARTESIAN_POINT('Ctrl Pts',(-36.6612956893197,90.7232150111251,110.153860760565));
#42274=CARTESIAN_POINT('Ctrl Pts',(-34.0483198616244,89.6403040780895,109.995912237372));
#42275=CARTESIAN_POINT('Ctrl Pts',(-33.5266737304351,86.8603357209029,109.83796371418));
#42276=CARTESIAN_POINT('Ctrl Pts',(-35.569317991866,84.9038226859369,109.680015190988));
#42277=CARTESIAN_POINT('Ctrl Pts',(-38.3242491892674,85.5446758664894,109.522066667795));
#42278=CARTESIAN_POINT('Ctrl Pts',(-39.2936550530951,88.2018531144783,109.364118144603));
#42279=CARTESIAN_POINT('Ctrl Pts',(-37.5986046470003,90.4661727568194,109.20616962141));
#42280=CARTESIAN_POINT('Ctrl Pts',(-34.775948874024,90.284644786456,109.048221098218));
#42281=CARTESIAN_POINT('Ctrl Pts',(-33.3849033571381,87.8218556145483,108.890272575025));
#42282=CARTESIAN_POINT('Ctrl Pts',(-34.686687827486,85.3107402087474,108.732324051833));
#42283=CARTESIAN_POINT('Ctrl Pts',(-37.5010117020144,85.0280527402971,108.57437552864));
#42284=CARTESIAN_POINT('Ctrl Pts',(-39.276217633105,87.2300928048423,108.416427005448));
#42285=CARTESIAN_POINT('Ctrl Pts',(-38.4027711070691,89.9203469730075,108.258478482255));
#42286=CARTESIAN_POINT('Ctrl Pts',(-35.6726186219733,90.6596244337072,108.100529959063));
#42287=CARTESIAN_POINT('Ctrl Pts',(-33.5610671278939,88.7776842354716,107.94258143587));
#42288=CARTESIAN_POINT('Ctrl Pts',(-33.9826769125213,85.9807432147986,107.784632912678));
#42289=CARTESIAN_POINT('Ctrl Pts',(-36.5550211069366,84.8048695224416,107.626684389486));
#42290=CARTESIAN_POINT('Ctrl Pts',(-38.9461750506382,86.3158490632487,107.468735866293));
#42291=CARTESIAN_POINT('Ctrl Pts',(-38.987449710725,89.144428091839,107.3107873431));
#42292=CARTESIAN_POINT('Ctrl Pts',(-36.6428674306544,90.7245693543756,107.152838819908));
#42293=CARTESIAN_POINT('Ctrl Pts',(-34.0352179374292,89.6266035901596,106.994890296715));
#42294=CARTESIAN_POINT('Ctrl Pts',(-33.5349383123317,86.8398752713272,106.836941773523));
#42295=CARTESIAN_POINT('Ctrl Pts',(-34.9001756782213,85.551559245903,106.731642758061));
#42296=CARTESIAN_POINT('Ctrl Pts',(-35.7047260767084,85.3364687865372,106.678993250331));
#42297=CARTESIAN_POINT('Ctrl Pts',(-34.3005945243415,89.5249809097991,122.10700224989));
#42298=CARTESIAN_POINT('Ctrl Pts',(-33.7195574121284,88.8453944468204,122.054352742159));
#42299=CARTESIAN_POINT('Ctrl Pts',(-33.2951142337176,86.8752722762228,121.949053726697));
#42300=CARTESIAN_POINT('Ctrl Pts',(-35.4324729631248,84.7138976896414,121.791105203505));
#42301=CARTESIAN_POINT('Ctrl Pts',(-38.4073636837697,85.328270422665,121.633156680312));
#42302=CARTESIAN_POINT('Ctrl Pts',(-39.5208314127741,88.1521715901997,121.47520815712));
#42303=CARTESIAN_POINT('Ctrl Pts',(-37.7641356572001,90.6297145644623,121.317259633928));
#42304=CARTESIAN_POINT('Ctrl Pts',(-34.7296229112774,90.5124243092589,121.159311110735));
#42305=CARTESIAN_POINT('Ctrl Pts',(-33.1687861076298,87.9076956980619,121.001362587543));
#42306=CARTESIAN_POINT('Ctrl Pts',(-34.4966948782785,85.176645725828,120.84341406435));
#42307=CARTESIAN_POINT('Ctrl Pts',(-37.5094202542551,84.7956829265805,120.685465541158));
#42308=CARTESIAN_POINT('Ctrl Pts',(-39.4753936270609,87.1100938065847,120.527517017965));
#42309=CARTESIAN_POINT('Ctrl Pts',(-38.6121374968021,90.0215311885463,120.369568494773));
#42310=CARTESIAN_POINT('Ctrl Pts',(-35.7023347075049,90.8902547641484,120.21161997158));
#42311=CARTESIAN_POINT('Ctrl Pts',(-33.3842174959234,88.9286331864827,120.053671448388));
#42312=CARTESIAN_POINT('Ctrl Pts',(-33.7595509977455,85.9152023219081,119.895722925195));
#42313=CARTESIAN_POINT('Ctrl Pts',(-36.4880323439696,84.5821515721737,119.737774402003));
#42314=CARTESIAN_POINT('Ctrl Pts',(-39.0958301883279,86.1381159112078,119.57982587881));
#42315=CARTESIAN_POINT('Ctrl Pts',(-39.2185336802339,89.1723505723458,119.421877355618));
#42316=CARTESIAN_POINT('Ctrl Pts',(-36.7448912262361,90.9338068925739,119.263928832425));
#42317=CARTESIAN_POINT('Ctrl Pts',(-33.9176792405883,89.8254261823407,119.105980309233));
#42318=CARTESIAN_POINT('Ctrl Pts',(-33.3002448285499,86.8521434323996,118.94803178604));
#42319=CARTESIAN_POINT('Ctrl Pts',(-35.4523970010533,84.7097437272575,118.790083262848));
#42320=CARTESIAN_POINT('Ctrl Pts',(-38.4228448341706,85.3406757003008,118.632134739656));
#42321=CARTESIAN_POINT('Ctrl Pts',(-39.5183736215825,88.1728925307714,118.474186216463));
#42322=CARTESIAN_POINT('Ctrl Pts',(-37.7457007298299,90.6385093514682,118.316237693271));
#42323=CARTESIAN_POINT('Ctrl Pts',(-34.7120547569007,90.5020263818399,118.158289170078));
#42324=CARTESIAN_POINT('Ctrl Pts',(-33.1679502420619,87.8871885783255,118.000340646886));
#42325=CARTESIAN_POINT('Ctrl Pts',(-34.5133797872072,85.1647898512491,117.842392123693));
#42326=CARTESIAN_POINT('Ctrl Pts',(-37.5284833430919,84.803146328157,117.684443600501));
#42327=CARTESIAN_POINT('Ctrl Pts',(-39.4795582158498,87.130149192682,117.526495077308));
#42328=CARTESIAN_POINT('Ctrl Pts',(-38.5976241575991,90.0359757200862,117.368546554116));
#42329=CARTESIAN_POINT('Ctrl Pts',(-35.6823039561497,90.8860013747233,117.210598030923));
#42330=CARTESIAN_POINT('Ctrl Pts',(-33.3768297726969,88.9095337478797,117.052649507731));
#42331=CARTESIAN_POINT('Ctrl Pts',(-33.7715049315512,85.8985759252767,116.894700984538));
#42332=CARTESIAN_POINT('Ctrl Pts',(-36.5084894696809,84.5830717905218,116.736752461346));
#42333=CARTESIAN_POINT('Ctrl Pts',(-39.1062427479862,86.1557489333497,116.578803938153));
#42334=CARTESIAN_POINT('Ctrl Pts',(-39.2094608761219,89.1907088191703,116.420855414961));
#42335=CARTESIAN_POINT('Ctrl Pts',(-36.724559116545,90.9362456236433,116.262906891769));
#42336=CARTESIAN_POINT('Ctrl Pts',(-33.9045223197931,89.8097342142547,116.104958368576));
#42337=CARTESIAN_POINT('Ctrl Pts',(-33.306192081939,86.8325482246015,115.947009845384));
#42338=CARTESIAN_POINT('Ctrl Pts',(-35.4720562322533,84.7040116444835,115.789061322191));
#42339=CARTESIAN_POINT('Ctrl Pts',(-38.4383916174267,85.3540038545799,115.631112798999));
#42340=CARTESIAN_POINT('Ctrl Pts',(-39.5157121607349,88.1931966866157,115.473164275806));
#42341=CARTESIAN_POINT('Ctrl Pts',(-37.7272440907837,90.6473803499308,115.315215752614));
#42342=CARTESIAN_POINT('Ctrl Pts',(-34.6945370128002,90.4914211576192,115.157267229421));
#42343=CARTESIAN_POINT('Ctrl Pts',(-33.1672541987757,87.8667225660659,114.999318706229));
#42344=CARTESIAN_POINT('Ctrl Pts',(-34.5301365259792,85.1530189616324,114.841370183036));
#42345=CARTESIAN_POINT('Ctrl Pts',(-37.5475000385275,84.8107428688949,114.683421659844));
#42346=CARTESIAN_POINT('Ctrl Pts',(-39.483593008556,87.1502256112813,114.525473136651));
#42347=CARTESIAN_POINT('Ctrl Pts',(-38.5830188237458,90.0503293384212,114.367524613459));
#42348=CARTESIAN_POINT('Ctrl Pts',(-35.6623007077386,90.8816182035847,114.209576090267));
#42349=CARTESIAN_POINT('Ctrl Pts',(-33.369564946692,88.890387875236,114.051627567074));
#42350=CARTESIAN_POINT('Ctrl Pts',(-33.7835653247409,85.8820263315559,113.893679043881));
#42351=CARTESIAN_POINT('Ctrl Pts',(-36.5289402903607,84.5841234890188,113.735730520689));
#42352=CARTESIAN_POINT('Ctrl Pts',(-39.1165418590291,86.1734483810226,113.577781997497));
#42353=CARTESIAN_POINT('Ctrl Pts',(-39.2002703867787,89.2090084651187,113.419833474304));
#42354=CARTESIAN_POINT('Ctrl Pts',(-36.7042117639871,90.9385537354442,113.261884951112));
#42355=CARTESIAN_POINT('Ctrl Pts',(-33.8914664297479,89.7939580971363,113.103936427919));
#42356=CARTESIAN_POINT('Ctrl Pts',(-33.3122650328336,86.8129916041461,112.945987904727));
#42357=CARTESIAN_POINT('Ctrl Pts',(-35.491751864212,84.6984059136703,112.788039381534));
#42358=CARTESIAN_POINT('Ctrl Pts',(-38.4538524999681,85.3674315590464,112.630090858342));
#42359=CARTESIAN_POINT('Ctrl Pts',(-39.5129203818802,88.2134833351076,112.472142335149));
#42360=CARTESIAN_POINT('Ctrl Pts',(-37.7087308715124,90.6561326552505,112.314193811957));
#42361=CARTESIAN_POINT('Ctrl Pts',(-34.6770877259713,90.4807036707234,112.156245288764));
#42362=CARTESIAN_POINT('Ctrl Pts',(-33.1666895820614,87.8462525063644,111.998296765572));
#42363=CARTESIAN_POINT('Ctrl Pts',(-34.5469685001814,85.1413559096893,111.840348242379));
#42364=CARTESIAN_POINT('Ctrl Pts',(-37.5664675645602,84.8184613591891,111.682399719187));
#42365=CARTESIAN_POINT('Ctrl Pts',(-39.4874988074331,87.1703275234143,111.524451195995));
#42366=CARTESIAN_POINT('Ctrl Pts',(-38.5683216264223,90.0645888800265,111.366502672802));
#42367=CARTESIAN_POINT('Ctrl Pts',(-35.6423260160173,90.8771066819885,111.20855414961));
#42368=CARTESIAN_POINT('Ctrl Pts',(-33.3624232060857,88.8711957498261,111.050605626417));
#42369=CARTESIAN_POINT('Ctrl Pts',(-33.7957317341856,85.8655545188049,110.892657103225));
#42370=CARTESIAN_POINT('Ctrl Pts',(-36.5493839365723,84.5853064804455,110.734708580032));
#42371=CARTESIAN_POINT('Ctrl Pts',(-39.1267271094758,86.1912135945574,110.57676005684));
#42372=CARTESIAN_POINT('Ctrl Pts',(-39.190962585221,89.2272487213821,110.418811533647));
#42373=CARTESIAN_POINT('Ctrl Pts',(-36.683850009841,90.9407311500115,110.260863010455));
#42374=CARTESIAN_POINT('Ctrl Pts',(-33.8785121086339,89.7780984720215,110.102914487262));
#42375=CARTESIAN_POINT('Ctrl Pts',(-33.3184634287599,86.7934743840708,109.94496596407));
#42376=CARTESIAN_POINT('Ctrl Pts',(-35.511483090304,84.6929267582488,109.787017440877));
#42377=CARTESIAN_POINT('Ctrl Pts',(-38.4692268326581,85.380958272914,109.629068917685));
#42378=CARTESIAN_POINT('Ctrl Pts',(-39.5099984244287,88.233751614896,109.471120394493));
#42379=CARTESIAN_POINT('Ctrl Pts',(-37.6901617851941,90.6647659571563,109.3131718713));
#42380=CARTESIAN_POINT('Ctrl Pts',(-34.6597077189672,90.4698742593489,109.155223348108));
#42381=CARTESIAN_POINT('Ctrl Pts',(-33.1662562030891,87.8257794562487,108.997274824915));
#42382=CARTESIAN_POINT('Ctrl Pts',(-34.5638754520551,85.1298007382167,108.839326301723));
#42383=CARTESIAN_POINT('Ctrl Pts',(-37.5853842420734,84.8263023816555,108.68137777853));
#42384=CARTESIAN_POINT('Ctrl Pts',(-39.4912772963268,87.1904522477083,108.523429255338));
#42385=CARTESIAN_POINT('Ctrl Pts',(-38.5535293775764,90.0787575668171,108.365480732145));
#42386=CARTESIAN_POINT('Ctrl Pts',(-35.6223885069509,90.8724591610021,108.207532208953));
#42387=CARTESIAN_POINT('Ctrl Pts',(-33.3553887996033,88.8519742755479,108.04958368576));
#42388=CARTESIAN_POINT('Ctrl Pts',(-33.8080366564257,85.8491280304466,107.891635162568));
#42389=CARTESIAN_POINT('Ctrl Pts',(-36.5697517044782,84.5866888600426,107.733686639375));
#42390=CARTESIAN_POINT('Ctrl Pts',(-39.1369376366204,86.2089037036881,107.575738116183));
#42391=CARTESIAN_POINT('Ctrl Pts',(-39.1812508549341,89.2457170838043,107.41778959299));
#42392=CARTESIAN_POINT('Ctrl Pts',(-36.6640650994951,90.9421851973131,107.259841069798));
#42393=CARTESIAN_POINT('Ctrl Pts',(-33.8644456468879,89.7633893814714,107.101892546605));
#42394=CARTESIAN_POINT('Ctrl Pts',(-33.3273364327067,86.7715076769693,106.943944023413));
#42395=CARTESIAN_POINT('Ctrl Pts',(-34.7930798529405,85.3883483930034,106.838645007951));
#42396=CARTESIAN_POINT('Ctrl Pts',(-35.6568596485225,85.1574234026336,106.78599550022));
#42397=CARTESIAN_POINT('Ctrl Pts',(-34.1597289706644,89.645419027651,122.21400449978));
#42398=CARTESIAN_POINT('Ctrl Pts',(-33.53885013256,88.919233307915,122.161354992049));
#42399=CARTESIAN_POINT('Ctrl Pts',(-33.085302877292,86.8140198224193,122.056055976587));
#42400=CARTESIAN_POINT('Ctrl Pts',(-35.3692203356319,84.5044397391195,121.898107453395));
#42401=CARTESIAN_POINT('Ctrl Pts',(-38.5480993698586,85.160940022191,121.740158930202));
#42402=CARTESIAN_POINT('Ctrl Pts',(-39.7379176023256,88.1784761467643,121.58221040701));
#42403=CARTESIAN_POINT('Ctrl Pts',(-37.8607651852114,90.8259042901323,121.424261883817));
#42404=CARTESIAN_POINT('Ctrl Pts',(-34.6181758422938,90.7005714398875,121.266313360625));
#42405=CARTESIAN_POINT('Ctrl Pts',(-32.9503124291835,87.9172365380294,121.108364837432));
#42406=CARTESIAN_POINT('Ctrl Pts',(-34.3692759296196,84.9989184169933,120.95041631424));
#42407=CARTESIAN_POINT('Ctrl Pts',(-37.5885839422172,84.5918329913191,120.792467791047));
#42408=CARTESIAN_POINT('Ctrl Pts',(-39.6893641467774,87.0649430696068,120.634519267855));
#42409=CARTESIAN_POINT('Ctrl Pts',(-38.7669145271651,90.1760177685039,120.476570744663));
#42410=CARTESIAN_POINT('Ctrl Pts',(-35.6575865049826,91.1043097362912,120.31862222147));
#42411=CARTESIAN_POINT('Ctrl Pts',(-33.1805159518906,89.0081797295473,120.160673698278));
#42412=CARTESIAN_POINT('Ctrl Pts',(-33.5815860791074,85.7881178529846,120.002725175085));
#42413=CARTESIAN_POINT('Ctrl Pts',(-36.497159443399,84.3636597878589,119.844776651893));
#42414=CARTESIAN_POINT('Ctrl Pts',(-39.2837740357949,86.0263166313638,119.6868281287));
#42415=CARTESIAN_POINT('Ctrl Pts',(-39.4148913084864,89.2686088212177,119.528879605508));
#42416=CARTESIAN_POINT('Ctrl Pts',(-36.7716311441325,91.1508482349954,119.370931082315));
#42417=CARTESIAN_POINT('Ctrl Pts',(-33.7505571785846,89.9664658382739,119.212982559123));
#42418=CARTESIAN_POINT('Ctrl Pts',(-33.09078527711,86.789305033333,119.05503403593));
#42419=CARTESIAN_POINT('Ctrl Pts',(-35.3905105652219,84.5000009394557,118.897085512738));
#42420=CARTESIAN_POINT('Ctrl Pts',(-38.5646420630384,85.1741959299512,118.739136989545));
#42421=CARTESIAN_POINT('Ctrl Pts',(-39.735291280345,88.2006179226272,118.581188466353));
#42422=CARTESIAN_POINT('Ctrl Pts',(-37.8410661745189,90.8353021358514,118.42323994316));
#42423=CARTESIAN_POINT('Ctrl Pts',(-34.5994030392356,90.6894605263865,118.265291419968));
#42424=CARTESIAN_POINT('Ctrl Pts',(-32.9494192482977,87.8953232447007,118.107342896775));
#42425=CARTESIAN_POINT('Ctrl Pts',(-34.3871049230724,84.9862495848679,117.949394373583));
#42426=CARTESIAN_POINT('Ctrl Pts',(-37.6089541874201,84.5998081584843,117.791445850391));
#42427=CARTESIAN_POINT('Ctrl Pts',(-39.6938143014992,87.0863736539122,117.633497327198));
#42428=CARTESIAN_POINT('Ctrl Pts',(-38.7514060080155,90.1914527618476,117.475548804006));
#42429=CARTESIAN_POINT('Ctrl Pts',(-35.6361822446241,91.0997646918721,117.317600280813));
#42430=CARTESIAN_POINT('Ctrl Pts',(-33.1726216523412,88.9877706420741,117.159651757621));
#42431=CARTESIAN_POINT('Ctrl Pts',(-33.5943596943826,85.7703513840185,117.001703234428));
#42432=CARTESIAN_POINT('Ctrl Pts',(-36.5190193146114,84.3646431055967,116.843754711236));
#42433=CARTESIAN_POINT('Ctrl Pts',(-39.294900584868,86.0451587501709,116.685806188043));
#42434=CARTESIAN_POINT('Ctrl Pts',(-39.4051963820231,89.2882258933781,116.527857664851));
#42435=CARTESIAN_POINT('Ctrl Pts',(-36.7499048612913,91.1534541899008,116.369909141658));
#42436=CARTESIAN_POINT('Ctrl Pts',(-33.736498087479,89.9496978716363,116.211960618466));
#42437=CARTESIAN_POINT('Ctrl Pts',(-33.0971403337776,86.7683661817615,116.054012095273));
#42438=CARTESIAN_POINT('Ctrl Pts',(-35.4115178302812,84.4938758076564,115.896063572081));
#42439=CARTESIAN_POINT('Ctrl Pts',(-38.5812548895196,85.1884379960241,115.738115048888));
#42440=CARTESIAN_POINT('Ctrl Pts',(-39.7324473230763,88.2223143348259,115.580166525696));
#42441=CARTESIAN_POINT('Ctrl Pts',(-37.8213439633806,90.844781418848,115.422218002504));
#42442=CARTESIAN_POINT('Ctrl Pts',(-34.5806841030873,90.6781281017385,115.264269479311));
#42443=CARTESIAN_POINT('Ctrl Pts',(-32.94867547731,87.873453877589,115.106320956119));
#42444=CARTESIAN_POINT('Ctrl Pts',(-34.4050106717424,84.9736715651254,114.948372432926));
#42445=CARTESIAN_POINT('Ctrl Pts',(-37.6292748580252,84.6079255941658,114.790423909734));
#42446=CARTESIAN_POINT('Ctrl Pts',(-39.6981257600185,87.1078267129187,114.632475386541));
#42447=CARTESIAN_POINT('Ctrl Pts',(-38.7357991861407,90.2067906080661,114.474526863349));
#42448=CARTESIAN_POINT('Ctrl Pts',(-35.6148073730872,91.0950809666047,114.316578340156));
#42449=CARTESIAN_POINT('Ctrl Pts',(-33.1648586770783,88.9673119365771,114.158629816964));
#42450=CARTESIAN_POINT('Ctrl Pts',(-33.6072470689639,85.7526669843399,114.000681293771));
#42451=CARTESIAN_POINT('Ctrl Pts',(-36.5408724484561,84.3657669190797,113.842732770579));
#42452=CARTESIAN_POINT('Ctrl Pts',(-39.3059059061521,86.0640718493091,113.684784247386));
#42453=CARTESIAN_POINT('Ctrl Pts',(-39.39537570065,89.307780346399,113.526835724194));
#42454=CARTESIAN_POINT('Ctrl Pts',(-36.7281622903795,91.155920568972,113.368887201001));
#42455=CARTESIAN_POINT('Ctrl Pts',(-33.7225469548038,89.9328399858657,113.210938677809));
#42456=CARTESIAN_POINT('Ctrl Pts',(-33.1036297070312,86.7474685634676,113.052990154616));
#42457=CARTESIAN_POINT('Ctrl Pts',(-35.4325639920998,84.4878856917742,112.895041631424));
#42458=CARTESIAN_POINT('Ctrl Pts',(-38.5977759250725,85.2027864384426,112.737093108232));
#42459=CARTESIAN_POINT('Ctrl Pts',(-39.7294641118921,88.2439920391926,112.579144585039));
#42460=CARTESIAN_POINT('Ctrl Pts',(-37.8015612923099,90.8541338699109,112.421196061847));
#42461=CARTESIAN_POINT('Ctrl Pts',(-34.562038318327,90.6666757165611,112.263247538654));
#42462=CARTESIAN_POINT('Ctrl Pts',(-32.9480721448167,87.8515801855026,112.105299015462));
#42463=CARTESIAN_POINT('Ctrl Pts',(-34.4229968147373,84.9612087774874,111.947350492269));
#42464=CARTESIAN_POINT('Ctrl Pts',(-37.6495429876806,84.616173341487,111.789401969077));
#42465=CARTESIAN_POINT('Ctrl Pts',(-39.7022993795991,87.1293070135509,111.631453445884));
#42466=CARTESIAN_POINT('Ctrl Pts',(-38.7200942017158,90.2220279267117,111.473504922692));
#42467=CARTESIAN_POINT('Ctrl Pts',(-35.5934630163727,91.0902600898865,111.315556399499));
#42468=CARTESIAN_POINT('Ctrl Pts',(-33.157227227182,88.9468038067609,111.157607876307));
#42469=CARTESIAN_POINT('Ctrl Pts',(-33.6202477293367,85.7350656990739,110.999659353114));
#42470=CARTESIAN_POINT('Ctrl Pts',(-36.5627179158792,84.3670310282509,110.841710829922));
#42471=CARTESIAN_POINT('Ctrl Pts',(-39.3167895594165,86.0830552238758,110.683762306729));
#42472=CARTESIAN_POINT('Ctrl Pts',(-39.3854296629615,89.3272713373828,110.525813783537));
#42473=CARTESIAN_POINT('Ctrl Pts',(-36.7064043303624,91.1582472888979,110.367865260345));
#42474=CARTESIAN_POINT('Ctrl Pts',(-33.7087043556433,89.9158928659535,110.209916737152));
#42475=CARTESIAN_POINT('Ctrl Pts',(-33.1102531270847,86.7266130472388,110.05196821396));
#42476=CARTESIAN_POINT('Ctrl Pts',(-35.4536481887421,84.4820308305605,109.894019690767));
#42477=CARTESIAN_POINT('Ctrl Pts',(-38.6142044760489,85.2172406793387,109.736071167575));
#42478=CARTESIAN_POINT('Ctrl Pts',(-39.7263417957622,88.2656501153136,109.578122644382));
#42479=CARTESIAN_POINT('Ctrl Pts',(-37.7817189233878,90.8633591574933,109.42017412119));
#42480=CARTESIAN_POINT('Ctrl Pts',(-34.5434665639104,90.6551037322417,109.262225597997));
#42481=CARTESIAN_POINT('Ctrl Pts',(-32.9476090490401,87.8297032979492,109.104277074805));
#42482=CARTESIAN_POINT('Ctrl Pts',(-34.4410630766242,84.948861267686,108.946328551612));
#42483=CARTESIAN_POINT('Ctrl Pts',(-37.6697567821324,84.6245520230139,108.78838002842));
#42484=CARTESIAN_POINT('Ctrl Pts',(-39.7063369595486,87.1508116905743,108.630431505227));
#42485=CARTESIAN_POINT('Ctrl Pts',(-38.7042876480837,90.2371681606266,108.472482982035));
#42486=CARTESIAN_POINT('Ctrl Pts',(-35.5721583919285,91.0852938882971,108.314534458842));
#42487=CARTESIAN_POINT('Ctrl Pts',(-33.1497104713126,88.9262643156241,108.15658593565));
#42488=CARTESIAN_POINT('Ctrl Pts',(-33.6333964003301,85.7175128460946,107.998637412458));
#42489=CARTESIAN_POINT('Ctrl Pts',(-36.5844823020197,84.3685081976436,107.840688889265));
#42490=CARTESIAN_POINT('Ctrl Pts',(-39.3277002226027,86.1019583441278,107.682740366073));
#42491=CARTESIAN_POINT('Ctrl Pts',(-39.3750519991432,89.3470060757694,107.52479184288));
#42492=CARTESIAN_POINT('Ctrl Pts',(-36.6852627683359,91.1598010402508,107.366843319688));
#42493=CARTESIAN_POINT('Ctrl Pts',(-33.6936733563466,89.9001751727833,107.208894796495));
#42494=CARTESIAN_POINT('Ctrl Pts',(-33.1197345530817,86.7031400826113,107.050946273303));
#42495=CARTESIAN_POINT('Ctrl Pts',(-34.6859840276597,85.2251375401038,106.945647257841));
#42496=CARTESIAN_POINT('Ctrl Pts',(-35.6089932203365,84.9783780187301,106.89299775011));
#42497=CARTESIAN_POINT('Ctrl Pts',(-34.0188634169874,89.7658571455029,122.321006749669));
#42498=CARTESIAN_POINT('Ctrl Pts',(-33.3581428529915,88.9930721690097,122.268357241939));
#42499=CARTESIAN_POINT('Ctrl Pts',(-32.8754915208664,86.7527673686156,122.163058226477));
#42500=CARTESIAN_POINT('Ctrl Pts',(-35.3059677081389,84.2949817885978,122.005109703285));
#42501=CARTESIAN_POINT('Ctrl Pts',(-38.6888350559476,84.9936096217169,121.847161180092));
#42502=CARTESIAN_POINT('Ctrl Pts',(-39.9550037918771,88.204780703329,121.6892126569));
#42503=CARTESIAN_POINT('Ctrl Pts',(-37.9573947132227,91.0220940158023,121.531264133707));
#42504=CARTESIAN_POINT('Ctrl Pts',(-34.5067287733102,90.8887185705161,121.373315610515));
#42505=CARTESIAN_POINT('Ctrl Pts',(-32.7318387507372,87.9267773779968,121.215367087322));
#42506=CARTESIAN_POINT('Ctrl Pts',(-34.2418569809606,84.8211911081587,121.05741856413));
#42507=CARTESIAN_POINT('Ctrl Pts',(-37.6677476301795,84.3879830560575,120.899470040937));
#42508=CARTESIAN_POINT('Ctrl Pts',(-39.903334666494,87.019792332629,120.741521517745));
#42509=CARTESIAN_POINT('Ctrl Pts',(-38.921691557528,90.3305043484613,120.583572994552));
#42510=CARTESIAN_POINT('Ctrl Pts',(-35.6128383024604,91.3183647084341,120.42562447136));
#42511=CARTESIAN_POINT('Ctrl Pts',(-32.9768144078577,89.0877262726116,120.267675948167));
#42512=CARTESIAN_POINT('Ctrl Pts',(-33.4036211604692,85.6610333840612,120.109727424975));
#42513=CARTESIAN_POINT('Ctrl Pts',(-36.5062865428284,84.1451680035439,119.951778901782));
#42514=CARTESIAN_POINT('Ctrl Pts',(-39.4717178832619,85.9145173515199,119.79383037859));
#42515=CARTESIAN_POINT('Ctrl Pts',(-39.611248936739,89.3648670700897,119.635881855398));
#42516=CARTESIAN_POINT('Ctrl Pts',(-36.7983710620289,91.3678895774169,119.477933332205));
#42517=CARTESIAN_POINT('Ctrl Pts',(-33.583435116581,90.1075054942073,119.319984809013));
#42518=CARTESIAN_POINT('Ctrl Pts',(-32.8813257256701,86.7264666342663,119.16203628582));
#42519=CARTESIAN_POINT('Ctrl Pts',(-35.3286241293906,84.2902581516539,119.004087762628));
#42520=CARTESIAN_POINT('Ctrl Pts',(-38.7064392919062,85.0077161596018,118.846139239435));
#42521=CARTESIAN_POINT('Ctrl Pts',(-39.9522089391075,88.2283433144829,118.688190716243));
#42522=CARTESIAN_POINT('Ctrl Pts',(-37.936431619208,91.0320949202345,118.53024219305));
#42523=CARTESIAN_POINT('Ctrl Pts',(-34.4867513215705,90.8768946709331,118.372293669858));
#42524=CARTESIAN_POINT('Ctrl Pts',(-32.7308882545334,87.903457911076,118.214345146665));
#42525=CARTESIAN_POINT('Ctrl Pts',(-34.2608300589376,84.8077093184867,118.056396623473));
#42526=CARTESIAN_POINT('Ctrl Pts',(-37.6894250317483,84.3964699888117,117.89844810028));
#42527=CARTESIAN_POINT('Ctrl Pts',(-39.9080703871487,87.0425981151423,117.740499577088));
#42528=CARTESIAN_POINT('Ctrl Pts',(-38.9051878584318,90.346929803609,117.582551053895));
#42529=CARTESIAN_POINT('Ctrl Pts',(-35.5900605330986,91.3135280090206,117.424602530703));
#42530=CARTESIAN_POINT('Ctrl Pts',(-32.9684135319854,89.0660075362686,117.26665400751));
#42531=CARTESIAN_POINT('Ctrl Pts',(-33.417214457214,85.6421268427602,117.108705484318));
#42532=CARTESIAN_POINT('Ctrl Pts',(-36.5295491595418,84.1462144206715,116.950756961126));
#42533=CARTESIAN_POINT('Ctrl Pts',(-39.4835584217499,85.9345685669924,116.792808437933));
#42534=CARTESIAN_POINT('Ctrl Pts',(-39.6009318879243,89.3857429675857,116.634859914741));
#42535=CARTESIAN_POINT('Ctrl Pts',(-36.7752506060375,91.3706627561583,116.476911391548));
#42536=CARTESIAN_POINT('Ctrl Pts',(-33.5684738551649,90.0896615290181,116.318962868356));
#42537=CARTESIAN_POINT('Ctrl Pts',(-32.8880885856163,86.7041841389216,116.161014345163));
#42538=CARTESIAN_POINT('Ctrl Pts',(-35.3509794283091,84.2837399708291,116.003065821971));
#42539=CARTESIAN_POINT('Ctrl Pts',(-38.7241181616125,85.0228721374683,115.845117298778));
#42540=CARTESIAN_POINT('Ctrl Pts',(-39.9491824854176,88.251431983036,115.687168775586));
#42541=CARTESIAN_POINT('Ctrl Pts',(-37.9154438359774,91.0421824877652,115.529220252393));
#42542=CARTESIAN_POINT('Ctrl Pts',(-34.4668311933744,90.8648350458576,115.371271729201));
#42543=CARTESIAN_POINT('Ctrl Pts',(-32.7300967558443,87.8801851891123,115.213323206008));
#42544=CARTESIAN_POINT('Ctrl Pts',(-34.2798848175055,84.7943241686182,115.055374682816));
#42545=CARTESIAN_POINT('Ctrl Pts',(-37.7110496775229,84.4051083194366,114.897426159624));
#42546=CARTESIAN_POINT('Ctrl Pts',(-39.9126585114809,87.065427814556,114.739477636431));
#42547=CARTESIAN_POINT('Ctrl Pts',(-38.8885795485355,90.3632518777111,114.581529113238));
#42548=CARTESIAN_POINT('Ctrl Pts',(-35.5673140384357,91.3085437296246,114.423580590046));
#42549=CARTESIAN_POINT('Ctrl Pts',(-32.9601524074645,89.0442359979183,114.265632066854));
#42550=CARTESIAN_POINT('Ctrl Pts',(-33.4309288131869,85.623307637124,114.107683543661));
#42551=CARTESIAN_POINT('Ctrl Pts',(-36.5528046065515,84.1474103491404,113.949735020469));
#42552=CARTESIAN_POINT('Ctrl Pts',(-39.495269953275,85.9546953175959,113.791786497276));
#42553=CARTESIAN_POINT('Ctrl Pts',(-39.5904810145212,89.406552227679,113.633837974084));
#42554=CARTESIAN_POINT('Ctrl Pts',(-36.7521128167719,91.3732874025,113.475889450891));
#42555=CARTESIAN_POINT('Ctrl Pts',(-33.5536274798598,90.071721874595,113.317940927699));
#42556=CARTESIAN_POINT('Ctrl Pts',(-32.8949943812288,86.6819455227893,113.159992404506));
#42557=CARTESIAN_POINT('Ctrl Pts',(-35.3733761199876,84.2773654698779,113.002043881314));
#42558=CARTESIAN_POINT('Ctrl Pts',(-38.7416993501767,85.0381413178388,112.844095358121));
#42559=CARTESIAN_POINT('Ctrl Pts',(-39.946007841904,88.2745007432776,112.686146834929));
#42560=CARTESIAN_POINT('Ctrl Pts',(-37.8943917131075,91.0521350845713,112.528198311736));
#42561=CARTESIAN_POINT('Ctrl Pts',(-34.4469889106826,90.8526477623989,112.370249788544));
#42562=CARTESIAN_POINT('Ctrl Pts',(-32.7294547075721,87.8569078646409,112.212301265352));
#42563=CARTESIAN_POINT('Ctrl Pts',(-34.2990251292932,84.7810616452854,112.054352742159));
#42564=CARTESIAN_POINT('Ctrl Pts',(-37.732618410801,84.413885323785,111.896404218967));
#42565=CARTESIAN_POINT('Ctrl Pts',(-39.9170999517652,87.0882865036874,111.738455695774));
#42566=CARTESIAN_POINT('Ctrl Pts',(-38.8718667770092,90.3794669733972,111.580507172582));
#42567=CARTESIAN_POINT('Ctrl Pts',(-35.544600016728,91.3034134977843,111.422558649389));
#42568=CARTESIAN_POINT('Ctrl Pts',(-32.9520312482784,89.0224118636959,111.264610126197));
#42569=CARTESIAN_POINT('Ctrl Pts',(-33.4447637244879,85.6045768793427,111.106661603004));
#42570=CARTESIAN_POINT('Ctrl Pts',(-36.5760518951862,84.1487555760565,110.948713079812));
#42571=CARTESIAN_POINT('Ctrl Pts',(-39.5068520093573,85.9748968531942,110.790764556619));
#42572=CARTESIAN_POINT('Ctrl Pts',(-39.579896740702,89.4272939533835,110.632816033427));
#42573=CARTESIAN_POINT('Ctrl Pts',(-36.7289586508838,91.3757634277843,110.474867510234));
#42574=CARTESIAN_POINT('Ctrl Pts',(-33.5388966026528,90.0536872598855,110.316918987042));
#42575=CARTESIAN_POINT('Ctrl Pts',(-32.9020428254094,86.6597517104068,110.158970463849));
#42576=CARTESIAN_POINT('Ctrl Pts',(-35.3958132871802,84.2711349028723,110.001021940657));
#42577=CARTESIAN_POINT('Ctrl Pts',(-38.7591821194396,85.0535230857633,109.843073417464));
#42578=CARTESIAN_POINT('Ctrl Pts',(-39.9426851670958,88.2975486157311,109.685124894272));
#42579=CARTESIAN_POINT('Ctrl Pts',(-37.8732760615816,91.0619523578304,109.527176371079));
#42580=CARTESIAN_POINT('Ctrl Pts',(-34.4272254088536,90.8403332051346,109.369227847887));
#42581=CARTESIAN_POINT('Ctrl Pts',(-32.7289618949911,87.8336271396496,109.211279324695));
#42582=CARTESIAN_POINT('Ctrl Pts',(-34.3182507011933,84.7679217971554,109.053330801502));
#42583=CARTESIAN_POINT('Ctrl Pts',(-37.7541293221915,84.4228016643723,108.89538227831));
#42584=CARTESIAN_POINT('Ctrl Pts',(-39.9213966227703,87.1111711334404,108.737433755117));
#42585=CARTESIAN_POINT('Ctrl Pts',(-38.855045918591,90.3955787544361,108.579485231925));
#42586=CARTESIAN_POINT('Ctrl Pts',(-35.521928276906,91.298128615592,108.421536708732));
#42587=CARTESIAN_POINT('Ctrl Pts',(-32.944032143022,89.0005543557004,108.26358818554));
#42588=CARTESIAN_POINT('Ctrl Pts',(-33.4587561442345,85.5858976617427,108.105639662347));
#42589=CARTESIAN_POINT('Ctrl Pts',(-36.5992128995613,84.1503275352445,107.947691139155));
#42590=CARTESIAN_POINT('Ctrl Pts',(-39.5184628085849,85.9950129845674,107.789742615962));
#42591=CARTESIAN_POINT('Ctrl Pts',(-39.5688531433523,89.4482950677345,107.63179409277));
#42592=CARTESIAN_POINT('Ctrl Pts',(-36.7064604371766,91.3774168831885,107.473845569577));
#42593=CARTESIAN_POINT('Ctrl Pts',(-33.5229010658053,90.036960964095,107.315897046385));
#42594=CARTESIAN_POINT('Ctrl Pts',(-32.9121326734567,86.6347724882534,107.157948523192));
#42595=CARTESIAN_POINT('Ctrl Pts',(-34.578888202379,85.0619266872042,107.052649507731));
#42596=CARTESIAN_POINT('Ctrl Pts',(-35.5611267921506,84.7993326348266,107.));
#42597=CARTESIAN_POINT('Ctrl Pts',(-34.4414600780185,89.4045427919472,122.));
#42598=CARTESIAN_POINT('Ctrl Pts',(-34.3798518540623,89.3466461894736,122.));
#42599=CARTESIAN_POINT('Ctrl Pts',(-34.3216127823397,89.2855988291107,122.));
#42600=CARTESIAN_POINT('Ctrl Pts',(-34.2667404771132,89.2217855293614,122.));
#42601=CARTESIAN_POINT('Ctrl Pts',(-34.2104152444954,89.1562825595543,122.));
#42602=CARTESIAN_POINT('Ctrl Pts',(-34.1576369947234,89.0878648044825,122.));
#42603=CARTESIAN_POINT('Ctrl Pts',(-34.1084286552735,89.0168999163865,122.));
#42604=CARTESIAN_POINT('Ctrl Pts',(-34.057870758409,88.9439887892591,122.));
#42605=CARTESIAN_POINT('Ctrl Pts',(-34.0110807367076,88.86838834465,122.));
#42606=CARTESIAN_POINT('Ctrl Pts',(-33.9681175240201,88.7904543421215,122.));
#42607=CARTESIAN_POINT('Ctrl Pts',(-33.9492075685674,88.7561522398373,122.));
#42608=CARTESIAN_POINT('Ctrl Pts',(-33.9310394493789,88.7213975690564,122.));
#42609=CARTESIAN_POINT('Ctrl Pts',(-33.9136206166358,88.6862185871068,122.));
#42610=CARTESIAN_POINT('Ctrl Pts',(-33.9036897724251,88.6661623069653,122.));
#42611=CARTESIAN_POINT('Ctrl Pts',(-33.8940025031947,88.6459680887744,122.));
#42612=CARTESIAN_POINT('Ctrl Pts',(-33.8845604238774,88.6256410205665,122.));
#42613=CARTESIAN_POINT('Ctrl Pts',(-33.8760548331441,88.6073300408371,122.));
#42614=CARTESIAN_POINT('Ctrl Pts',(-33.8677458327171,88.5889055291902,122.));
#42615=CARTESIAN_POINT('Ctrl Pts',(-33.8596482636109,88.5704029596064,122.));
#42616=CARTESIAN_POINT('Ctrl Pts',(-33.8230866066973,88.4868612704561,122.));
#42617=CARTESIAN_POINT('Ctrl Pts',(-33.7907851307286,88.4016360383248,122.));
#42618=CARTESIAN_POINT('Ctrl Pts',(-33.7627688719189,88.3151260404377,122.));
#42619=CARTESIAN_POINT('Ctrl Pts',(-33.7342895213475,88.227186084768,122.));
#42620=CARTESIAN_POINT('Ctrl Pts',(-33.7102377294814,88.1379177844905,122.));
#42621=CARTESIAN_POINT('Ctrl Pts',(-33.6906788696645,88.0477028957553,122.));
#42622=CARTESIAN_POINT('Ctrl Pts',(-33.6717103782297,87.9602110705522,122.));
#42623=CARTESIAN_POINT('Ctrl Pts',(-33.6569675246869,87.8718280211553,122.));
#42624=CARTESIAN_POINT('Ctrl Pts',(-33.6465506821664,87.7828801024266,122.));
#42625=CARTESIAN_POINT('Ctrl Pts',(-33.6421818440549,87.7455752227077,122.));
#42626=CARTESIAN_POINT('Ctrl Pts',(-33.638574456279,87.7081707917553,122.));
#42627=CARTESIAN_POINT('Ctrl Pts',(-33.6357382583831,87.6706902671327,122.));
#42628=CARTESIAN_POINT('Ctrl Pts',(-33.6339591268603,87.6471789377781,122.));
#42629=CARTESIAN_POINT('Ctrl Pts',(-33.6324834856474,87.6236376602105,122.));
#42630=CARTESIAN_POINT('Ctrl Pts',(-33.6313140348496,87.6000721918068,122.));
#42631=CARTESIAN_POINT('Ctrl Pts',(-33.6306296486946,87.5862812051798,122.));
#42632=CARTESIAN_POINT('Ctrl Pts',(-33.630050417326,87.5724868801265,122.));
#42633=CARTESIAN_POINT('Ctrl Pts',(-33.6295768415433,87.5586982075279,122.));
#42634=CARTESIAN_POINT('Ctrl Pts',(-33.6262494419034,87.461817357796,122.));
#42635=CARTESIAN_POINT('Ctrl Pts',(-33.6281279592553,87.3651015105385,122.));
#42636=CARTESIAN_POINT('Ctrl Pts',(-33.6352767760794,87.268970431256,122.));
#42637=CARTESIAN_POINT('Ctrl Pts',(-33.6424255929035,87.1728393519736,122.));
#42638=CARTESIAN_POINT('Ctrl Pts',(-33.6548442788849,87.0772919966335,122.));
#42639=CARTESIAN_POINT('Ctrl Pts',(-33.6726496794354,86.9827293452592,122.));
#42640=CARTESIAN_POINT('Ctrl Pts',(-33.6897076975519,86.8921359651379,122.));
#42641=CARTESIAN_POINT('Ctrl Pts',(-33.7117095737827,86.8024453892223,122.));
#42642=CARTESIAN_POINT('Ctrl Pts',(-33.738380698432,86.7138969574772,122.));
#42643=CARTESIAN_POINT('Ctrl Pts',(-33.7472500404817,86.684450642804,122.));
#42644=CARTESIAN_POINT('Ctrl Pts',(-33.756636166633,86.6551306692652,122.));
#42645=CARTESIAN_POINT('Ctrl Pts',(-33.7665302267902,86.6259460129984,122.));
#42646=CARTESIAN_POINT('Ctrl Pts',(-33.7758505040486,86.598453852674,122.));
#42647=CARTESIAN_POINT('Ctrl Pts',(-33.7856215168716,86.5710817688634,122.));
#42648=CARTESIAN_POINT('Ctrl Pts',(-33.7958363420113,86.5438373897669,122.));
#42649=CARTESIAN_POINT('Ctrl Pts',(-33.8009941567469,86.5300807705352,122.));
#42650=CARTESIAN_POINT('Ctrl Pts',(-33.8062620516302,86.5163649848821,122.));
#42651=CARTESIAN_POINT('Ctrl Pts',(-33.8116373565419,86.5026943515934,122.));
#42652=CARTESIAN_POINT('Ctrl Pts',(-33.845888676196,86.4155853897129,122.));
#42653=CARTESIAN_POINT('Ctrl Pts',(-33.8845134961369,86.3302652389299,122.));
#42654=CARTESIAN_POINT('Ctrl Pts',(-33.927181830165,86.2469683145023,122.));
#42655=CARTESIAN_POINT('Ctrl Pts',(-33.9714116396017,86.1606230850008,122.));
#42656=CARTESIAN_POINT('Ctrl Pts',(-34.0199864581995,86.076451143434,122.));
#42657=CARTESIAN_POINT('Ctrl Pts',(-34.0725945744941,85.9947170694416,122.));
#42658=CARTESIAN_POINT('Ctrl Pts',(-34.1257656479925,85.9121083626172,122.));
#42659=CARTESIAN_POINT('Ctrl Pts',(-34.1830572163906,85.8319891559087,122.));
#42660=CARTESIAN_POINT('Ctrl Pts',(-34.2441989619735,85.7546479784666,122.));
#42661=CARTESIAN_POINT('Ctrl Pts',(-34.2668877934898,85.7259477683643,122.));
#42662=CARTESIAN_POINT('Ctrl Pts',(-34.2901072857831,85.697630319848,122.));
#42663=CARTESIAN_POINT('Ctrl Pts',(-34.3138452200131,85.6697112650143,122.));
#42664=CARTESIAN_POINT('Ctrl Pts',(-34.3346002693604,85.645300490463,122.));
#42665=CARTESIAN_POINT('Ctrl Pts',(-34.3557516672241,85.6211942822015,122.));
#42666=CARTESIAN_POINT('Ctrl Pts',(-34.3772917361037,85.5974034716814,122.));
#42667=CARTESIAN_POINT('Ctrl Pts',(-34.3890554697408,85.5844105346794,122.));
#42668=CARTESIAN_POINT('Ctrl Pts',(-34.4009304534246,85.5715169185705,122.));
#42669=CARTESIAN_POINT('Ctrl Pts',(-34.4129093606097,85.5587302471734,122.));
#42670=CARTESIAN_POINT('Ctrl Pts',(-34.4819201604098,85.4850658964735,122.));
#42671=CARTESIAN_POINT('Ctrl Pts',(-34.554433357923,85.4148860760258,122.));
#42672=CARTESIAN_POINT('Ctrl Pts',(-34.6301404311514,85.3484820008986,122.));
#42673=CARTESIAN_POINT('Ctrl Pts',(-34.6923345902646,85.2939303528409,122.));
#42674=CARTESIAN_POINT('Ctrl Pts',(-34.7566853223865,85.2419269392842,122.));
#42675=CARTESIAN_POINT('Ctrl Pts',(-34.8230438595686,85.1926465506592,122.));
#42676=CARTESIAN_POINT('Ctrl Pts',(-34.8476613986356,85.1743646242677,122.));
#42677=CARTESIAN_POINT('Ctrl Pts',(-34.8725554416842,85.1564575983159,122.));
#42678=CARTESIAN_POINT('Ctrl Pts',(-34.8977190002205,85.1389349616694,122.));
#42679=CARTESIAN_POINT('Ctrl Pts',(-34.9145299551421,85.1272286581135,122.));
#42680=CARTESIAN_POINT('Ctrl Pts',(-34.9314623353314,85.1156932828469,122.));
#42681=CARTESIAN_POINT('Ctrl Pts',(-34.9484989961695,85.1043414885822,122.));
#42682=CARTESIAN_POINT('Ctrl Pts',(-35.033409495634,85.0477642913257,122.));
#42683=CARTESIAN_POINT('Ctrl Pts',(-35.1209892714876,84.995686394659,122.));
#42684=CARTESIAN_POINT('Ctrl Pts',(-35.2109479651256,84.9484157153952,122.));
#42685=CARTESIAN_POINT('Ctrl Pts',(-35.2944060214804,84.904560932112,122.));
#42686=CARTESIAN_POINT('Ctrl Pts',(-35.3799124172306,84.8648434346886,122.));
#42687=CARTESIAN_POINT('Ctrl Pts',(-35.4672630109208,84.8295381485711,122.));
#42688=CARTESIAN_POINT('Ctrl Pts',(-35.4976931912937,84.8172389050366,122.));
#42689=CARTESIAN_POINT('Ctrl Pts',(-35.5283473918442,84.8054754204773,122.));
#42690=CARTESIAN_POINT('Ctrl Pts',(-35.5592127063051,84.7942439724069,122.));
#42691=CARTESIAN_POINT('Ctrl Pts',(-38.8730930351581,87.7663573574127,120.387416697508));
#42692=CARTESIAN_POINT('Ctrl Pts',(-38.8746753948415,87.5919909412047,120.398449387697));
#42693=CARTESIAN_POINT('Ctrl Pts',(-38.8580898013711,87.4179235704137,120.409482077886));
#42694=CARTESIAN_POINT('Ctrl Pts',(-38.8222182436848,87.2479259407801,120.420514768075));
#42695=CARTESIAN_POINT('Ctrl Pts',(-38.6510342603271,86.436673982989,120.473164275806));
#42696=CARTESIAN_POINT('Ctrl Pts',(-38.04064541331,85.7181034224155,120.525813783537));
#42697=CARTESIAN_POINT('Ctrl Pts',(-37.2677605332422,85.4179581709321,120.578463291268));
#42698=CARTESIAN_POINT('Ctrl Pts',(-36.4948756531744,85.1178129194488,120.631112798999));
#42699=CARTESIAN_POINT('Ctrl Pts',(-35.5594947400559,85.2360929770557,120.683762306729));
#42700=CARTESIAN_POINT('Ctrl Pts',(-34.8856619433531,85.7191966430978,120.73641181446));
#42701=CARTESIAN_POINT('Ctrl Pts',(-34.2118291466503,86.2023003091399,120.789061322191));
#42702=CARTESIAN_POINT('Ctrl Pts',(-33.7995444663632,87.0502275836171,120.841710829922));
#42703=CARTESIAN_POINT('Ctrl Pts',(-33.8357038252505,87.8785449409451,120.894360337653));
#42704=CARTESIAN_POINT('Ctrl Pts',(-33.8718631841377,88.7068622982731,120.947009845384));
#42705=CARTESIAN_POINT('Ctrl Pts',(-34.3564665821994,89.5155697384517,120.999659353114));
#42706=CARTESIAN_POINT('Ctrl Pts',(-35.0698409727182,89.9381314019014,121.052308860845));
#42707=CARTESIAN_POINT('Ctrl Pts',(-35.783215363237,90.360693065351,121.104958368576));
#42708=CARTESIAN_POINT('Ctrl Pts',(-36.725360746213,90.3971089520717,121.157607876307));
#42709=CARTESIAN_POINT('Ctrl Pts',(-37.4691399533732,90.0307072612391,121.210257384038));
#42710=CARTESIAN_POINT('Ctrl Pts',(-38.2129191605335,89.6643055704066,121.262906891768));
#42711=CARTESIAN_POINT('Ctrl Pts',(-38.758332191878,88.8950863020207,121.315556399499));
#42712=CARTESIAN_POINT('Ctrl Pts',(-38.8581858366267,88.0720989660786,121.36820590723));
#42713=CARTESIAN_POINT('Ctrl Pts',(-38.8703307265502,87.9720015622371,121.374609503989));
#42714=CARTESIAN_POINT('Ctrl Pts',(-38.8758844099473,87.8711087617585,121.381013100749));
#42715=CARTESIAN_POINT('Ctrl Pts',(-38.8751286390733,87.7701344517389,121.387416697508));
#42716=CARTESIAN_POINT('Ctrl Pts',(-37.1487253572165,84.7993326348266,122.));
#42717=CARTESIAN_POINT('Ctrl Pts',(-38.1309639469882,85.0619266872043,121.947350492269));
#42718=CARTESIAN_POINT('Ctrl Pts',(-39.7977194028581,86.634772993702,121.842051476808));
#42719=CARTESIAN_POINT('Ctrl Pts',(-39.186951146607,90.036960832952,121.684102953615));
#42720=CARTESIAN_POINT('Ctrl Pts',(-36.0033917073514,91.3774170351665,121.526154430422));
#42721=CARTESIAN_POINT('Ctrl Pts',(-33.1409989526284,89.4482950386239,121.36820590723));
#42722=CARTESIAN_POINT('Ctrl Pts',(-33.1913893007143,85.9950129878222,121.210257384038));
#42723=CARTESIAN_POINT('Ctrl Pts',(-36.1106392417851,84.1503274667491,121.052308860845));
#42724=CARTESIAN_POINT('Ctrl Pts',(-39.2510960503128,85.5858976381881,120.894360337653));
#42725=CARTESIAN_POINT('Ctrl Pts',(-39.765820054418,89.0005543692986,120.73641181446));
#42726=CARTESIAN_POINT('Ctrl Pts',(-37.1879238856457,91.2981286694523,120.578463291268));
#42727=CARTESIAN_POINT('Ctrl Pts',(-33.854806193682,90.395578791602,120.420514768075));
#42728=CARTESIAN_POINT('Ctrl Pts',(-32.7884554748253,87.1111711244642,120.262566244883));
#42729=CARTESIAN_POINT('Ctrl Pts',(-34.9557228065637,84.4228016151801,120.10461772169));
#42730=CARTESIAN_POINT('Ctrl Pts',(-38.3916014780163,84.7679217534951,119.946669198498));
#42731=CARTESIAN_POINT('Ctrl Pts',(-39.9808903072863,87.8336271405144,119.788720675305));
#42732=CARTESIAN_POINT('Ctrl Pts',(-38.2826267686962,90.8403332500451,119.630772152113));
#42733=CARTESIAN_POINT('Ctrl Pts',(-34.8365760655942,91.0619524059114,119.47282362892));
#42734=CARTESIAN_POINT('Ctrl Pts',(-32.7671669298757,88.2975486234688,119.314875105728));
#42735=CARTESIAN_POINT('Ctrl Pts',(-33.9506699948071,85.0535230461015,119.156926582536));
#42736=CARTESIAN_POINT('Ctrl Pts',(-37.3140388761979,84.2711348517919,118.998978059343));
#42737=CARTESIAN_POINT('Ctrl Pts',(-39.8078093743896,86.65975169421,118.841029536151));
#42738=CARTESIAN_POINT('Ctrl Pts',(-39.1709555878457,90.0536872932633,118.683081012958));
#42739=CARTESIAN_POINT('Ctrl Pts',(-35.9808934930197,91.3757634804708,118.525132489766));
#42740=CARTESIAN_POINT('Ctrl Pts',(-33.1299553615612,89.4272939776113,118.367183966573));
#42741=CARTESIAN_POINT('Ctrl Pts',(-33.2030000939727,85.9748968269957,118.209235443381));
#42742=CARTESIAN_POINT('Ctrl Pts',(-36.1338002509514,84.1487555231856,118.051286920188));
#42743=CARTESIAN_POINT('Ctrl Pts',(-39.2650884673852,85.6045768477356,117.893338396996));
#42744=CARTESIAN_POINT('Ctrl Pts',(-39.7578209507915,89.0224118820099,117.735389873803));
#42745=CARTESIAN_POINT('Ctrl Pts',(-37.1652521444745,91.3034135494146,117.577441350611));
#42746=CARTESIAN_POINT('Ctrl Pts',(-33.8379853355952,90.3794670115321,117.419492827418));
#42747=CARTESIAN_POINT('Ctrl Pts',(-32.7927521455727,87.0882864937512,117.261544304226));
#42748=CARTESIAN_POINT('Ctrl Pts',(-34.9772337184436,84.4138852747866,117.103595781033));
#42749=CARTESIAN_POINT('Ctrl Pts',(-38.4108270501026,84.7810616016501,116.945647257841));
#42750=CARTESIAN_POINT('Ctrl Pts',(-39.9803974947487,87.8569078659315,116.787698734648));
#42751=CARTESIAN_POINT('Ctrl Pts',(-38.2628632665517,90.8526478074454,116.629750211456));
#42752=CARTESIAN_POINT('Ctrl Pts',(-34.8154604137739,91.0521351325312,116.471801688264));
#42753=CARTESIAN_POINT('Ctrl Pts',(-32.7638442550116,88.2745007506674,116.313853165071));
#42754=CARTESIAN_POINT('Ctrl Pts',(-33.9681527643291,85.0381412779581,116.155904641879));
#42755=CARTESIAN_POINT('Ctrl Pts',(-37.3364760437162,84.2773654188855,115.997956118686));
#42756=CARTESIAN_POINT('Ctrl Pts',(-39.8148578186742,86.6819455069184,115.840007595494));
#42757=CARTESIAN_POINT('Ctrl Pts',(-39.1562247104231,90.0717219082352,115.682059072301));
#42758=CARTESIAN_POINT('Ctrl Pts',(-35.9577393267937,91.3732874551507,115.524110549109));
#42759=CARTESIAN_POINT('Ctrl Pts',(-33.1193710875871,89.4065522516036,115.366162025916));
#42760=CARTESIAN_POINT('Ctrl Pts',(-33.2145821502242,85.9546952911023,115.208213502724));
#42761=CARTESIAN_POINT('Ctrl Pts',(-36.1570475399255,84.14741029625,115.050264979531));
#42762=CARTESIAN_POINT('Ctrl Pts',(-39.2789233788883,85.6233076057904,114.892316456339));
#42763=CARTESIAN_POINT('Ctrl Pts',(-39.7496997914867,89.0442360165511,114.734367933146));
#42764=CARTESIAN_POINT('Ctrl Pts',(-37.1425381224351,91.3085437813298,114.576419409954));
#42765=CARTESIAN_POINT('Ctrl Pts',(-33.8212725638248,90.3632519156092,114.418470886762));
#42766=CARTESIAN_POINT('Ctrl Pts',(-32.7971935859219,87.0654278042858,114.260522363569));
#42767=CARTESIAN_POINT('Ctrl Pts',(-34.9988024520367,84.4051082703102,114.102573840377));
#42768=CARTESIAN_POINT('Ctrl Pts',(-38.4299673621699,84.7943241251765,113.944625317184));
#42769=CARTESIAN_POINT('Ctrl Pts',(-39.9797554464671,87.8801851907431,113.786676793992));
#42770=CARTESIAN_POINT('Ctrl Pts',(-38.2430209835701,90.864835091082,113.628728270799));
#42771=CARTESIAN_POINT('Ctrl Pts',(-34.7944082905965,91.0421825355799,113.470779747607));
#42772=CARTESIAN_POINT('Ctrl Pts',(-32.7606696114516,88.2514319900887,113.312831224414));
#42773=CARTESIAN_POINT('Ctrl Pts',(-33.9857339531502,85.0228720973646,113.154882701222));
#42774=CARTESIAN_POINT('Ctrl Pts',(-37.3588727357218,84.2837399199298,112.996934178029));
#42775=CARTESIAN_POINT('Ctrl Pts',(-39.8217636143875,86.7041841233756,112.838985654837));
#42776=CARTESIAN_POINT('Ctrl Pts',(-39.1413783349011,90.0896615629203,112.681037131644));
#42777=CARTESIAN_POINT('Ctrl Pts',(-35.93460153719,91.3706628087708,112.523088608452));
#42778=CARTESIAN_POINT('Ctrl Pts',(-33.1089202140314,89.3857429912062,112.365140085259));
#42779=CARTESIAN_POINT('Ctrl Pts',(-33.2262936819204,85.934568540205,112.207191562067));
#42780=CARTESIAN_POINT('Ctrl Pts',(-36.1803029872748,84.1462143677634,112.049243038875));
#42781=CARTESIAN_POINT('Ctrl Pts',(-39.2926377350615,85.6421268117017,111.891294515682));
#42782=CARTESIAN_POINT('Ctrl Pts',(-39.741438666845,89.0660075552192,111.733345992489));
#42783=CARTESIAN_POINT('Ctrl Pts',(-37.11979162744,91.3135280607988,111.575397469297));
#42784=CARTESIAN_POINT('Ctrl Pts',(-33.8046642536859,90.3469298412686,111.417448946105));
#42785=CARTESIAN_POINT('Ctrl Pts',(-32.8017817103211,87.0425981045389,111.259500422912));
#42786=CARTESIAN_POINT('Ctrl Pts',(-35.0204270981272,84.3964699395587,111.10155189972));
#42787=CARTESIAN_POINT('Ctrl Pts',(-38.449022121016,84.8077092752406,110.943603376527));
#42788=CARTESIAN_POINT('Ctrl Pts',(-39.9789639477665,87.9034579130465,110.785654853335));
#42789=CARTESIAN_POINT('Ctrl Pts',(-38.223100855083,90.8768947163338,110.627706330142));
#42790=CARTESIAN_POINT('Ctrl Pts',(-34.7734205070594,91.0320949679017,110.46975780695));
#42791=CARTESIAN_POINT('Ctrl Pts',(-32.7576431577175,88.2283433211983,110.311809283757));
#42792=CARTESIAN_POINT('Ctrl Pts',(-34.0034128231148,85.0077161192772,110.153860760565));
#42793=CARTESIAN_POINT('Ctrl Pts',(-37.3812280349669,84.2902581008489,109.995912237372));
#42794=CARTESIAN_POINT('Ctrl Pts',(-39.8285264744325,86.7264666190477,109.83796371418));
#42795=CARTESIAN_POINT('Ctrl Pts',(-39.1264170732664,90.1075055283665,109.680015190987));
#42796=CARTESIAN_POINT('Ctrl Pts',(-35.9114810808611,91.3678896299961,109.522066667795));
#42797=CARTESIAN_POINT('Ctrl Pts',(-33.0986031650656,89.3648670933915,109.364118144603));
#42798=CARTESIAN_POINT('Ctrl Pts',(-33.2381342205824,85.9145173244662,109.20616962141));
#42799=CARTESIAN_POINT('Ctrl Pts',(-36.2035656043253,84.1451679505691,109.048221098218));
#42800=CARTESIAN_POINT('Ctrl Pts',(-39.3062310320116,85.6610333533782,108.890272575025));
#42801=CARTESIAN_POINT('Ctrl Pts',(-39.7330377908336,89.0877262916886,108.732324051833));
#42802=CARTESIAN_POINT('Ctrl Pts',(-37.0970138577844,91.3183647606488,108.57437552864));
#42803=CARTESIAN_POINT('Ctrl Pts',(-33.7881605542584,90.3305043851839,108.416427005448));
#42804=CARTESIAN_POINT('Ctrl Pts',(-32.8065174312516,87.0197923230117,108.258478482255));
#42805=CARTESIAN_POINT('Ctrl Pts',(-35.0421044995447,84.3879830042027,108.100529959063));
#42806=CARTESIAN_POINT('Ctrl Pts',(-38.4679952003212,84.8211910697221,107.94258143587));
#42807=CARTESIAN_POINT('Ctrl Pts',(-39.9780134492052,87.9267773718166,107.784632912678));
#42808=CARTESIAN_POINT('Ctrl Pts',(-38.2031234082454,90.8887186315066,107.626684389485));
#42809=CARTESIAN_POINT('Ctrl Pts',(-34.7524574012803,91.0220940358159,107.468735866293));
#42810=CARTESIAN_POINT('Ctrl Pts',(-32.7548483299835,88.204780757559,107.3107873431));
#42811=CARTESIAN_POINT('Ctrl Pts',(-34.0210170033453,84.9936094992121,107.152838819908));
#42812=CARTESIAN_POINT('Ctrl Pts',(-37.4038845674691,84.2949818609618,106.994890296715));
#42813=CARTESIAN_POINT('Ctrl Pts',(-39.8343602819912,86.7527669934546,106.836941773523));
#42814=CARTESIAN_POINT('Ctrl Pts',(-39.3517092963754,88.9930721690098,106.731642758061));
#42815=CARTESIAN_POINT('Ctrl Pts',(-38.6909887323795,89.7658571455031,106.678993250331));
#42816=CARTESIAN_POINT('Ctrl Pts',(-37.1008589290306,84.9783780187301,122.10700224989));
#42817=CARTESIAN_POINT('Ctrl Pts',(-38.0238681217074,85.2251375401039,122.054352742159));
#42818=CARTESIAN_POINT('Ctrl Pts',(-39.5901175276382,86.7031405575811,121.949053726697));
#42819=CARTESIAN_POINT('Ctrl Pts',(-39.016178852264,89.9001750495482,121.791105203505));
#42820=CARTESIAN_POINT('Ctrl Pts',(-36.024589376484,91.1598011830645,121.633156680313));
#42821=CARTESIAN_POINT('Ctrl Pts',(-33.3348001000567,89.3470060484142,121.47520815712));
#42822=CARTESIAN_POINT('Ctrl Pts',(-33.3821518891126,86.1019583471864,121.317259633927));
#42823=CARTESIAN_POINT('Ctrl Pts',(-36.1253698398103,84.3685081332785,121.159311110735));
#42824=CARTESIAN_POINT('Ctrl Pts',(-39.0764557914928,85.7175128239604,121.001362587543));
#42825=CARTESIAN_POINT('Ctrl Pts',(-39.5601417232285,88.9262643284023,120.84341406435));
#42826=CARTESIAN_POINT('Ctrl Pts',(-37.1376937698282,91.0852939389096,120.685465541158));
#42827=CARTESIAN_POINT('Ctrl Pts',(-34.0055644664261,90.2371681955513,120.527517017965));
#42828=CARTESIAN_POINT('Ctrl Pts',(-33.0035151411689,87.1508116821394,120.369568494773));
#42829=CARTESIAN_POINT('Ctrl Pts',(-35.0400953478657,84.6245519767882,120.21161997158));
#42830=CARTESIAN_POINT('Ctrl Pts',(-38.2687891007858,84.9488612266584,120.053671448388));
#42831=CARTESIAN_POINT('Ctrl Pts',(-39.7622431500468,87.8297032987619,119.895722925195));
#42832=CARTESIAN_POINT('Ctrl Pts',(-38.16638561194,90.6551037744441,119.737774402003));
#42833=CARTESIAN_POINT('Ctrl Pts',(-34.928133205126,90.863359202675,119.57982587881));
#42834=CARTESIAN_POINT('Ctrl Pts',(-32.9835103043688,88.2656501225846,119.421877355618));
#42835=CARTESIAN_POINT('Ctrl Pts',(-34.0956476403156,85.2172406420686,119.263928832425));
#42836=CARTESIAN_POINT('Ctrl Pts',(-37.2562039737911,84.4820307825603,119.105980309233));
#42837=CARTESIAN_POINT('Ctrl Pts',(-39.5995990696733,86.7266130320189,118.94803178604));
#42838=CARTESIAN_POINT('Ctrl Pts',(-39.0011478323748,89.9158928973185,118.790083262848));
#42839=CARTESIAN_POINT('Ctrl Pts',(-36.0034478138706,91.1582473384075,118.632134739656));
#42840=CARTESIAN_POINT('Ctrl Pts',(-33.324422442142,89.3272713601495,118.474186216463));
#42841=CARTESIAN_POINT('Ctrl Pts',(-33.3930625466895,86.0830551992572,118.316237693271));
#42842=CARTESIAN_POINT('Ctrl Pts',(-36.147134230453,84.3670309785681,118.158289170078));
#42843=CARTESIAN_POINT('Ctrl Pts',(-39.0896044599732,85.7350656693728,118.000340646886));
#42844=CARTESIAN_POINT('Ctrl Pts',(-39.5526249688907,88.9468038239705,117.842392123693));
#42845=CARTESIAN_POINT('Ctrl Pts',(-37.1163891441162,91.0902601384036,117.684443600501));
#42846=CARTESIAN_POINT('Ctrl Pts',(-33.9897579131054,90.222027962547,117.526495077308));
#42847=CARTESIAN_POINT('Ctrl Pts',(-33.0075527208761,87.1293070042139,117.368546554116));
#42848=CARTESIAN_POINT('Ctrl Pts',(-35.0603091427774,84.6161732954432,117.210598030923));
#42849=CARTESIAN_POINT('Ctrl Pts',(-38.2868553628477,84.9612087364832,117.052649507731));
#42850=CARTESIAN_POINT('Ctrl Pts',(-39.7617800543109,87.8515801867154,116.894700984538));
#42851=CARTESIAN_POINT('Ctrl Pts',(-38.147813857227,90.6666757588912,116.736752461346));
#42852=CARTESIAN_POINT('Ctrl Pts',(-34.9082908359274,90.8541339149789,116.578803938153));
#42853=CARTESIAN_POINT('Ctrl Pts',(-32.9803879881863,88.2439920461367,116.420855414961));
#42854=CARTESIAN_POINT('Ctrl Pts',(-34.1120761915356,85.2027864009668,116.262906891768));
#42855=CARTESIAN_POINT('Ctrl Pts',(-37.2772881707395,84.4878856438566,116.104958368576));
#42856=CARTESIAN_POINT('Ctrl Pts',(-39.6062224898245,86.7474685485538,115.947009845384));
#42857=CARTESIAN_POINT('Ctrl Pts',(-38.9873052330117,89.9328400174774,115.789061322191));
#42858=CARTESIAN_POINT('Ctrl Pts',(-35.9816898535359,91.155920618448,115.631112798999));
#42859=CARTESIAN_POINT('Ctrl Pts',(-33.3144764043081,89.3077803688807,115.473164275806));
#42860=CARTESIAN_POINT('Ctrl Pts',(-33.403946200113,86.0640718244132,115.315215752614));
#42861=CARTESIAN_POINT('Ctrl Pts',(-36.1689796981952,84.3657668693785,115.157267229421));
#42862=CARTESIAN_POINT('Ctrl Pts',(-39.1026051205359,85.7526669548959,114.999318706229));
#42863=CARTESIAN_POINT('Ctrl Pts',(-39.544993518883,88.9673119540864,114.841370183036));
#42864=CARTESIAN_POINT('Ctrl Pts',(-37.09504478709,91.095081015192,114.683421659844));
#42865=CARTESIAN_POINT('Ctrl Pts',(-33.9740529284511,90.206790643679,114.525473136651));
#42866=CARTESIAN_POINT('Ctrl Pts',(-33.0117263405178,87.1078267032678,114.367524613459));
#42867=CARTESIAN_POINT('Ctrl Pts',(-35.0805772727288,84.6079255480015,114.209576090266));
#42868=CARTESIAN_POINT('Ctrl Pts',(-38.3048415061054,84.9736715243033,114.051627567074));
#42869=CARTESIAN_POINT('Ctrl Pts',(-39.7611767218088,87.8734538791213,113.893679043882));
#42870=CARTESIAN_POINT('Ctrl Pts',(-38.1291680721943,90.678128144236,113.735730520689));
#42871=CARTESIAN_POINT('Ctrl Pts',(-34.8885081645678,90.8447814637793,113.577781997497));
#42872=CARTESIAN_POINT('Ctrl Pts',(-32.9774047769586,88.2223143414533,113.419833474304));
#42873=CARTESIAN_POINT('Ctrl Pts',(-34.1285972273298,85.1884379583387,113.261884951112));
#42874=CARTESIAN_POINT('Ctrl Pts',(-37.2983343328655,84.4938757598263,113.103936427919));
#42875=CARTESIAN_POINT('Ctrl Pts',(-39.6127118631728,86.7683661671529,112.945987904727));
#42876=CARTESIAN_POINT('Ctrl Pts',(-38.9733541001328,89.9496979034943,112.788039381534));
#42877=CARTESIAN_POINT('Ctrl Pts',(-35.9599472823065,91.1534542393407,112.630090858342));
#42878=CARTESIAN_POINT('Ctrl Pts',(-33.3046557227915,89.2882259155742,112.472142335149));
#42879=CARTESIAN_POINT('Ctrl Pts',(-33.4149515215578,86.0451587249989,112.314193811957));
#42880=CARTESIAN_POINT('Ctrl Pts',(-36.190832832359,84.3646430558789,112.156245288764));
#42881=CARTESIAN_POINT('Ctrl Pts',(-39.1154924953055,85.7703513548328,111.998296765572));
#42882=CARTESIAN_POINT('Ctrl Pts',(-39.5372305435066,88.9877706598821,111.840348242379));
#42883=CARTESIAN_POINT('Ctrl Pts',(-37.0736699152408,91.0997647405279,111.682399719187));
#42884=CARTESIAN_POINT('Ctrl Pts',(-33.9584461063484,90.1914527972364,111.524451195994));
#42885=CARTESIAN_POINT('Ctrl Pts',(-33.0160377990999,87.0863736439481,111.366502672802));
#42886=CARTESIAN_POINT('Ctrl Pts',(-35.1008979436308,84.5998081122014,111.20855414961));
#42887=CARTESIAN_POINT('Ctrl Pts',(-38.3227472550368,84.9862495442295,111.050605626417));
#42888=CARTESIAN_POINT('Ctrl Pts',(-39.7604329508104,87.8953232465526,110.892657103225));
#42889=CARTESIAN_POINT('Ctrl Pts',(-38.1104491357725,90.6894605690494,110.734708580032));
#42890=CARTESIAN_POINT('Ctrl Pts',(-34.8687859531413,90.8353021806444,110.57676005684));
#42891=CARTESIAN_POINT('Ctrl Pts',(-32.9745608196483,88.2006179289376,110.418811533647));
#42892=CARTESIAN_POINT('Ctrl Pts',(-34.1452100540536,85.1741958920582,110.260863010455));
#42893=CARTESIAN_POINT('Ctrl Pts',(-37.3193415982316,84.5000008917143,110.102914487262));
#42894=CARTESIAN_POINT('Ctrl Pts',(-39.6190669199333,86.789305019032,109.94496596407));
#42895=CARTESIAN_POINT('Ctrl Pts',(-38.9592950088217,89.9664658703735,109.787017440877));
#42896=CARTESIAN_POINT('Ctrl Pts',(-35.9382209991481,91.1508482844039,109.629068917685));
#42897=CARTESIAN_POINT('Ctrl Pts',(-33.2949607961862,89.2686088431145,109.471120394492));
#42898=CARTESIAN_POINT('Ctrl Pts',(-33.4260780707944,86.0263166059414,109.3131718713));
#42899=CARTESIAN_POINT('Ctrl Pts',(-36.2126927038881,84.3636597380785,109.155223348107));
#42900=CARTESIAN_POINT('Ctrl Pts',(-39.1282661107737,85.7881178241517,108.997274824915));
#42901=CARTESIAN_POINT('Ctrl Pts',(-39.5293362438264,89.0081797474739,108.839326301723));
#42902=CARTESIAN_POINT('Ctrl Pts',(-37.0522656546062,91.1043097853572,108.68137777853));
#42903=CARTESIAN_POINT('Ctrl Pts',(-33.9429375868874,90.1760178030121,108.523429255338));
#42904=CARTESIAN_POINT('Ctrl Pts',(-33.0204879540809,87.0649430605694,108.365480732145));
#42905=CARTESIAN_POINT('Ctrl Pts',(-35.1212681886914,84.591832942591,108.207532208953));
#42906=CARTESIAN_POINT('Ctrl Pts',(-38.3405762497377,84.9989183808745,108.04958368576));
#42907=CARTESIAN_POINT('Ctrl Pts',(-39.7595397677092,87.9172365322217,107.891635162568));
#42908=CARTESIAN_POINT('Ctrl Pts',(-38.0916763373207,90.7005714972004,107.733686639375));
#42909=CARTESIAN_POINT('Ctrl Pts',(-34.8490869313939,90.825904308939,107.575738116183));
#42910=CARTESIAN_POINT('Ctrl Pts',(-32.9719345211937,88.1784761977243,107.41778959299));
#42911=CARTESIAN_POINT('Ctrl Pts',(-34.1617526948657,85.1609399070733,107.259841069798));
#42912=CARTESIAN_POINT('Ctrl Pts',(-37.3406319323637,84.50443980712,107.101892546605));
#42913=CARTESIAN_POINT('Ctrl Pts',(-39.6245489464603,86.8140194698805,106.943944023413));
#42914=CARTESIAN_POINT('Ctrl Pts',(-39.171002016807,88.9192333079152,106.838645007951));
#42915=CARTESIAN_POINT('Ctrl Pts',(-38.5501231787025,89.6454190276512,106.78599550022));
#42916=CARTESIAN_POINT('Ctrl Pts',(-37.0529925008447,85.1574234026337,122.21400449978));
#42917=CARTESIAN_POINT('Ctrl Pts',(-37.9167722964266,85.3883483930035,122.161354992049));
#42918=CARTESIAN_POINT('Ctrl Pts',(-39.3825156524183,86.7715081214603,122.056055976587));
#42919=CARTESIAN_POINT('Ctrl Pts',(-38.845406557921,89.7633892661443,121.898107453395));
#42920=CARTESIAN_POINT('Ctrl Pts',(-36.0457870456165,90.9421853309626,121.740158930202));
#42921=CARTESIAN_POINT('Ctrl Pts',(-33.528601247485,89.2457170582044,121.58221040701));
#42922=CARTESIAN_POINT('Ctrl Pts',(-33.5729144775109,86.2089037065505,121.424261883817));
#42923=CARTESIAN_POINT('Ctrl Pts',(-36.1401004378356,84.5866887998078,121.266313360625));
#42924=CARTESIAN_POINT('Ctrl Pts',(-38.9018155326728,85.8491280097327,121.108364837432));
#42925=CARTESIAN_POINT('Ctrl Pts',(-39.354463392039,88.8519742875062,120.95041631424));
#42926=CARTESIAN_POINT('Ctrl Pts',(-37.0874636540108,90.8724592083668,120.792467791047));
#42927=CARTESIAN_POINT('Ctrl Pts',(-34.1563227391702,90.0787575995008,120.634519267855));
#42928=CARTESIAN_POINT('Ctrl Pts',(-33.2185748075125,87.1904522398145,120.476570744663));
#42929=CARTESIAN_POINT('Ctrl Pts',(-35.1244678891676,84.8263023383961,120.31862222147));
#42930=CARTESIAN_POINT('Ctrl Pts',(-38.1459767235555,85.1298006998218,120.160673698278));
#42931=CARTESIAN_POINT('Ctrl Pts',(-39.5435959928072,87.8257794570092,120.002725175085));
#42932=CARTESIAN_POINT('Ctrl Pts',(-38.0501444551837,90.4698742988431,119.844776651893));
#42933=CARTESIAN_POINT('Ctrl Pts',(-35.0196903446579,90.6647659994386,119.6868281287));
#42934=CARTESIAN_POINT('Ctrl Pts',(-33.1998536788618,88.2337516217006,119.528879605508));
#42935=CARTESIAN_POINT('Ctrl Pts',(-34.2406252858241,85.3809582380354,119.370931082315));
#42936=CARTESIAN_POINT('Ctrl Pts',(-37.1983690713843,84.6929267133288,119.212982559123));
#42937=CARTESIAN_POINT('Ctrl Pts',(-39.391388764957,86.7934743698275,119.05503403593));
#42938=CARTESIAN_POINT('Ctrl Pts',(-38.8313400769042,89.7780985013739,118.897085512738));
#42939=CARTESIAN_POINT('Ctrl Pts',(-36.0260021347214,90.940731196344,118.739136989545));
#42940=CARTESIAN_POINT('Ctrl Pts',(-33.5188895227229,89.2272487426878,118.581188466353));
#42941=CARTESIAN_POINT('Ctrl Pts',(-33.5831249994063,86.1912135715186,118.42323994316));
#42942=CARTESIAN_POINT('Ctrl Pts',(-36.1604682099547,84.5853064339508,118.265291419968));
#42943=CARTESIAN_POINT('Ctrl Pts',(-38.9141204525613,85.8655544910099,118.107342896776));
#42944=CARTESIAN_POINT('Ctrl Pts',(-39.3474289869899,88.8711957659313,117.949394373583));
#42945=CARTESIAN_POINT('Ctrl Pts',(-37.0675261437579,90.8771067273923,117.791445850391));
#42946=CARTESIAN_POINT('Ctrl Pts',(-34.1415304906156,90.0645889135622,117.633497327198));
#42947=CARTESIAN_POINT('Ctrl Pts',(-33.2223532961796,87.1703275146764,117.475548804006));
#42948=CARTESIAN_POINT('Ctrl Pts',(-35.1433845671111,84.8184613160999,117.317600280813));
#42949=CARTESIAN_POINT('Ctrl Pts',(-38.162883675593,85.1413558713164,117.159651757621));
#42950=CARTESIAN_POINT('Ctrl Pts',(-39.5431626138732,87.8462525074993,117.001703234428));
#42951=CARTESIAN_POINT('Ctrl Pts',(-38.0327644479022,90.4807037103371,116.843754711236));
#42952=CARTESIAN_POINT('Ctrl Pts',(-35.0011212580808,90.6561326974266,116.685806188043));
#42953=CARTESIAN_POINT('Ctrl Pts',(-33.1969317213611,88.2134833416061,116.527857664851));
#42954=CARTESIAN_POINT('Ctrl Pts',(-34.255999618742,85.3674315239755,116.369909141658));
#42955=CARTESIAN_POINT('Ctrl Pts',(-37.2181002977627,84.6984058688277,116.211960618466));
#42956=CARTESIAN_POINT('Ctrl Pts',(-39.3975871609747,86.8129915901892,116.054012095273));
#42957=CARTESIAN_POINT('Ctrl Pts',(-38.8183857556004,89.7939581267197,115.896063572081));
#42958=CARTESIAN_POINT('Ctrl Pts',(-36.0056403802781,90.9385537817452,115.738115048888));
#42959=CARTESIAN_POINT('Ctrl Pts',(-33.5095817210291,89.209008486158,115.580166525696));
#42960=CARTESIAN_POINT('Ctrl Pts',(-33.5933102500017,86.1734483577242,115.422218002503));
#42961=CARTESIAN_POINT('Ctrl Pts',(-36.1809118564649,84.584123442507,115.264269479311));
#42962=CARTESIAN_POINT('Ctrl Pts',(-38.9262868621835,85.8820263040013,115.106320956119));
#42963=CARTESIAN_POINT('Ctrl Pts',(-39.3402872462792,88.8903878916216,114.948372432926));
#42964=CARTESIAN_POINT('Ctrl Pts',(-37.0475514517448,90.8816182490542,114.790423909734));
#42965=CARTESIAN_POINT('Ctrl Pts',(-34.1268332930775,90.0503293717488,114.632475386541));
#42966=CARTESIAN_POINT('Ctrl Pts',(-33.2262590951137,87.1502256022498,114.474526863349));
#42967=CARTESIAN_POINT('Ctrl Pts',(-35.1623520934209,84.8107428256929,114.316578340156));
#42968=CARTESIAN_POINT('Ctrl Pts',(-38.1797156500409,85.1530189234301,114.158629816964));
#42969=CARTESIAN_POINT('Ctrl Pts',(-39.5425979971506,87.8667225674997,114.000681293771));
#42970=CARTESIAN_POINT('Ctrl Pts',(-38.0153151608184,90.4914211973897,113.842732770579));
#42971=CARTESIAN_POINT('Ctrl Pts',(-34.9826080385391,90.6473803919789,113.684784247386));
#42972=CARTESIAN_POINT('Ctrl Pts',(-33.1941399424655,88.1931966928179,113.526835724194));
#42973=CARTESIAN_POINT('Ctrl Pts',(-34.2714605015093,85.3540038193127,113.368887201001));
#42974=CARTESIAN_POINT('Ctrl Pts',(-37.2377959300091,84.7040115997228,113.210938677809));
#42975=CARTESIAN_POINT('Ctrl Pts',(-39.4036601119581,86.8325482109303,113.052990154616));
#42976=CARTESIAN_POINT('Ctrl Pts',(-38.8053298653645,89.8097342440683,112.895041631424));
#42977=CARTESIAN_POINT('Ctrl Pts',(-35.985293027423,90.9362456699106,112.737093108231));
#42978=CARTESIAN_POINT('Ctrl Pts',(-33.5003912315516,89.1907088399423,112.579144585039));
#42979=CARTESIAN_POINT('Ctrl Pts',(-33.6036093611951,86.1557489097928,112.421196061847));
#42980=CARTESIAN_POINT('Ctrl Pts',(-36.2013626774433,84.5830717439945,112.263247538654));
#42981=CARTESIAN_POINT('Ctrl Pts',(-38.9383472555495,85.8985758979639,112.105299015462));
#42982=CARTESIAN_POINT('Ctrl Pts',(-39.3330224201682,88.909533764545,111.947350492269));
#42983=CARTESIAN_POINT('Ctrl Pts',(-37.0275482030416,90.886001420257,111.789401969077));
#42984=CARTESIAN_POINT('Ctrl Pts',(-34.1122279590109,90.0359757532041,111.631453445884));
#42985=CARTESIAN_POINT('Ctrl Pts',(-33.2302938878788,87.1301491833573,111.473504922692));
#42986=CARTESIAN_POINT('Ctrl Pts',(-35.1813687891343,84.803146284844,111.315556399499));
#42987=CARTESIAN_POINT('Ctrl Pts',(-38.1964723890577,85.1647898132184,111.157607876307));
#42988=CARTESIAN_POINT('Ctrl Pts',(-39.5419019538542,87.8871885800586,110.999659353114));
#42989=CARTESIAN_POINT('Ctrl Pts',(-37.9977974164621,90.502026421765,110.841710829922));
#42990=CARTESIAN_POINT('Ctrl Pts',(-34.9641513992233,90.6385093933869,110.683762306729));
#42991=CARTESIAN_POINT('Ctrl Pts',(-33.1914784815791,88.1728925366768,110.525813783537));
#42992=CARTESIAN_POINT('Ctrl Pts',(-34.2870072849925,85.3406756648394,110.367865260344));
#42993=CARTESIAN_POINT('Ctrl Pts',(-37.2574551614964,84.7097436825796,110.209916737152));
#42994=CARTESIAN_POINT('Ctrl Pts',(-39.409607365434,86.8521434190164,110.05196821396));
#42995=CARTESIAN_POINT('Ctrl Pts',(-38.792172944377,89.8254262123803,109.894019690767));
#42996=CARTESIAN_POINT('Ctrl Pts',(-35.9649609174351,90.9338069388119,109.736071167575));
#42997=CARTESIAN_POINT('Ctrl Pts',(-33.4913184273068,89.1723505928374,109.578122644382));
#42998=CARTESIAN_POINT('Ctrl Pts',(-33.6140219210065,86.1381158874167,109.42017412119));
#42999=CARTESIAN_POINT('Ctrl Pts',(-36.221819803451,84.5821515255878,109.262225597997));
#43000=CARTESIAN_POINT('Ctrl Pts',(-38.9503011895357,85.9152022949253,109.104277074805));
#43001=CARTESIAN_POINT('Ctrl Pts',(-39.3256346968193,88.9286332032591,108.946328551612));
#43002=CARTESIAN_POINT('Ctrl Pts',(-37.0075174514281,90.8902548100658,108.78838002842));
#43003=CARTESIAN_POINT('Ctrl Pts',(-34.0977146195165,90.0215312208402,108.630431505227));
#43004=CARTESIAN_POINT('Ctrl Pts',(-33.2344584769103,87.1100937981272,108.472482982035));
#43005=CARTESIAN_POINT('Ctrl Pts',(-35.2004318778381,84.7956828809793,108.314534458842));
#43006=CARTESIAN_POINT('Ctrl Pts',(-38.2131572991543,85.1766456920269,108.15658593565));
#43007=CARTESIAN_POINT('Ctrl Pts',(-39.5410660862132,87.907695692627,107.998637412457));
#43008=CARTESIAN_POINT('Ctrl Pts',(-37.9802292663962,90.5124243628941,107.840688889265));
#43009=CARTESIAN_POINT('Ctrl Pts',(-34.9457164615075,90.6297145820622,107.682740366073));
#43010=CARTESIAN_POINT('Ctrl Pts',(-33.1890207124038,88.1521716378895,107.52479184288));
#43011=CARTESIAN_POINT('Ctrl Pts',(-34.3024883863861,85.3282703149345,107.366843319688));
#43012=CARTESIAN_POINT('Ctrl Pts',(-37.2773792972584,84.7138977532781,107.208894796495));
#43013=CARTESIAN_POINT('Ctrl Pts',(-39.4147376109293,86.8752719463065,107.050946273303));
#43014=CARTESIAN_POINT('Ctrl Pts',(-38.9902947372386,88.8453944468205,106.945647257841));
#43015=CARTESIAN_POINT('Ctrl Pts',(-38.4092576250255,89.5249809097992,106.89299775011));
#43016=CARTESIAN_POINT('Ctrl Pts',(-37.0051260726588,85.3364687865372,122.321006749669));
#43017=CARTESIAN_POINT('Ctrl Pts',(-37.8096764711459,85.551559245903,122.268357241939));
#43018=CARTESIAN_POINT('Ctrl Pts',(-39.1749137771984,86.8398756853395,122.163058226477));
#43019=CARTESIAN_POINT('Ctrl Pts',(-38.674634263578,89.6266034827405,122.005109703284));
#43020=CARTESIAN_POINT('Ctrl Pts',(-36.0669847147491,90.7245694788604,121.847161180092));
#43021=CARTESIAN_POINT('Ctrl Pts',(-33.7224023949133,89.1444280679948,121.6892126569));
#43022=CARTESIAN_POINT('Ctrl Pts',(-33.7636770659093,86.3158490659145,121.531264133707));
#43023=CARTESIAN_POINT('Ctrl Pts',(-36.1548310358608,84.8048694663372,121.373315610515));
#43024=CARTESIAN_POINT('Ctrl Pts',(-38.7271752738528,85.980743195505,121.215367087322));
#43025=CARTESIAN_POINT('Ctrl Pts',(-39.1487850608496,88.7776842466098,121.05741856413));
#43026=CARTESIAN_POINT('Ctrl Pts',(-37.0372335381933,90.6596244778241,120.899470040937));
#43027=CARTESIAN_POINT('Ctrl Pts',(-34.3070810119143,89.9203470034502,120.741521517745));
#43028=CARTESIAN_POINT('Ctrl Pts',(-33.4336344738561,87.2300927974898,120.583572994552));
#43029=CARTESIAN_POINT('Ctrl Pts',(-35.2088404304695,85.028052700004,120.42562447136));
#43030=CARTESIAN_POINT('Ctrl Pts',(-38.023164346325,85.3107401729852,120.267675948167));
#43031=CARTESIAN_POINT('Ctrl Pts',(-39.3249488355677,87.8218556152566,120.109727424975));
#43032=CARTESIAN_POINT('Ctrl Pts',(-37.9339032984275,90.2846448232422,119.951778901782));
#43033=CARTESIAN_POINT('Ctrl Pts',(-35.1112474841897,90.4661727962024,119.79383037859));
#43034=CARTESIAN_POINT('Ctrl Pts',(-33.4161970533549,88.2018531208163,119.635881855397));
#43035=CARTESIAN_POINT('Ctrl Pts',(-34.3856029313326,85.5446758340026,119.477933332205));
#43036=CARTESIAN_POINT('Ctrl Pts',(-37.1405341689775,84.903822644097,119.319984809013));
#43037=CARTESIAN_POINT('Ctrl Pts',(-39.1831784602407,86.8603357076363,119.16203628582));
#43038=CARTESIAN_POINT('Ctrl Pts',(-38.6615323214334,89.6403041054291,119.004087762628));
#43039=CARTESIAN_POINT('Ctrl Pts',(-36.0485564555722,90.7232150542806,118.846139239435));
#43040=CARTESIAN_POINT('Ctrl Pts',(-33.7133566033038,89.1272261252261,118.688190716243));
#43041=CARTESIAN_POINT('Ctrl Pts',(-33.7731874521231,86.2993719437801,118.53024219305));
#43042=CARTESIAN_POINT('Ctrl Pts',(-36.1738021894563,84.8035818893332,118.372293669858));
#43043=CARTESIAN_POINT('Ctrl Pts',(-38.7386364451493,85.9960433126471,118.214345146665));
#43044=CARTESIAN_POINT('Ctrl Pts',(-39.1422330050891,88.7955877078919,118.056396623473));
#43045=CARTESIAN_POINT('Ctrl Pts',(-37.0186631433996,90.6639533163812,117.89844810028));
#43046=CARTESIAN_POINT('Ctrl Pts',(-34.2933030681259,89.9071498645772,117.740499577088));
#43047=CARTESIAN_POINT('Ctrl Pts',(-33.4371538714831,87.2113480251391,117.582551053896));
#43048=CARTESIAN_POINT('Ctrl Pts',(-35.2264599914449,85.0207493367565,117.424602530703));
#43049=CARTESIAN_POINT('Ctrl Pts',(-38.0389119883381,85.3215030061496,117.266654007511));
#43050=CARTESIAN_POINT('Ctrl Pts',(-39.3245451734354,87.8409248282832,117.108705484318));
#43051=CARTESIAN_POINT('Ctrl Pts',(-37.9177150385775,90.2947316617829,116.950756961126));
#43052=CARTESIAN_POINT('Ctrl Pts',(-35.0939516802342,90.4581314798742,116.792808437933));
#43053=CARTESIAN_POINT('Ctrl Pts',(-33.4134754545358,88.1829746370754,116.634859914741));
#43054=CARTESIAN_POINT('Ctrl Pts',(-34.3999230459485,85.5320766469841,116.476911391548));
#43055=CARTESIAN_POINT('Ctrl Pts',(-37.158912424786,84.9089260937988,116.318962868356));
#43056=CARTESIAN_POINT('Ctrl Pts',(-39.188951832125,86.8785146318246,116.161014345163));
#43057=CARTESIAN_POINT('Ctrl Pts',(-38.6494662781891,89.6550762359618,116.003065821971));
#43058=CARTESIAN_POINT('Ctrl Pts',(-36.0295909070203,90.7211869450424,115.845117298778));
#43059=CARTESIAN_POINT('Ctrl Pts',(-33.70468703775,89.1102366034352,115.687168775586));
#43060=CARTESIAN_POINT('Ctrl Pts',(-33.7826742998905,86.2828248910351,115.529220252393));
#43061=CARTESIAN_POINT('Ctrl Pts',(-36.1928440147345,84.8024800156354,115.371271729201));
#43062=CARTESIAN_POINT('Ctrl Pts',(-38.7499686038312,86.0113856531068,115.213323206008));
#43063=CARTESIAN_POINT('Ctrl Pts',(-39.1355809736756,88.8134638291569,115.055374682816));
#43064=CARTESIAN_POINT('Ctrl Pts',(-37.0000581163997,90.6681554829164,114.897426159623));
#43065=CARTESIAN_POINT('Ctrl Pts',(-34.2796136577039,89.8938680998186,114.739477636431));
#43066=CARTESIAN_POINT('Ctrl Pts',(-33.4407918497096,87.1926245012317,114.581529113239));
#43067=CARTESIAN_POINT('Ctrl Pts',(-35.2441269141131,85.0135601033844,114.423580590046));
#43068=CARTESIAN_POINT('Ctrl Pts',(-38.0545897939765,85.3323663225568,114.265632066854));
#43069=CARTESIAN_POINT('Ctrl Pts',(-39.3240192724923,87.8599912558781,114.107683543661));
#43070=CARTESIAN_POINT('Ctrl Pts',(-37.9014622494426,90.3047142505435,113.949735020469));
#43071=CARTESIAN_POINT('Ctrl Pts',(-35.0767079125104,90.4499793201784,113.791786497276));
#43072=CARTESIAN_POINT('Ctrl Pts',(-33.4108751079725,88.1640790441824,113.633837974084));
#43073=CARTESIAN_POINT('Ctrl Pts',(-34.4143237756889,85.5195696802868,113.475889450891));
#43074=CARTESIAN_POINT('Ctrl Pts',(-37.1772575271527,84.9141474396192,113.317940927699));
#43075=CARTESIAN_POINT('Ctrl Pts',(-39.1946083607433,86.8967302547077,113.159992404506));
#43076=CARTESIAN_POINT('Ctrl Pts',(-38.6373056305963,89.6697705846423,113.002043881314));
#43077=CARTESIAN_POINT('Ctrl Pts',(-36.0106387725394,90.7190371004805,112.844095358121));
#43078=CARTESIAN_POINT('Ctrl Pts',(-33.6961267403118,89.0931917643103,112.686146834929));
#43079=CARTESIAN_POINT('Ctrl Pts',(-33.7922672008325,86.2663390945867,112.528198311736));
#43080=CARTESIAN_POINT('Ctrl Pts',(-36.2118925225276,84.8015004321101,112.370249788544));
#43081=CARTESIAN_POINT('Ctrl Pts',(-38.7612020157935,86.026800441095,112.212301265352));
#43082=CARTESIAN_POINT('Ctrl Pts',(-39.1288142968298,88.8312968692079,112.054352742159));
#43083=CARTESIAN_POINT('Ctrl Pts',(-36.9814264908424,90.6722380999861,111.896404218967));
#43084=CARTESIAN_POINT('Ctrl Pts',(-34.2660098116734,89.8804987091719,111.738455695774));
#43085=CARTESIAN_POINT('Ctrl Pts',(-33.4445499766577,87.1739247227665,111.580507172582));
#43086=CARTESIAN_POINT('Ctrl Pts',(-35.2618396346379,85.0064844574867,111.422558649389));
#43087=CARTESIAN_POINT('Ctrl Pts',(-38.0701975230785,85.3433300822074,111.264610126197));
#43088=CARTESIAN_POINT('Ctrl Pts',(-39.3233709568981,87.8790539135646,111.106661603004));
#43089=CARTESIAN_POINT('Ctrl Pts',(-37.8851456971516,90.3145922744807,110.948713079812));
#43090=CARTESIAN_POINT('Ctrl Pts',(-35.0595168453053,90.4417166061294,110.790764556619));
#43091=CARTESIAN_POINT('Ctrl Pts',(-33.40839614351,88.1451671444161,110.632816033427));
#43092=CARTESIAN_POINT('Ctrl Pts',(-34.4288045159315,85.5071554376204,110.474867510234));
#43093=CARTESIAN_POINT('Ctrl Pts',(-37.1955687247611,84.919486473445,110.316918987042));
#43094=CARTESIAN_POINT('Ctrl Pts',(-39.2001478109348,86.9149818190007,110.158970463849));
#43095=CARTESIAN_POINT('Ctrl Pts',(-38.6250508799324,89.6843865543872,110.001021940657));
#43096=CARTESIAN_POINT('Ctrl Pts',(-35.9917008357221,90.7167655932198,109.843073417465));
#43097=CARTESIAN_POINT('Ctrl Pts',(-33.6876760584274,89.0760923425604,109.685124894272));
#43098=CARTESIAN_POINT('Ctrl Pts',(-33.8019657712185,86.2499151688921,109.52717637108));
#43099=CARTESIAN_POINT('Ctrl Pts',(-36.2309469030138,84.8006433130971,109.369227847887));
#43100=CARTESIAN_POINT('Ctrl Pts',(-38.7723362682978,86.042286765699,109.211279324695));
#43101=CARTESIAN_POINT('Ctrl Pts',(-39.1219331498121,88.8490866590441,109.053330801502));
#43102=CARTESIAN_POINT('Ctrl Pts',(-36.9627692482499,90.6761998347745,108.89538227831));
#43103=CARTESIAN_POINT('Ctrl Pts',(-34.2524916521456,89.8670446386682,108.737433755117));
#43104=CARTESIAN_POINT('Ctrl Pts',(-33.4484289997396,87.1552445356851,108.579485231925));
#43105=CARTESIAN_POINT('Ctrl Pts',(-35.2795955669848,84.9995328193676,108.421536708732));
#43106=CARTESIAN_POINT('Ctrl Pts',(-38.0857383485708,85.3543730031793,108.26358818554));
#43107=CARTESIAN_POINT('Ctrl Pts',(-39.3225924047172,87.8981548530322,108.105639662347));
#43108=CARTESIAN_POINT('Ctrl Pts',(-37.8687821954715,90.3242772285877,107.947691139155));
#43109=CARTESIAN_POINT('Ctrl Pts',(-35.0423459916211,90.4335248551855,107.789742615962));
#43110=CARTESIAN_POINT('Ctrl Pts',(-33.406106903614,88.1258670780547,107.63179409277));
#43111=CARTESIAN_POINT('Ctrl Pts',(-34.4432240779066,85.4956007227958,107.473845569577));
#43112=CARTESIAN_POINT('Ctrl Pts',(-37.2141266621531,84.9233556994363,107.315897046385));
#43113=CARTESIAN_POINT('Ctrl Pts',(-39.2049262753984,86.9365244227325,107.157948523192));
#43114=CARTESIAN_POINT('Ctrl Pts',(-38.8095874576701,88.7715555857258,107.052649507731));
#43115=CARTESIAN_POINT('Ctrl Pts',(-38.2683920713485,89.4045427919473,107.));
#43116=CARTESIAN_POINT('Ctrl Pts',(-38.8699207989934,87.7703173750275,121.112583302492));
#43117=CARTESIAN_POINT('Ctrl Pts',(-38.8718336645079,88.0618702234686,121.094195056371));
#43118=CARTESIAN_POINT('Ctrl Pts',(-38.8249623706359,88.3528282219475,121.07580681025));
#43119=CARTESIAN_POINT('Ctrl Pts',(-38.7265915092407,88.6251841099614,121.05741856413));
#43120=CARTESIAN_POINT('Ctrl Pts',(-38.4449345532975,89.4049976570146,121.004769056399));
#43121=CARTESIAN_POINT('Ctrl Pts',(-37.7410840457454,90.0323110674193,120.952119548668));
#43122=CARTESIAN_POINT('Ctrl Pts',(-36.9341333709228,90.2227548602261,120.899470040937));
#43123=CARTESIAN_POINT('Ctrl Pts',(-36.1271826961003,90.4131986530328,120.846820533206));
#43124=CARTESIAN_POINT('Ctrl Pts',(-35.2171318540073,90.1667728282415,120.794171025476));
#43125=CARTESIAN_POINT('Ctrl Pts',(-34.6165320099511,89.5951842148525,120.741521517745));
#43126=CARTESIAN_POINT('Ctrl Pts',(-34.0159321658949,89.0235956014634,120.688872010014));
#43127=CARTESIAN_POINT('Ctrl Pts',(-33.7247833198755,88.1268441994766,120.636222502283));
#43128=CARTESIAN_POINT('Ctrl Pts',(-33.8750765563014,87.3114618155689,120.583572994552));
#43129=CARTESIAN_POINT('Ctrl Pts',(-34.0253697927272,86.4960794316612,120.530923486822));
#43130=CARTESIAN_POINT('Ctrl Pts',(-34.6171051115984,85.7620660658326,120.478273979091));
#43131=CARTESIAN_POINT('Ctrl Pts',(-35.3820267570099,85.4421739617485,120.42562447136));
#43132=CARTESIAN_POINT('Ctrl Pts',(-36.1469484024214,85.1222818576644,120.372974963629));
#43133=CARTESIAN_POINT('Ctrl Pts',(-37.0850563743732,85.2165110153248,120.320325455898));
#43134=CARTESIAN_POINT('Ctrl Pts',(-37.7710744418896,85.6821448345336,120.267675948167));
#43135=CARTESIAN_POINT('Ctrl Pts',(-38.4446885721246,86.1393594983833,120.215978399609));
#43136=CARTESIAN_POINT('Ctrl Pts',(-38.8752464913585,86.9546694615518,120.16428085105));
#43137=CARTESIAN_POINT('Ctrl Pts',(-38.8765117847785,87.7688288397063,120.112583302492));
#43138=CARTESIAN_POINT('Ctrl Pts',(-37.1487253572165,84.7993326348266,122.));
#43139=CARTESIAN_POINT('Ctrl Pts',(-37.2417753891008,84.8333707521416,122.));
#43140=CARTESIAN_POINT('Ctrl Pts',(-37.3327602562807,84.8721775720516,122.));
#43141=CARTESIAN_POINT('Ctrl Pts',(-37.4214714739468,84.9154247709244,122.));
#43142=CARTESIAN_POINT('Ctrl Pts',(-37.5121496630562,84.9596308790244,122.));
#43143=CARTESIAN_POINT('Ctrl Pts',(-37.6004529266836,85.0084770764388,122.));
#43144=CARTESIAN_POINT('Ctrl Pts',(-37.6861296852363,85.0616582541536,122.));
#43145=CARTESIAN_POINT('Ctrl Pts',(-37.7685611201985,85.1128249983916,122.));
#43146=CARTESIAN_POINT('Ctrl Pts',(-37.8485615426075,85.1680054118964,122.));
#43147=CARTESIAN_POINT('Ctrl Pts',(-37.9258739256416,85.2269578069965,122.));
#43148=CARTESIAN_POINT('Ctrl Pts',(-37.9935222607964,85.2785411527092,122.));
#43149=CARTESIAN_POINT('Ctrl Pts',(-38.059112275569,85.3330131191914,122.));
#43150=CARTESIAN_POINT('Ctrl Pts',(-38.1224471612445,85.3902244937864,122.));
#43151=CARTESIAN_POINT('Ctrl Pts',(-38.1365836289362,85.402994182086,122.));
#43152=CARTESIAN_POINT('Ctrl Pts',(-38.1506103907732,85.4159030811327,122.));
#43153=CARTESIAN_POINT('Ctrl Pts',(-38.1645056734731,85.428930998852,122.));
#43154=CARTESIAN_POINT('Ctrl Pts',(-38.236935765249,85.4968398925705,122.));
#43155=CARTESIAN_POINT('Ctrl Pts',(-38.3059001696468,85.5680707029916,122.));
#43156=CARTESIAN_POINT('Ctrl Pts',(-38.3711589370242,85.6423327060287,122.));
#43157=CARTESIAN_POINT('Ctrl Pts',(-38.4360586851855,85.7161861588099,122.));
#43158=CARTESIAN_POINT('Ctrl Pts',(-38.4972939435271,85.7930383408696,122.));
#43159=CARTESIAN_POINT('Ctrl Pts',(-38.5545850913186,85.8726300682051,122.));
#43160=CARTESIAN_POINT('Ctrl Pts',(-38.6097480011666,85.9492651409677,122.));
#43161=CARTESIAN_POINT('Ctrl Pts',(-38.6612545505178,86.0284407407527,122.));
#43162=CARTESIAN_POINT('Ctrl Pts',(-38.7088102913344,86.1099390932959,122.));
#43163=CARTESIAN_POINT('Ctrl Pts',(-38.7287566222569,86.144121992806,122.));
#43164=CARTESIAN_POINT('Ctrl Pts',(-38.7480073496925,86.1787136222189,122.));
#43165=CARTESIAN_POINT('Ctrl Pts',(-38.7665381634545,86.2136982099032,122.));
#43166=CARTESIAN_POINT('Ctrl Pts',(-38.7794207042811,86.2380193425275,122.));
#43167=CARTESIAN_POINT('Ctrl Pts',(-38.7919552805797,86.2625303934131,122.));
#43168=CARTESIAN_POINT('Ctrl Pts',(-38.8041332584856,86.2872260692728,122.));
#43169=CARTESIAN_POINT('Ctrl Pts',(-38.8120415994691,86.3032633643826,122.));
#43170=CARTESIAN_POINT('Ctrl Pts',(-38.8198006651,86.319381131767,122.));
#43171=CARTESIAN_POINT('Ctrl Pts',(-38.8273979149827,86.3355557323494,122.));
#43172=CARTESIAN_POINT('Ctrl Pts',(-38.8695182138971,86.4252301568939,122.));
#43173=CARTESIAN_POINT('Ctrl Pts',(-38.9067396802643,86.5167881682253,122.));
#43174=CARTESIAN_POINT('Ctrl Pts',(-38.9387710306477,86.6099574003158,122.));
#43175=CARTESIAN_POINT('Ctrl Pts',(-38.9686507850787,86.6968683092245,122.));
#43176=CARTESIAN_POINT('Ctrl Pts',(-38.9940140885018,86.7851820439995,122.));
#43177=CARTESIAN_POINT('Ctrl Pts',(-39.0145739632211,86.8746862171339,122.));
#43178=CARTESIAN_POINT('Ctrl Pts',(-39.0160544487227,86.8811312773528,122.));
#43179=CARTESIAN_POINT('Ctrl Pts',(-39.0175100048601,86.8875825114178,122.));
#43180=CARTESIAN_POINT('Ctrl Pts',(-39.0189405138548,86.8940398403423,122.));
#43181=CARTESIAN_POINT('Ctrl Pts',(-39.0395467338659,86.9870564805743,122.));
#43182=CARTESIAN_POINT('Ctrl Pts',(-39.0549599296115,87.0813387804123,122.));
#43183=CARTESIAN_POINT('Ctrl Pts',(-39.0652570210305,87.1764788744327,122.));
#43184=CARTESIAN_POINT('Ctrl Pts',(-39.0710535407633,87.2300358848478,122.));
#43185=CARTESIAN_POINT('Ctrl Pts',(-39.0752279006169,87.2838645309515,122.));
#43186=CARTESIAN_POINT('Ctrl Pts',(-39.0777870601897,87.3378894180018,122.));
#43187=CARTESIAN_POINT('Ctrl Pts',(-39.0784479432014,87.3518409239729,122.));
#43188=CARTESIAN_POINT('Ctrl Pts',(-39.07900098961,87.3658049179873,122.));
#43189=CARTESIAN_POINT('Ctrl Pts',(-39.0794460778701,87.3797667321621,122.));
#43190=CARTESIAN_POINT('Ctrl Pts',(-39.0824174908988,87.4729759229344,122.));
#43191=CARTESIAN_POINT('Ctrl Pts',(-39.0805897501033,87.5662433468626,122.));
#43192=CARTESIAN_POINT('Ctrl Pts',(-39.0740977497051,87.659193925161,122.));
#43193=CARTESIAN_POINT('Ctrl Pts',(-39.0675949549735,87.7522990535925,122.));
#43194=CARTESIAN_POINT('Ctrl Pts',(-39.0564119991282,87.845087261528,122.));
#43195=CARTESIAN_POINT('Ctrl Pts',(-39.0406335176743,87.9371695003463,122.));
#43196=CARTESIAN_POINT('Ctrl Pts',(-39.0250806320128,88.0279351761161,122.));
#43197=CARTESIAN_POINT('Ctrl Pts',(-39.0050622311029,88.1180157699776,122.));
#43198=CARTESIAN_POINT('Ctrl Pts',(-38.9806163469264,88.2070134839553,122.));
#43199=CARTESIAN_POINT('Ctrl Pts',(-38.9715175827602,88.2401384552168,122.));
#43200=CARTESIAN_POINT('Ctrl Pts',(-38.9618050679078,88.2731130950482,122.));
#43201=CARTESIAN_POINT('Ctrl Pts',(-38.9514794019202,88.3059156261388,122.));
#43202=CARTESIAN_POINT('Ctrl Pts',(-38.944484882208,88.328135786136,122.));
#43203=CARTESIAN_POINT('Ctrl Pts',(-38.9372089974467,88.3502769571618,122.));
#43204=CARTESIAN_POINT('Ctrl Pts',(-38.9296517548766,88.3723321568593,122.));
#43205=CARTESIAN_POINT('Ctrl Pts',(-38.9251356923547,88.3855119191658,122.));
#43206=CARTESIAN_POINT('Ctrl Pts',(-38.9205195020769,88.3986598081647,122.));
#43207=CARTESIAN_POINT('Ctrl Pts',(-38.9158066558644,88.4117651858116,122.));
#43208=CARTESIAN_POINT('Ctrl Pts',(-38.8841749038243,88.4997260564677,122.));
#43209=CARTESIAN_POINT('Ctrl Pts',(-38.8481539347597,88.5858891804725,122.));
#43210=CARTESIAN_POINT('Ctrl Pts',(-38.8078083123978,88.6698403149831,122.));
#43211=CARTESIAN_POINT('Ctrl Pts',(-38.7775490956264,88.7328036658661,122.));
#43212=CARTESIAN_POINT('Ctrl Pts',(-38.7448562140504,88.7945222807168,122.));
#43213=CARTESIAN_POINT('Ctrl Pts',(-38.7097409437031,88.8548058697244,122.));
#43214=CARTESIAN_POINT('Ctrl Pts',(-38.6962715801236,88.8779291881608,122.));
#43215=CARTESIAN_POINT('Ctrl Pts',(-38.6824456762413,88.900841209529,122.));
#43216=CARTESIAN_POINT('Ctrl Pts',(-38.6682633879976,88.9235305507161,122.));
#43217=CARTESIAN_POINT('Ctrl Pts',(-38.6581392015999,88.9397275927922,122.));
#43218=CARTESIAN_POINT('Ctrl Pts',(-38.6478325658439,88.9558122233299,122.));
#43219=CARTESIAN_POINT('Ctrl Pts',(-38.6373536122841,88.9717652973009,122.));
#43220=CARTESIAN_POINT('Ctrl Pts',(-38.5901670347616,89.04360176049,122.));
#43221=CARTESIAN_POINT('Ctrl Pts',(-38.5394455308257,89.112844773472,122.));
#43222=CARTESIAN_POINT('Ctrl Pts',(-38.4852219917805,89.1791423373427,122.));
#43223=CARTESIAN_POINT('Ctrl Pts',(-38.4364255687668,89.2388043223104,122.));
#43224=CARTESIAN_POINT('Ctrl Pts',(-38.3847924489325,89.2960808804698,122.));
#43225=CARTESIAN_POINT('Ctrl Pts',(-38.3303261109488,89.3506856727381,122.));
#43226=CARTESIAN_POINT('Ctrl Pts',(-38.3112435400582,89.369816751823,122.));
#43227=CARTESIAN_POINT('Ctrl Pts',(-38.2918130242121,89.3886195826515,122.));
#43228=CARTESIAN_POINT('Ctrl Pts',(-38.272045138338,89.4070896778011,122.));
#43229=CARTESIAN_POINT('Origin',(-36.3549260746835,87.7685555885722,114.));
#43230=CARTESIAN_POINT('Origin',(36.3549260746835,-87.7685555885722,107.));
#43231=CARTESIAN_POINT('Ctrl Pts',(34.441460078019,-86.1325683851967,107.));
#43232=CARTESIAN_POINT('Ctrl Pts',(34.3793224918267,-86.1909624581861,107.));
#43233=CARTESIAN_POINT('Ctrl Pts',(34.320560277281,-86.2526104359851,107.));
#43234=CARTESIAN_POINT('Ctrl Pts',(34.2651854154857,-86.3171358435518,107.));
#43235=CARTESIAN_POINT('Ctrl Pts',(34.2084554811663,-86.383240245703,107.));
#43236=CARTESIAN_POINT('Ctrl Pts',(34.1552802428995,-86.4523651183919,107.));
#43237=CARTESIAN_POINT('Ctrl Pts',(34.1057014708844,-86.5241519419432,107.));
#43238=CARTESIAN_POINT('Ctrl Pts',(34.0927636287905,-86.5428850922367,107.));
#43239=CARTESIAN_POINT('Ctrl Pts',(34.080070868449,-86.5617997318037,107.));
#43240=CARTESIAN_POINT('Ctrl Pts',(34.0676243075757,-86.5808899227627,107.));
#43241=CARTESIAN_POINT('Ctrl Pts',(34.0574544824683,-86.5964881193486,107.));
#43242=CARTESIAN_POINT('Ctrl Pts',(34.0474485842597,-86.612204424695,107.));
#43243=CARTESIAN_POINT('Ctrl Pts',(34.0376160702623,-86.6280210049421,107.));
#43244=CARTESIAN_POINT('Ctrl Pts',(33.9901718947115,-86.7043396971966,107.));
#43245=CARTESIAN_POINT('Ctrl Pts',(33.9467112825774,-86.783065746378,107.));
#43246=CARTESIAN_POINT('Ctrl Pts',(33.9072689218163,-86.8638066024608,107.));
#43247=CARTESIAN_POINT('Ctrl Pts',(33.8754404287267,-86.9289614190155,107.));
#43248=CARTESIAN_POINT('Ctrl Pts',(33.8462290730293,-86.9954293421335,107.));
#43249=CARTESIAN_POINT('Ctrl Pts',(33.819670241093,-87.0630218995359,107.));
#43250=CARTESIAN_POINT('Ctrl Pts',(33.8090685977204,-87.0900032136971,107.));
#43251=CARTESIAN_POINT('Ctrl Pts',(33.7988897945031,-87.1171638805078,107.));
#43252=CARTESIAN_POINT('Ctrl Pts',(33.7891368427985,-87.1444924579589,107.));
#43253=CARTESIAN_POINT('Ctrl Pts',(33.7838959378683,-87.1591779071067,107.));
#43254=CARTESIAN_POINT('Ctrl Pts',(33.7787783829148,-87.1739110234873,107.));
#43255=CARTESIAN_POINT('Ctrl Pts',(33.7737886445088,-87.1886775541965,107.));
#43256=CARTESIAN_POINT('Ctrl Pts',(33.744249812514,-87.2760941749241,107.));
#43257=CARTESIAN_POINT('Ctrl Pts',(33.7191464479123,-87.3647918982878,107.));
#43258=CARTESIAN_POINT('Ctrl Pts',(33.6985111208832,-87.4543729160899,107.));
#43259=CARTESIAN_POINT('Ctrl Pts',(33.6775543388031,-87.5453494179855,107.));
#43260=CARTESIAN_POINT('Ctrl Pts',(33.6612053831337,-87.6372377538553,107.));
#43261=CARTESIAN_POINT('Ctrl Pts',(33.6495401950691,-87.729654418924,107.));
#43262=CARTESIAN_POINT('Ctrl Pts',(33.6379657251133,-87.821352375899,107.));
#43263=CARTESIAN_POINT('Ctrl Pts',(33.631002112185,-87.9135714065299,107.));
#43264=CARTESIAN_POINT('Ctrl Pts',(33.6287704839946,-88.0059560939408,107.));
#43265=CARTESIAN_POINT('Ctrl Pts',(33.6276598722209,-88.0519330725417,107.));
#43266=CARTESIAN_POINT('Ctrl Pts',(33.6277220148865,-88.0979512931867,107.));
#43267=CARTESIAN_POINT('Ctrl Pts',(33.6289766402602,-88.1439676459876,107.));
#43268=CARTESIAN_POINT('Ctrl Pts',(33.6293464212451,-88.1575302381508,107.));
#43269=CARTESIAN_POINT('Ctrl Pts',(33.6298198132723,-88.1710926687391,107.));
#43270=CARTESIAN_POINT('Ctrl Pts',(33.6303973778168,-88.1846538340193,107.));
#43271=CARTESIAN_POINT('Ctrl Pts',(33.6310178764361,-88.199223087642,107.));
#43272=CARTESIAN_POINT('Ctrl Pts',(33.6317582082676,-88.2137810937379,107.));
#43273=CARTESIAN_POINT('Ctrl Pts',(33.6326184218729,-88.2283239261021,107.));
#43274=CARTESIAN_POINT('Ctrl Pts',(33.6382702188031,-88.3238736067939,107.));
#43275=CARTESIAN_POINT('Ctrl Pts',(33.6490946590568,-88.4188015746807,107.));
#43276=CARTESIAN_POINT('Ctrl Pts',(33.6651621993108,-88.5127121877848,107.));
#43277=CARTESIAN_POINT('Ctrl Pts',(33.6675425111235,-88.5266244940976,107.));
#43278=CARTESIAN_POINT('Ctrl Pts',(33.6700379786409,-88.5405145062868,107.));
#43279=CARTESIAN_POINT('Ctrl Pts',(33.6726489234542,-88.5543809687066,107.));
#43280=CARTESIAN_POINT('Ctrl Pts',(33.6895945630855,-88.6443775377394,107.));
#43281=CARTESIAN_POINT('Ctrl Pts',(33.7114000884911,-88.733381941817,107.));
#43282=CARTESIAN_POINT('Ctrl Pts',(33.737762949146,-88.8211619318416,107.));
#43283=CARTESIAN_POINT('Ctrl Pts',(33.7647217588965,-88.9109262439152,107.));
#43284=CARTESIAN_POINT('Ctrl Pts',(33.7964464848098,-88.9994108591658,107.));
#43285=CARTESIAN_POINT('Ctrl Pts',(33.8326678325411,-89.086363731768,107.));
#43286=CARTESIAN_POINT('Ctrl Pts',(33.845157910542,-89.1163473803409,107.));
#43287=CARTESIAN_POINT('Ctrl Pts',(33.8581831105127,-89.1461488154908,107.));
#43288=CARTESIAN_POINT('Ctrl Pts',(33.8717337628504,-89.1757573633716,107.));
#43289=CARTESIAN_POINT('Ctrl Pts',(33.8784247684257,-89.1903773944972,107.));
#43290=CARTESIAN_POINT('Ctrl Pts',(33.8852438980845,-89.2049503931226,107.));
#43291=CARTESIAN_POINT('Ctrl Pts',(33.8921900469341,-89.219475051693,107.));
#43292=CARTESIAN_POINT('Ctrl Pts',(33.8976838231309,-89.2309627444056,107.));
#43293=CARTESIAN_POINT('Ctrl Pts',(33.9032566146494,-89.2424191739447,107.));
#43294=CARTESIAN_POINT('Ctrl Pts',(33.9089032804855,-89.253834763427,107.));
#43295=CARTESIAN_POINT('Ctrl Pts',(33.9516272055465,-89.3402076432341,107.));
#43296=CARTESIAN_POINT('Ctrl Pts',(33.9986419909546,-89.424382211309,107.));
#43297=CARTESIAN_POINT('Ctrl Pts',(34.0496049802514,-89.506108829215,107.));
#43298=CARTESIAN_POINT('Ctrl Pts',(34.1015786903742,-89.5894562860063,107.));
#43299=CARTESIAN_POINT('Ctrl Pts',(34.1576590761245,-89.6702585036094,107.));
#43300=CARTESIAN_POINT('Ctrl Pts',(34.2175376968044,-89.7482436651937,107.));
#43301=CARTESIAN_POINT('Ctrl Pts',(34.2779031585332,-89.8268628824301,107.));
#43302=CARTESIAN_POINT('Ctrl Pts',(34.342129327908,-89.9026198862294,107.));
#43303=CARTESIAN_POINT('Ctrl Pts',(34.4099495107696,-89.9752168962673,107.));
#43304=CARTESIAN_POINT('Ctrl Pts',(34.4469502263334,-90.0148237095471,107.));
#43305=CARTESIAN_POINT('Ctrl Pts',(34.4850215078373,-90.0534895501217,107.));
#43306=CARTESIAN_POINT('Ctrl Pts',(34.5241253959326,-90.0911622835395,107.));
#43307=CARTESIAN_POINT('Ctrl Pts',(34.536092533356,-90.1026914383087,107.));
#43308=CARTESIAN_POINT('Ctrl Pts',(34.5481564062128,-90.1141275592007,107.));
#43309=CARTESIAN_POINT('Ctrl Pts',(34.560315989506,-90.1254690898891,107.));
#43310=CARTESIAN_POINT('Ctrl Pts',(34.5708617769609,-90.1353053950623,107.));
#43311=CARTESIAN_POINT('Ctrl Pts',(34.5814784435051,-90.145069435766,107.));
#43312=CARTESIAN_POINT('Ctrl Pts',(34.5921562070644,-90.154752216978,107.));
#43313=CARTESIAN_POINT('Ctrl Pts',(34.6677306685615,-90.2232844495778,107.));
#43314=CARTESIAN_POINT('Ctrl Pts',(34.746481851648,-90.2878603390861,107.));
#43315=CARTESIAN_POINT('Ctrl Pts',(34.82808240795,-90.3481981124324,107.));
#43316=CARTESIAN_POINT('Ctrl Pts',(34.9097871680395,-90.4086129370245,107.));
#43317=CARTESIAN_POINT('Ctrl Pts',(34.9943491566684,-90.46477965297,107.));
#43318=CARTESIAN_POINT('Ctrl Pts',(35.0814850443532,-90.5163896064528,107.));
#43319=CARTESIAN_POINT('Ctrl Pts',(35.1668886983011,-90.5669735704729,107.));
#43320=CARTESIAN_POINT('Ctrl Pts',(35.2547655959762,-90.613180823026,107.));
#43321=CARTESIAN_POINT('Ctrl Pts',(35.3448830612224,-90.6546849506116,107.));
#43322=CARTESIAN_POINT('Ctrl Pts',(35.3852331814247,-90.6732684353156,107.));
#43323=CARTESIAN_POINT('Ctrl Pts',(35.4260328929523,-90.6909084910784,107.));
#43324=CARTESIAN_POINT('Ctrl Pts',(35.4672630634612,-90.7075728698848,107.));
#43325=CARTESIAN_POINT('Ctrl Pts',(35.4976827134229,-90.7198678607583,107.));
#43326=CARTESIAN_POINT('Ctrl Pts',(35.5283367073931,-90.7316316981734,107.));
#43327=CARTESIAN_POINT('Ctrl Pts',(35.5592127764326,-90.7428670628568,107.));
#43328=CARTESIAN_POINT('Ctrl Pts',(37.1487253572158,-90.7377785423181,107.));
#43329=CARTESIAN_POINT('Ctrl Pts',(37.2435592465647,-90.703087881974,107.));
#43330=CARTESIAN_POINT('Ctrl Pts',(37.3363499820799,-90.6634063347566,107.));
#43331=CARTESIAN_POINT('Ctrl Pts',(37.4268566408666,-90.6190542519878,107.));
#43332=CARTESIAN_POINT('Ctrl Pts',(37.5186361899685,-90.5740783992404,107.));
#43333=CARTESIAN_POINT('Ctrl Pts',(37.6080676322742,-90.5242990120235,107.));
#43334=CARTESIAN_POINT('Ctrl Pts',(37.6948657117722,-90.4700094660602,107.));
#43335=CARTESIAN_POINT('Ctrl Pts',(37.7193787255217,-90.4546773251379,107.));
#43336=CARTESIAN_POINT('Ctrl Pts',(37.7436814680841,-90.4389852541544,107.));
#43337=CARTESIAN_POINT('Ctrl Pts',(37.7677669178499,-90.4229394055795,107.));
#43338=CARTESIAN_POINT('Ctrl Pts',(37.7870964822202,-90.4100619519335,107.));
#43339=CARTESIAN_POINT('Ctrl Pts',(37.8062881985499,-90.3969550139071,107.));
#43340=CARTESIAN_POINT('Ctrl Pts',(37.8253191512513,-90.3836355366237,107.));
#43341=CARTESIAN_POINT('Ctrl Pts',(37.9080262499151,-90.3257500834303,107.));
#43342=CARTESIAN_POINT('Ctrl Pts',(37.9877784886294,-90.263802481533,107.));
#43343=CARTESIAN_POINT('Ctrl Pts',(38.0643095059346,-90.1980900928801,107.));
#43344=CARTESIAN_POINT('Ctrl Pts',(38.1233026941829,-90.1474363390095,107.));
#43345=CARTESIAN_POINT('Ctrl Pts',(38.1803812147524,-90.0945446577292,107.));
#43346=CARTESIAN_POINT('Ctrl Pts',(38.2354054997586,-90.0395394799401,107.));
#43347=CARTESIAN_POINT('Ctrl Pts',(38.2646942393973,-90.0102609108346,107.));
#43348=CARTESIAN_POINT('Ctrl Pts',(38.2934006760903,-89.9803833759801,107.));
#43349=CARTESIAN_POINT('Ctrl Pts',(38.3215017395818,-89.9499248098952,107.));
#43350=CARTESIAN_POINT('Ctrl Pts',(38.3311377428159,-89.9394804065583,107.));
#43351=CARTESIAN_POINT('Ctrl Pts',(38.3407018304141,-89.9289683913002,107.));
#43352=CARTESIAN_POINT('Ctrl Pts',(38.3501864357286,-89.9183970998547,107.));
#43353=CARTESIAN_POINT('Ctrl Pts',(38.4159836260407,-89.8450612833374,107.));
#43354=CARTESIAN_POINT('Ctrl Pts',(38.4780486658794,-89.7687788430213,107.));
#43355=CARTESIAN_POINT('Ctrl Pts',(38.5361377867705,-89.6898283382125,107.));
#43356=CARTESIAN_POINT('Ctrl Pts',(38.5937004502349,-89.6115933560172,107.));
#43357=CARTESIAN_POINT('Ctrl Pts',(38.6473593689752,-89.5307376665252,107.));
#43358=CARTESIAN_POINT('Ctrl Pts',(38.6968315991878,-89.4475099381577,107.));
#43359=CARTESIAN_POINT('Ctrl Pts',(38.7448895391944,-89.3666614872271,107.));
#43360=CARTESIAN_POINT('Ctrl Pts',(38.7889969518342,-89.2835739814083,107.));
#43361=CARTESIAN_POINT('Ctrl Pts',(38.8288466859154,-89.1984650429878,107.));
#43362=CARTESIAN_POINT('Ctrl Pts',(38.8496511020266,-89.1540320797447,107.));
#43363=CARTESIAN_POINT('Ctrl Pts',(38.8692942322878,-89.1090480478038,107.));
#43364=CARTESIAN_POINT('Ctrl Pts',(38.8877266765946,-89.0635436780106,107.));
#43365=CARTESIAN_POINT('Ctrl Pts',(38.8947847579787,-89.046119318008,107.));
#43366=CARTESIAN_POINT('Ctrl Pts',(38.9016652800419,-89.0286186647692,107.));
#43367=CARTESIAN_POINT('Ctrl Pts',(38.9083653072029,-89.0110434524178,107.));
#43368=CARTESIAN_POINT('Ctrl Pts',(38.9136070431997,-88.9972935643921,107.));
#43369=CARTESIAN_POINT('Ctrl Pts',(38.9187384030901,-88.9834975405313,107.));
#43370=CARTESIAN_POINT('Ctrl Pts',(38.9237528516952,-88.9696709241645,107.));
#43371=CARTESIAN_POINT('Ctrl Pts',(38.9554365396406,-88.8823077397353,107.));
#43372=CARTESIAN_POINT('Ctrl Pts',(38.9825114019973,-88.7935836147519,107.));
#43373=CARTESIAN_POINT('Ctrl Pts',(39.0047261827264,-88.7037221014846,107.));
#43374=CARTESIAN_POINT('Ctrl Pts',(39.0097101548453,-88.6835613228504,107.));
#43375=CARTESIAN_POINT('Ctrl Pts',(39.0144492932001,-88.6633432545392,107.));
#43376=CARTESIAN_POINT('Ctrl Pts',(39.0189403996523,-88.6430703655259,107.));
#43377=CARTESIAN_POINT('Ctrl Pts',(39.0393061529012,-88.5511391989667,107.));
#43378=CARTESIAN_POINT('Ctrl Pts',(39.054575694401,-88.4580804162001,107.));
#43379=CARTESIAN_POINT('Ctrl Pts',(39.0648588490549,-88.3642856036222,107.));
#43380=CARTESIAN_POINT('Ctrl Pts',(39.0755927118845,-88.2663797871473,107.));
#43381=CARTESIAN_POINT('Ctrl Pts',(39.0808934919427,-88.1676707693011,107.));
#43382=CARTESIAN_POINT('Ctrl Pts',(39.0808286362865,-88.0686185665232,107.));
#43383=CARTESIAN_POINT('Ctrl Pts',(39.0808032678039,-88.0298740031761,107.));
#43384=CARTESIAN_POINT('Ctrl Pts',(39.0799563544502,-87.9910771891197,107.));
#43385=CARTESIAN_POINT('Ctrl Pts',(39.0782897088242,-87.9522568820768,107.));
#43386=CARTESIAN_POINT('Ctrl Pts',(39.0777566699434,-87.9398410855225,107.));
#43387=CARTESIAN_POINT('Ctrl Pts',(39.0771397845791,-87.9274241972147,107.));
#43388=CARTESIAN_POINT('Ctrl Pts',(39.0764398138567,-87.9150168265058,107.));
#43389=CARTESIAN_POINT('Ctrl Pts',(39.0712006005755,-87.822148854568,107.));
#43390=CARTESIAN_POINT('Ctrl Pts',(39.0613049669259,-87.7296641169378,107.));
#43391=CARTESIAN_POINT('Ctrl Pts',(39.0468763718403,-87.6379341904711,107.));
#43392=CARTESIAN_POINT('Ctrl Pts',(39.0324817650919,-87.5464203451715,107.));
#43393=CARTESIAN_POINT('Ctrl Pts',(39.0135751177459,-87.4556568137981,107.));
#43394=CARTESIAN_POINT('Ctrl Pts',(38.9902303422857,-87.3660295059385,107.));
#43395=CARTESIAN_POINT('Ctrl Pts',(38.9672817156295,-87.2779231272848,107.));
#43396=CARTESIAN_POINT('Ctrl Pts',(38.9400438408593,-87.190913951763,107.));
#43397=CARTESIAN_POINT('Ctrl Pts',(38.9085464901449,-87.1053976716856,107.));
#43398=CARTESIAN_POINT('Ctrl Pts',(38.8927050482775,-87.0623876677065,107.));
#43399=CARTESIAN_POINT('Ctrl Pts',(38.8757855564829,-87.0197558321219,107.));
#43400=CARTESIAN_POINT('Ctrl Pts',(38.8577883849998,-86.9775562961909,107.));
#43401=CARTESIAN_POINT('Ctrl Pts',(38.8522226745452,-86.9645058899906,107.));
#43402=CARTESIAN_POINT('Ctrl Pts',(38.8465538809276,-86.9514968490023,107.));
#43403=CARTESIAN_POINT('Ctrl Pts',(38.8407819742204,-86.9385308318502,107.));
#43404=CARTESIAN_POINT('Ctrl Pts',(38.8351025159904,-86.9257724910523,107.));
#43405=CARTESIAN_POINT('Ctrl Pts',(38.8293267026267,-86.9130636714118,107.));
#43406=CARTESIAN_POINT('Ctrl Pts',(38.8234563238127,-86.9004088584368,107.));
#43407=CARTESIAN_POINT('Ctrl Pts',(38.7859765239624,-86.8196134153368,107.));
#43408=CARTESIAN_POINT('Ctrl Pts',(38.7446265669885,-86.7409747507621,107.));
#43409=CARTESIAN_POINT('Ctrl Pts',(38.6994761290357,-86.6648404554994,107.));
#43410=CARTESIAN_POINT('Ctrl Pts',(38.6550831229752,-86.5899833691838,107.));
#43411=CARTESIAN_POINT('Ctrl Pts',(38.6070156240331,-86.5175466622143,107.));
#43412=CARTESIAN_POINT('Ctrl Pts',(38.5553036472175,-86.4478949012765,107.));
#43413=CARTESIAN_POINT('Ctrl Pts',(38.5051691862912,-86.380367923926,107.));
#43414=CARTESIAN_POINT('Ctrl Pts',(38.4516087686083,-86.3154581290589,107.));
#43415=CARTESIAN_POINT('Ctrl Pts',(38.3946220345055,-86.2535380111354,107.));
#43416=CARTESIAN_POINT('Ctrl Pts',(38.373654460502,-86.2307552587053,107.));
#43417=CARTESIAN_POINT('Ctrl Pts',(38.3522227934278,-86.2083776778821,107.));
#43418=CARTESIAN_POINT('Ctrl Pts',(38.3303262041782,-86.1864254330304,107.));
#43419=CARTESIAN_POINT('Ctrl Pts',(38.311248768753,-86.1672995075806,107.));
#43420=CARTESIAN_POINT('Ctrl Pts',(38.2918183998859,-86.1484964687257,107.));
#43421=CARTESIAN_POINT('Ctrl Pts',(38.2720452344324,-86.1300214449938,107.));
#43422=CARTESIAN_POINT('Origin',(36.3549260746835,-87.7685555885722,124.208423447177));
#43423=CARTESIAN_POINT('Ctrl Pts',(33.2781264274053,-87.766627982914,121.708423447177));
#43424=CARTESIAN_POINT('Ctrl Pts',(33.2772037481594,-87.6433530720069,121.702019850418));
#43425=CARTESIAN_POINT('Ctrl Pts',(33.3397302338269,-86.5074461871871,121.642966745928));
#43426=CARTESIAN_POINT('Ctrl Pts',(34.7524572651294,-84.5150170630276,121.531264133707));
#43427=CARTESIAN_POINT('Ctrl Pts',(38.2031235339731,-84.6483923074236,121.373315610515));
#43428=CARTESIAN_POINT('Ctrl Pts',(39.9780136468089,-87.6103338294361,121.215367087322));
#43429=CARTESIAN_POINT('Ctrl Pts',(38.4679953249988,-90.71592025761,121.05741856413));
#43430=CARTESIAN_POINT('Ctrl Pts',(35.0421044228056,-91.1491283755177,120.899470040937));
#43431=CARTESIAN_POINT('Ctrl Pts',(33.3955573955644,-89.2107570630753,120.783138335287));
#43432=CARTESIAN_POINT('Ctrl Pts',(33.2786797629631,-87.9841152617576,120.719456137367));
#43433=CARTESIAN_POINT('Ctrl Pts',(33.2806115932904,-87.7712393060438,120.708423447177));
#43434=CARTESIAN_POINT('Ctrl Pts',(33.2846473629325,-87.7715718261144,121.791576552823));
#43435=CARTESIAN_POINT('Ctrl Pts',(33.2896323807993,-87.078553038224,121.755752019753));
#43436=CARTESIAN_POINT('Ctrl Pts',(33.862020072503,-85.3573618548392,121.667277978953));
#43437=CARTESIAN_POINT('Ctrl Pts',(36.7064604149176,-84.1596949927803,121.526154430422));
#43438=CARTESIAN_POINT('Ctrl Pts',(39.5688528980205,-86.0888159753533,121.36820590723));
#43439=CARTESIAN_POINT('Ctrl Pts',(39.5184626244884,-89.5420982077003,121.210257384038));
#43440=CARTESIAN_POINT('Ctrl Pts',(36.5992128626851,-91.3867833270583,121.052308860845));
#43441=CARTESIAN_POINT('Ctrl Pts',(33.8243658940394,-90.1183413579956,120.912748583774));
#43442=CARTESIAN_POINT('Ctrl Pts',(33.2888361264505,-88.4296039786679,120.825837814433));
#43443=CARTESIAN_POINT('Ctrl Pts',(33.2844849022013,-87.7664047084671,120.791576552823));
#43444=CARTESIAN_POINT('Ctrl Pts',(38.2683920713486,-86.1325683851972,122.));
#43445=CARTESIAN_POINT('Ctrl Pts',(38.8095874576702,-86.7655555914187,121.947350492269));
#43446=CARTESIAN_POINT('Ctrl Pts',(39.2049251670254,-88.6005879544937,121.842051476808));
#43447=CARTESIAN_POINT('Ctrl Pts',(37.2141270656728,-90.6137552465961,121.684102953615));
#43448=CARTESIAN_POINT('Ctrl Pts',(34.4432237898319,-90.0415108461503,121.526154430423));
#43449=CARTESIAN_POINT('Ctrl Pts',(33.4061068154979,-87.4112439256985,121.36820590723));
#43450=CARTESIAN_POINT('Ctrl Pts',(35.0423458801,-85.1035862578228,121.210257384038));
#43451=CARTESIAN_POINT('Ctrl Pts',(37.868782298455,-85.2128337534358,121.052308860845));
#43452=CARTESIAN_POINT('Ctrl Pts',(39.3225925665741,-87.6389563438593,120.894360337653));
#43453=CARTESIAN_POINT('Ctrl Pts',(38.0857384506941,-90.1827382969836,120.73641181446));
#43454=CARTESIAN_POINT('Ctrl Pts',(35.2795955041279,-90.5375785237065,120.578463291268));
#43455=CARTESIAN_POINT('Ctrl Pts',(33.448428834545,-88.3818666722405,120.420514768075));
#43456=CARTESIAN_POINT('Ctrl Pts',(34.2524915318856,-85.670066420957,120.262566244883));
#43457=CARTESIAN_POINT('Ctrl Pts',(36.96276928306,-84.8609111752806,120.10461772169));
#43458=CARTESIAN_POINT('Ctrl Pts',(39.1219333076541,-86.6880244570525,119.946669198498));
#43459=CARTESIAN_POINT('Ctrl Pts',(38.7723364062652,-89.4948245096349,119.788720675306));
#43460=CARTESIAN_POINT('Ctrl Pts',(36.2309468959301,-90.7364680335706,119.630772152113));
#43461=CARTESIAN_POINT('Ctrl Pts',(33.8019656255414,-89.2871960948262,119.472823628921));
#43462=CARTESIAN_POINT('Ctrl Pts',(33.6876759062241,-86.4610187600149,119.314875105728));
#43463=CARTESIAN_POINT('Ctrl Pts',(35.9917008149959,-84.8203454156677,119.156926582536));
#43464=CARTESIAN_POINT('Ctrl Pts',(38.6250510094734,-85.8527245134451,118.998978059343));
#43465=CARTESIAN_POINT('Ctrl Pts',(39.2001479732925,-88.622129406846,118.841029536151));
#43466=CARTESIAN_POINT('Ctrl Pts',(37.1955687727307,-90.6176248662799,118.683081012958));
#43467=CARTESIAN_POINT('Ctrl Pts',(34.4288044060203,-90.0299558685653,118.525132489766));
#43468=CARTESIAN_POINT('Ctrl Pts',(33.4083959753712,-87.3919440112382,118.367183966573));
#43469=CARTESIAN_POINT('Ctrl Pts',(35.0595167713852,-85.095394418475,118.209235443381));
#43470=CARTESIAN_POINT('Ctrl Pts',(37.8851457844713,-85.2225187573788,118.051286920188));
#43471=CARTESIAN_POINT('Ctrl Pts',(39.3233711262874,-87.6580572572747,117.893338396996));
#43472=CARTESIAN_POINT('Ctrl Pts',(38.0701976209574,-90.1937812333288,117.735389873803));
#43473=CARTESIAN_POINT('Ctrl Pts',(35.2618395722624,-90.5306268772706,117.577441350611));
#43474=CARTESIAN_POINT('Ctrl Pts',(33.4445498105818,-88.3631864883094,117.419492827419));
#43475=CARTESIAN_POINT('Ctrl Pts',(34.2660096924731,-85.6566123474577,117.261544304226));
#43476=CARTESIAN_POINT('Ctrl Pts',(36.9814265265929,-84.8648729114648,117.103595781034));
#43477=CARTESIAN_POINT('Ctrl Pts',(39.1288144551173,-86.7058142472931,116.945647257841));
#43478=CARTESIAN_POINT('Ctrl Pts',(38.7612021531035,-89.5103108354403,116.787698734649));
#43479=CARTESIAN_POINT('Ctrl Pts',(36.2118925143652,-90.7356109143443,116.629750211456));
#43480=CARTESIAN_POINT('Ctrl Pts',(33.7922670545985,-89.2707721682791,116.471801688264));
#43481=CARTESIAN_POINT('Ctrl Pts',(33.6961265885919,-86.4439193372456,116.313853165071));
#43482=CARTESIAN_POINT('Ctrl Pts',(36.0106387528937,-84.8180739082996,116.155904641879));
#43483=CARTESIAN_POINT('Ctrl Pts',(38.6373057608367,-85.8673404840128,115.997956118686));
#43484=CARTESIAN_POINT('Ctrl Pts',(39.194608522785,-88.6403809721864,115.840007595494));
#43485=CARTESIAN_POINT('Ctrl Pts',(37.1772575740773,-90.6229639004075,115.682059072301));
#43486=CARTESIAN_POINT('Ctrl Pts',(34.4143236649513,-90.0175416251921,115.524110549109));
#43487=CARTESIAN_POINT('Ctrl Pts',(33.4108749399752,-87.3730321103917,115.366162025916));
#43488=CARTESIAN_POINT('Ctrl Pts',(35.0767078395714,-85.0871317039549,115.208213502724));
#43489=CARTESIAN_POINT('Ctrl Pts',(37.9014623376935,-85.2323967818796,115.050264979531));
#43490=CARTESIAN_POINT('Ctrl Pts',(39.3240194419186,-87.6771199160491,114.892316456339));
#43491=CARTESIAN_POINT('Ctrl Pts',(38.0545898909647,-90.2047449936051,114.734367933147));
#43492=CARTESIAN_POINT('Ctrl Pts',(35.2441268507267,-90.5235512309691,114.576419409954));
#43493=CARTESIAN_POINT('Ctrl Pts',(33.4407916834193,-88.3444867087769,114.418470886762));
#43494=CARTESIAN_POINT('Ctrl Pts',(34.27961353928,-85.6432429560481,114.260522363569));
#43495=CARTESIAN_POINT('Ctrl Pts',(37.0000581532135,-84.8689555287672,114.102573840377));
#43496=CARTESIAN_POINT('Ctrl Pts',(39.1355811323492,-86.7236472883622,113.944625317184));
#43497=CARTESIAN_POINT('Ctrl Pts',(38.7499687405001,-89.525725624308,113.786676793992));
#43498=CARTESIAN_POINT('Ctrl Pts',(36.1928440054851,-90.7346313307632,113.628728270799));
#43499=CARTESIAN_POINT('Ctrl Pts',(33.782674153109,-89.2542863708898,113.470779747607));
#43500=CARTESIAN_POINT('Ctrl Pts',(33.7046868865187,-86.426874497148,113.312831224414));
#43501=CARTESIAN_POINT('Ctrl Pts',(36.0295908884562,-84.815924063615,113.154882701222));
#43502=CARTESIAN_POINT('Ctrl Pts',(38.6494664091236,-85.882034833532,112.996934178029));
#43503=CARTESIAN_POINT('Ctrl Pts',(39.1889519938438,-88.658596596109,112.838985654837));
#43504=CARTESIAN_POINT('Ctrl Pts',(37.1589124706636,-90.6281852465259,112.681037131644));
#43505=CARTESIAN_POINT('Ctrl Pts',(34.3999229343891,-90.005034657781,112.523088608452));
#43506=CARTESIAN_POINT('Ctrl Pts',(33.4134752866869,-87.3541365164204,112.365140085259));
#43507=CARTESIAN_POINT('Ctrl Pts',(35.0939516082793,-85.0789795437939,112.207191562067));
#43508=CARTESIAN_POINT('Ctrl Pts',(37.9177151277559,-85.2423793712098,112.049243038874));
#43509=CARTESIAN_POINT('Ctrl Pts',(39.3245453428919,-87.6961863447321,111.891294515682));
#43510=CARTESIAN_POINT('Ctrl Pts',(38.0389120844315,-90.2156083106323,111.733345992489));
#43511=CARTESIAN_POINT('Ctrl Pts',(35.2264599270504,-90.5163619971867,111.575397469297));
#43512=CARTESIAN_POINT('Ctrl Pts',(33.4371537049852,-88.325763183801,111.417448946105));
#43513=CARTESIAN_POINT('Ctrl Pts',(34.2933029504833,-85.6299611905315,111.259500422912));
#43514=CARTESIAN_POINT('Ctrl Pts',(37.0186631812752,-84.8731576955424,111.10155189972));
#43515=CARTESIAN_POINT('Ctrl Pts',(39.1422331641425,-86.7415234106471,110.943603376527));
#43516=CARTESIAN_POINT('Ctrl Pts',(38.7386365811713,-89.5410679656435,110.785654853335));
#43517=CARTESIAN_POINT('Ctrl Pts',(36.1738021791204,-90.7335294570022,110.627706330142));
#43518=CARTESIAN_POINT('Ctrl Pts',(33.7731873047999,-89.2377393172008,110.46975780695));
#43519=CARTESIAN_POINT('Ctrl Pts',(33.7133564525678,-86.4098849743869,110.311809283757));
#43520=CARTESIAN_POINT('Ctrl Pts',(36.0485564380895,-84.8138959542623,110.153860760565));
#43521=CARTESIAN_POINT('Ctrl Pts',(38.6615324530581,-85.8968069649053,109.995912237372));
#43522=CARTESIAN_POINT('Ctrl Pts',(39.1831786216268,-88.6767755213396,109.83796371418));
#43523=CARTESIAN_POINT('Ctrl Pts',(37.1405342138127,-90.6332886965093,109.680015190987));
#43524=CARTESIAN_POINT('Ctrl Pts',(34.3856028189437,-89.9924354700622,109.522066667795));
#43525=CARTESIAN_POINT('Ctrl Pts',(33.4161968856849,-87.3352580315655,109.364118144603));
#43526=CARTESIAN_POINT('Ctrl Pts',(35.1112474131768,-85.0709382270786,109.20616962141));
#43527=CARTESIAN_POINT('Ctrl Pts',(37.9339033886155,-85.2524662101859,109.048221098218));
#43528=CARTESIAN_POINT('Ctrl Pts',(39.3249490048854,-87.7152555591209,108.890272575025));
#43529=CARTESIAN_POINT('Ctrl Pts',(38.0231644418222,-90.2263711438778,108.732324051833));
#43530=CARTESIAN_POINT('Ctrl Pts',(35.2088403645094,-90.5090586345567,108.57437552864));
#43531=CARTESIAN_POINT('Ctrl Pts',(33.4336343081817,-88.3070184083814,108.416427005448));
#43532=CARTESIAN_POINT('Ctrl Pts',(34.3070808932133,-85.6167640547538,108.258478482255));
#43533=CARTESIAN_POINT('Ctrl Pts',(37.0372335803832,-84.8774865269729,108.100529959063));
#43534=CARTESIAN_POINT('Ctrl Pts',(39.1487852146927,-86.7594268870025,107.94258143587));
#43535=CARTESIAN_POINT('Ctrl Pts',(38.7271754184244,-89.5563680570491,107.784632912678));
#43536=CARTESIAN_POINT('Ctrl Pts',(36.1548310102042,-90.7322419299408,107.626684389485));
#43537=CARTESIAN_POINT('Ctrl Pts',(33.7636769376747,-89.2212621009139,107.468735866293));
#43538=CARTESIAN_POINT('Ctrl Pts',(33.7224022240811,-86.3926832021283,107.3107873431));
#43539=CARTESIAN_POINT('Ctrl Pts',(36.0669846992798,-84.812541212222,107.152838819908));
#43540=CARTESIAN_POINT('Ctrl Pts',(38.6746344652086,-85.9105081134349,106.994890296715));
#43541=CARTESIAN_POINT('Ctrl Pts',(39.1749135435619,-88.6972338749877,106.836941773523));
#43542=CARTESIAN_POINT('Ctrl Pts',(37.8096764711453,-89.9855519312418,106.731642758061));
#43543=CARTESIAN_POINT('Ctrl Pts',(37.0051260726582,-90.2006423906074,106.678993250331));
#43544=CARTESIAN_POINT('Ctrl Pts',(38.4092576250256,-86.0121302673453,122.10700224989));
#43545=CARTESIAN_POINT('Ctrl Pts',(38.9902947372386,-86.6917167303241,122.054352742159));
#43546=CARTESIAN_POINT('Ctrl Pts',(39.4147364209601,-88.6618405192673,121.949053726697));
#43547=CARTESIAN_POINT('Ctrl Pts',(37.2773797304845,-90.8232131757403,121.791105203505));
#43548=CARTESIAN_POINT('Ctrl Pts',(34.302488077104,-90.2088412828551,121.633156680312));
#43549=CARTESIAN_POINT('Ctrl Pts',(33.1890206178008,-87.3849393530991,121.47520815712));
#43550=CARTESIAN_POINT('Ctrl Pts',(34.9457163417765,-84.9073965262243,121.317259633928));
#43551=CARTESIAN_POINT('Ctrl Pts',(37.980229376961,-85.0246866047652,121.159311110735));
#43552=CARTESIAN_POINT('Ctrl Pts',(39.5410662599857,-87.6294155057182,121.001362587543));
#43553=CARTESIAN_POINT('Ctrl Pts',(38.2131574087957,-90.3604656171925,120.84341406435));
#43554=CARTESIAN_POINT('Ctrl Pts',(35.2004318103538,-90.7414284743101,120.685465541158));
#43555=CARTESIAN_POINT('Ctrl Pts',(33.2344582995543,-88.4270174120644,120.527517017965));
#43556=CARTESIAN_POINT('Ctrl Pts',(34.0977144904032,-85.5155798301335,120.369568494773));
#43557=CARTESIAN_POINT('Ctrl Pts',(37.0075174888008,-84.6468561876885,120.21161997158));
#43558=CARTESIAN_POINT('Ctrl Pts',(39.3256348662813,-86.6084779083434,120.053671448388));
#43559=CARTESIAN_POINT('Ctrl Pts',(38.9503013376599,-89.6219089876371,119.895722925195));
#43560=CARTESIAN_POINT('Ctrl Pts',(36.2218197958458,-90.9549598335599,119.737774402003));
#43561=CARTESIAN_POINT('Ctrl Pts',(33.6140217646049,-89.3989953826749,119.57982587881));
#43562=CARTESIAN_POINT('Ctrl Pts',(33.4913182638986,-86.3647605042483,119.421877355618));
#43563=CARTESIAN_POINT('Ctrl Pts',(35.9649608951831,-84.6033040576888,119.263928832425));
#43564=CARTESIAN_POINT('Ctrl Pts',(38.7921730834546,-85.7116848474046,119.105980309233));
#43565=CARTESIAN_POINT('Ctrl Pts',(39.4096075397443,-88.6849678104158,118.948031786041));
#43566=CARTESIAN_POINT('Ctrl Pts',(37.2574552129974,-90.8273676691141,118.790083262848));
#43567=CARTESIAN_POINT('Ctrl Pts',(34.28700716699,-90.1964356508463,118.632134739656));
#43568=CARTESIAN_POINT('Ctrl Pts',(33.1914783010623,-87.3642186173953,118.474186216463));
#43569=CARTESIAN_POINT('Ctrl Pts',(34.9641513198614,-84.8986016199879,118.316237693271));
#43570=CARTESIAN_POINT('Ctrl Pts',(37.9977975102101,-85.0350845993988,118.158289170078));
#43571=CARTESIAN_POINT('Ctrl Pts',(39.5419021357137,-87.6499225903166,118.000340646886));
#43572=CARTESIAN_POINT('Ctrl Pts',(38.1964724941422,-90.3723215125058,117.842392123693));
#43573=CARTESIAN_POINT('Ctrl Pts',(35.1813687221669,-90.7339650615165,117.684443600501));
#43574=CARTESIAN_POINT('Ctrl Pts',(33.2302937095768,-88.4069620302165,117.526495077308));
#43575=CARTESIAN_POINT('Ctrl Pts',(34.1122278310353,-85.5011352945534,117.368546554116));
#43576=CARTESIAN_POINT('Ctrl Pts',(37.027548241424,-84.6511095789959,117.210598030923));
#43577=CARTESIAN_POINT('Ctrl Pts',(39.3330225901084,-86.6275773474915,117.052649507731));
#43578=CARTESIAN_POINT('Ctrl Pts',(38.938347402968,-89.6385353858884,116.894700984538));
#43579=CARTESIAN_POINT('Ctrl Pts',(36.20136266868,-90.9540396149241,116.736752461346));
#43580=CARTESIAN_POINT('Ctrl Pts',(33.6036092041957,-89.3813623593836,116.578803938154));
#43581=CARTESIAN_POINT('Ctrl Pts',(33.5003910686625,-86.3464022560491,116.420855414961));
#43582=CARTESIAN_POINT('Ctrl Pts',(35.9852930063309,-84.6008653264748,116.262906891769));
#43583=CARTESIAN_POINT('Ctrl Pts',(38.805330005193,-85.7273768166001,116.104958368576));
#43584=CARTESIAN_POINT('Ctrl Pts',(39.4036602859289,-88.7045630196262,115.947009845384));
#43585=CARTESIAN_POINT('Ctrl Pts',(37.2377959803882,-90.8330997522951,115.789061322191));
#43586=CARTESIAN_POINT('Ctrl Pts',(34.2714603826195,-90.1831074956138,115.631112798999));
#43587=CARTESIAN_POINT('Ctrl Pts',(33.1941397621006,-87.3439144600947,115.473164275806));
#43588=CARTESIAN_POINT('Ctrl Pts',(34.9826079602305,-84.8897306208901,115.315215752614));
#43589=CARTESIAN_POINT('Ctrl Pts',(38.0153152555662,-85.0456898243793,115.157267229421));
#43590=CARTESIAN_POINT('Ctrl Pts',(39.5425981790498,-87.6703886040434,114.999318706229));
#43591=CARTESIAN_POINT('Ctrl Pts',(38.1797157541692,-90.3840924029661,114.841370183036));
#43592=CARTESIAN_POINT('Ctrl Pts',(35.1623520253682,-90.7263685202339,114.683421659844));
#43593=CARTESIAN_POINT('Ctrl Pts',(33.2262589165814,-88.3868856101783,114.525473136651));
#43594=CARTESIAN_POINT('Ctrl Pts',(34.1268331659355,-85.4867816751897,114.367524613459));
#43595=CARTESIAN_POINT('Ctrl Pts',(37.0475514912688,-84.6554927504486,114.209576090266));
#43596=CARTESIAN_POINT('Ctrl Pts',(39.3402874166341,-86.6467232215078,114.051627567074));
#43597=CARTESIAN_POINT('Ctrl Pts',(38.9262870089137,-89.6550849807952,113.893679043881));
#43598=CARTESIAN_POINT('Ctrl Pts',(36.1809118465345,-90.9529879163518,113.735730520689));
#43599=CARTESIAN_POINT('Ctrl Pts',(33.5933100924145,-89.3636629104421,113.577781997497));
#43600=CARTESIAN_POINT('Ctrl Pts',(33.5095815586644,-86.3281026087889,113.419833474304));
#43601=CARTESIAN_POINT('Ctrl Pts',(36.0056403603473,-84.5985572145086,113.261884951112));
#43602=CARTESIAN_POINT('Ctrl Pts',(38.818385896174,-85.7431529348491,113.103936427919));
#43603=CARTESIAN_POINT('Ctrl Pts',(39.397587334599,-88.7241196414834,112.945987904727));
#43604=CARTESIAN_POINT('Ctrl Pts',(37.2181003470178,-90.83870548351,112.788039381534));
#43605=CARTESIAN_POINT('Ctrl Pts',(34.2559994989699,-90.1696797901849,112.630090858342));
#43606=CARTESIAN_POINT('Ctrl Pts',(33.1969315411555,-87.3236278101488,112.472142335149));
#43607=CARTESIAN_POINT('Ctrl Pts',(35.0011211808287,-84.8809783149429,112.314193811957));
#43608=CARTESIAN_POINT('Ctrl Pts',(38.0327645436458,-85.0564073120434,112.156245288764));
#43609=CARTESIAN_POINT('Ctrl Pts',(39.5431627958047,-87.6908586652121,111.998296765572));
#43610=CARTESIAN_POINT('Ctrl Pts',(38.1628837787605,-90.3957554557452,111.840348242379));
#43611=CARTESIAN_POINT('Ctrl Pts',(35.143384497976,-90.7186500293867,111.682399719187));
#43612=CARTESIAN_POINT('Ctrl Pts',(33.2223531174244,-88.3667836966043,111.524451195994));
#43613=CARTESIAN_POINT('Ctrl Pts',(34.1415303643124,-85.4725221325625,111.366502672802));
#43614=CARTESIAN_POINT('Ctrl Pts',(37.0675261844218,-84.6600042723681,111.208554149609));
#43615=CARTESIAN_POINT('Ctrl Pts',(39.3474291577524,-86.6659153482933,111.050605626417));
#43616=CARTESIAN_POINT('Ctrl Pts',(38.914120598597,-89.6715567947269,110.892657103225));
#43617=CARTESIAN_POINT('Ctrl Pts',(36.1604681988578,-90.9518049248403,110.734708580032));
#43618=CARTESIAN_POINT('Ctrl Pts',(33.5831248412375,-89.3458976956341,110.57676005684));
#43619=CARTESIAN_POINT('Ctrl Pts',(33.51888936089,-86.3098623512175,110.418811533647));
#43620=CARTESIAN_POINT('Ctrl Pts',(36.0260021159516,-84.5963797997868,110.260863010455));
#43621=CARTESIAN_POINT('Ctrl Pts',(38.8313402182188,-85.7590125610974,110.102914487262));
#43622=CARTESIAN_POINT('Ctrl Pts',(39.391388938224,-88.743636862964,109.94496596407));
#43623=CARTESIAN_POINT('Ctrl Pts',(37.1983691195202,-90.8441846393115,109.787017440877));
#43624=CARTESIAN_POINT('Ctrl Pts',(34.2406251651613,-90.1561530753728,109.629068917685));
#43625=CARTESIAN_POINT('Ctrl Pts',(33.1998534988484,-87.3033595288585,109.471120394492));
#43626=CARTESIAN_POINT('Ctrl Pts',(35.0196902684171,-84.8723450125151,109.3131718713));
#43627=CARTESIAN_POINT('Ctrl Pts',(38.0501445520112,-85.0672367240047,109.155223348108));
#43628=CARTESIAN_POINT('Ctrl Pts',(39.5435961745898,-87.7113317171647,108.997274824915));
#43629=CARTESIAN_POINT('Ctrl Pts',(38.1459768260829,-90.4073106273269,108.839326301723));
#43630=CARTESIAN_POINT('Ctrl Pts',(35.1244678183516,-90.7108090077533,108.68137777853));
#43631=CARTESIAN_POINT('Ctrl Pts',(33.2185746296415,-88.3466589681714,108.523429255338));
#43632=CARTESIAN_POINT('Ctrl Pts',(34.1563226117307,-85.458353449947,108.365480732145));
#43633=CARTESIAN_POINT('Ctrl Pts',(37.0874636993066,-84.6646517837423,108.207532208953));
#43634=CARTESIAN_POINT('Ctrl Pts',(39.3544635572078,-86.6851368429016,108.04958368576));
#43635=CARTESIAN_POINT('Ctrl Pts',(38.9018156878874,-89.6879832483728,107.891635162568));
#43636=CARTESIAN_POINT('Ctrl Pts',(36.1401004102902,-90.9504226126024,107.733686639375));
#43637=CARTESIAN_POINT('Ctrl Pts',(33.572914339836,-89.3282074595185,107.575738116183));
#43638=CARTESIAN_POINT('Ctrl Pts',(33.5286010640765,-86.2913942187635,107.41778959299));
#43639=CARTESIAN_POINT('Ctrl Pts',(36.0457870290084,-84.5949253243372,107.259841069798));
#43640=CARTESIAN_POINT('Ctrl Pts',(38.8454067743952,-85.7737223608792,107.101892546605));
#43641=CARTESIAN_POINT('Ctrl Pts',(39.3825154015819,-88.76560131984,106.943944023413));
#43642=CARTESIAN_POINT('Ctrl Pts',(37.916772296426,-90.1487627841414,106.838645007951));
#43643=CARTESIAN_POINT('Ctrl Pts',(37.052992500844,-90.379687774511,106.78599550022));
#43644=CARTESIAN_POINT('Ctrl Pts',(38.5501231787026,-85.8916921494934,122.21400449978));
#43645=CARTESIAN_POINT('Ctrl Pts',(39.1710020168071,-86.6178778692294,122.161354992049));
#43646=CARTESIAN_POINT('Ctrl Pts',(39.6245476748949,-88.7230930840409,122.056055976587));
#43647=CARTESIAN_POINT('Ctrl Pts',(37.3406323952962,-91.0326711048844,121.898107453395));
#43648=CARTESIAN_POINT('Ctrl Pts',(34.1617523643761,-90.37617171956,121.740158930202));
#43649=CARTESIAN_POINT('Ctrl Pts',(32.9719344201038,-87.3586347804996,121.58221040701));
#43650=CARTESIAN_POINT('Ctrl Pts',(34.8490868034529,-84.7112067946259,121.424261883817));
#43651=CARTESIAN_POINT('Ctrl Pts',(38.0916764554671,-84.8365394560944,121.266313360625));
#43652=CARTESIAN_POINT('Ctrl Pts',(39.7595399533973,-87.6198746675772,121.108364837432));
#43653=CARTESIAN_POINT('Ctrl Pts',(38.3405763668972,-90.5381929374012,120.95041631424));
#43654=CARTESIAN_POINT('Ctrl Pts',(35.1212681165797,-90.9452784249139,120.792467791047));
#43655=CARTESIAN_POINT('Ctrl Pts',(33.0204877645637,-88.4721681518882,120.634519267855));
#43656=CARTESIAN_POINT('Ctrl Pts',(33.9429374489209,-85.3610932393102,120.476570744662));
#43657=CARTESIAN_POINT('Ctrl Pts',(37.0522656945416,-84.4328012000962,120.31862222147));
#43658=CARTESIAN_POINT('Ctrl Pts',(39.5293364249085,-86.5289313596344,120.160673698277));
#43659=CARTESIAN_POINT('Ctrl Pts',(39.1282662690547,-89.7489934656392,120.002725175085));
#43660=CARTESIAN_POINT('Ctrl Pts',(36.2126926957615,-91.1734516335492,119.844776651893));
#43661=CARTESIAN_POINT('Ctrl Pts',(33.4260779036684,-89.5107946705236,119.6868281287));
#43662=CARTESIAN_POINT('Ctrl Pts',(33.2949606215731,-86.2685022484816,119.528879605508));
#43663=CARTESIAN_POINT('Ctrl Pts',(35.9382209753702,-84.38626269971,119.370931082315));
#43664=CARTESIAN_POINT('Ctrl Pts',(38.9592951574358,-85.5706451813641,119.212982559123));
#43665=CARTESIAN_POINT('Ctrl Pts',(39.619067106196,-88.7478062139855,119.05503403593));
#43666=CARTESIAN_POINT('Ctrl Pts',(37.3193416532641,-91.0371104719483,118.897085512738));
#43667=CARTESIAN_POINT('Ctrl Pts',(34.1452099279596,-90.3629154331271,118.739136989545));
#43668=CARTESIAN_POINT('Ctrl Pts',(32.9745606267535,-87.3364932235525,118.581188466353));
#43669=CARTESIAN_POINT('Ctrl Pts',(34.8687858683375,-84.7018088215008,118.42323994316));
#43670=CARTESIAN_POINT('Ctrl Pts',(38.1104492359489,-84.8476504414188,118.265291419968));
#43671=CARTESIAN_POINT('Ctrl Pts',(39.7604331451399,-87.6417879233585,118.107342896775));
#43672=CARTESIAN_POINT('Ctrl Pts',(38.322747367327,-90.5508617916828,117.949394373583));
#43673=CARTESIAN_POINT('Ctrl Pts',(35.1008978720714,-90.9373032457623,117.79144585039));
#43674=CARTESIAN_POINT('Ctrl Pts',(33.0160376085718,-88.4507375721237,117.633497327198));
#43675=CARTESIAN_POINT('Ctrl Pts',(33.9584459695975,-85.3456582416492,117.475548804005));
#43676=CARTESIAN_POINT('Ctrl Pts',(37.0736699562551,-84.4373462465268,117.317600280813));
#43677=CARTESIAN_POINT('Ctrl Pts',(39.5372307250997,-86.5493404476901,117.159651757621));
#43678=CARTESIAN_POINT('Ctrl Pts',(39.1154926528324,-89.7667599363363,117.001703234428));
#43679=CARTESIAN_POINT('Ctrl Pts',(36.190832822995,-91.172468315504,116.843754711236));
#43680=CARTESIAN_POINT('Ctrl Pts',(33.4149513537928,-89.491952550488,116.685806188043));
#43681=CARTESIAN_POINT('Ctrl Pts',(33.3046555487331,-86.2488851748525,116.527857664851));
#43682=CARTESIAN_POINT('Ctrl Pts',(35.9599472597682,-84.38365674465,116.369909141658));
#43683=CARTESIAN_POINT('Ctrl Pts',(38.9733542495494,-85.5874131491874,116.211960618466));
#43684=CARTESIAN_POINT('Ctrl Pts',(39.6127120490728,-88.7687450670661,116.054012095273));
#43685=CARTESIAN_POINT('Ctrl Pts',(37.2983343866991,-91.0432356041825,115.896063572081));
#43686=CARTESIAN_POINT('Ctrl Pts',(34.1285971002877,-90.3486733660357,115.738115048889));
#43687=CARTESIAN_POINT('Ctrl Pts',(32.977404584226,-87.3147968097978,115.580166525696));
#43688=CARTESIAN_POINT('Ctrl Pts',(34.8885080808896,-84.6923295378252,115.422218002504));
#43689=CARTESIAN_POINT('Ctrl Pts',(38.1291681734389,-84.858982866879,115.264269479311));
#43690=CARTESIAN_POINT('Ctrl Pts',(39.7611769161809,-87.6636572920377,115.106320956119));
#43691=CARTESIAN_POINT('Ctrl Pts',(38.3048416173737,-90.5634398123269,114.948372432926));
#43692=CARTESIAN_POINT('Ctrl Pts',(35.0805772000098,-90.9291858094989,114.790423909734));
#43693=CARTESIAN_POINT('Ctrl Pts',(33.0117261497435,-88.4292845115796,114.632475386541));
#43694=CARTESIAN_POINT('Ctrl Pts',(33.974052792591,-85.3303203943313,114.474526863349));
#43695=CARTESIAN_POINT('Ctrl Pts',(37.0950448293241,-84.4420299721299,114.316578340156));
#43696=CARTESIAN_POINT('Ctrl Pts',(39.5449937009191,-86.5697991546535,114.158629816964));
#43697=CARTESIAN_POINT('Ctrl Pts',(39.1026052773274,-89.7844443372823,114.000681293771));
#43698=CARTESIAN_POINT('Ctrl Pts',(36.1689796875839,-91.1713445019405,113.842732770579));
#43699=CARTESIAN_POINT('Ctrl Pts',(33.40394603172,-89.4730394499943,113.684784247386));
#43700=CARTESIAN_POINT('Ctrl Pts',(33.3144762308101,-86.2293307204299,113.526835724194));
#43701=CARTESIAN_POINT('Ctrl Pts',(35.9816898322384,-84.3811903654021,113.368887201001));
#43702=CARTESIAN_POINT('Ctrl Pts',(38.9873053832245,-85.6042710361663,113.210938677809));
#43703=CARTESIAN_POINT('Ctrl Pts',(39.6062226753541,-88.7896426868578,113.052990154617));
#43704=CARTESIAN_POINT('Ctrl Pts',(37.277288223372,-91.0492257204941,112.895041631424));
#43705=CARTESIAN_POINT('Ctrl Pts',(34.1120760635507,-90.3343249225886,112.737093108232));
#43706=CARTESIAN_POINT('Ctrl Pts',(32.980387795624,-87.2931191038772,112.579144585039));
#43707=CARTESIAN_POINT('Ctrl Pts',(34.9082907533782,-84.6829770860919,112.421196061847));
#43708=CARTESIAN_POINT('Ctrl Pts',(38.1478139595356,-84.8704352528771,112.263247538654));
#43709=CARTESIAN_POINT('Ctrl Pts',(39.7617802487174,-87.685530985692,112.105299015462));
#43710=CARTESIAN_POINT('Ctrl Pts',(38.2868554730895,-90.5759026008582,111.947350492269));
#43711=CARTESIAN_POINT('Ctrl Pts',(35.0603090689016,-90.9209380615865,111.789401969077));
#43712=CARTESIAN_POINT('Ctrl Pts',(33.0075525298637,-88.4078042094077,111.631453445884));
#43713=CARTESIAN_POINT('Ctrl Pts',(33.9897577781416,-85.3150830745935,111.473504922692));
#43714=CARTESIAN_POINT('Ctrl Pts',(37.1163891875685,-84.4468508491938,111.315556399499));
#43715=CARTESIAN_POINT('Ctrl Pts',(39.5526251513623,-86.5903072859396,111.157607876307));
#43716=CARTESIAN_POINT('Ctrl Pts',(39.0896046160226,-89.8020456238101,110.999659353114));
#43717=CARTESIAN_POINT('Ctrl Pts',(36.1471342185952,-91.1700803926785,110.841710829922));
#43718=CARTESIAN_POINT('Ctrl Pts',(33.393062377675,-89.4540560740673,110.683762306729));
#43719=CARTESIAN_POINT('Ctrl Pts',(33.3244222692122,-86.2098397280481,110.525813783537));
#43720=CARTESIAN_POINT('Ctrl Pts',(36.0034477938138,-84.3788636453113,110.367865260344));
#43721=CARTESIAN_POINT('Ctrl Pts',(39.0011479833795,-85.6212181572896,110.209916737152));
#43722=CARTESIAN_POINT('Ctrl Pts',(39.5995992548212,-88.8104982045884,110.05196821396));
#43723=CARTESIAN_POINT('Ctrl Pts',(37.2562040252276,-91.0550805821136,109.894019690767));
#43724=CARTESIAN_POINT('Ctrl Pts',(34.095647511379,-90.3198706806834,109.736071167575));
#43725=CARTESIAN_POINT('Ctrl Pts',(32.9835101120118,-87.2714610261512,109.578122644382));
#43726=CARTESIAN_POINT('Ctrl Pts',(34.9281331236574,-84.6737517979516,109.42017412119));
#43727=CARTESIAN_POINT('Ctrl Pts',(38.166385715407,-84.8820072378236,109.262225597997));
#43728=CARTESIAN_POINT('Ctrl Pts',(39.7622433442942,-87.7074078752085,109.104277074805));
#43729=CARTESIAN_POINT('Ctrl Pts',(38.2687892103436,-90.5882501107759,108.946328551612));
#43730=CARTESIAN_POINT('Ctrl Pts',(35.0400952721938,-90.91255938095,108.78838002842));
#43731=CARTESIAN_POINT('Ctrl Pts',(33.0035149511013,-88.3862995279612,108.630431505227));
#43732=CARTESIAN_POINT('Ctrl Pts',(34.0055643302481,-85.2999428451404,108.472482982035));
#43733=CARTESIAN_POINT('Ctrl Pts',(37.1376938182299,-84.4518170405117,108.314534458842));
#43734=CARTESIAN_POINT('Ctrl Pts',(39.5601418997229,-86.6108467988005,108.15658593565));
#43735=CARTESIAN_POINT('Ctrl Pts',(39.0764559573505,-89.8195984396968,107.998637412457));
#43736=CARTESIAN_POINT('Ctrl Pts',(36.1253698103761,-91.1686032952638,107.840688889265));
#43737=CARTESIAN_POINT('Ctrl Pts',(33.3821517419973,-89.4351528181232,107.682740366073));
#43738=CARTESIAN_POINT('Ctrl Pts',(33.3347999040718,-86.1901052353986,107.52479184288));
#43739=CARTESIAN_POINT('Ctrl Pts',(36.0245893587371,-84.3773094364523,107.366843319688));
#43740=CARTESIAN_POINT('Ctrl Pts',(39.0161790835818,-85.6369366083236,107.208894796495));
#43741=CARTESIAN_POINT('Ctrl Pts',(39.590117259602,-88.8339687646923,107.050946273303));
#43742=CARTESIAN_POINT('Ctrl Pts',(38.0238681217068,-90.311973637041,106.945647257841));
#43743=CARTESIAN_POINT('Ctrl Pts',(37.1008589290299,-90.5587331584145,106.89299775011));
#43744=CARTESIAN_POINT('Ctrl Pts',(38.6909887323796,-85.7712540316415,122.321006749669));
#43745=CARTESIAN_POINT('Ctrl Pts',(39.3517092963755,-86.5440390081348,122.268357241939));
#43746=CARTESIAN_POINT('Ctrl Pts',(39.8343589288296,-88.7843456488144,122.163058226477));
#43747=CARTESIAN_POINT('Ctrl Pts',(37.4038850601078,-91.2421290340287,122.005109703285));
#43748=CARTESIAN_POINT('Ctrl Pts',(34.0210166516482,-90.5435021562648,121.847161180092));
#43749=CARTESIAN_POINT('Ctrl Pts',(32.7548482224067,-87.3323302079001,121.6892126569));
#43750=CARTESIAN_POINT('Ctrl Pts',(34.7524572651294,-84.5150170630276,121.531264133707));
#43751=CARTESIAN_POINT('Ctrl Pts',(38.2031235339731,-84.6483923074236,121.373315610515));
#43752=CARTESIAN_POINT('Ctrl Pts',(39.9780136468089,-87.6103338294361,121.215367087322));
#43753=CARTESIAN_POINT('Ctrl Pts',(38.4679953249988,-90.71592025761,121.05741856413));
#43754=CARTESIAN_POINT('Ctrl Pts',(35.0421044228056,-91.1491283755177,120.899470040937));
#43755=CARTESIAN_POINT('Ctrl Pts',(32.806517229573,-88.517318891712,120.741521517745));
#43756=CARTESIAN_POINT('Ctrl Pts',(33.7881604074385,-85.2066066484868,120.583572994552));
#43757=CARTESIAN_POINT('Ctrl Pts',(37.0970139002824,-84.2187462125039,120.42562447136));
#43758=CARTESIAN_POINT('Ctrl Pts',(39.7330379835356,-86.4493848109254,120.267675948167));
#43759=CARTESIAN_POINT('Ctrl Pts',(39.3062312004495,-89.8760779436413,120.109727424975));
#43760=CARTESIAN_POINT('Ctrl Pts',(36.2035655956772,-91.3919434335384,119.951778901782));
#43761=CARTESIAN_POINT('Ctrl Pts',(33.2381340427318,-89.6225939583723,119.79383037859));
#43762=CARTESIAN_POINT('Ctrl Pts',(33.0986029792476,-86.1722439927149,119.635881855398));
#43763=CARTESIAN_POINT('Ctrl Pts',(35.9114810555574,-84.1692213417312,119.477933332205));
#43764=CARTESIAN_POINT('Ctrl Pts',(39.1264172314171,-85.4296055153237,119.319984809012));
#43765=CARTESIAN_POINT('Ctrl Pts',(39.8285266726477,-88.8106446175552,119.16203628582));
#43766=CARTESIAN_POINT('Ctrl Pts',(37.3812280935308,-91.2468532747826,119.004087762628));
#43767=CARTESIAN_POINT('Ctrl Pts',(34.0034126889292,-90.529395215408,118.846139239435));
#43768=CARTESIAN_POINT('Ctrl Pts',(32.7576429524446,-87.3087678297098,118.688190716243));
#43769=CARTESIAN_POINT('Ctrl Pts',(34.7734204168137,-84.5050160230137,118.53024219305));
#43770=CARTESIAN_POINT('Ctrl Pts',(38.2231009616876,-84.6602162834389,118.372293669858));
#43771=CARTESIAN_POINT('Ctrl Pts',(39.9789641545662,-87.6336532564003,118.214345146665));
#43772=CARTESIAN_POINT('Ctrl Pts',(38.4490222405119,-90.7294020708598,118.056396623473));
#43773=CARTESIAN_POINT('Ctrl Pts',(35.0204270219759,-91.1406414300081,117.89844810028));
#43774=CARTESIAN_POINT('Ctrl Pts',(32.8017815075667,-88.4945131140308,117.740499577088));
#43775=CARTESIAN_POINT('Ctrl Pts',(33.8046641081597,-85.1901811887448,117.582551053895));
#43776=CARTESIAN_POINT('Ctrl Pts',(37.1197916710861,-84.2235829140579,117.424602530703));
#43777=CARTESIAN_POINT('Ctrl Pts',(39.7414388600909,-86.4711035478885,117.26665400751));
#43778=CARTESIAN_POINT('Ctrl Pts',(39.2926379026969,-89.8949844867843,117.108705484318));
#43779=CARTESIAN_POINT('Ctrl Pts',(36.1803029773098,-91.3908970160839,116.950756961125));
#43780=CARTESIAN_POINT('Ctrl Pts',(33.22629350339,-89.6025427415926,116.792808437933));
#43781=CARTESIAN_POINT('Ctrl Pts',(33.1089200288037,-86.1513680936557,116.634859914741));
#43782=CARTESIAN_POINT('Ctrl Pts',(35.9346015132054,-84.1664481628253,116.476911391548));
#43783=CARTESIAN_POINT('Ctrl Pts',(39.1413784939057,-85.4474494817745,116.318962868356));
#43784=CARTESIAN_POINT('Ctrl Pts',(39.8217638122167,-88.8329271145059,116.161014345163));
#43785=CARTESIAN_POINT('Ctrl Pts',(37.35887279301,-91.2533714560701,116.003065821971));
#43786=CARTESIAN_POINT('Ctrl Pts',(33.9857338179559,-90.5142392364574,115.845117298778));
#43787=CARTESIAN_POINT('Ctrl Pts',(32.7606694063514,-87.2856791595006,115.687168775586));
#43788=CARTESIAN_POINT('Ctrl Pts',(34.7944082015486,-84.4949284547604,115.529220252393));
#43789=CARTESIAN_POINT('Ctrl Pts',(38.2430210913116,-84.6722759093786,115.371271729201));
#43790=CARTESIAN_POINT('Ctrl Pts',(39.979755653312,-87.6569259800321,115.213323206008));
#43791=CARTESIAN_POINT('Ctrl Pts',(38.4299674805782,-90.7427872216878,115.055374682816));
#43792=CARTESIAN_POINT('Ctrl Pts',(34.9988023746513,-91.1320030987637,114.897426159623));
#43793=CARTESIAN_POINT('Ctrl Pts',(32.7971933829057,-88.471683412981,114.739477636431));
#43794=CARTESIAN_POINT('Ctrl Pts',(33.8212724192465,-85.1738591134728,114.581529113239));
#43795=CARTESIAN_POINT('Ctrl Pts',(37.1425381673794,-84.2285671938113,114.423580590046));
#43796=CARTESIAN_POINT('Ctrl Pts',(39.749699985204,-86.4928750877993,114.265632066854));
#43797=CARTESIAN_POINT('Ctrl Pts',(39.278923545741,-89.9138036937695,114.107683543661));
#43798=CARTESIAN_POINT('Ctrl Pts',(36.1570475286333,-91.3897010875291,113.949735020469));
#43799=CARTESIAN_POINT('Ctrl Pts',(33.2145819710255,-89.5824159895466,113.791786497276));
#43800=CARTESIAN_POINT('Ctrl Pts',(33.1193709029558,-86.1305588320708,113.633837974084));
#43801=CARTESIAN_POINT('Ctrl Pts',(35.9577393041295,-84.1638235162957,113.475889450891));
#43802=CARTESIAN_POINT('Ctrl Pts',(39.1562248702749,-85.4653891374834,113.317940927699));
#43803=CARTESIAN_POINT('Ctrl Pts',(39.8148580161093,-88.8551657322322,113.159992404506));
#43804=CARTESIAN_POINT('Ctrl Pts',(37.3364760997262,-91.2597459574781,113.002043881314));
#43805=CARTESIAN_POINT('Ctrl Pts',(33.9681526281314,-90.4989700549925,112.844095358121));
#43806=CARTESIAN_POINT('Ctrl Pts',(32.7638440500926,-87.2626103976056,112.686146834929));
#43807=CARTESIAN_POINT('Ctrl Pts',(34.8154603259275,-84.484975857241,112.528198311736));
#43808=CARTESIAN_POINT('Ctrl Pts',(38.2628633754255,-84.6844631937108,112.370249788544));
#43809=CARTESIAN_POINT('Ctrl Pts',(39.9803977016302,-87.6802033061719,112.212301265351));
#43810=CARTESIAN_POINT('Ctrl Pts',(38.4108271674185,-90.7560497459711,112.054352742159));
#43811=CARTESIAN_POINT('Ctrl Pts',(34.9772336398273,-91.1232260937864,111.896404218966));
#43812=CARTESIAN_POINT('Ctrl Pts',(32.792751942303,-88.448824722211,111.738455695774));
#43813=CARTESIAN_POINT('Ctrl Pts',(33.8379851919707,-85.1576440166245,111.580507172582));
#43814=CARTESIAN_POINT('Ctrl Pts',(37.1652521907151,-84.2336974260193,111.422558649389));
#43815=CARTESIAN_POINT('Ctrl Pts',(39.7578211449723,-86.5146992235859,111.264610126197));
#43816=CARTESIAN_POINT('Ctrl Pts',(39.2650886334483,-89.9325344528934,111.106661603004));
#43817=CARTESIAN_POINT('Ctrl Pts',(36.1338002383326,-91.3883558605165,110.948713079812));
#43818=CARTESIAN_POINT('Ctrl Pts',(33.2029999141126,-89.5622144525007,110.790764556619));
#43819=CARTESIAN_POINT('Ctrl Pts',(33.1299551775344,-86.1098171048787,110.632816033427));
#43820=CARTESIAN_POINT('Ctrl Pts',(35.9808934716759,-84.1613474908357,110.474867510234));
#43821=CARTESIAN_POINT('Ctrl Pts',(39.1709557485403,-85.4834237534817,110.316918987042));
#43822=CARTESIAN_POINT('Ctrl Pts',(39.8078095714184,-88.8773595462129,110.158970463849));
#43823=CARTESIAN_POINT('Ctrl Pts',(37.3140389309351,-91.2659765249159,110.001021940657));
#43824=CARTESIAN_POINT('Ctrl Pts',(33.9506698575966,-90.4835882859939,109.843073417465));
#43825=CARTESIAN_POINT('Ctrl Pts',(32.7671667251752,-87.2395625234441,109.685124894272));
#43826=CARTESIAN_POINT('Ctrl Pts',(34.8365759788977,-84.4751585833882,109.527176371079));
#43827=CARTESIAN_POINT('Ctrl Pts',(38.2826268788027,-84.6967777516425,109.369227847887));
#43828=CARTESIAN_POINT('Ctrl Pts',(39.9808905139985,-87.7034840332521,109.211279324694));
#43829=CARTESIAN_POINT('Ctrl Pts',(38.3916015946044,-90.7691895942252,109.053330801502));
#43830=CARTESIAN_POINT('Ctrl Pts',(34.9557227260359,-91.1143097541466,108.89538227831));
#43831=CARTESIAN_POINT('Ctrl Pts',(32.7884552725611,-88.4259400877512,108.737433755117));
#43832=CARTESIAN_POINT('Ctrl Pts',(33.8548060487655,-85.1415322403337,108.579485231925));
#43833=CARTESIAN_POINT('Ctrl Pts',(37.1879239371534,-84.238982297281,108.421536708732));
#43834=CARTESIAN_POINT('Ctrl Pts',(39.7658202422379,-86.5365567546996,108.26358818554));
#43835=CARTESIAN_POINT('Ctrl Pts',(39.2510962268136,-89.9512136310206,108.105639662347));
#43836=CARTESIAN_POINT('Ctrl Pts',(36.1106392104622,-91.3867839779253,107.947691139155));
#43837=CARTESIAN_POINT('Ctrl Pts',(33.1913891441585,-89.5420981767279,107.789742615962));
#43838=CARTESIAN_POINT('Ctrl Pts',(33.1409987440672,-86.0888162520338,107.63179409277));
#43839=CARTESIAN_POINT('Ctrl Pts',(36.0033916884657,-84.1596935485673,107.473845569577));
#43840=CARTESIAN_POINT('Ctrl Pts',(39.1869513927685,-85.500150855768,107.315897046385));
#43841=CARTESIAN_POINT('Ctrl Pts',(39.797719117622,-88.9023362095446,107.157948523192));
#43842=CARTESIAN_POINT('Ctrl Pts',(38.1309639469875,-90.4751844899406,107.052649507731));
#43843=CARTESIAN_POINT('Ctrl Pts',(37.1487253572158,-90.7377785423181,107.));
#43844=CARTESIAN_POINT('Ctrl Pts',(38.2683920713486,-86.1325683851972,122.));
#43845=CARTESIAN_POINT('Ctrl Pts',(38.3300002507757,-86.1904649458245,122.));
#43846=CARTESIAN_POINT('Ctrl Pts',(38.3882392757579,-86.251512267457,122.));
#43847=CARTESIAN_POINT('Ctrl Pts',(38.4431115334664,-86.315325530903,122.));
#43848=CARTESIAN_POINT('Ctrl Pts',(38.4994367220781,-86.3808284689928,122.));
#43849=CARTESIAN_POINT('Ctrl Pts',(38.5522149264209,-86.4492461953977,122.));
#43850=CARTESIAN_POINT('Ctrl Pts',(38.6014232205322,-86.5202110570223,122.));
#43851=CARTESIAN_POINT('Ctrl Pts',(38.651981111331,-86.5931222153823,122.));
#43852=CARTESIAN_POINT('Ctrl Pts',(38.6987711210245,-86.6687226978473,122.));
#43853=CARTESIAN_POINT('Ctrl Pts',(38.7417343172596,-86.7466567430807,122.));
#43854=CARTESIAN_POINT('Ctrl Pts',(38.7606443000318,-86.7809589268538,122.));
#43855=CARTESIAN_POINT('Ctrl Pts',(38.7788124429666,-86.8157136817185,122.));
#43856=CARTESIAN_POINT('Ctrl Pts',(38.7962312959641,-86.850892750047,122.));
#43857=CARTESIAN_POINT('Ctrl Pts',(38.8061621411259,-86.8709490580347,122.));
#43858=CARTESIAN_POINT('Ctrl Pts',(38.815849410692,-86.8911433045237,122.));
#43859=CARTESIAN_POINT('Ctrl Pts',(38.8252914897478,-86.9114704014436,122.));
#43860=CARTESIAN_POINT('Ctrl Pts',(38.8337970736902,-86.9297813929251,122.));
#43861=CARTESIAN_POINT('Ctrl Pts',(38.8421060671472,-86.9482059164998,122.));
#43862=CARTESIAN_POINT('Ctrl Pts',(38.8502036291305,-86.9667084981428,122.));
#43863=CARTESIAN_POINT('Ctrl Pts',(38.8867652309718,-87.0502501893895,122.));
#43864=CARTESIAN_POINT('Ctrl Pts',(38.9190666540545,-87.1354754242206,122.));
#43865=CARTESIAN_POINT('Ctrl Pts',(38.947082863758,-87.2219854243391,122.));
#43866=CARTESIAN_POINT('Ctrl Pts',(38.9755621712229,-87.3099254033098,122.));
#43867=CARTESIAN_POINT('Ctrl Pts',(38.9996139217682,-87.3991937270396,122.));
#43868=CARTESIAN_POINT('Ctrl Pts',(39.0191727436887,-87.4894086379833,122.));
#43869=CARTESIAN_POINT('Ctrl Pts',(39.0381412062379,-87.5769005210103,122.));
#43870=CARTESIAN_POINT('Ctrl Pts',(39.0528840306109,-87.6652836278016,122.));
#43871=CARTESIAN_POINT('Ctrl Pts',(39.0633008450673,-87.7542316018242,122.));
#43872=CARTESIAN_POINT('Ctrl Pts',(39.0676696750207,-87.791536535576,122.));
#43873=CARTESIAN_POINT('Ctrl Pts',(39.0712770535737,-87.8289410203567,122.));
#43874=CARTESIAN_POINT('Ctrl Pts',(39.0741132412595,-87.8664215984214,122.));
#43875=CARTESIAN_POINT('Ctrl Pts',(39.0758923650537,-87.8899329438063,122.));
#43876=CARTESIAN_POINT('Ctrl Pts',(39.0773679986009,-87.9134742372075,122.));
#43877=CARTESIAN_POINT('Ctrl Pts',(39.0785374418203,-87.9370397212164,122.));
#43878=CARTESIAN_POINT('Ctrl Pts',(39.0792218231253,-87.950830708611,122.));
#43879=CARTESIAN_POINT('Ctrl Pts',(39.0798010498032,-87.964625034357,122.));
#43880=CARTESIAN_POINT('Ctrl Pts',(39.0802746210619,-87.9784137075555,122.));
#43881=CARTESIAN_POINT('Ctrl Pts',(39.0836019902155,-88.0752945993602,122.));
#43882=CARTESIAN_POINT('Ctrl Pts',(39.0817234464995,-88.172010484153,122.));
#43883=CARTESIAN_POINT('Ctrl Pts',(39.074574609124,-88.2681415945912,122.));
#43884=CARTESIAN_POINT('Ctrl Pts',(39.0674257717486,-88.3642727050294,122.));
#43885=CARTESIAN_POINT('Ctrl Pts',(39.0550070710252,-88.4598200851495,122.));
#43886=CARTESIAN_POINT('Ctrl Pts',(39.0372016632323,-88.5543827530839,122.));
#43887=CARTESIAN_POINT('Ctrl Pts',(39.0201436337382,-88.6449761726466,122.));
#43888=CARTESIAN_POINT('Ctrl Pts',(38.9981417504386,-88.7346667799934,122.));
#43889=CARTESIAN_POINT('Ctrl Pts',(38.9714706220827,-88.8232152361145,122.));
#43890=CARTESIAN_POINT('Ctrl Pts',(38.9626012728804,-88.852661578548,122.));
#43891=CARTESIAN_POINT('Ctrl Pts',(38.9532151392587,-88.8819815788975,122.));
#43892=CARTESIAN_POINT('Ctrl Pts',(38.9433210712961,-88.9111662610406,122.));
#43893=CARTESIAN_POINT('Ctrl Pts',(38.9340007339025,-88.9386586014335,122.));
#43894=CARTESIAN_POINT('Ctrl Pts',(38.9242296555423,-88.9660308631234,122.));
#43895=CARTESIAN_POINT('Ctrl Pts',(38.9140147595642,-88.9932754177916,122.));
#43896=CARTESIAN_POINT('Ctrl Pts',(38.9088570148167,-89.007031843607,122.));
#43897=CARTESIAN_POINT('Ctrl Pts',(38.9035891933686,-89.0207474361896,122.));
#43898=CARTESIAN_POINT('Ctrl Pts',(38.8982139648971,-89.034417877811,122.));
#43899=CARTESIAN_POINT('Ctrl Pts',(38.8639626423259,-89.121526864554,122.));
#43900=CARTESIAN_POINT('Ctrl Pts',(38.8253378210354,-89.2068470331141,122.));
#43901=CARTESIAN_POINT('Ctrl Pts',(38.7826694863704,-89.2901439691626,122.));
#43902=CARTESIAN_POINT('Ctrl Pts',(38.7384396869984,-89.3764891897729,122.));
#43903=CARTESIAN_POINT('Ctrl Pts',(38.6898648813373,-89.4606611168872,122.));
#43904=CARTESIAN_POINT('Ctrl Pts',(38.6372567796703,-89.5423951719936,122.));
#43905=CARTESIAN_POINT('Ctrl Pts',(38.5840857288504,-89.6250038474651,122.));
#43906=CARTESIAN_POINT('Ctrl Pts',(38.5267941860822,-89.7051230190292,122.));
#43907=CARTESIAN_POINT('Ctrl Pts',(38.4656524677661,-89.7824641587497,122.));
#43908=CARTESIAN_POINT('Ctrl Pts',(38.4429635855522,-89.8111644317832,122.));
#43909=CARTESIAN_POINT('Ctrl Pts',(38.4197440399425,-89.8394819408235,122.));
#43910=CARTESIAN_POINT('Ctrl Pts',(38.3960060498082,-89.867401053708,122.));
#43911=CARTESIAN_POINT('Ctrl Pts',(38.3752506128797,-89.8918122773753,122.));
#43912=CARTESIAN_POINT('Ctrl Pts',(38.3540988125212,-89.9159189229224,122.));
#43913=CARTESIAN_POINT('Ctrl Pts',(38.3325583266211,-89.9397101583158,122.));
#43914=CARTESIAN_POINT('Ctrl Pts',(38.3207950958777,-89.9527025203685,122.));
#43915=CARTESIAN_POINT('Ctrl Pts',(38.3089206259342,-89.9655955686881,122.));
#43916=CARTESIAN_POINT('Ctrl Pts',(38.2969422410122,-89.9783816819787,122.));
#43917=CARTESIAN_POINT('Ctrl Pts',(38.2279314720012,-90.0520459962072,122.));
#43918=CARTESIAN_POINT('Ctrl Pts',(38.1554183053285,-90.1222257786201,122.));
#43919=CARTESIAN_POINT('Ctrl Pts',(38.0797112616787,-90.1886298153968,122.));
#43920=CARTESIAN_POINT('Ctrl Pts',(38.0175171475697,-90.2431814137882,122.));
#43921=CARTESIAN_POINT('Ctrl Pts',(37.9531664610367,-90.2951847791595,122.));
#43922=CARTESIAN_POINT('Ctrl Pts',(37.8868079691602,-90.3444651219269,122.));
#43923=CARTESIAN_POINT('Ctrl Pts',(37.8621903721155,-90.3627470868445,122.));
#43924=CARTESIAN_POINT('Ctrl Pts',(37.8372962693708,-90.3806541493651,122.));
#43925=CARTESIAN_POINT('Ctrl Pts',(37.8121326494392,-90.39817682058,122.));
#43926=CARTESIAN_POINT('Ctrl Pts',(37.7953218298329,-90.4098830244416,122.));
#43927=CARTESIAN_POINT('Ctrl Pts',(37.7783895868136,-90.4214183026613,122.));
#43928=CARTESIAN_POINT('Ctrl Pts',(37.7613530646459,-90.4327700028003,122.));
#43929=CARTESIAN_POINT('Ctrl Pts',(37.6764426037664,-90.4893471657374,122.));
#43930=CARTESIAN_POINT('Ctrl Pts',(37.5888628636194,-90.5414250307333,122.));
#43931=CARTESIAN_POINT('Ctrl Pts',(37.4989042014469,-90.5886956823262,122.));
#43932=CARTESIAN_POINT('Ctrl Pts',(37.4154461624309,-90.6325504461663,122.));
#43933=CARTESIAN_POINT('Ctrl Pts',(37.3299397797897,-90.6722679264133,122.));
#43934=CARTESIAN_POINT('Ctrl Pts',(37.2425891939653,-90.7075731985908,122.));
#43935=CARTESIAN_POINT('Ctrl Pts',(37.2121590204155,-90.7198724356188,122.));
#43936=CARTESIAN_POINT('Ctrl Pts',(37.1815048261116,-90.7316359142083,122.));
#43937=CARTESIAN_POINT('Ctrl Pts',(37.1506395173467,-90.742867356818,122.));
#43938=CARTESIAN_POINT('Ctrl Pts',(33.8367589339947,-87.7707538181913,120.387416697508));
#43939=CARTESIAN_POINT('Ctrl Pts',(33.8351765741934,-87.9451202468588,120.398449387697));
#43940=CARTESIAN_POINT('Ctrl Pts',(33.851762168828,-88.119187630204,120.409482077886));
#43941=CARTESIAN_POINT('Ctrl Pts',(33.8876337290323,-88.2891852722709,120.420514768075));
#43942=CARTESIAN_POINT('Ctrl Pts',(34.058817724406,-89.1004372893958,120.473164275806));
#43943=CARTESIAN_POINT('Ctrl Pts',(34.669206614267,-89.8190079065511,120.525813783537));
#43944=CARTESIAN_POINT('Ctrl Pts',(35.4420915502918,-90.1191531773417,120.578463291268));
#43945=CARTESIAN_POINT('Ctrl Pts',(36.2149764863167,-90.4192984481322,120.631112798999));
#43946=CARTESIAN_POINT('Ctrl Pts',(37.1503574685054,-90.3010183725579,120.683762306729));
#43947=CARTESIAN_POINT('Ctrl Pts',(37.8241903122464,-89.8179146759167,120.73641181446));
#43948=CARTESIAN_POINT('Ctrl Pts',(38.4980231559875,-89.3348109792755,120.789061322191));
#43949=CARTESIAN_POINT('Ctrl Pts',(38.9103078612808,-88.4868836615674,120.841710829922));
#43950=CARTESIAN_POINT('Ctrl Pts',(38.8741485025743,-87.6585662376428,120.894360337653));
#43951=CARTESIAN_POINT('Ctrl Pts',(38.8379891438677,-86.8302488137182,120.947009845384));
#43952=CARTESIAN_POINT('Ctrl Pts',(38.3533857211613,-86.021541283577,120.999659353114));
#43953=CARTESIAN_POINT('Ctrl Pts',(37.6400112734157,-85.5989796025709,121.052308860845));
#43954=CARTESIAN_POINT('Ctrl Pts',(36.92663682567,-85.1764179215648,121.104958368576));
#43955=CARTESIAN_POINT('Ctrl Pts',(35.984491352885,-85.1400020896938,121.157607876307));
#43956=CARTESIAN_POINT('Ctrl Pts',(35.2407121057255,-85.5064037850709,121.210257384038));
#43957=CARTESIAN_POINT('Ctrl Pts',(34.496932858566,-85.872805480448,121.262906891769));
#43958=CARTESIAN_POINT('Ctrl Pts',(33.9515198370319,-86.6420247030733,121.315556399499));
#43959=CARTESIAN_POINT('Ctrl Pts',(33.8516661553206,-87.4650121344612,121.36820590723));
#43960=CARTESIAN_POINT('Ctrl Pts',(33.8395212609014,-87.5651095499113,121.374609503989));
#43961=CARTESIAN_POINT('Ctrl Pts',(33.8339675723167,-87.6660023640875,121.381013100749));
#43962=CARTESIAN_POINT('Ctrl Pts',(33.8347233377312,-87.7669766891919,121.387416697508));
#43963=CARTESIAN_POINT('Ctrl Pts',(35.5611267921506,-90.7377785423179,122.));
#43964=CARTESIAN_POINT('Ctrl Pts',(34.5788882023789,-90.4751844899402,121.947350492269));
#43965=CARTESIAN_POINT('Ctrl Pts',(32.9121323375455,-88.9023410125859,121.842051476808));
#43966=CARTESIAN_POINT('Ctrl Pts',(33.5229013557052,-85.5001496093779,121.684102953615));
#43967=CARTESIAN_POINT('Ctrl Pts',(36.7064604149176,-84.1596949927803,121.526154430422));
#43968=CARTESIAN_POINT('Ctrl Pts',(39.5688528980205,-86.0888159753533,121.36820590723));
#43969=CARTESIAN_POINT('Ctrl Pts',(39.5184626244884,-89.5420982077003,121.210257384038));
#43970=CARTESIAN_POINT('Ctrl Pts',(36.5992128626851,-91.3867833270583,121.052308860845));
#43971=CARTESIAN_POINT('Ctrl Pts',(33.4587563518577,-89.9512134072174,120.894360337653));
#43972=CARTESIAN_POINT('Ctrl Pts',(32.944032363916,-86.5365568838997,120.73641181446));
#43973=CARTESIAN_POINT('Ctrl Pts',(35.5219283374979,-84.238982809065,120.578463291268));
#43974=CARTESIAN_POINT('Ctrl Pts',(38.8550457481358,-85.1415325934838,120.420514768075));
#43975=CARTESIAN_POINT('Ctrl Pts',(39.921396384874,-88.4259400024622,120.262566244883));
#43976=CARTESIAN_POINT('Ctrl Pts',(37.7541292274747,-91.1143092867255,120.10461772169));
#43977=CARTESIAN_POINT('Ctrl Pts',(34.3182508383241,-90.7691891793635,119.946669198498));
#43978=CARTESIAN_POINT('Ctrl Pts',(32.7289621381221,-87.7034840414673,119.788720675305));
#43979=CARTESIAN_POINT('Ctrl Pts',(34.4272255383588,-84.6967781783805,119.630772152113));
#43980=CARTESIAN_POINT('Ctrl Pts',(37.8732759596097,-84.4751590402537,119.47282362892));
#43981=CARTESIAN_POINT('Ctrl Pts',(39.9426849263303,-87.2395625969708,119.314875105728));
#43982=CARTESIAN_POINT('Ctrl Pts',(38.7591819580553,-90.4835879091297,119.156926582536));
#43983=CARTESIAN_POINT('Ctrl Pts',(35.3958133515618,-91.2659760395494,118.998978059343));
#43984=CARTESIAN_POINT('Ctrl Pts',(32.9020430571518,-88.877359392311,118.841029536151));
#43985=CARTESIAN_POINT('Ctrl Pts',(33.5388967916589,-85.4834240706333,118.683081012958));
#43986=CARTESIAN_POINT('Ctrl Pts',(36.7289586257789,-84.1613479914634,118.525132489766));
#43987=CARTESIAN_POINT('Ctrl Pts',(39.5798965242524,-86.1098173350916,118.367183966573));
#43988=CARTESIAN_POINT('Ctrl Pts',(39.506851797809,-89.5622142035652,118.209235443381));
#43989=CARTESIAN_POINT('Ctrl Pts',(36.5760518803447,-91.3883553581382,118.051286920188));
#43990=CARTESIAN_POINT('Ctrl Pts',(33.444763919809,-89.9325341525616,117.893338396996));
#43991=CARTESIAN_POINT('Ctrl Pts',(32.9520314766706,-86.5146993976035,117.735389873803));
#43992=CARTESIAN_POINT('Ctrl Pts',(35.544600071115,-84.2336979166091,117.577441350611));
#43993=CARTESIAN_POINT('Ctrl Pts',(38.87186660808,-85.1576443789841,117.419492827418));
#43994=CARTESIAN_POINT('Ctrl Pts',(39.9170997126827,-88.4488246277999,117.261544304226));
#43995=CARTESIAN_POINT('Ctrl Pts',(37.7326183183341,-91.1232256282042,117.103595781033));
#43996=CARTESIAN_POINT('Ctrl Pts',(34.2990252672788,-90.7560493313473,116.945647257841));
#43997=CARTESIAN_POINT('Ctrl Pts',(32.7294549509029,-87.6802033184331,116.787698734649));
#43998=CARTESIAN_POINT('Ctrl Pts',(34.446989038738,-84.6844636217403,116.629750211456));
#43999=CARTESIAN_POINT('Ctrl Pts',(37.8943916097836,-84.4849763129574,116.471801688264));
#44000=CARTESIAN_POINT('Ctrl Pts',(39.9460076008814,-87.2626104678248,116.313853165071));
#44001=CARTESIAN_POINT('Ctrl Pts',(38.7416991899834,-90.4989696760488,116.155904641879));
#44002=CARTESIAN_POINT('Ctrl Pts',(35.3733761858658,-91.2597454729484,115.997956118686));
#44003=CARTESIAN_POINT('Ctrl Pts',(32.8949946134489,-88.8551655814247,115.840007595494));
#44004=CARTESIAN_POINT('Ctrl Pts',(33.5536276678748,-85.4653894571308,115.682059072301));
#44005=CARTESIAN_POINT('Ctrl Pts',(36.7521127901144,-84.1638240165833,115.524110549109));
#44006=CARTESIAN_POINT('Ctrl Pts',(39.5904807973608,-86.1305590594033,115.366162025916));
#44007=CARTESIAN_POINT('Ctrl Pts',(39.4952697425043,-89.5824157378083,115.208213502724));
#44008=CARTESIAN_POINT('Ctrl Pts',(36.55280459327,-91.3897005849636,115.050264979531));
#44009=CARTESIAN_POINT('Ctrl Pts',(33.4309290094365,-89.9138033960376,114.892316456339));
#44010=CARTESIAN_POINT('Ctrl Pts',(32.9601526353117,-86.4928752648455,114.734367933146));
#44011=CARTESIAN_POINT('Ctrl Pts',(35.5673140912984,-84.2285676851132,114.576419409954));
#44012=CARTESIAN_POINT('Ctrl Pts',(38.8885793784847,-85.1738594735819,114.418470886761));
#44013=CARTESIAN_POINT('Ctrl Pts',(39.9126582726965,-88.4716833153973,114.260522363569));
#44014=CARTESIAN_POINT('Ctrl Pts',(37.7110495865035,-91.1320026319635,114.102573840377));
#44015=CARTESIAN_POINT('Ctrl Pts',(34.2798849567756,-90.7427868089045,113.944625317184));
#44016=CARTESIAN_POINT('Ctrl Pts',(32.730096999132,-87.6569259955238,113.786676793992));
#44017=CARTESIAN_POINT('Ctrl Pts',(34.4668313200981,-84.6722763390996,113.628728270799));
#44018=CARTESIAN_POINT('Ctrl Pts',(37.9154437312407,-84.4949289090955,113.470779747607));
#44019=CARTESIAN_POINT('Ctrl Pts',(39.949182244182,-87.2856792265183,113.312831224414));
#44020=CARTESIAN_POINT('Ctrl Pts',(38.724118002599,-90.5142388553946,113.154882701222));
#44021=CARTESIAN_POINT('Ctrl Pts',(35.3509794956904,-91.2533709724249,112.996934178029));
#44022=CARTESIAN_POINT('Ctrl Pts',(32.8880888182999,-88.832926966785,112.838985654837));
#44023=CARTESIAN_POINT('Ctrl Pts',(33.5684740421835,-85.4474498039115,112.681037131644));
#44024=CARTESIAN_POINT('Ctrl Pts',(36.7752505778273,-84.1664486627489,112.523088608452));
#44025=CARTESIAN_POINT('Ctrl Pts',(39.6009316700625,-86.1513683181001,112.365140085259));
#44026=CARTESIAN_POINT('Ctrl Pts',(39.4835582117651,-89.6025424870611,112.207191562067));
#44027=CARTESIAN_POINT('Ctrl Pts',(36.5295491478211,-91.3908965133523,112.049243038874));
#44028=CARTESIAN_POINT('Ctrl Pts',(33.417214654384,-89.8949841916642,111.891294515682));
#44029=CARTESIAN_POINT('Ctrl Pts',(32.9684137592783,-86.4711037279564,111.73334599249));
#44030=CARTESIAN_POINT('Ctrl Pts',(35.5900605844347,-84.2235834060515,111.575397469297));
#44031=CARTESIAN_POINT('Ctrl Pts',(38.9051876872665,-85.1901815465887,111.417448946105));
#44032=CARTESIAN_POINT('Ctrl Pts',(39.9080701486722,-88.4945130132787,111.259500422912));
#44033=CARTESIAN_POINT('Ctrl Pts',(37.6894249421801,-91.1406409620089,111.10155189972));
#44034=CARTESIAN_POINT('Ctrl Pts',(34.2608301994864,-90.7294016599341,110.943603376527));
#44035=CARTESIAN_POINT('Ctrl Pts',(32.730888497768,-87.6336532751223,110.785654853335));
#44036=CARTESIAN_POINT('Ctrl Pts',(34.4867514469574,-84.660216714833,110.627706330142));
#44037=CARTESIAN_POINT('Ctrl Pts',(37.9364315130628,-84.5050164759499,110.46975780695));
#44038=CARTESIAN_POINT('Ctrl Pts',(39.9522086976689,-87.3087678935207,110.311809283757));
#44039=CARTESIAN_POINT('Ctrl Pts',(38.7064391340791,-90.5293948322461,110.153860760565));
#44040=CARTESIAN_POINT('Ctrl Pts',(35.3286241982722,-91.2468527920333,109.995912237372));
#44041=CARTESIAN_POINT('Ctrl Pts',(32.8813259588075,-88.8106444729439,109.83796371418));
#44042=CARTESIAN_POINT('Ctrl Pts',(33.5834353025955,-85.4296058399034,109.680015190987));
#44043=CARTESIAN_POINT('Ctrl Pts',(36.7983710322676,-84.1692218413362,109.522066667795));
#44044=CARTESIAN_POINT('Ctrl Pts',(39.611248718183,-86.1722442141325,109.364118144603));
#44045=CARTESIAN_POINT('Ctrl Pts',(39.4717176740767,-89.6225937013098,109.20616962141));
#44046=CARTESIAN_POINT('Ctrl Pts',(36.506286532656,-91.3919429301732,109.048221098218));
#44047=CARTESIAN_POINT('Ctrl Pts',(33.4036213585832,-89.8760776520892,108.890272575025));
#44048=CARTESIAN_POINT('Ctrl Pts',(32.9768146345105,-86.4493849921911,108.732324051833));
#44049=CARTESIAN_POINT('Ctrl Pts',(35.6128383524474,-84.2187467086474,108.57437552864));
#44050=CARTESIAN_POINT('Ctrl Pts',(38.9216913848391,-85.2066069974257,108.416427005448));
#44051=CARTESIAN_POINT('Ctrl Pts',(39.9033344292869,-88.5173188003331,108.258478482255));
#44052=CARTESIAN_POINT('Ctrl Pts',(37.6677475399111,-91.14912788279,108.100529959063));
#44053=CARTESIAN_POINT('Ctrl Pts',(34.2418571276214,-90.7159198923917,107.94258143587));
#44054=CARTESIAN_POINT('Ctrl Pts',(32.7318389831201,-87.6103337706953,107.784632912678));
#44055=CARTESIAN_POINT('Ctrl Pts',(34.5067289212608,-84.6483928869776,107.626684389485));
#44056=CARTESIAN_POINT('Ctrl Pts',(37.9573945529429,-84.5150172531596,107.468735866293));
#44057=CARTESIAN_POINT('Ctrl Pts',(39.9550036656341,-87.3323307232591,107.3107873431));
#44058=CARTESIAN_POINT('Ctrl Pts',(38.68883464176,-90.5435009921344,107.152838819908));
#44059=CARTESIAN_POINT('Ctrl Pts',(35.3059682889895,-91.2421297218218,106.994890296715));
#44060=CARTESIAN_POINT('Ctrl Pts',(32.8754899278038,-88.7843420838406,106.836941773523));
#44061=CARTESIAN_POINT('Ctrl Pts',(33.3581428529919,-86.544039008134,106.731642758061));
#44062=CARTESIAN_POINT('Ctrl Pts',(34.018863416988,-85.7712540316409,106.678993250331));
#44063=CARTESIAN_POINT('Ctrl Pts',(35.6089932203365,-90.5587331584144,122.10700224989));
#44064=CARTESIAN_POINT('Ctrl Pts',(34.6859840276597,-90.3119736370406,122.054352742159));
#44065=CARTESIAN_POINT('Ctrl Pts',(33.1197342374261,-88.8339732781081,121.949053726697));
#44066=CARTESIAN_POINT('Ctrl Pts',(33.6936736287654,-85.6369354370915,121.791105203505));
#44067=CARTESIAN_POINT('Ctrl Pts',(36.6852627474191,-84.3773107935785,121.633156680312));
#44068=CARTESIAN_POINT('Ctrl Pts',(39.375051768605,-86.1901049754021,121.47520815712));
#44069=CARTESIAN_POINT('Ctrl Pts',(39.3277000496072,-89.435152847228,121.317259633928));
#44070=CARTESIAN_POINT('Ctrl Pts',(36.5844822673672,-91.1686026836444,121.159311110735));
#44071=CARTESIAN_POINT('Ctrl Pts',(33.6333965954336,-89.8195982293889,121.001362587543));
#44072=CARTESIAN_POINT('Ctrl Pts',(33.1497106788866,-86.6108469202099,120.84341406435));
#44073=CARTESIAN_POINT('Ctrl Pts',(35.5721584488666,-84.4518175214348,120.685465541157));
#44074=CARTESIAN_POINT('Ctrl Pts',(38.704287487907,-85.2999431769956,120.527517017965));
#44075=CARTESIAN_POINT('Ctrl Pts',(39.7063367359976,-88.3862994478151,120.369568494773));
#44076=CARTESIAN_POINT('Ctrl Pts',(37.6697566931271,-90.9125589417146,120.21161997158));
#44077=CARTESIAN_POINT('Ctrl Pts',(34.441063205486,-90.5882497209306,120.053671448388));
#44078=CARTESIAN_POINT('Ctrl Pts',(32.9476092775101,-87.7074078829283,119.895722925195));
#44079=CARTESIAN_POINT('Ctrl Pts',(34.5434666856064,-84.882007638829,119.737774402003));
#44080=CARTESIAN_POINT('Ctrl Pts',(37.7817188275649,-84.673752227268,119.57982587881));
#44081=CARTESIAN_POINT('Ctrl Pts',(39.726341569515,-87.2714610952442,119.421877355618));
#44082=CARTESIAN_POINT('Ctrl Pts',(38.6142043243961,-90.3198703265441,119.263928832425));
#44083=CARTESIAN_POINT('Ctrl Pts',(35.4536482492415,-91.0550801260151,119.105980309233));
#44084=CARTESIAN_POINT('Ctrl Pts',(33.1102533448528,-88.8104980599669,118.94803178604));
#44085=CARTESIAN_POINT('Ctrl Pts',(33.7087045332523,-85.6212184553168,118.790083262848));
#44086=CARTESIAN_POINT('Ctrl Pts',(36.7064043067714,-84.378864115751,118.632134739655));
#44087=CARTESIAN_POINT('Ctrl Pts',(39.3854294595639,-86.209839944379,118.474186216463));
#44088=CARTESIAN_POINT('Ctrl Pts',(39.3167893606247,-89.4540558401428,118.31623769327));
#44089=CARTESIAN_POINT('Ctrl Pts',(36.5627179019327,-91.1700799205937,118.158289170078));
#44090=CARTESIAN_POINT('Ctrl Pts',(33.6202479128799,-89.8020453415885,118.000340646886));
#44091=CARTESIAN_POINT('Ctrl Pts',(33.1572274418021,-86.5903074494638,117.842392123693));
#44092=CARTESIAN_POINT('Ctrl Pts',(35.5934630674801,-84.4468513102008,117.684443600501));
#44093=CARTESIAN_POINT('Ctrl Pts',(38.7200940429731,-85.3150834151026,117.526495077308));
#44094=CARTESIAN_POINT('Ctrl Pts',(39.7022991549334,-88.4078041206896,117.368546554116));
#44095=CARTESIAN_POINT('Ctrl Pts',(37.6495429007895,-90.920937624079,117.210598030923));
#44096=CARTESIAN_POINT('Ctrl Pts',(34.4229969444023,-90.5759022112363,117.052649507731));
#44097=CARTESIAN_POINT('Ctrl Pts',(32.9480723734746,-87.6855309972138,116.894700984538));
#44098=CARTESIAN_POINT('Ctrl Pts',(34.5620384386605,-84.8704356550963,116.736752461346));
#44099=CARTESIAN_POINT('Ctrl Pts',(37.8015611952165,-84.6829775143284,116.578803938153));
#44100=CARTESIAN_POINT('Ctrl Pts',(39.7294638854033,-87.2931191698622,116.420855414961));
#44101=CARTESIAN_POINT('Ctrl Pts',(38.5977757745388,-90.3343245664954,116.262906891769));
#44102=CARTESIAN_POINT('Ctrl Pts',(35.4325640540056,-91.0492252651816,116.104958368576));
#44103=CARTESIAN_POINT('Ctrl Pts',(33.1036299252483,-88.7896425451441,115.947009845384));
#44104=CARTESIAN_POINT('Ctrl Pts',(33.7225471314815,-85.6042713365387,115.789061322191));
#44105=CARTESIAN_POINT('Ctrl Pts',(36.7281622653295,-84.3811908355222,115.631112798999));
#44106=CARTESIAN_POINT('Ctrl Pts',(39.3953754965844,-86.229330934054,115.473164275806));
#44107=CARTESIAN_POINT('Ctrl Pts',(39.305905708091,-89.473039213436,115.315215752614));
#44108=CARTESIAN_POINT('Ctrl Pts',(36.5408724359755,-91.1713440296798,115.157267229421));
#44109=CARTESIAN_POINT('Ctrl Pts',(33.6072472533796,-89.7844440575038,114.999318706229));
#44110=CARTESIAN_POINT('Ctrl Pts',(33.1648588911862,-86.5697993210237,114.841370183036));
#44111=CARTESIAN_POINT('Ctrl Pts',(35.6148074227622,-84.4420304338062,114.683421659844));
#44112=CARTESIAN_POINT('Ctrl Pts',(38.735799026344,-85.3303207327256,114.525473136651));
#44113=CARTESIAN_POINT('Ctrl Pts',(39.6981255356329,-88.4292844198803,114.367524613459));
#44114=CARTESIAN_POINT('Ctrl Pts',(37.6292747724943,-90.9291853708469,114.209576090266));
#44115=CARTESIAN_POINT('Ctrl Pts',(34.4050108026144,-90.5634394244347,114.051627567074));
#44116=CARTESIAN_POINT('Ctrl Pts',(32.9486757059274,-87.6636573065954,113.893679043881));
#44117=CARTESIAN_POINT('Ctrl Pts',(34.5806842221695,-84.8589832706875,113.735730520689));
#44118=CARTESIAN_POINT('Ctrl Pts',(37.8213438649595,-84.6923299647638,113.577781997497));
#44119=CARTESIAN_POINT('Ctrl Pts',(39.7324470963873,-87.3147968727741,113.419833474304));
#44120=CARTESIAN_POINT('Ctrl Pts',(38.5812547400947,-90.348673007951,113.261884951112));
#44121=CARTESIAN_POINT('Ctrl Pts',(35.4115178935994,-91.0432351497015,113.103936427919));
#44122=CARTESIAN_POINT('Ctrl Pts',(33.0971405524303,-88.7687449282526,112.945987904727));
#44123=CARTESIAN_POINT('Ctrl Pts',(33.7364982632203,-85.5874134518995,112.788039381534));
#44124=CARTESIAN_POINT('Ctrl Pts',(36.7499048347821,-84.3836572144279,112.630090858342));
#44125=CARTESIAN_POINT('Ctrl Pts',(39.4051961772984,-86.2488853857627,112.472142335149));
#44126=CARTESIAN_POINT('Ctrl Pts',(39.2949003875455,-89.4919523113047,112.314193811957));
#44127=CARTESIAN_POINT('Ctrl Pts',(36.5190193035974,-91.1724678430876,112.156245288764));
#44128=CARTESIAN_POINT('Ctrl Pts',(33.5943598796632,-89.766759659012,111.998296765572));
#44129=CARTESIAN_POINT('Ctrl Pts',(33.1726218659282,-86.5493406168999,111.840348242379));
#44130=CARTESIAN_POINT('Ctrl Pts',(35.6361822928647,-84.437346708853,111.682399719187));
#44131=CARTESIAN_POINT('Ctrl Pts',(38.7514058471714,-85.3456585779148,111.524451195994));
#44132=CARTESIAN_POINT('Ctrl Pts',(39.693814077403,-88.4507374774469,111.366502672802));
#44133=CARTESIAN_POINT('Ctrl Pts',(37.6089541032529,-90.9373028059837,111.208554149609));
#44134=CARTESIAN_POINT('Ctrl Pts',(34.3871050551461,-90.5508614055361,111.050605626417));
#44135=CARTESIAN_POINT('Ctrl Pts',(32.9494194768651,-87.6417879409515,110.892657103225));
#44136=CARTESIAN_POINT('Ctrl Pts',(34.5994031570616,-84.8476508467996,110.734708580032));
#44137=CARTESIAN_POINT('Ctrl Pts',(37.8410660747743,-84.7018092471248,110.57676005684));
#44138=CARTESIAN_POINT('Ctrl Pts',(39.7352910534652,-87.3364932835156,110.418811533647));
#44139=CARTESIAN_POINT('Ctrl Pts',(38.5646419147283,-90.3629150730701,110.260863010455));
#44140=CARTESIAN_POINT('Ctrl Pts',(35.39051062995,-91.0371100183091,110.102914487262));
#44141=CARTESIAN_POINT('Ctrl Pts',(33.0907854961891,-88.7478060780943,109.94496596407));
#44142=CARTESIAN_POINT('Ctrl Pts',(33.7505573533824,-85.5706454863716,109.787017440877));
#44143=CARTESIAN_POINT('Ctrl Pts',(36.7716311161658,-84.3862631691886,109.629068917685));
#44144=CARTESIAN_POINT('Ctrl Pts',(39.4148911031094,-86.2685024565476,109.471120394492));
#44145=CARTESIAN_POINT('Ctrl Pts',(39.2837738392237,-89.510794428962,109.3131718713));
#44146=CARTESIAN_POINT('Ctrl Pts',(36.49715943384,-91.173451160537,109.155223348107));
#44147=CARTESIAN_POINT('Ctrl Pts',(33.581586265275,-89.7489931916678,108.997274824915));
#44148=CARTESIAN_POINT('Ctrl Pts',(33.1805161648761,-86.5289315299698,108.839326301722));
#44149=CARTESIAN_POINT('Ctrl Pts',(35.6575865519554,-84.4328016663219,108.68137777853));
#44150=CARTESIAN_POINT('Ctrl Pts',(38.7669143648894,-85.361093567208,108.523429255338));
#44151=CARTESIAN_POINT('Ctrl Pts',(39.689363923874,-88.4721680660194,108.365480732145));
#44152=CARTESIAN_POINT('Ctrl Pts',(37.5885838573921,-90.9452779618979,108.207532208953));
#44153=CARTESIAN_POINT('Ctrl Pts',(34.3692760674367,-90.5381925942059,108.04958368576));
#44154=CARTESIAN_POINT('Ctrl Pts',(32.9503126475537,-87.6198746123785,107.891635162568));
#44155=CARTESIAN_POINT('Ctrl Pts',(34.6181759813229,-84.836540000701,107.733686639375));
#44156=CARTESIAN_POINT('Ctrl Pts',(37.8607650345966,-84.7112069732929,107.575738116183));
#44157=CARTESIAN_POINT('Ctrl Pts',(39.7379174836951,-87.3586352647822,107.41778959299));
#44158=CARTESIAN_POINT('Ctrl Pts',(38.5480989806468,-90.3761706256272,107.259841069798));
#44159=CARTESIAN_POINT('Ctrl Pts',(35.3692208814569,-91.0326717512034,107.101892546605));
#44160=CARTESIAN_POINT('Ctrl Pts',(33.0853013802918,-88.7230897340364,106.943944023413));
#44161=CARTESIAN_POINT('Ctrl Pts',(33.5388501325603,-86.6178778692287,106.838645007951));
#44162=CARTESIAN_POINT('Ctrl Pts',(34.159728970665,-85.8916921494928,106.78599550022));
#44163=CARTESIAN_POINT('Ctrl Pts',(35.6568596485224,-90.3796877745108,122.21400449978));
#44164=CARTESIAN_POINT('Ctrl Pts',(34.7930798529405,-90.1487627841411,122.161354992049));
#44165=CARTESIAN_POINT('Ctrl Pts',(33.3273361373066,-88.7656055436304,122.056055976587));
#44166=CARTESIAN_POINT('Ctrl Pts',(33.8644459018257,-85.7737212648049,121.898107453395));
#44167=CARTESIAN_POINT('Ctrl Pts',(36.6640650799205,-84.5949265943767,121.740158930202));
#44168=CARTESIAN_POINT('Ctrl Pts',(39.1812506391896,-86.2913939754508,121.58221040701));
#44169=CARTESIAN_POINT('Ctrl Pts',(39.1369374747261,-89.3282074867557,121.424261883817));
#44170=CARTESIAN_POINT('Ctrl Pts',(36.5697516720493,-90.9504220402305,121.266313360625));
#44171=CARTESIAN_POINT('Ctrl Pts',(33.8080368390094,-89.6879830515605,121.108364837433));
#44172=CARTESIAN_POINT('Ctrl Pts',(33.3553889938573,-86.6851369565202,120.95041631424));
#44173=CARTESIAN_POINT('Ctrl Pts',(35.6223885602353,-84.6646522338046,120.792467791047));
#44174=CARTESIAN_POINT('Ctrl Pts',(38.5535292276782,-85.4583537605072,120.634519267855));
#44175=CARTESIAN_POINT('Ctrl Pts',(39.491277087121,-88.3466588931682,120.476570744662));
#44176=CARTESIAN_POINT('Ctrl Pts',(37.5853841587796,-90.7108085967037,120.31862222147));
#44177=CARTESIAN_POINT('Ctrl Pts',(34.5638755726478,-90.4073102624978,120.160673698277));
#44178=CARTESIAN_POINT('Ctrl Pts',(33.1662564168983,-87.7113317243892,120.002725175085));
#44179=CARTESIAN_POINT('Ctrl Pts',(34.659707832854,-85.0672370992777,119.844776651893));
#44180=CARTESIAN_POINT('Ctrl Pts',(37.6901616955201,-84.8723454142823,119.6868281287));
#44181=CARTESIAN_POINT('Ctrl Pts',(39.5099982126997,-87.3033595935177,119.528879605508));
#44182=CARTESIAN_POINT('Ctrl Pts',(38.4692266907368,-90.1561527439587,119.370931082315));
#44183=CARTESIAN_POINT('Ctrl Pts',(35.5114831469213,-90.8441842124806,119.212982559123));
#44184=CARTESIAN_POINT('Ctrl Pts',(33.3184636325538,-88.7436367276228,119.05503403593));
#44185=CARTESIAN_POINT('Ctrl Pts',(33.8785122748457,-85.7590128400003,118.897085512738));
#44186=CARTESIAN_POINT('Ctrl Pts',(36.6838499877638,-84.5963802400384,118.739136989545));
#44187=CARTESIAN_POINT('Ctrl Pts',(39.1909623948755,-86.3098625536665,118.581188466353));
#44188=CARTESIAN_POINT('Ctrl Pts',(39.1267269234404,-89.3458974767205,118.42323994316));
#44189=CARTESIAN_POINT('Ctrl Pts',(36.5493839235208,-90.9518044830492,118.265291419968));
#44190=CARTESIAN_POINT('Ctrl Pts',(33.7957319059508,-89.6715565306153,118.107342896775));
#44191=CARTESIAN_POINT('Ctrl Pts',(33.3624234069336,-86.6659155013242,117.949394373583));
#44192=CARTESIAN_POINT('Ctrl Pts',(35.6423260638452,-84.6600047037924,117.79144585039));
#44193=CARTESIAN_POINT('Ctrl Pts',(38.5683214778662,-85.4725224512211,117.633497327198));
#44194=CARTESIAN_POINT('Ctrl Pts',(39.4874985971841,-88.3667836135794,117.475548804005));
#44195=CARTESIAN_POINT('Ctrl Pts',(37.5664674832449,-90.718649619954,117.317600280813));
#44196=CARTESIAN_POINT('Ctrl Pts',(34.5469686215258,-90.3957550911254,117.159651757621));
#44197=CARTESIAN_POINT('Ctrl Pts',(33.1666897960462,-87.6908586759945,117.001703234428));
#44198=CARTESIAN_POINT('Ctrl Pts',(34.6770878385831,-85.0564076884523,116.843754711236));
#44199=CARTESIAN_POINT('Ctrl Pts',(37.7087307806494,-84.8809787156995,116.685806188043));
#44200=CARTESIAN_POINT('Ctrl Pts',(39.5129201699252,-87.3236278718996,116.527857664851));
#44201=CARTESIAN_POINT('Ctrl Pts',(38.4538523590942,-90.169679456942,116.369909141658));
#44202=CARTESIAN_POINT('Ctrl Pts',(35.4917519221453,-90.8387050574149,116.211960618466));
#44203=CARTESIAN_POINT('Ctrl Pts',(33.3122652370477,-88.7241195088633,116.054012095273));
#44204=CARTESIAN_POINT('Ctrl Pts',(33.8914665950882,-85.7431532159467,115.896063572081));
#44205=CARTESIAN_POINT('Ctrl Pts',(36.7042117405445,-84.5985576544611,115.738115048888));
#44206=CARTESIAN_POINT('Ctrl Pts',(39.200270195808,-86.3281028087049,115.580166525696));
#44207=CARTESIAN_POINT('Ctrl Pts',(39.1165416736776,-89.3636626890636,115.422218002503));
#44208=CARTESIAN_POINT('Ctrl Pts',(36.528940278681,-90.9529874743961,115.264269479311));
#44209=CARTESIAN_POINT('Ctrl Pts',(33.7835654973227,-89.6550847189701,115.106320956118));
#44210=CARTESIAN_POINT('Ctrl Pts',(33.3695651470607,-86.6467233772021,114.948372432926));
#44211=CARTESIAN_POINT('Ctrl Pts',(35.662300754226,-84.6554931824991,114.790423909734));
#44212=CARTESIAN_POINT('Ctrl Pts',(38.5830186742033,-85.4867819918694,114.632475386541));
#44213=CARTESIAN_POINT('Ctrl Pts',(39.4835927985692,-88.3868855243633,114.474526863349));
#44214=CARTESIAN_POINT('Ctrl Pts',(37.5474999584851,-90.7263681097303,114.316578340156));
#44215=CARTESIAN_POINT('Ctrl Pts',(34.5301366484532,-90.3840920399647,114.158629816964));
#44216=CARTESIAN_POINT('Ctrl Pts',(33.1672544127228,-87.6703886176669,114.000681293771));
#44217=CARTESIAN_POINT('Ctrl Pts',(34.6945371242409,-85.0456902022755,113.842732770579));
#44218=CARTESIAN_POINT('Ctrl Pts',(37.7272439986783,-84.889731020432,113.684784247386));
#44219=CARTESIAN_POINT('Ctrl Pts',(39.5157119485926,-87.3439145190299,113.526835724194));
#44220=CARTESIAN_POINT('Ctrl Pts',(38.4383914775904,-90.1831071605076,113.368887201001));
#44221=CARTESIAN_POINT('Ctrl Pts',(35.4720562915084,-90.8330993269778,113.210938677809));
#44222=CARTESIAN_POINT('Ctrl Pts',(33.3061922865607,-88.7045628897205,113.052990154617));
#44223=CARTESIAN_POINT('Ctrl Pts',(33.9045224842572,-85.7273770998871,112.895041631424));
#44224=CARTESIAN_POINT('Ctrl Pts',(36.724559091737,-84.6008657661072,112.737093108232));
#44225=CARTESIAN_POINT('Ctrl Pts',(39.2094606845344,-86.3464024534252,112.579144585039));
#44226=CARTESIAN_POINT('Ctrl Pts',(39.1062425633258,-89.3813621355486,112.421196061847));
#44227=CARTESIAN_POINT('Ctrl Pts',(36.5084894593737,-90.9540391728226,112.263247538654));
#44228=CARTESIAN_POINT('Ctrl Pts',(33.7715051049423,-89.6385351263598,112.105299015462));
#44229=CARTESIAN_POINT('Ctrl Pts',(33.3768299725781,-86.6275775058433,111.947350492269));
#44230=CARTESIAN_POINT('Ctrl Pts',(35.6823040012946,-84.6511100116545,111.789401969077));
#44231=CARTESIAN_POINT('Ctrl Pts',(38.5976240070764,-85.5011356092412,111.631453445884));
#44232=CARTESIAN_POINT('Ctrl Pts',(39.4795580061338,-88.4069619416151,111.473504922692));
#44233=CARTESIAN_POINT('Ctrl Pts',(37.5284832643257,-90.7339646499585,111.315556399499));
#44234=CARTESIAN_POINT('Ctrl Pts',(34.5133799108057,-90.3723211511379,111.157607876307));
#44235=CARTESIAN_POINT('Ctrl Pts',(33.1679504559622,-87.6499226067807,110.999659353114));
#44236=CARTESIAN_POINT('Ctrl Pts',(34.7120548671658,-85.0350849787663,110.841710829922));
#44237=CARTESIAN_POINT('Ctrl Pts',(37.7457006364858,-84.8986020182997,110.683762306729));
#44238=CARTESIAN_POINT('Ctrl Pts',(39.5183734092616,-87.3642186735107,110.525813783537));
#44239=CARTESIAN_POINT('Ctrl Pts',(38.4228446953775,-90.1964353138941,110.367865260344));
#44240=CARTESIAN_POINT('Ctrl Pts',(35.4523970616278,-90.8273672445848,110.209916737152));
#44241=CARTESIAN_POINT('Ctrl Pts',(33.3002450335707,-88.6849676832447,110.051968213959));
#44242=CARTESIAN_POINT('Ctrl Pts',(33.9176794041694,-85.7116851328398,109.894019690767));
#44243=CARTESIAN_POINT('Ctrl Pts',(36.744891200064,-84.6033044970411,109.736071167575));
#44244=CARTESIAN_POINT('Ctrl Pts',(39.2185334880359,-86.3647606989627,109.578122644382));
#44245=CARTESIAN_POINT('Ctrl Pts',(39.0958300043706,-89.3989951566143,109.42017412119));
#44246=CARTESIAN_POINT('Ctrl Pts',(36.488032335024,-90.9549593909009,109.262225597997));
#44247=CARTESIAN_POINT('Ctrl Pts',(33.7595511719668,-89.6219087312464,109.104277074805));
#44248=CARTESIAN_POINT('Ctrl Pts',(33.3842176952418,-86.6084780677483,108.946328551612));
#44249=CARTESIAN_POINT('Ctrl Pts',(35.7023347514634,-84.6468566239965,108.78838002842));
#44250=CARTESIAN_POINT('Ctrl Pts',(38.6121373449396,-85.5155801369902,108.630431505227));
#44251=CARTESIAN_POINT('Ctrl Pts',(39.4753934184612,-88.4270173317057,108.472482982035));
#44252=CARTESIAN_POINT('Ctrl Pts',(37.5094201748731,-90.741428041006,108.314534458842));
#44253=CARTESIAN_POINT('Ctrl Pts',(34.496695007252,-90.3604652960198,108.15658593565));
#44254=CARTESIAN_POINT('Ctrl Pts',(33.1687863119872,-87.6294154540617,107.998637412457));
#44255=CARTESIAN_POINT('Ctrl Pts',(34.7296230413851,-85.0246871144243,107.840688889265));
#44256=CARTESIAN_POINT('Ctrl Pts',(37.7641355162503,-84.9073966934263,107.682740366073));
#44257=CARTESIAN_POINT('Ctrl Pts',(39.5208313017561,-87.3849398063052,107.52479184288));
#44258=CARTESIAN_POINT('Ctrl Pts',(38.4073633195336,-90.2088402591199,107.366843319688));
#44259=CARTESIAN_POINT('Ctrl Pts',(35.4324734739243,-90.823213780585,107.208894796495));
#44260=CARTESIAN_POINT('Ctrl Pts',(33.2951128327798,-88.6618373842322,107.050946273303));
#44261=CARTESIAN_POINT('Ctrl Pts',(33.7195574121287,-86.6917167303234,106.945647257841));
#44262=CARTESIAN_POINT('Ctrl Pts',(34.300594524342,-86.0121302673448,106.89299775011));
#44263=CARTESIAN_POINT('Ctrl Pts',(35.7047260767084,-90.2006423906073,122.321006749669));
#44264=CARTESIAN_POINT('Ctrl Pts',(34.9001756782213,-89.9855519312415,122.268357241939));
#44265=CARTESIAN_POINT('Ctrl Pts',(33.5349380371872,-88.6972378091528,122.163058226477));
#44266=CARTESIAN_POINT('Ctrl Pts',(34.0352181748859,-85.9105070925183,122.005109703285));
#44267=CARTESIAN_POINT('Ctrl Pts',(36.642867412422,-84.8125423951751,121.847161180092));
#44268=CARTESIAN_POINT('Ctrl Pts',(38.9874495097741,-86.3926829754995,121.6892126569));
#44269=CARTESIAN_POINT('Ctrl Pts',(38.9461748998449,-89.2212621262834,121.531264133707));
#44270=CARTESIAN_POINT('Ctrl Pts',(36.5550210767314,-90.7322413968164,121.373315610515));
#44271=CARTESIAN_POINT('Ctrl Pts',(33.9826770825852,-89.5563678737322,121.215367087322));
#44272=CARTESIAN_POINT('Ctrl Pts',(33.5610673088279,-86.7594269928302,121.05741856413));
#44273=CARTESIAN_POINT('Ctrl Pts',(35.672618671604,-84.8774869461745,120.899470040937));
#44274=CARTESIAN_POINT('Ctrl Pts',(38.4027709674495,-85.6167643440188,120.741521517745));
#44275=CARTESIAN_POINT('Ctrl Pts',(39.2762174382445,-88.3070183385212,120.583572994552));
#44276=CARTESIAN_POINT('Ctrl Pts',(37.5010116244319,-90.5090582516927,120.42562447136));
#44277=CARTESIAN_POINT('Ctrl Pts',(34.6866879398097,-90.2263708040651,120.267675948167));
#44278=CARTESIAN_POINT('Ctrl Pts',(33.3849035562864,-87.71525556585,120.109727424975));
#44279=CARTESIAN_POINT('Ctrl Pts',(34.7759489801016,-85.2524665597263,119.951778901782));
#44280=CARTESIAN_POINT('Ctrl Pts',(37.5986045634753,-85.0709386012965,119.79383037859));
#44281=CARTESIAN_POINT('Ctrl Pts',(39.2936548558844,-87.3352580917912,119.635881855397));
#44282=CARTESIAN_POINT('Ctrl Pts',(38.3242490570776,-89.9924351613731,119.477933332205));
#44283=CARTESIAN_POINT('Ctrl Pts',(35.569318044601,-90.6332882989464,119.319984809013));
#44284=CARTESIAN_POINT('Ctrl Pts',(33.5266739202549,-88.6767753952787,119.16203628582));
#44285=CARTESIAN_POINT('Ctrl Pts',(34.048320016439,-85.8968072246837,119.004087762628));
#44286=CARTESIAN_POINT('Ctrl Pts',(36.6612956687563,-84.8138963643259,118.846139239435));
#44287=CARTESIAN_POINT('Ctrl Pts',(38.996495330187,-86.4098851629539,118.688190716243));
#44288=CARTESIAN_POINT('Ctrl Pts',(38.9366644862561,-89.2377391132981,118.53024219305));
#44289=CARTESIAN_POINT('Ctrl Pts',(36.5360499451088,-90.7335290455047,118.372293669858));
#44290=CARTESIAN_POINT('Ctrl Pts',(33.9712158990217,-89.5410677196422,118.214345146665));
#44291=CARTESIAN_POINT('Ctrl Pts',(33.5676193720652,-86.7415235531845,118.056396623473));
#44292=CARTESIAN_POINT('Ctrl Pts',(35.6911890602102,-84.873158097384,117.89844810028));
#44293=CARTESIAN_POINT('Ctrl Pts',(38.4165489127592,-85.6299614873397,117.740499577088));
#44294=CARTESIAN_POINT('Ctrl Pts',(39.2726980394348,-88.3257631064689,117.582551053895));
#44295=CARTESIAN_POINT('Ctrl Pts',(37.4833920657004,-90.5163616158289,117.424602530703));
#44296=CARTESIAN_POINT('Ctrl Pts',(34.6709402986493,-90.2156079710144,117.26665400751));
#44297=CARTESIAN_POINT('Ctrl Pts',(33.3853072186179,-87.6961863547752,117.108705484318));
#44298=CARTESIAN_POINT('Ctrl Pts',(34.7921372385056,-85.2423797218082,116.950756961126));
#44299=CARTESIAN_POINT('Ctrl Pts',(37.6159003660824,-85.0789799170705,116.792808437933));
#44300=CARTESIAN_POINT('Ctrl Pts',(39.2963764544471,-87.3541365739369,116.634859914741));
#44301=CARTESIAN_POINT('Ctrl Pts',(38.3099289436496,-90.0050343473886,116.476911391548));
#44302=CARTESIAN_POINT('Ctrl Pts',(35.5509397902851,-90.6281848496482,116.318962868356));
#44303=CARTESIAN_POINT('Ctrl Pts',(33.5209005488471,-88.6585964725826,116.161014345163));
#44304=CARTESIAN_POINT('Ctrl Pts',(34.0603860586949,-85.8820350953548,116.003065821971));
#44305=CARTESIAN_POINT('Ctrl Pts',(36.6802612157596,-84.8159244733999,115.845117298778));
#44306=CARTESIAN_POINT('Ctrl Pts',(39.0051648950316,-86.4268746833558,115.687168775586));
#44307=CARTESIAN_POINT('Ctrl Pts',(38.9271776392642,-89.2542861646912,115.529220252393));
#44308=CARTESIAN_POINT('Ctrl Pts',(36.5170081213865,-90.7346309191124,115.371271729201));
#44309=CARTESIAN_POINT('Ctrl Pts',(33.9598837412658,-89.5257253804362,115.213323206008));
#44310=CARTESIAN_POINT('Ctrl Pts',(33.5742714029352,-86.7236474333804,115.055374682816));
#44311=CARTESIAN_POINT('Ctrl Pts',(35.7097940856898,-84.8689559311919,114.897426159624));
#44312=CARTESIAN_POINT('Ctrl Pts',(38.4302383220626,-85.6432432510131,114.739477636431));
#44313=CARTESIAN_POINT('Ctrl Pts',(39.2690600615056,-88.3444866288462,114.581529113239));
#44314=CARTESIAN_POINT('Ctrl Pts',(37.4657251444759,-90.5235508486137,114.423580590046));
#44315=CARTESIAN_POINT('Ctrl Pts',(34.655262494292,-90.2047446554949,114.265632066854));
#44316=CARTESIAN_POINT('Ctrl Pts',(33.3858331195181,-87.6771199287383,114.107683543661));
#44317=CARTESIAN_POINT('Ctrl Pts',(34.8083900263124,-85.2323971338635,113.949735020469));
#44318=CARTESIAN_POINT('Ctrl Pts',(37.6331441323971,-85.0871320761002,113.791786497276));
#44319=CARTESIAN_POINT('Ctrl Pts',(39.2989768007979,-87.3730321652858,113.633837974084));
#44320=CARTESIAN_POINT('Ctrl Pts',(38.2955282150861,-90.0175413130639,113.475889450891));
#44321=CARTESIAN_POINT('Ctrl Pts',(35.5325946894174,-90.6229635042544,113.317940927699));
#44322=CARTESIAN_POINT('Ctrl Pts',(33.5152440206911,-88.6403808511882,113.159992404506));
#44323=CARTESIAN_POINT('Ctrl Pts',(34.072546705294,-85.8673407478749,113.002043881314));
#44324=CARTESIAN_POINT('Ctrl Pts',(36.6992133486918,-84.8180743177863,112.844095358121));
#44325=CARTESIAN_POINT('Ctrl Pts',(39.0137251917704,-86.4439195210878,112.686146834929));
#44326=CARTESIAN_POINT('Ctrl Pts',(38.9175847391062,-89.2707719597925,112.528198311736));
#44327=CARTESIAN_POINT('Ctrl Pts',(36.49795961515,-90.7356105025577,112.370249788544));
#44328=CARTESIAN_POINT('Ctrl Pts',(33.9486503302215,-89.5103105937078,112.212301265351));
#44329=CARTESIAN_POINT('Ctrl Pts',(33.581038079228,-86.7058143947865,112.054352742159));
#44330=CARTESIAN_POINT('Ctrl Pts',(35.7284257097246,-84.8648733144562,111.896404218967));
#44331=CARTESIAN_POINT('Ctrl Pts',(38.4438421669814,-85.6566126405671,111.738455695774));
#44332=CARTESIAN_POINT('Ctrl Pts',(39.2653019348646,-88.3631864057835,111.580507172582));
#44333=CARTESIAN_POINT('Ctrl Pts',(37.4480124253985,-90.5306264939331,111.422558649389));
#44334=CARTESIAN_POINT('Ctrl Pts',(34.6396547664653,-90.1937808967399,111.264610126197));
#44335=CARTESIAN_POINT('Ctrl Pts',(33.3864814350593,-87.6580572726099,111.106661603004));
#44336=CARTESIAN_POINT('Ctrl Pts',(34.82470657727,-85.2225191107331,110.948713079812));
#44337=CARTESIAN_POINT('Ctrl Pts',(37.6503351981973,-85.0953947894745,110.790764556619));
#44338=CARTESIAN_POINT('Ctrl Pts',(39.3014557650579,-87.3919440635056,110.632816033427));
#44339=CARTESIAN_POINT('Ctrl Pts',(38.2810474760267,-90.029955554718,110.474867510234));
#44340=CARTESIAN_POINT('Ctrl Pts',(35.5142834933055,-90.6176244708606,110.316918987042));
#44341=CARTESIAN_POINT('Ctrl Pts',(33.5097045709523,-88.622129288395,110.158970463849));
#44342=CARTESIAN_POINT('Ctrl Pts',(34.0848014549563,-85.8527247793081,110.001021940657));
#44343=CARTESIAN_POINT('Ctrl Pts',(36.7181512839622,-84.8203458248934,109.843073417464));
#44344=CARTESIAN_POINT('Ctrl Pts',(39.0221758729624,-86.4610189413778,109.685124894272));
#44345=CARTESIAN_POINT('Ctrl Pts',(38.9078861695176,-89.2871958842667,109.527176371079));
#44346=CARTESIAN_POINT('Ctrl Pts',(36.4789052362081,-90.7364676212647,109.369227847887));
#44347=CARTESIAN_POINT('Ctrl Pts',(33.9375160786586,-89.4948242708249,109.211279324695));
#44348=CARTESIAN_POINT('Ctrl Pts',(33.5879192256074,-86.6880246055271,109.053330801502));
#44349=CARTESIAN_POINT('Ctrl Pts',(35.7470829509713,-84.860911581671,108.89538227831));
#44350=CARTESIAN_POINT('Ctrl Pts',(38.4573603249899,-85.6700667067725,108.737433755117));
#44351=CARTESIAN_POINT('Ctrl Pts',(39.2614229130483,-88.3818665973921,108.579485231925));
#44352=CARTESIAN_POINT('Ctrl Pts',(37.4302564923541,-90.5375781201139,108.421536708732));
#44353=CARTESIAN_POINT('Ctrl Pts',(34.6241139470672,-90.1827379978339,108.26358818554));
#44354=CARTESIAN_POINT('Ctrl Pts',(33.3872599764207,-87.6389562957449,108.105639662347));
#44355=CARTESIAN_POINT('Ctrl Pts',(34.8410701014472,-85.2128342281477,107.947691139155));
#44356=CARTESIAN_POINT('Ctrl Pts',(37.667505997904,-85.1035864135597,107.789742615962));
#44357=CARTESIAN_POINT('Ctrl Pts',(39.3037451198171,-87.4112443478284,107.63179409277));
#44358=CARTESIAN_POINT('Ctrl Pts',(38.2666276584204,-90.0415098926125,107.473845569578));
#44359=CARTESIAN_POINT('Ctrl Pts',(35.4957260663917,-90.6137558099667,107.315897046385));
#44360=CARTESIAN_POINT('Ctrl Pts',(33.5049242852677,-88.6005850344281,107.157948523192));
#44361=CARTESIAN_POINT('Ctrl Pts',(33.9002646916971,-86.7655555914181,107.052649507731));
#44362=CARTESIAN_POINT('Ctrl Pts',(34.441460078019,-86.1325683851967,107.));
#44363=CARTESIAN_POINT('Ctrl Pts',(33.8399315564717,-87.7667938053724,121.112583302492));
#44364=CARTESIAN_POINT('Ctrl Pts',(33.8380186898685,-87.4752409773549,121.094195056371));
#44365=CARTESIAN_POINT('Ctrl Pts',(33.8848899787242,-87.1842829992347,121.07580681025));
#44366=CARTESIAN_POINT('Ctrl Pts',(33.9832608315835,-86.9119271318713,121.05741856413));
#44367=CARTESIAN_POINT('Ctrl Pts',(34.2649177630866,-86.132113643945,121.004769056399));
#44368=CARTESIAN_POINT('Ctrl Pts',(34.9687682173453,-85.5048002950597,120.952119548668));
#44369=CARTESIAN_POINT('Ctrl Pts',(35.7757188271156,-85.3143565202578,120.899470040937));
#44370=CARTESIAN_POINT('Ctrl Pts',(36.5826694368858,-85.1239127454559,120.846820533206));
#44371=CARTESIAN_POINT('Ctrl Pts',(37.4927202021677,-85.3703385447374,120.794171025476));
#44372=CARTESIAN_POINT('Ctrl Pts',(38.0933199966077,-85.9419271101285,120.741521517745));
#44373=CARTESIAN_POINT('Ctrl Pts',(38.6939197910478,-86.5135156755196,120.688872010014));
#44374=CARTESIAN_POINT('Ctrl Pts',(38.9850686146462,-87.4102670070204,120.636222502283));
#44375=CARTESIAN_POINT('Ctrl Pts',(38.8347753908099,-88.225649324966,120.583572994552));
#44376=CARTESIAN_POINT('Ctrl Pts',(38.6844821669737,-89.0410316429117,120.530923486821));
#44377=CARTESIAN_POINT('Ctrl Pts',(38.0927468957028,-89.7750449473022,120.478273979091));
#44378=CARTESIAN_POINT('Ctrl Pts',(37.3278253126303,-90.0949370248928,120.42562447136));
#44379=CARTESIAN_POINT('Ctrl Pts',(36.5629037295579,-90.4148291024835,120.372974963629));
#44380=CARTESIAN_POINT('Ctrl Pts',(35.6247958346838,-90.3205999532743,120.320325455898));
#44381=CARTESIAN_POINT('Ctrl Pts',(34.9387778233262,-89.8549661723005,120.267675948167));
#44382=CARTESIAN_POINT('Ctrl Pts',(34.2651637482346,-89.3977515459945,120.215978399609));
#44383=CARTESIAN_POINT('Ctrl Pts',(33.8346058639746,-88.5824416490861,120.16428085105));
#44384=CARTESIAN_POINT('Ctrl Pts',(33.8333405706013,-87.7682823373648,120.112583302492));
#44385=CARTESIAN_POINT('Ctrl Pts',(35.5611267921506,-90.7377785423179,122.));
#44386=CARTESIAN_POINT('Ctrl Pts',(35.4680767052966,-90.7037404048947,122.));
#44387=CARTESIAN_POINT('Ctrl Pts',(35.3770917836601,-90.664933572561,122.));
#44388=CARTESIAN_POINT('Ctrl Pts',(35.2883805128425,-90.6216863669008,122.));
#44389=CARTESIAN_POINT('Ctrl Pts',(35.197702296709,-90.5774802651747,122.));
#44390=CARTESIAN_POINT('Ctrl Pts',(35.1093990059899,-90.5286340828183,122.));
#44391=CARTESIAN_POINT('Ctrl Pts',(35.0237222209495,-90.4754529263978,122.));
#44392=CARTESIAN_POINT('Ctrl Pts',(34.9412907936686,-90.424286223234,122.));
#44393=CARTESIAN_POINT('Ctrl Pts',(34.861290377545,-90.3691058598076,122.));
#44394=CARTESIAN_POINT('Ctrl Pts',(34.7839779997226,-90.3101535213279,122.));
#44395=CARTESIAN_POINT('Ctrl Pts',(34.7163296691279,-90.2585702251582,122.));
#44396=CARTESIAN_POINT('Ctrl Pts',(34.6507396580929,-90.2040983132303,122.));
#44397=CARTESIAN_POINT('Ctrl Pts',(34.5874047755446,-90.1468869965436,122.));
#44398=CARTESIAN_POINT('Ctrl Pts',(34.5732683536243,-90.1341173618848,122.));
#44399=CARTESIAN_POINT('Ctrl Pts',(34.5592416368608,-90.1212085175659,122.));
#44400=CARTESIAN_POINT('Ctrl Pts',(34.5453463983788,-90.1081806554779,122.));
#44401=CARTESIAN_POINT('Ctrl Pts',(34.4729162970605,-90.040271826693,122.));
#44402=CARTESIAN_POINT('Ctrl Pts',(34.403951882981,-89.9690410838559,122.));
#44403=CARTESIAN_POINT('Ctrl Pts',(34.3386931062104,-89.8947791484553,122.));
#44404=CARTESIAN_POINT('Ctrl Pts',(34.2737933595084,-89.8209257752296,122.));
#44405=CARTESIAN_POINT('Ctrl Pts',(34.2125581016922,-89.7440736737795,122.));
#44406=CARTESIAN_POINT('Ctrl Pts',(34.1552669537762,-89.6644820254102,122.));
#44407=CARTESIAN_POINT('Ctrl Pts',(34.1001040339643,-89.5878470150046,122.));
#44408=CARTESIAN_POINT('Ctrl Pts',(34.0485974753497,-89.5086714751506,122.));
#44409=CARTESIAN_POINT('Ctrl Pts',(34.0010417263708,-89.4271731777542,122.));
#44410=CARTESIAN_POINT('Ctrl Pts',(33.9810953973884,-89.392990310566,122.));
#44411=CARTESIAN_POINT('Ctrl Pts',(33.9618446717128,-89.3583987128521,122.));
#44412=CARTESIAN_POINT('Ctrl Pts',(33.9433138595418,-89.3234141560505,122.));
#44413=CARTESIAN_POINT('Ctrl Pts',(33.9304313294793,-89.2990930631293,122.));
#44414=CARTESIAN_POINT('Ctrl Pts',(33.9178967633415,-89.274582051837,122.));
#44415=CARTESIAN_POINT('Ctrl Pts',(33.9057187949769,-89.2498864153828,122.));
#44416=CARTESIAN_POINT('Ctrl Pts',(33.8978104365748,-89.2338490979749,122.));
#44417=CARTESIAN_POINT('Ctrl Pts',(33.8900513541417,-89.2177313077059,122.));
#44418=CARTESIAN_POINT('Ctrl Pts',(33.8824540881418,-89.2015566837388,122.));
#44419=CARTESIAN_POINT('Ctrl Pts',(33.8403337819923,-89.1118823043832,122.));
#44420=CARTESIAN_POINT('Ctrl Pts',(33.8031123102296,-89.0203243302145,122.));
#44421=CARTESIAN_POINT('Ctrl Pts',(33.7710809567661,-88.9271551245399,122.));
#44422=CARTESIAN_POINT('Ctrl Pts',(33.7412012053114,-88.8402442572872,122.));
#44423=CARTESIAN_POINT('Ctrl Pts',(33.7158379051123,-88.7519305553683,122.));
#44424=CARTESIAN_POINT('Ctrl Pts',(33.6952780341048,-88.662426403845,122.));
#44425=CARTESIAN_POINT('Ctrl Pts',(33.6937975445556,-88.6559813263984,122.));
#44426=CARTESIAN_POINT('Ctrl Pts',(33.6923419845185,-88.6495300750113,122.));
#44427=CARTESIAN_POINT('Ctrl Pts',(33.6909114717731,-88.6430727286702,122.));
#44428=CARTESIAN_POINT('Ctrl Pts',(33.6703052539739,-88.5500560914257,122.));
#44429=CARTESIAN_POINT('Ctrl Pts',(33.6548920629776,-88.4557737818519,122.));
#44430=CARTESIAN_POINT('Ctrl Pts',(33.6445949784327,-88.3606336675157,122.));
#44431=CARTESIAN_POINT('Ctrl Pts',(33.6387984637639,-88.3070766566996,122.));
#44432=CARTESIAN_POINT('Ctrl Pts',(33.6346241089796,-88.2532480069532,122.));
#44433=CARTESIAN_POINT('Ctrl Pts',(33.6320649544127,-88.1992231133509,122.));
#44434=CARTESIAN_POINT('Ctrl Pts',(33.6314040725555,-88.1852716027681,122.));
#44435=CARTESIAN_POINT('Ctrl Pts',(33.6308510273416,-88.1713076039324,122.));
#44436=CARTESIAN_POINT('Ctrl Pts',(33.6304059403149,-88.15734578475,122.));
#44437=CARTESIAN_POINT('Ctrl Pts',(33.627434535562,-88.0641365618572,122.));
#44438=CARTESIAN_POINT('Ctrl Pts',(33.6292622862227,-87.9708690974207,122.));
#44439=CARTESIAN_POINT('Ctrl Pts',(33.6357542976629,-87.877918472349,122.));
#44440=CARTESIAN_POINT('Ctrl Pts',(33.6422571034003,-87.7848132978462,122.));
#44441=CARTESIAN_POINT('Ctrl Pts',(33.6534400713544,-87.6920250375438,122.));
#44442=CARTESIAN_POINT('Ctrl Pts',(33.6692185656195,-87.5999427421327,122.));
#44443=CARTESIAN_POINT('Ctrl Pts',(33.6847714619004,-87.5091770223002,122.));
#44444=CARTESIAN_POINT('Ctrl Pts',(33.7047898729604,-87.4190963800901,122.));
#44445=CARTESIAN_POINT('Ctrl Pts',(33.7292357664442,-87.3300986153128,122.));
#44446=CARTESIAN_POINT('Ctrl Pts',(33.7383345299043,-87.2969736403256,122.));
#44447=CARTESIAN_POINT('Ctrl Pts',(33.7480470433711,-87.2639989962916,122.));
#44448=CARTESIAN_POINT('Ctrl Pts',(33.7583727072738,-87.2311964605871,122.));
#44449=CARTESIAN_POINT('Ctrl Pts',(33.7653671455383,-87.2089765517205,122.));
#44450=CARTESIAN_POINT('Ctrl Pts',(33.7726429420923,-87.1868356298293,122.));
#44451=CARTESIAN_POINT('Ctrl Pts',(33.7802000896882,-87.1647806770501,122.));
#44452=CARTESIAN_POINT('Ctrl Pts',(33.784716145434,-87.1516009164385,122.));
#44453=CARTESIAN_POINT('Ctrl Pts',(33.7893323288939,-87.1384530285915,122.));
#44454=CARTESIAN_POINT('Ctrl Pts',(33.7940451680849,-87.1253476520519,122.));
#44455=CARTESIAN_POINT('Ctrl Pts',(33.8256769306868,-87.0373866284082,122.));
#44456=CARTESIAN_POINT('Ctrl Pts',(33.8616979180992,-86.9512233528443,122.));
#44457=CARTESIAN_POINT('Ctrl Pts',(33.9020435658716,-86.8672720713196,122.));
#44458=CARTESIAN_POINT('Ctrl Pts',(33.9323028017008,-86.8043086101762,122.));
#44459=CARTESIAN_POINT('Ctrl Pts',(33.9649957063116,-86.7425898876219,122.));
#44460=CARTESIAN_POINT('Ctrl Pts',(34.0001110034215,-86.6823061948472,122.));
#44461=CARTESIAN_POINT('Ctrl Pts',(34.0135802871606,-86.6591829912964,122.));
#44462=CARTESIAN_POINT('Ctrl Pts',(34.0274061069814,-86.6362710825671,122.));
#44463=CARTESIAN_POINT('Ctrl Pts',(34.0415883069323,-86.6135818516236,122.));
#44464=CARTESIAN_POINT('Ctrl Pts',(34.051712699879,-86.5973844569652,122.));
#44465=CARTESIAN_POINT('Ctrl Pts',(34.0620195498418,-86.5812994784565,122.));
#44466=CARTESIAN_POINT('Ctrl Pts',(34.0724987247553,-86.5653460621708,122.));
#44467=CARTESIAN_POINT('Ctrl Pts',(34.1196853014102,-86.4935095763133,122.));
#44468=CARTESIAN_POINT('Ctrl Pts',(34.1704068011088,-86.4242665432395,122.));
#44469=CARTESIAN_POINT('Ctrl Pts',(34.2246303322527,-86.3579689632954,122.));
#44470=CARTESIAN_POINT('Ctrl Pts',(34.2734267450191,-86.2983069676984,122.));
#44471=CARTESIAN_POINT('Ctrl Pts',(34.3250598512736,-86.2410304018568,122.));
#44472=CARTESIAN_POINT('Ctrl Pts',(34.3795261720882,-86.1864256058779,122.));
#44473=CARTESIAN_POINT('Ctrl Pts',(34.3986087445119,-86.1672945179254,122.));
#44474=CARTESIAN_POINT('Ctrl Pts',(34.4180392617253,-86.1484916789768,122.));
#44475=CARTESIAN_POINT('Ctrl Pts',(34.4378071488064,-86.1300215764195,122.));
#44476=CARTESIAN_POINT('Origin',(36.3549260746835,-87.7685555885722,114.));
#44477=CARTESIAN_POINT('Origin',(-87.7685555885722,-36.3549260746835,107.));
#44478=CARTESIAN_POINT('Ctrl Pts',(-89.6820215852368,-34.718938871308,107.));
#44479=CARTESIAN_POINT('Ctrl Pts',(-89.7441591022264,-34.7773328792639,
107.));
#44480=CARTESIAN_POINT('Ctrl Pts',(-89.8029212433459,-34.8389807974981,
107.));
#44481=CARTESIAN_POINT('Ctrl Pts',(-89.858296029888,-34.9035061497367,107.));
#44482=CARTESIAN_POINT('Ctrl Pts',(-89.9150258984937,-34.9696105084677,
107.));
#44483=CARTESIAN_POINT('Ctrl Pts',(-89.9682010676987,-35.038735343394,107.));
#44484=CARTESIAN_POINT('Ctrl Pts',(-90.0177797698294,-35.1105221332789,
107.));
#44485=CARTESIAN_POINT('Ctrl Pts',(-90.0307174577489,-35.1292550779578,
107.));
#44486=CARTESIAN_POINT('Ctrl Pts',(-90.0434100690099,-35.1481695083757,
107.));
#44487=CARTESIAN_POINT('Ctrl Pts',(-90.0558564859775,-35.1672594868097,
107.));
#44488=CARTESIAN_POINT('Ctrl Pts',(-90.0660265385985,-35.1828580390446,
107.));
#44489=CARTESIAN_POINT('Ctrl Pts',(-90.0760326568071,-35.1985747060449,
107.));
#44490=CARTESIAN_POINT('Ctrl Pts',(-90.0858653827356,-35.2143916528229,
107.));
#44491=CARTESIAN_POINT('Ctrl Pts',(-90.1333094775083,-35.2907103387503,
107.));
#44492=CARTESIAN_POINT('Ctrl Pts',(-90.1767700081504,-35.3694363854873,
107.));
#44493=CARTESIAN_POINT('Ctrl Pts',(-90.2162122893232,-35.4501772412122,
107.));
#44494=CARTESIAN_POINT('Ctrl Pts',(-90.2480407463799,-35.5153321151888,
107.));
#44495=CARTESIAN_POINT('Ctrl Pts',(-90.2772520626476,-35.5818000994126,
107.));
#44496=CARTESIAN_POINT('Ctrl Pts',(-90.3038108530357,-35.6493927201715,
107.));
#44497=CARTESIAN_POINT('Ctrl Pts',(-90.3144122571216,-35.6763734928431,
107.));
#44498=CARTESIAN_POINT('Ctrl Pts',(-90.3245908384771,-35.7035336109894,
107.));
#44499=CARTESIAN_POINT('Ctrl Pts',(-90.3343435860193,-35.7308616332299,
107.));
#44500=CARTESIAN_POINT('Ctrl Pts',(-90.3395845428334,-35.745547236826,107.));
#44501=CARTESIAN_POINT('Ctrl Pts',(-90.3447021475068,-35.7602805096407,
107.));
#44502=CARTESIAN_POINT('Ctrl Pts',(-90.3496919330262,-35.7750471974551,
107.));
#44503=CARTESIAN_POINT('Ctrl Pts',(-90.379230726078,-35.8624638075913,107.));
#44504=CARTESIAN_POINT('Ctrl Pts',(-90.4043340580788,-35.951161521916,107.));
#44505=CARTESIAN_POINT('Ctrl Pts',(-90.4249693616929,-36.0407425302748,
107.));
#44506=CARTESIAN_POINT('Ctrl Pts',(-90.4459261369105,-36.1317190960213,
107.));
#44507=CARTESIAN_POINT('Ctrl Pts',(-90.4622750877517,-36.2236074967956,
107.));
#44508=CARTESIAN_POINT('Ctrl Pts',(-90.4739402758961,-36.3160242249173,
107.));
#44509=CARTESIAN_POINT('Ctrl Pts',(-90.4855147505546,-36.4077222810838,
107.));
#44510=CARTESIAN_POINT('Ctrl Pts',(-90.492478369332,-36.4999414095043,107.));
#44511=CARTESIAN_POINT('Ctrl Pts',(-90.4947100072084,-36.5923261901315,
107.));
#44512=CARTESIAN_POINT('Ctrl Pts',(-90.4958206266717,-36.6383033339006,
107.));
#44513=CARTESIAN_POINT('Ctrl Pts',(-90.4957584865878,-36.6843217187953,
107.));
#44514=CARTESIAN_POINT('Ctrl Pts',(-90.494503858864,-36.7303382342054,107.));
#44515=CARTESIAN_POINT('Ctrl Pts',(-90.4941340858137,-36.7439005578688,
107.));
#44516=CARTESIAN_POINT('Ctrl Pts',(-90.4936607061271,-36.7574627198223,
107.));
#44517=CARTESIAN_POINT('Ctrl Pts',(-90.4930831583726,-36.7710236163914,
107.));
#44518=CARTESIAN_POINT('Ctrl Pts',(-90.4924626435032,-36.785593386418,107.));
#44519=CARTESIAN_POINT('Ctrl Pts',(-90.491722287192,-36.8001519099739,107.));
#44520=CARTESIAN_POINT('Ctrl Pts',(-90.4908620410004,-36.8146952575918,
107.));
#44521=CARTESIAN_POINT('Ctrl Pts',(-90.4852102271911,-36.9102449894035,
107.));
#44522=CARTESIAN_POINT('Ctrl Pts',(-90.4743857795999,-37.0051729993,107.));
#44523=CARTESIAN_POINT('Ctrl Pts',(-90.458318244262,-37.0990836424695,107.));
#44524=CARTESIAN_POINT('Ctrl Pts',(-90.4559379034287,-37.1129961271111,
107.));
#44525=CARTESIAN_POINT('Ctrl Pts',(-90.4534424042812,-37.1268863168099,
107.));
#44526=CARTESIAN_POINT('Ctrl Pts',(-90.4508314252251,-37.1407529558637,
107.));
#44527=CARTESIAN_POINT('Ctrl Pts',(-90.433885764654,-37.2307496021864,107.));
#44528=CARTESIAN_POINT('Ctrl Pts',(-90.4120802238171,-37.3197540702518,
107.));
#44529=CARTESIAN_POINT('Ctrl Pts',(-90.385717351839,-37.4075341124589,107.));
#44530=CARTESIAN_POINT('Ctrl Pts',(-90.3587585371945,-37.4972984556344,
107.));
#44531=CARTESIAN_POINT('Ctrl Pts',(-90.3270338130467,-37.5857830902758,
107.));
#44532=CARTESIAN_POINT('Ctrl Pts',(-90.2908124720421,-37.6727359721983,
107.));
#44533=CARTESIAN_POINT('Ctrl Pts',(-90.2783223243084,-37.7027197969535,
107.));
#44534=CARTESIAN_POINT('Ctrl Pts',(-90.2652970490218,-37.7325214049852,
107.));
#44535=CARTESIAN_POINT('Ctrl Pts',(-90.2517463158813,-37.7621301223255,
107.));
#44536=CARTESIAN_POINT('Ctrl Pts',(-90.245055229323,-37.7767503268968,107.));
#44537=CARTESIAN_POINT('Ctrl Pts',(-90.2382360157698,-37.7913234975559,
107.));
#44538=CARTESIAN_POINT('Ctrl Pts',(-90.2312897801449,-37.8058483267084,
107.));
#44539=CARTESIAN_POINT('Ctrl Pts',(-90.2257960066309,-37.8173360052153,
107.));
#44540=CARTESIAN_POINT('Ctrl Pts',(-90.220223218393,-37.8287924197308,107.));
#44541=CARTESIAN_POINT('Ctrl Pts',(-90.2145765560449,-37.840207994202,107.));
#44542=CARTESIAN_POINT('Ctrl Pts',(-90.1718526024324,-37.926580871506,107.));
#44543=CARTESIAN_POINT('Ctrl Pts',(-90.1248377921968,-38.0107554256567,
107.));
#44544=CARTESIAN_POINT('Ctrl Pts',(-90.0738747799873,-38.0924820198704,
107.));
#44545=CARTESIAN_POINT('Ctrl Pts',(-90.0219010618754,-38.1758294278385,
107.));
#44546=CARTESIAN_POINT('Ctrl Pts',(-89.9658206725573,-38.2566315879641,
107.));
#44547=CARTESIAN_POINT('Ctrl Pts',(-89.9059420505749,-38.3346166852078,
107.));
#44548=CARTESIAN_POINT('Ctrl Pts',(-89.8455766045364,-38.4132358154351,
107.));
#44549=CARTESIAN_POINT('Ctrl Pts',(-89.7813504553299,-38.4889927268592,
107.));
#44550=CARTESIAN_POINT('Ctrl Pts',(-89.7135302947394,-38.5615896410769,
107.));
#44551=CARTESIAN_POINT('Ctrl Pts',(-89.6765296427799,-38.6011963470019,
107.));
#44552=CARTESIAN_POINT('Ctrl Pts',(-89.6384584284845,-38.6398620818104,
107.));
#44553=CARTESIAN_POINT('Ctrl Pts',(-89.5993546106677,-38.6775347115697,
107.));
#44554=CARTESIAN_POINT('Ctrl Pts',(-89.5873868339339,-38.6890644712479,
107.));
#44555=CARTESIAN_POINT('Ctrl Pts',(-89.5753223113711,-38.7005011869721,
107.));
#44556=CARTESIAN_POINT('Ctrl Pts',(-89.5631620681302,-38.7118433021718,
107.));
#44557=CARTESIAN_POINT('Ctrl Pts',(-89.5526162948829,-38.7216795671767,
107.));
#44558=CARTESIAN_POINT('Ctrl Pts',(-89.5419996446347,-38.7314435662217,
107.));
#44559=CARTESIAN_POINT('Ctrl Pts',(-89.531321897357,-38.7411263062964,107.));
#44560=CARTESIAN_POINT('Ctrl Pts',(-89.4557474041478,-38.8096583809928,
107.));
#44561=CARTESIAN_POINT('Ctrl Pts',(-89.3769961916351,-38.8742341081678,
107.));
#44562=CARTESIAN_POINT('Ctrl Pts',(-89.2953956054652,-38.9345717165341,
107.));
#44563=CARTESIAN_POINT('Ctrl Pts',(-89.2136908377845,-38.9949863594351,
107.));
#44564=CARTESIAN_POINT('Ctrl Pts',(-89.1291288426842,-39.051152893352,107.));
#44565=CARTESIAN_POINT('Ctrl Pts',(-89.0419929468074,-39.102762666281,107.));
#44566=CARTESIAN_POINT('Ctrl Pts',(-88.9565892880383,-39.1533464514366,
107.));
#44567=CARTESIAN_POINT('Ctrl Pts',(-88.8687123840793,-39.1995535268664,
107.));
#44568=CARTESIAN_POINT('Ctrl Pts',(-88.7785949084889,-39.2410574806785,
107.));
#44569=CARTESIAN_POINT('Ctrl Pts',(-88.7382460236614,-39.2596403164856,
107.));
#44570=CARTESIAN_POINT('Ctrl Pts',(-88.6974475743233,-39.2772797819957,
107.));
#44571=CARTESIAN_POINT('Ctrl Pts',(-88.6562186908398,-39.2939436323372,
107.));
#44572=CARTESIAN_POINT('Ctrl Pts',(-88.6257990519939,-39.3062386126117,
107.));
#44573=CARTESIAN_POINT('Ctrl Pts',(-88.595145068204,-39.3180024402984,107.));
#44574=CARTESIAN_POINT('Ctrl Pts',(-88.5642690084499,-39.3292377960812,
107.));
#44575=CARTESIAN_POINT('Ctrl Pts',(-86.97475630604,-39.3241490284294,107.));
#44576=CARTESIAN_POINT('Ctrl Pts',(-86.8799223996403,-39.2894583618481,
107.));
#44577=CARTESIAN_POINT('Ctrl Pts',(-86.7871316469804,-39.2497768123283,
107.));
#44578=CARTESIAN_POINT('Ctrl Pts',(-86.6966249712659,-39.2054247302432,
107.));
#44579=CARTESIAN_POINT('Ctrl Pts',(-86.6048454170698,-39.1604488841048,
107.));
#44580=CARTESIAN_POINT('Ctrl Pts',(-86.515413969275,-39.1106695078317,107.));
#44581=CARTESIAN_POINT('Ctrl Pts',(-86.4286158841239,-39.0563799760475,
107.));
#44582=CARTESIAN_POINT('Ctrl Pts',(-86.4041028655354,-39.0410478371015,
107.));
#44583=CARTESIAN_POINT('Ctrl Pts',(-86.3798001181766,-39.0253557682571,
107.));
#44584=CARTESIAN_POINT('Ctrl Pts',(-86.3557146636652,-39.009309921962,107.));
#44585=CARTESIAN_POINT('Ctrl Pts',(-86.3363851178117,-38.9964324850188,
107.));
#44586=CARTESIAN_POINT('Ctrl Pts',(-86.3171934197275,-38.9833255643263,
107.));
#44587=CARTESIAN_POINT('Ctrl Pts',(-86.2981624849453,-38.9700061049476,
107.));
#44588=CARTESIAN_POINT('Ctrl Pts',(-86.215455383929,-38.912120673416,107.));
#44589=CARTESIAN_POINT('Ctrl Pts',(-86.1357031424774,-38.8501730961047,
107.));
#44590=CARTESIAN_POINT('Ctrl Pts',(-86.0591721222282,-38.7844607338344,
107.));
#44591=CARTESIAN_POINT('Ctrl Pts',(-86.0001789319485,-38.7338070005048,
107.));
#44592=CARTESIAN_POINT('Ctrl Pts',(-85.943100409209,-38.6809153408518,107.));
#44593=CARTESIAN_POINT('Ctrl Pts',(-85.8880761219746,-38.6259101852584,
107.));
#44594=CARTESIAN_POINT('Ctrl Pts',(-85.8587873766259,-38.5966316234449,
107.));
#44595=CARTESIAN_POINT('Ctrl Pts',(-85.8300809343862,-38.5667540958584,
107.));
#44596=CARTESIAN_POINT('Ctrl Pts',(-85.8019798655343,-38.5362955369464,
107.));
#44597=CARTESIAN_POINT('Ctrl Pts',(-85.7923438617004,-38.5258511374114,
107.));
#44598=CARTESIAN_POINT('Ctrl Pts',(-85.7827797735159,-38.5153391259719,
107.));
#44599=CARTESIAN_POINT('Ctrl Pts',(-85.7732951676183,-38.5047678383442,
107.));
#44600=CARTESIAN_POINT('Ctrl Pts',(-85.7074979757394,-38.4314320510738,
107.));
#44601=CARTESIAN_POINT('Ctrl Pts',(-85.6454329342682,-38.3551496402824,
107.));
#44602=CARTESIAN_POINT('Ctrl Pts',(-85.5873438118379,-38.276199164193,107.));
#44603=CARTESIAN_POINT('Ctrl Pts',(-85.5297811470021,-38.197964210666,107.));
#44604=CARTESIAN_POINT('Ctrl Pts',(-85.4761222269613,-38.1171085490677,
107.));
#44605=CARTESIAN_POINT('Ctrl Pts',(-85.4266499956721,-38.0338808467508,
107.));
#44606=CARTESIAN_POINT('Ctrl Pts',(-85.3785920566061,-37.9530324244677,
107.));
#44607=CARTESIAN_POINT('Ctrl Pts',(-85.3344846447919,-37.8699449457437,
107.));
#44608=CARTESIAN_POINT('Ctrl Pts',(-85.2946349115255,-37.7848360318206,
107.));
#44609=CARTESIAN_POINT('Ctrl Pts',(-85.273830494568,-37.7404030786508,107.));
#44610=CARTESIAN_POINT('Ctrl Pts',(-85.2541873635994,-37.6954190560072,
107.));
#44611=CARTESIAN_POINT('Ctrl Pts',(-85.2357549187479,-37.6499146945858,
107.));
#44612=CARTESIAN_POINT('Ctrl Pts',(-85.2286968353362,-37.6324903332981,
107.));
#44613=CARTESIAN_POINT('Ctrl Pts',(-85.2218163113607,-37.6149896785989,
107.));
#44614=CARTESIAN_POINT('Ctrl Pts',(-85.2151162824064,-37.597414464605,107.));
#44615=CARTESIAN_POINT('Ctrl Pts',(-85.2098745474931,-37.5836645818168,
107.));
#44616=CARTESIAN_POINT('Ctrl Pts',(-85.2047431886565,-37.5698685631309,
107.));
#44617=CARTESIAN_POINT('Ctrl Pts',(-85.1997287410707,-37.5560419518582,
107.));
#44618=CARTESIAN_POINT('Ctrl Pts',(-85.1680450550389,-37.4686787871323,
107.));
#44619=CARTESIAN_POINT('Ctrl Pts',(-85.1409701945636,-37.3799546783075,
107.));
#44620=CARTESIAN_POINT('Ctrl Pts',(-85.1187554157791,-37.2900931766429,
107.));
#44621=CARTESIAN_POINT('Ctrl Pts',(-85.1137714424873,-37.2699323941024,
107.));
#44622=CARTESIAN_POINT('Ctrl Pts',(-85.1090323031209,-37.2497143216185,
107.));
#44623=CARTESIAN_POINT('Ctrl Pts',(-85.1045411958224,-37.2294414281565,
107.));
#44624=CARTESIAN_POINT('Ctrl Pts',(-85.0841754438542,-37.1375102645286,
107.));
#44625=CARTESIAN_POINT('Ctrl Pts',(-85.0689059044723,-37.0444514795905,
107.));
#44626=CARTESIAN_POINT('Ctrl Pts',(-85.0586227526078,-36.950656660602,107.));
#44627=CARTESIAN_POINT('Ctrl Pts',(-85.0478888926271,-36.8527508368625,
107.));
#44628=CARTESIAN_POINT('Ctrl Pts',(-85.0425881162133,-36.7540418071215,
107.));
#44629=CARTESIAN_POINT('Ctrl Pts',(-85.0426529761227,-36.654989588785,107.));
#44630=CARTESIAN_POINT('Ctrl Pts',(-85.0426783462698,-36.6162450179075,
107.));
#44631=CARTESIAN_POINT('Ctrl Pts',(-85.0435252614424,-36.5774481957561,
107.));
#44632=CARTESIAN_POINT('Ctrl Pts',(-85.0451919090303,-36.5386278801149,
107.));
#44633=CARTESIAN_POINT('Ctrl Pts',(-85.045724948488,-36.5262120819881,107.));
#44634=CARTESIAN_POINT('Ctrl Pts',(-85.0463418344278,-36.5137951920582,
107.));
#44635=CARTESIAN_POINT('Ctrl Pts',(-85.0470418057235,-36.5013878196786,
107.));
#44636=CARTESIAN_POINT('Ctrl Pts',(-85.0522810236674,-36.4085198286572,
107.));
#44637=CARTESIAN_POINT('Ctrl Pts',(-85.062176662527,-36.3160350692795,107.));
#44638=CARTESIAN_POINT('Ctrl Pts',(-85.0766052632011,-36.2243051192734,
107.));
#44639=CARTESIAN_POINT('Ctrl Pts',(-85.0909998752463,-36.1327912522612,
107.));
#44640=CARTESIAN_POINT('Ctrl Pts',(-85.1099065280918,-36.0420276973609,
107.));
#44641=CARTESIAN_POINT('Ctrl Pts',(-85.1332513090946,-35.9524003649907,
107.));
#44642=CARTESIAN_POINT('Ctrl Pts',(-85.156199939792,-35.8642939676463,107.));
#44643=CARTESIAN_POINT('Ctrl Pts',(-85.1834378181195,-35.7772847723475,
107.));
#44644=CARTESIAN_POINT('Ctrl Pts',(-85.2149351717563,-35.6917684721328,
107.));
#44645=CARTESIAN_POINT('Ctrl Pts',(-85.230776616366,-35.6487584545708,107.));
#44646=CARTESIAN_POINT('Ctrl Pts',(-85.2476961109153,-35.6061266053731,
107.));
#44647=CARTESIAN_POINT('Ctrl Pts',(-85.2656932851445,-35.5639270559061,
107.));
#44648=CARTESIAN_POINT('Ctrl Pts',(-85.2712589917432,-35.5508766565523,
107.));
#44649=CARTESIAN_POINT('Ctrl Pts',(-85.2769277813298,-35.5378676223478,
107.));
#44650=CARTESIAN_POINT('Ctrl Pts',(-85.2826996838302,-35.5249016119162,
107.));
#44651=CARTESIAN_POINT('Ctrl Pts',(-85.2883791474132,-35.5121432564074,
107.));
#44652=CARTESIAN_POINT('Ctrl Pts',(-85.2941549663054,-35.499434422109,107.));
#44653=CARTESIAN_POINT('Ctrl Pts',(-85.3000253507934,-35.486779594601,107.));
#44654=CARTESIAN_POINT('Ctrl Pts',(-85.3375051537983,-35.4059841300047,
107.));
#44655=CARTESIAN_POINT('Ctrl Pts',(-85.3788551133841,-35.3273454443705,
107.));
#44656=CARTESIAN_POINT('Ctrl Pts',(-85.4240055532635,-35.2512111292096,
107.));
#44657=CARTESIAN_POINT('Ctrl Pts',(-85.4683985586388,-35.1763540276795,
107.));
#44658=CARTESIAN_POINT('Ctrl Pts',(-85.5164660558066,-35.103917306336,107.));
#44659=CARTESIAN_POINT('Ctrl Pts',(-85.5681780296166,-35.0342655325047,
107.));
#44660=CARTESIAN_POINT('Ctrl Pts',(-85.6183124836241,-34.9667385480481,
107.));
#44661=CARTESIAN_POINT('Ctrl Pts',(-85.6718728926839,-34.901828747048,107.));
#44662=CARTESIAN_POINT('Ctrl Pts',(-85.7288596163099,-34.8399086244755,
107.));
#44663=CARTESIAN_POINT('Ctrl Pts',(-85.7498272120257,-34.8171258425545,
107.));
#44664=CARTESIAN_POINT('Ctrl Pts',(-85.7712589016926,-34.7947482334293,
107.));
#44665=CARTESIAN_POINT('Ctrl Pts',(-85.7931555144105,-34.7727959615648,
107.));
#44666=CARTESIAN_POINT('Ctrl Pts',(-85.8122329504701,-34.7536700324426,
107.));
#44667=CARTESIAN_POINT('Ctrl Pts',(-85.8316633199033,-34.7348669902236,
107.));
#44668=CARTESIAN_POINT('Ctrl Pts',(-85.8514364858567,-34.7163919634216,
107.));
#44669=CARTESIAN_POINT('Origin',(-87.7685555885722,-36.3549260746835,124.208423447177));
#44670=CARTESIAN_POINT('Ctrl Pts',(-90.8453551362697,-36.3529984899081,
121.708423447177));
#44671=CARTESIAN_POINT('Ctrl Pts',(-90.8462778186642,-36.2297235877034,
121.702019850418));
#44672=CARTESIAN_POINT('Ctrl Pts',(-90.7837513605892,-35.0938167757587,
121.642966745928));
#44673=CARTESIAN_POINT('Ctrl Pts',(-89.3710243173134,-33.1013875956417,
121.531264133707));
#44674=CARTESIAN_POINT('Ctrl Pts',(-85.9203582039126,-33.2347629349336,
121.373315610515));
#44675=CARTESIAN_POINT('Ctrl Pts',(-84.1454681337529,-36.1967043012439,
121.215367087322));
#44676=CARTESIAN_POINT('Ctrl Pts',(-85.6554864122685,-39.3022906545617,
121.05741856413));
#44677=CARTESIAN_POINT('Ctrl Pts',(-89.0813771948967,-39.735498741376,120.899470040937));
#44678=CARTESIAN_POINT('Ctrl Pts',(-90.7279241675112,-37.7971275010703,
120.783138335286));
#44679=CARTESIAN_POINT('Ctrl Pts',(-90.8448017962344,-36.5704857415671,
120.719456137367));
#44680=CARTESIAN_POINT('Ctrl Pts',(-90.8428699659751,-36.357609793043,120.708423447177));
#44681=CARTESIAN_POINT('Ctrl Pts',(-90.8388341582581,-36.3579404435482,
121.791576552823));
#44682=CARTESIAN_POINT('Ctrl Pts',(-90.8338492651609,-35.6649221393835,
121.755752019753));
#44683=CARTESIAN_POINT('Ctrl Pts',(-90.2614620369657,-33.9437331486761,
121.667277978953));
#44684=CARTESIAN_POINT('Ctrl Pts',(-87.417021209647,-32.7460642638912,121.526154430423));
#44685=CARTESIAN_POINT('Ctrl Pts',(-84.5546283385357,-34.6751866943283,
121.36820590723));
#44686=CARTESIAN_POINT('Ctrl Pts',(-84.6050187185395,-38.1284686676829,
121.210257384038));
#44687=CARTESIAN_POINT('Ctrl Pts',(-87.5242687364515,-39.9731543606838,
121.052308860845));
#44688=CARTESIAN_POINT('Ctrl Pts',(-90.2991160808229,-38.7047120741592,
120.912748583773));
#44689=CARTESIAN_POINT('Ctrl Pts',(-90.8346458997654,-37.0159745254743,
120.825837814433));
#44690=CARTESIAN_POINT('Ctrl Pts',(-90.8389971204791,-36.3527751889037,
120.791576552823));
#44691=CARTESIAN_POINT('Ctrl Pts',(-85.855089591907,-34.7189388713087,122.));
#44692=CARTESIAN_POINT('Ctrl Pts',(-85.3138942055855,-35.3519260775303,
121.947350492269));
#44693=CARTESIAN_POINT('Ctrl Pts',(-84.9185558383608,-37.1869577282907,
121.842051476807));
#44694=CARTESIAN_POINT('Ctrl Pts',(-86.9093548370361,-39.2001258698145,
121.684102953615));
#44695=CARTESIAN_POINT('Ctrl Pts',(-89.6802577024474,-38.6278810997191,
121.526154430422));
#44696=CARTESIAN_POINT('Ctrl Pts',(-90.7173747954316,-35.9976145147108,
121.36820590723));
#44697=CARTESIAN_POINT('Ctrl Pts',(-89.081135716962,-33.6899567820244,121.210257384038));
#44698=CARTESIAN_POINT('Ctrl Pts',(-86.2546994259301,-33.7992043553666,
121.052308860845));
#44699=CARTESIAN_POINT('Ctrl Pts',(-84.8008891927669,-36.2253268182546,
120.894360337653));
#44700=CARTESIAN_POINT('Ctrl Pts',(-86.0377432731843,-38.7691087100644,
120.73641181446));
#44701=CARTESIAN_POINT('Ctrl Pts',(-88.8438861218152,-39.1239489113188,
120.578463291268));
#44702=CARTESIAN_POINT('Ctrl Pts',(-90.675052730646,-36.9682371400777,120.420514768075));
#44703=CARTESIAN_POINT('Ctrl Pts',(-89.8709900599802,-34.2564369768315,
120.262566244883));
#44704=CARTESIAN_POINT('Ctrl Pts',(-87.1607124008595,-33.4472817605808,
120.10461772169));
#44705=CARTESIAN_POINT('Ctrl Pts',(-85.0015484493013,-35.2743949794042,
119.946669198498));
#44706=CARTESIAN_POINT('Ctrl Pts',(-85.3511453388923,-38.0811949374583,
119.788720675305));
#44707=CARTESIAN_POINT('Ctrl Pts',(-87.892534763121,-39.3228384190479,119.630772152113));
#44708=CARTESIAN_POINT('Ctrl Pts',(-90.3215159512363,-37.8735665295443,
119.472823628921));
#44709=CARTESIAN_POINT('Ctrl Pts',(-90.4358056666791,-35.0473892903923,
119.314875105728));
#44710=CARTESIAN_POINT('Ctrl Pts',(-88.1317808359558,-33.4067160016613,
119.156926582536));
#44711=CARTESIAN_POINT('Ctrl Pts',(-85.4984307306815,-34.4390950644477,
118.998978059343));
#44712=CARTESIAN_POINT('Ctrl Pts',(-84.9233337863437,-37.2084998640467,
118.841029536151));
#44713=CARTESIAN_POINT('Ctrl Pts',(-86.9279129190018,-39.2039952558787,
118.683081012958));
#44714=CARTESIAN_POINT('Ctrl Pts',(-89.6946771919892,-38.6163262780736,
118.525132489766));
#44715=CARTESIAN_POINT('Ctrl Pts',(-90.7150855880725,-35.9783145101063,
118.367183966573));
#44716=CARTESIAN_POINT('Ctrl Pts',(-89.063964847989,-33.6817649951384,118.209235443381));
#44717=CARTESIAN_POINT('Ctrl Pts',(-86.2383359306196,-33.8088893297358,
118.051286920188));
#44718=CARTESIAN_POINT('Ctrl Pts',(-84.8001106375229,-36.2444277471294,
117.893338396996));
#44719=CARTESIAN_POINT('Ctrl Pts',(-86.0532841004025,-38.7801516372869,
117.735389873803));
#44720=CARTESIAN_POINT('Ctrl Pts',(-88.861642053966,-39.1169972698181,117.577441350611));
#44721=CARTESIAN_POINT('Ctrl Pts',(-90.6789317540865,-36.9495569542776,
117.419492827418));
#44722=CARTESIAN_POINT('Ctrl Pts',(-89.8574719000215,-34.2429829051099,
117.261544304226));
#44723=CARTESIAN_POINT('Ctrl Pts',(-87.1420551578849,-33.4512434959369,
117.103595781033));
#44724=CARTESIAN_POINT('Ctrl Pts',(-84.9946673021025,-35.2921847694046,
116.945647257841));
#44725=CARTESIAN_POINT('Ctrl Pts',(-85.3622795916639,-38.0966812625507,
116.787698734649));
#44726=CARTESIAN_POINT('Ctrl Pts',(-87.9115891440455,-39.3219812999482,
116.629750211456));
#44727=CARTESIAN_POINT('Ctrl Pts',(-90.3312145218488,-37.8571426035032,
116.471801688264));
#44728=CARTESIAN_POINT('Ctrl Pts',(-90.4273549845983,-35.0302898682282,
116.313853165071));
#44729=CARTESIAN_POINT('Ctrl Pts',(-88.1128428986993,-33.4044444943569,
116.155904641879));
#44730=CARTESIAN_POINT('Ctrl Pts',(-85.4861759797334,-34.453711034527,115.997956118686));
#44731=CARTESIAN_POINT('Ctrl Pts',(-84.9288732366636,-37.2267514287653,
115.840007595494));
#44732=CARTESIAN_POINT('Ctrl Pts',(-86.9462241170348,-39.2093342898272,
115.682059072301));
#44733=CARTESIAN_POINT('Ctrl Pts',(-89.7091579325677,-38.6039120351199,
115.524110549109));
#44734=CARTESIAN_POINT('Ctrl Pts',(-90.7126066235523,-35.959402609901,115.366162025916));
#44735=CARTESIAN_POINT('Ctrl Pts',(-89.0467737803853,-33.673502280898,115.208213502724));
#44736=CARTESIAN_POINT('Ctrl Pts',(-86.2220193779501,-33.818767353902,115.050264979531));
#44737=CARTESIAN_POINT('Ctrl Pts',(-84.7994623219137,-36.263490405258,114.892316456339));
#44738=CARTESIAN_POINT('Ctrl Pts',(-86.0688918298665,-38.7911153971918,
114.734367933147));
#44739=CARTESIAN_POINT('Ctrl Pts',(-88.8793547749015,-39.1099216237564,
114.576419409954));
#44740=CARTESIAN_POINT('Ctrl Pts',(-90.6826898811218,-36.9308571753786,
114.418470886762));
#44741=CARTESIAN_POINT('Ctrl Pts',(-89.8438680536754,-34.2296135141532,
114.260522363569));
#44742=CARTESIAN_POINT('Ctrl Pts',(-87.1234235318957,-33.455326113101,114.102573840377));
#44743=CARTESIAN_POINT('Ctrl Pts',(-84.9879006250997,-35.3100178098693,
113.944625317184));
#44744=CARTESIAN_POINT('Ctrl Pts',(-85.3735130038868,-38.1120960508962,
113.786676793992));
#44745=CARTESIAN_POINT('Ctrl Pts',(-87.9306376522803,-39.3210017164002,
113.628728270799));
#44746=CARTESIAN_POINT('Ctrl Pts',(-90.3408074230132,-37.8406568066725,
113.470779747607));
#44747=CARTESIAN_POINT('Ctrl Pts',(-90.4187946869615,-35.013245028708,113.312831224414));
#44748=CARTESIAN_POINT('Ctrl Pts',(-88.093890763779,-33.4022946497451,113.154882701222));
#44749=CARTESIAN_POINT('Ctrl Pts',(-85.4740153318585,-34.4684053835483,
112.996934178029));
#44750=CARTESIAN_POINT('Ctrl Pts',(-84.9345297654133,-37.2449670520707,
112.838985654837));
#44751=CARTESIAN_POINT('Ctrl Pts',(-86.9645692198269,-39.2145556357687,
112.681037131644));
#44752=CARTESIAN_POINT('Ctrl Pts',(-89.7235586626422,-38.5914050681325,
112.523088608452));
#44753=CARTESIAN_POINT('Ctrl Pts',(-90.7100062769287,-35.9405070165698,
112.365140085259));
#44754=CARTESIAN_POINT('Ctrl Pts',(-89.0295300122615,-33.6653501210131,
112.207191562067));
#44755=CARTESIAN_POINT('Ctrl Pts',(-86.2057665884384,-33.8287499428941,
112.049243038875));
#44756=CARTESIAN_POINT('Ctrl Pts',(-84.7989364209583,-36.282556833295,111.891294515682));
#44757=CARTESIAN_POINT('Ctrl Pts',(-86.0845696358685,-38.8019787138511,
111.73334599249));
#44758=CARTESIAN_POINT('Ctrl Pts',(-88.8970216979793,-39.1027323902174,
111.575397469297));
#44759=CARTESIAN_POINT('Ctrl Pts',(-90.6863278594327,-36.9121336510371,
111.417448946105));
#44760=CARTESIAN_POINT('Ctrl Pts',(-89.830178642936,-34.2163317490865,111.259500422912));
#44761=CARTESIAN_POINT('Ctrl Pts',(-87.1048185044643,-33.4595282797339,
111.10155189972));
#44762=CARTESIAN_POINT('Ctrl Pts',(-84.9812485935319,-35.3278939315487,
110.943603376527));
#44763=CARTESIAN_POINT('Ctrl Pts',(-85.3848451628316,-38.1274383917119,
110.785654853335));
#44764=CARTESIAN_POINT('Ctrl Pts',(-87.949679478,-39.3198998426766,110.627706330142));
#44765=CARTESIAN_POINT('Ctrl Pts',(-90.3502942710008,-37.824109753544,110.46975780695));
#44766=CARTESIAN_POINT('Ctrl Pts',(-90.4101251212064,-34.9962555065228,
110.311809283757));
#44767=CARTESIAN_POINT('Ctrl Pts',(-88.0749252147876,-33.4002665404604,
110.153860760565));
#44768=CARTESIAN_POINT('Ctrl Pts',(-85.4619492883336,-34.4831775144226,
109.995912237372));
#44769=CARTESIAN_POINT('Ctrl Pts',(-84.9403031374328,-37.2631459766827,
109.83796371418));
#44770=CARTESIAN_POINT('Ctrl Pts',(-86.982947476059,-39.219659085585,109.680015190988));
#44771=CARTESIAN_POINT('Ctrl Pts',(-89.737878777595,-38.5788058808295,109.522066667795));
#44772=CARTESIAN_POINT('Ctrl Pts',(-90.7072846780369,-35.9216285323762,
109.364118144603));
#44773=CARTESIAN_POINT('Ctrl Pts',(-89.0122342079233,-33.6573088045276,
109.20616962141));
#44774=CARTESIAN_POINT('Ctrl Pts',(-86.1895783281781,-33.8388367816117,
109.048221098218));
#44775=CARTESIAN_POINT('Ctrl Pts',(-84.7985327588824,-36.3016260468753,
108.890272575025));
#44776=CARTESIAN_POINT('Ctrl Pts',(-86.1003172781239,-38.8127415470481,
108.732324051833));
#44777=CARTESIAN_POINT('Ctrl Pts',(-88.914641259591,-39.0954290272211,108.57437552864));
#44778=CARTESIAN_POINT('Ctrl Pts',(-90.6898472567247,-36.8933888774387,
108.416427005448));
#44779=CARTESIAN_POINT('Ctrl Pts',(-89.8164006995781,-34.2031346114724,
108.258478482255));
#44780=CARTESIAN_POINT('Ctrl Pts',(-87.0862481079167,-33.463857115393,108.100529959063));
#44781=CARTESIAN_POINT('Ctrl Pts',(-84.9746965398898,-35.3457973989596,
107.94258143587));
#44782=CARTESIAN_POINT('Ctrl Pts',(-85.396306330652,-38.1427384983891,107.784632912678));
#44783=CARTESIAN_POINT('Ctrl Pts',(-87.9686506378239,-39.3186122859791,
107.626684389485));
#44784=CARTESIAN_POINT('Ctrl Pts',(-90.3598046494548,-37.8076325931292,
107.468735866293));
#44785=CARTESIAN_POINT('Ctrl Pts',(-90.401079337765,-34.9790536330783,107.3107873431));
#44786=CARTESIAN_POINT('Ctrl Pts',(-88.0564969547953,-33.3989119868201,
107.152838819908));
#44787=CARTESIAN_POINT('Ctrl Pts',(-85.4488473177177,-34.4968783509201,
106.994890296716));
#44788=CARTESIAN_POINT('Ctrl Pts',(-84.9485679810268,-37.2836053207636,
106.836941773523));
#44789=CARTESIAN_POINT('Ctrl Pts',(-86.3138051921105,-38.5719224173531,
106.731642758061));
#44790=CARTESIAN_POINT('Ctrl Pts',(-87.1183555905977,-38.7870128767187,
106.678993250331));
#44791=CARTESIAN_POINT('Ctrl Pts',(-85.71422403823,-34.5985007534569,122.10700224989));
#44792=CARTESIAN_POINT('Ctrl Pts',(-85.133186926017,-35.2780872164357,122.054352742159));
#44793=CARTESIAN_POINT('Ctrl Pts',(-84.708744535995,-37.2482102406252,121.949053726697));
#44794=CARTESIAN_POINT('Ctrl Pts',(-86.8461021898526,-39.4095838090522,
121.791105203505));
#44795=CARTESIAN_POINT('Ctrl Pts',(-89.8209934025883,-38.7952115193046,
121.633156680312));
#44796=CARTESIAN_POINT('Ctrl Pts',(-90.9344609892766,-35.9713099496867,
121.47520815712));
#44797=CARTESIAN_POINT('Ctrl Pts',(-89.1777652504124,-33.4937670532302,
121.317259633927));
#44798=CARTESIAN_POINT('Ctrl Pts',(-86.1432523519242,-33.6110572152223,
121.159311110735));
#44799=CARTESIAN_POINT('Ctrl Pts',(-84.5824155064289,-36.215785979251,121.001362587543));
#44800=CARTESIAN_POINT('Ctrl Pts',(-85.9103243195458,-38.9468360248968,
120.84341406435));
#44801=CARTESIAN_POINT('Ctrl Pts',(-88.9230498128423,-39.3277988546712,
120.685465541158));
#44802=CARTESIAN_POINT('Ctrl Pts',(-90.8890232584176,-37.0133878785563,
120.527517017965));
#44803=CARTESIAN_POINT('Ctrl Pts',(-90.0257670962068,-34.1019503911438,
120.369568494773));
#44804=CARTESIAN_POINT('Ctrl Pts',(-87.11596419664,-33.2332267802908,120.21161997158));
#44805=CARTESIAN_POINT('Ctrl Pts',(-84.7978468975721,-35.1948484333631,
120.053671448388));
#44806=CARTESIAN_POINT('Ctrl Pts',(-85.173180413527,-38.2082794111694,119.895722925195));
#44807=CARTESIAN_POINT('Ctrl Pts',(-87.9016618628959,-39.5413302116287,
119.737774402003));
#44808=CARTESIAN_POINT('Ctrl Pts',(-90.5094598058065,-37.9853658136096,
119.57982587881));
#44809=CARTESIAN_POINT('Ctrl Pts',(-90.632163302353,-34.9511310378844,119.421877355618));
#44810=CARTESIAN_POINT('Ctrl Pts',(-88.1585207548627,-33.1896746510356,
119.263928832425));
#44811=CARTESIAN_POINT('Ctrl Pts',(-85.3313086623614,-34.2980554031843,
119.105980309233));
#44812=CARTESIAN_POINT('Ctrl Pts',(-84.7138742269874,-37.2713382654881,
118.948031786041));
#44813=CARTESIAN_POINT('Ctrl Pts',(-86.8660264808315,-39.4137380516079,
118.790083262848));
#44814=CARTESIAN_POINT('Ctrl Pts',(-89.8364744262163,-38.7828060547151,
118.632134739655));
#44815=CARTESIAN_POINT('Ctrl Pts',(-90.9320032550333,-35.9505891172026,
118.474186216463));
#44816=CARTESIAN_POINT('Ctrl Pts',(-89.1593302962823,-33.4849722033175,
118.316237693271));
#44817=CARTESIAN_POINT('Ctrl Pts',(-86.1256842086968,-33.6214551781051,
118.158289170078));
#44818=CARTESIAN_POINT('Ctrl Pts',(-84.5815796354993,-36.2362930804469,
118.000340646886));
#44819=CARTESIAN_POINT('Ctrl Pts',(-85.9270092314952,-38.958691910416,117.842392123693));
#44820=CARTESIAN_POINT('Ctrl Pts',(-88.9421129013356,-39.3203354471759,
117.684443600501));
#44821=CARTESIAN_POINT('Ctrl Pts',(-90.8931878478337,-36.9933324947018,
117.526495077308));
#44822=CARTESIAN_POINT('Ctrl Pts',(-90.0112537562499,-34.0875058574723,
117.368546554116));
#44823=CARTESIAN_POINT('Ctrl Pts',(-87.0959334446163,-33.237480170709,117.210598030923));
#44824=CARTESIAN_POINT('Ctrl Pts',(-84.7904591740287,-35.2139478722533,
117.052649507731));
#44825=CARTESIAN_POINT('Ctrl Pts',(-85.1851343478002,-38.2249058086552,
116.894700984538));
#44826=CARTESIAN_POINT('Ctrl Pts',(-87.9221189893741,-39.5404099931289,
116.736752461346));
#44827=CARTESIAN_POINT('Ctrl Pts',(-90.5198723658608,-37.9677327908616,
116.578803938154));
#44828=CARTESIAN_POINT('Ctrl Pts',(-90.6230904978973,-34.9327727903349,
116.420855414961));
#44829=CARTESIAN_POINT('Ctrl Pts',(-88.1381886444035,-33.18723591989,116.262906891769));
#44830=CARTESIAN_POINT('Ctrl Pts',(-85.3181517410688,-34.3137473718554,
116.104958368576));
#44831=CARTESIAN_POINT('Ctrl Pts',(-84.7198214806012,-37.290933474031,115.947009845384));
#44832=CARTESIAN_POINT('Ctrl Pts',(-86.8856857127746,-39.4194701345965,
115.789061322191));
#44833=CARTESIAN_POINT('Ctrl Pts',(-89.8520212100601,-38.7694778999333,
115.631112798999));
#44834=CARTESIAN_POINT('Ctrl Pts',(-90.9293417940852,-35.9302849605903,
115.473164275806));
#44835=CARTESIAN_POINT('Ctrl Pts',(-89.1408736565385,-33.47610120452,115.315215752614));
#44836=CARTESIAN_POINT('Ctrl Pts',(-86.1081664639344,-33.6320604027263,
115.157267229421));
#44837=CARTESIAN_POINT('Ctrl Pts',(-84.5808835921868,-36.2567590934803,
114.999318706229));
#44838=CARTESIAN_POINT('Ctrl Pts',(-85.9437659709006,-38.9704628004774,
114.841370183036));
#44839=CARTESIAN_POINT('Ctrl Pts',(-88.9611295974899,-39.3127389061509,
114.683421659844));
#44840=CARTESIAN_POINT('Ctrl Pts',(-90.8972226406924,-36.9732560753437,
114.525473136651));
#44841=CARTESIAN_POINT('Ctrl Pts',(-89.9966484218447,-34.0731522385948,
114.367524613459));
#44842=CARTESIAN_POINT('Ctrl Pts',(-87.0759301954492,-33.2418633420133,
114.209576090267));
#44843=CARTESIAN_POINT('Ctrl Pts',(-84.7831943477492,-35.2330937456208,
114.051627567074));
#44844=CARTESIAN_POINT('Ctrl Pts',(-85.1971947414458,-38.2414554030014,
113.893679043882));
#44845=CARTESIAN_POINT('Ctrl Pts',(-87.9425698108267,-39.5393582945921,
113.735730520689));
#44846=CARTESIAN_POINT('Ctrl Pts',(-90.5301714772931,-37.9500333425197,
113.577781997497));
#44847=CARTESIAN_POINT('Ctrl Pts',(-90.6139000082066,-34.9144731436948,
113.419833474304));
#44848=CARTESIAN_POINT('Ctrl Pts',(-88.1178412910765,-33.1849278080018,
113.261884951112));
#44849=CARTESIAN_POINT('Ctrl Pts',(-85.3050958505301,-34.32952348957,113.103936427919));
#44850=CARTESIAN_POINT('Ctrl Pts',(-84.7258944317255,-37.3104900952256,
112.945987904727));
#44851=CARTESIAN_POINT('Ctrl Pts',(-86.9053813454777,-39.4250758656216,
112.788039381534));
#44852=CARTESIAN_POINT('Ctrl Pts',(-89.867482093186,-38.7560501949591,112.630090858342));
#44853=CARTESIAN_POINT('Ctrl Pts',(-90.9265500151248,-35.9099983113317,
112.472142335149));
#44854=CARTESIAN_POINT('Ctrl Pts',(-89.1223604365675,-33.4673488988693,
112.314193811957));
#44855=CARTESIAN_POINT('Ctrl Pts',(-86.0907171764458,-33.6427778900275,
112.156245288764));
#44856=CARTESIAN_POINT('Ctrl Pts',(-84.580318975451,-36.2772291539554,111.998296765572));
#44857=CARTESIAN_POINT('Ctrl Pts',(-85.960597945739,-38.9821258528616,111.840348242379));
#44858=CARTESIAN_POINT('Ctrl Pts',(-88.9800971242396,-39.3050204155649,
111.682399719187));
#44859=CARTESIAN_POINT('Ctrl Pts',(-90.901128439717,-36.9531541624509,111.524451195994));
#44860=CARTESIAN_POINT('Ctrl Pts',(-89.9819512239657,-34.0588926964507,
111.366502672802));
#44861=CARTESIAN_POINT('Ctrl Pts',(-87.0559555029728,-33.24637486378,111.208554149609));
#44862=CARTESIAN_POINT('Ctrl Pts',(-84.7760526068729,-35.2522858717561,
111.050605626417));
#44863=CARTESIAN_POINT('Ctrl Pts',(-85.2093611513503,-38.257927216375,110.892657103225));
#44864=CARTESIAN_POINT('Ctrl Pts',(-87.963013457811,-39.5381753031207,110.734708580032));
#44865=CARTESIAN_POINT('Ctrl Pts',(-90.5403567281249,-37.9322681283135,
110.57676005684));
#44866=CARTESIAN_POINT('Ctrl Pts',(-90.6045922062968,-34.8962328867416,
110.418811533647));
#44867=CARTESIAN_POINT('Ctrl Pts',(-88.0974795361613,-33.1827503933531,
110.260863010455));
#44868=CARTESIAN_POINT('Ctrl Pts',(-85.2921415289253,-34.3453831152826,
110.102914487262));
#44869=CARTESIAN_POINT('Ctrl Pts',(-84.7320928278883,-37.330007316042,109.94496596407));
#44870=CARTESIAN_POINT('Ctrl Pts',(-86.925112572311,-39.4305550212435,109.787017440877));
#44871=CARTESIAN_POINT('Ctrl Pts',(-89.8828564264658,-38.7425234805934,
109.629068917685));
#44872=CARTESIAN_POINT('Ctrl Pts',(-90.923628057546,-35.8897300307512,109.471120394492));
#44873=CARTESIAN_POINT('Ctrl Pts',(-89.1037913495795,-33.4587155966883,
109.3131718713));
#44874=CARTESIAN_POINT('Ctrl Pts',(-86.0733371687237,-33.6536073017113,
109.155223348107));
#44875=CARTESIAN_POINT('Ctrl Pts',(-84.5798855965776,-36.29770220504,108.997274824915));
#44876=CARTESIAN_POINT('Ctrl Pts',(-85.9775048980366,-38.9936810243913,
108.839326301722));
#44877=CARTESIAN_POINT('Ctrl Pts',(-88.9990138028663,-39.2971793935384,
108.68137777853));
#44878=CARTESIAN_POINT('Ctrl Pts',(-90.9049069280247,-36.9330294359731,
108.523429255337));
#44879=CARTESIAN_POINT('Ctrl Pts',(-89.9671589758732,-34.0447240118636,
108.365480732145));
#44880=CARTESIAN_POINT('Ctrl Pts',(-87.036017990837,-33.2510223796941,108.207532208953));
#44881=CARTESIAN_POINT('Ctrl Pts',(-84.769018204098,-35.2715073567614,108.04958368576));
#44882=CARTESIAN_POINT('Ctrl Pts',(-85.2216660675069,-38.274353686417,107.891635162568));
#44883=CARTESIAN_POINT('Ctrl Pts',(-87.9833812366168,-39.5367929590649,
107.733686639375));
#44884=CARTESIAN_POINT('Ctrl Pts',(-90.5505672416893,-37.9145779521832,
107.575738116183));
#44885=CARTESIAN_POINT('Ctrl Pts',(-90.5948804903041,-34.8777646456526,
107.41778959299));
#44886=CARTESIAN_POINT('Ctrl Pts',(-88.0776946243907,-33.181296120173,107.259841069798));
#44887=CARTESIAN_POINT('Ctrl Pts',(-85.2780750173411,-34.3600925800612,
107.101892546605));
#44888=CARTESIAN_POINT('Ctrl Pts',(-84.7409661127983,-37.3519728362644,
106.943944023413));
#44889=CARTESIAN_POINT('Ctrl Pts',(-86.2067093668298,-38.7351332702527,
106.838645007951));
#44890=CARTESIAN_POINT('Ctrl Pts',(-87.0704891624118,-38.9660582606223,
106.78599550022));
#44891=CARTESIAN_POINT('Ctrl Pts',(-85.573358484553,-34.478062635605,122.21400449978));
#44892=CARTESIAN_POINT('Ctrl Pts',(-84.9524796464486,-35.2042483553411,
122.161354992049));
#44893=CARTESIAN_POINT('Ctrl Pts',(-84.4989332336292,-37.3094627529595,
122.056055976587));
#44894=CARTESIAN_POINT('Ctrl Pts',(-86.782849542669,-39.6190417482899,121.898107453395));
#44895=CARTESIAN_POINT('Ctrl Pts',(-89.9617291027293,-38.9625419388902,
121.740158930202));
#44896=CARTESIAN_POINT('Ctrl Pts',(-91.1515471831214,-35.9450053846625,
121.58221040701));
#44897=CARTESIAN_POINT('Ctrl Pts',(-89.274394783863,-33.2975773244359,121.424261883817));
#44898=CARTESIAN_POINT('Ctrl Pts',(-86.0318052779183,-33.4229100750779,
121.266313360625));
#44899=CARTESIAN_POINT('Ctrl Pts',(-84.3639418200909,-36.2062451402475,
121.108364837432));
#44900=CARTESIAN_POINT('Ctrl Pts',(-85.7829053659071,-39.1245633397293,
120.95041631424));
#44901=CARTESIAN_POINT('Ctrl Pts',(-89.0022135038696,-39.5316487980236,
120.792467791047));
#44902=CARTESIAN_POINT('Ctrl Pts',(-91.1029937861889,-37.0585386170348,
120.634519267855));
#44903=CARTESIAN_POINT('Ctrl Pts',(-90.1805441324336,-33.9474638054562,
120.476570744663));
#44904=CARTESIAN_POINT('Ctrl Pts',(-87.0712159924203,-33.0191718000006,
120.31862222147));
#44905=CARTESIAN_POINT('Ctrl Pts',(-84.594145345843,-35.115301887322,120.160673698277));
#44906=CARTESIAN_POINT('Ctrl Pts',(-84.9952154881615,-38.3353638848805,
120.002725175085));
#44907=CARTESIAN_POINT('Ctrl Pts',(-87.9107889626707,-39.7598220042095,
119.844776651893));
#44908=CARTESIAN_POINT('Ctrl Pts',(-90.6974036603767,-38.0971650976748,
119.6868281287));
#44909=CARTESIAN_POINT('Ctrl Pts',(-90.8285209380269,-34.8548727853765,
119.528879605508));
#44910=CARTESIAN_POINT('Ctrl Pts',(-88.1852606737698,-32.9726333004099,
119.370931082315));
#44911=CARTESIAN_POINT('Ctrl Pts',(-85.1641865940414,-34.157015741921,119.212982559123));
#44912=CARTESIAN_POINT('Ctrl Pts',(-84.504414667631,-37.3341766669294,119.05503403593));
#44913=CARTESIAN_POINT('Ctrl Pts',(-86.8041400426611,-39.623480847337,118.897085512738));
#44914=CARTESIAN_POINT('Ctrl Pts',(-89.9782716604433,-38.9492858313566,
118.739136989545));
#44915=CARTESIAN_POINT('Ctrl Pts',(-91.1489209219942,-35.9228637242989,
118.581188466353));
#44916=CARTESIAN_POINT('Ctrl Pts',(-89.2546957445757,-33.2881794114966,
118.42323994316));
#44917=CARTESIAN_POINT('Ctrl Pts',(-86.0130324867741,-33.4340210264743,
118.265291419968));
#44918=CARTESIAN_POINT('Ctrl Pts',(-84.3630486334757,-36.2281584137643,
118.107342896775));
#44919=CARTESIAN_POINT('Ctrl Pts',(-85.8007343625879,-39.1372321835451,
117.949394373583));
#44920=CARTESIAN_POINT('Ctrl Pts',(-89.022583748705,-39.5236736245337,117.791445850391));
#44921=CARTESIAN_POINT('Ctrl Pts',(-91.107443941581,-37.0371080351261,117.633497327198));
#44922=CARTESIAN_POINT('Ctrl Pts',(-90.1650356124785,-33.9320288098347,
117.475548804006));
#44923=CARTESIAN_POINT('Ctrl Pts',(-87.0498117313475,-33.0237168454812,
117.317600280813));
#44924=CARTESIAN_POINT('Ctrl Pts',(-84.586251045955,-35.135710975102,117.159651757621));
#44925=CARTESIAN_POINT('Ctrl Pts',(-85.0079891039364,-38.3531303547597,
117.001703234428));
#44926=CARTESIAN_POINT('Ctrl Pts',(-87.9326488347025,-39.7588386863096,
116.843754711236));
#44927=CARTESIAN_POINT('Ctrl Pts',(-90.708530209873,-38.0783229782199,116.685806188043));
#44928=CARTESIAN_POINT('Ctrl Pts',(-90.8188260111962,-34.8352557124416,
116.527857664851));
#44929=CARTESIAN_POINT('Ctrl Pts',(-88.1635343901077,-32.970027345423,116.369909141658));
#44930=CARTESIAN_POINT('Ctrl Pts',(-85.1501275024042,-34.1737837091839,
116.211960618466));
#44931=CARTESIAN_POINT('Ctrl Pts',(-84.5107697245388,-37.3551155192967,
116.054012095273));
#44932=CARTESIAN_POINT('Ctrl Pts',(-86.8251473085145,-39.6296059793658,
115.896063572081));
#44933=CARTESIAN_POINT('Ctrl Pts',(-89.9948844875526,-38.9350437647466,
115.738115048888));
#44934=CARTESIAN_POINT('Ctrl Pts',(-91.146076964618,-35.9011673112796,115.580166525696));
#44935=CARTESIAN_POINT('Ctrl Pts',(-89.2349735326918,-33.278700128142,115.422218002504));
#44936=CARTESIAN_POINT('Ctrl Pts',(-85.9943135499183,-33.4453534515506,
115.264269479311));
#44937=CARTESIAN_POINT('Ctrl Pts',(-84.3623048624599,-36.2500277817027,
115.106320956119));
#44938=CARTESIAN_POINT('Ctrl Pts',(-85.8186401119347,-39.1498102037631,
114.948372432926));
#44939=CARTESIAN_POINT('Ctrl Pts',(-89.0429044200783,-39.5155561885454,
114.790423909734));
#44940=CARTESIAN_POINT('Ctrl Pts',(-91.1117554002631,-37.0156549753088,
114.632475386541));
#44941=CARTESIAN_POINT('Ctrl Pts',(-90.1494287900138,-33.9166909630364,
114.474526863349));
#44942=CARTESIAN_POINT('Ctrl Pts',(-87.0284368590026,-33.0284005709257,
114.316578340156));
#44943=CARTESIAN_POINT('Ctrl Pts',(-84.5784880703985,-35.1561696813723,
114.158629816964));
#44944=CARTESIAN_POINT('Ctrl Pts',(-85.0208764790048,-38.3708147551066,
114.000681293771));
#44945=CARTESIAN_POINT('Ctrl Pts',(-87.9545019693732,-39.757714872784,113.842732770579));
#44946=CARTESIAN_POINT('Ctrl Pts',(-90.7195355315731,-38.0594098783669,
113.684784247386));
#44947=CARTESIAN_POINT('Ctrl Pts',(-90.8090053294518,-34.8157012586816,
113.526835724194));
#44948=CARTESIAN_POINT('Ctrl Pts',(-88.1417918183741,-32.9675609662586,
113.368887201001));
#44949=CARTESIAN_POINT('Ctrl Pts',(-85.1361763692016,-34.1906415955917,
113.210938677809));
#44950=CARTESIAN_POINT('Ctrl Pts',(-84.5172590980378,-37.3760131383805,
113.052990154616));
#44951=CARTESIAN_POINT('Ctrl Pts',(-86.8461934711285,-39.6355960954744,
112.895041631424));
#44952=CARTESIAN_POINT('Ctrl Pts',(-90.0114055237299,-38.9206953217857,
112.737093108232));
#44953=CARTESIAN_POINT('Ctrl Pts',(-91.143093753321,-35.8794896060935,112.579144585039));
#44954=CARTESIAN_POINT('Ctrl Pts',(-89.2151908608736,-33.2693476767256,
112.421196061847));
#44955=CARTESIAN_POINT('Ctrl Pts',(-85.9756677644532,-33.4568058371609,
112.263247538654));
#44956=CARTESIAN_POINT('Ctrl Pts',(-84.3617015299438,-36.2719014746159,
112.105299015462));
#44957=CARTESIAN_POINT('Ctrl Pts',(-85.8366262556094,-39.1622729918721,
111.947350492269));
#44958=CARTESIAN_POINT('Ctrl Pts',(-89.0631725504999,-39.5073084409124,
111.789401969077));
#44959=CARTESIAN_POINT('Ctrl Pts',(-91.1159290200014,-36.9941746738646,
111.631453445884));
#44960=CARTESIAN_POINT('Ctrl Pts',(-90.1337238049953,-33.9014536438148,
111.473504922692));
#44961=CARTESIAN_POINT('Ctrl Pts',(-87.0070925014814,-33.0332214478261,
111.315556399499));
#44962=CARTESIAN_POINT('Ctrl Pts',(-84.5708566202139,-35.1766778119636,
111.157607876307));
#44963=CARTESIAN_POINT('Ctrl Pts',(-85.033877139869,-38.388416041038,110.999659353114));
#44964=CARTESIAN_POINT('Ctrl Pts',(-87.976347437622,-39.7564507635648,110.841710829922));
#44965=CARTESIAN_POINT('Ctrl Pts',(-90.7304191852489,-38.040426503083,110.683762306729));
#44966=CARTESIAN_POINT('Ctrl Pts',(-90.7990592913871,-34.7962102669604,
110.525813783537));
#44967=CARTESIAN_POINT('Ctrl Pts',(-88.1200338575352,-32.9652342462458,
110.367865260344));
#44968=CARTESIAN_POINT('Ctrl Pts',(-85.1223337695167,-34.2075887161425,
110.209916737152));
#44969=CARTESIAN_POINT('Ctrl Pts',(-84.5238825183441,-37.3968686554014,
110.051968213959));
#44970=CARTESIAN_POINT('Ctrl Pts',(-86.8672776685629,-39.641450956902,109.894019690767));
#44971=CARTESIAN_POINT('Ctrl Pts',(-90.0278340753366,-38.9062410803574,
109.736071167575));
#44972=CARTESIAN_POINT('Ctrl Pts',(-91.1399714370551,-35.8578315291262,
109.578122644382));
#44973=CARTESIAN_POINT('Ctrl Pts',(-89.1953484912358,-33.2601223888489,
109.42017412119));
#44974=CARTESIAN_POINT('Ctrl Pts',(-85.9570960092694,-33.4683778218109,
109.262225597997));
#44975=CARTESIAN_POINT('Ctrl Pts',(-84.3612384342726,-36.2937783632046,
109.104277074805));
#44976=CARTESIAN_POINT('Ctrl Pts',(-85.8546925179493,-39.1746205017346,
108.946328551612));
#44977=CARTESIAN_POINT('Ctrl Pts',(-89.0833863461416,-39.4989297598556,
108.78838002842));
#44978=CARTESIAN_POINT('Ctrl Pts',(-91.1199665993245,-36.9726699945077,
108.630431505227));
#44979=CARTESIAN_POINT('Ctrl Pts',(-90.1179172521685,-33.8863134122548,
108.472482982035));
#44980=CARTESIAN_POINT('Ctrl Pts',(-86.9857878737573,-33.0381876439953,
108.314534458842));
#44981=CARTESIAN_POINT('Ctrl Pts',(-84.5633398683062,-35.1972173145631,
108.15658593565));
#44982=CARTESIAN_POINT('Ctrl Pts',(-85.0470258043618,-38.4059688744449,
107.998637412457));
#44983=CARTESIAN_POINT('Ctrl Pts',(-87.9981118354098,-39.7549736321506,
107.840688889265));
#44984=CARTESIAN_POINT('Ctrl Pts',(-90.7413298339237,-38.0215233112373,
107.682740366072));
#44985=CARTESIAN_POINT('Ctrl Pts',(-90.7886816428431,-34.7764756582269,
107.52479184288));
#44986=CARTESIAN_POINT('Ctrl Pts',(-88.0988922939863,-32.963680253526,107.366843319688));
#44987=CARTESIAN_POINT('Ctrl Pts',(-85.1073027169643,-34.2233068092021,
107.208894796495));
#44988=CARTESIAN_POINT('Ctrl Pts',(-84.5333642445699,-37.4203403517654,
107.050946273303));
#44989=CARTESIAN_POINT('Ctrl Pts',(-86.099613541549,-38.8983441231523,106.945647257841));
#44990=CARTESIAN_POINT('Ctrl Pts',(-87.0226227342259,-39.1451036445258,
106.89299775011));
#44991=CARTESIAN_POINT('Ctrl Pts',(-85.4324929308759,-34.3576245177531,
122.321006749669));
#44992=CARTESIAN_POINT('Ctrl Pts',(-84.7717723668801,-35.1304094942464,
122.268357241939));
#44993=CARTESIAN_POINT('Ctrl Pts',(-84.2891219312635,-37.3707152652939,
122.163058226477));
#44994=CARTESIAN_POINT('Ctrl Pts',(-86.7195968954854,-39.8284996875276,
122.005109703284));
#44995=CARTESIAN_POINT('Ctrl Pts',(-90.1024648028703,-39.1298723584757,
121.847161180092));
#44996=CARTESIAN_POINT('Ctrl Pts',(-91.3686333769664,-35.9187008196384,
121.6892126569));
#44997=CARTESIAN_POINT('Ctrl Pts',(-89.3710243173134,-33.1013875956417,
121.531264133707));
#44998=CARTESIAN_POINT('Ctrl Pts',(-85.9203582039126,-33.2347629349336,
121.373315610515));
#44999=CARTESIAN_POINT('Ctrl Pts',(-84.1454681337529,-36.1967043012439,
121.215367087322));
#45000=CARTESIAN_POINT('Ctrl Pts',(-85.6554864122685,-39.3022906545617,
121.05741856413));
#45001=CARTESIAN_POINT('Ctrl Pts',(-89.0813771948967,-39.735498741376,120.899470040937));
#45002=CARTESIAN_POINT('Ctrl Pts',(-91.3169643139602,-37.1036893555134,
120.741521517745));
#45003=CARTESIAN_POINT('Ctrl Pts',(-90.3353211686605,-33.7929772197686,
120.583572994552));
#45004=CARTESIAN_POINT('Ctrl Pts',(-87.0264677882008,-32.8051168197105,
120.42562447136));
#45005=CARTESIAN_POINT('Ctrl Pts',(-84.3904437941137,-35.0357553412809,
120.267675948167));
#45006=CARTESIAN_POINT('Ctrl Pts',(-84.8172505627962,-38.4624483585915,
120.109727424975));
#45007=CARTESIAN_POINT('Ctrl Pts',(-87.9199160624454,-39.9783137967903,
119.951778901782));
#45008=CARTESIAN_POINT('Ctrl Pts',(-90.8853475149469,-38.20896438174,119.79383037859));
#45009=CARTESIAN_POINT('Ctrl Pts',(-91.0248785737008,-34.7586145328686,
119.635881855397));
#45010=CARTESIAN_POINT('Ctrl Pts',(-88.2120005926768,-32.7555919497842,
119.477933332205));
#45011=CARTESIAN_POINT('Ctrl Pts',(-84.9970645257212,-34.0159760806577,
119.319984809012));
#45012=CARTESIAN_POINT('Ctrl Pts',(-84.2949551082748,-37.3970150683708,
119.16203628582));
#45013=CARTESIAN_POINT('Ctrl Pts',(-86.7422536044908,-39.8332236430662,
119.004087762628));
#45014=CARTESIAN_POINT('Ctrl Pts',(-90.1200688946704,-39.1157656079981,
118.846139239435));
#45015=CARTESIAN_POINT('Ctrl Pts',(-91.3658385889551,-35.8951383313953,
118.688190716243));
#45016=CARTESIAN_POINT('Ctrl Pts',(-89.350061192869,-33.0913866196758,118.53024219305));
#45017=CARTESIAN_POINT('Ctrl Pts',(-85.9003807648513,-33.2465868748436,
118.372293669858));
#45018=CARTESIAN_POINT('Ctrl Pts',(-84.1445176314521,-36.2200237470817,
118.214345146665));
#45019=CARTESIAN_POINT('Ctrl Pts',(-85.6744594936806,-39.3157724566742,
118.056396623473));
#45020=CARTESIAN_POINT('Ctrl Pts',(-89.1030545960746,-39.7270118018916,
117.89844810028));
#45021=CARTESIAN_POINT('Ctrl Pts',(-91.3217000353283,-37.0808835755504,
117.740499577088));
#45022=CARTESIAN_POINT('Ctrl Pts',(-90.3188174687069,-33.7765517621971,
117.582551053895));
#45023=CARTESIAN_POINT('Ctrl Pts',(-87.0036900180789,-32.8099535202534,
117.424602530703));
#45024=CARTESIAN_POINT('Ctrl Pts',(-84.382042917881,-35.0574740779507,117.26665400751));
#45025=CARTESIAN_POINT('Ctrl Pts',(-84.8308438600728,-38.4813549008641,
117.108705484318));
#45026=CARTESIAN_POINT('Ctrl Pts',(-87.9431786800308,-39.9772673794902,
116.950756961126));
#45027=CARTESIAN_POINT('Ctrl Pts',(-90.8971880538853,-38.1889131655783,
116.792808437933));
#45028=CARTESIAN_POINT('Ctrl Pts',(-91.0145615244951,-34.7377386345482,
116.634859914741));
#45029=CARTESIAN_POINT('Ctrl Pts',(-88.1888801358119,-32.7528187709561,
116.476911391548));
#45030=CARTESIAN_POINT('Ctrl Pts',(-84.9821032637396,-34.0338200465123,
116.318962868356));
#45031=CARTESIAN_POINT('Ctrl Pts',(-84.3017179684765,-37.4192975645625,
116.161014345163));
#45032=CARTESIAN_POINT('Ctrl Pts',(-86.7646089042542,-39.839741824135,116.003065821971));
#45033=CARTESIAN_POINT('Ctrl Pts',(-90.1377477650451,-39.10060962956,115.845117298778));
#45034=CARTESIAN_POINT('Ctrl Pts',(-91.3628121351507,-35.8720496619689,
115.687168775586));
#45035=CARTESIAN_POINT('Ctrl Pts',(-89.3290734088453,-33.081299051764,115.529220252393));
#45036=CARTESIAN_POINT('Ctrl Pts',(-85.8804606359022,-33.2586465003749,
115.371271729201));
#45037=CARTESIAN_POINT('Ctrl Pts',(-84.1437261327331,-36.243296469925,115.213323206008));
#45038=CARTESIAN_POINT('Ctrl Pts',(-85.6935142529687,-39.3291576070487,
115.055374682816));
#45039=CARTESIAN_POINT('Ctrl Pts',(-89.1246792426668,-39.7183734709399,
114.897426159623));
#45040=CARTESIAN_POINT('Ctrl Pts',(-91.3262881598338,-37.0580538752739,
114.739477636431));
#45041=CARTESIAN_POINT('Ctrl Pts',(-90.3022091581829,-33.760229687478,114.581529113238));
#45042=CARTESIAN_POINT('Ctrl Pts',(-86.9809435225561,-32.814937799838,114.423580590046));
#45043=CARTESIAN_POINT('Ctrl Pts',(-84.3737817930479,-35.0792456171238,
114.265632066854));
#45044=CARTESIAN_POINT('Ctrl Pts',(-84.8445582165638,-38.5001741072118,
114.107683543661));
#45045=CARTESIAN_POINT('Ctrl Pts',(-87.9664341279196,-39.9760714509759,
113.949735020469));
#45046=CARTESIAN_POINT('Ctrl Pts',(-90.9088995858529,-38.1687864142141,
113.791786497276));
#45047=CARTESIAN_POINT('Ctrl Pts',(-91.0041106506971,-34.7169293736683,
113.633837974084));
#45048=CARTESIAN_POINT('Ctrl Pts',(-88.1657423456717,-32.7501941245154,
113.475889450891));
#45049=CARTESIAN_POINT('Ctrl Pts',(-84.9672568878733,-34.0517597016134,
113.317940927699));
#45050=CARTESIAN_POINT('Ctrl Pts',(-84.3086237643501,-37.4415361815354,
113.159992404506));
#45051=CARTESIAN_POINT('Ctrl Pts',(-86.7870055967793,-39.8461163253272,
113.002043881314));
#45052=CARTESIAN_POINT('Ctrl Pts',(-90.1553289542737,-39.0853404486122,
112.844095358121));
#45053=CARTESIAN_POINT('Ctrl Pts',(-91.3596374915171,-35.8489809008554,
112.686146834929));
#45054=CARTESIAN_POINT('Ctrl Pts',(-89.3080212851796,-33.0713464545818,
112.528198311736));
#45055=CARTESIAN_POINT('Ctrl Pts',(-85.8606183524605,-33.2708337842943,
112.370249788544));
#45056=CARTESIAN_POINT('Ctrl Pts',(-84.1430840844366,-36.2665737952763,
112.212301265351));
#45057=CARTESIAN_POINT('Ctrl Pts',(-85.7126545654799,-39.3424201308827,
112.054352742159));
#45058=CARTESIAN_POINT('Ctrl Pts',(-89.1462479767601,-39.7095964662598,
111.896404218967));
#45059=CARTESIAN_POINT('Ctrl Pts',(-91.3307296002859,-37.0351951852785,
111.738455695774));
#45060=CARTESIAN_POINT('Ctrl Pts',(-90.285496386025,-33.744014591179,111.580507172582));
#45061=CARTESIAN_POINT('Ctrl Pts',(-86.9582294999899,-32.8200680318722,
111.422558649389));
#45062=CARTESIAN_POINT('Ctrl Pts',(-84.3656606335548,-35.1010697521711,
111.264610126197));
#45063=CARTESIAN_POINT('Ctrl Pts',(-84.8583931283879,-38.5189048657011,
111.106661603004));
#45064=CARTESIAN_POINT('Ctrl Pts',(-87.9896814174328,-39.974726224009,110.948713079812));
#45065=CARTESIAN_POINT('Ctrl Pts',(-90.9204816423732,-38.1485848778524,
110.790764556619));
#45066=CARTESIAN_POINT('Ctrl Pts',(-90.9935263764774,-34.6961876471792,
110.632816033427));
#45067=CARTESIAN_POINT('Ctrl Pts',(-88.142588178909,-32.7477180991385,110.474867510234));
#45068=CARTESIAN_POINT('Ctrl Pts',(-84.9525260101083,-34.0697943170025,
110.316918987042));
#45069=CARTESIAN_POINT('Ctrl Pts',(-84.3156722087998,-37.4637299947607,
110.158970463849));
#45070=CARTESIAN_POINT('Ctrl Pts',(-86.8094427648148,-39.8523468925606,
110.001021940657));
#45071=CARTESIAN_POINT('Ctrl Pts',(-90.1728117242074,-39.0699586801214,
109.843073417464));
#45072=CARTESIAN_POINT('Ctrl Pts',(-91.3563148165642,-35.8259330275012,
109.685124894272));
#45073=CARTESIAN_POINT('Ctrl Pts',(-89.2869056328921,-33.0615291810096,
109.52717637108));
#45074=CARTESIAN_POINT('Ctrl Pts',(-85.840854849815,-33.2831483419104,109.369227847887));
#45075=CARTESIAN_POINT('Ctrl Pts',(-84.1425912719677,-36.2898545213693,
109.211279324695));
#45076=CARTESIAN_POINT('Ctrl Pts',(-85.731880137862,-39.3555599790778,109.053330801502));
#45077=CARTESIAN_POINT('Ctrl Pts',(-89.1677588894168,-39.7006801261729,
108.89538227831));
#45078=CARTESIAN_POINT('Ctrl Pts',(-91.3350262706245,-37.0123105530422,
108.737433755117));
#45079=CARTESIAN_POINT('Ctrl Pts',(-90.2686755284635,-33.727902812646,108.579485231925));
#45080=CARTESIAN_POINT('Ctrl Pts',(-86.9355577566776,-32.8253529082965,
108.421536708732));
#45081=CARTESIAN_POINT('Ctrl Pts',(-84.3576615325144,-35.1229272723648,
108.26358818554));
#45082=CARTESIAN_POINT('Ctrl Pts',(-84.8723855412168,-38.5375840624727,
108.105639662347));
#45083=CARTESIAN_POINT('Ctrl Pts',(-88.0128424342027,-39.9731543052364,
107.947691139155));
#45084=CARTESIAN_POINT('Ctrl Pts',(-90.9320924261582,-38.1284686702913,
107.789742615962));
#45085=CARTESIAN_POINT('Ctrl Pts',(-90.9824827953822,-34.6751866708012,
107.63179409277));
#45086=CARTESIAN_POINT('Ctrl Pts',(-88.1200899635817,-32.7460643868788,
107.473845569577));
#45087=CARTESIAN_POINT('Ctrl Pts',(-84.9365304165877,-34.0865210383432,
107.315897046385));
#45088=CARTESIAN_POINT('Ctrl Pts',(-84.3257623763415,-37.4887078672662,
107.157948523192));
#45089=CARTESIAN_POINT('Ctrl Pts',(-85.9925177162683,-39.0615549760519,
107.052649507731));
#45090=CARTESIAN_POINT('Ctrl Pts',(-86.97475630604,-39.3241490284294,107.));
#45091=CARTESIAN_POINT('Ctrl Pts',(-85.855089591907,-34.7189388713087,122.));
#45092=CARTESIAN_POINT('Ctrl Pts',(-85.7934813914369,-34.7768354517112,
122.));
#45093=CARTESIAN_POINT('Ctrl Pts',(-85.735242344367,-34.8378827916466,122.));
#45094=CARTESIAN_POINT('Ctrl Pts',(-85.6803700642034,-34.9016960722485,
122.));
#45095=CARTESIAN_POINT('Ctrl Pts',(-85.6240448547982,-34.9671990253247,
122.));
#45096=CARTESIAN_POINT('Ctrl Pts',(-85.5712666289892,-35.0356167652744,
122.));
#45097=CARTESIAN_POINT('Ctrl Pts',(-85.5220583134545,-35.1065816394062,
122.));
#45098=CARTESIAN_POINT('Ctrl Pts',(-85.4715004197893,-35.1794927830071,
122.));
#45099=CARTESIAN_POINT('Ctrl Pts',(-85.4247104044215,-35.2550932475831,
122.));
#45100=CARTESIAN_POINT('Ctrl Pts',(-85.3817472004119,-35.3330272726362,
122.));
#45101=CARTESIAN_POINT('Ctrl Pts',(-85.3628372305493,-35.3673294179019,
122.));
#45102=CARTESIAN_POINT('Ctrl Pts',(-85.3446690988358,-35.402084133033,122.));
#45103=CARTESIAN_POINT('Ctrl Pts',(-85.3272502554093,-35.4372631605433,
122.));
#45104=CARTESIAN_POINT('Ctrl Pts',(-85.3173194106968,-35.4573194553726,
122.));
#45105=CARTESIAN_POINT('Ctrl Pts',(-85.3076321412892,-35.4775136884896,
122.));
#45106=CARTESIAN_POINT('Ctrl Pts',(-85.2981900621096,-35.497840771842,122.));
#45107=CARTESIAN_POINT('Ctrl Pts',(-85.2896844749579,-35.5161517577706,
122.));
#45108=CARTESIAN_POINT('Ctrl Pts',(-85.281375478207,-35.5345762757094,122.));
#45109=CARTESIAN_POINT('Ctrl Pts',(-85.2732779128575,-35.5530788516544,
122.));
#45110=CARTESIAN_POINT('Ctrl Pts',(-85.2367162849915,-35.636620541911,122.));
#45111=CARTESIAN_POINT('Ctrl Pts',(-85.2044148369174,-35.7218457754668,
122.));
#45112=CARTESIAN_POINT('Ctrl Pts',(-85.1763986040086,-35.8083557745312,
122.));
#45113=CARTESIAN_POINT('Ctrl Pts',(-85.147919276174,-35.8962957424901,122.));
#45114=CARTESIAN_POINT('Ctrl Pts',(-85.1238675061027,-35.9855640551364,
122.));
#45115=CARTESIAN_POINT('Ctrl Pts',(-85.1043086662742,-36.0757789555843,
122.));
#45116=CARTESIAN_POINT('Ctrl Pts',(-85.0853401900751,-36.1632708112854,
122.));
#45117=CARTESIAN_POINT('Ctrl Pts',(-85.0705973519178,-36.2516538909537,
122.));
#45118=CARTESIAN_POINT('Ctrl Pts',(-85.0601805241994,-36.3406018388456,
122.));
#45119=CARTESIAN_POINT('Ctrl Pts',(-85.0558116903908,-36.3779067470632,
122.));
#45120=CARTESIAN_POINT('Ctrl Pts',(-85.0522043074793,-36.4153112064065,
122.));
#45121=CARTESIAN_POINT('Ctrl Pts',(-85.0493681149686,-36.4527917592161,
122.));
#45122=CARTESIAN_POINT('Ctrl Pts',(-85.0475889875222,-36.4763030970235,
122.));
#45123=CARTESIAN_POINT('Ctrl Pts',(-85.0461133503525,-36.4998443829401,
122.));
#45124=CARTESIAN_POINT('Ctrl Pts',(-85.0449439035519,-36.5234098595724,
122.));
#45125=CARTESIAN_POINT('Ctrl Pts',(-85.0442595199509,-36.5372008466837,
122.));
#45126=CARTESIAN_POINT('Ctrl Pts',(-85.0436802910536,-36.5509951721818,
122.));
#45127=CARTESIAN_POINT('Ctrl Pts',(-85.0432067176554,-36.5647838451762,
122.));
#45128=CARTESIAN_POINT('Ctrl Pts',(-85.0398793341044,-36.6616647170585,
122.));
#45129=CARTESIAN_POINT('Ctrl Pts',(-85.0417578653667,-36.7583805840727,
122.));
#45130=CARTESIAN_POINT('Ctrl Pts',(-85.0489066930308,-36.8545116797471,
122.));
#45131=CARTESIAN_POINT('Ctrl Pts',(-85.0560555206949,-36.9506427754215,
122.));
#45132=CARTESIAN_POINT('Ctrl Pts',(-85.0684742144477,-37.0461901437907,
122.));
#45133=CARTESIAN_POINT('Ctrl Pts',(-85.0862796188093,-37.1407528038591,
122.));
#45134=CARTESIAN_POINT('Ctrl Pts',(-85.1033376429253,-37.2313462047815,
122.));
#45135=CARTESIAN_POINT('Ctrl Pts',(-85.1253395228826,-37.3210367972729,
122.));
#45136=CARTESIAN_POINT('Ctrl Pts',(-85.1520106494849,-37.4095852418723,
122.));
#45137=CARTESIAN_POINT('Ctrl Pts',(-85.1608799953067,-37.4390315711875,
122.));
#45138=CARTESIAN_POINT('Ctrl Pts',(-85.1702661253978,-37.4683515588674,
122.));
#45139=CARTESIAN_POINT('Ctrl Pts',(-85.1801601896715,-37.4975362287825,
122.));
#45140=CARTESIAN_POINT('Ctrl Pts',(-85.1894804986475,-37.5250284840829,
122.));
#45141=CARTESIAN_POINT('Ctrl Pts',(-85.1992515460373,-37.5524006617149,
122.));
#45142=CARTESIAN_POINT('Ctrl Pts',(-85.2094664085399,-37.5796451334156,
122.));
#45143=CARTESIAN_POINT('Ctrl Pts',(-85.2146241863597,-37.593401650629,122.));
#45144=CARTESIAN_POINT('Ctrl Pts',(-85.2198920425091,-37.607117334446,122.));
#45145=CARTESIAN_POINT('Ctrl Pts',(-85.2252673071018,-37.6207878666389,
122.));
#45146=CARTESIAN_POINT('Ctrl Pts',(-85.2595186282914,-37.7078968416282,
122.));
#45147=CARTESIAN_POINT('Ctrl Pts',(-85.2981434489407,-37.793217001783,122.));
#45148=CARTESIAN_POINT('Ctrl Pts',(-85.3408117833009,-37.8765139323352,
122.));
#45149=CARTESIAN_POINT('Ctrl Pts',(-85.3850415874262,-37.9628591571441,
122.));
#45150=CARTESIAN_POINT('Ctrl Pts',(-85.4336163991975,-38.047031091085,122.));
#45151=CARTESIAN_POINT('Ctrl Pts',(-85.4862245077739,-38.1287651551131,
122.));
#45152=CARTESIAN_POINT('Ctrl Pts',(-85.5393955693074,-38.2113738453971,
122.));
#45153=CARTESIAN_POINT('Ctrl Pts',(-85.5966871241838,-38.2914930335655,
122.));
#45154=CARTESIAN_POINT('Ctrl Pts',(-85.6578288553816,-38.3688341911083,
122.));
#45155=CARTESIAN_POINT('Ctrl Pts',(-85.6805177136348,-38.3975344343995,
122.));
#45156=CARTESIAN_POINT('Ctrl Pts',(-85.7037372340462,-38.4258519148351,
122.));
#45157=CARTESIAN_POINT('Ctrl Pts',(-85.727475197759,-38.4537710002837,122.));
#45158=CARTESIAN_POINT('Ctrl Pts',(-85.7482304515194,-38.4781820117021,
122.));
#45159=CARTESIAN_POINT('Ctrl Pts',(-85.7693820616618,-38.5022884505914,
122.));
#45160=CARTESIAN_POINT('Ctrl Pts',(-85.790922350481,-38.5260794851929,122.));
#45161=CARTESIAN_POINT('Ctrl Pts',(-85.8026858188802,-38.5390721189532,
122.));
#45162=CARTESIAN_POINT('Ctrl Pts',(-85.8145605316052,-38.5519654355969,
122.));
#45163=CARTESIAN_POINT('Ctrl Pts',(-85.8265391633365,-38.5647518126357,
122.));
#45164=CARTESIAN_POINT('Ctrl Pts',(-85.8955499468916,-38.6384161440946,
122.));
#45165=CARTESIAN_POINT('Ctrl Pts',(-85.9680631281327,-38.7085959444771,
122.));
#45166=CARTESIAN_POINT('Ctrl Pts',(-86.0437701857546,-38.7749999993731,
122.));
#45167=CARTESIAN_POINT('Ctrl Pts',(-86.1059643211302,-38.8295516212355,
122.));
#45168=CARTESIAN_POINT('Ctrl Pts',(-86.1703150292066,-38.8815550093779,
122.));
#45169=CARTESIAN_POINT('Ctrl Pts',(-86.2366735424928,-38.9308353738164,
122.));
#45170=CARTESIAN_POINT('Ctrl Pts',(-86.26129111213,-38.9491173205212,122.));
#45171=CARTESIAN_POINT('Ctrl Pts',(-86.286185186655,-38.9670243657543,122.));
#45172=CARTESIAN_POINT('Ctrl Pts',(-86.3113487775637,-38.9845470206273,
122.));
#45173=CARTESIAN_POINT('Ctrl Pts',(-86.3281596610916,-38.9962532715847,
122.));
#45174=CARTESIAN_POINT('Ctrl Pts',(-86.3450919689086,-39.0077885956498,
122.));
#45175=CARTESIAN_POINT('Ctrl Pts',(-86.3621285565829,-39.0191403402542,
122.));
#45176=CARTESIAN_POINT('Ctrl Pts',(-86.447039035685,-39.0757175194072,122.));
#45177=CARTESIAN_POINT('Ctrl Pts',(-86.5346187926945,-39.1277953993686,
122.));
#45178=CARTESIAN_POINT('Ctrl Pts',(-86.6245774697256,-39.1750660640383,
122.));
#45179=CARTESIAN_POINT('Ctrl Pts',(-86.7080355169804,-39.218920837096,122.));
#45180=CARTESIAN_POINT('Ctrl Pts',(-86.7935419058644,-39.2586383254852,
122.));
#45181=CARTESIAN_POINT('Ctrl Pts',(-86.8808924954566,-39.2939436042708,
122.));
#45182=CARTESIAN_POINT('Ctrl Pts',(-86.9113226722305,-39.3062428443735,
122.));
#45183=CARTESIAN_POINT('Ctrl Pts',(-86.9419768694861,-39.3180063257841,
122.));
#45184=CARTESIAN_POINT('Ctrl Pts',(-86.9728421809426,-39.3292377709744,
122.));
#45185=CARTESIAN_POINT('Ctrl Pts',(-90.2867226440827,-36.3571243050301,
120.387416697508));
#45186=CARTESIAN_POINT('Ctrl Pts',(-90.2883050038283,-36.5314907278085,
120.398449387697));
#45187=CARTESIAN_POINT('Ctrl Pts',(-90.271719409744,-36.7055581052199,120.409482077886));
#45188=CARTESIAN_POINT('Ctrl Pts',(-90.2358478507299,-36.8755557414102,
120.420514768075));
#45189=CARTESIAN_POINT('Ctrl Pts',(-90.0646638610358,-37.6868077304914,
120.473164275806));
#45190=CARTESIAN_POINT('Ctrl Pts',(-89.4542749914255,-38.4053783209051,
120.525813783537));
#45191=CARTESIAN_POINT('Ctrl Pts',(-88.6813900818485,-38.7055235825695,
120.578463291268));
#45192=CARTESIAN_POINT('Ctrl Pts',(-87.9085051722716,-39.005668844234,120.631112798999));
#45193=CARTESIAN_POINT('Ctrl Pts',(-86.973124222728,-38.8873887771492,120.683762306729));
#45194=CARTESIAN_POINT('Ctrl Pts',(-86.2992914012199,-38.4042850949718,
120.73641181446));
#45195=CARTESIAN_POINT('Ctrl Pts',(-85.6254585797119,-37.9211814127945,
120.789061322191));
#45196=CARTESIAN_POINT('Ctrl Pts',(-85.2131738862394,-37.0732541155246,
120.841710829922));
#45197=CARTESIAN_POINT('Ctrl Pts',(-85.2493332450303,-36.2449367230749,
120.894360337653));
#45198=CARTESIAN_POINT('Ctrl Pts',(-85.2854926038213,-35.4166193306253,
120.947009845384));
#45199=CARTESIAN_POINT('Ctrl Pts',(-85.7700960148757,-34.6079118429959,
120.999659353114));
#45200=CARTESIAN_POINT('Ctrl Pts',(-86.4834704355749,-34.1853501702909,
121.052308860845));
#45201=CARTESIAN_POINT('Ctrl Pts',(-87.196844856274,-33.7627884975859,121.104958368576));
#45202=CARTESIAN_POINT('Ctrl Pts',(-88.138990286618,-33.7263726398051,121.157607876307));
#45203=CARTESIAN_POINT('Ctrl Pts',(-88.8827695148683,-34.0927743330292,
121.210257384038));
#45204=CARTESIAN_POINT('Ctrl Pts',(-89.6265487431185,-34.4591760262532,
121.262906891768));
#45205=CARTESIAN_POINT('Ctrl Pts',(-90.1719617692751,-35.228395270482,121.315556399499));
#45206=CARTESIAN_POINT('Ctrl Pts',(-90.2718154335226,-36.0513826567645,
121.36820590723));
#45207=CARTESIAN_POINT('Ctrl Pts',(-90.2839603258177,-36.1514800667287,
121.374609503989));
#45208=CARTESIAN_POINT('Ctrl Pts',(-90.2895140119517,-36.2523728744322,
121.381013100749));
#45209=CARTESIAN_POINT('Ctrl Pts',(-90.2887582439581,-36.3533471924086,
121.387416697508));
#45210=CARTESIAN_POINT('Ctrl Pts',(-88.5623548711056,-39.3241490284291,
122.));
#45211=CARTESIAN_POINT('Ctrl Pts',(-89.5445934608772,-39.0615549760513,
121.947350492269));
#45212=CARTESIAN_POINT('Ctrl Pts',(-91.2113487416866,-37.4887074581619,
121.842051476808));
#45213=CARTESIAN_POINT('Ctrl Pts',(-90.6005808115744,-34.0865211443674,
121.684102953615));
#45214=CARTESIAN_POINT('Ctrl Pts',(-87.417021209647,-32.7460642638912,121.526154430423));
#45215=CARTESIAN_POINT('Ctrl Pts',(-84.5546283385357,-34.6751866943283,
121.36820590723));
#45216=CARTESIAN_POINT('Ctrl Pts',(-84.6050187185395,-38.1284686676829,
121.210257384038));
#45217=CARTESIAN_POINT('Ctrl Pts',(-87.5242687364515,-39.9731543606838,
121.052308860845));
#45218=CARTESIAN_POINT('Ctrl Pts',(-90.6647256725097,-38.5375840815526,
120.894360337653));
#45219=CARTESIAN_POINT('Ctrl Pts',(-91.1794496835569,-35.1229272613484,
120.73641181446));
#45220=CARTESIAN_POINT('Ctrl Pts',(-88.6015534311407,-32.8253528646868,
120.578463291268));
#45221=CARTESIAN_POINT('Ctrl Pts',(-85.2684356186448,-33.7279027825514,
120.420514768075));
#45222=CARTESIAN_POINT('Ctrl Pts',(-84.2020848645994,-37.0123105603124,
120.262566244883));
#45223=CARTESIAN_POINT('Ctrl Pts',(-86.3693522710391,-39.7006801660047,
120.10461772169));
#45224=CARTESIAN_POINT('Ctrl Pts',(-89.8052310634475,-39.3555600144301,
119.946669198498));
#45225=CARTESIAN_POINT('Ctrl Pts',(-91.3945199480195,-36.2898545206677,
119.788720675305));
#45226=CARTESIAN_POINT('Ctrl Pts',(-89.6962563501485,-33.2831483055448,
119.630772152113));
#45227=CARTESIAN_POINT('Ctrl Pts',(-86.2502055262826,-33.0615291420779,
119.47282362892));
#45228=CARTESIAN_POINT('Ctrl Pts',(-84.1807963181542,-35.8259330212369,
119.314875105728));
#45229=CARTESIAN_POINT('Ctrl Pts',(-85.3642994245004,-39.0699587122372,
119.156926582536));
#45230=CARTESIAN_POINT('Ctrl Pts',(-88.7276684236758,-39.8523469339212,
118.998978059343));
#45231=CARTESIAN_POINT('Ctrl Pts',(-91.2214390091811,-37.4637300078743,
118.841029536151));
#45232=CARTESIAN_POINT('Ctrl Pts',(-90.5845852003404,-34.069794289975,118.683081012958));
#45233=CARTESIAN_POINT('Ctrl Pts',(-87.3945229938104,-32.7477180564772,
118.525132489766));
#45234=CARTESIAN_POINT('Ctrl Pts',(-84.5435847625254,-34.6961876275626,
118.367183966573));
#45235=CARTESIAN_POINT('Ctrl Pts',(-84.6166294974947,-38.1485848990669,
118.209235443381));
#45236=CARTESIAN_POINT('Ctrl Pts',(-87.5474297570977,-39.9747262668198,
118.051286920188));
#45237=CARTESIAN_POINT('Ctrl Pts',(-90.6787180831755,-38.518904891293,117.893338396996));
#45238=CARTESIAN_POINT('Ctrl Pts',(-91.1714505838346,-35.1010697373407,
117.735389873803));
#45239=CARTESIAN_POINT('Ctrl Pts',(-88.5788816867368,-32.8200679900657,
117.577441350611));
#45240=CARTESIAN_POINT('Ctrl Pts',(-85.2516147613512,-33.7440145603012,
117.419492827418));
#45241=CARTESIAN_POINT('Ctrl Pts',(-84.2063815347296,-37.0351951933252,
117.261544304226));
#45242=CARTESIAN_POINT('Ctrl Pts',(-86.390863184092,-39.7095965059354,117.103595781033));
#45243=CARTESIAN_POINT('Ctrl Pts',(-89.8244566359805,-39.3424201662145,
116.945647257841));
#45244=CARTESIAN_POINT('Ctrl Pts',(-91.3940271355856,-36.26657379423,116.787698734648));
#45245=CARTESIAN_POINT('Ctrl Pts',(-89.6764928472477,-33.2708337478186,
116.629750211456));
#45246=CARTESIAN_POINT('Ctrl Pts',(-86.2290898737567,-33.071346415748,116.471801688264));
#45247=CARTESIAN_POINT('Ctrl Pts',(-84.1774736431561,-35.848980894873,116.313853165071));
#45248=CARTESIAN_POINT('Ctrl Pts',(-85.3817821946438,-39.0853404809052,
116.155904641879));
#45249=CARTESIAN_POINT('Ctrl Pts',(-88.7501055919751,-39.8461163666165,
115.997956118686));
#45250=CARTESIAN_POINT('Ctrl Pts',(-91.2284874537149,-37.4415361943852,
115.840007595494));
#45251=CARTESIAN_POINT('Ctrl Pts',(-90.5698543224008,-34.0517596743733,
115.682059072301));
#45252=CARTESIAN_POINT('Ctrl Pts',(-87.3713688267741,-32.750194081883,115.524110549109));
#45253=CARTESIAN_POINT('Ctrl Pts',(-84.5330004881805,-34.7169293542972,
115.366162025916));
#45254=CARTESIAN_POINT('Ctrl Pts',(-84.628211554152,-38.1687864356674,115.208213502724));
#45255=CARTESIAN_POINT('Ctrl Pts',(-87.5706770468859,-39.9760714938026,
115.050264979531));
#45256=CARTESIAN_POINT('Ctrl Pts',(-90.6925529951631,-38.5001741325821,
114.892316456339));
#45257=CARTESIAN_POINT('Ctrl Pts',(-91.1633294242455,-35.0792456020353,
114.734367933146));
#45258=CARTESIAN_POINT('Ctrl Pts',(-88.556167663902,-32.8149377579708,114.576419409954));
#45259=CARTESIAN_POINT('Ctrl Pts',(-85.2349019889955,-33.760229656792,114.418470886761));
#45260=CARTESIAN_POINT('Ctrl Pts',(-84.2108229752343,-37.058053883591,114.260522363569));
#45261=CARTESIAN_POINT('Ctrl Pts',(-86.4124319184404,-39.7183735107193,
114.102573840377));
#45262=CARTESIAN_POINT('Ctrl Pts',(-89.8435969487181,-39.3291576422236,
113.944625317184));
#45263=CARTESIAN_POINT('Ctrl Pts',(-91.3933850872816,-36.2432964686034,
113.786676793992));
#45264=CARTESIAN_POINT('Ctrl Pts',(-89.6566505635712,-33.2586464637551,
113.628728270799));
#45265=CARTESIAN_POINT('Ctrl Pts',(-86.2080377498421,-33.081299013048,113.470779747607));
#45266=CARTESIAN_POINT('Ctrl Pts',(-84.1742989994849,-35.8720496562593,
113.312831224414));
#45267=CARTESIAN_POINT('Ctrl Pts',(-85.3993633840806,-39.1006096620336,
113.154882701222));
#45268=CARTESIAN_POINT('Ctrl Pts',(-88.7725022847651,-39.8397418653489,
112.996934178029));
#45269=CARTESIAN_POINT('Ctrl Pts',(-91.23539324967,-37.4192975771493,112.838985654837));
#45270=CARTESIAN_POINT('Ctrl Pts',(-90.555007946359,-34.0338200190599,112.681037131644));
#45271=CARTESIAN_POINT('Ctrl Pts',(-87.3482310363601,-32.7528187283548,
112.523088608452));
#45272=CARTESIAN_POINT('Ctrl Pts',(-84.5225496142588,-34.7377386154233,
112.365140085259));
#45273=CARTESIAN_POINT('Ctrl Pts',(-84.6399230862583,-38.1889131872696,
112.207191562067));
#45274=CARTESIAN_POINT('Ctrl Pts',(-87.5939324950497,-39.9772674223311,
112.049243038875));
#45275=CARTESIAN_POINT('Ctrl Pts',(-90.7062673518165,-38.4813549260119,
111.891294515682));
#45276=CARTESIAN_POINT('Ctrl Pts',(-91.1550682993145,-35.0574740626047,
111.733345992489));
#45277=CARTESIAN_POINT('Ctrl Pts',(-88.5334211681103,-32.8099534783274,
111.575397469297));
#45278=CARTESIAN_POINT('Ctrl Pts',(-85.218293678275,-33.7765517317041,111.417448946105));
#45279=CARTESIAN_POINT('Ctrl Pts',(-84.2154110997942,-37.0808835841375,
111.259500422912));
#45280=CARTESIAN_POINT('Ctrl Pts',(-86.4340565652882,-39.7270118417731,
111.10155189972));
#45281=CARTESIAN_POINT('Ctrl Pts',(-89.8626517082315,-39.3157724916908,
110.943603376527));
#45282=CARTESIAN_POINT('Ctrl Pts',(-91.3925935885532,-36.2200237454849,
110.785654853335));
#45283=CARTESIAN_POINT('Ctrl Pts',(-89.6367304343865,-33.2465868380812,
110.627706330142));
#45284=CARTESIAN_POINT('Ctrl Pts',(-86.18704996557,-33.091386581079,110.46975780695));
#45285=CARTESIAN_POINT('Ctrl Pts',(-84.1712725456449,-35.8951383259589,
110.311809283757));
#45286=CARTESIAN_POINT('Ctrl Pts',(-85.4170422546641,-39.1157656406506,
110.153860760565));
#45287=CARTESIAN_POINT('Ctrl Pts',(-88.794857584793,-39.8332236842038,109.995912237372));
#45288=CARTESIAN_POINT('Ctrl Pts',(-91.2421561099518,-37.3970150806926,
109.83796371418));
#45289=CARTESIAN_POINT('Ctrl Pts',(-90.5400466842003,-34.0159760529972,
109.680015190987));
#45290=CARTESIAN_POINT('Ctrl Pts',(-87.3251105792218,-32.7555919072101,
109.522066667795));
#45291=CARTESIAN_POINT('Ctrl Pts',(-84.5122325649308,-34.7586145140015,
109.364118144603));
#45292=CARTESIAN_POINT('Ctrl Pts',(-84.6517636253375,-38.2089644036472,
109.20616962141));
#45293=CARTESIAN_POINT('Ctrl Pts',(-87.6171951129081,-39.9783138396851,
109.048221098218));
#45294=CARTESIAN_POINT('Ctrl Pts',(-90.7198606492592,-38.4624483834354,
108.890272575025));
#45295=CARTESIAN_POINT('Ctrl Pts',(-91.1466674229692,-35.0357553258326,
108.732324051833));
#45296=CARTESIAN_POINT('Ctrl Pts',(-88.5106433977503,-32.8051167774314,
108.57437552864));
#45297=CARTESIAN_POINT('Ctrl Pts',(-85.2017899780534,-33.7929771900336,
108.416427005448));
#45298=CARTESIAN_POINT('Ctrl Pts',(-84.2201468213852,-37.1036893633033,
108.258478482255));
#45299=CARTESIAN_POINT('Ctrl Pts',(-86.4557339663443,-39.7354987833619,
108.100529959063));
#45300=CARTESIAN_POINT('Ctrl Pts',(-89.8816247907176,-39.3022906856884,
107.94258143587));
#45301=CARTESIAN_POINT('Ctrl Pts',(-91.3916430843464,-36.1967043062389,
107.784632912678));
#45302=CARTESIAN_POINT('Ctrl Pts',(-89.6167529992886,-33.2347628855613,
107.626684389485));
#45303=CARTESIAN_POINT('Ctrl Pts',(-86.1660868316116,-33.1013875794135,
107.468735866293));
#45304=CARTESIAN_POINT('Ctrl Pts',(-84.1684777778814,-35.918700775767,107.3107873431));
#45305=CARTESIAN_POINT('Ctrl Pts',(-85.434646301384,-39.1298724576138,107.152838819908));
#45306=CARTESIAN_POINT('Ctrl Pts',(-88.8175143837618,-39.8284996290504,
106.994890296716));
#45307=CARTESIAN_POINT('Ctrl Pts',(-91.2479889654302,-37.3707155689491,
106.836941773523));
#45308=CARTESIAN_POINT('Ctrl Pts',(-90.7653388102639,-35.1304094942453,
106.731642758061));
#45309=CARTESIAN_POINT('Ctrl Pts',(-90.1046182462678,-34.3576245177522,
106.678993250331));
#45310=CARTESIAN_POINT('Ctrl Pts',(-88.5144884429196,-39.1451036445255,
122.10700224989));
#45311=CARTESIAN_POINT('Ctrl Pts',(-89.4374976355964,-38.8983441231517,
122.054352742159));
#45312=CARTESIAN_POINT('Ctrl Pts',(-91.003746877023,-37.4203399673302,121.949053726697));
#45313=CARTESIAN_POINT('Ctrl Pts',(-90.4298085081212,-34.223306908833,121.791105203505));
#45314=CARTESIAN_POINT('Ctrl Pts',(-87.4382188794787,-32.9636801379545,
121.633156680312));
#45315=CARTESIAN_POINT('Ctrl Pts',(-84.7484294936813,-34.7764756803353,
121.47520815712));
#45316=CARTESIAN_POINT('Ctrl Pts',(-84.7957813127306,-38.0215233087861,
121.317259633928));
#45317=CARTESIAN_POINT('Ctrl Pts',(-87.5389993356358,-39.7549736842546,
121.159311110735));
#45318=CARTESIAN_POINT('Ctrl Pts',(-90.4900854071588,-38.4059688923743,
121.001362587543));
#45319=CARTESIAN_POINT('Ctrl Pts',(-90.9737713454176,-35.1972173042109,
120.84341406435));
#45320=CARTESIAN_POINT('Ctrl Pts',(-88.5513233134175,-33.0381876030153,
120.685465541158));
#45321=CARTESIAN_POINT('Ctrl Pts',(-85.4191938967511,-33.8863133839749,
120.527517017965));
#45322=CARTESIAN_POINT('Ctrl Pts',(-84.4171445384271,-36.9726700013395,
120.369568494773));
#45323=CARTESIAN_POINT('Ctrl Pts',(-86.4537248153207,-39.4989297972856,
120.21161997158));
#45324=CARTESIAN_POINT('Ctrl Pts',(-89.6824186819031,-39.1746205349551,
120.053671448388));
#45325=CARTESIAN_POINT('Ctrl Pts',(-91.175872783131,-36.2937783625453,119.895722925195));
#45326=CARTESIAN_POINT('Ctrl Pts',(-89.5800151893182,-33.4683777876381,
119.737774402003));
#45327=CARTESIAN_POINT('Ctrl Pts',(-86.3417626690224,-33.2601223522649,
119.57982587881));
#45328=CARTESIAN_POINT('Ctrl Pts',(-84.3971397002217,-35.8578315232397,
119.421877355618));
#45329=CARTESIAN_POINT('Ctrl Pts',(-85.5092770750858,-38.9062411105366,
119.263928832425));
#45330=CARTESIAN_POINT('Ctrl Pts',(-88.6698335192436,-39.6414509957686,
119.105980309233));
#45331=CARTESIAN_POINT('Ctrl Pts',(-91.0132286971742,-37.3968686677242,
118.94803178604));
#45332=CARTESIAN_POINT('Ctrl Pts',(-90.4147774389237,-34.2075886907448,
118.790083262848));
#45333=CARTESIAN_POINT('Ctrl Pts',(-87.4170773154511,-32.965234206157,118.632134739655));
#45334=CARTESIAN_POINT('Ctrl Pts',(-84.7380518499156,-34.7962102485267,
118.474186216463));
#45335=CARTESIAN_POINT('Ctrl Pts',(-84.8066919568667,-38.0404265230182,
118.316237693271));
#45336=CARTESIAN_POINT('Ctrl Pts',(-87.5607637370663,-39.7564508037941,
118.158289170078));
#45337=CARTESIAN_POINT('Ctrl Pts',(-90.5032340696187,-38.3884160650867,
118.000340646886));
#45338=CARTESIAN_POINT('Ctrl Pts',(-90.9662545947489,-35.1766777980275,
117.842392123693));
#45339=CARTESIAN_POINT('Ctrl Pts',(-88.5300186846675,-33.0332214085406,
117.684443600501));
#45340=CARTESIAN_POINT('Ctrl Pts',(-85.4033873441759,-33.9014536147989,
117.526495077308));
#45341=CARTESIAN_POINT('Ctrl Pts',(-84.4211821175544,-36.9941746814262,
117.368546554116));
#45342=CARTESIAN_POINT('Ctrl Pts',(-86.4739386113346,-39.5073084781955,
117.210598030923));
#45343=CARTESIAN_POINT('Ctrl Pts',(-89.7004849443846,-39.1622730250734,
117.052649507731));
#45344=CARTESIAN_POINT('Ctrl Pts',(-91.1754096874929,-36.2719014736327,
116.894700984538));
#45345=CARTESIAN_POINT('Ctrl Pts',(-89.5614434338944,-33.4568058028847,
116.736752461346));
#45346=CARTESIAN_POINT('Ctrl Pts',(-86.3219202991608,-33.2693476402335,
116.578803938153));
#45347=CARTESIAN_POINT('Ctrl Pts',(-84.3940173839133,-35.8794896004719,
116.420855414961));
#45348=CARTESIAN_POINT('Ctrl Pts',(-85.5257056268899,-38.9206953521314,
116.262906891768));
#45349=CARTESIAN_POINT('Ctrl Pts',(-88.6909177169257,-39.6355961342739,
116.104958368576));
#45350=CARTESIAN_POINT('Ctrl Pts',(-91.0198521175596,-37.3760131504555,
115.947009845384));
#45351=CARTESIAN_POINT('Ctrl Pts',(-90.4009348390746,-34.1906415699941,
115.789061322191));
#45352=CARTESIAN_POINT('Ctrl Pts',(-87.395319354355,-32.967560926197,115.631112798999));
#45353=CARTESIAN_POINT('Ctrl Pts',(-84.7281058117332,-34.8157012404785,
115.473164275806));
#45354=CARTESIAN_POINT('Ctrl Pts',(-84.8175756106714,-38.0594098985265,
115.315215752614));
#45355=CARTESIAN_POINT('Ctrl Pts',(-87.5826092055734,-39.7577149130283,
115.157267229421));
#45356=CARTESIAN_POINT('Ctrl Pts',(-90.5162347306368,-38.3708147789471,
114.999318706229));
#45357=CARTESIAN_POINT('Ctrl Pts',(-90.9586231444738,-35.1561696671936,
114.841370183036));
#45358=CARTESIAN_POINT('Ctrl Pts',(-88.508674326894,-33.0284005315831,114.683421659844));
#45359=CARTESIAN_POINT('Ctrl Pts',(-85.3876823589715,-33.9166909342007,
114.525473136651));
#45360=CARTESIAN_POINT('Ctrl Pts',(-84.4253557373423,-37.0156549831244,
114.367524613459));
#45361=CARTESIAN_POINT('Ctrl Pts',(-86.4942067419958,-39.515556225926,114.209576090266));
#45362=CARTESIAN_POINT('Ctrl Pts',(-89.7184710882722,-39.1498102368169,
114.051627567074));
#45363=CARTESIAN_POINT('Ctrl Pts',(-91.1748063549696,-36.2500277804607,
113.893679043881));
#45364=CARTESIAN_POINT('Ctrl Pts',(-89.5427976482087,-33.445353417139,113.735730520689));
#45365=CARTESIAN_POINT('Ctrl Pts',(-86.3021376271084,-33.2787000917606,
113.577781997497));
#45366=CARTESIAN_POINT('Ctrl Pts',(-84.3910341725811,-35.9011673059144,
113.419833474304));
#45367=CARTESIAN_POINT('Ctrl Pts',(-85.5422266632625,-38.935043795262,113.261884951112));
#45368=CARTESIAN_POINT('Ctrl Pts',(-88.7119638797888,-39.6296060180944,
113.103936427919));
#45369=CARTESIAN_POINT('Ctrl Pts',(-91.0263414911353,-37.3551155311246,
112.945987904727));
#45370=CARTESIAN_POINT('Ctrl Pts',(-90.3869837057071,-34.1737836833869,
112.788039381534));
#45371=CARTESIAN_POINT('Ctrl Pts',(-87.3735767823643,-32.9700273053906,
112.630090858342));
#45372=CARTESIAN_POINT('Ctrl Pts',(-84.7182851298726,-34.8352556944698,
112.472142335149));
#45373=CARTESIAN_POINT('Ctrl Pts',(-84.8285809325017,-38.0783229986033,
112.314193811957));
#45374=CARTESIAN_POINT('Ctrl Pts',(-87.6044623405025,-39.7588387265671,
112.156245288764));
#45375=CARTESIAN_POINT('Ctrl Pts',(-90.5291221058576,-38.353130378391,111.998296765572));
#45376=CARTESIAN_POINT('Ctrl Pts',(-90.9508601688256,-35.1357109606813,
111.840348242379));
#45377=CARTESIAN_POINT('Ctrl Pts',(-88.4872994542962,-33.0237168060833,
111.682399719187));
#45378=CARTESIAN_POINT('Ctrl Pts',(-85.3720755363224,-33.9320287811804,
111.524451195994));
#45379=CARTESIAN_POINT('Ctrl Pts',(-84.4296671960753,-37.0371080431954,
111.366502672802));
#45380=CARTESIAN_POINT('Ctrl Pts',(-86.5145274136095,-39.5236736620104,
111.20855414961));
#45381=CARTESIAN_POINT('Ctrl Pts',(-89.7363768378307,-39.1372322164502,
111.050605626417));
#45382=CARTESIAN_POINT('Ctrl Pts',(-91.1740625839451,-36.2281584122637,
110.892657103225));
#45383=CARTESIAN_POINT('Ctrl Pts',(-89.5240787111315,-33.4340209919287,
110.734708580032));
#45384=CARTESIAN_POINT('Ctrl Pts',(-86.2824154149913,-33.2881793752273,
110.57676005684));
#45385=CARTESIAN_POINT('Ctrl Pts',(-84.3881902151712,-35.9228637191904,
110.418811533647));
#45386=CARTESIAN_POINT('Ctrl Pts',(-85.5588394905682,-38.9492858620401,
110.260863010455));
#45387=CARTESIAN_POINT('Ctrl Pts',(-88.7329711458906,-39.623480885994,110.102914487262));
#45388=CARTESIAN_POINT('Ctrl Pts',(-91.0326965481183,-37.3341766785082,
109.94496596407));
#45389=CARTESIAN_POINT('Ctrl Pts',(-90.3729246139036,-34.1570157159285,
109.787017440877));
#45390=CARTESIAN_POINT('Ctrl Pts',(-87.3518504984453,-32.972633260403,109.629068917685));
#45391=CARTESIAN_POINT('Ctrl Pts',(-84.708590202927,-34.8548727676472,109.471120394492));
#45392=CARTESIAN_POINT('Ctrl Pts',(-84.8397074821303,-38.0971651182609,
109.3131718713));
#45393=CARTESIAN_POINT('Ctrl Pts',(-87.6263222127909,-39.7598220445177,
109.155223348107));
#45394=CARTESIAN_POINT('Ctrl Pts',(-90.5418957217887,-38.3353639082262,
108.997274824915));
#45395=CARTESIAN_POINT('Ctrl Pts',(-90.9429658688318,-35.1153018728052,
108.839326301722));
#45396=CARTESIAN_POINT('Ctrl Pts',(-88.4658951929996,-33.0191717602709,
108.68137777853));
#45397=CARTESIAN_POINT('Ctrl Pts',(-85.3565670161152,-33.9474637775143,
108.523429255337));
#45398=CARTESIAN_POINT('Ctrl Pts',(-84.4341173516769,-37.058538624355,108.365480732145));
#45399=CARTESIAN_POINT('Ctrl Pts',(-86.5348976583306,-39.5316488374778,
108.207532208953));
#45400=CARTESIAN_POINT('Ctrl Pts',(-89.7542058355207,-39.124563368979,108.04958368576));
#45401=CARTESIAN_POINT('Ctrl Pts',(-91.1731693955388,-36.2062451449413,
107.891635162568));
#45402=CARTESIAN_POINT('Ctrl Pts',(-89.5053059237116,-33.4229100286828,
107.733686639375));
#45403=CARTESIAN_POINT('Ctrl Pts',(-86.2627163667637,-33.2975773091863,
107.575738116183));
#45404=CARTESIAN_POINT('Ctrl Pts',(-84.3855639730709,-35.9450053434366,
107.41778959299));
#45405=CARTESIAN_POINT('Ctrl Pts',(-85.5753820059203,-38.9625420320502,
107.259841069798));
#45406=CARTESIAN_POINT('Ctrl Pts',(-88.7542617304213,-39.6190416933389,
107.101892546605));
#45407=CARTESIAN_POINT('Ctrl Pts',(-91.0381776799758,-37.3094630383042,
106.943944023413));
#45408=CARTESIAN_POINT('Ctrl Pts',(-90.5846315306955,-35.2042483553399,
106.838645007951));
#45409=CARTESIAN_POINT('Ctrl Pts',(-89.9637526925908,-34.4780626356041,
106.78599550022));
#45410=CARTESIAN_POINT('Ctrl Pts',(-88.4666220147337,-38.966058260622,122.21400449978));
#45411=CARTESIAN_POINT('Ctrl Pts',(-89.3304018103156,-38.7351332702521,
122.161354992049));
#45412=CARTESIAN_POINT('Ctrl Pts',(-90.7961450123593,-37.3519724764984,
122.056055976587));
#45413=CARTESIAN_POINT('Ctrl Pts',(-90.2590362046681,-34.3600926732987,
121.898107453395));
#45414=CARTESIAN_POINT('Ctrl Pts',(-87.4594165493103,-33.1812960120178,
121.740158930202));
#45415=CARTESIAN_POINT('Ctrl Pts',(-84.942230648827,-34.8777646663423,121.58221040701));
#45416=CARTESIAN_POINT('Ctrl Pts',(-84.9865439069216,-37.9145779498893,
121.424261883817));
#45417=CARTESIAN_POINT('Ctrl Pts',(-87.5537299348201,-39.5367930078253,
121.266313360625));
#45418=CARTESIAN_POINT('Ctrl Pts',(-90.3154451418077,-38.2743537031959,
121.108364837432));
#45419=CARTESIAN_POINT('Ctrl Pts',(-90.7680930072786,-35.2715073470735,
120.95041631424));
#45420=CARTESIAN_POINT('Ctrl Pts',(-88.5010931956941,-33.2510223413438,
120.792467791047));
#45421=CARTESIAN_POINT('Ctrl Pts',(-85.5699521748575,-34.0447239853984,
120.634519267855));
#45422=CARTESIAN_POINT('Ctrl Pts',(-84.6322042122549,-36.9330294423666,
120.476570744662));
#45423=CARTESIAN_POINT('Ctrl Pts',(-86.5380973596023,-39.2971794285665,
120.31862222147));
#45424=CARTESIAN_POINT('Ctrl Pts',(-89.5596063003586,-38.9936810554801,
120.160673698277));
#45425=CARTESIAN_POINT('Ctrl Pts',(-90.9572256182428,-36.297702204423,120.002725175085));
#45426=CARTESIAN_POINT('Ctrl Pts',(-89.4637740284878,-33.6536072697314,
119.844776651892));
#45427=CARTESIAN_POINT('Ctrl Pts',(-86.4333198117624,-33.4587155624518,
119.6868281287));
#45428=CARTESIAN_POINT('Ctrl Pts',(-84.613483082289,-35.8897300252424,119.528879605508));
#45429=CARTESIAN_POINT('Ctrl Pts',(-85.6542547256714,-38.7425235088361,
119.370931082315));
#45430=CARTESIAN_POINT('Ctrl Pts',(-88.6119986148113,-39.430555057616,119.212982559123));
#45431=CARTESIAN_POINT('Ctrl Pts',(-90.8050183851675,-37.3300073275741,
119.05503403593));
#45432=CARTESIAN_POINT('Ctrl Pts',(-90.244969677507,-34.3453830915146,118.897085512738));
#45433=CARTESIAN_POINT('Ctrl Pts',(-87.4396316370916,-33.1827503558368,
118.739136989545));
#45434=CARTESIAN_POINT('Ctrl Pts',(-84.932518937306,-34.8962328694908,118.581188466353));
#45435=CARTESIAN_POINT('Ctrl Pts',(-84.9967544162386,-37.9322681469695,
118.42323994316));
#45436=CARTESIAN_POINT('Ctrl Pts',(-87.5740977170349,-39.5381753407685,
118.265291419968));
#45437=CARTESIAN_POINT('Ctrl Pts',(-90.327750056062,-38.2579272388805,118.107342896775));
#45438=CARTESIAN_POINT('Ctrl Pts',(-90.761058605663,-35.2522858587143,117.949394373583));
#45439=CARTESIAN_POINT('Ctrl Pts',(-88.4811556825983,-33.2463748270155,
117.79144585039));
#45440=CARTESIAN_POINT('Ctrl Pts',(-85.5551599270005,-34.0588926692967,
117.633497327198));
#45441=CARTESIAN_POINT('Ctrl Pts',(-84.6359827003793,-36.9531541695272,
117.475548804006));
#45442=CARTESIAN_POINT('Ctrl Pts',(-86.5570140385773,-39.3050204504555,
117.317600280813));
#45443=CARTESIAN_POINT('Ctrl Pts',(-89.5765132527889,-38.9821258839323,
117.159651757621));
#45444=CARTESIAN_POINT('Ctrl Pts',(-90.9567922394001,-36.2772291530353,
117.001703234428));
#45445=CARTESIAN_POINT('Ctrl Pts',(-89.4463940205411,-33.6427778579508,
116.843754711236));
#45446=CARTESIAN_POINT('Ctrl Pts',(-86.4147507245648,-33.4673488647189,
116.685806188043));
#45447=CARTESIAN_POINT('Ctrl Pts',(-84.6105611246705,-35.9099983060708,
116.527857664851));
#45448=CARTESIAN_POINT('Ctrl Pts',(-85.6696290591357,-38.7560502233575,
116.369909141658));
#45449=CARTESIAN_POINT('Ctrl Pts',(-88.6317298418765,-39.4250759019314,
116.211960618466));
#45450=CARTESIAN_POINT('Ctrl Pts',(-90.8112167814044,-37.3104901065257,
116.054012095273));
#45451=CARTESIAN_POINT('Ctrl Pts',(-90.2320153557485,-34.329523465615,115.896063572081));
#45452=CARTESIAN_POINT('Ctrl Pts',(-87.4192698819359,-33.184927770511,115.738115048888));
#45453=CARTESIAN_POINT('Ctrl Pts',(-84.9232111352859,-34.9144731266598,
115.580166525696));
#45454=CARTESIAN_POINT('Ctrl Pts',(-85.006939667191,-37.9500333613858,115.422218002503));
#45455=CARTESIAN_POINT('Ctrl Pts',(-87.5945413642607,-39.5393583322538,
115.264269479311));
#45456=CARTESIAN_POINT('Ctrl Pts',(-90.3399164661106,-38.2414554253121,
115.106320956119));
#45457=CARTESIAN_POINT('Ctrl Pts',(-90.7539168647021,-35.2330937323519,
114.948372432926));
#45458=CARTESIAN_POINT('Ctrl Pts',(-88.4611809898858,-33.2418633051955,
114.790423909734));
#45459=CARTESIAN_POINT('Ctrl Pts',(-85.5404627289477,-34.0731522116095,
114.632475386541));
#45460=CARTESIAN_POINT('Ctrl Pts',(-84.6398884994501,-36.9732560826578,
114.474526863349));
#45461=CARTESIAN_POINT('Ctrl Pts',(-86.5759815655513,-39.3127389411328,
114.316578340156));
#45462=CARTESIAN_POINT('Ctrl Pts',(-89.5933452278263,-38.9704628314102,
114.158629816964));
#45463=CARTESIAN_POINT('Ctrl Pts',(-90.9562276226576,-36.2567590923181,
114.000681293771));
#45464=CARTESIAN_POINT('Ctrl Pts',(-89.4289447328463,-33.6320603705229,
113.842732770579));
#45465=CARTESIAN_POINT('Ctrl Pts',(-86.3962375043747,-33.4761011704732,
113.684784247386));
#45466=CARTESIAN_POINT('Ctrl Pts',(-84.6077693456771,-35.9302849555694,
113.526835724194));
#45467=CARTESIAN_POINT('Ctrl Pts',(-85.6850899424446,-38.7694779284905,
113.368887201001));
#45468=CARTESIAN_POINT('Ctrl Pts',(-88.6514254748125,-39.41947017084,113.210938677809));
#45469=CARTESIAN_POINT('Ctrl Pts',(-90.8172897326005,-37.2909334850999,
113.052990154616));
#45470=CARTESIAN_POINT('Ctrl Pts',(-90.2189594650554,-34.3137473477138,
112.895041631424));
#45471=CARTESIAN_POINT('Ctrl Pts',(-87.3989225283682,-33.1872358824264,
112.737093108232));
#45472=CARTESIAN_POINT('Ctrl Pts',(-84.9140206454866,-34.9327727735164,
112.579144585039));
#45473=CARTESIAN_POINT('Ctrl Pts',(-85.017238778745,-37.967732809937,112.421196061847));
#45474=CARTESIAN_POINT('Ctrl Pts',(-87.6149921859555,-39.5404100308031,
112.263247538654));
#45475=CARTESIAN_POINT('Ctrl Pts',(-90.3519768598988,-38.2249058307701,
112.105299015462));
#45476=CARTESIAN_POINT('Ctrl Pts',(-90.7466520383367,-35.213947858758,111.947350492269));
#45477=CARTESIAN_POINT('Ctrl Pts',(-88.441177740482,-33.2374801338393,111.789401969077));
#45478=CARTESIAN_POINT('Ctrl Pts',(-85.5258573943697,-34.0875058306568,
111.631453445884));
#45479=CARTESIAN_POINT('Ctrl Pts',(-84.6439232923566,-36.9933325022533,
111.473504922692));
#45480=CARTESIAN_POINT('Ctrl Pts',(-86.5949982619306,-39.3203354822477,
111.315556399499));
#45481=CARTESIAN_POINT('Ctrl Pts',(-89.6101019674299,-38.9586919412095,
111.157607876307));
#45482=CARTESIAN_POINT('Ctrl Pts',(-90.9555315793369,-36.2362930790426,
110.999659353114));
#45483=CARTESIAN_POINT('Ctrl Pts',(-89.4114269878765,-33.6214551457762,
110.841710829922));
#45484=CARTESIAN_POINT('Ctrl Pts',(-86.3777808644127,-33.4849721693756,
110.683762306729));
#45485=CARTESIAN_POINT('Ctrl Pts',(-84.6051078846975,-35.9505891124219,
110.525813783537));
#45486=CARTESIAN_POINT('Ctrl Pts',(-85.7006367264722,-38.7828060834297,
110.367865260344));
#45487=CARTESIAN_POINT('Ctrl Pts',(-88.6710847069883,-39.4137380877842,
110.209916737152));
#45488=CARTESIAN_POINT('Ctrl Pts',(-90.8232369862847,-37.2713382763238,
110.05196821396));
#45489=CARTESIAN_POINT('Ctrl Pts',(-90.2058025436072,-34.2980553788597,
109.894019690767));
#45490=CARTESIAN_POINT('Ctrl Pts',(-87.3785904176685,-33.1896746135959,
109.736071167575));
#45491=CARTESIAN_POINT('Ctrl Pts',(-84.9049478409233,-34.9511310212928,
109.578122644382));
#45492=CARTESIAN_POINT('Ctrl Pts',(-85.0276513389231,-37.9853658328746,
109.42017412119));
#45493=CARTESIAN_POINT('Ctrl Pts',(-87.6354493126737,-39.5413302493503,
109.262225597997));
#45494=CARTESIAN_POINT('Ctrl Pts',(-90.3639307943181,-38.208279433017,109.104277074805));
#45495=CARTESIAN_POINT('Ctrl Pts',(-90.7392643146943,-35.1948484197779,
108.946328551612));
#45496=CARTESIAN_POINT('Ctrl Pts',(-88.421146988249,-33.2332267431105,108.78838002842));
#45497=CARTESIAN_POINT('Ctrl Pts',(-85.511344054177,-34.1019503649949,108.630431505227));
#45498=CARTESIAN_POINT('Ctrl Pts',(-84.6480878819688,-37.0133878854068,
108.472482982035));
#45499=CARTESIAN_POINT('Ctrl Pts',(-86.6140613503167,-39.3277988915936,
108.314534458842));
#45500=CARTESIAN_POINT('Ctrl Pts',(-89.6267868803239,-38.9468360522697,
108.15658593565));
#45501=CARTESIAN_POINT('Ctrl Pts',(-90.9546957067312,-36.2157859836437,
107.998637412458));
#45502=CARTESIAN_POINT('Ctrl Pts',(-89.3938588481345,-33.6110571718043,
107.840688889265));
#45503=CARTESIAN_POINT('Ctrl Pts',(-86.3593459019159,-33.4937670389591,
107.682740366073));
#45504=CARTESIAN_POINT('Ctrl Pts',(-84.6026501682603,-35.9713099111062,
107.52479184288));
#45505=CARTESIAN_POINT('Ctrl Pts',(-85.7161177104565,-38.7952116064866,
107.366843319688));
#45506=CARTESIAN_POINT('Ctrl Pts',(-88.6910090770809,-39.4095837576274,
107.208894796495));
#45507=CARTESIAN_POINT('Ctrl Pts',(-90.8283663945213,-37.2482105076592,
107.050946273303));
#45508=CARTESIAN_POINT('Ctrl Pts',(-90.4039242511271,-35.2780872164347,
106.945647257841));
#45509=CARTESIAN_POINT('Ctrl Pts',(-89.8228871389138,-34.5985007534561,
106.89299775011));
#45510=CARTESIAN_POINT('Ctrl Pts',(-88.4187555865477,-38.7870128767185,
122.321006749669));
#45511=CARTESIAN_POINT('Ctrl Pts',(-89.2233059850348,-38.5719224173526,
122.268357241939));
#45512=CARTESIAN_POINT('Ctrl Pts',(-90.5885431476955,-37.2836049856667,
122.163058226477));
#45513=CARTESIAN_POINT('Ctrl Pts',(-90.0882639012151,-34.4968784377644,
122.005109703284));
#45514=CARTESIAN_POINT('Ctrl Pts',(-87.4806142191418,-33.3989118860811,
121.847161180092));
#45515=CARTESIAN_POINT('Ctrl Pts',(-85.1360318039727,-34.9790536523493,
121.689212656899));
#45516=CARTESIAN_POINT('Ctrl Pts',(-85.1773065011126,-37.8076325909925,
121.531264133707));
#45517=CARTESIAN_POINT('Ctrl Pts',(-87.5684605340043,-39.318612331396,121.373315610515));
#45518=CARTESIAN_POINT('Ctrl Pts',(-90.1408048764567,-38.1427385140175,
121.215367087322));
#45519=CARTESIAN_POINT('Ctrl Pts',(-90.5624146691395,-35.3457973899361,
121.05741856413));
#45520=CARTESIAN_POINT('Ctrl Pts',(-88.4508630779708,-33.4638570796724,
120.899470040937));
#45521=CARTESIAN_POINT('Ctrl Pts',(-85.7207104529639,-34.2031345868219,
120.741521517745));
#45522=CARTESIAN_POINT('Ctrl Pts',(-84.8472638860827,-36.8933888833937,
120.583572994552));
#45523=CARTESIAN_POINT('Ctrl Pts',(-86.6224699038839,-39.0954290598474,
120.42562447136));
#45524=CARTESIAN_POINT('Ctrl Pts',(-89.4367939188142,-38.8127415760051,
120.267675948167));
#45525=CARTESIAN_POINT('Ctrl Pts',(-90.7385784533545,-36.3016260463006,
120.109727424975));
#45526=CARTESIAN_POINT('Ctrl Pts',(-89.3475328676574,-33.8388367518247,
119.951778901782));
#45527=CARTESIAN_POINT('Ctrl Pts',(-86.5248769545022,-33.6573087726388,
119.79383037859));
#45528=CARTESIAN_POINT('Ctrl Pts',(-84.8298264643564,-35.9216285272452,
119.635881855397));
#45529=CARTESIAN_POINT('Ctrl Pts',(-85.7992323762569,-38.5788059071355,
119.477933332205));
#45530=CARTESIAN_POINT('Ctrl Pts',(-88.554163710379,-39.2196591194634,119.319984809013));
#45531=CARTESIAN_POINT('Ctrl Pts',(-90.5968080731607,-37.263145987424,119.16203628582));
#45532=CARTESIAN_POINT('Ctrl Pts',(-90.0751619160902,-34.4831774922844,
119.004087762628));
#45533=CARTESIAN_POINT('Ctrl Pts',(-87.4621859587324,-33.4002665055166,
118.846139239435));
#45534=CARTESIAN_POINT('Ctrl Pts',(-85.1269860246962,-34.9962554904548,
118.688190716243));
#45535=CARTESIAN_POINT('Ctrl Pts',(-85.1868168756106,-37.8241097709208,
118.53024219305));
#45536=CARTESIAN_POINT('Ctrl Pts',(-87.5874316970034,-39.3198998777429,
118.372293669858));
#45537=CARTESIAN_POINT('Ctrl Pts',(-90.1522660425053,-38.1274384126742,
118.214345146665));
#45538=CARTESIAN_POINT('Ctrl Pts',(-90.5558626165772,-35.3278939194011,
118.056396623473));
#45539=CARTESIAN_POINT('Ctrl Pts',(-88.4322926805291,-33.4595282454904,
117.89844810028));
#45540=CARTESIAN_POINT('Ctrl Pts',(-85.7069325098252,-34.2163317237944,
117.740499577088));
#45541=CARTESIAN_POINT('Ctrl Pts',(-84.8507832832042,-36.9121336576282,
117.582551053895));
#45542=CARTESIAN_POINT('Ctrl Pts',(-86.64008946582,-39.1027324227156,117.424602530703));
#45543=CARTESIAN_POINT('Ctrl Pts',(-89.4525415611931,-38.8019787427913,
117.26665400751));
#45544=CARTESIAN_POINT('Ctrl Pts',(-90.7381747913074,-36.2825568324379,
117.108705484318));
#45545=CARTESIAN_POINT('Ctrl Pts',(-89.3313446071879,-33.8287499130169,
116.950756961126));
#45546=CARTESIAN_POINT('Ctrl Pts',(-86.5075811499688,-33.6653500892044,
116.792808437933));
#45547=CARTESIAN_POINT('Ctrl Pts',(-84.8271048654275,-35.9405070116697,
116.634859914741));
#45548=CARTESIAN_POINT('Ctrl Pts',(-85.8135524913818,-38.5914050945837,
116.476911391548));
#45549=CARTESIAN_POINT('Ctrl Pts',(-88.5725419668272,-39.2145556695888,
116.318962868356));
#45550=CARTESIAN_POINT('Ctrl Pts',(-90.6025814452492,-37.244967062596,116.161014345163));
#45551=CARTESIAN_POINT('Ctrl Pts',(-90.0630958724223,-34.4684053612359,
116.003065821971));
#45552=CARTESIAN_POINT('Ctrl Pts',(-87.4432204095168,-33.4022946148249,
115.845117298778));
#45553=CARTESIAN_POINT('Ctrl Pts',(-85.1183164588386,-35.0132450128412,
115.687168775586));
#45554=CARTESIAN_POINT('Ctrl Pts',(-85.1963037237104,-37.8406568242449,
115.529220252393));
#45555=CARTESIAN_POINT('Ctrl Pts',(-87.6064735229483,-39.3210017514795,
115.371271729201));
#45556=CARTESIAN_POINT('Ctrl Pts',(-90.1635982015843,-38.1120960716771,
115.213323206008));
#45557=CARTESIAN_POINT('Ctrl Pts',(-90.5492105849305,-35.3100177975103,
115.055374682816));
#45558=CARTESIAN_POINT('Ctrl Pts',(-88.4136876528777,-33.4553260788078,
114.897426159623));
#45559=CARTESIAN_POINT('Ctrl Pts',(-85.6932430989239,-34.2296134890183,
114.739477636431));
#45560=CARTESIAN_POINT('Ctrl Pts',(-84.854421261558,-36.9308571821911,114.581529113239));
#45561=CARTESIAN_POINT('Ctrl Pts',(-86.6577563891068,-39.1099216563396,
114.423580590046));
#45562=CARTESIAN_POINT('Ctrl Pts',(-89.4682193673805,-38.7911154260036,
114.265632066854));
#45563=CARTESIAN_POINT('Ctrl Pts',(-90.7376488903457,-36.2634904041754,
114.107683543661));
#45564=CARTESIAN_POINT('Ctrl Pts',(-89.3150918174839,-33.8187673239068,
113.949735020469));
#45565=CARTESIAN_POINT('Ctrl Pts',(-86.490337381641,-33.6735022491857,113.791786497276));
#45566=CARTESIAN_POINT('Ctrl Pts',(-84.8245045187733,-35.9594026052244,
113.633837974084));
#45567=CARTESIAN_POINT('Ctrl Pts',(-85.8279532216264,-38.603912061719,113.475889450891));
#45568=CARTESIAN_POINT('Ctrl Pts',(-88.5908870698365,-39.2093343235855,
113.317940927699));
#45569=CARTESIAN_POINT('Ctrl Pts',(-90.6082379740656,-37.2267514390751,
113.159992404506));
#45570=CARTESIAN_POINT('Ctrl Pts',(-90.0509352244037,-34.4537110120408,
113.002043881314));
#45571=CARTESIAN_POINT('Ctrl Pts',(-87.4242682743722,-33.4044444594622,
112.844095358121));
#45572=CARTESIAN_POINT('Ctrl Pts',(-85.1097561611006,-35.030289852563,112.686146834929));
#45573=CARTESIAN_POINT('Ctrl Pts',(-85.2058966249883,-37.8571426212706,
112.528198311736));
#45574=CARTESIAN_POINT('Ctrl Pts',(-87.6255220314084,-39.3219813350391,
112.370249788544));
#45575=CARTESIAN_POINT('Ctrl Pts',(-90.1748316139398,-38.0966812831492,
112.212301265352));
#45576=CARTESIAN_POINT('Ctrl Pts',(-90.5424439078479,-35.2921847568347,
112.054352742159));
#45577=CARTESIAN_POINT('Ctrl Pts',(-88.3950560266678,-33.4512434615953,
111.896404218967));
#45578=CARTESIAN_POINT('Ctrl Pts',(-85.6796392524171,-34.2429828801331,
111.738455695774));
#45579=CARTESIAN_POINT('Ctrl Pts',(-84.8581793886376,-36.9495569613113,
111.580507172582));
#45580=CARTESIAN_POINT('Ctrl Pts',(-86.6754691102519,-39.116997302485,111.422558649389));
#45581=CARTESIAN_POINT('Ctrl Pts',(-89.483827097029,-38.780151665969,111.264610126197));
#45582=CARTESIAN_POINT('Ctrl Pts',(-90.7370005747289,-36.2444277458214,
111.106661603004));
#45583=CARTESIAN_POINT('Ctrl Pts',(-89.2987752646214,-33.8088892996237,
110.948713079812));
#45584=CARTESIAN_POINT('Ctrl Pts',(-86.473146313834,-33.6817649635238,110.790764556619));
#45585=CARTESIAN_POINT('Ctrl Pts',(-84.8220255542238,-35.9783145056534,
110.632816033427));
#45586=CARTESIAN_POINT('Ctrl Pts',(-85.8424339623762,-38.6163263048192,
110.474867510234));
#45587=CARTESIAN_POINT('Ctrl Pts',(-88.6091982680859,-39.2039952895745,
110.316918987042));
#45588=CARTESIAN_POINT('Ctrl Pts',(-90.613777424451,-37.2084998741394,110.158970463849));
#45589=CARTESIAN_POINT('Ctrl Pts',(-90.0386804733106,-34.439095041791,110.001021940657));
#45590=CARTESIAN_POINT('Ctrl Pts',(-87.4053303368919,-33.4067159667888,
109.843073417464));
#45591=CARTESIAN_POINT('Ctrl Pts',(-85.1013054789195,-35.0473892749383,
109.685124894272));
#45592=CARTESIAN_POINT('Ctrl Pts',(-85.215595195716,-37.8735665474884,109.52717637108));
#45593=CARTESIAN_POINT('Ctrl Pts',(-87.6445764125565,-39.3228384541829,
109.369227847887));
#45594=CARTESIAN_POINT('Ctrl Pts',(-90.1859658668476,-38.0811949578079,
109.211279324695));
#45595=CARTESIAN_POINT('Ctrl Pts',(-90.5355627605568,-35.2743949667504,
109.053330801502));
#45596=CARTESIAN_POINT('Ctrl Pts',(-88.3763987834983,-33.4472817259501,
108.89538227831));
#45597=CARTESIAN_POINT('Ctrl Pts',(-85.6661210922389,-34.2564369524755,
108.737433755117));
#45598=CARTESIAN_POINT('Ctrl Pts',(-84.8620584122606,-36.9682371464585,
108.579485231925));
#45599=CARTESIAN_POINT('Ctrl Pts',(-86.6932250423031,-39.1239489457093,
108.421536708732));
#45600=CARTESIAN_POINT('Ctrl Pts',(-89.4993679251268,-38.7691087355603,
108.26358818554));
#45601=CARTESIAN_POINT('Ctrl Pts',(-90.7362220179238,-36.225326822346,108.105639662347));
#45602=CARTESIAN_POINT('Ctrl Pts',(-89.2824117725574,-33.7992043149259,
107.947691139155));
#45603=CARTESIAN_POINT('Ctrl Pts',(-86.455975437068,-33.6899567687319,107.789742615962));
#45604=CARTESIAN_POINT('Ctrl Pts',(-84.8197363634497,-35.9976144787758,
107.63179409277));
#45605=CARTESIAN_POINT('Ctrl Pts',(-85.8568534149928,-38.627881180923,107.473845569577));
#45606=CARTESIAN_POINT('Ctrl Pts',(-88.6277564237406,-39.2001258219159,
107.315897046385));
#45607=CARTESIAN_POINT('Ctrl Pts',(-90.6185551090667,-37.1869579770143,
107.157948523193));
#45608=CARTESIAN_POINT('Ctrl Pts',(-90.2232169715586,-35.3519260775293,
107.052649507731));
#45609=CARTESIAN_POINT('Ctrl Pts',(-89.6820215852368,-34.718938871308,107.));
#45610=CARTESIAN_POINT('Ctrl Pts',(-90.2835504011883,-36.3531642868356,
121.112583302492));
#45611=CARTESIAN_POINT('Ctrl Pts',(-90.2854632662372,-36.0616114296406,
121.094195056371));
#45612=CARTESIAN_POINT('Ctrl Pts',(-90.2385919702165,-35.7706534224358,
121.07580681025));
#45613=CARTESIAN_POINT('Ctrl Pts',(-90.1402211051642,-35.4982975255724,
121.05741856413));
#45614=CARTESIAN_POINT('Ctrl Pts',(-89.8585641387499,-34.7184839531815,
121.004769056399));
#45615=CARTESIAN_POINT('Ctrl Pts',(-89.1547136083603,-34.0911705164269,
120.952119548668));
#45616=CARTESIAN_POINT('Ctrl Pts',(-88.3477629056644,-33.9007267159079,
120.899470040937));
#45617=CARTESIAN_POINT('Ctrl Pts',(-87.5408122029685,-33.7102829153889,
120.846820533206));
#45618=CARTESIAN_POINT('Ctrl Pts',(-86.6307613279662,-33.9567087511054,
120.794171025476));
#45619=CARTESIAN_POINT('Ctrl Pts',(-86.0301614626515,-34.5282973850589,
120.741521517745));
#45620=CARTESIAN_POINT('Ctrl Pts',(-85.4295615973368,-35.0998860190125,
120.688872010014));
#45621=CARTESIAN_POINT('Ctrl Pts',(-85.1384127417097,-35.9966374512031,
120.636222502283));
#45622=CARTESIAN_POINT('Ctrl Pts',(-85.2887059835297,-36.812019863374,120.583572994552));
#45623=CARTESIAN_POINT('Ctrl Pts',(-85.4389992253497,-37.6274022755449,
120.530923486821));
#45624=CARTESIAN_POINT('Ctrl Pts',(-86.0307345646168,-38.3614156676962,
120.478273979091));
#45625=CARTESIAN_POINT('Ctrl Pts',(-86.7956562367387,-38.6813077831314,
120.42562447136));
#45626=CARTESIAN_POINT('Ctrl Pts',(-87.5605779088606,-39.0011998985666,
120.372974963629));
#45627=CARTESIAN_POINT('Ctrl Pts',(-88.4986859138374,-38.9069707372859,
120.320325455898));
#45628=CARTESIAN_POINT('Ctrl Pts',(-89.1847040054158,-38.4413369016947,
120.267675948167));
#45629=CARTESIAN_POINT('Ctrl Pts',(-89.8583181592778,-37.9841222217589,
120.215978399609));
#45630=CARTESIAN_POINT('Ctrl Pts',(-90.288876093497,-37.1688122301997,120.16428085105));
#45631=CARTESIAN_POINT('Ctrl Pts',(-90.290141386937,-36.3546528235808,120.112583302492));
#45632=CARTESIAN_POINT('Ctrl Pts',(-88.5623548711056,-39.3241490284291,
122.));
#45633=CARTESIAN_POINT('Ctrl Pts',(-88.6554048794521,-39.2901109197242,
122.));
#45634=CARTESIAN_POINT('Ctrl Pts',(-88.7463897233141,-39.2513041051342,
122.));
#45635=CARTESIAN_POINT('Ctrl Pts',(-88.8351009182216,-39.2080569091679,
122.));
#45636=CARTESIAN_POINT('Ctrl Pts',(-88.9257790957573,-39.1638507983401,
122.));
#45637=CARTESIAN_POINT('Ctrl Pts',(-89.0140823477826,-39.1150045944796,
122.));
#45638=CARTESIAN_POINT('Ctrl Pts',(-89.0997590949921,-39.0618234076486,
122.));
#45639=CARTESIAN_POINT('Ctrl Pts',(-89.1821905332446,-39.010656645823,122.));
#45640=CARTESIAN_POINT('Ctrl Pts',(-89.2621909583464,-38.955476210875,122.));
#45641=CARTESIAN_POINT('Ctrl Pts',(-89.3395033436134,-38.8965237915301,
122.));
#45642=CARTESIAN_POINT('Ctrl Pts',(-89.4071516807222,-38.8449404246033,
122.));
#45643=CARTESIAN_POINT('Ctrl Pts',(-89.4727416970966,-38.7904684347609,
122.));
#45644=CARTESIAN_POINT('Ctrl Pts',(-89.5360765841124,-38.7332570353692,
122.));
#45645=CARTESIAN_POINT('Ctrl Pts',(-89.5502130714439,-38.7204873240644,
122.));
#45646=CARTESIAN_POINT('Ctrl Pts',(-89.564239852621,-38.7075784015462,122.));
#45647=CARTESIAN_POINT('Ctrl Pts',(-89.5781351542939,-38.6945504599679,
122.));
#45648=CARTESIAN_POINT('Ctrl Pts',(-89.6505652419802,-38.6266415384422,
122.));
#45649=CARTESIAN_POINT('Ctrl Pts',(-89.7195296422287,-38.5554106990788,
122.));
#45650=CARTESIAN_POINT('Ctrl Pts',(-89.7847884055803,-38.4811486670768,
122.));
#45651=CARTESIAN_POINT('Ctrl Pts',(-89.8496881543617,-38.4072951802285,
122.));
#45652=CARTESIAN_POINT('Ctrl Pts',(-89.9109234129235,-38.33044296365,122.));
#45653=CARTESIAN_POINT('Ctrl Pts',(-89.9682145606571,-38.2508512024992,
122.));
#45654=CARTESIAN_POINT('Ctrl Pts',(-90.0233774662291,-38.1742161030403,
122.));
#45655=CARTESIAN_POINT('Ctrl Pts',(-90.0748840116051,-38.0950404775979,
122.));
#45656=CARTESIAN_POINT('Ctrl Pts',(-90.1224397489187,-38.0135421014459,
122.));
#45657=CARTESIAN_POINT('Ctrl Pts',(-90.1423860806803,-37.9793591880777,
122.));
#45658=CARTESIAN_POINT('Ctrl Pts',(-90.1616368088772,-37.944767545073,122.));
#45659=CARTESIAN_POINT('Ctrl Pts',(-90.1801676233274,-37.9097829441458,
122.));
#45660=CARTESIAN_POINT('Ctrl Pts',(-90.1930501688088,-37.8854617944305,
122.));
#45661=CARTESIAN_POINT('Ctrl Pts',(-90.2055847495013,-37.8609507264995,
122.));
#45662=CARTESIAN_POINT('Ctrl Pts',(-90.2177627315331,-37.8362550336735,
122.));
#45663=CARTESIAN_POINT('Ctrl Pts',(-90.2256710650464,-37.8202177481283,
122.));
#45664=CARTESIAN_POINT('Ctrl Pts',(-90.2334301234711,-37.80409999056,122.));
#45665=CARTESIAN_POINT('Ctrl Pts',(-90.2410273664413,-37.787925400008,122.));
#45666=CARTESIAN_POINT('Ctrl Pts',(-90.283147662217,-37.6982509561637,122.));
#45667=CARTESIAN_POINT('Ctrl Pts',(-90.3203691262393,-37.6066929289713,
122.));
#45668=CARTESIAN_POINT('Ctrl Pts',(-90.3524004752756,-37.513523685623,122.));
#45669=CARTESIAN_POINT('Ctrl Pts',(-90.382280230974,-37.426612758871,122.));
#45670=CARTESIAN_POINT('Ctrl Pts',(-90.4076435357704,-37.3382990100201,
122.));
#45671=CARTESIAN_POINT('Ctrl Pts',(-90.4282034120715,-37.248794827624,122.));
#45672=CARTESIAN_POINT('Ctrl Pts',(-90.4296838958252,-37.2423497748434,
122.));
#45673=CARTESIAN_POINT('Ctrl Pts',(-90.4311394502785,-37.2358985482571,
122.));
#45674=CARTESIAN_POINT('Ctrl Pts',(-90.4325699576533,-37.229441226852,122.));
#45675=CARTESIAN_POINT('Ctrl Pts',(-90.4531761786108,-37.1364245853336,
122.));
#45676=CARTESIAN_POINT('Ctrl Pts',(-90.4685893763891,-37.0421422896564,
122.));
#45677=CARTESIAN_POINT('Ctrl Pts',(-90.4788864707506,-36.9470022043264,
122.));
#45678=CARTESIAN_POINT('Ctrl Pts',(-90.4846829926509,-36.8934451940809,
122.));
#45679=CARTESIAN_POINT('Ctrl Pts',(-90.4888573546745,-36.8396165495347,
122.));
#45680=CARTESIAN_POINT('Ctrl Pts',(-90.4914165163901,-36.7855916652876,
122.));
#45681=CARTESIAN_POINT('Ctrl Pts',(-90.4920773998915,-36.7716401613846,
122.));
#45682=CARTESIAN_POINT('Ctrl Pts',(-90.4926304468087,-36.7576761695281,
122.));
#45683=CARTESIAN_POINT('Ctrl Pts',(-90.4930755355952,-36.7437143575909,
122.));
#45684=CARTESIAN_POINT('Ctrl Pts',(-90.4960469521765,-36.6505051805635,
122.));
#45685=CARTESIAN_POINT('Ctrl Pts',(-90.4942192156142,-36.557237773971,122.));
#45686=CARTESIAN_POINT('Ctrl Pts',(-90.4877272199528,-36.4642872156905,
122.));
#45687=CARTESIAN_POINT('Ctrl Pts',(-90.4812244299425,-36.3711821069759,
122.));
#45688=CARTESIAN_POINT('Ctrl Pts',(-90.4700414792909,-36.2783939214527,
122.));
#45689=CARTESIAN_POINT('Ctrl Pts',(-90.4542630033313,-36.1863117068558,
122.));
#45690=CARTESIAN_POINT('Ctrl Pts',(-90.4387101222259,-36.0955460499439,
122.));
#45691=CARTESIAN_POINT('Ctrl Pts',(-90.4186917256712,-36.0054654767755,
122.));
#45692=CARTESIAN_POINT('Ctrl Pts',(-90.3942458454892,-35.9164677845401,
122.));
#45693=CARTESIAN_POINT('Ctrl Pts',(-90.3851470810519,-35.8833428149709,
122.));
#45694=CARTESIAN_POINT('Ctrl Pts',(-90.375434565641,-35.8503681770352,122.));
#45695=CARTESIAN_POINT('Ctrl Pts',(-90.3651088987993,-35.8175656480154,
122.));
#45696=CARTESIAN_POINT('Ctrl Pts',(-90.3581143447969,-35.7953453823259,
122.));
#45697=CARTESIAN_POINT('Ctrl Pts',(-90.3508384228978,-35.7732041064495,
122.));
#45698=CARTESIAN_POINT('Ctrl Pts',(-90.3432811403389,-35.7511488028356,
122.));
#45699=CARTESIAN_POINT('Ctrl Pts',(-90.338765074935,-35.7379690397597,122.));
#45700=CARTESIAN_POINT('Ctrl Pts',(-90.3341488817557,-35.724821150221,122.));
#45701=CARTESIAN_POINT('Ctrl Pts',(-90.3294360325543,-35.711715772054,122.));
#45702=CARTESIAN_POINT('Ctrl Pts',(-90.2978042850547,-35.6237549663183,
122.));
#45703=CARTESIAN_POINT('Ctrl Pts',(-90.261783323813,-35.5375919066344,122.));
#45704=CARTESIAN_POINT('Ctrl Pts',(-90.2214377122488,-35.4536408345172,
122.));
#45705=CARTESIAN_POINT('Ctrl Pts',(-90.1911785035756,-35.3906775304294,
122.));
#45706=CARTESIAN_POINT('Ctrl Pts',(-90.1584856317728,-35.3289589612895,
122.));
#45707=CARTESIAN_POINT('Ctrl Pts',(-90.1233703727677,-35.2686754163207,
122.));
#45708=CARTESIAN_POINT('Ctrl Pts',(-90.1099009754952,-35.2455520494658,
122.));
#45709=CARTESIAN_POINT('Ctrl Pts',(-90.0960750361369,-35.2226399806261,
122.));
#45710=CARTESIAN_POINT('Ctrl Pts',(-90.0818927106299,-35.1999505929771,
122.));
#45711=CARTESIAN_POINT('Ctrl Pts',(-90.0717686114082,-35.1837536997579,
122.));
#45712=CARTESIAN_POINT('Ctrl Pts',(-90.0614620660595,-35.1676692161304,
122.));
#45713=CARTESIAN_POINT('Ctrl Pts',(-90.0509832059227,-35.1517162866814,
122.));
#45714=CARTESIAN_POINT('Ctrl Pts',(-90.0037966280057,-35.0798798332293,
122.));
#45715=CARTESIAN_POINT('Ctrl Pts',(-89.9530751222339,-35.0106368288827,
122.));
#45716=CARTESIAN_POINT('Ctrl Pts',(-89.8988515797855,-34.9443392719291,
122.));
#45717=CARTESIAN_POINT('Ctrl Pts',(-89.850055152577,-34.8846772918016,122.));
#45718=CARTESIAN_POINT('Ctrl Pts',(-89.7984220271467,-34.8274007372017,
122.));
#45719=CARTESIAN_POINT('Ctrl Pts',(-89.7439556820556,-34.7727959467699,
122.));
#45720=CARTESIAN_POINT('Ctrl Pts',(-89.7248731118213,-34.7536648714829,
122.));
#45721=CARTESIAN_POINT('Ctrl Pts',(-89.7054425965606,-34.7348620441323,
122.));
#45722=CARTESIAN_POINT('Ctrl Pts',(-89.6856747112033,-34.7163919521557,
122.));
#45723=CARTESIAN_POINT('Origin',(-87.7685555885722,-36.3549260746835,114.));
#45724=CARTESIAN_POINT('Origin',(-36.3549260746835,-87.7685555885722,107.));
#45725=CARTESIAN_POINT('Ctrl Pts',(-38.2683920713481,-86.1325683851967,
107.));
#45726=CARTESIAN_POINT('Ctrl Pts',(-38.3305295883356,-86.1909623931506,
107.));
#45727=CARTESIAN_POINT('Ctrl Pts',(-38.3892917294532,-86.2526103113827,
107.));
#45728=CARTESIAN_POINT('Ctrl Pts',(-38.4446665159936,-86.3171356636189,
107.));
#45729=CARTESIAN_POINT('Ctrl Pts',(-38.5013963845958,-86.3832400223452,
107.));
#45730=CARTESIAN_POINT('Ctrl Pts',(-38.5545715537976,-86.4523648572664,
107.));
#45731=CARTESIAN_POINT('Ctrl Pts',(-38.6041502559258,-86.524151647146,107.));
#45732=CARTESIAN_POINT('Ctrl Pts',(-38.6170879438391,-86.5428845918156,
107.));
#45733=CARTESIAN_POINT('Ctrl Pts',(-38.6297805550942,-86.5617990222241,
107.));
#45734=CARTESIAN_POINT('Ctrl Pts',(-38.6422269720562,-86.5808890006484,
107.));
#45735=CARTESIAN_POINT('Ctrl Pts',(-38.6523970248712,-86.59648755318,107.));
#45736=CARTESIAN_POINT('Ctrl Pts',(-38.6624031432674,-86.6122042204815,
107.));
#45737=CARTESIAN_POINT('Ctrl Pts',(-38.6722358693769,-86.6280211675642,
107.));
#45738=CARTESIAN_POINT('Ctrl Pts',(-38.7196799641235,-86.7043398535153,
107.));
#45739=CARTESIAN_POINT('Ctrl Pts',(-38.7631404947387,-86.7830659002748,
107.));
#45740=CARTESIAN_POINT('Ctrl Pts',(-38.8025827758839,-86.863806756021,107.));
#45741=CARTESIAN_POINT('Ctrl Pts',(-38.8344112328972,-86.9289616299717,
107.));
#45742=CARTESIAN_POINT('Ctrl Pts',(-38.8636225491245,-86.9954296141671,
107.));
#45743=CARTESIAN_POINT('Ctrl Pts',(-38.8901813394751,-87.0630222348955,
107.));
#45744=CARTESIAN_POINT('Ctrl Pts',(-38.9007827444047,-87.0900030097402,
107.));
#45745=CARTESIAN_POINT('Ctrl Pts',(-38.9109613265359,-87.1171631300883,
107.));
#45746=CARTESIAN_POINT('Ctrl Pts',(-38.920714074785,-87.1444911545565,107.));
#45747=CARTESIAN_POINT('Ctrl Pts',(-38.9259550311851,-87.1591767571254,
107.));
#45748=CARTESIAN_POINT('Ctrl Pts',(-38.9310726354609,-87.1739100289027,
107.));
#45749=CARTESIAN_POINT('Ctrl Pts',(-38.9360624206009,-87.1886767156748,
107.));
#45750=CARTESIAN_POINT('Ctrl Pts',(-38.9656012135239,-87.2760933259059,
107.));
#45751=CARTESIAN_POINT('Ctrl Pts',(-38.9907045453902,-87.3647910403201,
107.));
#45752=CARTESIAN_POINT('Ctrl Pts',(-39.0113398488637,-87.4543720487631,
107.));
#45753=CARTESIAN_POINT('Ctrl Pts',(-39.0322966239254,-87.5453486145384,
107.));
#45754=CARTESIAN_POINT('Ctrl Pts',(-39.04864557461,-87.6372370153347,107.));
#45755=CARTESIAN_POINT('Ctrl Pts',(-39.0603107625964,-87.7296537434723,
107.));
#45756=CARTESIAN_POINT('Ctrl Pts',(-39.0718852370958,-87.8213517996373,
107.));
#45757=CARTESIAN_POINT('Ctrl Pts',(-39.0788488557146,-87.9135709280502,
107.));
#45758=CARTESIAN_POINT('Ctrl Pts',(-39.0810804934318,-88.0059557086637,
107.));
#45759=CARTESIAN_POINT('Ctrl Pts',(-39.0821911128068,-88.0519328520486,
107.));
#45760=CARTESIAN_POINT('Ctrl Pts',(-39.0821289726537,-88.0979512365569,
107.));
#45761=CARTESIAN_POINT('Ctrl Pts',(-39.0808743448802,-88.1439677515796,
107.));
#45762=CARTESIAN_POINT('Ctrl Pts',(-39.0805045717962,-88.1575300758302,
107.));
#45763=CARTESIAN_POINT('Ctrl Pts',(-39.0800311920668,-88.1710922383706,
107.));
#45764=CARTESIAN_POINT('Ctrl Pts',(-39.0794536442604,-88.1846531355265,
107.));
#45765=CARTESIAN_POINT('Ctrl Pts',(-39.0788331294174,-88.1992229042558,
107.));
#45766=CARTESIAN_POINT('Ctrl Pts',(-39.0780927731541,-88.2137814265114,
107.));
#45767=CARTESIAN_POINT('Ctrl Pts',(-39.0772325270316,-88.2283247728338,
107.));
#45768=CARTESIAN_POINT('Ctrl Pts',(-39.0715807131733,-88.3238745046424,
107.));
#45769=CARTESIAN_POINT('Ctrl Pts',(-39.0607562655325,-88.4188025145338,
107.));
#45770=CARTESIAN_POINT('Ctrl Pts',(-39.0446887301443,-88.5127131576963,
107.));
#45771=CARTESIAN_POINT('Ctrl Pts',(-39.0423083893799,-88.5266256418905,
107.));
#45772=CARTESIAN_POINT('Ctrl Pts',(-39.0398128903088,-88.5405158311432,
107.));
#45773=CARTESIAN_POINT('Ctrl Pts',(-39.0372019113363,-88.5543824697525,
107.));
#45774=CARTESIAN_POINT('Ctrl Pts',(-39.020256250766,-88.6443791160708,107.));
#45775=CARTESIAN_POINT('Ctrl Pts',(-38.9984507099304,-88.733383584132,107.));
#45776=CARTESIAN_POINT('Ctrl Pts',(-38.972087837954,-88.821163626335,107.));
#45777=CARTESIAN_POINT('Ctrl Pts',(-38.9451290233172,-88.9109279694868,
107.));
#45778=CARTESIAN_POINT('Ctrl Pts',(-38.9134042991795,-88.9994126041051,
107.));
#45779=CARTESIAN_POINT('Ctrl Pts',(-38.8771829581873,-89.0863654860054,
107.));
#45780=CARTESIAN_POINT('Ctrl Pts',(-38.864692810473,-89.1163493107169,107.));
#45781=CARTESIAN_POINT('Ctrl Pts',(-38.8516675352072,-89.1461509187054,
107.));
#45782=CARTESIAN_POINT('Ctrl Pts',(-38.8381168020892,-89.1757596360031,
107.));
#45783=CARTESIAN_POINT('Ctrl Pts',(-38.8314257154722,-89.1903798407058,
107.));
#45784=CARTESIAN_POINT('Ctrl Pts',(-38.824606501858,-89.2049530114955,107.));
#45785=CARTESIAN_POINT('Ctrl Pts',(-38.8176602661698,-89.2194778407777,
107.));
#45786=CARTESIAN_POINT('Ctrl Pts',(-38.8121664927493,-89.2309655190869,
107.));
#45787=CARTESIAN_POINT('Ctrl Pts',(-38.8065937046077,-89.2424219334059,
107.));
#45788=CARTESIAN_POINT('Ctrl Pts',(-38.8009470423584,-89.253837507682,107.));
#45789=CARTESIAN_POINT('Ctrl Pts',(-38.7582230887587,-89.3402103849944,
107.));
#45790=CARTESIAN_POINT('Ctrl Pts',(-38.7112082785351,-89.4243849391538,
107.));
#45791=CARTESIAN_POINT('Ctrl Pts',(-38.660245266337,-89.5061115333766,107.));
#45792=CARTESIAN_POINT('Ctrl Pts',(-38.6082715482375,-89.5894589413528,
107.));
#45793=CARTESIAN_POINT('Ctrl Pts',(-38.5521911589312,-89.670261101487,107.));
#45794=CARTESIAN_POINT('Ctrl Pts',(-38.4923125369602,-89.7482461987396,
107.));
#45795=CARTESIAN_POINT('Ctrl Pts',(-38.431947090932,-89.8268653289775,107.));
#45796=CARTESIAN_POINT('Ctrl Pts',(-38.3677209417352,-89.9026222404123,
107.));
#45797=CARTESIAN_POINT('Ctrl Pts',(-38.2999007811538,-89.9752191546411,
107.));
#45798=CARTESIAN_POINT('Ctrl Pts',(-38.2629001291875,-90.0148258605848,
107.));
#45799=CARTESIAN_POINT('Ctrl Pts',(-38.2248289148845,-90.0534915954115,
107.));
#45800=CARTESIAN_POINT('Ctrl Pts',(-38.1857250970592,-90.0911642251884,
107.));
#45801=CARTESIAN_POINT('Ctrl Pts',(-38.1737573203776,-90.1026939848193,
107.));
#45802=CARTESIAN_POINT('Ctrl Pts',(-38.1616927978678,-90.1141307004969,
107.));
#45803=CARTESIAN_POINT('Ctrl Pts',(-38.1495325546806,-90.1254728156509,
107.));
#45804=CARTESIAN_POINT('Ctrl Pts',(-38.1389867814773,-90.1353090806185,
107.));
#45805=CARTESIAN_POINT('Ctrl Pts',(-38.1283701312735,-90.1450730796272,
107.));
#45806=CARTESIAN_POINT('Ctrl Pts',(-38.1176923840407,-90.1547558196661,
107.));
#45807=CARTESIAN_POINT('Ctrl Pts',(-38.0421178908384,-90.2232878943906,
107.));
#45808=CARTESIAN_POINT('Ctrl Pts',(-37.9633666783311,-90.2878636215937,
107.));
#45809=CARTESIAN_POINT('Ctrl Pts',(-37.881766092165,-90.3482012299876,107.));
#45810=CARTESIAN_POINT('Ctrl Pts',(-37.8000613244985,-90.4086158729087,
107.));
#45811=CARTESIAN_POINT('Ctrl Pts',(-37.7154993294117,-90.4647824068464,
107.));
#45812=CARTESIAN_POINT('Ctrl Pts',(-37.6283634335479,-90.516392179797,107.));
#45813=CARTESIAN_POINT('Ctrl Pts',(-37.5429597747808,-90.5669759649802,
107.));
#45814=CARTESIAN_POINT('Ctrl Pts',(-37.4550828708226,-90.6131830404371,
107.));
#45815=CARTESIAN_POINT('Ctrl Pts',(-37.364965395232,-90.6546869942762,107.));
#45816=CARTESIAN_POINT('Ctrl Pts',(-37.3246165101986,-90.6732698301902,
107.));
#45817=CARTESIAN_POINT('Ctrl Pts',(-37.2838180606497,-90.6909092957975,
107.));
#45818=CARTESIAN_POINT('Ctrl Pts',(-37.242589176951,-90.7075731462259,107.));
#45819=CARTESIAN_POINT('Ctrl Pts',(-37.2121695381052,-90.7198681265004,
107.));
#45820=CARTESIAN_POINT('Ctrl Pts',(-37.1815155543152,-90.7316319541871,
107.));
#45821=CARTESIAN_POINT('Ctrl Pts',(-37.1506394945611,-90.7428673099699,
107.));
#45822=CARTESIAN_POINT('Ctrl Pts',(-35.5611267921512,-90.7377785423181,
107.));
#45823=CARTESIAN_POINT('Ctrl Pts',(-35.4662928857449,-90.7030878757344,
107.));
#45824=CARTESIAN_POINT('Ctrl Pts',(-35.3735021330788,-90.6634063262115,
107.));
#45825=CARTESIAN_POINT('Ctrl Pts',(-35.2829954573582,-90.6190542441227,
107.));
#45826=CARTESIAN_POINT('Ctrl Pts',(-35.1912159031789,-90.5740783979917,
107.));
#45827=CARTESIAN_POINT('Ctrl Pts',(-35.1017844554001,-90.5242990217277,
107.));
#45828=CARTESIAN_POINT('Ctrl Pts',(-35.014986370264,-90.4700094899543,107.));
#45829=CARTESIAN_POINT('Ctrl Pts',(-34.9904733516654,-90.4546773510023,
107.));
#45830=CARTESIAN_POINT('Ctrl Pts',(-34.9661706042967,-90.4389852821517,
107.));
#45831=CARTESIAN_POINT('Ctrl Pts',(-34.9420851497754,-90.42293943585,107.));
#45832=CARTESIAN_POINT('Ctrl Pts',(-34.9227556040072,-90.4100619989637,
107.));
#45833=CARTESIAN_POINT('Ctrl Pts',(-34.9035639060071,-90.39695507833,107.));
#45834=CARTESIAN_POINT('Ctrl Pts',(-34.8845329713075,-90.3836356190119,
107.));
#45835=CARTESIAN_POINT('Ctrl Pts',(-34.8018258702773,-90.325750187483,107.));
#45836=CARTESIAN_POINT('Ctrl Pts',(-34.7220736288122,-90.2638026101735,
107.));
#45837=CARTESIAN_POINT('Ctrl Pts',(-34.6455426085499,-90.1980902479038,
107.));
#45838=CARTESIAN_POINT('Ctrl Pts',(-34.5865494182568,-90.147436514572,107.));
#45839=CARTESIAN_POINT('Ctrl Pts',(-34.5294708955044,-90.094544854916,107.));
#45840=CARTESIAN_POINT('Ctrl Pts',(-34.4744466082576,-90.0395396993188,
107.));
#45841=CARTESIAN_POINT('Ctrl Pts',(-34.4451578629574,-90.0102611375584,
107.));
#45842=CARTESIAN_POINT('Ctrl Pts',(-34.4164514207639,-89.9803836100269,
107.));
#45843=CARTESIAN_POINT('Ctrl Pts',(-34.3883503519563,-89.949925051172,107.));
#45844=CARTESIAN_POINT('Ctrl Pts',(-34.3787143478639,-89.9394806513599,
107.));
#45845=CARTESIAN_POINT('Ctrl Pts',(-34.3691502594248,-89.9289686396398,
107.));
#45846=CARTESIAN_POINT('Ctrl Pts',(-34.3596656532768,-89.9183973517283,
107.));
#45847=CARTESIAN_POINT('Ctrl Pts',(-34.2938684614213,-89.8450615644514,
107.));
#45848=CARTESIAN_POINT('Ctrl Pts',(-34.2318034199732,-89.7687791536545,
107.));
#45849=CARTESIAN_POINT('Ctrl Pts',(-34.1737142975659,-89.6898286775609,
107.));
#45850=CARTESIAN_POINT('Ctrl Pts',(-34.1161516327794,-89.6115937240657,
107.));
#45851=CARTESIAN_POINT('Ctrl Pts',(-34.0624927127841,-89.5307380625027,
107.));
#45852=CARTESIAN_POINT('Ctrl Pts',(-34.0130204815364,-89.447510360224,107.));
#45853=CARTESIAN_POINT('Ctrl Pts',(-33.9649625424885,-89.366661937941,107.));
#45854=CARTESIAN_POINT('Ctrl Pts',(-33.9208551306922,-89.283574459218,107.));
#45855=CARTESIAN_POINT('Ctrl Pts',(-33.8810053974435,-89.1984655452966,
107.));
#45856=CARTESIAN_POINT('Ctrl Pts',(-33.8602009805094,-89.1540325921578,
107.));
#45857=CARTESIAN_POINT('Ctrl Pts',(-33.8405578495624,-89.1090485695462,
107.));
#45858=CARTESIAN_POINT('Ctrl Pts',(-33.8221254047308,-89.0635442081576,
107.));
#45859=CARTESIAN_POINT('Ctrl Pts',(-33.815067321247,-89.0461198466857,107.));
#45860=CARTESIAN_POINT('Ctrl Pts',(-33.8081867972032,-89.0286191918009,
107.));
#45861=CARTESIAN_POINT('Ctrl Pts',(-33.8014867681844,-89.0110439776197,
107.));
#45862=CARTESIAN_POINT('Ctrl Pts',(-33.7962450333404,-88.9972940949988,
107.));
#45863=CARTESIAN_POINT('Ctrl Pts',(-33.7911136745704,-88.9834980764818,
107.));
#45864=CARTESIAN_POINT('Ctrl Pts',(-33.7860992270484,-88.9696714653787,
107.));
#45865=CARTESIAN_POINT('Ctrl Pts',(-33.7544155410359,-88.8823083006666,
107.));
#45866=CARTESIAN_POINT('Ctrl Pts',(-33.7273406805785,-88.7935841918564,
107.));
#45867=CARTESIAN_POINT('Ctrl Pts',(-33.7051259018102,-88.7037226902072,
107.));
#45868=CARTESIAN_POINT('Ctrl Pts',(-33.7001419285477,-88.6835619077742,
107.));
#45869=CARTESIAN_POINT('Ctrl Pts',(-33.6954027892081,-88.6633438353985,
107.));
#45870=CARTESIAN_POINT('Ctrl Pts',(-33.6909116819337,-88.6430709420454,
107.));
#45871=CARTESIAN_POINT('Ctrl Pts',(-33.6705459299635,-88.5511397784083,
107.));
#45872=CARTESIAN_POINT('Ctrl Pts',(-33.6552763905805,-88.4580809934608,
107.));
#45873=CARTESIAN_POINT('Ctrl Pts',(-33.6449932387159,-88.3642861744627,
107.));
#45874=CARTESIAN_POINT('Ctrl Pts',(-33.6342593787364,-88.2663803507243,
107.));
#45875=CARTESIAN_POINT('Ctrl Pts',(-33.6289586023237,-88.1676713209843,
107.));
#45876=CARTESIAN_POINT('Ctrl Pts',(-33.6290234622339,-88.0686191026489,
107.));
#45877=CARTESIAN_POINT('Ctrl Pts',(-33.6290488323814,-88.0298745317877,
107.));
#45878=CARTESIAN_POINT('Ctrl Pts',(-33.6298957475537,-87.9910777096528,
107.));
#45879=CARTESIAN_POINT('Ctrl Pts',(-33.6315623951404,-87.9522573940279,
107.));
#45880=CARTESIAN_POINT('Ctrl Pts',(-33.6320954345873,-87.9398415961512,
107.));
#45881=CARTESIAN_POINT('Ctrl Pts',(-33.6327123205129,-87.9274247064713,
107.));
#45882=CARTESIAN_POINT('Ctrl Pts',(-33.6334122917911,-87.9150173343413,
107.));
#45883=CARTESIAN_POINT('Ctrl Pts',(-33.6386515097086,-87.8221493433258,
107.));
#45884=CARTESIAN_POINT('Ctrl Pts',(-33.6485471485414,-87.729664583953,107.));
#45885=CARTESIAN_POINT('Ctrl Pts',(-33.6629757491884,-87.6379346339504,
107.));
#45886=CARTESIAN_POINT('Ctrl Pts',(-33.6773703612078,-87.5464207669331,
107.));
#45887=CARTESIAN_POINT('Ctrl Pts',(-33.6962770140278,-87.4556572120266,
107.));
#45888=CARTESIAN_POINT('Ctrl Pts',(-33.7196217950054,-87.3660298796492,
107.));
#45889=CARTESIAN_POINT('Ctrl Pts',(-33.74257042567,-87.2779234823281,107.));
#45890=CARTESIAN_POINT('Ctrl Pts',(-33.7698083039621,-87.1909142870507,
107.));
#45891=CARTESIAN_POINT('Ctrl Pts',(-33.8013056575605,-87.1053979868551,
107.));
#45892=CARTESIAN_POINT('Ctrl Pts',(-33.8171471021691,-87.0623879692535,
107.));
#45893=CARTESIAN_POINT('Ctrl Pts',(-33.834066596719,-87.0197561200163,107.));
#45894=CARTESIAN_POINT('Ctrl Pts',(-33.8520637709505,-86.9775565705104,
107.));
#45895=CARTESIAN_POINT('Ctrl Pts',(-33.8576294774237,-86.9645061714404,
107.));
#45896=CARTESIAN_POINT('Ctrl Pts',(-33.8632982668804,-86.9514971375181,
107.));
#45897=CARTESIAN_POINT('Ctrl Pts',(-33.8690701692463,-86.9385311273666,
107.));
#45898=CARTESIAN_POINT('Ctrl Pts',(-33.8747496330137,-86.9257727714217,
107.));
#45899=CARTESIAN_POINT('Ctrl Pts',(-33.8805254520977,-86.9130639366889,
107.));
#45900=CARTESIAN_POINT('Ctrl Pts',(-33.8863958367835,-86.9004091087509,
107.));
#45901=CARTESIAN_POINT('Ctrl Pts',(-33.9238756397803,-86.8196136441493,
107.));
#45902=CARTESIAN_POINT('Ctrl Pts',(-33.9652255993582,-86.7409749585095,
107.));
#45903=CARTESIAN_POINT('Ctrl Pts',(-34.0103760392298,-86.6648406433426,
107.));
#45904=CARTESIAN_POINT('Ctrl Pts',(-34.0547690445968,-86.5899835418078,
107.));
#45905=CARTESIAN_POINT('Ctrl Pts',(-34.1028365417562,-86.5175468204594,
107.));
#45906=CARTESIAN_POINT('Ctrl Pts',(-34.1545485155578,-86.4478950466225,
107.));
#45907=CARTESIAN_POINT('Ctrl Pts',(-34.2046829695647,-86.3803680621503,
107.));
#45908=CARTESIAN_POINT('Ctrl Pts',(-34.2582433786248,-86.315458261135,107.));
#45909=CARTESIAN_POINT('Ctrl Pts',(-34.3152301022523,-86.2535381385478,
107.));
#45910=CARTESIAN_POINT('Ctrl Pts',(-34.3361976980218,-86.2307553565634,
107.));
#45911=CARTESIAN_POINT('Ctrl Pts',(-34.3576293877451,-86.2083777473769,
107.));
#45912=CARTESIAN_POINT('Ctrl Pts',(-34.3795260005218,-86.1864254754535,
107.));
#45913=CARTESIAN_POINT('Ctrl Pts',(-34.3986034365815,-86.1672995463313,
107.));
#45914=CARTESIAN_POINT('Ctrl Pts',(-34.4180338060146,-86.1484965041123,
107.));
#45915=CARTESIAN_POINT('Ctrl Pts',(-34.437806971968,-86.1300214773104,107.));
#45916=CARTESIAN_POINT('Origin',(-36.3549260746835,-87.7685555885722,124.208423447177));
#45917=CARTESIAN_POINT('Ctrl Pts',(-39.4317256223809,-87.7666280037969,
121.708423447177));
#45918=CARTESIAN_POINT('Ctrl Pts',(-39.4326483047755,-87.6433531015923,
121.702019850418));
#45919=CARTESIAN_POINT('Ctrl Pts',(-39.3701218467006,-86.5074462896477,
121.642966745928));
#45920=CARTESIAN_POINT('Ctrl Pts',(-37.9573948034252,-84.5150171095306,
121.531264133707));
#45921=CARTESIAN_POINT('Ctrl Pts',(-34.5067286900242,-84.648392448822,121.373315610515));
#45922=CARTESIAN_POINT('Ctrl Pts',(-32.7318386198642,-87.6103338151322,
121.215367087322));
#45923=CARTESIAN_POINT('Ctrl Pts',(-34.2418568983793,-90.7159201684501,
121.05741856413));
#45924=CARTESIAN_POINT('Ctrl Pts',(-37.6677476810076,-91.149128255265,120.899470040937));
#45925=CARTESIAN_POINT('Ctrl Pts',(-39.3142946536224,-89.2107570149594,
120.783138335286));
#45926=CARTESIAN_POINT('Ctrl Pts',(-39.4311722823457,-87.984115255456,120.719456137367));
#45927=CARTESIAN_POINT('Ctrl Pts',(-39.4292404520863,-87.7712393069318,
120.708423447177));
#45928=CARTESIAN_POINT('Ctrl Pts',(-39.4252046443693,-87.771569957437,121.791576552823));
#45929=CARTESIAN_POINT('Ctrl Pts',(-39.4202197512721,-87.0785516532724,
121.755752019753));
#45930=CARTESIAN_POINT('Ctrl Pts',(-38.847832523077,-85.3573626625651,121.667277978953));
#45931=CARTESIAN_POINT('Ctrl Pts',(-36.0033916957587,-84.1596937777799,
121.526154430423));
#45932=CARTESIAN_POINT('Ctrl Pts',(-33.1409988246472,-86.0888162082167,
121.36820590723));
#45933=CARTESIAN_POINT('Ctrl Pts',(-33.1913892046506,-89.5420981815712,
121.210257384038));
#45934=CARTESIAN_POINT('Ctrl Pts',(-36.1106392225623,-91.3867838745725,
121.052308860845));
#45935=CARTESIAN_POINT('Ctrl Pts',(-38.8854865669341,-90.1183415880482,
120.912748583774));
#45936=CARTESIAN_POINT('Ctrl Pts',(-39.4210163858766,-88.4296040393632,
120.825837814433));
#45937=CARTESIAN_POINT('Ctrl Pts',(-39.4253676065904,-87.7664047027925,
120.791576552823));
#45938=CARTESIAN_POINT('Ctrl Pts',(-34.4414600780185,-86.1325683851972,
122.));
#45939=CARTESIAN_POINT('Ctrl Pts',(-33.9002646916969,-86.7655555914187,
121.947350492269));
#45940=CARTESIAN_POINT('Ctrl Pts',(-33.5049263244719,-88.6005872421791,
121.842051476808));
#45941=CARTESIAN_POINT('Ctrl Pts',(-35.495725323147,-90.613755383703,121.684102953615));
#45942=CARTESIAN_POINT('Ctrl Pts',(-38.2666281885584,-90.0415106136082,
121.526154430423));
#45943=CARTESIAN_POINT('Ctrl Pts',(-39.3037452815429,-87.4112440285999,
121.36820590723));
#45944=CARTESIAN_POINT('Ctrl Pts',(-37.6675062030737,-85.1035862959133,
121.210257384038));
#45945=CARTESIAN_POINT('Ctrl Pts',(-34.8410699120416,-85.2128338692552,
121.052308860845));
#45946=CARTESIAN_POINT('Ctrl Pts',(-33.3872596788782,-87.6389563321429,
120.894360337653));
#45947=CARTESIAN_POINT('Ctrl Pts',(-34.6241137592953,-90.182738223953,120.73641181446));
#45948=CARTESIAN_POINT('Ctrl Pts',(-37.430256607926,-90.5375784252076,120.578463291268));
#45949=CARTESIAN_POINT('Ctrl Pts',(-39.2614232167573,-88.3818666539668,
120.420514768075));
#45950=CARTESIAN_POINT('Ctrl Pts',(-38.4573605460916,-85.6700664907204,
120.262566244883));
#45951=CARTESIAN_POINT('Ctrl Pts',(-35.7470828869712,-84.8609112744695,
120.10461772169));
#45952=CARTESIAN_POINT('Ctrl Pts',(-33.5879189354126,-86.6880244932926,
119.946669198498));
#45953=CARTESIAN_POINT('Ctrl Pts',(-33.9375158250034,-89.4948244513467,
119.788720675305));
#45954=CARTESIAN_POINT('Ctrl Pts',(-36.4789052492319,-90.7364679329367,
119.630772152113));
#45955=CARTESIAN_POINT('Ctrl Pts',(-38.9078864373474,-89.2871960434334,
119.472823628921));
#45956=CARTESIAN_POINT('Ctrl Pts',(-39.0221761527905,-86.4610188042813,
119.314875105728));
#45957=CARTESIAN_POINT('Ctrl Pts',(-36.7181513220674,-84.82034551555,119.156926582536));
#45958=CARTESIAN_POINT('Ctrl Pts',(-34.0848012167929,-85.8527245783361,
118.998978059343));
#45959=CARTESIAN_POINT('Ctrl Pts',(-33.5097042724549,-88.6221293779351,
118.841029536151));
#45960=CARTESIAN_POINT('Ctrl Pts',(-35.5142834051126,-90.6176247697674,
118.683081012958));
#45961=CARTESIAN_POINT('Ctrl Pts',(-38.2810476781003,-90.0299557919626,
118.525132489766));
#45962=CARTESIAN_POINT('Ctrl Pts',(-39.3014560741837,-87.3919440239953,
118.367183966573));
#45963=CARTESIAN_POINT('Ctrl Pts',(-37.6503353341005,-85.0953945090273,
118.209235443381));
#45964=CARTESIAN_POINT('Ctrl Pts',(-34.8247064167312,-85.2225188436243,
118.051286920188));
#45965=CARTESIAN_POINT('Ctrl Pts',(-33.3864811236342,-87.6580572610179,
117.893338396996));
#45966=CARTESIAN_POINT('Ctrl Pts',(-34.6396545865135,-90.1937811511754,
117.735389873803));
#45967=CARTESIAN_POINT('Ctrl Pts',(-37.4480125400769,-90.530626783707,117.577441350611));
#45968=CARTESIAN_POINT('Ctrl Pts',(-39.2653022401977,-88.3631864681666,
117.419492827418));
#45969=CARTESIAN_POINT('Ctrl Pts',(-38.443842386133,-85.6566124189988,117.261544304226));
#45970=CARTESIAN_POINT('Ctrl Pts',(-35.7284256439965,-84.8648730098256,
117.103595781034));
#45971=CARTESIAN_POINT('Ctrl Pts',(-33.5810377882138,-86.7058142832929,
116.945647257841));
#45972=CARTESIAN_POINT('Ctrl Pts',(-33.9486500777749,-89.5103107764393,
116.787698734649));
#45973=CARTESIAN_POINT('Ctrl Pts',(-36.4979596301566,-90.7356108138369,
116.629750211456));
#45974=CARTESIAN_POINT('Ctrl Pts',(-38.9175850079598,-89.2707721173922,
116.471801688264));
#45975=CARTESIAN_POINT('Ctrl Pts',(-39.0137254707097,-86.4439193821171,
116.313853165071));
#45976=CARTESIAN_POINT('Ctrl Pts',(-36.6992133848109,-84.8180740082457,
116.155904641879));
#45977=CARTESIAN_POINT('Ctrl Pts',(-34.0725464658448,-85.8673405484154,
115.997956118686));
#45978=CARTESIAN_POINT('Ctrl Pts',(-33.5152437227748,-88.6403809426538,
115.840007595494));
#45979=CARTESIAN_POINT('Ctrl Pts',(-35.5325946031457,-90.6229638037158,
115.682059072301));
#45980=CARTESIAN_POINT('Ctrl Pts',(-38.2955284186788,-90.0175415490088,
115.524110549109));
#45981=CARTESIAN_POINT('Ctrl Pts',(-39.2989771096636,-87.37303212379,115.366162025916));
#45982=CARTESIAN_POINT('Ctrl Pts',(-37.6331442664967,-85.0871317947868,
115.208213502724));
#45983=CARTESIAN_POINT('Ctrl Pts',(-34.8083898640617,-85.2323968677906,
115.050264979531));
#45984=CARTESIAN_POINT('Ctrl Pts',(-33.3858328080249,-87.6771199191464,
114.892316456339));
#45985=CARTESIAN_POINT('Ctrl Pts',(-34.6552623159776,-90.2047449110804,
114.734367933147));
#45986=CARTESIAN_POINT('Ctrl Pts',(-37.4657252610125,-90.5235511376453,
114.576419409954));
#45987=CARTESIAN_POINT('Ctrl Pts',(-39.269060367233,-88.3444866892675,114.418470886762));
#45988=CARTESIAN_POINT('Ctrl Pts',(-38.430238539787,-85.6432430280421,114.260522363569));
#45989=CARTESIAN_POINT('Ctrl Pts',(-35.7097940180071,-84.8689556269897,
114.102573840377));
#45990=CARTESIAN_POINT('Ctrl Pts',(-33.5742711112112,-86.7236473237577,
113.944625317184));
#45991=CARTESIAN_POINT('Ctrl Pts',(-33.9598834899978,-89.5257255647848,
113.786676793992));
#45992=CARTESIAN_POINT('Ctrl Pts',(-36.5170081383915,-90.734631230289,113.628728270799));
#45993=CARTESIAN_POINT('Ctrl Pts',(-38.9271779091243,-89.2542863205614,
113.470779747607));
#45994=CARTESIAN_POINT('Ctrl Pts',(-39.0051651730729,-86.4268745425969,
113.312831224414));
#45995=CARTESIAN_POINT('Ctrl Pts',(-36.6802612498903,-84.8159241636338,
113.154882701222));
#45996=CARTESIAN_POINT('Ctrl Pts',(-34.0603858179699,-85.8820348974369,
112.996934178029));
#45997=CARTESIAN_POINT('Ctrl Pts',(-33.5209002515244,-88.6585965659594,
112.838985654837));
#45998=CARTESIAN_POINT('Ctrl Pts',(-35.550939705938,-90.6281851496574,112.681037131644));
#45999=CARTESIAN_POINT('Ctrl Pts',(-38.3099291487532,-90.0050345820214,
112.523088608452));
#46000=CARTESIAN_POINT('Ctrl Pts',(-39.29637676304,-87.3541365304588,112.365140085259));
#46001=CARTESIAN_POINT('Ctrl Pts',(-37.6159004983729,-85.0789796349018,
112.207191562067));
#46002=CARTESIAN_POINT('Ctrl Pts',(-34.7921370745499,-85.2423794567828,
112.049243038875));
#46003=CARTESIAN_POINT('Ctrl Pts',(-33.3853069070695,-87.6961863471835,
111.891294515682));
#46004=CARTESIAN_POINT('Ctrl Pts',(-34.6709401219796,-90.2156082277396,
111.733345992489));
#46005=CARTESIAN_POINT('Ctrl Pts',(-37.4833921840904,-90.5163619041062,
111.575397469297));
#46006=CARTESIAN_POINT('Ctrl Pts',(-39.2726983455438,-88.325763164926,111.417448946105));
#46007=CARTESIAN_POINT('Ctrl Pts',(-38.4165491290474,-85.6299612629752,
111.259500422912));
#46008=CARTESIAN_POINT('Ctrl Pts',(-35.6911889905757,-84.8731577936227,
111.10155189972));
#46009=CARTESIAN_POINT('Ctrl Pts',(-33.5676190796432,-86.7415234454372,
110.943603376527));
#46010=CARTESIAN_POINT('Ctrl Pts',(-33.9712156489426,-89.5410679056005,
110.785654853335));
#46011=CARTESIAN_POINT('Ctrl Pts',(-36.5360499641112,-90.7335293565653,
110.627706330142));
#46012=CARTESIAN_POINT('Ctrl Pts',(-38.9366647571119,-89.2377392674329,
110.46975780695));
#46013=CARTESIAN_POINT('Ctrl Pts',(-38.9964956073178,-86.4098850204116,
110.311809283757));
#46014=CARTESIAN_POINT('Ctrl Pts',(-36.6612957008989,-84.8138960543492,
110.153860760565));
#46015=CARTESIAN_POINT('Ctrl Pts',(-34.0483197744451,-85.8968070283112,
109.995912237372));
#46016=CARTESIAN_POINT('Ctrl Pts',(-33.5266736235439,-88.6767754905713,
109.83796371418));
#46017=CARTESIAN_POINT('Ctrl Pts',(-35.5693179621701,-90.6332885994736,
109.680015190987));
#46018=CARTESIAN_POINT('Ctrl Pts',(-38.3242492637062,-89.9924353947184,
109.522066667795));
#46019=CARTESIAN_POINT('Ctrl Pts',(-39.2936551641482,-87.335258046265,109.364118144603));
#46020=CARTESIAN_POINT('Ctrl Pts',(-37.5986046940346,-85.0709383184164,
109.20616962141));
#46021=CARTESIAN_POINT('Ctrl Pts',(-34.7759488142895,-85.2524662955004,
109.048221098218));
#46022=CARTESIAN_POINT('Ctrl Pts',(-33.3849032449937,-87.7152555607639,
108.890272575025));
#46023=CARTESIAN_POINT('Ctrl Pts',(-34.686687764235,-90.2263710609368,108.732324051833));
#46024=CARTESIAN_POINT('Ctrl Pts',(-37.5010117457022,-90.5090585411099,
108.57437552864));
#46025=CARTESIAN_POINT('Ctrl Pts',(-39.2762177428359,-88.3070183913275,
108.416427005448));
#46026=CARTESIAN_POINT('Ctrl Pts',(-38.4027711856895,-85.6167641253612,
108.258478482255));
#46027=CARTESIAN_POINT('Ctrl Pts',(-35.672618594028,-84.8774866292816,108.100529959063));
#46028=CARTESIAN_POINT('Ctrl Pts',(-33.5610670260011,-86.7594269128483,
107.94258143587));
#46029=CARTESIAN_POINT('Ctrl Pts',(-33.9826768167633,-89.5563680122778,
107.784632912678));
#46030=CARTESIAN_POINT('Ctrl Pts',(-36.555021123935,-90.7322417998678,107.626684389485));
#46031=CARTESIAN_POINT('Ctrl Pts',(-38.9461751355661,-89.2212621070181,
107.468735866293));
#46032=CARTESIAN_POINT('Ctrl Pts',(-38.9874498238763,-86.392683146967,107.3107873431));
#46033=CARTESIAN_POINT('Ctrl Pts',(-36.6428674409066,-84.8125415007088,
107.152838819908));
#46034=CARTESIAN_POINT('Ctrl Pts',(-34.035217803829,-85.9105078648088,106.994890296715));
#46035=CARTESIAN_POINT('Ctrl Pts',(-33.534938467138,-88.6972348346522,106.836941773523));
#46036=CARTESIAN_POINT('Ctrl Pts',(-34.9001756782217,-89.9855519312418,
106.731642758061));
#46037=CARTESIAN_POINT('Ctrl Pts',(-35.7047260767089,-90.2006423906074,
106.678993250331));
#46038=CARTESIAN_POINT('Ctrl Pts',(-34.3005945243415,-86.0121302673453,
122.10700224989));
#46039=CARTESIAN_POINT('Ctrl Pts',(-33.7195574121284,-86.691716730324,122.054352742159));
#46040=CARTESIAN_POINT('Ctrl Pts',(-33.2951150221062,-88.6618397545135,
121.949053726697));
#46041=CARTESIAN_POINT('Ctrl Pts',(-35.4324726759634,-90.8232133229407,
121.791105203505));
#46042=CARTESIAN_POINT('Ctrl Pts',(-38.4073638886993,-90.2088410331937,
121.633156680312));
#46043=CARTESIAN_POINT('Ctrl Pts',(-39.5208314753878,-87.3849394635757,
121.47520815712));
#46044=CARTESIAN_POINT('Ctrl Pts',(-37.7641357365242,-84.9073965671192,
121.317259633927));
#46045=CARTESIAN_POINT('Ctrl Pts',(-34.7296228380358,-85.0246867291107,
121.159311110735));
#46046=CARTESIAN_POINT('Ctrl Pts',(-33.1687859925402,-87.6294154931395,
121.001362587543));
#46047=CARTESIAN_POINT('Ctrl Pts',(-34.4966948056566,-90.3604655387852,
120.84341406435));
#46048=CARTESIAN_POINT('Ctrl Pts',(-37.5094202989532,-90.7414283685601,
120.685465541158));
#46049=CARTESIAN_POINT('Ctrl Pts',(-39.4753937445287,-88.4270173924454,
120.527517017965));
#46050=CARTESIAN_POINT('Ctrl Pts',(-38.6121375823184,-85.5155799050329,
120.369568494773));
#46051=CARTESIAN_POINT('Ctrl Pts',(-35.7023346827516,-84.6468562941794,
120.21161997158));
#46052=CARTESIAN_POINT('Ctrl Pts',(-33.3842173836834,-86.6084779472515,
120.053671448388));
#46053=CARTESIAN_POINT('Ctrl Pts',(-33.759550899638,-89.6219089250578,119.895722925195));
#46054=CARTESIAN_POINT('Ctrl Pts',(-36.4880323490067,-90.9549597255175,
119.737774402003));
#46055=CARTESIAN_POINT('Ctrl Pts',(-39.0958302919176,-89.3989953274986,
119.57982587881));
#46056=CARTESIAN_POINT('Ctrl Pts',(-39.2185337884644,-86.3647605517735,
119.421877355618));
#46057=CARTESIAN_POINT('Ctrl Pts',(-36.7448912409745,-84.6033041649243,
119.263928832425));
#46058=CARTESIAN_POINT('Ctrl Pts',(-33.9176791484729,-85.7116849170728,
119.105980309233));
#46059=CARTESIAN_POINT('Ctrl Pts',(-33.3002447130985,-88.6849677793764,
118.94803178604));
#46060=CARTESIAN_POINT('Ctrl Pts',(-35.4523969669423,-90.8273675654965,
118.790083262848));
#46061=CARTESIAN_POINT('Ctrl Pts',(-38.4228449123274,-90.1964355686042,
118.632134739656));
#46062=CARTESIAN_POINT('Ctrl Pts',(-39.5183737411446,-87.3642186310916,
118.474186216463));
#46063=CARTESIAN_POINT('Ctrl Pts',(-37.7457007823939,-84.8986017172065,
118.316237693271));
#46064=CARTESIAN_POINT('Ctrl Pts',(-34.7120546948084,-85.0350846919935,
118.158289170078));
#46065=CARTESIAN_POINT('Ctrl Pts',(-33.1679501216105,-87.6499225943353,
118.000340646886));
#46066=CARTESIAN_POINT('Ctrl Pts',(-34.5133797176062,-90.3723214243045,
117.842392123693));
#46067=CARTESIAN_POINT('Ctrl Pts',(-37.5284833874464,-90.7339649610648,
117.684443600501));
#46068=CARTESIAN_POINT('Ctrl Pts',(-39.4795583339449,-88.4069620085909,
117.526495077308));
#46069=CARTESIAN_POINT('Ctrl Pts',(-38.5976242423615,-85.5011353713612,
117.368546554116));
#46070=CARTESIAN_POINT('Ctrl Pts',(-35.6823039307278,-84.6511096845977,
117.210598030923));
#46071=CARTESIAN_POINT('Ctrl Pts',(-33.3768296601401,-86.6275773861417,
117.052649507731));
#46072=CARTESIAN_POINT('Ctrl Pts',(-33.7715048339112,-89.6385353225436,
116.894700984538));
#46073=CARTESIAN_POINT('Ctrl Pts',(-36.508489475485,-90.9540395070176,116.736752461346));
#46074=CARTESIAN_POINT('Ctrl Pts',(-39.1062428519719,-89.3813623047506,
116.578803938153));
#46075=CARTESIAN_POINT('Ctrl Pts',(-39.2094609840087,-86.3464023042238,
116.420855414961));
#46076=CARTESIAN_POINT('Ctrl Pts',(-36.7245591305151,-84.6008654337788,
116.262906891769));
#46077=CARTESIAN_POINT('Ctrl Pts',(-33.9045222271802,-85.7273768857439,
116.104958368576));
#46078=CARTESIAN_POINT('Ctrl Pts',(-33.3061919667124,-88.7045629879195,
115.947009845384));
#46079=CARTESIAN_POINT('Ctrl Pts',(-35.4720561988855,-90.8330996484852,
115.789061322191));
#46080=CARTESIAN_POINT('Ctrl Pts',(-38.4383916961712,-90.1831074138222,
115.631112798999));
#46081=CARTESIAN_POINT('Ctrl Pts',(-39.5157122801964,-87.3439144744794,
115.473164275806));
#46082=CARTESIAN_POINT('Ctrl Pts',(-37.72724414265,-84.8897307184088,115.315215752614));
#46083=CARTESIAN_POINT('Ctrl Pts',(-34.6945369500458,-85.0456899166149,
115.157267229421));
#46084=CARTESIAN_POINT('Ctrl Pts',(-33.167254078298,-87.6703886073687,114.999318706229));
#46085=CARTESIAN_POINT('Ctrl Pts',(-34.5301364570117,-90.384092314366,114.841370183036));
#46086=CARTESIAN_POINT('Ctrl Pts',(-37.5475000836009,-90.7263684200397,
114.683421659844));
#46087=CARTESIAN_POINT('Ctrl Pts',(-39.4835931268037,-88.3868855892327,
114.525473136651));
#46088=CARTESIAN_POINT('Ctrl Pts',(-38.5830189079561,-85.4867817524837,
114.367524613459));
#46089=CARTESIAN_POINT('Ctrl Pts',(-35.6623006815607,-84.655492855902,114.209576090266));
#46090=CARTESIAN_POINT('Ctrl Pts',(-33.3695648338605,-86.6467232595093,
114.051627567074));
#46091=CARTESIAN_POINT('Ctrl Pts',(-33.7835652275568,-89.6550849168899,
113.893679043881));
#46092=CARTESIAN_POINT('Ctrl Pts',(-36.5289402969378,-90.9529878084809,
113.735730520689));
#46093=CARTESIAN_POINT('Ctrl Pts',(-39.1165419634042,-89.3636628564086,
113.577781997497));
#46094=CARTESIAN_POINT('Ctrl Pts',(-39.200270494318,-86.3281026575837,113.419833474304));
#46095=CARTESIAN_POINT('Ctrl Pts',(-36.7042117771879,-84.5985573218906,
113.261884951112));
#46096=CARTESIAN_POINT('Ctrl Pts',(-33.8914663366415,-85.7431530034586,
113.103936427919));
#46097=CARTESIAN_POINT('Ctrl Pts',(-33.3122649178366,-88.7241196091141,
112.945987904727));
#46098=CARTESIAN_POINT('Ctrl Pts',(-35.4917518315888,-90.8387053795102,
112.788039381534));
#46099=CARTESIAN_POINT('Ctrl Pts',(-38.453852579297,-90.169679708848,112.630090858342));
#46100=CARTESIAN_POINT('Ctrl Pts',(-39.5129205012362,-87.3236278252206,
112.472142335149));
#46101=CARTESIAN_POINT('Ctrl Pts',(-37.7087309226789,-84.8809784127581,
112.314193811957));
#46102=CARTESIAN_POINT('Ctrl Pts',(-34.6770876625573,-85.0564074039161,
112.156245288764));
#46103=CARTESIAN_POINT('Ctrl Pts',(-33.1666894615623,-87.690858667844,111.998296765572));
#46104=CARTESIAN_POINT('Ctrl Pts',(-34.5469684318501,-90.3957553667502,
111.840348242379));
#46105=CARTESIAN_POINT('Ctrl Pts',(-37.5664676103507,-90.7186499294537,
111.682399719187));
#46106=CARTESIAN_POINT('Ctrl Pts',(-39.4874989258283,-88.3667836763398,
111.524451195994));
#46107=CARTESIAN_POINT('Ctrl Pts',(-38.5683217100771,-85.4725222103394,
111.366502672802));
#46108=CARTESIAN_POINT('Ctrl Pts',(-35.6423259890843,-84.6600043776687,
111.20855414961));
#46109=CARTESIAN_POINT('Ctrl Pts',(-33.3624230929842,-86.6659153856447,
111.050605626417));
#46110=CARTESIAN_POINT('Ctrl Pts',(-33.7957316374614,-89.6715567302636,
110.892657103225));
#46111=CARTESIAN_POINT('Ctrl Pts',(-36.5493839439221,-90.9518048170095,
110.734708580032));
#46112=CARTESIAN_POINT('Ctrl Pts',(-39.1267272142361,-89.3458976422023,
110.57676005684));
#46113=CARTESIAN_POINT('Ctrl Pts',(-39.1909626924081,-86.3098624006304,
110.418811533647));
#46114=CARTESIAN_POINT('Ctrl Pts',(-36.6838500222728,-84.5963799072419,
110.260863010455));
#46115=CARTESIAN_POINT('Ctrl Pts',(-33.8785120150366,-85.7590126291711,
110.102914487262));
#46116=CARTESIAN_POINT('Ctrl Pts',(-33.3184633139996,-88.7436368299307,
109.94496596407));
#46117=CARTESIAN_POINT('Ctrl Pts',(-35.5114830584221,-90.8441845351322,
109.787017440877));
#46118=CARTESIAN_POINT('Ctrl Pts',(-38.469226912577,-90.1561529944824,109.629068917685));
#46119=CARTESIAN_POINT('Ctrl Pts',(-39.5099985436573,-87.30335954464,109.471120394492));
#46120=CARTESIAN_POINT('Ctrl Pts',(-37.6901618356908,-84.8723451105772,
109.3131718713));
#46121=CARTESIAN_POINT('Ctrl Pts',(-34.6597076548352,-85.0672368155999,
109.155223348107));
#46122=CARTESIAN_POINT('Ctrl Pts',(-33.1662560826888,-87.7113317189285,
108.997274824915));
#46123=CARTESIAN_POINT('Ctrl Pts',(-34.5638753841477,-90.40731053828,108.839326301722));
#46124=CARTESIAN_POINT('Ctrl Pts',(-37.5853842889775,-90.7108089074273,
108.68137777853));
#46125=CARTESIAN_POINT('Ctrl Pts',(-39.4912774141359,-88.3466589498619,
108.523429255338));
#46126=CARTESIAN_POINT('Ctrl Pts',(-38.5535294619846,-85.4583535257525,
108.365480732145));
#46127=CARTESIAN_POINT('Ctrl Pts',(-35.6223884769483,-84.6646518935827,
108.207532208953));
#46128=CARTESIAN_POINT('Ctrl Pts',(-33.3553886902093,-86.68513687065,108.04958368576));
#46129=CARTESIAN_POINT('Ctrl Pts',(-33.8080365536181,-89.6879832003056,
107.891635162568));
#46130=CARTESIAN_POINT('Ctrl Pts',(-36.5697517227279,-90.9504224729536,
107.733686639375));
#46131=CARTESIAN_POINT('Ctrl Pts',(-39.1369377278005,-89.328207466072,107.575738116183));
#46132=CARTESIAN_POINT('Ctrl Pts',(-39.1812509764153,-86.2913941595414,
107.41778959299));
#46133=CARTESIAN_POINT('Ctrl Pts',(-36.6640651105022,-84.5949256340617,
107.259841069798));
#46134=CARTESIAN_POINT('Ctrl Pts',(-33.8644455034523,-85.7737220939498,
107.101892546605));
#46135=CARTESIAN_POINT('Ctrl Pts',(-33.3273365989096,-88.7656023501531,
106.943944023413));
#46136=CARTESIAN_POINT('Ctrl Pts',(-34.793079852941,-90.1487627841414,106.838645007951));
#46137=CARTESIAN_POINT('Ctrl Pts',(-35.656859648523,-90.379687774511,106.78599550022));
#46138=CARTESIAN_POINT('Ctrl Pts',(-34.1597289706645,-85.8916921494934,
122.21400449978));
#46139=CARTESIAN_POINT('Ctrl Pts',(-33.53885013256,-86.6178778692294,122.161354992049));
#46140=CARTESIAN_POINT('Ctrl Pts',(-33.0853037197404,-88.7230922668478,
122.056055976587));
#46141=CARTESIAN_POINT('Ctrl Pts',(-35.3692200287798,-91.0326712621785,
121.898107453395));
#46142=CARTESIAN_POINT('Ctrl Pts',(-38.5480995888403,-90.3761714527792,
121.740158930202));
#46143=CARTESIAN_POINT('Ctrl Pts',(-39.7379176692327,-87.3586348985517,
121.58221040701));
#46144=CARTESIAN_POINT('Ctrl Pts',(-37.8607652699747,-84.7112068383249,
121.424261883817));
#46145=CARTESIAN_POINT('Ctrl Pts',(-34.61817576403,-84.8365395889664,121.266313360625));
#46146=CARTESIAN_POINT('Ctrl Pts',(-32.9503123062022,-87.6198746541358,
121.108364837432));
#46147=CARTESIAN_POINT('Ctrl Pts',(-34.369275852018,-90.5381928536177,120.95041631424));
#46148=CARTESIAN_POINT('Ctrl Pts',(-37.5885839899804,-90.9452783119125,
120.792467791047));
#46149=CARTESIAN_POINT('Ctrl Pts',(-39.6893642723,-88.472168130924,120.634519267855));
#46150=CARTESIAN_POINT('Ctrl Pts',(-38.7669146185452,-85.3610933193452,
120.476570744662));
#46151=CARTESIAN_POINT('Ctrl Pts',(-35.6575864785321,-84.4328013138893,
120.31862222147));
#46152=CARTESIAN_POINT('Ctrl Pts',(-33.1805158319542,-86.5289314012103,
120.160673698278));
#46153=CARTESIAN_POINT('Ctrl Pts',(-33.5815859742726,-89.7489933987689,
120.002725175085));
#46154=CARTESIAN_POINT('Ctrl Pts',(-36.4971594487814,-91.1734515180982,
119.844776651893));
#46155=CARTESIAN_POINT('Ctrl Pts',(-39.2837741464878,-89.510794611564,119.6868281287));
#46156=CARTESIAN_POINT('Ctrl Pts',(-39.4148914241384,-86.2685022992656,
119.528879605508));
#46157=CARTESIAN_POINT('Ctrl Pts',(-36.7716311598815,-84.3862628142986,
119.370931082315));
#46158=CARTESIAN_POINT('Ctrl Pts',(-33.7505570801529,-85.5706452558094,
119.212982559123));
#46159=CARTESIAN_POINT('Ctrl Pts',(-33.0907851537421,-88.7478061808178,
119.05503403593));
#46160=CARTESIAN_POINT('Ctrl Pts',(-35.390510528772,-91.0371103612257,118.897085512738));
#46161=CARTESIAN_POINT('Ctrl Pts',(-38.5646421465544,-90.3629153452456,
118.739136989545));
#46162=CARTESIAN_POINT('Ctrl Pts',(-39.7352914081054,-87.336493238188,118.581188466353));
#46163=CARTESIAN_POINT('Ctrl Pts',(-37.8410662306873,-84.7018089253856,
118.42323994316));
#46164=CARTESIAN_POINT('Ctrl Pts',(-34.5994029728857,-84.8476505403629,
118.265291419968));
#46165=CARTESIAN_POINT('Ctrl Pts',(-32.9494191195869,-87.6417879276527,
118.107342896776));
#46166=CARTESIAN_POINT('Ctrl Pts',(-34.3871048486989,-90.5508616974336,
117.949394373583));
#46167=CARTESIAN_POINT('Ctrl Pts',(-37.608954234816,-90.9373031384225,117.79144585039));
#46168=CARTESIAN_POINT('Ctrl Pts',(-39.6938144276922,-88.4507375490153,
117.633497327198));
#46169=CARTESIAN_POINT('Ctrl Pts',(-38.75140609859,-85.3456583237236,117.475548804006));
#46170=CARTESIAN_POINT('Ctrl Pts',(-35.6361822174592,-84.4373463593699,
117.317600280813));
#46171=CARTESIAN_POINT('Ctrl Pts',(-33.1726215320663,-86.5493404889904,
117.159651757621));
#46172=CARTESIAN_POINT('Ctrl Pts',(-33.5943595900474,-89.7667598686481,
117.001703234428));
#46173=CARTESIAN_POINT('Ctrl Pts',(-36.5190193208135,-91.1724682001983,
116.843754711236));
#46174=CARTESIAN_POINT('Ctrl Pts',(-39.2949006959841,-89.4919524921089,
116.685806188043));
#46175=CARTESIAN_POINT('Ctrl Pts',(-39.4051964973076,-86.2488852263305,
116.527857664851));
#46176=CARTESIAN_POINT('Ctrl Pts',(-36.7499048762192,-84.3836568593119,
116.369909141658));
#46177=CARTESIAN_POINT('Ctrl Pts',(-33.7364979885157,-85.5874132230723,
116.211960618466));
#46178=CARTESIAN_POINT('Ctrl Pts',(-33.09714021065,-88.7687450331853,116.054012095273));
#46179=CARTESIAN_POINT('Ctrl Pts',(-35.4115177946254,-91.0432354932543,
115.896063572081));
#46180=CARTESIAN_POINT('Ctrl Pts',(-38.5812549736636,-90.3486732786356,
115.738115048888));
#46181=CARTESIAN_POINT('Ctrl Pts',(-39.7324474507292,-87.3147968251685,
115.580166525696));
#46182=CARTESIAN_POINT('Ctrl Pts',(-37.8213440188034,-84.6923296420309,
115.422218002503));
#46183=CARTESIAN_POINT('Ctrl Pts',(-34.5806840360298,-84.8589829654392,
115.264269479311));
#46184=CARTESIAN_POINT('Ctrl Pts',(-32.9486753485711,-87.6636572955911,
115.106320956118));
#46185=CARTESIAN_POINT('Ctrl Pts',(-34.4050105980457,-90.5634397176517,
114.948372432926));
#46186=CARTESIAN_POINT('Ctrl Pts',(-37.6292749061893,-90.9291857024342,
114.790423909734));
#46187=CARTESIAN_POINT('Ctrl Pts',(-39.6981258863743,-88.4292844891979,
114.632475386541));
#46188=CARTESIAN_POINT('Ctrl Pts',(-38.7357992761253,-85.3303204769252,
114.474526863349));
#46189=CARTESIAN_POINT('Ctrl Pts',(-35.6148073451141,-84.4420300848144,
114.316578340156));
#46190=CARTESIAN_POINT('Ctrl Pts',(-33.1648585565099,-86.5697991952607,
114.158629816964));
#46191=CARTESIAN_POINT('Ctrl Pts',(-33.6072469651159,-89.7844442689952,
114.000681293771));
#46192=CARTESIAN_POINT('Ctrl Pts',(-36.5408724554843,-91.1713443866728,
113.842732770579));
#46193=CARTESIAN_POINT('Ctrl Pts',(-39.3059060176841,-89.4730393922558,
113.684784247386));
#46194=CARTESIAN_POINT('Ctrl Pts',(-39.3953758155633,-86.2293307725704,
113.526835724194));
#46195=CARTESIAN_POINT('Ctrl Pts',(-36.7281623044855,-84.3811904801474,
113.368887201001));
#46196=CARTESIAN_POINT('Ctrl Pts',(-33.7225468553131,-85.6042711094801,
113.210938677809));
#46197=CARTESIAN_POINT('Ctrl Pts',(-33.1036295841489,-88.7896426522691,
113.052990154616));
#46198=CARTESIAN_POINT('Ctrl Pts',(-35.4325639572396,-91.049225609363,112.895041631424));
#46199=CARTESIAN_POINT('Ctrl Pts',(-38.5977760098409,-90.3343248356746,
112.737093108231));
#46200=CARTESIAN_POINT('Ctrl Pts',(-39.7294642394323,-87.2931191199824,
112.579144585039));
#46201=CARTESIAN_POINT('Ctrl Pts',(-37.8015613469849,-84.6829771906143,
112.421196061847));
#46202=CARTESIAN_POINT('Ctrl Pts',(-34.5620382505646,-84.8704353510495,
112.263247538654));
#46203=CARTESIAN_POINT('Ctrl Pts',(-32.9480720160551,-87.6855309885044,
112.105299015462));
#46204=CARTESIAN_POINT('Ctrl Pts',(-34.4229967417206,-90.5759025057607,
111.947350492269));
#46205=CARTESIAN_POINT('Ctrl Pts',(-37.6495430366109,-90.9209379548012,
111.789401969077));
#46206=CARTESIAN_POINT('Ctrl Pts',(-39.7022995061128,-88.4078041877537,
111.631453445884));
#46207=CARTESIAN_POINT('Ctrl Pts',(-38.7200942911067,-85.3150831577036,
111.473504922692));
#46208=CARTESIAN_POINT('Ctrl Pts',(-35.5934629875929,-84.4468509617149,
111.315556399499));
#46209=CARTESIAN_POINT('Ctrl Pts',(-33.1572271063251,-86.590307325852,111.157607876307));
#46210=CARTESIAN_POINT('Ctrl Pts',(-33.6202476259802,-89.8020455549267,
110.999659353114));
#46211=CARTESIAN_POINT('Ctrl Pts',(-36.562717923733,-91.1700802774536,110.841710829922));
#46212=CARTESIAN_POINT('Ctrl Pts',(-39.3167896713602,-89.4540560169718,
110.683762306729));
#46213=CARTESIAN_POINT('Ctrl Pts',(-39.3854297774984,-86.2098397808493,
110.525813783537));
#46214=CARTESIAN_POINT('Ctrl Pts',(-36.7064043436466,-84.3788637601345,
110.367865260344));
#46215=CARTESIAN_POINT('Ctrl Pts',(-33.7087042556281,-85.6212182300311,
110.209916737152));
#46216=CARTESIAN_POINT('Ctrl Pts',(-33.1102530044553,-88.81049816929,110.05196821396));
#46217=CARTESIAN_POINT('Ctrl Pts',(-35.453648154674,-91.0550804707907,109.894019690767));
#46218=CARTESIAN_POINT('Ctrl Pts',(-38.6142045614478,-90.3198705942462,
109.736071167574));
#46219=CARTESIAN_POINT('Ctrl Pts',(-39.7263419231664,-87.2714610430151,
109.578122644382));
#46220=CARTESIAN_POINT('Ctrl Pts',(-37.7817189773471,-84.6737519027377,
109.42017412119));
#46221=CARTESIAN_POINT('Ctrl Pts',(-34.5434664953808,-84.8820073356995,
109.262225597997));
#46222=CARTESIAN_POINT('Ctrl Pts',(-32.9476089203839,-87.7074078770932,
109.104277074805));
#46223=CARTESIAN_POINT('Ctrl Pts',(-34.4410630040604,-90.5882500156232,
108.946328551612));
#46224=CARTESIAN_POINT('Ctrl Pts',(-37.6697568322527,-90.9125592737444,
108.78838002842));
#46225=CARTESIAN_POINT('Ctrl Pts',(-39.7063370854358,-88.3862995083966,
108.630431505227));
#46226=CARTESIAN_POINT('Ctrl Pts',(-38.7042877382798,-85.2999429261436,
108.472482982035));
#46227=CARTESIAN_POINT('Ctrl Pts',(-35.5721583598686,-84.451817157884,108.314534458842));
#46228=CARTESIAN_POINT('Ctrl Pts',(-33.1497103544175,-86.6108468284517,
108.15658593565));
#46229=CARTESIAN_POINT('Ctrl Pts',(-33.633396290473,-89.8195983883335,107.998637412457));
#46230=CARTESIAN_POINT('Ctrl Pts',(-36.5844823215209,-91.1686031460394,
107.840688889265));
#46231=CARTESIAN_POINT('Ctrl Pts',(-39.327700320035,-89.4351528251261,107.682740366072));
#46232=CARTESIAN_POINT('Ctrl Pts',(-39.3750521289544,-86.1901051721157,
107.52479184288));
#46233=CARTESIAN_POINT('Ctrl Pts',(-36.6852627800977,-84.3773097674146,
107.366843319688));
#46234=CARTESIAN_POINT('Ctrl Pts',(-33.6936732030756,-85.6369363230908,
107.208894796495));
#46235=CARTESIAN_POINT('Ctrl Pts',(-33.1197347306812,-88.833969865654,107.050946273303));
#46236=CARTESIAN_POINT('Ctrl Pts',(-34.6859840276602,-90.311973637041,106.945647257841));
#46237=CARTESIAN_POINT('Ctrl Pts',(-35.6089932203371,-90.5587331584145,
106.89299775011));
#46238=CARTESIAN_POINT('Ctrl Pts',(-34.0188634169875,-85.7712540316415,
122.321006749669));
#46239=CARTESIAN_POINT('Ctrl Pts',(-33.3581428529916,-86.5440390081347,
122.268357241939));
#46240=CARTESIAN_POINT('Ctrl Pts',(-32.8754924173746,-88.7843447791822,
122.163058226477));
#46241=CARTESIAN_POINT('Ctrl Pts',(-35.3059673815962,-91.2421292014162,
122.005109703285));
#46242=CARTESIAN_POINT('Ctrl Pts',(-38.6888352889812,-90.5435018723648,
121.847161180092));
#46243=CARTESIAN_POINT('Ctrl Pts',(-39.9550038630777,-87.3323303335276,
121.6892126569));
#46244=CARTESIAN_POINT('Ctrl Pts',(-37.9573948034252,-84.5150171095306,
121.531264133707));
#46245=CARTESIAN_POINT('Ctrl Pts',(-34.5067286900242,-84.648392448822,121.373315610515));
#46246=CARTESIAN_POINT('Ctrl Pts',(-32.7318386198642,-87.6103338151322,
121.215367087322));
#46247=CARTESIAN_POINT('Ctrl Pts',(-34.2418568983793,-90.7159201684501,
121.05741856413));
#46248=CARTESIAN_POINT('Ctrl Pts',(-37.6677476810076,-91.149128255265,120.899470040937));
#46249=CARTESIAN_POINT('Ctrl Pts',(-39.9033348000714,-88.5173188694026,
120.741521517745));
#46250=CARTESIAN_POINT('Ctrl Pts',(-38.921691654772,-85.2066067336577,120.583572994552));
#46251=CARTESIAN_POINT('Ctrl Pts',(-35.6128382743126,-84.2187463335991,
120.42562447136));
#46252=CARTESIAN_POINT('Ctrl Pts',(-32.976814280225,-86.4493848551693,120.267675948167));
#46253=CARTESIAN_POINT('Ctrl Pts',(-33.4036210489072,-89.8760778724798,
120.109727424975));
#46254=CARTESIAN_POINT('Ctrl Pts',(-36.5062865485562,-91.3919433106791,
119.951778901783));
#46255=CARTESIAN_POINT('Ctrl Pts',(-39.4717180010579,-89.6225938956291,
119.79383037859));
#46256=CARTESIAN_POINT('Ctrl Pts',(-39.6112490598123,-86.1722440467577,
119.635881855397));
#46257=CARTESIAN_POINT('Ctrl Pts',(-36.7983710787885,-84.169221463673,119.477933332205));
#46258=CARTESIAN_POINT('Ctrl Pts',(-33.5834350118328,-85.4296055945461,
119.319984809013));
#46259=CARTESIAN_POINT('Ctrl Pts',(-32.8813255943857,-88.8106445822591,
119.16203628582));
#46260=CARTESIAN_POINT('Ctrl Pts',(-35.3286240906017,-91.2468531569549,
119.004087762628));
#46261=CARTESIAN_POINT('Ctrl Pts',(-38.7064393807814,-90.5293951218872,
118.846139239435));
#46262=CARTESIAN_POINT('Ctrl Pts',(-39.9522090750663,-87.3087678452843,
118.688190716243));
#46263=CARTESIAN_POINT('Ctrl Pts',(-37.9364316789807,-84.5050161335647,
118.53024219305));
#46264=CARTESIAN_POINT('Ctrl Pts',(-34.4867512509629,-84.6602163887321,
118.372293669858));
#46265=CARTESIAN_POINT('Ctrl Pts',(-32.7308881175633,-87.6336532609701,
118.214345146665));
#46266=CARTESIAN_POINT('Ctrl Pts',(-34.2608299797916,-90.7294019705626,
118.056396623473));
#46267=CARTESIAN_POINT('Ctrl Pts',(-37.6894250821856,-91.1406413157804,
117.89844810028));
#46268=CARTESIAN_POINT('Ctrl Pts',(-39.9080705214394,-88.4945130894395,
117.740499577088));
#46269=CARTESIAN_POINT('Ctrl Pts',(-38.9051879548185,-85.190181276086,117.582551053895));
#46270=CARTESIAN_POINT('Ctrl Pts',(-35.5900605041904,-84.2235830341421,
117.424602530703));
#46271=CARTESIAN_POINT('Ctrl Pts',(-32.9684134039925,-86.4711035918391,
117.26665400751));
#46272=CARTESIAN_POINT('Ctrl Pts',(-33.4172143461837,-89.8949844147526,
117.108705484318));
#46273=CARTESIAN_POINT('Ctrl Pts',(-36.5295491661419,-91.390896893379,116.950756961125));
#46274=CARTESIAN_POINT('Ctrl Pts',(-39.4835585399962,-89.6025426794672,
116.792808437933));
#46275=CARTESIAN_POINT('Ctrl Pts',(-39.6009320106065,-86.1513681484373,
116.634859914741));
#46276=CARTESIAN_POINT('Ctrl Pts',(-36.7752506219235,-84.1664482848449,
116.476911391548));
#46277=CARTESIAN_POINT('Ctrl Pts',(-33.568473749851,-85.4474495604007,116.318962868356));
#46278=CARTESIAN_POINT('Ctrl Pts',(-32.8880884545876,-88.8329270784509,
116.161014345163));
#46279=CARTESIAN_POINT('Ctrl Pts',(-35.3509793903652,-91.2533713380237,
116.003065821971));
#46280=CARTESIAN_POINT('Ctrl Pts',(-38.724118251156,-90.5142391434489,115.845117298778));
#46281=CARTESIAN_POINT('Ctrl Pts',(-39.949182621262,-87.2856791758579,115.687168775586));
#46282=CARTESIAN_POINT('Ctrl Pts',(-37.9154438949567,-84.494928565653,115.529220252393));
#46283=CARTESIAN_POINT('Ctrl Pts',(-34.4668311220138,-84.6722760142634,
115.371271729201));
#46284=CARTESIAN_POINT('Ctrl Pts',(-32.7300966188443,-87.6569259838135,
115.213323206008));
#46285=CARTESIAN_POINT('Ctrl Pts',(-34.2798847390797,-90.7427871209372,
115.055374682816));
#46286=CARTESIAN_POINT('Ctrl Pts',(-37.7110497287778,-91.1320029848287,
114.897426159623));
#46287=CARTESIAN_POINT('Ctrl Pts',(-39.912658645945,-88.4716833891629,114.739477636431));
#46288=CARTESIAN_POINT('Ctrl Pts',(-38.8885796442944,-85.173859201367,114.581529113239));
#46289=CARTESIAN_POINT('Ctrl Pts',(-35.5673140086676,-84.2285673137265,
114.423580590046));
#46290=CARTESIAN_POINT('Ctrl Pts',(-32.9601522791593,-86.4928751310124,
114.265632066854));
#46291=CARTESIAN_POINT('Ctrl Pts',(-33.4309287026749,-89.9138036211001,
114.107683543661));
#46292=CARTESIAN_POINT('Ctrl Pts',(-36.5528046140307,-91.3897009648648,
113.949735020469));
#46293=CARTESIAN_POINT('Ctrl Pts',(-39.495270071964,-89.582415928103,113.791786497276));
#46294=CARTESIAN_POINT('Ctrl Pts',(-39.5904811368084,-86.1305588875572,
113.633837974084));
#46295=CARTESIAN_POINT('Ctrl Pts',(-36.7521128317831,-84.1638236384041,
113.475889450891));
#46296=CARTESIAN_POINT('Ctrl Pts',(-33.5536273739847,-85.4653892155019,
113.317940927699));
#46297=CARTESIAN_POINT('Ctrl Pts',(-32.8949942504612,-88.8551656954239,
113.159992404506));
#46298=CARTESIAN_POINT('Ctrl Pts',(-35.3733760828904,-91.2597458392159,
113.002043881314));
#46299=CARTESIAN_POINT('Ctrl Pts',(-38.7416994403848,-90.4989699625011,
112.844095358121));
#46300=CARTESIAN_POINT('Ctrl Pts',(-39.9460079776284,-87.2626104147444,
112.686146834929));
#46301=CARTESIAN_POINT('Ctrl Pts',(-37.8943917712909,-84.4849759684705,
112.528198311736));
#46302=CARTESIAN_POINT('Ctrl Pts',(-34.446988838572,-84.684463298183,112.370249788544));
#46303=CARTESIAN_POINT('Ctrl Pts',(-32.7294545705478,-87.6802033091648,
112.212301265352));
#46304=CARTESIAN_POINT('Ctrl Pts',(-34.299025051591,-90.7560496447713,112.054352742159));
#46305=CARTESIAN_POINT('Ctrl Pts',(-37.7326184628711,-91.1232259801486,
111.896404218966));
#46306=CARTESIAN_POINT('Ctrl Pts',(-39.9171000863972,-88.4488246991674,
111.738455695774));
#46307=CARTESIAN_POINT('Ctrl Pts',(-38.8718668721363,-85.1576441050679,
111.580507172582));
#46308=CARTESIAN_POINT('Ctrl Pts',(-35.5445999861014,-84.2336975457609,
111.422558649389));
#46309=CARTESIAN_POINT('Ctrl Pts',(-32.9520311196661,-86.5146992660596,
111.264610126197));
#46310=CARTESIAN_POINT('Ctrl Pts',(-33.444763614499,-89.9325343795896,111.106661603004));
#46311=CARTESIAN_POINT('Ctrl Pts',(-36.5760519035439,-91.3883557378978,
110.948713079812));
#46312=CARTESIAN_POINT('Ctrl Pts',(-39.5068521284844,-89.5622143917412,
110.790764556619));
#46313=CARTESIAN_POINT('Ctrl Pts',(-39.5798968625887,-86.1098171610682,
110.632816033427));
#46314=CARTESIAN_POINT('Ctrl Pts',(-36.7289586650204,-84.1613476130271,
110.474867510234));
#46315=CARTESIAN_POINT('Ctrl Pts',(-33.5388964962196,-85.4834238308911,
110.316918987042));
#46316=CARTESIAN_POINT('Ctrl Pts',(-32.9020426949109,-88.8773595086493,
110.158970463849));
#46317=CARTESIAN_POINT('Ctrl Pts',(-35.3958132509259,-91.2659764064493,
110.001021940657));
#46318=CARTESIAN_POINT('Ctrl Pts',(-38.7591822103186,-90.4835881940102,
109.843073417464));
#46319=CARTESIAN_POINT('Ctrl Pts',(-39.9426853026755,-87.23956254139,109.685124894272));
#46320=CARTESIAN_POINT('Ctrl Pts',(-37.8732761190034,-84.4751586948984,
109.52717637108));
#46321=CARTESIAN_POINT('Ctrl Pts',(-34.4272253359264,-84.6967778557991,
109.369227847887));
#46322=CARTESIAN_POINT('Ctrl Pts',(-32.728961758079,-87.7034840352579,109.211279324695));
#46323=CARTESIAN_POINT('Ctrl Pts',(-34.3182506239731,-90.7691894929664,
109.053330801502));
#46324=CARTESIAN_POINT('Ctrl Pts',(-37.754129375528,-91.1143096400617,108.89538227831));
#46325=CARTESIAN_POINT('Ctrl Pts',(-39.9213967567358,-88.425940066931,108.737433755117));
#46326=CARTESIAN_POINT('Ctrl Pts',(-38.8550460145749,-85.1415323265349,
108.579485231925));
#46327=CARTESIAN_POINT('Ctrl Pts',(-35.5219282427889,-84.238982422185,108.421536708732));
#46328=CARTESIAN_POINT('Ctrl Pts',(-32.9440320186257,-86.5365567862535,
108.26358818554));
#46329=CARTESIAN_POINT('Ctrl Pts',(-33.4587560273279,-89.9512135763613,
108.105639662347));
#46330=CARTESIAN_POINT('Ctrl Pts',(-36.5992129203138,-91.3867838191251,
107.947691139155));
#46331=CARTESIAN_POINT('Ctrl Pts',(-39.5184629122695,-89.5420981841802,
107.789742615962));
#46332=CARTESIAN_POINT('Ctrl Pts',(-39.5688532814934,-86.0888161846899,
107.63179409277));
#46333=CARTESIAN_POINT('Ctrl Pts',(-36.7064604496932,-84.1596939007676,
107.473845569577));
#46334=CARTESIAN_POINT('Ctrl Pts',(-33.5229009026989,-85.5001505522318,
107.315897046385));
#46335=CARTESIAN_POINT('Ctrl Pts',(-32.9121328624527,-88.9023373811549,
107.157948523192));
#46336=CARTESIAN_POINT('Ctrl Pts',(-34.5788882023795,-90.4751844899406,
107.052649507731));
#46337=CARTESIAN_POINT('Ctrl Pts',(-35.5611267921512,-90.7377785423181,
107.));
#46338=CARTESIAN_POINT('Ctrl Pts',(-34.4414600780185,-86.1325683851972,
122.));
#46339=CARTESIAN_POINT('Ctrl Pts',(-34.3798518775506,-86.1904649655976,
122.));
#46340=CARTESIAN_POINT('Ctrl Pts',(-34.3216128304826,-86.2515123055306,
122.));
#46341=CARTESIAN_POINT('Ctrl Pts',(-34.2667405503208,-86.3153255861301,
122.));
#46342=CARTESIAN_POINT('Ctrl Pts',(-34.2104153409142,-86.3808285392073,
122.));
#46343=CARTESIAN_POINT('Ctrl Pts',(-34.1576371151041,-86.4492462791581,
122.));
#46344=CARTESIAN_POINT('Ctrl Pts',(-34.1084287995683,-86.5202111532911,
122.));
#46345=CARTESIAN_POINT('Ctrl Pts',(-34.0578709059029,-86.5931222968921,
122.));
#46346=CARTESIAN_POINT('Ctrl Pts',(-34.0110808905349,-86.6687227614682,
122.));
#46347=CARTESIAN_POINT('Ctrl Pts',(-33.9681176865251,-86.7466567865213,
122.));
#46348=CARTESIAN_POINT('Ctrl Pts',(-33.9492077166618,-86.7809589317883,
122.));
#46349=CARTESIAN_POINT('Ctrl Pts',(-33.9310395849474,-86.8157136469207,
122.));
#46350=CARTESIAN_POINT('Ctrl Pts',(-33.9136207415204,-86.8508926744324,
122.));
#46351=CARTESIAN_POINT('Ctrl Pts',(-33.9036898968079,-86.8709489692613,
122.));
#46352=CARTESIAN_POINT('Ctrl Pts',(-33.8940026274005,-86.8911432023781,
122.));
#46353=CARTESIAN_POINT('Ctrl Pts',(-33.8845605482211,-86.9114702857301,
122.));
#46354=CARTESIAN_POINT('Ctrl Pts',(-33.8760549610638,-86.9297812716708,
122.));
#46355=CARTESIAN_POINT('Ctrl Pts',(-33.8677459643075,-86.9482057896219,
122.));
#46356=CARTESIAN_POINT('Ctrl Pts',(-33.8596483989529,-86.9667083655792,
122.));
#46357=CARTESIAN_POINT('Ctrl Pts',(-33.8230867710876,-87.0502500558377,
122.));
#46358=CARTESIAN_POINT('Ctrl Pts',(-33.7907853230142,-87.1354752893954,
122.));
#46359=CARTESIAN_POINT('Ctrl Pts',(-33.7627690901063,-87.2219852884617,
122.));
#46360=CARTESIAN_POINT('Ctrl Pts',(-33.7342897622732,-87.3099252564206,
122.));
#46361=CARTESIAN_POINT('Ctrl Pts',(-33.7102379922034,-87.399193569067,122.));
#46362=CARTESIAN_POINT('Ctrl Pts',(-33.6906791523764,-87.4894084695148,
122.));
#46363=CARTESIAN_POINT('Ctrl Pts',(-33.6717106761794,-87.5769003252127,
122.));
#46364=CARTESIAN_POINT('Ctrl Pts',(-33.6569678380238,-87.6652834048776,
122.));
#46365=CARTESIAN_POINT('Ctrl Pts',(-33.6465510103069,-87.754231352766,122.));
#46366=CARTESIAN_POINT('Ctrl Pts',(-33.6421821764996,-87.7915362609761,
122.));
#46367=CARTESIAN_POINT('Ctrl Pts',(-33.6385747935892,-87.8289407203117,
122.));
#46368=CARTESIAN_POINT('Ctrl Pts',(-33.6357386010791,-87.8664212731137,
122.));
#46369=CARTESIAN_POINT('Ctrl Pts',(-33.6339594736333,-87.8899326109151,
122.));
#46370=CARTESIAN_POINT('Ctrl Pts',(-33.632483836464,-87.9134738968258,122.));
#46371=CARTESIAN_POINT('Ctrl Pts',(-33.6313143896635,-87.937039373452,122.));
#46372=CARTESIAN_POINT('Ctrl Pts',(-33.6306300060648,-87.9508303605176,
122.));
#46373=CARTESIAN_POINT('Ctrl Pts',(-33.630050777169,-87.96462468597,122.));
#46374=CARTESIAN_POINT('Ctrl Pts',(-33.6295772037717,-87.9784133589186,
122.));
#46375=CARTESIAN_POINT('Ctrl Pts',(-33.6262498202146,-88.0752942308254,
122.));
#46376=CARTESIAN_POINT('Ctrl Pts',(-33.6281283514734,-88.1720100978643,
122.));
#46377=CARTESIAN_POINT('Ctrl Pts',(-33.6352771791366,-88.2681411935631,
122.));
#46378=CARTESIAN_POINT('Ctrl Pts',(-33.6424260067998,-88.3642722892619,
122.));
#46379=CARTESIAN_POINT('Ctrl Pts',(-33.6548447005543,-88.4598196576553,
122.));
#46380=CARTESIAN_POINT('Ctrl Pts',(-33.6726501049204,-88.5543823177475,
122.));
#46381=CARTESIAN_POINT('Ctrl Pts',(-33.6897081290363,-88.6449757186696,
122.));
#46382=CARTESIAN_POINT('Ctrl Pts',(-33.7117100089936,-88.7346663111608,
122.));
#46383=CARTESIAN_POINT('Ctrl Pts',(-33.7383811355958,-88.8232147557601,
122.));
#46384=CARTESIAN_POINT('Ctrl Pts',(-33.7472504814174,-88.8526610850746,
122.));
#46385=CARTESIAN_POINT('Ctrl Pts',(-33.7566366115083,-88.8819810727538,
122.));
#46386=CARTESIAN_POINT('Ctrl Pts',(-33.7665306757816,-88.9111657426682,
122.));
#46387=CARTESIAN_POINT('Ctrl Pts',(-33.7758509847573,-88.9386579979677,
122.));
#46388=CARTESIAN_POINT('Ctrl Pts',(-33.7856220321467,-88.9660301755988,
122.));
#46389=CARTESIAN_POINT('Ctrl Pts',(-33.795836894649,-88.9932746472985,122.));
#46390=CARTESIAN_POINT('Ctrl Pts',(-33.8009946724693,-89.0070311645134,
122.));
#46391=CARTESIAN_POINT('Ctrl Pts',(-33.8062625286193,-89.020746848332,122.));
#46392=CARTESIAN_POINT('Ctrl Pts',(-33.8116377932126,-89.0344173805264,
122.));
#46393=CARTESIAN_POINT('Ctrl Pts',(-33.8458891144019,-89.1215263555152,
122.));
#46394=CARTESIAN_POINT('Ctrl Pts',(-33.8845139350508,-89.2068465156693,
122.));
#46395=CARTESIAN_POINT('Ctrl Pts',(-33.9271822694107,-89.2901434462211,
122.));
#46396=CARTESIAN_POINT('Ctrl Pts',(-33.971412073536,-89.3764886710304,122.));
#46397=CARTESIAN_POINT('Ctrl Pts',(-34.0199868853076,-89.4606606049718,
122.));
#46398=CARTESIAN_POINT('Ctrl Pts',(-34.0725949938842,-89.5423946690003,
122.));
#46399=CARTESIAN_POINT('Ctrl Pts',(-34.125766055418,-89.6250033592851,122.));
#46400=CARTESIAN_POINT('Ctrl Pts',(-34.183057610295,-89.7051225474543,122.));
#46401=CARTESIAN_POINT('Ctrl Pts',(-34.2441993414934,-89.7824637049978,
122.));
#46402=CARTESIAN_POINT('Ctrl Pts',(-34.2668881997465,-89.8111639482889,
122.));
#46403=CARTESIAN_POINT('Ctrl Pts',(-34.2901077201578,-89.8394814287244,
122.));
#46404=CARTESIAN_POINT('Ctrl Pts',(-34.3138456838706,-89.8674005141729,
122.));
#46405=CARTESIAN_POINT('Ctrl Pts',(-34.3346009376308,-89.891811525591,122.));
#46406=CARTESIAN_POINT('Ctrl Pts',(-34.3557525477729,-89.91591796448,122.));
#46407=CARTESIAN_POINT('Ctrl Pts',(-34.3772928365918,-89.9397089990812,
122.));
#46408=CARTESIAN_POINT('Ctrl Pts',(-34.3890563049912,-89.9527016328417,
122.));
#46409=CARTESIAN_POINT('Ctrl Pts',(-34.4009310177164,-89.9655949494855,
122.));
#46410=CARTESIAN_POINT('Ctrl Pts',(-34.4129096494478,-89.9783813265245,
122.));
#46411=CARTESIAN_POINT('Ctrl Pts',(-34.4819204330028,-90.0520456579833,
122.));
#46412=CARTESIAN_POINT('Ctrl Pts',(-34.5544336142438,-90.1222254583658,
122.));
#46413=CARTESIAN_POINT('Ctrl Pts',(-34.6301406718656,-90.1886295132617,
122.));
#46414=CARTESIAN_POINT('Ctrl Pts',(-34.6923348072412,-90.243181135124,122.));
#46415=CARTESIAN_POINT('Ctrl Pts',(-34.7566855153176,-90.2951845232665,
122.));
#46416=CARTESIAN_POINT('Ctrl Pts',(-34.8230440286038,-90.344464887705,122.));
#46417=CARTESIAN_POINT('Ctrl Pts',(-34.847661598239,-90.3627468344084,122.));
#46418=CARTESIAN_POINT('Ctrl Pts',(-34.8725556727621,-90.3806538796401,
122.));
#46419=CARTESIAN_POINT('Ctrl Pts',(-34.8977192636688,-90.3981765345118,
122.));
#46420=CARTESIAN_POINT('Ctrl Pts',(-34.9145301473448,-90.4098827855725,
122.));
#46421=CARTESIAN_POINT('Ctrl Pts',(-34.9314624553121,-90.4214181097377,
122.));
#46422=CARTESIAN_POINT('Ctrl Pts',(-34.9484990431383,-90.4327698544389,
122.));
#46423=CARTESIAN_POINT('Ctrl Pts',(-35.0334095222549,-90.4893470335797,
122.));
#46424=CARTESIAN_POINT('Ctrl Pts',(-35.1209892792786,-90.5414249135277,
122.));
#46425=CARTESIAN_POINT('Ctrl Pts',(-35.2109479563236,-90.5886955781829,
122.));
#46426=CARTESIAN_POINT('Ctrl Pts',(-35.2944060034241,-90.6325503511392,
122.));
#46427=CARTESIAN_POINT('Ctrl Pts',(-35.3799123921453,-90.6722678394425,
122.));
#46428=CARTESIAN_POINT('Ctrl Pts',(-35.4672629815674,-90.7075731181594,
122.));
#46429=CARTESIAN_POINT('Ctrl Pts',(-35.4976931583414,-90.7198723582621,
122.));
#46430=CARTESIAN_POINT('Ctrl Pts',(-35.5283473555972,-90.7316358396728,
122.));
#46431=CARTESIAN_POINT('Ctrl Pts',(-35.5592126670537,-90.7428672848631,
122.));
#46432=CARTESIAN_POINT('Ctrl Pts',(-38.873093130194,-87.7707538189189,120.387416697508));
#46433=CARTESIAN_POINT('Ctrl Pts',(-38.8746754899396,-87.9451202416974,
120.398449387697));
#46434=CARTESIAN_POINT('Ctrl Pts',(-38.8580898958553,-88.1191876191089,
120.409482077886));
#46435=CARTESIAN_POINT('Ctrl Pts',(-38.8222183368412,-88.2891852552992,
120.420514768075));
#46436=CARTESIAN_POINT('Ctrl Pts',(-38.6510343471469,-89.1004372443804,
120.473164275806));
#46437=CARTESIAN_POINT('Ctrl Pts',(-38.0406454775365,-89.819007834794,120.525813783537));
#46438=CARTESIAN_POINT('Ctrl Pts',(-37.2677605679595,-90.1191530964584,
120.578463291268));
#46439=CARTESIAN_POINT('Ctrl Pts',(-36.4948756583824,-90.4192983581227,
120.631112798999));
#46440=CARTESIAN_POINT('Ctrl Pts',(-35.5594947088388,-90.3010182910378,
120.683762306729));
#46441=CARTESIAN_POINT('Ctrl Pts',(-34.8856618873309,-89.8179146088604,
120.73641181446));
#46442=CARTESIAN_POINT('Ctrl Pts',(-34.2118290658229,-89.3348109266829,
120.789061322191));
#46443=CARTESIAN_POINT('Ctrl Pts',(-33.7995443723506,-88.4868836294129,
120.841710829922));
#46444=CARTESIAN_POINT('Ctrl Pts',(-33.8357037311416,-87.6585662369633,
120.894360337653));
#46445=CARTESIAN_POINT('Ctrl Pts',(-33.8718630899327,-86.8302488445136,
120.947009845384));
#46446=CARTESIAN_POINT('Ctrl Pts',(-34.3564665009871,-86.0215413568844,
120.999659353114));
#46447=CARTESIAN_POINT('Ctrl Pts',(-35.0698409216864,-85.5989796841795,
121.052308860845));
#46448=CARTESIAN_POINT('Ctrl Pts',(-35.7832153423856,-85.1764180114746,
121.104958368576));
#46449=CARTESIAN_POINT('Ctrl Pts',(-36.7253607727297,-85.1400021536939,
121.157607876307));
#46450=CARTESIAN_POINT('Ctrl Pts',(-37.4691400009799,-85.506403846918,121.210257384038));
#46451=CARTESIAN_POINT('Ctrl Pts',(-38.2129192292301,-85.8728055401422,
121.262906891769));
#46452=CARTESIAN_POINT('Ctrl Pts',(-38.7583322553865,-86.642024784371,121.315556399499));
#46453=CARTESIAN_POINT('Ctrl Pts',(-38.8581859196339,-87.4650121706535,
121.36820590723));
#46454=CARTESIAN_POINT('Ctrl Pts',(-38.870330811929,-87.5651095806176,121.374609503989));
#46455=CARTESIAN_POINT('Ctrl Pts',(-38.8758844980629,-87.6660023883209,
121.381013100749));
#46456=CARTESIAN_POINT('Ctrl Pts',(-38.8751287300693,-87.7669767062971,
121.387416697508));
#46457=CARTESIAN_POINT('Ctrl Pts',(-37.1487253572165,-90.7377785423179,
122.));
#46458=CARTESIAN_POINT('Ctrl Pts',(-38.1309639469881,-90.4751844899402,
121.947350492269));
#46459=CARTESIAN_POINT('Ctrl Pts',(-39.7977192277978,-88.9023369720511,
121.842051476808));
#46460=CARTESIAN_POINT('Ctrl Pts',(-39.1869512976859,-85.5001506582564,
121.684102953615));
#46461=CARTESIAN_POINT('Ctrl Pts',(-36.0033916957587,-84.1596937777799,
121.526154430423));
#46462=CARTESIAN_POINT('Ctrl Pts',(-33.1409988246472,-86.0888162082167,
121.36820590723));
#46463=CARTESIAN_POINT('Ctrl Pts',(-33.1913892046506,-89.5420981815712,
121.210257384038));
#46464=CARTESIAN_POINT('Ctrl Pts',(-36.1106392225623,-91.3867838745725,
121.052308860845));
#46465=CARTESIAN_POINT('Ctrl Pts',(-39.2510961586208,-89.9512135954417,
120.894360337653));
#46466=CARTESIAN_POINT('Ctrl Pts',(-39.7658201696681,-86.5365567752375,
120.73641181446));
#46467=CARTESIAN_POINT('Ctrl Pts',(-37.1879239172525,-84.2389823785756,
120.578463291268));
#46468=CARTESIAN_POINT('Ctrl Pts',(-33.8548061047563,-85.1415322964398,
120.420514768075));
#46469=CARTESIAN_POINT('Ctrl Pts',(-32.7884553507106,-88.4259400742007,
120.262566244883));
#46470=CARTESIAN_POINT('Ctrl Pts',(-34.9557227571499,-91.1143096798933,
120.10461772169));
#46471=CARTESIAN_POINT('Ctrl Pts',(-38.3916015495585,-90.769189528319,119.946669198498));
#46472=CARTESIAN_POINT('Ctrl Pts',(-39.9808904341307,-87.7034840345569,
119.788720675305));
#46473=CARTESIAN_POINT('Ctrl Pts',(-38.2826268362602,-84.6967778194338,
119.630772152113));
#46474=CARTESIAN_POINT('Ctrl Pts',(-34.8365760123942,-84.4751586559665,
119.472823628921));
#46475=CARTESIAN_POINT('Ctrl Pts',(-32.7671668042656,-87.2395625351253,
119.314875105728));
#46476=CARTESIAN_POINT('Ctrl Pts',(-33.9506699106112,-90.4835882261257,
119.156926582536));
#46477=CARTESIAN_POINT('Ctrl Pts',(-37.3140389097867,-91.26597644781,118.998978059343));
#46478=CARTESIAN_POINT('Ctrl Pts',(-39.8078094952921,-88.8773595217634,
118.841029536151));
#46479=CARTESIAN_POINT('Ctrl Pts',(-39.170955686452,-85.483423803864,118.683081012958));
#46480=CARTESIAN_POINT('Ctrl Pts',(-35.980893479922,-84.1613475703659,118.525132489766));
#46481=CARTESIAN_POINT('Ctrl Pts',(-33.1299552486368,-86.109817141451,118.367183966573));
#46482=CARTESIAN_POINT('Ctrl Pts',(-33.2029999836058,-89.5622144129554,
118.209235443381));
#46483=CARTESIAN_POINT('Ctrl Pts',(-36.1338002432087,-91.3883557807084,
118.051286920188));
#46484=CARTESIAN_POINT('Ctrl Pts',(-39.2650885692864,-89.932534405182,117.893338396996));
#46485=CARTESIAN_POINT('Ctrl Pts',(-39.7578210699461,-86.5146992512298,
117.735389873803));
#46486=CARTESIAN_POINT('Ctrl Pts',(-37.1652521728484,-84.2336975039545,
117.577441350611));
#46487=CARTESIAN_POINT('Ctrl Pts',(-33.8379852474627,-85.1576440741897,
117.419492827418));
#46488=CARTESIAN_POINT('Ctrl Pts',(-32.7927520208408,-88.4488247072137,
117.261544304226));
#46489=CARTESIAN_POINT('Ctrl Pts',(-34.9772336702029,-91.123226019824,117.103595781034));
#46490=CARTESIAN_POINT('Ctrl Pts',(-38.4108271220914,-90.7560496801034,
116.945647257841));
#46491=CARTESIAN_POINT('Ctrl Pts',(-39.980397621697,-87.680203308119,116.787698734649));
#46492=CARTESIAN_POINT('Ctrl Pts',(-38.2628633333592,-84.6844632617075,
116.629750211456));
#46493=CARTESIAN_POINT('Ctrl Pts',(-34.8154603598683,-84.4849759296366,
116.471801688264));
#46494=CARTESIAN_POINT('Ctrl Pts',(-32.7638441292674,-87.2626104087614,
116.313853165071));
#46495=CARTESIAN_POINT('Ctrl Pts',(-33.9681526807548,-90.4989699947938,
116.155904641879));
#46496=CARTESIAN_POINT('Ctrl Pts',(-37.336476078086,-91.2597458805054,115.997956118686));
#46497=CARTESIAN_POINT('Ctrl Pts',(-39.8148579398261,-88.8551657082742,
115.840007595494));
#46498=CARTESIAN_POINT('Ctrl Pts',(-39.1562248085122,-85.4653891882622,
115.682059072301));
#46499=CARTESIAN_POINT('Ctrl Pts',(-35.9577393128856,-84.1638235957717,
115.524110549109));
#46500=CARTESIAN_POINT('Ctrl Pts',(-33.1193709742919,-86.1305588681857,
115.366162025916));
#46501=CARTESIAN_POINT('Ctrl Pts',(-33.2145820402631,-89.5824159495559,
115.208213502724));
#46502=CARTESIAN_POINT('Ctrl Pts',(-36.1570475329969,-91.3897010076914,
115.050264979531));
#46503=CARTESIAN_POINT('Ctrl Pts',(-39.2789234812742,-89.9138036464711,
114.892316456339));
#46504=CARTESIAN_POINT('Ctrl Pts',(-39.7496999103568,-86.4928751159242,
114.734367933147));
#46505=CARTESIAN_POINT('Ctrl Pts',(-37.1425381500136,-84.2285672718597,
114.576419409954));
#46506=CARTESIAN_POINT('Ctrl Pts',(-33.821272475107,-85.1738591706804,114.418470886761));
#46507=CARTESIAN_POINT('Ctrl Pts',(-32.7971934613455,-88.4716833974796,
114.260522363569));
#46508=CARTESIAN_POINT('Ctrl Pts',(-34.9988024045514,-91.1320030246078,
114.102573840377));
#46509=CARTESIAN_POINT('Ctrl Pts',(-38.4299674348291,-90.7427871561125,
113.944625317184));
#46510=CARTESIAN_POINT('Ctrl Pts',(-39.9797555733929,-87.6569259824923,
113.786676793992));
#46511=CARTESIAN_POINT('Ctrl Pts',(-38.2430210496827,-84.672275977644,113.628728270799));
#46512=CARTESIAN_POINT('Ctrl Pts',(-34.7944082359535,-84.4949285269366,
113.470779747607));
#46513=CARTESIAN_POINT('Ctrl Pts',(-32.7606694855963,-87.2856791701479,
113.312831224414));
#46514=CARTESIAN_POINT('Ctrl Pts',(-33.9857338701916,-90.514239175922,113.154882701222));
#46515=CARTESIAN_POINT('Ctrl Pts',(-37.3588727708761,-91.2533713792378,
112.996934178029));
#46516=CARTESIAN_POINT('Ctrl Pts',(-39.8217637357813,-88.8329270910382,
112.838985654837));
#46517=CARTESIAN_POINT('Ctrl Pts',(-39.1413784324703,-85.4474495329488,
112.681037131644));
#46518=CARTESIAN_POINT('Ctrl Pts',(-35.9346015224717,-84.1664482422435,
112.523088608452));
#46519=CARTESIAN_POINT('Ctrl Pts',(-33.1089201003701,-86.1513681293118,
112.365140085259));
#46520=CARTESIAN_POINT('Ctrl Pts',(-33.2262935723694,-89.6025427011582,
112.207191562067));
#46521=CARTESIAN_POINT('Ctrl Pts',(-36.1803029811607,-91.3908969362198,
112.049243038874));
#46522=CARTESIAN_POINT('Ctrl Pts',(-39.2926378379277,-89.8949844399009,
111.891294515682));
#46523=CARTESIAN_POINT('Ctrl Pts',(-39.7414387854258,-86.4711035764935,
111.733345992489));
#46524=CARTESIAN_POINT('Ctrl Pts',(-37.1197916542217,-84.2235829922162,
111.575397469297));
#46525=CARTESIAN_POINT('Ctrl Pts',(-33.8046641643864,-85.1901812455926,
111.417448946105));
#46526=CARTESIAN_POINT('Ctrl Pts',(-32.8017815859054,-88.494513098026,111.259500422912));
#46527=CARTESIAN_POINT('Ctrl Pts',(-35.0204270513993,-91.1406413556617,
111.10155189972));
#46528=CARTESIAN_POINT('Ctrl Pts',(-38.4490221943426,-90.7294020055796,
110.943603376527));
#46529=CARTESIAN_POINT('Ctrl Pts',(-39.9789640746645,-87.6336532593737,
110.785654853335));
#46530=CARTESIAN_POINT('Ctrl Pts',(-38.2231009204979,-84.66021635197,110.627706330142));
#46531=CARTESIAN_POINT('Ctrl Pts',(-34.7734204516813,-84.5050160949677,
110.46975780695));
#46532=CARTESIAN_POINT('Ctrl Pts',(-32.7576430317562,-87.3087678398475,
110.311809283757));
#46533=CARTESIAN_POINT('Ctrl Pts',(-34.0034127407753,-90.5293951545392,
110.153860760565));
#46534=CARTESIAN_POINT('Ctrl Pts',(-37.381228070904,-91.2468531980925,109.995912237372));
#46535=CARTESIAN_POINT('Ctrl Pts',(-39.8285265960631,-88.8106445945815,
109.83796371418));
#46536=CARTESIAN_POINT('Ctrl Pts',(-39.1264171703115,-85.429605566886,109.680015190987));
#46537=CARTESIAN_POINT('Ctrl Pts',(-35.9114810653333,-84.1692214210988,
109.522066667795));
#46538=CARTESIAN_POINT('Ctrl Pts',(-33.098603051042,-86.1722440278901,109.364118144602));
#46539=CARTESIAN_POINT('Ctrl Pts',(-33.2381341114487,-89.6225939175359,
109.20616962141));
#46540=CARTESIAN_POINT('Ctrl Pts',(-36.2035655990193,-91.3919433535738,
109.048221098218));
#46541=CARTESIAN_POINT('Ctrl Pts',(-39.3062311353703,-89.8760778973243,
108.890272575025));
#46542=CARTESIAN_POINT('Ctrl Pts',(-39.7330379090806,-86.4493848397213,
108.732324051833));
#46543=CARTESIAN_POINT('Ctrl Pts',(-37.0970138838616,-84.2187462913202,
108.57437552864));
#46544=CARTESIAN_POINT('Ctrl Pts',(-33.7881604641648,-85.2066067039222,
108.416427005448));
#46545=CARTESIAN_POINT('Ctrl Pts',(-32.8065173074963,-88.517318877192,108.258478482255));
#46546=CARTESIAN_POINT('Ctrl Pts',(-35.0421044524555,-91.1491282972506,
108.100529959063));
#46547=CARTESIAN_POINT('Ctrl Pts',(-38.4679952768287,-90.7159201995772,
107.94258143587));
#46548=CARTESIAN_POINT('Ctrl Pts',(-39.9780135704577,-87.6103338201277,
107.784632912678));
#46549=CARTESIAN_POINT('Ctrl Pts',(-38.2031234854001,-84.6483923994501,
107.626684389485));
#46550=CARTESIAN_POINT('Ctrl Pts',(-34.7524573177229,-84.5150170933021,
107.468735866293));
#46551=CARTESIAN_POINT('Ctrl Pts',(-32.7548482639927,-87.3323302896557,
107.3107873431));
#46552=CARTESIAN_POINT('Ctrl Pts',(-34.0210167874952,-90.5435019715025,
107.152838819908));
#46553=CARTESIAN_POINT('Ctrl Pts',(-37.403884869873,-91.2421291429392,106.994890296715));
#46554=CARTESIAN_POINT('Ctrl Pts',(-39.8343594515415,-88.7843450828379,
106.836941773523));
#46555=CARTESIAN_POINT('Ctrl Pts',(-39.3517092963752,-86.544039008134,106.731642758061));
#46556=CARTESIAN_POINT('Ctrl Pts',(-38.6909887323791,-85.7712540316409,
106.678993250331));
#46557=CARTESIAN_POINT('Ctrl Pts',(-37.1008589290305,-90.5587331584144,
122.10700224989));
#46558=CARTESIAN_POINT('Ctrl Pts',(-38.0238681217073,-90.3119736370407,
122.054352742159));
#46559=CARTESIAN_POINT('Ctrl Pts',(-39.5901173631341,-88.8339694812193,
121.949053726697));
#46560=CARTESIAN_POINT('Ctrl Pts',(-39.0161789942328,-85.6369364227221,
121.791105203505));
#46561=CARTESIAN_POINT('Ctrl Pts',(-36.0245893655903,-84.3773096518432,
121.633156680312));
#46562=CARTESIAN_POINT('Ctrl Pts',(-33.3347999797929,-86.1901051942237,
121.47520815712));
#46563=CARTESIAN_POINT('Ctrl Pts',(-33.3821517988416,-89.4351528226744,
121.317259633928));
#46564=CARTESIAN_POINT('Ctrl Pts',(-36.1253698217467,-91.1686031981433,
121.159311110735));
#46565=CARTESIAN_POINT('Ctrl Pts',(-39.0764558932698,-89.8195984062634,
121.001362587543));
#46566=CARTESIAN_POINT('Ctrl Pts',(-39.5601418315291,-86.6108468181,120.84341406435));
#46567=CARTESIAN_POINT('Ctrl Pts',(-37.1376937995291,-84.4518171169042,
120.685465541158));
#46568=CARTESIAN_POINT('Ctrl Pts',(-34.0055643828626,-85.2999428978633,
120.527517017965));
#46569=CARTESIAN_POINT('Ctrl Pts',(-33.0035150245384,-88.3862995152278,
120.369568494773));
#46570=CARTESIAN_POINT('Ctrl Pts',(-35.0400953014315,-90.9125593111742,
120.21161997158));
#46571=CARTESIAN_POINT('Ctrl Pts',(-38.2687891680141,-90.588250048844,120.053671448388));
#46572=CARTESIAN_POINT('Ctrl Pts',(-39.7622432692423,-87.7074078764345,
119.895722925195));
#46573=CARTESIAN_POINT('Ctrl Pts',(-38.1663856754298,-84.882007301527,119.737774402003));
#46574=CARTESIAN_POINT('Ctrl Pts',(-34.928133155134,-84.6737518661535,119.57982587881));
#46575=CARTESIAN_POINT('Ctrl Pts',(-32.983510186333,-87.271461037128,119.421877355618));
#46576=CARTESIAN_POINT('Ctrl Pts',(-34.0956475611968,-90.3198706244251,
119.263928832425));
#46577=CARTESIAN_POINT('Ctrl Pts',(-37.2562040053545,-91.0550805096574,
119.105980309233));
#46578=CARTESIAN_POINT('Ctrl Pts',(-39.5995991832854,-88.8104981816133,
118.94803178604));
#46579=CARTESIAN_POINT('Ctrl Pts',(-39.0011479250352,-85.6212182046338,
118.790083262848));
#46580=CARTESIAN_POINT('Ctrl Pts',(-36.0034478015626,-84.3788637200456,
118.632134739656));
#46581=CARTESIAN_POINT('Ctrl Pts',(-33.3244223360271,-86.2098397624152,
118.474186216463));
#46582=CARTESIAN_POINT('Ctrl Pts',(-33.3930624429777,-89.4540560369066,
118.316237693271));
#46583=CARTESIAN_POINT('Ctrl Pts',(-36.1471342231772,-91.1700803176829,
118.158289170078));
#46584=CARTESIAN_POINT('Ctrl Pts',(-39.0896045557298,-89.8020455789757,
118.000340646886));
#46585=CARTESIAN_POINT('Ctrl Pts',(-39.5526250808602,-86.5903073119166,
117.842392123693));
#46586=CARTESIAN_POINT('Ctrl Pts',(-37.1163891707791,-84.4468509224294,
117.684443600501));
#46587=CARTESIAN_POINT('Ctrl Pts',(-33.9897578302874,-85.3150831286874,
117.526495077308));
#46588=CARTESIAN_POINT('Ctrl Pts',(-33.0075526036656,-88.4078041953146,
117.368546554116));
#46589=CARTESIAN_POINT('Ctrl Pts',(-35.0603090974456,-90.920937992084,117.210598030923));
#46590=CARTESIAN_POINT('Ctrl Pts',(-38.2868554304956,-90.5759025389624,
117.052649507731));
#46591=CARTESIAN_POINT('Ctrl Pts',(-39.7617801736042,-87.6855309875216,
116.894700984538));
#46592=CARTESIAN_POINT('Ctrl Pts',(-38.1478139200059,-84.8704353167736,
116.736752461346));
#46593=CARTESIAN_POINT('Ctrl Pts',(-34.9082907852723,-84.6829771541221,
116.578803938153));
#46594=CARTESIAN_POINT('Ctrl Pts',(-32.9803878700246,-87.2931191143603,
116.420855414961));
#46595=CARTESIAN_POINT('Ctrl Pts',(-34.1120761130008,-90.33432486602,116.262906891769));
#46596=CARTESIAN_POINT('Ctrl Pts',(-37.2772882030368,-91.0492256481627,
116.104958368576));
#46597=CARTESIAN_POINT('Ctrl Pts',(-39.6062226036708,-88.7896426643444,
115.947009845384));
#46598=CARTESIAN_POINT('Ctrl Pts',(-38.9873053251861,-85.6042710838831,
115.789061322191));
#46599=CARTESIAN_POINT('Ctrl Pts',(-35.9816898404665,-84.3811904400857,
115.631112798999));
#46600=CARTESIAN_POINT('Ctrl Pts',(-33.3144762978446,-86.229330754367,115.473164275806));
#46601=CARTESIAN_POINT('Ctrl Pts',(-33.4039460967826,-89.4730394124151,
115.315215752614));
#46602=CARTESIAN_POINT('Ctrl Pts',(-36.1689796916844,-91.171344426917,115.157267229421));
#46603=CARTESIAN_POINT('Ctrl Pts',(-39.1026052167479,-89.784444292836,114.999318706229));
#46604=CARTESIAN_POINT('Ctrl Pts',(-39.5449936305852,-86.5697991810826,
114.841370183036));
#46605=CARTESIAN_POINT('Ctrl Pts',(-37.0950448130054,-84.4420300454719,
114.683421659844));
#46606=CARTESIAN_POINT('Ctrl Pts',(-33.974052845083,-85.3303204480892,114.525473136651));
#46607=CARTESIAN_POINT('Ctrl Pts',(-33.0117262234534,-88.4292844970128,
114.367524613459));
#46608=CARTESIAN_POINT('Ctrl Pts',(-35.0805772281069,-90.9291857398147,
114.209576090266));
#46609=CARTESIAN_POINT('Ctrl Pts',(-38.3048415743832,-90.5634397507058,
114.051627567074));
#46610=CARTESIAN_POINT('Ctrl Pts',(-39.761176841081,-87.6636572943497,113.893679043881));
#46611=CARTESIAN_POINT('Ctrl Pts',(-38.1291681343202,-84.8589829310279,
113.735730520689));
#46612=CARTESIAN_POINT('Ctrl Pts',(-34.8885081132199,-84.6923296056491,
113.577781997496));
#46613=CARTESIAN_POINT('Ctrl Pts',(-32.9774046586924,-87.314796819803,113.419833474304));
#46614=CARTESIAN_POINT('Ctrl Pts',(-34.1285971493736,-90.3486733091506,
113.261884951111));
#46615=CARTESIAN_POINT('Ctrl Pts',(-37.2983343658999,-91.0432355319833,
113.103936427919));
#46616=CARTESIAN_POINT('Ctrl Pts',(-39.6127119772464,-88.7687450450135,
112.945987904727));
#46617=CARTESIAN_POINT('Ctrl Pts',(-38.9733541918185,-85.5874131972758,
112.788039381534));
#46618=CARTESIAN_POINT('Ctrl Pts',(-35.9599472684757,-84.3836568192793,
112.630090858342));
#46619=CARTESIAN_POINT('Ctrl Pts',(-33.3046556159841,-86.2488852083584,
112.472142335149));
#46620=CARTESIAN_POINT('Ctrl Pts',(-33.4149514186127,-89.4919525124918,
112.314193811957));
#46621=CARTESIAN_POINT('Ctrl Pts',(-36.1908328266136,-91.1724682404558,
112.156245288764));
#46622=CARTESIAN_POINT('Ctrl Pts',(-39.1154925919688,-89.7667598922799,
111.998296765572));
#46623=CARTESIAN_POINT('Ctrl Pts',(-39.537230654937,-86.5493404745703,111.840348242379));
#46624=CARTESIAN_POINT('Ctrl Pts',(-37.0736699404075,-84.437346319972,111.682399719187));
#46625=CARTESIAN_POINT('Ctrl Pts',(-33.9584460224337,-85.345658295069,111.524451195995));
#46626=CARTESIAN_POINT('Ctrl Pts',(-33.0160376821866,-88.450737557084,111.366502672802));
#46627=CARTESIAN_POINT('Ctrl Pts',(-35.1008978997205,-90.937303175899,111.20855414961));
#46628=CARTESIAN_POINT('Ctrl Pts',(-38.3227473239418,-90.550861730339,111.050605626417));
#46629=CARTESIAN_POINT('Ctrl Pts',(-39.7604330700564,-87.6417879261526,
110.892657103225));
#46630=CARTESIAN_POINT('Ctrl Pts',(-38.1104491972429,-84.8476505058174,
110.734708580032));
#46631=CARTESIAN_POINT('Ctrl Pts',(-34.8687859011027,-84.701808889116,110.57676005684));
#46632=CARTESIAN_POINT('Ctrl Pts',(-32.9745607012825,-87.336493233079,110.418811533647));
#46633=CARTESIAN_POINT('Ctrl Pts',(-34.1452099766793,-90.3629153759288,
110.260863010455));
#46634=CARTESIAN_POINT('Ctrl Pts',(-37.3193416320017,-91.0371103998827,
110.102914487262));
#46635=CARTESIAN_POINT('Ctrl Pts',(-39.6190670342295,-88.7478061923971,
109.94496596407));
#46636=CARTESIAN_POINT('Ctrl Pts',(-38.959295100015,-85.5706452298173,109.787017440877));
#46637=CARTESIAN_POINT('Ctrl Pts',(-35.9382209845566,-84.3862627742917,
109.629068917685));
#46638=CARTESIAN_POINT('Ctrl Pts',(-33.2949606890383,-86.2685022815357,
109.471120394492));
#46639=CARTESIAN_POINT('Ctrl Pts',(-33.4260779682415,-89.5107946321496,
109.3131718713));
#46640=CARTESIAN_POINT('Ctrl Pts',(-36.2126926989021,-91.1734515584065,
109.155223348107));
#46641=CARTESIAN_POINT('Ctrl Pts',(-39.1282662078998,-89.748993422115,108.997274824915));
#46642=CARTESIAN_POINT('Ctrl Pts',(-39.5293363549431,-86.5289313866941,
108.839326301722));
#46643=CARTESIAN_POINT('Ctrl Pts',(-37.052265679111,-84.4328012741596,108.68137777853));
#46644=CARTESIAN_POINT('Ctrl Pts',(-33.9429375022266,-85.3610932914029,
108.523429255338));
#46645=CARTESIAN_POINT('Ctrl Pts',(-33.0204878377882,-88.4721681382437,
108.365480732145));
#46646=CARTESIAN_POINT('Ctrl Pts',(-35.1212681444417,-90.9452783513664,
108.207532208953));
#46647=CARTESIAN_POINT('Ctrl Pts',(-38.3405763216318,-90.5381928828679,
108.04958368576));
#46648=CARTESIAN_POINT('Ctrl Pts',(-39.7595398816501,-87.6198746588301,
107.891635162568));
#46649=CARTESIAN_POINT('Ctrl Pts',(-38.0916764098229,-84.8365395425716,
107.733686639375));
#46650=CARTESIAN_POINT('Ctrl Pts',(-34.849086852875,-84.711206823075,107.575738116183));
#46651=CARTESIAN_POINT('Ctrl Pts',(-32.9719344591821,-87.3586348573252,
107.41778959299));
#46652=CARTESIAN_POINT('Ctrl Pts',(-34.1617524920315,-90.376171545939,107.259841069798));
#46653=CARTESIAN_POINT('Ctrl Pts',(-37.3406322165325,-91.0326712072276,
107.101892546605));
#46654=CARTESIAN_POINT('Ctrl Pts',(-39.624548166087,-88.723092552193,106.943944023413));
#46655=CARTESIAN_POINT('Ctrl Pts',(-39.1710020168068,-86.6178778692287,
106.838645007951));
#46656=CARTESIAN_POINT('Ctrl Pts',(-38.5501231787021,-85.8916921494929,
106.78599550022));
#46657=CARTESIAN_POINT('Ctrl Pts',(-37.0529925008446,-90.3796877745108,
122.21400449978));
#46658=CARTESIAN_POINT('Ctrl Pts',(-37.9167722964266,-90.1487627841411,
122.161354992049));
#46659=CARTESIAN_POINT('Ctrl Pts',(-39.3825154984704,-88.7656019903875,
122.056055976587));
#46660=CARTESIAN_POINT('Ctrl Pts',(-38.8454066907797,-85.7737221871878,
121.898107453395));
#46661=CARTESIAN_POINT('Ctrl Pts',(-36.0457870354219,-84.5949255259064,
121.740158930202));
#46662=CARTESIAN_POINT('Ctrl Pts',(-33.5286011349385,-86.2913941802307,
121.58221040701));
#46663=CARTESIAN_POINT('Ctrl Pts',(-33.5729143930326,-89.3282074637777,
121.424261883817));
#46664=CARTESIAN_POINT('Ctrl Pts',(-36.140100420931,-90.950422521714,121.266313360625));
#46665=CARTESIAN_POINT('Ctrl Pts',(-38.9018156279188,-89.6879832170849,
121.108364837432));
#46666=CARTESIAN_POINT('Ctrl Pts',(-39.35446349339,-86.6851368609626,120.95041631424));
#46667=CARTESIAN_POINT('Ctrl Pts',(-37.0874636818057,-84.6646518552326,
120.792467791047));
#46668=CARTESIAN_POINT('Ctrl Pts',(-34.156322660969,-85.4583534992869,120.634519267855));
#46669=CARTESIAN_POINT('Ctrl Pts',(-33.2185746983661,-88.346658956255,120.476570744663));
#46670=CARTESIAN_POINT('Ctrl Pts',(-35.1244678457132,-90.7108089424551,
120.31862222147));
#46671=CARTESIAN_POINT('Ctrl Pts',(-38.1459767864696,-90.407310569369,120.160673698278));
#46672=CARTESIAN_POINT('Ctrl Pts',(-39.5435961043541,-87.7113317183121,
120.002725175085));
#46673=CARTESIAN_POINT('Ctrl Pts',(-38.0501445145994,-85.0672367836203,
119.844776651893));
#46674=CARTESIAN_POINT('Ctrl Pts',(-35.0196902978739,-84.8723450763404,
119.6868281287));
#46675=CARTESIAN_POINT('Ctrl Pts',(-33.1998535684004,-87.3033595391308,
119.528879605508));
#46676=CARTESIAN_POINT('Ctrl Pts',(-34.2406252117824,-90.1561530227245,
119.370931082315));
#46677=CARTESIAN_POINT('Ctrl Pts',(-37.1983691009222,-90.8441845715049,
119.212982559123));
#46678=CARTESIAN_POINT('Ctrl Pts',(-39.3913888712786,-88.7436368414631,
119.05503403593));
#46679=CARTESIAN_POINT('Ctrl Pts',(-38.8313401636184,-85.7590126054036,
118.897085512738));
#46680=CARTESIAN_POINT('Ctrl Pts',(-36.0260021232032,-84.5963798697255,
118.739136989545));
#46681=CARTESIAN_POINT('Ctrl Pts',(-33.5188894234174,-86.3098623833792,
118.581188466353));
#46682=CARTESIAN_POINT('Ctrl Pts',(-33.5831249023497,-89.345897660858,118.42323994316));
#46683=CARTESIAN_POINT('Ctrl Pts',(-36.1604682031458,-90.9518048546572,
118.265291419968));
#46684=CARTESIAN_POINT('Ctrl Pts',(-38.9141205421731,-89.6715567527695,
118.107342896775));
#46685=CARTESIAN_POINT('Ctrl Pts',(-39.3474290917744,-86.6659153726033,
117.949394373583));
#46686=CARTESIAN_POINT('Ctrl Pts',(-37.0675261687099,-84.6600043409043,
117.791445850391));
#46687=CARTESIAN_POINT('Ctrl Pts',(-34.141530413112,-85.4725221831851,117.633497327198));
#46688=CARTESIAN_POINT('Ctrl Pts',(-33.2223531864905,-88.3667836834157,
117.475548804005));
#46689=CARTESIAN_POINT('Ctrl Pts',(-35.1433845246883,-90.7186499643442,
117.317600280813));
#46690=CARTESIAN_POINT('Ctrl Pts',(-38.1628837388999,-90.3957553978212,
117.159651757621));
#46691=CARTESIAN_POINT('Ctrl Pts',(-39.5431627255114,-87.6908586669244,
117.001703234428));
#46692=CARTESIAN_POINT('Ctrl Pts',(-38.0327645066527,-85.0564073718396,
116.843754711236));
#46693=CARTESIAN_POINT('Ctrl Pts',(-35.0011212106762,-84.8809783786076,
116.685806188043));
#46694=CARTESIAN_POINT('Ctrl Pts',(-33.1969316107817,-87.3236278199592,
116.527857664851));
#46695=CARTESIAN_POINT('Ctrl Pts',(-34.2559995452469,-90.1696797372461,
116.369909141658));
#46696=CARTESIAN_POINT('Ctrl Pts',(-37.2181003279875,-90.8387054158202,
116.211960618466));
#46697=CARTESIAN_POINT('Ctrl Pts',(-39.3975872675156,-88.7241196204147,
116.054012095273));
#46698=CARTESIAN_POINT('Ctrl Pts',(-38.8183858418599,-85.743152979504,115.896063572081));
#46699=CARTESIAN_POINT('Ctrl Pts',(-36.0056403680474,-84.5985572843997,
115.738115048888));
#46700=CARTESIAN_POINT('Ctrl Pts',(-33.5095816213973,-86.3281026405484,
115.580166525696));
#46701=CARTESIAN_POINT('Ctrl Pts',(-33.593310153302,-89.3636628752742,115.422218002503));
#46702=CARTESIAN_POINT('Ctrl Pts',(-36.1809118503718,-90.9529878461426,
115.264269479311));
#46703=CARTESIAN_POINT('Ctrl Pts',(-38.9262869522217,-89.655084939201,115.106320956118));
#46704=CARTESIAN_POINT('Ctrl Pts',(-39.3402873508135,-86.6467232462409,
114.948372432926));
#46705=CARTESIAN_POINT('Ctrl Pts',(-37.0475514759973,-84.6554928190843,
114.790423909734));
#46706=CARTESIAN_POINT('Ctrl Pts',(-34.1268332150591,-85.486781725498,114.632475386541));
#46707=CARTESIAN_POINT('Ctrl Pts',(-33.2262589855613,-88.3868855965463,
114.474526863349));
#46708=CARTESIAN_POINT('Ctrl Pts',(-35.1623520516624,-90.7263684550214,
114.316578340156));
#46709=CARTESIAN_POINT('Ctrl Pts',(-38.1797157139374,-90.3840923452991,
114.158629816964));
#46710=CARTESIAN_POINT('Ctrl Pts',(-39.542598108769,-87.670388606207,114.000681293771));
#46711=CARTESIAN_POINT('Ctrl Pts',(-38.0153152189578,-85.0456898844117,
113.842732770579));
#46712=CARTESIAN_POINT('Ctrl Pts',(-34.9826079904861,-84.8897306843618,
113.684784247386));
#46713=CARTESIAN_POINT('Ctrl Pts',(-33.1941398317884,-87.3439144694579,
113.526835724194));
#46714=CARTESIAN_POINT('Ctrl Pts',(-34.2714604285556,-90.1831074423791,
113.368887201001));
#46715=CARTESIAN_POINT('Ctrl Pts',(-37.2377959609237,-90.8330996847288,
113.210938677809));
#46716=CARTESIAN_POINT('Ctrl Pts',(-39.4036602187116,-88.7045629989887,
113.052990154616));
#46717=CARTESIAN_POINT('Ctrl Pts',(-38.8053299511668,-85.7273768616027,
112.895041631424));
#46718=CARTESIAN_POINT('Ctrl Pts',(-35.9852930144797,-84.6008653963151,
112.737093108231));
#46719=CARTESIAN_POINT('Ctrl Pts',(-33.500391131598,-86.346402287405,112.579144585039));
#46720=CARTESIAN_POINT('Ctrl Pts',(-33.6036092648561,-89.3813623238255,
112.421196061847));
#46721=CARTESIAN_POINT('Ctrl Pts',(-36.2013626720665,-90.9540395446918,
112.263247538654));
#46722=CARTESIAN_POINT('Ctrl Pts',(-38.9383473460099,-89.638535344659,112.105299015462));
#46723=CARTESIAN_POINT('Ctrl Pts',(-39.3330225244481,-86.6275773726469,
111.947350492269));
#46724=CARTESIAN_POINT('Ctrl Pts',(-37.0275482265935,-84.6511096477281,
111.789401969077));
#46725=CARTESIAN_POINT('Ctrl Pts',(-34.112227880481,-85.5011353445453,111.631453445884));
#46726=CARTESIAN_POINT('Ctrl Pts',(-33.2302937784678,-88.4069620161419,
111.473504922692));
#46727=CARTESIAN_POINT('Ctrl Pts',(-35.1813687480418,-90.7339649961363,
111.315556399499));
#46728=CARTESIAN_POINT('Ctrl Pts',(-38.196472453541,-90.3723214550984,111.157607876307));
#46729=CARTESIAN_POINT('Ctrl Pts',(-39.5419020654483,-87.6499225929314,
110.999659353114));
#46730=CARTESIAN_POINT('Ctrl Pts',(-37.9977974739878,-85.0350846596649,
110.841710829922));
#46731=CARTESIAN_POINT('Ctrl Pts',(-34.964151350524,-84.8986016832643,110.68376230673));
#46732=CARTESIAN_POINT('Ctrl Pts',(-33.1914783708088,-87.3642186263104,
110.525813783537));
#46733=CARTESIAN_POINT('Ctrl Pts',(-34.2870072125833,-90.1964355973184,
110.367865260345));
#46734=CARTESIAN_POINT('Ctrl Pts',(-37.2574551930994,-90.827367601673,110.209916737152));
#46735=CARTESIAN_POINT('Ctrl Pts',(-39.4096074723959,-88.6849677902127,
110.05196821396));
#46736=CARTESIAN_POINT('Ctrl Pts',(-38.7921730297185,-85.7116848927485,
109.894019690767));
#46737=CARTESIAN_POINT('Ctrl Pts',(-35.9649609037799,-84.6033041274846,
109.736071167575));
#46738=CARTESIAN_POINT('Ctrl Pts',(-33.4913183270346,-86.3647605351813,
109.578122644382));
#46739=CARTESIAN_POINT('Ctrl Pts',(-33.6140218250344,-89.3989953467633,
109.42017412119));
#46740=CARTESIAN_POINT('Ctrl Pts',(-36.2218197987848,-90.954959763239,109.262225597997));
#46741=CARTESIAN_POINT('Ctrl Pts',(-38.9503012804293,-89.6219089469059,
109.104277074805));
#46742=CARTESIAN_POINT('Ctrl Pts',(-39.3256348008056,-86.6084779336666,
108.946328551612));
#46743=CARTESIAN_POINT('Ctrl Pts',(-37.0075174743604,-84.6468562569993,
108.78838002842));
#46744=CARTESIAN_POINT('Ctrl Pts',(-34.0977145402883,-85.5155798788835,
108.630431505227));
#46745=CARTESIAN_POINT('Ctrl Pts',(-33.2344583680801,-88.4270173992954,
108.472482982035));
#46746=CARTESIAN_POINT('Ctrl Pts',(-35.2004318364279,-90.7414284054822,
108.314534458842));
#46747=CARTESIAN_POINT('Ctrl Pts',(-38.213157366435,-90.3604655661585,108.15658593565));
#46748=CARTESIAN_POINT('Ctrl Pts',(-39.5410661928425,-87.6294154975324,
107.998637412457));
#46749=CARTESIAN_POINT('Ctrl Pts',(-37.9802293342459,-85.0246866856932,
107.840688889265));
#46750=CARTESIAN_POINT('Ctrl Pts',(-34.9457163880272,-84.9073965528478,
107.682740366073));
#46751=CARTESIAN_POINT('Ctrl Pts',(-33.1890206543715,-87.3849394249949,
107.52479184288));
#46752=CARTESIAN_POINT('Ctrl Pts',(-34.3024881965678,-90.2088411203753,
107.366843319688));
#46753=CARTESIAN_POINT('Ctrl Pts',(-37.2773795631922,-90.8232132715162,
107.208894796495));
#46754=CARTESIAN_POINT('Ctrl Pts',(-39.4147368806325,-88.661840021548,107.050946273303));
#46755=CARTESIAN_POINT('Ctrl Pts',(-38.9902947372383,-86.6917167303234,
106.945647257841));
#46756=CARTESIAN_POINT('Ctrl Pts',(-38.4092576250251,-86.0121302673448,
106.89299775011));
#46757=CARTESIAN_POINT('Ctrl Pts',(-37.0051260726587,-90.2006423906073,
122.321006749669));
#46758=CARTESIAN_POINT('Ctrl Pts',(-37.8096764711458,-89.9855519312415,
122.268357241939));
#46759=CARTESIAN_POINT('Ctrl Pts',(-39.1749136338067,-88.6972344995558,
122.163058226477));
#46760=CARTESIAN_POINT('Ctrl Pts',(-38.6746343873266,-85.9105079516534,
122.005109703285));
#46761=CARTESIAN_POINT('Ctrl Pts',(-36.0669847052535,-84.8125413999697,
121.847161180092));
#46762=CARTESIAN_POINT('Ctrl Pts',(-33.7224022900841,-86.3926831662377,
121.6892126569));
#46763=CARTESIAN_POINT('Ctrl Pts',(-33.7636769872236,-89.221262104881,121.531264133707));
#46764=CARTESIAN_POINT('Ctrl Pts',(-36.1548310201154,-90.7322418452847,
121.373315610515));
#46765=CARTESIAN_POINT('Ctrl Pts',(-38.7271753625677,-89.5563680279066,
121.215367087322));
#46766=CARTESIAN_POINT('Ctrl Pts',(-39.1487851552509,-86.7594269038251,
121.05741856413));
#46767=CARTESIAN_POINT('Ctrl Pts',(-37.0372335640824,-84.8774865935611,
120.899470040937));
#46768=CARTESIAN_POINT('Ctrl Pts',(-34.3070809390753,-85.6167641007104,
120.741521517745));
#46769=CARTESIAN_POINT('Ctrl Pts',(-33.4336343721939,-88.3070183972821,
120.583572994552));
#46770=CARTESIAN_POINT('Ctrl Pts',(-35.2088403899947,-90.5090585737361,
120.42562447136));
#46771=CARTESIAN_POINT('Ctrl Pts',(-38.0231644049252,-90.226371089894,120.267675948167));
#46772=CARTESIAN_POINT('Ctrl Pts',(-39.3249489394657,-87.7152555601897,
120.109727424975));
#46773=CARTESIAN_POINT('Ctrl Pts',(-37.933903353769,-85.2524662657136,119.951778901782));
#46774=CARTESIAN_POINT('Ctrl Pts',(-35.1112474406138,-85.0709382865273,
119.79383037859));
#46775=CARTESIAN_POINT('Ctrl Pts',(-33.4161969504678,-87.3352580411336,
119.635881855397));
#46776=CARTESIAN_POINT('Ctrl Pts',(-34.3856028623679,-89.9924354210241,
119.477933332205));
#46777=CARTESIAN_POINT('Ctrl Pts',(-37.14053419649,-90.6332886333521,119.319984809013));
#46778=CARTESIAN_POINT('Ctrl Pts',(-39.1831785592718,-88.676775501313,119.16203628582));
#46779=CARTESIAN_POINT('Ctrl Pts',(-38.6615324022017,-85.8968070061733,
119.004087762628));
#46780=CARTESIAN_POINT('Ctrl Pts',(-36.0485564448438,-84.8138960194053,
118.846139239435));
#46781=CARTESIAN_POINT('Ctrl Pts',(-33.7133565108077,-86.4098850043433,
118.688190716243));
#46782=CARTESIAN_POINT('Ctrl Pts',(-33.7731873617217,-89.2377392848093,
118.53024219305));
#46783=CARTESIAN_POINT('Ctrl Pts',(-36.1738021831143,-90.7335293916316,
118.372293669858));
#46784=CARTESIAN_POINT('Ctrl Pts',(-38.7386365286165,-89.5410679265632,
118.214345146665));
#46785=CARTESIAN_POINT('Ctrl Pts',(-39.1422331026885,-86.7415234332901,
118.056396623473));
#46786=CARTESIAN_POINT('Ctrl Pts',(-37.0186631666406,-84.8731577593791,
117.89844810028));
#46787=CARTESIAN_POINT('Ctrl Pts',(-34.2933029959367,-85.629961237683,117.740499577088));
#46788=CARTESIAN_POINT('Ctrl Pts',(-33.4371537693153,-88.3257631715166,
117.582551053895));
#46789=CARTESIAN_POINT('Ctrl Pts',(-35.226459951931,-90.5163619366043,117.424602530703));
#46790=CARTESIAN_POINT('Ctrl Pts',(-38.0389120473041,-90.2156082566802,
117.26665400751));
#46791=CARTESIAN_POINT('Ctrl Pts',(-39.3245452774186,-87.696186346327,117.108705484318));
#46792=CARTESIAN_POINT('Ctrl Pts',(-37.9177150932994,-85.2423794269058,
116.950756961126));
#46793=CARTESIAN_POINT('Ctrl Pts',(-35.0939516360802,-85.0789796030929,
116.792808437933));
#46794=CARTESIAN_POINT('Ctrl Pts',(-33.4134753515389,-87.3541365255583,
116.634859914741));
#46795=CARTESIAN_POINT('Ctrl Pts',(-34.3999229774928,-90.0050346084722,
116.476911391548));
#46796=CARTESIAN_POINT('Ctrl Pts',(-37.1589124529382,-90.6281851834776,
116.318962868356));
#46797=CARTESIAN_POINT('Ctrl Pts',(-39.1889519313604,-88.658596576485,116.161014345163));
#46798=CARTESIAN_POINT('Ctrl Pts',(-38.6494663585338,-85.8820348751248,
116.003065821971));
#46799=CARTESIAN_POINT('Ctrl Pts',(-36.0295908956283,-84.8159241287137,
115.845117298778));
#46800=CARTESIAN_POINT('Ctrl Pts',(-33.70468694495,-86.4268745267296,115.687168775586));
#46801=CARTESIAN_POINT('Ctrl Pts',(-33.7826742098215,-89.2542863381334,
115.529220252393));
#46802=CARTESIAN_POINT('Ctrl Pts',(-36.1928440090593,-90.7346312653682,
115.371271729201));
#46803=CARTESIAN_POINT('Ctrl Pts',(-38.7499686876954,-89.525725585566,115.213323206008));
#46804=CARTESIAN_POINT('Ctrl Pts',(-39.1355810710419,-86.7236473113992,
115.055374682816));
#46805=CARTESIAN_POINT('Ctrl Pts',(-37.0000581389892,-84.8689555926966,
114.897426159623));
#46806=CARTESIAN_POINT('Ctrl Pts',(-34.2796135850352,-85.6432430029069,
114.739477636431));
#46807=CARTESIAN_POINT('Ctrl Pts',(-33.4407917476692,-88.3444866960797,
114.581529113239));
#46808=CARTESIAN_POINT('Ctrl Pts',(-35.2441268752179,-90.5235511702282,
114.423580590046));
#46809=CARTESIAN_POINT('Ctrl Pts',(-38.0545898534915,-90.2047449398924,
114.265632066854));
#46810=CARTESIAN_POINT('Ctrl Pts',(-39.324019376457,-87.6771199180644,114.107683543661));
#46811=CARTESIAN_POINT('Ctrl Pts',(-37.9014623035953,-85.2323968377956,
113.949735020469));
#46812=CARTESIAN_POINT('Ctrl Pts',(-35.0767078677524,-85.0871317630744,
113.791786497276));
#46813=CARTESIAN_POINT('Ctrl Pts',(-33.4108750048845,-87.3730321191129,
113.633837974084));
#46814=CARTESIAN_POINT('Ctrl Pts',(-34.4143237077375,-90.0175415756076,
113.475889450891));
#46815=CARTESIAN_POINT('Ctrl Pts',(-37.1772575559475,-90.6229638374742,
113.317940927699));
#46816=CARTESIAN_POINT('Ctrl Pts',(-39.1946084601768,-88.6403809529641,
113.159992404506));
#46817=CARTESIAN_POINT('Ctrl Pts',(-38.6373057105151,-85.8673405259296,
113.002043881314));
#46818=CARTESIAN_POINT('Ctrl Pts',(-36.0106387604836,-84.8180739733509,
112.844095358121));
#46819=CARTESIAN_POINT('Ctrl Pts',(-33.6961266472119,-86.4439193664515,
112.686146834929));
#46820=CARTESIAN_POINT('Ctrl Pts',(-33.7922671110994,-89.2707721351592,
112.528198311736));
#46821=CARTESIAN_POINT('Ctrl Pts',(-36.2118925175195,-90.7356108489278,
112.370249788544));
#46822=CARTESIAN_POINT('Ctrl Pts',(-38.7612021000511,-89.5103107970381,
112.212301265351));
#46823=CARTESIAN_POINT('Ctrl Pts',(-39.1288143939592,-86.7058142707235,
112.054352742159));
#46824=CARTESIAN_POINT('Ctrl Pts',(-36.9814265127793,-84.8648729754841,
111.896404218966));
#46825=CARTESIAN_POINT('Ctrl Pts',(-34.2660097385283,-85.6566123940217,
111.738455695774));
#46826=CARTESIAN_POINT('Ctrl Pts',(-33.444549874749,-88.3631864751999,111.580507172581));
#46827=CARTESIAN_POINT('Ctrl Pts',(-35.261839596363,-90.5306268163736,111.422558649389));
#46828=CARTESIAN_POINT('Ctrl Pts',(-38.0701975831402,-90.1937811798578,
111.264610126197));
#46829=CARTESIAN_POINT('Ctrl Pts',(-39.3233710608401,-87.6580572597103,
111.106661603004));
#46830=CARTESIAN_POINT('Ctrl Pts',(-37.8851457507329,-85.2225188135125,
110.948713079812));
#46831=CARTESIAN_POINT('Ctrl Pts',(-35.0595167999453,-85.0953944774125,
110.790764556619));
#46832=CARTESIAN_POINT('Ctrl Pts',(-33.4083960403351,-87.391944019542,110.632816033427));
#46833=CARTESIAN_POINT('Ctrl Pts',(-34.4288044484873,-90.0299558187079,
110.474867510234));
#46834=CARTESIAN_POINT('Ctrl Pts',(-37.1955687541971,-90.6176248034632,
110.316918987042));
#46835=CARTESIAN_POINT('Ctrl Pts',(-39.2001479105622,-88.6221293880284,
110.158970463849));
#46836=CARTESIAN_POINT('Ctrl Pts',(-38.625050959422,-85.8527245556798,110.001021940657));
#46837=CARTESIAN_POINT('Ctrl Pts',(-35.9917008230032,-84.8203454806775,
109.843073417464));
#46838=CARTESIAN_POINT('Ctrl Pts',(-33.6876759650309,-86.4610187888269,
109.685124894272));
#46839=CARTESIAN_POINT('Ctrl Pts',(-33.8019656818272,-89.287196061377,109.527176371079));
#46840=CARTESIAN_POINT('Ctrl Pts',(-36.2309468986677,-90.7364679680718,
109.369227847887));
#46841=CARTESIAN_POINT('Ctrl Pts',(-38.7723363529588,-89.4948244716966,
109.211279324695));
#46842=CARTESIAN_POINT('Ctrl Pts',(-39.1219332466681,-86.6880244806394,
109.053330801502));
#46843=CARTESIAN_POINT('Ctrl Pts',(-36.9627692696098,-84.8609112398387,
108.89538227831));
#46844=CARTESIAN_POINT('Ctrl Pts',(-34.2524915783501,-85.6700664663643,
108.737433755117));
#46845=CARTESIAN_POINT('Ctrl Pts',(-33.4484288983719,-88.381866660347,108.579485231925));
#46846=CARTESIAN_POINT('Ctrl Pts',(-35.2795955284141,-90.5375784595981,
108.421536708732));
#46847=CARTESIAN_POINT('Ctrl Pts',(-38.0857384112381,-90.1827382494491,
108.26358818554));
#46848=CARTESIAN_POINT('Ctrl Pts',(-39.3225925040349,-87.6389563362348,
108.105639662347));
#46849=CARTESIAN_POINT('Ctrl Pts',(-37.8687822586688,-85.2128338288146,
107.947691139155));
#46850=CARTESIAN_POINT('Ctrl Pts',(-35.0423459231792,-85.1035862826206,
107.789742615962));
#46851=CARTESIAN_POINT('Ctrl Pts',(-33.406106849561,-87.4112439926645,107.63179409277));
#46852=CARTESIAN_POINT('Ctrl Pts',(-34.443223901104,-90.0415106948117,107.473845569577));
#46853=CARTESIAN_POINT('Ctrl Pts',(-37.2141269098517,-90.6137553358046,
107.315897046385));
#46854=CARTESIAN_POINT('Ctrl Pts',(-39.204925595178,-88.6005874909031,107.157948523193));
#46855=CARTESIAN_POINT('Ctrl Pts',(-38.8095874576699,-86.7655555914181,
107.052649507731));
#46856=CARTESIAN_POINT('Ctrl Pts',(-38.2683920713481,-86.1325683851967,
107.));
#46857=CARTESIAN_POINT('Ctrl Pts',(-38.8699208872996,-87.7667938007243,
121.112583302492));
#46858=CARTESIAN_POINT('Ctrl Pts',(-38.8718337523485,-87.4752409435295,
121.094195056371));
#46859=CARTESIAN_POINT('Ctrl Pts',(-38.8249624563278,-87.1842829363247,
121.07580681025));
#46860=CARTESIAN_POINT('Ctrl Pts',(-38.7265915912756,-86.9119270394614,
121.05741856413));
#46861=CARTESIAN_POINT('Ctrl Pts',(-38.4449346248614,-86.1321134670705,
121.004769056399));
#46862=CARTESIAN_POINT('Ctrl Pts',(-37.7410840944719,-85.5048000303158,
120.952119548668));
#46863=CARTESIAN_POINT('Ctrl Pts',(-36.934133391776,-85.3143562297967,120.899470040937));
#46864=CARTESIAN_POINT('Ctrl Pts',(-36.12718268908,-85.1239124292776,120.846820533206));
#46865=CARTESIAN_POINT('Ctrl Pts',(-35.2171318140777,-85.370338264994,120.794171025476));
#46866=CARTESIAN_POINT('Ctrl Pts',(-34.6165319487629,-85.9419268989475,
120.741521517745));
#46867=CARTESIAN_POINT('Ctrl Pts',(-34.0159320834482,-86.513515532901,120.688872010014));
#46868=CARTESIAN_POINT('Ctrl Pts',(-33.724783227821,-87.4102669650915,120.636222502283));
#46869=CARTESIAN_POINT('Ctrl Pts',(-33.8750764696409,-88.2256493772624,
120.583572994552));
#46870=CARTESIAN_POINT('Ctrl Pts',(-34.0253697114608,-89.0410317894334,
120.530923486821));
#46871=CARTESIAN_POINT('Ctrl Pts',(-34.6171050507278,-89.7750451815847,
120.478273979091));
#46872=CARTESIAN_POINT('Ctrl Pts',(-35.3820267228497,-90.09493729702,120.42562447136));
#46873=CARTESIAN_POINT('Ctrl Pts',(-36.1469483949716,-90.4148294124554,
120.372974963629));
#46874=CARTESIAN_POINT('Ctrl Pts',(-37.0850563999484,-90.3206002511747,
120.320325455898));
#46875=CARTESIAN_POINT('Ctrl Pts',(-37.7710744915269,-89.8549664155836,
120.267675948167));
#46876=CARTESIAN_POINT('Ctrl Pts',(-38.4446886453889,-89.3977517356478,
120.215978399609));
#46877=CARTESIAN_POINT('Ctrl Pts',(-38.8752465796083,-88.5824417440886,
120.16428085105));
#46878=CARTESIAN_POINT('Ctrl Pts',(-38.8765118730483,-87.7682823374696,
120.112583302492));
#46879=CARTESIAN_POINT('Ctrl Pts',(-37.1487253572165,-90.7377785423179,
122.));
#46880=CARTESIAN_POINT('Ctrl Pts',(-37.2417753655626,-90.7037404336132,
122.));
#46881=CARTESIAN_POINT('Ctrl Pts',(-37.3327602094243,-90.6649336190233,
122.));
#46882=CARTESIAN_POINT('Ctrl Pts',(-37.4214714043315,-90.6216864230573,
122.));
#46883=CARTESIAN_POINT('Ctrl Pts',(-37.5121495818684,-90.577480312229,122.));
#46884=CARTESIAN_POINT('Ctrl Pts',(-37.6004528338949,-90.5286341083678,
122.));
#46885=CARTESIAN_POINT('Ctrl Pts',(-37.6861295811054,-90.475452921536,122.));
#46886=CARTESIAN_POINT('Ctrl Pts',(-37.7685610193578,-90.4242861597104,
122.));
#46887=CARTESIAN_POINT('Ctrl Pts',(-37.8485614444594,-90.3691057247624,
122.));
#46888=CARTESIAN_POINT('Ctrl Pts',(-37.9258738297264,-90.3101533054175,
122.));
#46889=CARTESIAN_POINT('Ctrl Pts',(-37.993522166835,-90.2585699384908,122.));
#46890=CARTESIAN_POINT('Ctrl Pts',(-38.0591121832093,-90.2040979486484,
122.));
#46891=CARTESIAN_POINT('Ctrl Pts',(-38.122447070225,-90.1468865492567,122.));
#46892=CARTESIAN_POINT('Ctrl Pts',(-38.1365835575632,-90.1341168379459,
122.));
#46893=CARTESIAN_POINT('Ctrl Pts',(-38.1506103387469,-90.1212079154214,
122.));
#46894=CARTESIAN_POINT('Ctrl Pts',(-38.1645056404263,-90.1081799738368,
122.));
#46895=CARTESIAN_POINT('Ctrl Pts',(-38.2369357281125,-90.0402710523098,
122.));
#46896=CARTESIAN_POINT('Ctrl Pts',(-38.3059001283609,-89.9690402129453,
122.));
#46897=CARTESIAN_POINT('Ctrl Pts',(-38.3711588917122,-89.894778180942,122.));
#46898=CARTESIAN_POINT('Ctrl Pts',(-38.4360586404937,-89.8209246940919,
122.));
#46899=CARTESIAN_POINT('Ctrl Pts',(-38.4972938990556,-89.7440724775117,
122.));
#46900=CARTESIAN_POINT('Ctrl Pts',(-38.554585046789,-89.6644807163591,122.));
#46901=CARTESIAN_POINT('Ctrl Pts',(-38.6097479523584,-89.587845616902,122.));
#46902=CARTESIAN_POINT('Ctrl Pts',(-38.6612544977319,-89.5086699914616,
122.));
#46903=CARTESIAN_POINT('Ctrl Pts',(-38.7088102350433,-89.4271716153117,
122.));
#46904=CARTESIAN_POINT('Ctrl Pts',(-38.7287565668071,-89.3929887019389,
122.));
#46905=CARTESIAN_POINT('Ctrl Pts',(-38.7480072950061,-89.3583970589295,
122.));
#46906=CARTESIAN_POINT('Ctrl Pts',(-38.7665381094582,-89.3234124579976,
122.));
#46907=CARTESIAN_POINT('Ctrl Pts',(-38.7794206549516,-89.2990913082588,
122.));
#46908=CARTESIAN_POINT('Ctrl Pts',(-38.7919552356554,-89.2745802403039,
122.));
#46909=CARTESIAN_POINT('Ctrl Pts',(-38.8041332176979,-89.2498845474537,
122.));
#46910=CARTESIAN_POINT('Ctrl Pts',(-38.8120415511817,-89.2338472619665,
122.));
#46911=CARTESIAN_POINT('Ctrl Pts',(-38.819800609578,-89.2177295044568,122.));
#46912=CARTESIAN_POINT('Ctrl Pts',(-38.827397852521,-89.2015549139639,122.));
#46913=CARTESIAN_POINT('Ctrl Pts',(-38.8695181483044,-89.1118804701093,
122.));
#46914=CARTESIAN_POINT('Ctrl Pts',(-38.9067396123332,-89.0203224429062,
122.));
#46915=CARTESIAN_POINT('Ctrl Pts',(-38.9387709613748,-88.9271531995467,
122.));
#46916=CARTESIAN_POINT('Ctrl Pts',(-38.9686507170741,-88.840242272796,122.));
#46917=CARTESIAN_POINT('Ctrl Pts',(-38.9940140218715,-88.7519285239463,
122.));
#46918=CARTESIAN_POINT('Ctrl Pts',(-39.0145738981738,-88.6624243415515,
122.));
#46919=CARTESIAN_POINT('Ctrl Pts',(-39.0160543819306,-88.6559792887581,
122.));
#46920=CARTESIAN_POINT('Ctrl Pts',(-39.0175099363868,-88.649528062159,122.));
#46921=CARTESIAN_POINT('Ctrl Pts',(-39.0189404437644,-88.6430707407411,
122.));
#46922=CARTESIAN_POINT('Ctrl Pts',(-39.0395466647231,-88.5500540992174,
122.));
#46923=CARTESIAN_POINT('Ctrl Pts',(-39.0549598625021,-88.4557718035346,
122.));
#46924=CARTESIAN_POINT('Ctrl Pts',(-39.0652569568635,-88.3606317181991,
122.));
#46925=CARTESIAN_POINT('Ctrl Pts',(-39.0710534787644,-88.3070747079457,
122.));
#46926=CARTESIAN_POINT('Ctrl Pts',(-39.075227840788,-88.2532460633916,122.));
#46927=CARTESIAN_POINT('Ctrl Pts',(-39.0777870025032,-88.1992211791364,
122.));
#46928=CARTESIAN_POINT('Ctrl Pts',(-39.0784478860045,-88.1852696752318,
122.));
#46929=CARTESIAN_POINT('Ctrl Pts',(-39.0790009329215,-88.1713056833736,
122.));
#46930=CARTESIAN_POINT('Ctrl Pts',(-39.0794460217079,-88.1573438714348,
122.));
#46931=CARTESIAN_POINT('Ctrl Pts',(-39.0824174382877,-88.0641346944071,
122.));
#46932=CARTESIAN_POINT('Ctrl Pts',(-39.0805897017238,-87.9708672878142,
122.));
#46933=CARTESIAN_POINT('Ctrl Pts',(-39.0740977060608,-87.8779167295335,
122.));
#46934=CARTESIAN_POINT('Ctrl Pts',(-39.067594916049,-87.7848116208187,122.));
#46935=CARTESIAN_POINT('Ctrl Pts',(-39.0564119653958,-87.6920234352952,
122.));
#46936=CARTESIAN_POINT('Ctrl Pts',(-39.0406334894346,-87.5999412206982,
122.));
#46937=CARTESIAN_POINT('Ctrl Pts',(-39.0250806083283,-87.5091755637904,
122.));
#46938=CARTESIAN_POINT('Ctrl Pts',(-39.0050622117732,-87.4190949906259,
122.));
#46939=CARTESIAN_POINT('Ctrl Pts',(-38.980616331591,-87.3300972983945,122.));
#46940=CARTESIAN_POINT('Ctrl Pts',(-38.97151756715,-87.2969723288138,122.));
#46941=CARTESIAN_POINT('Ctrl Pts',(-38.9618050517351,-87.2639976908667,
122.));
#46942=CARTESIAN_POINT('Ctrl Pts',(-38.951479384889,-87.2311951618355,122.));
#46943=CARTESIAN_POINT('Ctrl Pts',(-38.9444848308163,-87.2089748959248,
122.));
#46944=CARTESIAN_POINT('Ctrl Pts',(-38.9372089088412,-87.1868336198287,
122.));
#46945=CARTESIAN_POINT('Ctrl Pts',(-38.9296516262008,-87.1647783159968,
122.));
#46946=CARTESIAN_POINT('Ctrl Pts',(-38.9251355607667,-87.1515985528445,
122.));
#46947=CARTESIAN_POINT('Ctrl Pts',(-38.920519367556,-87.1384506632302,122.));
#46948=CARTESIAN_POINT('Ctrl Pts',(-38.9158065183222,-87.125345284988,122.));
#46949=CARTESIAN_POINT('Ctrl Pts',(-38.8841747708194,-87.0373844793449,
122.));
#46950=CARTESIAN_POINT('Ctrl Pts',(-38.8481538095828,-86.9512214197519,
122.));
#46951=CARTESIAN_POINT('Ctrl Pts',(-38.8078081980317,-86.8672703477228,
122.));
#46952=CARTESIAN_POINT('Ctrl Pts',(-38.7775489893683,-86.8043070437009,
122.));
#46953=CARTESIAN_POINT('Ctrl Pts',(-38.7448561175797,-86.7425884746254,
122.));
#46954=CARTESIAN_POINT('Ctrl Pts',(-38.7097408585933,-86.6823049297191,
122.));
#46955=CARTESIAN_POINT('Ctrl Pts',(-38.696271461237,-86.659181562732,122.));
#46956=CARTESIAN_POINT('Ctrl Pts',(-38.6824455217908,-86.6362694937627,
122.));
#46957=CARTESIAN_POINT('Ctrl Pts',(-38.6682631961917,-86.6135801059869,
122.));
#46958=CARTESIAN_POINT('Ctrl Pts',(-38.6581390971867,-86.5973832131288,
122.));
#46959=CARTESIAN_POINT('Ctrl Pts',(-38.6478325520626,-86.5812987298577,
122.));
#46960=CARTESIAN_POINT('Ctrl Pts',(-38.6373536921582,-86.5653458007593,
122.));
#46961=CARTESIAN_POINT('Ctrl Pts',(-38.5901671142441,-86.4935093472977,
122.));
#46962=CARTESIAN_POINT('Ctrl Pts',(-38.5394456084747,-86.4242663429416,
122.));
#46963=CARTESIAN_POINT('Ctrl Pts',(-38.4852220660282,-86.3579687859785,
122.));
#46964=CARTESIAN_POINT('Ctrl Pts',(-38.4364256387811,-86.2983068057933,
122.));
#46965=CARTESIAN_POINT('Ctrl Pts',(-38.384792513307,-86.2410302511397,122.));
#46966=CARTESIAN_POINT('Ctrl Pts',(-38.3303261681671,-86.1864254606589,
122.));
#46967=CARTESIAN_POINT('Ctrl Pts',(-38.3112435979327,-86.1672943853717,
122.));
#46968=CARTESIAN_POINT('Ctrl Pts',(-38.2918130826719,-86.1484915580211,
122.));
#46969=CARTESIAN_POINT('Ctrl Pts',(-38.2720451973146,-86.1300214660444,
122.));
#46970=CARTESIAN_POINT('Origin',(-36.3549260746835,-87.7685555885722,114.));
#46971=CARTESIAN_POINT('Origin',(87.7685555885722,36.3549260746835,107.));
#46972=CARTESIAN_POINT('Ctrl Pts',(85.8550895919077,37.990913278059,107.));
#46973=CARTESIAN_POINT('Ctrl Pts',(85.7929520311059,37.9325192289305,107.));
#46974=CARTESIAN_POINT('Ctrl Pts',(85.7341898434987,37.870871272988,107.));
#46975=CARTESIAN_POINT('Ctrl Pts',(85.6788150093107,37.8063458857252,107.));
#46976=CARTESIAN_POINT('Ctrl Pts',(85.6220850990849,37.7402414994929,107.));
#46977=CARTESIAN_POINT('Ctrl Pts',(85.5689098861403,37.6711166406476,107.));
#46978=CARTESIAN_POINT('Ctrl Pts',(85.5193311397496,37.5993298294372,107.));
#46979=CARTESIAN_POINT('Ctrl Pts',(85.5063933542064,37.5805967545636,107.));
#46980=CARTESIAN_POINT('Ctrl Pts',(85.4937006485471,37.5616821917131,107.));
#46981=CARTESIAN_POINT('Ctrl Pts',(85.4812541404578,37.5425920787089,107.));
#46982=CARTESIAN_POINT('Ctrl Pts',(85.4710842317646,37.5269937514671,107.));
#46983=CARTESIAN_POINT('Ctrl Pts',(85.4610782527306,37.5112773132593,107.));
#46984=CARTESIAN_POINT('Ctrl Pts',(85.451245660872,37.4954605983594,107.));
#46985=CARTESIAN_POINT('Ctrl Pts',(85.4038015149672,37.4191419084113,107.));
#46986=CARTESIAN_POINT('Ctrl Pts',(85.3603409327412,37.3404158601138,107.));
#46987=CARTESIAN_POINT('Ctrl Pts',(85.3208986011901,37.2596750041506,107.));
#46988=CARTESIAN_POINT('Ctrl Pts',(85.289070121347,37.1945201665567,107.));
#46989=CARTESIAN_POINT('Ctrl Pts',(85.2598587801396,37.1280522210504,107.));
#46990=CARTESIAN_POINT('Ctrl Pts',(85.2332999634681,37.0604596404359,107.));
#46991=CARTESIAN_POINT('Ctrl Pts',(85.222698407226,37.03347852325,107.));
#46992=CARTESIAN_POINT('Ctrl Pts',(85.2125196847992,37.0063180560248,107.));
#46993=CARTESIAN_POINT('Ctrl Pts',(85.202766807445,36.9789896805406,107.));
#46994=CARTESIAN_POINT('Ctrl Pts',(85.1975258836901,36.9643041752218,107.));
#46995=CARTESIAN_POINT('Ctrl Pts',(85.1924083106982,36.9495710019478,107.));
#46996=CARTESIAN_POINT('Ctrl Pts',(85.1874185552013,36.9348044141012,107.));
#46997=CARTESIAN_POINT('Ctrl Pts',(85.1578797376145,36.8473877971847,107.));
#46998=CARTESIAN_POINT('Ctrl Pts',(85.1327763850984,36.7586900770684,107.));
#46999=CARTESIAN_POINT('Ctrl Pts',(85.1121410667902,36.6691090626677,107.));
#47000=CARTESIAN_POINT('Ctrl Pts',(85.0911842873704,36.5781325373261,107.));
#47001=CARTESIAN_POINT('Ctrl Pts',(85.0748353336161,36.4862441776303,107.));
#47002=CARTESIAN_POINT('Ctrl Pts',(85.063170145668,36.3938274894209,107.));
#47003=CARTESIAN_POINT('Ctrl Pts',(85.0515956741347,36.302129496071,107.));
#47004=CARTESIAN_POINT('Ctrl Pts',(85.044632059208,36.2099104295858,107.));
#47005=CARTESIAN_POINT('Ctrl Pts',(85.0424004276122,36.1175257080037,107.));
#47006=CARTESIAN_POINT('Ctrl Pts',(85.0412898130999,36.0715486691903,107.));
#47007=CARTESIAN_POINT('Ctrl Pts',(85.0413519548824,36.0255303886718,107.));
#47008=CARTESIAN_POINT('Ctrl Pts',(85.0426065811632,35.9795139766001,107.));
#47009=CARTESIAN_POINT('Ctrl Pts',(85.0429763592658,35.9659514824889,107.));
#47010=CARTESIAN_POINT('Ctrl Pts',(85.0434497468013,35.9523891500023,107.));
#47011=CARTESIAN_POINT('Ctrl Pts',(85.0440273052287,35.9388280828518,107.));
#47012=CARTESIAN_POINT('Ctrl Pts',(85.0446478097844,35.9242586409637,107.));
#47013=CARTESIAN_POINT('Ctrl Pts',(85.0453881505517,35.9097004462176,107.));
#47014=CARTESIAN_POINT('Ctrl Pts',(85.0462483760475,35.8951574260082,107.));
#47015=CARTESIAN_POINT('Ctrl Pts',(85.0519001792078,35.7996077265604,107.));
#47016=CARTESIAN_POINT('Ctrl Pts',(85.062724622194,35.704679743261,107.));
#47017=CARTESIAN_POINT('Ctrl Pts',(85.0787921606883,35.6107691191273,107.));
#47018=CARTESIAN_POINT('Ctrl Pts',(85.0811724830822,35.5968567478123,107.));
#47019=CARTESIAN_POINT('Ctrl Pts',(85.0836679621313,35.58296667092,107.));
#47020=CARTESIAN_POINT('Ctrl Pts',(85.0862789194279,35.5691001441169,107.));
#47021=CARTESIAN_POINT('Ctrl Pts',(85.1032245667356,35.4791035467392,107.));
#47022=CARTESIAN_POINT('Ctrl Pts',(85.1250300977973,35.3900991191957,107.));
#47023=CARTESIAN_POINT('Ctrl Pts',(85.1513929626019,35.3023191100351,107.));
#47024=CARTESIAN_POINT('Ctrl Pts',(85.1783517741502,35.2125547865366,107.));
#47025=CARTESIAN_POINT('Ctrl Pts',(85.2100764994212,35.124070164157,107.));
#47026=CARTESIAN_POINT('Ctrl Pts',(85.2462978446929,35.0371172881203,107.));
#47027=CARTESIAN_POINT('Ctrl Pts',(85.2587879482913,35.0071335748779,107.));
#47028=CARTESIAN_POINT('Ctrl Pts',(85.271813175909,34.9773320762697,107.));
#47029=CARTESIAN_POINT('Ctrl Pts',(85.285363857908,34.9477234661865,107.));
#47030=CARTESIAN_POINT('Ctrl Pts',(85.2920548932063,34.9331033714035,107.));
#47031=CARTESIAN_POINT('Ctrl Pts',(85.2988740536566,34.9185303096388,107.));
#47032=CARTESIAN_POINT('Ctrl Pts',(85.3058202343552,34.9040055884619,107.));
#47033=CARTESIAN_POINT('Ctrl Pts',(85.311314009465,34.8925179011785,107.));
#47034=CARTESIAN_POINT('Ctrl Pts',(85.3168867996743,34.8810614773674,107.));
#47035=CARTESIAN_POINT('Ctrl Pts',(85.3225334641222,34.8696458936071,107.));
#47036=CARTESIAN_POINT('Ctrl Pts',(85.3652573996406,34.7832730147196,107.));
#47037=CARTESIAN_POINT('Ctrl Pts',(85.4122721941406,34.6990984517528,107.));
#47038=CARTESIAN_POINT('Ctrl Pts',(85.4632351918275,34.617371842537,107.));
#47039=CARTESIAN_POINT('Ctrl Pts',(85.5152089048678,34.5340244036513,107.));
#47040=CARTESIAN_POINT('Ctrl Pts',(85.5712892919147,34.4532222071275,107.));
#47041=CARTESIAN_POINT('Ctrl Pts',(85.6311679130609,34.375237069139,107.));
#47042=CARTESIAN_POINT('Ctrl Pts',(85.6915333690277,34.2966178838074,107.));
#47043=CARTESIAN_POINT('Ctrl Pts',(85.7557595309992,34.2208609138809,107.));
#47044=CARTESIAN_POINT('Ctrl Pts',(85.8235797056875,34.148263938979,107.));
#47045=CARTESIAN_POINT('Ctrl Pts',(85.8605803979252,34.1086571650643,107.));
#47046=CARTESIAN_POINT('Ctrl Pts',(85.8986516547817,34.0699913632724,107.));
#47047=CARTESIAN_POINT('Ctrl Pts',(85.9377555171043,34.0323186678644,107.));
#47048=CARTESIAN_POINT('Ctrl Pts',(85.9497228887807,34.0207892914493,107.));
#47049=CARTESIAN_POINT('Ctrl Pts',(85.9617869996997,34.0093529526037,107.));
#47050=CARTESIAN_POINT('Ctrl Pts',(85.9739468248078,33.9980112077434,107.));
#47051=CARTESIAN_POINT('Ctrl Pts',(85.9844926071238,33.988174917228,107.));
#47052=CARTESIAN_POINT('Ctrl Pts',(85.9951092677648,33.9784108917292,107.));
#47053=CARTESIAN_POINT('Ctrl Pts',(86.0057870254269,33.9687281255323,107.));
#47054=CARTESIAN_POINT('Ctrl Pts',(86.0813614985429,33.9001959508192,107.));
#47055=CARTESIAN_POINT('Ctrl Pts',(86.1601126924122,33.835620120822,107.));
#47056=CARTESIAN_POINT('Ctrl Pts',(86.2417132596611,33.7752824079571,107.));
#47057=CARTESIAN_POINT('Ctrl Pts',(86.3234180225243,33.7148676499775,107.));
#47058=CARTESIAN_POINT('Ctrl Pts',(86.407980013518,33.6587010007676,107.));
#47059=CARTESIAN_POINT('Ctrl Pts',(86.4951159042006,33.6070911134787,107.));
#47060=CARTESIAN_POINT('Ctrl Pts',(86.5805195599158,33.55650721503,107.));
#47061=CARTESIAN_POINT('Ctrl Pts',(86.6683964598967,33.5103000274096,107.));
#47062=CARTESIAN_POINT('Ctrl Pts',(86.7585139289399,33.4687959635278,107.));
#47063=CARTESIAN_POINT('Ctrl Pts',(86.7988635962662,33.4502127167045,107.));
#47064=CARTESIAN_POINT('Ctrl Pts',(86.8396628450883,33.4325728773236,107.));
#47065=CARTESIAN_POINT('Ctrl Pts',(86.8808925437874,33.4159086922478,107.));
#47066=CARTESIAN_POINT('Ctrl Pts',(86.9113121896724,33.4036137052611,107.));
#47067=CARTESIAN_POINT('Ctrl Pts',(86.9419661799092,33.3918498714135,107.));
#47068=CARTESIAN_POINT('Ctrl Pts',(86.9728422455434,33.3806145099939,107.));
#47069=CARTESIAN_POINT('Ctrl Pts',(88.5623548711045,33.3857031209377,107.));
#47070=CARTESIAN_POINT('Ctrl Pts',(88.6571887453956,33.4203937757735,107.));
#47071=CARTESIAN_POINT('Ctrl Pts',(88.7499794657697,33.4600753209604,107.));
#47072=CARTESIAN_POINT('Ctrl Pts',(88.8404861096065,33.5044274043379,107.));
#47073=CARTESIAN_POINT('Ctrl Pts',(88.9322656542038,33.5494032629243,107.));
#47074=CARTESIAN_POINT('Ctrl Pts',(89.0216970916563,33.5991826598102,107.));
#47075=CARTESIAN_POINT('Ctrl Pts',(89.1084951661564,33.6534722183007,107.));
#47076=CARTESIAN_POINT('Ctrl Pts',(89.1330081756223,33.6688043609645,107.));
#47077=CARTESIAN_POINT('Ctrl Pts',(89.1573109139389,33.6844964338333,107.));
#47078=CARTESIAN_POINT('Ctrl Pts',(89.181396359504,33.7005422844173,107.));
#47079=CARTESIAN_POINT('Ctrl Pts',(89.2007259405543,33.7134197530341,107.));
#47080=CARTESIAN_POINT('Ctrl Pts',(89.2199176733195,33.7265267065963,107.));
#47081=CARTESIAN_POINT('Ctrl Pts',(89.2389486421628,33.7398461999266,107.));
#47082=CARTESIAN_POINT('Ctrl Pts',(89.3216557387194,33.7977316722863,107.));
#47083=CARTESIAN_POINT('Ctrl Pts',(89.4014079749861,33.859679295932,107.));
#47084=CARTESIAN_POINT('Ctrl Pts',(89.4779389896606,33.9253917079193,107.));
#47085=CARTESIAN_POINT('Ctrl Pts',(89.5369321760609,33.9760454799314,107.));
#47086=CARTESIAN_POINT('Ctrl Pts',(89.5940106946619,34.02893718031,107.));
#47087=CARTESIAN_POINT('Ctrl Pts',(89.6490349776499,34.0839423776965,107.));
#47088=CARTESIAN_POINT('Ctrl Pts',(89.67832371242,34.1132209534407,107.));
#47089=CARTESIAN_POINT('Ctrl Pts',(89.7070301443814,34.14309849492,107.));
#47090=CARTESIAN_POINT('Ctrl Pts',(89.7351312032978,34.1735570675531,107.));
#47091=CARTESIAN_POINT('Ctrl Pts',(89.7447672055864,34.184001473811,107.));
#47092=CARTESIAN_POINT('Ctrl Pts',(89.754331292257,34.1945134919992,107.));
#47093=CARTESIAN_POINT('Ctrl Pts',(89.7638158966534,34.2050847863686,107.));
#47094=CARTESIAN_POINT('Ctrl Pts',(89.8296130855822,34.2784206287274,107.));
#47095=CARTESIAN_POINT('Ctrl Pts',(89.8916781239792,34.3547030951306,107.));
#47096=CARTESIAN_POINT('Ctrl Pts',(89.9497672435115,34.4336536253152,107.));
#47097=CARTESIAN_POINT('Ctrl Pts',(90.007329905769,34.5118886328459,107.));
#47098=CARTESIAN_POINT('Ctrl Pts',(90.0609888233644,34.5927443469894,107.));
#47099=CARTESIAN_POINT('Ctrl Pts',(90.1104610526296,34.6759720983802,107.));
#47100=CARTESIAN_POINT('Ctrl Pts',(90.158518993482,34.7568205746472,107.));
#47101=CARTESIAN_POINT('Ctrl Pts',(90.2026264068637,34.8399081044317,107.));
#47102=CARTESIAN_POINT('Ctrl Pts',(90.2424761416749,34.9250170645243,107.));
#47103=CARTESIAN_POINT('Ctrl Pts',(90.2632805570366,34.969450036667,107.));
#47104=CARTESIAN_POINT('Ctrl Pts',(90.2829236866711,35.0144340768218,107.));
#47105=CARTESIAN_POINT('Ctrl Pts',(90.3013561304951,35.059938454011,107.));
#47106=CARTESIAN_POINT('Ctrl Pts',(90.3084142100976,35.077362812904,107.));
#47107=CARTESIAN_POINT('Ctrl Pts',(90.3152947304807,35.0948634648789,107.));
#47108=CARTESIAN_POINT('Ctrl Pts',(90.3219947560663,35.1124386758054,107.));
#47109=CARTESIAN_POINT('Ctrl Pts',(90.3272364930471,35.1261885685308,107.));
#47110=CARTESIAN_POINT('Ctrl Pts',(90.3323678538939,35.1399845970363,107.));
#47111=CARTESIAN_POINT('Ctrl Pts',(90.3373823034241,35.1538112179767,107.));
#47112=CARTESIAN_POINT('Ctrl Pts',(90.3690659930617,35.2411744198563,107.));
#47113=CARTESIAN_POINT('Ctrl Pts',(90.3961408570781,35.3298985591593,107.));
#47114=CARTESIAN_POINT('Ctrl Pts',(90.4183556395185,35.4197600827214,107.));
#47115=CARTESIAN_POINT('Ctrl Pts',(90.4233396105618,35.4399208577615,107.));
#47116=CARTESIAN_POINT('Ctrl Pts',(90.428078747987,35.4601389222423,107.));
#47117=CARTESIAN_POINT('Ctrl Pts',(90.4325698536593,35.4804118071808,107.));
#47118=CARTESIAN_POINT('Ctrl Pts',(90.4529356080426,35.5723429763467,107.));
#47119=CARTESIAN_POINT('Ctrl Pts',(90.4682051514147,35.6654017572121,107.));
#47120=CARTESIAN_POINT('Ctrl Pts',(90.4784883085329,35.7591965641434,107.));
#47121=CARTESIAN_POINT('Ctrl Pts',(90.4892221738777,35.8571023742028,107.));
#47122=CARTESIAN_POINT('Ctrl Pts',(90.4945229571543,35.9558113815426,107.));
#47123=CARTESIAN_POINT('Ctrl Pts',(90.4944581052541,36.0548635705765,107.));
#47124=CARTESIAN_POINT('Ctrl Pts',(90.4944327382416,36.0936081272758,107.));
#47125=CARTESIAN_POINT('Ctrl Pts',(90.4935858264941,36.1324049341854,107.));
#47126=CARTESIAN_POINT('Ctrl Pts',(90.4919191826006,36.1712252336368,107.));
#47127=CARTESIAN_POINT('Ctrl Pts',(90.4913861442009,36.1836410294607,107.));
#47128=CARTESIAN_POINT('Ctrl Pts',(90.4907692593077,36.196057916994,107.));
#47129=CARTESIAN_POINT('Ctrl Pts',(90.4900692890457,36.2084652868845,107.));
#47130=CARTESIAN_POINT('Ctrl Pts',(90.4848300798159,36.3013332419655,107.));
#47131=CARTESIAN_POINT('Ctrl Pts',(90.4749344507016,36.3938179603827,107.));
#47132=CARTESIAN_POINT('Ctrl Pts',(90.460505860486,36.4855478660498,107.));
#47133=CARTESIAN_POINT('Ctrl Pts',(90.4461112583523,36.5770616921485,107.));
#47134=CARTESIAN_POINT('Ctrl Pts',(90.4272046158018,36.6678252027151,107.));
#47135=CARTESIAN_POINT('Ctrl Pts',(90.4038598451766,36.757452488896,107.));
#47136=CARTESIAN_POINT('Ctrl Pts',(90.3809112220297,36.845558851013,107.));
#47137=CARTESIAN_POINT('Ctrl Pts',(90.3536733503429,36.9325680090356,107.));
#47138=CARTESIAN_POINT('Ctrl Pts',(90.3221760021516,37.0180842712926,107.));
#47139=CARTESIAN_POINT('Ctrl Pts',(90.3063345627045,37.0610942631835,107.));
#47140=CARTESIAN_POINT('Ctrl Pts',(90.2894150733447,37.1037260866538,107.));
#47141=CARTESIAN_POINT('Ctrl Pts',(90.271417904293,37.1459256105394,107.));
#47142=CARTESIAN_POINT('Ctrl Pts',(90.2658521901144,37.1589760235097,107.));
#47143=CARTESIAN_POINT('Ctrl Pts',(90.2601833926065,37.1719850712082,107.));
#47144=CARTESIAN_POINT('Ctrl Pts',(90.2544114818424,37.1849510950093,107.));
#47145=CARTESIAN_POINT('Ctrl Pts',(90.2487320287865,37.1977094217589,107.));
#47146=CARTESIAN_POINT('Ctrl Pts',(90.2429562207695,37.2104182274025,107.));
#47147=CARTESIAN_POINT('Ctrl Pts',(90.2370858474454,37.223073026501,107.));
#47148=CARTESIAN_POINT('Ctrl Pts',(90.1996060503623,37.3038684505993,107.));
#47149=CARTESIAN_POINT('Ctrl Pts',(90.1582560956766,37.3825070965564,107.));
#47150=CARTESIAN_POINT('Ctrl Pts',(90.1131056594066,37.4586413742266,107.));
#47151=CARTESIAN_POINT('Ctrl Pts',(90.0687126527172,37.5334984470951,107.));
#47152=CARTESIAN_POINT('Ctrl Pts',(90.0206451521835,37.6059351413586,107.));
#47153=CARTESIAN_POINT('Ctrl Pts',(89.9689331726878,37.6755868908959,107.));
#47154=CARTESIAN_POINT('Ctrl Pts',(89.9187987056358,37.7431138619449,107.));
#47155=CARTESIAN_POINT('Ctrl Pts',(89.8652382803223,37.8080236513692,107.));
#47156=CARTESIAN_POINT('Ctrl Pts',(89.8082515369522,37.8699437651603,107.));
#47157=CARTESIAN_POINT('Ctrl Pts',(89.7872839822743,37.8927264913663,107.));
#47158=CARTESIAN_POINT('Ctrl Pts',(89.7658523353103,37.9151040470214,107.));
#47159=CARTESIAN_POINT('Ctrl Pts',(89.7439557669509,37.9370562678499,107.));
#47160=CARTESIAN_POINT('Ctrl Pts',(89.7248783320863,37.9561821900545,107.));
#47161=CARTESIAN_POINT('Ctrl Pts',(89.7054479637193,37.9749852259363,107.));
#47162=CARTESIAN_POINT('Ctrl Pts',(89.6856747987074,37.9934602469551,107.));
#47163=CARTESIAN_POINT('Origin',(87.7685555885722,36.3549260746835,124.208423447177));
#47164=CARTESIAN_POINT('Ctrl Pts',(84.6917558532639,36.3568536987801,121.708423447177));
#47165=CARTESIAN_POINT('Ctrl Pts',(84.6908331767989,36.4801286173767,121.702019850418));
#47166=CARTESIAN_POINT('Ctrl Pts',(84.7533596868374,37.6160355665901,121.642966745928));
#47167=CARTESIAN_POINT('Ctrl Pts',(86.1660867076132,39.608464641385,121.531264133707));
#47168=CARTESIAN_POINT('Ctrl Pts',(89.6167531138159,39.4750894807855,121.373315610515));
#47169=CARTESIAN_POINT('Ctrl Pts',(91.3916432643928,36.5131478211936,121.215367087322));
#47170=CARTESIAN_POINT('Ctrl Pts',(89.8816249043036,33.4075613268254,121.05741856413));
#47171=CARTESIAN_POINT('Ctrl Pts',(86.4557338964297,32.9743531814506,120.899470040937));
#47172=CARTESIAN_POINT('Ctrl Pts',(84.8091868209017,34.9127245576495,120.783138335287));
#47173=CARTESIAN_POINT('Ctrl Pts',(84.6923091848726,36.1393663959276,120.719456137367));
#47174=CARTESIAN_POINT('Ctrl Pts',(84.6942410152602,36.3522423579965,120.708423447177));
#47175=CARTESIAN_POINT('Ctrl Pts',(84.6982769289315,36.3519105223041,121.791576552823));
#47176=CARTESIAN_POINT('Ctrl Pts',(84.7032619010314,37.0449291327262,121.755752019753));
#47177=CARTESIAN_POINT('Ctrl Pts',(85.2756494227156,38.7661195118029,121.667277978953));
#47178=CARTESIAN_POINT('Ctrl Pts',(88.1200899430042,39.9637871161453,121.526154430423));
#47179=CARTESIAN_POINT('Ctrl Pts',(90.9824825683396,38.0346656023702,121.36820590723));
#47180=CARTESIAN_POINT('Ctrl Pts',(90.9320922557558,34.5813834652293,121.210257384038));
#47181=CARTESIAN_POINT('Ctrl Pts',(88.0128424000897,32.736698135431,121.052308860845));
#47182=CARTESIAN_POINT('Ctrl Pts',(85.2379952936913,34.0051402209467,120.912748583773));
#47183=CARTESIAN_POINT('Ctrl Pts',(84.702465507281,35.6938776623451,120.825837814433));
#47184=CARTESIAN_POINT('Ctrl Pts',(84.6981142843292,36.357076956871,120.791576552823));
#47185=CARTESIAN_POINT('Ctrl Pts',(89.6820215852375,37.9909132780583,122.));
#47186=CARTESIAN_POINT('Ctrl Pts',(90.223216971559,37.3579260718367,121.947350492269));
#47187=CARTESIAN_POINT('Ctrl Pts',(90.6185540996391,35.5228930793523,121.842051476808));
#47188=CARTESIAN_POINT('Ctrl Pts',(88.6277567910025,33.5097265376366,121.684102953615));
#47189=CARTESIAN_POINT('Ctrl Pts',(85.856853152671,34.0819706116619,121.526154430423));
#47190=CARTESIAN_POINT('Ctrl Pts',(84.8197362830911,36.7122378284436,121.36820590723));
#47191=CARTESIAN_POINT('Ctrl Pts',(86.455975335501,39.0198954391445,121.210257384038));
#47192=CARTESIAN_POINT('Ctrl Pts',(89.2824118663666,38.910648012169,121.052308860845));
#47193=CARTESIAN_POINT('Ctrl Pts',(90.7362221653994,36.4845253090545,120.894360337653));
#47194=CARTESIAN_POINT('Ctrl Pts',(89.4993680181651,33.9407433017105,120.73641181446));
#47195=CARTESIAN_POINT('Ctrl Pts',(86.693224985036,33.5859030524893,120.578463291268));
#47196=CARTESIAN_POINT('Ctrl Pts',(84.8620582617521,35.7416149748606,120.420514768075));
#47197=CARTESIAN_POINT('Ctrl Pts',(85.6661209826721,38.4534153039653,120.262566244883));
#47198=CARTESIAN_POINT('Ctrl Pts',(88.3763988152143,39.2625705756491,120.10461772169));
#47199=CARTESIAN_POINT('Ctrl Pts',(90.5355629043657,37.4354572382365,119.946669198498));
#47200=CARTESIAN_POINT('Ctrl Pts',(90.1859659925477,34.6286571020984,119.788720675305));
#47201=CARTESIAN_POINT('Ctrl Pts',(87.6445764061016,33.3870135407333,119.630772152113));
#47202=CARTESIAN_POINT('Ctrl Pts',(85.2155950629905,34.8362855230027,119.472823628921));
#47203=CARTESIAN_POINT('Ctrl Pts',(85.1013053402489,37.6624629423688,119.314875105728));
#47204=CARTESIAN_POINT('Ctrl Pts',(87.4053303180094,39.3031363358758,119.156926582536));
#47205=CARTESIAN_POINT('Ctrl Pts',(90.0386805913348,38.2707572071686,118.998978059343));
#47206=CARTESIAN_POINT('Ctrl Pts',(90.6137775723734,35.5013522308546,118.841029536151));
#47207=CARTESIAN_POINT('Ctrl Pts',(88.6091983117898,33.5058567116668,118.683081012958));
#47208=CARTESIAN_POINT('Ctrl Pts',(85.8424338622364,34.09352572698,118.525132489766));
#47209=CARTESIAN_POINT('Ctrl Pts',(84.8220254010344,36.7315376632941,118.367183966573));
#47210=CARTESIAN_POINT('Ctrl Pts',(86.4731462464867,39.0280873248214,118.209235443381));
#47211=CARTESIAN_POINT('Ctrl Pts',(89.2987753441784,38.9009629821107,118.051286920188));
#47212=CARTESIAN_POINT('Ctrl Pts',(90.737000729058,36.4654244092894,117.893338396996));
#47213=CARTESIAN_POINT('Ctrl Pts',(89.4838271862048,33.9297003573102,117.735389873803));
#47214=CARTESIAN_POINT('Ctrl Pts',(86.6754690534216,33.5928547032827,117.577441350611));
#47215=CARTESIAN_POINT('Ctrl Pts',(84.8581792373272,35.7602951571421,117.419492827418));
#47216=CARTESIAN_POINT('Ctrl Pts',(85.6796391438154,38.4668693790345,117.261544304226));
#47217=CARTESIAN_POINT('Ctrl Pts',(88.3950560592406,39.2586088387336,117.103595781033));
#47218=CARTESIAN_POINT('Ctrl Pts',(90.5424440520624,37.4176674477831,116.945647257841));
#47219=CARTESIAN_POINT('Ctrl Pts',(90.1748317390413,34.6131707756633,116.787698734649));
#47220=CARTESIAN_POINT('Ctrl Pts',(87.6255220239709,33.3878706600712,116.629750211456));
#47221=CARTESIAN_POINT('Ctrl Pts',(85.2058964917554,34.8527094499973,116.471801688264));
#47222=CARTESIAN_POINT('Ctrl Pts',(85.1097560228704,37.6795623656728,116.313853165071));
#47223=CARTESIAN_POINT('Ctrl Pts',(87.4242682564739,39.3054078433001,116.155904641879));
#47224=CARTESIAN_POINT('Ctrl Pts',(90.050935343065,38.2561412361693,115.997956118686));
#47225=CARTESIAN_POINT('Ctrl Pts',(90.6082381217001,35.4831006649647,115.840007595494));
#47226=CARTESIAN_POINT('Ctrl Pts',(88.5908871125881,33.5005176773809,115.682059072301));
#47227=CARTESIAN_POINT('Ctrl Pts',(85.827953120734,34.1059399707242,115.524110549109));
#47228=CARTESIAN_POINT('Ctrl Pts',(84.8245043657124,36.750449564707,115.366162025916));
#47229=CARTESIAN_POINT('Ctrl Pts',(86.4903373151876,39.0363500395887,115.208213502724));
#47230=CARTESIAN_POINT('Ctrl Pts',(89.3150918978891,38.8910849573142,115.050264979531));
#47231=CARTESIAN_POINT('Ctrl Pts',(90.7376490447086,36.4463617499443,114.892316456339));
#47232=CARTESIAN_POINT('Ctrl Pts',(89.4682194557448,33.9187365967057,114.734367933146));
#47233=CARTESIAN_POINT('Ctrl Pts',(86.6577563313556,33.599930349796,114.576419409954));
#47234=CARTESIAN_POINT('Ctrl Pts',(84.8544211100522,35.7789949372344,114.418470886761));
#47235=CARTESIAN_POINT('Ctrl Pts',(85.6932429910294,38.4802387708443,114.260522363569));
#47236=CARTESIAN_POINT('Ctrl Pts',(88.4136876864191,39.2545262213089,114.102573840377));
#47237=CARTESIAN_POINT('Ctrl Pts',(90.5492107294969,37.3998344061804,113.944625317184));
#47238=CARTESIAN_POINT('Ctrl Pts',(90.1635983261015,34.597755986334,113.786676793992));
#47239=CARTESIAN_POINT('Ctrl Pts',(87.6064735145206,33.3888502436817,113.628728270799));
#47240=CARTESIAN_POINT('Ctrl Pts',(85.1963035899787,34.8691952478801,113.470779747607));
#47241=CARTESIAN_POINT('Ctrl Pts',(85.1183163210536,37.6966072062807,113.312831224414));
#47242=CARTESIAN_POINT('Ctrl Pts',(87.4432203926037,39.3075576880492,113.154882701222));
#47243=CARTESIAN_POINT('Ctrl Pts',(90.0630959917161,38.2414468862103,112.996934178029));
#47244=CARTESIAN_POINT('Ctrl Pts',(90.6025815925894,35.4648850404968,112.838985654837));
#47245=CARTESIAN_POINT('Ctrl Pts',(88.5725420086254,33.4952963311062,112.681037131644));
#47246=CARTESIAN_POINT('Ctrl Pts',(85.8135523897406,34.1184469385098,112.523088608452));
#47247=CARTESIAN_POINT('Ctrl Pts',(84.8271047125021,36.769345159244,112.365140085259));
#47248=CARTESIAN_POINT('Ctrl Pts',(86.5075810844117,39.0445021999939,112.207191562067));
#47249=CARTESIAN_POINT('Ctrl Pts',(89.3313446884382,38.8811023676852,112.049243038875));
#47250=CARTESIAN_POINT('Ctrl Pts',(90.7381749456975,36.4272953206904,111.891294515682));
#47251=CARTESIAN_POINT('Ctrl Pts',(89.4525416487424,33.9078732793532,111.73334599249));
#47252=CARTESIAN_POINT('Ctrl Pts',(86.6400894071501,33.6071195837937,111.575397469297));
#47253=CARTESIAN_POINT('Ctrl Pts',(84.8507831315093,35.7977184627708,111.417448946105));
#47254=CARTESIAN_POINT('Ctrl Pts',(85.7069324026425,38.4935205367586,111.259500422912));
#47255=CARTESIAN_POINT('Ctrl Pts',(88.4322927150377,39.2503240544078,111.10155189972));
#47256=CARTESIAN_POINT('Ctrl Pts',(90.5558627614894,37.3819582833603,110.943603376527));
#47257=CARTESIAN_POINT('Ctrl Pts',(90.1522661664334,34.5824136445391,110.785654853335));
#47258=CARTESIAN_POINT('Ctrl Pts',(87.5874316875858,33.3899521174758,110.627706330142));
#47259=CARTESIAN_POINT('Ctrl Pts',(85.1868167413855,34.8857423020643,110.46975780695));
#47260=CARTESIAN_POINT('Ctrl Pts',(85.1269858873624,37.7135967295509,110.311809283757));
#47261=CARTESIAN_POINT('Ctrl Pts',(87.4621859428045,39.3095857974618,110.153860760565));
#47262=CARTESIAN_POINT('Ctrl Pts',(90.0751620360126,38.226674754396,109.995912237372));
#47263=CARTESIAN_POINT('Ctrl Pts',(90.5968082201978,35.4467061147194,109.83796371418));
#47264=CARTESIAN_POINT('Ctrl Pts',(88.5541637512274,33.4901928809749,109.680015190988));
#47265=CARTESIAN_POINT('Ctrl Pts',(85.7992322738601,34.131046126596,109.522066667795));
#47266=CARTESIAN_POINT('Ctrl Pts',(84.829826311594,36.7882236446833,109.364118144603));
#47267=CARTESIAN_POINT('Ctrl Pts',(86.5248768898034,39.0525435169123,109.20616962141));
#47268=CARTESIAN_POINT('Ctrl Pts',(89.3475329498274,38.8710155284806,109.048221098218));
#47269=CARTESIAN_POINT('Ctrl Pts',(90.7385786076185,36.4082261055872,108.890272575025));
#47270=CARTESIAN_POINT('Ctrl Pts',(89.4367940058201,33.8971104460649,108.732324051833));
#47271=CARTESIAN_POINT('Ctrl Pts',(86.6224698437883,33.6144229461006,108.57437552864));
#47272=CARTESIAN_POINT('Ctrl Pts',(84.8472637351372,35.8164632397989,108.416427005448));
#47273=CARTESIAN_POINT('Ctrl Pts',(85.7207103448185,38.5067176709154,108.258478482255));
#47274=CARTESIAN_POINT('Ctrl Pts',(88.4508631164072,39.2459952267107,108.100529959063));
#47275=CARTESIAN_POINT('Ctrl Pts',(90.5624148093091,37.3640547991069,107.94258143587));
#47276=CARTESIAN_POINT('Ctrl Pts',(90.1408050081674,34.5671135666176,107.784632912678));
#47277=CARTESIAN_POINT('Ctrl Pts',(87.568460510638,33.391239618368,107.626684389485));
#47278=CARTESIAN_POINT('Ctrl Pts',(85.1773063842678,34.9022195676905,107.468735866293));
#47279=CARTESIAN_POINT('Ctrl Pts',(85.1360316483359,37.7307984124518,107.3107873431));
#47280=CARTESIAN_POINT('Ctrl Pts',(87.4806142050603,39.310940705901,107.152838819908));
#47281=CARTESIAN_POINT('Ctrl Pts',(90.08826408482,38.2129733303543,106.994890296716));
#47282=CARTESIAN_POINT('Ctrl Pts',(90.5885429349443,35.4262486362238,106.836941773523));
#47283=CARTESIAN_POINT('Ctrl Pts',(89.223305985034,34.1379297320139,106.731642758061));
#47284=CARTESIAN_POINT('Ctrl Pts',(88.4187555865468,33.9228392726483,106.678993250331));
#47285=CARTESIAN_POINT('Ctrl Pts',(89.8228871389145,38.1113513959102,122.10700224989));
#47286=CARTESIAN_POINT('Ctrl Pts',(90.4039242511275,37.4317649329314,122.054352742159));
#47287=CARTESIAN_POINT('Ctrl Pts',(90.8283653107815,35.4616404682428,121.949053726697));
#47288=CARTESIAN_POINT('Ctrl Pts',(88.6910094713799,33.3002686173985,121.791105203505));
#47289=CARTESIAN_POINT('Ctrl Pts',(85.716117428823,33.9146401598327,121.633156680312));
#47290=CARTESIAN_POINT('Ctrl Pts',(84.6026500819859,36.7385424077339,121.47520815712));
#47291=CARTESIAN_POINT('Ctrl Pts',(86.3593457928718,39.2160851732247,121.317259633928));
#47292=CARTESIAN_POINT('Ctrl Pts',(89.3938589488496,39.0987951683745,121.159311110735));
#47293=CARTESIAN_POINT('Ctrl Pts',(90.9546958650639,36.4940661464342,121.001362587542));
#47294=CARTESIAN_POINT('Ctrl Pts',(89.6267869802113,33.7630159767488,120.84341406435));
#47295=CARTESIAN_POINT('Ctrl Pts',(86.6140612888339,33.3820530954764,120.685465541158));
#47296=CARTESIAN_POINT('Ctrl Pts',(84.6480877203801,35.6964642338475,120.527517017965));
#47297=CARTESIAN_POINT('Ctrl Pts',(85.5113439365442,38.6079018993285,120.369568494773));
#47298=CARTESIAN_POINT('Ctrl Pts',(88.4211470222998,39.4766255696957,120.21161997158));
#47299=CARTESIAN_POINT('Ctrl Pts',(90.7392644690901,37.5150037893038,120.053671448388));
#47300=CARTESIAN_POINT('Ctrl Pts',(90.363930929272,34.5015726203033,119.895722925195));
#47301=CARTESIAN_POINT('Ctrl Pts',(87.6354493057437,33.1685217341956,119.737774402003));
#47302=CARTESIAN_POINT('Ctrl Pts',(85.0276511964266,34.7244862318098,119.57982587881));
#47303=CARTESIAN_POINT('Ctrl Pts',(84.904947692044,37.758721201016,119.421877355618));
#47304=CARTESIAN_POINT('Ctrl Pts',(87.3785903973958,39.5201777003541,119.263928832425));
#47305=CARTESIAN_POINT('Ctrl Pts',(90.2058026703201,38.4117968774317,119.105980309233));
#47306=CARTESIAN_POINT('Ctrl Pts',(90.8232371450967,35.4385138254036,118.94803178604));
#47307=CARTESIAN_POINT('Ctrl Pts',(88.6710847539095,33.2961139025523,118.790083262848));
#47308=CARTESIAN_POINT('Ctrl Pts',(85.7006366189604,33.9270459397144,118.632134739656));
#47309=CARTESIAN_POINT('Ctrl Pts',(84.6051077202304,36.759263057967,118.474186216463));
#47310=CARTESIAN_POINT('Ctrl Pts',(86.3777807921075,39.224880129201,118.316237693271));
#47311=CARTESIAN_POINT('Ctrl Pts',(89.4114270732902,39.0883971457029,118.158289170078));
#47312=CARTESIAN_POINT('Ctrl Pts',(90.9555317450275,36.4735590764911,118.000340646886));
#47313=CARTESIAN_POINT('Ctrl Pts',(89.6101020631707,33.7511600727872,117.842392123693));
#47314=CARTESIAN_POINT('Ctrl Pts',(86.5949982009164,33.3895165129485,117.684443600501));
#47315=CARTESIAN_POINT('Ctrl Pts',(84.6439231299071,35.7165196139242,117.526495077308));
#47316=CARTESIAN_POINT('Ctrl Pts',(85.5258572777729,38.6223464365941,117.368546554116));
#47317=CARTESIAN_POINT('Ctrl Pts',(88.4411777754528,39.4723721776031,117.210598030923));
#47318=CARTESIAN_POINT('Ctrl Pts',(90.746652193168,37.4959043499272,117.052649507731));
#47319=CARTESIAN_POINT('Ctrl Pts',(90.3519769942099,34.4849462213759,116.894700984538));
#47320=CARTESIAN_POINT('Ctrl Pts',(87.6149921779705,33.1694419529511,116.736752461346));
#47321=CARTESIAN_POINT('Ctrl Pts',(85.0172386357038,34.7421192555815,116.578803938153));
#47322=CARTESIAN_POINT('Ctrl Pts',(84.9140204970802,37.7770794497893,116.420855414961));
#47323=CARTESIAN_POINT('Ctrl Pts',(87.3989225091523,39.5226164316286,116.262906891769));
#47324=CARTESIAN_POINT('Ctrl Pts',(90.2189595924524,38.3961049077729,116.104958368576));
#47325=CARTESIAN_POINT('Ctrl Pts',(90.8172898911033,35.4189186156031,115.947009845384));
#47326=CARTESIAN_POINT('Ctrl Pts',(88.6514255207118,33.2903818192015,115.789061322191));
#47327=CARTESIAN_POINT('Ctrl Pts',(85.6850898341244,33.9403740953451,115.631112798999));
#47328=CARTESIAN_POINT('Ctrl Pts',(84.6077691813485,36.7795672158759,115.473164275806));
#47329=CARTESIAN_POINT('Ctrl Pts',(86.3962374330291,39.2337511285642,115.315215752614));
#47330=CARTESIAN_POINT('Ctrl Pts',(89.4289448191708,39.077791920405,115.157267229421));
#47331=CARTESIAN_POINT('Ctrl Pts',(90.9562277883844,36.4530930621514,114.999318706229));
#47332=CARTESIAN_POINT('Ctrl Pts',(89.5933453226959,33.7393891819747,114.841370183036));
#47333=CARTESIAN_POINT('Ctrl Pts',(86.5759815035485,33.3971130544583,114.683421659844));
#47334=CARTESIAN_POINT('Ctrl Pts',(84.6398883367908,35.7365960345636,114.525473136651));
#47335=CARTESIAN_POINT('Ctrl Pts',(85.5404626131103,38.6367000563875,114.367524613459));
#47336=CARTESIAN_POINT('Ctrl Pts',(88.4611810258964,39.4679890060191,114.209576090266));
#47337=CARTESIAN_POINT('Ctrl Pts',(90.7539170199113,37.4767584753379,114.051627567074));
#47338=CARTESIAN_POINT('Ctrl Pts',(90.3399165997945,34.4683966259736,113.893679043881));
#47339=CARTESIAN_POINT('Ctrl Pts',(87.5945413552127,33.170493651555,113.735730520689));
#47340=CARTESIAN_POINT('Ctrl Pts',(85.0069395236142,34.7598187050529,113.577781997496));
#47341=CARTESIAN_POINT('Ctrl Pts',(84.9232109873573,37.7953790975972,113.419833474304));
#47342=CARTESIAN_POINT('Ctrl Pts',(87.4192698637778,39.5249245436641,113.261884951112));
#47343=CARTESIAN_POINT('Ctrl Pts',(90.2320154838242,38.3803287890515,113.103936427919));
#47344=CARTESIAN_POINT('Ctrl Pts',(90.8112169395917,35.3993619931605,112.945987904727));
#47345=CARTESIAN_POINT('Ctrl Pts',(88.6317298867517,33.2847760878186,112.788039381534));
#47346=CARTESIAN_POINT('Ctrl Pts',(85.669628950012,33.9538018011761,112.630090858342));
#47347=CARTESIAN_POINT('Ctrl Pts',(84.6105609604868,36.7998538664292,112.472142335149));
#47348=CARTESIAN_POINT('Ctrl Pts',(86.4147506541817,39.2425034347734,112.314193811957));
#47349=CARTESIAN_POINT('Ctrl Pts',(89.4463941077727,39.0670744324199,112.156245288764));
#47350=CARTESIAN_POINT('Ctrl Pts',(90.9567924051563,36.43262300037,111.998296765572));
#47351=CARTESIAN_POINT('Ctrl Pts',(89.5765133467833,33.7277261288462,111.840348242379));
#47352=CARTESIAN_POINT('Ctrl Pts',(86.5570139755884,33.4048315455369,111.682399719187));
#47353=CARTESIAN_POINT('Ctrl Pts',(84.6359825375168,35.7566979487393,111.524451195994));
#47354=CARTESIAN_POINT('Ctrl Pts',(85.5551598119273,38.6509595994417,111.366502672802));
#47355=CARTESIAN_POINT('Ctrl Pts',(88.4811557196474,39.4634774839645,111.208554149609));
#47356=CARTESIAN_POINT('Ctrl Pts',(90.7610587612434,37.4575663479778,111.050605626417));
#47357=CARTESIAN_POINT('Ctrl Pts',(90.3277501891135,34.4519248115488,110.892657103225));
#47358=CARTESIAN_POINT('Ctrl Pts',(87.574097706924,33.171676643102,110.734708580032));
#47359=CARTESIAN_POINT('Ctrl Pts',(84.9967542721322,34.7775839203925,110.57676005684));
#47360=CARTESIAN_POINT('Ctrl Pts',(84.9325187898617,37.8136193557152,110.418811533647));
#47361=CARTESIAN_POINT('Ctrl Pts',(87.4396316199912,39.5271019584502,110.260863010455));
#47362=CARTESIAN_POINT('Ctrl Pts',(90.244969806258,38.3644691623298,110.102914487262));
#47363=CARTESIAN_POINT('Ctrl Pts',(90.8050185430291,35.3798447710928,109.94496596407));
#47364=CARTESIAN_POINT('Ctrl Pts',(88.6119986586669,33.2792969318584,109.787017440877));
#47365=CARTESIAN_POINT('Ctrl Pts',(85.6542546157362,33.9673285163827,109.629068917685));
#47366=CARTESIAN_POINT('Ctrl Pts',(84.6134829182805,36.820122148347,109.471120394492));
#47367=CARTESIAN_POINT('Ctrl Pts',(86.4333197423005,39.2511367374193,109.3131718713));
#47368=CARTESIAN_POINT('Ctrl Pts',(89.4637741167068,39.0562450202134,109.155223348107));
#47369=CARTESIAN_POINT('Ctrl Pts',(90.9572257838634,36.4121499476504,108.997274824915));
#47370=CARTESIAN_POINT('Ctrl Pts',(89.5596063937697,33.7161709572185,108.839326301722));
#47371=CARTESIAN_POINT('Ctrl Pts',(86.5380972950825,33.4126725668232,108.68137777853));
#47372=CARTESIAN_POINT('Ctrl Pts',(84.6322040501972,35.7768226788991,108.523429255338));
#47373=CARTESIAN_POINT('Ctrl Pts',(85.5699520587506,38.6651282803169,108.365480732145));
#47374=CARTESIAN_POINT('Ctrl Pts',(88.5010932369602,39.4588299765984,108.207532208953));
#47375=CARTESIAN_POINT('Ctrl Pts',(90.7680931577672,37.4383448448904,108.04958368576));
#47376=CARTESIAN_POINT('Ctrl Pts',(90.3154452832148,34.4354983723793,107.891635162568));
#47377=CARTESIAN_POINT('Ctrl Pts',(87.5537299097335,33.1730589272443,107.733686639375));
#47378=CARTESIAN_POINT('Ctrl Pts',(84.986543781475,34.7952742094795,107.575738116183));
#47379=CARTESIAN_POINT('Ctrl Pts',(84.9422304817326,37.8320873922332,107.41778959299));
#47380=CARTESIAN_POINT('Ctrl Pts',(87.4594165341921,39.5285566125487,107.259841069798));
#47381=CARTESIAN_POINT('Ctrl Pts',(90.2590364017897,38.3497590667532,107.101892546605));
#47382=CARTESIAN_POINT('Ctrl Pts',(90.7961447839457,35.3578812537963,106.943944023413));
#47383=CARTESIAN_POINT('Ctrl Pts',(89.3304018103147,33.9747188791143,106.838645007951));
#47384=CARTESIAN_POINT('Ctrl Pts',(88.4666220147327,33.7437938887448,106.78599550022));
#47385=CARTESIAN_POINT('Ctrl Pts',(89.9637526925915,38.2317895137621,122.21400449978));
#47386=CARTESIAN_POINT('Ctrl Pts',(90.5846315306959,37.505603794026,122.161354992049));
#47387=CARTESIAN_POINT('Ctrl Pts',(91.0381765219239,35.4003878571334,122.056055976587));
#47388=CARTESIAN_POINT('Ctrl Pts',(88.7542621517574,33.0908106971605,121.898107453395));
#47389=CARTESIAN_POINT('Ctrl Pts',(85.5753817049752,33.7473097080035,121.740158930202));
#47390=CARTESIAN_POINT('Ctrl Pts',(84.3855638808806,36.7648469870243,121.58221040701));
#47391=CARTESIAN_POINT('Ctrl Pts',(86.2627162502425,39.4122749073048,121.424261883817));
#47392=CARTESIAN_POINT('Ctrl Pts',(89.5053060313328,39.28694232458,121.266313360625));
#47393=CARTESIAN_POINT('Ctrl Pts',(91.1731695647284,36.5036069838139,121.108364837432));
#47394=CARTESIAN_POINT('Ctrl Pts',(89.7542059422574,33.5852886517871,120.95041631424));
#47395=CARTESIAN_POINT('Ctrl Pts',(86.5348975926318,33.1782031384635,120.792467791047));
#47396=CARTESIAN_POINT('Ctrl Pts',(84.434117179008,35.6513134928344,120.634519267855));
#47397=CARTESIAN_POINT('Ctrl Pts',(85.3565668904165,38.7623884946917,120.476570744662));
#47398=CARTESIAN_POINT('Ctrl Pts',(88.4658952293851,39.6906805637423,120.31862222147));
#47399=CARTESIAN_POINT('Ctrl Pts',(90.9429660338145,37.5945503403711,120.160673698278));
#47400=CARTESIAN_POINT('Ctrl Pts',(90.5418958659962,34.3744881385083,120.002725175085));
#47401=CARTESIAN_POINT('Ctrl Pts',(87.6263222053857,32.9500299276578,119.844776651893));
#47402=CARTESIAN_POINT('Ctrl Pts',(84.8397073298627,34.6126869406169,119.6868281287));
#47403=CARTESIAN_POINT('Ctrl Pts',(84.7085900438391,37.8549794596632,119.528879605508));
#47404=CARTESIAN_POINT('Ctrl Pts',(87.3518504767824,39.7372190648325,119.370931082315));
#47405=CARTESIAN_POINT('Ctrl Pts',(90.3729247493053,38.5528365476947,119.212982559123));
#47406=CARTESIAN_POINT('Ctrl Pts',(91.0326967178202,35.3756754199526,119.05503403593));
#47407=CARTESIAN_POINT('Ctrl Pts',(88.7329711960293,33.0863710934378,118.897085512738));
#47408=CARTESIAN_POINT('Ctrl Pts',(85.5588393756842,33.7605661524489,118.739136989545));
#47409=CARTESIAN_POINT('Ctrl Pts',(84.3881900394267,36.78698845264,118.581188466353));
#47410=CARTESIAN_POINT('Ctrl Pts',(86.2824153377281,39.4216729335805,118.42323994316));
#47411=CARTESIAN_POINT('Ctrl Pts',(89.5240788024021,39.275831309295,118.265291419968));
#47412=CARTESIAN_POINT('Ctrl Pts',(91.1740627609971,36.4816937436928,118.107342896775));
#47413=CARTESIAN_POINT('Ctrl Pts',(89.7363769401363,33.5726197882643,117.949394373583));
#47414=CARTESIAN_POINT('Ctrl Pts',(86.5145273484115,33.1861783226143,117.791445850391));
#47415=CARTESIAN_POINT('Ctrl Pts',(84.4296670224867,35.6727440707063,117.633497327198));
#47416=CARTESIAN_POINT('Ctrl Pts',(85.3720754117306,38.7778234941537,117.475548804006));
#47417=CARTESIAN_POINT('Ctrl Pts',(88.4872994916648,39.6861355164726,117.317600280813));
#47418=CARTESIAN_POINT('Ctrl Pts',(90.9508603342737,37.5741412520713,117.159651757621));
#47419=CARTESIAN_POINT('Ctrl Pts',(90.5291222493784,34.3567216670886,117.001703234428));
#47420=CARTESIAN_POINT('Ctrl Pts',(87.6044623319701,32.951013245831,116.843754711236));
#47421=CARTESIAN_POINT('Ctrl Pts',(84.8285807796521,34.6315290611657,116.685806188043));
#47422=CARTESIAN_POINT('Ctrl Pts',(84.7182849712901,37.8745965339058,116.527857664851));
#47423=CARTESIAN_POINT('Ctrl Pts',(87.3735767618306,39.7398250199571,116.369909141658));
#47424=CARTESIAN_POINT('Ctrl Pts',(90.3869838418398,38.5360685793765,116.211960618466));
#47425=CARTESIAN_POINT('Ctrl Pts',(91.0263416605067,35.3547365662415,116.054012095273));
#47426=CARTESIAN_POINT('Ctrl Pts',(88.7119639288353,33.080245961022,115.896063572081));
#47427=CARTESIAN_POINT('Ctrl Pts',(85.5422265475149,33.7748082199658,115.738115048889));
#47428=CARTESIAN_POINT('Ctrl Pts',(84.3910339969842,36.8086848670448,115.580166525696));
#47429=CARTESIAN_POINT('Ctrl Pts',(86.3021375508707,39.4311522175397,115.422218002504));
#47430=CARTESIAN_POINT('Ctrl Pts',(89.5427977404525,39.2644988834957,115.264269479311));
#47431=CARTESIAN_POINT('Ctrl Pts',(91.1748065320602,36.4598243743587,115.106320956119));
#47432=CARTESIAN_POINT('Ctrl Pts',(89.7184711896471,33.5600417672437,114.948372432926));
#47433=CARTESIAN_POINT('Ctrl Pts',(86.4942066757414,33.1942957591207,114.790423909734));
#47434=CARTESIAN_POINT('Ctrl Pts',(84.4253555635294,35.6941971318927,114.632475386541));
#47435=CARTESIAN_POINT('Ctrl Pts',(85.3876822351913,38.7931613419308,114.474526863349));
#47436=CARTESIAN_POINT('Ctrl Pts',(88.5086743653739,39.6814517907293,114.316578340156));
#47437=CARTESIAN_POINT('Ctrl Pts',(90.9586233103255,37.5536825444954,114.158629816964));
#47438=CARTESIAN_POINT('Ctrl Pts',(90.5162348734876,34.3390372656131,114.000681293771));
#47439=CARTESIAN_POINT('Ctrl Pts',(87.5826091959047,32.9521370594283,113.842732770579));
#47440=CARTESIAN_POINT('Ctrl Pts',(84.8175754572497,34.6504421622257,113.684784247386));
#47441=CARTESIAN_POINT('Ctrl Pts',(84.7281056536611,37.8941509889138,113.526835724194));
#47442=CARTESIAN_POINT('Ctrl Pts',(87.3953193349517,39.7422913992789,113.368887201001));
#47443=CARTESIAN_POINT('Ctrl Pts',(90.4009349759326,38.5192106918928,113.210938677809));
#47444=CARTESIAN_POINT('Ctrl Pts',(91.0198522865937,35.3338389458242,113.052990154616));
#47445=CARTESIAN_POINT('Ctrl Pts',(88.6909177648781,33.0742558445311,112.895041631424));
#47446=CARTESIAN_POINT('Ctrl Pts',(85.5257055102833,33.7891566638425,112.737093108231));
#47447=CARTESIAN_POINT('Ctrl Pts',(84.3940172084717,36.8303625736143,112.579144585039));
#47448=CARTESIAN_POINT('Ctrl Pts',(86.3219202239515,39.440504669553,112.421196061847));
#47449=CARTESIAN_POINT('Ctrl Pts',(89.5614435271075,39.2530464971546,112.263247538654));
#47450=CARTESIAN_POINT('Ctrl Pts',(91.1754098646149,36.4379506800496,112.105299015462));
#47451=CARTESIAN_POINT('Ctrl Pts',(89.7004850448244,33.5475789783393,111.947350492269));
#47452=CARTESIAN_POINT('Ctrl Pts',(86.4739385440265,33.2025435072801,111.789401969077));
#47453=CARTESIAN_POINT('Ctrl Pts',(84.4211819435246,35.7156774347077,111.631453445884));
#47454=CARTESIAN_POINT('Ctrl Pts',(85.403387221212,38.8083986621247,111.473504922692));
#47455=CARTESIAN_POINT('Ctrl Pts',(88.5300187242571,39.6766309135212,111.315556399499));
#47456=CARTESIAN_POINT('Ctrl Pts',(90.9662547609973,37.5331744125954,111.157607876307));
#47457=CARTESIAN_POINT('Ctrl Pts',(90.5032342117935,34.3214359785583,110.999659353114));
#47458=CARTESIAN_POINT('Ctrl Pts',(87.5607637262621,32.9534011687283,110.841710829922));
#47459=CARTESIAN_POINT('Ctrl Pts',(84.8066918028788,34.6694255387206,110.683762306729));
#47460=CARTESIAN_POINT('Ctrl Pts',(84.7380516923612,37.9136419818796,110.525813783537));
#47461=CARTESIAN_POINT('Ctrl Pts',(87.417077297178,39.7446181194386,110.367865260344));
#47462=CARTESIAN_POINT('Ctrl Pts',(90.4147775765031,38.5022635702636,110.209916737152));
#47463=CARTESIAN_POINT('Ctrl Pts',(91.0132288658605,35.3129834274662,110.051968213959));
#47464=CARTESIAN_POINT('Ctrl Pts',(88.6698335661064,33.0684009827419,109.894019690767));
#47465=CARTESIAN_POINT('Ctrl Pts',(85.5092769576124,33.8036109061693,109.736071167575));
#47466=CARTESIAN_POINT('Ctrl Pts',(84.3971395249671,36.8520206520106,109.578122644382));
#47467=CARTESIAN_POINT('Ctrl Pts',(86.3417625947976,39.4497299579264,109.42017412119));
#47468=CARTESIAN_POINT('Ctrl Pts',(89.5800152835865,39.241474511946,109.262225597997));
#47469=CARTESIAN_POINT('Ctrl Pts',(91.1758729601082,36.4160737897136,109.104277074805));
#47470=CARTESIAN_POINT('Ctrl Pts',(89.6824187817193,33.5352314683722,108.946328551612));
#47471=CARTESIAN_POINT('Ctrl Pts',(86.4537247463768,33.2109221875459,108.78838002842));
#47472=CARTESIAN_POINT('Ctrl Pts',(84.4171443652571,35.7371821179993,108.630431505227));
#47473=CARTESIAN_POINT('Ctrl Pts',(85.4191937726829,38.8235388897184,108.472482982035));
#47474=CARTESIAN_POINT('Ctrl Pts',(88.5513233575131,39.6716647264861,108.314534458842));
#47475=CARTESIAN_POINT('Ctrl Pts',(90.9737715062253,37.5126348906738,108.15658593565));
#47476=CARTESIAN_POINT('Ctrl Pts',(90.4900855582621,34.303883178141,107.998637412457));
#47477=CARTESIAN_POINT('Ctrl Pts',(87.538999308829,32.9548782361206,107.840688889265));
#47478=CARTESIAN_POINT('Ctrl Pts',(84.7957811786821,34.6883288512686,107.682740366072));
#47479=CARTESIAN_POINT('Ctrl Pts',(84.7484293151293,37.9333763720146,107.52479184288));
#47480=CARTESIAN_POINT('Ctrl Pts',(87.4382188633238,39.7461725191965,107.366843319687));
#47481=CARTESIAN_POINT('Ctrl Pts',(90.4298087187594,38.4865448031522,107.208894796495));
#47482=CARTESIAN_POINT('Ctrl Pts',(91.0037466329471,35.2895138713688,107.050946273303));
#47483=CARTESIAN_POINT('Ctrl Pts',(89.4374976355954,33.8115080262147,106.945647257841));
#47484=CARTESIAN_POINT('Ctrl Pts',(88.5144884429186,33.5647485048412,106.89299775011));
#47485=CARTESIAN_POINT('Ctrl Pts',(90.1046182462686,38.352227631614,122.321006749669));
#47486=CARTESIAN_POINT('Ctrl Pts',(90.7653388102644,37.5794426551206,122.268357241939));
#47487=CARTESIAN_POINT('Ctrl Pts',(91.2479877330663,35.3391352460239,122.163058226477));
#47488=CARTESIAN_POINT('Ctrl Pts',(88.8175148321351,32.8813527769224,122.005109703284));
#47489=CARTESIAN_POINT('Ctrl Pts',(85.4346459811273,33.5799792561743,121.847161180092));
#47490=CARTESIAN_POINT('Ctrl Pts',(84.1684776797754,36.7911515663147,121.6892126569));
#47491=CARTESIAN_POINT('Ctrl Pts',(86.1660867076132,39.608464641385,121.531264133707));
#47492=CARTESIAN_POINT('Ctrl Pts',(89.6167531138159,39.4750894807855,121.373315610515));
#47493=CARTESIAN_POINT('Ctrl Pts',(91.3916432643928,36.5131478211936,121.215367087322));
#47494=CARTESIAN_POINT('Ctrl Pts',(89.8816249043036,33.4075613268254,121.05741856413));
#47495=CARTESIAN_POINT('Ctrl Pts',(86.4557338964297,32.9743531814506,120.899470040937));
#47496=CARTESIAN_POINT('Ctrl Pts',(84.220146637636,35.6061627518213,120.741521517745));
#47497=CARTESIAN_POINT('Ctrl Pts',(85.2017898442886,38.9168750900549,120.583572994552));
#47498=CARTESIAN_POINT('Ctrl Pts',(88.5106434364707,39.9047355577889,120.42562447136));
#47499=CARTESIAN_POINT('Ctrl Pts',(91.146667598539,37.6740968914383,120.267675948167));
#47500=CARTESIAN_POINT('Ctrl Pts',(90.7198608027206,34.2474036567132,120.109727424975));
#47501=CARTESIAN_POINT('Ctrl Pts',(87.6171951050278,32.7315381211201,119.951778901782));
#47502=CARTESIAN_POINT('Ctrl Pts',(84.6517634632988,34.5008876494239,119.79383037859));
#47503=CARTESIAN_POINT('Ctrl Pts',(84.5122323956342,37.9512377183104,119.635881855397));
#47504=CARTESIAN_POINT('Ctrl Pts',(87.325110556169,39.9542604293109,119.477933332205));
#47505=CARTESIAN_POINT('Ctrl Pts',(90.5400468282905,38.6938762179578,119.319984809012));
#47506=CARTESIAN_POINT('Ctrl Pts',(91.2421562905436,35.3128370145015,119.16203628582));
#47507=CARTESIAN_POINT('Ctrl Pts',(88.7948576381488,32.8766282843233,119.004087762628));
#47508=CARTESIAN_POINT('Ctrl Pts',(85.4170421324083,33.5940863651833,118.846139239435));
#47509=CARTESIAN_POINT('Ctrl Pts',(84.1712723586227,36.814713847313,118.688190716243));
#47510=CARTESIAN_POINT('Ctrl Pts',(86.1870498833489,39.6184657379601,118.53024219305));
#47511=CARTESIAN_POINT('Ctrl Pts',(89.6367305315139,39.4632654728871,118.372293669858));
#47512=CARTESIAN_POINT('Ctrl Pts',(91.3925937769666,36.4898284108945,118.214345146665));
#47513=CARTESIAN_POINT('Ctrl Pts',(89.8626518171021,33.3940795037413,118.056396623473));
#47514=CARTESIAN_POINT('Ctrl Pts',(86.4340564959065,32.9828401322801,117.89844810028));
#47515=CARTESIAN_POINT('Ctrl Pts',(84.2154109150663,35.6289685274884,117.740499577088));
#47516=CARTESIAN_POINT('Ctrl Pts',(85.2182935456883,38.9333005517133,117.582551053896));
#47517=CARTESIAN_POINT('Ctrl Pts',(88.5334212078769,39.8998988553421,117.424602530703));
#47518=CARTESIAN_POINT('Ctrl Pts',(91.1550684753794,37.6523781542154,117.266654007511));
#47519=CARTESIAN_POINT('Ctrl Pts',(90.7062675045469,34.2284971128012,117.108705484318));
#47520=CARTESIAN_POINT('Ctrl Pts',(87.5939324859696,32.7325845387109,116.950756961126));
#47521=CARTESIAN_POINT('Ctrl Pts',(84.6399229236004,34.5209388667498,116.792808437933));
#47522=CARTESIAN_POINT('Ctrl Pts',(84.5225494454999,37.9721136180223,116.634859914741));
#47523=CARTESIAN_POINT('Ctrl Pts',(87.3482310145089,39.9570336082856,116.476911391548));
#47524=CARTESIAN_POINT('Ctrl Pts',(90.5550080912271,38.6760322509801,116.318962868356));
#47525=CARTESIAN_POINT('Ctrl Pts',(91.2353934299102,35.2905545168799,116.161014345163));
#47526=CARTESIAN_POINT('Ctrl Pts',(88.7725023369588,32.8701101028426,116.003065821971));
#47527=CARTESIAN_POINT('Ctrl Pts',(85.3993632609055,33.6092423445867,115.845117298778));
#47528=CARTESIAN_POINT('Ctrl Pts',(84.1742988126201,36.8378025182137,115.687168775586));
#47529=CARTESIAN_POINT('Ctrl Pts',(86.2080376687123,39.6285533065152,115.529220252393));
#47530=CARTESIAN_POINT('Ctrl Pts',(89.6566506617342,39.4512058465864,115.371271729201));
#47531=CARTESIAN_POINT('Ctrl Pts',(91.3933852757362,36.4665556865659,115.213323206008));
#47532=CARTESIAN_POINT('Ctrl Pts',(89.843597056598,33.3806943525127,115.055374682816));
#47533=CARTESIAN_POINT('Ctrl Pts',(86.4124318479345,32.9914784637831,114.897426159623));
#47534=CARTESIAN_POINT('Ctrl Pts',(84.2108227902679,35.6517982292218,114.739477636431));
#47535=CARTESIAN_POINT('Ctrl Pts',(85.2349018572721,38.949622627474,114.581529113238));
#47536=CARTESIAN_POINT('Ctrl Pts',(88.5561677048511,39.8949145754395,114.423580590046));
#47537=CARTESIAN_POINT('Ctrl Pts',(91.1633296007399,37.630606613653,114.265632066854));
#47538=CARTESIAN_POINT('Ctrl Pts',(90.6925531471805,34.2096779052527,114.107683543661));
#47539=CARTESIAN_POINT('Ctrl Pts',(87.5706770365969,32.7337804673015,113.949735020469));
#47540=CARTESIAN_POINT('Ctrl Pts',(84.6282113908853,34.5410656193985,113.791786497276));
#47541=CARTESIAN_POINT('Ctrl Pts',(84.5330003199649,37.9929228802303,113.633837974084));
#47542=CARTESIAN_POINT('Ctrl Pts',(87.3713688061258,39.9596582548938,113.475889450891));
#47543=CARTESIAN_POINT('Ctrl Pts',(90.5698544680408,38.6580925947341,113.317940927699));
#47544=CARTESIAN_POINT('Ctrl Pts',(91.2284876335959,35.2683158984878,113.159992404506));
#47545=CARTESIAN_POINT('Ctrl Pts',(88.7501056430045,32.8637356012436,113.002043881314));
#47546=CARTESIAN_POINT('Ctrl Pts',(85.3817820705547,33.6245115265088,112.844095358121));
#47547=CARTESIAN_POINT('Ctrl Pts',(84.1774734564564,36.8608712807994,112.686146834929));
#47548=CARTESIAN_POINT('Ctrl Pts',(86.2290897937213,39.6385059043325,112.528198311736));
#47549=CARTESIAN_POINT('Ctrl Pts',(89.6764929464422,39.4390185618894,112.370249788544));
#47550=CARTESIAN_POINT('Ctrl Pts',(91.3940273240736,36.4432783597291,112.212301265351));
#47551=CARTESIAN_POINT('Ctrl Pts',(89.8244567428654,33.3674318278324,112.054352742159));
#47552=CARTESIAN_POINT('Ctrl Pts',(86.3908631124647,33.0002554690232,111.896404218966));
#47553=CARTESIAN_POINT('Ctrl Pts',(84.2063813495323,35.6746569206761,111.738455695774));
#47554=CARTESIAN_POINT('Ctrl Pts',(85.2516146304968,38.9658377248078,111.580507172581));
#47555=CARTESIAN_POINT('Ctrl Pts',(88.5788817288668,39.8897843430778,111.422558649389));
#47556=CARTESIAN_POINT('Ctrl Pts',(91.1714507607514,37.608782477213,111.264610126197));
#47557=CARTESIAN_POINT('Ctrl Pts',(90.6787182344735,34.1909471455679,111.106661603004));
#47558=CARTESIAN_POINT('Ctrl Pts',(87.5474297456003,32.7351256943546,110.948713079812));
#47559=CARTESIAN_POINT('Ctrl Pts',(84.6166293336255,34.5612671570488,110.790764556619));
#47560=CARTESIAN_POINT('Ctrl Pts',(84.5435845948607,38.0136646080439,110.632816033427));
#47561=CARTESIAN_POINT('Ctrl Pts',(87.3945229743647,39.962134280427,110.474867510234));
#47562=CARTESIAN_POINT('Ctrl Pts',(90.5845853467483,38.6400579781975,110.316918987042));
#47563=CARTESIAN_POINT('Ctrl Pts',(91.2214391886919,35.2461220838395,110.158970463849));
#47564=CARTESIAN_POINT('Ctrl Pts',(88.7276684735458,32.8575050336255,110.001021940657));
#47565=CARTESIAN_POINT('Ctrl Pts',(85.3642992994886,33.6398932959559,109.843073417464));
#47566=CARTESIAN_POINT('Ctrl Pts',(84.1807961316536,36.8839191556743,109.685124894272));
#47567=CARTESIAN_POINT('Ctrl Pts',(86.2502054472947,39.6483231784334,109.527176371079));
#47568=CARTESIAN_POINT('Ctrl Pts',(89.696256450466,39.4267040036787,109.369227847887));
#47569=CARTESIAN_POINT('Ctrl Pts',(91.3945201363532,36.4199976317768,109.211279324695));
#47570=CARTESIAN_POINT('Ctrl Pts',(89.805231169669,33.3542919795258,109.053330801502));
#47571=CARTESIAN_POINT('Ctrl Pts',(86.3693521976711,33.0091718082685,108.89538227831));
#47572=CARTESIAN_POINT('Ctrl Pts',(84.202084680317,35.6975415570995,108.737433755117));
#47573=CARTESIAN_POINT('Ctrl Pts',(85.268435486615,38.9819494991199,108.579485231925));
#47574=CARTESIAN_POINT('Ctrl Pts',(88.6015534780661,39.8844994763739,108.421536708732));
#47575=CARTESIAN_POINT('Ctrl Pts',(91.1794498546833,37.5869249364573,108.26358818554));
#47576=CARTESIAN_POINT('Ctrl Pts',(90.6647258333095,34.1722679839027,108.105639662347));
#47577=CARTESIAN_POINT('Ctrl Pts',(87.5242687079243,32.736697544997,107.947691139155));
#47578=CARTESIAN_POINT('Ctrl Pts',(84.6050185758893,34.5813834930577,107.789742615962));
#47579=CARTESIAN_POINT('Ctrl Pts',(84.5546281485259,38.034665351796,107.63179409277));
#47580=CARTESIAN_POINT('Ctrl Pts',(87.4170211924556,39.9637884258442,107.473845569577));
#47581=CARTESIAN_POINT('Ctrl Pts',(90.6005810357291,38.6233305395511,107.315897046385));
#47582=CARTESIAN_POINT('Ctrl Pts',(91.2113484819485,35.2211464889414,107.157948523192));
#47583=CARTESIAN_POINT('Ctrl Pts',(89.5445934608762,33.6482971733151,107.052649507731));
#47584=CARTESIAN_POINT('Ctrl Pts',(88.5623548711045,33.3857031209377,107.));
#47585=CARTESIAN_POINT('Ctrl Pts',(89.6820215852375,37.9909132780583,122.));
#47586=CARTESIAN_POINT('Ctrl Pts',(89.7436297460741,37.9330167349015,122.));
#47587=CARTESIAN_POINT('Ctrl Pts',(89.8018687515423,37.8719694294382,122.));
#47588=CARTESIAN_POINT('Ctrl Pts',(89.8567409894119,37.8081561811477,122.));
#47589=CARTESIAN_POINT('Ctrl Pts',(89.9130661596494,37.7426532563005,122.));
#47590=CARTESIAN_POINT('Ctrl Pts',(89.9658443450239,37.6742355418645,122.));
#47591=CARTESIAN_POINT('Ctrl Pts',(90.0150526202045,37.603270691292,122.));
#47592=CARTESIAN_POINT('Ctrl Pts',(90.0656105084705,37.5303595198906,122.));
#47593=CARTESIAN_POINT('Ctrl Pts',(90.11240051315,37.4547590216188,122.));
#47594=CARTESIAN_POINT('Ctrl Pts',(90.1553637025152,37.3768249585536,122.));
#47595=CARTESIAN_POINT('Ctrl Pts',(90.1742736966932,37.3425227407573,122.));
#47596=CARTESIAN_POINT('Ctrl Pts',(90.1924418495419,37.307767950786,122.));
#47597=CARTESIAN_POINT('Ctrl Pts',(90.2098607109953,37.2725888463926,122.));
#47598=CARTESIAN_POINT('Ctrl Pts',(90.2197915565536,37.2525325267792,122.));
#47599=CARTESIAN_POINT('Ctrl Pts',(90.2294788262591,37.2323382684758,122.));
#47600=CARTESIAN_POINT('Ctrl Pts',(90.2389209052051,37.2120111595686,122.));
#47601=CARTESIAN_POINT('Ctrl Pts',(90.2474264863267,37.1937001631485,122.));
#47602=CARTESIAN_POINT('Ctrl Pts',(90.2557354768874,37.1752756345613,122.));
#47603=CARTESIAN_POINT('Ctrl Pts',(90.26383303591,37.1567730478507,122.));
#47604=CARTESIAN_POINT('Ctrl Pts',(90.3003946147543,37.0732313557234,122.));
#47605=CARTESIAN_POINT('Ctrl Pts',(90.3326960157527,36.9880061197598,122.));
#47606=CARTESIAN_POINT('Ctrl Pts',(90.3607122049495,36.9014961187041,122.));
#47607=CARTESIAN_POINT('Ctrl Pts',(90.3891914944112,36.8135561300035,122.));
#47608=CARTESIAN_POINT('Ctrl Pts',(90.4132432276989,36.7242877964807,122.));
#47609=CARTESIAN_POINT('Ctrl Pts',(90.4328020337916,36.6340728762632,122.));
#47610=CARTESIAN_POINT('Ctrl Pts',(90.4517704842742,36.5465809690975,122.));
#47611=CARTESIAN_POINT('Ctrl Pts',(90.4665132964625,36.4581978383469,122.));
#47612=CARTESIAN_POINT('Ctrl Pts',(90.4769300991962,36.369249841242,122.));
#47613=CARTESIAN_POINT('Ctrl Pts',(90.4812989257395,36.3319448849463,122.));
#47614=CARTESIAN_POINT('Ctrl Pts',(90.4849063004385,36.2945403777073,122.));
#47615=CARTESIAN_POINT('Ctrl Pts',(90.4877424838587,36.2570597773456,122.));
#47616=CARTESIAN_POINT('Ctrl Pts',(90.489521604424,36.2335484252839,122.));
#47617=CARTESIAN_POINT('Ctrl Pts',(90.4909972347691,36.210007125288,122.));
#47618=CARTESIAN_POINT('Ctrl Pts',(90.4921666748232,36.1864416347799,122.));
#47619=CARTESIAN_POINT('Ctrl Pts',(90.4928510541084,36.1726506469527,122.));
#47620=CARTESIAN_POINT('Ctrl Pts',(90.4934302788315,36.1588563208053,122.));
#47621=CARTESIAN_POINT('Ctrl Pts',(90.4939038482032,36.1450676472443,122.));
#47622=CARTESIAN_POINT('Ctrl Pts',(90.497231204613,36.0481867379194,122.));
#47623=CARTESIAN_POINT('Ctrl Pts',(90.4953526498791,35.9514708375007,122.));
#47624=CARTESIAN_POINT('Ctrl Pts',(90.4882038039179,35.8553397140996,122.));
#47625=CARTESIAN_POINT('Ctrl Pts',(90.4810549579567,35.7592085906985,122.));
#47626=CARTESIAN_POINT('Ctrl Pts',(90.4686362510781,35.6636612002769,122.));
#47627=CARTESIAN_POINT('Ctrl Pts',(90.4508308402664,35.5690985254714,122.));
#47628=CARTESIAN_POINT('Ctrl Pts',(90.4337728060187,35.4785050894403,122.));
#47629=CARTESIAN_POINT('Ctrl Pts',(90.4117709197647,35.388814468969,122.));
#47630=CARTESIAN_POINT('Ctrl Pts',(90.3850997898583,35.3002660026689,122.));
#47631=CARTESIAN_POINT('Ctrl Pts',(90.3762304376694,35.2708196486464,122.));
#47632=CARTESIAN_POINT('Ctrl Pts',(90.3668443009283,35.2414996371044,122.));
#47633=CARTESIAN_POINT('Ctrl Pts',(90.3569502297067,35.2123149441589,122.));
#47634=CARTESIAN_POINT('Ctrl Pts',(90.3476298672125,35.184822528606,122.));
#47635=CARTESIAN_POINT('Ctrl Pts',(90.3378587614969,35.1574501926698,122.));
#47636=CARTESIAN_POINT('Ctrl Pts',(90.3276438359507,35.1302055647186,122.));
#47637=CARTESIAN_POINT('Ctrl Pts',(90.3224861204142,35.1164492196299,122.));
#47638=CARTESIAN_POINT('Ctrl Pts',(90.3172183296157,35.1027337076298,122.));
#47639=CARTESIAN_POINT('Ctrl Pts',(90.3118431330481,35.0890633460052,122.));
#47640=CARTESIAN_POINT('Ctrl Pts',(90.2775918092556,35.0019543488783,122.));
#47641=CARTESIAN_POINT('Ctrl Pts',(90.2389669873983,34.9166341728923,122.));
#47642=CARTESIAN_POINT('Ctrl Pts',(90.1962986524644,34.8333372319883,122.));
#47643=CARTESIAN_POINT('Ctrl Pts',(90.1520688572906,34.7469920150849,122.));
#47644=CARTESIAN_POINT('Ctrl Pts',(90.103494057027,34.6628200939995,122.));
#47645=CARTESIAN_POINT('Ctrl Pts',(90.0508859614636,34.581086046773,122.));
#47646=CARTESIAN_POINT('Ctrl Pts',(89.9977149201083,34.498477384386,122.));
#47647=CARTESIAN_POINT('Ctrl Pts',(89.940423388037,34.4183582274894,122.));
#47648=CARTESIAN_POINT('Ctrl Pts',(89.8792816811015,34.3410171035127,122.));
#47649=CARTESIAN_POINT('Ctrl Pts',(89.8565927777255,34.3123168042104,122.));
#47650=CARTESIAN_POINT('Ctrl Pts',(89.8333732098606,34.2839992699063,122.));
#47651=CARTESIAN_POINT('Ctrl Pts',(89.8096351963912,34.2560801327903,122.));
#47652=CARTESIAN_POINT('Ctrl Pts',(89.7888795976702,34.2316687216432,122.));
#47653=CARTESIAN_POINT('Ctrl Pts',(89.7677276292938,34.2075618935548,122.));
#47654=CARTESIAN_POINT('Ctrl Pts',(89.7461869693122,34.1837704808018,122.));
#47655=CARTESIAN_POINT('Ctrl Pts',(89.734423948481,34.1707783587378,122.));
#47656=CARTESIAN_POINT('Ctrl Pts',(89.7225496929772,34.1578855474185,122.));
#47657=CARTESIAN_POINT('Ctrl Pts',(89.7105715260522,34.1450996670866,122.));
#47658=CARTESIAN_POINT('Ctrl Pts',(89.6415607698904,34.0714353680812,122.));
#47659=CARTESIAN_POINT('Ctrl Pts',(89.5690476160887,34.0012556015445,122.));
#47660=CARTESIAN_POINT('Ctrl Pts',(89.4933405847835,33.9348515807767,122.));
#47661=CARTESIAN_POINT('Ctrl Pts',(89.4311464894629,33.8803000031212,122.));
#47662=CARTESIAN_POINT('Ctrl Pts',(89.3667958219628,33.8282966578679,122.));
#47663=CARTESIAN_POINT('Ctrl Pts',(89.3004373490015,33.7790163342467,122.));
#47664=CARTESIAN_POINT('Ctrl Pts',(89.275819727738,33.7607343532348,122.));
#47665=CARTESIAN_POINT('Ctrl Pts',(89.2509256000565,33.7428272754375,122.));
#47666=CARTESIAN_POINT('Ctrl Pts',(89.2257619544786,33.7253045897815,122.));
#47667=CARTESIAN_POINT('Ctrl Pts',(89.2089511913507,33.7135984275319,122.));
#47668=CARTESIAN_POINT('Ctrl Pts',(89.1920190055838,33.7020631898191,122.));
#47669=CARTESIAN_POINT('Ctrl Pts',(89.174982541295,33.6907115289679,122.));
#47670=CARTESIAN_POINT('Ctrl Pts',(89.0900720965275,33.634134380366,122.));
#47671=CARTESIAN_POINT('Ctrl Pts',(89.0024923712921,33.5820565285997,122.));
#47672=CARTESIAN_POINT('Ctrl Pts',(88.9125337222617,33.5347858885666,122.));
#47673=CARTESIAN_POINT('Ctrl Pts',(88.8290756905137,33.4909311328633,122.));
#47674=CARTESIAN_POINT('Ctrl Pts',(88.7435693133768,33.4512136598047,122.));
#47675=CARTESIAN_POINT('Ctrl Pts',(88.6562187308696,33.4159083934617,122.));
#47676=CARTESIAN_POINT('Ctrl Pts',(88.6257885601688,33.4036091591507,122.));
#47677=CARTESIAN_POINT('Ctrl Pts',(88.5951343684732,33.3918456830543,122.));
#47678=CARTESIAN_POINT('Ctrl Pts',(88.5642690620869,33.3806142427251,122.));
#47679=CARTESIAN_POINT('Ctrl Pts',(85.2503883725927,36.3527278457068,120.387416697508));
#47680=CARTESIAN_POINT('Ctrl Pts',(85.2488060127422,36.178361411834,120.398449387697));
#47681=CARTESIAN_POINT('Ctrl Pts',(85.2653916078632,36.0042940232439,120.409482077886));
#47682=CARTESIAN_POINT('Ctrl Pts',(85.3012631691194,35.8342963759829,120.420514768075));
#47683=CARTESIAN_POINT('Ctrl Pts',(85.4724471695134,35.0230443340702,120.473164275806));
#47684=CARTESIAN_POINT('Ctrl Pts',(86.0828360772747,34.3044736932798,120.525813783537));
#47685=CARTESIAN_POINT('Ctrl Pts',(86.8557210366768,34.0043284144214,120.578463291268));
#47686=CARTESIAN_POINT('Ctrl Pts',(87.628605996079,33.704183135563,120.631112798999));
#47687=CARTESIAN_POINT('Ctrl Pts',(88.563987007122,33.8224632186368,120.683762306729));
#47688=CARTESIAN_POINT('Ctrl Pts',(89.2378198705159,34.3055669280643,120.73641181446));
#47689=CARTESIAN_POINT('Ctrl Pts',(89.9116527339098,34.7886706374918,120.789061322191));
#47690=CARTESIAN_POINT('Ctrl Pts',(90.3239374496546,35.6365979732731,120.841710829922));
#47691=CARTESIAN_POINT('Ctrl Pts',(90.2877780910216,36.4649154250162,120.894360337653));
#47692=CARTESIAN_POINT('Ctrl Pts',(90.2516187323885,37.2932328767593,120.947009845383));
#47693=CARTESIAN_POINT('Ctrl Pts',(89.7670152993775,38.1019404444642,120.999659353114));
#47694=CARTESIAN_POINT('Ctrl Pts',(89.0536408277278,38.5245021328125,121.052308860845));
#47695=CARTESIAN_POINT('Ctrl Pts',(88.3402663560781,38.9470638211609,121.104958368576));
#47696=CARTESIAN_POINT('Ctrl Pts',(87.3981208457895,38.9834796301527,121.157607876307));
#47697=CARTESIAN_POINT('Ctrl Pts',(86.6543415819103,38.6170779328651,121.210257384038));
#47698=CARTESIAN_POINT('Ctrl Pts',(85.9105623180311,38.2506762355775,121.262906891768));
#47699=CARTESIAN_POINT('Ctrl Pts',(85.3651493005611,37.4814570320105,121.315556399499));
#47700=CARTESIAN_POINT('Ctrl Pts',(85.2652956034228,36.6584695607634,121.36820590723));
#47701=CARTESIAN_POINT('Ctrl Pts',(85.2531507071272,36.5583721404652,121.374609503989));
#47702=CARTESIAN_POINT('Ctrl Pts',(85.2475970163779,36.4574793205693,121.381013100749));
#47703=CARTESIAN_POINT('Ctrl Pts',(85.2483527795145,36.3565049891663,121.387416697508));
#47704=CARTESIAN_POINT('Ctrl Pts',(86.9747563060389,33.385703120938,122.));
#47705=CARTESIAN_POINT('Ctrl Pts',(85.9925177162673,33.6482971733158,121.947350492269));
#47706=CARTESIAN_POINT('Ctrl Pts',(84.3257620656596,35.2211421325034,121.842051476808));
#47707=CARTESIAN_POINT('Ctrl Pts',(84.9365306847115,38.623331668768,121.684102953615));
#47708=CARTESIAN_POINT('Ctrl Pts',(88.1200899430042,39.9637871161453,121.526154430423));
#47709=CARTESIAN_POINT('Ctrl Pts',(90.9824825683396,38.0346656023702,121.36820590723));
#47710=CARTESIAN_POINT('Ctrl Pts',(90.9320922557558,34.5813834652293,121.210257384038));
#47711=CARTESIAN_POINT('Ctrl Pts',(88.0128424000897,32.736698135431,121.052308860845));
#47712=CARTESIAN_POINT('Ctrl Pts',(84.8723857333594,34.1722681870687,120.894360337653));
#47713=CARTESIAN_POINT('Ctrl Pts',(84.3576617369607,37.5869248191736,120.73641181446));
#47714=CARTESIAN_POINT('Ctrl Pts',(86.9355578127517,39.8844990120122,120.578463291268));
#47715=CARTESIAN_POINT('Ctrl Pts',(90.2686753707106,38.9819491786592,120.420514768075));
#47716=CARTESIAN_POINT('Ctrl Pts',(91.3350260504491,35.6975416344974,120.262566244883));
#47717=CARTESIAN_POINT('Ctrl Pts',(89.1677588017562,33.0091722323982,120.10461772169));
#47718=CARTESIAN_POINT('Ctrl Pts',(85.7318802647753,33.3542923559705,119.946669198498));
#47719=CARTESIAN_POINT('Ctrl Pts',(84.1425914969864,36.4199976243217,119.788720675305));
#47720=CARTESIAN_POINT('Ctrl Pts',(85.8408549696731,39.426703616461,119.630772152113));
#47721=CARTESIAN_POINT('Ctrl Pts',(89.286905538518,39.6483227638767,119.472823628921));
#47722=CARTESIAN_POINT('Ctrl Pts',(91.3563145937352,36.8839190889564,119.314875105728));
#47723=CARTESIAN_POINT('Ctrl Pts',(90.1728115748451,33.639893637919,119.156926582536));
#47724=CARTESIAN_POINT('Ctrl Pts',(86.8094428243991,32.8575054740432,118.998978059343));
#47725=CARTESIAN_POINT('Ctrl Pts',(84.3156724232774,35.2461222234895,118.841029536151));
#47726=CARTESIAN_POINT('Ctrl Pts',(84.9525261850344,38.6400576904171,118.683081012958));
#47727=CARTESIAN_POINT('Ctrl Pts',(88.1425881556754,39.9621338261614,118.525132489766));
#47728=CARTESIAN_POINT('Ctrl Pts',(90.9935261761534,38.0136643991501,118.367183966573));
#47729=CARTESIAN_POINT('Ctrl Pts',(90.9204814465843,34.5612673829304,118.209235443381));
#47730=CARTESIAN_POINT('Ctrl Pts',(87.989681403696,32.7351261502086,118.051286920188));
#47731=CARTESIAN_POINT('Ctrl Pts',(84.8583933091573,34.1909474180868,117.893338396996));
#47732=CARTESIAN_POINT('Ctrl Pts',(84.3656608449326,37.6087823193115,117.735389873803));
#47733=CARTESIAN_POINT('Ctrl Pts',(86.9582295503262,39.8897838979207,117.577441350611));
#47734=CARTESIAN_POINT('Ctrl Pts',(90.2854962296813,38.9658373960053,117.419492827418));
#47735=CARTESIAN_POINT('Ctrl Pts',(91.3307293790144,35.6746570063435,117.261544304226));
#47736=CARTESIAN_POINT('Ctrl Pts',(89.1462478911809,33.0002558914885,117.103595781033));
#47737=CARTESIAN_POINT('Ctrl Pts',(85.712654693185,33.367432204059,116.945647257841));
#47738=CARTESIAN_POINT('Ctrl Pts',(84.1430843096398,36.443278348604,116.787698734649));
#47739=CARTESIAN_POINT('Ctrl Pts',(85.8606184709768,39.4390181734991,116.629750211456));
#47740=CARTESIAN_POINT('Ctrl Pts',(89.3080211895539,39.6385054908189,116.471801688264));
#47741=CARTESIAN_POINT('Ctrl Pts',(91.3596372684504,36.8608712170826,116.313853165071));
#47742=CARTESIAN_POINT('Ctrl Pts',(90.1553288060137,33.6245118703589,116.155904641879));
#47743=CARTESIAN_POINT('Ctrl Pts',(86.7870056577489,32.8637360409022,115.997956118686));
#47744=CARTESIAN_POINT('Ctrl Pts',(84.30862397927,35.2683160353299,115.840007595494));
#47745=CARTESIAN_POINT('Ctrl Pts',(84.9672570618822,38.6580923046891,115.682059072301));
#47746=CARTESIAN_POINT('Ctrl Pts',(88.1657423210009,39.9596578009367,115.524110549109));
#47747=CARTESIAN_POINT('Ctrl Pts',(91.0041104497151,37.9929226739502,115.366162025916));
#47748=CARTESIAN_POINT('Ctrl Pts',(90.9088993907837,34.5410658478232,115.208213502724));
#47749=CARTESIAN_POINT('Ctrl Pts',(87.9664341156267,32.7337809233254,115.050264979531));
#47750=CARTESIAN_POINT('Ctrl Pts',(84.8445583981927,34.2096781754126,114.892316456339));
#47751=CARTESIAN_POINT('Ctrl Pts',(84.3737820039213,37.6306064530032,114.734367933146));
#47752=CARTESIAN_POINT('Ctrl Pts',(86.9809435714815,39.8949141296362,114.576419409954));
#47753=CARTESIAN_POINT('Ctrl Pts',(90.3022090008012,38.9496223007136,114.418470886762));
#47754=CARTESIAN_POINT('Ctrl Pts',(91.3262879388381,35.6517983177679,114.260522363569));
#47755=CARTESIAN_POINT('Ctrl Pts',(89.1246791584273,32.9914788873536,114.102573840377));
#47756=CARTESIAN_POINT('Ctrl Pts',(85.6935143818628,33.3806947270693,113.944625317184));
#47757=CARTESIAN_POINT('Ctrl Pts',(84.1437263578963,36.4665556725093,113.786676793992));
#47758=CARTESIAN_POINT('Ctrl Pts',(85.880460753186,39.4512054566615,113.628728270799));
#47759=CARTESIAN_POINT('Ctrl Pts',(89.3290733119119,39.6285528942548,113.470779747607));
#47760=CARTESIAN_POINT('Ctrl Pts',(91.3628119118867,36.837802457402,113.312831224414));
#47761=CARTESIAN_POINT('Ctrl Pts',(90.1377476178771,33.6092426903596,113.154882701222));
#47762=CARTESIAN_POINT('Ctrl Pts',(86.7646089666149,32.8701105416984,112.996934178029));
#47763=CARTESIAN_POINT('Ctrl Pts',(84.3017181838254,35.2905546509213,112.838985654837));
#47764=CARTESIAN_POINT('Ctrl Pts',(84.9821034368262,38.6760319586759,112.681037131644));
#47765=CARTESIAN_POINT('Ctrl Pts',(88.188880109704,39.957033154659,112.523088608452));
#47766=CARTESIAN_POINT('Ctrl Pts',(91.0145613228638,37.9721134143629,112.365140085259));
#47767=CARTESIAN_POINT('Ctrl Pts',(90.8971878595435,34.5209390977093,112.207191562067));
#47768=CARTESIAN_POINT('Ctrl Pts',(87.9431786691826,32.7325849948854,112.049243038874));
#47769=CARTESIAN_POINT('Ctrl Pts',(84.8308440425533,34.2284973805913,111.891294515682));
#47770=CARTESIAN_POINT('Ctrl Pts',(84.3820431282414,37.6523779908239,111.73334599249));
#47771=CARTESIAN_POINT('Ctrl Pts',(87.0036900655912,39.8998984089112,111.575397469297));
#47772=CARTESIAN_POINT('Ctrl Pts',(90.3188173102936,38.9333002270083,111.417448946105));
#47773=CARTESIAN_POINT('Ctrl Pts',(91.3216998146175,35.6289686189096,111.259500422912));
#47774=CARTESIAN_POINT('Ctrl Pts',(89.1030545131784,32.9828405569386,111.10155189972));
#47775=CARTESIAN_POINT('Ctrl Pts',(85.6744596237584,33.3940798766124,110.943603376527));
#47776=CARTESIAN_POINT('Ctrl Pts',(84.1445178565661,36.4898283939069,110.785654853335));
#47777=CARTESIAN_POINT('Ctrl Pts',(85.9003808808979,39.463265081444,110.627706330142));
#47778=CARTESIAN_POINT('Ctrl Pts',(89.3500610946321,39.6184653269691,110.46975780695));
#47779=CARTESIAN_POINT('Ctrl Pts',(91.365838365503,36.8147137894109,110.311809283757));
#47780=CARTESIAN_POINT('Ctrl Pts',(90.1200687486007,33.5940867128609,110.153860760565));
#47781=CARTESIAN_POINT('Ctrl Pts',(86.7422536682402,32.8766287223663,109.995912237372));
#47782=CARTESIAN_POINT('Ctrl Pts',(84.2949553240436,35.3128371457212,109.83796371418));
#47783=CARTESIAN_POINT('Ctrl Pts',(84.9970646978785,38.6938759234372,109.680015190987));
#47784=CARTESIAN_POINT('Ctrl Pts',(88.2120005651333,39.9542599759734,109.522066667795));
#47785=CARTESIAN_POINT('Ctrl Pts',(91.0248783714271,37.9512375173972,109.364118144602));
#47786=CARTESIAN_POINT('Ctrl Pts',(90.8853473213453,34.5008878826802,109.20616962141));
#47787=CARTESIAN_POINT('Ctrl Pts',(87.9199160530301,32.731538577869,109.048221098218));
#47788=CARTESIAN_POINT('Ctrl Pts',(84.8172507461507,34.247403921267,108.890272575025));
#47789=CARTESIAN_POINT('Ctrl Pts',(84.3904440038818,37.6740967269575,108.732324051833));
#47790=CARTESIAN_POINT('Ctrl Pts',(87.0264678344641,39.9047351075969,108.57437552864));
#47791=CARTESIAN_POINT('Ctrl Pts',(90.3353210088379,38.9168747734219,108.416427005448));
#47792=CARTESIAN_POINT('Ctrl Pts',(91.3169640944224,35.6061628347523,108.258478482255));
#47793=CARTESIAN_POINT('Ctrl Pts',(89.0813771113567,32.9743536285202,108.100529959063));
#47794=CARTESIAN_POINT('Ctrl Pts',(85.6554865479944,33.4075616582705,107.94258143587));
#47795=CARTESIAN_POINT('Ctrl Pts',(84.1454683488411,36.5131478744096,107.784632912678));
#47796=CARTESIAN_POINT('Ctrl Pts',(85.920358340807,39.4750889550508,107.626684389485));
#47797=CARTESIAN_POINT('Ctrl Pts',(89.3710241690437,39.6084644686119,107.468735866293));
#47798=CARTESIAN_POINT('Ctrl Pts',(91.3686332599885,36.7911510990924,107.3107873431));
#47799=CARTESIAN_POINT('Ctrl Pts',(90.1024644197946,33.5799803118859,107.152838819908));
#47800=CARTESIAN_POINT('Ctrl Pts',(86.7195974323738,32.8813521540788,106.994890296716));
#47801=CARTESIAN_POINT('Ctrl Pts',(84.2891204576078,35.33913847958,106.836941773523));
#47802=CARTESIAN_POINT('Ctrl Pts',(84.7717723668806,37.5794426551218,106.731642758061));
#47803=CARTESIAN_POINT('Ctrl Pts',(85.4324929308767,38.3522276316149,106.678993250331));
#47804=CARTESIAN_POINT('Ctrl Pts',(87.0226227342249,33.5647485048415,122.10700224989));
#47805=CARTESIAN_POINT('Ctrl Pts',(86.0996135415481,33.8115080262153,122.054352742159));
#47806=CARTESIAN_POINT('Ctrl Pts',(84.5333639526222,35.2895097776259,121.949053726697));
#47807=CARTESIAN_POINT('Ctrl Pts',(85.1073029689203,38.4865458642768,121.791105203505));
#47808=CARTESIAN_POINT('Ctrl Pts',(88.0988922746495,39.746171288473,121.633156680312));
#47809=CARTESIAN_POINT('Ctrl Pts',(90.7886814294914,37.933376607479,121.47520815712));
#47810=CARTESIAN_POINT('Ctrl Pts',(90.7413296737966,34.6883288251183,121.317259633928));
#47811=CARTESIAN_POINT('Ctrl Pts',(87.9981118033538,32.9548787909513,121.159311110735));
#47812=CARTESIAN_POINT('Ctrl Pts',(85.0470259849183,34.3038833690559,121.001362587543));
#47813=CARTESIAN_POINT('Ctrl Pts',(84.5633400604243,37.5126347804625,120.84341406435));
#47814=CARTESIAN_POINT('Ctrl Pts',(86.9857879264501,39.6716642901257,120.685465541158));
#47815=CARTESIAN_POINT('Ctrl Pts',(90.117917103928,38.8235385885816,120.527517017965));
#47816=CARTESIAN_POINT('Ctrl Pts',(91.1199663924258,35.7371821907302,120.369568494773));
#47817=CARTESIAN_POINT('Ctrl Pts',(89.0833862637669,33.2109225861004,120.21161997158));
#47818=CARTESIAN_POINT('Ctrl Pts',(85.8546926372097,33.5352318221171,120.053671448388));
#47819=CARTESIAN_POINT('Ctrl Pts',(84.3612386457225,36.4160737827081,119.895722925195));
#47820=CARTESIAN_POINT('Ctrl Pts',(85.9570961219,39.2414741480778,119.737774402003));
#47821=CARTESIAN_POINT('Ctrl Pts',(89.1953484025524,39.4497295683677,119.57982587881));
#47822=CARTESIAN_POINT('Ctrl Pts',(91.1399712276629,36.8520205893159,119.421877355618));
#47823=CARTESIAN_POINT('Ctrl Pts',(90.0278339349809,33.8036112275119,119.263928832425));
#47824=CARTESIAN_POINT('Ctrl Pts',(86.8672777245543,33.0684013966023,119.105980309233));
#47825=CARTESIAN_POINT('Ctrl Pts',(84.5238827198886,35.3129835586951,118.948031786041));
#47826=CARTESIAN_POINT('Ctrl Pts',(85.1223339338948,38.5022632998365,118.790083262848));
#47827=CARTESIAN_POINT('Ctrl Pts',(88.1200338357027,39.7446176925654,118.632134739656));
#47828=CARTESIAN_POINT('Ctrl Pts',(90.7990591031426,37.9136417855822,118.474186216463));
#47829=CARTESIAN_POINT('Ctrl Pts',(90.7304190012663,34.6694257509815,118.316237693271));
#47830=CARTESIAN_POINT('Ctrl Pts',(87.9763474247134,32.9534015970941,118.158289170078));
#47831=CARTESIAN_POINT('Ctrl Pts',(85.033877309738,34.3214362346443,118.000340646886));
#47832=CARTESIAN_POINT('Ctrl Pts',(84.5708568188455,37.5331742642154,117.842392123693));
#47833=CARTESIAN_POINT('Ctrl Pts',(87.0070925487824,39.6766304952072,117.684443600501));
#47834=CARTESIAN_POINT('Ctrl Pts',(90.1337236580792,38.8083983531492,117.526495077308));
#47835=CARTESIAN_POINT('Ctrl Pts',(91.1159288120728,35.7156775152093,117.368546554116));
#47836=CARTESIAN_POINT('Ctrl Pts',(89.063172470081,33.2025439042705,117.210598030923));
#47837=CARTESIAN_POINT('Ctrl Pts',(85.836626375614,33.5475793318793,117.052649507731));
#47838=CARTESIAN_POINT('Ctrl Pts',(84.3617017415672,36.4379506695953,116.894700984538));
#47839=CARTESIAN_POINT('Ctrl Pts',(85.9756678758229,39.2530461321845,116.736752461346));
#47840=CARTESIAN_POINT('Ctrl Pts',(89.2151907710141,39.4405042809744,116.578803938153));
#47841=CARTESIAN_POINT('Ctrl Pts',(91.1430935437054,36.8303625137396,116.420855414961));
#47842=CARTESIAN_POINT('Ctrl Pts',(90.0114053844099,33.7891569869583,116.262906891768));
#47843=CARTESIAN_POINT('Ctrl Pts',(86.8461935284216,33.0742562576781,116.104958368576));
#47844=CARTESIAN_POINT('Ctrl Pts',(84.5172592999978,35.3338390744146,115.947009845384));
#47845=CARTESIAN_POINT('Ctrl Pts',(85.1361765327179,38.5192104193376,115.789061322191));
#47846=CARTESIAN_POINT('Ctrl Pts',(88.141791795191,39.7422909726956,115.631112798999));
#47847=CARTESIAN_POINT('Ctrl Pts',(90.8090051405891,37.8941507950725,115.473164275806));
#47848=CARTESIAN_POINT('Ctrl Pts',(90.7195353482665,34.6504423768763,115.315215752614));
#47849=CARTESIAN_POINT('Ctrl Pts',(87.9545019578215,32.9521374879537,115.157267229421));
#47850=CARTESIAN_POINT('Ctrl Pts',(85.0208766496814,34.3390375194823,114.999318706229));
#47851=CARTESIAN_POINT('Ctrl Pts',(84.5784882685562,37.5536823935329,114.841370183036));
#47852=CARTESIAN_POINT('Ctrl Pts',(87.0284369049777,39.6814513718082,114.683421659844));
#47853=CARTESIAN_POINT('Ctrl Pts',(90.1494286421223,38.7931610348741,114.525473136651));
#47854=CARTESIAN_POINT('Ctrl Pts',(91.1117551925935,35.6941972150994,114.367524613459));
#47855=CARTESIAN_POINT('Ctrl Pts',(89.0429043409186,33.1942961571498,114.209576090266));
#47856=CARTESIAN_POINT('Ctrl Pts',(85.8186402330563,33.5600421192143,114.051627567074));
#47857=CARTESIAN_POINT('Ctrl Pts',(84.3623050740457,36.4598243611497,113.893679043881));
#47858=CARTESIAN_POINT('Ctrl Pts',(85.9943136601298,39.2644985170834,113.735730520689));
#47859=CARTESIAN_POINT('Ctrl Pts',(89.2349734416037,39.4311518301388,113.577781997497));
#47860=CARTESIAN_POINT('Ctrl Pts',(91.1460767548168,36.8086848099001,113.419833474304));
#47861=CARTESIAN_POINT('Ctrl Pts',(89.994884349259,33.7748085448886,113.261884951112));
#47862=CARTESIAN_POINT('Ctrl Pts',(86.8251473671147,33.0802463734147,113.103936427919));
#47863=CARTESIAN_POINT('Ctrl Pts',(84.5107699269021,35.3547366922002,112.945987904727));
#47864=CARTESIAN_POINT('Ctrl Pts',(85.1501276650537,38.5360683046983,112.788039381534));
#47865=CARTESIAN_POINT('Ctrl Pts',(88.1635343655741,39.7398245936844,112.630090858342));
#47866=CARTESIAN_POINT('Ctrl Pts',(90.8188258217234,37.8745963425271,112.472142335149));
#47867=CARTESIAN_POINT('Ctrl Pts',(90.7085300272501,34.6315292781982,112.314193811957));
#47868=CARTESIAN_POINT('Ctrl Pts',(87.9326488245083,32.9510136744979,112.156245288764));
#47869=CARTESIAN_POINT('Ctrl Pts',(85.0079892754134,34.3567219187308,111.998296765572));
#47870=CARTESIAN_POINT('Ctrl Pts',(84.5862512436303,37.5741410985324,111.840348242379));
#47871=CARTESIAN_POINT('Ctrl Pts',(87.049811775995,39.6861350969617,111.682399719187));
#47872=CARTESIAN_POINT('Ctrl Pts',(90.1650354636175,38.7778231890285,111.524451195994));
#47873=CARTESIAN_POINT('Ctrl Pts',(91.1074437341793,35.6727441566147,111.366502672802));
#47874=CARTESIAN_POINT('Ctrl Pts',(89.0225836708075,33.1861787216656,111.20855414961));
#47875=CARTESIAN_POINT('Ctrl Pts',(85.8007344848218,33.5726201386511,111.050605626417));
#47876=CARTESIAN_POINT('Ctrl Pts',(84.3630488450153,36.4816937277295,110.892657103225));
#47877=CARTESIAN_POINT('Ctrl Pts',(86.0130325958229,39.275830941456,110.734708580032));
#47878=CARTESIAN_POINT('Ctrl Pts',(89.2546956522624,39.4216725473725,110.57676005684));
#47879=CARTESIAN_POINT('Ctrl Pts',(91.1489207120165,36.7869883982294,110.418811533647));
#47880=CARTESIAN_POINT('Ctrl Pts',(89.9782715231816,33.7605664791613,110.260863010455));
#47881=CARTESIAN_POINT('Ctrl Pts',(86.8041401025664,33.0863715050666,110.102914487262));
#47882=CARTESIAN_POINT('Ctrl Pts',(84.504414870389,35.3756755432596,109.94496596407));
#47883=CARTESIAN_POINT('Ctrl Pts',(85.1641867558175,38.5528362709339,109.787017440877));
#47884=CARTESIAN_POINT('Ctrl Pts',(88.1852606478871,39.7372186388315,109.629068917685));
#47885=CARTESIAN_POINT('Ctrl Pts',(90.8285207479504,37.8549792708652,109.471120394492));
#47886=CARTESIAN_POINT('Ctrl Pts',(90.6974034784492,34.6126871598077,109.3131718713));
#47887=CARTESIAN_POINT('Ctrl Pts',(87.9107889538232,32.9500303568646,109.155223348107));
#47888=CARTESIAN_POINT('Ctrl Pts',(84.9952156604596,34.3744883871094,108.997274824915));
#47889=CARTESIAN_POINT('Ctrl Pts',(84.5941455429619,37.5945501858085,108.839326301722));
#47890=CARTESIAN_POINT('Ctrl Pts',(87.071216035894,39.6906801406971,108.68137777853));
#47891=CARTESIAN_POINT('Ctrl Pts',(90.1805439822485,38.7623881971518,108.523429255338));
#47892=CARTESIAN_POINT('Ctrl Pts',(91.1029935798892,35.6513135707646,108.365480732145));
#47893=CARTESIAN_POINT('Ctrl Pts',(89.002213425367,33.1782035585746,108.207532208953));
#47894=CARTESIAN_POINT('Ctrl Pts',(85.7829054934487,33.5852889632459,108.04958368576));
#47895=CARTESIAN_POINT('Ctrl Pts',(84.3639420222092,36.503607033821,107.891635162568));
#47896=CARTESIAN_POINT('Ctrl Pts',(86.031805406558,39.2869418305473,107.733686639375));
#47897=CARTESIAN_POINT('Ctrl Pts',(89.2743946445339,39.4122747449501,107.575738116183));
#47898=CARTESIAN_POINT('Ctrl Pts',(91.1515470731975,36.7648465479756,107.41778959299));
#47899=CARTESIAN_POINT('Ctrl Pts',(89.9617287427533,33.7473107000553,107.259841069798));
#47900=CARTESIAN_POINT('Ctrl Pts',(86.7828500471828,33.0908101118746,107.101892546605));
#47901=CARTESIAN_POINT('Ctrl Pts',(84.4989318488357,35.4003908957046,106.943944023413));
#47902=CARTESIAN_POINT('Ctrl Pts',(84.952479646449,37.5056037940271,106.838645007951));
#47903=CARTESIAN_POINT('Ctrl Pts',(85.5733584845537,38.2317895137629,106.78599550022));
#47904=CARTESIAN_POINT('Ctrl Pts',(87.0704891624108,33.743793888745,122.21400449978));
#47905=CARTESIAN_POINT('Ctrl Pts',(86.2067093668289,33.9747188791149,122.161354992049));
#47906=CARTESIAN_POINT('Ctrl Pts',(84.7409658395849,35.3578774227484,122.056055976587));
#47907=CARTESIAN_POINT('Ctrl Pts',(85.2780752531291,38.3497600597857,121.898107453395));
#47908=CARTESIAN_POINT('Ctrl Pts',(88.0776946062948,39.5285554608006,121.740158930202));
#47909=CARTESIAN_POINT('Ctrl Pts',(90.5948802906431,37.8320876125879,121.58221040701));
#47910=CARTESIAN_POINT('Ctrl Pts',(90.5505670918375,34.7952741850072,121.424261883817));
#47911=CARTESIAN_POINT('Ctrl Pts',(87.9833812066179,33.1730594464715,121.266313360625));
#47912=CARTESIAN_POINT('Ctrl Pts',(85.221666236477,34.4354985510432,121.108364837432));
#47913=CARTESIAN_POINT('Ctrl Pts',(84.7690183838881,37.4383447417513,120.95041631424));
#47914=CARTESIAN_POINT('Ctrl Pts',(87.0360180401483,39.4588295682391,120.792467791047));
#47915=CARTESIAN_POINT('Ctrl Pts',(89.9671588371456,38.665127998504,120.634519267855));
#47916=CARTESIAN_POINT('Ctrl Pts',(90.9049067344024,35.7768227469628,120.476570744662));
#47917=CARTESIAN_POINT('Ctrl Pts',(88.9990137257777,33.4126729398025,120.31862222147));
#47918=CARTESIAN_POINT('Ctrl Pts',(85.977505009644,33.7161712882636,120.160673698278));
#47919=CARTESIAN_POINT('Ctrl Pts',(84.5798857944587,36.4121499410944,120.002725175085));
#47920=CARTESIAN_POINT('Ctrl Pts',(86.0733372741268,39.0562446796945,119.844776651893));
#47921=CARTESIAN_POINT('Ctrl Pts',(89.103791266587,39.2511363728585,119.6868281287));
#47922=CARTESIAN_POINT('Ctrl Pts',(90.9236278615904,36.8201220896753,119.528879605508));
#47923=CARTESIAN_POINT('Ctrl Pts',(89.8828562951167,33.9673288171048,119.370931082315));
#47924=CARTESIAN_POINT('Ctrl Pts',(86.9251126247094,33.2792973191614,119.212982559123));
#47925=CARTESIAN_POINT('Ctrl Pts',(84.7320930164998,35.3798448939008,119.05503403593));
#47926=CARTESIAN_POINT('Ctrl Pts',(85.2921416827553,38.364468909256,118.897085512738));
#47927=CARTESIAN_POINT('Ctrl Pts',(88.0974795157296,39.5271015589694,118.739136989545));
#47928=CARTESIAN_POINT('Ctrl Pts',(90.6045920301321,37.8136191720142,118.581188466353));
#47929=CARTESIAN_POINT('Ctrl Pts',(90.5403565559482,34.7775841190325,118.42323994316));
#47930=CARTESIAN_POINT('Ctrl Pts',(87.963013445731,33.1716770439797,118.265291419968));
#47931=CARTESIAN_POINT('Ctrl Pts',(85.2093613103188,34.4519250512017,118.107342896775));
#47932=CARTESIAN_POINT('Ctrl Pts',(84.7760527927585,37.4575662091194,117.949394373583));
#47933=CARTESIAN_POINT('Ctrl Pts',(87.0559555472384,39.4634770924937,117.79144585039));
#47934=CARTESIAN_POINT('Ctrl Pts',(89.9819510864773,38.6509593102931,117.633497327198));
#47935=CARTESIAN_POINT('Ctrl Pts',(90.901128245131,35.7566980240751,117.475548804005));
#47936=CARTESIAN_POINT('Ctrl Pts',(88.9800970489813,33.4048319170525,117.317600280813));
#47937=CARTESIAN_POINT('Ctrl Pts',(85.9605980580428,33.7277264596997,117.159651757621));
#47938=CARTESIAN_POINT('Ctrl Pts',(84.5803191734944,36.4326229905866,117.001703234428));
#47939=CARTESIAN_POINT('Ctrl Pts',(86.0907172806691,39.0670740908699,116.843754711236));
#47940=CARTESIAN_POINT('Ctrl Pts',(89.1223603524743,39.2425030711299,116.685806188043));
#47941=CARTESIAN_POINT('Ctrl Pts',(90.9265498189602,36.7998538103966,116.527857664851));
#47942=CARTESIAN_POINT('Ctrl Pts',(89.8674819628062,33.9538021035576,116.369909141658));
#47943=CARTESIAN_POINT('Ctrl Pts',(86.9053813990943,33.284776474454,116.211960618466));
#47944=CARTESIAN_POINT('Ctrl Pts',(84.7258946207258,35.3993621134993,116.054012095273));
#47945=CARTESIAN_POINT('Ctrl Pts',(85.3050960035535,38.3803285339862,115.896063572081));
#47946=CARTESIAN_POINT('Ctrl Pts',(88.1178412693811,39.5249241444546,115.738115048888));
#47947=CARTESIAN_POINT('Ctrl Pts',(90.6138998314632,37.7953789161947,115.580166525696));
#47948=CARTESIAN_POINT('Ctrl Pts',(90.5301713057494,34.7598189059295,115.422218002503));
#47949=CARTESIAN_POINT('Ctrl Pts',(87.9425698000164,33.170494052582,115.264269479311));
#47950=CARTESIAN_POINT('Ctrl Pts',(85.19719490117,34.468396863552,115.106320956119));
#47951=CARTESIAN_POINT('Ctrl Pts',(84.7831945331911,37.4767583340626,114.948372432926));
#47952=CARTESIAN_POINT('Ctrl Pts',(87.0759302384741,39.4679886139801,114.790423909734));
#47953=CARTESIAN_POINT('Ctrl Pts',(89.9966482834433,38.6366997690347,114.632475386541));
#47954=CARTESIAN_POINT('Ctrl Pts',(90.897222446349,35.7365961124309,114.474526863349));
#47955=CARTESIAN_POINT('Ctrl Pts',(88.9611295234098,33.397113426946,114.316578340156));
#47956=CARTESIAN_POINT('Ctrl Pts',(85.9437660842499,33.7393895113594,114.158629816964));
#47957=CARTESIAN_POINT('Ctrl Pts',(84.5808837901952,36.4530930497901,114.000681293771));
#47958=CARTESIAN_POINT('Ctrl Pts',(86.1081665670736,39.0777915775053,113.842732770579));
#47959=CARTESIAN_POINT('Ctrl Pts',(89.1408735712955,39.2337507660228,113.684784247386));
#47960=CARTESIAN_POINT('Ctrl Pts',(90.929341597747,36.7795671623981,113.526835724194));
#47961=CARTESIAN_POINT('Ctrl Pts',(89.8520210806407,33.9403743994175,113.368887201002));
#47962=CARTESIAN_POINT('Ctrl Pts',(86.8856857676146,33.2903822051309,113.210938677809));
#47963=CARTESIAN_POINT('Ctrl Pts',(84.7198216699789,35.4189187334791,113.052990154617));
#47964=CARTESIAN_POINT('Ctrl Pts',(85.3181518932811,38.3961046507208,112.895041631424));
#47965=CARTESIAN_POINT('Ctrl Pts',(88.1381886214443,39.5226160327098,112.737093108232));
#47966=CARTESIAN_POINT('Ctrl Pts',(90.6230903205828,37.7770792706913,112.579144585039));
#47967=CARTESIAN_POINT('Ctrl Pts',(90.519872194957,34.742119458687,112.421196061847));
#47968=CARTESIAN_POINT('Ctrl Pts',(87.9221189798339,33.1694423541105,112.263247538654));
#47969=CARTESIAN_POINT('Ctrl Pts',(85.1851345082736,34.4849464568703,112.105299015462));
#47970=CARTESIAN_POINT('Ctrl Pts',(84.7904593590192,37.4959042062408,111.947350492269));
#47971=CARTESIAN_POINT('Ctrl Pts',(87.0959334863987,39.4723717850122,111.789401969077));
#47972=CARTESIAN_POINT('Ctrl Pts',(90.0112536169413,38.6223461510488,111.631453445884));
#47973=CARTESIAN_POINT('Ctrl Pts',(90.8931876537409,35.7165196943199,111.473504922692));
#47974=CARTESIAN_POINT('Ctrl Pts',(88.9421128284366,33.3895168863927,111.315556399499));
#47975=CARTESIAN_POINT('Ctrl Pts',(85.9270093458854,33.7511604006897,111.157607876307));
#47976=CARTESIAN_POINT('Ctrl Pts',(84.5815798334644,36.4735590615522,110.999659353114));
#47977=CARTESIAN_POINT('Ctrl Pts',(86.125684310748,39.0883968014681,110.841710829922));
#47978=CARTESIAN_POINT('Ctrl Pts',(89.1593302098928,39.2248797677758,110.683762306729));
#47979=CARTESIAN_POINT('Ctrl Pts',(90.9320030585298,36.759263007048,110.525813783537));
#47980=CARTESIAN_POINT('Ctrl Pts',(89.8364742977627,33.9270462454618,110.367865260344));
#47981=CARTESIAN_POINT('Ctrl Pts',(86.8660265368926,33.2961142877669,110.209916737152));
#47982=CARTESIAN_POINT('Ctrl Pts',(84.7138744167345,35.4385139407981,110.05196821396));
#47983=CARTESIAN_POINT('Ctrl Pts',(85.3313088137564,38.4117966184305,109.894019690767));
#47984=CARTESIAN_POINT('Ctrl Pts',(88.158520730641,39.5201773016895,109.736071167575));
#47985=CARTESIAN_POINT('Ctrl Pts',(90.6321631244736,37.7587210243331,109.578122644382));
#47986=CARTESIAN_POINT('Ctrl Pts',(90.5094596355534,34.7244864369352,109.42017412119));
#47987=CARTESIAN_POINT('Ctrl Pts',(87.901661854616,33.1685221358602,109.262225597997));
#47988=CARTESIAN_POINT('Ctrl Pts',(85.1731805747687,34.5015728529517,109.104277074805));
#47989=CARTESIAN_POINT('Ctrl Pts',(84.7978470820419,37.5150036446594,108.946328551612));
#47990=CARTESIAN_POINT('Ctrl Pts',(87.1159642373238,39.4766251737973,108.78838002842));
#47991=CARTESIAN_POINT('Ctrl Pts',(90.0257669556591,38.6079016208817,108.630431505227));
#47992=CARTESIAN_POINT('Ctrl Pts',(90.8890230653562,35.696464306777,108.472482982035));
#47993=CARTESIAN_POINT('Ctrl Pts',(88.9230497393773,33.382053488629,108.314534458842));
#47994=CARTESIAN_POINT('Ctrl Pts',(85.9103244389029,33.7630162682213,108.15658593565));
#47995=CARTESIAN_POINT('Ctrl Pts',(84.5824156955773,36.4940661932323,107.998637412457));
#47996=CARTESIAN_POINT('Ctrl Pts',(86.143252472309,39.0987947060438,107.840688889265));
#47997=CARTESIAN_POINT('Ctrl Pts',(89.1777651200243,39.2160850212882,107.682740366073));
#47998=CARTESIAN_POINT('Ctrl Pts',(90.9344608864062,36.738541996859,107.52479184288));
#47999=CARTESIAN_POINT('Ctrl Pts',(89.8209930657121,33.9146410882247,107.366843319688));
#48000=CARTESIAN_POINT('Ctrl Pts',(86.8461026619917,33.3002680696704,107.208894796495));
#48001=CARTESIAN_POINT('Ctrl Pts',(84.7087432400635,35.4616433118293,107.050946273303));
#48002=CARTESIAN_POINT('Ctrl Pts',(85.1331869260174,37.4317649329324,106.945647257841));
#48003=CARTESIAN_POINT('Ctrl Pts',(85.7142240382307,38.111351395911,106.89299775011));
#48004=CARTESIAN_POINT('Ctrl Pts',(87.1183555905968,33.9228392726486,122.321006749669));
#48005=CARTESIAN_POINT('Ctrl Pts',(86.3138051921097,34.1379297320145,122.268357241939));
#48006=CARTESIAN_POINT('Ctrl Pts',(84.9485677265476,35.4262450678709,122.163058226477));
#48007=CARTESIAN_POINT('Ctrl Pts',(85.4488475373378,38.2129742552945,122.005109703284));
#48008=CARTESIAN_POINT('Ctrl Pts',(88.0564969379401,39.3109396331282,121.847161180092));
#48009=CARTESIAN_POINT('Ctrl Pts',(90.4010791517949,37.7307986176968,121.6892126569));
#48010=CARTESIAN_POINT('Ctrl Pts',(90.3598045098783,34.9022195448962,121.531264133707));
#48011=CARTESIAN_POINT('Ctrl Pts',(87.968650609882,33.3912401019918,121.373315610515));
#48012=CARTESIAN_POINT('Ctrl Pts',(85.3963064880358,34.5671137330305,121.215367087322));
#48013=CARTESIAN_POINT('Ctrl Pts',(84.9746967073516,37.3640547030401,121.05741856413));
#48014=CARTESIAN_POINT('Ctrl Pts',(87.0862481538468,39.2459948463526,120.899470040937));
#48015=CARTESIAN_POINT('Ctrl Pts',(89.816400570363,38.5067174084264,120.741521517745));
#48016=CARTESIAN_POINT('Ctrl Pts',(90.6898470763792,35.8164633031955,120.583572994552));
#48017=CARTESIAN_POINT('Ctrl Pts',(88.9146411877884,33.6144232935047,120.42562447136));
#48018=CARTESIAN_POINT('Ctrl Pts',(86.1003173820783,33.8971107544102,120.267675948167));
#48019=CARTESIAN_POINT('Ctrl Pts',(84.7985329431949,36.4082260994807,120.109727424975));
#48020=CARTESIAN_POINT('Ctrl Pts',(86.1895784263537,38.8710152113111,119.951778901782));
#48021=CARTESIAN_POINT('Ctrl Pts',(89.0122341306214,39.0525431773495,119.79383037859));
#48022=CARTESIAN_POINT('Ctrl Pts',(90.7072844955181,36.7882235900348,119.635881855397));
#48023=CARTESIAN_POINT('Ctrl Pts',(89.7378786552524,34.1310464066976,119.477933332205));
#48024=CARTESIAN_POINT('Ctrl Pts',(86.9829475248645,33.4901932417205,119.319984809013));
#48025=CARTESIAN_POINT('Ctrl Pts',(84.9403033131111,35.4467062291065,119.16203628582));
#48026=CARTESIAN_POINT('Ctrl Pts',(85.4619494316156,38.2266745186755,119.004087762628));
#48027=CARTESIAN_POINT('Ctrl Pts',(88.074925195757,39.3095854253735,118.846139239435));
#48028=CARTESIAN_POINT('Ctrl Pts',(90.4101249571212,37.7135965584462,118.688190716243));
#48029=CARTESIAN_POINT('Ctrl Pts',(90.3502941106303,34.8857424870836,118.53024219305));
#48030=CARTESIAN_POINT('Ctrl Pts',(87.9496794667482,33.3899524908652,118.372293669858));
#48031=CARTESIAN_POINT('Ctrl Pts',(85.3848453108996,34.5824138677591,118.214345146665));
#48032=CARTESIAN_POINT('Ctrl Pts',(84.9812487666711,37.3819581540233,118.056396623473));
#48033=CARTESIAN_POINT('Ctrl Pts',(87.1048185456946,39.2503236897802,117.89844810028));
#48034=CARTESIAN_POINT('Ctrl Pts',(89.8301785148752,38.4935202674369,117.740499577088));
#48035=CARTESIAN_POINT('Ctrl Pts',(90.6863276781894,35.7977185329409,117.582551053895));
#48036=CARTESIAN_POINT('Ctrl Pts',(88.8970216278814,33.6071199298345,117.424602530703));
#48037=CARTESIAN_POINT('Ctrl Pts',(86.0845697404717,33.90787358752,117.266654007511));
#48038=CARTESIAN_POINT('Ctrl Pts',(84.7989366054219,36.4272953115779,117.108705484318));
#48039=CARTESIAN_POINT('Ctrl Pts',(86.205766685515,38.8811020495552,116.950756961125));
#48040=CARTESIAN_POINT('Ctrl Pts',(89.0295299339346,39.0445018612854,116.792808437933));
#48041=CARTESIAN_POINT('Ctrl Pts',(90.710006094215,36.7693451070536,116.634859914741));
#48042=CARTESIAN_POINT('Ctrl Pts',(89.7235585412025,34.118447220157,116.476911391548));
#48043=CARTESIAN_POINT('Ctrl Pts',(86.9645692697669,33.4952966912299,116.318962868356));
#48044=CARTESIAN_POINT('Ctrl Pts',(84.9345299414539,35.464885152584,116.161014345163));
#48045=CARTESIAN_POINT('Ctrl Pts',(85.474015474389,38.2414466486347,116.003065821971));
#48046=CARTESIAN_POINT('Ctrl Pts',(88.0938907435712,39.3075573162135,115.845117298778));
#48047=CARTESIAN_POINT('Ctrl Pts',(90.4187945223373,37.696607037317,115.687168775586));
#48048=CARTESIAN_POINT('Ctrl Pts',(90.3408072632322,34.8691954349826,115.529220252393));
#48049=CARTESIAN_POINT('Ctrl Pts',(87.9306376422113,33.3888506172103,115.371271729201));
#48050=CARTESIAN_POINT('Ctrl Pts',(85.3735131526587,34.5977562076217,115.213323206008));
#48051=CARTESIAN_POINT('Ctrl Pts',(84.9879007978259,37.3998342745923,115.055374682816));
#48052=CARTESIAN_POINT('Ctrl Pts',(87.1234235719704,39.254525856152,114.897426159623));
#48053=CARTESIAN_POINT('Ctrl Pts',(89.8438679247643,38.4802385031952,114.739477636431));
#48054=CARTESIAN_POINT('Ctrl Pts',(90.6826897001046,35.7789950097624,114.581529113238));
#48055=CARTESIAN_POINT('Ctrl Pts',(88.879354705901,33.5999306967421,114.423580590046));
#48056=CARTESIAN_POINT('Ctrl Pts',(86.0688919354435,33.9187369035045,114.265632066854));
#48057=CARTESIAN_POINT('Ctrl Pts',(84.7994625063446,36.4463617384305,114.107683543661));
#48058=CARTESIAN_POINT('Ctrl Pts',(86.2220194740172,38.8910846379272,113.949735020469));
#48059=CARTESIAN_POINT('Ctrl Pts',(89.0467737009874,39.0363497019068,113.791786497276));
#48060=CARTESIAN_POINT('Ctrl Pts',(90.712606440677,36.7504495148962,113.633837974084));
#48061=CARTESIAN_POINT('Ctrl Pts',(89.7091578120227,34.1059402539464,113.475889450891));
#48062=CARTESIAN_POINT('Ctrl Pts',(86.9462241681142,33.5005180368472,113.317940927699));
#48063=CARTESIAN_POINT('Ctrl Pts',(84.9288734130558,35.4831007747579,113.159992404506));
#48064=CARTESIAN_POINT('Ctrl Pts',(85.4861761215085,38.2561409967433,113.002043881314));
#48065=CARTESIAN_POINT('Ctrl Pts',(88.1128428773144,39.3054074717351,112.844095358121));
#48066=CARTESIAN_POINT('Ctrl Pts',(90.4273548194423,37.6795621988556,112.686146834929));
#48067=CARTESIAN_POINT('Ctrl Pts',(90.3312143626637,34.8527096391759,112.528198311737));
#48068=CARTESIAN_POINT('Ctrl Pts',(87.9115891351597,33.3878710337231,112.370249788544));
#48069=CARTESIAN_POINT('Ctrl Pts',(85.3622797411336,34.6131709950098,112.212301265351));
#48070=CARTESIAN_POINT('Ctrl Pts',(84.9946674744083,37.4176673139493,112.054352742159));
#48071=CARTESIAN_POINT('Ctrl Pts',(87.1420551968024,39.2586084730626,111.896404218967));
#48072=CARTESIAN_POINT('Ctrl Pts',(89.8574717702652,38.466869113069,111.738455695774));
#48073=CARTESIAN_POINT('Ctrl Pts',(90.6789315733027,35.760295232025,111.580507172582));
#48074=CARTESIAN_POINT('Ctrl Pts',(88.8616419860657,33.5928550511199,111.422558649389));
#48075=CARTESIAN_POINT('Ctrl Pts',(86.0532842069489,33.9297006627284,111.264610126197));
#48076=CARTESIAN_POINT('Ctrl Pts',(84.8001108219136,36.4654243953749,111.106661603004));
#48077=CARTESIAN_POINT('Ctrl Pts',(86.2383360256732,38.9009626614801,110.948713079812));
#48078=CARTESIAN_POINT('Ctrl Pts',(89.0639647675231,39.0280869881792,110.790764556619));
#48079=CARTESIAN_POINT('Ctrl Pts',(90.7150854050432,36.7315376158666,110.632816033427));
#48080=CARTESIAN_POINT('Ctrl Pts',(89.6946770723436,34.0935260117623,110.474867510234));
#48081=CARTESIAN_POINT('Ctrl Pts',(86.9279129712189,33.5058570704672,110.316918987042));
#48082=CARTESIAN_POINT('Ctrl Pts',(84.9233339630798,35.5013523383365,110.158970463849));
#48083=CARTESIAN_POINT('Ctrl Pts',(85.4984308716953,38.2707569659272,110.001021940657));
#48084=CARTESIAN_POINT('Ctrl Pts',(88.1317808133949,39.3031359645476,109.843073417464));
#48085=CARTESIAN_POINT('Ctrl Pts',(90.4358055009968,37.662462777801,109.685124894272));
#48086=CARTESIAN_POINT('Ctrl Pts',(90.3215157926575,34.8362857140626,109.52717637108));
#48087=CARTESIAN_POINT('Ctrl Pts',(87.892534755409,33.3870139148558,109.369227847887));
#48088=CARTESIAN_POINT('Ctrl Pts',(85.3511454890778,34.6286573187941,109.211279324695));
#48089=CARTESIAN_POINT('Ctrl Pts',(85.001548621122,37.4354571035105,109.053330801502));
#48090=CARTESIAN_POINT('Ctrl Pts',(87.1607124387537,39.2625702068974,108.89538227831));
#48091=CARTESIAN_POINT('Ctrl Pts',(89.8709899290696,38.4534150446116,108.737433755117));
#48092=CARTESIAN_POINT('Ctrl Pts',(90.6750525508231,35.7416150427893,108.579485231925));
#48093=CARTESIAN_POINT('Ctrl Pts',(88.8438860533876,33.5859034186835,108.421536708732));
#48094=CARTESIAN_POINT('Ctrl Pts',(86.0377433843573,33.9407435731967,108.26358818554));
#48095=CARTESIAN_POINT('Ctrl Pts',(84.8008893689454,36.4845253526437,108.105639662347));
#48096=CARTESIAN_POINT('Ctrl Pts',(86.25469953806,38.9106475815404,107.947691139155));
#48097=CARTESIAN_POINT('Ctrl Pts',(89.0811355955146,39.0198952976263,107.789742615962));
#48098=CARTESIAN_POINT('Ctrl Pts',(90.717374699615,36.7122374457423,107.63179409277));
#48099=CARTESIAN_POINT('Ctrl Pts',(89.6802573886707,34.081971476394,107.473845569577));
#48100=CARTESIAN_POINT('Ctrl Pts',(86.9093552768007,33.5097260274662,107.315897046385));
#48101=CARTESIAN_POINT('Ctrl Pts',(84.9185546312914,35.522895727954,107.157948523192));
#48102=CARTESIAN_POINT('Ctrl Pts',(85.3138942055859,37.3579260718377,107.052649507731));
#48103=CARTESIAN_POINT('Ctrl Pts',(85.8550895919077,37.990913278059,107.));
#48104=CARTESIAN_POINT('Ctrl Pts',(85.2535609624353,36.356687859589,121.112583302492));
#48105=CARTESIAN_POINT('Ctrl Pts',(85.2516480964026,36.6482406983004,121.094195056371));
#48106=CARTESIAN_POINT('Ctrl Pts',(85.2985193878855,36.9391986870805,121.07580681025));
#48107=CARTESIAN_POINT('Ctrl Pts',(85.3968902452148,37.2115545652573,121.05741856413));
#48108=CARTESIAN_POINT('Ctrl Pts',(85.6785471895167,37.9913680841443,121.004769056399));
#48109=CARTESIAN_POINT('Ctrl Pts',(86.3823976716817,38.6186814652484,120.952119548668));
#48110=CARTESIAN_POINT('Ctrl Pts',(87.189348315517,38.8091252494795,120.899470040937));
#48111=CARTESIAN_POINT('Ctrl Pts',(87.9962989593522,38.9995690337106,120.846820533206));
#48112=CARTESIAN_POINT('Ctrl Pts',(88.9063497648576,38.7531432210685,120.794171025476));
#48113=CARTESIAN_POINT('Ctrl Pts',(89.5069495852796,38.1815546305423,120.741521517745));
#48114=CARTESIAN_POINT('Ctrl Pts',(90.1075494057017,37.6099660400161,120.688872010014));
#48115=CARTESIAN_POINT('Ctrl Pts',(90.3986982410404,36.7132146716058,120.636222502283));
#48116=CARTESIAN_POINT('Ctrl Pts',(90.2484050106114,35.8978323191188,120.583572994552));
#48117=CARTESIAN_POINT('Ctrl Pts',(90.0981117801823,35.0824499666319,120.530923486821));
#48118=CARTESIAN_POINT('Ctrl Pts',(89.5063764839853,34.3484366300683,120.478273979091));
#48119=CARTESIAN_POINT('Ctrl Pts',(88.7414548682685,34.0285445386041,120.42562447136));
#48120=CARTESIAN_POINT('Ctrl Pts',(87.9765332525517,33.7086524471399,120.372974963629));
#48121=CARTESIAN_POINT('Ctrl Pts',(87.038425317315,33.802881600775,120.320325455898));
#48122=CARTESIAN_POINT('Ctrl Pts',(86.3524072765494,34.268515401771,120.267675948167));
#48123=CARTESIAN_POINT('Ctrl Pts',(85.6787931725816,34.7257300477372,120.215978399609));
#48124=CARTESIAN_POINT('Ctrl Pts',(85.2482352700075,35.5410399793431,120.16428085105));
#48125=CARTESIAN_POINT('Ctrl Pts',(85.2469699766098,36.3551993258525,120.112583302492));
#48126=CARTESIAN_POINT('Ctrl Pts',(86.9747563060389,33.385703120938,122.));
#48127=CARTESIAN_POINT('Ctrl Pts',(86.8817062479769,33.419741247829,122.));
#48128=CARTESIAN_POINT('Ctrl Pts',(86.7907213548637,33.4585480736554,122.));
#48129=CARTESIAN_POINT('Ctrl Pts',(86.7020101118859,33.5017952757603,122.));
#48130=CARTESIAN_POINT('Ctrl Pts',(86.611331909906,33.5460013808254,122.));
#48131=CARTESIAN_POINT('Ctrl Pts',(86.5230286333761,33.5948475710693,122.));
#48132=CARTESIAN_POINT('Ctrl Pts',(86.4373518622086,33.6480287386438,122.));
#48133=CARTESIAN_POINT('Ctrl Pts',(86.3549204309049,33.6991954633212,122.));
#48134=CARTESIAN_POINT('Ctrl Pts',(86.2749200114897,33.7543758529771,122.));
#48135=CARTESIAN_POINT('Ctrl Pts',(86.1976076309381,33.8133282211128,122.));
#48136=CARTESIAN_POINT('Ctrl Pts',(86.1299592979554,33.8649115432316,122.));
#48137=CARTESIAN_POINT('Ctrl Pts',(86.0643692849632,33.9193834837333,122.));
#48138=CARTESIAN_POINT('Ctrl Pts',(86.0010344007775,33.9765948307505,122.));
#48139=CARTESIAN_POINT('Ctrl Pts',(85.9868979548522,33.989364493533,122.));
#48140=CARTESIAN_POINT('Ctrl Pts',(85.9728712144497,34.0022733665456,122.));
#48141=CARTESIAN_POINT('Ctrl Pts',(85.9589759527776,34.015301257801,122.));
#48142=CARTESIAN_POINT('Ctrl Pts',(85.8865458564609,34.0832101205986,122.));
#48143=CARTESIAN_POINT('Ctrl Pts',(85.8175814474561,34.1544408988363,122.));
#48144=CARTESIAN_POINT('Ctrl Pts',(85.7523226756092,34.2287028696647,122.));
#48145=CARTESIAN_POINT('Ctrl Pts',(85.6874229281471,34.3025562845606,122.));
#48146=CARTESIAN_POINT('Ctrl Pts',(85.6261876700599,34.3794084282326,122.));
#48147=CARTESIAN_POINT('Ctrl Pts',(85.5688965222133,34.4590001179627,122.));
#48148=CARTESIAN_POINT('Ctrl Pts',(85.5137336076299,34.5356351610219,122.));
#48149=CARTESIAN_POINT('Ctrl Pts',(85.4622270538762,34.6148107322579,122.));
#48150=CARTESIAN_POINT('Ctrl Pts',(85.4146713091807,34.6963090585297,122.));
#48151=CARTESIAN_POINT('Ctrl Pts',(85.3947249791741,34.7304919426631,122.));
#48152=CARTESIAN_POINT('Ctrl Pts',(85.3754742525693,34.7650835569962,122.));
#48153=CARTESIAN_POINT('Ctrl Pts',(85.3569434395582,34.8000681299898,122.));
#48154=CARTESIAN_POINT('Ctrl Pts',(85.344060903815,34.8243892437899,122.));
#48155=CARTESIAN_POINT('Ctrl Pts',(85.3315263323148,34.8489002759048,122.));
#48156=CARTESIAN_POINT('Ctrl Pts',(85.3193483589149,34.8735959330844,122.));
#48157=CARTESIAN_POINT('Ctrl Pts',(85.3114400096724,34.8896332387456,122.));
#48158=CARTESIAN_POINT('Ctrl Pts',(85.3036809360749,34.9057510169598,122.));
#48159=CARTESIAN_POINT('Ctrl Pts',(85.2960836785505,34.9219256286096,122.));
#48160=CARTESIAN_POINT('Ctrl Pts',(85.2539633762117,35.0116000316037,122.));
#48161=CARTESIAN_POINT('Ctrl Pts',(85.2167419072931,35.1031580252053,122.));
#48162=CARTESIAN_POINT('Ctrl Pts',(85.1847105554573,35.1963272446824,122.));
#48163=CARTESIAN_POINT('Ctrl Pts',(85.1548308024479,35.2832381337491,122.));
#48164=CARTESIAN_POINT('Ctrl Pts',(85.1294675005642,35.3715518528724,122.));
#48165=CARTESIAN_POINT('Ctrl Pts',(85.1089076276163,35.4610560157098,122.));
#48166=CARTESIAN_POINT('Ctrl Pts',(85.1074271401942,35.4675010841028,122.));
#48167=CARTESIAN_POINT('Ctrl Pts',(85.1059715822065,35.4739523263869,122.));
#48168=CARTESIAN_POINT('Ctrl Pts',(85.1045410714323,35.4804096635754,122.));
#48169=CARTESIAN_POINT('Ctrl Pts',(85.0839348524742,35.5734263023821,122.));
#48170=CARTESIAN_POINT('Ctrl Pts',(85.06852165899,35.6677086068536,122.));
#48171=CARTESIAN_POINT('Ctrl Pts',(85.0582245708442,35.7628487105457,122.));
#48172=CARTESIAN_POINT('Ctrl Pts',(85.0524280535226,35.8164057211517,122.));
#48173=CARTESIAN_POINT('Ctrl Pts',(85.0482536960829,35.8702343689899,122.));
#48174=CARTESIAN_POINT('Ctrl Pts',(85.0456945388939,35.9242592591601,122.));
#48175=CARTESIAN_POINT('Ctrl Pts',(85.0450336564343,35.9382107672774,122.));
#48176=CARTESIAN_POINT('Ctrl Pts',(85.0444806105962,35.9521747635378,122.));
#48177=CARTESIAN_POINT('Ctrl Pts',(85.0440355229243,35.9661365800473,122.));
#48178=CARTESIAN_POINT('Ctrl Pts',(85.0410641138316,36.0593457861118,122.));
#48179=CARTESIAN_POINT('Ctrl Pts',(85.0428918593198,36.1526132293267,122.));
#48180=CARTESIAN_POINT('Ctrl Pts',(85.0493838649713,36.2455638298956,122.));
#48181=CARTESIAN_POINT('Ctrl Pts',(85.055886664939,36.3386689802641,122.));
#48182=CARTESIAN_POINT('Ctrl Pts',(85.0670696265457,36.4314572131348,122.));
#48183=CARTESIAN_POINT('Ctrl Pts',(85.0828481140956,36.5235394789013,122.));
#48184=CARTESIAN_POINT('Ctrl Pts',(85.0984010048097,36.6143051756542,122.));
#48185=CARTESIAN_POINT('Ctrl Pts',(85.1184194105491,36.7043857925402,122.));
#48186=CARTESIAN_POINT('Ctrl Pts',(85.142865299154,36.7933835307099,122.));
#48187=CARTESIAN_POINT('Ctrl Pts',(85.1519640629711,36.8265085037045,122.));
#48188=CARTESIAN_POINT('Ctrl Pts',(85.1616765771494,36.8594831454966,122.));
#48189=CARTESIAN_POINT('Ctrl Pts',(85.1720022421283,36.8922856787441,122.));
#48190=CARTESIAN_POINT('Ctrl Pts',(85.1789967228274,36.9145057184361,122.));
#48191=CARTESIAN_POINT('Ctrl Pts',(85.1862725653383,36.9366467701123,122.));
#48192=CARTESIAN_POINT('Ctrl Pts',(85.1938297624176,36.9587018515215,122.));
#48193=CARTESIAN_POINT('Ctrl Pts',(85.1983458216605,36.9718816129072,122.));
#48194=CARTESIAN_POINT('Ctrl Pts',(85.202962008638,36.9850295012457,122.));
#48195=CARTESIAN_POINT('Ctrl Pts',(85.2076748514515,36.9981348782542,122.));
#48196=CARTESIAN_POINT('Ctrl Pts',(85.2393066085118,37.0860958220241,122.));
#48197=CARTESIAN_POINT('Ctrl Pts',(85.2753275863277,37.1722590184577,122.));
#48198=CARTESIAN_POINT('Ctrl Pts',(85.3156732208267,37.2562102232251,122.));
#48199=CARTESIAN_POINT('Ctrl Pts',(85.3459324467009,37.3191736268007,122.));
#48200=CARTESIAN_POINT('Ctrl Pts',(85.3786253392863,37.3808922931221,122.));
#48201=CARTESIAN_POINT('Ctrl Pts',(85.4137406224306,37.4411759317203,122.));
#48202=CARTESIAN_POINT('Ctrl Pts',(85.4272099477612,37.4642991950884,122.));
#48203=CARTESIAN_POINT('Ctrl Pts',(85.4410358113732,37.4872111624651,122.));
#48204=CARTESIAN_POINT('Ctrl Pts',(85.4552180573203,37.5099004508088,122.));
#48205=CARTESIAN_POINT('Ctrl Pts',(85.4653423426853,37.526097661799,122.));
#48206=CARTESIAN_POINT('Ctrl Pts',(85.475649081078,37.5421824590417,122.));
#48207=CARTESIAN_POINT('Ctrl Pts',(85.4861281406993,37.5581356970078,122.));
#48208=CARTESIAN_POINT('Ctrl Pts',(85.5333147178236,37.629972170974,122.));
#48209=CARTESIAN_POINT('Ctrl Pts',(85.5840362197561,37.699215193506,122.));
#48210=CARTESIAN_POINT('Ctrl Pts',(85.6382597550527,37.7655127650129,122.));
#48211=CARTESIAN_POINT('Ctrl Pts',(85.6870561730674,37.8251747548651,122.));
#48212=CARTESIAN_POINT('Ctrl Pts',(85.7386892863001,37.8824513165183,122.));
#48213=CARTESIAN_POINT('Ctrl Pts',(85.7931556159572,37.9370561104042,122.));
#48214=CARTESIAN_POINT('Ctrl Pts',(85.8122381875779,37.9561871937123,122.));
#48215=CARTESIAN_POINT('Ctrl Pts',(85.831668704075,37.9749900284081,122.));
#48216=CARTESIAN_POINT('Ctrl Pts',(85.8514365905237,37.9934601270859,122.));
#48217=CARTESIAN_POINT('Origin',(87.7685555885722,36.3549260746835,114.));
#48218=CARTESIAN_POINT('Origin',(36.3549260746835,87.7685555885722,107.));
#48219=CARTESIAN_POINT('Ctrl Pts',(34.441460078019,89.4045427919478,107.));
#48220=CARTESIAN_POINT('Ctrl Pts',(34.3793225172007,89.3461487428037,107.));
#48221=CARTESIAN_POINT('Ctrl Pts',(34.3205603295786,89.2845007868439,107.));
#48222=CARTESIAN_POINT('Ctrl Pts',(34.2651854953777,89.2199753995623,107.));
#48223=CARTESIAN_POINT('Ctrl Pts',(34.2084555851626,89.1538710133388,107.));
#48224=CARTESIAN_POINT('Ctrl Pts',(34.1552803722276,89.0847461545033,107.));
#48225=CARTESIAN_POINT('Ctrl Pts',(34.1057016258454,89.0129593433036,107.));
#48226=CARTESIAN_POINT('Ctrl Pts',(34.0927638402984,88.9942262684241,107.));
#48227=CARTESIAN_POINT('Ctrl Pts',(34.0800711346354,88.9753117055674,107.));
#48228=CARTESIAN_POINT('Ctrl Pts',(34.0676246265426,88.9562215925571,107.));
#48229=CARTESIAN_POINT('Ctrl Pts',(34.0574547177416,88.9406232651493,107.));
#48230=CARTESIAN_POINT('Ctrl Pts',(34.0474487386034,88.924906826773,107.));
#48231=CARTESIAN_POINT('Ctrl Pts',(34.0376161466441,88.9090901117026,107.));
#48232=CARTESIAN_POINT('Ctrl Pts',(33.9901720007546,88.832771421737,107.));
#48233=CARTESIAN_POINT('Ctrl Pts',(33.9467114185444,88.7540453734224,107.));
#48234=CARTESIAN_POINT('Ctrl Pts',(33.90726908701,88.6733045174429,107.));
#48235=CARTESIAN_POINT('Ctrl Pts',(33.875440607195,88.6081496798658,107.));
#48236=CARTESIAN_POINT('Ctrl Pts',(33.8462292660138,88.5416817343779,107.));
#48237=CARTESIAN_POINT('Ctrl Pts',(33.8196704493666,88.4740891537832,107.));
#48238=CARTESIAN_POINT('Ctrl Pts',(33.8090688925697,88.4471080351685,107.));
#48239=CARTESIAN_POINT('Ctrl Pts',(33.7988901696328,88.4199475664955,107.));
#48240=CARTESIAN_POINT('Ctrl Pts',(33.7891372918137,88.3926191895465,107.));
#48241=CARTESIAN_POINT('Ctrl Pts',(33.7838963682359,88.377933684637,107.));
#48242=CARTESIAN_POINT('Ctrl Pts',(33.778778795415,88.3632005117775,107.));
#48243=CARTESIAN_POINT('Ctrl Pts',(33.7737890400817,88.3484339243473,107.));
#48244=CARTESIAN_POINT('Ctrl Pts',(33.7442502226087,88.261017307367,107.));
#48245=CARTESIAN_POINT('Ctrl Pts',(33.7191468702095,88.1723195871917,107.));
#48246=CARTESIAN_POINT('Ctrl Pts',(33.6985115520217,88.0827385727371,107.));
#48247=CARTESIAN_POINT('Ctrl Pts',(33.6775547727315,87.9917620473723,107.));
#48248=CARTESIAN_POINT('Ctrl Pts',(33.6612058191073,87.899873687659,107.));
#48249=CARTESIAN_POINT('Ctrl Pts',(33.6495406312905,87.8074569994372,107.));
#48250=CARTESIAN_POINT('Ctrl Pts',(33.6379661598897,87.7157590060932,107.));
#48251=CARTESIAN_POINT('Ctrl Pts',(33.6310025450947,87.623539939619,107.));
#48252=CARTESIAN_POINT('Ctrl Pts',(33.6287709136307,87.5311552180529,107.));
#48253=CARTESIAN_POINT('Ctrl Pts',(33.6276602991915,87.4851781795572,107.));
#48254=CARTESIAN_POINT('Ctrl Pts',(33.6277224410312,87.4391598993582,107.));
#48255=CARTESIAN_POINT('Ctrl Pts',(33.628977067353,87.3931434876068,107.));
#48256=CARTESIAN_POINT('Ctrl Pts',(33.6293468454931,87.3795809926617,107.));
#48257=CARTESIAN_POINT('Ctrl Pts',(33.6298202330787,87.3660186593414,107.));
#48258=CARTESIAN_POINT('Ctrl Pts',(33.6303977915693,87.3524575913575,107.));
#48259=CARTESIAN_POINT('Ctrl Pts',(33.6310182960977,87.337888150802,107.));
#48260=CARTESIAN_POINT('Ctrl Pts',(33.6317586368159,87.323329957392,107.));
#48261=CARTESIAN_POINT('Ctrl Pts',(33.6326188622406,87.3087869385134,107.));
#48262=CARTESIAN_POINT('Ctrl Pts',(33.6382706654492,87.2132372391001,107.));
#48263=CARTESIAN_POINT('Ctrl Pts',(33.6490951084808,87.1183092558368,107.));
#48264=CARTESIAN_POINT('Ctrl Pts',(33.6651626470178,87.0243986317404,107.));
#48265=CARTESIAN_POINT('Ctrl Pts',(33.667542969346,87.0104862608519,107.));
#48266=CARTESIAN_POINT('Ctrl Pts',(33.6700384483224,86.996596184385,107.));
#48267=CARTESIAN_POINT('Ctrl Pts',(33.6726494055391,86.9827296580056,107.));
#48268=CARTESIAN_POINT('Ctrl Pts',(33.6895950528478,86.8927330606227,107.));
#48269=CARTESIAN_POINT('Ctrl Pts',(33.7114005839111,86.8037286330741,107.));
#48270=CARTESIAN_POINT('Ctrl Pts',(33.7377634487177,86.7159486239087,107.));
#48271=CARTESIAN_POINT('Ctrl Pts',(33.7647222602648,86.6261843004161,107.));
#48272=CARTESIAN_POINT('Ctrl Pts',(33.796446985534,86.5376996780423,107.));
#48273=CARTESIAN_POINT('Ctrl Pts',(33.8326683308032,86.4507468020112,107.));
#48274=CARTESIAN_POINT('Ctrl Pts',(33.8451584343998,86.4207630887731,107.));
#48275=CARTESIAN_POINT('Ctrl Pts',(33.8581836620157,86.390961590169,107.));
#48276=CARTESIAN_POINT('Ctrl Pts',(33.8717343440126,86.3613529800899,107.));
#48277=CARTESIAN_POINT('Ctrl Pts',(33.8784253792389,86.3467328854639,107.));
#48278=CARTESIAN_POINT('Ctrl Pts',(33.8852445396145,86.3321598238552,107.));
#48279=CARTESIAN_POINT('Ctrl Pts',(33.8921907202356,86.3176351028333,107.));
#48280=CARTESIAN_POINT('Ctrl Pts',(33.8976844953031,86.306147415633,107.));
#48281=CARTESIAN_POINT('Ctrl Pts',(33.903257285469,86.2946909919042,107.));
#48282=CARTESIAN_POINT('Ctrl Pts',(33.9089039498725,86.2832754082256,107.));
#48283=CARTESIAN_POINT('Ctrl Pts',(33.951627885367,86.1969025293251,107.));
#48284=CARTESIAN_POINT('Ctrl Pts',(33.9986426798443,86.1127279663445,107.));
#48285=CARTESIAN_POINT('Ctrl Pts',(34.0496056775094,86.0310013571143,107.));
#48286=CARTESIAN_POINT('Ctrl Pts',(34.1015793905264,85.9476539182156,107.));
#48287=CARTESIAN_POINT('Ctrl Pts',(34.1576597775509,85.8668517216779,107.));
#48288=CARTESIAN_POINT('Ctrl Pts',(34.2175383986755,85.7888665836747,107.));
#48289=CARTESIAN_POINT('Ctrl Pts',(34.2779038546066,85.7102473983462,107.));
#48290=CARTESIAN_POINT('Ctrl Pts',(34.3421300165413,85.6344904284207,107.));
#48291=CARTESIAN_POINT('Ctrl Pts',(34.4099501911919,85.5618934535173,107.));
#48292=CARTESIAN_POINT('Ctrl Pts',(34.4469508834432,85.5222866795653,107.));
#48293=CARTESIAN_POINT('Ctrl Pts',(34.485022140315,85.483620877737,107.));
#48294=CARTESIAN_POINT('Ctrl Pts',(34.5241260026544,85.4459481822937,107.));
#48295=CARTESIAN_POINT('Ctrl Pts',(34.5360933740782,85.4344188061162,107.));
#48296=CARTESIAN_POINT('Ctrl Pts',(34.5481574847406,85.4229824675042,107.));
#48297=CARTESIAN_POINT('Ctrl Pts',(34.5603173095881,85.4116407228736,107.));
#48298=CARTESIAN_POINT('Ctrl Pts',(34.5708630920203,85.4018044322382,107.));
#48299=CARTESIAN_POINT('Ctrl Pts',(34.5814797527798,85.3920404066204,107.));
#48300=CARTESIAN_POINT('Ctrl Pts',(34.5921575105618,85.3823576403064,107.));
#48301=CARTESIAN_POINT('Ctrl Pts',(34.6677319836388,85.3138254655697,107.));
#48302=CARTESIAN_POINT('Ctrl Pts',(34.7464831774698,85.2492496355464,107.));
#48303=CARTESIAN_POINT('Ctrl Pts',(34.8280837446808,85.1889119226529,107.));
#48304=CARTESIAN_POINT('Ctrl Pts',(34.9097885075176,85.1284971646361,107.));
#48305=CARTESIAN_POINT('Ctrl Pts',(34.9943504984862,85.0723305153877,107.));
#48306=CARTESIAN_POINT('Ctrl Pts',(35.0814863891448,85.0207206280586,107.));
#48307=CARTESIAN_POINT('Ctrl Pts',(35.1668900448395,84.9701367295688,107.));
#48308=CARTESIAN_POINT('Ctrl Pts',(35.2547669448013,84.923929541906,107.));
#48309=CARTESIAN_POINT('Ctrl Pts',(35.3448844138265,84.8824254779805,107.));
#48310=CARTESIAN_POINT('Ctrl Pts',(35.3852340815519,84.8638422309501,107.));
#48311=CARTESIAN_POINT('Ctrl Pts',(35.4260333307823,84.8462023913809,107.));
#48312=CARTESIAN_POINT('Ctrl Pts',(35.4672630298986,84.8295382061365,107.));
#48313=CARTESIAN_POINT('Ctrl Pts',(35.4976826757836,84.8172432191498,107.));
#48314=CARTESIAN_POINT('Ctrl Pts',(35.5283366660204,84.8054793853022,107.));
#48315=CARTESIAN_POINT('Ctrl Pts',(35.5592127316546,84.7942440238826,107.));
#48316=CARTESIAN_POINT('Ctrl Pts',(37.1487253572157,84.7993326348264,107.));
#48317=CARTESIAN_POINT('Ctrl Pts',(37.2435592315062,84.834023289662,107.));
#48318=CARTESIAN_POINT('Ctrl Pts',(37.3363499518797,84.8737048348486,107.));
#48319=CARTESIAN_POINT('Ctrl Pts',(37.426856595716,84.9180569182258,107.));
#48320=CARTESIAN_POINT('Ctrl Pts',(37.5186361403217,84.9630327768162,107.));
#48321=CARTESIAN_POINT('Ctrl Pts',(37.6080675777822,85.012812173707,107.));
#48322=CARTESIAN_POINT('Ctrl Pts',(37.6948656522897,85.0671017322032,107.));
#48323=CARTESIAN_POINT('Ctrl Pts',(37.7193786617565,85.0824338748678,107.));
#48324=CARTESIAN_POINT('Ctrl Pts',(37.7436814000741,85.0981259477375,107.));
#48325=CARTESIAN_POINT('Ctrl Pts',(37.7677668456399,85.1141717983225,107.));
#48326=CARTESIAN_POINT('Ctrl Pts',(37.7870964269421,85.1270492671074,107.));
#48327=CARTESIAN_POINT('Ctrl Pts',(37.8062881599554,85.1401562208434,107.));
#48328=CARTESIAN_POINT('Ctrl Pts',(37.8253191290425,85.1534757143532,107.));
#48329=CARTESIAN_POINT('Ctrl Pts',(37.9080262255787,85.2113611867365,107.));
#48330=CARTESIAN_POINT('Ctrl Pts',(37.9877784618244,85.2733088104048,107.));
#48331=CARTESIAN_POINT('Ctrl Pts',(38.0643094764772,85.3390212224136,107.));
#48332=CARTESIAN_POINT('Ctrl Pts',(38.1233026628328,85.3896749944183,107.));
#48333=CARTESIAN_POINT('Ctrl Pts',(38.1803811813906,85.4425666947868,107.));
#48334=CARTESIAN_POINT('Ctrl Pts',(38.2354054643368,85.4975718921607,107.));
#48335=CARTESIAN_POINT('Ctrl Pts',(38.2646941992609,85.5268504680742,107.));
#48336=CARTESIAN_POINT('Ctrl Pts',(38.2934006313696,85.5567280097293,107.));
#48337=CARTESIAN_POINT('Ctrl Pts',(38.3215016904264,85.5871865825445,107.));
#48338=CARTESIAN_POINT('Ctrl Pts',(38.3311376927784,85.5976309888813,107.));
#48339=CARTESIAN_POINT('Ctrl Pts',(38.3407017795108,85.6081430071488,107.));
#48340=CARTESIAN_POINT('Ctrl Pts',(38.350186383968,85.6187143015985,107.));
#48341=CARTESIAN_POINT('Ctrl Pts',(38.4159835728468,85.6920501439884,107.));
#48342=CARTESIAN_POINT('Ctrl Pts',(38.4780486111932,85.7683326104205,107.));
#48343=CARTESIAN_POINT('Ctrl Pts',(38.5361377306736,85.847283140632,107.));
#48344=CARTESIAN_POINT('Ctrl Pts',(38.5937003927959,85.9255181480756,107.));
#48345=CARTESIAN_POINT('Ctrl Pts',(38.6473593102664,86.0063738621224,107.));
#48346=CARTESIAN_POINT('Ctrl Pts',(38.6968315394181,86.0896016134082,107.));
#48347=CARTESIAN_POINT('Ctrl Pts',(38.7448894802278,86.1704500896869,107.));
#48348=CARTESIAN_POINT('Ctrl Pts',(38.7889968935663,86.2535376194815,107.));
#48349=CARTESIAN_POINT('Ctrl Pts',(38.8288466283339,86.3386465795827,107.));
#48350=CARTESIAN_POINT('Ctrl Pts',(38.8496510436295,86.3830795516376,107.));
#48351=CARTESIAN_POINT('Ctrl Pts',(38.8692941732027,86.4280635917019,107.));
#48352=CARTESIAN_POINT('Ctrl Pts',(38.8877266169703,86.4735679687981,107.));
#48353=CARTESIAN_POINT('Ctrl Pts',(38.8947846967753,86.4909923282087,107.));
#48354=CARTESIAN_POINT('Ctrl Pts',(38.9016652173504,86.5084929807057,107.));
#48355=CARTESIAN_POINT('Ctrl Pts',(38.9083652431171,86.5260681921585,107.));
#48356=CARTESIAN_POINT('Ctrl Pts',(38.913606979836,86.5398180842369,107.));
#48357=CARTESIAN_POINT('Ctrl Pts',(38.9187383404309,86.5536141120902,107.));
#48358=CARTESIAN_POINT('Ctrl Pts',(38.9237527897203,86.5674407323754,107.));
#48359=CARTESIAN_POINT('Ctrl Pts',(38.9554364793356,86.6548039342482,107.));
#48360=CARTESIAN_POINT('Ctrl Pts',(38.9825113433306,86.7435280735438,107.));
#48361=CARTESIAN_POINT('Ctrl Pts',(39.0047261257503,86.8333895970977,107.));
#48362=CARTESIAN_POINT('Ctrl Pts',(39.0097100967495,86.8535503719762,107.));
#48363=CARTESIAN_POINT('Ctrl Pts',(39.0144492341345,86.8737684362943,107.));
#48364=CARTESIAN_POINT('Ctrl Pts',(39.0189403397705,86.8940413210693,107.));
#48365=CARTESIAN_POINT('Ctrl Pts',(39.0393060941569,86.9859724902492,107.));
#48366=CARTESIAN_POINT('Ctrl Pts',(39.0545756375306,87.0790312711289,107.));
#48367=CARTESIAN_POINT('Ctrl Pts',(39.0648587946489,87.1728260780746,107.));
#48368=CARTESIAN_POINT('Ctrl Pts',(39.0755926599919,87.2707318881325,107.));
#48369=CARTESIAN_POINT('Ctrl Pts',(39.0808934432669,87.3694408954707,107.));
#48370=CARTESIAN_POINT('Ctrl Pts',(39.0808285913654,87.4684930845029,107.));
#48371=CARTESIAN_POINT('Ctrl Pts',(39.0808032243523,87.5072376411785,107.));
#48372=CARTESIAN_POINT('Ctrl Pts',(39.0799563126054,87.5460344480642,107.));
#48373=CARTESIAN_POINT('Ctrl Pts',(39.0782896687133,87.5848547474918,107.));
#48374=CARTESIAN_POINT('Ctrl Pts',(39.0777566303355,87.5972705428099,107.));
#48375=CARTESIAN_POINT('Ctrl Pts',(39.077139745471,87.6096874298378,107.));
#48376=CARTESIAN_POINT('Ctrl Pts',(39.0764397752444,87.6220947992235,107.));
#48377=CARTESIAN_POINT('Ctrl Pts',(39.0712005660668,87.714962754302,107.));
#48378=CARTESIAN_POINT('Ctrl Pts',(39.0613049370046,87.8074474727188,107.));
#48379=CARTESIAN_POINT('Ctrl Pts',(39.0468763468412,87.8991773783878,107.));
#48380=CARTESIAN_POINT('Ctrl Pts',(39.032481744757,87.9906912045047,107.));
#48381=CARTESIAN_POINT('Ctrl Pts',(39.0135751022545,88.0814547150913,107.));
#48382=CARTESIAN_POINT('Ctrl Pts',(38.9902303316761,88.1710820012943,107.));
#48383=CARTESIAN_POINT('Ctrl Pts',(38.9672817085728,88.2591883634421,107.));
#48384=CARTESIAN_POINT('Ctrl Pts',(38.9400438369275,88.3461975214973,107.));
#48385=CARTESIAN_POINT('Ctrl Pts',(38.908546488776,88.4317137837883,107.));
#48386=CARTESIAN_POINT('Ctrl Pts',(38.8927050493307,88.4747237757455,107.));
#48387=CARTESIAN_POINT('Ctrl Pts',(38.87578555997,88.5173555992814,107.));
#48388=CARTESIAN_POINT('Ctrl Pts',(38.8577883909143,88.5595551232321,107.));
#48389=CARTESIAN_POINT('Ctrl Pts',(38.8522226770006,88.5726055355986,107.));
#48390=CARTESIAN_POINT('Ctrl Pts',(38.8465538797673,88.5856145826971,107.));
#48391=CARTESIAN_POINT('Ctrl Pts',(38.8407819692872,88.5985806059024,107.));
#48392=CARTESIAN_POINT('Ctrl Pts',(38.8351025158747,88.6113389334947,107.));
#48393=CARTESIAN_POINT('Ctrl Pts',(38.8293267074872,88.6240477399775,107.));
#48394=CARTESIAN_POINT('Ctrl Pts',(38.8234563337807,88.6367025399068,107.));
#48395=CARTESIAN_POINT('Ctrl Pts',(38.7859765367107,88.7174979640187,107.));
#48396=CARTESIAN_POINT('Ctrl Pts',(38.7446265820373,88.79613660999,107.));
#48397=CARTESIAN_POINT('Ctrl Pts',(38.6994761457792,88.8722708876746,107.));
#48398=CARTESIAN_POINT('Ctrl Pts',(38.6550831391013,88.9471279605575,107.));
#48399=CARTESIAN_POINT('Ctrl Pts',(38.6070156385787,89.0195646548357,107.));
#48400=CARTESIAN_POINT('Ctrl Pts',(38.5553036590933,89.0892164043883,107.));
#48401=CARTESIAN_POINT('Ctrl Pts',(38.5051691920445,89.1567433754613,107.));
#48402=CARTESIAN_POINT('Ctrl Pts',(38.4516087667327,89.2216531649094,107.));
#48403=CARTESIAN_POINT('Ctrl Pts',(38.3946220233629,89.2835732787236,107.));
#48404=CARTESIAN_POINT('Ctrl Pts',(38.3736544685896,89.306356005042,107.));
#48405=CARTESIAN_POINT('Ctrl Pts',(38.3522228215257,89.3287335608056,107.));
#48406=CARTESIAN_POINT('Ctrl Pts',(38.3303262530622,89.3506857817386,107.));
#48407=CARTESIAN_POINT('Ctrl Pts',(38.3112488181976,89.3698117039432,107.));
#48408=CARTESIAN_POINT('Ctrl Pts',(38.2918184498306,89.388614739825,107.));
#48409=CARTESIAN_POINT('Ctrl Pts',(38.2720452848187,89.4070897608438,107.));
#48410=CARTESIAN_POINT('Origin',(36.3549260746835,87.7685555885722,124.208423447177));
#48411=CARTESIAN_POINT('Ctrl Pts',(33.2781263393751,87.7704832126688,121.708423447178));
#48412=CARTESIAN_POINT('Ctrl Pts',(33.2772036629102,87.8937581312653,121.702019850418));
#48413=CARTESIAN_POINT('Ctrl Pts',(33.3397301729486,89.0296650804786,121.642966745928));
#48414=CARTESIAN_POINT('Ctrl Pts',(34.7524571937242,91.0220941552736,121.531264133707));
#48415=CARTESIAN_POINT('Ctrl Pts',(38.2031235999269,90.8887189946743,121.373315610515));
#48416=CARTESIAN_POINT('Ctrl Pts',(39.9780137505041,87.9267773350827,121.215367087322));
#48417=CARTESIAN_POINT('Ctrl Pts',(38.4679953904151,84.8211908407143,121.05741856413));
#48418=CARTESIAN_POINT('Ctrl Pts',(35.0421043825414,84.3879826953392,120.899470040937));
#48419=CARTESIAN_POINT('Ctrl Pts',(33.395557307013,86.3263540715381,120.783138335286));
#48420=CARTESIAN_POINT('Ctrl Pts',(33.2786796709839,87.5529959098163,120.719456137367));
#48421=CARTESIAN_POINT('Ctrl Pts',(33.2806115013714,87.7658718718852,120.708423447177));
#48422=CARTESIAN_POINT('Ctrl Pts',(33.2846474150427,87.7655400361928,121.791576552823));
#48423=CARTESIAN_POINT('Ctrl Pts',(33.2896323871427,88.4585586466148,121.755752019753));
#48424=CARTESIAN_POINT('Ctrl Pts',(33.8620199088269,90.1797490256915,121.667277978953));
#48425=CARTESIAN_POINT('Ctrl Pts',(36.7064604291151,91.377416630034,121.526154430423));
#48426=CARTESIAN_POINT('Ctrl Pts',(39.5688530544509,89.4482951162593,121.36820590723));
#48427=CARTESIAN_POINT('Ctrl Pts',(39.5184627418672,85.9950129791182,121.210257384038));
#48428=CARTESIAN_POINT('Ctrl Pts',(36.5992128862014,84.1503276493198,121.052308860845));
#48429=CARTESIAN_POINT('Ctrl Pts',(33.8243657798026,85.4187697348352,120.912748583773));
#48430=CARTESIAN_POINT('Ctrl Pts',(33.2888359933922,87.1075071762337,120.825837814433));
#48431=CARTESIAN_POINT('Ctrl Pts',(33.2844847704405,87.7707064707598,120.791576552823));
#48432=CARTESIAN_POINT('Ctrl Pts',(38.2683920713486,89.4045427919472,122.));
#48433=CARTESIAN_POINT('Ctrl Pts',(38.8095874576702,88.7715555857257,121.947350492269));
#48434=CARTESIAN_POINT('Ctrl Pts',(39.2049245857504,86.9365225932413,121.842051476808));
#48435=CARTESIAN_POINT('Ctrl Pts',(37.214127277114,84.9233560515254,121.684102953615));
#48436=CARTESIAN_POINT('Ctrl Pts',(34.4432236387825,85.4956001255505,121.526154430423));
#48437=CARTESIAN_POINT('Ctrl Pts',(33.4061067692024,88.125867342332,121.36820590723));
#48438=CARTESIAN_POINT('Ctrl Pts',(35.0423458216121,90.4335249530331,121.210257384038));
#48439=CARTESIAN_POINT('Ctrl Pts',(37.8687823524776,90.3242775260579,121.052308860845));
#48440=CARTESIAN_POINT('Ctrl Pts',(39.3225926515107,87.8981548229434,120.894360337653));
#48441=CARTESIAN_POINT('Ctrl Pts',(38.0857385042766,85.3543728155993,120.73641181446));
#48442=CARTESIAN_POINT('Ctrl Pts',(35.2795954711475,84.999532566378,120.578463291268));
#48443=CARTESIAN_POINT('Ctrl Pts',(33.4484287478634,87.1552444887491,120.420514768075));
#48444=CARTESIAN_POINT('Ctrl Pts',(34.2524914687833,89.8670448178538,120.262566244883));
#48445=CARTESIAN_POINT('Ctrl Pts',(36.9627693013253,90.6762000895379,120.10461772169));
#48446=CARTESIAN_POINT('Ctrl Pts',(39.1219333904769,88.8490867521255,119.946669198498));
#48447=CARTESIAN_POINT('Ctrl Pts',(38.7723364786591,86.0422866159873,119.788720675305));
#48448=CARTESIAN_POINT('Ctrl Pts',(36.2309468922132,84.800643054622,119.630772152113));
#48449=CARTESIAN_POINT('Ctrl Pts',(33.8019655491018,86.2499150368912,119.472823628921));
#48450=CARTESIAN_POINT('Ctrl Pts',(33.6876758263602,89.0760924562573,119.314875105728));
#48451=CARTESIAN_POINT('Ctrl Pts',(35.9917008041203,90.7167658497645,119.156926582536));
#48452=CARTESIAN_POINT('Ctrl Pts',(38.625051077446,89.6843867210575,118.998978059343));
#48453=CARTESIAN_POINT('Ctrl Pts',(39.2001480584847,86.9149817447435,118.841029536151));
#48454=CARTESIAN_POINT('Ctrl Pts',(37.1955687979013,84.9194862255556,118.683081012958));
#48455=CARTESIAN_POINT('Ctrl Pts',(34.4288043483479,85.5071552408685,118.525132489766));
#48456=CARTESIAN_POINT('Ctrl Pts',(33.4083958871456,88.1451671771827,118.367183966573));
#48457=CARTESIAN_POINT('Ctrl Pts',(35.0595167325978,90.44171683871,118.209235443381));
#48458=CARTESIAN_POINT('Ctrl Pts',(37.8851458302896,90.3145924959996,118.051286920188));
#48459=CARTESIAN_POINT('Ctrl Pts',(39.3233712151692,87.8790539231783,117.893338396996));
#48460=CARTESIAN_POINT('Ctrl Pts',(38.0701976723164,85.343329871199,117.735389873803));
#48461=CARTESIAN_POINT('Ctrl Pts',(35.2618395395329,85.0064842171713,117.577441350611));
#48462=CARTESIAN_POINT('Ctrl Pts',(33.4445497234387,87.1739246710306,117.419492827418));
#48463=CARTESIAN_POINT('Ctrl Pts',(34.2660096299264,89.8804988929231,117.261544304226));
#48464=CARTESIAN_POINT('Ctrl Pts',(36.9814265453518,90.6722383526224,117.103595781034));
#48465=CARTESIAN_POINT('Ctrl Pts',(39.1288145381736,88.831296961672,116.945647257841));
#48466=CARTESIAN_POINT('Ctrl Pts',(38.7612022251526,86.0268002895521,116.787698734649));
#48467=CARTESIAN_POINT('Ctrl Pts',(36.2118925100824,84.8015001739599,116.629750211456));
#48468=CARTESIAN_POINT('Ctrl Pts',(33.7922669778667,86.2663389638858,116.471801688264));
#48469=CARTESIAN_POINT('Ctrl Pts',(33.6961265089816,89.0931918795614,116.313853165071));
#48470=CARTESIAN_POINT('Ctrl Pts',(36.010638742585,90.7190373571888,116.155904641879));
#48471=CARTESIAN_POINT('Ctrl Pts',(38.6373058291762,89.6697707500582,115.997956118686));
#48472=CARTESIAN_POINT('Ctrl Pts',(39.1946086078113,86.8967301788536,115.840007595494));
#48473=CARTESIAN_POINT('Ctrl Pts',(37.1772575986997,84.9141471912696,115.682059072301));
#48474=CARTESIAN_POINT('Ctrl Pts',(34.4143236068453,85.5195694846129,115.524110549109));
#48475=CARTESIAN_POINT('Ctrl Pts',(33.4108748518238,88.1640790785956,115.366162025916));
#48476=CARTESIAN_POINT('Ctrl Pts',(35.0767078012988,90.4499795534774,115.208213502724));
#48477=CARTESIAN_POINT('Ctrl Pts',(37.9014623840002,90.3047144712031,115.050264979531));
#48478=CARTESIAN_POINT('Ctrl Pts',(39.3240195308199,87.8599912638331,114.892316456339));
#48479=CARTESIAN_POINT('Ctrl Pts',(38.0545899418562,85.3323661105944,114.734367933147));
#48480=CARTESIAN_POINT('Ctrl Pts',(35.2441268174668,85.0135598636845,114.576419409954));
#48481=CARTESIAN_POINT('Ctrl Pts',(33.4407915961636,87.192624451123,114.418470886762));
#48482=CARTESIAN_POINT('Ctrl Pts',(34.2796134771405,89.8938682847329,114.260522363569));
#48483=CARTESIAN_POINT('Ctrl Pts',(37.0000581725303,90.6681557351977,114.102573840377));
#48484=CARTESIAN_POINT('Ctrl Pts',(39.1355812156081,88.8134639200691,113.944625317184));
#48485=CARTESIAN_POINT('Ctrl Pts',(38.7499688122129,86.0113855002229,113.786676793992));
#48486=CARTESIAN_POINT('Ctrl Pts',(36.1928440006319,84.8024797575703,113.628728270799));
#48487=CARTESIAN_POINT('Ctrl Pts',(33.78267407609,86.2828247617688,113.470779747607));
#48488=CARTESIAN_POINT('Ctrl Pts',(33.7046868071648,89.1102367201694,113.312831224414));
#48489=CARTESIAN_POINT('Ctrl Pts',(36.0295908787149,90.7211872019379,113.154882701222));
#48490=CARTESIAN_POINT('Ctrl Pts',(38.6494664778272,89.6550764000991,112.996934178029));
#48491=CARTESIAN_POINT('Ctrl Pts',(39.1889520787008,86.8785145543856,112.838985654837));
#48492=CARTESIAN_POINT('Ctrl Pts',(37.1589124947367,84.9089258449949,112.681037131644));
#48493=CARTESIAN_POINT('Ctrl Pts',(34.3999228758519,85.5320764523986,112.523088608452));
#48494=CARTESIAN_POINT('Ctrl Pts',(33.4134751986133,88.1829746731326,112.365140085259));
#48495=CARTESIAN_POINT('Ctrl Pts',(35.093951570523,90.4581317138827,112.207191562067));
#48496=CARTESIAN_POINT('Ctrl Pts',(37.9177151745493,90.2947318815738,112.049243038874));
#48497=CARTESIAN_POINT('Ctrl Pts',(39.3245454318088,87.8409248345793,111.891294515682));
#48498=CARTESIAN_POINT('Ctrl Pts',(38.0389121348537,85.3215027932418,111.73334599249));
#48499=CARTESIAN_POINT('Ctrl Pts',(35.2264598932615,85.0207490976825,111.575397469297));
#48500=CARTESIAN_POINT('Ctrl Pts',(33.4371536176206,87.2113479766595,111.417448946105));
#48501=CARTESIAN_POINT('Ctrl Pts',(34.2933028887537,89.9071500506473,111.259500422912));
#48502=CARTESIAN_POINT('Ctrl Pts',(37.018663201149,90.6639535682966,111.10155189972));
#48503=CARTESIAN_POINT('Ctrl Pts',(39.1422332476006,88.795587797249,110.943603376527));
#48504=CARTESIAN_POINT('Ctrl Pts',(38.7386366525448,85.9960431584279,110.785654853335));
#48505=CARTESIAN_POINT('Ctrl Pts',(36.1738021736971,84.8035816313644,110.627706330142));
#48506=CARTESIAN_POINT('Ctrl Pts',(33.7731872274968,86.299371815953,110.46975780695));
#48507=CARTESIAN_POINT('Ctrl Pts',(33.7133563734736,89.1272262434396,110.311809283757));
#48508=CARTESIAN_POINT('Ctrl Pts',(36.0485564289157,90.7232153113506,110.153860760565));
#48509=CARTESIAN_POINT('Ctrl Pts',(38.6615325221239,89.6403042682848,109.995912237372));
#48510=CARTESIAN_POINT('Ctrl Pts',(39.1831787063092,86.8603356286082,109.83796371418));
#48511=CARTESIAN_POINT('Ctrl Pts',(37.1405342373388,84.9038223948635,109.680015190987));
#48512=CARTESIAN_POINT('Ctrl Pts',(34.3856027599713,85.5446756404848,109.522066667795));
#48513=CARTESIAN_POINT('Ctrl Pts',(33.4161967977053,88.2018531585721,109.364118144603));
#48514=CARTESIAN_POINT('Ctrl Pts',(35.1112473759147,90.466173030801,109.20616962141));
#48515=CARTESIAN_POINT('Ctrl Pts',(37.9339034359386,90.2846450423694,109.048221098218));
#48516=CARTESIAN_POINT('Ctrl Pts',(39.3249490937297,87.8218556194758,108.890272575025));
#48517=CARTESIAN_POINT('Ctrl Pts',(38.0231644919314,85.3107399599536,108.732324051833));
#48518=CARTESIAN_POINT('Ctrl Pts',(35.2088403298994,85.0280524599893,108.57437552864));
#48519=CARTESIAN_POINT('Ctrl Pts',(33.4336342212486,87.2300927536877,108.416427005448));
#48520=CARTESIAN_POINT('Ctrl Pts',(34.3070808309297,89.9203471848041,108.258478482255));
#48521=CARTESIAN_POINT('Ctrl Pts',(37.0372336025185,90.6596247405995,108.100529959063));
#48522=CARTESIAN_POINT('Ctrl Pts',(39.1487852954204,88.7776843129956,107.94258143587));
#48523=CARTESIAN_POINT('Ctrl Pts',(38.7271754942787,85.9807430805063,107.784632912678));
#48524=CARTESIAN_POINT('Ctrl Pts',(36.1548309967493,84.8048691322566,107.626684389485));
#48525=CARTESIAN_POINT('Ctrl Pts',(33.7636768703791,86.3158490815793,107.468735866293));
#48526=CARTESIAN_POINT('Ctrl Pts',(33.7224021344473,89.1444279263405,107.310787343101));
#48527=CARTESIAN_POINT('Ctrl Pts',(36.0669846911716,90.7245702197898,107.152838819908));
#48528=CARTESIAN_POINT('Ctrl Pts',(38.6746345709313,89.6266028442429,106.994890296716));
#48529=CARTESIAN_POINT('Ctrl Pts',(39.1749134210556,86.8398781501125,106.836941773523));
#48530=CARTESIAN_POINT('Ctrl Pts',(37.8096764711452,85.5515592459026,106.731642758061));
#48531=CARTESIAN_POINT('Ctrl Pts',(37.0051260726581,85.336468786537,106.678993250331));
#48532=CARTESIAN_POINT('Ctrl Pts',(38.4092576250256,89.5249809097991,122.10700224989));
#48533=CARTESIAN_POINT('Ctrl Pts',(38.9902947372387,88.8453944468204,122.054352742159));
#48534=CARTESIAN_POINT('Ctrl Pts',(39.4147357968929,86.8752699821318,121.949053726697));
#48535=CARTESIAN_POINT('Ctrl Pts',(37.2773799574915,84.7138981312874,121.791105203505));
#48536=CARTESIAN_POINT('Ctrl Pts',(34.3024879149346,85.3282696737212,121.633156680312));
#48537=CARTESIAN_POINT('Ctrl Pts',(33.1890205680971,88.1521719216224,121.47520815712));
#48538=CARTESIAN_POINT('Ctrl Pts',(34.9457162789828,90.6297146871132,121.317259633927));
#48539=CARTESIAN_POINT('Ctrl Pts',(37.9802294349607,90.5124246822634,121.159311110735));
#48540=CARTESIAN_POINT('Ctrl Pts',(39.5410663511752,87.9076956603232,121.001362587542));
#48541=CARTESIAN_POINT('Ctrl Pts',(38.2131574663228,85.1766454906377,120.84341406435));
#48542=CARTESIAN_POINT('Ctrl Pts',(35.2004317749455,84.7956826093651,120.685465541158));
#48543=CARTESIAN_POINT('Ctrl Pts',(33.2344582064914,87.1100937477359,120.527517017965));
#48544=CARTESIAN_POINT('Ctrl Pts',(34.0977144226554,90.0215314132171,120.369568494773));
#48545=CARTESIAN_POINT('Ctrl Pts',(37.0075175084107,90.8902550835844,120.21161997158));
#48546=CARTESIAN_POINT('Ctrl Pts',(39.3256349552013,88.9286333031928,120.053671448388));
#48547=CARTESIAN_POINT('Ctrl Pts',(38.9503014153834,85.9152021341922,119.895722925195));
#48548=CARTESIAN_POINT('Ctrl Pts',(36.2218197918553,84.5821512480842,119.737774402003));
#48549=CARTESIAN_POINT('Ctrl Pts',(33.614021682538,86.1381157456983,119.57982587881));
#48550=CARTESIAN_POINT('Ctrl Pts',(33.4913181781552,89.1723507149046,119.421877355618));
#48551=CARTESIAN_POINT('Ctrl Pts',(35.9649608835069,90.9338072142428,119.263928832425));
#48552=CARTESIAN_POINT('Ctrl Pts',(38.7921731564312,89.8254263913206,119.105980309233));
#48553=CARTESIAN_POINT('Ctrl Pts',(39.4096076312081,86.8521433392924,118.94803178604));
#48554=CARTESIAN_POINT('Ctrl Pts',(37.2574552400211,84.7097434164411,118.790083262848));
#48555=CARTESIAN_POINT('Ctrl Pts',(34.2870071050718,85.3406754536029,118.632134739656));
#48556=CARTESIAN_POINT('Ctrl Pts',(33.1914782063417,88.1728925718556,118.474186216463));
#48557=CARTESIAN_POINT('Ctrl Pts',(34.9641512782186,90.6385096430895,118.316237693271));
#48558=CARTESIAN_POINT('Ctrl Pts',(37.9977975594013,90.5020266595918,118.158289170078));
#48559=CARTESIAN_POINT('Ctrl Pts',(39.5419022311388,87.8871885903799,118.000340646886));
#48560=CARTESIAN_POINT('Ctrl Pts',(38.1964725492822,85.1647895866762,117.842392123693));
#48561=CARTESIAN_POINT('Ctrl Pts',(35.1813686870279,84.803146026837,117.684443600501));
#48562=CARTESIAN_POINT('Ctrl Pts',(33.2302936160184,87.1301491278129,117.526495077308));
#48563=CARTESIAN_POINT('Ctrl Pts',(34.112227763884,90.0359759504825,117.368546554116));
#48564=CARTESIAN_POINT('Ctrl Pts',(37.0275482615639,90.8860016914921,117.210598030923));
#48565=CARTESIAN_POINT('Ctrl Pts',(39.3330226792793,88.909533863816,117.052649507731));
#48566=CARTESIAN_POINT('Ctrl Pts',(38.9383474803212,85.8985757352649,116.894700984538));
#48567=CARTESIAN_POINT('Ctrl Pts',(36.201362664082,84.5830714668398,116.736752461346));
#48568=CARTESIAN_POINT('Ctrl Pts',(33.6036091218151,86.15574876947,116.578803938153));
#48569=CARTESIAN_POINT('Ctrl Pts',(33.5003909831914,89.1907089636779,116.420855414961));
#48570=CARTESIAN_POINT('Ctrl Pts',(35.9852929952633,90.9362459455173,116.262906891768));
#48571=CARTESIAN_POINT('Ctrl Pts',(38.8053300785636,89.8097344216618,116.104958368576));
#48572=CARTESIAN_POINT('Ctrl Pts',(39.4036603772148,86.8325481294921,115.947009845384));
#48573=CARTESIAN_POINT('Ctrl Pts',(37.2377960068232,84.7040113330902,115.789061322191));
#48574=CARTESIAN_POINT('Ctrl Pts',(34.2714603202359,85.3540036092337,115.631112798999));
#48575=CARTESIAN_POINT('Ctrl Pts',(33.1941396674596,88.1931967297645,115.473164275806));
#48576=CARTESIAN_POINT('Ctrl Pts',(34.9826079191403,90.6473806424528,115.315215752614));
#48577=CARTESIAN_POINT('Ctrl Pts',(38.0153153052819,90.4914214342938,115.157267229421));
#48578=CARTESIAN_POINT('Ctrl Pts',(39.5425982744958,87.8667225760403,114.999318706229));
#48579=CARTESIAN_POINT('Ctrl Pts',(38.1797158088073,85.1530186958635,114.841370183036));
#48580=CARTESIAN_POINT('Ctrl Pts',(35.1623519896598,84.810742568347,114.683421659844));
#48581=CARTESIAN_POINT('Ctrl Pts',(33.2262588229021,87.1502255484521,114.525473136651));
#48582=CARTESIAN_POINT('Ctrl Pts',(34.1268330992215,90.0503295702762,114.367524613459));
#48583=CARTESIAN_POINT('Ctrl Pts',(37.0475515120076,90.8816185199078,114.209576090267));
#48584=CARTESIAN_POINT('Ctrl Pts',(39.3402875060225,88.8903879892268,114.051627567074));
#48585=CARTESIAN_POINT('Ctrl Pts',(38.9262870859059,85.8820261398624,113.893679043881));
#48586=CARTESIAN_POINT('Ctrl Pts',(36.1809118413241,84.5841231654436,113.735730520689));
#48587=CARTESIAN_POINT('Ctrl Pts',(33.5933100097256,86.1734482189416,113.577781997497));
#48588=CARTESIAN_POINT('Ctrl Pts',(33.5095814734685,89.2090086114858,113.419833474304));
#48589=CARTESIAN_POINT('Ctrl Pts',(36.005640349889,90.9385540575528,113.261884951112));
#48590=CARTESIAN_POINT('Ctrl Pts',(38.8183859699355,89.7939583029403,113.103936427919));
#48591=CARTESIAN_POINT('Ctrl Pts',(39.397587425703,86.8129915070493,112.945987904727));
#48592=CARTESIAN_POINT('Ctrl Pts',(37.218100372863,84.6984056017074,112.788039381534));
#48593=CARTESIAN_POINT('Ctrl Pts',(34.2559994361233,85.3674313150648,112.630090858342));
#48594=CARTESIAN_POINT('Ctrl Pts',(33.1969314465981,88.2134833803179,112.472142335149));
#48595=CARTESIAN_POINT('Ctrl Pts',(35.0011211402929,90.656132948662,112.314193811957));
#48596=CARTESIAN_POINT('Ctrl Pts',(38.032764593884,90.4807039463087,112.156245288764));
#48597=CARTESIAN_POINT('Ctrl Pts',(39.5431628912675,87.8462525142588,111.998296765572));
#48598=CARTESIAN_POINT('Ctrl Pts',(38.1628838328947,85.141355642735,111.840348242379));
#48599=CARTESIAN_POINT('Ctrl Pts',(35.1433844616997,84.8184610594256,111.682399719187));
#48600=CARTESIAN_POINT('Ctrl Pts',(33.2223530236282,87.1703274626279,111.524451195995));
#48601=CARTESIAN_POINT('Ctrl Pts',(34.1415302980385,90.0645891133304,111.366502672802));
#48602=CARTESIAN_POINT('Ctrl Pts',(37.0675262057587,90.8771069978532,111.20855414961));
#48603=CARTESIAN_POINT('Ctrl Pts',(39.3474292473546,88.8711958618666,111.050605626417));
#48604=CARTESIAN_POINT('Ctrl Pts',(38.9141206752248,85.8655543254375,110.892657103225));
#48605=CARTESIAN_POINT('Ctrl Pts',(36.1604681930353,84.5853061569907,110.734708580032));
#48606=CARTESIAN_POINT('Ctrl Pts',(33.5831247582434,86.1912134342811,110.57676005684));
#48607=CARTESIAN_POINT('Ctrl Pts',(33.5188892759731,89.2272488696041,110.418811533647));
#48608=CARTESIAN_POINT('Ctrl Pts',(36.0260021061025,90.9407314723389,110.260863010455));
#48609=CARTESIAN_POINT('Ctrl Pts',(38.8313402923692,89.7780986762186,110.102914487262));
#48610=CARTESIAN_POINT('Ctrl Pts',(39.3913890291405,86.7934742849815,109.94496596407));
#48611=CARTESIAN_POINT('Ctrl Pts',(37.1983691447782,84.6929264457471,109.787017440877));
#48612=CARTESIAN_POINT('Ctrl Pts',(34.2406251018475,85.3809580302714,109.629068917685));
#48613=CARTESIAN_POINT('Ctrl Pts',(33.1998534043918,88.2337516622358,109.471120394492));
#48614=CARTESIAN_POINT('Ctrl Pts',(35.0196902284118,90.664766251308,109.3131718713));
#48615=CARTESIAN_POINT('Ctrl Pts',(38.0501446028181,90.469874534102,109.155223348107));
#48616=CARTESIAN_POINT('Ctrl Pts',(39.5435962699747,87.8257794615391,108.997274824915));
#48617=CARTESIAN_POINT('Ctrl Pts',(38.145976879881,85.1298004711073,108.839326301723));
#48618=CARTESIAN_POINT('Ctrl Pts',(35.1244677811938,84.826302080712,108.68137777853));
#48619=CARTESIAN_POINT('Ctrl Pts',(33.2185745363085,87.1904521927878,108.523429255338));
#48620=CARTESIAN_POINT('Ctrl Pts',(34.1563225448619,90.0787577942057,108.365480732145));
#48621=CARTESIAN_POINT('Ctrl Pts',(37.0874637230715,90.8724594904871,108.207532208953));
#48622=CARTESIAN_POINT('Ctrl Pts',(39.3544636438785,88.8519743587791,108.04958368576));
#48623=CARTESIAN_POINT('Ctrl Pts',(38.901815769326,85.849127886268,107.891635162568));
#48624=CARTESIAN_POINT('Ctrl Pts',(36.1401003958448,84.5866884411331,107.733686639375));
#48625=CARTESIAN_POINT('Ctrl Pts',(33.5729142675862,86.2089037233683,107.575738116183));
#48626=CARTESIAN_POINT('Ctrl Pts',(33.5286009678439,89.245716906122,107.41778959299));
#48627=CARTESIAN_POINT('Ctrl Pts',(36.0457870203034,90.9421861264375,107.259841069798));
#48628=CARTESIAN_POINT('Ctrl Pts',(38.845406887901,89.7633885806419,107.101892546605));
#48629=CARTESIAN_POINT('Ctrl Pts',(39.382515270057,86.771510767685,106.943944023413));
#48630=CARTESIAN_POINT('Ctrl Pts',(37.916772296426,85.388348393003,106.838645007951));
#48631=CARTESIAN_POINT('Ctrl Pts',(37.052992500844,85.1574234026335,106.78599550022));
#48632=CARTESIAN_POINT('Ctrl Pts',(38.5501231787026,89.645419027651,122.21400449978));
#48633=CARTESIAN_POINT('Ctrl Pts',(39.1710020168071,88.919233307915,122.161354992049));
#48634=CARTESIAN_POINT('Ctrl Pts',(39.6245470080353,86.8140173710224,122.056055976587));
#48635=CARTESIAN_POINT('Ctrl Pts',(37.3406326378691,84.5044402110492,121.898107453395));
#48636=CARTESIAN_POINT('Ctrl Pts',(34.1617521910867,85.160939221892,121.740158930202));
#48637=CARTESIAN_POINT('Ctrl Pts',(32.9719343669918,88.1784765009128,121.58221040701));
#48638=CARTESIAN_POINT('Ctrl Pts',(34.8490867363534,90.8259044211933,121.424261883817));
#48639=CARTESIAN_POINT('Ctrl Pts',(38.0916765174438,90.700571838469,121.266313360625));
#48640=CARTESIAN_POINT('Ctrl Pts',(39.7595400508396,87.9172364977028,121.108364837432));
#48641=CARTESIAN_POINT('Ctrl Pts',(38.3405764283689,84.9989181656761,120.95041631424));
#48642=CARTESIAN_POINT('Ctrl Pts',(35.1212680787434,84.5918326523521,120.792467791047));
#48643=CARTESIAN_POINT('Ctrl Pts',(33.0204876651193,87.0649430067228,120.634519267855));
#48644=CARTESIAN_POINT('Ctrl Pts',(33.9429373765276,90.1760180085803,120.476570744662));
#48645=CARTESIAN_POINT('Ctrl Pts',(37.0522657154962,91.104310077631,120.31862222147));
#48646=CARTESIAN_POINT('Ctrl Pts',(39.5293365199257,89.0081798542601,120.160673698278));
#48647=CARTESIAN_POINT('Ctrl Pts',(39.1282663521078,85.7881176523972,120.002725175085));
#48648=CARTESIAN_POINT('Ctrl Pts',(36.2126926914973,84.3636594415466,119.844776651893));
#48649=CARTESIAN_POINT('Ctrl Pts',(33.4260778159742,86.0263164545053,119.6868281287));
#48650=CARTESIAN_POINT('Ctrl Pts',(33.2949605299503,89.2686089735517,119.528879605508));
#48651=CARTESIAN_POINT('Ctrl Pts',(35.9382209628934,91.1508485787212,119.370931082315));
#48652=CARTESIAN_POINT('Ctrl Pts',(38.9592952354164,89.9664660615837,119.212982559123));
#48653=CARTESIAN_POINT('Ctrl Pts',(39.6190672039315,86.7893049338414,119.05503403593));
#48654=CARTESIAN_POINT('Ctrl Pts',(37.3193416821408,84.5000006073266,118.897085512738));
#48655=CARTESIAN_POINT('Ctrl Pts',(34.1452098617957,85.1741956663374,118.739136989545));
#48656=CARTESIAN_POINT('Ctrl Pts',(32.9745605255379,88.2006179665285,118.581188466353));
#48657=CARTESIAN_POINT('Ctrl Pts',(34.8687858238393,90.8353024474691,118.42323994316));
#48658=CARTESIAN_POINT('Ctrl Pts',(38.1104492885132,90.6894608231839,118.265291419968));
#48659=CARTESIAN_POINT('Ctrl Pts',(39.7604332471084,87.8953232575818,118.107342896775));
#48660=CARTESIAN_POINT('Ctrl Pts',(38.3227474262479,84.9862493021531,117.949394373583));
#48661=CARTESIAN_POINT('Ctrl Pts',(35.1008978345229,84.5998078365029,117.79144585039));
#48662=CARTESIAN_POINT('Ctrl Pts',(33.016037508598,87.0863735845948,117.633497327198));
#48663=CARTESIAN_POINT('Ctrl Pts',(33.9584458978417,90.1914530080422,117.475548804005));
#48664=CARTESIAN_POINT('Ctrl Pts',(37.0736699777759,91.0997650303614,117.317600280813));
#48665=CARTESIAN_POINT('Ctrl Pts',(39.537230820385,88.9877707659602,117.159651757621));
#48666=CARTESIAN_POINT('Ctrl Pts',(39.1154927354898,85.7703511809776,117.001703234428));
#48667=CARTESIAN_POINT('Ctrl Pts',(36.1908328180816,84.3646427597196,116.843754711236));
#48668=CARTESIAN_POINT('Ctrl Pts',(33.4149512657634,86.0451585750542,116.685806188043));
#48669=CARTESIAN_POINT('Ctrl Pts',(33.3046554574013,89.2882260477943,116.527857664851));
#48670=CARTESIAN_POINT('Ctrl Pts',(35.9599472479417,91.1534545338459,116.369909141658));
#48671=CARTESIAN_POINT('Ctrl Pts',(38.9733543279509,89.9496980932653,116.211960618466));
#48672=CARTESIAN_POINT('Ctrl Pts',(39.6127121466181,86.7683660801305,116.054012095273));
#48673=CARTESIAN_POINT('Ctrl Pts',(37.2983344149467,84.4938754749107,115.896063572081));
#48674=CARTESIAN_POINT('Ctrl Pts',(34.1285970336264,85.1884377338545,115.738115048889));
#48675=CARTESIAN_POINT('Ctrl Pts',(32.9774044830955,88.2223143809333,115.580166525696));
#48676=CARTESIAN_POINT('Ctrl Pts',(34.8885080369818,90.8447817314284,115.422218002503));
#48677=CARTESIAN_POINT('Ctrl Pts',(38.1291682265636,90.6781283973845,115.264269479311));
#48678=CARTESIAN_POINT('Ctrl Pts',(39.7611770181716,87.8734538882476,115.106320956119));
#48679=CARTESIAN_POINT('Ctrl Pts',(38.3048416757584,84.9736712811325,114.948372432926));
#48680=CARTESIAN_POINT('Ctrl Pts',(35.0805771618529,84.6079252730093,114.790423909734));
#48681=CARTESIAN_POINT('Ctrl Pts',(33.0117260496407,87.1078266457813,114.632475386541));
#48682=CARTESIAN_POINT('Ctrl Pts',(33.9740527213024,90.2067908558194,114.474526863349));
#48683=CARTESIAN_POINT('Ctrl Pts',(37.095044851485,91.0950813046181,114.316578340156));
#48684=CARTESIAN_POINT('Ctrl Pts',(39.5449937964367,88.9673120583842,114.158629816964));
#48685=CARTESIAN_POINT('Ctrl Pts',(39.1026053595989,85.752666779502,114.000681293771));
#48686=CARTESIAN_POINT('Ctrl Pts',(36.1689796820162,84.365766573317,113.842732770579));
#48687=CARTESIAN_POINT('Ctrl Pts',(33.403945943361,86.0640716761142,113.684784247386));
#48688=CARTESIAN_POINT('Ctrl Pts',(33.3144761397724,89.3077805028025,113.526835724194));
#48689=CARTESIAN_POINT('Ctrl Pts',(35.9816898210629,91.1559209131676,113.368887201001));
#48690=CARTESIAN_POINT('Ctrl Pts',(38.9873054620438,89.9328402057817,113.210938677809));
#48691=CARTESIAN_POINT('Ctrl Pts',(39.6062227727051,86.7474684597129,113.052990154616));
#48692=CARTESIAN_POINT('Ctrl Pts',(37.2772882509894,84.4878853584198,112.895041631424));
#48693=CARTESIAN_POINT('Ctrl Pts',(34.1120759963947,85.2027861777312,112.737093108232));
#48694=CARTESIAN_POINT('Ctrl Pts',(32.9803876945829,88.2439920875028,112.579144585039));
#48695=CARTESIAN_POINT('Ctrl Pts',(34.9082907100627,90.8541341834417,112.421196061847));
#48696=CARTESIAN_POINT('Ctrl Pts',(38.1478140132187,90.6666760110434,112.263247538654));
#48697=CARTESIAN_POINT('Ctrl Pts',(39.7617803507262,87.8515801939384,112.105299015462));
#48698=CARTESIAN_POINT('Ctrl Pts',(38.2868555309357,84.961208492228,111.947350492269));
#48699=CARTESIAN_POINT('Ctrl Pts',(35.0603090301378,84.6161730211687,111.789401969077));
#48700=CARTESIAN_POINT('Ctrl Pts',(33.0075524296359,87.1293069485963,111.631453445884));
#48701=CARTESIAN_POINT('Ctrl Pts',(33.9897577073232,90.2220281760135,111.473504922692));
#48702=CARTESIAN_POINT('Ctrl Pts',(37.1163892103684,91.0902604274099,111.315556399499));
#48703=CARTESIAN_POINT('Ctrl Pts',(39.5526252471086,88.9468039264842,111.157607876307));
#48704=CARTESIAN_POINT('Ctrl Pts',(39.0896046979049,85.735065492447,110.999659353114));
#48705=CARTESIAN_POINT('Ctrl Pts',(36.1471342123734,84.3670306826171,110.841710829922));
#48706=CARTESIAN_POINT('Ctrl Pts',(33.3930622889901,86.0830550526093,110.683762306729));
#48707=CARTESIAN_POINT('Ctrl Pts',(33.3244221784725,89.3272714957683,110.525813783537));
#48708=CARTESIAN_POINT('Ctrl Pts',(36.0034477832893,91.1582476333273,110.367865260344));
#48709=CARTESIAN_POINT('Ctrl Pts',(39.0011480626143,89.9158930841524,110.209916737152));
#48710=CARTESIAN_POINT('Ctrl Pts',(39.5995993519719,86.7266129413549,110.05196821396));
#48711=CARTESIAN_POINT('Ctrl Pts',(37.2562040522177,84.4820304966307,109.894019690767));
#48712=CARTESIAN_POINT('Ctrl Pts',(34.0956474437237,85.217240420058,109.736071167575));
#48713=CARTESIAN_POINT('Ctrl Pts',(32.9835100110784,88.2656501658994,109.578122644382));
#48714=CARTESIAN_POINT('Ctrl Pts',(34.9281330809089,90.863359471815,109.42017412119));
#48715=CARTESIAN_POINT('Ctrl Pts',(38.1663857696977,90.6551040258348,109.262225597997));
#48716=CARTESIAN_POINT('Ctrl Pts',(39.7622434462196,87.8297033036023,109.104277074805));
#48717=CARTESIAN_POINT('Ctrl Pts',(38.2687892678307,84.9488609822609,108.946328551612));
#48718=CARTESIAN_POINT('Ctrl Pts',(35.0400952324881,84.6245517014347,108.78838002842));
#48719=CARTESIAN_POINT('Ctrl Pts',(33.0035148513684,87.1508116318879,108.630431505227));
#48720=CARTESIAN_POINT('Ctrl Pts',(34.0055642587942,90.2371684036073,108.472482982035));
#48721=CARTESIAN_POINT('Ctrl Pts',(37.1376938436244,91.0852942403748,108.314534458842));
#48722=CARTESIAN_POINT('Ctrl Pts',(39.5601419923366,88.9262644045625,108.15658593565));
#48723=CARTESIAN_POINT('Ctrl Pts',(39.0764560443734,85.7175126920297,107.998637412457));
#48724=CARTESIAN_POINT('Ctrl Pts',(36.1253697949403,84.3685077500094,107.840688889265));
#48725=CARTESIAN_POINT('Ctrl Pts',(33.3821516647933,86.1019583651574,107.682740366072));
#48726=CARTESIAN_POINT('Ctrl Pts',(33.3347998012407,89.3470058859034,107.52479184288));
#48727=CARTESIAN_POINT('Ctrl Pts',(36.0245893494351,91.1598020330852,107.366843319687));
#48728=CARTESIAN_POINT('Ctrl Pts',(39.0161792048708,89.9001743170408,107.208894796495));
#48729=CARTESIAN_POINT('Ctrl Pts',(39.5901171190583,86.7031433852574,107.050946273303));
#48730=CARTESIAN_POINT('Ctrl Pts',(38.0238681217067,85.2251375401034,106.945647257841));
#48731=CARTESIAN_POINT('Ctrl Pts',(37.1008589290298,84.9783780187299,106.89299775011));
#48732=CARTESIAN_POINT('Ctrl Pts',(38.6909887323797,89.7658571455029,122.321006749669));
#48733=CARTESIAN_POINT('Ctrl Pts',(39.3517092963755,88.9930721690097,122.268357241939));
#48734=CARTESIAN_POINT('Ctrl Pts',(39.8343582191777,86.7527647599131,122.163058226477));
#48735=CARTESIAN_POINT('Ctrl Pts',(37.4038853182466,84.2949822908111,122.005109703285));
#48736=CARTESIAN_POINT('Ctrl Pts',(34.0210164672389,84.9936087700628,121.847161180092));
#48737=CARTESIAN_POINT('Ctrl Pts',(32.7548481658866,88.204781080203,121.6892126569));
#48738=CARTESIAN_POINT('Ctrl Pts',(34.7524571937242,91.0220941552736,121.531264133707));
#48739=CARTESIAN_POINT('Ctrl Pts',(38.2031235999269,90.8887189946743,121.373315610515));
#48740=CARTESIAN_POINT('Ctrl Pts',(39.9780137505041,87.9267773350827,121.215367087322));
#48741=CARTESIAN_POINT('Ctrl Pts',(38.4679953904151,84.8211908407143,121.05741856413));
#48742=CARTESIAN_POINT('Ctrl Pts',(35.0421043825414,84.3879826953392,120.899470040937));
#48743=CARTESIAN_POINT('Ctrl Pts',(32.8065171237473,87.0197922657097,120.741521517745));
#48744=CARTESIAN_POINT('Ctrl Pts',(33.7881603303997,90.3305046039434,120.583572994552));
#48745=CARTESIAN_POINT('Ctrl Pts',(37.0970139225816,91.3183650716777,120.42562447136));
#48746=CARTESIAN_POINT('Ctrl Pts',(39.7330380846501,89.0877264053273,120.267675948167));
#48747=CARTESIAN_POINT('Ctrl Pts',(39.3062312888321,85.6610331706022,120.109727424975));
#48748=CARTESIAN_POINT('Ctrl Pts',(36.2035655911394,84.1451676350087,119.951778901782));
#48749=CARTESIAN_POINT('Ctrl Pts',(33.2381339494103,85.9145171633124,119.79383037859));
#48750=CARTESIAN_POINT('Ctrl Pts',(33.0986028817453,89.3648672321989,119.635881855398));
#48751=CARTESIAN_POINT('Ctrl Pts',(35.91148104228,91.3678899431996,119.477933332205));
#48752=CARTESIAN_POINT('Ctrl Pts',(39.1264173144016,90.1075057318468,119.319984809013));
#48753=CARTESIAN_POINT('Ctrl Pts',(39.8285267766549,86.7264665283904,119.16203628582));
#48754=CARTESIAN_POINT('Ctrl Pts',(37.3812281242605,84.2902577982121,119.004087762628));
#48755=CARTESIAN_POINT('Ctrl Pts',(34.0034126185196,85.0077158790718,118.846139239435));
#48756=CARTESIAN_POINT('Ctrl Pts',(32.757642844734,88.2283433612014,118.688190716243));
#48757=CARTESIAN_POINT('Ctrl Pts',(34.7734203694599,91.0320952518487,118.53024219305));
#48758=CARTESIAN_POINT('Ctrl Pts',(38.223101017625,90.876894986776,118.372293669858));
#48759=CARTESIAN_POINT('Ctrl Pts',(39.9789642630779,87.9034579247835,118.214345146665));
#48760=CARTESIAN_POINT('Ctrl Pts',(38.4490223032137,84.8077090176302,118.056396623473));
#48761=CARTESIAN_POINT('Ctrl Pts',(35.020426982018,84.3964696461687,117.89844810028));
#48762=CARTESIAN_POINT('Ctrl Pts',(32.8017814011777,87.042598041377,117.740499577088));
#48763=CARTESIAN_POINT('Ctrl Pts',(33.8046640317993,90.3469300656019,117.582551053895));
#48764=CARTESIAN_POINT('Ctrl Pts',(37.1197916939879,91.3135283692309,117.424602530703));
#48765=CARTESIAN_POINT('Ctrl Pts',(39.7414389614906,89.0660076681044,117.26665400751));
#48766=CARTESIAN_POINT('Ctrl Pts',(39.2926379906584,85.6421266266902,117.108705484318));
#48767=CARTESIAN_POINT('Ctrl Pts',(36.1803029720811,84.1462140525996,116.950756961126));
#48768=CARTESIAN_POINT('Ctrl Pts',(33.2262934097118,85.9345683806384,116.792808437933));
#48769=CARTESIAN_POINT('Ctrl Pts',(33.1089199316111,89.3857431319108,116.634859914741));
#48770=CARTESIAN_POINT('Ctrl Pts',(35.93460150062,91.3706631221744,116.476911391548));
#48771=CARTESIAN_POINT('Ctrl Pts',(39.1413785773383,90.0896617648689,116.318962868356));
#48772=CARTESIAN_POINT('Ctrl Pts',(39.8217639160215,86.7041840307689,116.161014345163));
#48773=CARTESIAN_POINT('Ctrl Pts',(37.3588728230703,84.2837396167312,116.003065821971));
#48774=CARTESIAN_POINT('Ctrl Pts',(33.9857337470169,85.0228718584753,115.845117298778));
#48775=CARTESIAN_POINT('Ctrl Pts',(32.7606692987314,88.2514320321021,115.687168775586));
#48776=CARTESIAN_POINT('Ctrl Pts',(34.7944081548233,91.0421828204038,115.529220252393));
#48777=CARTESIAN_POINT('Ctrl Pts',(38.2430211478453,90.8648353604754,115.371271729201));
#48778=CARTESIAN_POINT('Ctrl Pts',(39.9797557618474,87.8801852004548,115.213323206008));
#48779=CARTESIAN_POINT('Ctrl Pts',(38.4299675427095,84.7943238664015,115.055374682816));
#48780=CARTESIAN_POINT('Ctrl Pts',(34.9988023340458,84.4051079776717,114.897426159623));
#48781=CARTESIAN_POINT('Ctrl Pts',(32.7971932763793,87.0654277431103,114.739477636431));
#48782=CARTESIAN_POINT('Ctrl Pts',(33.8212723433833,90.3632521413627,114.581529113238));
#48783=CARTESIAN_POINT('Ctrl Pts',(37.1425381909624,91.3085440893281,114.423580590046));
#48784=CARTESIAN_POINT('Ctrl Pts',(39.749700086851,89.0442361275419,114.265632066853));
#48785=CARTESIAN_POINT('Ctrl Pts',(39.2789236332919,85.6233074191414,114.107683543661));
#48786=CARTESIAN_POINT('Ctrl Pts',(36.1570475227083,84.1474099811903,113.949735020469));
#48787=CARTESIAN_POINT('Ctrl Pts',(33.2145818769966,85.954695133287,113.791786497276));
#48788=CARTESIAN_POINT('Ctrl Pts',(33.1193708060762,89.4065523941189,113.633837974084));
#48789=CARTESIAN_POINT('Ctrl Pts',(35.9577392922369,91.3732877687825,113.475889450891));
#48790=CARTESIAN_POINT('Ctrl Pts',(39.1562249541521,90.071722108623,113.317940927699));
#48791=CARTESIAN_POINT('Ctrl Pts',(39.8148581197072,86.6819454123766,113.159992404506));
#48792=CARTESIAN_POINT('Ctrl Pts',(37.3364761291159,84.2773651151324,113.002043881314));
#48793=CARTESIAN_POINT('Ctrl Pts',(33.9681525566661,85.0381410403975,112.844095358121));
#48794=CARTESIAN_POINT('Ctrl Pts',(32.7638439425676,88.2745007946881,112.686146834929));
#48795=CARTESIAN_POINT('Ctrl Pts',(34.8154602798326,91.0521354182212,112.528198311736));
#48796=CARTESIAN_POINT('Ctrl Pts',(38.2628634325534,90.8526480757781,112.370249788544));
#48797=CARTESIAN_POINT('Ctrl Pts',(39.9803978101849,87.856907873618,112.212301265351));
#48798=CARTESIAN_POINT('Ctrl Pts',(38.4108272289767,84.7810613417211,112.054352742159));
#48799=CARTESIAN_POINT('Ctrl Pts',(34.977233598576,84.4138849829118,111.896404218966));
#48800=CARTESIAN_POINT('Ctrl Pts',(32.7927518356436,87.0882864345648,111.738455695774));
#48801=CARTESIAN_POINT('Ctrl Pts',(33.837985116608,90.3794672386964,111.580507172581));
#48802=CARTESIAN_POINT('Ctrl Pts',(37.1652522149781,91.3034138569667,111.422558649389));
#48803=CARTESIAN_POINT('Ctrl Pts',(39.7578212468625,89.0224119911016,111.264610126197));
#48804=CARTESIAN_POINT('Ctrl Pts',(39.2650887205849,85.6045766594567,111.106661603004));
#48805=CARTESIAN_POINT('Ctrl Pts',(36.1338002317116,84.1487552082432,110.948713079812));
#48806=CARTESIAN_POINT('Ctrl Pts',(33.2029998197368,85.9748966709376,110.790764556619));
#48807=CARTESIAN_POINT('Ctrl Pts',(33.129955080972,89.4272941219325,110.632816033427));
#48808=CARTESIAN_POINT('Ctrl Pts',(35.980893460476,91.3757637943158,110.474867510234));
#48809=CARTESIAN_POINT('Ctrl Pts',(39.1709558328596,90.0536874920861,110.316918987042));
#48810=CARTESIAN_POINT('Ctrl Pts',(39.8078096748032,86.6597515977284,110.158970463849));
#48811=CARTESIAN_POINT('Ctrl Pts',(37.3140389596571,84.2711345475141,110.001021940657));
#48812=CARTESIAN_POINT('Ctrl Pts',(33.9506697855998,85.0535228098446,109.843073417464));
#48813=CARTESIAN_POINT('Ctrl Pts',(32.7671666177649,88.2975486695631,109.685124894272));
#48814=CARTESIAN_POINT('Ctrl Pts',(34.836575933406,91.0619526923221,109.527176371079));
#48815=CARTESIAN_POINT('Ctrl Pts',(38.2826269365773,90.8403335175675,109.369227847887));
#48816=CARTESIAN_POINT('Ctrl Pts',(39.9808906224645,87.8336271456654,109.211279324694));
#48817=CARTESIAN_POINT('Ctrl Pts',(38.3916016557803,84.7679214934147,109.053330801502));
#48818=CARTESIAN_POINT('Ctrl Pts',(34.9557226837823,84.4228013221572,108.89538227831));
#48819=CARTESIAN_POINT('Ctrl Pts',(32.7884551664283,87.1111710709882,108.737433755117));
#48820=CARTESIAN_POINT('Ctrl Pts',(33.8548059727263,90.3955790130086,108.579485231925));
#48821=CARTESIAN_POINT('Ctrl Pts',(37.1879239641774,91.2981289902626,108.421536708732));
#48822=CARTESIAN_POINT('Ctrl Pts',(39.7658203407947,89.0005544503459,108.26358818554));
#48823=CARTESIAN_POINT('Ctrl Pts',(39.2510963194207,85.5858974977915,108.105639662347));
#48824=CARTESIAN_POINT('Ctrl Pts',(36.1106391940357,84.1503270588856,107.947691139155));
#48825=CARTESIAN_POINT('Ctrl Pts',(33.1913890620005,85.9950130069465,107.789742615962));
#48826=CARTESIAN_POINT('Ctrl Pts',(33.1409986346373,89.4482948656848,107.63179409277));
#48827=CARTESIAN_POINT('Ctrl Pts',(36.0033916785668,91.377417939733,107.473845569577));
#48828=CARTESIAN_POINT('Ctrl Pts',(39.1869515218405,90.0369600534397,107.315897046385));
#48829=CARTESIAN_POINT('Ctrl Pts',(39.7977189680597,86.63477600283,107.157948523192));
#48830=CARTESIAN_POINT('Ctrl Pts',(38.1309639469874,85.0619266872038,107.052649507731));
#48831=CARTESIAN_POINT('Ctrl Pts',(37.1487253572157,84.7993326348264,107.));
#48832=CARTESIAN_POINT('Ctrl Pts',(38.2683920713486,89.4045427919472,122.));
#48833=CARTESIAN_POINT('Ctrl Pts',(38.3300002321833,89.3466462487923,122.));
#48834=CARTESIAN_POINT('Ctrl Pts',(38.3882392376497,89.285598943331,122.));
#48835=CARTESIAN_POINT('Ctrl Pts',(38.4431114755178,89.2217856950428,122.));
#48836=CARTESIAN_POINT('Ctrl Pts',(38.4994366457555,89.1562827701958,122.));
#48837=CARTESIAN_POINT('Ctrl Pts',(38.5522148311301,89.08786505576,122.));
#48838=CARTESIAN_POINT('Ctrl Pts',(38.6014231063109,89.0169002051877,122.));
#48839=CARTESIAN_POINT('Ctrl Pts',(38.6519809945774,88.9439890337863,122.));
#48840=CARTESIAN_POINT('Ctrl Pts',(38.6987709992573,88.8683885355143,122.));
#48841=CARTESIAN_POINT('Ctrl Pts',(38.7417341886229,88.7904544724489,122.));
#48842=CARTESIAN_POINT('Ctrl Pts',(38.7606441828022,88.7561522546505,122.));
#48843=CARTESIAN_POINT('Ctrl Pts',(38.778812335652,88.7213974646771,122.));
#48844=CARTESIAN_POINT('Ctrl Pts',(38.7962311971065,88.6862183602815,122.));
#48845=CARTESIAN_POINT('Ctrl Pts',(38.8061620426653,88.6661620406672,122.));
#48846=CARTESIAN_POINT('Ctrl Pts',(38.8158493123712,88.6459677823628,122.));
#48847=CARTESIAN_POINT('Ctrl Pts',(38.8252913913176,88.6256406734547,122.));
#48848=CARTESIAN_POINT('Ctrl Pts',(38.8337969724246,88.6073296770662,122.));
#48849=CARTESIAN_POINT('Ctrl Pts',(38.8421059629712,88.5889051485111,122.));
#48850=CARTESIAN_POINT('Ctrl Pts',(38.8502035219805,88.5704025618327,122.));
#48851=CARTESIAN_POINT('Ctrl Pts',(38.8867651008279,88.4868608697069,122.));
#48852=CARTESIAN_POINT('Ctrl Pts',(38.9190665018293,88.4016356337446,122.));
#48853=CARTESIAN_POINT('Ctrl Pts',(38.9470826910293,88.3151256326902,122.));
#48854=CARTESIAN_POINT('Ctrl Pts',(38.9755619804946,88.2271856439894,122.));
#48855=CARTESIAN_POINT('Ctrl Pts',(38.9996137137859,88.1379173104662,122.));
#48856=CARTESIAN_POINT('Ctrl Pts',(39.0191725198821,88.0477023902482,122.));
#48857=CARTESIAN_POINT('Ctrl Pts',(39.0381409703695,87.9602104830752,122.));
#48858=CARTESIAN_POINT('Ctrl Pts',(39.0528837825619,87.871827352317,122.));
#48859=CARTESIAN_POINT('Ctrl Pts',(39.0633005852989,87.7828793552042,122.));
#48860=CARTESIAN_POINT('Ctrl Pts',(39.0676694118452,87.7455743988912,122.));
#48861=CARTESIAN_POINT('Ctrl Pts',(39.0712767865467,87.7081698916346,122.));
#48862=CARTESIAN_POINT('Ctrl Pts',(39.0741129699685,87.6706892912553,122.));
#48863=CARTESIAN_POINT('Ctrl Pts',(39.0758920905351,87.6471779391791,122.));
#48864=CARTESIAN_POINT('Ctrl Pts',(39.077367720881,87.6236366391684,122.));
#48865=CARTESIAN_POINT('Ctrl Pts',(39.0785371609356,87.6000711486457,122.));
#48866=CARTESIAN_POINT('Ctrl Pts',(39.0792215402202,87.5862801608281,122.));
#48867=CARTESIAN_POINT('Ctrl Pts',(39.0798007649429,87.5724858346905,122.));
#48868=CARTESIAN_POINT('Ctrl Pts',(39.0802743343143,87.5586971611392,122.));
#48869=CARTESIAN_POINT('Ctrl Pts',(39.0836016907244,87.4618162518133,122.));
#48870=CARTESIAN_POINT('Ctrl Pts',(39.0817231359907,87.3651003513936,122.));
#48871=CARTESIAN_POINT('Ctrl Pts',(39.0745742900295,87.2689692279916,122.));
#48872=CARTESIAN_POINT('Ctrl Pts',(39.0674254440683,87.1728381045895,122.));
#48873=CARTESIAN_POINT('Ctrl Pts',(39.0550067371896,87.0772907141668,122.));
#48874=CARTESIAN_POINT('Ctrl Pts',(39.0372013263777,86.9827280393604,122.));
#48875=CARTESIAN_POINT('Ctrl Pts',(39.0201432921301,86.8921346033293,122.));
#48876=CARTESIAN_POINT('Ctrl Pts',(38.9981414058761,86.802443982858,122.));
#48877=CARTESIAN_POINT('Ctrl Pts',(38.9714702759697,86.7138955165579,122.));
#48878=CARTESIAN_POINT('Ctrl Pts',(38.9626009237809,86.6844491625357,122.));
#48879=CARTESIAN_POINT('Ctrl Pts',(38.9532147870399,86.6551291509939,122.));
#48880=CARTESIAN_POINT('Ctrl Pts',(38.9433207158183,86.6259444580485,122.));
#48881=CARTESIAN_POINT('Ctrl Pts',(38.9340003533245,86.5984520424969,122.));
#48882=CARTESIAN_POINT('Ctrl Pts',(38.9242292476095,86.571079706562,122.));
#48883=CARTESIAN_POINT('Ctrl Pts',(38.9140143220638,86.543835078612,122.));
#48884=CARTESIAN_POINT('Ctrl Pts',(38.9088566065269,86.5300787335221,122.));
#48885=CARTESIAN_POINT('Ctrl Pts',(38.9035888157279,86.5163632215208,122.));
#48886=CARTESIAN_POINT('Ctrl Pts',(38.8982136191598,86.502692859895,122.));
#48887=CARTESIAN_POINT('Ctrl Pts',(38.863962295366,86.4155838627646,122.));
#48888=CARTESIAN_POINT('Ctrl Pts',(38.8253374735071,86.3302636867753,122.));
#48889=CARTESIAN_POINT('Ctrl Pts',(38.7826691385711,86.2469667458681,122.));
#48890=CARTESIAN_POINT('Ctrl Pts',(38.7384393433969,86.1606215289644,122.));
#48891=CARTESIAN_POINT('Ctrl Pts',(38.6898645431327,86.0764496078788,122.));
#48892=CARTESIAN_POINT('Ctrl Pts',(38.6372564475687,85.994715560652,122.));
#48893=CARTESIAN_POINT('Ctrl Pts',(38.5840854062126,85.9121068982645,122.));
#48894=CARTESIAN_POINT('Ctrl Pts',(38.5267938741405,85.8319877413674,122.));
#48895=CARTESIAN_POINT('Ctrl Pts',(38.465652167204,85.7546466173903,122.));
#48896=CARTESIAN_POINT('Ctrl Pts',(38.4429632638252,85.7259463180847,122.));
#48897=CARTESIAN_POINT('Ctrl Pts',(38.4197436959574,85.6976287837773,122.));
#48898=CARTESIAN_POINT('Ctrl Pts',(38.3960056824848,85.6697096466582,122.));
#48899=CARTESIAN_POINT('Ctrl Pts',(38.3752500837481,85.6452982354931,122.));
#48900=CARTESIAN_POINT('Ctrl Pts',(38.3540981153553,85.621191407387,122.));
#48901=CARTESIAN_POINT('Ctrl Pts',(38.3325574553569,85.5973999946169,122.));
#48902=CARTESIAN_POINT('Ctrl Pts',(38.3207944345455,85.5844078725757,122.));
#48903=CARTESIAN_POINT('Ctrl Pts',(38.3089201790621,85.5715150612789,122.));
#48904=CARTESIAN_POINT('Ctrl Pts',(38.2969420121577,85.5587291809691,122.));
#48905=CARTESIAN_POINT('Ctrl Pts',(38.227931255996,85.4850648819642,122.));
#48906=CARTESIAN_POINT('Ctrl Pts',(38.1554181021943,85.4148851154279,122.));
#48907=CARTESIAN_POINT('Ctrl Pts',(38.0797110708892,85.3484810946605,122.));
#48908=CARTESIAN_POINT('Ctrl Pts',(38.0175169755689,85.2939295170056,122.));
#48909=CARTESIAN_POINT('Ctrl Pts',(37.9531663080692,85.2419261717527,122.));
#48910=CARTESIAN_POINT('Ctrl Pts',(37.8868078351083,85.192645848132,122.));
#48911=CARTESIAN_POINT('Ctrl Pts',(37.8621902138447,85.1743638671202,122.));
#48912=CARTESIAN_POINT('Ctrl Pts',(37.8372960861632,85.1564567893229,122.));
#48913=CARTESIAN_POINT('Ctrl Pts',(37.8121324405853,85.138934103667,122.));
#48914=CARTESIAN_POINT('Ctrl Pts',(37.7953216774585,85.1272279414182,122.));
#48915=CARTESIAN_POINT('Ctrl Pts',(37.7783894916928,85.1156927037062,122.));
#48916=CARTESIAN_POINT('Ctrl Pts',(37.7613530274051,85.1043410428558,122.));
#48917=CARTESIAN_POINT('Ctrl Pts',(37.6764425826325,85.0477638942505,122.));
#48918=CARTESIAN_POINT('Ctrl Pts',(37.5888628573917,84.9956860424815,122.));
#48919=CARTESIAN_POINT('Ctrl Pts',(37.4989042083555,84.9484154024461,122.));
#48920=CARTESIAN_POINT('Ctrl Pts',(37.4154461766131,84.9045606467465,122.));
#48921=CARTESIAN_POINT('Ctrl Pts',(37.3299397994821,84.864843173691,122.));
#48922=CARTESIAN_POINT('Ctrl Pts',(37.2425892169811,84.8295379073505,122.));
#48923=CARTESIAN_POINT('Ctrl Pts',(37.2121590462802,84.8172386730395,122.));
#48924=CARTESIAN_POINT('Ctrl Pts',(37.1815048545845,84.805475196943,122.));
#48925=CARTESIAN_POINT('Ctrl Pts',(37.1506395481981,84.7942437566138,122.));
#48926=CARTESIAN_POINT('Ctrl Pts',(33.836758858704,87.7663573595953,120.387416697508));
#48927=CARTESIAN_POINT('Ctrl Pts',(33.8351764988534,87.5919909257225,120.398449387697));
#48928=CARTESIAN_POINT('Ctrl Pts',(33.8517620939745,87.4179235371324,120.409482077886));
#48929=CARTESIAN_POINT('Ctrl Pts',(33.8876336552307,87.2479258898714,120.420514768075));
#48930=CARTESIAN_POINT('Ctrl Pts',(34.0588176556247,86.4366738479587,120.473164275806));
#48931=CARTESIAN_POINT('Ctrl Pts',(34.6692065633861,85.7181032071684,120.525813783537));
#48932=CARTESIAN_POINT('Ctrl Pts',(35.4420915227883,85.4179579283101,120.578463291268));
#48933=CARTESIAN_POINT('Ctrl Pts',(36.2149764821905,85.1178126494518,120.631112798999));
#48934=CARTESIAN_POINT('Ctrl Pts',(37.1503574932336,85.2360927325255,120.683762306729));
#48935=CARTESIAN_POINT('Ctrl Pts',(37.8241903566274,85.7191964419531,120.73641181446));
#48936=CARTESIAN_POINT('Ctrl Pts',(38.4980232200213,86.2023001513807,120.789061322191));
#48937=CARTESIAN_POINT('Ctrl Pts',(38.910307935766,87.050227487162,120.841710829922));
#48938=CARTESIAN_POINT('Ctrl Pts',(38.8741485771328,87.8785449389051,120.894360337653));
#48939=CARTESIAN_POINT('Ctrl Pts',(38.8379892184997,88.7068623906482,120.947009845384));
#48940=CARTESIAN_POINT('Ctrl Pts',(38.3533857854887,89.5155699583531,120.999659353114));
#48941=CARTESIAN_POINT('Ctrl Pts',(37.6400113138389,89.9381316467014,121.052308860845));
#48942=CARTESIAN_POINT('Ctrl Pts',(36.9266368421891,90.3606933350496,121.104958368576));
#48943=CARTESIAN_POINT('Ctrl Pts',(35.9844913319006,90.3971091440414,121.157607876307));
#48944=CARTESIAN_POINT('Ctrl Pts',(35.2407120680214,90.0307074467537,121.210257384038));
#48945=CARTESIAN_POINT('Ctrl Pts',(34.4969328041422,89.6643057494661,121.262906891768));
#48946=CARTESIAN_POINT('Ctrl Pts',(33.9515197866723,88.895086545899,121.315556399499));
#48947=CARTESIAN_POINT('Ctrl Pts',(33.851666089534,88.0720990746519,121.36820590723));
#48948=CARTESIAN_POINT('Ctrl Pts',(33.8395211932385,87.9720016543538,121.374609503989));
#48949=CARTESIAN_POINT('Ctrl Pts',(33.8339675024891,87.8711088344579,121.381013100749));
#48950=CARTESIAN_POINT('Ctrl Pts',(33.8347232656258,87.7701345030551,121.387416697508));
#48951=CARTESIAN_POINT('Ctrl Pts',(35.5611267921505,84.7993326348266,122.));
#48952=CARTESIAN_POINT('Ctrl Pts',(34.5788882023788,85.0619266872043,121.947350492269));
#48953=CARTESIAN_POINT('Ctrl Pts',(32.9121325517709,86.6347716463917,121.842051476808));
#48954=CARTESIAN_POINT('Ctrl Pts',(33.5229011708227,90.0369611826565,121.684102953615));
#48955=CARTESIAN_POINT('Ctrl Pts',(36.7064604291151,91.377416630034,121.526154430423));
#48956=CARTESIAN_POINT('Ctrl Pts',(39.5688530544509,89.4482951162593,121.36820590723));
#48957=CARTESIAN_POINT('Ctrl Pts',(39.5184627418672,85.9950129791182,121.210257384038));
#48958=CARTESIAN_POINT('Ctrl Pts',(36.5992128862014,84.1503276493198,121.052308860845));
#48959=CARTESIAN_POINT('Ctrl Pts',(33.4587562194708,85.585897700957,120.894360337653));
#48960=CARTESIAN_POINT('Ctrl Pts',(32.9440322230719,89.0005543330621,120.73641181446));
#48961=CARTESIAN_POINT('Ctrl Pts',(35.5219282988626,91.2981285259009,120.578463291268));
#48962=CARTESIAN_POINT('Ctrl Pts',(38.8550458568218,90.3955786925481,120.420514768075));
#48963=CARTESIAN_POINT('Ctrl Pts',(39.9213965365604,87.1111711483864,120.262566244883));
#48964=CARTESIAN_POINT('Ctrl Pts',(37.7541292878677,84.4228017462871,120.10461772169));
#48965=CARTESIAN_POINT('Ctrl Pts',(34.3182507508869,84.7679218698591,119.946669198498));
#48966=CARTESIAN_POINT('Ctrl Pts',(32.7289619830976,87.8336271382101,119.788720675305));
#48967=CARTESIAN_POINT('Ctrl Pts',(34.4272254557842,90.8403331303497,119.630772152113));
#48968=CARTESIAN_POINT('Ctrl Pts',(37.873276024629,91.0619522777656,119.47282362892));
#48969=CARTESIAN_POINT('Ctrl Pts',(39.9426850798466,88.2975486028455,119.314875105728));
#48970=CARTESIAN_POINT('Ctrl Pts',(38.7591820609565,85.0535231518079,119.156926582535));
#48971=CARTESIAN_POINT('Ctrl Pts',(35.3958133105107,84.2711349879319,118.998978059343));
#48972=CARTESIAN_POINT('Ctrl Pts',(32.9020429093888,86.6597517373779,118.841029536151));
#48973=CARTESIAN_POINT('Ctrl Pts',(33.5388966711455,90.0536872043056,118.683081012958));
#48974=CARTESIAN_POINT('Ctrl Pts',(36.7289586417865,91.3757633400502,118.525132489766));
#48975=CARTESIAN_POINT('Ctrl Pts',(39.5798966622645,89.4272939130391,118.367183966573));
#48976=CARTESIAN_POINT('Ctrl Pts',(39.5068519326957,85.9748968968193,118.209235443381));
#48977=CARTESIAN_POINT('Ctrl Pts',(36.5760518898075,84.1487556640973,118.051286920188));
#48978=CARTESIAN_POINT('Ctrl Pts',(33.4447637952687,85.6045769319753,117.893338396996));
#48979=CARTESIAN_POINT('Ctrl Pts',(32.9520313310439,89.0224118332001,117.735389873803));
#48980=CARTESIAN_POINT('Ctrl Pts',(35.5446000364372,91.3034134118094,117.577441350611));
#48981=CARTESIAN_POINT('Ctrl Pts',(38.8718667157924,90.3794669098942,117.419492827418));
#48982=CARTESIAN_POINT('Ctrl Pts',(39.9170998651258,87.0882865202323,117.261544304226));
#48983=CARTESIAN_POINT('Ctrl Pts',(37.7326183772922,84.4138854053773,117.103595781033));
#48984=CARTESIAN_POINT('Ctrl Pts',(34.2990251792965,84.7810617179477,116.945647257841));
#48985=CARTESIAN_POINT('Ctrl Pts',(32.729454795751,87.8569078624924,116.787698734649));
#48986=CARTESIAN_POINT('Ctrl Pts',(34.446988957088,90.8526476873878,116.629750211456));
#48987=CARTESIAN_POINT('Ctrl Pts',(37.894391675665,91.0521350047077,116.471801688264));
#48988=CARTESIAN_POINT('Ctrl Pts',(39.9460077545616,88.2745007309714,116.313853165071));
#48989=CARTESIAN_POINT('Ctrl Pts',(38.7416992921252,85.0381413842478,116.155904641879));
#48990=CARTESIAN_POINT('Ctrl Pts',(35.3733761438603,84.2773655547908,115.997956118686));
#48991=CARTESIAN_POINT('Ctrl Pts',(32.8949944653812,86.6819455492183,115.840007595494));
#48992=CARTESIAN_POINT('Ctrl Pts',(33.5536275479934,90.0717218185778,115.682059072301));
#48993=CARTESIAN_POINT('Ctrl Pts',(36.752112807112,91.3732873148253,115.524110549109));
#48994=CARTESIAN_POINT('Ctrl Pts',(39.5904809358262,89.4065521878392,115.366162025916));
#48995=CARTESIAN_POINT('Ctrl Pts',(39.4952698768951,85.954695361712,115.208213502724));
#48996=CARTESIAN_POINT('Ctrl Pts',(36.5528046017381,84.1474104372141,115.050264979531));
#48997=CARTESIAN_POINT('Ctrl Pts',(33.4309288843041,85.6233076893012,114.892316456339));
#48998=CARTESIAN_POINT('Ctrl Pts',(32.9601524900325,89.0442359668917,114.734367933146));
#48999=CARTESIAN_POINT('Ctrl Pts',(35.5673140575926,91.308543643525,114.576419409954));
#49000=CARTESIAN_POINT('Ctrl Pts',(38.8885794869123,90.3632518146024,114.418470886761));
#49001=CARTESIAN_POINT('Ctrl Pts',(39.9126584249495,87.0654278316568,114.260522363569));
#49002=CARTESIAN_POINT('Ctrl Pts',(37.7110496445387,84.4051084012425,114.102573840377));
#49003=CARTESIAN_POINT('Ctrl Pts',(34.2798848679742,84.7943242409579,113.944625317184));
#49004=CARTESIAN_POINT('Ctrl Pts',(32.7300968440076,87.8801851863978,113.786676793992));
#49005=CARTESIAN_POINT('Ctrl Pts',(34.4668312392973,90.8648349705502,113.628728270799));
#49006=CARTESIAN_POINT('Ctrl Pts',(37.915443798023,91.0421824081436,113.470779747607));
#49007=CARTESIAN_POINT('Ctrl Pts',(39.9491823979981,88.2514319712908,113.312831224414));
#49008=CARTESIAN_POINT('Ctrl Pts',(38.7241181039884,85.0228722042484,113.154882701222));
#49009=CARTESIAN_POINT('Ctrl Pts',(35.3509794527264,84.2837400555871,112.996934178029));
#49010=CARTESIAN_POINT('Ctrl Pts',(32.8880886699367,86.7041841648099,112.838985654837));
#49011=CARTESIAN_POINT('Ctrl Pts',(33.5684739229375,90.0896614725645,112.681037131644));
#49012=CARTESIAN_POINT('Ctrl Pts',(36.7752505958151,91.3706626685477,112.523088608452));
#49013=CARTESIAN_POINT('Ctrl Pts',(39.6009318089752,89.3857429282516,112.365140085259));
#49014=CARTESIAN_POINT('Ctrl Pts',(39.4835583456547,85.9345686115981,112.207191562067));
#49015=CARTESIAN_POINT('Ctrl Pts',(36.5295491552939,84.1462145087741,112.049243038874));
#49016=CARTESIAN_POINT('Ctrl Pts',(33.4172145286647,85.6421268944799,111.891294515682));
#49017=CARTESIAN_POINT('Ctrl Pts',(32.9684136143526,89.0660075047125,111.733345992489));
#49018=CARTESIAN_POINT('Ctrl Pts',(35.5900605517025,91.3135279228,111.575397469297));
#49019=CARTESIAN_POINT('Ctrl Pts',(38.9051877964048,90.346929740897,111.417448946105));
#49020=CARTESIAN_POINT('Ctrl Pts',(39.9080703007288,87.0425981327984,111.259500422912));
#49021=CARTESIAN_POINT('Ctrl Pts',(37.6894249992898,84.3964700708273,111.10155189972));
#49022=CARTESIAN_POINT('Ctrl Pts',(34.2608301098696,84.8077093905011,110.943603376527));
#49023=CARTESIAN_POINT('Ctrl Pts',(32.7308883426774,87.9034579077955,110.785654853335));
#49024=CARTESIAN_POINT('Ctrl Pts',(34.4867513670091,90.8768945953326,110.627706330142));
#49025=CARTESIAN_POINT('Ctrl Pts',(37.9364315807433,91.0320948408579,110.46975780695));
#49026=CARTESIAN_POINT('Ctrl Pts',(39.9522088516144,88.2283433032996,110.311809283757));
#49027=CARTESIAN_POINT('Ctrl Pts',(38.7064392347119,85.0077162267496,110.153860760565));
#49028=CARTESIAN_POINT('Ctrl Pts',(35.3286241543516,84.290258236255,109.995912237372));
#49029=CARTESIAN_POINT('Ctrl Pts',(32.8813258101548,86.7264666596099,109.83796371418));
#49030=CARTESIAN_POINT('Ctrl Pts',(33.5834351839898,90.1075054373259,109.680015190987));
#49031=CARTESIAN_POINT('Ctrl Pts',(36.7983710512446,91.3678894898621,109.522066667795));
#49032=CARTESIAN_POINT('Ctrl Pts',(39.6112488575384,89.3648670312859,109.364118144603));
#49033=CARTESIAN_POINT('Ctrl Pts',(39.4717178074565,85.914517396569,109.20616962141));
#49034=CARTESIAN_POINT('Ctrl Pts',(36.5062865391415,84.1451680917577,109.048221098218));
#49035=CARTESIAN_POINT('Ctrl Pts',(33.4036212322619,85.6610334351557,108.890272575025));
#49036=CARTESIAN_POINT('Ctrl Pts',(32.976814489993,89.0877262408462,108.732324051833));
#49037=CARTESIAN_POINT('Ctrl Pts',(35.6128383205754,91.3183646214857,108.57437552864));
#49038=CARTESIAN_POINT('Ctrl Pts',(38.9216914949492,90.3305042873106,108.416427005448));
#49039=CARTESIAN_POINT('Ctrl Pts',(39.9033345805337,87.019792348641,108.258478482255));
#49040=CARTESIAN_POINT('Ctrl Pts',(37.667747597468,84.3879831424088,108.100529959063));
#49041=CARTESIAN_POINT('Ctrl Pts',(34.2418570341057,84.8211911721592,107.94258143587));
#49042=CARTESIAN_POINT('Ctrl Pts',(32.7318388349523,87.9267773882983,107.784632912678));
#49043=CARTESIAN_POINT('Ctrl Pts',(34.5067288269183,90.8887184689395,107.626684389486));
#49044=CARTESIAN_POINT('Ctrl Pts',(37.957394655155,91.0220939825006,107.468735866293));
#49045=CARTESIAN_POINT('Ctrl Pts',(39.9550037460998,88.2047806129811,107.310787343101));
#49046=CARTESIAN_POINT('Ctrl Pts',(38.6888349059059,84.9936098257745,107.152838819908));
#49047=CARTESIAN_POINT('Ctrl Pts',(35.305967918485,84.2949816679675,106.994890296715));
#49048=CARTESIAN_POINT('Ctrl Pts',(32.8754909437191,86.7527679934688,106.836941773523));
#49049=CARTESIAN_POINT('Ctrl Pts',(33.3581428529919,88.9930721690106,106.731642758061));
#49050=CARTESIAN_POINT('Ctrl Pts',(34.018863416988,89.7658571455036,106.678993250331));
#49051=CARTESIAN_POINT('Ctrl Pts',(35.6089932203364,84.9783780187302,122.10700224989));
#49052=CARTESIAN_POINT('Ctrl Pts',(34.6859840276596,85.2251375401039,122.054352742159));
#49053=CARTESIAN_POINT('Ctrl Pts',(33.1197344387336,86.7031392915142,121.949053726697));
#49054=CARTESIAN_POINT('Ctrl Pts',(33.6936734550314,89.9001753781653,121.791105203505));
#49055=CARTESIAN_POINT('Ctrl Pts',(36.6852627607604,91.1598008023617,121.633156680312));
#49056=CARTESIAN_POINT('Ctrl Pts',(39.3750519156026,89.3470061213681,121.47520815712));
#49057=CARTESIAN_POINT('Ctrl Pts',(39.327700159908,86.1019583390072,121.317259633928));
#49058=CARTESIAN_POINT('Ctrl Pts',(36.5844822894654,84.36850830484,121.159311110735));
#49059=CARTESIAN_POINT('Ctrl Pts',(33.6333964710297,85.7175128829444,121.001362587543));
#49060=CARTESIAN_POINT('Ctrl Pts',(33.1497105465355,88.926264294351,120.84341406435));
#49061=CARTESIAN_POINT('Ctrl Pts',(35.5721584125611,91.0852938040143,120.685465541158));
#49062=CARTESIAN_POINT('Ctrl Pts',(38.7042875900392,90.2371681024705,120.527517017965));
#49063=CARTESIAN_POINT('Ctrl Pts',(39.7063368785371,87.1508117046191,120.369568494773));
#49064=CARTESIAN_POINT('Ctrl Pts',(37.6697567498784,84.6245520999892,120.21161997158));
#49065=CARTESIAN_POINT('Ctrl Pts',(34.4410631233212,84.9488613360056,120.053671448388));
#49066=CARTESIAN_POINT('Ctrl Pts',(32.9476091318338,87.8297032965965,119.895722925195));
#49067=CARTESIAN_POINT('Ctrl Pts',(34.5434666080111,90.6551036619663,119.737774402003));
#49068=CARTESIAN_POINT('Ctrl Pts',(37.7817188886635,90.8633590822565,119.57982587881));
#49069=CARTESIAN_POINT('Ctrl Pts',(39.7263417137742,88.2656501032049,119.421877355618));
#49070=CARTESIAN_POINT('Ctrl Pts',(38.6142044210923,85.2172407414007,119.263928832425));
#49071=CARTESIAN_POINT('Ctrl Pts',(35.4536482106658,84.4820309104909,119.105980309233));
#49072=CARTESIAN_POINT('Ctrl Pts',(33.110253206,86.7266130725836,118.948031786041));
#49073=CARTESIAN_POINT('Ctrl Pts',(33.7087044200059,89.9158928137251,118.790083262848));
#49074=CARTESIAN_POINT('Ctrl Pts',(36.7064043218137,91.1582472064541,118.632134739656));
#49075=CARTESIAN_POINT('Ctrl Pts',(39.3854295892538,89.3272712994712,118.474186216463));
#49076=CARTESIAN_POINT('Ctrl Pts',(39.3167894873777,86.0830552648703,118.316237693271));
#49077=CARTESIAN_POINT('Ctrl Pts',(36.5627179108249,84.3670311109829,118.158289170078));
#49078=CARTESIAN_POINT('Ctrl Pts',(33.6202477958494,85.7350657485328,118.000340646886));
#49079=CARTESIAN_POINT('Ctrl Pts',(33.1572273049567,88.946803778104,117.842392123693));
#49080=CARTESIAN_POINT('Ctrl Pts',(35.5934630348934,91.0902600090959,117.684443600501));
#49081=CARTESIAN_POINT('Ctrl Pts',(38.7200941441904,90.222027867038,117.526495077308));
#49082=CARTESIAN_POINT('Ctrl Pts',(39.7022992981841,87.1293070290982,117.368546554116));
#49083=CARTESIAN_POINT('Ctrl Pts',(37.6495429561925,84.6161734181593,117.210598030923));
#49084=CARTESIAN_POINT('Ctrl Pts',(34.4229968617254,84.9612088457679,117.052649507731));
#49085=CARTESIAN_POINT('Ctrl Pts',(32.9480722276783,87.8515801834838,116.894700984538));
#49086=CARTESIAN_POINT('Ctrl Pts',(34.562038361934,90.6666756460731,116.736752461346));
#49087=CARTESIAN_POINT('Ctrl Pts',(37.8015612571253,90.8541337948632,116.578803938153));
#49088=CARTESIAN_POINT('Ctrl Pts',(39.7294640298165,88.2439920276285,116.420855414961));
#49089=CARTESIAN_POINT('Ctrl Pts',(38.5977758705214,85.2027865008471,116.262906891769));
#49090=CARTESIAN_POINT('Ctrl Pts',(35.432564014533,84.4878857715667,116.104958368576));
#49091=CARTESIAN_POINT('Ctrl Pts',(33.1036297861092,86.7474685883031,115.947009845383));
#49092=CARTESIAN_POINT('Ctrl Pts',(33.722547018829,89.9328399332263,115.789061322191));
#49093=CARTESIAN_POINT('Ctrl Pts',(36.7281622813021,91.1559204865843,115.631112798999));
#49094=CARTESIAN_POINT('Ctrl Pts',(39.3953756267003,89.3077803089614,115.473164275806));
#49095=CARTESIAN_POINT('Ctrl Pts',(39.3059058343779,86.0640718907652,115.315215752614));
#49096=CARTESIAN_POINT('Ctrl Pts',(36.540872443933,84.3657670018423,115.157267229421));
#49097=CARTESIAN_POINT('Ctrl Pts',(33.6072471357927,85.7526670333709,114.999318706229));
#49098=CARTESIAN_POINT('Ctrl Pts',(33.1648587546674,88.9673119074215,114.841370183036));
#49099=CARTESIAN_POINT('Ctrl Pts',(35.6148073910889,91.0950808856969,114.683421659844));
#49100=CARTESIAN_POINT('Ctrl Pts',(38.7357991282334,90.2067905487629,114.525473136651));
#49101=CARTESIAN_POINT('Ctrl Pts',(39.6981256787049,87.1078267289883,114.367524613459));
#49102=CARTESIAN_POINT('Ctrl Pts',(37.6292748270299,84.6079256710386,114.209576090266));
#49103=CARTESIAN_POINT('Ctrl Pts',(34.4050107191677,84.9736716331029,114.051627567074));
#49104=CARTESIAN_POINT('Ctrl Pts',(32.948675560157,87.8734538750383,113.893679043881));
#49105=CARTESIAN_POINT('Ctrl Pts',(34.580684146241,90.6781280309721,113.735730520689));
#49106=CARTESIAN_POINT('Ctrl Pts',(37.8213439277149,90.8447813440276,113.577781997497));
#49107=CARTESIAN_POINT('Ctrl Pts',(39.7324472409282,88.2223143237889,113.419833474304));
#49108=CARTESIAN_POINT('Ctrl Pts',(38.5812548353702,85.1884380587774,113.261884951112));
#49109=CARTESIAN_POINT('Ctrl Pts',(35.4115178532262,84.4938758873033,113.103936427919));
#49110=CARTESIAN_POINT('Ctrl Pts',(33.0971404130134,86.7683662060889,112.945987904727));
#49111=CARTESIAN_POINT('Ctrl Pts',(33.7364981511649,89.949697818587,112.788039381534));
#49112=CARTESIAN_POINT('Ctrl Pts',(36.7499048516853,91.1534541075731,112.630090858342));
#49113=CARTESIAN_POINT('Ctrl Pts',(39.4051963078346,89.2882258564159,112.472142335149));
#49114=CARTESIAN_POINT('Ctrl Pts',(39.2949005133615,86.0451587920869,112.314193811957));
#49115=CARTESIAN_POINT('Ctrl Pts',(36.5190193106196,84.3646431883867,112.156245288764));
#49116=CARTESIAN_POINT('Ctrl Pts',(33.5943597615248,85.7703514326194,111.998296765572));
#49117=CARTESIAN_POINT('Ctrl Pts',(33.1726217297416,88.987770612421,111.840348242379));
#49118=CARTESIAN_POINT('Ctrl Pts',(35.6361822621062,91.0997646108504,111.682399719187));
#49119=CARTESIAN_POINT('Ctrl Pts',(38.7514059497287,90.1914527029174,111.524451195994));
#49120=CARTESIAN_POINT('Ctrl Pts',(39.6938142202905,87.0863736705035,111.366502672802));
#49121=CARTESIAN_POINT('Ctrl Pts',(37.6089541569189,84.5998082355544,111.20855414961));
#49122=CARTESIAN_POINT('Ctrl Pts',(34.3871049709332,84.9862496525397,111.050605626417));
#49123=CARTESIAN_POINT('Ctrl Pts',(32.9494193311266,87.8953232416183,110.892657103225));
#49124=CARTESIAN_POINT('Ctrl Pts',(34.5994030819342,90.6894604553447,110.734708580032));
#49125=CARTESIAN_POINT('Ctrl Pts',(37.8410661383737,90.8353020612612,110.57676005684));
#49126=CARTESIAN_POINT('Ctrl Pts',(39.7352911981278,88.2006179121182,110.418811533647));
#49127=CARTESIAN_POINT('Ctrl Pts',(38.5646420092929,85.17419599305,110.260863010455));
#49128=CARTESIAN_POINT('Ctrl Pts',(35.3905105886778,84.5000010189553,110.102914487262));
#49129=CARTESIAN_POINT('Ctrl Pts',(33.0907853565002,86.7893050571483,109.94496596407));
#49130=CARTESIAN_POINT('Ctrl Pts',(33.7505572419288,89.9664657848225,109.787017440877));
#49131=CARTESIAN_POINT('Ctrl Pts',(36.7716311339984,91.1508481527202,109.629068917685));
#49132=CARTESIAN_POINT('Ctrl Pts',(39.4148912340616,89.2686087847539,109.471120394492));
#49133=CARTESIAN_POINT('Ctrl Pts',(39.2837739645606,86.0263166736965,109.3131718713));
#49134=CARTESIAN_POINT('Ctrl Pts',(36.4971594399344,84.3636598707533,109.155223348107));
#49135=CARTESIAN_POINT('Ctrl Pts',(33.5815861465709,85.7881179009981,108.997274824915));
#49136=CARTESIAN_POINT('Ctrl Pts',(33.1805160290731,89.0081796996972,108.839326301723));
#49137=CARTESIAN_POINT('Ctrl Pts',(35.6575865220053,91.1043096545859,108.68137777853));
#49138=CARTESIAN_POINT('Ctrl Pts',(38.7669144683598,90.1760177110405,108.523429255338));
#49139=CARTESIAN_POINT('Ctrl Pts',(39.6893640660006,87.0649430846534,108.365480732145));
#49140=CARTESIAN_POINT('Ctrl Pts',(37.5885839114783,84.5918330724633,108.207532208953));
#49141=CARTESIAN_POINT('Ctrl Pts',(34.36927597956,84.9989184771347,108.04958368576));
#49142=CARTESIAN_POINT('Ctrl Pts',(32.9503125083204,87.9172365477096,107.891635162568));
#49143=CARTESIAN_POINT('Ctrl Pts',(34.6181758926694,90.7005713444361,107.733686639375));
#49144=CARTESIAN_POINT('Ctrl Pts',(37.8607651306453,90.8259042588387,107.575738116183));
#49145=CARTESIAN_POINT('Ctrl Pts',(39.7379175593087,88.1784760618644,107.41778959299));
#49146=CARTESIAN_POINT('Ctrl Pts',(38.5480992288646,85.1609402139439,107.259841069798));
#49147=CARTESIAN_POINT('Ctrl Pts',(35.369220533294,84.5044396257634,107.101892546605));
#49148=CARTESIAN_POINT('Ctrl Pts',(33.0853023349469,86.8140204095934,106.943944023413));
#49149=CARTESIAN_POINT('Ctrl Pts',(33.5388501325603,88.9192333079159,106.838645007951));
#49150=CARTESIAN_POINT('Ctrl Pts',(34.159728970665,89.6454190276517,106.78599550022));
#49151=CARTESIAN_POINT('Ctrl Pts',(35.6568596485223,85.1574234026337,122.21400449978));
#49152=CARTESIAN_POINT('Ctrl Pts',(34.7930798529404,85.3883483930035,122.161354992049));
#49153=CARTESIAN_POINT('Ctrl Pts',(33.3273363256962,86.7715069366368,122.056055976587));
#49154=CARTESIAN_POINT('Ctrl Pts',(33.8644457392402,89.7633895736742,121.898107453395));
#49155=CARTESIAN_POINT('Ctrl Pts',(36.6640650924058,90.9421849746893,121.740158930202));
#49156=CARTESIAN_POINT('Ctrl Pts',(39.1812507767543,89.245717126477,121.58221040701));
#49157=CARTESIAN_POINT('Ctrl Pts',(39.1369375779489,86.2089036988962,121.424261883817));
#49158=CARTESIAN_POINT('Ctrl Pts',(36.5697516927295,84.5866889603602,121.266313360625));
#49159=CARTESIAN_POINT('Ctrl Pts',(33.8080367225885,85.8491280649318,121.108364837432));
#49160=CARTESIAN_POINT('Ctrl Pts',(33.3553888699991,88.8519742556397,120.95041631424));
#49161=CARTESIAN_POINT('Ctrl Pts',(35.6223885262595,90.8724590821279,120.792467791047));
#49162=CARTESIAN_POINT('Ctrl Pts',(38.5535293232566,90.0787575123929,120.634519267855));
#49163=CARTESIAN_POINT('Ctrl Pts',(39.4912772205139,87.1904522608518,120.476570744663));
#49164=CARTESIAN_POINT('Ctrl Pts',(37.5853842118891,84.8263024536913,120.31862222147));
#49165=CARTESIAN_POINT('Ctrl Pts',(34.5638754957556,85.1298008021523,120.160673698278));
#49166=CARTESIAN_POINT('Ctrl Pts',(33.1662562805699,87.8257794549828,120.002725175085));
#49167=CARTESIAN_POINT('Ctrl Pts',(34.659707760238,90.4698741935831,119.844776651893));
#49168=CARTESIAN_POINT('Ctrl Pts',(37.690161752698,90.6647658867473,119.6868281287));
#49169=CARTESIAN_POINT('Ctrl Pts',(39.5099983477018,88.2337516035643,119.528879605508));
#49170=CARTESIAN_POINT('Ctrl Pts',(38.4692267812281,85.3809583309936,119.370931082315));
#49171=CARTESIAN_POINT('Ctrl Pts',(35.5114831108209,84.69292683305,119.212982559123));
#49172=CARTESIAN_POINT('Ctrl Pts',(33.3184635026112,86.7934744077893,119.05503403593));
#49173=CARTESIAN_POINT('Ctrl Pts',(33.8785121688663,89.7780984231445,118.897085512738));
#49174=CARTESIAN_POINT('Ctrl Pts',(36.6838500018409,90.9407310728582,118.739136989545));
#49175=CARTESIAN_POINT('Ctrl Pts',(39.1909625162432,89.2272486859031,118.581188466353));
#49176=CARTESIAN_POINT('Ctrl Pts',(39.1267270420596,86.1912136329214,118.42323994316));
#49177=CARTESIAN_POINT('Ctrl Pts',(36.5493839318423,84.5853065578684,118.265291419968));
#49178=CARTESIAN_POINT('Ctrl Pts',(33.7957317964302,85.8655545650902,118.107342896775));
#49179=CARTESIAN_POINT('Ctrl Pts',(33.3624232788696,88.871195723008,117.949394373583));
#49180=CARTESIAN_POINT('Ctrl Pts',(35.6423260333496,90.8771066063823,117.79144585039));
#49181=CARTESIAN_POINT('Ctrl Pts',(38.5683215725883,90.0645888241819,117.633497327198));
#49182=CARTESIAN_POINT('Ctrl Pts',(39.4874987312424,87.1703275379639,117.475548804005));
#49183=CARTESIAN_POINT('Ctrl Pts',(37.5664675350927,84.8184614309413,117.317600280813));
#49184=CARTESIAN_POINT('Ctrl Pts',(34.5469685441542,85.1413559735884,117.159651757621));
#49185=CARTESIAN_POINT('Ctrl Pts',(33.1666896596057,87.846252504475,117.001703234428));
#49186=CARTESIAN_POINT('Ctrl Pts',(34.6770877667801,90.4807036047585,116.843754711236));
#49187=CARTESIAN_POINT('Ctrl Pts',(37.7087308385855,90.6561325850187,116.685806188043));
#49188=CARTESIAN_POINT('Ctrl Pts',(39.5129203050714,88.2134833242854,116.527857664851));
#49189=CARTESIAN_POINT('Ctrl Pts',(38.4538524489176,85.3674316174465,116.369909141658));
#49190=CARTESIAN_POINT('Ctrl Pts',(35.4917518852057,84.6984059883427,116.211960618466));
#49191=CARTESIAN_POINT('Ctrl Pts',(33.3122651068371,86.8129916273879,116.054012095273));
#49192=CARTESIAN_POINT('Ctrl Pts',(33.8914664896646,89.7939580478747,115.896063572081));
#49193=CARTESIAN_POINT('Ctrl Pts',(36.7042117554922,90.9385536583433,115.738115048888));
#49194=CARTESIAN_POINT('Ctrl Pts',(39.2002703175744,89.2090084300835,115.580166525696));
#49195=CARTESIAN_POINT('Ctrl Pts',(39.1165417918607,86.1734484198183,115.422218002503));
#49196=CARTESIAN_POINT('Ctrl Pts',(36.5289402861278,84.5841235664707,115.264269479311));
#49197=CARTESIAN_POINT('Ctrl Pts',(33.7835653872813,85.8820263774406,115.106320956119));
#49198=CARTESIAN_POINT('Ctrl Pts',(33.3695650193023,88.8903878479511,114.948372432926));
#49199=CARTESIAN_POINT('Ctrl Pts',(35.6623007245852,90.8816181278689,114.790423909734));
#49200=CARTESIAN_POINT('Ctrl Pts',(38.5830187695545,90.0503292829234,114.632475386541));
#49201=CARTESIAN_POINT('Ctrl Pts',(39.4835929324604,87.1502256263198,114.474526863349));
#49202=CARTESIAN_POINT('Ctrl Pts',(37.5475000095212,84.8107429408348,114.316578340156));
#49203=CARTESIAN_POINT('Ctrl Pts',(34.5301365703613,85.153019025248,114.158629816964));
#49204=CARTESIAN_POINT('Ctrl Pts',(33.1672542763064,87.8667225636788,114.000681293771));
#49205=CARTESIAN_POINT('Ctrl Pts',(34.6945370531848,90.491421091394,113.842732770579));
#49206=CARTESIAN_POINT('Ctrl Pts',(37.7272440574067,90.6473802799116,113.684784247386));
#49207=CARTESIAN_POINT('Ctrl Pts',(39.5157120838583,88.1931966762869,113.526835724194));
#49208=CARTESIAN_POINT('Ctrl Pts',(38.4383915667521,85.3540039133063,113.368887201001));
#49209=CARTESIAN_POINT('Ctrl Pts',(35.472056253726,84.7040117190196,113.210938677809));
#49210=CARTESIAN_POINT('Ctrl Pts',(33.3061921560902,86.8325482473677,113.052990154616));
#49211=CARTESIAN_POINT('Ctrl Pts',(33.9045223793923,89.8097341646095,112.895041631424));
#49212=CARTESIAN_POINT('Ctrl Pts',(36.7245591075554,90.9362455465985,112.737093108232));
#49213=CARTESIAN_POINT('Ctrl Pts',(39.2094608066942,89.1907087845802,112.579144585039));
#49214=CARTESIAN_POINT('Ctrl Pts',(39.1062426810682,86.1557489725758,112.421196061847));
#49215=CARTESIAN_POINT('Ctrl Pts',(36.5084894659453,84.5830718679992,112.263247538654));
#49216=CARTESIAN_POINT('Ctrl Pts',(33.7715049943849,85.898575970759,112.105299015462));
#49217=CARTESIAN_POINT('Ctrl Pts',(33.3768298451305,88.9095337201295,111.947350492269));
#49218=CARTESIAN_POINT('Ctrl Pts',(35.6823039725099,90.8860012989009,111.789401969077));
#49219=CARTESIAN_POINT('Ctrl Pts',(38.5976241030526,90.0359756649375,111.631453445884));
#49220=CARTESIAN_POINT('Ctrl Pts',(39.4795581398523,87.1301492082086,111.473504922692));
#49221=CARTESIAN_POINT('Ctrl Pts',(37.5284833145479,84.8031464002815,111.315556399499));
#49222=CARTESIAN_POINT('Ctrl Pts',(34.5133798319967,85.1647899145784,111.157607876307));
#49223=CARTESIAN_POINT('Ctrl Pts',(33.1679503195757,87.8871885754409,110.999659353114));
#49224=CARTESIAN_POINT('Ctrl Pts',(34.7120547968593,90.5020263153568,110.841710829922));
#49225=CARTESIAN_POINT('Ctrl Pts',(37.7457006960041,90.6385092816646,110.683762306729));
#49226=CARTESIAN_POINT('Ctrl Pts',(39.5183735446411,88.1728925209367,110.525813783537));
#49227=CARTESIAN_POINT('Ctrl Pts',(38.422844783874,85.3406757593505,110.367865260344));
#49228=CARTESIAN_POINT('Ctrl Pts',(35.4523970230039,84.7097438016556,110.209916737152));
#49229=CARTESIAN_POINT('Ctrl Pts',(33.3002449028457,86.8521434546867,110.05196821396));
#49230=CARTESIAN_POINT('Ctrl Pts',(33.9176792998676,89.8254261323192,109.894019690767));
#49231=CARTESIAN_POINT('Ctrl Pts',(36.7448912167523,90.9338068155782,109.736071167575));
#49232=CARTESIAN_POINT('Ctrl Pts',(39.2185336105849,89.1723505382218,109.578122644382));
#49233=CARTESIAN_POINT('Ctrl Pts',(39.0958301216647,86.1381159508238,109.42017412119));
#49234=CARTESIAN_POINT('Ctrl Pts',(36.4880323407273,84.5821516497489,109.262225597997));
#49235=CARTESIAN_POINT('Ctrl Pts',(33.75955106088,85.9152023668404,109.104277074805));
#49236=CARTESIAN_POINT('Ctrl Pts',(33.3842175681532,88.9286331585482,108.946328551612));
#49237=CARTESIAN_POINT('Ctrl Pts',(35.7023347234351,90.890254687686,108.78838002842));
#49238=CARTESIAN_POINT('Ctrl Pts',(38.6121374417704,90.0215311347704,108.630431505227));
#49239=CARTESIAN_POINT('Ctrl Pts',(39.4753935514674,87.1100938206657,108.472482982035));
#49240=CARTESIAN_POINT('Ctrl Pts',(37.5094202254886,84.7956830025177,108.314534458842));
#49241=CARTESIAN_POINT('Ctrl Pts',(34.4966949250142,85.17664578211,108.15658593565));
#49242=CARTESIAN_POINT('Ctrl Pts',(33.1687861816885,87.907695707121,107.998637412457));
#49243=CARTESIAN_POINT('Ctrl Pts',(34.7296229584204,90.5124242199326,107.840688889265));
#49244=CARTESIAN_POINT('Ctrl Pts',(37.7641356061356,90.6297145351769,107.682740366072));
#49245=CARTESIAN_POINT('Ctrl Pts',(39.5208313725176,88.1521715107477,107.52479184288));
#49246=CARTESIAN_POINT('Ctrl Pts',(38.4073635518233,85.3282706021133,107.366843319688));
#49247=CARTESIAN_POINT('Ctrl Pts',(35.432473148103,84.7138975835592,107.208894796495));
#49248=CARTESIAN_POINT('Ctrl Pts',(33.2951137261748,86.8752728257181,107.050946273303));
#49249=CARTESIAN_POINT('Ctrl Pts',(33.7195574121287,88.8453944468211,106.945647257841));
#49250=CARTESIAN_POINT('Ctrl Pts',(34.300594524342,89.5249809097997,106.89299775011));
#49251=CARTESIAN_POINT('Ctrl Pts',(35.7047260767083,85.3364687865372,122.321006749669));
#49252=CARTESIAN_POINT('Ctrl Pts',(34.9001756782212,85.5515592459031,122.268357241939));
#49253=CARTESIAN_POINT('Ctrl Pts',(33.534938212659,86.8398745817594,122.163058226477));
#49254=CARTESIAN_POINT('Ctrl Pts',(34.0352180234489,89.6266037691829,122.005109703284));
#49255=CARTESIAN_POINT('Ctrl Pts',(36.6428674240512,90.7245691470171,121.847161180092));
#49256=CARTESIAN_POINT('Ctrl Pts',(38.987449637906,89.1444281315857,121.6892126569));
#49257=CARTESIAN_POINT('Ctrl Pts',(38.9461749959898,86.3158490587852,121.531264133707));
#49258=CARTESIAN_POINT('Ctrl Pts',(36.5550210959935,84.8048696158805,121.373315610515));
#49259=CARTESIAN_POINT('Ctrl Pts',(33.9826769741474,85.9807432469191,121.215367087322));
#49260=CARTESIAN_POINT('Ctrl Pts',(33.5610671934627,88.7776842169286,121.05741856413));
#49261=CARTESIAN_POINT('Ctrl Pts',(35.672618639958,90.6596243602414,120.899470040937));
#49262=CARTESIAN_POINT('Ctrl Pts',(38.402771056474,89.9203469223153,120.741521517745));
#49263=CARTESIAN_POINT('Ctrl Pts',(39.2762175624906,87.2300928170844,120.583572994552));
#49264=CARTESIAN_POINT('Ctrl Pts',(37.5010116738998,85.0280528073935,120.42562447136));
#49265=CARTESIAN_POINT('Ctrl Pts',(34.6866878681899,85.3107402682988,120.267675948167));
#49266=CARTESIAN_POINT('Ctrl Pts',(33.3849034293061,87.8218556133692,120.109727424975));
#49267=CARTESIAN_POINT('Ctrl Pts',(34.7759489124649,90.2846447251997,119.951778901782));
#49268=CARTESIAN_POINT('Ctrl Pts',(37.5986046167326,90.4661726912383,119.79383037859));
#49269=CARTESIAN_POINT('Ctrl Pts',(39.2936549816293,88.2018531039237,119.635881855397));
#49270=CARTESIAN_POINT('Ctrl Pts',(38.3242491413639,85.5446759205865,119.477933332205));
#49271=CARTESIAN_POINT('Ctrl Pts',(35.569318010976,84.9038227556091,119.319984809012));
#49272=CARTESIAN_POINT('Ctrl Pts',(33.5266737992225,86.860335742995,119.16203628582));
#49273=CARTESIAN_POINT('Ctrl Pts',(34.0483199177267,89.640304032564,119.004087762628));
#49274=CARTESIAN_POINT('Ctrl Pts',(36.6612956818681,90.7232149392622,118.846139239435));
#49275=CARTESIAN_POINT('Ctrl Pts',(38.9964954432325,89.1272260723352,118.688190716243));
#49276=CARTESIAN_POINT('Ctrl Pts',(38.9366645967416,86.2993720009723,118.53024219305));
#49277=CARTESIAN_POINT('Ctrl Pts',(36.5360499528598,84.803582004754,118.372293669858));
#49278=CARTESIAN_POINT('Ctrl Pts',(33.9712157970109,85.9960433816476,118.214345146665));
#49279=CARTESIAN_POINT('Ctrl Pts',(33.5676192527825,88.795587667912,118.056396623473));
#49280=CARTESIAN_POINT('Ctrl Pts',(35.6911890318057,90.6639532036688,117.89844810028));
#49281=CARTESIAN_POINT('Ctrl Pts',(38.4165490009863,89.9071497813258,117.740499577088));
#49282=CARTESIAN_POINT('Ctrl Pts',(39.2726981643007,87.2113480468297,117.582551053895));
#49283=CARTESIAN_POINT('Ctrl Pts',(37.4833921139929,85.0207494437233,117.424602530703));
#49284=CARTESIAN_POINT('Ctrl Pts',(34.670940226583,85.3215031014086,117.266654007511));
#49285=CARTESIAN_POINT('Ctrl Pts',(33.3853070915332,87.8409248254664,117.108705484318));
#49286=CARTESIAN_POINT('Ctrl Pts',(34.7921371716262,90.2947315634439,116.950756961126));
#49287=CARTESIAN_POINT('Ctrl Pts',(37.6159004200458,90.4581313751741,116.792808437933));
#49288=CARTESIAN_POINT('Ctrl Pts',(39.2963765803263,88.1829746209424,116.634859914741));
#49289=CARTESIAN_POINT('Ctrl Pts',(38.3099290273138,85.5320767340458,116.476911391548));
#49290=CARTESIAN_POINT('Ctrl Pts',(35.5509397558784,84.9089262051186,116.318962868356));
#49291=CARTESIAN_POINT('Ctrl Pts',(33.5209004275651,86.8785146664726,116.161014345163));
#49292=CARTESIAN_POINT('Ctrl Pts',(34.0603859605002,89.6550761625235,116.003065821971));
#49293=CARTESIAN_POINT('Ctrl Pts',(36.6802612296823,90.7211868301021,115.845117298778));
#49294=CARTESIAN_POINT('Ctrl Pts',(39.0051650084485,89.1102365512059,115.687168775586));
#49295=CARTESIAN_POINT('Ctrl Pts',(38.9271777493435,86.2828249488715,115.529220252393));
#49296=CARTESIAN_POINT('Ctrl Pts',(36.5170081283227,84.8024801310989,115.371271729201));
#49297=CARTESIAN_POINT('Ctrl Pts',(33.95988363877,86.0113857215104,115.213323206008));
#49298=CARTESIAN_POINT('Ctrl Pts',(33.5742712839372,88.8134637884809,115.055374682816));
#49299=CARTESIAN_POINT('Ctrl Pts',(35.7097940580815,90.6681553700408,114.897426159623));
#49300=CARTESIAN_POINT('Ctrl Pts',(38.4302384108755,89.8938680170839,114.739477636431));
#49301=CARTESIAN_POINT('Ctrl Pts',(39.2690601862158,87.1926245236512,114.581529113238));
#49302=CARTESIAN_POINT('Ctrl Pts',(37.4657251920124,85.0135602106309,114.423580590046));
#49303=CARTESIAN_POINT('Ctrl Pts',(34.6552624215549,85.3323664173931,114.265632066854));
#49304=CARTESIAN_POINT('Ctrl Pts',(33.3858329924558,87.8599912523192,114.107683543661));
#49305=CARTESIAN_POINT('Ctrl Pts',(34.8083899601285,90.3047141518159,113.949735020469));
#49306=CARTESIAN_POINT('Ctrl Pts',(37.6331441870985,90.4499792157957,113.791786497276));
#49307=CARTESIAN_POINT('Ctrl Pts',(39.2989769267884,88.1640790287851,113.633837974084));
#49308=CARTESIAN_POINT('Ctrl Pts',(38.295528298134,85.5195697678351,113.475889450891));
#49309=CARTESIAN_POINT('Ctrl Pts',(35.5325946542257,84.9141475507359,113.317940927699));
#49310=CARTESIAN_POINT('Ctrl Pts',(33.5152438991669,86.8967302886466,113.159992404506));
#49311=CARTESIAN_POINT('Ctrl Pts',(34.0725466076197,89.669770510632,113.002043881314));
#49312=CARTESIAN_POINT('Ctrl Pts',(36.6992133634256,90.719036985624,112.844095358121));
#49313=CARTESIAN_POINT('Ctrl Pts',(39.0137253055536,89.0931917127443,112.686146834929));
#49314=CARTESIAN_POINT('Ctrl Pts',(38.917584848775,86.2663391530647,112.528198311737));
#49315=CARTESIAN_POINT('Ctrl Pts',(36.497959621271,84.8015005476119,112.370249788544));
#49316=CARTESIAN_POINT('Ctrl Pts',(33.9486502272449,86.0268005088984,112.212301265351));
#49317=CARTESIAN_POINT('Ctrl Pts',(33.5810379605196,88.831296827838,112.054352742159));
#49318=CARTESIAN_POINT('Ctrl Pts',(35.7284256829136,90.6722379869513,111.896404218967));
#49319=CARTESIAN_POINT('Ctrl Pts',(38.4438422563765,89.8804986269578,111.738455695774));
#49320=CARTESIAN_POINT('Ctrl Pts',(39.265302059414,87.1739247459138,111.580507172582));
#49321=CARTESIAN_POINT('Ctrl Pts',(37.448012472177,85.0064845650086,111.422558649389));
#49322=CARTESIAN_POINT('Ctrl Pts',(34.6396546930603,85.3433301766171,111.264610126197));
#49323=CARTESIAN_POINT('Ctrl Pts',(33.3864813080249,87.8790539092635,111.106661603004));
#49324=CARTESIAN_POINT('Ctrl Pts',(34.8247065117844,90.3145921753689,110.948713079812));
#49325=CARTESIAN_POINT('Ctrl Pts',(37.6503352536344,90.4417165020679,110.790764556619));
#49326=CARTESIAN_POINT('Ctrl Pts',(39.3014558911545,88.1451671297553,110.632816033427));
#49327=CARTESIAN_POINT('Ctrl Pts',(38.2810475584549,85.507155525651,110.474867510234));
#49328=CARTESIAN_POINT('Ctrl Pts',(35.5142834573301,84.919486584356,110.316918987042));
#49329=CARTESIAN_POINT('Ctrl Pts',(33.5097044491911,86.9149818522253,110.158970463849));
#49330=CARTESIAN_POINT('Ctrl Pts',(34.0848013578066,89.6843864798158,110.001021940657));
#49331=CARTESIAN_POINT('Ctrl Pts',(36.7181512995062,90.7167654784365,109.843073417464));
#49332=CARTESIAN_POINT('Ctrl Pts',(39.0221759871081,89.0760922916896,109.685124894272));
#49333=CARTESIAN_POINT('Ctrl Pts',(38.9078862787688,86.2499152279515,109.52717637108));
#49334=CARTESIAN_POINT('Ctrl Pts',(36.4789052415203,84.8006434287444,109.369227847887));
#49335=CARTESIAN_POINT('Ctrl Pts',(33.937515975189,86.0422868326829,109.211279324695));
#49336=CARTESIAN_POINT('Ctrl Pts',(33.5879191072333,88.8490866173992,109.053330801502));
#49337=CARTESIAN_POINT('Ctrl Pts',(35.747082924865,90.6761997207862,108.89538227831));
#49338=CARTESIAN_POINT('Ctrl Pts',(38.457360415181,89.8670445585003,108.737433755117));
#49339=CARTESIAN_POINT('Ctrl Pts',(39.2614230369343,87.155244556678,108.579485231925));
#49340=CARTESIAN_POINT('Ctrl Pts',(37.4302565394989,84.9995329325722,108.421536708732));
#49341=CARTESIAN_POINT('Ctrl Pts',(34.6241138704685,85.3543730870854,108.26358818554));
#49342=CARTESIAN_POINT('Ctrl Pts',(33.3872598550566,87.8981548665324,108.105639662347));
#49343=CARTESIAN_POINT('Ctrl Pts',(34.8410700241714,90.3242770954292,107.947691139155));
#49344=CARTESIAN_POINT('Ctrl Pts',(37.6675060816258,90.433524811515,107.789742615962));
#49345=CARTESIAN_POINT('Ctrl Pts',(39.3037451857265,88.125866959631,107.63179409277));
#49346=CARTESIAN_POINT('Ctrl Pts',(38.2666278747819,85.4956009902827,107.473845569577));
#49347=CARTESIAN_POINT('Ctrl Pts',(35.495725762912,84.9233555413549,107.315897046385));
#49348=CARTESIAN_POINT('Ctrl Pts',(33.5049251174026,86.9365252418428,107.157948523192));
#49349=CARTESIAN_POINT('Ctrl Pts',(33.9002646916971,88.7715555857264,107.052649507731));
#49350=CARTESIAN_POINT('Ctrl Pts',(34.441460078019,89.4045427919478,107.));
#49351=CARTESIAN_POINT('Ctrl Pts',(33.8399314485466,87.7703173734778,121.112583302492));
#49352=CARTESIAN_POINT('Ctrl Pts',(33.8380185825139,88.0618702121891,121.094195056371));
#49353=CARTESIAN_POINT('Ctrl Pts',(33.8848898739967,88.3528282009691,121.07580681025));
#49354=CARTESIAN_POINT('Ctrl Pts',(33.983260731326,88.6251840791458,121.05741856413));
#49355=CARTESIAN_POINT('Ctrl Pts',(34.2649176756278,89.4049975980328,121.004769056399));
#49356=CARTESIAN_POINT('Ctrl Pts',(34.9687681577929,90.0323109791371,120.952119548668));
#49357=CARTESIAN_POINT('Ctrl Pts',(35.7757188016281,90.2227547633682,120.899470040937));
#49358=CARTESIAN_POINT('Ctrl Pts',(36.5826694454633,90.4131985475994,120.846820533206));
#49359=CARTESIAN_POINT('Ctrl Pts',(37.4927202509686,90.1667727349573,120.794171025476));
#49360=CARTESIAN_POINT('Ctrl Pts',(38.0933200713907,89.5951841444312,120.741521517745));
#49361=CARTESIAN_POINT('Ctrl Pts',(38.6939198918129,89.023595553905,120.688872010014));
#49362=CARTESIAN_POINT('Ctrl Pts',(38.9850687271518,88.1268441854947,120.636222502283));
#49363=CARTESIAN_POINT('Ctrl Pts',(38.8347754967227,87.3114618330078,120.583572994552));
#49364=CARTESIAN_POINT('Ctrl Pts',(38.6844822662937,86.4960794805208,120.530923486821));
#49365=CARTESIAN_POINT('Ctrl Pts',(38.0927469700967,85.7620661439571,120.478273979091));
#49366=CARTESIAN_POINT('Ctrl Pts',(37.3278253543799,85.4421740524928,120.42562447136));
#49367=CARTESIAN_POINT('Ctrl Pts',(36.5629037386632,85.1222819610286,120.372974963629));
#49368=CARTESIAN_POINT('Ctrl Pts',(35.6247958034265,85.2165111146637,120.320325455898));
#49369=CARTESIAN_POINT('Ctrl Pts',(34.9387777626609,85.6821449156596,120.267675948167));
#49370=CARTESIAN_POINT('Ctrl Pts',(34.265163658693,86.1393595616258,120.215978399609));
#49371=CARTESIAN_POINT('Ctrl Pts',(33.8346057561187,86.9546694932317,120.16428085105));
#49372=CARTESIAN_POINT('Ctrl Pts',(33.833340462721,87.7688288397412,120.112583302492));
#49373=CARTESIAN_POINT('Ctrl Pts',(35.5611267921505,84.7993326348266,122.));
#49374=CARTESIAN_POINT('Ctrl Pts',(35.4680767340868,84.8333707617182,122.));
#49375=CARTESIAN_POINT('Ctrl Pts',(35.3770918409722,84.8721775875453,122.));
#49376=CARTESIAN_POINT('Ctrl Pts',(35.2883805979929,84.9154247896511,122.));
#49377=CARTESIAN_POINT('Ctrl Pts',(35.197702396015,84.9596308947154,122.));
#49378=CARTESIAN_POINT('Ctrl Pts',(35.109399119487,85.0084770849584,122.));
#49379=CARTESIAN_POINT('Ctrl Pts',(35.0237223483213,85.0616582525317,122.));
#49380=CARTESIAN_POINT('Ctrl Pts',(34.9412909170175,85.112824977209,122.));
#49381=CARTESIAN_POINT('Ctrl Pts',(34.8612904976022,85.168005366865,122.));
#49382=CARTESIAN_POINT('Ctrl Pts',(34.7839781170505,85.2269577350007,122.));
#49383=CARTESIAN_POINT('Ctrl Pts',(34.7163297840678,85.2785410571195,122.));
#49384=CARTESIAN_POINT('Ctrl Pts',(34.6507397710755,85.3330129976211,122.));
#49385=CARTESIAN_POINT('Ctrl Pts',(34.5874048868897,85.3902243446383,122.));
#49386=CARTESIAN_POINT('Ctrl Pts',(34.5732684409796,85.4029940074072,122.));
#49387=CARTESIAN_POINT('Ctrl Pts',(34.5592417005919,85.4159028804059,122.));
#49388=CARTESIAN_POINT('Ctrl Pts',(34.5453464389343,85.4289307716471,122.));
#49389=CARTESIAN_POINT('Ctrl Pts',(34.4729163426157,85.4968396344438,122.));
#49390=CARTESIAN_POINT('Ctrl Pts',(34.4039519336089,85.5680704126807,122.));
#49391=CARTESIAN_POINT('Ctrl Pts',(34.33869316176,85.6423323835084,122.));
#49392=CARTESIAN_POINT('Ctrl Pts',(34.2737934142962,85.7161857984033,122.));
#49393=CARTESIAN_POINT('Ctrl Pts',(34.2125581562074,85.7930379420743,122.));
#49394=CARTESIAN_POINT('Ctrl Pts',(34.1552670083591,85.8726296318035,122.));
#49395=CARTESIAN_POINT('Ctrl Pts',(34.1001040937713,85.9492646748656,122.));
#49396=CARTESIAN_POINT('Ctrl Pts',(34.0485975400135,86.0284402461049,122.));
#49397=CARTESIAN_POINT('Ctrl Pts',(34.0010417953143,86.1099385723801,122.));
#49398=CARTESIAN_POINT('Ctrl Pts',(33.9810954653113,86.144121456506,122.));
#49399=CARTESIAN_POINT('Ctrl Pts',(33.9618447387099,86.1787130708316,122.));
#49400=CARTESIAN_POINT('Ctrl Pts',(33.9433139257018,86.2136976438174,122.));
#49401=CARTESIAN_POINT('Ctrl Pts',(33.9304313899784,86.2380187575787,122.));
#49402=CARTESIAN_POINT('Ctrl Pts',(33.9178968184969,86.2625297896542,122.));
#49403=CARTESIAN_POINT('Ctrl Pts',(33.9057188451145,86.2872254467939,122.));
#49404=CARTESIAN_POINT('Ctrl Pts',(33.8978104958471,86.3032627525029,122.));
#49405=CARTESIAN_POINT('Ctrl Pts',(33.8900514222255,86.3193805307655,122.));
#49406=CARTESIAN_POINT('Ctrl Pts',(33.8824541646778,86.335555142464,122.));
#49407=CARTESIAN_POINT('Ctrl Pts',(33.8403338623352,86.4252295454634,122.));
#49408=CARTESIAN_POINT('Ctrl Pts',(33.8031123934132,86.5167875390704,122.));
#49409=CARTESIAN_POINT('Ctrl Pts',(33.7710810415748,86.6099567585531,122.));
#49410=CARTESIAN_POINT('Ctrl Pts',(33.7412012885639,86.696867647622,122.));
#49411=CARTESIAN_POINT('Ctrl Pts',(33.715837986679,86.7851813667476,122.));
#49412=CARTESIAN_POINT('Ctrl Pts',(33.6952781137301,86.8746855295874,122.));
#49413=CARTESIAN_POINT('Ctrl Pts',(33.6937976263072,86.881130597984,122.));
#49414=CARTESIAN_POINT('Ctrl Pts',(33.6923420683187,86.8875818402717,122.));
#49415=CARTESIAN_POINT('Ctrl Pts',(33.6909115575437,86.8940391774638,122.));
#49416=CARTESIAN_POINT('Ctrl Pts',(33.6703053385859,86.987055816269,122.));
#49417=CARTESIAN_POINT('Ctrl Pts',(33.6548921451018,87.081338120739,122.));
#49418=CARTESIAN_POINT('Ctrl Pts',(33.6445950569561,87.1764782244295,122.));
#49419=CARTESIAN_POINT('Ctrl Pts',(33.6387985396345,87.2300352350339,122.));
#49420=CARTESIAN_POINT('Ctrl Pts',(33.6346241821948,87.2838638828705,122.));
#49421=CARTESIAN_POINT('Ctrl Pts',(33.6320650250057,87.3378887730391,122.));
#49422=CARTESIAN_POINT('Ctrl Pts',(33.6314041425466,87.3518402811434,122.));
#49423=CARTESIAN_POINT('Ctrl Pts',(33.6308510967089,87.3658042773908,122.));
#49424=CARTESIAN_POINT('Ctrl Pts',(33.6304060090372,87.3797660938872,122.));
#49425=CARTESIAN_POINT('Ctrl Pts',(33.6274345999427,87.4729752999515,122.));
#49426=CARTESIAN_POINT('Ctrl Pts',(33.6292623454294,87.5662427431663,122.));
#49427=CARTESIAN_POINT('Ctrl Pts',(33.6357543510792,87.6591933437351,122.));
#49428=CARTESIAN_POINT('Ctrl Pts',(33.6422571510453,87.7522984941045,122.));
#49429=CARTESIAN_POINT('Ctrl Pts',(33.6534401126504,87.8450867269761,122.));
#49430=CARTESIAN_POINT('Ctrl Pts',(33.6692186001989,87.9371689927436,122.));
#49431=CARTESIAN_POINT('Ctrl Pts',(33.6847714909114,88.0279346894962,122.));
#49432=CARTESIAN_POINT('Ctrl Pts',(33.7047898966492,88.1180153063821,122.));
#49433=CARTESIAN_POINT('Ctrl Pts',(33.7292357852524,88.2070130445517,122.));
#49434=CARTESIAN_POINT('Ctrl Pts',(33.7383345490649,88.2401380175319,122.));
#49435=CARTESIAN_POINT('Ctrl Pts',(33.7480470632381,88.2731126593096,122.));
#49436=CARTESIAN_POINT('Ctrl Pts',(33.7583727282114,88.305915192543,122.));
#49437=CARTESIAN_POINT('Ctrl Pts',(33.7653672088676,88.3281352321018,122.));
#49438=CARTESIAN_POINT('Ctrl Pts',(33.7726430513325,88.3502762836458,122.));
#49439=CARTESIAN_POINT('Ctrl Pts',(33.7802002483622,88.3723313649238,122.));
#49440=CARTESIAN_POINT('Ctrl Pts',(33.7847163076137,88.3855111263426,122.));
#49441=CARTESIAN_POINT('Ctrl Pts',(33.7893324946004,88.3986590147143,122.));
#49442=CARTESIAN_POINT('Ctrl Pts',(33.7940453374235,88.4117643917557,122.));
#49443=CARTESIAN_POINT('Ctrl Pts',(33.8256770944825,88.4997253355632,122.));
#49444=CARTESIAN_POINT('Ctrl Pts',(33.8616980723005,88.5858885320335,122.));
#49445=CARTESIAN_POINT('Ctrl Pts',(33.9020437068047,88.6698397368365,122.));
#49446=CARTESIAN_POINT('Ctrl Pts',(33.9323029326829,88.7328031404388,122.));
#49447=CARTESIAN_POINT('Ctrl Pts',(33.964995825274,88.7945218067863,122.));
#49448=CARTESIAN_POINT('Ctrl Pts',(34.0001111084258,88.8548054454097,122.));
#49449=CARTESIAN_POINT('Ctrl Pts',(34.0135804337297,88.8779287087366,122.));
#49450=CARTESIAN_POINT('Ctrl Pts',(34.0274062973137,88.900840676073,122.));
#49451=CARTESIAN_POINT('Ctrl Pts',(34.0415885432314,88.9235299643773,122.));
#49452=CARTESIAN_POINT('Ctrl Pts',(34.0517128286096,88.939727175394,122.));
#49453=CARTESIAN_POINT('Ctrl Pts',(34.0620195670163,88.9558119726629,122.));
#49454=CARTESIAN_POINT('Ctrl Pts',(34.0724986266519,88.971765210655,122.));
#49455=CARTESIAN_POINT('Ctrl Pts',(34.1196852037718,89.0436016846323,122.));
#49456=CARTESIAN_POINT('Ctrl Pts',(34.1704067057004,89.1128447071754,122.));
#49457=CARTESIAN_POINT('Ctrl Pts',(34.2246302409937,89.1791422786934,122.));
#49458=CARTESIAN_POINT('Ctrl Pts',(34.2734266590585,89.2388042686205,122.));
#49459=CARTESIAN_POINT('Ctrl Pts',(34.3250597723479,89.2960808303433,122.));
#49460=CARTESIAN_POINT('Ctrl Pts',(34.3795261020684,89.3506856242928,122.));
#49461=CARTESIAN_POINT('Ctrl Pts',(34.398608673689,89.3698167076009,122.));
#49462=CARTESIAN_POINT('Ctrl Pts',(34.4180391901862,89.3886195422968,122.));
#49463=CARTESIAN_POINT('Ctrl Pts',(34.437807076635,89.4070896409747,122.));
#49464=CARTESIAN_POINT('Origin',(36.3549260746835,87.7685555885722,114.));
#49465=CARTESIAN_POINT('Origin',(87.7685555885722,-36.3549260746835,107.));
#49466=CARTESIAN_POINT('Ctrl Pts',(85.8550895919077,-34.718938871308,107.));
#49467=CARTESIAN_POINT('Ctrl Pts',(85.7929520057252,-34.7773329442881,107.));
#49468=CARTESIAN_POINT('Ctrl Pts',(85.7341897911883,-34.8389809220769,107.));
#49469=CARTESIAN_POINT('Ctrl Pts',(85.6788149294007,-34.9035063296324,107.));
#49470=CARTESIAN_POINT('Ctrl Pts',(85.6220849950857,-34.9696107317763,107.));
#49471=CARTESIAN_POINT('Ctrl Pts',(85.5689097568226,-35.0387356044574,107.));
#49472=CARTESIAN_POINT('Ctrl Pts',(85.5193309848105,-35.1105224280004,107.));
#49473=CARTESIAN_POINT('Ctrl Pts',(85.5063931427471,-35.1292555782486,107.));
#49474=CARTESIAN_POINT('Ctrl Pts',(85.493700382435,-35.1481702177695,107.));
#49475=CARTESIAN_POINT('Ctrl Pts',(85.4812538215899,-35.1672604086816,107.));
#49476=CARTESIAN_POINT('Ctrl Pts',(85.4710839964377,-35.1828586053331,107.));
#49477=CARTESIAN_POINT('Ctrl Pts',(85.4610780981857,-35.1985749107462,107.));
#49478=CARTESIAN_POINT('Ctrl Pts',(85.4512455841464,-35.2143914910608,107.));
#49479=CARTESIAN_POINT('Ctrl Pts',(85.4038014085985,-35.2907101833113,107.));
#49480=CARTESIAN_POINT('Ctrl Pts',(85.3603407964668,-35.3694362324884,107.));
#49481=CARTESIAN_POINT('Ctrl Pts',(85.3208984357077,-35.4501770885667,107.));
#49482=CARTESIAN_POINT('Ctrl Pts',(85.2890699426178,-35.5153319051215,107.));
#49483=CARTESIAN_POINT('Ctrl Pts',(85.2598585869202,-35.5817998282397,107.));
#49484=CARTESIAN_POINT('Ctrl Pts',(85.2332997549837,-35.6493923856423,107.));
#49485=CARTESIAN_POINT('Ctrl Pts',(85.2226981116036,-35.6763736998223,107.));
#49486=CARTESIAN_POINT('Ctrl Pts',(85.2125193083794,-35.7035343666522,107.));
#49487=CARTESIAN_POINT('Ctrl Pts',(85.2027663566685,-35.7308629441227,107.));
#49488=CARTESIAN_POINT('Ctrl Pts',(85.1975254516455,-35.7455483935316,107.));
#49489=CARTESIAN_POINT('Ctrl Pts',(85.1924078966035,-35.7602815101748,107.));
#49490=CARTESIAN_POINT('Ctrl Pts',(85.1874181581136,-35.7750480411479,107.));
#49491=CARTESIAN_POINT('Ctrl Pts',(85.1578793261422,-35.8624646618987,107.));
#49492=CARTESIAN_POINT('Ctrl Pts',(85.1327759615655,-35.9511623852848,107.));
#49493=CARTESIAN_POINT('Ctrl Pts',(85.112140634563,-36.0407434031081,107.));
#49494=CARTESIAN_POINT('Ctrl Pts',(85.0911838525134,-36.1317199050104,107.));
#49495=CARTESIAN_POINT('Ctrl Pts',(85.0748348968748,-36.2236082408856,107.));
#49496=CARTESIAN_POINT('Ctrl Pts',(85.0631697088413,-36.3160249059585,107.));
#49497=CARTESIAN_POINT('Ctrl Pts',(85.0515952389178,-36.4077228629263,107.));
#49498=CARTESIAN_POINT('Ctrl Pts',(85.0446316260211,-36.4999418935486,107.));
#49499=CARTESIAN_POINT('Ctrl Pts',(85.0423999978617,-36.5923265809498,107.));
#49500=CARTESIAN_POINT('Ctrl Pts',(85.041289386105,-36.6383035594764,107.));
#49501=CARTESIAN_POINT('Ctrl Pts',(85.041351528784,-36.6843217800467,107.));
#49502=CARTESIAN_POINT('Ctrl Pts',(85.0426061541673,-36.7303381327728,107.));
#49503=CARTESIAN_POINT('Ctrl Pts',(85.0429759351538,-36.7439007248693,107.));
#49504=CARTESIAN_POINT('Ctrl Pts',(85.0434493271816,-36.7574631553908,107.));
#49505=CARTESIAN_POINT('Ctrl Pts',(85.0440268917257,-36.7710243206044,107.));
#49506=CARTESIAN_POINT('Ctrl Pts',(85.0446473903427,-36.7855935741113,107.));
#49507=CARTESIAN_POINT('Ctrl Pts',(85.0453877221699,-36.8001515800913,107.));
#49508=CARTESIAN_POINT('Ctrl Pts',(85.0462479357691,-36.81469441234,107.));
#49509=CARTESIAN_POINT('Ctrl Pts',(85.0518997327028,-36.9102440930122,107.));
#49510=CARTESIAN_POINT('Ctrl Pts',(85.0627241729578,-37.0051720608794,107.));
#49511=CARTESIAN_POINT('Ctrl Pts',(85.0787917132112,-37.0990826739641,107.));
#49512=CARTESIAN_POINT('Ctrl Pts',(85.0811720250204,-37.1129949802541,107.));
#49513=CARTESIAN_POINT('Ctrl Pts',(85.0836674925339,-37.1268849924206,107.));
#49514=CARTESIAN_POINT('Ctrl Pts',(85.0862784373429,-37.1407514548178,107.));
#49515=CARTESIAN_POINT('Ctrl Pts',(85.1032240769739,-37.2307480238492,107.));
#49516=CARTESIAN_POINT('Ctrl Pts',(85.125029602379,-37.3197524279253,107.));
#49517=CARTESIAN_POINT('Ctrl Pts',(85.1513924630333,-37.4075324179485,107.));
#49518=CARTESIAN_POINT('Ctrl Pts',(85.1783512727901,-37.4972967300434,107.));
#49519=CARTESIAN_POINT('Ctrl Pts',(85.2100759987119,-37.5857813453147,107.));
#49520=CARTESIAN_POINT('Ctrl Pts',(85.2462973464537,-37.6727342179368,107.));
#49521=CARTESIAN_POINT('Ctrl Pts',(85.2587874244706,-37.7027178665459,107.));
#49522=CARTESIAN_POINT('Ctrl Pts',(85.2718126244585,-37.7325193017317,107.));
#49523=CARTESIAN_POINT('Ctrl Pts',(85.2853632768146,-37.7621278496479,107.));
#49524=CARTESIAN_POINT('Ctrl Pts',(85.2920542822302,-37.776747880422,107.));
#49525=CARTESIAN_POINT('Ctrl Pts',(85.2988734117231,-37.7913208786982,107.));
#49526=CARTESIAN_POINT('Ctrl Pts',(85.3058195604008,-37.8058455369217,107.));
#49527=CARTESIAN_POINT('Ctrl Pts',(85.3113133364161,-37.8173332292649,107.));
#49528=CARTESIAN_POINT('Ctrl Pts',(85.3168861277483,-37.8287896584371,107.));
#49529=CARTESIAN_POINT('Ctrl Pts',(85.3225327933933,-37.8402052475552,107.));
#49530=CARTESIAN_POINT('Ctrl Pts',(85.3652567183844,-37.9265781273875,107.));
#49531=CARTESIAN_POINT('Ctrl Pts',(85.4122715037245,-38.0107526954899,107.));
#49532=CARTESIAN_POINT('Ctrl Pts',(85.4632344929551,-38.0924793134259,107.));
#49533=CARTESIAN_POINT('Ctrl Pts',(85.5152082030099,-38.175826770247,107.));
#49534=CARTESIAN_POINT('Ctrl Pts',(85.5712885886939,-38.2566289878826,107.));
#49535=CARTESIAN_POINT('Ctrl Pts',(85.6311672093088,-38.3346141495021,107.));
#49536=CARTESIAN_POINT('Ctrl Pts',(85.6915326709731,-38.4132333667752,107.));
#49537=CARTESIAN_POINT('Ctrl Pts',(85.755758840285,-38.488990370614,107.));
#49538=CARTESIAN_POINT('Ctrl Pts',(85.8235790230849,-38.5615873806944,107.));
#49539=CARTESIAN_POINT('Ctrl Pts',(85.8605797386839,-38.601194194071,107.));
#49540=CARTESIAN_POINT('Ctrl Pts',(85.8986510202273,-38.6398600347398,107.));
#49541=CARTESIAN_POINT('Ctrl Pts',(85.9377549083663,-38.677532768249,107.));
#49542=CARTESIAN_POINT('Ctrl Pts',(85.9497220449507,-38.6890619222251,107.));
#49543=CARTESIAN_POINT('Ctrl Pts',(85.9617859169551,-38.7004980423369,107.));
#49544=CARTESIAN_POINT('Ctrl Pts',(85.9739454993829,-38.7118395722585,107.));
#49545=CARTESIAN_POINT('Ctrl Pts',(85.9844912868876,-38.7216758775132,107.));
#49546=CARTESIAN_POINT('Ctrl Pts',(85.995107953485,-38.7314399182998,107.));
#49547=CARTESIAN_POINT('Ctrl Pts',(86.0057857170979,-38.7411226995933,107.));
#49548=CARTESIAN_POINT('Ctrl Pts',(86.0813601784838,-38.8096549323251,107.));
#49549=CARTESIAN_POINT('Ctrl Pts',(86.1601113614648,-38.8742308219701,107.));
#49550=CARTESIAN_POINT('Ctrl Pts',(86.2417119176664,-38.9345685954586,107.));
#49551=CARTESIAN_POINT('Ctrl Pts',(86.3234166776699,-38.9949834202038,107.));
#49552=CARTESIAN_POINT('Ctrl Pts',(86.4079786662187,-39.0511501363062,107.));
#49553=CARTESIAN_POINT('Ctrl Pts',(86.4951145538286,-39.1027600899502,107.));
#49554=CARTESIAN_POINT('Ctrl Pts',(86.5805182077147,-39.1533440541351,107.));
#49555=CARTESIAN_POINT('Ctrl Pts',(86.6683951053336,-39.1995513068559,107.));
#49556=CARTESIAN_POINT('Ctrl Pts',(86.7585125705286,-39.2410554346124,107.));
#49557=CARTESIAN_POINT('Ctrl Pts',(86.7988626922243,-39.2596389200914,107.));
#49558=CARTESIAN_POINT('Ctrl Pts',(86.8396624052801,-39.2772789765588,107.));
#49559=CARTESIAN_POINT('Ctrl Pts',(86.8808925773498,-39.2939433559961,107.));
#49560=CARTESIAN_POINT('Ctrl Pts',(86.9113122273115,-39.3062383468696,107.));
#49561=CARTESIAN_POINT('Ctrl Pts',(86.9419662212818,-39.3180021842847,107.));
#49562=CARTESIAN_POINT('Ctrl Pts',(86.9728422903212,-39.3292375489681,107.));
#49563=CARTESIAN_POINT('Ctrl Pts',(88.5623548711045,-39.3241490284294,107.));
#49564=CARTESIAN_POINT('Ctrl Pts',(88.657188760456,-39.2894583680844,107.));
#49565=CARTESIAN_POINT('Ctrl Pts',(88.7499794959736,-39.2497768208657,107.));
#49566=CARTESIAN_POINT('Ctrl Pts',(88.8404861547626,-39.2054247380955,107.));
#49567=CARTESIAN_POINT('Ctrl Pts',(88.9322657038653,-39.1604488853474,107.));
#49568=CARTESIAN_POINT('Ctrl Pts',(89.0216971461717,-39.1106694981297,107.));
#49569=CARTESIAN_POINT('Ctrl Pts',(89.1084952256704,-39.0563799521656,107.));
#49570=CARTESIAN_POINT('Ctrl Pts',(89.1330082394292,-39.0410478112373,107.));
#49571=CARTESIAN_POINT('Ctrl Pts',(89.1573109820009,-39.0253557402474,107.));
#49572=CARTESIAN_POINT('Ctrl Pts',(89.1813964317758,-39.009309891666,107.));
#49573=CARTESIAN_POINT('Ctrl Pts',(89.2007259962726,-38.9964324379353,107.));
#49574=CARTESIAN_POINT('Ctrl Pts',(89.2199177127268,-38.9833254998213,107.));
#49575=CARTESIAN_POINT('Ctrl Pts',(89.2389486655507,-38.9700060224475,107.));
#49576=CARTESIAN_POINT('Ctrl Pts',(89.3216557642,-38.912120569244,107.));
#49577=CARTESIAN_POINT('Ctrl Pts',(89.4014080028997,-38.8501729673376,107.));
#49578=CARTESIAN_POINT('Ctrl Pts',(89.4779390201902,-38.7844605786764,107.));
#49579=CARTESIAN_POINT('Ctrl Pts',(89.5369322084152,-38.7338068248096,107.));
#49580=CARTESIAN_POINT('Ctrl Pts',(89.5940107289622,-38.6809151435346,107.));
#49581=CARTESIAN_POINT('Ctrl Pts',(89.6490350139468,-38.6259099657521,107.));
#49582=CARTESIAN_POINT('Ctrl Pts',(89.6783237536614,-38.5966313965626,107.));
#49583=CARTESIAN_POINT('Ctrl Pts',(89.7070301904271,-38.5667538616209,107.));
#49584=CARTESIAN_POINT('Ctrl Pts',(89.7351312539879,-38.5362952954457,107.));
#49585=CARTESIAN_POINT('Ctrl Pts',(89.7447672571528,-38.5258508921785,107.));
#49586=CARTESIAN_POINT('Ctrl Pts',(89.7543313446827,-38.5153388769912,107.));
#49587=CARTESIAN_POINT('Ctrl Pts',(89.7638159499299,-38.5047675856174,107.));
#49588=CARTESIAN_POINT('Ctrl Pts',(89.8296131402258,-38.4314317690959,107.));
#49589=CARTESIAN_POINT('Ctrl Pts',(89.8916781800482,-38.3551493287763,107.));
#49590=CARTESIAN_POINT('Ctrl Pts',(89.9497673009232,-38.2761988239649,107.));
#49591=CARTESIAN_POINT('Ctrl Pts',(90.0073299643537,-38.1979638417915,107.));
#49592=CARTESIAN_POINT('Ctrl Pts',(90.0609888830627,-38.1171081523236,107.));
#49593=CARTESIAN_POINT('Ctrl Pts',(90.1104611132468,-38.0338804239825,107.));
#49594=CARTESIAN_POINT('Ctrl Pts',(90.1585190532459,-37.9530319730435,107.));
#49595=CARTESIAN_POINT('Ctrl Pts',(90.2026264658774,-37.8699444672167,107.));
#49596=CARTESIAN_POINT('Ctrl Pts',(90.2424761999497,-37.784835528788,107.));
#49597=CARTESIAN_POINT('Ctrl Pts',(90.2632806160433,-37.7404025655683,107.));
#49598=CARTESIAN_POINT('Ctrl Pts',(90.2829237462882,-37.6954185336514,107.));
#49599=CARTESIAN_POINT('Ctrl Pts',(90.3013561905801,-37.649914163883,107.));
#49600=CARTESIAN_POINT('Ctrl Pts',(90.3084142720207,-37.6324898037361,107.));
#49601=CARTESIAN_POINT('Ctrl Pts',(90.3152947941375,-37.6149891503516,107.));
#49602=CARTESIAN_POINT('Ctrl Pts',(90.3219948213491,-37.5974139378534,107.));
#49603=CARTESIAN_POINT('Ctrl Pts',(90.3272365572998,-37.5836640499377,107.));
#49604=CARTESIAN_POINT('Ctrl Pts',(90.3323679171457,-37.5698680261879,107.));
#49605=CARTESIAN_POINT('Ctrl Pts',(90.3373823657084,-37.5560414099326,107.));
#49606=CARTESIAN_POINT('Ctrl Pts',(90.3690660536423,-37.4686782254983,107.));
#49607=CARTESIAN_POINT('Ctrl Pts',(90.396140915987,-37.3799541005099,107.));
#49608=CARTESIAN_POINT('Ctrl Pts',(90.4183556967036,-37.290092587238,107.));
#49609=CARTESIAN_POINT('Ctrl Pts',(90.4233396687901,-37.2699318087223,107.));
#49610=CARTESIAN_POINT('Ctrl Pts',(90.4280788071154,-37.2497137405306,107.));
#49611=CARTESIAN_POINT('Ctrl Pts',(90.432569913541,-37.2294408516372,107.));
#49612=CARTESIAN_POINT('Ctrl Pts',(90.4529356667892,-37.1375096850815,107.));
#49613=CARTESIAN_POINT('Ctrl Pts',(90.4682052082885,-37.0444509023185,107.));
#49614=CARTESIAN_POINT('Ctrl Pts',(90.4784883629424,-36.9506560897443,107.));
#49615=CARTESIAN_POINT('Ctrl Pts',(90.4892222257724,-36.852750273269,107.));
#49616=CARTESIAN_POINT('Ctrl Pts',(90.4945230058311,-36.7540412554223,107.));
#49617=CARTESIAN_POINT('Ctrl Pts',(90.4944581501752,-36.654989052644,107.));
#49618=CARTESIAN_POINT('Ctrl Pts',(90.4944327816927,-36.616244489274,107.));
#49619=CARTESIAN_POINT('Ctrl Pts',(90.4935858683382,-36.5774476751947,107.));
#49620=CARTESIAN_POINT('Ctrl Pts',(90.4919192227104,-36.5386273681288,107.));
#49621=CARTESIAN_POINT('Ctrl Pts',(90.4913861838263,-36.526211571505,107.));
#49622=CARTESIAN_POINT('Ctrl Pts',(90.4907692984578,-36.5137946831277,107.));
#49623=CARTESIAN_POINT('Ctrl Pts',(90.4900693277303,-36.5013873123494,107.));
#49624=CARTESIAN_POINT('Ctrl Pts',(90.4848301144401,-36.4085193404114,107.));
#49625=CARTESIAN_POINT('Ctrl Pts',(90.4749344807815,-36.3160346027814,107.));
#49626=CARTESIAN_POINT('Ctrl Pts',(90.460505885687,-36.2243046763152,107.));
#49627=CARTESIAN_POINT('Ctrl Pts',(90.4461112789299,-36.132790831018,107.));
#49628=CARTESIAN_POINT('Ctrl Pts',(90.4272046315754,-36.0420272996474,107.));
#49629=CARTESIAN_POINT('Ctrl Pts',(90.403859856107,-35.9523999917909,107.));
#49630=CARTESIAN_POINT('Ctrl Pts',(90.38091122944,-35.8642936131306,107.));
#49631=CARTESIAN_POINT('Ctrl Pts',(90.3536733546584,-35.7772844376027,107.));
#49632=CARTESIAN_POINT('Ctrl Pts',(90.3221760039316,-35.69176815752,107.));
#49633=CARTESIAN_POINT('Ctrl Pts',(90.3063345620639,-35.6487581535541,107.));
#49634=CARTESIAN_POINT('Ctrl Pts',(90.2894150702694,-35.6061263179827,107.));
#49635=CARTESIAN_POINT('Ctrl Pts',(90.2714178987872,-35.5639267820646,107.));
#49636=CARTESIAN_POINT('Ctrl Pts',(90.2658521882548,-35.5508763756854,107.));
#49637=CARTESIAN_POINT('Ctrl Pts',(90.2601833945565,-35.537867334519,107.));
#49638=CARTESIAN_POINT('Ctrl Pts',(90.2544114877658,-35.5249013171903,107.));
#49639=CARTESIAN_POINT('Ctrl Pts',(90.2487320296277,-35.5121429766095,107.));
#49640=CARTESIAN_POINT('Ctrl Pts',(90.2429562163594,-35.4994341571851,107.));
#49641=CARTESIAN_POINT('Ctrl Pts',(90.2370858376439,-35.4867793444242,107.));
#49642=CARTESIAN_POINT('Ctrl Pts',(90.1996060377885,-35.4059839013239,107.));
#49643=CARTESIAN_POINT('Ctrl Pts',(90.1582560808094,-35.3273452367495,107.));
#49644=CARTESIAN_POINT('Ctrl Pts',(90.1131056428511,-35.2512109414872,107.));
#49645=CARTESIAN_POINT('Ctrl Pts',(90.0687126367815,-35.1763538551657,107.));
#49646=CARTESIAN_POINT('Ctrl Pts',(90.0206451378295,-35.1039171481911,107.));
#49647=CARTESIAN_POINT('Ctrl Pts',(89.9689331610032,-35.0342653872491,107.));
#49648=CARTESIAN_POINT('Ctrl Pts',(89.9187987000732,-34.9667384099034,107.));
#49649=CARTESIAN_POINT('Ctrl Pts',(89.8652382823866,-34.9018286150414,107.));
#49650=CARTESIAN_POINT('Ctrl Pts',(89.8082515482804,-34.8399084971231,107.));
#49651=CARTESIAN_POINT('Ctrl Pts',(89.7872839743132,-34.8171257447357,107.));
#49652=CARTESIAN_POINT('Ctrl Pts',(89.7658523072769,-34.7947481639537,107.));
#49653=CARTESIAN_POINT('Ctrl Pts',(89.7439557180669,-34.7727959191418,107.));
#49654=CARTESIAN_POINT('Ctrl Pts',(89.7248782826417,-34.7536699936919,107.));
#49655=CARTESIAN_POINT('Ctrl Pts',(89.7054479137747,-34.7348669548371,107.));
#49656=CARTESIAN_POINT('Ctrl Pts',(89.6856747483211,-34.7163919311051,107.));
#49657=CARTESIAN_POINT('Origin',(87.7685555885722,-36.3549260746835,124.208423447177));
#49658=CARTESIAN_POINT('Ctrl Pts',(84.691755941294,-36.3529984690253,121.708423447177));
#49659=CARTESIAN_POINT('Ctrl Pts',(84.6908332620481,-36.2297235581181,121.702019850418));
#49660=CARTESIAN_POINT('Ctrl Pts',(84.7533597477157,-35.0938166732982,121.642966745928));
#49661=CARTESIAN_POINT('Ctrl Pts',(86.1660867790185,-33.1013875491387,121.531264133707));
#49662=CARTESIAN_POINT('Ctrl Pts',(89.6167530478622,-33.2347627935352,121.373315610515));
#49663=CARTESIAN_POINT('Ctrl Pts',(91.3916431606975,-36.1967043155478,121.215367087322));
#49664=CARTESIAN_POINT('Ctrl Pts',(89.8816248388871,-39.3022907437215,121.05741856413));
#49665=CARTESIAN_POINT('Ctrl Pts',(86.455733936694,-39.7354988616288,120.899470040937));
#49666=CARTESIAN_POINT('Ctrl Pts',(84.8091869094529,-37.7971275491863,120.783138335286));
#49667=CARTESIAN_POINT('Ctrl Pts',(84.6923092768517,-36.5704857478685,120.719456137367));
#49668=CARTESIAN_POINT('Ctrl Pts',(84.6942411071791,-36.3576097921547,120.708423447177));
#49669=CARTESIAN_POINT('Ctrl Pts',(84.6982768768212,-36.3579423122256,121.791576552823));
#49670=CARTESIAN_POINT('Ctrl Pts',(84.7032618946881,-35.6649235243351,121.755752019753));
#49671=CARTESIAN_POINT('Ctrl Pts',(85.2756495863919,-33.9437323409503,121.667277978953));
#49672=CARTESIAN_POINT('Ctrl Pts',(88.1200899288066,-32.7460654788916,121.526154430423));
#49673=CARTESIAN_POINT('Ctrl Pts',(90.9824824119093,-34.6751864614649,121.36820590723));
#49674=CARTESIAN_POINT('Ctrl Pts',(90.9320921383769,-38.128468693812,121.210257384038));
#49675=CARTESIAN_POINT('Ctrl Pts',(88.0128423765734,-39.9731538131696,121.052308860845));
#49676=CARTESIAN_POINT('Ctrl Pts',(85.237995407928,-38.7047118441066,120.912748583773));
#49677=CARTESIAN_POINT('Ctrl Pts',(84.7024656403392,-37.0159744647791,120.825837814433));
#49678=CARTESIAN_POINT('Ctrl Pts',(84.69811441609,-36.3527751945784,120.791576552823));
#49679=CARTESIAN_POINT('Ctrl Pts',(89.6820215852375,-34.7189388713087,122.));
#49680=CARTESIAN_POINT('Ctrl Pts',(90.223216971559,-35.3519260775303,121.947350492269));
#49681=CARTESIAN_POINT('Ctrl Pts',(90.618554680914,-37.1869584406053,121.842051476808));
#49682=CARTESIAN_POINT('Ctrl Pts',(88.6277565795612,-39.2001257327075,121.684102953615));
#49683=CARTESIAN_POINT('Ctrl Pts',(85.8568533037203,-38.6278813322613,121.526154430423));
#49684=CARTESIAN_POINT('Ctrl Pts',(84.8197363293867,-35.9976144118095,121.36820590723));
#49685=CARTESIAN_POINT('Ctrl Pts',(86.455975393989,-33.6899567439338,121.210257384038));
#49686=CARTESIAN_POINT('Ctrl Pts',(89.282411812344,-33.7992042395474,121.052308860845));
#49687=CARTESIAN_POINT('Ctrl Pts',(90.7362220804628,-36.2253268299709,120.894360337653));
#49688=CARTESIAN_POINT('Ctrl Pts',(89.4993679645826,-38.7691087830952,120.73641181446));
#49689=CARTESIAN_POINT('Ctrl Pts',(86.6932250180163,-39.1239490098176,120.578463291268));
#49690=CARTESIAN_POINT('Ctrl Pts',(84.8620583484337,-36.9682371583514,120.420514768075));
#49691=CARTESIAN_POINT('Ctrl Pts',(85.6661210457745,-34.2564369070682,120.262566244883));
#49692=CARTESIAN_POINT('Ctrl Pts',(88.376398796949,-33.4472816613919,120.10461772169));
#49693=CARTESIAN_POINT('Ctrl Pts',(90.5355628215429,-35.2743949431641,119.946669198498));
#49694=CARTESIAN_POINT('Ctrl Pts',(90.1859659201536,-38.0811949957465,119.788720675306));
#49695=CARTESIAN_POINT('Ctrl Pts',(87.6445764098185,-39.3228385196818,119.630772152113));
#49696=CARTESIAN_POINT('Ctrl Pts',(85.2155951394299,-37.8735665809373,119.47282362892));
#49697=CARTESIAN_POINT('Ctrl Pts',(85.101305420113,-35.047389246126,119.314875105728));
#49698=CARTESIAN_POINT('Ctrl Pts',(87.4053303288848,-33.4067159017789,119.156926582536));
#49699=CARTESIAN_POINT('Ctrl Pts',(90.0386805233624,-34.4390949995566,118.998978059343));
#49700=CARTESIAN_POINT('Ctrl Pts',(90.613777487181,-37.2084998929576,118.841029536151));
#49701=CARTESIAN_POINT('Ctrl Pts',(88.6091982866193,-39.2039953523912,118.683081012958));
#49702=CARTESIAN_POINT('Ctrl Pts',(85.8424339199087,-38.6163263546765,118.525132489766));
#49703=CARTESIAN_POINT('Ctrl Pts',(84.82202548926,-35.9783144973492,118.367183966573));
#49704=CARTESIAN_POINT('Ctrl Pts',(86.4731462852742,-33.6817649045862,118.209235443381));
#49705=CARTESIAN_POINT('Ctrl Pts',(89.2987752983603,-33.8088892434902,118.051286920188));
#49706=CARTESIAN_POINT('Ctrl Pts',(90.7370006401761,-36.2444277433863,117.893338396996));
#49707=CARTESIAN_POINT('Ctrl Pts',(89.4838271348459,-38.7801517194402,117.735389873803));
#49708=CARTESIAN_POINT('Ctrl Pts',(86.6754690861509,-39.1169973633819,117.577441350611));
#49709=CARTESIAN_POINT('Ctrl Pts',(84.8581793244705,-36.9495569744204,117.419492827418));
#49710=CARTESIAN_POINT('Ctrl Pts',(85.679639206362,-34.2429828335689,117.261544304226));
#49711=CARTESIAN_POINT('Ctrl Pts',(88.3950560404819,-33.4512433975761,117.103595781033));
#49712=CARTESIAN_POINT('Ctrl Pts',(90.5424439690061,-35.2921847334048,116.945647257841));
#49713=CARTESIAN_POINT('Ctrl Pts',(90.174831666992,-38.0966813215517,116.787698734649));
#49714=CARTESIAN_POINT('Ctrl Pts',(87.6255220282537,-39.3219814004557,116.629750211456));
#49715=CARTESIAN_POINT('Ctrl Pts',(85.2058965684871,-37.8571426543901,116.471801688264));
#49716=CARTESIAN_POINT('Ctrl Pts',(85.1097561024807,-35.0302898233568,116.313853165071));
#49717=CARTESIAN_POINT('Ctrl Pts',(87.4242682667827,-33.4044443944109,116.155904641879));
#49718=CARTESIAN_POINT('Ctrl Pts',(90.0509352747254,-34.4537109701243,115.997956118686));
#49719=CARTESIAN_POINT('Ctrl Pts',(90.6082380366736,-37.2267514582979,115.840007595494));
#49720=CARTESIAN_POINT('Ctrl Pts',(88.5908870879659,-39.2093343865188,115.682059072301));
#49721=CARTESIAN_POINT('Ctrl Pts',(85.8279531788398,-38.6039121113032,115.524110549109));
#49722=CARTESIAN_POINT('Ctrl Pts',(84.824504453864,-35.9594025965029,115.366162025916));
#49723=CARTESIAN_POINT('Ctrl Pts',(86.4903373534603,-33.6735021900661,115.208213502724));
#49724=CARTESIAN_POINT('Ctrl Pts',(89.3150918515823,-33.818767267991,115.050264979531));
#49725=CARTESIAN_POINT('Ctrl Pts',(90.7376489558074,-36.2634904021606,114.892316456339));
#49726=CARTESIAN_POINT('Ctrl Pts',(89.4682194048531,-38.7911154797165,114.734367933146));
#49727=CARTESIAN_POINT('Ctrl Pts',(86.6577563646153,-39.1099217170804,114.576419409954));
#49728=CARTESIAN_POINT('Ctrl Pts',(84.8544211973079,-36.9308571948879,114.418470886761));
#49729=CARTESIAN_POINT('Ctrl Pts',(85.6932430531688,-34.2296134421594,114.260522363569));
#49730=CARTESIAN_POINT('Ctrl Pts',(88.4136876671025,-33.4553260148786,114.102573840377));
#49731=CARTESIAN_POINT('Ctrl Pts',(90.5492106462378,-35.3100177744735,113.944625317184));
#49732=CARTESIAN_POINT('Ctrl Pts',(90.1635982543887,-38.1120961104195,113.786676793992));
#49733=CARTESIAN_POINT('Ctrl Pts',(87.6064735193736,-39.3210018168745,113.628728270799));
#49734=CARTESIAN_POINT('Ctrl Pts',(85.1963036669977,-37.8406568570009,113.470779747607));
#49735=CARTESIAN_POINT('Ctrl Pts',(85.1183164004075,-35.0132449832592,113.312831224414));
#49736=CARTESIAN_POINT('Ctrl Pts',(87.443220402345,-33.4022945497262,113.154882701222));
#49737=CARTESIAN_POINT('Ctrl Pts',(90.0630959230123,-34.4684053196434,112.996934178029));
#49738=CARTESIAN_POINT('Ctrl Pts',(90.6025815077325,-37.2449670822204,112.838985654837));
#49739=CARTESIAN_POINT('Ctrl Pts',(88.5725419845522,-39.2145557326372,112.681037131644));
#49740=CARTESIAN_POINT('Ctrl Pts',(85.8135524482776,-38.5914051438921,112.523088608452));
#49741=CARTESIAN_POINT('Ctrl Pts',(84.8271048005757,-35.9405070025316,112.365140085259));
#49742=CARTESIAN_POINT('Ctrl Pts',(86.5075811221681,-33.6653500299051,112.207191562067));
#49743=CARTESIAN_POINT('Ctrl Pts',(89.3313446416448,-33.8287498573211,112.049243038874));
#49744=CARTESIAN_POINT('Ctrl Pts',(90.7381748567804,-36.2825568308435,111.891294515682));
#49745=CARTESIAN_POINT('Ctrl Pts',(89.4525415983201,-38.8019787967437,111.73334599249));
#49746=CARTESIAN_POINT('Ctrl Pts',(86.6400894409389,-39.1027324832979,111.575397469297));
#49747=CARTESIAN_POINT('Ctrl Pts',(84.8507832188739,-36.9121336699122,111.417448946105));
#49748=CARTESIAN_POINT('Ctrl Pts',(85.706932464372,-34.2163316766427,111.259500422912));
#49749=CARTESIAN_POINT('Ctrl Pts',(88.432292695164,-33.4595281816538,111.10155189972));
#49750=CARTESIAN_POINT('Ctrl Pts',(90.5558626780312,-35.3278938967584,110.943603376527));
#49751=CARTESIAN_POINT('Ctrl Pts',(90.1522660950599,-38.1274384517549,110.785654853335));
#49752=CARTESIAN_POINT('Ctrl Pts',(87.587431693009,-39.3198999431135,110.627706330142));
#49753=CARTESIAN_POINT('Ctrl Pts',(85.1868168186886,-37.8241098033121,110.46975780695));
#49754=CARTESIAN_POINT('Ctrl Pts',(85.1269859664566,-34.9962554604981,110.311809283757));
#49755=CARTESIAN_POINT('Ctrl Pts',(87.4621859519783,-33.4002664403736,110.153860760565));
#49756=CARTESIAN_POINT('Ctrl Pts',(90.0751619669469,-34.4831774510166,109.995912237372));
#49757=CARTESIAN_POINT('Ctrl Pts',(90.5968081355154,-37.263146007451,109.83796371418));
#49758=CARTESIAN_POINT('Ctrl Pts',(88.5541637277013,-39.2196591826207,109.680015190987));
#49759=CARTESIAN_POINT('Ctrl Pts',(85.7992323328324,-38.5788059561733,109.522066667795));
#49760=CARTESIAN_POINT('Ctrl Pts',(84.8298263995735,-35.9216285176768,109.364118144602));
#49761=CARTESIAN_POINT('Ctrl Pts',(86.5248769270656,-33.6573087131898,109.20616962141));
#49762=CARTESIAN_POINT('Ctrl Pts',(89.3475329025042,-33.8388366962972,109.048221098218));
#49763=CARTESIAN_POINT('Ctrl Pts',(90.7385785187742,-36.3016260452323,108.890272575025));
#49764=CARTESIAN_POINT('Ctrl Pts',(89.4367939557108,-38.812741629989,108.732324051833));
#49765=CARTESIAN_POINT('Ctrl Pts',(86.6224698783981,-39.095429120668,108.57437552864));
#49766=CARTESIAN_POINT('Ctrl Pts',(84.8472638220703,-36.8933888944926,108.416427005448));
#49767=CARTESIAN_POINT('Ctrl Pts',(85.7207104071022,-34.2031345408651,108.258478482255));
#49768=CARTESIAN_POINT('Ctrl Pts',(88.4508630942718,-33.4638570130842,108.100529959063));
#49769=CARTESIAN_POINT('Ctrl Pts',(90.5624147285815,-35.3457973731139,107.94258143587));
#49770=CARTESIAN_POINT('Ctrl Pts',(90.140804932313,-38.1427385431604,107.784632912678));
#49771=CARTESIAN_POINT('Ctrl Pts',(87.5684605240929,-39.3186124160521,107.626684389485));
#49772=CARTESIAN_POINT('Ctrl Pts',(85.1773064515634,-37.8076325870251,107.468735866293));
#49773=CARTESIAN_POINT('Ctrl Pts',(85.1360317379698,-34.9790536882396,107.3107873431));
#49774=CARTESIAN_POINT('Ctrl Pts',(87.4806142131685,-33.3989116983333,107.152838819908));
#49775=CARTESIAN_POINT('Ctrl Pts',(90.0882639790973,-34.4968785995462,106.994890296715));
#49776=CARTESIAN_POINT('Ctrl Pts',(90.5885430574506,-37.283604361099,106.836941773523));
#49777=CARTESIAN_POINT('Ctrl Pts',(89.223305985034,-38.5719224173531,106.731642758061));
#49778=CARTESIAN_POINT('Ctrl Pts',(88.4187555865469,-38.7870128767187,106.678993250331));
#49779=CARTESIAN_POINT('Ctrl Pts',(89.8228871389145,-34.5985007534568,122.10700224989));
#49780=CARTESIAN_POINT('Ctrl Pts',(90.4039242511275,-35.2780872164357,122.054352742159));
#49781=CARTESIAN_POINT('Ctrl Pts',(90.8283659348487,-37.2482110053789,121.949053726697));
#49782=CARTESIAN_POINT('Ctrl Pts',(88.6910092443729,-39.4095836618517,121.791105203505));
#49783=CARTESIAN_POINT('Ctrl Pts',(85.7161175909924,-38.7952117689661,121.633156680312));
#49784=CARTESIAN_POINT('Ctrl Pts',(84.6026501316896,-35.9713098392101,121.47520815712));
#49785=CARTESIAN_POINT('Ctrl Pts',(86.3593458556655,-33.4937670123354,121.317259633928));
#49786=CARTESIAN_POINT('Ctrl Pts',(89.3938588908501,-33.6110570908767,121.159311110735));
#49787=CARTESIAN_POINT('Ctrl Pts',(90.9546957738743,-36.2157859918298,121.001362587543));
#49788=CARTESIAN_POINT('Ctrl Pts',(89.6267869226841,-38.946836103304,120.84341406435));
#49789=CARTESIAN_POINT('Ctrl Pts',(86.6140613242422,-39.3277989604213,120.685465541158));
#49790=CARTESIAN_POINT('Ctrl Pts',(84.6480878134429,-37.0133878981752,120.527517017965));
#49791=CARTESIAN_POINT('Ctrl Pts',(85.5113440042922,-34.1019503162447,120.369568494773));
#49792=CARTESIAN_POINT('Ctrl Pts',(88.4211470026898,-33.2332266737997,120.21161997158));
#49793=CARTESIAN_POINT('Ctrl Pts',(90.7392643801702,-35.1948483944551,120.053671448388));
#49794=CARTESIAN_POINT('Ctrl Pts',(90.3639308515484,-38.2082794737486,119.895722925195));
#49795=CARTESIAN_POINT('Ctrl Pts',(87.6354493097342,-39.5413303196711,119.737774402003));
#49796=CARTESIAN_POINT('Ctrl Pts',(85.0276512784935,-37.9853658687859,119.57982587881));
#49797=CARTESIAN_POINT('Ctrl Pts',(84.9049477777875,-34.9511309903593,119.421877355618));
#49798=CARTESIAN_POINT('Ctrl Pts',(87.378590409072,-33.1896745438001,119.263928832425));
#49799=CARTESIAN_POINT('Ctrl Pts',(90.2058025973435,-34.2980553335162,119.105980309233));
#49800=CARTESIAN_POINT('Ctrl Pts',(90.8232370536329,-37.2713382965273,118.948031786041));
#49801=CARTESIAN_POINT('Ctrl Pts',(88.6710847268857,-39.4137381552255,118.790083262848));
#49802=CARTESIAN_POINT('Ctrl Pts',(85.7006366808786,-38.7828061369573,118.632134739656));
#49803=CARTESIAN_POINT('Ctrl Pts',(84.605107814951,-35.9505891035064,118.474186216463));
#49804=CARTESIAN_POINT('Ctrl Pts',(86.3777808337504,-33.4849721060991,118.316237693271));
#49805=CARTESIAN_POINT('Ctrl Pts',(89.4114270240989,-33.6214550855102,118.158289170078));
#49806=CARTESIAN_POINT('Ctrl Pts',(90.9555316496024,-36.2362930764281,118.000340646886));
#49807=CARTESIAN_POINT('Ctrl Pts',(89.6101020080307,-38.9586919986172,117.842392123693));
#49808=CARTESIAN_POINT('Ctrl Pts',(86.5949982360553,-39.3203355476276,117.684443600501));
#49809=CARTESIAN_POINT('Ctrl Pts',(84.6439232234655,-36.9933325163275,117.526495077308));
#49810=CARTESIAN_POINT('Ctrl Pts',(85.5258573449243,-34.0875057806646,117.368546554116));
#49811=CARTESIAN_POINT('Ctrl Pts',(88.4411777553128,-33.2374800651071,117.210598030923));
#49812=CARTESIAN_POINT('Ctrl Pts',(90.7466521039974,-35.2139478336032,117.052649507731));
#49813=CARTESIAN_POINT('Ctrl Pts',(90.3519769168565,-38.2249058719997,116.894700984538));
#49814=CARTESIAN_POINT('Ctrl Pts',(87.6149921825685,-39.5404101010355,116.736752461346));
#49815=CARTESIAN_POINT('Ctrl Pts',(85.0172387180843,-37.9677328454945,116.578803938154));
#49816=CARTESIAN_POINT('Ctrl Pts',(84.9140205825513,-34.9327727421602,116.420855414961));
#49817=CARTESIAN_POINT('Ctrl Pts',(87.3989225202199,-33.1872358125861,116.262906891769));
#49818=CARTESIAN_POINT('Ctrl Pts',(90.2189595190818,-34.3137473027115,116.104958368576));
#49819=CARTESIAN_POINT('Ctrl Pts',(90.8172897998176,-37.2909335057378,115.947009845384));
#49820=CARTESIAN_POINT('Ctrl Pts',(88.6514254942766,-39.4194702384063,115.789061322191));
#49821=CARTESIAN_POINT('Ctrl Pts',(85.6850898965081,-38.7694779817249,115.631112798999));
#49822=CARTESIAN_POINT('Ctrl Pts',(84.6077692759893,-35.9302849462058,115.473164275806));
#49823=CARTESIAN_POINT('Ctrl Pts',(86.3962374741195,-33.4761011070012,115.315215752614));
#49824=CARTESIAN_POINT('Ctrl Pts',(89.428944769455,-33.6320603104907,115.157267229421));
#49825=CARTESIAN_POINT('Ctrl Pts',(90.9562276929385,-36.2567590901549,114.999318706229));
#49826=CARTESIAN_POINT('Ctrl Pts',(89.5933452680577,-38.9704628890774,114.841370183036));
#49827=CARTESIAN_POINT('Ctrl Pts',(86.5759815392568,-39.3127390063453,114.683421659844));
#49828=CARTESIAN_POINT('Ctrl Pts',(84.63988843047,-36.9732560962893,114.525473136651));
#49829=CARTESIAN_POINT('Ctrl Pts',(85.5404626798244,-34.0731521613009,114.367524613459));
#49830=CARTESIAN_POINT('Ctrl Pts',(88.4611810051576,-33.2418632365599,114.209576090266));
#49831=CARTESIAN_POINT('Ctrl Pts',(90.7539169305229,-35.2330937076193,114.051627567074));
#49832=CARTESIAN_POINT('Ctrl Pts',(90.3399165228022,-38.2414554669066,113.893679043881));
#49833=CARTESIAN_POINT('Ctrl Pts',(87.5945413604231,-39.5393584024631,113.735730520689));
#49834=CARTESIAN_POINT('Ctrl Pts',(85.0069396063031,-37.9500333965531,113.577781997497));
#49835=CARTESIAN_POINT('Ctrl Pts',(84.9232110725532,-34.9144730949001,113.419833474304));
#49836=CARTESIAN_POINT('Ctrl Pts',(87.4192698742361,-33.1849277006198,113.261884951112));
#49837=CARTESIAN_POINT('Ctrl Pts',(90.2320154100628,-34.3295234209606,113.103936427919));
#49838=CARTESIAN_POINT('Ctrl Pts',(90.8112168484876,-37.3104901275948,112.945987904727));
#49839=CARTESIAN_POINT('Ctrl Pts',(88.6317298609064,-39.4250759696213,112.788039381534));
#49840=CARTESIAN_POINT('Ctrl Pts',(85.6696290128585,-38.7560502762959,112.630090858342));
#49841=CARTESIAN_POINT('Ctrl Pts',(84.6105610550442,-35.90999829626,112.472142335149));
#49842=CARTESIAN_POINT('Ctrl Pts',(86.4147506947176,-33.4673488010541,112.314193811957));
#49843=CARTESIAN_POINT('Ctrl Pts',(89.4463940575345,-33.6427777981548,112.156245288764));
#49844=CARTESIAN_POINT('Ctrl Pts',(90.9567923096934,-36.2772291513235,111.998296765572));
#49845=CARTESIAN_POINT('Ctrl Pts',(89.5765132926491,-38.9821259418566,111.840348242379));
#49846=CARTESIAN_POINT('Ctrl Pts',(86.5570140118646,-39.3050205154978,111.682399719187));
#49847=CARTESIAN_POINT('Ctrl Pts',(84.635982631313,-36.9531541827155,111.524451195994));
#49848=CARTESIAN_POINT('Ctrl Pts',(85.5551598782013,-34.0588926186737,111.366502672802));
#49849=CARTESIAN_POINT('Ctrl Pts',(88.4811556983105,-33.2463747584794,111.208554149609));
#49850=CARTESIAN_POINT('Ctrl Pts',(90.7610586716412,-35.2522858344048,111.050605626417));
#49851=CARTESIAN_POINT('Ctrl Pts',(90.3277501124856,-38.2579272808382,110.892657103225));
#49852=CARTESIAN_POINT('Ctrl Pts',(87.5740977127464,-39.5381754109516,110.734708580032));
#49853=CARTESIAN_POINT('Ctrl Pts',(84.9967543551262,-37.9322681817453,110.57676005684));
#49854=CARTESIAN_POINT('Ctrl Pts',(84.9325188747787,-34.8962328373287,110.418811533647));
#49855=CARTESIAN_POINT('Ctrl Pts',(87.4396316298405,-33.182750285898,110.260863010455));
#49856=CARTESIAN_POINT('Ctrl Pts',(90.2449697321076,-34.3453830472088,110.102914487262));
#49857=CARTESIAN_POINT('Ctrl Pts',(90.8050184521126,-37.3300073490754,109.94496596407));
#49858=CARTESIAN_POINT('Ctrl Pts',(88.6119986334088,-39.4305551254228,109.787017440877));
#49859=CARTESIAN_POINT('Ctrl Pts',(85.65425467905,-38.7425235614839,109.629068917685));
#49860=CARTESIAN_POINT('Ctrl Pts',(84.6134830127371,-35.8897300149696,109.471120394492));
#49861=CARTESIAN_POINT('Ctrl Pts',(86.4333197823059,-33.4587154986263,109.3131718713));
#49862=CARTESIAN_POINT('Ctrl Pts',(89.4637740659,-33.6536072101161,109.155223348107));
#49863=CARTESIAN_POINT('Ctrl Pts',(90.9572256884785,-36.297702203276,108.997274824915));
#49864=CARTESIAN_POINT('Ctrl Pts',(89.5596063399716,-38.9936811134381,108.839326301722));
#49865=CARTESIAN_POINT('Ctrl Pts',(86.5380973322402,-39.2971794938646,108.68137777853));
#49866=CARTESIAN_POINT('Ctrl Pts',(84.6322041435302,-36.9330294542826,108.523429255337));
#49867=CARTESIAN_POINT('Ctrl Pts',(85.5699521256195,-34.0447239360583,108.365480732145));
#49868=CARTESIAN_POINT('Ctrl Pts',(88.5010932131953,-33.2510222698536,108.207532208953));
#49869=CARTESIAN_POINT('Ctrl Pts',(90.7680930710965,-35.2715073290129,108.04958368576));
#49870=CARTESIAN_POINT('Ctrl Pts',(90.3154452017761,-38.2743537344842,107.891635162568));
#49871=CARTESIAN_POINT('Ctrl Pts',(87.5537299241789,-39.5367930987136,107.733686639375));
#49872=CARTESIAN_POINT('Ctrl Pts',(84.9865438537246,-37.9145779456297,107.575738116183));
#49873=CARTESIAN_POINT('Ctrl Pts',(84.9422305779652,-34.8777647048748,107.41778959299));
#49874=CARTESIAN_POINT('Ctrl Pts',(87.4594165428971,-33.1812958104484,107.259841069798));
#49875=CARTESIAN_POINT('Ctrl Pts',(90.2590362882839,-34.3600928469906,107.101892546605));
#49876=CARTESIAN_POINT('Ctrl Pts',(90.7961449154706,-37.3519718059513,106.943944023413));
#49877=CARTESIAN_POINT('Ctrl Pts',(89.3304018103147,-38.7351332702527,106.838645007951));
#49878=CARTESIAN_POINT('Ctrl Pts',(88.4666220147327,-38.9660582606223,106.78599550022));
#49879=CARTESIAN_POINT('Ctrl Pts',(89.9637526925915,-34.478062635605,122.21400449978));
#49880=CARTESIAN_POINT('Ctrl Pts',(90.5846315306959,-35.204248355341,122.161354992049));
#49881=CARTESIAN_POINT('Ctrl Pts',(91.0381771887835,-37.3094635701525,122.056055976587));
#49882=CARTESIAN_POINT('Ctrl Pts',(88.7542619091845,-39.6190415909959,121.898107453395));
#49883=CARTESIAN_POINT('Ctrl Pts',(85.5753818782645,-38.962542205671,121.740158930202));
#49884=CARTESIAN_POINT('Ctrl Pts',(84.3855639339925,-35.9450052666105,121.58221040701));
#49885=CARTESIAN_POINT('Ctrl Pts',(86.262716317342,-33.297577280737,121.424261883817));
#49886=CARTESIAN_POINT('Ctrl Pts',(89.5053059693561,-33.4229099422059,121.266313360625));
#49887=CARTESIAN_POINT('Ctrl Pts',(91.1731694672859,-36.2062451536888,121.108364837432));
#49888=CARTESIAN_POINT('Ctrl Pts',(89.7542058807856,-39.1245634235127,120.95041631424));
#49889=CARTESIAN_POINT('Ctrl Pts',(86.5348976304681,-39.5316489110251,120.792467791048));
#49890=CARTESIAN_POINT('Ctrl Pts',(84.4341172784523,-37.058538637999,120.634519267855));
#49891=CARTESIAN_POINT('Ctrl Pts',(85.3565669628098,-33.9474637254213,120.476570744663));
#49892=CARTESIAN_POINT('Ctrl Pts',(88.4658952084306,-33.0191716862075,120.31862222147));
#49893=CARTESIAN_POINT('Ctrl Pts',(90.9429659387973,-35.1153018457461,120.160673698277));
#49894=CARTESIAN_POINT('Ctrl Pts',(90.5418957829432,-38.3353639517507,120.002725175085));
#49895=CARTESIAN_POINT('Ctrl Pts',(87.6263222096498,-39.7598221196604,119.844776651893));
#49896=CARTESIAN_POINT('Ctrl Pts',(84.8397074175569,-38.0971651566346,119.6868281287));
#49897=CARTESIAN_POINT('Ctrl Pts',(84.7085901354619,-34.8548727345926,119.528879605508));
#49898=CARTESIAN_POINT('Ctrl Pts',(87.3518504892593,-32.9726331858213,119.370931082315));
#49899=CARTESIAN_POINT('Ctrl Pts',(90.3729246713247,-34.1570156674757,119.212982559123));
#49900=CARTESIAN_POINT('Ctrl Pts',(91.0326966200846,-37.3341767000971,119.05503403593));
#49901=CARTESIAN_POINT('Ctrl Pts',(88.7329711671524,-39.6234809580597,118.897085512738));
#49902=CARTESIAN_POINT('Ctrl Pts',(85.5588394418481,-38.9492859192382,118.739136989545));
#49903=CARTESIAN_POINT('Ctrl Pts',(84.3881901406422,-35.9228637096635,118.581188466353));
#49904=CARTESIAN_POINT('Ctrl Pts',(86.2824153822265,-33.2881793076119,118.42323994316));
#49905=CARTESIAN_POINT('Ctrl Pts',(89.5240787498378,-33.4340209275303,118.265291419968));
#49906=CARTESIAN_POINT('Ctrl Pts',(91.1740626590286,-36.22815840947,118.107342896775));
#49907=CARTESIAN_POINT('Ctrl Pts',(89.7363768812154,-39.1372322777943,117.949394373583));
#49908=CARTESIAN_POINT('Ctrl Pts',(86.5145273859598,-39.5236737318734,117.791445850391));
#49909=CARTESIAN_POINT('Ctrl Pts',(84.4296671224604,-37.0371080582347,117.633497327198));
#49910=CARTESIAN_POINT('Ctrl Pts',(85.3720754834864,-33.9320287277603,117.475548804006));
#49911=CARTESIAN_POINT('Ctrl Pts',(88.487299470144,-33.0237167326382,117.317600280813));
#49912=CARTESIAN_POINT('Ctrl Pts',(90.9508602389886,-35.1357109338017,117.159651757621));
#49913=CARTESIAN_POINT('Ctrl Pts',(90.5291221667209,-38.3531304224478,117.001703234428));
#49914=CARTESIAN_POINT('Ctrl Pts',(87.6044623368834,-39.7588388016154,116.843754711236));
#49915=CARTESIAN_POINT('Ctrl Pts',(84.8285808676813,-38.0783230365991,116.685806188043));
#49916=CARTESIAN_POINT('Ctrl Pts',(84.718285062622,-34.8352556609635,116.527857664851));
#49917=CARTESIAN_POINT('Ctrl Pts',(87.3735767736571,-32.9700272307613,116.369909141658));
#49918=CARTESIAN_POINT('Ctrl Pts',(90.3869837634382,-34.1737836352987,116.211960618466));
#49919=CARTESIAN_POINT('Ctrl Pts',(91.0263415629614,-37.3551155531776,116.054012095273));
#49920=CARTESIAN_POINT('Ctrl Pts',(88.7119639005876,-39.6296060902939,115.896063572081));
#49921=CARTESIAN_POINT('Ctrl Pts',(85.5422266141761,-38.9350438521467,115.738115048888));
#49922=CARTESIAN_POINT('Ctrl Pts',(84.3910340981148,-35.9011672959088,115.580166525696));
#49923=CARTESIAN_POINT('Ctrl Pts',(86.3021375947785,-33.2787000239364,115.422218002504));
#49924=CARTESIAN_POINT('Ctrl Pts',(89.5427976873277,-33.4453533529904,115.264269479311));
#49925=CARTESIAN_POINT('Ctrl Pts',(91.1748064300696,-36.2500277781493,115.106320956119));
#49926=CARTESIAN_POINT('Ctrl Pts',(89.7184711312623,-39.1498102984383,114.948372432926));
#49927=CARTESIAN_POINT('Ctrl Pts',(86.4942067138983,-39.5155562956101,114.790423909734));
#49928=CARTESIAN_POINT('Ctrl Pts',(84.4253556636322,-37.0156549976906,114.632475386541));
#49929=CARTESIAN_POINT('Ctrl Pts',(85.3876823064798,-33.9166908804425,114.474526863349));
#49930=CARTESIAN_POINT('Ctrl Pts',(88.508674343213,-33.0284004582413,114.316578340156));
#49931=CARTESIAN_POINT('Ctrl Pts',(90.9586232148078,-35.156169640765,114.158629816964));
#49932=CARTESIAN_POINT('Ctrl Pts',(90.5162347912159,-38.3708148233938,114.000681293771));
#49933=CARTESIAN_POINT('Ctrl Pts',(87.5826092014724,-39.7577149880517,113.842732770579));
#49934=CARTESIAN_POINT('Ctrl Pts',(84.8175755456086,-38.0594099361054,113.684784247386));
#49935=CARTESIAN_POINT('Ctrl Pts',(84.7281057446989,-34.8157012065411,113.526835724194));
#49936=CARTESIAN_POINT('Ctrl Pts',(87.3953193461272,-32.9675608515133,113.368887201001));
#49937=CARTESIAN_POINT('Ctrl Pts',(90.4009348971133,-34.1906415222777,113.210938677809));
#49938=CARTESIAN_POINT('Ctrl Pts',(91.0198521892427,-37.3760131729692,113.052990154616));
#49939=CARTESIAN_POINT('Ctrl Pts',(88.6909177372605,-39.6355962066054,112.895041631424));
#49940=CARTESIAN_POINT('Ctrl Pts',(85.5257055774393,-38.9206954086998,112.737093108231));
#49941=CARTESIAN_POINT('Ctrl Pts',(84.3940173095128,-35.8794895899884,112.579144585039));
#49942=CARTESIAN_POINT('Ctrl Pts',(86.321920267267,-33.2693475722032,112.421196061847));
#49943=CARTESIAN_POINT('Ctrl Pts',(89.5614434734244,-33.4568057389885,112.263247538654));
#49944=CARTESIAN_POINT('Ctrl Pts',(91.1754097626062,-36.2719014718034,112.105299015462));
#49945=CARTESIAN_POINT('Ctrl Pts',(89.7004849869781,-39.1622730869696,111.947350492269));
#49946=CARTESIAN_POINT('Ctrl Pts',(86.4739385827902,-39.5073085476977,111.789401969077));
#49947=CARTESIAN_POINT('Ctrl Pts',(84.4211820437524,-36.9941746955189,111.631453445884));
#49948=CARTESIAN_POINT('Ctrl Pts',(85.4033872920303,-33.9014535607047,111.473504922692));
#49949=CARTESIAN_POINT('Ctrl Pts',(88.5300187014573,-33.0332213353051,111.315556399499));
#49950=CARTESIAN_POINT('Ctrl Pts',(90.9662546652511,-35.176677772051,111.157607876307));
#49951=CARTESIAN_POINT('Ctrl Pts',(90.5032341299113,-38.3884161099215,110.999659353114));
#49952=CARTESIAN_POINT('Ctrl Pts',(87.5607637324837,-39.7564508787897,110.841710829922));
#49953=CARTESIAN_POINT('Ctrl Pts',(84.8066918915637,-38.0404265601786,110.683762306729));
#49954=CARTESIAN_POINT('Ctrl Pts',(84.738051783101,-34.7962102141593,110.525813783537));
#49955=CARTESIAN_POINT('Ctrl Pts',(87.4170773077025,-32.9652341314225,110.367865260344));
#49956=CARTESIAN_POINT('Ctrl Pts',(90.4147774972684,-34.2075886434009,110.209916737152));
#49957=CARTESIAN_POINT('Ctrl Pts',(91.0132287687098,-37.3968686906999,110.051968213959));
#49958=CARTESIAN_POINT('Ctrl Pts',(88.6698335391163,-39.6414510682249,109.894019690767));
#49959=CARTESIAN_POINT('Ctrl Pts',(85.5092770252676,-38.9062411667946,109.736071167575));
#49960=CARTESIAN_POINT('Ctrl Pts',(84.3971396259005,-35.8578315122625,109.578122644382));
#49961=CARTESIAN_POINT('Ctrl Pts',(86.3417626375461,-33.2601222840629,109.42017412119));
#49962=CARTESIAN_POINT('Ctrl Pts',(89.5800152292957,-33.4683777239349,109.262225597997));
#49963=CARTESIAN_POINT('Ctrl Pts',(91.1758728581828,-36.2937783613198,109.104277074805));
#49964=CARTESIAN_POINT('Ctrl Pts',(89.6824187242323,-39.1746205968873,108.946328551612));
#49965=CARTESIAN_POINT('Ctrl Pts',(86.4537247860825,-39.4989298670612,108.78838002842));
#49966=CARTESIAN_POINT('Ctrl Pts',(84.41714446499,-36.9726700140725,108.630431505227));
#49967=CARTESIAN_POINT('Ctrl Pts',(85.4191938441369,-33.8863133312516,108.472482982035));
#49968=CARTESIAN_POINT('Ctrl Pts',(88.5513233321187,-33.038187526623,108.314534458842));
#49969=CARTESIAN_POINT('Ctrl Pts',(90.9737714136116,-35.1972172849119,108.15658593565));
#49970=CARTESIAN_POINT('Ctrl Pts',(90.4900854712392,-38.405968925808,107.998637412458));
#49971=CARTESIAN_POINT('Ctrl Pts',(87.5389993242649,-39.7549737813751,107.840688889265));
#49972=CARTESIAN_POINT('Ctrl Pts',(84.795781255886,-38.0215233042344,107.682740366073));
#49973=CARTESIAN_POINT('Ctrl Pts',(84.7484294179605,-34.77647572151,107.52479184288));
#49974=CARTESIAN_POINT('Ctrl Pts',(87.4382188726258,-32.9636799225635,107.366843319688));
#49975=CARTESIAN_POINT('Ctrl Pts',(90.4298085974705,-34.223307094435,107.208894796495));
#49976=CARTESIAN_POINT('Ctrl Pts',(91.0037467734906,-37.4203392508036,107.050946273303));
#49977=CARTESIAN_POINT('Ctrl Pts',(89.4374976355955,-38.8983441231523,106.945647257841));
#49978=CARTESIAN_POINT('Ctrl Pts',(88.5144884429186,-39.1451036445258,106.89299775011));
#49979=CARTESIAN_POINT('Ctrl Pts',(90.1046182462686,-34.3576245177531,122.321006749669));
#49980=CARTESIAN_POINT('Ctrl Pts',(90.7653388102644,-35.1304094942464,122.268357241939));
#49981=CARTESIAN_POINT('Ctrl Pts',(91.2479884427182,-37.3707161349261,122.163058226477));
#49982=CARTESIAN_POINT('Ctrl Pts',(88.8175145739961,-39.82849952014,122.005109703284));
#49983=CARTESIAN_POINT('Ctrl Pts',(85.4346461655366,-39.1298726423758,121.847161180092));
#49984=CARTESIAN_POINT('Ctrl Pts',(84.1684777362954,-35.918700694011,121.6892126569));
#49985=CARTESIAN_POINT('Ctrl Pts',(86.1660867790185,-33.1013875491387,121.531264133707));
#49986=CARTESIAN_POINT('Ctrl Pts',(89.6167530478622,-33.2347627935352,121.373315610515));
#49987=CARTESIAN_POINT('Ctrl Pts',(91.3916431606975,-36.1967043155478,121.215367087322));
#49988=CARTESIAN_POINT('Ctrl Pts',(89.8816248388871,-39.3022907437215,121.05741856413));
#49989=CARTESIAN_POINT('Ctrl Pts',(86.455733936694,-39.7354988616288,120.899470040937));
#49990=CARTESIAN_POINT('Ctrl Pts',(84.2201467434616,-37.1036893778229,120.741521517745));
#49991=CARTESIAN_POINT('Ctrl Pts',(85.2017899213274,-33.7929771345978,120.583572994552));
#49992=CARTESIAN_POINT('Ctrl Pts',(88.5106434141715,-32.8051166986153,120.42562447136));
#49993=CARTESIAN_POINT('Ctrl Pts',(91.1466674974244,-35.0357552970371,120.267675948167));
#49994=CARTESIAN_POINT('Ctrl Pts',(90.7198607143381,-38.4624484297529,120.109727424975));
#49995=CARTESIAN_POINT('Ctrl Pts',(87.6171951095654,-39.9783139196497,119.951778901782));
#49996=CARTESIAN_POINT('Ctrl Pts',(84.6517635566205,-38.2089644444833,119.79383037859));
#49997=CARTESIAN_POINT('Ctrl Pts',(84.5122324931363,-34.7586144788259,119.635881855397));
#49998=CARTESIAN_POINT('Ctrl Pts',(87.3251105694465,-32.7555918278425,119.477933332205));
#49999=CARTESIAN_POINT('Ctrl Pts',(90.540046745306,-34.0159760014353,119.319984809013));
#50000=CARTESIAN_POINT('Ctrl Pts',(91.2421561865363,-37.3970151036668,119.16203628582));
#50001=CARTESIAN_POINT('Ctrl Pts',(88.7948576074191,-39.8332237608939,119.004087762628));
#50002=CARTESIAN_POINT('Ctrl Pts',(85.4170422028178,-39.115765701519,118.846139239435));
#50003=CARTESIAN_POINT('Ctrl Pts',(84.1712724663333,-35.8951383158207,118.688190716243));
#50004=CARTESIAN_POINT('Ctrl Pts',(86.1870499307028,-33.0913865091248,118.53024219305));
#50005=CARTESIAN_POINT('Ctrl Pts',(89.6367304755765,-33.2465867695503,118.372293669858));
#50006=CARTESIAN_POINT('Ctrl Pts',(91.3925936684549,-36.2200237425119,118.214345146665));
#50007=CARTESIAN_POINT('Ctrl Pts',(89.8626517544002,-39.3157725569713,118.056396623473));
#50008=CARTESIAN_POINT('Ctrl Pts',(86.4340565358644,-39.7270119161192,117.89844810028));
#50009=CARTESIAN_POINT('Ctrl Pts',(84.2154110214554,-37.0808836001418,117.740499577088));
#50010=CARTESIAN_POINT('Ctrl Pts',(85.2182936220487,-33.776551674856,117.582551053895));
#50011=CARTESIAN_POINT('Ctrl Pts',(88.5334211849751,-32.8099534001692,117.424602530703));
#50012=CARTESIAN_POINT('Ctrl Pts',(91.1550683739797,-35.0574740340002,117.26665400751));
#50013=CARTESIAN_POINT('Ctrl Pts',(90.7062674165854,-38.4813549728958,117.108705484318));
#50014=CARTESIAN_POINT('Ctrl Pts',(87.5939324911983,-39.9772675021952,116.950756961125));
#50015=CARTESIAN_POINT('Ctrl Pts',(84.6399230172785,-38.1889132277036,116.792808437933));
#50016=CARTESIAN_POINT('Ctrl Pts',(84.5225495426926,-34.7377385797668,116.63485991474));
#50017=CARTESIAN_POINT('Ctrl Pts',(87.3482310270943,-32.7528186489366,116.476911391548));
#50018=CARTESIAN_POINT('Ctrl Pts',(90.5550080077946,-34.0338199678859,116.318962868355));
#50019=CARTESIAN_POINT('Ctrl Pts',(91.2353933261053,-37.4192976006176,116.161014345163));
#50020=CARTESIAN_POINT('Ctrl Pts',(88.7725023068986,-39.8397419421814,116.003065821971));
#50021=CARTESIAN_POINT('Ctrl Pts',(85.3993633318442,-39.1006097225685,115.845117298778));
#50022=CARTESIAN_POINT('Ctrl Pts',(84.1742989202403,-35.8720496456117,115.687168775586));
#50023=CARTESIAN_POINT('Ctrl Pts',(86.2080377154374,-33.0812989408716,115.529220252393));
#50024=CARTESIAN_POINT('Ctrl Pts',(89.6566506052006,-33.2586463954901,115.371271729201));
#50025=CARTESIAN_POINT('Ctrl Pts',(91.3933851672007,-36.2432964661436,115.213323206008));
#50026=CARTESIAN_POINT('Ctrl Pts',(89.8435969944667,-39.3291577077992,115.055374682816));
#50027=CARTESIAN_POINT('Ctrl Pts',(86.4124318885398,-39.718373584875,114.897426159624));
#50028=CARTESIAN_POINT('Ctrl Pts',(84.2108228967943,-37.058053899092,114.739477636431));
#50029=CARTESIAN_POINT('Ctrl Pts',(85.2349019331354,-33.760229599584,114.581529113239));
#50030=CARTESIAN_POINT('Ctrl Pts',(88.5561676812683,-32.8149376799226,114.423580590046));
#50031=CARTESIAN_POINT('Ctrl Pts',(91.1633294990928,-35.0792455739108,114.265632066854));
#50032=CARTESIAN_POINT('Ctrl Pts',(90.6925530596296,-38.5001741798809,114.107683543661));
#50033=CARTESIAN_POINT('Ctrl Pts',(87.5706770425218,-39.9760715736404,113.949735020469));
#50034=CARTESIAN_POINT('Ctrl Pts',(84.6282114849141,-38.1687864756576,113.791786497276));
#50035=CARTESIAN_POINT('Ctrl Pts',(84.5330004168447,-34.716929318182,113.633837974084));
#50036=CARTESIAN_POINT('Ctrl Pts',(87.3713688180184,-32.7501940024069,113.475889450891));
#50037=CARTESIAN_POINT('Ctrl Pts',(90.5698543841637,-34.0517596235948,113.317940927699));
#50038=CARTESIAN_POINT('Ctrl Pts',(91.2284875299979,-37.4415362183437,113.159992404506));
#50039=CARTESIAN_POINT('Ctrl Pts',(88.7501056136147,-39.8461164435895,113.002043881314));
#50040=CARTESIAN_POINT('Ctrl Pts',(85.38178214202,-39.0853405411036,112.844095358121));
#50041=CARTESIAN_POINT('Ctrl Pts',(84.1774735639814,-35.8489808837167,112.686146834929));
#50042=CARTESIAN_POINT('Ctrl Pts',(86.2290898398163,-33.0713463433522,112.528198311736));
#50043=CARTESIAN_POINT('Ctrl Pts',(89.6764928893144,-33.2708336798222,112.370249788544));
#50044=CARTESIAN_POINT('Ctrl Pts',(91.3940272155189,-36.2665737922834,112.212301265351));
#50045=CARTESIAN_POINT('Ctrl Pts',(89.8244566813072,-39.3424202320825,112.054352742159));
#50046=CARTESIAN_POINT('Ctrl Pts',(86.3908631537158,-39.7095965798975,111.896404218966));
#50047=CARTESIAN_POINT('Ctrl Pts',(84.2063814561917,-37.0351952083222,111.738455695774));
#50048=CARTESIAN_POINT('Ctrl Pts',(85.2516147058595,-33.7440145027357,111.580507172582));
#50049=CARTESIAN_POINT('Ctrl Pts',(88.5788817046039,-32.8200679121307,111.422558649389));
#50050=CARTESIAN_POINT('Ctrl Pts',(91.1714506588609,-35.1010697096973,111.264610126197));
#50051=CARTESIAN_POINT('Ctrl Pts',(90.6787181473369,-38.5189049390048,111.106661603004));
#50052=CARTESIAN_POINT('Ctrl Pts',(87.5474297522212,-39.9747263466277,110.948713079812));
#50053=CARTESIAN_POINT('Ctrl Pts',(84.6166294280013,-38.1485849386119,110.790764556619));
#50054=CARTESIAN_POINT('Ctrl Pts',(84.5435846914231,-34.6961875909898,110.632816033427));
#50055=CARTESIAN_POINT('Ctrl Pts',(87.3945229855647,-32.747717976947,110.474867510234));
#50056=CARTESIAN_POINT('Ctrl Pts',(90.584585262429,-34.069794239593,110.316918987042));
#50057=CARTESIAN_POINT('Ctrl Pts',(91.221439085307,-37.4637300323244,110.158970463849));
#50058=CARTESIAN_POINT('Ctrl Pts',(88.7276684448237,-39.8523470110271,110.001021940657));
#50059=CARTESIAN_POINT('Ctrl Pts',(85.3642993714853,-39.0699587721052,109.843073417464));
#50060=CARTESIAN_POINT('Ctrl Pts',(84.1807962390639,-35.8259330095553,109.685124894272));
#50061=CARTESIAN_POINT('Ctrl Pts',(86.2502054927865,-33.0615290694994,109.527176371079));
#50062=CARTESIAN_POINT('Ctrl Pts',(89.6962563926914,-33.2831482377538,109.369227847887));
#50063=CARTESIAN_POINT('Ctrl Pts',(91.3945200278872,-36.2898545193635,109.211279324695));
#50064=CARTESIAN_POINT('Ctrl Pts',(89.805231108493,-39.3555600803365,109.053330801502));
#50065=CARTESIAN_POINT('Ctrl Pts',(86.3693522399246,-39.7006802402578,108.89538227831));
#50066=CARTESIAN_POINT('Ctrl Pts',(84.2020847864498,-37.0123105738625,108.737433755117));
#50067=CARTESIAN_POINT('Ctrl Pts',(85.2684355626542,-33.7279027264448,108.579485231925));
#50068=CARTESIAN_POINT('Ctrl Pts',(88.6015534510421,-32.8253527833924,108.421536708732));
#50069=CARTESIAN_POINT('Ctrl Pts',(91.1794497561267,-35.1229272408109,108.26358818554));
#50070=CARTESIAN_POINT('Ctrl Pts',(90.6647257407023,-38.5375841171318,108.105639662347));
#50071=CARTESIAN_POINT('Ctrl Pts',(87.5242687243508,-39.9731544640366,107.947691139155));
#50072=CARTESIAN_POINT('Ctrl Pts',(84.6050186580472,-38.1284686628391,107.789742615962));
#50073=CARTESIAN_POINT('Ctrl Pts',(84.5546282579559,-34.6751867381451,107.63179409277));
#50074=CARTESIAN_POINT('Ctrl Pts',(87.4170212023543,-32.7460640346786,107.473845569577));
#50075=CARTESIAN_POINT('Ctrl Pts',(90.6005809066571,-34.0865213418793,107.315897046385));
#50076=CARTESIAN_POINT('Ctrl Pts',(91.2113486315107,-37.4887066956559,107.157948523193));
#50077=CARTESIAN_POINT('Ctrl Pts',(89.5445934608762,-39.0615549760519,107.052649507731));
#50078=CARTESIAN_POINT('Ctrl Pts',(88.5623548711045,-39.3241490284294,107.));
#50079=CARTESIAN_POINT('Ctrl Pts',(89.6820215852375,-34.7189388713087,122.));
#50080=CARTESIAN_POINT('Ctrl Pts',(89.7436297646655,-34.7768354319368,122.));
#50081=CARTESIAN_POINT('Ctrl Pts',(89.8018687896484,-34.8378827535703,122.));
#50082=CARTESIAN_POINT('Ctrl Pts',(89.8567410473575,-34.9016960170172,122.));
#50083=CARTESIAN_POINT('Ctrl Pts',(89.9130662359688,-34.9671989551066,122.));
#50084=CARTESIAN_POINT('Ctrl Pts',(89.9658444403112,-35.0356166815112,122.));
#50085=CARTESIAN_POINT('Ctrl Pts',(90.0150527344221,-35.1065815431353,122.));
#50086=CARTESIAN_POINT('Ctrl Pts',(90.0656106252208,-35.1794927014953,122.));
#50087=CARTESIAN_POINT('Ctrl Pts',(90.1124006349142,-35.2550931839603,122.));
#50088=CARTESIAN_POINT('Ctrl Pts',(90.1553638311491,-35.3330272291937,122.));
#50089=CARTESIAN_POINT('Ctrl Pts',(90.1742738139209,-35.3673294129661,122.));
#50090=CARTESIAN_POINT('Ctrl Pts',(90.1924419568553,-35.4020841678299,122.));
#50091=CARTESIAN_POINT('Ctrl Pts',(90.2098608098524,-35.4372632361576,122.));
#50092=CARTESIAN_POINT('Ctrl Pts',(90.2197916550143,-35.4573195441454,122.));
#50093=CARTESIAN_POINT('Ctrl Pts',(90.2294789245804,-35.4775137906346,122.));
#50094=CARTESIAN_POINT('Ctrl Pts',(90.2389210036363,-35.4978408875546,122.));
#50095=CARTESIAN_POINT('Ctrl Pts',(90.2474265875847,-35.516151879049,122.));
#50096=CARTESIAN_POINT('Ctrl Pts',(90.2557355810474,-35.5345764026367,122.));
#50097=CARTESIAN_POINT('Ctrl Pts',(90.2638331430362,-35.5530789842928,122.));
#50098=CARTESIAN_POINT('Ctrl Pts',(90.3003947448764,-35.6366206755408,122.));
#50099=CARTESIAN_POINT('Ctrl Pts',(90.332696167958,-35.721845910373,122.));
#50100=CARTESIAN_POINT('Ctrl Pts',(90.3607123776603,-35.8083559104926,122.));
#50101=CARTESIAN_POINT('Ctrl Pts',(90.3891916851232,-35.8962958894621,122.));
#50102=CARTESIAN_POINT('Ctrl Pts',(90.4132434356667,-35.9855642131905,122.));
#50103=CARTESIAN_POINT('Ctrl Pts',(90.4328022575856,-36.0757791241328,122.));
#50104=CARTESIAN_POINT('Ctrl Pts',(90.4517707201329,-36.1632710071569,122.));
#50105=CARTESIAN_POINT('Ctrl Pts',(90.4665135445043,-36.2516541139452,122.));
#50106=CARTESIAN_POINT('Ctrl Pts',(90.4769303589594,-36.3406020879646,122.));
#50107=CARTESIAN_POINT('Ctrl Pts',(90.4812991889115,-36.3779070217092,122.));
#50108=CARTESIAN_POINT('Ctrl Pts',(90.4849065674636,-36.4153115064826,122.));
#50109=CARTESIAN_POINT('Ctrl Pts',(90.4877427551487,-36.45279208454,122.));
#50110=CARTESIAN_POINT('Ctrl Pts',(90.4895218789421,-36.4763034299149,122.));
#50111=CARTESIAN_POINT('Ctrl Pts',(90.4909975124888,-36.4998447233063,122.));
#50112=CARTESIAN_POINT('Ctrl Pts',(90.4921669557079,-36.5234102073052,122.));
#50113=CARTESIAN_POINT('Ctrl Pts',(90.4928513370157,-36.5372011947559,122.));
#50114=CARTESIAN_POINT('Ctrl Pts',(90.4934305636957,-36.550995520558,122.));
#50115=CARTESIAN_POINT('Ctrl Pts',(90.4939041349555,-36.5647841938125,122.));
#50116=CARTESIAN_POINT('Ctrl Pts',(90.4972315041031,-36.6616650855928,122.));
#50117=CARTESIAN_POINT('Ctrl Pts',(90.4953529603836,-36.7583809703611,122.));
#50118=CARTESIAN_POINT('Ctrl Pts',(90.4882041230073,-36.854512080775,122.));
#50119=CARTESIAN_POINT('Ctrl Pts',(90.481055285631,-36.9506431911888,122.));
#50120=CARTESIAN_POINT('Ctrl Pts',(90.4686365849094,-37.0461905712847,122.));
#50121=CARTESIAN_POINT('Ctrl Pts',(90.4508311771209,-37.1407532391955,122.));
#50122=CARTESIAN_POINT('Ctrl Pts',(90.4337731476271,-37.2313466587568,122.));
#50123=CARTESIAN_POINT('Ctrl Pts',(90.4117712643279,-37.3210372661022,122.));
#50124=CARTESIAN_POINT('Ctrl Pts',(90.3851001359725,-37.4095857222218,122.));
#50125=CARTESIAN_POINT('Ctrl Pts',(90.3762307867704,-37.4390320646551,122.));
#50126=CARTESIAN_POINT('Ctrl Pts',(90.3668446531488,-37.4683520650043,122.));
#50127=CARTESIAN_POINT('Ctrl Pts',(90.3569505851863,-37.4975367471472,122.));
#50128=CARTESIAN_POINT('Ctrl Pts',(90.3476302477942,-37.5250290875361,122.));
#50129=CARTESIAN_POINT('Ctrl Pts',(90.3378591694355,-37.5524013492222,122.));
#50130=CARTESIAN_POINT('Ctrl Pts',(90.327644273459,-37.5796459038865,122.));
#50131=CARTESIAN_POINT('Ctrl Pts',(90.32248652871,-37.5934023297063,122.));
#50132=CARTESIAN_POINT('Ctrl Pts',(90.3172187072603,-37.6071179222931,122.));
#50133=CARTESIAN_POINT('Ctrl Pts',(90.3118434787871,-37.6207883639188,122.));
#50134=CARTESIAN_POINT('Ctrl Pts',(90.2775921562166,-37.7078973506603,122.));
#50135=CARTESIAN_POINT('Ctrl Pts',(90.2389673349269,-37.7932175192191,122.));
#50136=CARTESIAN_POINT('Ctrl Pts',(90.1962990002629,-37.8765144552663,122.));
#50137=CARTESIAN_POINT('Ctrl Pts',(90.1520692008913,-37.9628596758764,122.));
#50138=CARTESIAN_POINT('Ctrl Pts',(90.1034943952308,-38.0470316029905,122.));
#50139=CARTESIAN_POINT('Ctrl Pts',(90.0508862935642,-38.1287656580968,122.));
#50140=CARTESIAN_POINT('Ctrl Pts',(89.9977152427445,-38.2113743335685,122.));
#50141=CARTESIAN_POINT('Ctrl Pts',(89.9404236999765,-38.2914935051329,122.));
#50142=CARTESIAN_POINT('Ctrl Pts',(89.8792819816606,-38.3688346448537,122.));
#50143=CARTESIAN_POINT('Ctrl Pts',(89.8565930994489,-38.3975349178845,122.));
#50144=CARTESIAN_POINT('Ctrl Pts',(89.8333735538416,-38.4258524269221,122.));
#50145=CARTESIAN_POINT('Ctrl Pts',(89.8096355637098,-38.4537715398041,122.));
#50146=CARTESIAN_POINT('Ctrl Pts',(89.7888801267933,-38.4781827634574,122.));
#50147=CARTESIAN_POINT('Ctrl Pts',(89.7677283264474,-38.502289408991,122.));
#50148=CARTESIAN_POINT('Ctrl Pts',(89.7461878405604,-38.5260806443712,122.));
#50149=CARTESIAN_POINT('Ctrl Pts',(89.7344246098016,-38.5390730064415,122.));
#50150=CARTESIAN_POINT('Ctrl Pts',(89.7225501398425,-38.5519660547785,122.));
#50151=CARTESIAN_POINT('Ctrl Pts',(89.7105717549045,-38.5647521680861,122.));
#50152=CARTESIAN_POINT('Ctrl Pts',(89.6415609858971,-38.638416482311,122.));
#50153=CARTESIAN_POINT('Ctrl Pts',(89.5690478192282,-38.7085962647208,122.));
#50154=CARTESIAN_POINT('Ctrl Pts',(89.4933407755827,-38.7750003014946,122.));
#50155=CARTESIAN_POINT('Ctrl Pts',(89.4311466614727,-38.8295518998876,122.));
#50156=CARTESIAN_POINT('Ctrl Pts',(89.3667959749386,-38.8815552652603,122.));
#50157=CARTESIAN_POINT('Ctrl Pts',(89.300437483061,-38.9308356080291,122.));
#50158=CARTESIAN_POINT('Ctrl Pts',(89.2758198860226,-38.9491175729423,122.));
#50159=CARTESIAN_POINT('Ctrl Pts',(89.2509257832841,-38.9670246354587,122.));
#50160=CARTESIAN_POINT('Ctrl Pts',(89.2257621633589,-38.9845473066697,122.));
#50161=CARTESIAN_POINT('Ctrl Pts',(89.2089513436832,-38.9962535105799,122.));
#50162=CARTESIAN_POINT('Ctrl Pts',(89.1920191005935,-39.0077887888468,122.));
#50163=CARTESIAN_POINT('Ctrl Pts',(89.1749825783546,-39.0191404890314,122.));
#50164=CARTESIAN_POINT('Ctrl Pts',(89.0900721174774,-39.0757176519581,122.));
#50165=CARTESIAN_POINT('Ctrl Pts',(89.0024923773335,-39.127795516944,122.));
#50166=CARTESIAN_POINT('Ctrl Pts',(88.9125337151644,-39.1750661685274,122.));
#50167=CARTESIAN_POINT('Ctrl Pts',(88.8290756762026,-39.2189209323319,122.));
#50168=CARTESIAN_POINT('Ctrl Pts',(88.7435692936185,-39.2586384125487,122.));
#50169=CARTESIAN_POINT('Ctrl Pts',(88.6562187078536,-39.2939436847022,122.));
#50170=CARTESIAN_POINT('Ctrl Pts',(88.6257885343039,-39.3062429217301,122.));
#50171=CARTESIAN_POINT('Ctrl Pts',(88.5951343400001,-39.3180064003196,122.));
#50172=CARTESIAN_POINT('Ctrl Pts',(88.5642690312354,-39.3292378429292,122.));
#50173=CARTESIAN_POINT('Ctrl Pts',(85.2503884478834,-36.3571243043025,120.387416697508));
#50174=CARTESIAN_POINT('Ctrl Pts',(85.2488060880821,-36.5314907329699,120.398449387697));
#50175=CARTESIAN_POINT('Ctrl Pts',(85.2653916827167,-36.7055581163151,120.409482077886));
#50176=CARTESIAN_POINT('Ctrl Pts',(85.3012632429209,-36.8755557583819,120.420514768075));
#50177=CARTESIAN_POINT('Ctrl Pts',(85.4724472382946,-37.6868077755068,120.473164275806));
#50178=CARTESIAN_POINT('Ctrl Pts',(86.0828361281554,-38.4053783926622,120.525813783537));
#50179=CARTESIAN_POINT('Ctrl Pts',(86.8557210641803,-38.7055236634528,120.578463291268));
#50180=CARTESIAN_POINT('Ctrl Pts',(87.6286060002051,-39.0056689342435,120.631112798999));
#50181=CARTESIAN_POINT('Ctrl Pts',(88.5639869823939,-38.8873888586693,120.683762306729));
#50182=CARTESIAN_POINT('Ctrl Pts',(89.2378198261349,-38.4042851620282,120.73641181446));
#50183=CARTESIAN_POINT('Ctrl Pts',(89.911652669876,-37.9211814653871,120.789061322191));
#50184=CARTESIAN_POINT('Ctrl Pts',(90.3239373751694,-37.073254147679,120.841710829922));
#50185=CARTESIAN_POINT('Ctrl Pts',(90.2877780164629,-36.2449367237544,120.894360337653));
#50186=CARTESIAN_POINT('Ctrl Pts',(90.2516186577565,-35.4166192998297,120.947009845384));
#50187=CARTESIAN_POINT('Ctrl Pts',(89.7670152350502,-34.6079117696885,120.999659353114));
#50188=CARTESIAN_POINT('Ctrl Pts',(89.0536407873046,-34.1853500886824,121.052308860845));
#50189=CARTESIAN_POINT('Ctrl Pts',(88.340266339559,-33.7627884076762,121.104958368576));
#50190=CARTESIAN_POINT('Ctrl Pts',(87.398120866774,-33.726372575805,121.157607876307));
#50191=CARTESIAN_POINT('Ctrl Pts',(86.6543416196145,-34.092774271182,121.210257384038));
#50192=CARTESIAN_POINT('Ctrl Pts',(85.9105623724549,-34.4591759665591,121.262906891768));
#50193=CARTESIAN_POINT('Ctrl Pts',(85.3651493509208,-35.2283951891843,121.315556399499));
#50194=CARTESIAN_POINT('Ctrl Pts',(85.2652956692094,-36.0513826205722,121.36820590723));
#50195=CARTESIAN_POINT('Ctrl Pts',(85.2531507747902,-36.1514800360225,121.374609503989));
#50196=CARTESIAN_POINT('Ctrl Pts',(85.2475970862054,-36.2523728501989,121.381013100749));
#50197=CARTESIAN_POINT('Ctrl Pts',(85.2483528516199,-36.3533471753035,121.387416697508));
#50198=CARTESIAN_POINT('Ctrl Pts',(86.9747563060389,-39.3241490284291,122.));
#50199=CARTESIAN_POINT('Ctrl Pts',(85.9925177162673,-39.0615549760513,121.947350492269));
#50200=CARTESIAN_POINT('Ctrl Pts',(84.3257618514341,-37.4887114986967,121.842051476808));
#50201=CARTESIAN_POINT('Ctrl Pts',(84.9365308695941,-34.0865200954889,121.684102953615));
#50202=CARTESIAN_POINT('Ctrl Pts',(88.1200899288066,-32.7460654788916,121.526154430423));
#50203=CARTESIAN_POINT('Ctrl Pts',(90.9824824119093,-34.6751864614649,121.36820590723));
#50204=CARTESIAN_POINT('Ctrl Pts',(90.9320921383769,-38.128468693812,121.210257384038));
#50205=CARTESIAN_POINT('Ctrl Pts',(88.0128423765734,-39.9731538131696,121.052308860845));
#50206=CARTESIAN_POINT('Ctrl Pts',(84.8723858657462,-38.5375838933282,120.894360337653));
#50207=CARTESIAN_POINT('Ctrl Pts',(84.3576618778048,-35.1229273700108,120.73641181446));
#50208=CARTESIAN_POINT('Ctrl Pts',(86.935557851387,-32.8253532951761,120.578463291268));
#50209=CARTESIAN_POINT('Ctrl Pts',(90.2686752620247,-33.7279030795955,120.420514768075));
#50210=CARTESIAN_POINT('Ctrl Pts',(91.3350258987628,-37.0123104885738,120.262566244883));
#50211=CARTESIAN_POINT('Ctrl Pts',(89.167758741363,-39.7006797728369,120.10461772169));
#50212=CARTESIAN_POINT('Ctrl Pts',(85.7318803522126,-39.3555596654746,119.946669198498));
#50213=CARTESIAN_POINT('Ctrl Pts',(84.1425916520107,-36.2898545275783,119.788720675305));
#50214=CARTESIAN_POINT('Ctrl Pts',(85.8408550522478,-33.2831486644916,119.630772152113));
#50215=CARTESIAN_POINT('Ctrl Pts',(89.2869054734986,-33.0615295263651,119.472823628921));
#50216=CARTESIAN_POINT('Ctrl Pts',(91.3563144402191,-35.8259330830824,119.314875105728));
#50217=CARTESIAN_POINT('Ctrl Pts',(90.1728114719436,-39.0699583952412,119.156926582536));
#50218=CARTESIAN_POINT('Ctrl Pts',(86.8094428654503,-39.8523465256606,118.998978059343));
#50219=CARTESIAN_POINT('Ctrl Pts',(84.3156725710403,-37.4637298784219,118.841029536151));
#50220=CARTESIAN_POINT('Ctrl Pts',(84.9525263055479,-34.0697945567443,118.683081012958));
#50221=CARTESIAN_POINT('Ctrl Pts',(88.1425881396678,-32.7477184775748,118.525132489766));
#50222=CARTESIAN_POINT('Ctrl Pts',(90.9935260381413,-34.6961878212031,118.367183966573));
#50223=CARTESIAN_POINT('Ctrl Pts',(90.9204813116975,-38.1485846896768,118.209235443381));
#50224=CARTESIAN_POINT('Ctrl Pts',(87.9896813942331,-39.9747258442494,118.051286920188));
#50225=CARTESIAN_POINT('Ctrl Pts',(84.8583934336975,-38.5189046386728,117.893338396996));
#50226=CARTESIAN_POINT('Ctrl Pts',(84.3656609905594,-35.1010698837144,117.735389873803));
#50227=CARTESIAN_POINT('Ctrl Pts',(86.9582295850041,-32.8200684027204,117.577441350611));
#50228=CARTESIAN_POINT('Ctrl Pts',(90.2854961219689,-33.7440148650956,117.419492827418));
#50229=CARTESIAN_POINT('Ctrl Pts',(91.3307292265714,-37.0351951139114,117.261544304226));
#50230=CARTESIAN_POINT('Ctrl Pts',(89.1462478322224,-39.7095961143156,117.103595781033));
#50231=CARTESIAN_POINT('Ctrl Pts',(85.7126547811673,-39.3424198174583,116.945647257841));
#50232=CARTESIAN_POINT('Ctrl Pts',(84.1430844647916,-36.2665738045441,116.787698734649));
#50233=CARTESIAN_POINT('Ctrl Pts',(85.860618552627,-33.2708341078515,116.629750211456));
#50234=CARTESIAN_POINT('Ctrl Pts',(89.3080211236725,-33.0713467990688,116.471801688264));
#50235=CARTESIAN_POINT('Ctrl Pts',(91.3596371147702,-35.8489809539364,116.313853165071));
#50236=CARTESIAN_POINT('Ctrl Pts',(90.1553287038718,-39.0853401621602,116.155904641879));
#50237=CARTESIAN_POINT('Ctrl Pts',(86.7870056997543,-39.8461159590596,115.997956118686));
#50238=CARTESIAN_POINT('Ctrl Pts',(84.3086241273375,-37.4415360675358,115.840007595494));
#50239=CARTESIAN_POINT('Ctrl Pts',(84.9672571817637,-34.0517599432419,115.682059072301));
#50240=CARTESIAN_POINT('Ctrl Pts',(88.1657423040033,-32.7501945026947,115.524110549109));
#50241=CARTESIAN_POINT('Ctrl Pts',(91.0041103112496,-34.7169295455148,115.366162025916));
#50242=CARTESIAN_POINT('Ctrl Pts',(90.9088992563929,-38.1687862239197,115.208213502724));
#50243=CARTESIAN_POINT('Ctrl Pts',(87.9664341071585,-39.9760710710749,115.050264979531));
#50244=CARTESIAN_POINT('Ctrl Pts',(84.8445585233251,-38.5001738821487,114.892316456339));
#50245=CARTESIAN_POINT('Ctrl Pts',(84.3737821492005,-35.0792457509566,114.734367933146));
#50246=CARTESIAN_POINT('Ctrl Pts',(86.9809436051873,-32.8149381712244,114.576419409954));
#50247=CARTESIAN_POINT('Ctrl Pts',(90.3022088923736,-33.7602299596934,114.418470886762));
#50248=CARTESIAN_POINT('Ctrl Pts',(91.3262877865851,-37.0580538015087,114.260522363569));
#50249=CARTESIAN_POINT('Ctrl Pts',(89.124679100392,-39.7183731180749,114.102573840377));
#50250=CARTESIAN_POINT('Ctrl Pts',(85.6935144706641,-39.3291572950157,113.944625317184));
#50251=CARTESIAN_POINT('Ctrl Pts',(84.1437265130207,-36.2432964816349,113.786676793992));
#50252=CARTESIAN_POINT('Ctrl Pts',(85.8804608339871,-33.2586468252107,113.628728270799));
#50253=CARTESIAN_POINT('Ctrl Pts',(89.3290732451296,-33.0812993952069,113.470779747607));
#50254=CARTESIAN_POINT('Ctrl Pts',(91.3628117580707,-35.8720497126298,113.312831224414));
#50255=CARTESIAN_POINT('Ctrl Pts',(90.1377475164876,-39.100609341506,113.154882701222));
#50256=CARTESIAN_POINT('Ctrl Pts',(86.7646090095788,-39.8397414585361,112.996934178029));
#50257=CARTESIAN_POINT('Ctrl Pts',(84.3017183321886,-37.419297452896,112.838985654837));
#50258=CARTESIAN_POINT('Ctrl Pts',(84.9821035560724,-34.0338202900228,112.681037131644));
#50259=CARTESIAN_POINT('Ctrl Pts',(88.1888800917162,-32.7528191488601,112.523088608452));
#50260=CARTESIAN_POINT('Ctrl Pts',(91.0145611839512,-34.7377388042116,112.365140085259));
#50261=CARTESIAN_POINT('Ctrl Pts',(90.8971877256538,-38.1889129731724,112.207191562067));
#50262=CARTESIAN_POINT('Ctrl Pts',(87.9431786617096,-39.9772669994637,112.049243038874));
#50263=CARTESIAN_POINT('Ctrl Pts',(84.8308441682727,-38.4813546777754,111.891294515682));
#50264=CARTESIAN_POINT('Ctrl Pts',(84.382043273167,-35.0574742140675,111.733345992489));
#50265=CARTESIAN_POINT('Ctrl Pts',(87.0036900983236,-32.8099538921628,111.575397469297));
#50266=CARTESIAN_POINT('Ctrl Pts',(90.3188172011552,-33.7765520327001,111.417448946105));
#50267=CARTESIAN_POINT('Ctrl Pts',(91.3216996625609,-37.0808834993901,111.259500422912));
#50268=CARTESIAN_POINT('Ctrl Pts',(89.1030544560686,-39.7270114481203,111.10155189972));
#50269=CARTESIAN_POINT('Ctrl Pts',(85.6744597133751,-39.3157721460453,110.943603376527));
#50270=CARTESIAN_POINT('Ctrl Pts',(84.1445180116567,-36.2200237612334,110.785654853335));
#50271=CARTESIAN_POINT('Ctrl Pts',(85.9003809608462,-33.2465872009442,110.627706330142));
#50272=CARTESIAN_POINT('Ctrl Pts',(89.3500610269517,-33.0913869620613,110.46975780695));
#50273=CARTESIAN_POINT('Ctrl Pts',(91.3658382115574,-35.895138379632,110.311809283757));
#50274=CARTESIAN_POINT('Ctrl Pts',(90.1200686479678,-39.1157653183575,110.153860760565));
#50275=CARTESIAN_POINT('Ctrl Pts',(86.7422537121608,-39.8332232781445,109.995912237372));
#50276=CARTESIAN_POINT('Ctrl Pts',(84.2949554726962,-37.397014959055,109.83796371418));
#50277=CARTESIAN_POINT('Ctrl Pts',(84.9970648164843,-34.0159763260146,109.680015190987));
#50278=CARTESIAN_POINT('Ctrl Pts',(88.2120005461565,-32.7555923274475,109.522066667795));
#50279=CARTESIAN_POINT('Ctrl Pts',(91.0248782320717,-34.7586147002439,109.364118144602));
#50280=CARTESIAN_POINT('Ctrl Pts',(90.8853471879654,-38.2089641874212,109.20616962141));
#50281=CARTESIAN_POINT('Ctrl Pts',(87.9199160465446,-39.9783134162844,109.048221098218));
#50282=CARTESIAN_POINT('Ctrl Pts',(84.8172508724717,-38.4624481382004,108.890272575025));
#50283=CARTESIAN_POINT('Ctrl Pts',(84.3904441483993,-35.0357554783023,108.732324051833));
#50284=CARTESIAN_POINT('Ctrl Pts',(87.0264678663363,-32.8051171947587,108.57437552864));
#50285=CARTESIAN_POINT('Ctrl Pts',(90.3353208987278,-33.792977483537,108.416427005448));
#50286=CARTESIAN_POINT('Ctrl Pts',(91.3169639431757,-37.1036892864445,108.258478482255));
#50287=CARTESIAN_POINT('Ctrl Pts',(89.0813770537997,-39.7354983689013,108.100529959063));
#50288=CARTESIAN_POINT('Ctrl Pts',(85.6554866415101,-39.302290378503,107.94258143587));
#50289=CARTESIAN_POINT('Ctrl Pts',(84.1454684970089,-36.1967042568066,107.784632912678));
#50290=CARTESIAN_POINT('Ctrl Pts',(85.9203584351496,-33.2347633730889,107.626684389485));
#50291=CARTESIAN_POINT('Ctrl Pts',(89.3710240668315,-33.1013877392709,107.468735866293));
#50292=CARTESIAN_POINT('Ctrl Pts',(91.3686331795228,-35.9187012093704,107.3107873431));
#50293=CARTESIAN_POINT('Ctrl Pts',(90.1024641556487,-39.1298714782457,107.152838819908));
#50294=CARTESIAN_POINT('Ctrl Pts',(86.7195978028781,-39.8285002079331,106.994890296716));
#50295=CARTESIAN_POINT('Ctrl Pts',(84.2891194416926,-37.3707125699518,106.836941773523));
#50296=CARTESIAN_POINT('Ctrl Pts',(84.7717723668806,-35.1304094942453,106.731642758061));
#50297=CARTESIAN_POINT('Ctrl Pts',(85.4324929308767,-34.3576245177522,106.678993250331));
#50298=CARTESIAN_POINT('Ctrl Pts',(87.0226227342249,-39.1451036445255,122.10700224989));
#50299=CARTESIAN_POINT('Ctrl Pts',(86.0996135415481,-38.8983441231517,122.054352742159));
#50300=CARTESIAN_POINT('Ctrl Pts',(84.5333637513147,-37.4203437642191,121.949053726697));
#50301=CARTESIAN_POINT('Ctrl Pts',(85.1073031426544,-34.2233059232024,121.791105203505));
#50302=CARTESIAN_POINT('Ctrl Pts',(88.0988922613081,-32.9636812796899,121.633156680312));
#50303=CARTESIAN_POINT('Ctrl Pts',(90.7886812824939,-34.7764754615136,121.47520815712));
#50304=CARTESIAN_POINT('Ctrl Pts',(90.7413295634957,-38.0215233333396,121.317259633928));
#50305=CARTESIAN_POINT('Ctrl Pts',(87.9981117812556,-39.7549731697557,121.159311110735));
#50306=CARTESIAN_POINT('Ctrl Pts',(85.047026109322,-38.4059687154998,121.001362587542));
#50307=CARTESIAN_POINT('Ctrl Pts',(84.5633401927755,-35.197217406321,120.84341406435));
#50308=CARTESIAN_POINT('Ctrl Pts',(86.9857879627557,-33.038188007546,120.685465541157));
#50309=CARTESIAN_POINT('Ctrl Pts',(90.1179170017959,-33.8863136631071,120.527517017965));
#50310=CARTESIAN_POINT('Ctrl Pts',(91.1199662498861,-36.9726699339268,120.369568494773));
#50311=CARTESIAN_POINT('Ctrl Pts',(89.0833862070155,-39.498929427826,120.21161997158));
#50312=CARTESIAN_POINT('Ctrl Pts',(85.8546927193744,-39.1746202070418,120.053671448388));
#50313=CARTESIAN_POINT('Ctrl Pts',(84.361238791399,-36.2937783690392,119.895722925195));
#50314=CARTESIAN_POINT('Ctrl Pts',(85.9570961994953,-33.4683781249403,119.737774402003));
#50315=CARTESIAN_POINT('Ctrl Pts',(89.1953483414539,-33.2601227133794,119.57982587881));
#50316=CARTESIAN_POINT('Ctrl Pts',(91.1399710834037,-35.8578315813559,119.421877355618));
#50317=CARTESIAN_POINT('Ctrl Pts',(90.0278338382846,-38.9062408126556,119.263928832425));
#50318=CARTESIAN_POINT('Ctrl Pts',(86.8672777631298,-39.6414506121262,119.105980309233));
#50319=CARTESIAN_POINT('Ctrl Pts',(84.5238828587414,-37.3968685460779,118.94803178604));
#50320=CARTESIAN_POINT('Ctrl Pts',(85.1223340471412,-34.2075889414278,118.790083262848));
#50321=CARTESIAN_POINT('Ctrl Pts',(88.1200338206604,-32.9652346018622,118.632134739655));
#50322=CARTESIAN_POINT('Ctrl Pts',(90.7990589734528,-34.7962104304906,118.474186216463));
#50323=CARTESIAN_POINT('Ctrl Pts',(90.7304188745133,-38.0404263262544,118.316237693271));
#50324=CARTESIAN_POINT('Ctrl Pts',(87.976347415821,-39.756450406705,118.158289170078));
#50325=CARTESIAN_POINT('Ctrl Pts',(85.0338774267685,-38.3884158276996,118.000340646886));
#50326=CARTESIAN_POINT('Ctrl Pts',(84.5708569556909,-35.1766779355748,117.842392123693));
#50327=CARTESIAN_POINT('Ctrl Pts',(87.0070925813691,-33.033221796312,117.684443600501));
#50328=CARTESIAN_POINT('Ctrl Pts',(90.133723556862,-33.9014539012141,117.526495077308));
#50329=CARTESIAN_POINT('Ctrl Pts',(91.115928668822,-36.9941746068011,117.368546554116));
#50330=CARTESIAN_POINT('Ctrl Pts',(89.0631724146781,-39.5073081101905,117.210598030923));
#50331=CARTESIAN_POINT('Ctrl Pts',(85.8366264582907,-39.1622726973474,117.052649507731));
#50332=CARTESIAN_POINT('Ctrl Pts',(84.3617018873633,-36.2719014833249,116.894700984538));
#50333=CARTESIAN_POINT('Ctrl Pts',(85.9756679525495,-33.4568061412075,116.736752461346));
#50334=CARTESIAN_POINT('Ctrl Pts',(89.2151907091054,-33.2693480004399,116.578803938154));
#50335=CARTESIAN_POINT('Ctrl Pts',(91.1430933992921,-35.8794896559737,116.420855414961));
#50336=CARTESIAN_POINT('Ctrl Pts',(90.0114052884273,-38.9206950526068,116.262906891769));
#50337=CARTESIAN_POINT('Ctrl Pts',(86.846193567894,-39.6355957512928,116.104958368576));
#50338=CARTESIAN_POINT('Ctrl Pts',(84.5172594391369,-37.3760130312551,115.947009845384));
#50339=CARTESIAN_POINT('Ctrl Pts',(85.1361766453704,-34.1906418226499,115.789061322191));
#50340=CARTESIAN_POINT('Ctrl Pts',(88.1417917792184,-32.9675613216336,115.631112798999));
#50341=CARTESIAN_POINT('Ctrl Pts',(90.8090050104732,-34.8157014201656,115.473164275806));
#50342=CARTESIAN_POINT('Ctrl Pts',(90.7195352219795,-38.0594096995474,115.315215752614));
#50343=CARTESIAN_POINT('Ctrl Pts',(87.954501949864,-39.7577145157911,115.157267229421));
#50344=CARTESIAN_POINT('Ctrl Pts',(85.0208767672683,-38.370814543615,114.999318706229));
#50345=CARTESIAN_POINT('Ctrl Pts',(84.5784884050749,-35.1561698071348,114.841370183036));
#50346=CARTESIAN_POINT('Ctrl Pts',(87.0284369366511,-33.0284009199174,114.683421659844));
#50347=CARTESIAN_POINT('Ctrl Pts',(90.1494285402328,-33.9166912188371,114.525473136651));
#50348=CARTESIAN_POINT('Ctrl Pts',(91.1117550495216,-37.0156549059918,114.367524613459));
#50349=CARTESIAN_POINT('Ctrl Pts',(89.0429042863828,-39.5155558569582,114.209576090266));
#50350=CARTESIAN_POINT('Ctrl Pts',(85.818640316503,-39.1498099105458,114.051627567074));
#50351=CARTESIAN_POINT('Ctrl Pts',(84.3623052198161,-36.2500277927064,113.893679043881));
#50352=CARTESIAN_POINT('Ctrl Pts',(85.9943137360584,-33.4453537567987,113.735730520689));
#50353=CARTESIAN_POINT('Ctrl Pts',(89.2349733788484,-33.2787004508751,113.577781997497));
#50354=CARTESIAN_POINT('Ctrl Pts',(91.146076610276,-35.9011673588856,113.419833474304));
#50355=CARTESIAN_POINT('Ctrl Pts',(89.9948842539832,-38.9350434940625,113.261884951112));
#50356=CARTESIAN_POINT('Ctrl Pts',(86.8251474074879,-39.6296056358126,113.103936427919));
#50357=CARTESIAN_POINT('Ctrl Pts',(84.5107700663189,-37.3551154143638,112.945987904727));
#50358=CARTESIAN_POINT('Ctrl Pts',(85.1501277771093,-34.1737839380106,112.788039381534));
#50359=CARTESIAN_POINT('Ctrl Pts',(88.163534348671,-32.9700277005393,112.630090858342));
#50360=CARTESIAN_POINT('Ctrl Pts',(90.8188256911872,-34.8352558718741,112.472142335149));
#50361=CARTESIAN_POINT('Ctrl Pts',(90.7085299014341,-38.0783227974162,112.314193811957));
#50362=CARTESIAN_POINT('Ctrl Pts',(87.9326488174859,-39.7588383291988,112.156245288764));
#50363=CARTESIAN_POINT('Ctrl Pts',(85.0079893935519,-38.3531301451233,111.998296765572));
#50364=CARTESIAN_POINT('Ctrl Pts',(84.5862513798169,-35.1357111030109,111.840348242379));
#50365=CARTESIAN_POINT('Ctrl Pts',(87.0498118067535,-33.0237171949643,111.682399719187));
#50366=CARTESIAN_POINT('Ctrl Pts',(90.1650353610602,-33.9320290640263,111.524451195994));
#50367=CARTESIAN_POINT('Ctrl Pts',(91.1074435912917,-37.0371079635583,111.366502672802));
#50368=CARTESIAN_POINT('Ctrl Pts',(89.0225836171414,-39.523673292095,111.208554149609));
#50369=CARTESIAN_POINT('Ctrl Pts',(85.8007345690348,-39.1372318916473,111.050605626417));
#50370=CARTESIAN_POINT('Ctrl Pts',(84.3630489907538,-36.2281584270626,110.892657103224));
#50371=CARTESIAN_POINT('Ctrl Pts',(86.0130326709505,-33.4340213329109,110.734708580032));
#50372=CARTESIAN_POINT('Ctrl Pts',(89.2546955886631,-33.2881797332362,110.57676005684));
#50373=CARTESIAN_POINT('Ctrl Pts',(91.1489205673539,-35.922863769627,110.418811533647));
#50374=CARTESIAN_POINT('Ctrl Pts',(89.978271428617,-38.9492855591815,110.260863010455));
#50375=CARTESIAN_POINT('Ctrl Pts',(86.8041401438386,-39.6234805044202,110.102914487262));
#50376=CARTESIAN_POINT('Ctrl Pts',(84.5044150100778,-37.3341765642054,109.94496596407));
#50377=CARTESIAN_POINT('Ctrl Pts',(85.1641868672712,-34.1570159724828,109.787017440877));
#50378=CARTESIAN_POINT('Ctrl Pts',(88.1852606300547,-32.9726336552999,109.629068917685));
#50379=CARTESIAN_POINT('Ctrl Pts',(90.8285206169981,-34.854872942659,109.471120394492));
#50380=CARTESIAN_POINT('Ctrl Pts',(90.6974033531124,-38.0971649150734,109.3131718713));
#50381=CARTESIAN_POINT('Ctrl Pts',(87.9107889477286,-39.7598216466482,109.155223348107));
#50382=CARTESIAN_POINT('Ctrl Pts',(84.9952157791636,-38.335363677779,108.997274824915));
#50383=CARTESIAN_POINT('Ctrl Pts',(84.5941456787648,-35.1153020160809,108.839326301722));
#50384=CARTESIAN_POINT('Ctrl Pts',(87.0712160658443,-33.0191721524332,108.68137777853));
#50385=CARTESIAN_POINT('Ctrl Pts',(90.180543878778,-33.9474640533193,108.523429255338));
#50386=CARTESIAN_POINT('Ctrl Pts',(91.1029934377628,-37.0585385521308,108.365480732145));
#50387=CARTESIAN_POINT('Ctrl Pts',(89.0022133712807,-39.5316484480093,108.207532208953));
#50388=CARTESIAN_POINT('Ctrl Pts',(85.7829055813253,-39.124563080317,108.04958368576));
#50389=CARTESIAN_POINT('Ctrl Pts',(84.3639421614424,-36.2062450984898,107.891635162568));
#50390=CARTESIAN_POINT('Ctrl Pts',(86.0318054952116,-33.4229104868122,107.733686639375));
#50391=CARTESIAN_POINT('Ctrl Pts',(89.2743945484854,-33.2975774594042,107.575738116183));
#50392=CARTESIAN_POINT('Ctrl Pts',(91.1515469975838,-35.9450057508935,107.41778959299));
#50393=CARTESIAN_POINT('Ctrl Pts',(89.9617284945354,-38.9625411117384,107.259841069798));
#50394=CARTESIAN_POINT('Ctrl Pts',(86.7828503953456,-39.6190422373148,107.101892546605));
#50395=CARTESIAN_POINT('Ctrl Pts',(84.4989308941805,-37.3094602201476,106.943944023413));
#50396=CARTESIAN_POINT('Ctrl Pts',(84.952479646449,-35.2042483553399,106.838645007951));
#50397=CARTESIAN_POINT('Ctrl Pts',(85.5733584845537,-34.4780626356041,106.78599550022));
#50398=CARTESIAN_POINT('Ctrl Pts',(87.0704891624108,-38.966058260622,122.21400449978));
#50399=CARTESIAN_POINT('Ctrl Pts',(86.2067093668289,-38.7351332702521,122.161354992049));
#50400=CARTESIAN_POINT('Ctrl Pts',(84.7409656511953,-37.3519760297414,122.056055976587));
#50401=CARTESIAN_POINT('Ctrl Pts',(85.2780754157145,-34.3600917509159,121.898107453395));
#50402=CARTESIAN_POINT('Ctrl Pts',(88.0776945938096,-33.1812970804881,121.740158930202));
#50403=CARTESIAN_POINT('Ctrl Pts',(90.5948801530784,-34.8777644615624,121.58221040701));
#50404=CARTESIAN_POINT('Ctrl Pts',(90.5505669886146,-37.9145779728672,121.424261883817));
#50405=CARTESIAN_POINT('Ctrl Pts',(87.9833811859376,-39.5367925263418,121.266313360625));
#50406=CARTESIAN_POINT('Ctrl Pts',(85.2216663528979,-38.2743535376715,121.108364837432));
#50407=CARTESIAN_POINT('Ctrl Pts',(84.7690185077461,-35.2715074426312,120.95041631424));
#50408=CARTESIAN_POINT('Ctrl Pts',(87.0360180741243,-33.2510227199158,120.792467791047));
#50409=CARTESIAN_POINT('Ctrl Pts',(89.9671587415673,-34.0447242466188,120.634519267855));
#50410=CARTESIAN_POINT('Ctrl Pts',(90.9049066010096,-36.9330293792797,120.476570744662));
#50411=CARTESIAN_POINT('Ctrl Pts',(88.999013672668,-39.2971790828151,120.31862222147));
#50412=CARTESIAN_POINT('Ctrl Pts',(85.9775050865362,-38.9936807486089,120.160673698277));
#50413=CARTESIAN_POINT('Ctrl Pts',(84.579885930787,-36.2977022105001,120.002725175085));
#50414=CARTESIAN_POINT('Ctrl Pts',(86.0733373467429,-33.6536075853888,119.844776651893));
#50415=CARTESIAN_POINT('Ctrl Pts',(89.1037912094091,-33.4587159003937,119.6868281287));
#50416=CARTESIAN_POINT('Ctrl Pts',(90.9236277265884,-35.8897300796293,119.528879605508));
#50417=CARTESIAN_POINT('Ctrl Pts',(89.8828562046253,-38.7425232300701,119.370931082315));
#50418=CARTESIAN_POINT('Ctrl Pts',(86.9251126608097,-39.4305546985919,119.212982559123));
#50419=CARTESIAN_POINT('Ctrl Pts',(84.7320931464425,-37.3300072137338,119.05503403593));
#50420=CARTESIAN_POINT('Ctrl Pts',(85.2921417887346,-34.3453833261113,118.897085512738));
#50421=CARTESIAN_POINT('Ctrl Pts',(88.0974795016528,-33.1827507261497,118.739136989545));
#50422=CARTESIAN_POINT('Ctrl Pts',(90.6045919087642,-34.896233039778,118.581188466353));
#50423=CARTESIAN_POINT('Ctrl Pts',(90.540356437329,-37.932267962832,118.42323994316));
#50424=CARTESIAN_POINT('Ctrl Pts',(87.9630134374091,-39.5381749691605,118.265291419968));
#50425=CARTESIAN_POINT('Ctrl Pts',(85.2093614198393,-38.2579270167265,118.107342896775));
#50426=CARTESIAN_POINT('Ctrl Pts',(84.7760529208225,-35.2522859874351,117.949394373583));
#50427=CARTESIAN_POINT('Ctrl Pts',(87.055955577734,-33.2463751899036,117.791445850391));
#50428=CARTESIAN_POINT('Ctrl Pts',(89.9819509917552,-34.0588929373327,117.633497327198));
#50429=CARTESIAN_POINT('Ctrl Pts',(90.9011281110726,-36.9531540996908,117.475548804005));
#50430=CARTESIAN_POINT('Ctrl Pts',(88.9800969971335,-39.3050201060654,117.317600280813));
#50431=CARTESIAN_POINT('Ctrl Pts',(85.9605981354142,-38.9821255772365,117.159651757621));
#50432=CARTESIAN_POINT('Ctrl Pts',(84.5803193099349,-36.2772291621056,117.001703234428));
#50433=CARTESIAN_POINT('Ctrl Pts',(86.0907173524721,-33.6427781745634,116.843754711236));
#50434=CARTESIAN_POINT('Ctrl Pts',(89.1223602945383,-33.4673492018109,116.685806188043));
#50435=CARTESIAN_POINT('Ctrl Pts',(90.926549683814,-35.9099983580111,116.527857664851));
#50436=CARTESIAN_POINT('Ctrl Pts',(89.8674818729827,-38.7560499430534,116.369909141658));
#50437=CARTESIAN_POINT('Ctrl Pts',(86.9053814360339,-39.4250755435261,116.211960618466));
#50438=CARTESIAN_POINT('Ctrl Pts',(84.7258947509363,-37.3104899949744,116.054012095273));
#50439=CARTESIAN_POINT('Ctrl Pts',(85.3050961089771,-34.329523702058,115.896063572081));
#50440=CARTESIAN_POINT('Ctrl Pts',(88.1178412544334,-33.1849281405724,115.738115048888));
#50441=CARTESIAN_POINT('Ctrl Pts',(90.6138997096969,-34.9144732948164,115.580166525696));
#50442=CARTESIAN_POINT('Ctrl Pts',(90.5301711875661,-37.950033175175,115.422218002503));
#50443=CARTESIAN_POINT('Ctrl Pts',(87.9425697925695,-39.5393579605074,115.264269479311));
#50444=CARTESIAN_POINT('Ctrl Pts',(85.1971950112113,-38.2414552050812,115.106320956119));
#50445=CARTESIAN_POINT('Ctrl Pts',(84.7831946609494,-35.2330938633132,114.948372432926));
#50446=CARTESIAN_POINT('Ctrl Pts',(87.075930268115,-33.2418636686103,114.790423909734));
#50447=CARTESIAN_POINT('Ctrl Pts',(89.9966481880921,-34.0731524779808,114.632475386541));
#50448=CARTESIAN_POINT('Ctrl Pts',(90.8972223124579,-36.9732560104747,114.474526863349));
#50449=CARTESIAN_POINT('Ctrl Pts',(88.9611294723736,-39.3127385958416,114.316578340156));
#50450=CARTESIAN_POINT('Ctrl Pts',(85.9437661623417,-38.9704625260759,114.158629816964));
#50451=CARTESIAN_POINT('Ctrl Pts',(84.5808839266114,-36.256759103778,114.000681293771));
#50452=CARTESIAN_POINT('Ctrl Pts',(86.1081666381298,-33.6320606883866,113.842732770579));
#50453=CARTESIAN_POINT('Ctrl Pts',(89.1408735125671,-33.4761015065434,113.684784247386));
#50454=CARTESIAN_POINT('Ctrl Pts',(90.9293414624814,-35.9302850051414,113.526835724194));
#50455=CARTESIAN_POINT('Ctrl Pts',(89.8520209914789,-38.7694776466189,113.368887201001));
#50456=CARTESIAN_POINT('Ctrl Pts',(86.8856858053969,-39.4194698130891,113.210938677809));
#50457=CARTESIAN_POINT('Ctrl Pts',(84.7198218004494,-37.2909333758316,113.052990154616));
#50458=CARTESIAN_POINT('Ctrl Pts',(85.318151998146,-34.3137475859984,112.895041631424));
#50459=CARTESIAN_POINT('Ctrl Pts',(88.1381886056259,-33.1872362522184,112.737093108232));
#50460=CARTESIAN_POINT('Ctrl Pts',(90.6230901984232,-34.9327729395367,112.579144585039));
#50461=CARTESIAN_POINT('Ctrl Pts',(90.5198720772144,-37.96773262166,112.421196061847));
#50462=CARTESIAN_POINT('Ctrl Pts',(87.9221189732622,-39.5404096589339,112.263247538654));
#50463=CARTESIAN_POINT('Ctrl Pts',(85.185134618831,-38.2249056124711,112.105299015462));
#50464=CARTESIAN_POINT('Ctrl Pts',(84.7904594864668,-35.2139479919543,111.947350492269));
#50465=CARTESIAN_POINT('Ctrl Pts',(87.0959335151835,-33.2374804977659,111.789401969077));
#50466=CARTESIAN_POINT('Ctrl Pts',(90.0112535209652,-34.0875060953524,111.631453445884));
#50467=CARTESIAN_POINT('Ctrl Pts',(90.8931875200224,-36.9933324277266,111.473504922692));
#50468=CARTESIAN_POINT('Ctrl Pts',(88.9421127782144,-39.3203351360697,111.315556399499));
#50469=CARTESIAN_POINT('Ctrl Pts',(85.9270094246943,-38.9586916372493,111.157607876307));
#50470=CARTESIAN_POINT('Ctrl Pts',(84.5815799698509,-36.2362930928918,110.999659353114));
#50471=CARTESIAN_POINT('Ctrl Pts',(86.1256843810546,-33.6214554648776,110.841710829922));
#50472=CARTESIAN_POINT('Ctrl Pts',(89.1593301503747,-33.484972504411,110.683762306729));
#50473=CARTESIAN_POINT('Ctrl Pts',(90.9320029231501,-35.950589159622,110.525813783537));
#50474=CARTESIAN_POINT('Ctrl Pts',(89.8364742092662,-38.7828058000054,110.367865260344));
#50475=CARTESIAN_POINT('Ctrl Pts',(86.8660265755163,-39.413737730696,110.209916737152));
#50476=CARTESIAN_POINT('Ctrl Pts',(84.7138745474594,-37.2713381693559,110.051968213959));
#50477=CARTESIAN_POINT('Ctrl Pts',(85.3313089180581,-34.298055618951,109.894019690767));
#50478=CARTESIAN_POINT('Ctrl Pts',(88.1585207139529,-33.1896749831523,109.736071167575));
#50479=CARTESIAN_POINT('Ctrl Pts',(90.6321630019245,-34.9511311850741,109.578122644382));
#50480=CARTESIAN_POINT('Ctrl Pts',(90.5094595182593,-37.9853656427257,109.42017412119));
#50481=CARTESIAN_POINT('Ctrl Pts',(87.9016618489127,-39.5413298770121,109.262225597997));
#50482=CARTESIAN_POINT('Ctrl Pts',(85.1731806858554,-38.2082792173576,109.104277074805));
#50483=CARTESIAN_POINT('Ctrl Pts',(84.7978472091305,-35.1948485538596,108.946328551612));
#50484=CARTESIAN_POINT('Ctrl Pts',(87.1159642653522,-33.2332271101078,108.78838002842));
#50485=CARTESIAN_POINT('Ctrl Pts',(90.0257668588284,-34.1019506231015,108.630431505227));
#50486=CARTESIAN_POINT('Ctrl Pts',(90.8890229323498,-37.0133878178172,108.472482982035));
#50487=CARTESIAN_POINT('Ctrl Pts',(88.9230496887618,-39.3277985271172,108.314534458842));
#50488=CARTESIAN_POINT('Ctrl Pts',(85.9103245211404,-38.946835782131,108.15658593565));
#50489=CARTESIAN_POINT('Ctrl Pts',(84.582415825876,-36.2157859401729,107.998637412457));
#50490=CARTESIAN_POINT('Ctrl Pts',(86.1432525552737,-33.6110576005356,107.840688889265));
#50491=CARTESIAN_POINT('Ctrl Pts',(89.1777650301391,-33.4937671795376,107.682740366073));
#50492=CARTESIAN_POINT('Ctrl Pts',(90.9344608156447,-35.9713102924167,107.52479184288));
#50493=CARTESIAN_POINT('Ctrl Pts',(89.8209928334223,-38.7952107452311,107.366843319688));
#50494=CARTESIAN_POINT('Ctrl Pts',(86.846102987813,-39.4095842666964,107.208894796495));
#50495=CARTESIAN_POINT('Ctrl Pts',(84.7087423466685,-37.2482078703435,107.050946273303));
#50496=CARTESIAN_POINT('Ctrl Pts',(85.1331869260174,-35.2780872164347,106.945647257841));
#50497=CARTESIAN_POINT('Ctrl Pts',(85.7142240382307,-34.5985007534561,106.89299775011));
#50498=CARTESIAN_POINT('Ctrl Pts',(87.1183555905968,-38.7870128767185,122.321006749669));
#50499=CARTESIAN_POINT('Ctrl Pts',(86.3138051921097,-38.5719224173526,122.268357241939));
#50500=CARTESIAN_POINT('Ctrl Pts',(84.9485675510758,-37.2836082952637,122.163058226477));
#50501=CARTESIAN_POINT('Ctrl Pts',(85.4488476887748,-34.4968775786294,122.005109703285));
#50502=CARTESIAN_POINT('Ctrl Pts',(88.056496926311,-33.3989128812863,121.847161180092));
#50503=CARTESIAN_POINT('Ctrl Pts',(90.401079023663,-34.9790534616111,121.6892126569));
#50504=CARTESIAN_POINT('Ctrl Pts',(90.3598044137333,-37.8076326123949,121.531264133707));
#50505=CARTESIAN_POINT('Ctrl Pts',(87.9686505906198,-39.3186118829278,121.373315610515));
#50506=CARTESIAN_POINT('Ctrl Pts',(85.3963065964737,-38.1427383598431,121.215367087322));
#50507=CARTESIAN_POINT('Ctrl Pts',(84.9746968227168,-35.3457974789413,121.05741856413));
#50508=CARTESIAN_POINT('Ctrl Pts',(87.086248185493,-33.4638574322856,120.899470040937));
#50509=CARTESIAN_POINT('Ctrl Pts',(89.8164004813384,-34.2031348301304,120.741521517745));
#50510=CARTESIAN_POINT('Ctrl Pts',(90.6898469521331,-36.8933888246327,120.583572994552));
#50511=CARTESIAN_POINT('Ctrl Pts',(88.9146411383204,-39.0954287378041,120.42562447136));
#50512=CARTESIAN_POINT('Ctrl Pts',(86.1003174536982,-38.8127412901761,120.267675948167));
#50513=CARTESIAN_POINT('Ctrl Pts',(84.798533070175,-36.3016260519611,120.109727424975));
#50514=CARTESIAN_POINT('Ctrl Pts',(86.1895784939907,-33.8388370458375,119.951778901782));
#50515=CARTESIAN_POINT('Ctrl Pts',(89.0122340773642,-33.657309087408,119.79383037859));
#50516=CARTESIAN_POINT('Ctrl Pts',(90.7072843697732,-35.9216285779027,119.635881855397));
#50517=CARTESIAN_POINT('Ctrl Pts',(89.737878570966,-38.5788056474845,119.477933332205));
#50518=CARTESIAN_POINT('Ctrl Pts',(86.9829475584895,-39.2196587850576,119.319984809012));
#50519=CARTESIAN_POINT('Ctrl Pts',(84.9403034341435,-37.2631458813898,119.16203628582));
#50520=CARTESIAN_POINT('Ctrl Pts',(85.4619495303279,-34.4831777107948,119.004087762628));
#50521=CARTESIAN_POINT('Ctrl Pts',(88.0749251826453,-33.4002668504372,118.846139239435));
#50522=CARTESIAN_POINT('Ctrl Pts',(90.4101248440757,-34.9962556490655,118.688190716243));
#50523=CARTESIAN_POINT('Ctrl Pts',(90.3502940001447,-37.8241095994096,118.53024219305));
#50524=CARTESIAN_POINT('Ctrl Pts',(87.9496794589972,-39.319899531616,118.372293669858));
#50525=CARTESIAN_POINT('Ctrl Pts',(85.3848454129102,-38.1274382057533,118.214345146665));
#50526=CARTESIAN_POINT('Ctrl Pts',(84.981248885954,-35.3278940392956,118.056396623473));
#50527=CARTESIAN_POINT('Ctrl Pts',(87.1048185740992,-33.4595285834953,117.89844810028));
#50528=CARTESIAN_POINT('Ctrl Pts',(89.8301784266481,-34.2163319734512,117.740499577088));
#50529=CARTESIAN_POINT('Ctrl Pts',(90.6863275533235,-36.9121335925805,117.582551053895));
#50530=CARTESIAN_POINT('Ctrl Pts',(88.8970215795888,-39.1027321019403,117.424602530703));
#50531=CARTESIAN_POINT('Ctrl Pts',(86.0845698125377,-38.8019784571255,117.26665400751));
#50532=CARTESIAN_POINT('Ctrl Pts',(84.7989367325066,-36.2825568408863,117.108705484318));
#50533=CARTESIAN_POINT('Ctrl Pts',(86.2057667523946,-33.8287502079193,116.950756961126));
#50534=CARTESIAN_POINT('Ctrl Pts',(89.0295298799712,-33.665350403182,116.792808437933));
#50535=CARTESIAN_POINT('Ctrl Pts',(90.7100059683359,-35.9405070600484,116.634859914741));
#50536=CARTESIAN_POINT('Ctrl Pts',(89.7235584575382,-38.5914048335001,116.476911391548));
#50537=CARTESIAN_POINT('Ctrl Pts',(86.9645693041736,-39.2145553357593,116.318962868356));
#50538=CARTESIAN_POINT('Ctrl Pts',(84.9345300627357,-37.2449669586938,116.161014345163));
#50539=CARTESIAN_POINT('Ctrl Pts',(85.4740155725839,-34.4684055814659,116.003065821971));
#50540=CARTESIAN_POINT('Ctrl Pts',(88.0938907296483,-33.4022949595113,115.845117298778));
#50541=CARTESIAN_POINT('Ctrl Pts',(90.4187944089205,-35.0132451694672,115.687168775586));
#50542=CARTESIAN_POINT('Ctrl Pts',(90.3408071531528,-37.8406566508026,115.529220252393));
#50543=CARTESIAN_POINT('Ctrl Pts',(87.930637635275,-39.3210014052237,115.371271729201));
#50544=CARTESIAN_POINT('Ctrl Pts',(85.3735132551544,-38.1120958665474,115.213323206008));
#50545=CARTESIAN_POINT('Ctrl Pts',(84.9879009168238,-35.3100179194915,115.055374682816));
#50546=CARTESIAN_POINT('Ctrl Pts',(87.1234235995788,-33.4553264173033,114.897426159623));
#50547=CARTESIAN_POINT('Ctrl Pts',(89.8438678359514,-34.2296137371245,114.739477636431));
#50548=CARTESIAN_POINT('Ctrl Pts',(90.6826895753943,-36.9308571149577,114.581529113239));
#50549=CARTESIAN_POINT('Ctrl Pts',(88.8793546583644,-39.1099213347251,114.423580590046));
#50550=CARTESIAN_POINT('Ctrl Pts',(86.0688920081806,-38.791115141606,114.265632066854));
#50551=CARTESIAN_POINT('Ctrl Pts',(84.7994626334068,-36.2634904148495,114.107683543661));
#50552=CARTESIAN_POINT('Ctrl Pts',(86.2220195402012,-33.8187676199746,113.949735020469));
#50553=CARTESIAN_POINT('Ctrl Pts',(89.0467736462859,-33.6735025622116,113.791786497276));
#50554=CARTESIAN_POINT('Ctrl Pts',(90.7126063146866,-35.9594026513973,113.633837974084));
#50555=CARTESIAN_POINT('Ctrl Pts',(89.7091577289746,-38.6039117991753,113.475889450891));
#50556=CARTESIAN_POINT('Ctrl Pts',(86.946224203306,-39.2093339903656,113.317940927699));
#50557=CARTESIAN_POINT('Ctrl Pts',(84.9288735345797,-37.2267513372994,113.159992404506));
#50558=CARTESIAN_POINT('Ctrl Pts',(85.4861762191828,-34.4537112339862,113.002043881314));
#50559=CARTESIAN_POINT('Ctrl Pts',(88.1128428625806,-33.4044448038976,112.844095358121));
#50560=CARTESIAN_POINT('Ctrl Pts',(90.4273547056591,-35.0302900071992,112.686146834929));
#50561=CARTESIAN_POINT('Ctrl Pts',(90.3312142529948,-37.8571424459038,112.528198311737));
#50562=CARTESIAN_POINT('Ctrl Pts',(87.9115891290386,-39.3219809886689,112.370249788544));
#50563=CARTESIAN_POINT('Ctrl Pts',(85.3622798441101,-38.0966810798189,112.212301265352));
#50564=CARTESIAN_POINT('Ctrl Pts',(84.9946675931167,-35.2921848808977,112.054352742159));
#50565=CARTESIAN_POINT('Ctrl Pts',(87.1420552236133,-33.4512438005674,111.896404218967));
#50566=CARTESIAN_POINT('Ctrl Pts',(89.8574716808703,-34.2429831266786,111.738455695774));
#50567=CARTESIAN_POINT('Ctrl Pts',(90.6789314487532,-36.9495568918948,111.580507172582));
#50568=CARTESIAN_POINT('Ctrl Pts',(88.8616419392871,-39.1169969800445,111.422558649389));
#50569=CARTESIAN_POINT('Ctrl Pts',(86.0532842803539,-38.7801513828512,111.264610126197));
#50570=CARTESIAN_POINT('Ctrl Pts',(84.8001109489481,-36.244427758721,111.106661603004));
#50571=CARTESIAN_POINT('Ctrl Pts',(86.2383360911588,-33.8088895968443,110.948713079812));
#50572=CARTESIAN_POINT('Ctrl Pts',(89.0639647120862,-33.6817652755859,110.790764556619));
#50573=CARTESIAN_POINT('Ctrl Pts',(90.7150852789466,-35.9783145496169,110.632816033427));
#50574=CARTESIAN_POINT('Ctrl Pts',(89.6946769899154,-38.6163260408294,110.474867510234));
#50575=CARTESIAN_POINT('Ctrl Pts',(86.9279130071941,-39.2039949569718,110.316918987042));
#50576=CARTESIAN_POINT('Ctrl Pts',(84.9233340848409,-37.2084997745063,110.158970463849));
#50577=CARTESIAN_POINT('Ctrl Pts',(85.4984309688452,-34.4390952654192,110.001021940657));
#50578=CARTESIAN_POINT('Ctrl Pts',(88.131780797851,-33.4067163110047,109.843073417464));
#50579=CARTESIAN_POINT('Ctrl Pts',(90.4358053868511,-35.0473894274892,109.685124894272));
#50580=CARTESIAN_POINT('Ctrl Pts',(90.3215156834062,-37.873566370378,109.52717637108));
#50581=CARTESIAN_POINT('Ctrl Pts',(87.8925347500967,-39.322838107376,109.369227847887));
#50582=CARTESIAN_POINT('Ctrl Pts',(85.3511455925472,-38.0811947569362,109.211279324695));
#50583=CARTESIAN_POINT('Ctrl Pts',(85.0015487394962,-35.2743950916382,109.053330801502));
#50584=CARTESIAN_POINT('Ctrl Pts',(87.1607124648601,-33.4472820677823,108.89538227831));
#50585=CARTESIAN_POINT('Ctrl Pts',(89.8709898388786,-34.2564371928838,108.737433755117));
#50586=CARTESIAN_POINT('Ctrl Pts',(90.675052426937,-36.9682370835035,108.579485231925));
#50587=CARTESIAN_POINT('Ctrl Pts',(88.8438860062427,-39.1239486062252,108.421536708732));
#50588=CARTESIAN_POINT('Ctrl Pts',(86.0377434609558,-38.7691084839451,108.26358818554));
#50589=CARTESIAN_POINT('Ctrl Pts',(84.8008894903094,-36.225326781856,108.105639662347));
#50590=CARTESIAN_POINT('Ctrl Pts',(86.254699615336,-33.799204714259,107.947691139155));
#50591=CARTESIAN_POINT('Ctrl Pts',(89.0811355117927,-33.6899568996709,107.789742615962));
#50592=CARTESIAN_POINT('Ctrl Pts',(90.7173746337058,-35.9976148339398,107.63179409277));
#50593=CARTESIAN_POINT('Ctrl Pts',(89.6802571723091,-38.6278803787238,107.473845569577));
#50594=CARTESIAN_POINT('Ctrl Pts',(86.9093555802804,-39.200126296078,107.315897046385));
#50595=CARTESIAN_POINT('Ctrl Pts',(84.9185537991564,-37.1869555205393,107.157948523193));
#50596=CARTESIAN_POINT('Ctrl Pts',(85.3138942055859,-35.3519260775293,107.052649507731));
#50597=CARTESIAN_POINT('Ctrl Pts',(85.8550895919077,-34.718938871308,107.));
#50598=CARTESIAN_POINT('Ctrl Pts',(85.2535610703604,-36.3531642914838,121.112583302492));
#50599=CARTESIAN_POINT('Ctrl Pts',(85.2516482037573,-36.0616114634661,121.094195056371));
#50600=CARTESIAN_POINT('Ctrl Pts',(85.298519492613,-35.7706534853458,121.07580681025));
#50601=CARTESIAN_POINT('Ctrl Pts',(85.3968903454723,-35.4982976179823,121.05741856413));
#50602=CARTESIAN_POINT('Ctrl Pts',(85.6785472769755,-34.7184841300561,121.004769056399));
#50603=CARTESIAN_POINT('Ctrl Pts',(86.3823977312343,-34.0911707811709,120.952119548668));
#50604=CARTESIAN_POINT('Ctrl Pts',(87.1893483410045,-33.9007270063691,120.899470040937));
#50605=CARTESIAN_POINT('Ctrl Pts',(87.9962989507748,-33.7102832315672,120.846820533206));
#50606=CARTESIAN_POINT('Ctrl Pts',(88.9063497160566,-33.9567090308488,120.794171025476));
#50607=CARTESIAN_POINT('Ctrl Pts',(89.5069495104966,-34.52829759624,120.741521517745));
#50608=CARTESIAN_POINT('Ctrl Pts',(90.1075493049366,-35.0998861616311,120.688872010014));
#50609=CARTESIAN_POINT('Ctrl Pts',(90.3986981285349,-35.9966374931319,120.636222502283));
#50610=CARTESIAN_POINT('Ctrl Pts',(90.2484049046985,-36.8120198110775,120.583572994552));
#50611=CARTESIAN_POINT('Ctrl Pts',(90.0981116808622,-37.6274021290232,120.530923486821));
#50612=CARTESIAN_POINT('Ctrl Pts',(89.5063764095913,-38.3614154334136,120.478273979091));
#50613=CARTESIAN_POINT('Ctrl Pts',(88.7414548265188,-38.6813075110042,120.42562447136));
#50614=CARTESIAN_POINT('Ctrl Pts',(87.9765332434463,-39.0011995885948,120.372974963629));
#50615=CARTESIAN_POINT('Ctrl Pts',(87.0384253485722,-38.9069704393855,120.320325455898));
#50616=CARTESIAN_POINT('Ctrl Pts',(86.3524073372147,-38.4413366584116,120.267675948167));
#50617=CARTESIAN_POINT('Ctrl Pts',(85.6787932621231,-37.9841220321056,120.215978399609));
#50618=CARTESIAN_POINT('Ctrl Pts',(85.2482353778633,-37.1688121351973,120.16428085105));
#50619=CARTESIAN_POINT('Ctrl Pts',(85.2469700844899,-36.3546528234761,120.112583302492));
#50620=CARTESIAN_POINT('Ctrl Pts',(86.9747563060389,-39.3241490284291,122.));
#50621=CARTESIAN_POINT('Ctrl Pts',(86.8817062191854,-39.290110891006,122.));
#50622=CARTESIAN_POINT('Ctrl Pts',(86.7907212975493,-39.2513040586725,122.));
#50623=CARTESIAN_POINT('Ctrl Pts',(86.7020100267322,-39.2080568530126,122.));
#50624=CARTESIAN_POINT('Ctrl Pts',(86.6113318105991,-39.1638507512867,122.));
#50625=CARTESIAN_POINT('Ctrl Pts',(86.5230285198804,-39.1150045689307,122.));
#50626=CARTESIAN_POINT('Ctrl Pts',(86.4373517348404,-39.0618234125105,122.));
#50627=CARTESIAN_POINT('Ctrl Pts',(86.3549203075593,-39.0106567093467,122.));
#50628=CARTESIAN_POINT('Ctrl Pts',(86.2749198914356,-38.9554763459202,122.));
#50629=CARTESIAN_POINT('Ctrl Pts',(86.197607513613,-38.8965240074405,122.));
#50630=CARTESIAN_POINT('Ctrl Pts',(86.1299591830182,-38.8449407112708,122.));
#50631=CARTESIAN_POINT('Ctrl Pts',(86.0643691719831,-38.7904687993429,122.));
#50632=CARTESIAN_POINT('Ctrl Pts',(86.0010342894347,-38.7332574826561,122.));
#50633=CARTESIAN_POINT('Ctrl Pts',(85.986897867521,-38.7204878480034,122.));
#50634=CARTESIAN_POINT('Ctrl Pts',(85.9728711507639,-38.7075790036905,122.));
#50635=CARTESIAN_POINT('Ctrl Pts',(85.9589759122883,-38.6945511416087,122.));
#50636=CARTESIAN_POINT('Ctrl Pts',(85.8865458109709,-38.6266423128259,122.));
#50637=CARTESIAN_POINT('Ctrl Pts',(85.8175813968922,-38.5554115699911,122.));
#50638=CARTESIAN_POINT('Ctrl Pts',(85.7523226201221,-38.4811496345928,122.));
#50639=CARTESIAN_POINT('Ctrl Pts',(85.687422873419,-38.4072962613675,122.));
#50640=CARTESIAN_POINT('Ctrl Pts',(85.6261876156017,-38.3304441599178,122.));
#50641=CARTESIAN_POINT('Ctrl Pts',(85.5688964676845,-38.2508525115488,122.));
#50642=CARTESIAN_POINT('Ctrl Pts',(85.5137335478701,-38.1742175011415,122.));
#50643=CARTESIAN_POINT('Ctrl Pts',(85.4622269892531,-38.0950419612856,122.));
#50644=CARTESIAN_POINT('Ctrl Pts',(85.4146712402722,-38.0135436638871,122.));
#50645=CARTESIAN_POINT('Ctrl Pts',(85.3947249112917,-37.9793607967031,122.));
#50646=CARTESIAN_POINT('Ctrl Pts',(85.375474185618,-37.9447691989933,122.));
#50647=CARTESIAN_POINT('Ctrl Pts',(85.3569433734486,-37.9097846421959,122.));
#50648=CARTESIAN_POINT('Ctrl Pts',(85.3440608433971,-37.8854635492962,122.));
#50649=CARTESIAN_POINT('Ctrl Pts',(85.3315262772696,-37.8609525380258,122.));
#50650=CARTESIAN_POINT('Ctrl Pts',(85.3193483089147,-37.8362569015937,122.));
#50651=CARTESIAN_POINT('Ctrl Pts',(85.3114399504896,-37.8202195841407,122.));
#50652=CARTESIAN_POINT('Ctrl Pts',(85.3036808680344,-37.8041017938262,122.));
#50653=CARTESIAN_POINT('Ctrl Pts',(85.2960836020132,-37.7879271698132,122.));
#50654=CARTESIAN_POINT('Ctrl Pts',(85.2539632958679,-37.6982527904632,122.));
#50655=CARTESIAN_POINT('Ctrl Pts',(85.2167418241088,-37.6066948163004,122.));
#50656=CARTESIAN_POINT('Ctrl Pts',(85.1847104706482,-37.5135256106319,122.));
#50657=CARTESIAN_POINT('Ctrl Pts',(85.1548307191947,-37.4266147433807,122.));
#50658=CARTESIAN_POINT('Ctrl Pts',(85.1294674189967,-37.3383010414635,122.));
#50659=CARTESIAN_POINT('Ctrl Pts',(85.1089075479901,-37.2487968899418,122.));
#50660=CARTESIAN_POINT('Ctrl Pts',(85.1074270584421,-37.2423518125,122.));
#50661=CARTESIAN_POINT('Ctrl Pts',(85.105971498406,-37.2359005611176,122.));
#50662=CARTESIAN_POINT('Ctrl Pts',(85.1045409856617,-37.2294432147812,122.));
#50663=CARTESIAN_POINT('Ctrl Pts',(85.0839347678633,-37.1364265775401,122.));
#50664=CARTESIAN_POINT('Ctrl Pts',(85.0685215768674,-37.04214426797,122.));
#50665=CARTESIAN_POINT('Ctrl Pts',(85.0582244923225,-36.9470041536375,122.));
#50666=CARTESIAN_POINT('Ctrl Pts',(85.0524279776539,-36.8934471428256,122.));
#50667=CARTESIAN_POINT('Ctrl Pts',(85.0482536228696,-36.8396184930835,122.));
#50668=CARTESIAN_POINT('Ctrl Pts',(85.0456944683025,-36.7855935994856,122.));
#50669=CARTESIAN_POINT('Ctrl Pts',(85.0450335864434,-36.7716420888667,122.));
#50670=CARTESIAN_POINT('Ctrl Pts',(85.0444805412283,-36.7576780899949,122.));
#50671=CARTESIAN_POINT('Ctrl Pts',(85.0440354542009,-36.7437162707763,122.));
#50672=CARTESIAN_POINT('Ctrl Pts',(85.0410640494509,-36.6505070478834,122.));
#50673=CARTESIAN_POINT('Ctrl Pts',(85.0428918001145,-36.557239583447,122.));
#50674=CARTESIAN_POINT('Ctrl Pts',(85.0493838115575,-36.4642889583755,122.));
#50675=CARTESIAN_POINT('Ctrl Pts',(85.0558866172978,-36.3711837838725,122.));
#50676=CARTESIAN_POINT('Ctrl Pts',(85.0670695852548,-36.27839552357,122.));
#50677=CARTESIAN_POINT('Ctrl Pts',(85.0828480795227,-36.1863132281589,122.));
#50678=CARTESIAN_POINT('Ctrl Pts',(85.0984009758062,-36.0955475083282,122.));
#50679=CARTESIAN_POINT('Ctrl Pts',(85.1184193868686,-36.0054668661199,122.));
#50680=CARTESIAN_POINT('Ctrl Pts',(85.1428652803547,-35.9164691013446,122.));
#50681=CARTESIAN_POINT('Ctrl Pts',(85.1519640438232,-35.8833441263305,122.));
#50682=CARTESIAN_POINT('Ctrl Pts',(85.1616765572995,-35.8503694822698,122.));
#50683=CARTESIAN_POINT('Ctrl Pts',(85.1720022212126,-35.817566946539,122.));
#50684=CARTESIAN_POINT('Ctrl Pts',(85.1789966596367,-35.7953470371703,122.));
#50685=CARTESIAN_POINT('Ctrl Pts',(85.1862724563629,-35.7732061147807,122.));
#50686=CARTESIAN_POINT('Ctrl Pts',(85.1938296041438,-35.751151161507,122.));
#50687=CARTESIAN_POINT('Ctrl Pts',(85.1983456598534,-35.737971401028,122.));
#50688=CARTESIAN_POINT('Ctrl Pts',(85.2029618432749,-35.7248235133138,122.));
#50689=CARTESIAN_POINT('Ctrl Pts',(85.2076746824257,-35.7117181369059,122.));
#50690=CARTESIAN_POINT('Ctrl Pts',(85.2393064450318,-35.6237571133841,122.));
#50691=CARTESIAN_POINT('Ctrl Pts',(85.2753274324375,-35.5375938379398,122.));
#50692=CARTESIAN_POINT('Ctrl Pts',(85.3156730801928,-35.4536425565309,122.));
#50693=CARTESIAN_POINT('Ctrl Pts',(85.3459323160092,-35.3906790954742,122.));
#50694=CARTESIAN_POINT('Ctrl Pts',(85.3786252206014,-35.3289603730047,122.));
#50695=CARTESIAN_POINT('Ctrl Pts',(85.4137405176868,-35.268676680312,122.));
#50696=CARTESIAN_POINT('Ctrl Pts',(85.4272098015241,-35.2455534766078,122.));
#50697=CARTESIAN_POINT('Ctrl Pts',(85.4410356214481,-35.2226415677282,122.));
#50698=CARTESIAN_POINT('Ctrl Pts',(85.4552178215069,-35.1999523366376,122.));
#50699=CARTESIAN_POINT('Ctrl Pts',(85.4653422141899,-35.1837549424194,122.));
#50700=CARTESIAN_POINT('Ctrl Pts',(85.475649063879,-35.1676699643451,122.));
#50701=CARTESIAN_POINT('Ctrl Pts',(85.4861282385094,-35.1517165484869,122.));
#50702=CARTESIAN_POINT('Ctrl Pts',(85.5333148151565,-35.0798800626262,122.));
#50703=CARTESIAN_POINT('Ctrl Pts',(85.584036314847,-35.0106370295489,122.));
#50704=CARTESIAN_POINT('Ctrl Pts',(85.6382598459827,-34.9443394496007,122.));
#50705=CARTESIAN_POINT('Ctrl Pts',(85.6870562587959,-34.8846774539338,122.));
#50706=CARTESIAN_POINT('Ctrl Pts',(85.7386893651034,-34.8274008880271,122.));
#50707=CARTESIAN_POINT('Ctrl Pts',(85.7931556859771,-34.772796091989,122.));
#50708=CARTESIAN_POINT('Ctrl Pts',(85.8122382584008,-34.7536650040366,122.));
#50709=CARTESIAN_POINT('Ctrl Pts',(85.8316687756141,-34.734862165088,122.));
#50710=CARTESIAN_POINT('Ctrl Pts',(85.8514366626951,-34.7163920625308,122.));
#50711=CARTESIAN_POINT('Origin',(87.7685555885722,-36.3549260746835,114.));
#50712=CARTESIAN_POINT('Origin',(-87.7685555885722,36.3549260746835,107.));
#50713=CARTESIAN_POINT('Ctrl Pts',(-89.6820215852368,37.9909132780591,107.));
#50714=CARTESIAN_POINT('Ctrl Pts',(-89.744159122969,37.9325192506103,107.));
#50715=CARTESIAN_POINT('Ctrl Pts',(-89.8029212860977,37.8708713145233,107.));
#50716=CARTESIAN_POINT('Ctrl Pts',(-89.8582960951973,37.8063459457027,107.));
#50717=CARTESIAN_POINT('Ctrl Pts',(-89.915025983506,37.7402415739533,107.));
#50718=CARTESIAN_POINT('Ctrl Pts',(-89.9682011734176,37.671116727705,107.));
#50719=CARTESIAN_POINT('Ctrl Pts',(-90.0177798965015,37.599329927726,107.));
#50720=CARTESIAN_POINT('Ctrl Pts',(-90.0307176306391,37.580596921409,107.));
#50721=CARTESIAN_POINT('Ctrl Pts',(-90.0434102865912,37.5616824282935,107.));
#50722=CARTESIAN_POINT('Ctrl Pts',(-90.0558567466988,37.5425923861499,107.));
#50723=CARTESIAN_POINT('Ctrl Pts',(-90.066026731285,37.5269939402728,107.));
#50724=CARTESIAN_POINT('Ctrl Pts',(-90.0760327837056,37.5112773814265,107.));
#50725=CARTESIAN_POINT('Ctrl Pts',(-90.0858654462594,37.4954605442615,107.));
#50726=CARTESIAN_POINT('Ctrl Pts',(-90.1333095652244,37.4191418564184,107.));
#50727=CARTESIAN_POINT('Ctrl Pts',(-90.1767701202724,37.3404158089311,107.));
#50728=CARTESIAN_POINT('Ctrl Pts',(-90.21621242528,37.2596749530829,107.));
#50729=CARTESIAN_POINT('Ctrl Pts',(-90.2480408931,37.1945200963464,107.));
#50730=CARTESIAN_POINT('Ctrl Pts',(-90.2772522211522,37.1280521304697,107.));
#50731=CARTESIAN_POINT('Ctrl Pts',(-90.3038110239626,37.0604595287346,107.));
#50732=CARTESIAN_POINT('Ctrl Pts',(-90.3144125005572,37.0334785917407,107.));
#50733=CARTESIAN_POINT('Ctrl Pts',(-90.3245911491353,37.0063183070948,107.));
#50734=CARTESIAN_POINT('Ctrl Pts',(-90.3343439585311,36.9789901163685,107.));
#50735=CARTESIAN_POINT('Ctrl Pts',(-90.3395848995591,36.9643045596036,107.));
#50736=CARTESIAN_POINT('Ctrl Pts',(-90.3447024891032,36.9495713342223,107.));
#50737=CARTESIAN_POINT('Ctrl Pts',(-90.3496922602842,36.934804694045,107.));
#50738=CARTESIAN_POINT('Ctrl Pts',(-90.3792310648457,36.8473880806567,107.));
#50739=CARTESIAN_POINT('Ctrl Pts',(-90.4043344064517,36.7586903635531,107.));
#50740=CARTESIAN_POINT('Ctrl Pts',(-90.4249697169135,36.6691093523015,107.));
#50741=CARTESIAN_POINT('Ctrl Pts',(-90.4459264940065,36.5781328056661,107.));
#50742=CARTESIAN_POINT('Ctrl Pts',(-90.4622754461125,36.486244424327,107.));
#50743=CARTESIAN_POINT('Ctrl Pts',(-90.4739406340489,36.393827715093,107.));
#50744=CARTESIAN_POINT('Ctrl Pts',(-90.4855151071126,36.3021296886663,107.));
#50745=CARTESIAN_POINT('Ctrl Pts',(-90.4924787239518,36.209910589573,107.));
#50746=CARTESIAN_POINT('Ctrl Pts',(-90.4947103587392,36.1175258369092,107.));
#50747=CARTESIAN_POINT('Ctrl Pts',(-90.4958209757943,36.0715487431124,107.));
#50748=CARTESIAN_POINT('Ctrl Pts',(-90.4957588348561,36.0255304079173,107.));
#50749=CARTESIAN_POINT('Ctrl Pts',(-90.4945042077797,35.9795139417161,107.));
#50750=CARTESIAN_POINT('Ctrl Pts',(-90.4941344323082,35.9659515367551,107.));
#50751=CARTESIAN_POINT('Ctrl Pts',(-90.4936610488672,35.9523892934637,107.));
#50752=CARTESIAN_POINT('Ctrl Pts',(-90.4930834960119,35.9388283155341,107.));
#50753=CARTESIAN_POINT('Ctrl Pts',(-90.4924629860478,35.9242587019428,107.));
#50754=CARTESIAN_POINT('Ctrl Pts',(-90.4917226371359,35.9097003351427,107.));
#50755=CARTESIAN_POINT('Ctrl Pts',(-90.4908624008004,35.895157143613,107.));
#50756=CARTESIAN_POINT('Ctrl Pts',(-90.4852105919944,35.7996074271386,107.));
#50757=CARTESIAN_POINT('Ctrl Pts',(-90.4743861465461,35.7046794298511,107.));
#50758=CARTESIAN_POINT('Ctrl Pts',(-90.4583186096772,35.6107687957121,107.));
#50759=CARTESIAN_POINT('Ctrl Pts',(-90.455938277629,35.5968563650806,107.));
#50760=CARTESIAN_POINT('Ctrl Pts',(-90.4534427880579,35.5829662291446,107.));
#50761=CARTESIAN_POINT('Ctrl Pts',(-90.4508318193706,35.5690996435893,107.));
#50762=CARTESIAN_POINT('Ctrl Pts',(-90.4338861650802,35.4791030204387,107.));
#50763=CARTESIAN_POINT('Ctrl Pts',(-90.4120806288724,35.3900985715579,107.));
#50764=CARTESIAN_POINT('Ctrl Pts',(-90.3857177602916,35.3023185449965,107.));
#50765=CARTESIAN_POINT('Ctrl Pts',(-90.3587589471203,35.2125542111576,107.));
#50766=CARTESIAN_POINT('Ctrl Pts',(-90.3270342224501,35.1240695823419,107.));
#50767=CARTESIAN_POINT('Ctrl Pts',(-90.2908128794366,35.0371167032257,107.));
#50768=CARTESIAN_POINT('Ctrl Pts',(-90.2783227526108,35.0071329312927,107.));
#50769=CARTESIAN_POINT('Ctrl Pts',(-90.2652974999059,34.9773313750936,107.));
#50770=CARTESIAN_POINT('Ctrl Pts',(-90.2517467909923,34.9477227085599,107.));
#50771=CARTESIAN_POINT('Ctrl Pts',(-90.2450557286484,34.9331025558462,107.));
#50772=CARTESIAN_POINT('Ctrl Pts',(-90.2382365401799,34.9185294366221,107.));
#50773=CARTESIAN_POINT('Ctrl Pts',(-90.2312903305009,34.9040046584706,107.));
#50774=CARTESIAN_POINT('Ctrl Pts',(-90.2257965562483,34.8925169758462,107.));
#50775=CARTESIAN_POINT('Ctrl Pts',(-90.2202237670946,34.8810605569674,107.));
#50776=CARTESIAN_POINT('Ctrl Pts',(-90.2145771037702,34.8696449781357,107.));
#50777=CARTESIAN_POINT('Ctrl Pts',(-90.1718531587215,34.7832721000849,107.));
#50778=CARTESIAN_POINT('Ctrl Pts',(-90.124838355933,34.6990975417634,107.));
#50779=CARTESIAN_POINT('Ctrl Pts',(-90.0738753505963,34.6173709404504,107.));
#50780=CARTESIAN_POINT('Ctrl Pts',(-90.0219016348831,34.5340235178487,107.));
#50781=CARTESIAN_POINT('Ctrl Pts',(-89.965821246638,34.453221340495,107.));
#50782=CARTESIAN_POINT('Ctrl Pts',(-89.9059426250489,34.3752362239655,107.));
#50783=CARTESIAN_POINT('Ctrl Pts',(-89.845577174311,34.2966170676586,107.));
#50784=CARTESIAN_POINT('Ctrl Pts',(-89.7813510190625,34.2208601285459,107.));
#50785=CARTESIAN_POINT('Ctrl Pts',(-89.7135308517992,34.1482631856065,107.));
#50786=CARTESIAN_POINT('Ctrl Pts',(-89.676530180774,34.1086564475,107.));
#50787=CARTESIAN_POINT('Ctrl Pts',(-89.6384589463324,34.0699906809862,107.));
#50788=CARTESIAN_POINT('Ctrl Pts',(-89.5993551074488,34.0323180201534,107.));
#50789=CARTESIAN_POINT('Ctrl Pts',(-89.587387522292,34.0207884417418,107.));
#50790=CARTESIAN_POINT('Ctrl Pts',(-89.5753231944213,34.0093519042645,107.));
#50791=CARTESIAN_POINT('Ctrl Pts',(-89.5631631489415,33.9980099642189,107.));
#50792=CARTESIAN_POINT('Ctrl Pts',(-89.5526173715299,33.9881736872628,107.));
#50793=CARTESIAN_POINT('Ctrl Pts',(-89.5420007164926,33.9784096758184,107.));
#50794=CARTESIAN_POINT('Ctrl Pts',(-89.5313229644313,33.9687269234992,107.));
#50795=CARTESIAN_POINT('Ctrl Pts',(-89.4557484807192,33.9001948014544,107.));
#50796=CARTESIAN_POINT('Ctrl Pts',(-89.3769972770167,33.8356190256038,107.));
#50797=CARTESIAN_POINT('Ctrl Pts',(-89.2953966997877,33.7752813677694,107.));
#50798=CARTESIAN_POINT('Ctrl Pts',(-89.2136919343842,33.7148666704013,107.));
#50799=CARTESIAN_POINT('Ctrl Pts',(-89.1291299412249,33.6587000819157,107.));
#50800=CARTESIAN_POINT('Ctrl Pts',(-89.0419940478043,33.6070902548594,107.));
#50801=CARTESIAN_POINT('Ctrl Pts',(-88.9565903904741,33.5565064160789,107.));
#50802=CARTESIAN_POINT('Ctrl Pts',(-88.8687134883914,33.5102992875464,107.));
#50803=CARTESIAN_POINT('Ctrl Pts',(-88.7785960158935,33.4687952816358,107.));
#50804=CARTESIAN_POINT('Ctrl Pts',(-88.7382467607252,33.4502122513025,107.));
#50805=CARTESIAN_POINT('Ctrl Pts',(-88.6974479330077,33.4325726088462,107.));
#50806=CARTESIAN_POINT('Ctrl Pts',(-88.6562186636994,33.4159086000809,107.));
#50807=CARTESIAN_POINT('Ctrl Pts',(-88.625799021521,33.4036136166285,107.));
#50808=CARTESIAN_POINT('Ctrl Pts',(-88.5951450346788,33.3918497860248,107.));
#50809=CARTESIAN_POINT('Ctrl Pts',(-88.5642689721408,33.3806144275731,107.));
#50810=CARTESIAN_POINT('Ctrl Pts',(-86.97475630604,33.3857031209377,107.));
#50811=CARTESIAN_POINT('Ctrl Pts',(-86.8799223806133,33.4203937944791,107.));
#50812=CARTESIAN_POINT('Ctrl Pts',(-86.7871316088213,33.4600753465665,107.));
#50813=CARTESIAN_POINT('Ctrl Pts',(-86.6966249142161,33.5044274278858,107.));
#50814=CARTESIAN_POINT('Ctrl Pts',(-86.6048453543519,33.5494032666378,107.));
#50815=CARTESIAN_POINT('Ctrl Pts',(-86.5154139004472,33.5991826306842,107.));
#50816=CARTESIAN_POINT('Ctrl Pts',(-86.4286158090018,33.6534721466289,107.));
#50817=CARTESIAN_POINT('Ctrl Pts',(-86.4041027850013,33.6688042833748,107.));
#50818=CARTESIAN_POINT('Ctrl Pts',(-86.3798000322781,33.6844963498378,107.));
#50819=CARTESIAN_POINT('Ctrl Pts',(-86.355714572459,33.7005421935948,107.));
#50820=CARTESIAN_POINT('Ctrl Pts',(-86.3363850476719,33.7134196116288,107.));
#50821=CARTESIAN_POINT('Ctrl Pts',(-86.3171933703453,33.7265265126986,107.));
#50822=CARTESIAN_POINT('Ctrl Pts',(-86.2981624559498,33.7398459518088,107.));
#50823=CARTESIAN_POINT('Ctrl Pts',(-86.2154553522762,33.7977313591239,107.));
#50824=CARTESIAN_POINT('Ctrl Pts',(-86.135703107737,33.8596789089563,107.));
#50825=CARTESIAN_POINT('Ctrl Pts',(-86.0591720841681,33.9253912417443,107.));
#50826=CARTESIAN_POINT('Ctrl Pts',(-86.0001788915497,33.9760449521586,107.));
#50827=CARTESIAN_POINT('Ctrl Pts',(-85.9431003663192,34.0289365876881,107.));
#50828=CARTESIAN_POINT('Ctrl Pts',(-85.8880760765311,34.0839417185279,107.));
#50829=CARTESIAN_POINT('Ctrl Pts',(-85.8587873250428,34.1132202719441,107.));
#50830=CARTESIAN_POINT('Ctrl Pts',(-85.8300808768359,34.1430977911502,107.));
#50831=CARTESIAN_POINT('Ctrl Pts',(-85.8019798022141,34.1735563417783,107.));
#50832=CARTESIAN_POINT('Ctrl Pts',(-85.7923437973743,34.1840007374187,107.));
#50833=CARTESIAN_POINT('Ctrl Pts',(-85.7827797082033,34.1945127449497,107.));
#50834=CARTESIAN_POINT('Ctrl Pts',(-85.7732951013283,34.205084028674,107.));
#50835=CARTESIAN_POINT('Ctrl Pts',(-85.7074979076647,34.2784197832977,107.));
#50836=CARTESIAN_POINT('Ctrl Pts',(-85.6454328643358,34.354702161135,107.));
#50837=CARTESIAN_POINT('Ctrl Pts',(-85.5873437401534,34.4336526051709,107.));
#50838=CARTESIAN_POINT('Ctrl Pts',(-85.5297810737241,34.5118875267408,107.));
#50839=CARTESIAN_POINT('Ctrl Pts',(-85.4761221521735,34.5927431572512,107.));
#50840=CARTESIAN_POINT('Ctrl Pts',(-85.4266499196299,34.6759708305421,107.));
#50841=CARTESIAN_POINT('Ctrl Pts',(-85.3785919815987,34.7568192208378,107.));
#50842=CARTESIAN_POINT('Ctrl Pts',(-85.33448457069,34.839906669308,107.));
#50843=CARTESIAN_POINT('Ctrl Pts',(-85.2946348383161,34.9250155558773,107.));
#50844=CARTESIAN_POINT('Ctrl Pts',(-85.2738304203819,34.9694484978478,107.));
#50845=CARTESIAN_POINT('Ctrl Pts',(-85.2541872885939,35.0144325101597,107.));
#50846=CARTESIAN_POINT('Ctrl Pts',(-85.2357548431069,35.0599368622838,107.));
#50847=CARTESIAN_POINT('Ctrl Pts',(-85.2286967575318,35.0773612247515,107.));
#50848=CARTESIAN_POINT('Ctrl Pts',(-85.2218162315165,35.0948618808238,107.));
#50849=CARTESIAN_POINT('Ctrl Pts',(-85.2151162006499,35.1124370963924,107.));
#50850=CARTESIAN_POINT('Ctrl Pts',(-85.2098744667648,35.1261869737912,107.));
#50851=CARTESIAN_POINT('Ctrl Pts',(-85.2047431089301,35.1399829871612,107.));
#50852=CARTESIAN_POINT('Ctrl Pts',(-85.1997286623157,35.1538095932101,107.));
#50853=CARTESIAN_POINT('Ctrl Pts',(-85.1680449784376,35.2411727359168,107.));
#50854=CARTESIAN_POINT('Ctrl Pts',(-85.1409701200769,35.329896826678,107.));
#50855=CARTESIAN_POINT('Ctrl Pts',(-85.1187553434742,35.419758315364,107.));
#50856=CARTESIAN_POINT('Ctrl Pts',(-85.1137713688799,35.4399191022416,107.));
#50857=CARTESIAN_POINT('Ctrl Pts',(-85.1090322283903,35.4601371793599,107.));
#50858=CARTESIAN_POINT('Ctrl Pts',(-85.1045411201527,35.4804100777641,107.));
#50859=CARTESIAN_POINT('Ctrl Pts',(-85.0841753696162,35.5723412381177,107.));
#50860=CARTESIAN_POINT('Ctrl Pts',(-85.0689058325994,35.6654000254775,107.));
#50861=CARTESIAN_POINT('Ctrl Pts',(-85.058622683849,35.7591948516197,107.));
#50862=CARTESIAN_POINT('Ctrl Pts',(-85.0478888270477,35.8571006834755,107.));
#50863=CARTESIAN_POINT('Ctrl Pts',(-85.0425880547018,35.9558097265016,107.));
#50864=CARTESIAN_POINT('Ctrl Pts',(-85.0426529193585,36.054861962213,107.));
#50865=CARTESIAN_POINT('Ctrl Pts',(-85.0426782913636,36.0936065414948,107.));
#50866=CARTESIAN_POINT('Ctrl Pts',(-85.0435252085663,36.1324033726805,107.));
#50867=CARTESIAN_POINT('Ctrl Pts',(-85.0451918583437,36.1712236979182,107.));
#50868=CARTESIAN_POINT('Ctrl Pts',(-85.0457248984063,36.1836394968929,107.));
#50869=CARTESIAN_POINT('Ctrl Pts',(-85.0463417849372,36.1960563877264,107.));
#50870=CARTESIAN_POINT('Ctrl Pts',(-85.0470417568095,36.2084637610652,107.));
#50871=CARTESIAN_POINT('Ctrl Pts',(-85.0522809798664,36.3013317733989,107.));
#50872=CARTESIAN_POINT('Ctrl Pts',(-85.0621766244509,36.3938165570659,107.));
#50873=CARTESIAN_POINT('Ctrl Pts',(-85.0766052312734,36.4855465333652,107.));
#50874=CARTESIAN_POINT('Ctrl Pts',(-85.0909998491431,36.5770604246414,107.));
#50875=CARTESIAN_POINT('Ctrl Pts',(-85.1099065080408,36.6678240058344,107.));
#50876=CARTESIAN_POINT('Ctrl Pts',(-85.1332512951455,36.7574513655987,107.));
#50877=CARTESIAN_POINT('Ctrl Pts',(-85.1561999302651,36.8455577838216,107.));
#50878=CARTESIAN_POINT('Ctrl Pts',(-85.1834378124742,36.9325670012153,107.));
#50879=CARTESIAN_POINT('Ctrl Pts',(-85.2149351692827,37.0180833239309,107.));
#50880=CARTESIAN_POINT('Ctrl Pts',(-85.2307766169503,37.0610933567811,107.));
#50881=CARTESIAN_POINT('Ctrl Pts',(-85.2476961145767,37.1037252212997,107.));
#50882=CARTESIAN_POINT('Ctrl Pts',(-85.265693291879,37.1459247860001,107.));
#50883=CARTESIAN_POINT('Ctrl Pts',(-85.2712589937397,37.158975176727,107.));
#50884=CARTESIAN_POINT('Ctrl Pts',(-85.2769277783773,37.1719842023805,107.));
#50885=CARTESIAN_POINT('Ctrl Pts',(-85.2826996757167,37.184950204339,107.));
#50886=CARTESIAN_POINT('Ctrl Pts',(-85.2883791458889,37.1977085777205,107.));
#50887=CARTESIAN_POINT('Ctrl Pts',(-85.2941549715906,37.2104174298264,107.));
#50888=CARTESIAN_POINT('Ctrl Pts',(-85.3000253630705,37.2230722749883,107.));
#50889=CARTESIAN_POINT('Ctrl Pts',(-85.3375051695688,37.3038677635949,107.));
#50890=CARTESIAN_POINT('Ctrl Pts',(-85.3788551320423,37.382506472753,107.));
#50891=CARTESIAN_POINT('Ctrl Pts',(-85.4240055740443,37.4586408101418,107.));
#50892=CARTESIAN_POINT('Ctrl Pts',(-85.4683985786282,37.5334979286735,107.));
#50893=CARTESIAN_POINT('Ctrl Pts',(-85.5164660737889,37.6059346660804,107.));
#50894=CARTESIAN_POINT('Ctrl Pts',(-85.5681780442174,37.6755864543237,107.));
#50895=CARTESIAN_POINT('Ctrl Pts',(-85.6183124904752,37.7431134467302,107.));
#50896=CARTESIAN_POINT('Ctrl Pts',(-85.6718728898827,37.8080232545947,107.));
#50897=CARTESIAN_POINT('Ctrl Pts',(-85.7288596017871,37.8699433823759,107.));
#50898=CARTESIAN_POINT('Ctrl Pts',(-85.7498272219443,37.892726197457,107.));
#50899=CARTESIAN_POINT('Ctrl Pts',(-85.7712589370451,37.915103838407,107.));
#50900=CARTESIAN_POINT('Ctrl Pts',(-85.7931555761837,37.9370561406484,107.));
#50901=CARTESIAN_POINT('Ctrl Pts',(-85.8122330129516,37.9561820738691,107.));
#50902=CARTESIAN_POINT('Ctrl Pts',(-85.8316633830167,37.9749851198425,107.));
#50903=CARTESIAN_POINT('Ctrl Pts',(-85.8514365495281,37.9934601500705,107.));
#50904=CARTESIAN_POINT('Origin',(-87.7685555885722,36.3549260746835,124.208423447177));
#50905=CARTESIAN_POINT('Ctrl Pts',(-90.8453550251768,36.3568536361305,121.708423447177));
#50906=CARTESIAN_POINT('Ctrl Pts',(-90.8462777110879,36.4801285286213,121.702019850418));
#50907=CARTESIAN_POINT('Ctrl Pts',(-90.783751283825,37.6160352592255,121.642966745928));
#50908=CARTESIAN_POINT('Ctrl Pts',(-89.371024227111,39.6084645019137,121.531264133707));
#50909=CARTESIAN_POINT('Ctrl Pts',(-85.9203582871986,39.4750890566271,121.373315610515));
#50910=CARTESIAN_POINT('Ctrl Pts',(-84.1454682646258,36.5131478641077,121.215367087322));
#50911=CARTESIAN_POINT('Ctrl Pts',(-85.6554864948497,33.4075615942697,121.05741856413));
#50912=CARTESIAN_POINT('Ctrl Pts',(-89.0813771440687,32.974353542169,120.899470040937));
#50913=CARTESIAN_POINT('Ctrl Pts',(-90.7279240557369,34.9127247019801,120.783138335286));
#50914=CARTESIAN_POINT('Ctrl Pts',(-90.8448016801335,36.1393664148291,120.719456137367));
#50915=CARTESIAN_POINT('Ctrl Pts',(-90.84286984995,36.3522423553315,120.708423447177));
#50916=CARTESIAN_POINT('Ctrl Pts',(-90.8388342008425,36.3519111454271,121.791576552823));
#50917=CARTESIAN_POINT('Ctrl Pts',(-90.833849270346,37.0449295945579,121.755752019753));
#50918=CARTESIAN_POINT('Ctrl Pts',(-90.2614619032149,38.7661192425051,121.667277978953));
#50919=CARTESIAN_POINT('Ctrl Pts',(-87.4170212212397,39.9637875212778,121.526154430423));
#50920=CARTESIAN_POINT('Ctrl Pts',(-84.554628466517,38.0346655247349,121.36820590723));
#50921=CARTESIAN_POINT('Ctrl Pts',(-84.6050188146032,34.5813834739332,121.210257384038));
#50922=CARTESIAN_POINT('Ctrl Pts',(-87.5242687556742,32.7366979528604,121.052308860845));
#50923=CARTESIAN_POINT('Ctrl Pts',(-90.2991159873621,34.0051401442305,120.912748583773));
#50924=CARTESIAN_POINT('Ctrl Pts',(-90.8346457908973,35.6938776421048,120.825837814433));
#50925=CARTESIAN_POINT('Ctrl Pts',(-90.8389970126702,36.3570769587632,120.791576552823));
#50926=CARTESIAN_POINT('Ctrl Pts',(-85.855089591907,37.9909132780583,122.));
#50927=CARTESIAN_POINT('Ctrl Pts',(-85.3138942055855,37.3579260718368,121.947350492269));
#50928=CARTESIAN_POINT('Ctrl Pts',(-84.918555104032,35.5228952161373,121.842051476807));
#50929=CARTESIAN_POINT('Ctrl Pts',(-86.9093551045068,33.5097261262742,121.684102953615));
#50930=CARTESIAN_POINT('Ctrl Pts',(-89.6802575115698,34.0819713092507,121.526154430423));
#50931=CARTESIAN_POINT('Ctrl Pts',(-90.7173747371113,36.7122375197466,121.36820590723));
#50932=CARTESIAN_POINT('Ctrl Pts',(-89.0811356430773,39.0198953249038,121.210257384038));
#50933=CARTESIAN_POINT('Ctrl Pts',(-86.2546994941495,38.9106476647415,121.052308860845));
#50934=CARTESIAN_POINT('Ctrl Pts',(-84.8008892999648,36.4845253442053,120.894360337653));
#50935=CARTESIAN_POINT('Ctrl Pts',(-86.0377433408264,33.9407435207737,120.73641181446));
#50936=CARTESIAN_POINT('Ctrl Pts',(-88.843886080182,33.5859033479533,120.578463291268));
#50937=CARTESIAN_POINT('Ctrl Pts',(-90.675052621233,35.7416150296742,120.420514768075));
#50938=CARTESIAN_POINT('Ctrl Pts',(-89.8709899803276,38.4534150947004,120.262566244883));
#50939=CARTESIAN_POINT('Ctrl Pts',(-87.1607124239154,39.2625702781167,120.10461772169));
#50940=CARTESIAN_POINT('Ctrl Pts',(-85.0015485538449,37.4354571295292,119.946669198498));
#50941=CARTESIAN_POINT('Ctrl Pts',(-85.3511454302727,34.6286572769424,119.788720675305));
#50942=CARTESIAN_POINT('Ctrl Pts',(-87.8925347584294,33.3870138425999,119.630772152113));
#50943=CARTESIAN_POINT('Ctrl Pts',(-90.3215158547498,34.8362856771634,119.472823628921));
#50944=CARTESIAN_POINT('Ctrl Pts',(-90.4358055658698,37.6624628095854,119.314875105728));
#50945=CARTESIAN_POINT('Ctrl Pts',(-88.131780822228,39.3031360362638,119.156926582536));
#50946=CARTESIAN_POINT('Ctrl Pts',(-85.4984308164805,38.2707570125183,118.998978059343));
#50947=CARTESIAN_POINT('Ctrl Pts',(-84.9233338938786,35.5013523175772,118.841029536151));
#50948=CARTESIAN_POINT('Ctrl Pts',(-86.9279129507738,33.5058570011705,118.683081012958));
#50949=CARTESIAN_POINT('Ctrl Pts',(-89.6946771191916,34.0935259567618,118.525132489766));
#50950=CARTESIAN_POINT('Ctrl Pts',(-90.7150854767087,36.7315376250273,118.367183966573));
#50951=CARTESIAN_POINT('Ctrl Pts',(-89.0639647990291,39.0280870531966,118.209235443381));
#50952=CARTESIAN_POINT('Ctrl Pts',(-86.2383359884542,38.9009627234043,118.051286920188));
#50953=CARTESIAN_POINT('Ctrl Pts',(-84.8001107497149,36.4654243980613,117.893338396996));
#50954=CARTESIAN_POINT('Ctrl Pts',(-86.053284165231,33.9297006037413,117.735389873803));
#50955=CARTESIAN_POINT('Ctrl Pts',(-88.8616420126528,33.5928549839411,117.577441350611));
#50956=CARTESIAN_POINT('Ctrl Pts',(-90.6789316440892,35.7602952175635,117.419492827418));
#50957=CARTESIAN_POINT('Ctrl Pts',(-89.8574718210711,38.4668691644366,117.261544304226));
#50958=CARTESIAN_POINT('Ctrl Pts',(-87.1420551815635,39.2586085436859,117.103595781033));
#50959=CARTESIAN_POINT('Ctrl Pts',(-84.9946674069412,37.4176673397963,116.945647257841));
#50960=CARTESIAN_POINT('Ctrl Pts',(-85.3622796826088,34.6131709526458,116.787698734649));
#50961=CARTESIAN_POINT('Ctrl Pts',(-87.9115891386397,33.3878709615584,116.629750211456));
#50962=CARTESIAN_POINT('Ctrl Pts',(-90.3312144249933,34.8527096026399,116.471801688264));
#50963=CARTESIAN_POINT('Ctrl Pts',(-90.4273548841092,37.6795622310744,116.313853165071));
#50964=CARTESIAN_POINT('Ctrl Pts',(-88.1128428856871,39.305407543497,116.155904641879));
#50965=CARTESIAN_POINT('Ctrl Pts',(-85.4861760659956,38.2561410429839,115.997956118686));
#50966=CARTESIAN_POINT('Ctrl Pts',(-84.9288733439891,35.4831007535523,115.840007595494));
#50967=CARTESIAN_POINT('Ctrl Pts',(-86.9462241481147,33.5005179674218,115.682059072301));
#50968=CARTESIAN_POINT('Ctrl Pts',(-89.7091578592229,34.1059401992473,115.524110549109));
#50969=CARTESIAN_POINT('Ctrl Pts',(-90.7126065122823,36.7504495245173,115.366162025916));
#50970=CARTESIAN_POINT('Ctrl Pts',(-89.0467737320752,39.036349767125,115.208213502724));
#50971=CARTESIAN_POINT('Ctrl Pts',(-86.2220194364013,38.8910846996112,115.050264979531));
#50972=CARTESIAN_POINT('Ctrl Pts',(-84.7994624341302,36.4463617406534,114.892316456339));
#50973=CARTESIAN_POINT('Ctrl Pts',(-86.0688918941051,33.9187368442507,114.734367933146));
#50974=CARTESIAN_POINT('Ctrl Pts',(-88.879354732919,33.5999306297355,114.576419409954));
#50975=CARTESIAN_POINT('Ctrl Pts',(-90.6826897709824,35.7789949957557,114.418470886762));
#50976=CARTESIAN_POINT('Ctrl Pts',(-89.8438679752394,38.4802385548879,114.260522363569));
#50977=CARTESIAN_POINT('Ctrl Pts',(-87.1234235562783,39.254525926676,114.102573840377));
#50978=CARTESIAN_POINT('Ctrl Pts',(-84.9879007301944,37.3998343000056,113.944625317184));
#50979=CARTESIAN_POINT('Ctrl Pts',(-85.373513094407,34.5977561648829,113.786676793992));
#50980=CARTESIAN_POINT('Ctrl Pts',(-87.9306376461546,33.3888505450693,113.628728270799));
#50981=CARTESIAN_POINT('Ctrl Pts',(-90.3408073257951,34.8691953988476,113.470779747607));
#50982=CARTESIAN_POINT('Ctrl Pts',(-90.418794586796,37.6966070699504,113.312831224414));
#50983=CARTESIAN_POINT('Ctrl Pts',(-88.0938907514829,39.3075573880276,113.154882701222));
#50984=CARTESIAN_POINT('Ctrl Pts',(-85.4740154185804,38.2414466945179,112.996934178029));
#50985=CARTESIAN_POINT('Ctrl Pts',(-84.9345298725249,35.4648851309353,112.838985654837));
#50986=CARTESIAN_POINT('Ctrl Pts',(-86.9645692502135,33.4952966216777,112.681037131644));
#50987=CARTESIAN_POINT('Ctrl Pts',(-89.7235585887529,34.118447165762,112.523088608452));
#50988=CARTESIAN_POINT('Ctrl Pts',(-90.7100061657571,36.7693451171343,112.365140085259));
#50989=CARTESIAN_POINT('Ctrl Pts',(-89.029529964603,39.0445019267018,112.207191562067));
#50990=CARTESIAN_POINT('Ctrl Pts',(-86.2057666475039,38.8811021109965,112.049243038874));
#50991=CARTESIAN_POINT('Ctrl Pts',(-84.7989365331946,36.4272953133369,111.891294515682));
#50992=CARTESIAN_POINT('Ctrl Pts',(-86.0845696995146,33.907873528002,111.733345992489));
#50993=CARTESIAN_POINT('Ctrl Pts',(-88.8970216553292,33.6071198630027,111.575397469297));
#50994=CARTESIAN_POINT('Ctrl Pts',(-90.6863277491557,35.7977185193896,111.417448946105));
#50995=CARTESIAN_POINT('Ctrl Pts',(-89.8301785650173,38.4935203194527,111.259500422912));
#50996=CARTESIAN_POINT('Ctrl Pts',(-87.1048185295501,39.250323760202,111.10155189972));
#50997=CARTESIAN_POINT('Ctrl Pts',(-84.9812486988779,37.3819581790018,110.943603376527));
#50998=CARTESIAN_POINT('Ctrl Pts',(-85.3848452529235,34.5824138246471,110.785654853335));
#50999=CARTESIAN_POINT('Ctrl Pts',(-87.9496794711547,33.3899524187512,110.627706330142));
#51000=CARTESIAN_POINT('Ctrl Pts',(-90.3502941734241,34.8857424513509,110.46975780695));
#51001=CARTESIAN_POINT('Ctrl Pts',(-90.4101250213688,37.7135965914931,110.311809283757));
#51002=CARTESIAN_POINT('Ctrl Pts',(-88.0749252032079,39.3095854972364,110.153860760565));
#51003=CARTESIAN_POINT('Ctrl Pts',(-85.4619493755126,38.2266745642004,109.995912237372));
#51004=CARTESIAN_POINT('Ctrl Pts',(-84.9403032443241,35.4467062070136,109.83796371418));
#51005=CARTESIAN_POINT('Ctrl Pts',(-86.9829475057552,33.4901931720481,109.680015190987));
#51006=CARTESIAN_POINT('Ctrl Pts',(-89.7378787031565,34.1310463526011,109.522066667795));
#51007=CARTESIAN_POINT('Ctrl Pts',(-90.7072845669837,36.7882236005902,109.364118144602));
#51008=CARTESIAN_POINT('Ctrl Pts',(-89.0122341608886,39.0525432429309,109.20616962141));
#51009=CARTESIAN_POINT('Ctrl Pts',(-86.1895783879121,38.871015272567,109.048221098218));
#51010=CARTESIAN_POINT('Ctrl Pts',(-84.7985328710269,36.4082261006589,108.890272575025));
#51011=CARTESIAN_POINT('Ctrl Pts',(-86.1003173413752,33.8971106948583,108.732324051833));
#51012=CARTESIAN_POINT('Ctrl Pts',(-88.9146412159036,33.6144232264086,108.57437552864));
#51013=CARTESIAN_POINT('Ctrl Pts',(-90.6898471469939,35.8164632909541,108.416427005448));
#51014=CARTESIAN_POINT('Ctrl Pts',(-89.8164006209573,38.5067174591193,108.258478482255));
#51015=CARTESIAN_POINT('Ctrl Pts',(-87.0862481358614,39.2459949198183,108.100529959063));
#51016=CARTESIAN_POINT('Ctrl Pts',(-84.9746966417824,37.3640547215823,107.94258143587));
#51017=CARTESIAN_POINT('Ctrl Pts',(-85.3963064264104,34.5671137009093,107.784632912678));
#51018=CARTESIAN_POINT('Ctrl Pts',(-87.9686506208259,33.391240008553,107.626684389485));
#51019=CARTESIAN_POINT('Ctrl Pts',(-90.3598045645273,34.9022195493604,107.468735866293));
#51020=CARTESIAN_POINT('Ctrl Pts',(-90.4010792246134,37.7307985779511,107.3107873431));
#51021=CARTESIAN_POINT('Ctrl Pts',(-88.0564969445425,39.3109398404868,107.152838819908));
#51022=CARTESIAN_POINT('Ctrl Pts',(-85.4488474513176,38.2129740762705,106.994890296715));
#51023=CARTESIAN_POINT('Ctrl Pts',(-84.9485678262205,35.4262457574378,106.836941773523));
#51024=CARTESIAN_POINT('Ctrl Pts',(-86.3138051921105,34.137929732014,106.731642758061));
#51025=CARTESIAN_POINT('Ctrl Pts',(-87.1183555905977,33.9228392726483,106.678993250331));
#51026=CARTESIAN_POINT('Ctrl Pts',(-85.71422403823,38.1113513959102,122.10700224989));
#51027=CARTESIAN_POINT('Ctrl Pts',(-85.133186926017,37.4317649329314,122.054352742159));
#51028=CARTESIAN_POINT('Ctrl Pts',(-84.7087437476064,35.4616427623337,121.949053726697));
#51029=CARTESIAN_POINT('Ctrl Pts',(-86.8461024770139,33.3002681757525,121.791105203505));
#51030=CARTESIAN_POINT('Ctrl Pts',(-89.8209931976587,33.9146409087766,121.633156680313));
#51031=CARTESIAN_POINT('Ctrl Pts',(-90.9344609266627,36.7385420763113,121.47520815712));
#51032=CARTESIAN_POINT('Ctrl Pts',(-89.1777651710886,39.2160850505738,121.317259633928));
#51033=CARTESIAN_POINT('Ctrl Pts',(-86.1432524251657,39.09879479537,121.159311110735));
#51034=CARTESIAN_POINT('Ctrl Pts',(-84.5824156215186,36.4940661841728,121.001362587543));
#51035=CARTESIAN_POINT('Ctrl Pts',(-85.9103243921675,33.763016211939,120.84341406435));
#51036=CARTESIAN_POINT('Ctrl Pts',(-88.9230497681442,33.3820534126919,120.685465541158));
#51037=CARTESIAN_POINT('Ctrl Pts',(-90.8890231409496,35.6964642926964,120.527517017965));
#51038=CARTESIAN_POINT('Ctrl Pts',(-90.0257670106906,38.6079016746579,120.369568494773));
#51039=CARTESIAN_POINT('Ctrl Pts',(-87.1159642213932,39.4766252502595,120.21161997158));
#51040=CARTESIAN_POINT('Ctrl Pts',(-84.797847009812,37.5150036725937,120.053671448388));
#51041=CARTESIAN_POINT('Ctrl Pts',(-85.1731805116345,34.501572808019,119.895722925195));
#51042=CARTESIAN_POINT('Ctrl Pts',(-87.9016618578588,33.168522058285,119.737774402003));
#51043=CARTESIAN_POINT('Ctrl Pts',(-90.5094597022168,34.7244863973195,119.57982587881));
#51044=CARTESIAN_POINT('Ctrl Pts',(-90.6321631941225,37.7587210584574,119.421877355618));
#51045=CARTESIAN_POINT('Ctrl Pts',(-88.1585207401243,39.5201773786853,119.263928832425));
#51046=CARTESIAN_POINT('Ctrl Pts',(-85.3313087544768,38.4117966684516,119.105980309233));
#51047=CARTESIAN_POINT('Ctrl Pts',(-84.7138743424387,35.4385139185105,118.94803178604));
#51048=CARTESIAN_POINT('Ctrl Pts',(-86.8660265149425,33.2961142133687,118.790083262848));
#51049=CARTESIAN_POINT('Ctrl Pts',(-89.8364743480595,33.9270461864123,118.632134739655));
#51050=CARTESIAN_POINT('Ctrl Pts',(-90.9320031354711,36.7592630168832,118.474186216463));
#51051=CARTESIAN_POINT('Ctrl Pts',(-89.1593302437182,39.2248798375797,118.316237693271));
#51052=CARTESIAN_POINT('Ctrl Pts',(-86.1256842707891,39.088396867951,118.158289170078));
#51053=CARTESIAN_POINT('Ctrl Pts',(-84.5815797559506,36.4735590644364,118.000340646886));
#51054=CARTESIAN_POINT('Ctrl Pts',(-85.9270093010962,33.7511603373601,117.842392123693));
#51055=CARTESIAN_POINT('Ctrl Pts',(-88.942112856981,33.3895168142684,117.684443600501));
#51056=CARTESIAN_POINT('Ctrl Pts',(-90.8931877297387,35.7165196787937,117.526495077308));
#51057=CARTESIAN_POINT('Ctrl Pts',(-90.0112536714875,38.6223462061979,117.368546554116));
#51058=CARTESIAN_POINT('Ctrl Pts',(-87.095933470038,39.4723718608345,117.210598030923));
#51059=CARTESIAN_POINT('Ctrl Pts',(-84.7904592865855,37.4959042339906,117.052649507731));
#51060=CARTESIAN_POINT('Ctrl Pts',(-85.1851344454402,34.4849464113876,116.894700984538));
#51061=CARTESIAN_POINT('Ctrl Pts',(-87.9221189835702,33.1694422766331,116.736752461346));
#51062=CARTESIAN_POINT('Ctrl Pts',(-90.5198722618751,34.7421194194613,116.578803938153));
#51063=CARTESIAN_POINT('Ctrl Pts',(-90.6230903900105,37.7770793052821,116.420855414961));
#51064=CARTESIAN_POINT('Ctrl Pts',(-88.1381886304332,39.5226161097546,116.262906891769));
#51065=CARTESIAN_POINT('Ctrl Pts',(-85.3181518336815,38.3961047003655,116.104958368576));
#51066=CARTESIAN_POINT('Ctrl Pts',(-84.7198215958278,35.4189187107123,115.947009845384));
#51067=CARTESIAN_POINT('Ctrl Pts',(-86.8856857461426,33.2903821305947,115.789061322191));
#51068=CARTESIAN_POINT('Ctrl Pts',(-89.8520211313158,33.9403743406915,115.631112798999));
#51069=CARTESIAN_POINT('Ctrl Pts',(-90.9293416746237,36.7795671727275,115.473164275806));
#51070=CARTESIAN_POINT('Ctrl Pts',(-89.1408736046719,39.2337508360423,115.315215752614));
#51071=CARTESIAN_POINT('Ctrl Pts',(-86.1081665266886,39.0777916437303,115.157267229421));
#51072=CARTESIAN_POINT('Ctrl Pts',(-84.5808837126644,36.4530930521766,114.999318706229));
#51073=CARTESIAN_POINT('Ctrl Pts',(-85.9437660398683,33.7393894477435,114.841370183036));
#51074=CARTESIAN_POINT('Ctrl Pts',(-88.9611295524168,33.3971133550064,114.683421659844));
#51075=CARTESIAN_POINT('Ctrl Pts',(-90.8972225224448,35.7365960973931,114.525473136651));
#51076=CARTESIAN_POINT('Ctrl Pts',(-89.9966483376343,38.6366998245329,114.367524613459));
#51077=CARTESIAN_POINT('Ctrl Pts',(-87.0759302216267,39.4679886896959,114.209576090266));
#51078=CARTESIAN_POINT('Ctrl Pts',(-84.7831944605806,37.4767583613467,114.051627567074));
#51079=CARTESIAN_POINT('Ctrl Pts',(-85.1971948386299,34.4683968176668,113.893679043881));
#51080=CARTESIAN_POINT('Ctrl Pts',(-87.94256980425,33.1704939751301,113.735730520689));
#51081=CARTESIAN_POINT('Ctrl Pts',(-90.530171372918,34.7598188671343,113.577781997496));
#51082=CARTESIAN_POINT('Ctrl Pts',(-90.6138999006673,37.7953789512305,113.419833474304));
#51083=CARTESIAN_POINT('Ctrl Pts',(-88.1178412778752,39.5249242215556,113.261884951112));
#51084=CARTESIAN_POINT('Ctrl Pts',(-85.3050959436363,38.3803285832472,113.103936427919));
#51085=CARTESIAN_POINT('Ctrl Pts',(-84.7258945467225,35.3993620902569,112.945987904727));
#51086=CARTESIAN_POINT('Ctrl Pts',(-86.9053813781013,33.2847763997814,112.788039381534));
#51087=CARTESIAN_POINT('Ctrl Pts',(-89.8674820138573,33.9538020451582,112.630090858342));
#51088=CARTESIAN_POINT('Ctrl Pts',(-90.9265498957688,36.7998538212194,112.472142335149));
#51089=CARTESIAN_POINT('Ctrl Pts',(-89.1223603854006,39.2425031413621,112.314193811957));
#51090=CARTESIAN_POINT('Ctrl Pts',(-86.0907172398595,39.0670741568343,112.156245288764));
#51091=CARTESIAN_POINT('Ctrl Pts',(-84.5803190959501,36.4326229924751,111.998296765572));
#51092=CARTESIAN_POINT('Ctrl Pts',(-85.9605980140705,33.7277263958002,111.840348242379));
#51093=CARTESIAN_POINT('Ctrl Pts',(-88.9800970784496,33.4048318453007,111.682399719187));
#51094=CARTESIAN_POINT('Ctrl Pts',(-90.9011283213218,35.7566980095261,111.524451195994));
#51095=CARTESIAN_POINT('Ctrl Pts',(-89.9819511403106,38.6509593661381,111.366502672802));
#51096=CARTESIAN_POINT('Ctrl Pts',(-87.0559555299054,39.4634771680998,111.208554149609));
#51097=CARTESIAN_POINT('Ctrl Pts',(-84.7760527199742,37.4575662359367,111.050605626417));
#51098=CARTESIAN_POINT('Ctrl Pts',(-85.2093612480747,34.4519250049159,110.892657103225));
#51099=CARTESIAN_POINT('Ctrl Pts',(-87.9630134504616,33.1716769665567,110.734708580032));
#51100=CARTESIAN_POINT('Ctrl Pts',(-90.5403566233648,34.7775840806693,110.57676005684));
#51101=CARTESIAN_POINT('Ctrl Pts',(-90.6045920991094,37.8136192074939,110.418811533647));
#51102=CARTESIAN_POINT('Ctrl Pts',(-88.0974795237292,39.5271016361228,110.260863010455));
#51103=CARTESIAN_POINT('Ctrl Pts',(-85.2921416225221,38.3644689581323,110.102914487262));
#51104=CARTESIAN_POINT('Ctrl Pts',(-84.7320929426489,35.3798448701815,109.94496596407));
#51105=CARTESIAN_POINT('Ctrl Pts',(-86.9251126041933,33.2792972443598,109.787017440877));
#51106=CARTESIAN_POINT('Ctrl Pts',(-89.8828563465474,33.9673287590258,109.629068917685));
#51107=CARTESIAN_POINT('Ctrl Pts',(-90.9236279383172,36.8201221010078,109.471120394492));
#51108=CARTESIAN_POINT('Ctrl Pts',(-89.1037912990822,39.2511364432679,109.3131718713));
#51109=CARTESIAN_POINT('Ctrl Pts',(-86.0733372328554,39.0562447454598,109.155223348107));
#51110=CARTESIAN_POINT('Ctrl Pts',(-84.5798857169778,36.4121499423593,108.997274824915));
#51111=CARTESIAN_POINT('Ctrl Pts',(-85.9775049659444,33.7161712243276,108.839326301723));
#51112=CARTESIAN_POINT('Ctrl Pts',(-88.9990137559626,33.412672867767,108.68137777853));
#51113=CARTESIAN_POINT('Ctrl Pts',(-90.9049068102157,35.7768227338202,108.523429255338));
#51114=CARTESIAN_POINT('Ctrl Pts',(-89.9671588914646,38.6651280529288,108.365480732145));
#51115=CARTESIAN_POINT('Ctrl Pts',(-87.0360180208389,39.4588296471133,108.207532208953));
#51116=CARTESIAN_POINT('Ctrl Pts',(-84.7690183134918,37.4383447616585,108.04958368576));
#51117=CARTESIAN_POINT('Ctrl Pts',(-85.2216661703148,34.4354985165574,107.891635162568));
#51118=CARTESIAN_POINT('Ctrl Pts',(-87.9833812183675,33.1730593461539,107.733686639375));
#51119=CARTESIAN_POINT('Ctrl Pts',(-90.5505671505095,34.7952741898001,107.575738116183));
#51120=CARTESIAN_POINT('Ctrl Pts',(-90.5948803688225,37.8320875699162,107.41778959299));
#51121=CARTESIAN_POINT('Ctrl Pts',(-88.0776946133833,39.5285556834245,107.259841069798));
#51122=CARTESIAN_POINT('Ctrl Pts',(-85.2780751607762,38.3497598675822,107.101892546605));
#51123=CARTESIAN_POINT('Ctrl Pts',(-84.7409659465956,35.3578781630799,106.943944023413));
#51124=CARTESIAN_POINT('Ctrl Pts',(-86.2067093668298,33.9747188791143,106.838645007951));
#51125=CARTESIAN_POINT('Ctrl Pts',(-87.0704891624118,33.7437938887448,106.78599550022));
#51126=CARTESIAN_POINT('Ctrl Pts',(-85.573358484553,38.2317895137621,122.21400449978));
#51127=CARTESIAN_POINT('Ctrl Pts',(-84.9524796464486,37.505603794026,122.161354992049));
#51128=CARTESIAN_POINT('Ctrl Pts',(-84.4989323911808,35.4003903085301,122.056055976587));
#51129=CARTESIAN_POINT('Ctrl Pts',(-86.782849849521,33.0908102252307,121.898107453395));
#51130=CARTESIAN_POINT('Ctrl Pts',(-89.9617288837476,33.7473105083025,121.740158930202));
#51131=CARTESIAN_POINT('Ctrl Pts',(-91.1515471162143,36.764846632876,121.58221040701));
#51132=CARTESIAN_POINT('Ctrl Pts',(-89.2743946990997,39.4122747762438,121.424261883817));
#51133=CARTESIAN_POINT('Ctrl Pts',(-86.0318053561822,39.2869419259985,121.266313360625));
#51134=CARTESIAN_POINT('Ctrl Pts',(-84.3639419430722,36.5036070241402,121.108364837432));
#51135=CARTESIAN_POINT('Ctrl Pts',(-85.7829054435086,33.5852889031044,120.95041631424));
#51136=CARTESIAN_POINT('Ctrl Pts',(-89.0022134561064,33.1782034774305,120.792467791047));
#51137=CARTESIAN_POINT('Ctrl Pts',(-91.1029936606662,35.6513135557185,120.634519267855));
#51138=CARTESIAN_POINT('Ctrl Pts',(-90.1805440410535,38.7623882546154,120.476570744662));
#51139=CARTESIAN_POINT('Ctrl Pts',(-87.0712160188709,39.6906802224024,120.31862222147));
#51140=CARTESIAN_POINT('Ctrl Pts',(-84.5941454657791,37.5945502156581,120.160673698277));
#51141=CARTESIAN_POINT('Ctrl Pts',(-84.9952155929964,34.3744883390956,120.002725175085));
#51142=CARTESIAN_POINT('Ctrl Pts',(-87.9107889572882,32.9500302739701,119.844776651893));
#51143=CARTESIAN_POINT('Ctrl Pts',(-90.6974035496838,34.6126871174756,119.6868281287));
#51144=CARTESIAN_POINT('Ctrl Pts',(-90.8285208223751,37.8549793073293,119.528879605508));
#51145=CARTESIAN_POINT('Ctrl Pts',(-88.1852606580207,39.7372187211068,119.370931082315));
#51146=CARTESIAN_POINT('Ctrl Pts',(-85.1641866924731,38.5528363243849,119.212982559123));
#51147=CARTESIAN_POINT('Ctrl Pts',(-84.5044147909987,35.3756755194439,119.05503403593));
#51148=CARTESIAN_POINT('Ctrl Pts',(-86.8041400791112,33.0863714255669,118.897085512738));
#51149=CARTESIAN_POINT('Ctrl Pts',(-89.9782715769274,33.7605664160628,118.739136989545));
#51150=CARTESIAN_POINT('Ctrl Pts',(-91.1489207942337,36.786988408739,118.581188466353));
#51151=CARTESIAN_POINT('Ctrl Pts',(-89.2546956884071,39.4216726219628,118.42323994316));
#51152=CARTESIAN_POINT('Ctrl Pts',(-86.013032553124,39.2758310124976,118.265291419968));
#51153=CARTESIAN_POINT('Ctrl Pts',(-84.3630487621863,36.4816937308115,118.107342896775));
#51154=CARTESIAN_POINT('Ctrl Pts',(-85.8007344369615,33.5726200709789,117.949394373583));
#51155=CARTESIAN_POINT('Ctrl Pts',(-89.0225837013092,33.1861786445957,117.79144585039));
#51156=CARTESIAN_POINT('Ctrl Pts',(-91.1074438153881,35.6727441400239,117.633497327198));
#51157=CARTESIAN_POINT('Ctrl Pts',(-90.1650355219039,38.7778232479593,117.475548804006));
#51158=CARTESIAN_POINT('Ctrl Pts',(-87.0498117585123,39.6861351779832,117.317600280813));
#51159=CARTESIAN_POINT('Ctrl Pts',(-84.5862511662297,37.574141128185,117.159651757621));
#51160=CARTESIAN_POINT('Ctrl Pts',(-85.0079892082717,34.3567218701293,117.001703234428));
#51161=CARTESIAN_POINT('Ctrl Pts',(-87.9326488285006,32.9510135917079,116.843754711236));
#51162=CARTESIAN_POINT('Ctrl Pts',(-90.708530098757,34.6315292362828,116.685806188043));
#51163=CARTESIAN_POINT('Ctrl Pts',(-90.8188258959115,37.8745963794897,116.527857664851));
#51164=CARTESIAN_POINT('Ctrl Pts',(-88.1635343751796,39.7398246760122,116.369909141658));
#51165=CARTESIAN_POINT('Ctrl Pts',(-85.1501276013673,38.5360683577472,116.211960618466));
#51166=CARTESIAN_POINT('Ctrl Pts',(-84.5107698476665,35.3547366678723,116.054012095273));
#51167=CARTESIAN_POINT('Ctrl Pts',(-86.8251473441704,33.0802462937674,115.896063572081));
#51168=CARTESIAN_POINT('Ctrl Pts',(-89.9948844034088,33.7748084821357,115.738115048888));
#51169=CARTESIAN_POINT('Ctrl Pts',(-91.1460768369648,36.8086848209377,115.580166525696));
#51170=CARTESIAN_POINT('Ctrl Pts',(-89.2349734772688,39.4311519049595,115.422218002504));
#51171=CARTESIAN_POINT('Ctrl Pts',(-85.9943136169755,39.2644985878494,115.264269479311));
#51172=CARTESIAN_POINT('Ctrl Pts',(-84.3623049911988,36.4598243636998,115.106320956119));
#51173=CARTESIAN_POINT('Ctrl Pts',(-85.8186401856314,33.5600420512363,114.948372432926));
#51174=CARTESIAN_POINT('Ctrl Pts',(-89.0429043719145,33.1942960802773,114.790423909734));
#51175=CARTESIAN_POINT('Ctrl Pts',(-91.1117552739073,35.6941971990304,114.632475386541));
#51176=CARTESIAN_POINT('Ctrl Pts',(-90.1494287000289,38.7931610941779,114.474526863349));
#51177=CARTESIAN_POINT('Ctrl Pts',(-87.0284368869753,39.6814514527158,114.316578340156));
#51178=CARTESIAN_POINT('Ctrl Pts',(-84.5784881909668,37.5536824226879,114.158629816964));
#51179=CARTESIAN_POINT('Ctrl Pts',(-85.020876582853,34.3390374704508,114.000681293771));
#51180=CARTESIAN_POINT('Ctrl Pts',(-87.9545019623453,32.952137405191,113.842732770579));
#51181=CARTESIAN_POINT('Ctrl Pts',(-90.7195354200411,34.650442335421,113.684784247386));
#51182=CARTESIAN_POINT('Ctrl Pts',(-90.8090052145385,37.8941508325107,113.526835724194));
#51183=CARTESIAN_POINT('Ctrl Pts',(-88.1417918042676,39.7422910550834,113.368887201001));
#51184=CARTESIAN_POINT('Ctrl Pts',(-85.1361764686922,38.5192104719765,113.210938677809));
#51185=CARTESIAN_POINT('Ctrl Pts',(-84.5172592209201,35.3338390495785,113.052990154617));
#51186=CARTESIAN_POINT('Ctrl Pts',(-86.846193505989,33.0742561778852,112.895041631424));
#51187=CARTESIAN_POINT('Ctrl Pts',(-90.0114054389617,33.7891569245543,112.737093108232));
#51188=CARTESIAN_POINT('Ctrl Pts',(-91.1430936257806,36.8303625253044,112.579144585039));
#51189=CARTESIAN_POINT('Ctrl Pts',(-89.2151908061982,39.4405043560225,112.421196061847));
#51190=CARTESIAN_POINT('Ctrl Pts',(-85.975667832215,39.2530462026721,112.263247538654));
#51191=CARTESIAN_POINT('Ctrl Pts',(-84.3617016587055,36.4379506716133,112.105299015462));
#51192=CARTESIAN_POINT('Ctrl Pts',(-85.8366263286264,33.5475792635982,111.947350492269));
#51193=CARTESIAN_POINT('Ctrl Pts',(-89.06317250157,33.2025438275986,111.789401969077));
#51194=CARTESIAN_POINT('Ctrl Pts',(-91.115928893488,35.7156774996627,111.631453445884));
#51195=CARTESIAN_POINT('Ctrl Pts',(-90.133723715604,38.8083984128235,111.473504922692));
#51196=CARTESIAN_POINT('Ctrl Pts',(-87.0070925302608,39.6766305759976,111.315556399499));
#51197=CARTESIAN_POINT('Ctrl Pts',(-84.5708567410705,37.5331742928717,111.157607876307));
#51198=CARTESIAN_POINT('Ctrl Pts',(-85.0338772432258,34.3214361851846,110.999659353114));
#51199=CARTESIAN_POINT('Ctrl Pts',(-87.9763474297686,32.9534015143623,110.841710829922));
#51200=CARTESIAN_POINT('Ctrl Pts',(-90.7304190733056,34.6694257099876,110.683762306729));
#51201=CARTESIAN_POINT('Ctrl Pts',(-90.7990591768499,37.9136418234947,110.525813783537));
#51202=CARTESIAN_POINT('Ctrl Pts',(-88.1200338442505,39.7446177750092,110.367865260345));
#51203=CARTESIAN_POINT('Ctrl Pts',(-85.1223338695316,38.5022633520643,110.209916737152));
#51204=CARTESIAN_POINT('Ctrl Pts',(-84.5238826409736,35.3129835333494,110.05196821396));
#51205=CARTESIAN_POINT('Ctrl Pts',(-86.8672777026315,33.0684013166716,109.894019690767));
#51206=CARTESIAN_POINT('Ctrl Pts',(-90.027833989938,33.8036111654504,109.736071167575));
#51207=CARTESIAN_POINT('Ctrl Pts',(-91.1399713096509,36.8520206014254,109.578122644382));
#51208=CARTESIAN_POINT('Ctrl Pts',(-89.1953484372759,39.449729643605,109.42017412119));
#51209=CARTESIAN_POINT('Ctrl Pts',(-85.9570960777986,39.2414742183526,109.262225597997));
#51210=CARTESIAN_POINT('Ctrl Pts',(-84.3612385629288,36.4160737840598,109.104277074805));
#51211=CARTESIAN_POINT('Ctrl Pts',(-85.8546925905136,33.535231753797,108.946328551612));
#51212=CARTESIAN_POINT('Ctrl Pts',(-89.0833862960218,33.2109225091254,108.78838002842));
#51213=CARTESIAN_POINT('Ctrl Pts',(-91.1199664734373,35.7371821766864,108.630431505227));
#51214=CARTESIAN_POINT('Ctrl Pts',(-90.117917161972,38.8235386467383,108.472482982035));
#51215=CARTESIAN_POINT('Ctrl Pts',(-86.9857879058164,39.6716643744082,108.314534458842));
#51216=CARTESIAN_POINT('Ctrl Pts',(-84.5633399852011,37.5126348017347,108.15658593565));
#51217=CARTESIAN_POINT('Ctrl Pts',(-85.0470259142193,34.3038833322054,107.998637412457));
#51218=CARTESIAN_POINT('Ctrl Pts',(-87.9981118159091,32.9548786837549,107.840688889265));
#51219=CARTESIAN_POINT('Ctrl Pts',(-90.7413297364918,34.6883288302397,107.682740366073));
#51220=CARTESIAN_POINT('Ctrl Pts',(-90.7886815130315,37.9333765618813,107.52479184288));
#51221=CARTESIAN_POINT('Ctrl Pts',(-88.0988922822239,39.7461715263621,107.366843319688));
#51222=CARTESIAN_POINT('Ctrl Pts',(-85.1073028702349,38.486545658894,107.208894796495));
#51223=CARTESIAN_POINT('Ctrl Pts',(-84.5333640669706,35.2895105687219,107.050946273303));
#51224=CARTESIAN_POINT('Ctrl Pts',(-86.099613541549,33.8115080262147,106.945647257841));
#51225=CARTESIAN_POINT('Ctrl Pts',(-87.0226227342259,33.5647485048412,106.89299775011));
#51226=CARTESIAN_POINT('Ctrl Pts',(-85.4324929308759,38.352227631614,122.321006749669));
#51227=CARTESIAN_POINT('Ctrl Pts',(-84.7717723668801,37.5794426551206,122.268357241939));
#51228=CARTESIAN_POINT('Ctrl Pts',(-84.2891210347552,35.3391378547265,122.163058226477));
#51229=CARTESIAN_POINT('Ctrl Pts',(-86.719597222028,32.881352274709,122.005109703284));
#51230=CARTESIAN_POINT('Ctrl Pts',(-90.1024645698366,33.5799801078284,121.847161180092));
#51231=CARTESIAN_POINT('Ctrl Pts',(-91.3686333057658,36.7911511894407,121.6892126569));
#51232=CARTESIAN_POINT('Ctrl Pts',(-89.371024227111,39.6084645019137,121.531264133707));
#51233=CARTESIAN_POINT('Ctrl Pts',(-85.9203582871986,39.4750890566271,121.373315610515));
#51234=CARTESIAN_POINT('Ctrl Pts',(-84.1454682646258,36.5131478641077,121.215367087322));
#51235=CARTESIAN_POINT('Ctrl Pts',(-85.6554864948497,33.4075615942697,121.05741856413));
#51236=CARTESIAN_POINT('Ctrl Pts',(-89.0813771440687,32.974353542169,120.899470040937));
#51237=CARTESIAN_POINT('Ctrl Pts',(-91.3169641803828,35.6061628187407,120.741521517745));
#51238=CARTESIAN_POINT('Ctrl Pts',(-90.3353210714164,38.916874834573,120.583572994552));
#51239=CARTESIAN_POINT('Ctrl Pts',(-87.0264678163487,39.9047351945452,120.42562447136));
#51240=CARTESIAN_POINT('Ctrl Pts',(-84.3904439217461,37.6740967587225,120.267675948167));
#51241=CARTESIAN_POINT('Ctrl Pts',(-84.8172506743583,34.2474038701722,120.109727424975));
#51242=CARTESIAN_POINT('Ctrl Pts',(-87.9199160567175,32.7315384896552,119.951778901782));
#51243=CARTESIAN_POINT('Ctrl Pts',(-90.8853473971509,34.5008878376316,119.79383037859));
#51244=CARTESIAN_POINT('Ctrl Pts',(-91.0248784506275,37.9512375562013,119.635881855397));
#51245=CARTESIAN_POINT('Ctrl Pts',(-88.2120005759172,39.9542600635284,119.477933332205));
#51246=CARTESIAN_POINT('Ctrl Pts',(-84.9970646304694,38.6938759803182,119.319984809012));
#51247=CARTESIAN_POINT('Ctrl Pts',(-84.2949552395589,35.3128371203772,119.16203628582));
#51248=CARTESIAN_POINT('Ctrl Pts',(-86.7422536432798,32.8766286377651,119.004087762628));
#51249=CARTESIAN_POINT('Ctrl Pts',(-90.1200688057952,33.5940866457133,118.846139239435));
#51250=CARTESIAN_POINT('Ctrl Pts',(-91.3658384529962,36.8147138005949,118.688190716243));
#51251=CARTESIAN_POINT('Ctrl Pts',(-89.3500611330962,39.6184654063458,118.53024219305));
#51252=CARTESIAN_POINT('Ctrl Pts',(-85.9003808354589,39.4632651570443,118.372293669858));
#51253=CARTESIAN_POINT('Ctrl Pts',(-84.144517768422,36.4898283971866,118.214345146665));
#51254=CARTESIAN_POINT('Ctrl Pts',(-85.6744595728268,33.3940798045978,118.056396623473));
#51255=CARTESIAN_POINT('Ctrl Pts',(-89.1030545456374,32.9828404749231,117.89844810028));
#51256=CARTESIAN_POINT('Ctrl Pts',(-91.3216999010375,35.6289686012542,117.740499577088));
#51257=CARTESIAN_POINT('Ctrl Pts',(-90.3188173723202,38.9333002897206,117.582551053895));
#51258=CARTESIAN_POINT('Ctrl Pts',(-87.0036900469868,39.8998984951319,117.424602530703));
#51259=CARTESIAN_POINT('Ctrl Pts',(-84.3820430458739,37.6523780223793,117.26665400751));
#51260=CARTESIAN_POINT('Ctrl Pts',(-84.8308439711031,34.228497328871,117.108705484318));
#51261=CARTESIAN_POINT('Ctrl Pts',(-87.9431786734311,32.7325849067827,116.950756961125));
#51262=CARTESIAN_POINT('Ctrl Pts',(-90.8971879356389,34.5209390531042,116.792808437933));
#51263=CARTESIAN_POINT('Ctrl Pts',(-91.0145614018127,37.9721134536974,116.634859914741));
#51264=CARTESIAN_POINT('Ctrl Pts',(-88.1888801199258,39.9570332422698,116.476911391548));
#51265=CARTESIAN_POINT('Ctrl Pts',(-84.9821033690532,38.6760320151288,116.318962868356));
#51266=CARTESIAN_POINT('Ctrl Pts',(-84.3017180995052,35.2905546250324,116.161014345163));
#51267=CARTESIAN_POINT('Ctrl Pts',(-86.7646089421984,32.8701104569402,116.003065821971));
#51268=CARTESIAN_POINT('Ctrl Pts',(-90.1377476755016,33.6092426235799,115.845117298778));
#51269=CARTESIAN_POINT('Ctrl Pts',(-91.3628119993062,36.8378024691479,115.687168775586));
#51270=CARTESIAN_POINT('Ctrl Pts',(-89.3290733498657,39.6285529738767,115.529220252393));
#51271=CARTESIAN_POINT('Ctrl Pts',(-85.8804607072626,39.4512055319686,115.371271729201));
#51272=CARTESIAN_POINT('Ctrl Pts',(-84.143726269733,36.466555675223,115.213323206008));
#51273=CARTESIAN_POINT('Ctrl Pts',(-85.6935143313946,33.3806946547291,115.055374682816));
#51274=CARTESIAN_POINT('Ctrl Pts',(-89.1246791914122,32.9914788055483,114.897426159624));
#51275=CARTESIAN_POINT('Ctrl Pts',(-91.3262880253696,35.6517983006678,114.739477636431));
#51276=CARTESIAN_POINT('Ctrl Pts',(-90.3022090624238,38.9496223638228,114.581529113239));
#51277=CARTESIAN_POINT('Ctrl Pts',(-86.9809435523238,39.8949142157357,114.423580590046));
#51278=CARTESIAN_POINT('Ctrl Pts',(-84.373781921353,37.630606484029,114.265632066854));
#51279=CARTESIAN_POINT('Ctrl Pts',(-84.8445583270759,34.2096781232347,114.107683543661));
#51280=CARTESIAN_POINT('Ctrl Pts',(-87.9664341204409,32.7337808352518,113.949735020469));
#51281=CARTESIAN_POINT('Ctrl Pts',(-90.9088994671639,34.5410658037077,113.791786497276));
#51282=CARTESIAN_POINT('Ctrl Pts',(-91.0041105284097,37.9929227137908,113.633837974084));
#51283=CARTESIAN_POINT('Ctrl Pts',(-88.16574233066,39.9596578886113,113.475889450891));
#51284=CARTESIAN_POINT('Ctrl Pts',(-84.9672569937481,38.6580923607057,113.317940927699));
#51285=CARTESIAN_POINT('Ctrl Pts',(-84.3086238951178,35.2683160089,113.159992404506));
#51286=CARTESIAN_POINT('Ctrl Pts',(-86.7870056338769,32.863735955989,113.002043881314));
#51287=CARTESIAN_POINT('Ctrl Pts',(-90.155328864066,33.6245118039505,112.844095358121));
#51288=CARTESIAN_POINT('Ctrl Pts',(-91.3596373557926,36.8608712293895,112.686146834929));
#51289=CARTESIAN_POINT('Ctrl Pts',(-89.3080212269955,39.6385055706828,112.528198311736));
#51290=CARTESIAN_POINT('Ctrl Pts',(-85.8606184245708,39.4390182485099,112.370249788544));
#51291=CARTESIAN_POINT('Ctrl Pts',(-84.1430842214608,36.4432783507515,112.212301265351));
#51292=CARTESIAN_POINT('Ctrl Pts',(-85.7126546431824,33.3674321313963,112.054352742159));
#51293=CARTESIAN_POINT('Ctrl Pts',(-89.1462479246903,33.0002558098966,111.896404218967));
#51294=CARTESIAN_POINT('Ctrl Pts',(-91.330729465654,35.6746569897993,111.738455695774));
#51295=CARTESIAN_POINT('Ctrl Pts',(-90.2854962908975,38.9658374595089,111.580507172582));
#51296=CARTESIAN_POINT('Ctrl Pts',(-86.9582295306161,39.8897839838954,111.422558649389));
#51297=CARTESIAN_POINT('Ctrl Pts',(-84.3656607621669,37.6087823498066,111.264610126197));
#51298=CARTESIAN_POINT('Ctrl Pts',(-84.858393238377,34.1909473654533,111.106661603004));
#51299=CARTESIAN_POINT('Ctrl Pts',(-87.9896814090755,32.7351260621679,110.948713079812));
#51300=CARTESIAN_POINT('Ctrl Pts',(-90.9204815232464,34.561267339306,110.790764556619));
#51301=CARTESIAN_POINT('Ctrl Pts',(-90.9935262545903,38.0136644394956,110.632816033427));
#51302=CARTESIAN_POINT('Ctrl Pts',(-88.1425881647719,39.9621339138956,110.474867510234));
#51303=CARTESIAN_POINT('Ctrl Pts',(-84.952526116541,38.6400577459963,110.316918987042));
#51304=CARTESIAN_POINT('Ctrl Pts',(-84.3156723392984,35.2461221965173,110.158970463849));
#51305=CARTESIAN_POINT('Ctrl Pts',(-86.8094428010696,32.8575053889834,110.001021940657));
#51306=CARTESIAN_POINT('Ctrl Pts',(-90.1728116333289,33.6398935718751,109.843073417464));
#51307=CARTESIAN_POINT('Ctrl Pts',(-91.3563146809844,36.883919101843,109.685124894272));
#51308=CARTESIAN_POINT('Ctrl Pts',(-89.2869055754696,39.648322843942,109.52717637108));
#51309=CARTESIAN_POINT('Ctrl Pts',(-85.8408549227417,39.4267036912455,109.369227847887));
#51310=CARTESIAN_POINT('Ctrl Pts',(-84.1425914088798,36.4199976257601,109.211279324695));
#51311=CARTESIAN_POINT('Ctrl Pts',(-85.7318802150827,33.3542922832663,109.053330801502));
#51312=CARTESIAN_POINT('Ctrl Pts',(-89.1677588360808,33.0091721504837,108.89538227831));
#51313=CARTESIAN_POINT('Ctrl Pts',(-91.3350261366591,35.6975416195525,108.737433755117));
#51314=CARTESIAN_POINT('Ctrl Pts',(-90.2686754324792,38.9819492405478,108.579485231925));
#51315=CARTESIAN_POINT('Ctrl Pts',(-86.9355577907939,39.8844991017031,108.421536708732));
#51316=CARTESIAN_POINT('Ctrl Pts',(-84.3576616569105,37.5869248418109,108.26358818554));
#51317=CARTESIAN_POINT('Ctrl Pts',(-84.8723856581236,34.1722681478534,108.105639662347));
#51318=CARTESIAN_POINT('Ctrl Pts',(-88.0128424134507,32.7366980213559,107.947691139155));
#51319=CARTESIAN_POINT('Ctrl Pts',(-90.932092322474,34.5813834706793,107.789742615963));
#51320=CARTESIAN_POINT('Ctrl Pts',(-90.9824826572406,38.0346655538465,107.63179409277));
#51321=CARTESIAN_POINT('Ctrl Pts',(-88.1200899510646,39.9637873692998,107.473845569578));
#51322=CARTESIAN_POINT('Ctrl Pts',(-84.9365305796935,38.6233314502058,107.315897046385));
#51323=CARTESIAN_POINT('Ctrl Pts',(-84.3257621873457,35.2211429743639,107.157948523192));
#51324=CARTESIAN_POINT('Ctrl Pts',(-85.9925177162683,33.6482971733151,107.052649507731));
#51325=CARTESIAN_POINT('Ctrl Pts',(-86.97475630604,33.3857031209377,107.));
#51326=CARTESIAN_POINT('Ctrl Pts',(-85.855089591907,37.9909132780583,122.));
#51327=CARTESIAN_POINT('Ctrl Pts',(-85.7934813679502,37.9330166755841,122.));
#51328=CARTESIAN_POINT('Ctrl Pts',(-85.7352422962271,37.8719693152205,122.));
#51329=CARTESIAN_POINT('Ctrl Pts',(-85.6803699910001,37.8081560154705,122.));
#51330=CARTESIAN_POINT('Ctrl Pts',(-85.624044758381,37.7426530456618,122.));
#51331=CARTESIAN_POINT('Ctrl Pts',(-85.5712665086079,37.6742352905882,122.));
#51332=CARTESIAN_POINT('Ctrl Pts',(-85.522058169157,37.6032704024903,122.));
#51333=CARTESIAN_POINT('Ctrl Pts',(-85.471500272293,37.530359275363,122.));
#51334=CARTESIAN_POINT('Ctrl Pts',(-85.4247102505921,37.4547588307541,122.));
#51335=CARTESIAN_POINT('Ctrl Pts',(-85.3817470379049,37.3768248282257,122.));
#51336=CARTESIAN_POINT('Ctrl Pts',(-85.3628370824531,37.3425227259429,122.));
#51337=CARTESIAN_POINT('Ctrl Pts',(-85.3446689632654,37.3077680551632,122.));
#51338=CARTESIAN_POINT('Ctrl Pts',(-85.327250130523,37.2725890732149,122.));
#51339=CARTESIAN_POINT('Ctrl Pts',(-85.3173192863124,37.2525327930737,122.));
#51340=CARTESIAN_POINT('Ctrl Pts',(-85.3076320170822,37.2323385748829,122.));
#51341=CARTESIAN_POINT('Ctrl Pts',(-85.2981899377649,37.2120115066752,122.));
#51342=CARTESIAN_POINT('Ctrl Pts',(-85.2896843470291,37.1937005269402,122.));
#51343=CARTESIAN_POINT('Ctrl Pts',(-85.2813753465996,37.1752760152876,122.));
#51344=CARTESIAN_POINT('Ctrl Pts',(-85.2732777774911,37.1567734456981,122.));
#51345=CARTESIAN_POINT('Ctrl Pts',(-85.2367161205784,37.0732317565482,122.));
#51346=CARTESIAN_POINT('Ctrl Pts',(-85.2044146446107,36.9880065244174,122.));
#51347=CARTESIAN_POINT('Ctrl Pts',(-85.1763983858018,36.9014965265309,122.));
#51348=CARTESIAN_POINT('Ctrl Pts',(-85.1479190352312,36.8135565708614,122.));
#51349=CARTESIAN_POINT('Ctrl Pts',(-85.1238672433657,36.7242882705842,122.));
#51350=CARTESIAN_POINT('Ctrl Pts',(-85.1043083835495,36.6340733818492,122.));
#51351=CARTESIAN_POINT('Ctrl Pts',(-85.0853398921155,36.5465815566475,122.));
#51352=CARTESIAN_POINT('Ctrl Pts',(-85.0705970385735,36.4581985072518,122.));
#51353=CARTESIAN_POINT('Ctrl Pts',(-85.0601801960536,36.3692505885246,122.));
#51354=CARTESIAN_POINT('Ctrl Pts',(-85.0558113579426,36.3319457088082,122.));
#51355=CARTESIAN_POINT('Ctrl Pts',(-85.0522039701671,36.2945412778582,122.));
#51356=CARTESIAN_POINT('Ctrl Pts',(-85.0493677722714,36.2570607532382,122.));
#51357=CARTESIAN_POINT('Ctrl Pts',(-85.0475886407492,36.2335494238905,122.));
#51358=CARTESIAN_POINT('Ctrl Pts',(-85.0461129995367,36.2100081463298,122.));
#51359=CARTESIAN_POINT('Ctrl Pts',(-85.0449435487391,36.1864426779331,122.));
#51360=CARTESIAN_POINT('Ctrl Pts',(-85.0442591625791,36.1726516912063,122.));
#51361=CARTESIAN_POINT('Ctrl Pts',(-85.043679931207,36.1588573660533,122.));
#51362=CARTESIAN_POINT('Ctrl Pts',(-85.0432063554223,36.1450686933549,122.));
#51363=CARTESIAN_POINT('Ctrl Pts',(-85.0398789557942,36.0481878436707,122.));
#51364=CARTESIAN_POINT('Ctrl Pts',(-85.0417574731529,35.9514719964611,122.));
#51365=CARTESIAN_POINT('Ctrl Pts',(-85.0489062899786,35.8553409172261,122.));
#51366=CARTESIAN_POINT('Ctrl Pts',(-85.0560551068044,35.7592098379912,122.));
#51367=CARTESIAN_POINT('Ctrl Pts',(-85.0684737927824,35.6636624826983,122.));
#51368=CARTESIAN_POINT('Ctrl Pts',(-85.0862791933242,35.5690998313702,122.));
#51369=CARTESIAN_POINT('Ctrl Pts',(-85.1033372114407,35.4785064512488,122.));
#51370=CARTESIAN_POINT('Ctrl Pts',(-85.1253390876716,35.3888158753331,122.));
#51371=CARTESIAN_POINT('Ctrl Pts',(-85.1520102123209,35.3002674435879,122.));
#51372=CARTESIAN_POINT('Ctrl Pts',(-85.1608795543707,35.2708211289146,122.));
#51373=CARTESIAN_POINT('Ctrl Pts',(-85.1702656805221,35.2415011553756,122.));
#51374=CARTESIAN_POINT('Ctrl Pts',(-85.1801597406793,35.2123164991087,122.));
#51375=CARTESIAN_POINT('Ctrl Pts',(-85.1894800179375,35.1848243387849,122.));
#51376=CARTESIAN_POINT('Ctrl Pts',(-85.1992510307603,35.157452254975,122.));
#51377=CARTESIAN_POINT('Ctrl Pts',(-85.2094658558997,35.1302078758792,122.));
#51378=CARTESIAN_POINT('Ctrl Pts',(-85.2146236706355,35.1164512566469,122.));
#51379=CARTESIAN_POINT('Ctrl Pts',(-85.219891565519,35.1027354709933,122.));
#51380=CARTESIAN_POINT('Ctrl Pts',(-85.2252668704309,35.089064837704,122.));
#51381=CARTESIAN_POINT('Ctrl Pts',(-85.2595181900841,35.0019558758258,122.));
#51382=CARTESIAN_POINT('Ctrl Pts',(-85.298143010024,34.9166357250449,122.));
#51383=CARTESIAN_POINT('Ctrl Pts',(-85.3408113440508,34.8333388006193,122.));
#51384=CARTESIAN_POINT('Ctrl Pts',(-85.3850411534874,34.7469935711176,122.));
#51385=CARTESIAN_POINT('Ctrl Pts',(-85.4336159720851,34.6628216295505,122.));
#51386=CARTESIAN_POINT('Ctrl Pts',(-85.4862240883796,34.5810875555579,122.));
#51387=CARTESIAN_POINT('Ctrl Pts',(-85.5393951618781,34.498478848733,122.));
#51388=CARTESIAN_POINT('Ctrl Pts',(-85.5966867302764,34.418359642024,122.));
#51389=CARTESIAN_POINT('Ctrl Pts',(-85.6578284758595,34.3410184645814,122.));
#51390=CARTESIAN_POINT('Ctrl Pts',(-85.6805173073739,34.3123182544813,122.));
#51391=CARTESIAN_POINT('Ctrl Pts',(-85.7037367996653,34.2840008059673,122.));
#51392=CARTESIAN_POINT('Ctrl Pts',(-85.7274747338933,34.2560817511357,122.));
#51393=CARTESIAN_POINT('Ctrl Pts',(-85.7482297832317,34.2316709765946,122.));
#51394=CARTESIAN_POINT('Ctrl Pts',(-85.7693811810863,34.207564768343,122.));
#51395=CARTESIAN_POINT('Ctrl Pts',(-85.7909212499565,34.1837739578324,122.));
#51396=CARTESIAN_POINT('Ctrl Pts',(-85.8026849836044,34.1707810208181,122.));
#51397=CARTESIAN_POINT('Ctrl Pts',(-85.8145599672992,34.157887404697,122.));
#51398=CARTESIAN_POINT('Ctrl Pts',(-85.8265388744956,34.1451007332879,122.));
#51399=CARTESIAN_POINT('Ctrl Pts',(-85.895549674298,34.0714363825852,122.));
#51400=CARTESIAN_POINT('Ctrl Pts',(-85.9680628718138,34.0012565621351,122.));
#51401=CARTESIAN_POINT('Ctrl Pts',(-86.043769945045,33.9348524870057,122.));
#51402=CARTESIAN_POINT('Ctrl Pts',(-86.1059641041579,33.8803008389485,122.));
#51403=CARTESIAN_POINT('Ctrl Pts',(-86.1703148362795,33.8282974253922,122.));
#51404=CARTESIAN_POINT('Ctrl Pts',(-86.2366733734612,33.7790170367676,122.));
#51405=CARTESIAN_POINT('Ctrl Pts',(-86.2612909125297,33.7607351103751,122.));
#51406=CARTESIAN_POINT('Ctrl Pts',(-86.2861849555798,33.7428280844223,122.));
#51407=CARTESIAN_POINT('Ctrl Pts',(-86.3113485141177,33.7253054477748,122.));
#51408=CARTESIAN_POINT('Ctrl Pts',(-86.3281594689655,33.7135991442704,122.));
#51409=CARTESIAN_POINT('Ctrl Pts',(-86.3450918490799,33.7020637690538,122.));
#51410=CARTESIAN_POINT('Ctrl Pts',(-86.3621285098423,33.6907119748374,122.));
#51411=CARTESIAN_POINT('Ctrl Pts',(-86.4470390092949,33.6341347775783,122.));
#51412=CARTESIAN_POINT('Ctrl Pts',(-86.5346187851364,33.5820568809078,122.));
#51413=CARTESIAN_POINT('Ctrl Pts',(-86.6245774787622,33.534786201639,122.));
#51414=CARTESIAN_POINT('Ctrl Pts',(-86.7080355351971,33.4909314183033,122.));
#51415=CARTESIAN_POINT('Ctrl Pts',(-86.7935419310316,33.4512139208354,122.));
#51416=CARTESIAN_POINT('Ctrl Pts',(-86.8808925248099,33.4159086346823,122.));
#51417=CARTESIAN_POINT('Ctrl Pts',(-86.9113227051827,33.4036093911479,122.));
#51418=CARTESIAN_POINT('Ctrl Pts',(-86.941976905733,33.3918459065886,122.));
#51419=CARTESIAN_POINT('Ctrl Pts',(-86.9728422201938,33.3806144585182,122.));
#51420=CARTESIAN_POINT('Ctrl Pts',(-90.2867225490468,36.352727843524,120.387416697508));
#51421=CARTESIAN_POINT('Ctrl Pts',(-90.2883049087302,36.1783614273162,120.398449387697));
#51422=CARTESIAN_POINT('Ctrl Pts',(-90.2717193152599,36.0042940565252,120.409482077886));
#51423=CARTESIAN_POINT('Ctrl Pts',(-90.2358477575736,35.8342964268918,120.420514768075));
#51424=CARTESIAN_POINT('Ctrl Pts',(-90.064663774216,35.0230444691006,120.473164275806));
#51425=CARTESIAN_POINT('Ctrl Pts',(-89.454274927199,34.304473908527,120.525813783537));
#51426=CARTESIAN_POINT('Ctrl Pts',(-88.6813900471312,34.0043286570435,120.578463291268));
#51427=CARTESIAN_POINT('Ctrl Pts',(-87.9085051670634,33.7041834055601,120.631112798999));
#51428=CARTESIAN_POINT('Ctrl Pts',(-86.9731242539449,33.8224634631669,120.683762306729));
#51429=CARTESIAN_POINT('Ctrl Pts',(-86.2992914572421,34.3055671292089,120.73641181446));
#51430=CARTESIAN_POINT('Ctrl Pts',(-85.6254586605392,34.7886707952509,120.789061322191));
#51431=CARTESIAN_POINT('Ctrl Pts',(-85.213173980252,35.6365980697281,120.841710829922));
#51432=CARTESIAN_POINT('Ctrl Pts',(-85.2493333391392,36.4649154270561,120.894360337653));
#51433=CARTESIAN_POINT('Ctrl Pts',(-85.2854926980264,37.293232784384,120.947009845384));
#51434=CARTESIAN_POINT('Ctrl Pts',(-85.7700960960879,38.1019402245628,120.999659353114));
#51435=CARTESIAN_POINT('Ctrl Pts',(-86.4834704866067,38.5245018880125,121.052308860845));
#51436=CARTESIAN_POINT('Ctrl Pts',(-87.1968448771254,38.9470635514623,121.104958368576));
#51437=CARTESIAN_POINT('Ctrl Pts',(-88.1389902601014,38.983479438183,121.157607876307));
#51438=CARTESIAN_POINT('Ctrl Pts',(-88.8827694672617,38.6170777473505,121.210257384038));
#51439=CARTESIAN_POINT('Ctrl Pts',(-89.626548674422,38.250676056518,121.262906891768));
#51440=CARTESIAN_POINT('Ctrl Pts',(-90.1719617057666,37.4814567881323,121.315556399499));
#51441=CARTESIAN_POINT('Ctrl Pts',(-90.2718153505154,36.6584694521901,121.36820590723));
#51442=CARTESIAN_POINT('Ctrl Pts',(-90.2839602404389,36.5583720483486,121.374609503989));
#51443=CARTESIAN_POINT('Ctrl Pts',(-90.289513923836,36.4574792478699,121.381013100749));
#51444=CARTESIAN_POINT('Ctrl Pts',(-90.2887581529621,36.3565049378502,121.387416697508));
#51445=CARTESIAN_POINT('Ctrl Pts',(-88.5623548711056,33.385703120938,122.));
#51446=CARTESIAN_POINT('Ctrl Pts',(-89.5445934608772,33.6482971733158,121.947350492269));
#51447=CARTESIAN_POINT('Ctrl Pts',(-91.2113489167469,35.2211434798136,121.842051476807));
#51448=CARTESIAN_POINT('Ctrl Pts',(-90.6005806604956,38.6233313190636,121.684102953615));
#51449=CARTESIAN_POINT('Ctrl Pts',(-87.4170212212397,39.9637875212778,121.526154430423));
#51450=CARTESIAN_POINT('Ctrl Pts',(-84.554628466517,38.0346655247349,121.36820590723));
#51451=CARTESIAN_POINT('Ctrl Pts',(-84.6050188146032,34.5813834739332,121.210257384038));
#51452=CARTESIAN_POINT('Ctrl Pts',(-87.5242687556742,32.7366979528604,121.052308860845));
#51453=CARTESIAN_POINT('Ctrl Pts',(-90.6647255642019,34.1722681242997,120.894360337653));
#51454=CARTESIAN_POINT('Ctrl Pts',(-91.1794495683065,37.5869248554102,120.73641181446));
#51455=CARTESIAN_POINT('Ctrl Pts',(-88.601553399534,39.8844991555637,120.578463291268));
#51456=CARTESIAN_POINT('Ctrl Pts',(-85.2684357075705,38.981949277713,120.420514768075));
#51457=CARTESIAN_POINT('Ctrl Pts',(-84.202084988714,35.697541610575,120.262566244883));
#51458=CARTESIAN_POINT('Ctrl Pts',(-86.3693523204529,33.0091721012914,120.10461772169));
#51459=CARTESIAN_POINT('Ctrl Pts',(-89.8052309919053,33.3542922396066,119.946669198498));
#51460=CARTESIAN_POINT('Ctrl Pts',(-91.3945198211751,36.4199976266262,119.788720675305));
#51461=CARTESIAN_POINT('Ctrl Pts',(-89.6962562825846,39.4267037361566,119.630772152113));
#51462=CARTESIAN_POINT('Ctrl Pts',(-86.2502055794825,39.6483228920224,119.47282362892));
#51463=CARTESIAN_POINT('Ctrl Pts',(-84.1807964437643,36.8839191095796,119.314875105728));
#51464=CARTESIAN_POINT('Ctrl Pts',(-85.3642995086962,33.6398935322125,119.156926582536));
#51465=CARTESIAN_POINT('Ctrl Pts',(-88.727668390087,32.8575053379033,118.998978059343));
#51466=CARTESIAN_POINT('Ctrl Pts',(-91.2214388882784,35.2461221803218,118.841029536151));
#51467=CARTESIAN_POINT('Ctrl Pts',(-90.5845851017341,38.6400577793749,118.683081012958));
#51468=CARTESIAN_POINT('Ctrl Pts',(-87.394523006908,39.962133966582,118.525132489766));
#51469=CARTESIAN_POINT('Ctrl Pts',(-84.5435848754497,38.0136644637222,118.367183966573));
#51470=CARTESIAN_POINT('Ctrl Pts',(-84.6166296078616,34.5612673131065,118.209235443381));
#51471=CARTESIAN_POINT('Ctrl Pts',(-87.5474297648405,32.7351260092969,118.051286920188));
#51472=CARTESIAN_POINT('Ctrl Pts',(-90.6787179812742,34.1909473338473,117.893338396996));
#51473=CARTESIAN_POINT('Ctrl Pts',(-91.17145046468,37.6087823681217,117.735389873803));
#51474=CARTESIAN_POINT('Ctrl Pts',(-88.5788816583627,39.8897840355259,117.577441350611));
#51475=CARTESIAN_POINT('Ctrl Pts',(-85.2516148494836,38.9658374976431,117.419492827418));
#51476=CARTESIAN_POINT('Ctrl Pts',(-84.2063816594615,35.6746569798619,117.261544304226));
#51477=CARTESIAN_POINT('Ctrl Pts',(-86.3908632323328,33.0002557608977,117.103595781033));
#51478=CARTESIAN_POINT('Ctrl Pts',(-89.8244565639917,33.3674320877617,116.945647257841));
#51479=CARTESIAN_POINT('Ctrl Pts',(-91.3940270086374,36.4432783520433,116.787698734648));
#51480=CARTESIAN_POINT('Ctrl Pts',(-89.6764927804399,39.4390182935569,116.629750211456));
#51481=CARTESIAN_POINT('Ctrl Pts',(-86.2290899276622,39.6385056186423,116.471801688264));
#51482=CARTESIAN_POINT('Ctrl Pts',(-84.1774737689002,36.8608712367781,116.313853165071));
#51483=CARTESIAN_POINT('Ctrl Pts',(-85.3817822782182,33.6245117640691,116.155904641879));
#51484=CARTESIAN_POINT('Ctrl Pts',(-88.7501055576055,32.8637359049969,115.997956118686));
#51485=CARTESIAN_POINT('Ctrl Pts',(-91.228487332563,35.2683159930302,115.840007595494));
#51486=CARTESIAN_POINT('Ctrl Pts',(-90.5698542243114,38.6580923943469,115.682059072301));
#51487=CARTESIAN_POINT('Ctrl Pts',(-87.3713688406819,39.959657941262,115.524110549109));
#51488=CARTESIAN_POINT('Ctrl Pts',(-84.5330006014756,37.9929227377143,115.366162025916));
#51489=CARTESIAN_POINT('Ctrl Pts',(-84.6282116641132,34.5410657772132,115.208213502724));
#51490=CARTESIAN_POINT('Ctrl Pts',(-87.5706770538148,32.7337807823612,115.050264979531));
#51491=CARTESIAN_POINT('Ctrl Pts',(-90.6925528927773,34.2096780919022,114.892316456339));
#51492=CARTESIAN_POINT('Ctrl Pts',(-91.1633293053753,37.630606502663,114.734367933146));
#51493=CARTESIAN_POINT('Ctrl Pts',(-88.5561676363232,39.8949142674411,114.576419409954));
#51494=CARTESIAN_POINT('Ctrl Pts',(-85.2349020777131,38.9496224017201,114.418470886762));
#51495=CARTESIAN_POINT('Ctrl Pts',(-84.2108230998106,35.6517982903965,114.260522363569));
#51496=CARTESIAN_POINT('Ctrl Pts',(-86.412431965926,32.9914787564211,114.102573840377));
#51497=CARTESIAN_POINT('Ctrl Pts',(-89.8435968760591,33.3806946112882,113.944625317184));
#51498=CARTESIAN_POINT('Ctrl Pts',(-91.3933849603557,36.4665556768548,113.786676793992));
#51499=CARTESIAN_POINT('Ctrl Pts',(-89.6566504974584,39.4512055771937,113.628728270799));
#51500=CARTESIAN_POINT('Ctrl Pts',(-86.2080378044846,39.6285530216908,113.470779747607));
#51501=CARTESIAN_POINT('Ctrl Pts',(-84.1742991253402,36.8378024761994,113.312831224414));
#51502=CARTESIAN_POINT('Ctrl Pts',(-85.3993634670394,33.6092425834755,113.154882701222));
#51503=CARTESIAN_POINT('Ctrl Pts',(-88.7725022496111,32.8701104060413,112.996934178029));
#51504=CARTESIAN_POINT('Ctrl Pts',(-91.2353931282765,35.2905546094874,112.838985654837));
#51505=CARTESIAN_POINT('Ctrl Pts',(-90.5550078487894,38.6760320490321,112.681037131644));
#51506=CARTESIAN_POINT('Ctrl Pts',(-87.3482310510782,39.957033294882,112.523088608452));
#51507=CARTESIAN_POINT('Ctrl Pts',(-84.5225497279198,37.9721134773169,112.365140085259));
#51508=CARTESIAN_POINT('Ctrl Pts',(-84.6399231958095,34.5209390263157,112.207191562067));
#51509=CARTESIAN_POINT('Ctrl Pts',(-87.5939325011642,32.7325848538746,112.049243038874));
#51510=CARTESIAN_POINT('Ctrl Pts',(-90.7062672489506,34.2284972978135,111.891294515682));
#51511=CARTESIAN_POINT('Ctrl Pts',(-91.1550681807335,37.6523780413312,111.73334599249));
#51512=CARTESIAN_POINT('Ctrl Pts',(-88.5334211413281,39.8998985469101,111.575397469297));
#51513=CARTESIAN_POINT('Ctrl Pts',(-85.2182937675741,38.9333003273795,111.417448946105));
#51514=CARTESIAN_POINT('Ctrl Pts',(-84.21541122421,35.6289685906495,111.259500422912));
#51515=CARTESIAN_POINT('Ctrl Pts',(-86.4340566120166,32.9828404256698,111.10155189972));
#51516=CARTESIAN_POINT('Ctrl Pts',(-89.8626516349053,33.3940797613523,110.943603376527));
#51517=CARTESIAN_POINT('Ctrl Pts',(-91.3925934616552,36.4898283991584,110.785654853335));
#51518=CARTESIAN_POINT('Ctrl Pts',(-89.6367303689711,39.4632652024454,110.627706330142));
#51519=CARTESIAN_POINT('Ctrl Pts',(-86.1870500209474,39.6184654540127,110.46975780695));
#51520=CARTESIAN_POINT('Ctrl Pts',(-84.1712726716061,36.8147138073089,110.311809283757));
#51521=CARTESIAN_POINT('Ctrl Pts',(-85.417042337004,33.594086605388,110.153860760565));
#51522=CARTESIAN_POINT('Ctrl Pts',(-88.7948575488562,32.8766285869604,109.995912237372));
#51523=CARTESIAN_POINT('Ctrl Pts',(-91.2421559883216,35.3128371051595,109.83796371418));
#51524=CARTESIAN_POINT('Ctrl Pts',(-90.5400465871546,38.6938760144785,109.680015190987));
#51525=CARTESIAN_POINT('Ctrl Pts',(-87.325110594749,39.9542601161072,109.522066667795));
#51526=CARTESIAN_POINT('Ctrl Pts',(-84.512232678954,37.9512375795022,109.364118144602));
#51527=CARTESIAN_POINT('Ctrl Pts',(-84.6517637344715,34.5008878105768,109.20616962141));
#51528=CARTESIAN_POINT('Ctrl Pts',(-87.6171951182148,32.7315384366804,109.048221098217));
#51529=CARTESIAN_POINT('Ctrl Pts',(-90.7198605459008,34.2474038394901,108.890272575025));
#51530=CARTESIAN_POINT('Ctrl Pts',(-91.146667304722,37.6740967778006,108.732324051833));
#51531=CARTESIAN_POINT('Ctrl Pts',(-88.5106433716724,39.9047352467602,108.57437552864));
#51532=CARTESIAN_POINT('Ctrl Pts',(-85.2017900681466,38.9168748712948,108.416427005448));
#51533=CARTESIAN_POINT('Ctrl Pts',(-84.2201469451404,35.6061628091222,108.258478482255));
#51534=CARTESIAN_POINT('Ctrl Pts',(-86.4557340134341,32.9743534903137,108.100529959063));
#51535=CARTESIAN_POINT('Ctrl Pts',(-89.8816247142105,33.4075615558338,107.94258143587));
#51536=CARTESIAN_POINT('Ctrl Pts',(-91.3916429630939,36.5131478579286,107.784632912678));
#51537=CARTESIAN_POINT('Ctrl Pts',(-89.6167529221334,39.4750891176184,107.626684389485));
#51538=CARTESIAN_POINT('Ctrl Pts',(-86.1660869151683,39.6084645219268,107.468735866293));
#51539=CARTESIAN_POINT('Ctrl Pts',(-84.1684778438722,36.7911512436696,107.310787343101));
#51540=CARTESIAN_POINT('Ctrl Pts',(-85.4346465172346,33.5799799853229,107.152838819908));
#51541=CARTESIAN_POINT('Ctrl Pts',(-88.8175140813586,32.8813523470733,106.994890296716));
#51542=CARTESIAN_POINT('Ctrl Pts',(-91.2479897958802,35.3391374795667,106.836941773523));
#51543=CARTESIAN_POINT('Ctrl Pts',(-90.7653388102639,37.5794426551218,106.731642758061));
#51544=CARTESIAN_POINT('Ctrl Pts',(-90.1046182462678,38.3522276316149,106.678993250331));
#51545=CARTESIAN_POINT('Ctrl Pts',(-88.5144884429196,33.5647485048415,122.10700224989));
#51546=CARTESIAN_POINT('Ctrl Pts',(-89.4374976355964,33.8115080262153,122.054352742159));
#51547=CARTESIAN_POINT('Ctrl Pts',(-91.003747041527,35.2895110436928,121.949053726697));
#51548=CARTESIAN_POINT('Ctrl Pts',(-90.4298083661526,38.4865455356597,121.791105203505));
#51549=CARTESIAN_POINT('Ctrl Pts',(-87.4382188903723,39.7461716691758,121.633156680312));
#51550=CARTESIAN_POINT('Ctrl Pts',(-84.7484296139453,37.9333765345252,121.47520815712));
#51551=CARTESIAN_POINT('Ctrl Pts',(-84.7957814030015,34.6883288332973,121.317259633928));
#51552=CARTESIAN_POINT('Ctrl Pts',(-87.5389993536994,32.9548786193897,121.159311110735));
#51553=CARTESIAN_POINT('Ctrl Pts',(-90.4900853053818,34.3038833100721,121.001362587543));
#51554=CARTESIAN_POINT('Ctrl Pts',(-90.9737712371171,37.512634814514,120.84341406435));
#51555=CARTESIAN_POINT('Ctrl Pts',(-88.5513232837166,39.671664425021,120.685465541158));
#51556=CARTESIAN_POINT('Ctrl Pts',(-85.4191939803146,38.8235386816624,120.527517017965));
#51557=CARTESIAN_POINT('Ctrl Pts',(-84.4171446550577,35.7371821682502,120.369568494773));
#51558=CARTESIAN_POINT('Ctrl Pts',(-86.4537248617547,33.2109224628993,120.21161997158));
#51559=CARTESIAN_POINT('Ctrl Pts',(-89.6824186146749,33.5352317127699,120.053671448388));
#51560=CARTESIAN_POINT('Ctrl Pts',(-91.1758726639355,36.4160737848735,119.895722925195));
#51561=CARTESIAN_POINT('Ctrl Pts',(-89.5800151258284,39.2414742605557,119.737774402003));
#51562=CARTESIAN_POINT('Ctrl Pts',(-86.3417627190143,39.4497296887861,119.57982587881));
#51563=CARTESIAN_POINT('Ctrl Pts',(-84.3971398182574,36.8520206086955,119.421877355618));
#51564=CARTESIAN_POINT('Ctrl Pts',(-85.5092771542047,33.8036111281796,119.263928832425));
#51565=CARTESIAN_POINT('Ctrl Pts',(-88.6698334876803,33.0684012686717,119.105980309233));
#51566=CARTESIAN_POINT('Ctrl Pts',(-91.0132285835621,35.3129835181305,118.948031786041));
#51567=CARTESIAN_POINT('Ctrl Pts',(-90.4147773462634,38.5022633834302,118.790083262848));
#51568=CARTESIAN_POINT('Ctrl Pts',(-87.4170773277588,39.7446178245186,118.632134739655));
#51569=CARTESIAN_POINT('Ctrl Pts',(-84.7380519560306,37.9136418462605,118.474186216463));
#51570=CARTESIAN_POINT('Ctrl Pts',(-84.8066920605784,34.669425685368,118.316237693271));
#51571=CARTESIAN_POINT('Ctrl Pts',(-87.5607637443422,32.9534014646795,118.158289170078));
#51572=CARTESIAN_POINT('Ctrl Pts',(-90.5032339738622,34.3214361554844,118.000340646886));
#51573=CARTESIAN_POINT('Ctrl Pts',(-90.9662544827793,37.5331743100824,117.842392123693));
#51574=CARTESIAN_POINT('Ctrl Pts',(-88.5300186580045,39.6766306245147,117.684443600501));
#51575=CARTESIAN_POINT('Ctrl Pts',(-85.4033874269938,38.8083984486582,117.526495077308));
#51576=CARTESIAN_POINT('Ctrl Pts',(-84.421182234765,35.7156774903246,117.368546554116));
#51577=CARTESIAN_POINT('Ctrl Pts',(-86.4739386566664,33.2025437815544,117.210598030923));
#51578=CARTESIAN_POINT('Ctrl Pts',(-89.7004848767369,33.5475792225948,117.052649507731));
#51579=CARTESIAN_POINT('Ctrl Pts',(-91.1754095681997,36.4379506728273,116.894700984538));
#51580=CARTESIAN_POINT('Ctrl Pts',(-89.5614433711151,39.2530462450027,116.736752461346));
#51581=CARTESIAN_POINT('Ctrl Pts',(-86.3219203498158,39.44050440109,116.578803938153));
#51582=CARTESIAN_POINT('Ctrl Pts',(-84.3940175020749,36.8303625322474,116.420855414961));
#51583=CARTESIAN_POINT('Ctrl Pts',(-85.5257057054248,33.7891568870778,116.262906891768));
#51584=CARTESIAN_POINT('Ctrl Pts',(-88.6909176846287,33.074256129968,116.104958368576));
#51585=CARTESIAN_POINT('Ctrl Pts',(-91.0198520037133,35.3338390346656,115.947009845384));
#51586=CARTESIAN_POINT('Ctrl Pts',(-90.4009347469002,38.5192105035891,115.789061322191));
#51587=CARTESIAN_POINT('Ctrl Pts',(-87.3953193674241,39.7422911045592,115.631112798999));
#51588=CARTESIAN_POINT('Ctrl Pts',(-84.7281059181966,37.8941508549915,115.473164275806));
#51589=CARTESIAN_POINT('Ctrl Pts',(-84.817575714002,34.6504423105241,115.315215752614));
#51590=CARTESIAN_POINT('Ctrl Pts',(-87.5826092120844,32.9521373554897,115.157267229421));
#51591=CARTESIAN_POINT('Ctrl Pts',(-90.516234634425,34.3390374410077,114.999318706229));
#51592=CARTESIAN_POINT('Ctrl Pts',(-90.9586230327715,37.5536824401982,114.841370183036));
#51593=CARTESIAN_POINT('Ctrl Pts',(-88.5086743009781,39.6814515013034,114.683421659844));
#51594=CARTESIAN_POINT('Ctrl Pts',(-85.3876824423395,38.7931611297899,114.525473136651));
#51595=CARTESIAN_POINT('Ctrl Pts',(-84.4253558544066,35.6941971893785,114.367524613459));
#51596=CARTESIAN_POINT('Ctrl Pts',(-86.494206786618,33.1942960341126,114.209576090266));
#51597=CARTESIAN_POINT('Ctrl Pts',(-89.7184710199947,33.5600420104149,114.051627567074));
#51598=CARTESIAN_POINT('Ctrl Pts',(-91.1748062356975,36.4598243652332,113.893679043881));
#51599=CARTESIAN_POINT('Ctrl Pts',(-89.5427975860825,39.2644986303475,113.735730520689));
#51600=CARTESIAN_POINT('Ctrl Pts',(-86.302137678456,39.4311519498904,113.577781997497));
#51601=CARTESIAN_POINT('Ctrl Pts',(-84.3910342908472,36.808684827564,113.419833474304));
#51602=CARTESIAN_POINT('Ctrl Pts',(-85.5422267412189,33.7748084444496,113.261884951112));
#51603=CARTESIAN_POINT('Ctrl Pts',(-88.7119638467548,33.0802462459377,113.103936427919));
#51604=CARTESIAN_POINT('Ctrl Pts',(-91.0263413770617,35.3547366532648,112.945987904727));
#51605=CARTESIAN_POINT('Ctrl Pts',(-90.3869836140211,38.536068389606,112.788039381534));
#51606=CARTESIAN_POINT('Ctrl Pts',(-87.3735767961947,39.739824725452,112.630090858342));
#51607=CARTESIAN_POINT('Ctrl Pts',(-84.71828523668,37.874596401685,112.472142335149));
#51608=CARTESIAN_POINT('Ctrl Pts',(-84.8285810354468,34.6315292111096,112.314193811957));
#51609=CARTESIAN_POINT('Ctrl Pts',(-87.6044623462484,32.9510135419902,112.156245288764));
#51610=CARTESIAN_POINT('Ctrl Pts',(-90.5291220091947,34.3567218409445,111.998296765572));
#51611=CARTESIAN_POINT('Ctrl Pts',(-90.950860057395,37.5741411459941,111.840348242379));
#51612=CARTESIAN_POINT('Ctrl Pts',(-88.4872994291289,39.6861352266392,111.682399719187));
#51613=CARTESIAN_POINT('Ctrl Pts',(-85.3720756202366,38.7778232833473,111.524451195994));
#51614=CARTESIAN_POINT('Ctrl Pts',(-84.4296673129889,35.6727441300587,111.366502672802));
#51615=CARTESIAN_POINT('Ctrl Pts',(-86.51452745752,33.1861785983124,111.208554149609));
#51616=CARTESIAN_POINT('Ctrl Pts',(-89.7363767689262,33.5726200303412,111.050605626417));
#51617=CARTESIAN_POINT('Ctrl Pts',(-91.174062464699,36.4816937326644,110.892657103225));
#51618=CARTESIAN_POINT('Ctrl Pts',(-89.5240786496606,39.2758310551611,110.734708580032));
#51619=CARTESIAN_POINT('Ctrl Pts',(-86.2824154670296,39.4216726667553,110.57676005684));
#51620=CARTESIAN_POINT('Ctrl Pts',(-84.3881903335369,36.7869884150482,110.418811533647));
#51621=CARTESIAN_POINT('Ctrl Pts',(-85.5588395679429,33.7605663781691,110.260863010455));
#51622=CARTESIAN_POINT('Ctrl Pts',(-88.7329711121209,33.0863713778258,110.102914487262));
#51623=CARTESIAN_POINT('Ctrl Pts',(-91.0326964338223,35.3756755051439,109.94496596407));
#51624=CARTESIAN_POINT('Ctrl Pts',(-90.37292452271,38.5528363564853,109.787017440877));
#51625=CARTESIAN_POINT('Ctrl Pts',(-87.3518505130362,39.7372187705151,109.629068917685));
#51626=CARTESIAN_POINT('Ctrl Pts',(-84.7085903100746,37.8549793292252,109.471120394492));
#51627=CARTESIAN_POINT('Ctrl Pts',(-84.8397075846835,34.6126870920522,109.3131718713));
#51628=CARTESIAN_POINT('Ctrl Pts',(-87.6263222177776,32.9500302241897,109.155223348107));
#51629=CARTESIAN_POINT('Ctrl Pts',(-90.5418956246628,34.3744883102637,108.997274824915));
#51630=CARTESIAN_POINT('Ctrl Pts',(-90.942965757715,37.5945502335857,108.839326301722));
#51631=CARTESIAN_POINT('Ctrl Pts',(-88.4658951684941,39.6906802714687,108.68137777853));
#51632=CARTESIAN_POINT('Ctrl Pts',(-85.3565671007757,38.7623882891229,108.523429255338));
#51633=CARTESIAN_POINT('Ctrl Pts',(-84.4341174679698,35.65131354668,108.365480732145));
#51634=CARTESIAN_POINT('Ctrl Pts',(-86.5348977025807,33.178203428702,108.207532208953));
#51635=CARTESIAN_POINT('Ctrl Pts',(-89.7542057636271,33.5852888669862,108.04958368576));
#51636=CARTESIAN_POINT('Ctrl Pts',(-91.1731692815978,36.5036070183338,107.891635162568));
#51637=CARTESIAN_POINT('Ctrl Pts',(-89.5053058512089,39.286941983312,107.733686639375));
#51638=CARTESIAN_POINT('Ctrl Pts',(-86.2627164452819,39.4122747950501,107.575738116183));
#51639=CARTESIAN_POINT('Ctrl Pts',(-84.3855640350824,36.7648466838348,107.41778959299));
#51640=CARTESIAN_POINT('Ctrl Pts',(-85.5753822087549,33.7473103931842,107.259841069798));
#51641=CARTESIAN_POINT('Ctrl Pts',(-88.7542614462533,33.0908102932314,107.101892546605));
#51642=CARTESIAN_POINT('Ctrl Pts',(-91.0381784603491,35.4003899559926,106.943944023413));
#51643=CARTESIAN_POINT('Ctrl Pts',(-90.5846315306955,37.5056037940271,106.838645007951));
#51644=CARTESIAN_POINT('Ctrl Pts',(-89.9637526925908,38.2317895137629,106.78599550022));
#51645=CARTESIAN_POINT('Ctrl Pts',(-88.4666220147337,33.743793888745,122.21400449978));
#51646=CARTESIAN_POINT('Ctrl Pts',(-89.3304018103156,33.9747188791149,122.161354992049));
#51647=CARTESIAN_POINT('Ctrl Pts',(-90.7961451663071,35.3578786075719,122.056055976587));
#51648=CARTESIAN_POINT('Ctrl Pts',(-90.2590360718096,38.3497597522559,121.898107453395));
#51649=CARTESIAN_POINT('Ctrl Pts',(-87.4594165595049,39.5285558170738,121.740158930202));
#51650=CARTESIAN_POINT('Ctrl Pts',(-84.9422307613735,37.8320875443154,121.58221040701));
#51651=CARTESIAN_POINT('Ctrl Pts',(-84.9865439913999,34.7952741926615,121.424261883817));
#51652=CARTESIAN_POINT('Ctrl Pts',(-87.5537299517246,33.173059285919,121.266313360625));
#51653=CARTESIAN_POINT('Ctrl Pts',(-90.3154450465617,34.4354984958443,121.108364837432));
#51654=CARTESIAN_POINT('Ctrl Pts',(-90.7680929059277,37.4383447736177,120.95041631424));
#51655=CARTESIAN_POINT('Ctrl Pts',(-88.501093167899,39.4588296944782,120.792467791047));
#51656=CARTESIAN_POINT('Ctrl Pts',(-85.5699522530588,38.6651280856119,120.634519267855));
#51657=CARTESIAN_POINT('Ctrl Pts',(-84.6322043214011,35.7768227259254,120.476570744662));
#51658=CARTESIAN_POINT('Ctrl Pts',(-86.5380974030568,33.4126728245073,120.31862222147));
#51659=CARTESIAN_POINT('Ctrl Pts',(-89.5596062374444,33.7161711859333,120.160673698277));
#51660=CARTESIAN_POINT('Ctrl Pts',(-90.9572255066959,36.4121499431209,120.002725175085));
#51661=CARTESIAN_POINT('Ctrl Pts',(-89.4637739690721,39.0562447849546,119.844776651893));
#51662=CARTESIAN_POINT('Ctrl Pts',(-86.4333198585462,39.2511364855498,119.6868281287));
#51663=CARTESIAN_POINT('Ctrl Pts',(-84.6134831927505,36.8201221078114,119.528879605508));
#51664=CARTESIAN_POINT('Ctrl Pts',(-85.654254799713,33.9673287241466,119.370931082315));
#51665=CARTESIAN_POINT('Ctrl Pts',(-88.6119985852735,33.27929719944,119.212982559123));
#51666=CARTESIAN_POINT('Ctrl Pts',(-90.8050182788458,35.3798448559393,119.05503403593));
#51667=CARTESIAN_POINT('Ctrl Pts',(-90.2449695907927,38.3644689874854,118.897085512738));
#51668=CARTESIAN_POINT('Ctrl Pts',(-87.4396316486096,39.5271016824553,118.739136989545));
#51669=CARTESIAN_POINT('Ctrl Pts',(-84.9325190366115,37.8136192287988,118.581188466353));
#51670=CARTESIAN_POINT('Ctrl Pts',(-84.9967545132952,34.7775840576295,118.42323994316));
#51671=CARTESIAN_POINT('Ctrl Pts',(-87.5740977238439,33.171676920062,118.265291419968));
#51672=CARTESIAN_POINT('Ctrl Pts',(-90.3277499664502,34.4519249771215,118.107342896775));
#51673=CARTESIAN_POINT('Ctrl Pts',(-90.7610585008785,37.4575662520431,117.949394373583));
#51674=CARTESIAN_POINT('Ctrl Pts',(-88.4811556576462,39.4634772135036,117.79144585039));
#51675=CARTESIAN_POINT('Ctrl Pts',(-85.5551600045041,38.6509593996732,117.633497327198));
#51676=CARTESIAN_POINT('Ctrl Pts',(-84.6359828100684,35.7566980007872,117.475548804005));
#51677=CARTESIAN_POINT('Ctrl Pts',(-86.5570140810003,33.404831802211,117.317600280813));
#51678=CARTESIAN_POINT('Ctrl Pts',(-89.576513189482,33.7277263574279,117.159651757621));
#51679=CARTESIAN_POINT('Ctrl Pts',(-90.956792127762,36.4326229936112,117.001703234428));
#51680=CARTESIAN_POINT('Ctrl Pts',(-89.4463939617905,39.0670741964486,116.843754711236));
#51681=CARTESIAN_POINT('Ctrl Pts',(-86.4147507719692,39.2425031835377,116.685806188043));
#51682=CARTESIAN_POINT('Ctrl Pts',(-84.6105612352497,36.7998538277168,116.527857664851));
#51683=CARTESIAN_POINT('Ctrl Pts',(-85.6696291326311,33.9538020100865,116.369909141658));
#51684=CARTESIAN_POINT('Ctrl Pts',(-88.631729811652,33.284776354939,116.211960618466));
#51685=CARTESIAN_POINT('Ctrl Pts',(-90.8112166748635,35.3993620763011,116.054012095273));
#51686=CARTESIAN_POINT('Ctrl Pts',(-90.2320152694889,38.3803286128312,115.896063572081));
#51687=CARTESIAN_POINT('Ctrl Pts',(-87.4192698941663,39.5249242678565,115.738115048888));
#51688=CARTESIAN_POINT('Ctrl Pts',(-84.9232112349175,37.7953789722688,115.580166525696));
#51689=CARTESIAN_POINT('Ctrl Pts',(-85.0069397638907,34.7598188438351,115.422218002503));
#51690=CARTESIAN_POINT('Ctrl Pts',(-87.5945413703541,33.1704939286182,115.264269479311));
#51691=CARTESIAN_POINT('Ctrl Pts',(-90.3399163760726,34.4683967901131,115.106320956119));
#51692=CARTESIAN_POINT('Ctrl Pts',(-90.7539167601679,37.4767583777334,114.948372432926));
#51693=CARTESIAN_POINT('Ctrl Pts',(-88.461180965633,39.4679887351656,114.790423909734));
#51694=CARTESIAN_POINT('Ctrl Pts',(-85.5404628069659,38.6366998578597,114.632475386541));
#51695=CARTESIAN_POINT('Ctrl Pts',(-84.6398886090025,35.7365960883606,114.474526863349));
#51696=CARTESIAN_POINT('Ctrl Pts',(-86.5759816073101,33.397113311804,114.316578340156));
#51697=CARTESIAN_POINT('Ctrl Pts',(-89.5933451639302,33.7393894095416,114.158629816964));
#51698=CARTESIAN_POINT('Ctrl Pts',(-90.9562275110392,36.4530930536116,114.000681293771));
#51699=CARTESIAN_POINT('Ctrl Pts',(-89.4289446747066,39.0777916835012,113.842732770579));
#51700=CARTESIAN_POINT('Ctrl Pts',(-86.3962375524274,39.2337508780899,113.684784247386));
#51701=CARTESIAN_POINT('Ctrl Pts',(-84.6077694563542,36.7795671789286,113.526835724194));
#51702=CARTESIAN_POINT('Ctrl Pts',(-85.6850900153984,33.9403743054237,113.368887201001));
#51703=CARTESIAN_POINT('Ctrl Pts',(-88.6514254438984,33.2903820858341,113.210938677809));
#51704=CARTESIAN_POINT('Ctrl Pts',(-90.8172896258469,35.4189186970422,113.052990154617));
#51705=CARTESIAN_POINT('Ctrl Pts',(-90.2189593792529,38.39610473018,112.895041631424));
#51706=CARTESIAN_POINT('Ctrl Pts',(-87.3989225413111,39.5226161560218,112.737093108232));
#51707=CARTESIAN_POINT('Ctrl Pts',(-84.9140207454401,37.777079326053,112.579144585039));
#51708=CARTESIAN_POINT('Ctrl Pts',(-85.0172388750841,34.7421193959036,112.421196061847));
#51709=CARTESIAN_POINT('Ctrl Pts',(-87.6149921913326,33.1694422301058,112.263247538654));
#51710=CARTESIAN_POINT('Ctrl Pts',(-90.3519767694386,34.4849463840756,112.105299015462));
#51711=CARTESIAN_POINT('Ctrl Pts',(-90.7466519340567,37.4959042506569,111.947350492269));
#51712=CARTESIAN_POINT('Ctrl Pts',(-88.4411777169297,39.4723719063683,111.789401969077));
#51713=CARTESIAN_POINT('Ctrl Pts',(-85.5258574728992,38.622346239315,111.631453445884));
#51714=CARTESIAN_POINT('Ctrl Pts',(-84.6439234017677,35.716519669468,111.473504922692));
#51715=CARTESIAN_POINT('Ctrl Pts',(-86.5949983030236,33.3895167709551,111.315556399499));
#51716=CARTESIAN_POINT('Ctrl Pts',(-89.6101019029469,33.7511602993301,111.157607876307));
#51717=CARTESIAN_POINT('Ctrl Pts',(-90.9555314677429,36.4735590661704,110.999659353114));
#51718=CARTESIAN_POINT('Ctrl Pts',(-89.4114269303503,39.0883969078767,110.841710829922));
#51719=CARTESIAN_POINT('Ctrl Pts',(-86.3777809131116,39.2248798794979,110.683762306729));
#51720=CARTESIAN_POINT('Ctrl Pts',(-84.6051079954678,36.7592630227875,110.525813783537));
#51721=CARTESIAN_POINT('Ctrl Pts',(-85.7006367988817,33.9270461509502,110.367865260344));
#51722=CARTESIAN_POINT('Ctrl Pts',(-88.6710846753857,33.2961141686911,110.209916737152));
#51723=CARTESIAN_POINT('Ctrl Pts',(-90.8232368793229,35.4385139051282,110.05196821396));
#51724=CARTESIAN_POINT('Ctrl Pts',(-90.2058024582654,38.4117966984921,109.894019690767));
#51725=CARTESIAN_POINT('Ctrl Pts',(-87.3785904313232,39.5201774249231,109.736071167575));
#51726=CARTESIAN_POINT('Ctrl Pts',(-84.9049479411952,37.7587210789482,109.578122644382));
#51727=CARTESIAN_POINT('Ctrl Pts',(-85.0276514348956,34.7244863735275,109.42017412119));
#51728=CARTESIAN_POINT('Ctrl Pts',(-87.6354493173403,33.168522011699,109.262225597997));
#51729=CARTESIAN_POINT('Ctrl Pts',(-90.3639307034249,34.5015727810372,109.104277074805));
#51730=CARTESIAN_POINT('Ctrl Pts',(-90.7392642107077,37.5150036893709,108.946328551612));
#51731=CARTESIAN_POINT('Ctrl Pts',(-88.4211469653162,39.4766252961773,108.78838002842));
#51732=CARTESIAN_POINT('Ctrl Pts',(-85.5113441334047,38.607901706951,108.630431505227));
#51733=CARTESIAN_POINT('Ctrl Pts',(-84.6480879907992,35.6964642842379,108.472482982035));
#51734=CARTESIAN_POINT('Ctrl Pts',(-86.6140613917273,33.3820533670904,108.314534458842));
#51735=CARTESIAN_POINT('Ctrl Pts',(-89.6267868130435,33.7630161781385,108.15658593565));
#51736=CARTESIAN_POINT('Ctrl Pts',(-90.9546956001019,36.4940661787389,107.998637412457));
#51737=CARTESIAN_POINT('Ctrl Pts',(-89.3938587802843,39.0987948490057,107.840688889265));
#51738=CARTESIAN_POINT('Ctrl Pts',(-86.3593459753956,39.2160850681732,107.682740366072));
#51739=CARTESIAN_POINT('Ctrl Pts',(-84.6026502262925,36.7385421240001,107.52479184288));
#51740=CARTESIAN_POINT('Ctrl Pts',(-85.7161179002754,33.9146408010454,107.366843319688));
#51741=CARTESIAN_POINT('Ctrl Pts',(-88.6910088111477,33.3002682393896,107.208894796495));
#51742=CARTESIAN_POINT('Ctrl Pts',(-90.8283671248183,35.4616424324185,107.050946273303));
#51743=CARTESIAN_POINT('Ctrl Pts',(-90.4039242511271,37.4317649329324,106.945647257841));
#51744=CARTESIAN_POINT('Ctrl Pts',(-89.8228871389138,38.111351395911,106.89299775011));
#51745=CARTESIAN_POINT('Ctrl Pts',(-88.4187555865477,33.9228392726486,122.321006749669));
#51746=CARTESIAN_POINT('Ctrl Pts',(-89.2233059850348,34.1379297320145,122.268357241939));
#51747=CARTESIAN_POINT('Ctrl Pts',(-90.5885432910872,35.4262461714511,122.163058226477));
#51748=CARTESIAN_POINT('Ctrl Pts',(-90.0882637774666,38.212973968852,122.005109703285));
#51749=CARTESIAN_POINT('Ctrl Pts',(-87.4806142286375,39.3109399649718,121.847161180092));
#51750=CARTESIAN_POINT('Ctrl Pts',(-85.1360319088018,37.7307985541058,121.6892126569));
#51751=CARTESIAN_POINT('Ctrl Pts',(-85.1773065797982,34.9022195520257,121.531264133707));
#51752=CARTESIAN_POINT('Ctrl Pts',(-87.5684605497497,33.3912399524484,121.373315610515));
#51753=CARTESIAN_POINT('Ctrl Pts',(-90.1408047877418,34.5671136816166,121.215367087322));
#51754=CARTESIAN_POINT('Ctrl Pts',(-90.5624145747381,37.3640547327214,121.05741856413));
#51755=CARTESIAN_POINT('Ctrl Pts',(-88.4508630520817,39.2459949639355,120.899470040937));
#51756=CARTESIAN_POINT('Ctrl Pts',(-85.7207105258027,38.5067174895613,120.741521517745));
#51757=CARTESIAN_POINT('Ctrl Pts',(-84.8472639877449,35.8164632836006,120.583572994552));
#51758=CARTESIAN_POINT('Ctrl Pts',(-86.6224699443586,33.6144231861152,120.42562447136));
#51759=CARTESIAN_POINT('Ctrl Pts',(-89.436793860214,33.8971106590967,120.267675948167));
#51760=CARTESIAN_POINT('Ctrl Pts',(-90.7385783494564,36.4082261013683,120.109727424975));
#51761=CARTESIAN_POINT('Ctrl Pts',(-89.3475328123158,38.8710153093537,119.951778901782));
#51762=CARTESIAN_POINT('Ctrl Pts',(-86.5248769980782,39.0525432823135,119.79383037859));
#51763=CARTESIAN_POINT('Ctrl Pts',(-84.8298265672435,36.7882236069272,119.635881855398));
#51764=CARTESIAN_POINT('Ctrl Pts',(-85.7992324452217,34.1310463201136,119.477933332205));
#51765=CARTESIAN_POINT('Ctrl Pts',(-88.5541636828665,33.4901931302084,119.319984809013));
#51766=CARTESIAN_POINT('Ctrl Pts',(-90.5968079741295,35.446706193748,119.16203628582));
#51767=CARTESIAN_POINT('Ctrl Pts',(-90.0751618353219,38.2266745915407,119.004087762628));
#51768=CARTESIAN_POINT('Ctrl Pts',(-87.4621859694605,39.3095855403919,118.846139239435));
#51769=CARTESIAN_POINT('Ctrl Pts',(-85.1269861171924,37.7135966113371,118.688190716243));
#51770=CARTESIAN_POINT('Ctrl Pts',(-85.186816966012,34.8857424298909,118.53024219305));
#51771=CARTESIAN_POINT('Ctrl Pts',(-87.5874317033455,33.3899523754446,118.372293669858));
#51772=CARTESIAN_POINT('Ctrl Pts',(-90.1522659590382,34.5824137987586,118.214345146665));
#51773=CARTESIAN_POINT('Ctrl Pts',(-90.5558625189777,37.3819581940037,118.056396623473));
#51774=CARTESIAN_POINT('Ctrl Pts',(-88.4322926572878,39.2503238024924,117.89844810028));
#51775=CARTESIAN_POINT('Ctrl Pts',(-85.7069325820144,38.4935203506883,117.740499577088));
#51776=CARTESIAN_POINT('Ctrl Pts',(-84.8507833853719,35.7977185112499,117.582551053895));
#51777=CARTESIAN_POINT('Ctrl Pts',(-86.6400895053339,33.6071198228677,117.424602530703));
#51778=CARTESIAN_POINT('Ctrl Pts',(-89.4525415022272,33.907873492261,117.26665400751));
#51779=CARTESIAN_POINT('Ctrl Pts',(-90.7381746873242,36.4272953143951,117.108705484318));
#51780=CARTESIAN_POINT('Ctrl Pts',(-89.3313445524658,38.8811021478944,116.950756961125));
#51781=CARTESIAN_POINT('Ctrl Pts',(-86.5075811941226,39.0445019659854,116.792808437933));
#51782=CARTESIAN_POINT('Ctrl Pts',(-84.8271049684244,36.7693451231862,116.634859914741));
#51783=CARTESIAN_POINT('Ctrl Pts',(-85.8135525598376,34.1184471330952,116.476911391548));
#51784=CARTESIAN_POINT('Ctrl Pts',(-88.5725419386751,33.4952965799101,116.318962868356));
#51785=CARTESIAN_POINT('Ctrl Pts',(-90.602581346014,35.4648851179365,116.161014345163));
#51786=CARTESIAN_POINT('Ctrl Pts',(-90.0630957920775,38.2414467220733,116.003065821971));
#51787=CARTESIAN_POINT('Ctrl Pts',(-87.4432204209086,39.3075574311537,115.845117298778));
#51788=CARTESIAN_POINT('Ctrl Pts',(-85.1183165516385,37.6966070895461,115.687168775586));
#51789=CARTESIAN_POINT('Ctrl Pts',(-85.1963038137795,34.869195377146,115.529220252393));
#51790=CARTESIAN_POINT('Ctrl Pts',(-87.6064735286238,33.3888505017467,115.371271729201));
#51791=CARTESIAN_POINT('Ctrl Pts',(-90.1635981177202,34.5977561392184,115.213323206008));
#51792=CARTESIAN_POINT('Ctrl Pts',(-90.5492104875641,37.3998343152686,115.055374682816));
#51793=CARTESIAN_POINT('Ctrl Pts',(-88.413687630288,39.2545259690279,114.897426159623));
#51794=CARTESIAN_POINT('Ctrl Pts',(-85.6932431715923,38.4802385859295,114.739477636431));
#51795=CARTESIAN_POINT('Ctrl Pts',(-84.8544213635984,35.7789949873425,114.581529113238));
#51796=CARTESIAN_POINT('Ctrl Pts',(-86.6577564280022,33.5999305894954,114.423580590046));
#51797=CARTESIAN_POINT('Ctrl Pts',(-89.4682193078656,33.9187368086683,114.265632066854));
#51798=CARTESIAN_POINT('Ctrl Pts',(-90.737648786381,36.4463617419899,114.107683543661));
#51799=CARTESIAN_POINT('Ctrl Pts',(-89.3150917633309,38.891084736655,113.949735020469));
#51800=CARTESIAN_POINT('Ctrl Pts',(-86.4903374263987,39.0363498062895,113.791786497276));
#51801=CARTESIAN_POINT('Ctrl Pts',(-84.8245046218612,36.7504495302932,113.633837974084));
#51802=CARTESIAN_POINT('Ctrl Pts',(-85.827953289578,34.1059401663978,113.475889450891));
#51803=CARTESIAN_POINT('Ctrl Pts',(-88.5908870410419,33.5005179257306,113.317940927699));
#51804=CARTESIAN_POINT('Ctrl Pts',(-90.6082378746323,35.4831007408195,113.159992404506));
#51805=CARTESIAN_POINT('Ctrl Pts',(-90.0509351444846,38.2561410707539,113.002043881314));
#51806=CARTESIAN_POINT('Ctrl Pts',(-87.4242682864277,39.3054075865917,112.844095358121));
#51807=CARTESIAN_POINT('Ctrl Pts',(-85.1097562542002,37.6795622504211,112.686146834929));
#51808=CARTESIAN_POINT('Ctrl Pts',(-85.2058967147215,34.8527095806976,112.528198311736));
#51809=CARTESIAN_POINT('Ctrl Pts',(-87.6255220364168,33.3878709182214,112.370249788544));
#51810=CARTESIAN_POINT('Ctrl Pts',(-90.1748315296826,34.6131709272066,112.212301265351));
#51811=CARTESIAN_POINT('Ctrl Pts',(-90.5424438107183,37.4176673553198,112.054352742159));
#51812=CARTESIAN_POINT('Ctrl Pts',(-88.3950560047306,39.2586085860974,111.896404218966));
#51813=CARTESIAN_POINT('Ctrl Pts',(-85.6796393255617,38.4668691952829,111.738455695774));
#51814=CARTESIAN_POINT('Ctrl Pts',(-84.8581794905466,35.7602952088772,111.580507172582));
#51815=CARTESIAN_POINT('Ctrl Pts',(-86.6754691485269,33.5928549435978,111.422558649389));
#51816=CARTESIAN_POINT('Ctrl Pts',(-89.4838270369679,33.929700568319,111.264610126197));
#51817=CARTESIAN_POINT('Ctrl Pts',(-90.7370004707867,36.4654243996764,111.106661603004));
#51818=CARTESIAN_POINT('Ctrl Pts',(-89.2987752110399,38.9009627605923,110.948713079812));
#51819=CARTESIAN_POINT('Ctrl Pts',(-86.4731463591935,39.0280870922405,110.790764556619));
#51820=CARTESIAN_POINT('Ctrl Pts',(-84.8220256573987,36.7315376305268,110.632816033427));
#51821=CARTESIAN_POINT('Ctrl Pts',(-85.8424340298206,34.0935259237314,110.474867510234));
#51822=CARTESIAN_POINT('Ctrl Pts',(-88.6091982386503,33.5058569595565,110.316918987042));
#51823=CARTESIAN_POINT('Ctrl Pts',(-90.6137773248237,35.5013523051125,110.158970463849));
#51824=CARTESIAN_POINT('Ctrl Pts',(-90.0386803938207,38.270757040499,110.001021940657));
#51825=CARTESIAN_POINT('Ctrl Pts',(-87.4053303496102,39.303136079331,109.843073417464));
#51826=CARTESIAN_POINT('Ctrl Pts',(-85.1013055723159,37.6624628286712,109.685124894272));
#51827=CARTESIAN_POINT('Ctrl Pts',(-85.2155952851076,34.8362856550028,109.52717637108));
#51828=CARTESIAN_POINT('Ctrl Pts',(-87.6445764169031,33.3870137992084,109.369227847887));
#51829=CARTESIAN_POINT('Ctrl Pts',(-90.1859657821869,34.6286572518108,109.211279324695));
#51830=CARTESIAN_POINT('Ctrl Pts',(-90.5355626637006,37.435457145156,109.053330801502));
#51831=CARTESIAN_POINT('Ctrl Pts',(-88.3763987621381,39.2625703208859,108.89538227831));
#51832=CARTESIAN_POINT('Ctrl Pts',(-85.6661211660339,38.4534151247791,108.737433755117));
#51833=CARTESIAN_POINT('Ctrl Pts',(-84.8620585136285,35.7416150217957,108.579485231925));
#51834=CARTESIAN_POINT('Ctrl Pts',(-86.6932250808741,33.5859033054787,108.421536708732));
#51835=CARTESIAN_POINT('Ctrl Pts',(-89.49936786246,33.9407434892909,108.26358818554));
#51836=CARTESIAN_POINT('Ctrl Pts',(-90.7362219186059,36.4845253391441,108.105639662347));
#51837=CARTESIAN_POINT('Ctrl Pts',(-89.2824117093597,38.9106477146993,107.947691139155));
#51838=CARTESIAN_POINT('Ctrl Pts',(-86.4559755055092,39.0198953412964,107.789742615962));
#51839=CARTESIAN_POINT('Ctrl Pts',(-84.8197364175027,36.7122375641654,107.63179409277));
#51840=CARTESIAN_POINT('Ctrl Pts',(-85.8568535917958,34.0819712089066,107.473845569577));
#51841=CARTESIAN_POINT('Ctrl Pts',(-88.6277561760423,33.5097261855478,107.315897046385));
#51842=CARTESIAN_POINT('Ctrl Pts',(-90.6185557892874,35.5228949088443,107.157948523193));
#51843=CARTESIAN_POINT('Ctrl Pts',(-90.2232169715586,37.3579260718377,107.052649507731));
#51844=CARTESIAN_POINT('Ctrl Pts',(-89.6820215852368,37.9909132780591,107.));
#51845=CARTESIAN_POINT('Ctrl Pts',(-90.2835503128821,36.3566878611388,121.112583302492));
#51846=CARTESIAN_POINT('Ctrl Pts',(-90.2854631783966,36.64824070958,121.094195056371));
#51847=CARTESIAN_POINT('Ctrl Pts',(-90.2385918845246,36.9391987080589,121.07580681025));
#51848=CARTESIAN_POINT('Ctrl Pts',(-90.1402210231293,37.211554596073,121.05741856413));
#51849=CARTESIAN_POINT('Ctrl Pts',(-89.858564067186,37.9913681431261,121.004769056399));
#51850=CARTESIAN_POINT('Ctrl Pts',(-89.1547135596339,38.6186815535308,120.952119548668));
#51851=CARTESIAN_POINT('Ctrl Pts',(-88.3477628848113,38.8091253463374,120.899470040937));
#51852=CARTESIAN_POINT('Ctrl Pts',(-87.5408122099887,38.9995691391441,120.846820533206));
#51853=CARTESIAN_POINT('Ctrl Pts',(-86.6307613678957,38.7531433143527,120.794171025476));
#51854=CARTESIAN_POINT('Ctrl Pts',(-86.0301615238396,38.1815547009635,120.741521517745));
#51855=CARTESIAN_POINT('Ctrl Pts',(-85.4295616797834,37.6099660875744,120.688872010014));
#51856=CARTESIAN_POINT('Ctrl Pts',(-85.1384128337641,36.7132146855875,120.636222502283));
#51857=CARTESIAN_POINT('Ctrl Pts',(-85.2887060701901,35.8978323016798,120.583572994552));
#51858=CARTESIAN_POINT('Ctrl Pts',(-85.4389993066161,35.0824499177722,120.530923486821));
#51859=CARTESIAN_POINT('Ctrl Pts',(-86.0307346254874,34.3484365519437,120.478273979091));
#51860=CARTESIAN_POINT('Ctrl Pts',(-86.7956562708989,34.0285444478597,120.42562447136));
#51861=CARTESIAN_POINT('Ctrl Pts',(-87.5605779163104,33.7086523437757,120.372974963629));
#51862=CARTESIAN_POINT('Ctrl Pts',(-88.4986858882622,33.8028815014362,120.320325455898));
#51863=CARTESIAN_POINT('Ctrl Pts',(-89.1847039557785,34.268515320645,120.267675948167));
#51864=CARTESIAN_POINT('Ctrl Pts',(-89.8583180860134,34.7257299844947,120.215978399609));
#51865=CARTESIAN_POINT('Ctrl Pts',(-90.2888760052472,35.5410399476632,120.16428085105));
#51866=CARTESIAN_POINT('Ctrl Pts',(-90.2901412986672,36.3551993258176,120.112583302492));
#51867=CARTESIAN_POINT('Ctrl Pts',(-88.5623548711056,33.385703120938,122.));
#51868=CARTESIAN_POINT('Ctrl Pts',(-88.655404902989,33.4197412382527,122.));
#51869=CARTESIAN_POINT('Ctrl Pts',(-88.746389770168,33.4585480581623,122.));
#51870=CARTESIAN_POINT('Ctrl Pts',(-88.8351009878334,33.5017952570346,122.));
#51871=CARTESIAN_POINT('Ctrl Pts',(-88.9257791769406,33.5460013651335,122.));
#51872=CARTESIAN_POINT('Ctrl Pts',(-89.0140824405661,33.5948475625466,122.));
#51873=CARTESIAN_POINT('Ctrl Pts',(-89.099759199117,33.6480287402599,122.));
#51874=CARTESIAN_POINT('Ctrl Pts',(-89.1821906340797,33.6991954844978,122.));
#51875=CARTESIAN_POINT('Ctrl Pts',(-89.2621910564892,33.7543758980026,122.));
#51876=CARTESIAN_POINT('Ctrl Pts',(-89.3395034395237,33.8133282931028,122.));
#51877=CARTESIAN_POINT('Ctrl Pts',(-89.407151774679,33.8649116388154,122.));
#51878=CARTESIAN_POINT('Ctrl Pts',(-89.472741789452,33.9193836052977,122.));
#51879=CARTESIAN_POINT('Ctrl Pts',(-89.5360766751279,33.9765949798929,122.));
#51880=CARTESIAN_POINT('Ctrl Pts',(-89.5502131428364,33.9893646682076,122.));
#51881=CARTESIAN_POINT('Ctrl Pts',(-89.56423990469,34.0022735672698,122.));
#51882=CARTESIAN_POINT('Ctrl Pts',(-89.5781351874061,34.0153014850048,122.));
#51883=CARTESIAN_POINT('Ctrl Pts',(-89.650565279181,34.0832103787249,122.));
#51884=CARTESIAN_POINT('Ctrl Pts',(-89.7195296835776,34.1544411891477,122.));
#51885=CARTESIAN_POINT('Ctrl Pts',(-89.7847884509537,34.2287031921864,122.));
#51886=CARTESIAN_POINT('Ctrl Pts',(-89.8496881991125,34.3025566449677,122.));
#51887=CARTESIAN_POINT('Ctrl Pts',(-89.9109234574517,34.3794088270275,122.));
#51888=CARTESIAN_POINT('Ctrl Pts',(-89.9682146052408,34.4590005543629,122.));
#51889=CARTESIAN_POINT('Ctrl Pts',(-90.0233775150845,34.5356356271226,122.));
#51890=CARTESIAN_POINT('Ctrl Pts',(-90.0748840644318,34.6148112269046,122.));
#51891=CARTESIAN_POINT('Ctrl Pts',(-90.1224398052449,34.6963095794444,122.));
#51892=CARTESIAN_POINT('Ctrl Pts',(-90.142386136171,34.7304924789619,122.));
#51893=CARTESIAN_POINT('Ctrl Pts',(-90.1616368636099,34.7650841083823,122.));
#51894=CARTESIAN_POINT('Ctrl Pts',(-90.180167677375,34.8000686960743,122.));
#51895=CARTESIAN_POINT('Ctrl Pts',(-90.1930502182209,34.8243898287366,122.));
#51896=CARTESIAN_POINT('Ctrl Pts',(-90.2055847945378,34.8489008796607,122.));
#51897=CARTESIAN_POINT('Ctrl Pts',(-90.2177627724607,34.8735965555594,122.));
#51898=CARTESIAN_POINT('Ctrl Pts',(-90.2256711134462,34.8896338506758,122.));
#51899=CARTESIAN_POINT('Ctrl Pts',(-90.2334301790788,34.9057516180668,122.));
#51900=CARTESIAN_POINT('Ctrl Pts',(-90.241027428963,34.9219262186558,122.));
#51901=CARTESIAN_POINT('Ctrl Pts',(-90.2831477278551,35.0116006431706,122.));
#51902=CARTESIAN_POINT('Ctrl Pts',(-90.3203691942033,35.1031586544706,122.));
#51903=CARTESIAN_POINT('Ctrl Pts',(-90.3524005445713,35.1963278865285,122.));
#51904=CARTESIAN_POINT('Ctrl Pts',(-90.3822802989988,35.2832387954382,122.));
#51905=CARTESIAN_POINT('Ctrl Pts',(-90.4076436024182,35.3715525302143,122.));
#51906=CARTESIAN_POINT('Ctrl Pts',(-90.4282034771338,35.4610567033496,122.));
#51907=CARTESIAN_POINT('Ctrl Pts',(-90.4296839626272,35.4675017635338,122.));
#51908=CARTESIAN_POINT('Ctrl Pts',(-90.4311395187566,35.4739529975641,122.));
#51909=CARTESIAN_POINT('Ctrl Pts',(-90.4325700277436,35.4804103264538,122.));
#51910=CARTESIAN_POINT('Ctrl Pts',(-90.4531762477541,35.5734269666833,122.));
#51911=CARTESIAN_POINT('Ctrl Pts',(-90.4685894434994,35.6677092665185,122.));
#51912=CARTESIAN_POINT('Ctrl Pts',(-90.4788865349184,35.7628493605361,122.));
#51913=CARTESIAN_POINT('Ctrl Pts',(-90.484683054651,35.8164063709481,122.));
#51914=CARTESIAN_POINT('Ctrl Pts',(-90.4888574145047,35.8702350170487,122.));
#51915=CARTESIAN_POINT('Ctrl Pts',(-90.4914165740776,35.9242599040958,122.));
#51916=CARTESIAN_POINT('Ctrl Pts',(-90.4920774570878,35.9382114100347,122.));
#51917=CARTESIAN_POINT('Ctrl Pts',(-90.4926305034956,35.9521754040169,122.));
#51918=CARTESIAN_POINT('Ctrl Pts',(-90.4930755917552,35.9661372181595,122.));
#51919=CARTESIAN_POINT('Ctrl Pts',(-90.4960470047878,36.0593464089312,122.));
#51920=CARTESIAN_POINT('Ctrl Pts',(-90.4942192639962,36.152613832859,122.));
#51921=CARTESIAN_POINT('Ctrl Pts',(-90.4877272636018,36.2455644111571,122.));
#51922=CARTESIAN_POINT('Ctrl Pts',(-90.481224468874,36.3386695395895,122.));
#51923=CARTESIAN_POINT('Ctrl Pts',(-90.4700415130326,36.4314577475258,122.));
#51924=CARTESIAN_POINT('Ctrl Pts',(-90.4542630315823,36.5235399863453,122.));
#51925=CARTESIAN_POINT('Ctrl Pts',(-90.4387101459247,36.6143056621148,122.));
#51926=CARTESIAN_POINT('Ctrl Pts',(-90.4186917450187,36.7043862559761,122.));
#51927=CARTESIAN_POINT('Ctrl Pts',(-90.3942458608461,36.7933839699538,122.));
#51928=CARTESIAN_POINT('Ctrl Pts',(-90.3851470966912,36.8265089411795,122.));
#51929=CARTESIAN_POINT('Ctrl Pts',(-90.3754345818515,36.8594835809755,122.));
#51930=CARTESIAN_POINT('Ctrl Pts',(-90.3651089158779,36.8922861120309,122.));
#51931=CARTESIAN_POINT('Ctrl Pts',(-90.3581143964109,36.9145062712557,122.));
#51932=CARTESIAN_POINT('Ctrl Pts',(-90.3508385119144,36.9366474415144,122.));
#51933=CARTESIAN_POINT('Ctrl Pts',(-90.3432812696287,36.9587026404511,122.));
#51934=CARTESIAN_POINT('Ctrl Pts',(-90.3387652071146,36.971882402776,122.));
#51935=CARTESIAN_POINT('Ctrl Pts',(-90.3341490168439,36.9850302917945,122.));
#51936=CARTESIAN_POINT('Ctrl Pts',(-90.3294361706385,36.9981356694608,122.));
#51937=CARTESIAN_POINT('Ctrl Pts',(-90.2978044186066,37.0860965403558,122.));
#51938=CARTESIAN_POINT('Ctrl Pts',(-90.2617834495289,37.1722596645947,122.));
#51939=CARTESIAN_POINT('Ctrl Pts',(-90.2214378271335,37.2562107993322,122.));
#51940=CARTESIAN_POINT('Ctrl Pts',(-90.1911786103369,37.3191741503854,122.));
#51941=CARTESIAN_POINT('Ctrl Pts',(-90.1584857287241,37.3808927654021,122.));
#51942=CARTESIAN_POINT('Ctrl Pts',(-90.1233704583289,37.4411763545704,122.));
#51943=CARTESIAN_POINT('Ctrl Pts',(-90.1099010949563,37.4642996726816,122.));
#51944=CARTESIAN_POINT('Ctrl Pts',(-90.0960751912912,37.4872116937309,122.));
#51945=CARTESIAN_POINT('Ctrl Pts',(-90.0818929032749,37.5099010346059,122.));
#51946=CARTESIAN_POINT('Ctrl Pts',(-90.0717687163118,37.5260980776235,122.));
#51947=CARTESIAN_POINT('Ctrl Pts',(-90.0614620799691,37.5421827090904,122.));
#51948=CARTESIAN_POINT('Ctrl Pts',(-90.0509831258029,37.5581357839754,122.));
#51949=CARTESIAN_POINT('Ctrl Pts',(-90.0037965482649,37.6299722471464,122.));
#51950=CARTESIAN_POINT('Ctrl Pts',(-89.9530750443141,37.6992152601097,122.));
#51951=CARTESIAN_POINT('Ctrl Pts',(-89.8988515052545,37.7655128239611,122.));
#51952=CARTESIAN_POINT('Ctrl Pts',(-89.8500550823629,37.8251748087463,122.));
#51953=CARTESIAN_POINT('Ctrl Pts',(-89.7984219626668,37.882451366736,122.));
#51954=CARTESIAN_POINT('Ctrl Pts',(-89.7439556248374,37.9370561588495,122.));
#51955=CARTESIAN_POINT('Ctrl Pts',(-89.7248730539468,37.9561872379343,122.));
#51956=CARTESIAN_POINT('Ctrl Pts',(-89.7054425381007,37.9749900687628,122.));
#51957=CARTESIAN_POINT('Ctrl Pts',(-89.6856746522268,37.9934601639124,122.));
#51958=CARTESIAN_POINT('Origin',(-87.7685555885722,36.3549260746835,114.));
#51959=CARTESIAN_POINT('Origin',(36.3549260746835,-87.7685555885722,106.));
#51960=CARTESIAN_POINT('Origin',(-87.7685555885722,-36.3549260746835,106.));
#51961=CARTESIAN_POINT('Origin',(-36.3549260746835,87.7685555885722,106.));
#51962=CARTESIAN_POINT('Origin',(87.7685555885722,36.3549260746835,106.));
#51963=CARTESIAN_POINT('Origin',(36.3549260746835,87.7685555885722,106.));
#51964=CARTESIAN_POINT('Origin',(-87.7685555885722,36.3549260746835,106.));
#51965=CARTESIAN_POINT('Origin',(-36.3549260746835,-87.7685555885722,106.));
#51966=CARTESIAN_POINT('Origin',(87.7685555885722,-36.3549260746835,106.));
#51967=CARTESIAN_POINT('Origin',(-81.317279836453,-81.3172798364529,5.));
#51968=CARTESIAN_POINT('',(-86.817279836453,-81.3172798364529,10.));
#51969=CARTESIAN_POINT('Origin',(-81.317279836453,-81.3172798364529,10.));
#51970=CARTESIAN_POINT('',(-86.817279836453,-81.3172798364529,0.));
#51971=CARTESIAN_POINT('',(-86.817279836453,-81.3172798364529,5.));
#51972=CARTESIAN_POINT('Origin',(-81.317279836453,-81.3172798364529,0.));
#51973=CARTESIAN_POINT('Origin',(81.317279836453,81.3172798364529,5.));
#51974=CARTESIAN_POINT('',(75.817279836453,81.3172798364529,10.));
#51975=CARTESIAN_POINT('Origin',(81.317279836453,81.3172798364529,10.));
#51976=CARTESIAN_POINT('',(75.817279836453,81.3172798364529,0.));
#51977=CARTESIAN_POINT('',(75.817279836453,81.3172798364529,5.));
#51978=CARTESIAN_POINT('Origin',(81.317279836453,81.3172798364529,0.));
#51979=CARTESIAN_POINT('Origin',(-81.3172798364529,81.317279836453,5.));
#51980=CARTESIAN_POINT('',(-86.817279836453,81.317279836453,10.));
#51981=CARTESIAN_POINT('Origin',(-81.3172798364529,81.317279836453,10.));
#51982=CARTESIAN_POINT('',(-86.817279836453,81.317279836453,0.));
#51983=CARTESIAN_POINT('',(-86.817279836453,81.317279836453,5.));
#51984=CARTESIAN_POINT('Origin',(-81.3172798364529,81.317279836453,0.));
#51985=CARTESIAN_POINT('Origin',(81.3172798364529,-81.317279836453,5.));
#51986=CARTESIAN_POINT('',(75.817279836453,-81.317279836453,10.));
#51987=CARTESIAN_POINT('Origin',(81.3172798364529,-81.317279836453,10.));
#51988=CARTESIAN_POINT('',(75.817279836453,-81.317279836453,0.));
#51989=CARTESIAN_POINT('',(75.817279836453,-81.317279836453,5.));
#51990=CARTESIAN_POINT('Origin',(81.3172798364529,-81.317279836453,0.));
#51991=CARTESIAN_POINT('Origin',(0.,0.,6.));
#51992=CARTESIAN_POINT('',(-18.,2.20436423846524E-15,10.));
#51993=CARTESIAN_POINT('Origin',(0.,0.,10.));
#51994=CARTESIAN_POINT('',(-18.,2.20436423846524E-15,2.));
#51995=CARTESIAN_POINT('',(-18.,2.20436423846524E-15,6.));
#51996=CARTESIAN_POINT('Origin',(0.,0.,2.));
#51997=CARTESIAN_POINT('Origin',(0.,0.,2.));
#51998=CARTESIAN_POINT('',(-17.,-2.0818995585505E-15,2.));
#51999=CARTESIAN_POINT('Origin',(0.,0.,2.));
#52000=CARTESIAN_POINT('Origin',(0.,0.,10.));
#52001=CARTESIAN_POINT('',(-90.,-1.10218211923262E-14,122.));
#52002=CARTESIAN_POINT('Origin',(0.,0.,122.));
#52003=CARTESIAN_POINT('',(-90.,-1.10218211923262E-14,10.));
#52004=CARTESIAN_POINT('',(-90.,-1.10218211923262E-14,10.));
#52005=CARTESIAN_POINT('',(-90.,-1.10218211923262E-14,10.));
#52006=CARTESIAN_POINT('',(-90.,-1.10218211923262E-14,10.));
#52007=CARTESIAN_POINT('',(-90.,-1.10218211923262E-14,10.));
#52008=CARTESIAN_POINT('Origin',(0.,0.,10.));
#52009=CARTESIAN_POINT('Origin',(0.,0.,10.));
#52010=CARTESIAN_POINT('',(-100.,-1.22464679914735E-14,122.));
#52011=CARTESIAN_POINT('Origin',(0.,0.,122.));
#52012=CARTESIAN_POINT('',(-100.,-1.22464679914735E-14,10.));
#52013=CARTESIAN_POINT('',(-100.,-1.22464679914735E-14,10.));
#52014=CARTESIAN_POINT('',(-100.,-1.22464679914735E-14,10.));
#52015=CARTESIAN_POINT('',(-100.,-1.22464679914735E-14,10.));
#52016=CARTESIAN_POINT('',(-100.,-1.22464679914735E-14,10.));
#52017=CARTESIAN_POINT('Origin',(0.,0.,10.));
#52018=CARTESIAN_POINT('Origin',(0.,0.,122.));
#52019=CARTESIAN_POINT('Origin',(0.,0.,10.));
#52020=CARTESIAN_POINT('',(-140.,1.71450551880629E-14,10.));
#52021=CARTESIAN_POINT('Origin',(0.,0.,10.));
#52022=CARTESIAN_POINT('Origin',(0.,0.,0.));
#52023=CARTESIAN_POINT('',(-17.,-2.0818995585505E-15,0.));
#52024=CARTESIAN_POINT('',(-17.,-2.0818995585505E-15,0.));
#52025=CARTESIAN_POINT('Origin',(0.,0.,0.));
#52026=CARTESIAN_POINT('Origin',(0.,0.,0.));
#52027=CARTESIAN_POINT('',(-140.,1.71450551880629E-14,0.));
#52028=CARTESIAN_POINT('',(-140.,-1.71450551880629E-14,0.));
#52029=CARTESIAN_POINT('Origin',(0.,0.,0.));
#52030=CARTESIAN_POINT('Origin',(0.,0.,10.));
#52031=CARTESIAN_POINT('Origin',(0.,0.,0.));
#52032=CARTESIAN_POINT('',(0.,0.,0.));
#52033=CARTESIAN_POINT('Origin',(0.,-86.,4.));
#52034=CARTESIAN_POINT('',(0.,-90.,6.));
#52035=CARTESIAN_POINT('',(0.,-90.,2.));
#52036=CARTESIAN_POINT('Ctrl Pts',(-2.08166817117217E-16,-90.,6.));
#52037=CARTESIAN_POINT('Ctrl Pts',(0.251133328053566,-90.,6.));
#52038=CARTESIAN_POINT('Ctrl Pts',(0.519000232590761,-89.9988407998655,
5.94980925763969));
#52039=CARTESIAN_POINT('Ctrl Pts',(1.01175644254643,-89.9946501491172,5.74569936791146));
#52040=CARTESIAN_POINT('Ctrl Pts',(1.23664644642618,-89.9916787455059,5.59178067832001));
#52041=CARTESIAN_POINT('Ctrl Pts',(1.59178067978086,-89.9860976603374,5.23664644496533));
#52042=CARTESIAN_POINT('Ctrl Pts',(1.74569936855887,-89.9831259365723,5.01175644187864));
#52043=CARTESIAN_POINT('Ctrl Pts',(1.94980925677131,-89.9789345539658,4.51900023379203));
#52044=CARTESIAN_POINT('Ctrl Pts',(2.,-89.9777750336159,4.25113333011964));
#52045=CARTESIAN_POINT('Ctrl Pts',(2.,-89.9777750336159,3.74886666988036));
#52046=CARTESIAN_POINT('Ctrl Pts',(1.94980925677131,-89.9789345539658,3.48099976620797));
#52047=CARTESIAN_POINT('Ctrl Pts',(1.74569936855887,-89.9831259365723,2.98824355812136));
#52048=CARTESIAN_POINT('Ctrl Pts',(1.59178067978086,-89.9860976603374,2.76335355503467));
#52049=CARTESIAN_POINT('Ctrl Pts',(1.23664644642618,-89.9916787455059,2.40821932167999));
#52050=CARTESIAN_POINT('Ctrl Pts',(1.01175644254643,-89.9946501491172,2.25430063208854));
#52051=CARTESIAN_POINT('Ctrl Pts',(0.519000232590762,-89.9988407998655,
2.05019074236031));
#52052=CARTESIAN_POINT('Ctrl Pts',(0.251133328053567,-90.,2.));
#52053=CARTESIAN_POINT('Ctrl Pts',(4.16333634234434E-16,-90.,2.));
#52054=CARTESIAN_POINT('',(2.44929359829471E-16,-82.,6.));
#52055=CARTESIAN_POINT('',(2.44929359829471E-16,-86.,6.));
#52056=CARTESIAN_POINT('Origin',(0.,-82.,4.));
#52057=CARTESIAN_POINT('Ctrl Pts',(4.16333634234434E-16,-90.,2.));
#52058=CARTESIAN_POINT('Ctrl Pts',(-0.251133328053566,-90.,2.));
#52059=CARTESIAN_POINT('Ctrl Pts',(-0.519000232590761,-89.9988407998655,
2.05019074236031));
#52060=CARTESIAN_POINT('Ctrl Pts',(-1.01175644254643,-89.9946501491172,
2.25430063208854));
#52061=CARTESIAN_POINT('Ctrl Pts',(-1.23664644642618,-89.9916787455059,
2.40821932167999));
#52062=CARTESIAN_POINT('Ctrl Pts',(-1.59178067978086,-89.9860976603374,
2.76335355503467));
#52063=CARTESIAN_POINT('Ctrl Pts',(-1.74569936855887,-89.9831259365723,
2.98824355812136));
#52064=CARTESIAN_POINT('Ctrl Pts',(-1.94980925677131,-89.9789345539658,
3.48099976620797));
#52065=CARTESIAN_POINT('Ctrl Pts',(-2.,-89.9777750336159,3.74886666988036));
#52066=CARTESIAN_POINT('Ctrl Pts',(-2.,-89.9777750336159,4.));
#52067=CARTESIAN_POINT('Ctrl Pts',(-2.,-89.9777750336159,4.25113333011964));
#52068=CARTESIAN_POINT('Ctrl Pts',(-1.94980925677131,-89.9789345539658,
4.51900023379203));
#52069=CARTESIAN_POINT('Ctrl Pts',(-1.74569936855887,-89.9831259365723,
5.01175644187864));
#52070=CARTESIAN_POINT('Ctrl Pts',(-1.59178067978086,-89.9860976603374,
5.23664644496533));
#52071=CARTESIAN_POINT('Ctrl Pts',(-1.23664644642618,-89.9916787455059,
5.59178067832001));
#52072=CARTESIAN_POINT('Ctrl Pts',(-1.01175644254643,-89.9946501491172,
5.74569936791146));
#52073=CARTESIAN_POINT('Ctrl Pts',(-0.519000232590762,-89.9988407998655,
5.94980925763969));
#52074=CARTESIAN_POINT('Ctrl Pts',(-0.251133328053566,-90.,6.));
#52075=CARTESIAN_POINT('Ctrl Pts',(-2.08166817117217E-16,-90.,6.));
#52076=CARTESIAN_POINT('Origin',(0.,-82.,4.));
#52077=CARTESIAN_POINT('Origin',(0.,86.,4.));
#52078=CARTESIAN_POINT('',(0.,90.,6.));
#52079=CARTESIAN_POINT('',(0.,90.,2.));
#52080=CARTESIAN_POINT('Ctrl Pts',(6.93889390390723E-17,90.,6.));
#52081=CARTESIAN_POINT('Ctrl Pts',(-0.251133328053566,90.,6.));
#52082=CARTESIAN_POINT('Ctrl Pts',(-0.519000232590761,89.9988407998655,
5.94980925763969));
#52083=CARTESIAN_POINT('Ctrl Pts',(-1.01175644254643,89.9946501491172,5.74569936791146));
#52084=CARTESIAN_POINT('Ctrl Pts',(-1.23664644642618,89.9916787455059,5.59178067832001));
#52085=CARTESIAN_POINT('Ctrl Pts',(-1.59178067978086,89.9860976603374,5.23664644496533));
#52086=CARTESIAN_POINT('Ctrl Pts',(-1.74569936855887,89.9831259365723,5.01175644187864));
#52087=CARTESIAN_POINT('Ctrl Pts',(-1.94980925677131,89.9789345539658,4.51900023379203));
#52088=CARTESIAN_POINT('Ctrl Pts',(-2.,89.9777750336159,4.25113333011964));
#52089=CARTESIAN_POINT('Ctrl Pts',(-2.,89.9777750336159,3.74886666988036));
#52090=CARTESIAN_POINT('Ctrl Pts',(-1.94980925677131,89.9789345539658,3.48099976620797));
#52091=CARTESIAN_POINT('Ctrl Pts',(-1.74569936855887,89.9831259365723,2.98824355812136));
#52092=CARTESIAN_POINT('Ctrl Pts',(-1.59178067978086,89.9860976603374,2.76335355503467));
#52093=CARTESIAN_POINT('Ctrl Pts',(-1.23664644642618,89.9916787455059,2.40821932167999));
#52094=CARTESIAN_POINT('Ctrl Pts',(-1.01175644254643,89.9946501491172,2.25430063208854));
#52095=CARTESIAN_POINT('Ctrl Pts',(-0.519000232590762,89.9988407998655,
2.05019074236031));
#52096=CARTESIAN_POINT('Ctrl Pts',(-0.251133328053567,90.,2.));
#52097=CARTESIAN_POINT('Ctrl Pts',(-4.16333634234434E-16,90.,2.));
#52098=CARTESIAN_POINT('Ctrl Pts',(-3.46944695195361E-16,90.,2.));
#52099=CARTESIAN_POINT('Ctrl Pts',(0.251133328053566,90.,2.));
#52100=CARTESIAN_POINT('Ctrl Pts',(0.519000232590762,89.9988407998655,2.05019074236031));
#52101=CARTESIAN_POINT('Ctrl Pts',(1.01175644254643,89.9946501491172,2.25430063208854));
#52102=CARTESIAN_POINT('Ctrl Pts',(1.23664644642618,89.9916787455059,2.40821932167999));
#52103=CARTESIAN_POINT('Ctrl Pts',(1.59178067978086,89.9860976603374,2.76335355503467));
#52104=CARTESIAN_POINT('Ctrl Pts',(1.74569936855886,89.9831259365723,2.98824355812136));
#52105=CARTESIAN_POINT('Ctrl Pts',(1.94980925677131,89.9789345539658,3.48099976620797));
#52106=CARTESIAN_POINT('Ctrl Pts',(2.,89.9777750336159,3.74886666988036));
#52107=CARTESIAN_POINT('Ctrl Pts',(2.,89.9777750336159,4.));
#52108=CARTESIAN_POINT('Ctrl Pts',(2.,89.9777750336159,4.25113333011964));
#52109=CARTESIAN_POINT('Ctrl Pts',(1.94980925677131,89.9789345539658,4.51900023379203));
#52110=CARTESIAN_POINT('Ctrl Pts',(1.74569936855887,89.9831259365723,5.01175644187864));
#52111=CARTESIAN_POINT('Ctrl Pts',(1.59178067978086,89.9860976603374,5.23664644496533));
#52112=CARTESIAN_POINT('Ctrl Pts',(1.23664644642618,89.9916787455059,5.59178067832001));
#52113=CARTESIAN_POINT('Ctrl Pts',(1.01175644254643,89.9946501491172,5.74569936791146));
#52114=CARTESIAN_POINT('Ctrl Pts',(0.519000232590761,89.9988407998655,5.94980925763969));
#52115=CARTESIAN_POINT('Ctrl Pts',(0.251133328053566,90.,6.));
#52116=CARTESIAN_POINT('Ctrl Pts',(-6.93889390390723E-17,90.,6.));
#52117=CARTESIAN_POINT('',(2.44929359829471E-16,82.,2.));
#52118=CARTESIAN_POINT('',(2.44929359829471E-16,86.,2.));
#52119=CARTESIAN_POINT('Origin',(0.,82.,4.));
#52120=CARTESIAN_POINT('Origin',(0.,82.,4.));
#52121=CARTESIAN_POINT('Origin',(-86.,0.,4.));
#52122=CARTESIAN_POINT('',(-90.,0.,6.));
#52123=CARTESIAN_POINT('',(-90.,0.,2.));
#52124=CARTESIAN_POINT('Ctrl Pts',(-90.,4.16333634234434E-16,6.));
#52125=CARTESIAN_POINT('Ctrl Pts',(-90.,-0.251133328053566,6.));
#52126=CARTESIAN_POINT('Ctrl Pts',(-89.9988407998655,-0.519000232590761,
5.94980925763969));
#52127=CARTESIAN_POINT('Ctrl Pts',(-89.9946501491172,-1.01175644254643,
5.74569936791146));
#52128=CARTESIAN_POINT('Ctrl Pts',(-89.9916787455059,-1.23664644642618,
5.59178067832001));
#52129=CARTESIAN_POINT('Ctrl Pts',(-89.9860976603374,-1.59178067978086,
5.23664644496533));
#52130=CARTESIAN_POINT('Ctrl Pts',(-89.9831259365723,-1.74569936855887,
5.01175644187864));
#52131=CARTESIAN_POINT('Ctrl Pts',(-89.9789345539658,-1.94980925677131,
4.51900023379203));
#52132=CARTESIAN_POINT('Ctrl Pts',(-89.9777750336159,-2.,4.25113333011964));
#52133=CARTESIAN_POINT('Ctrl Pts',(-89.9777750336159,-2.,3.74886666988036));
#52134=CARTESIAN_POINT('Ctrl Pts',(-89.9789345539658,-1.94980925677131,
3.48099976620797));
#52135=CARTESIAN_POINT('Ctrl Pts',(-89.9831259365723,-1.74569936855887,
2.98824355812136));
#52136=CARTESIAN_POINT('Ctrl Pts',(-89.9860976603374,-1.59178067978086,
2.76335355503467));
#52137=CARTESIAN_POINT('Ctrl Pts',(-89.9916787455059,-1.23664644642618,
2.40821932167999));
#52138=CARTESIAN_POINT('Ctrl Pts',(-89.9946501491172,-1.01175644254643,
2.25430063208854));
#52139=CARTESIAN_POINT('Ctrl Pts',(-89.9988407998655,-0.519000232590762,
2.05019074236031));
#52140=CARTESIAN_POINT('Ctrl Pts',(-90.,-0.251133328053567,2.));
#52141=CARTESIAN_POINT('Ctrl Pts',(-90.,-5.55111512312578E-16,2.));
#52142=CARTESIAN_POINT('',(-89.9777750336159,2.,4.));
#52143=CARTESIAN_POINT('Ctrl Pts',(-89.9777750336159,2.,4.));
#52144=CARTESIAN_POINT('Ctrl Pts',(-89.9777750336159,2.,4.25113333011964));
#52145=CARTESIAN_POINT('Ctrl Pts',(-89.9789345539658,1.94980925677131,4.51900023379203));
#52146=CARTESIAN_POINT('Ctrl Pts',(-89.9831259365723,1.74569936855887,5.01175644187864));
#52147=CARTESIAN_POINT('Ctrl Pts',(-89.9860976603374,1.59178067978086,5.23664644496533));
#52148=CARTESIAN_POINT('Ctrl Pts',(-89.9916787455059,1.23664644642618,5.59178067832001));
#52149=CARTESIAN_POINT('Ctrl Pts',(-89.9946501491172,1.01175644254643,5.74569936791146));
#52150=CARTESIAN_POINT('Ctrl Pts',(-89.9988407998655,0.519000232590762,
5.94980925763969));
#52151=CARTESIAN_POINT('Ctrl Pts',(-90.,0.251133328053567,6.));
#52152=CARTESIAN_POINT('Ctrl Pts',(-90.,2.77555756156289E-16,6.));
#52153=CARTESIAN_POINT('',(-82.,2.,4.));
#52154=CARTESIAN_POINT('',(-86.,2.,4.));
#52155=CARTESIAN_POINT('Origin',(-82.,0.,4.));
#52156=CARTESIAN_POINT('Ctrl Pts',(-90.,-4.85722573273506E-16,2.));
#52157=CARTESIAN_POINT('Ctrl Pts',(-90.,0.251133328053565,2.));
#52158=CARTESIAN_POINT('Ctrl Pts',(-89.9988407998655,0.519000232590761,
2.05019074236031));
#52159=CARTESIAN_POINT('Ctrl Pts',(-89.9946501491172,1.01175644254643,2.25430063208854));
#52160=CARTESIAN_POINT('Ctrl Pts',(-89.9916787455059,1.23664644642618,2.40821932167999));
#52161=CARTESIAN_POINT('Ctrl Pts',(-89.9860976603374,1.59178067978086,2.76335355503467));
#52162=CARTESIAN_POINT('Ctrl Pts',(-89.9831259365723,1.74569936855886,2.98824355812136));
#52163=CARTESIAN_POINT('Ctrl Pts',(-89.9789345539658,1.94980925677131,3.48099976620797));
#52164=CARTESIAN_POINT('Ctrl Pts',(-89.9777750336159,2.,3.74886666988036));
#52165=CARTESIAN_POINT('Ctrl Pts',(-89.9777750336159,2.,4.));
#52166=CARTESIAN_POINT('Origin',(-82.,0.,4.));
#52167=CARTESIAN_POINT('Origin',(86.,0.,4.));
#52168=CARTESIAN_POINT('',(90.,0.,6.));
#52169=CARTESIAN_POINT('',(90.,0.,2.));
#52170=CARTESIAN_POINT('Ctrl Pts',(90.,-4.16333634234434E-16,6.));
#52171=CARTESIAN_POINT('Ctrl Pts',(90.,0.251133328053566,6.));
#52172=CARTESIAN_POINT('Ctrl Pts',(89.9988407998655,0.519000232590761,5.94980925763969));
#52173=CARTESIAN_POINT('Ctrl Pts',(89.9946501491172,1.01175644254643,5.74569936791146));
#52174=CARTESIAN_POINT('Ctrl Pts',(89.9916787455059,1.23664644642618,5.59178067832001));
#52175=CARTESIAN_POINT('Ctrl Pts',(89.9860976603374,1.59178067978086,5.23664644496533));
#52176=CARTESIAN_POINT('Ctrl Pts',(89.9831259365723,1.74569936855887,5.01175644187864));
#52177=CARTESIAN_POINT('Ctrl Pts',(89.9789345539658,1.94980925677131,4.51900023379203));
#52178=CARTESIAN_POINT('Ctrl Pts',(89.9777750336159,2.,4.25113333011964));
#52179=CARTESIAN_POINT('Ctrl Pts',(89.9777750336159,2.,3.74886666988036));
#52180=CARTESIAN_POINT('Ctrl Pts',(89.9789345539658,1.94980925677131,3.48099976620797));
#52181=CARTESIAN_POINT('Ctrl Pts',(89.9831259365723,1.74569936855887,2.98824355812136));
#52182=CARTESIAN_POINT('Ctrl Pts',(89.9860976603374,1.59178067978086,2.76335355503467));
#52183=CARTESIAN_POINT('Ctrl Pts',(89.9916787455059,1.23664644642618,2.40821932167999));
#52184=CARTESIAN_POINT('Ctrl Pts',(89.9946501491172,1.01175644254643,2.25430063208854));
#52185=CARTESIAN_POINT('Ctrl Pts',(89.9988407998655,0.519000232590762,2.05019074236031));
#52186=CARTESIAN_POINT('Ctrl Pts',(90.,0.251133328053567,2.));
#52187=CARTESIAN_POINT('Ctrl Pts',(90.,5.55111512312578E-16,2.));
#52188=CARTESIAN_POINT('',(89.9777750336159,-2.,4.));
#52189=CARTESIAN_POINT('Ctrl Pts',(89.9777750336159,-2.,4.));
#52190=CARTESIAN_POINT('Ctrl Pts',(89.9777750336159,-2.,4.25113333011964));
#52191=CARTESIAN_POINT('Ctrl Pts',(89.9789345539658,-1.94980925677131,4.51900023379203));
#52192=CARTESIAN_POINT('Ctrl Pts',(89.9831259365723,-1.74569936855887,5.01175644187864));
#52193=CARTESIAN_POINT('Ctrl Pts',(89.9860976603374,-1.59178067978086,5.23664644496533));
#52194=CARTESIAN_POINT('Ctrl Pts',(89.9916787455059,-1.23664644642618,5.59178067832001));
#52195=CARTESIAN_POINT('Ctrl Pts',(89.9946501491172,-1.01175644254643,5.74569936791146));
#52196=CARTESIAN_POINT('Ctrl Pts',(89.9988407998655,-0.519000232590762,
5.94980925763969));
#52197=CARTESIAN_POINT('Ctrl Pts',(90.,-0.251133328053567,6.));
#52198=CARTESIAN_POINT('Ctrl Pts',(90.,-2.77555756156289E-16,6.));
#52199=CARTESIAN_POINT('',(82.,-2.,4.));
#52200=CARTESIAN_POINT('',(86.,-2.,4.));
#52201=CARTESIAN_POINT('Origin',(82.,0.,4.));
#52202=CARTESIAN_POINT('Ctrl Pts',(90.,4.85722573273506E-16,2.));
#52203=CARTESIAN_POINT('Ctrl Pts',(90.,-0.251133328053565,2.));
#52204=CARTESIAN_POINT('Ctrl Pts',(89.9988407998655,-0.519000232590761,
2.05019074236031));
#52205=CARTESIAN_POINT('Ctrl Pts',(89.9946501491172,-1.01175644254643,2.25430063208854));
#52206=CARTESIAN_POINT('Ctrl Pts',(89.9916787455059,-1.23664644642618,2.40821932167999));
#52207=CARTESIAN_POINT('Ctrl Pts',(89.9860976603374,-1.59178067978086,2.76335355503467));
#52208=CARTESIAN_POINT('Ctrl Pts',(89.9831259365723,-1.74569936855886,2.98824355812136));
#52209=CARTESIAN_POINT('Ctrl Pts',(89.9789345539658,-1.94980925677131,3.48099976620797));
#52210=CARTESIAN_POINT('Ctrl Pts',(89.9777750336159,-2.,3.74886666988036));
#52211=CARTESIAN_POINT('Ctrl Pts',(89.9777750336159,-2.,4.));
#52212=CARTESIAN_POINT('Origin',(82.,0.,4.));
#52213=CARTESIAN_POINT('Origin',(0.,0.,0.));
#52214=CARTESIAN_POINT('',(-18.,-2.20436423846524E-15,8.));
#52215=CARTESIAN_POINT('Origin',(0.,0.,8.));
#52216=CARTESIAN_POINT('',(-18.,-2.20436423846524E-15,0.));
#52217=CARTESIAN_POINT('',(-18.,-2.20436423846524E-15,0.));
#52218=CARTESIAN_POINT('Origin',(0.,0.,0.));
#52219=CARTESIAN_POINT('Origin',(0.,0.,0.));
#52220=CARTESIAN_POINT('',(-90.,-1.10218211923262E-14,8.));
#52221=CARTESIAN_POINT('Origin',(0.,0.,8.));
#52222=CARTESIAN_POINT('',(-90.,-1.10218211923262E-14,0.));
#52223=CARTESIAN_POINT('',(-90.,-1.10218211923262E-14,0.));
#52224=CARTESIAN_POINT('',(-90.,-1.10218211923262E-14,0.));
#52225=CARTESIAN_POINT('Origin',(0.,0.,0.));
#52226=CARTESIAN_POINT('Origin',(0.,0.,8.));
#52227=CARTESIAN_POINT('Origin',(0.,0.,0.));
#52228=CARTESIAN_POINT('',(0.,0.,0.));
#52229=CARTESIAN_POINT('Origin',(36.3549260746835,-87.7685555885722,4.));
#52230=CARTESIAN_POINT('',(32.8549260746835,-87.7685555885722,8.));
#52231=CARTESIAN_POINT('Origin',(36.3549260746835,-87.7685555885722,8.));
#52232=CARTESIAN_POINT('',(32.8549260746835,-87.7685555885722,0.));
#52233=CARTESIAN_POINT('',(32.8549260746835,-87.7685555885722,4.));
#52234=CARTESIAN_POINT('Origin',(36.3549260746835,-87.7685555885722,0.));
#52235=CARTESIAN_POINT('Origin',(-87.7685555885722,-36.3549260746835,4.));
#52236=CARTESIAN_POINT('',(-91.2685555885722,-36.3549260746835,8.));
#52237=CARTESIAN_POINT('Origin',(-87.7685555885722,-36.3549260746835,8.));
#52238=CARTESIAN_POINT('',(-91.2685555885722,-36.3549260746835,0.));
#52239=CARTESIAN_POINT('',(-91.2685555885722,-36.3549260746835,4.));
#52240=CARTESIAN_POINT('Origin',(-87.7685555885722,-36.3549260746835,0.));
#52241=CARTESIAN_POINT('Origin',(-36.3549260746835,87.7685555885722,4.));
#52242=CARTESIAN_POINT('',(-39.8549260746835,87.7685555885722,8.));
#52243=CARTESIAN_POINT('Origin',(-36.3549260746835,87.7685555885722,8.));
#52244=CARTESIAN_POINT('',(-39.8549260746835,87.7685555885722,0.));
#52245=CARTESIAN_POINT('',(-39.8549260746835,87.7685555885722,4.));
#52246=CARTESIAN_POINT('Origin',(-36.3549260746835,87.7685555885722,0.));
#52247=CARTESIAN_POINT('Origin',(87.7685555885722,36.3549260746835,4.));
#52248=CARTESIAN_POINT('',(84.2685555885723,36.3549260746835,8.));
#52249=CARTESIAN_POINT('Origin',(87.7685555885722,36.3549260746835,8.));
#52250=CARTESIAN_POINT('',(84.2685555885723,36.3549260746835,0.));
#52251=CARTESIAN_POINT('',(84.2685555885723,36.3549260746835,4.));
#52252=CARTESIAN_POINT('Origin',(87.7685555885722,36.3549260746835,0.));
#52253=CARTESIAN_POINT('Origin',(36.3549260746835,87.7685555885722,4.));
#52254=CARTESIAN_POINT('',(32.8549260746835,87.7685555885722,8.));
#52255=CARTESIAN_POINT('Origin',(36.3549260746835,87.7685555885722,8.));
#52256=CARTESIAN_POINT('',(32.8549260746835,87.7685555885722,0.));
#52257=CARTESIAN_POINT('',(32.8549260746835,87.7685555885722,4.));
#52258=CARTESIAN_POINT('Origin',(36.3549260746835,87.7685555885722,0.));
#52259=CARTESIAN_POINT('Origin',(-87.7685555885722,36.3549260746835,4.));
#52260=CARTESIAN_POINT('',(-91.2685555885722,36.3549260746835,8.));
#52261=CARTESIAN_POINT('Origin',(-87.7685555885722,36.3549260746835,8.));
#52262=CARTESIAN_POINT('',(-91.2685555885722,36.3549260746835,0.));
#52263=CARTESIAN_POINT('',(-91.2685555885722,36.3549260746835,4.));
#52264=CARTESIAN_POINT('Origin',(-87.7685555885722,36.3549260746835,0.));
#52265=CARTESIAN_POINT('Origin',(-36.3549260746835,-87.7685555885722,4.));
#52266=CARTESIAN_POINT('',(-39.8549260746835,-87.7685555885722,8.));
#52267=CARTESIAN_POINT('Origin',(-36.3549260746835,-87.7685555885722,8.));
#52268=CARTESIAN_POINT('',(-39.8549260746835,-87.7685555885722,0.));
#52269=CARTESIAN_POINT('',(-39.8549260746835,-87.7685555885722,4.));
#52270=CARTESIAN_POINT('Origin',(-36.3549260746835,-87.7685555885722,0.));
#52271=CARTESIAN_POINT('Origin',(87.7685555885722,-36.3549260746835,4.));
#52272=CARTESIAN_POINT('',(84.2685555885723,-36.3549260746835,8.));
#52273=CARTESIAN_POINT('Origin',(87.7685555885722,-36.3549260746835,8.));
#52274=CARTESIAN_POINT('',(84.2685555885723,-36.3549260746835,0.));
#52275=CARTESIAN_POINT('',(84.2685555885723,-36.3549260746835,4.));
#52276=CARTESIAN_POINT('Origin',(87.7685555885722,-36.3549260746835,0.));
#52277=CARTESIAN_POINT('Origin',(0.,0.,0.));
#52278=CARTESIAN_POINT('',(-18.,-2.20436423846524E-15,8.));
#52279=CARTESIAN_POINT('Origin',(0.,0.,8.));
#52280=CARTESIAN_POINT('',(-18.,-2.20436423846524E-15,0.));
#52281=CARTESIAN_POINT('',(-18.,-2.20436423846524E-15,0.));
#52282=CARTESIAN_POINT('Origin',(0.,0.,0.));
#52283=CARTESIAN_POINT('Origin',(0.,0.,0.));
#52284=CARTESIAN_POINT('',(-100.,-1.22464679914735E-14,8.));
#52285=CARTESIAN_POINT('Origin',(0.,0.,8.));
#52286=CARTESIAN_POINT('',(-100.,-1.22464679914735E-14,0.));
#52287=CARTESIAN_POINT('',(-100.,-1.22464679914735E-14,0.));
#52288=CARTESIAN_POINT('Origin',(0.,0.,0.));
#52289=CARTESIAN_POINT('Origin',(0.,0.,8.));
#52290=CARTESIAN_POINT('Origin',(0.,0.,0.));
#52291=CARTESIAN_POINT('',(0.,0.,0.));
#52292=CARTESIAN_POINT('Origin',(11.,-3.,42.));
#52293=CARTESIAN_POINT('',(7.41619848709566,-3.,30.));
#52294=CARTESIAN_POINT('',(7.41619848709566,-3.,42.));
#52295=CARTESIAN_POINT('',(7.41619848709566,-3.,20.));
#52296=CARTESIAN_POINT('',(5.,-3.,30.));
#52297=CARTESIAN_POINT('',(5.,-3.,30.));
#52298=CARTESIAN_POINT('',(5.,-3.,42.));
#52299=CARTESIAN_POINT('',(5.,-3.,42.));
#52300=CARTESIAN_POINT('',(5.,-3.,42.));
#52301=CARTESIAN_POINT('Origin',(8.,0.,42.));
#52302=CARTESIAN_POINT('',(7.41619848709566,3.,42.));
#52303=CARTESIAN_POINT('Origin',(0.,0.,42.));
#52304=CARTESIAN_POINT('',(5.,3.,42.));
#52305=CARTESIAN_POINT('',(5.,3.,42.));
#52306=CARTESIAN_POINT('',(11.,3.,42.));
#52307=CARTESIAN_POINT('Origin',(5.,3.,42.));
#52308=CARTESIAN_POINT('',(7.41619848709566,3.,30.));
#52309=CARTESIAN_POINT('',(7.41619848709566,3.,20.));
#52310=CARTESIAN_POINT('',(5.,3.,30.));
#52311=CARTESIAN_POINT('',(5.,3.,42.));
#52312=CARTESIAN_POINT('',(11.,3.,30.));
#52313=CARTESIAN_POINT('Origin',(5.,-3.,42.));
#52314=CARTESIAN_POINT('',(5.,3.,30.));
#52315=CARTESIAN_POINT('Origin',(8.,0.,30.));
#52316=CARTESIAN_POINT('Origin',(0.,0.,30.));
#52317=CARTESIAN_POINT('Origin',(0.,0.,44.5));
#52318=CARTESIAN_POINT('',(-7.,-8.57252759403147E-16,44.));
#52319=CARTESIAN_POINT('Origin',(0.,0.,44.));
#52320=CARTESIAN_POINT('',(-7.,-8.57252759403147E-16,45.));
#52321=CARTESIAN_POINT('',(-7.,-8.57252759403147E-16,44.5));
#52322=CARTESIAN_POINT('Origin',(0.,0.,45.));
#52323=CARTESIAN_POINT('Origin',(11.,0.,44.));
#52324=CARTESIAN_POINT('',(-8.,9.79717439317883E-16,44.));
#52325=CARTESIAN_POINT('Origin',(0.,0.,44.));
#52326=CARTESIAN_POINT('Origin',(7.,0.,45.));
#52327=CARTESIAN_POINT('',(-8.,-9.79717439317883E-16,45.));
#52328=CARTESIAN_POINT('Origin',(0.,0.,45.));
#52329=CARTESIAN_POINT('Origin',(0.,0.,20.));
#52330=CARTESIAN_POINT('',(-8.,-9.79717439317883E-16,46.));
#52331=CARTESIAN_POINT('Origin',(0.,0.,46.));
#52332=CARTESIAN_POINT('',(-8.,-9.79717439317883E-16,20.));
#52333=CARTESIAN_POINT('Origin',(0.,0.,-2.5));
#52334=CARTESIAN_POINT('',(-15.,-1.83697019872103E-15,-3.));
#52335=CARTESIAN_POINT('Origin',(0.,0.,-3.));
#52336=CARTESIAN_POINT('',(-15.,-1.83697019872103E-15,-2.));
#52337=CARTESIAN_POINT('',(-15.,-1.83697019872103E-15,-2.5));
#52338=CARTESIAN_POINT('Origin',(0.,0.,-2.));
#52339=CARTESIAN_POINT('Origin',(19.,0.,-3.));
#52340=CARTESIAN_POINT('',(-16.,1.95943487863577E-15,-3.));
#52341=CARTESIAN_POINT('Origin',(0.,0.,-3.));
#52342=CARTESIAN_POINT('Origin',(15.,0.,-2.));
#52343=CARTESIAN_POINT('',(-16.,-1.95943487863577E-15,-2.));
#52344=CARTESIAN_POINT('Origin',(0.,0.,-2.));
#52345=CARTESIAN_POINT('Origin',(0.,0.,-4.));
#52346=CARTESIAN_POINT('',(-16.,1.95943487863577E-15,12.));
#52347=CARTESIAN_POINT('Origin',(0.,0.,12.));
#52348=CARTESIAN_POINT('',(-16.,-1.95943487863577E-15,-4.));
#52349=CARTESIAN_POINT('Origin',(0.,0.,28.));
#52350=CARTESIAN_POINT('',(-11.,-1.34711147906209E-15,28.));
#52351=CARTESIAN_POINT('Origin',(0.,0.,28.));
#52352=CARTESIAN_POINT('',(-8.,-9.79717439317883E-16,28.));
#52353=CARTESIAN_POINT('Origin',(0.,0.,28.));
#52354=CARTESIAN_POINT('Origin',(0.,0.,26.));
#52355=CARTESIAN_POINT('',(-11.,-1.34711147906209E-15,26.));
#52356=CARTESIAN_POINT('Origin',(0.,0.,26.));
#52357=CARTESIAN_POINT('',(-8.,9.79717439317883E-16,26.));
#52358=CARTESIAN_POINT('Origin',(0.,0.,26.));
#52359=CARTESIAN_POINT('Origin',(0.,0.,26.));
#52360=CARTESIAN_POINT('',(-11.,-1.34711147906209E-15,26.));
#52361=CARTESIAN_POINT('Origin',(0.,0.,20.));
#52362=CARTESIAN_POINT('',(-8.,-9.79717439317883E-16,20.));
#52363=CARTESIAN_POINT('',(-8.,-9.79717439317883E-16,20.));
#52364=CARTESIAN_POINT('Origin',(0.,0.,20.));
#52365=CARTESIAN_POINT('Origin',(0.,0.,14.));
#52366=CARTESIAN_POINT('',(-20.,-2.44929359829471E-15,14.));
#52367=CARTESIAN_POINT('Origin',(0.,0.,14.));
#52368=CARTESIAN_POINT('',(-16.,-1.95943487863577E-15,14.));
#52369=CARTESIAN_POINT('Origin',(0.,0.,14.));
#52370=CARTESIAN_POINT('Origin',(0.,0.,12.));
#52371=CARTESIAN_POINT('',(-20.,-2.44929359829471E-15,12.));
#52372=CARTESIAN_POINT('Origin',(0.,0.,12.));
#52373=CARTESIAN_POINT('Origin',(0.,0.,12.));
#52374=CARTESIAN_POINT('',(-20.,-2.44929359829471E-15,12.));
#52375=CARTESIAN_POINT('Origin',(0.,0.,-4.));
#52376=CARTESIAN_POINT('',(-16.,-1.95943487863577E-15,-4.));
#52377=CARTESIAN_POINT('',(-16.,-1.95943487863577E-15,-4.));
#52378=CARTESIAN_POINT('Origin',(0.,0.,-4.));
#52379=CARTESIAN_POINT('Origin',(0.,0.,20.));
#52380=CARTESIAN_POINT('',(-8.,-9.79717439317883E-16,20.));
#52381=CARTESIAN_POINT('Origin',(0.,0.,46.));
#52382=CARTESIAN_POINT('Origin',(0.,0.,-20.));
#52383=CARTESIAN_POINT('',(-8.,-9.79717439317883E-16,-4.));
#52384=CARTESIAN_POINT('Origin',(0.,0.,-4.));
#52385=CARTESIAN_POINT('',(-8.,-9.79717439317883E-16,-30.));
#52386=CARTESIAN_POINT('',(-8.,-9.79717439317883E-16,-20.));
#52387=CARTESIAN_POINT('Origin',(0.,0.,-30.));
#52388=CARTESIAN_POINT('Origin',(0.,0.,-30.));
#52389=CARTESIAN_POINT('Origin',(0.,0.,-4.));
#52390=CARTESIAN_POINT('',(-16.,-1.95943487863577E-15,20.));
#52391=CARTESIAN_POINT('Origin',(0.,0.,20.));
#52392=CARTESIAN_POINT('',(-16.,-1.95943487863577E-15,-4.));
#52393=CARTESIAN_POINT('Origin',(0.,0.,20.));
#52394=CARTESIAN_POINT('Origin',(0.,0.,-4.));
#52395=CARTESIAN_POINT('',(0.,0.,0.));
#52396=CARTESIAN_POINT('Origin',(0.,-86.,6.));
#52397=CARTESIAN_POINT('',(0.,-90.,8.));
#52398=CARTESIAN_POINT('',(0.,-90.,4.));
#52399=CARTESIAN_POINT('Ctrl Pts',(-2.08166817117217E-16,-90.,8.));
#52400=CARTESIAN_POINT('Ctrl Pts',(0.251133328053566,-90.,8.));
#52401=CARTESIAN_POINT('Ctrl Pts',(0.519000232590761,-89.9988407998655,
7.94980925763969));
#52402=CARTESIAN_POINT('Ctrl Pts',(1.01175644254643,-89.9946501491172,7.74569936791146));
#52403=CARTESIAN_POINT('Ctrl Pts',(1.23664644642618,-89.9916787455059,7.59178067832001));
#52404=CARTESIAN_POINT('Ctrl Pts',(1.59178067978086,-89.9860976603374,7.23664644496533));
#52405=CARTESIAN_POINT('Ctrl Pts',(1.74569936855887,-89.9831259365723,7.01175644187864));
#52406=CARTESIAN_POINT('Ctrl Pts',(1.94980925677131,-89.9789345539658,6.51900023379203));
#52407=CARTESIAN_POINT('Ctrl Pts',(2.,-89.9777750336159,6.25113333011964));
#52408=CARTESIAN_POINT('Ctrl Pts',(2.,-89.9777750336159,5.74886666988036));
#52409=CARTESIAN_POINT('Ctrl Pts',(1.94980925677131,-89.9789345539658,5.48099976620797));
#52410=CARTESIAN_POINT('Ctrl Pts',(1.74569936855887,-89.9831259365723,4.98824355812136));
#52411=CARTESIAN_POINT('Ctrl Pts',(1.59178067978086,-89.9860976603374,4.76335355503467));
#52412=CARTESIAN_POINT('Ctrl Pts',(1.23664644642618,-89.9916787455059,4.40821932167999));
#52413=CARTESIAN_POINT('Ctrl Pts',(1.01175644254643,-89.9946501491172,4.25430063208854));
#52414=CARTESIAN_POINT('Ctrl Pts',(0.519000232590762,-89.9988407998655,
4.05019074236031));
#52415=CARTESIAN_POINT('Ctrl Pts',(0.251133328053567,-90.,4.));
#52416=CARTESIAN_POINT('Ctrl Pts',(5.55111512312578E-16,-90.,4.));
#52417=CARTESIAN_POINT('',(2.44929359829471E-16,-82.,8.));
#52418=CARTESIAN_POINT('',(2.44929359829471E-16,-86.,8.));
#52419=CARTESIAN_POINT('Origin',(0.,-82.,6.));
#52420=CARTESIAN_POINT('Ctrl Pts',(4.85722573273506E-16,-90.,4.));
#52421=CARTESIAN_POINT('Ctrl Pts',(-0.251133328053566,-90.,4.));
#52422=CARTESIAN_POINT('Ctrl Pts',(-0.519000232590761,-89.9988407998655,
4.05019074236031));
#52423=CARTESIAN_POINT('Ctrl Pts',(-1.01175644254643,-89.9946501491172,
4.25430063208854));
#52424=CARTESIAN_POINT('Ctrl Pts',(-1.23664644642618,-89.9916787455059,
4.40821932167999));
#52425=CARTESIAN_POINT('Ctrl Pts',(-1.59178067978086,-89.9860976603374,
4.76335355503467));
#52426=CARTESIAN_POINT('Ctrl Pts',(-1.74569936855887,-89.9831259365723,
4.98824355812136));
#52427=CARTESIAN_POINT('Ctrl Pts',(-1.94980925677131,-89.9789345539658,
5.48099976620797));
#52428=CARTESIAN_POINT('Ctrl Pts',(-2.,-89.9777750336159,5.74886666988036));
#52429=CARTESIAN_POINT('Ctrl Pts',(-2.,-89.9777750336159,6.));
#52430=CARTESIAN_POINT('Ctrl Pts',(-2.,-89.9777750336159,6.25113333011964));
#52431=CARTESIAN_POINT('Ctrl Pts',(-1.94980925677131,-89.9789345539658,
6.51900023379203));
#52432=CARTESIAN_POINT('Ctrl Pts',(-1.74569936855887,-89.9831259365723,
7.01175644187864));
#52433=CARTESIAN_POINT('Ctrl Pts',(-1.59178067978086,-89.9860976603374,
7.23664644496533));
#52434=CARTESIAN_POINT('Ctrl Pts',(-1.23664644642618,-89.9916787455059,
7.59178067832001));
#52435=CARTESIAN_POINT('Ctrl Pts',(-1.01175644254643,-89.9946501491172,
7.74569936791146));
#52436=CARTESIAN_POINT('Ctrl Pts',(-0.519000232590761,-89.9988407998655,
7.94980925763969));
#52437=CARTESIAN_POINT('Ctrl Pts',(-0.251133328053566,-90.,8.));
#52438=CARTESIAN_POINT('Ctrl Pts',(-2.08166817117217E-16,-90.,8.));
#52439=CARTESIAN_POINT('Origin',(0.,-82.,6.));
#52440=CARTESIAN_POINT('Origin',(0.,86.,6.));
#52441=CARTESIAN_POINT('',(0.,90.,8.));
#52442=CARTESIAN_POINT('',(0.,90.,4.));
#52443=CARTESIAN_POINT('Ctrl Pts',(0.,90.,8.));
#52444=CARTESIAN_POINT('Ctrl Pts',(-0.251133328053566,90.,8.));
#52445=CARTESIAN_POINT('Ctrl Pts',(-0.519000232590761,89.9988407998655,
7.94980925763969));
#52446=CARTESIAN_POINT('Ctrl Pts',(-1.01175644254643,89.9946501491172,7.74569936791146));
#52447=CARTESIAN_POINT('Ctrl Pts',(-1.23664644642618,89.9916787455059,7.59178067832001));
#52448=CARTESIAN_POINT('Ctrl Pts',(-1.59178067978086,89.9860976603374,7.23664644496533));
#52449=CARTESIAN_POINT('Ctrl Pts',(-1.74569936855886,89.9831259365723,7.01175644187864));
#52450=CARTESIAN_POINT('Ctrl Pts',(-1.94980925677131,89.9789345539658,6.51900023379203));
#52451=CARTESIAN_POINT('Ctrl Pts',(-2.,89.9777750336159,6.25113333011964));
#52452=CARTESIAN_POINT('Ctrl Pts',(-2.,89.9777750336159,5.74886666988036));
#52453=CARTESIAN_POINT('Ctrl Pts',(-1.94980925677131,89.9789345539658,5.48099976620797));
#52454=CARTESIAN_POINT('Ctrl Pts',(-1.74569936855887,89.9831259365723,4.98824355812136));
#52455=CARTESIAN_POINT('Ctrl Pts',(-1.59178067978086,89.9860976603374,4.76335355503467));
#52456=CARTESIAN_POINT('Ctrl Pts',(-1.23664644642618,89.9916787455059,4.40821932167999));
#52457=CARTESIAN_POINT('Ctrl Pts',(-1.01175644254643,89.9946501491172,4.25430063208854));
#52458=CARTESIAN_POINT('Ctrl Pts',(-0.519000232590762,89.9988407998655,
4.05019074236031));
#52459=CARTESIAN_POINT('Ctrl Pts',(-0.251133328053566,90.,4.));
#52460=CARTESIAN_POINT('Ctrl Pts',(-2.08166817117217E-16,90.,4.));
#52461=CARTESIAN_POINT('Ctrl Pts',(-4.85722573273506E-16,90.,4.));
#52462=CARTESIAN_POINT('Ctrl Pts',(0.251133328053566,90.,4.));
#52463=CARTESIAN_POINT('Ctrl Pts',(0.519000232590762,89.9988407998655,4.05019074236031));
#52464=CARTESIAN_POINT('Ctrl Pts',(1.01175644254643,89.9946501491172,4.25430063208854));
#52465=CARTESIAN_POINT('Ctrl Pts',(1.23664644642618,89.9916787455059,4.40821932167999));
#52466=CARTESIAN_POINT('Ctrl Pts',(1.59178067978086,89.9860976603374,4.76335355503467));
#52467=CARTESIAN_POINT('Ctrl Pts',(1.74569936855886,89.9831259365723,4.98824355812136));
#52468=CARTESIAN_POINT('Ctrl Pts',(1.94980925677131,89.9789345539658,5.48099976620797));
#52469=CARTESIAN_POINT('Ctrl Pts',(2.,89.9777750336159,5.74886666988036));
#52470=CARTESIAN_POINT('Ctrl Pts',(2.,89.9777750336159,6.));
#52471=CARTESIAN_POINT('Ctrl Pts',(2.,89.9777750336159,6.25113333011964));
#52472=CARTESIAN_POINT('Ctrl Pts',(1.94980925677131,89.9789345539658,6.51900023379203));
#52473=CARTESIAN_POINT('Ctrl Pts',(1.74569936855887,89.9831259365723,7.01175644187864));
#52474=CARTESIAN_POINT('Ctrl Pts',(1.59178067978086,89.9860976603374,7.23664644496533));
#52475=CARTESIAN_POINT('Ctrl Pts',(1.23664644642618,89.9916787455059,7.59178067832001));
#52476=CARTESIAN_POINT('Ctrl Pts',(1.01175644254643,89.9946501491172,7.74569936791146));
#52477=CARTESIAN_POINT('Ctrl Pts',(0.519000232590761,89.9988407998655,7.94980925763969));
#52478=CARTESIAN_POINT('Ctrl Pts',(0.251133328053566,90.,8.));
#52479=CARTESIAN_POINT('Ctrl Pts',(-6.93889390390723E-17,90.,8.));
#52480=CARTESIAN_POINT('',(2.44929359829471E-16,82.,4.));
#52481=CARTESIAN_POINT('',(2.44929359829471E-16,86.,4.));
#52482=CARTESIAN_POINT('Origin',(0.,82.,6.));
#52483=CARTESIAN_POINT('Origin',(0.,82.,6.));
#52484=CARTESIAN_POINT('Origin',(-86.,0.,6.));
#52485=CARTESIAN_POINT('',(-90.,0.,8.));
#52486=CARTESIAN_POINT('',(-90.,0.,4.));
#52487=CARTESIAN_POINT('Ctrl Pts',(-90.,2.77555756156289E-16,8.));
#52488=CARTESIAN_POINT('Ctrl Pts',(-90.,-0.251133328053566,8.));
#52489=CARTESIAN_POINT('Ctrl Pts',(-89.9988407998655,-0.519000232590761,
7.94980925763969));
#52490=CARTESIAN_POINT('Ctrl Pts',(-89.9946501491172,-1.01175644254643,
7.74569936791146));
#52491=CARTESIAN_POINT('Ctrl Pts',(-89.9916787455059,-1.23664644642618,
7.59178067832001));
#52492=CARTESIAN_POINT('Ctrl Pts',(-89.9860976603374,-1.59178067978086,
7.23664644496533));
#52493=CARTESIAN_POINT('Ctrl Pts',(-89.9831259365723,-1.74569936855887,
7.01175644187864));
#52494=CARTESIAN_POINT('Ctrl Pts',(-89.9789345539658,-1.94980925677131,
6.51900023379203));
#52495=CARTESIAN_POINT('Ctrl Pts',(-89.9777750336159,-2.,6.25113333011964));
#52496=CARTESIAN_POINT('Ctrl Pts',(-89.9777750336159,-2.,5.74886666988036));
#52497=CARTESIAN_POINT('Ctrl Pts',(-89.9789345539658,-1.94980925677131,
5.48099976620797));
#52498=CARTESIAN_POINT('Ctrl Pts',(-89.9831259365723,-1.74569936855887,
4.98824355812136));
#52499=CARTESIAN_POINT('Ctrl Pts',(-89.9860976603374,-1.59178067978086,
4.76335355503467));
#52500=CARTESIAN_POINT('Ctrl Pts',(-89.9916787455059,-1.23664644642618,
4.40821932167999));
#52501=CARTESIAN_POINT('Ctrl Pts',(-89.9946501491172,-1.01175644254643,
4.25430063208854));
#52502=CARTESIAN_POINT('Ctrl Pts',(-89.9988407998655,-0.519000232590762,
4.05019074236031));
#52503=CARTESIAN_POINT('Ctrl Pts',(-90.,-0.251133328053567,4.));
#52504=CARTESIAN_POINT('Ctrl Pts',(-90.,-4.85722573273506E-16,4.));
#52505=CARTESIAN_POINT('',(-89.9777750336159,2.,6.));
#52506=CARTESIAN_POINT('Ctrl Pts',(-89.9777750336159,2.,6.));
#52507=CARTESIAN_POINT('Ctrl Pts',(-89.9777750336159,2.,6.25113333011964));
#52508=CARTESIAN_POINT('Ctrl Pts',(-89.9789345539658,1.94980925677131,6.51900023379203));
#52509=CARTESIAN_POINT('Ctrl Pts',(-89.9831259365723,1.74569936855887,7.01175644187864));
#52510=CARTESIAN_POINT('Ctrl Pts',(-89.9860976603374,1.59178067978086,7.23664644496533));
#52511=CARTESIAN_POINT('Ctrl Pts',(-89.9916787455059,1.23664644642618,7.59178067832001));
#52512=CARTESIAN_POINT('Ctrl Pts',(-89.9946501491172,1.01175644254643,7.74569936791146));
#52513=CARTESIAN_POINT('Ctrl Pts',(-89.9988407998655,0.519000232590762,
7.94980925763969));
#52514=CARTESIAN_POINT('Ctrl Pts',(-90.,0.251133328053567,8.));
#52515=CARTESIAN_POINT('Ctrl Pts',(-90.,2.77555756156289E-16,8.));
#52516=CARTESIAN_POINT('',(-82.,2.,6.));
#52517=CARTESIAN_POINT('',(-86.,2.,6.));
#52518=CARTESIAN_POINT('Origin',(-82.,0.,6.));
#52519=CARTESIAN_POINT('Ctrl Pts',(-90.,-4.16333634234434E-16,4.));
#52520=CARTESIAN_POINT('Ctrl Pts',(-90.,0.251133328053565,4.));
#52521=CARTESIAN_POINT('Ctrl Pts',(-89.9988407998655,0.519000232590761,
4.05019074236031));
#52522=CARTESIAN_POINT('Ctrl Pts',(-89.9946501491172,1.01175644254643,4.25430063208854));
#52523=CARTESIAN_POINT('Ctrl Pts',(-89.9916787455059,1.23664644642618,4.40821932167999));
#52524=CARTESIAN_POINT('Ctrl Pts',(-89.9860976603374,1.59178067978086,4.76335355503466));
#52525=CARTESIAN_POINT('Ctrl Pts',(-89.9831259365723,1.74569936855886,4.98824355812136));
#52526=CARTESIAN_POINT('Ctrl Pts',(-89.9789345539658,1.94980925677131,5.48099976620797));
#52527=CARTESIAN_POINT('Ctrl Pts',(-89.9777750336159,2.,5.74886666988035));
#52528=CARTESIAN_POINT('Ctrl Pts',(-89.9777750336159,2.,6.));
#52529=CARTESIAN_POINT('Origin',(-82.,0.,6.));
#52530=CARTESIAN_POINT('Origin',(86.,0.,6.));
#52531=CARTESIAN_POINT('',(90.,0.,8.));
#52532=CARTESIAN_POINT('',(90.,0.,4.));
#52533=CARTESIAN_POINT('Ctrl Pts',(90.,-2.77555756156289E-16,8.));
#52534=CARTESIAN_POINT('Ctrl Pts',(90.,0.251133328053566,8.));
#52535=CARTESIAN_POINT('Ctrl Pts',(89.9988407998655,0.519000232590761,7.94980925763969));
#52536=CARTESIAN_POINT('Ctrl Pts',(89.9946501491172,1.01175644254643,7.74569936791146));
#52537=CARTESIAN_POINT('Ctrl Pts',(89.9916787455059,1.23664644642618,7.59178067832001));
#52538=CARTESIAN_POINT('Ctrl Pts',(89.9860976603374,1.59178067978086,7.23664644496533));
#52539=CARTESIAN_POINT('Ctrl Pts',(89.9831259365723,1.74569936855887,7.01175644187864));
#52540=CARTESIAN_POINT('Ctrl Pts',(89.9789345539658,1.94980925677131,6.51900023379203));
#52541=CARTESIAN_POINT('Ctrl Pts',(89.9777750336159,2.,6.25113333011964));
#52542=CARTESIAN_POINT('Ctrl Pts',(89.9777750336159,2.,5.74886666988036));
#52543=CARTESIAN_POINT('Ctrl Pts',(89.9789345539658,1.94980925677131,5.48099976620797));
#52544=CARTESIAN_POINT('Ctrl Pts',(89.9831259365723,1.74569936855887,4.98824355812136));
#52545=CARTESIAN_POINT('Ctrl Pts',(89.9860976603374,1.59178067978086,4.76335355503467));
#52546=CARTESIAN_POINT('Ctrl Pts',(89.9916787455059,1.23664644642618,4.40821932167999));
#52547=CARTESIAN_POINT('Ctrl Pts',(89.9946501491172,1.01175644254643,4.25430063208854));
#52548=CARTESIAN_POINT('Ctrl Pts',(89.9988407998655,0.519000232590762,4.05019074236031));
#52549=CARTESIAN_POINT('Ctrl Pts',(90.,0.251133328053567,4.));
#52550=CARTESIAN_POINT('Ctrl Pts',(90.,4.85722573273506E-16,4.));
#52551=CARTESIAN_POINT('',(89.9777750336159,-2.,6.));
#52552=CARTESIAN_POINT('Ctrl Pts',(89.9777750336159,-2.,6.));
#52553=CARTESIAN_POINT('Ctrl Pts',(89.9777750336159,-2.,6.25113333011964));
#52554=CARTESIAN_POINT('Ctrl Pts',(89.9789345539658,-1.94980925677131,6.51900023379203));
#52555=CARTESIAN_POINT('Ctrl Pts',(89.9831259365723,-1.74569936855887,7.01175644187864));
#52556=CARTESIAN_POINT('Ctrl Pts',(89.9860976603374,-1.59178067978086,7.23664644496533));
#52557=CARTESIAN_POINT('Ctrl Pts',(89.9916787455059,-1.23664644642618,7.59178067832001));
#52558=CARTESIAN_POINT('Ctrl Pts',(89.9946501491172,-1.01175644254643,7.74569936791146));
#52559=CARTESIAN_POINT('Ctrl Pts',(89.9988407998655,-0.519000232590762,
7.94980925763969));
#52560=CARTESIAN_POINT('Ctrl Pts',(90.,-0.251133328053567,8.));
#52561=CARTESIAN_POINT('Ctrl Pts',(90.,-2.77555756156289E-16,8.));
#52562=CARTESIAN_POINT('',(82.,-2.,6.));
#52563=CARTESIAN_POINT('',(86.,-2.,6.));
#52564=CARTESIAN_POINT('Origin',(82.,0.,6.));
#52565=CARTESIAN_POINT('Ctrl Pts',(90.,4.16333634234434E-16,4.));
#52566=CARTESIAN_POINT('Ctrl Pts',(90.,-0.251133328053565,4.));
#52567=CARTESIAN_POINT('Ctrl Pts',(89.9988407998655,-0.519000232590761,
4.05019074236031));
#52568=CARTESIAN_POINT('Ctrl Pts',(89.9946501491172,-1.01175644254643,4.25430063208854));
#52569=CARTESIAN_POINT('Ctrl Pts',(89.9916787455059,-1.23664644642618,4.40821932167999));
#52570=CARTESIAN_POINT('Ctrl Pts',(89.9860976603374,-1.59178067978086,4.76335355503466));
#52571=CARTESIAN_POINT('Ctrl Pts',(89.9831259365723,-1.74569936855886,4.98824355812136));
#52572=CARTESIAN_POINT('Ctrl Pts',(89.9789345539658,-1.94980925677131,5.48099976620797));
#52573=CARTESIAN_POINT('Ctrl Pts',(89.9777750336159,-2.,5.74886666988035));
#52574=CARTESIAN_POINT('Ctrl Pts',(89.9777750336159,-2.,6.));
#52575=CARTESIAN_POINT('Origin',(82.,0.,6.));
#52576=CARTESIAN_POINT('Ctrl Pts',(74.4153560389001,-3.55032190142516,-5.55111512312578E-16));
#52577=CARTESIAN_POINT('Ctrl Pts',(74.4153560389001,-3.55032190142516,4.));
#52578=CARTESIAN_POINT('Ctrl Pts',(74.4153560389001,-3.55032190142516,8.));
#52579=CARTESIAN_POINT('Ctrl Pts',(74.4153560389001,-3.55032190142516,12.));
#52580=CARTESIAN_POINT('Ctrl Pts',(74.4101195539797,-3.66007952356781,-5.55111512312578E-16));
#52581=CARTESIAN_POINT('Ctrl Pts',(74.4101195539797,-3.66007952356781,4.));
#52582=CARTESIAN_POINT('Ctrl Pts',(74.4101195539797,-3.66007952356781,8.00000000000001));
#52583=CARTESIAN_POINT('Ctrl Pts',(74.4101195539797,-3.66007952356781,12.));
#52584=CARTESIAN_POINT('Ctrl Pts',(74.3352361483148,-3.84840282419241,-5.55111512312578E-16));
#52585=CARTESIAN_POINT('Ctrl Pts',(74.3352361483148,-3.84840282419241,4.));
#52586=CARTESIAN_POINT('Ctrl Pts',(74.3352361483148,-3.84840282419241,7.99999999999999));
#52587=CARTESIAN_POINT('Ctrl Pts',(74.3352361483148,-3.84840282419241,12.));
#52588=CARTESIAN_POINT('Ctrl Pts',(74.1732860426646,-3.96302207561158,-5.55111512312578E-16));
#52589=CARTESIAN_POINT('Ctrl Pts',(74.1732860426646,-3.96302207561158,4.));
#52590=CARTESIAN_POINT('Ctrl Pts',(74.1732860426646,-3.96302207561158,8.00000000000001));
#52591=CARTESIAN_POINT('Ctrl Pts',(74.1732860426646,-3.96302207561158,12.));
#52592=CARTESIAN_POINT('Ctrl Pts',(74.0964320765796,-3.99277406492185,-5.55111512312578E-16));
#52593=CARTESIAN_POINT('Ctrl Pts',(74.0964320765796,-3.99277406492185,4.));
#52594=CARTESIAN_POINT('Ctrl Pts',(74.0964320765796,-3.99277406492185,8.));
#52595=CARTESIAN_POINT('Ctrl Pts',(74.0964320765796,-3.99277406492185,12.));
#52596=CARTESIAN_POINT('',(74.4153560389001,-3.55032190142516,0.));
#52597=CARTESIAN_POINT('',(74.0964320765796,-3.99277406492185,0.));
#52598=CARTESIAN_POINT('Ctrl Pts',(74.4153560389001,-3.55032190142516,4.16333634234434E-16));
#52599=CARTESIAN_POINT('Ctrl Pts',(74.4101195539797,-3.66007952356781,4.16333634234433E-16));
#52600=CARTESIAN_POINT('Ctrl Pts',(74.3673290364569,-3.76769283821044,4.16333634234434E-16));
#52601=CARTESIAN_POINT('Ctrl Pts',(74.2961085760817,-3.85123952454109,4.16333634234434E-16));
#52602=CARTESIAN_POINT('Ctrl Pts',(74.2426932308004,-3.91389953928908,4.16333634234434E-16));
#52603=CARTESIAN_POINT('Ctrl Pts',(74.1732860426646,-3.96302207561158,4.16333634234433E-16));
#52604=CARTESIAN_POINT('Ctrl Pts',(74.0964320765796,-3.99277406492185,4.16333634234434E-16));
#52605=CARTESIAN_POINT('',(74.0964320765796,-3.99277406492185,12.));
#52606=CARTESIAN_POINT('Ctrl Pts',(74.0964320765796,-3.99277406492185,-5.55111512312578E-16));
#52607=CARTESIAN_POINT('Ctrl Pts',(74.0964320765796,-3.99277406492185,4.));
#52608=CARTESIAN_POINT('Ctrl Pts',(74.0964320765796,-3.99277406492185,8.));
#52609=CARTESIAN_POINT('Ctrl Pts',(74.0964320765796,-3.99277406492185,12.));
#52610=CARTESIAN_POINT('',(74.4153560389001,-3.55032190142516,12.));
#52611=CARTESIAN_POINT('Ctrl Pts',(74.0964320765796,-3.99277406492185,12.));
#52612=CARTESIAN_POINT('Ctrl Pts',(74.1732860426646,-3.96302207561158,12.));
#52613=CARTESIAN_POINT('Ctrl Pts',(74.2426932308004,-3.91389953928908,12.));
#52614=CARTESIAN_POINT('Ctrl Pts',(74.2961085760817,-3.85123952454109,12.));
#52615=CARTESIAN_POINT('Ctrl Pts',(74.3673290364569,-3.76769283821044,12.));
#52616=CARTESIAN_POINT('Ctrl Pts',(74.4101195539797,-3.66007952356781,12.));
#52617=CARTESIAN_POINT('Ctrl Pts',(74.4153560389001,-3.55032190142516,12.));
#52618=CARTESIAN_POINT('Ctrl Pts',(74.4153560389001,-3.55032190142516,12.));
#52619=CARTESIAN_POINT('Ctrl Pts',(74.4153560389001,-3.55032190142516,8.));
#52620=CARTESIAN_POINT('Ctrl Pts',(74.4153560389001,-3.55032190142516,4.));
#52621=CARTESIAN_POINT('Ctrl Pts',(74.4153560389001,-3.55032190142516,-5.55111512312578E-16));
#52622=CARTESIAN_POINT('Ctrl Pts',(69.8028570375097,-5.24987136994593,0.));
#52623=CARTESIAN_POINT('Ctrl Pts',(69.8028570375097,-5.24987136994593,12.));
#52624=CARTESIAN_POINT('Ctrl Pts',(69.8066748687772,-5.24915955997427,0.));
#52625=CARTESIAN_POINT('Ctrl Pts',(69.8066748687772,-5.24915955997427,12.));
#52626=CARTESIAN_POINT('Ctrl Pts',(69.8143154684204,-5.24773285666377,0.));
#52627=CARTESIAN_POINT('Ctrl Pts',(69.8143154684204,-5.24773285666377,12.));
#52628=CARTESIAN_POINT('Ctrl Pts',(69.8257911792159,-5.24558355159751,0.));
#52629=CARTESIAN_POINT('Ctrl Pts',(69.8257911792159,-5.24558355159751,12.));
#52630=CARTESIAN_POINT('Ctrl Pts',(69.841121750752,-5.2426993105457,0.));
#52631=CARTESIAN_POINT('Ctrl Pts',(69.841121750752,-5.2426993105457,12.));
#52632=CARTESIAN_POINT('Ctrl Pts',(69.8603343302743,-5.23906316634803,0.));
#52633=CARTESIAN_POINT('Ctrl Pts',(69.8603343302743,-5.23906316634803,12.));
#52634=CARTESIAN_POINT('Ctrl Pts',(69.8795962381599,-5.2353961627962,0.));
#52635=CARTESIAN_POINT('Ctrl Pts',(69.8795962381599,-5.2353961627962,12.));
#52636=CARTESIAN_POINT('Ctrl Pts',(69.8989073936688,-5.23169827290556,0.));
#52637=CARTESIAN_POINT('Ctrl Pts',(69.8989073936688,-5.23169827290556,12.));
#52638=CARTESIAN_POINT('Ctrl Pts',(69.9182676502048,-5.22796945602794,0.));
#52639=CARTESIAN_POINT('Ctrl Pts',(69.9182676502048,-5.22796945602794,12.));
#52640=CARTESIAN_POINT('Ctrl Pts',(69.9376767969095,-5.22420965879982,0.));
#52641=CARTESIAN_POINT('Ctrl Pts',(69.9376767969095,-5.22420965879982,12.));
#52642=CARTESIAN_POINT('Ctrl Pts',(69.9571345870076,-5.22041882075721,0.));
#52643=CARTESIAN_POINT('Ctrl Pts',(69.9571345870076,-5.22041882075721,12.));
#52644=CARTESIAN_POINT('Ctrl Pts',(69.9766407595385,-5.21659687881139,0.));
#52645=CARTESIAN_POINT('Ctrl Pts',(69.9766407595385,-5.21659687881139,12.));
#52646=CARTESIAN_POINT('Ctrl Pts',(69.9961950629965,-5.2127437720326,0.));
#52647=CARTESIAN_POINT('Ctrl Pts',(69.9961950629965,-5.2127437720326,12.));
#52648=CARTESIAN_POINT('Ctrl Pts',(70.0157972802182,-5.20885944672837,0.));
#52649=CARTESIAN_POINT('Ctrl Pts',(70.0157972802182,-5.20885944672837,12.));
#52650=CARTESIAN_POINT('Ctrl Pts',(70.0354472203546,-5.20494385478026,0.));
#52651=CARTESIAN_POINT('Ctrl Pts',(70.0354472203546,-5.20494385478026,12.));
#52652=CARTESIAN_POINT('Ctrl Pts',(70.0551447071082,-5.20099695122656,0.));
#52653=CARTESIAN_POINT('Ctrl Pts',(70.0551447071082,-5.20099695122656,12.));
#52654=CARTESIAN_POINT('Ctrl Pts',(70.0748895689729,-5.19701869225529,0.));
#52655=CARTESIAN_POINT('Ctrl Pts',(70.0748895689729,-5.19701869225529,12.));
#52656=CARTESIAN_POINT('Ctrl Pts',(70.0946816270997,-5.1930090327158,0.));
#52657=CARTESIAN_POINT('Ctrl Pts',(70.0946816270997,-5.1930090327158,12.));
#52658=CARTESIAN_POINT('Ctrl Pts',(70.1145206891885,-5.18896792486566,0.));
#52659=CARTESIAN_POINT('Ctrl Pts',(70.1145206891885,-5.18896792486566,12.));
#52660=CARTESIAN_POINT('Ctrl Pts',(70.1344065558145,-5.18489531966265,0.));
#52661=CARTESIAN_POINT('Ctrl Pts',(70.1344065558145,-5.18489531966265,12.));
#52662=CARTESIAN_POINT('Ctrl Pts',(70.1543390243892,-5.18079116757667,0.));
#52663=CARTESIAN_POINT('Ctrl Pts',(70.1543390243892,-5.18079116757667,12.));
#52664=CARTESIAN_POINT('Ctrl Pts',(70.1743178937077,-5.17665541952383,0.));
#52665=CARTESIAN_POINT('Ctrl Pts',(70.1743178937077,-5.17665541952383,12.));
#52666=CARTESIAN_POINT('Ctrl Pts',(70.1943429691167,-5.17248802793389,0.));
#52667=CARTESIAN_POINT('Ctrl Pts',(70.1943429691167,-5.17248802793389,12.));
#52668=CARTESIAN_POINT('Ctrl Pts',(70.2144140622953,-5.16828894670109,0.));
#52669=CARTESIAN_POINT('Ctrl Pts',(70.2144140622953,-5.16828894670109,12.));
#52670=CARTESIAN_POINT('Ctrl Pts',(70.2345309887833,-5.16405813066976,0.));
#52671=CARTESIAN_POINT('Ctrl Pts',(70.2345309887833,-5.16405813066976,12.));
#52672=CARTESIAN_POINT('Ctrl Pts',(70.2546935662722,-5.15979553528204,0.));
#52673=CARTESIAN_POINT('Ctrl Pts',(70.2546935662722,-5.15979553528204,12.));
#52674=CARTESIAN_POINT('Ctrl Pts',(70.2749016125105,-5.1555011161486,0.));
#52675=CARTESIAN_POINT('Ctrl Pts',(70.2749016125105,-5.1555011161486,12.));
#52676=CARTESIAN_POINT('Ctrl Pts',(70.2951549435512,-5.15117482869254,0.));
#52677=CARTESIAN_POINT('Ctrl Pts',(70.2951549435512,-5.15117482869254,12.));
#52678=CARTESIAN_POINT('Ctrl Pts',(70.3154533746736,-5.1468166283308,0.));
#52679=CARTESIAN_POINT('Ctrl Pts',(70.3154533746736,-5.1468166283308,12.));
#52680=CARTESIAN_POINT('Ctrl Pts',(70.3357967211796,-5.1424264706348,0.));
#52681=CARTESIAN_POINT('Ctrl Pts',(70.3357967211796,-5.1424264706348,12.));
#52682=CARTESIAN_POINT('Ctrl Pts',(70.3561847991714,-5.13800431148904,0.));
#52683=CARTESIAN_POINT('Ctrl Pts',(70.3561847991714,-5.13800431148904,12.));
#52684=CARTESIAN_POINT('Ctrl Pts',(70.3766174264757,-5.13355010728568,0.));
#52685=CARTESIAN_POINT('Ctrl Pts',(70.3766174264757,-5.13355010728568,12.));
#52686=CARTESIAN_POINT('Ctrl Pts',(70.3970944229851,-5.12906381499456,0.));
#52687=CARTESIAN_POINT('Ctrl Pts',(70.3970944229851,-5.12906381499456,12.));
#52688=CARTESIAN_POINT('Ctrl Pts',(70.417615610161,-5.12454539205329,0.));
#52689=CARTESIAN_POINT('Ctrl Pts',(70.417615610161,-5.12454539205329,12.));
#52690=CARTESIAN_POINT('Ctrl Pts',(70.4381808107245,-5.11999479630212,0.));
#52691=CARTESIAN_POINT('Ctrl Pts',(70.4381808107245,-5.11999479630212,12.));
#52692=CARTESIAN_POINT('Ctrl Pts',(70.458789848296,-5.11541198590933,0.));
#52693=CARTESIAN_POINT('Ctrl Pts',(70.458789848296,-5.11541198590933,12.));
#52694=CARTESIAN_POINT('Ctrl Pts',(70.4794425469825,-5.11079691929213,0.));
#52695=CARTESIAN_POINT('Ctrl Pts',(70.4794425469825,-5.11079691929213,12.));
#52696=CARTESIAN_POINT('Ctrl Pts',(70.500138731399,-5.10614955511664,0.));
#52697=CARTESIAN_POINT('Ctrl Pts',(70.500138731399,-5.10614955511664,12.));
#52698=CARTESIAN_POINT('Ctrl Pts',(70.5208782268497,-5.10146985232941,0.));
#52699=CARTESIAN_POINT('Ctrl Pts',(70.5208782268497,-5.10146985232941,12.));
#52700=CARTESIAN_POINT('Ctrl Pts',(70.5416608594526,-5.09675777018183,0.));
#52701=CARTESIAN_POINT('Ctrl Pts',(70.5416608594526,-5.09675777018183,12.));
#52702=CARTESIAN_POINT('Ctrl Pts',(70.5624864562824,-5.09201326826135,0.));
#52703=CARTESIAN_POINT('Ctrl Pts',(70.5624864562824,-5.09201326826135,12.));
#52704=CARTESIAN_POINT('Ctrl Pts',(70.5833548455014,-5.08723630652273,0.));
#52705=CARTESIAN_POINT('Ctrl Pts',(70.5833548455014,-5.08723630652273,12.));
#52706=CARTESIAN_POINT('Ctrl Pts',(70.6042658562923,-5.08242684526687,0.));
#52707=CARTESIAN_POINT('Ctrl Pts',(70.6042658562923,-5.08242684526687,12.));
#52708=CARTESIAN_POINT('Ctrl Pts',(70.6252193187878,-5.07758484512303,0.));
#52709=CARTESIAN_POINT('Ctrl Pts',(70.6252193187878,-5.07758484512303,12.));
#52710=CARTESIAN_POINT('Ctrl Pts',(70.6462150640015,-5.07271026703355,0.));
#52711=CARTESIAN_POINT('Ctrl Pts',(70.6462150640015,-5.07271026703355,12.));
#52712=CARTESIAN_POINT('Ctrl Pts',(70.6672529237455,-5.06780307224072,0.));
#52713=CARTESIAN_POINT('Ctrl Pts',(70.6672529237455,-5.06780307224072,12.));
#52714=CARTESIAN_POINT('Ctrl Pts',(70.6883327305784,-5.0628632222782,0.));
#52715=CARTESIAN_POINT('Ctrl Pts',(70.6883327305784,-5.0628632222782,12.));
#52716=CARTESIAN_POINT('Ctrl Pts',(70.7094543178438,-5.05789067897058,0.));
#52717=CARTESIAN_POINT('Ctrl Pts',(70.7094543178438,-5.05789067897058,12.));
#52718=CARTESIAN_POINT('Ctrl Pts',(70.7306175196863,-5.05288540443483,0.));
#52719=CARTESIAN_POINT('Ctrl Pts',(70.7306175196863,-5.05288540443483,12.));
#52720=CARTESIAN_POINT('Ctrl Pts',(70.7518221710706,-5.04784736108346,0.));
#52721=CARTESIAN_POINT('Ctrl Pts',(70.7518221710706,-5.04784736108346,12.));
#52722=CARTESIAN_POINT('Ctrl Pts',(70.7730681077983,-5.0427765116335,0.));
#52723=CARTESIAN_POINT('Ctrl Pts',(70.7730681077983,-5.0427765116335,12.));
#52724=CARTESIAN_POINT('Ctrl Pts',(70.7943551665059,-5.03767281910479,0.));
#52725=CARTESIAN_POINT('Ctrl Pts',(70.7943551665059,-5.03767281910479,12.));
#52726=CARTESIAN_POINT('Ctrl Pts',(70.8156831846488,-5.03253624680941,0.));
#52727=CARTESIAN_POINT('Ctrl Pts',(70.8156831846488,-5.03253624680941,12.));
#52728=CARTESIAN_POINT('Ctrl Pts',(70.8370520004843,-5.02736675834693,0.));
#52729=CARTESIAN_POINT('Ctrl Pts',(70.8370520004843,-5.02736675834693,12.));
#52730=CARTESIAN_POINT('Ctrl Pts',(70.8584614530519,-5.02216431760061,0.));
#52731=CARTESIAN_POINT('Ctrl Pts',(70.8584614530519,-5.02216431760061,12.));
#52732=CARTESIAN_POINT('Ctrl Pts',(70.8799113821452,-5.0169288887379,0.));
#52733=CARTESIAN_POINT('Ctrl Pts',(70.8799113821452,-5.0169288887379,12.));
#52734=CARTESIAN_POINT('Ctrl Pts',(70.9014016283124,-5.01166043620568,0.));
#52735=CARTESIAN_POINT('Ctrl Pts',(70.9014016283124,-5.01166043620568,12.));
#52736=CARTESIAN_POINT('Ctrl Pts',(70.9229320328589,-5.00635892472514,0.));
#52737=CARTESIAN_POINT('Ctrl Pts',(70.9229320328589,-5.00635892472514,12.));
#52738=CARTESIAN_POINT('Ctrl Pts',(70.9445024378439,-5.0010243192904,0.));
#52739=CARTESIAN_POINT('Ctrl Pts',(70.9445024378439,-5.0010243192904,12.));
#52740=CARTESIAN_POINT('Ctrl Pts',(70.9661126860773,-4.99565658516913,0.));
#52741=CARTESIAN_POINT('Ctrl Pts',(70.9661126860773,-4.99565658516913,12.));
#52742=CARTESIAN_POINT('Ctrl Pts',(70.9877626211113,-4.99025568790665,0.));
#52743=CARTESIAN_POINT('Ctrl Pts',(70.9877626211113,-4.99025568790665,12.));
#52744=CARTESIAN_POINT('Ctrl Pts',(71.0094520872377,-4.98482159331864,0.));
#52745=CARTESIAN_POINT('Ctrl Pts',(71.0094520872377,-4.98482159331864,12.));
#52746=CARTESIAN_POINT('Ctrl Pts',(71.0311809294821,-4.97935426748585,0.));
#52747=CARTESIAN_POINT('Ctrl Pts',(71.0311809294821,-4.97935426748585,12.));
#52748=CARTESIAN_POINT('Ctrl Pts',(71.0529489935961,-4.97385367675159,0.));
#52749=CARTESIAN_POINT('Ctrl Pts',(71.0529489935961,-4.97385367675159,12.));
#52750=CARTESIAN_POINT('Ctrl Pts',(71.0747561260436,-4.96831978772191,0.));
#52751=CARTESIAN_POINT('Ctrl Pts',(71.0747561260436,-4.96831978772191,12.));
#52752=CARTESIAN_POINT('Ctrl Pts',(71.0966021739907,-4.96275256726766,0.));
#52753=CARTESIAN_POINT('Ctrl Pts',(71.0966021739907,-4.96275256726766,12.));
#52754=CARTESIAN_POINT('Ctrl Pts',(71.1184869853056,-4.95715198251685,0.));
#52755=CARTESIAN_POINT('Ctrl Pts',(71.1184869853056,-4.95715198251685,12.));
#52756=CARTESIAN_POINT('Ctrl Pts',(71.1404104085552,-4.95151800085102,0.));
#52757=CARTESIAN_POINT('Ctrl Pts',(71.1404104085552,-4.95151800085102,12.));
#52758=CARTESIAN_POINT('Ctrl Pts',(71.1623722930001,-4.94585058990341,0.));
#52759=CARTESIAN_POINT('Ctrl Pts',(71.1623722930001,-4.94585058990341,12.));
#52760=CARTESIAN_POINT('Ctrl Pts',(71.1843724885847,-4.94014971756115,0.));
#52761=CARTESIAN_POINT('Ctrl Pts',(71.1843724885847,-4.94014971756115,12.));
#52762=CARTESIAN_POINT('Ctrl Pts',(71.2064108459286,-4.93441535196618,0.));
#52763=CARTESIAN_POINT('Ctrl Pts',(71.2064108459286,-4.93441535196618,12.));
#52764=CARTESIAN_POINT('Ctrl Pts',(71.2284872163273,-4.92864746150733,0.));
#52765=CARTESIAN_POINT('Ctrl Pts',(71.2284872163273,-4.92864746150733,12.));
#52766=CARTESIAN_POINT('Ctrl Pts',(71.250601451747,-4.92284601481722,0.));
#52767=CARTESIAN_POINT('Ctrl Pts',(71.250601451747,-4.92284601481722,12.));
#52768=CARTESIAN_POINT('Ctrl Pts',(71.2727534048192,-4.91701098077036,0.));
#52769=CARTESIAN_POINT('Ctrl Pts',(71.2727534048192,-4.91701098077036,12.));
#52770=CARTESIAN_POINT('Ctrl Pts',(71.294942928829,-4.91114232848603,0.));
#52771=CARTESIAN_POINT('Ctrl Pts',(71.294942928829,-4.91114232848603,12.));
#52772=CARTESIAN_POINT('Ctrl Pts',(71.3171698777084,-4.90524002732779,0.));
#52773=CARTESIAN_POINT('Ctrl Pts',(71.3171698777084,-4.90524002732779,12.));
#52774=CARTESIAN_POINT('Ctrl Pts',(71.3394341060359,-4.89930404689575,0.));
#52775=CARTESIAN_POINT('Ctrl Pts',(71.3394341060359,-4.89930404689575,12.));
#52776=CARTESIAN_POINT('Ctrl Pts',(71.3617354690325,-4.89333435702414,0.));
#52777=CARTESIAN_POINT('Ctrl Pts',(71.3617354690325,-4.89333435702414,12.));
#52778=CARTESIAN_POINT('Ctrl Pts',(71.3840738225562,-4.88733092777975,0.));
#52779=CARTESIAN_POINT('Ctrl Pts',(71.3840738225562,-4.88733092777975,12.));
#52780=CARTESIAN_POINT('Ctrl Pts',(71.4064490230899,-4.88129372946552,0.));
#52781=CARTESIAN_POINT('Ctrl Pts',(71.4064490230899,-4.88129372946552,12.));
#52782=CARTESIAN_POINT('Ctrl Pts',(71.4288609277374,-4.87522273261908,0.));
#52783=CARTESIAN_POINT('Ctrl Pts',(71.4288609277374,-4.87522273261908,12.));
#52784=CARTESIAN_POINT('Ctrl Pts',(71.4513093942255,-4.8691179080055,0.));
#52785=CARTESIAN_POINT('Ctrl Pts',(71.4513093942255,-4.8691179080055,12.));
#52786=CARTESIAN_POINT('Ctrl Pts',(71.4737942808982,-4.86297922661503,0.));
#52787=CARTESIAN_POINT('Ctrl Pts',(71.4737942808982,-4.86297922661503,12.));
#52788=CARTESIAN_POINT('Ctrl Pts',(71.4963154467113,-4.85680665966181,0.));
#52789=CARTESIAN_POINT('Ctrl Pts',(71.4963154467113,-4.85680665966181,12.));
#52790=CARTESIAN_POINT('Ctrl Pts',(71.5188727512197,-4.8506001785878,0.));
#52791=CARTESIAN_POINT('Ctrl Pts',(71.5188727512197,-4.8506001785878,12.));
#52792=CARTESIAN_POINT('Ctrl Pts',(71.5414660545739,-4.84435975506049,0.));
#52793=CARTESIAN_POINT('Ctrl Pts',(71.5414660545739,-4.84435975506049,12.));
#52794=CARTESIAN_POINT('Ctrl Pts',(71.564095217521,-4.83808536096584,0.));
#52795=CARTESIAN_POINT('Ctrl Pts',(71.564095217521,-4.83808536096584,12.));
#52796=CARTESIAN_POINT('Ctrl Pts',(71.5867601014,-4.83177696840638,0.));
#52797=CARTESIAN_POINT('Ctrl Pts',(71.5867601014,-4.83177696840638,12.));
#52798=CARTESIAN_POINT('Ctrl Pts',(71.6094605681366,-4.82543454970027,0.));
#52799=CARTESIAN_POINT('Ctrl Pts',(71.6094605681366,-4.82543454970027,12.));
#52800=CARTESIAN_POINT('Ctrl Pts',(71.6321964802326,-4.81905807738557,0.));
#52801=CARTESIAN_POINT('Ctrl Pts',(71.6321964802326,-4.81905807738557,12.));
#52802=CARTESIAN_POINT('Ctrl Pts',(71.6549677007613,-4.81264752421732,0.));
#52803=CARTESIAN_POINT('Ctrl Pts',(71.6549677007613,-4.81264752421732,12.));
#52804=CARTESIAN_POINT('Ctrl Pts',(71.6777740933705,-4.80620286316089,0.));
#52805=CARTESIAN_POINT('Ctrl Pts',(71.6777740933705,-4.80620286316089,12.));
#52806=CARTESIAN_POINT('Ctrl Pts',(71.7006155222766,-4.79972406739014,0.));
#52807=CARTESIAN_POINT('Ctrl Pts',(71.7006155222766,-4.79972406739014,12.));
#52808=CARTESIAN_POINT('Ctrl Pts',(71.7234918522604,-4.79321111028672,0.));
#52809=CARTESIAN_POINT('Ctrl Pts',(71.7234918522604,-4.79321111028672,12.));
#52810=CARTESIAN_POINT('Ctrl Pts',(71.7464029486552,-4.78666396544451,0.));
#52811=CARTESIAN_POINT('Ctrl Pts',(71.7464029486552,-4.78666396544451,12.));
#52812=CARTESIAN_POINT('Ctrl Pts',(71.7693486773449,-4.78008260666643,0.));
#52813=CARTESIAN_POINT('Ctrl Pts',(71.7693486773449,-4.78008260666643,12.));
#52814=CARTESIAN_POINT('Ctrl Pts',(71.7923289047636,-4.77346700795788,0.));
#52815=CARTESIAN_POINT('Ctrl Pts',(71.7923289047636,-4.77346700795788,12.));
#52816=CARTESIAN_POINT('Ctrl Pts',(71.8153434978924,-4.76681714352504,0.));
#52817=CARTESIAN_POINT('Ctrl Pts',(71.8153434978924,-4.76681714352504,12.));
#52818=CARTESIAN_POINT('Ctrl Pts',(71.8383923242533,-4.76013298777423,0.));
#52819=CARTESIAN_POINT('Ctrl Pts',(71.8383923242533,-4.76013298777423,12.));
#52820=CARTESIAN_POINT('Ctrl Pts',(71.8614752519008,-4.75341451531671,0.));
#52821=CARTESIAN_POINT('Ctrl Pts',(71.8614752519008,-4.75341451531671,12.));
#52822=CARTESIAN_POINT('Ctrl Pts',(71.8845921494186,-4.74666170096546,0.));
#52823=CARTESIAN_POINT('Ctrl Pts',(71.8845921494186,-4.74666170096546,12.));
#52824=CARTESIAN_POINT('Ctrl Pts',(71.9077428859207,-4.73987451972861,0.));
#52825=CARTESIAN_POINT('Ctrl Pts',(71.9077428859207,-4.73987451972861,12.));
#52826=CARTESIAN_POINT('Ctrl Pts',(71.9309273310469,-4.73305294680784,0.));
#52827=CARTESIAN_POINT('Ctrl Pts',(71.9309273310469,-4.73305294680784,12.));
#52828=CARTESIAN_POINT('Ctrl Pts',(71.9541453549582,-4.72619695759779,0.));
#52829=CARTESIAN_POINT('Ctrl Pts',(71.9541453549582,-4.72619695759779,12.));
#52830=CARTESIAN_POINT('Ctrl Pts',(71.9773968283267,-4.71930652769081,0.));
#52831=CARTESIAN_POINT('Ctrl Pts',(71.9773968283267,-4.71930652769081,12.));
#52832=CARTESIAN_POINT('Ctrl Pts',(72.0006816223335,-4.71238163287411,0.));
#52833=CARTESIAN_POINT('Ctrl Pts',(72.0006816223335,-4.71238163287411,12.));
#52834=CARTESIAN_POINT('Ctrl Pts',(72.0239996086694,-4.70542224912312,0.));
#52835=CARTESIAN_POINT('Ctrl Pts',(72.0239996086694,-4.70542224912312,12.));
#52836=CARTESIAN_POINT('Ctrl Pts',(72.047350659532,-4.69842835259997,0.));
#52837=CARTESIAN_POINT('Ctrl Pts',(72.047350659532,-4.69842835259997,12.));
#52838=CARTESIAN_POINT('Ctrl Pts',(72.070734647621,-4.6913999196528,0.));
#52839=CARTESIAN_POINT('Ctrl Pts',(72.070734647621,-4.6913999196528,12.));
#52840=CARTESIAN_POINT('Ctrl Pts',(72.0941514461283,-4.68433692682061,0.));
#52841=CARTESIAN_POINT('Ctrl Pts',(72.0941514461283,-4.68433692682061,12.));
#52842=CARTESIAN_POINT('Ctrl Pts',(72.1176009287349,-4.67723935083087,0.));
#52843=CARTESIAN_POINT('Ctrl Pts',(72.1176009287349,-4.67723935083087,12.));
#52844=CARTESIAN_POINT('Ctrl Pts',(72.1410829696129,-4.67010716859281,0.));
#52845=CARTESIAN_POINT('Ctrl Pts',(72.1410829696129,-4.67010716859281,12.));
#52846=CARTESIAN_POINT('Ctrl Pts',(72.1645974434218,-4.6629403571957,0.));
#52847=CARTESIAN_POINT('Ctrl Pts',(72.1645974434218,-4.6629403571957,12.));
#52848=CARTESIAN_POINT('Ctrl Pts',(72.1881442253052,-4.65573889390825,0.));
#52849=CARTESIAN_POINT('Ctrl Pts',(72.1881442253052,-4.65573889390825,12.));
#52850=CARTESIAN_POINT('Ctrl Pts',(72.2117231908816,-4.64850275618325,0.));
#52851=CARTESIAN_POINT('Ctrl Pts',(72.2117231908816,-4.64850275618325,12.));
#52852=CARTESIAN_POINT('Ctrl Pts',(72.2353342162408,-4.64123192165628,0.));
#52853=CARTESIAN_POINT('Ctrl Pts',(72.2353342162408,-4.64123192165628,12.));
#52854=CARTESIAN_POINT('Ctrl Pts',(72.2589771779447,-4.63392636813842,0.));
#52855=CARTESIAN_POINT('Ctrl Pts',(72.2589771779447,-4.63392636813842,12.));
#52856=CARTESIAN_POINT('Ctrl Pts',(72.2826519530254,-4.62658607361465,0.));
#52857=CARTESIAN_POINT('Ctrl Pts',(72.2826519530254,-4.62658607361465,12.));
#52858=CARTESIAN_POINT('Ctrl Pts',(72.306358418981,-4.61921101624295,0.));
#52859=CARTESIAN_POINT('Ctrl Pts',(72.306358418981,-4.61921101624295,12.));
#52860=CARTESIAN_POINT('Ctrl Pts',(72.330096453767,-4.61180117435869,0.));
#52861=CARTESIAN_POINT('Ctrl Pts',(72.330096453767,-4.61180117435869,12.));
#52862=CARTESIAN_POINT('Ctrl Pts',(72.3538659357932,-4.60435652647463,0.));
#52863=CARTESIAN_POINT('Ctrl Pts',(72.3538659357932,-4.60435652647463,12.));
#52864=CARTESIAN_POINT('Ctrl Pts',(72.3776667439244,-4.5968770512734,0.));
#52865=CARTESIAN_POINT('Ctrl Pts',(72.3776667439244,-4.5968770512734,12.));
#52866=CARTESIAN_POINT('Ctrl Pts',(72.4014987574789,-4.58936272760551,0.));
#52867=CARTESIAN_POINT('Ctrl Pts',(72.4014987574789,-4.58936272760551,12.));
#52868=CARTESIAN_POINT('Ctrl Pts',(72.4253618562249,-4.58181353448851,0.));
#52869=CARTESIAN_POINT('Ctrl Pts',(72.4253618562249,-4.58181353448851,12.));
#52870=CARTESIAN_POINT('Ctrl Pts',(72.449255920373,-4.57422945111094,0.));
#52871=CARTESIAN_POINT('Ctrl Pts',(72.449255920373,-4.57422945111094,12.));
#52872=CARTESIAN_POINT('Ctrl Pts',(72.473180830571,-4.56661045683367,0.));
#52873=CARTESIAN_POINT('Ctrl Pts',(72.473180830571,-4.56661045683367,12.));
#52874=CARTESIAN_POINT('Ctrl Pts',(72.4971364679055,-4.55895653118214,0.));
#52875=CARTESIAN_POINT('Ctrl Pts',(72.4971364679055,-4.55895653118214,12.));
#52876=CARTESIAN_POINT('Ctrl Pts',(72.5211227138997,-4.55126765384403,0.));
#52877=CARTESIAN_POINT('Ctrl Pts',(72.5211227138997,-4.55126765384403,12.));
#52878=CARTESIAN_POINT('Ctrl Pts',(72.5451394505106,-4.54354380466825,0.));
#52879=CARTESIAN_POINT('Ctrl Pts',(72.5451394505106,-4.54354380466825,12.));
#52880=CARTESIAN_POINT('Ctrl Pts',(72.5691865601225,-4.53578496366802,0.));
#52881=CARTESIAN_POINT('Ctrl Pts',(72.5691865601225,-4.53578496366802,12.));
#52882=CARTESIAN_POINT('Ctrl Pts',(72.5932639255406,-4.5279911110239,0.));
#52883=CARTESIAN_POINT('Ctrl Pts',(72.5932639255406,-4.5279911110239,12.));
#52884=CARTESIAN_POINT('Ctrl Pts',(72.6173714299935,-4.52016222707632,0.));
#52885=CARTESIAN_POINT('Ctrl Pts',(72.6173714299935,-4.52016222707632,12.));
#52886=CARTESIAN_POINT('Ctrl Pts',(72.6415089571314,-4.5122982923226,0.));
#52887=CARTESIAN_POINT('Ctrl Pts',(72.6415089571314,-4.5122982923226,12.));
#52888=CARTESIAN_POINT('Ctrl Pts',(72.6656763910241,-4.50439928741605,0.));
#52889=CARTESIAN_POINT('Ctrl Pts',(72.6656763910241,-4.50439928741605,12.));
#52890=CARTESIAN_POINT('Ctrl Pts',(72.689873616155,-4.49646519316822,0.));
#52891=CARTESIAN_POINT('Ctrl Pts',(72.689873616155,-4.49646519316822,12.));
#52892=CARTESIAN_POINT('Ctrl Pts',(72.7141005174153,-4.48849599055354,0.));
#52893=CARTESIAN_POINT('Ctrl Pts',(72.7141005174153,-4.48849599055354,12.));
#52894=CARTESIAN_POINT('Ctrl Pts',(72.7383569801042,-4.48049166070223,0.));
#52895=CARTESIAN_POINT('Ctrl Pts',(72.7383569801042,-4.48049166070223,12.));
#52896=CARTESIAN_POINT('Ctrl Pts',(72.7626428899287,-4.47245218489623,0.));
#52897=CARTESIAN_POINT('Ctrl Pts',(72.7626428899287,-4.47245218489623,12.));
#52898=CARTESIAN_POINT('Ctrl Pts',(72.7869581329994,-4.46437754456796,0.));
#52899=CARTESIAN_POINT('Ctrl Pts',(72.7869581329994,-4.46437754456796,12.));
#52900=CARTESIAN_POINT('Ctrl Pts',(72.8113025958258,-4.45626772130138,0.));
#52901=CARTESIAN_POINT('Ctrl Pts',(72.8113025958258,-4.45626772130138,12.));
#52902=CARTESIAN_POINT('Ctrl Pts',(72.8356761653064,-4.44812269683724,0.));
#52903=CARTESIAN_POINT('Ctrl Pts',(72.8356761653064,-4.44812269683724,12.));
#52904=CARTESIAN_POINT('Ctrl Pts',(72.8600787287316,-4.43994245306805,0.));
#52905=CARTESIAN_POINT('Ctrl Pts',(72.8600787287316,-4.43994245306805,12.));
#52906=CARTESIAN_POINT('Ctrl Pts',(72.8845101737856,-4.43172697203342,0.));
#52907=CARTESIAN_POINT('Ctrl Pts',(72.8845101737856,-4.43172697203342,12.));
#52908=CARTESIAN_POINT('Ctrl Pts',(72.9089703885463,-4.42347623591942,0.));
#52909=CARTESIAN_POINT('Ctrl Pts',(72.9089703885463,-4.42347623591942,12.));
#52910=CARTESIAN_POINT('Ctrl Pts',(72.9334592614828,-4.41519022705927,0.));
#52911=CARTESIAN_POINT('Ctrl Pts',(72.9334592614828,-4.41519022705927,12.));
#52912=CARTESIAN_POINT('Ctrl Pts',(72.9579766814495,-4.40686892793965,0.));
#52913=CARTESIAN_POINT('Ctrl Pts',(72.9579766814495,-4.40686892793965,12.));
#52914=CARTESIAN_POINT('Ctrl Pts',(72.9825225376839,-4.39851232119731,0.));
#52915=CARTESIAN_POINT('Ctrl Pts',(72.9825225376839,-4.39851232119731,12.));
#52916=CARTESIAN_POINT('Ctrl Pts',(73.0070967198033,-4.39012038961145,0.));
#52917=CARTESIAN_POINT('Ctrl Pts',(73.0070967198033,-4.39012038961145,12.));
#52918=CARTESIAN_POINT('Ctrl Pts',(73.031699117799,-4.38169311610153,0.));
#52919=CARTESIAN_POINT('Ctrl Pts',(73.031699117799,-4.38169311610153,12.));
#52920=CARTESIAN_POINT('Ctrl Pts',(73.0563296220301,-4.37323048372607,0.));
#52921=CARTESIAN_POINT('Ctrl Pts',(73.0563296220301,-4.37323048372607,12.));
#52922=CARTESIAN_POINT('Ctrl Pts',(73.0809881232111,-4.36473247568638,0.));
#52923=CARTESIAN_POINT('Ctrl Pts',(73.0809881232111,-4.36473247568638,12.));
#52924=CARTESIAN_POINT('Ctrl Pts',(73.1056745124099,-4.35619907532716,0.));
#52925=CARTESIAN_POINT('Ctrl Pts',(73.1056745124099,-4.35619907532716,12.));
#52926=CARTESIAN_POINT('Ctrl Pts',(73.1303886810602,-4.34763026613155,0.));
#52927=CARTESIAN_POINT('Ctrl Pts',(73.1303886810602,-4.34763026613155,12.));
#52928=CARTESIAN_POINT('Ctrl Pts',(73.1551305209692,-4.3390260317214,0.));
#52929=CARTESIAN_POINT('Ctrl Pts',(73.1551305209692,-4.3390260317214,12.));
#52930=CARTESIAN_POINT('Ctrl Pts',(73.1798999243234,-4.33038635585878,0.));
#52931=CARTESIAN_POINT('Ctrl Pts',(73.1798999243234,-4.33038635585878,12.));
#52932=CARTESIAN_POINT('Ctrl Pts',(73.204696783693,-4.32171122245219,0.));
#52933=CARTESIAN_POINT('Ctrl Pts',(73.204696783693,-4.32171122245219,12.));
#52934=CARTESIAN_POINT('Ctrl Pts',(73.2295209920319,-4.31300061556103,0.));
#52935=CARTESIAN_POINT('Ctrl Pts',(73.2295209920319,-4.31300061556103,12.));
#52936=CARTESIAN_POINT('Ctrl Pts',(73.2543724426562,-4.30425451938234,0.));
#52937=CARTESIAN_POINT('Ctrl Pts',(73.2543724426562,-4.30425451938234,12.));
#52938=CARTESIAN_POINT('Ctrl Pts',(73.2792510292243,-4.29547291824289,0.));
#52939=CARTESIAN_POINT('Ctrl Pts',(73.2792510292243,-4.29547291824289,12.));
#52940=CARTESIAN_POINT('Ctrl Pts',(73.3041566457134,-4.28665579659302,0.));
#52941=CARTESIAN_POINT('Ctrl Pts',(73.3041566457134,-4.28665579659302,12.));
#52942=CARTESIAN_POINT('Ctrl Pts',(73.3290891863959,-4.27780313900392,0.));
#52943=CARTESIAN_POINT('Ctrl Pts',(73.3290891863959,-4.27780313900392,12.));
#52944=CARTESIAN_POINT('Ctrl Pts',(73.354048545808,-4.26891493016703,0.));
#52945=CARTESIAN_POINT('Ctrl Pts',(73.354048545808,-4.26891493016703,12.));
#52946=CARTESIAN_POINT('Ctrl Pts',(73.3790346187953,-4.25999115489905,0.));
#52947=CARTESIAN_POINT('Ctrl Pts',(73.3790346187953,-4.25999115489905,12.));
#52948=CARTESIAN_POINT('Ctrl Pts',(73.4040473005603,-4.25103179814892,0.));
#52949=CARTESIAN_POINT('Ctrl Pts',(73.4040473005603,-4.25103179814892,12.));
#52950=CARTESIAN_POINT('Ctrl Pts',(73.4290864867103,-4.24203684500941,0.));
#52951=CARTESIAN_POINT('Ctrl Pts',(73.4290864867103,-4.24203684500941,12.));
#52952=CARTESIAN_POINT('Ctrl Pts',(73.4541520732943,-4.23300628072758,0.));
#52953=CARTESIAN_POINT('Ctrl Pts',(73.4541520732943,-4.23300628072758,12.));
#52954=CARTESIAN_POINT('Ctrl Pts',(73.4792439568624,-4.22394009072753,0.));
#52955=CARTESIAN_POINT('Ctrl Pts',(73.4792439568624,-4.22394009072753,12.));
#52956=CARTESIAN_POINT('Ctrl Pts',(73.5043620344107,-4.21483826059437,0.));
#52957=CARTESIAN_POINT('Ctrl Pts',(73.5043620344107,-4.21483826059437,12.));
#52958=CARTESIAN_POINT('Ctrl Pts',(73.5295062032621,-4.20570077603727,0.));
#52959=CARTESIAN_POINT('Ctrl Pts',(73.5295062032621,-4.20570077603727,12.));
#52960=CARTESIAN_POINT('Ctrl Pts',(73.554676360957,-4.19652762286127,0.));
#52961=CARTESIAN_POINT('Ctrl Pts',(73.554676360957,-4.19652762286127,12.));
#52962=CARTESIAN_POINT('Ctrl Pts',(73.5798724051519,-4.18731878694238,0.));
#52963=CARTESIAN_POINT('Ctrl Pts',(73.5798724051519,-4.18731878694238,12.));
#52964=CARTESIAN_POINT('Ctrl Pts',(73.6050942334773,-4.17807425419817,0.));
#52965=CARTESIAN_POINT('Ctrl Pts',(73.6050942334773,-4.17807425419817,12.));
#52966=CARTESIAN_POINT('Ctrl Pts',(73.6303417435262,-4.16879401058787,0.));
#52967=CARTESIAN_POINT('Ctrl Pts',(73.6303417435262,-4.16879401058787,12.));
#52968=CARTESIAN_POINT('Ctrl Pts',(73.6556148331504,-4.15947804217791,0.));
#52969=CARTESIAN_POINT('Ctrl Pts',(73.6556148331504,-4.15947804217791,12.));
#52970=CARTESIAN_POINT('Ctrl Pts',(73.6809134006909,-4.15012633519728,0.));
#52971=CARTESIAN_POINT('Ctrl Pts',(73.6809134006909,-4.15012633519728,12.));
#52972=CARTESIAN_POINT('Ctrl Pts',(73.7062373452344,-4.14073887610155,0.));
#52973=CARTESIAN_POINT('Ctrl Pts',(73.7062373452344,-4.14073887610155,12.));
#52974=CARTESIAN_POINT('Ctrl Pts',(73.7315865668508,-4.13131565163575,0.));
#52975=CARTESIAN_POINT('Ctrl Pts',(73.7315865668508,-4.13131565163575,12.));
#52976=CARTESIAN_POINT('Ctrl Pts',(73.7569609668501,-4.12185664890551,0.));
#52977=CARTESIAN_POINT('Ctrl Pts',(73.7569609668501,-4.12185664890551,12.));
#52978=CARTESIAN_POINT('Ctrl Pts',(73.7823604472126,-4.1123618552278,0.));
#52979=CARTESIAN_POINT('Ctrl Pts',(73.7823604472126,-4.1123618552278,12.));
#52980=CARTESIAN_POINT('Ctrl Pts',(73.8077849100314,-4.10283125798724,0.));
#52981=CARTESIAN_POINT('Ctrl Pts',(73.8077849100314,-4.10283125798724,12.));
#52982=CARTESIAN_POINT('Ctrl Pts',(73.8332342568978,-4.09326484448232,0.));
#52983=CARTESIAN_POINT('Ctrl Pts',(73.8332342568978,-4.09326484448232,12.));
#52984=CARTESIAN_POINT('Ctrl Pts',(73.8587083884208,-4.0836626018068,0.));
#52985=CARTESIAN_POINT('Ctrl Pts',(73.8587083884208,-4.0836626018068,12.));
#52986=CARTESIAN_POINT('Ctrl Pts',(73.884207203405,-4.07402451665253,0.));
#52987=CARTESIAN_POINT('Ctrl Pts',(73.884207203405,-4.07402451665253,12.));
#52988=CARTESIAN_POINT('Ctrl Pts',(73.9097305995173,-4.06435057547335,0.));
#52989=CARTESIAN_POINT('Ctrl Pts',(73.9097305995173,-4.06435057547335,12.));
#52990=CARTESIAN_POINT('Ctrl Pts',(73.9352784747665,-4.05464076484762,0.));
#52991=CARTESIAN_POINT('Ctrl Pts',(73.9352784747665,-4.05464076484762,12.));
#52992=CARTESIAN_POINT('Ctrl Pts',(73.9608507287943,-4.04489507179964,0.));
#52993=CARTESIAN_POINT('Ctrl Pts',(73.9608507287943,-4.04489507179964,12.));
#52994=CARTESIAN_POINT('Ctrl Pts',(73.9864472641025,-4.0351134841066,0.));
#52995=CARTESIAN_POINT('Ctrl Pts',(73.9864472641025,-4.0351134841066,12.));
#52996=CARTESIAN_POINT('Ctrl Pts',(74.0120679876396,-4.02529599070085,0.));
#52997=CARTESIAN_POINT('Ctrl Pts',(74.0120679876396,-4.02529599070085,12.));
#52998=CARTESIAN_POINT('Ctrl Pts',(74.0377128111754,-4.01544258176693,0.));
#52999=CARTESIAN_POINT('Ctrl Pts',(74.0377128111754,-4.01544258176693,12.));
#53000=CARTESIAN_POINT('Ctrl Pts',(74.0633816477912,-4.0055532478546,0.));
#53001=CARTESIAN_POINT('Ctrl Pts',(74.0633816477912,-4.0055532478546,12.));
#53002=CARTESIAN_POINT('Ctrl Pts',(74.0890744091088,-3.99562797918271,0.));
#53003=CARTESIAN_POINT('Ctrl Pts',(74.0890744091088,-3.99562797918271,12.));
#53004=CARTESIAN_POINT('Ctrl Pts',(74.1147910020869,-3.98566676483639,0.));
#53005=CARTESIAN_POINT('Ctrl Pts',(74.1147910020869,-3.98566676483639,12.));
#53006=CARTESIAN_POINT('Ctrl Pts',(74.1405313263198,-3.97566959209546,0.));
#53007=CARTESIAN_POINT('Ctrl Pts',(74.1405313263198,-3.97566959209546,12.));
#53008=CARTESIAN_POINT('Ctrl Pts',(74.1662952702689,-3.96563644549423,0.));
#53009=CARTESIAN_POINT('Ctrl Pts',(74.1662952702689,-3.96563644549423,12.));
#53010=CARTESIAN_POINT('Ctrl Pts',(74.1920827166861,-3.9555673082116,0.));
#53011=CARTESIAN_POINT('Ctrl Pts',(74.1920827166861,-3.9555673082116,12.));
#53012=CARTESIAN_POINT('Ctrl Pts',(74.217893549314,-3.94546216377499,0.));
#53013=CARTESIAN_POINT('Ctrl Pts',(74.217893549314,-3.94546216377499,12.));
#53014=CARTESIAN_POINT('Ctrl Pts',(74.2437276593763,-3.9353209977423,0.));
#53015=CARTESIAN_POINT('Ctrl Pts',(74.2437276593763,-3.9353209977423,12.));
#53016=CARTESIAN_POINT('Ctrl Pts',(74.2695849516134,-3.92514379920729,0.));
#53017=CARTESIAN_POINT('Ctrl Pts',(74.2695849516134,-3.92514379920729,12.));
#53018=CARTESIAN_POINT('Ctrl Pts',(74.2954653518346,-3.91493056284964,0.));
#53019=CARTESIAN_POINT('Ctrl Pts',(74.2954653518346,-3.91493056284964,12.));
#53020=CARTESIAN_POINT('Ctrl Pts',(74.3213688089495,-3.9046812890452,0.));
#53021=CARTESIAN_POINT('Ctrl Pts',(74.3213688089495,-3.9046812890452,12.));
#53022=CARTESIAN_POINT('Ctrl Pts',(74.3472952898,-3.89439598145194,0.));
#53023=CARTESIAN_POINT('Ctrl Pts',(74.3472952898,-3.89439598145194,12.));
#53024=CARTESIAN_POINT('Ctrl Pts',(74.3680548786039,-3.8861389124787,0.));
#53025=CARTESIAN_POINT('Ctrl Pts',(74.3680548786039,-3.8861389124787,12.));
#53026=CARTESIAN_POINT('Ctrl Pts',(74.3836349188809,-3.87992989995678,0.));
#53027=CARTESIAN_POINT('Ctrl Pts',(74.3836349188809,-3.87992989995678,12.));
#53028=CARTESIAN_POINT('Ctrl Pts',(74.3940262116251,-3.87578335377301,0.));
#53029=CARTESIAN_POINT('Ctrl Pts',(74.3940262116251,-3.87578335377301,12.));
#53030=CARTESIAN_POINT('Ctrl Pts',(74.3992230078037,-3.87370827955545,0.));
#53031=CARTESIAN_POINT('Ctrl Pts',(74.3992230078037,-3.87370827955545,12.));
#53032=CARTESIAN_POINT('',(69.8028570375097,-5.24987136994593,0.));
#53033=CARTESIAN_POINT('Ctrl Pts',(69.8028570375097,-5.24987136994593,0.));
#53034=CARTESIAN_POINT('Ctrl Pts',(69.8066748687772,-5.24915955997427,0.));
#53035=CARTESIAN_POINT('Ctrl Pts',(69.8143154684204,-5.24773285666377,0.));
#53036=CARTESIAN_POINT('Ctrl Pts',(69.8257911792159,-5.24558355159751,0.));
#53037=CARTESIAN_POINT('Ctrl Pts',(69.841121750752,-5.2426993105457,0.));
#53038=CARTESIAN_POINT('Ctrl Pts',(69.8603343302743,-5.23906316634803,0.));
#53039=CARTESIAN_POINT('Ctrl Pts',(69.8795962381599,-5.2353961627962,0.));
#53040=CARTESIAN_POINT('Ctrl Pts',(69.8989073936688,-5.23169827290556,0.));
#53041=CARTESIAN_POINT('Ctrl Pts',(69.9182676502048,-5.22796945602794,0.));
#53042=CARTESIAN_POINT('Ctrl Pts',(69.9376767969095,-5.22420965879982,0.));
#53043=CARTESIAN_POINT('Ctrl Pts',(69.9571345870076,-5.22041882075721,0.));
#53044=CARTESIAN_POINT('Ctrl Pts',(69.9766407595385,-5.21659687881139,0.));
#53045=CARTESIAN_POINT('Ctrl Pts',(69.9961950629965,-5.2127437720326,0.));
#53046=CARTESIAN_POINT('Ctrl Pts',(70.0157972802182,-5.20885944672837,0.));
#53047=CARTESIAN_POINT('Ctrl Pts',(70.0354472203546,-5.20494385478026,0.));
#53048=CARTESIAN_POINT('Ctrl Pts',(70.0551447071082,-5.20099695122656,0.));
#53049=CARTESIAN_POINT('Ctrl Pts',(70.0748895689729,-5.19701869225529,0.));
#53050=CARTESIAN_POINT('Ctrl Pts',(70.0946816270997,-5.1930090327158,0.));
#53051=CARTESIAN_POINT('Ctrl Pts',(70.1145206891885,-5.18896792486566,0.));
#53052=CARTESIAN_POINT('Ctrl Pts',(70.1344065558145,-5.18489531966265,0.));
#53053=CARTESIAN_POINT('Ctrl Pts',(70.1543390243892,-5.18079116757667,0.));
#53054=CARTESIAN_POINT('Ctrl Pts',(70.1743178937077,-5.17665541952383,0.));
#53055=CARTESIAN_POINT('Ctrl Pts',(70.1943429691167,-5.17248802793389,0.));
#53056=CARTESIAN_POINT('Ctrl Pts',(70.2144140622953,-5.16828894670109,0.));
#53057=CARTESIAN_POINT('Ctrl Pts',(70.2345309887833,-5.16405813066976,0.));
#53058=CARTESIAN_POINT('Ctrl Pts',(70.2546935662722,-5.15979553528204,0.));
#53059=CARTESIAN_POINT('Ctrl Pts',(70.2749016125105,-5.1555011161486,0.));
#53060=CARTESIAN_POINT('Ctrl Pts',(70.2951549435512,-5.15117482869254,0.));
#53061=CARTESIAN_POINT('Ctrl Pts',(70.3154533746736,-5.1468166283308,0.));
#53062=CARTESIAN_POINT('Ctrl Pts',(70.3357967211796,-5.1424264706348,0.));
#53063=CARTESIAN_POINT('Ctrl Pts',(70.3561847991714,-5.13800431148904,0.));
#53064=CARTESIAN_POINT('Ctrl Pts',(70.3766174264757,-5.13355010728568,0.));
#53065=CARTESIAN_POINT('Ctrl Pts',(70.3970944229851,-5.12906381499456,0.));
#53066=CARTESIAN_POINT('Ctrl Pts',(70.417615610161,-5.12454539205329,0.));
#53067=CARTESIAN_POINT('Ctrl Pts',(70.4381808107245,-5.11999479630212,0.));
#53068=CARTESIAN_POINT('Ctrl Pts',(70.458789848296,-5.11541198590933,0.));
#53069=CARTESIAN_POINT('Ctrl Pts',(70.4794425469825,-5.11079691929213,0.));
#53070=CARTESIAN_POINT('Ctrl Pts',(70.500138731399,-5.10614955511664,0.));
#53071=CARTESIAN_POINT('Ctrl Pts',(70.5208782268497,-5.10146985232941,0.));
#53072=CARTESIAN_POINT('Ctrl Pts',(70.5416608594526,-5.09675777018183,0.));
#53073=CARTESIAN_POINT('Ctrl Pts',(70.5624864562824,-5.09201326826135,0.));
#53074=CARTESIAN_POINT('Ctrl Pts',(70.5833548455014,-5.08723630652273,0.));
#53075=CARTESIAN_POINT('Ctrl Pts',(70.6042658562923,-5.08242684526687,0.));
#53076=CARTESIAN_POINT('Ctrl Pts',(70.6252193187878,-5.07758484512303,0.));
#53077=CARTESIAN_POINT('Ctrl Pts',(70.6462150640015,-5.07271026703355,0.));
#53078=CARTESIAN_POINT('Ctrl Pts',(70.6672529237455,-5.06780307224072,0.));
#53079=CARTESIAN_POINT('Ctrl Pts',(70.6883327305784,-5.0628632222782,0.));
#53080=CARTESIAN_POINT('Ctrl Pts',(70.7094543178438,-5.05789067897058,0.));
#53081=CARTESIAN_POINT('Ctrl Pts',(70.7306175196863,-5.05288540443483,0.));
#53082=CARTESIAN_POINT('Ctrl Pts',(70.7518221710706,-5.04784736108346,0.));
#53083=CARTESIAN_POINT('Ctrl Pts',(70.7730681077983,-5.0427765116335,0.));
#53084=CARTESIAN_POINT('Ctrl Pts',(70.7943551665059,-5.03767281910479,0.));
#53085=CARTESIAN_POINT('Ctrl Pts',(70.8156831846488,-5.03253624680941,0.));
#53086=CARTESIAN_POINT('Ctrl Pts',(70.8370520004843,-5.02736675834693,0.));
#53087=CARTESIAN_POINT('Ctrl Pts',(70.8584614530519,-5.02216431760061,0.));
#53088=CARTESIAN_POINT('Ctrl Pts',(70.8799113821452,-5.0169288887379,0.));
#53089=CARTESIAN_POINT('Ctrl Pts',(70.9014016283124,-5.01166043620568,0.));
#53090=CARTESIAN_POINT('Ctrl Pts',(70.9229320328589,-5.00635892472514,0.));
#53091=CARTESIAN_POINT('Ctrl Pts',(70.9445024378439,-5.0010243192904,0.));
#53092=CARTESIAN_POINT('Ctrl Pts',(70.9661126860773,-4.99565658516913,0.));
#53093=CARTESIAN_POINT('Ctrl Pts',(70.9877626211113,-4.99025568790665,0.));
#53094=CARTESIAN_POINT('Ctrl Pts',(71.0094520872377,-4.98482159331864,0.));
#53095=CARTESIAN_POINT('Ctrl Pts',(71.0311809294821,-4.97935426748585,0.));
#53096=CARTESIAN_POINT('Ctrl Pts',(71.0529489935961,-4.97385367675159,0.));
#53097=CARTESIAN_POINT('Ctrl Pts',(71.0747561260436,-4.96831978772191,0.));
#53098=CARTESIAN_POINT('Ctrl Pts',(71.0966021739907,-4.96275256726766,0.));
#53099=CARTESIAN_POINT('Ctrl Pts',(71.1184869853056,-4.95715198251685,0.));
#53100=CARTESIAN_POINT('Ctrl Pts',(71.1404104085552,-4.95151800085102,0.));
#53101=CARTESIAN_POINT('Ctrl Pts',(71.1623722930001,-4.94585058990341,0.));
#53102=CARTESIAN_POINT('Ctrl Pts',(71.1843724885847,-4.94014971756115,0.));
#53103=CARTESIAN_POINT('Ctrl Pts',(71.2064108459286,-4.93441535196618,0.));
#53104=CARTESIAN_POINT('Ctrl Pts',(71.2284872163273,-4.92864746150733,0.));
#53105=CARTESIAN_POINT('Ctrl Pts',(71.250601451747,-4.92284601481722,0.));
#53106=CARTESIAN_POINT('Ctrl Pts',(71.2727534048192,-4.91701098077036,0.));
#53107=CARTESIAN_POINT('Ctrl Pts',(71.294942928829,-4.91114232848603,0.));
#53108=CARTESIAN_POINT('Ctrl Pts',(71.3171698777084,-4.90524002732779,0.));
#53109=CARTESIAN_POINT('Ctrl Pts',(71.3394341060359,-4.89930404689575,0.));
#53110=CARTESIAN_POINT('Ctrl Pts',(71.3617354690325,-4.89333435702414,0.));
#53111=CARTESIAN_POINT('Ctrl Pts',(71.3840738225562,-4.88733092777975,0.));
#53112=CARTESIAN_POINT('Ctrl Pts',(71.4064490230899,-4.88129372946552,0.));
#53113=CARTESIAN_POINT('Ctrl Pts',(71.4288609277374,-4.87522273261908,0.));
#53114=CARTESIAN_POINT('Ctrl Pts',(71.4513093942255,-4.8691179080055,0.));
#53115=CARTESIAN_POINT('Ctrl Pts',(71.4737942808982,-4.86297922661503,0.));
#53116=CARTESIAN_POINT('Ctrl Pts',(71.4963154467113,-4.85680665966181,0.));
#53117=CARTESIAN_POINT('Ctrl Pts',(71.5188727512197,-4.8506001785878,0.));
#53118=CARTESIAN_POINT('Ctrl Pts',(71.5414660545739,-4.84435975506049,0.));
#53119=CARTESIAN_POINT('Ctrl Pts',(71.564095217521,-4.83808536096584,0.));
#53120=CARTESIAN_POINT('Ctrl Pts',(71.5867601014,-4.83177696840638,0.));
#53121=CARTESIAN_POINT('Ctrl Pts',(71.6094605681366,-4.82543454970027,0.));
#53122=CARTESIAN_POINT('Ctrl Pts',(71.6321964802326,-4.81905807738557,0.));
#53123=CARTESIAN_POINT('Ctrl Pts',(71.6549677007613,-4.81264752421732,0.));
#53124=CARTESIAN_POINT('Ctrl Pts',(71.6777740933705,-4.80620286316089,0.));
#53125=CARTESIAN_POINT('Ctrl Pts',(71.7006155222766,-4.79972406739014,0.));
#53126=CARTESIAN_POINT('Ctrl Pts',(71.7234918522604,-4.79321111028672,0.));
#53127=CARTESIAN_POINT('Ctrl Pts',(71.7464029486552,-4.78666396544451,0.));
#53128=CARTESIAN_POINT('Ctrl Pts',(71.7693486773449,-4.78008260666643,0.));
#53129=CARTESIAN_POINT('Ctrl Pts',(71.7923289047636,-4.77346700795788,0.));
#53130=CARTESIAN_POINT('Ctrl Pts',(71.8153434978924,-4.76681714352504,0.));
#53131=CARTESIAN_POINT('Ctrl Pts',(71.8383923242533,-4.76013298777423,0.));
#53132=CARTESIAN_POINT('Ctrl Pts',(71.8614752519008,-4.75341451531671,0.));
#53133=CARTESIAN_POINT('Ctrl Pts',(71.8845921494186,-4.74666170096546,0.));
#53134=CARTESIAN_POINT('Ctrl Pts',(71.9077428859207,-4.73987451972861,0.));
#53135=CARTESIAN_POINT('Ctrl Pts',(71.9309273310469,-4.73305294680784,0.));
#53136=CARTESIAN_POINT('Ctrl Pts',(71.9541453549582,-4.72619695759779,0.));
#53137=CARTESIAN_POINT('Ctrl Pts',(71.9773968283267,-4.71930652769081,0.));
#53138=CARTESIAN_POINT('Ctrl Pts',(72.0006816223335,-4.71238163287411,0.));
#53139=CARTESIAN_POINT('Ctrl Pts',(72.0239996086694,-4.70542224912312,0.));
#53140=CARTESIAN_POINT('Ctrl Pts',(72.047350659532,-4.69842835259997,0.));
#53141=CARTESIAN_POINT('Ctrl Pts',(72.070734647621,-4.6913999196528,0.));
#53142=CARTESIAN_POINT('Ctrl Pts',(72.0941514461283,-4.68433692682061,0.));
#53143=CARTESIAN_POINT('Ctrl Pts',(72.1176009287349,-4.67723935083087,0.));
#53144=CARTESIAN_POINT('Ctrl Pts',(72.1410829696129,-4.67010716859281,0.));
#53145=CARTESIAN_POINT('Ctrl Pts',(72.1645974434218,-4.6629403571957,0.));
#53146=CARTESIAN_POINT('Ctrl Pts',(72.1881442253052,-4.65573889390825,0.));
#53147=CARTESIAN_POINT('Ctrl Pts',(72.2117231908816,-4.64850275618325,0.));
#53148=CARTESIAN_POINT('Ctrl Pts',(72.2353342162408,-4.64123192165628,0.));
#53149=CARTESIAN_POINT('Ctrl Pts',(72.2589771779447,-4.63392636813842,0.));
#53150=CARTESIAN_POINT('Ctrl Pts',(72.2826519530254,-4.62658607361465,0.));
#53151=CARTESIAN_POINT('Ctrl Pts',(72.306358418981,-4.61921101624295,0.));
#53152=CARTESIAN_POINT('Ctrl Pts',(72.330096453767,-4.61180117435869,0.));
#53153=CARTESIAN_POINT('Ctrl Pts',(72.3538659357932,-4.60435652647463,0.));
#53154=CARTESIAN_POINT('Ctrl Pts',(72.3776667439244,-4.5968770512734,0.));
#53155=CARTESIAN_POINT('Ctrl Pts',(72.4014987574789,-4.58936272760551,0.));
#53156=CARTESIAN_POINT('Ctrl Pts',(72.4253618562249,-4.58181353448851,0.));
#53157=CARTESIAN_POINT('Ctrl Pts',(72.449255920373,-4.57422945111094,0.));
#53158=CARTESIAN_POINT('Ctrl Pts',(72.473180830571,-4.56661045683367,0.));
#53159=CARTESIAN_POINT('Ctrl Pts',(72.4971364679055,-4.55895653118214,0.));
#53160=CARTESIAN_POINT('Ctrl Pts',(72.5211227138997,-4.55126765384403,0.));
#53161=CARTESIAN_POINT('Ctrl Pts',(72.5451394505106,-4.54354380466825,0.));
#53162=CARTESIAN_POINT('Ctrl Pts',(72.5691865601225,-4.53578496366802,0.));
#53163=CARTESIAN_POINT('Ctrl Pts',(72.5932639255406,-4.5279911110239,0.));
#53164=CARTESIAN_POINT('Ctrl Pts',(72.6173714299935,-4.52016222707632,0.));
#53165=CARTESIAN_POINT('Ctrl Pts',(72.6415089571314,-4.5122982923226,0.));
#53166=CARTESIAN_POINT('Ctrl Pts',(72.6656763910241,-4.50439928741605,0.));
#53167=CARTESIAN_POINT('Ctrl Pts',(72.689873616155,-4.49646519316822,0.));
#53168=CARTESIAN_POINT('Ctrl Pts',(72.7141005174153,-4.48849599055354,0.));
#53169=CARTESIAN_POINT('Ctrl Pts',(72.7383569801042,-4.48049166070223,0.));
#53170=CARTESIAN_POINT('Ctrl Pts',(72.7626428899287,-4.47245218489623,0.));
#53171=CARTESIAN_POINT('Ctrl Pts',(72.7869581329994,-4.46437754456796,0.));
#53172=CARTESIAN_POINT('Ctrl Pts',(72.8113025958258,-4.45626772130138,0.));
#53173=CARTESIAN_POINT('Ctrl Pts',(72.8356761653064,-4.44812269683724,0.));
#53174=CARTESIAN_POINT('Ctrl Pts',(72.8600787287316,-4.43994245306805,0.));
#53175=CARTESIAN_POINT('Ctrl Pts',(72.8845101737856,-4.43172697203342,0.));
#53176=CARTESIAN_POINT('Ctrl Pts',(72.9089703885463,-4.42347623591942,0.));
#53177=CARTESIAN_POINT('Ctrl Pts',(72.9334592614828,-4.41519022705927,0.));
#53178=CARTESIAN_POINT('Ctrl Pts',(72.9579766814495,-4.40686892793965,0.));
#53179=CARTESIAN_POINT('Ctrl Pts',(72.9825225376839,-4.39851232119731,0.));
#53180=CARTESIAN_POINT('Ctrl Pts',(73.0070967198033,-4.39012038961145,0.));
#53181=CARTESIAN_POINT('Ctrl Pts',(73.031699117799,-4.38169311610153,0.));
#53182=CARTESIAN_POINT('Ctrl Pts',(73.0563296220301,-4.37323048372607,0.));
#53183=CARTESIAN_POINT('Ctrl Pts',(73.0809881232111,-4.36473247568638,0.));
#53184=CARTESIAN_POINT('Ctrl Pts',(73.1056745124099,-4.35619907532716,0.));
#53185=CARTESIAN_POINT('Ctrl Pts',(73.1303886810602,-4.34763026613155,0.));
#53186=CARTESIAN_POINT('Ctrl Pts',(73.1551305209692,-4.3390260317214,0.));
#53187=CARTESIAN_POINT('Ctrl Pts',(73.1798999243234,-4.33038635585878,0.));
#53188=CARTESIAN_POINT('Ctrl Pts',(73.204696783693,-4.32171122245219,0.));
#53189=CARTESIAN_POINT('Ctrl Pts',(73.2295209920319,-4.31300061556103,0.));
#53190=CARTESIAN_POINT('Ctrl Pts',(73.2543724426562,-4.30425451938234,0.));
#53191=CARTESIAN_POINT('Ctrl Pts',(73.2792510292243,-4.29547291824289,0.));
#53192=CARTESIAN_POINT('Ctrl Pts',(73.3041566457134,-4.28665579659302,0.));
#53193=CARTESIAN_POINT('Ctrl Pts',(73.3290891863959,-4.27780313900392,0.));
#53194=CARTESIAN_POINT('Ctrl Pts',(73.354048545808,-4.26891493016703,0.));
#53195=CARTESIAN_POINT('Ctrl Pts',(73.3790346187953,-4.25999115489905,0.));
#53196=CARTESIAN_POINT('Ctrl Pts',(73.4040473005603,-4.25103179814892,0.));
#53197=CARTESIAN_POINT('Ctrl Pts',(73.4290864867103,-4.24203684500941,0.));
#53198=CARTESIAN_POINT('Ctrl Pts',(73.4541520732943,-4.23300628072758,0.));
#53199=CARTESIAN_POINT('Ctrl Pts',(73.4792439568624,-4.22394009072753,0.));
#53200=CARTESIAN_POINT('Ctrl Pts',(73.5043620344107,-4.21483826059437,0.));
#53201=CARTESIAN_POINT('Ctrl Pts',(73.5295062032621,-4.20570077603727,0.));
#53202=CARTESIAN_POINT('Ctrl Pts',(73.554676360957,-4.19652762286127,0.));
#53203=CARTESIAN_POINT('Ctrl Pts',(73.5798724051519,-4.18731878694238,0.));
#53204=CARTESIAN_POINT('Ctrl Pts',(73.6050942334773,-4.17807425419817,0.));
#53205=CARTESIAN_POINT('Ctrl Pts',(73.6303417435262,-4.16879401058787,0.));
#53206=CARTESIAN_POINT('Ctrl Pts',(73.6556148331504,-4.15947804217791,0.));
#53207=CARTESIAN_POINT('Ctrl Pts',(73.6809134006909,-4.15012633519728,0.));
#53208=CARTESIAN_POINT('Ctrl Pts',(73.7062373452344,-4.14073887610155,0.));
#53209=CARTESIAN_POINT('Ctrl Pts',(73.7315865668508,-4.13131565163575,0.));
#53210=CARTESIAN_POINT('Ctrl Pts',(73.7569609668501,-4.12185664890551,0.));
#53211=CARTESIAN_POINT('Ctrl Pts',(73.7823604472126,-4.1123618552278,0.));
#53212=CARTESIAN_POINT('Ctrl Pts',(73.8077849100314,-4.10283125798724,0.));
#53213=CARTESIAN_POINT('Ctrl Pts',(73.8332342568978,-4.09326484448232,0.));
#53214=CARTESIAN_POINT('Ctrl Pts',(73.8587083884208,-4.0836626018068,0.));
#53215=CARTESIAN_POINT('Ctrl Pts',(73.884207203405,-4.07402451665253,0.));
#53216=CARTESIAN_POINT('Ctrl Pts',(73.9097305995173,-4.06435057547335,0.));
#53217=CARTESIAN_POINT('Ctrl Pts',(73.9352784747665,-4.05464076484762,0.));
#53218=CARTESIAN_POINT('Ctrl Pts',(73.9608507287943,-4.04489507179964,0.));
#53219=CARTESIAN_POINT('Ctrl Pts',(73.9864472641025,-4.0351134841066,0.));
#53220=CARTESIAN_POINT('Ctrl Pts',(74.0120679876396,-4.02529599070085,0.));
#53221=CARTESIAN_POINT('Ctrl Pts',(74.0377128111754,-4.01544258176693,0.));
#53222=CARTESIAN_POINT('Ctrl Pts',(74.0597159781918,-4.00696550627607,0.));
#53223=CARTESIAN_POINT('Ctrl Pts',(74.0765982943431,-4.00044689712493,0.));
#53224=CARTESIAN_POINT('Ctrl Pts',(74.0883491449661,-3.9959026674777,0.));
#53225=CARTESIAN_POINT('Ctrl Pts',(74.0949615399273,-3.99334334446576,0.));
#53226=CARTESIAN_POINT('Ctrl Pts',(74.0964320765796,-3.99277406492185,0.));
#53227=CARTESIAN_POINT('',(69.8028570375097,-5.24987136994593,12.));
#53228=CARTESIAN_POINT('',(69.8028570375097,-5.24987136994593,0.));
#53229=CARTESIAN_POINT('Ctrl Pts',(74.0964320765796,-3.99277406492185,12.));
#53230=CARTESIAN_POINT('Ctrl Pts',(74.0949615399273,-3.99334334446576,12.));
#53231=CARTESIAN_POINT('Ctrl Pts',(74.0883491449661,-3.9959026674777,12.));
#53232=CARTESIAN_POINT('Ctrl Pts',(74.0765982943431,-4.00044689712493,12.));
#53233=CARTESIAN_POINT('Ctrl Pts',(74.0597159781918,-4.00696550627607,12.));
#53234=CARTESIAN_POINT('Ctrl Pts',(74.0377128111754,-4.01544258176693,12.));
#53235=CARTESIAN_POINT('Ctrl Pts',(74.0120679876396,-4.02529599070085,12.));
#53236=CARTESIAN_POINT('Ctrl Pts',(73.9864472641025,-4.0351134841066,12.));
#53237=CARTESIAN_POINT('Ctrl Pts',(73.9608507287943,-4.04489507179964,12.));
#53238=CARTESIAN_POINT('Ctrl Pts',(73.9352784747665,-4.05464076484762,12.));
#53239=CARTESIAN_POINT('Ctrl Pts',(73.9097305995173,-4.06435057547335,12.));
#53240=CARTESIAN_POINT('Ctrl Pts',(73.884207203405,-4.07402451665253,12.));
#53241=CARTESIAN_POINT('Ctrl Pts',(73.8587083884208,-4.0836626018068,12.));
#53242=CARTESIAN_POINT('Ctrl Pts',(73.8332342568978,-4.09326484448232,12.));
#53243=CARTESIAN_POINT('Ctrl Pts',(73.8077849100314,-4.10283125798724,12.));
#53244=CARTESIAN_POINT('Ctrl Pts',(73.7823604472126,-4.1123618552278,12.));
#53245=CARTESIAN_POINT('Ctrl Pts',(73.7569609668501,-4.12185664890551,12.));
#53246=CARTESIAN_POINT('Ctrl Pts',(73.7315865668508,-4.13131565163575,12.));
#53247=CARTESIAN_POINT('Ctrl Pts',(73.7062373452344,-4.14073887610155,12.));
#53248=CARTESIAN_POINT('Ctrl Pts',(73.6809134006909,-4.15012633519728,12.));
#53249=CARTESIAN_POINT('Ctrl Pts',(73.6556148331504,-4.15947804217791,12.));
#53250=CARTESIAN_POINT('Ctrl Pts',(73.6303417435262,-4.16879401058787,12.));
#53251=CARTESIAN_POINT('Ctrl Pts',(73.6050942334773,-4.17807425419817,12.));
#53252=CARTESIAN_POINT('Ctrl Pts',(73.5798724051519,-4.18731878694238,12.));
#53253=CARTESIAN_POINT('Ctrl Pts',(73.554676360957,-4.19652762286127,12.));
#53254=CARTESIAN_POINT('Ctrl Pts',(73.5295062032621,-4.20570077603727,12.));
#53255=CARTESIAN_POINT('Ctrl Pts',(73.5043620344107,-4.21483826059437,12.));
#53256=CARTESIAN_POINT('Ctrl Pts',(73.4792439568624,-4.22394009072753,12.));
#53257=CARTESIAN_POINT('Ctrl Pts',(73.4541520732943,-4.23300628072758,12.));
#53258=CARTESIAN_POINT('Ctrl Pts',(73.4290864867103,-4.24203684500941,12.));
#53259=CARTESIAN_POINT('Ctrl Pts',(73.4040473005603,-4.25103179814892,12.));
#53260=CARTESIAN_POINT('Ctrl Pts',(73.3790346187953,-4.25999115489905,12.));
#53261=CARTESIAN_POINT('Ctrl Pts',(73.354048545808,-4.26891493016703,12.));
#53262=CARTESIAN_POINT('Ctrl Pts',(73.3290891863959,-4.27780313900392,12.));
#53263=CARTESIAN_POINT('Ctrl Pts',(73.3041566457134,-4.28665579659302,12.));
#53264=CARTESIAN_POINT('Ctrl Pts',(73.2792510292243,-4.29547291824289,12.));
#53265=CARTESIAN_POINT('Ctrl Pts',(73.2543724426562,-4.30425451938234,12.));
#53266=CARTESIAN_POINT('Ctrl Pts',(73.2295209920319,-4.31300061556103,12.));
#53267=CARTESIAN_POINT('Ctrl Pts',(73.204696783693,-4.32171122245219,12.));
#53268=CARTESIAN_POINT('Ctrl Pts',(73.1798999243234,-4.33038635585878,12.));
#53269=CARTESIAN_POINT('Ctrl Pts',(73.1551305209692,-4.3390260317214,12.));
#53270=CARTESIAN_POINT('Ctrl Pts',(73.1303886810602,-4.34763026613155,12.));
#53271=CARTESIAN_POINT('Ctrl Pts',(73.1056745124099,-4.35619907532716,12.));
#53272=CARTESIAN_POINT('Ctrl Pts',(73.0809881232111,-4.36473247568638,12.));
#53273=CARTESIAN_POINT('Ctrl Pts',(73.0563296220301,-4.37323048372607,12.));
#53274=CARTESIAN_POINT('Ctrl Pts',(73.031699117799,-4.38169311610153,12.));
#53275=CARTESIAN_POINT('Ctrl Pts',(73.0070967198033,-4.39012038961145,12.));
#53276=CARTESIAN_POINT('Ctrl Pts',(72.9825225376839,-4.39851232119731,12.));
#53277=CARTESIAN_POINT('Ctrl Pts',(72.9579766814495,-4.40686892793965,12.));
#53278=CARTESIAN_POINT('Ctrl Pts',(72.9334592614828,-4.41519022705927,12.));
#53279=CARTESIAN_POINT('Ctrl Pts',(72.9089703885463,-4.42347623591942,12.));
#53280=CARTESIAN_POINT('Ctrl Pts',(72.8845101737856,-4.43172697203342,12.));
#53281=CARTESIAN_POINT('Ctrl Pts',(72.8600787287316,-4.43994245306805,12.));
#53282=CARTESIAN_POINT('Ctrl Pts',(72.8356761653064,-4.44812269683724,12.));
#53283=CARTESIAN_POINT('Ctrl Pts',(72.8113025958258,-4.45626772130138,12.));
#53284=CARTESIAN_POINT('Ctrl Pts',(72.7869581329994,-4.46437754456796,12.));
#53285=CARTESIAN_POINT('Ctrl Pts',(72.7626428899287,-4.47245218489623,12.));
#53286=CARTESIAN_POINT('Ctrl Pts',(72.7383569801042,-4.48049166070223,12.));
#53287=CARTESIAN_POINT('Ctrl Pts',(72.7141005174153,-4.48849599055354,12.));
#53288=CARTESIAN_POINT('Ctrl Pts',(72.689873616155,-4.49646519316822,12.));
#53289=CARTESIAN_POINT('Ctrl Pts',(72.6656763910241,-4.50439928741605,12.));
#53290=CARTESIAN_POINT('Ctrl Pts',(72.6415089571314,-4.5122982923226,12.));
#53291=CARTESIAN_POINT('Ctrl Pts',(72.6173714299935,-4.52016222707632,12.));
#53292=CARTESIAN_POINT('Ctrl Pts',(72.5932639255406,-4.5279911110239,12.));
#53293=CARTESIAN_POINT('Ctrl Pts',(72.5691865601225,-4.53578496366802,12.));
#53294=CARTESIAN_POINT('Ctrl Pts',(72.5451394505106,-4.54354380466825,12.));
#53295=CARTESIAN_POINT('Ctrl Pts',(72.5211227138997,-4.55126765384403,12.));
#53296=CARTESIAN_POINT('Ctrl Pts',(72.4971364679055,-4.55895653118214,12.));
#53297=CARTESIAN_POINT('Ctrl Pts',(72.473180830571,-4.56661045683367,12.));
#53298=CARTESIAN_POINT('Ctrl Pts',(72.449255920373,-4.57422945111094,12.));
#53299=CARTESIAN_POINT('Ctrl Pts',(72.4253618562249,-4.58181353448851,12.));
#53300=CARTESIAN_POINT('Ctrl Pts',(72.4014987574789,-4.58936272760551,12.));
#53301=CARTESIAN_POINT('Ctrl Pts',(72.3776667439244,-4.5968770512734,12.));
#53302=CARTESIAN_POINT('Ctrl Pts',(72.3538659357932,-4.60435652647463,12.));
#53303=CARTESIAN_POINT('Ctrl Pts',(72.330096453767,-4.61180117435869,12.));
#53304=CARTESIAN_POINT('Ctrl Pts',(72.306358418981,-4.61921101624295,12.));
#53305=CARTESIAN_POINT('Ctrl Pts',(72.2826519530254,-4.62658607361465,12.));
#53306=CARTESIAN_POINT('Ctrl Pts',(72.2589771779447,-4.63392636813842,12.));
#53307=CARTESIAN_POINT('Ctrl Pts',(72.2353342162408,-4.64123192165628,12.));
#53308=CARTESIAN_POINT('Ctrl Pts',(72.2117231908816,-4.64850275618325,12.));
#53309=CARTESIAN_POINT('Ctrl Pts',(72.1881442253052,-4.65573889390825,12.));
#53310=CARTESIAN_POINT('Ctrl Pts',(72.1645974434218,-4.6629403571957,12.));
#53311=CARTESIAN_POINT('Ctrl Pts',(72.1410829696129,-4.67010716859281,12.));
#53312=CARTESIAN_POINT('Ctrl Pts',(72.1176009287349,-4.67723935083087,12.));
#53313=CARTESIAN_POINT('Ctrl Pts',(72.0941514461283,-4.68433692682061,12.));
#53314=CARTESIAN_POINT('Ctrl Pts',(72.070734647621,-4.6913999196528,12.));
#53315=CARTESIAN_POINT('Ctrl Pts',(72.047350659532,-4.69842835259997,12.));
#53316=CARTESIAN_POINT('Ctrl Pts',(72.0239996086694,-4.70542224912312,12.));
#53317=CARTESIAN_POINT('Ctrl Pts',(72.0006816223335,-4.71238163287411,12.));
#53318=CARTESIAN_POINT('Ctrl Pts',(71.9773968283267,-4.71930652769081,12.));
#53319=CARTESIAN_POINT('Ctrl Pts',(71.9541453549582,-4.72619695759779,12.));
#53320=CARTESIAN_POINT('Ctrl Pts',(71.9309273310469,-4.73305294680784,12.));
#53321=CARTESIAN_POINT('Ctrl Pts',(71.9077428859207,-4.73987451972861,12.));
#53322=CARTESIAN_POINT('Ctrl Pts',(71.8845921494186,-4.74666170096546,12.));
#53323=CARTESIAN_POINT('Ctrl Pts',(71.8614752519008,-4.75341451531671,12.));
#53324=CARTESIAN_POINT('Ctrl Pts',(71.8383923242533,-4.76013298777423,12.));
#53325=CARTESIAN_POINT('Ctrl Pts',(71.8153434978924,-4.76681714352504,12.));
#53326=CARTESIAN_POINT('Ctrl Pts',(71.7923289047636,-4.77346700795788,12.));
#53327=CARTESIAN_POINT('Ctrl Pts',(71.7693486773449,-4.78008260666643,12.));
#53328=CARTESIAN_POINT('Ctrl Pts',(71.7464029486552,-4.78666396544451,12.));
#53329=CARTESIAN_POINT('Ctrl Pts',(71.7234918522604,-4.79321111028672,12.));
#53330=CARTESIAN_POINT('Ctrl Pts',(71.7006155222766,-4.79972406739014,12.));
#53331=CARTESIAN_POINT('Ctrl Pts',(71.6777740933705,-4.80620286316089,12.));
#53332=CARTESIAN_POINT('Ctrl Pts',(71.6549677007613,-4.81264752421732,12.));
#53333=CARTESIAN_POINT('Ctrl Pts',(71.6321964802326,-4.81905807738557,12.));
#53334=CARTESIAN_POINT('Ctrl Pts',(71.6094605681366,-4.82543454970027,12.));
#53335=CARTESIAN_POINT('Ctrl Pts',(71.5867601014,-4.83177696840638,12.));
#53336=CARTESIAN_POINT('Ctrl Pts',(71.564095217521,-4.83808536096584,12.));
#53337=CARTESIAN_POINT('Ctrl Pts',(71.5414660545739,-4.84435975506049,12.));
#53338=CARTESIAN_POINT('Ctrl Pts',(71.5188727512197,-4.8506001785878,12.));
#53339=CARTESIAN_POINT('Ctrl Pts',(71.4963154467113,-4.85680665966181,12.));
#53340=CARTESIAN_POINT('Ctrl Pts',(71.4737942808982,-4.86297922661503,12.));
#53341=CARTESIAN_POINT('Ctrl Pts',(71.4513093942255,-4.8691179080055,12.));
#53342=CARTESIAN_POINT('Ctrl Pts',(71.4288609277374,-4.87522273261908,12.));
#53343=CARTESIAN_POINT('Ctrl Pts',(71.4064490230899,-4.88129372946552,12.));
#53344=CARTESIAN_POINT('Ctrl Pts',(71.3840738225562,-4.88733092777975,12.));
#53345=CARTESIAN_POINT('Ctrl Pts',(71.3617354690325,-4.89333435702414,12.));
#53346=CARTESIAN_POINT('Ctrl Pts',(71.3394341060359,-4.89930404689575,12.));
#53347=CARTESIAN_POINT('Ctrl Pts',(71.3171698777084,-4.90524002732779,12.));
#53348=CARTESIAN_POINT('Ctrl Pts',(71.294942928829,-4.91114232848603,12.));
#53349=CARTESIAN_POINT('Ctrl Pts',(71.2727534048192,-4.91701098077036,12.));
#53350=CARTESIAN_POINT('Ctrl Pts',(71.250601451747,-4.92284601481722,12.));
#53351=CARTESIAN_POINT('Ctrl Pts',(71.2284872163273,-4.92864746150733,12.));
#53352=CARTESIAN_POINT('Ctrl Pts',(71.2064108459286,-4.93441535196618,12.));
#53353=CARTESIAN_POINT('Ctrl Pts',(71.1843724885847,-4.94014971756115,12.));
#53354=CARTESIAN_POINT('Ctrl Pts',(71.1623722930001,-4.94585058990341,12.));
#53355=CARTESIAN_POINT('Ctrl Pts',(71.1404104085552,-4.95151800085102,12.));
#53356=CARTESIAN_POINT('Ctrl Pts',(71.1184869853056,-4.95715198251685,12.));
#53357=CARTESIAN_POINT('Ctrl Pts',(71.0966021739907,-4.96275256726766,12.));
#53358=CARTESIAN_POINT('Ctrl Pts',(71.0747561260436,-4.96831978772191,12.));
#53359=CARTESIAN_POINT('Ctrl Pts',(71.0529489935961,-4.97385367675159,12.));
#53360=CARTESIAN_POINT('Ctrl Pts',(71.0311809294821,-4.97935426748585,12.));
#53361=CARTESIAN_POINT('Ctrl Pts',(71.0094520872377,-4.98482159331864,12.));
#53362=CARTESIAN_POINT('Ctrl Pts',(70.9877626211113,-4.99025568790665,12.));
#53363=CARTESIAN_POINT('Ctrl Pts',(70.9661126860773,-4.99565658516913,12.));
#53364=CARTESIAN_POINT('Ctrl Pts',(70.9445024378439,-5.0010243192904,12.));
#53365=CARTESIAN_POINT('Ctrl Pts',(70.9229320328589,-5.00635892472514,12.));
#53366=CARTESIAN_POINT('Ctrl Pts',(70.9014016283124,-5.01166043620568,12.));
#53367=CARTESIAN_POINT('Ctrl Pts',(70.8799113821452,-5.0169288887379,12.));
#53368=CARTESIAN_POINT('Ctrl Pts',(70.8584614530519,-5.02216431760061,12.));
#53369=CARTESIAN_POINT('Ctrl Pts',(70.8370520004843,-5.02736675834693,12.));
#53370=CARTESIAN_POINT('Ctrl Pts',(70.8156831846488,-5.03253624680941,12.));
#53371=CARTESIAN_POINT('Ctrl Pts',(70.7943551665059,-5.03767281910479,12.));
#53372=CARTESIAN_POINT('Ctrl Pts',(70.7730681077983,-5.0427765116335,12.));
#53373=CARTESIAN_POINT('Ctrl Pts',(70.7518221710706,-5.04784736108346,12.));
#53374=CARTESIAN_POINT('Ctrl Pts',(70.7306175196863,-5.05288540443483,12.));
#53375=CARTESIAN_POINT('Ctrl Pts',(70.7094543178438,-5.05789067897058,12.));
#53376=CARTESIAN_POINT('Ctrl Pts',(70.6883327305784,-5.0628632222782,12.));
#53377=CARTESIAN_POINT('Ctrl Pts',(70.6672529237455,-5.06780307224072,12.));
#53378=CARTESIAN_POINT('Ctrl Pts',(70.6462150640015,-5.07271026703355,12.));
#53379=CARTESIAN_POINT('Ctrl Pts',(70.6252193187878,-5.07758484512303,12.));
#53380=CARTESIAN_POINT('Ctrl Pts',(70.6042658562923,-5.08242684526687,12.));
#53381=CARTESIAN_POINT('Ctrl Pts',(70.5833548455014,-5.08723630652273,12.));
#53382=CARTESIAN_POINT('Ctrl Pts',(70.5624864562824,-5.09201326826135,12.));
#53383=CARTESIAN_POINT('Ctrl Pts',(70.5416608594526,-5.09675777018183,12.));
#53384=CARTESIAN_POINT('Ctrl Pts',(70.5208782268497,-5.10146985232941,12.));
#53385=CARTESIAN_POINT('Ctrl Pts',(70.500138731399,-5.10614955511664,12.));
#53386=CARTESIAN_POINT('Ctrl Pts',(70.4794425469825,-5.11079691929213,12.));
#53387=CARTESIAN_POINT('Ctrl Pts',(70.458789848296,-5.11541198590933,12.));
#53388=CARTESIAN_POINT('Ctrl Pts',(70.4381808107245,-5.11999479630212,12.));
#53389=CARTESIAN_POINT('Ctrl Pts',(70.417615610161,-5.12454539205329,12.));
#53390=CARTESIAN_POINT('Ctrl Pts',(70.3970944229851,-5.12906381499456,12.));
#53391=CARTESIAN_POINT('Ctrl Pts',(70.3766174264757,-5.13355010728568,12.));
#53392=CARTESIAN_POINT('Ctrl Pts',(70.3561847991714,-5.13800431148904,12.));
#53393=CARTESIAN_POINT('Ctrl Pts',(70.3357967211796,-5.1424264706348,12.));
#53394=CARTESIAN_POINT('Ctrl Pts',(70.3154533746736,-5.1468166283308,12.));
#53395=CARTESIAN_POINT('Ctrl Pts',(70.2951549435512,-5.15117482869254,12.));
#53396=CARTESIAN_POINT('Ctrl Pts',(70.2749016125105,-5.1555011161486,12.));
#53397=CARTESIAN_POINT('Ctrl Pts',(70.2546935662722,-5.15979553528204,12.));
#53398=CARTESIAN_POINT('Ctrl Pts',(70.2345309887833,-5.16405813066976,12.));
#53399=CARTESIAN_POINT('Ctrl Pts',(70.2144140622953,-5.16828894670109,12.));
#53400=CARTESIAN_POINT('Ctrl Pts',(70.1943429691167,-5.17248802793389,12.));
#53401=CARTESIAN_POINT('Ctrl Pts',(70.1743178937077,-5.17665541952383,12.));
#53402=CARTESIAN_POINT('Ctrl Pts',(70.1543390243892,-5.18079116757667,12.));
#53403=CARTESIAN_POINT('Ctrl Pts',(70.1344065558145,-5.18489531966265,12.));
#53404=CARTESIAN_POINT('Ctrl Pts',(70.1145206891885,-5.18896792486566,12.));
#53405=CARTESIAN_POINT('Ctrl Pts',(70.0946816270997,-5.1930090327158,12.));
#53406=CARTESIAN_POINT('Ctrl Pts',(70.0748895689729,-5.19701869225529,12.));
#53407=CARTESIAN_POINT('Ctrl Pts',(70.0551447071082,-5.20099695122656,12.));
#53408=CARTESIAN_POINT('Ctrl Pts',(70.0354472203546,-5.20494385478026,12.));
#53409=CARTESIAN_POINT('Ctrl Pts',(70.0157972802182,-5.20885944672837,12.));
#53410=CARTESIAN_POINT('Ctrl Pts',(69.9961950629965,-5.2127437720326,12.));
#53411=CARTESIAN_POINT('Ctrl Pts',(69.9766407595385,-5.21659687881139,12.));
#53412=CARTESIAN_POINT('Ctrl Pts',(69.9571345870076,-5.22041882075721,12.));
#53413=CARTESIAN_POINT('Ctrl Pts',(69.9376767969095,-5.22420965879982,12.));
#53414=CARTESIAN_POINT('Ctrl Pts',(69.9182676502048,-5.22796945602794,12.));
#53415=CARTESIAN_POINT('Ctrl Pts',(69.8989073936688,-5.23169827290556,12.));
#53416=CARTESIAN_POINT('Ctrl Pts',(69.8795962381599,-5.2353961627962,12.));
#53417=CARTESIAN_POINT('Ctrl Pts',(69.8603343302743,-5.23906316634803,12.));
#53418=CARTESIAN_POINT('Ctrl Pts',(69.841121750752,-5.2426993105457,12.));
#53419=CARTESIAN_POINT('Ctrl Pts',(69.8257911792159,-5.24558355159751,12.));
#53420=CARTESIAN_POINT('Ctrl Pts',(69.8143154684204,-5.24773285666377,12.));
#53421=CARTESIAN_POINT('Ctrl Pts',(69.8066748687772,-5.24915955997427,12.));
#53422=CARTESIAN_POINT('Ctrl Pts',(69.8028570375097,-5.24987136994593,12.));
#53423=CARTESIAN_POINT('Ctrl Pts',(74.1624659714955,-2.48034921844903,0.));
#53424=CARTESIAN_POINT('Ctrl Pts',(74.1624659714955,-2.48034921844903,4.));
#53425=CARTESIAN_POINT('Ctrl Pts',(74.1624659714955,-2.48034921844902,8.));
#53426=CARTESIAN_POINT('Ctrl Pts',(74.1624659714955,-2.48034921844902,12.));
#53427=CARTESIAN_POINT('Ctrl Pts',(74.2610905805699,-2.52879860312842,0.));
#53428=CARTESIAN_POINT('Ctrl Pts',(74.2610905805699,-2.52879860312842,4.));
#53429=CARTESIAN_POINT('Ctrl Pts',(74.2610905805699,-2.52879860312839,8.));
#53430=CARTESIAN_POINT('Ctrl Pts',(74.2610905805699,-2.52879860312839,12.));
#53431=CARTESIAN_POINT('Ctrl Pts',(74.4041075779822,-2.67239300265256,0.));
#53432=CARTESIAN_POINT('Ctrl Pts',(74.4041075779822,-2.67239300265256,4.));
#53433=CARTESIAN_POINT('Ctrl Pts',(74.4041075779824,-2.67239300265254,8.));
#53434=CARTESIAN_POINT('Ctrl Pts',(74.4041075779824,-2.67239300265254,12.));
#53435=CARTESIAN_POINT('Ctrl Pts',(74.4448761712984,-2.86656650944691,0.));
#53436=CARTESIAN_POINT('Ctrl Pts',(74.4448761712984,-2.86656650944691,4.));
#53437=CARTESIAN_POINT('Ctrl Pts',(74.4448761712985,-2.86656650944694,8.00000000000001));
#53438=CARTESIAN_POINT('Ctrl Pts',(74.4448761712985,-2.86656650944694,12.));
#53439=CARTESIAN_POINT('Ctrl Pts',(74.4416140848743,-2.94891377268036,0.));
#53440=CARTESIAN_POINT('Ctrl Pts',(74.4416140848743,-2.94891377268036,4.));
#53441=CARTESIAN_POINT('Ctrl Pts',(74.4416140848744,-2.94891377268042,8.));
#53442=CARTESIAN_POINT('Ctrl Pts',(74.4416140848744,-2.94891377268042,12.));
#53443=CARTESIAN_POINT('',(74.1624659714955,-2.48034921844903,0.));
#53444=CARTESIAN_POINT('',(74.4416140848739,-2.94891377268035,0.));
#53445=CARTESIAN_POINT('Ctrl Pts',(74.1624659714955,-2.48034921844903,0.));
#53446=CARTESIAN_POINT('Ctrl Pts',(74.2610905805699,-2.52879860312842,0.));
#53447=CARTESIAN_POINT('Ctrl Pts',(74.3428145790912,-2.61085254571364,0.));
#53448=CARTESIAN_POINT('Ctrl Pts',(74.391151343622,-2.70942211516261,0.));
#53449=CARTESIAN_POINT('Ctrl Pts',(74.42740391702,-2.78334929224933,0.));
#53450=CARTESIAN_POINT('Ctrl Pts',(74.4448761712984,-2.86656650944691,0.));
#53451=CARTESIAN_POINT('Ctrl Pts',(74.4416140848743,-2.94891377268036,0.));
#53452=CARTESIAN_POINT('',(74.4416140848739,-2.9489137726804,12.));
#53453=CARTESIAN_POINT('Ctrl Pts',(74.4416140848743,-2.94891377268036,0.));
#53454=CARTESIAN_POINT('Ctrl Pts',(74.4416140848743,-2.94891377268036,4.));
#53455=CARTESIAN_POINT('Ctrl Pts',(74.4416140848744,-2.94891377268042,8.));
#53456=CARTESIAN_POINT('Ctrl Pts',(74.4416140848744,-2.94891377268042,12.));
#53457=CARTESIAN_POINT('',(74.1624659714955,-2.48034921844902,12.));
#53458=CARTESIAN_POINT('Ctrl Pts',(74.4416140848744,-2.94891377268042,12.));
#53459=CARTESIAN_POINT('Ctrl Pts',(74.4448761712985,-2.86656650944694,12.));
#53460=CARTESIAN_POINT('Ctrl Pts',(74.4274039170202,-2.78334929224934,12.));
#53461=CARTESIAN_POINT('Ctrl Pts',(74.3911513436221,-2.7094221151626,12.));
#53462=CARTESIAN_POINT('Ctrl Pts',(74.3428145790913,-2.61085254571361,12.));
#53463=CARTESIAN_POINT('Ctrl Pts',(74.2610905805699,-2.52879860312839,12.));
#53464=CARTESIAN_POINT('Ctrl Pts',(74.1624659714955,-2.48034921844902,12.));
#53465=CARTESIAN_POINT('Ctrl Pts',(74.1624659714955,-2.48034921844902,12.));
#53466=CARTESIAN_POINT('Ctrl Pts',(74.1624659714955,-2.48034921844902,8.));
#53467=CARTESIAN_POINT('Ctrl Pts',(74.1624659714955,-2.48034921844903,4.));
#53468=CARTESIAN_POINT('Ctrl Pts',(74.1624659714955,-2.48034921844903,0.));
#53469=CARTESIAN_POINT('Origin',(3.74491326291036E-10,-1.62512913209676E-11,
0.));
#53470=CARTESIAN_POINT('Origin',(3.74491326291036E-10,-1.62512913209676E-11,
12.));
#53471=CARTESIAN_POINT('Origin',(3.74491326291036E-10,-1.62512913209676E-11,
0.));
#53472=CARTESIAN_POINT('Ctrl Pts',(73.8227522002498,-10.0225374821205,0.));
#53473=CARTESIAN_POINT('Ctrl Pts',(73.8227522002498,-10.0225374821205,4.));
#53474=CARTESIAN_POINT('Ctrl Pts',(73.8227522002498,-10.0225374821205,8.));
#53475=CARTESIAN_POINT('Ctrl Pts',(73.8227522002498,-10.0225374821205,12.));
#53476=CARTESIAN_POINT('Ctrl Pts',(73.8079696346554,-10.1314210536415,0.));
#53477=CARTESIAN_POINT('Ctrl Pts',(73.8079696346554,-10.1314210536415,4.));
#53478=CARTESIAN_POINT('Ctrl Pts',(73.8079696346554,-10.1314210536415,8.00000000000001));
#53479=CARTESIAN_POINT('Ctrl Pts',(73.8079696346554,-10.1314210536415,12.));
#53480=CARTESIAN_POINT('Ctrl Pts',(73.7169567649191,-10.3125002643518,0.));
#53481=CARTESIAN_POINT('Ctrl Pts',(73.7169567649191,-10.3125002643518,4.));
#53482=CARTESIAN_POINT('Ctrl Pts',(73.7169567649191,-10.3125002643518,7.99999999999999));
#53483=CARTESIAN_POINT('Ctrl Pts',(73.7169567649191,-10.3125002643518,12.));
#53484=CARTESIAN_POINT('Ctrl Pts',(73.5456341632196,-10.4125694172277,0.));
#53485=CARTESIAN_POINT('Ctrl Pts',(73.5456341632196,-10.4125694172277,4.));
#53486=CARTESIAN_POINT('Ctrl Pts',(73.5456341632196,-10.4125694172277,8.00000000000001));
#53487=CARTESIAN_POINT('Ctrl Pts',(73.5456341632196,-10.4125694172277,12.));
#53488=CARTESIAN_POINT('Ctrl Pts',(73.4664795929519,-10.435509926739,0.));
#53489=CARTESIAN_POINT('Ctrl Pts',(73.4664795929519,-10.435509926739,4.));
#53490=CARTESIAN_POINT('Ctrl Pts',(73.4664795929519,-10.435509926739,8.));
#53491=CARTESIAN_POINT('Ctrl Pts',(73.4664795929519,-10.435509926739,12.));
#53492=CARTESIAN_POINT('',(73.8227522002498,-10.0225374821205,0.));
#53493=CARTESIAN_POINT('',(73.4664795929519,-10.4355099267391,0.));
#53494=CARTESIAN_POINT('Ctrl Pts',(73.8227522002498,-10.0225374821205,0.));
#53495=CARTESIAN_POINT('Ctrl Pts',(73.8079696346554,-10.1314210536415,0.));
#53496=CARTESIAN_POINT('Ctrl Pts',(73.7559622805204,-10.2348948883331,0.));
#53497=CARTESIAN_POINT('Ctrl Pts',(73.6777313404382,-10.311916459242,0.));
#53498=CARTESIAN_POINT('Ctrl Pts',(73.6190581353765,-10.3696826374238,0.));
#53499=CARTESIAN_POINT('Ctrl Pts',(73.5456341632196,-10.4125694172277,0.));
#53500=CARTESIAN_POINT('Ctrl Pts',(73.4664795929519,-10.435509926739,0.));
#53501=CARTESIAN_POINT('',(73.4664795929519,-10.4355099267391,12.));
#53502=CARTESIAN_POINT('Ctrl Pts',(73.4664795929519,-10.435509926739,0.));
#53503=CARTESIAN_POINT('Ctrl Pts',(73.4664795929519,-10.435509926739,4.));
#53504=CARTESIAN_POINT('Ctrl Pts',(73.4664795929519,-10.435509926739,8.));
#53505=CARTESIAN_POINT('Ctrl Pts',(73.4664795929519,-10.435509926739,12.));
#53506=CARTESIAN_POINT('',(73.8227522002498,-10.0225374821205,12.));
#53507=CARTESIAN_POINT('Ctrl Pts',(73.4664795929519,-10.435509926739,12.));
#53508=CARTESIAN_POINT('Ctrl Pts',(73.5456341632196,-10.4125694172277,12.));
#53509=CARTESIAN_POINT('Ctrl Pts',(73.6190581353765,-10.3696826374237,12.));
#53510=CARTESIAN_POINT('Ctrl Pts',(73.6777313404382,-10.311916459242,12.));
#53511=CARTESIAN_POINT('Ctrl Pts',(73.7559622805204,-10.2348948883331,12.));
#53512=CARTESIAN_POINT('Ctrl Pts',(73.8079696346554,-10.1314210536415,12.));
#53513=CARTESIAN_POINT('Ctrl Pts',(73.8227522002498,-10.0225374821205,12.));
#53514=CARTESIAN_POINT('Ctrl Pts',(73.8227522002498,-10.0225374821205,12.));
#53515=CARTESIAN_POINT('Ctrl Pts',(73.8227522002498,-10.0225374821205,8.));
#53516=CARTESIAN_POINT('Ctrl Pts',(73.8227522002498,-10.0225374821205,4.));
#53517=CARTESIAN_POINT('Ctrl Pts',(73.8227522002498,-10.0225374821205,0.));
#53518=CARTESIAN_POINT('Ctrl Pts',(69.079679653846,-11.3136138754165,0.));
#53519=CARTESIAN_POINT('Ctrl Pts',(69.079679653846,-11.3136138754165,12.));
#53520=CARTESIAN_POINT('Ctrl Pts',(69.0835449954396,-11.3132375200165,0.));
#53521=CARTESIAN_POINT('Ctrl Pts',(69.0835449954396,-11.3132375200165,12.));
#53522=CARTESIAN_POINT('Ctrl Pts',(69.0912808656811,-11.3124821678798,0.));
#53523=CARTESIAN_POINT('Ctrl Pts',(69.0912808656811,-11.3124821678798,12.));
#53524=CARTESIAN_POINT('Ctrl Pts',(69.1029002322118,-11.3113412156661,0.));
#53525=CARTESIAN_POINT('Ctrl Pts',(69.1029002322118,-11.3113412156661,12.));
#53526=CARTESIAN_POINT('Ctrl Pts',(69.118423844466,-11.3098040973713,0.));
#53527=CARTESIAN_POINT('Ctrl Pts',(69.118423844466,-11.3098040973713,12.));
#53528=CARTESIAN_POINT('Ctrl Pts',(69.1378802251711,-11.3078562764384,0.));
#53529=CARTESIAN_POINT('Ctrl Pts',(69.1378802251711,-11.3078562764384,12.));
#53530=CARTESIAN_POINT('Ctrl Pts',(69.1573884361,-11.3058820128307,0.));
#53531=CARTESIAN_POINT('Ctrl Pts',(69.1573884361,-11.3058820128307,12.));
#53532=CARTESIAN_POINT('Ctrl Pts',(69.1769483991721,-11.3038812726292,0.));
#53533=CARTESIAN_POINT('Ctrl Pts',(69.1769483991721,-11.3038812726292,12.));
#53534=CARTESIAN_POINT('Ctrl Pts',(69.1965599718914,-11.3018540025638,0.));
#53535=CARTESIAN_POINT('Ctrl Pts',(69.1965599718914,-11.3018540025638,12.));
#53536=CARTESIAN_POINT('Ctrl Pts',(69.2162229488531,-11.2998001310964,0.));
#53537=CARTESIAN_POINT('Ctrl Pts',(69.2162229488531,-11.2998001310964,12.));
#53538=CARTESIAN_POINT('Ctrl Pts',(69.2359370894907,-11.2977195764852,0.));
#53539=CARTESIAN_POINT('Ctrl Pts',(69.2359370894907,-11.2977195764852,12.));
#53540=CARTESIAN_POINT('Ctrl Pts',(69.255702139335,-11.2956122531375,0.));
#53541=CARTESIAN_POINT('Ctrl Pts',(69.255702139335,-11.2956122531375,12.));
#53542=CARTESIAN_POINT('Ctrl Pts',(69.275517853148,-11.2934780784351,0.));
#53543=CARTESIAN_POINT('Ctrl Pts',(69.275517853148,-11.2934780784351,12.));
#53544=CARTESIAN_POINT('Ctrl Pts',(69.295384019272,-11.2913169799628,0.));
#53545=CARTESIAN_POINT('Ctrl Pts',(69.295384019272,-11.2913169799628,12.));
#53546=CARTESIAN_POINT('Ctrl Pts',(69.3153004517783,-11.2891288931517,0.));
#53547=CARTESIAN_POINT('Ctrl Pts',(69.3153004517783,-11.2891288931517,12.));
#53548=CARTESIAN_POINT('Ctrl Pts',(69.3352669789587,-11.2869137578459,0.));
#53549=CARTESIAN_POINT('Ctrl Pts',(69.3352669789587,-11.2869137578459,12.));
#53550=CARTESIAN_POINT('Ctrl Pts',(69.3552834337784,-11.2846715154524,0.));
#53551=CARTESIAN_POINT('Ctrl Pts',(69.3552834337784,-11.2846715154524,12.));
#53552=CARTESIAN_POINT('Ctrl Pts',(69.3753496420039,-11.2824021054045,0.));
#53553=CARTESIAN_POINT('Ctrl Pts',(69.3753496420039,-11.2824021054045,12.));
#53554=CARTESIAN_POINT('Ctrl Pts',(69.3954654162281,-11.2801054633816,0.));
#53555=CARTESIAN_POINT('Ctrl Pts',(69.3954654162281,-11.2801054633816,12.));
#53556=CARTESIAN_POINT('Ctrl Pts',(69.4156305620593,-11.2777815231469,0.));
#53557=CARTESIAN_POINT('Ctrl Pts',(69.4156305620593,-11.2777815231469,12.));
#53558=CARTESIAN_POINT('Ctrl Pts',(69.4358448819967,-11.2754302177021,0.));
#53559=CARTESIAN_POINT('Ctrl Pts',(69.4358448819967,-11.2754302177021,12.));
#53560=CARTESIAN_POINT('Ctrl Pts',(69.456108179879,-11.2730514806139,0.));
#53561=CARTESIAN_POINT('Ctrl Pts',(69.456108179879,-11.2730514806139,12.));
#53562=CARTESIAN_POINT('Ctrl Pts',(69.4764202659397,-11.270645247528,0.));
#53563=CARTESIAN_POINT('Ctrl Pts',(69.4764202659397,-11.270645247528,12.));
#53564=CARTESIAN_POINT('Ctrl Pts',(69.4967809565929,-11.2682114561008,0.));
#53565=CARTESIAN_POINT('Ctrl Pts',(69.4967809565929,-11.2682114561008,12.));
#53566=CARTESIAN_POINT('Ctrl Pts',(69.5171900720158,-11.2657500452716,0.));
#53567=CARTESIAN_POINT('Ctrl Pts',(69.5171900720158,-11.2657500452716,12.));
#53568=CARTESIAN_POINT('Ctrl Pts',(69.5376474344771,-11.263260954763,0.));
#53569=CARTESIAN_POINT('Ctrl Pts',(69.5376474344771,-11.263260954763,12.));
#53570=CARTESIAN_POINT('Ctrl Pts',(69.5581528662877,-11.2607441244703,0.));
#53571=CARTESIAN_POINT('Ctrl Pts',(69.5581528662877,-11.2607441244703,12.));
#53572=CARTESIAN_POINT('Ctrl Pts',(69.5787061880857,-11.2581994939541,0.));
#53573=CARTESIAN_POINT('Ctrl Pts',(69.5787061880857,-11.2581994939541,12.));
#53574=CARTESIAN_POINT('Ctrl Pts',(69.599307219739,-11.2556270027016,0.));
#53575=CARTESIAN_POINT('Ctrl Pts',(69.599307219739,-11.2556270027016,12.));
#53576=CARTESIAN_POINT('Ctrl Pts',(69.6199557811245,-11.2530265903557,0.));
#53577=CARTESIAN_POINT('Ctrl Pts',(69.6199557811245,-11.2530265903557,12.));
#53578=CARTESIAN_POINT('Ctrl Pts',(69.6406516928891,-11.2503981969412,0.));
#53579=CARTESIAN_POINT('Ctrl Pts',(69.6406516928891,-11.2503981969412,12.));
#53580=CARTESIAN_POINT('Ctrl Pts',(69.6613947773534,-11.2477417631386,0.));
#53581=CARTESIAN_POINT('Ctrl Pts',(69.6613947773534,-11.2477417631386,12.));
#53582=CARTESIAN_POINT('Ctrl Pts',(69.6821848588457,-11.2450572303841,0.));
#53583=CARTESIAN_POINT('Ctrl Pts',(69.6821848588457,-11.2450572303841,12.));
#53584=CARTESIAN_POINT('Ctrl Pts',(69.7030217632164,-11.2423445407166,0.));
#53585=CARTESIAN_POINT('Ctrl Pts',(69.7030217632164,-11.2423445407166,12.));
#53586=CARTESIAN_POINT('Ctrl Pts',(69.7239053175356,-11.239603636686,0.));
#53587=CARTESIAN_POINT('Ctrl Pts',(69.7239053175356,-11.239603636686,12.));
#53588=CARTESIAN_POINT('Ctrl Pts',(69.7448353497408,-11.2368344612472,0.));
#53589=CARTESIAN_POINT('Ctrl Pts',(69.7448353497408,-11.2368344612472,12.));
#53590=CARTESIAN_POINT('Ctrl Pts',(69.7658116882324,-11.2340369576456,0.));
#53591=CARTESIAN_POINT('Ctrl Pts',(69.7658116882324,-11.2340369576456,12.));
#53592=CARTESIAN_POINT('Ctrl Pts',(69.7868341618954,-11.2312110694187,0.));
#53593=CARTESIAN_POINT('Ctrl Pts',(69.7868341618954,-11.2312110694187,12.));
#53594=CARTESIAN_POINT('Ctrl Pts',(69.8079026002768,-11.2283567404437,0.));
#53595=CARTESIAN_POINT('Ctrl Pts',(69.8079026002768,-11.2283567404437,12.));
#53596=CARTESIAN_POINT('Ctrl Pts',(69.8290168337076,-11.225473914972,0.));
#53597=CARTESIAN_POINT('Ctrl Pts',(69.8290168337076,-11.225473914972,12.));
#53598=CARTESIAN_POINT('Ctrl Pts',(69.8501766934428,-11.2225625376736,0.));
#53599=CARTESIAN_POINT('Ctrl Pts',(69.8501766934428,-11.2225625376736,12.));
#53600=CARTESIAN_POINT('Ctrl Pts',(69.871382011789,-11.219622553679,0.));
#53601=CARTESIAN_POINT('Ctrl Pts',(69.871382011789,-11.219622553679,12.));
#53602=CARTESIAN_POINT('Ctrl Pts',(69.8926326220385,-11.2166539085523,0.));
#53603=CARTESIAN_POINT('Ctrl Pts',(69.8926326220385,-11.2166539085523,12.));
#53604=CARTESIAN_POINT('Ctrl Pts',(69.9139283584022,-11.2136565482678,0.));
#53605=CARTESIAN_POINT('Ctrl Pts',(69.9139283584022,-11.2136565482678,12.));
#53606=CARTESIAN_POINT('Ctrl Pts',(69.9352690559405,-11.2106304191882,0.));
#53607=CARTESIAN_POINT('Ctrl Pts',(69.9352690559405,-11.2106304191882,12.));
#53608=CARTESIAN_POINT('Ctrl Pts',(69.9566545504837,-11.2075754680449,0.));
#53609=CARTESIAN_POINT('Ctrl Pts',(69.9566545504837,-11.2075754680449,12.));
#53610=CARTESIAN_POINT('Ctrl Pts',(69.97808467858,-11.2044916419244,0.));
#53611=CARTESIAN_POINT('Ctrl Pts',(69.97808467858,-11.2044916419244,12.));
#53612=CARTESIAN_POINT('Ctrl Pts',(69.9995592775343,-11.2013788882714,0.));
#53613=CARTESIAN_POINT('Ctrl Pts',(69.9995592775343,-11.2013788882714,12.));
#53614=CARTESIAN_POINT('Ctrl Pts',(70.0210781854243,-11.1982371548919,0.));
#53615=CARTESIAN_POINT('Ctrl Pts',(70.0210781854243,-11.1982371548919,12.));
#53616=CARTESIAN_POINT('Ctrl Pts',(70.0426412411185,-11.1950663899576,0.));
#53617=CARTESIAN_POINT('Ctrl Pts',(70.0426412411185,-11.1950663899576,12.));
#53618=CARTESIAN_POINT('Ctrl Pts',(70.0642482842928,-11.1918665420166,0.));
#53619=CARTESIAN_POINT('Ctrl Pts',(70.0642482842928,-11.1918665420166,12.));
#53620=CARTESIAN_POINT('Ctrl Pts',(70.0858991554283,-11.1886375599914,0.));
#53621=CARTESIAN_POINT('Ctrl Pts',(70.0858991554283,-11.1886375599914,12.));
#53622=CARTESIAN_POINT('Ctrl Pts',(70.1075936957968,-11.185379393167,0.));
#53623=CARTESIAN_POINT('Ctrl Pts',(70.1075936957968,-11.185379393167,12.));
#53624=CARTESIAN_POINT('Ctrl Pts',(70.1293317474432,-11.1820919911846,0.));
#53625=CARTESIAN_POINT('Ctrl Pts',(70.1293317474432,-11.1820919911846,12.));
#53626=CARTESIAN_POINT('Ctrl Pts',(70.1511131531674,-11.1787753040363,0.));
#53627=CARTESIAN_POINT('Ctrl Pts',(70.1511131531674,-11.1787753040363,12.));
#53628=CARTESIAN_POINT('Ctrl Pts',(70.1729377564956,-11.1754292820631,0.));
#53629=CARTESIAN_POINT('Ctrl Pts',(70.1729377564956,-11.1754292820631,12.));
#53630=CARTESIAN_POINT('Ctrl Pts',(70.1948054016817,-11.1720538759499,0.));
#53631=CARTESIAN_POINT('Ctrl Pts',(70.1948054016817,-11.1720538759499,12.));
#53632=CARTESIAN_POINT('Ctrl Pts',(70.2167159337095,-11.168649036721,0.));
#53633=CARTESIAN_POINT('Ctrl Pts',(70.2167159337095,-11.168649036721,12.));
#53634=CARTESIAN_POINT('Ctrl Pts',(70.2386691982902,-11.1652147157383,0.));
#53635=CARTESIAN_POINT('Ctrl Pts',(70.2386691982902,-11.1652147157383,12.));
#53636=CARTESIAN_POINT('Ctrl Pts',(70.2606650418589,-11.1617508647017,0.));
#53637=CARTESIAN_POINT('Ctrl Pts',(70.2606650418589,-11.1617508647017,12.));
#53638=CARTESIAN_POINT('Ctrl Pts',(70.2827033115662,-11.1582574356522,0.));
#53639=CARTESIAN_POINT('Ctrl Pts',(70.2827033115662,-11.1582574356522,12.));
#53640=CARTESIAN_POINT('Ctrl Pts',(70.3047838552758,-11.1547343809647,0.));
#53641=CARTESIAN_POINT('Ctrl Pts',(70.3047838552758,-11.1547343809647,12.));
#53642=CARTESIAN_POINT('Ctrl Pts',(70.3269065215591,-11.1511816533422,0.));
#53643=CARTESIAN_POINT('Ctrl Pts',(70.3269065215591,-11.1511816533422,12.));
#53644=CARTESIAN_POINT('Ctrl Pts',(70.3490711596882,-11.1475992058124,0.));
#53645=CARTESIAN_POINT('Ctrl Pts',(70.3490711596882,-11.1475992058124,12.));
#53646=CARTESIAN_POINT('Ctrl Pts',(70.3712776196216,-11.1439869917269,0.));
#53647=CARTESIAN_POINT('Ctrl Pts',(70.3712776196216,-11.1439869917269,12.));
#53648=CARTESIAN_POINT('Ctrl Pts',(70.3935257519945,-11.1403449647622,0.));
#53649=CARTESIAN_POINT('Ctrl Pts',(70.3935257519945,-11.1403449647622,12.));
#53650=CARTESIAN_POINT('Ctrl Pts',(70.415815408119,-11.1366730789122,0.));
#53651=CARTESIAN_POINT('Ctrl Pts',(70.415815408119,-11.1366730789122,12.));
#53652=CARTESIAN_POINT('Ctrl Pts',(70.438146439981,-11.1329712884845,0.));
#53653=CARTESIAN_POINT('Ctrl Pts',(70.438146439981,-11.1329712884845,12.));
#53654=CARTESIAN_POINT('Ctrl Pts',(70.4605187002356,-11.1292395480975,0.));
#53655=CARTESIAN_POINT('Ctrl Pts',(70.4605187002356,-11.1292395480975,12.));
#53656=CARTESIAN_POINT('Ctrl Pts',(70.4829320421973,-11.1254778126824,0.));
#53657=CARTESIAN_POINT('Ctrl Pts',(70.4829320421973,-11.1254778126824,12.));
#53658=CARTESIAN_POINT('Ctrl Pts',(70.5053863198306,-11.121686037483,0.));
#53659=CARTESIAN_POINT('Ctrl Pts',(70.5053863198306,-11.121686037483,12.));
#53660=CARTESIAN_POINT('Ctrl Pts',(70.5278813877519,-11.117864178048,0.));
#53661=CARTESIAN_POINT('Ctrl Pts',(70.5278813877519,-11.117864178048,12.));
#53662=CARTESIAN_POINT('Ctrl Pts',(70.5504171012247,-11.1140121902274,0.));
#53663=CARTESIAN_POINT('Ctrl Pts',(70.5504171012247,-11.1140121902274,12.));
#53664=CARTESIAN_POINT('Ctrl Pts',(70.5729933161538,-11.11013003017,0.));
#53665=CARTESIAN_POINT('Ctrl Pts',(70.5729933161538,-11.11013003017,12.));
#53666=CARTESIAN_POINT('Ctrl Pts',(70.5956098890744,-11.1062176543257,0.));
#53667=CARTESIAN_POINT('Ctrl Pts',(70.5956098890744,-11.1062176543257,12.));
#53668=CARTESIAN_POINT('Ctrl Pts',(70.6182666771441,-11.1022750194439,0.));
#53669=CARTESIAN_POINT('Ctrl Pts',(70.6182666771441,-11.1022750194439,12.));
#53670=CARTESIAN_POINT('Ctrl Pts',(70.6409635381446,-11.0983020825662,0.));
#53671=CARTESIAN_POINT('Ctrl Pts',(70.6409635381446,-11.0983020825662,12.));
#53672=CARTESIAN_POINT('Ctrl Pts',(70.6637003304768,-11.0942988010231,0.));
#53673=CARTESIAN_POINT('Ctrl Pts',(70.6637003304768,-11.0942988010231,12.));
#53674=CARTESIAN_POINT('Ctrl Pts',(70.686476913156,-11.0902651324325,0.));
#53675=CARTESIAN_POINT('Ctrl Pts',(70.686476913156,-11.0902651324325,12.));
#53676=CARTESIAN_POINT('Ctrl Pts',(70.7092931457996,-11.0862010347022,0.));
#53677=CARTESIAN_POINT('Ctrl Pts',(70.7092931457996,-11.0862010347022,12.));
#53678=CARTESIAN_POINT('Ctrl Pts',(70.7321488886229,-11.0821064660276,0.));
#53679=CARTESIAN_POINT('Ctrl Pts',(70.7321488886229,-11.0821064660276,12.));
#53680=CARTESIAN_POINT('Ctrl Pts',(70.7550440024422,-11.0779813848851,0.));
#53681=CARTESIAN_POINT('Ctrl Pts',(70.7550440024422,-11.0779813848851,12.));
#53682=CARTESIAN_POINT('Ctrl Pts',(70.7779783486689,-11.0738257500292,0.));
#53683=CARTESIAN_POINT('Ctrl Pts',(70.7779783486689,-11.0738257500292,12.));
#53684=CARTESIAN_POINT('Ctrl Pts',(70.8009517893042,-11.0696395204908,0.));
#53685=CARTESIAN_POINT('Ctrl Pts',(70.8009517893042,-11.0696395204908,12.));
#53686=CARTESIAN_POINT('Ctrl Pts',(70.8239641869266,-11.0654226555798,0.));
#53687=CARTESIAN_POINT('Ctrl Pts',(70.8239641869266,-11.0654226555798,12.));
#53688=CARTESIAN_POINT('Ctrl Pts',(70.847015404688,-11.061175114883,0.));
#53689=CARTESIAN_POINT('Ctrl Pts',(70.847015404688,-11.061175114883,12.));
#53690=CARTESIAN_POINT('Ctrl Pts',(70.8701053063158,-11.0568968582566,0.));
#53691=CARTESIAN_POINT('Ctrl Pts',(70.8701053063158,-11.0568968582566,12.));
#53692=CARTESIAN_POINT('Ctrl Pts',(70.8932337561078,-11.0525878458242,0.));
#53693=CARTESIAN_POINT('Ctrl Pts',(70.8932337561078,-11.0525878458242,12.));
#53694=CARTESIAN_POINT('Ctrl Pts',(70.9164006189283,-11.0482480379752,0.));
#53695=CARTESIAN_POINT('Ctrl Pts',(70.9164006189283,-11.0482480379752,12.));
#53696=CARTESIAN_POINT('Ctrl Pts',(70.9396057601953,-11.0438773953686,0.));
#53697=CARTESIAN_POINT('Ctrl Pts',(70.9396057601953,-11.0438773953686,12.));
#53698=CARTESIAN_POINT('Ctrl Pts',(70.9628490458779,-11.039475878929,0.));
#53699=CARTESIAN_POINT('Ctrl Pts',(70.9628490458779,-11.039475878929,12.));
#53700=CARTESIAN_POINT('Ctrl Pts',(70.9861303424989,-11.0350434498408,0.));
#53701=CARTESIAN_POINT('Ctrl Pts',(70.9861303424989,-11.0350434498408,12.));
#53702=CARTESIAN_POINT('Ctrl Pts',(71.0094495171295,-11.0305800695457,0.));
#53703=CARTESIAN_POINT('Ctrl Pts',(71.0094495171295,-11.0305800695457,12.));
#53704=CARTESIAN_POINT('Ctrl Pts',(71.0328064373849,-11.0260856997414,0.));
#53705=CARTESIAN_POINT('Ctrl Pts',(71.0328064373849,-11.0260856997414,12.));
#53706=CARTESIAN_POINT('Ctrl Pts',(71.0562009714125,-11.0215603023854,0.));
#53707=CARTESIAN_POINT('Ctrl Pts',(71.0562009714125,-11.0215603023854,12.));
#53708=CARTESIAN_POINT('Ctrl Pts',(71.0796329878896,-11.0170038396913,0.));
#53709=CARTESIAN_POINT('Ctrl Pts',(71.0796329878896,-11.0170038396913,12.));
#53710=CARTESIAN_POINT('Ctrl Pts',(71.1031023560243,-11.0124162741223,0.));
#53711=CARTESIAN_POINT('Ctrl Pts',(71.1031023560243,-11.0124162741223,12.));
#53712=CARTESIAN_POINT('Ctrl Pts',(71.1266089455517,-11.0077975683895,0.));
#53713=CARTESIAN_POINT('Ctrl Pts',(71.1266089455517,-11.0077975683895,12.));
#53714=CARTESIAN_POINT('Ctrl Pts',(71.1501526267288,-11.0031476854503,0.));
#53715=CARTESIAN_POINT('Ctrl Pts',(71.1501526267288,-11.0031476854503,12.));
#53716=CARTESIAN_POINT('Ctrl Pts',(71.1737332703248,-10.9984665885127,0.));
#53717=CARTESIAN_POINT('Ctrl Pts',(71.1737332703248,-10.9984665885127,12.));
#53718=CARTESIAN_POINT('Ctrl Pts',(71.1973507476188,-10.993754241032,0.));
#53719=CARTESIAN_POINT('Ctrl Pts',(71.1973507476188,-10.993754241032,12.));
#53720=CARTESIAN_POINT('Ctrl Pts',(71.221004930401,-10.9890106067038,0.));
#53721=CARTESIAN_POINT('Ctrl Pts',(71.221004930401,-10.9890106067038,12.));
#53722=CARTESIAN_POINT('Ctrl Pts',(71.2446956909685,-10.9842356494627,0.));
#53723=CARTESIAN_POINT('Ctrl Pts',(71.2446956909685,-10.9842356494627,12.));
#53724=CARTESIAN_POINT('Ctrl Pts',(71.2684229021209,-10.9794293334806,0.));
#53725=CARTESIAN_POINT('Ctrl Pts',(71.2684229021209,-10.9794293334806,12.));
#53726=CARTESIAN_POINT('Ctrl Pts',(71.2921864371499,-10.9745916231711,0.));
#53727=CARTESIAN_POINT('Ctrl Pts',(71.2921864371499,-10.9745916231711,12.));
#53728=CARTESIAN_POINT('Ctrl Pts',(71.3159861698368,-10.9697224831862,0.));
#53729=CARTESIAN_POINT('Ctrl Pts',(71.3159861698368,-10.9697224831862,12.));
#53730=CARTESIAN_POINT('Ctrl Pts',(71.3398219744547,-10.96482187841,0.));
#53731=CARTESIAN_POINT('Ctrl Pts',(71.3398219744547,-10.96482187841,12.));
#53732=CARTESIAN_POINT('Ctrl Pts',(71.3636937257651,-10.9598897739565,0.));
#53733=CARTESIAN_POINT('Ctrl Pts',(71.3636937257651,-10.9598897739565,12.));
#53734=CARTESIAN_POINT('Ctrl Pts',(71.3876012990135,-10.954926135169,0.));
#53735=CARTESIAN_POINT('Ctrl Pts',(71.3876012990135,-10.954926135169,12.));
#53736=CARTESIAN_POINT('Ctrl Pts',(71.411544569919,-10.9499309276235,0.));
#53737=CARTESIAN_POINT('Ctrl Pts',(71.411544569919,-10.9499309276235,12.));
#53738=CARTESIAN_POINT('Ctrl Pts',(71.4355234146718,-10.9449041171269,0.));
#53739=CARTESIAN_POINT('Ctrl Pts',(71.4355234146718,-10.9449041171269,12.));
#53740=CARTESIAN_POINT('Ctrl Pts',(71.4595377099352,-10.9398456697095,0.));
#53741=CARTESIAN_POINT('Ctrl Pts',(71.4595377099352,-10.9398456697095,12.));
#53742=CARTESIAN_POINT('Ctrl Pts',(71.4835873328425,-10.9347555516236,0.));
#53743=CARTESIAN_POINT('Ctrl Pts',(71.4835873328425,-10.9347555516236,12.));
#53744=CARTESIAN_POINT('Ctrl Pts',(71.5076721609936,-10.9296337293425,0.));
#53745=CARTESIAN_POINT('Ctrl Pts',(71.5076721609936,-10.9296337293425,12.));
#53746=CARTESIAN_POINT('Ctrl Pts',(71.5317920724453,-10.9244801695642,0.));
#53747=CARTESIAN_POINT('Ctrl Pts',(71.5317920724453,-10.9244801695642,12.));
#53748=CARTESIAN_POINT('Ctrl Pts',(71.5559469457082,-10.9192948392099,0.));
#53749=CARTESIAN_POINT('Ctrl Pts',(71.5559469457082,-10.9192948392099,12.));
#53750=CARTESIAN_POINT('Ctrl Pts',(71.5801366597479,-10.9140777054169,0.));
#53751=CARTESIAN_POINT('Ctrl Pts',(71.5801366597479,-10.9140777054169,12.));
#53752=CARTESIAN_POINT('Ctrl Pts',(71.604361093983,-10.9088287355364,0.));
#53753=CARTESIAN_POINT('Ctrl Pts',(71.604361093983,-10.9088287355364,12.));
#53754=CARTESIAN_POINT('Ctrl Pts',(71.6286201282815,-10.9035478971329,0.));
#53755=CARTESIAN_POINT('Ctrl Pts',(71.6286201282815,-10.9035478971329,12.));
#53756=CARTESIAN_POINT('Ctrl Pts',(71.6529136429515,-10.8982351579872,0.));
#53757=CARTESIAN_POINT('Ctrl Pts',(71.6529136429515,-10.8982351579872,12.));
#53758=CARTESIAN_POINT('Ctrl Pts',(71.6772415187382,-10.8928904860967,0.));
#53759=CARTESIAN_POINT('Ctrl Pts',(71.6772415187382,-10.8928904860967,12.));
#53760=CARTESIAN_POINT('Ctrl Pts',(71.7016036368254,-10.8875138496674,0.));
#53761=CARTESIAN_POINT('Ctrl Pts',(71.7016036368254,-10.8875138496674,12.));
#53762=CARTESIAN_POINT('Ctrl Pts',(71.7259998788337,-10.8821052171122,0.));
#53763=CARTESIAN_POINT('Ctrl Pts',(71.7259998788337,-10.8821052171122,12.));
#53764=CARTESIAN_POINT('Ctrl Pts',(71.7504301268177,-10.8766645570496,0.));
#53765=CARTESIAN_POINT('Ctrl Pts',(71.7504301268177,-10.8766645570496,12.));
#53766=CARTESIAN_POINT('Ctrl Pts',(71.7748942632578,-10.8711918383071,0.));
#53767=CARTESIAN_POINT('Ctrl Pts',(71.7748942632578,-10.8711918383071,12.));
#53768=CARTESIAN_POINT('Ctrl Pts',(71.7993921710546,-10.8656870299218,0.));
#53769=CARTESIAN_POINT('Ctrl Pts',(71.7993921710546,-10.8656870299218,12.));
#53770=CARTESIAN_POINT('Ctrl Pts',(71.8239237335318,-10.860150101133,0.));
#53771=CARTESIAN_POINT('Ctrl Pts',(71.8239237335318,-10.860150101133,12.));
#53772=CARTESIAN_POINT('Ctrl Pts',(71.8484888344335,-10.8545810213799,0.));
#53773=CARTESIAN_POINT('Ctrl Pts',(71.8484888344335,-10.8545810213799,12.));
#53774=CARTESIAN_POINT('Ctrl Pts',(71.8730873579226,-10.8489797602998,0.));
#53775=CARTESIAN_POINT('Ctrl Pts',(71.8730873579226,-10.8489797602998,12.));
#53776=CARTESIAN_POINT('Ctrl Pts',(71.8977191885726,-10.8433462877312,0.));
#53777=CARTESIAN_POINT('Ctrl Pts',(71.8977191885726,-10.8433462877312,12.));
#53778=CARTESIAN_POINT('Ctrl Pts',(71.9223842113622,-10.8376805737158,0.));
#53779=CARTESIAN_POINT('Ctrl Pts',(71.9223842113622,-10.8376805737158,12.));
#53780=CARTESIAN_POINT('Ctrl Pts',(71.9470823116777,-10.8319825884917,0.));
#53781=CARTESIAN_POINT('Ctrl Pts',(71.9470823116777,-10.8319825884917,12.));
#53782=CARTESIAN_POINT('Ctrl Pts',(71.971813375312,-10.8262523024897,0.));
#53783=CARTESIAN_POINT('Ctrl Pts',(71.971813375312,-10.8262523024897,12.));
#53784=CARTESIAN_POINT('Ctrl Pts',(71.996577288462,-10.8204896863328,0.));
#53785=CARTESIAN_POINT('Ctrl Pts',(71.996577288462,-10.8204896863328,12.));
#53786=CARTESIAN_POINT('Ctrl Pts',(72.0213739377231,-10.8146947108376,0.));
#53787=CARTESIAN_POINT('Ctrl Pts',(72.0213739377231,-10.8146947108376,12.));
#53788=CARTESIAN_POINT('Ctrl Pts',(72.0462032100828,-10.8088673470187,0.));
#53789=CARTESIAN_POINT('Ctrl Pts',(72.0462032100828,-10.8088673470187,12.));
#53790=CARTESIAN_POINT('Ctrl Pts',(72.0710649929214,-10.8030075660811,0.));
#53791=CARTESIAN_POINT('Ctrl Pts',(72.0710649929214,-10.8030075660811,12.));
#53792=CARTESIAN_POINT('Ctrl Pts',(72.095959174012,-10.7971153394168,0.));
#53793=CARTESIAN_POINT('Ctrl Pts',(72.095959174012,-10.7971153394168,12.));
#53794=CARTESIAN_POINT('Ctrl Pts',(72.1208856415171,-10.7911906386027,0.));
#53795=CARTESIAN_POINT('Ctrl Pts',(72.1208856415171,-10.7911906386027,12.));
#53796=CARTESIAN_POINT('Ctrl Pts',(72.145844283983,-10.7852334354015,0.));
#53797=CARTESIAN_POINT('Ctrl Pts',(72.145844283983,-10.7852334354015,12.));
#53798=CARTESIAN_POINT('Ctrl Pts',(72.17083499033,-10.779243701766,0.));
#53799=CARTESIAN_POINT('Ctrl Pts',(72.17083499033,-10.779243701766,12.));
#53800=CARTESIAN_POINT('Ctrl Pts',(72.1958576498556,-10.7732214098343,0.));
#53801=CARTESIAN_POINT('Ctrl Pts',(72.1958576498556,-10.7732214098343,12.));
#53802=CARTESIAN_POINT('Ctrl Pts',(72.2209121522367,-10.7671665319254,0.));
#53803=CARTESIAN_POINT('Ctrl Pts',(72.2209121522367,-10.7671665319254,12.));
#53804=CARTESIAN_POINT('Ctrl Pts',(72.2459983875298,-10.7610790405385,0.));
#53805=CARTESIAN_POINT('Ctrl Pts',(72.2459983875298,-10.7610790405385,12.));
#53806=CARTESIAN_POINT('Ctrl Pts',(72.2711162461679,-10.7549589083535,0.));
#53807=CARTESIAN_POINT('Ctrl Pts',(72.2711162461679,-10.7549589083535,12.));
#53808=CARTESIAN_POINT('Ctrl Pts',(72.296265618955,-10.7488061082368,0.));
#53809=CARTESIAN_POINT('Ctrl Pts',(72.296265618955,-10.7488061082368,12.));
#53810=CARTESIAN_POINT('Ctrl Pts',(72.3214463970634,-10.7426206132375,0.));
#53811=CARTESIAN_POINT('Ctrl Pts',(72.3214463970634,-10.7426206132375,12.));
#53812=CARTESIAN_POINT('Ctrl Pts',(72.3466584720311,-10.73640239658,0.));
#53813=CARTESIAN_POINT('Ctrl Pts',(72.3466584720311,-10.73640239658,12.));
#53814=CARTESIAN_POINT('Ctrl Pts',(72.3719017357568,-10.7301514316607,0.));
#53815=CARTESIAN_POINT('Ctrl Pts',(72.3719017357568,-10.7301514316607,12.));
#53816=CARTESIAN_POINT('Ctrl Pts',(72.3971760804935,-10.7238676920469,0.));
#53817=CARTESIAN_POINT('Ctrl Pts',(72.3971760804935,-10.7238676920469,12.));
#53818=CARTESIAN_POINT('Ctrl Pts',(72.4224813988355,-10.7175511514789,0.));
#53819=CARTESIAN_POINT('Ctrl Pts',(72.4224813988355,-10.7175511514789,12.));
#53820=CARTESIAN_POINT('Ctrl Pts',(72.4478175837168,-10.7112017838707,0.));
#53821=CARTESIAN_POINT('Ctrl Pts',(72.4478175837168,-10.7112017838707,12.));
#53822=CARTESIAN_POINT('Ctrl Pts',(72.4731845284238,-10.7048195633062,0.));
#53823=CARTESIAN_POINT('Ctrl Pts',(72.4731845284238,-10.7048195633062,12.));
#53824=CARTESIAN_POINT('Ctrl Pts',(72.4985821266031,-10.6984044640399,0.));
#53825=CARTESIAN_POINT('Ctrl Pts',(72.4985821266031,-10.6984044640399,12.));
#53826=CARTESIAN_POINT('Ctrl Pts',(72.5240102722662,-10.691956460499,0.));
#53827=CARTESIAN_POINT('Ctrl Pts',(72.5240102722662,-10.691956460499,12.));
#53828=CARTESIAN_POINT('Ctrl Pts',(72.5494688597951,-10.6854755272903,0.));
#53829=CARTESIAN_POINT('Ctrl Pts',(72.5494688597951,-10.6854755272903,12.));
#53830=CARTESIAN_POINT('Ctrl Pts',(72.57495778394,-10.6789616392041,0.));
#53831=CARTESIAN_POINT('Ctrl Pts',(72.57495778394,-10.6789616392041,12.));
#53832=CARTESIAN_POINT('Ctrl Pts',(72.6004769398004,-10.6724147711994,0.));
#53833=CARTESIAN_POINT('Ctrl Pts',(72.6004769398004,-10.6724147711994,12.));
#53834=CARTESIAN_POINT('Ctrl Pts',(72.6260262228055,-10.6658348983944,0.));
#53835=CARTESIAN_POINT('Ctrl Pts',(72.6260262228055,-10.6658348983944,12.));
#53836=CARTESIAN_POINT('Ctrl Pts',(72.6516055286908,-10.659221996058,0.));
#53837=CARTESIAN_POINT('Ctrl Pts',(72.6516055286908,-10.659221996058,12.));
#53838=CARTESIAN_POINT('Ctrl Pts',(72.6772147534762,-10.6525760396055,0.));
#53839=CARTESIAN_POINT('Ctrl Pts',(72.6772147534762,-10.6525760396055,12.));
#53840=CARTESIAN_POINT('Ctrl Pts',(72.7028537934332,-10.6458970045948,0.));
#53841=CARTESIAN_POINT('Ctrl Pts',(72.7028537934332,-10.6458970045948,12.));
#53842=CARTESIAN_POINT('Ctrl Pts',(72.7285225451309,-10.6391848667354,0.));
#53843=CARTESIAN_POINT('Ctrl Pts',(72.7285225451309,-10.6391848667354,12.));
#53844=CARTESIAN_POINT('Ctrl Pts',(72.7542209054823,-10.6324396018999,0.));
#53845=CARTESIAN_POINT('Ctrl Pts',(72.7542209054823,-10.6324396018999,12.));
#53846=CARTESIAN_POINT('Ctrl Pts',(72.7799487717914,-10.6256611861395,0.));
#53847=CARTESIAN_POINT('Ctrl Pts',(72.7799487717914,-10.6256611861395,12.));
#53848=CARTESIAN_POINT('Ctrl Pts',(72.8057060417882,-10.6188495956973,0.));
#53849=CARTESIAN_POINT('Ctrl Pts',(72.8057060417882,-10.6188495956973,12.));
#53850=CARTESIAN_POINT('Ctrl Pts',(72.8314926136872,-10.6120048070366,0.));
#53851=CARTESIAN_POINT('Ctrl Pts',(72.8314926136872,-10.6120048070366,12.));
#53852=CARTESIAN_POINT('Ctrl Pts',(72.8573083861328,-10.6051267968202,0.));
#53853=CARTESIAN_POINT('Ctrl Pts',(72.8573083861328,-10.6051267968202,12.));
#53854=CARTESIAN_POINT('Ctrl Pts',(72.8831532580839,-10.5982155418625,0.));
#53855=CARTESIAN_POINT('Ctrl Pts',(72.8831532580839,-10.5982155418625,12.));
#53856=CARTESIAN_POINT('Ctrl Pts',(72.9090271287081,-10.5912710190928,0.));
#53857=CARTESIAN_POINT('Ctrl Pts',(72.9090271287081,-10.5912710190928,12.));
#53858=CARTESIAN_POINT('Ctrl Pts',(72.9349298972823,-10.5842932055209,0.));
#53859=CARTESIAN_POINT('Ctrl Pts',(72.9349298972823,-10.5842932055209,12.));
#53860=CARTESIAN_POINT('Ctrl Pts',(72.9608614630539,-10.5772820781959,0.));
#53861=CARTESIAN_POINT('Ctrl Pts',(72.9608614630539,-10.5772820781959,12.));
#53862=CARTESIAN_POINT('Ctrl Pts',(72.9868217252293,-10.5702376142052,0.));
#53863=CARTESIAN_POINT('Ctrl Pts',(72.9868217252293,-10.5702376142052,12.));
#53864=CARTESIAN_POINT('Ctrl Pts',(73.0128105832635,-10.5631597907653,0.));
#53865=CARTESIAN_POINT('Ctrl Pts',(73.0128105832635,-10.5631597907653,12.));
#53866=CARTESIAN_POINT('Ctrl Pts',(73.0388279370845,-10.5560485852975,0.));
#53867=CARTESIAN_POINT('Ctrl Pts',(73.0388279370845,-10.5560485852975,12.));
#53868=CARTESIAN_POINT('Ctrl Pts',(73.0648736873435,-10.5489039755138,0.));
#53869=CARTESIAN_POINT('Ctrl Pts',(73.0648736873435,-10.5489039755138,12.));
#53870=CARTESIAN_POINT('Ctrl Pts',(73.090947735646,-10.5417259395001,0.));
#53871=CARTESIAN_POINT('Ctrl Pts',(73.090947735646,-10.5417259395001,12.));
#53872=CARTESIAN_POINT('Ctrl Pts',(73.1170499848012,-10.5345144558097,0.));
#53873=CARTESIAN_POINT('Ctrl Pts',(73.1170499848012,-10.5345144558097,12.));
#53874=CARTESIAN_POINT('Ctrl Pts',(73.1431803382677,-10.5272695032649,0.));
#53875=CARTESIAN_POINT('Ctrl Pts',(73.1431803382677,-10.5272695032649,12.));
#53876=CARTESIAN_POINT('Ctrl Pts',(73.169338699611,-10.5199910607652,0.));
#53877=CARTESIAN_POINT('Ctrl Pts',(73.169338699611,-10.5199910607652,12.));
#53878=CARTESIAN_POINT('Ctrl Pts',(73.1955249719037,-10.5126791070804,0.));
#53879=CARTESIAN_POINT('Ctrl Pts',(73.1955249719037,-10.5126791070804,12.));
#53880=CARTESIAN_POINT('Ctrl Pts',(73.2217390572578,-10.505333620691,0.));
#53881=CARTESIAN_POINT('Ctrl Pts',(73.2217390572578,-10.505333620691,12.));
#53882=CARTESIAN_POINT('Ctrl Pts',(73.247980856023,-10.4979545795197,0.));
#53883=CARTESIAN_POINT('Ctrl Pts',(73.247980856023,-10.4979545795197,12.));
#53884=CARTESIAN_POINT('Ctrl Pts',(73.2742502674361,-10.4905419611529,0.));
#53885=CARTESIAN_POINT('Ctrl Pts',(73.2742502674361,-10.4905419611529,12.));
#53886=CARTESIAN_POINT('Ctrl Pts',(73.3005471910639,-10.4830957433311,0.));
#53887=CARTESIAN_POINT('Ctrl Pts',(73.3005471910639,-10.4830957433311,12.));
#53888=CARTESIAN_POINT('Ctrl Pts',(73.3268715280609,-10.475615904381,0.));
#53889=CARTESIAN_POINT('Ctrl Pts',(73.3268715280609,-10.475615904381,12.));
#53890=CARTESIAN_POINT('Ctrl Pts',(73.353223182365,-10.4681024236288,0.));
#53891=CARTESIAN_POINT('Ctrl Pts',(73.353223182365,-10.4681024236288,12.));
#53892=CARTESIAN_POINT('Ctrl Pts',(73.3796020622437,-10.460555281939,0.));
#53893=CARTESIAN_POINT('Ctrl Pts',(73.3796020622437,-10.460555281939,12.));
#53894=CARTESIAN_POINT('Ctrl Pts',(73.4060080806577,-10.4529744618438,0.));
#53895=CARTESIAN_POINT('Ctrl Pts',(73.4060080806577,-10.4529744618438,12.));
#53896=CARTESIAN_POINT('Ctrl Pts',(73.432441151843,-10.4453599463534,0.));
#53897=CARTESIAN_POINT('Ctrl Pts',(73.432441151843,-10.4453599463534,12.));
#53898=CARTESIAN_POINT('Ctrl Pts',(73.45890118861,-10.4377117180212,0.));
#53899=CARTESIAN_POINT('Ctrl Pts',(73.45890118861,-10.4377117180212,12.));
#53900=CARTESIAN_POINT('Ctrl Pts',(73.4853880992228,-10.4300297578648,0.));
#53901=CARTESIAN_POINT('Ctrl Pts',(73.4853880992228,-10.4300297578648,12.));
#53902=CARTESIAN_POINT('Ctrl Pts',(73.5119017847664,-10.4223140444615,0.));
#53903=CARTESIAN_POINT('Ctrl Pts',(73.5119017847664,-10.4223140444615,12.));
#53904=CARTESIAN_POINT('Ctrl Pts',(73.5384421354746,-10.4145645526832,0.));
#53905=CARTESIAN_POINT('Ctrl Pts',(73.5384421354746,-10.4145645526832,12.));
#53906=CARTESIAN_POINT('Ctrl Pts',(73.5650090360114,-10.4067812555539,0.));
#53907=CARTESIAN_POINT('Ctrl Pts',(73.5650090360114,-10.4067812555539,12.));
#53908=CARTESIAN_POINT('Ctrl Pts',(73.5916023719976,-10.3989641265313,0.));
#53909=CARTESIAN_POINT('Ctrl Pts',(73.5916023719976,-10.3989641265313,12.));
#53910=CARTESIAN_POINT('Ctrl Pts',(73.6182220363295,-10.3911131417478,0.));
#53911=CARTESIAN_POINT('Ctrl Pts',(73.6182220363295,-10.3911131417478,12.));
#53912=CARTESIAN_POINT('Ctrl Pts',(73.6448679350605,-10.3832282820361,0.));
#53913=CARTESIAN_POINT('Ctrl Pts',(73.6448679350605,-10.3832282820361,12.));
#53914=CARTESIAN_POINT('Ctrl Pts',(73.6715399947459,-10.3753095356302,0.));
#53915=CARTESIAN_POINT('Ctrl Pts',(73.6715399947459,-10.3753095356302,12.));
#53916=CARTESIAN_POINT('Ctrl Pts',(73.6982381644571,-10.3673568984515,0.));
#53917=CARTESIAN_POINT('Ctrl Pts',(73.6982381644571,-10.3673568984515,12.));
#53918=CARTESIAN_POINT('Ctrl Pts',(73.7249624108433,-10.3593703712542,0.));
#53919=CARTESIAN_POINT('Ctrl Pts',(73.7249624108433,-10.3593703712542,12.));
#53920=CARTESIAN_POINT('Ctrl Pts',(73.7463626541235,-10.3529540403026,0.));
#53921=CARTESIAN_POINT('Ctrl Pts',(73.7463626541235,-10.3529540403026,12.));
#53922=CARTESIAN_POINT('Ctrl Pts',(73.7624245587416,-10.3481265449303,0.));
#53923=CARTESIAN_POINT('Ctrl Pts',(73.7624245587416,-10.3481265449303,12.));
#53924=CARTESIAN_POINT('Ctrl Pts',(73.7731377047922,-10.3449014384439,0.));
#53925=CARTESIAN_POINT('Ctrl Pts',(73.7731377047922,-10.3449014384439,12.));
#53926=CARTESIAN_POINT('Ctrl Pts',(73.778495580227,-10.343287191141,0.));
#53927=CARTESIAN_POINT('Ctrl Pts',(73.778495580227,-10.343287191141,12.));
#53928=CARTESIAN_POINT('',(69.079679653846,-11.3136138754165,0.));
#53929=CARTESIAN_POINT('Ctrl Pts',(69.079679653846,-11.3136138754165,0.));
#53930=CARTESIAN_POINT('Ctrl Pts',(69.0835449954396,-11.3132375200165,0.));
#53931=CARTESIAN_POINT('Ctrl Pts',(69.0912808656811,-11.3124821678798,0.));
#53932=CARTESIAN_POINT('Ctrl Pts',(69.1029002322118,-11.3113412156661,0.));
#53933=CARTESIAN_POINT('Ctrl Pts',(69.118423844466,-11.3098040973713,0.));
#53934=CARTESIAN_POINT('Ctrl Pts',(69.1378802251711,-11.3078562764384,0.));
#53935=CARTESIAN_POINT('Ctrl Pts',(69.1573884361,-11.3058820128307,0.));
#53936=CARTESIAN_POINT('Ctrl Pts',(69.1769483991721,-11.3038812726292,0.));
#53937=CARTESIAN_POINT('Ctrl Pts',(69.1965599718914,-11.3018540025638,0.));
#53938=CARTESIAN_POINT('Ctrl Pts',(69.2162229488531,-11.2998001310964,0.));
#53939=CARTESIAN_POINT('Ctrl Pts',(69.2359370894907,-11.2977195764852,0.));
#53940=CARTESIAN_POINT('Ctrl Pts',(69.255702139335,-11.2956122531375,0.));
#53941=CARTESIAN_POINT('Ctrl Pts',(69.275517853148,-11.2934780784351,0.));
#53942=CARTESIAN_POINT('Ctrl Pts',(69.295384019272,-11.2913169799628,0.));
#53943=CARTESIAN_POINT('Ctrl Pts',(69.3153004517783,-11.2891288931517,0.));
#53944=CARTESIAN_POINT('Ctrl Pts',(69.3352669789587,-11.2869137578459,0.));
#53945=CARTESIAN_POINT('Ctrl Pts',(69.3552834337784,-11.2846715154524,0.));
#53946=CARTESIAN_POINT('Ctrl Pts',(69.3753496420039,-11.2824021054045,0.));
#53947=CARTESIAN_POINT('Ctrl Pts',(69.3954654162281,-11.2801054633816,0.));
#53948=CARTESIAN_POINT('Ctrl Pts',(69.4156305620593,-11.2777815231469,0.));
#53949=CARTESIAN_POINT('Ctrl Pts',(69.4358448819967,-11.2754302177021,0.));
#53950=CARTESIAN_POINT('Ctrl Pts',(69.456108179879,-11.2730514806139,0.));
#53951=CARTESIAN_POINT('Ctrl Pts',(69.4764202659397,-11.270645247528,0.));
#53952=CARTESIAN_POINT('Ctrl Pts',(69.4967809565929,-11.2682114561008,0.));
#53953=CARTESIAN_POINT('Ctrl Pts',(69.5171900720158,-11.2657500452716,0.));
#53954=CARTESIAN_POINT('Ctrl Pts',(69.5376474344771,-11.263260954763,0.));
#53955=CARTESIAN_POINT('Ctrl Pts',(69.5581528662877,-11.2607441244703,0.));
#53956=CARTESIAN_POINT('Ctrl Pts',(69.5787061880857,-11.2581994939541,0.));
#53957=CARTESIAN_POINT('Ctrl Pts',(69.599307219739,-11.2556270027016,0.));
#53958=CARTESIAN_POINT('Ctrl Pts',(69.6199557811245,-11.2530265903557,0.));
#53959=CARTESIAN_POINT('Ctrl Pts',(69.6406516928891,-11.2503981969412,0.));
#53960=CARTESIAN_POINT('Ctrl Pts',(69.6613947773534,-11.2477417631386,0.));
#53961=CARTESIAN_POINT('Ctrl Pts',(69.6821848588457,-11.2450572303841,0.));
#53962=CARTESIAN_POINT('Ctrl Pts',(69.7030217632164,-11.2423445407166,0.));
#53963=CARTESIAN_POINT('Ctrl Pts',(69.7239053175356,-11.239603636686,0.));
#53964=CARTESIAN_POINT('Ctrl Pts',(69.7448353497408,-11.2368344612472,0.));
#53965=CARTESIAN_POINT('Ctrl Pts',(69.7658116882324,-11.2340369576456,0.));
#53966=CARTESIAN_POINT('Ctrl Pts',(69.7868341618954,-11.2312110694187,0.));
#53967=CARTESIAN_POINT('Ctrl Pts',(69.8079026002768,-11.2283567404437,0.));
#53968=CARTESIAN_POINT('Ctrl Pts',(69.8290168337076,-11.225473914972,0.));
#53969=CARTESIAN_POINT('Ctrl Pts',(69.8501766934428,-11.2225625376736,0.));
#53970=CARTESIAN_POINT('Ctrl Pts',(69.871382011789,-11.219622553679,0.));
#53971=CARTESIAN_POINT('Ctrl Pts',(69.8926326220385,-11.2166539085523,0.));
#53972=CARTESIAN_POINT('Ctrl Pts',(69.9139283584022,-11.2136565482678,0.));
#53973=CARTESIAN_POINT('Ctrl Pts',(69.9352690559405,-11.2106304191882,0.));
#53974=CARTESIAN_POINT('Ctrl Pts',(69.9566545504837,-11.2075754680449,0.));
#53975=CARTESIAN_POINT('Ctrl Pts',(69.97808467858,-11.2044916419244,0.));
#53976=CARTESIAN_POINT('Ctrl Pts',(69.9995592775343,-11.2013788882714,0.));
#53977=CARTESIAN_POINT('Ctrl Pts',(70.0210781854243,-11.1982371548919,0.));
#53978=CARTESIAN_POINT('Ctrl Pts',(70.0426412411185,-11.1950663899576,0.));
#53979=CARTESIAN_POINT('Ctrl Pts',(70.0642482842928,-11.1918665420166,0.));
#53980=CARTESIAN_POINT('Ctrl Pts',(70.0858991554283,-11.1886375599914,0.));
#53981=CARTESIAN_POINT('Ctrl Pts',(70.1075936957968,-11.185379393167,0.));
#53982=CARTESIAN_POINT('Ctrl Pts',(70.1293317474432,-11.1820919911846,0.));
#53983=CARTESIAN_POINT('Ctrl Pts',(70.1511131531674,-11.1787753040363,0.));
#53984=CARTESIAN_POINT('Ctrl Pts',(70.1729377564956,-11.1754292820631,0.));
#53985=CARTESIAN_POINT('Ctrl Pts',(70.1948054016817,-11.1720538759499,0.));
#53986=CARTESIAN_POINT('Ctrl Pts',(70.2167159337095,-11.168649036721,0.));
#53987=CARTESIAN_POINT('Ctrl Pts',(70.2386691982902,-11.1652147157383,0.));
#53988=CARTESIAN_POINT('Ctrl Pts',(70.2606650418589,-11.1617508647017,0.));
#53989=CARTESIAN_POINT('Ctrl Pts',(70.2827033115662,-11.1582574356522,0.));
#53990=CARTESIAN_POINT('Ctrl Pts',(70.3047838552758,-11.1547343809647,0.));
#53991=CARTESIAN_POINT('Ctrl Pts',(70.3269065215591,-11.1511816533422,0.));
#53992=CARTESIAN_POINT('Ctrl Pts',(70.3490711596882,-11.1475992058124,0.));
#53993=CARTESIAN_POINT('Ctrl Pts',(70.3712776196216,-11.1439869917269,0.));
#53994=CARTESIAN_POINT('Ctrl Pts',(70.3935257519945,-11.1403449647622,0.));
#53995=CARTESIAN_POINT('Ctrl Pts',(70.415815408119,-11.1366730789122,0.));
#53996=CARTESIAN_POINT('Ctrl Pts',(70.438146439981,-11.1329712884845,0.));
#53997=CARTESIAN_POINT('Ctrl Pts',(70.4605187002356,-11.1292395480975,0.));
#53998=CARTESIAN_POINT('Ctrl Pts',(70.4829320421973,-11.1254778126824,0.));
#53999=CARTESIAN_POINT('Ctrl Pts',(70.5053863198306,-11.121686037483,0.));
#54000=CARTESIAN_POINT('Ctrl Pts',(70.5278813877519,-11.117864178048,0.));
#54001=CARTESIAN_POINT('Ctrl Pts',(70.5504171012247,-11.1140121902274,0.));
#54002=CARTESIAN_POINT('Ctrl Pts',(70.5729933161538,-11.11013003017,0.));
#54003=CARTESIAN_POINT('Ctrl Pts',(70.5956098890744,-11.1062176543257,0.));
#54004=CARTESIAN_POINT('Ctrl Pts',(70.6182666771441,-11.1022750194439,0.));
#54005=CARTESIAN_POINT('Ctrl Pts',(70.6409635381446,-11.0983020825662,0.));
#54006=CARTESIAN_POINT('Ctrl Pts',(70.6637003304768,-11.0942988010231,0.));
#54007=CARTESIAN_POINT('Ctrl Pts',(70.686476913156,-11.0902651324325,0.));
#54008=CARTESIAN_POINT('Ctrl Pts',(70.7092931457996,-11.0862010347022,0.));
#54009=CARTESIAN_POINT('Ctrl Pts',(70.7321488886229,-11.0821064660276,0.));
#54010=CARTESIAN_POINT('Ctrl Pts',(70.7550440024422,-11.0779813848851,0.));
#54011=CARTESIAN_POINT('Ctrl Pts',(70.7779783486689,-11.0738257500292,0.));
#54012=CARTESIAN_POINT('Ctrl Pts',(70.8009517893042,-11.0696395204908,0.));
#54013=CARTESIAN_POINT('Ctrl Pts',(70.8239641869266,-11.0654226555798,0.));
#54014=CARTESIAN_POINT('Ctrl Pts',(70.847015404688,-11.061175114883,0.));
#54015=CARTESIAN_POINT('Ctrl Pts',(70.8701053063158,-11.0568968582566,0.));
#54016=CARTESIAN_POINT('Ctrl Pts',(70.8932337561078,-11.0525878458242,0.));
#54017=CARTESIAN_POINT('Ctrl Pts',(70.9164006189283,-11.0482480379752,0.));
#54018=CARTESIAN_POINT('Ctrl Pts',(70.9396057601953,-11.0438773953686,0.));
#54019=CARTESIAN_POINT('Ctrl Pts',(70.9628490458779,-11.039475878929,0.));
#54020=CARTESIAN_POINT('Ctrl Pts',(70.9861303424989,-11.0350434498408,0.));
#54021=CARTESIAN_POINT('Ctrl Pts',(71.0094495171295,-11.0305800695457,0.));
#54022=CARTESIAN_POINT('Ctrl Pts',(71.0328064373849,-11.0260856997414,0.));
#54023=CARTESIAN_POINT('Ctrl Pts',(71.0562009714125,-11.0215603023854,0.));
#54024=CARTESIAN_POINT('Ctrl Pts',(71.0796329878896,-11.0170038396913,0.));
#54025=CARTESIAN_POINT('Ctrl Pts',(71.1031023560243,-11.0124162741223,0.));
#54026=CARTESIAN_POINT('Ctrl Pts',(71.1266089455517,-11.0077975683895,0.));
#54027=CARTESIAN_POINT('Ctrl Pts',(71.1501526267288,-11.0031476854503,0.));
#54028=CARTESIAN_POINT('Ctrl Pts',(71.1737332703248,-10.9984665885127,0.));
#54029=CARTESIAN_POINT('Ctrl Pts',(71.1973507476188,-10.993754241032,0.));
#54030=CARTESIAN_POINT('Ctrl Pts',(71.221004930401,-10.9890106067038,0.));
#54031=CARTESIAN_POINT('Ctrl Pts',(71.2446956909685,-10.9842356494627,0.));
#54032=CARTESIAN_POINT('Ctrl Pts',(71.2684229021209,-10.9794293334806,0.));
#54033=CARTESIAN_POINT('Ctrl Pts',(71.2921864371499,-10.9745916231711,0.));
#54034=CARTESIAN_POINT('Ctrl Pts',(71.3159861698368,-10.9697224831862,0.));
#54035=CARTESIAN_POINT('Ctrl Pts',(71.3398219744547,-10.96482187841,0.));
#54036=CARTESIAN_POINT('Ctrl Pts',(71.3636937257651,-10.9598897739565,0.));
#54037=CARTESIAN_POINT('Ctrl Pts',(71.3876012990135,-10.954926135169,0.));
#54038=CARTESIAN_POINT('Ctrl Pts',(71.411544569919,-10.9499309276235,0.));
#54039=CARTESIAN_POINT('Ctrl Pts',(71.4355234146718,-10.9449041171269,0.));
#54040=CARTESIAN_POINT('Ctrl Pts',(71.4595377099352,-10.9398456697095,0.));
#54041=CARTESIAN_POINT('Ctrl Pts',(71.4835873328425,-10.9347555516236,0.));
#54042=CARTESIAN_POINT('Ctrl Pts',(71.5076721609936,-10.9296337293425,0.));
#54043=CARTESIAN_POINT('Ctrl Pts',(71.5317920724453,-10.9244801695642,0.));
#54044=CARTESIAN_POINT('Ctrl Pts',(71.5559469457082,-10.9192948392099,0.));
#54045=CARTESIAN_POINT('Ctrl Pts',(71.5801366597479,-10.9140777054169,0.));
#54046=CARTESIAN_POINT('Ctrl Pts',(71.604361093983,-10.9088287355364,0.));
#54047=CARTESIAN_POINT('Ctrl Pts',(71.6286201282815,-10.9035478971329,0.));
#54048=CARTESIAN_POINT('Ctrl Pts',(71.6529136429515,-10.8982351579872,0.));
#54049=CARTESIAN_POINT('Ctrl Pts',(71.6772415187382,-10.8928904860967,0.));
#54050=CARTESIAN_POINT('Ctrl Pts',(71.7016036368254,-10.8875138496674,0.));
#54051=CARTESIAN_POINT('Ctrl Pts',(71.7259998788337,-10.8821052171122,0.));
#54052=CARTESIAN_POINT('Ctrl Pts',(71.7504301268177,-10.8766645570496,0.));
#54053=CARTESIAN_POINT('Ctrl Pts',(71.7748942632578,-10.8711918383071,0.));
#54054=CARTESIAN_POINT('Ctrl Pts',(71.7993921710546,-10.8656870299218,0.));
#54055=CARTESIAN_POINT('Ctrl Pts',(71.8239237335318,-10.860150101133,0.));
#54056=CARTESIAN_POINT('Ctrl Pts',(71.8484888344335,-10.8545810213799,0.));
#54057=CARTESIAN_POINT('Ctrl Pts',(71.8730873579226,-10.8489797602998,0.));
#54058=CARTESIAN_POINT('Ctrl Pts',(71.8977191885726,-10.8433462877312,0.));
#54059=CARTESIAN_POINT('Ctrl Pts',(71.9223842113622,-10.8376805737158,0.));
#54060=CARTESIAN_POINT('Ctrl Pts',(71.9470823116777,-10.8319825884917,0.));
#54061=CARTESIAN_POINT('Ctrl Pts',(71.971813375312,-10.8262523024897,0.));
#54062=CARTESIAN_POINT('Ctrl Pts',(71.996577288462,-10.8204896863328,0.));
#54063=CARTESIAN_POINT('Ctrl Pts',(72.0213739377231,-10.8146947108376,0.));
#54064=CARTESIAN_POINT('Ctrl Pts',(72.0462032100828,-10.8088673470187,0.));
#54065=CARTESIAN_POINT('Ctrl Pts',(72.0710649929214,-10.8030075660811,0.));
#54066=CARTESIAN_POINT('Ctrl Pts',(72.095959174012,-10.7971153394168,0.));
#54067=CARTESIAN_POINT('Ctrl Pts',(72.1208856415171,-10.7911906386027,0.));
#54068=CARTESIAN_POINT('Ctrl Pts',(72.145844283983,-10.7852334354015,0.));
#54069=CARTESIAN_POINT('Ctrl Pts',(72.17083499033,-10.779243701766,0.));
#54070=CARTESIAN_POINT('Ctrl Pts',(72.1958576498556,-10.7732214098343,0.));
#54071=CARTESIAN_POINT('Ctrl Pts',(72.2209121522367,-10.7671665319254,0.));
#54072=CARTESIAN_POINT('Ctrl Pts',(72.2459983875298,-10.7610790405385,0.));
#54073=CARTESIAN_POINT('Ctrl Pts',(72.2711162461679,-10.7549589083535,0.));
#54074=CARTESIAN_POINT('Ctrl Pts',(72.296265618955,-10.7488061082368,0.));
#54075=CARTESIAN_POINT('Ctrl Pts',(72.3214463970634,-10.7426206132375,0.));
#54076=CARTESIAN_POINT('Ctrl Pts',(72.3466584720311,-10.73640239658,0.));
#54077=CARTESIAN_POINT('Ctrl Pts',(72.3719017357568,-10.7301514316607,0.));
#54078=CARTESIAN_POINT('Ctrl Pts',(72.3971760804935,-10.7238676920469,0.));
#54079=CARTESIAN_POINT('Ctrl Pts',(72.4224813988355,-10.7175511514789,0.));
#54080=CARTESIAN_POINT('Ctrl Pts',(72.4478175837168,-10.7112017838707,0.));
#54081=CARTESIAN_POINT('Ctrl Pts',(72.4731845284238,-10.7048195633062,0.));
#54082=CARTESIAN_POINT('Ctrl Pts',(72.4985821266031,-10.6984044640399,0.));
#54083=CARTESIAN_POINT('Ctrl Pts',(72.5240102722662,-10.691956460499,0.));
#54084=CARTESIAN_POINT('Ctrl Pts',(72.5494688597951,-10.6854755272903,0.));
#54085=CARTESIAN_POINT('Ctrl Pts',(72.57495778394,-10.6789616392041,0.));
#54086=CARTESIAN_POINT('Ctrl Pts',(72.6004769398004,-10.6724147711994,0.));
#54087=CARTESIAN_POINT('Ctrl Pts',(72.6260262228055,-10.6658348983944,0.));
#54088=CARTESIAN_POINT('Ctrl Pts',(72.6516055286908,-10.659221996058,0.));
#54089=CARTESIAN_POINT('Ctrl Pts',(72.6772147534762,-10.6525760396055,0.));
#54090=CARTESIAN_POINT('Ctrl Pts',(72.7028537934332,-10.6458970045948,0.));
#54091=CARTESIAN_POINT('Ctrl Pts',(72.7285225451309,-10.6391848667354,0.));
#54092=CARTESIAN_POINT('Ctrl Pts',(72.7542209054823,-10.6324396018999,0.));
#54093=CARTESIAN_POINT('Ctrl Pts',(72.7799487717914,-10.6256611861395,0.));
#54094=CARTESIAN_POINT('Ctrl Pts',(72.8057060417882,-10.6188495956973,0.));
#54095=CARTESIAN_POINT('Ctrl Pts',(72.8314926136872,-10.6120048070366,0.));
#54096=CARTESIAN_POINT('Ctrl Pts',(72.8573083861328,-10.6051267968202,0.));
#54097=CARTESIAN_POINT('Ctrl Pts',(72.8831532580839,-10.5982155418625,0.));
#54098=CARTESIAN_POINT('Ctrl Pts',(72.9090271287081,-10.5912710190928,0.));
#54099=CARTESIAN_POINT('Ctrl Pts',(72.9349298972823,-10.5842932055209,0.));
#54100=CARTESIAN_POINT('Ctrl Pts',(72.9608614630539,-10.5772820781959,0.));
#54101=CARTESIAN_POINT('Ctrl Pts',(72.9868217252293,-10.5702376142052,0.));
#54102=CARTESIAN_POINT('Ctrl Pts',(73.0128105832635,-10.5631597907653,0.));
#54103=CARTESIAN_POINT('Ctrl Pts',(73.0388279370845,-10.5560485852975,0.));
#54104=CARTESIAN_POINT('Ctrl Pts',(73.0648736873435,-10.5489039755138,0.));
#54105=CARTESIAN_POINT('Ctrl Pts',(73.090947735646,-10.5417259395001,0.));
#54106=CARTESIAN_POINT('Ctrl Pts',(73.1170499848012,-10.5345144558097,0.));
#54107=CARTESIAN_POINT('Ctrl Pts',(73.1431803382677,-10.5272695032649,0.));
#54108=CARTESIAN_POINT('Ctrl Pts',(73.169338699611,-10.5199910607652,0.));
#54109=CARTESIAN_POINT('Ctrl Pts',(73.1955249719037,-10.5126791070804,0.));
#54110=CARTESIAN_POINT('Ctrl Pts',(73.2217390572578,-10.505333620691,0.));
#54111=CARTESIAN_POINT('Ctrl Pts',(73.247980856023,-10.4979545795197,0.));
#54112=CARTESIAN_POINT('Ctrl Pts',(73.2742502674361,-10.4905419611529,0.));
#54113=CARTESIAN_POINT('Ctrl Pts',(73.3005471910639,-10.4830957433311,0.));
#54114=CARTESIAN_POINT('Ctrl Pts',(73.3268715280609,-10.475615904381,0.));
#54115=CARTESIAN_POINT('Ctrl Pts',(73.353223182365,-10.4681024236288,0.));
#54116=CARTESIAN_POINT('Ctrl Pts',(73.3796020622437,-10.460555281939,0.));
#54117=CARTESIAN_POINT('Ctrl Pts',(73.4060080806577,-10.4529744618438,0.));
#54118=CARTESIAN_POINT('Ctrl Pts',(73.4286663447915,-10.4464473465486,0.));
#54119=CARTESIAN_POINT('Ctrl Pts',(73.4460525528551,-10.4414249334768,0.));
#54120=CARTESIAN_POINT('Ctrl Pts',(73.4581547436539,-10.4379221501093,0.));
#54121=CARTESIAN_POINT('Ctrl Pts',(73.464965036154,-10.4359488742883,0.));
#54122=CARTESIAN_POINT('Ctrl Pts',(73.4664795929518,-10.4355099267391,0.));
#54123=CARTESIAN_POINT('',(69.079679653846,-11.3136138754165,12.));
#54124=CARTESIAN_POINT('',(69.079679653846,-11.3136138754165,0.));
#54125=CARTESIAN_POINT('Ctrl Pts',(73.4664795929519,-10.4355099267391,12.));
#54126=CARTESIAN_POINT('Ctrl Pts',(73.464965036154,-10.4359488742883,12.));
#54127=CARTESIAN_POINT('Ctrl Pts',(73.458154743654,-10.4379221501093,12.));
#54128=CARTESIAN_POINT('Ctrl Pts',(73.4460525528551,-10.4414249334768,12.));
#54129=CARTESIAN_POINT('Ctrl Pts',(73.4286663447915,-10.4464473465486,12.));
#54130=CARTESIAN_POINT('Ctrl Pts',(73.4060080806577,-10.4529744618438,12.));
#54131=CARTESIAN_POINT('Ctrl Pts',(73.3796020622437,-10.460555281939,12.));
#54132=CARTESIAN_POINT('Ctrl Pts',(73.353223182365,-10.4681024236288,12.));
#54133=CARTESIAN_POINT('Ctrl Pts',(73.3268715280609,-10.475615904381,12.));
#54134=CARTESIAN_POINT('Ctrl Pts',(73.3005471910639,-10.4830957433311,12.));
#54135=CARTESIAN_POINT('Ctrl Pts',(73.2742502674361,-10.4905419611529,12.));
#54136=CARTESIAN_POINT('Ctrl Pts',(73.247980856023,-10.4979545795197,12.));
#54137=CARTESIAN_POINT('Ctrl Pts',(73.2217390572578,-10.505333620691,12.));
#54138=CARTESIAN_POINT('Ctrl Pts',(73.1955249719037,-10.5126791070804,12.));
#54139=CARTESIAN_POINT('Ctrl Pts',(73.169338699611,-10.5199910607652,12.));
#54140=CARTESIAN_POINT('Ctrl Pts',(73.1431803382677,-10.5272695032649,12.));
#54141=CARTESIAN_POINT('Ctrl Pts',(73.1170499848012,-10.5345144558097,12.));
#54142=CARTESIAN_POINT('Ctrl Pts',(73.090947735646,-10.5417259395001,12.));
#54143=CARTESIAN_POINT('Ctrl Pts',(73.0648736873435,-10.5489039755138,12.));
#54144=CARTESIAN_POINT('Ctrl Pts',(73.0388279370845,-10.5560485852975,12.));
#54145=CARTESIAN_POINT('Ctrl Pts',(73.0128105832635,-10.5631597907653,12.));
#54146=CARTESIAN_POINT('Ctrl Pts',(72.9868217252293,-10.5702376142052,12.));
#54147=CARTESIAN_POINT('Ctrl Pts',(72.9608614630539,-10.5772820781959,12.));
#54148=CARTESIAN_POINT('Ctrl Pts',(72.9349298972823,-10.5842932055209,12.));
#54149=CARTESIAN_POINT('Ctrl Pts',(72.9090271287081,-10.5912710190928,12.));
#54150=CARTESIAN_POINT('Ctrl Pts',(72.8831532580839,-10.5982155418625,12.));
#54151=CARTESIAN_POINT('Ctrl Pts',(72.8573083861328,-10.6051267968202,12.));
#54152=CARTESIAN_POINT('Ctrl Pts',(72.8314926136872,-10.6120048070366,12.));
#54153=CARTESIAN_POINT('Ctrl Pts',(72.8057060417882,-10.6188495956973,12.));
#54154=CARTESIAN_POINT('Ctrl Pts',(72.7799487717914,-10.6256611861395,12.));
#54155=CARTESIAN_POINT('Ctrl Pts',(72.7542209054823,-10.6324396018999,12.));
#54156=CARTESIAN_POINT('Ctrl Pts',(72.7285225451309,-10.6391848667354,12.));
#54157=CARTESIAN_POINT('Ctrl Pts',(72.7028537934332,-10.6458970045948,12.));
#54158=CARTESIAN_POINT('Ctrl Pts',(72.6772147534762,-10.6525760396055,12.));
#54159=CARTESIAN_POINT('Ctrl Pts',(72.6516055286908,-10.659221996058,12.));
#54160=CARTESIAN_POINT('Ctrl Pts',(72.6260262228055,-10.6658348983944,12.));
#54161=CARTESIAN_POINT('Ctrl Pts',(72.6004769398004,-10.6724147711994,12.));
#54162=CARTESIAN_POINT('Ctrl Pts',(72.57495778394,-10.6789616392041,12.));
#54163=CARTESIAN_POINT('Ctrl Pts',(72.5494688597951,-10.6854755272903,12.));
#54164=CARTESIAN_POINT('Ctrl Pts',(72.5240102722662,-10.691956460499,12.));
#54165=CARTESIAN_POINT('Ctrl Pts',(72.4985821266031,-10.6984044640399,12.));
#54166=CARTESIAN_POINT('Ctrl Pts',(72.4731845284238,-10.7048195633062,12.));
#54167=CARTESIAN_POINT('Ctrl Pts',(72.4478175837168,-10.7112017838707,12.));
#54168=CARTESIAN_POINT('Ctrl Pts',(72.4224813988355,-10.7175511514789,12.));
#54169=CARTESIAN_POINT('Ctrl Pts',(72.3971760804935,-10.7238676920469,12.));
#54170=CARTESIAN_POINT('Ctrl Pts',(72.3719017357568,-10.7301514316607,12.));
#54171=CARTESIAN_POINT('Ctrl Pts',(72.3466584720311,-10.73640239658,12.));
#54172=CARTESIAN_POINT('Ctrl Pts',(72.3214463970634,-10.7426206132375,12.));
#54173=CARTESIAN_POINT('Ctrl Pts',(72.296265618955,-10.7488061082368,12.));
#54174=CARTESIAN_POINT('Ctrl Pts',(72.2711162461679,-10.7549589083535,12.));
#54175=CARTESIAN_POINT('Ctrl Pts',(72.2459983875298,-10.7610790405385,12.));
#54176=CARTESIAN_POINT('Ctrl Pts',(72.2209121522367,-10.7671665319254,12.));
#54177=CARTESIAN_POINT('Ctrl Pts',(72.1958576498556,-10.7732214098343,12.));
#54178=CARTESIAN_POINT('Ctrl Pts',(72.17083499033,-10.779243701766,12.));
#54179=CARTESIAN_POINT('Ctrl Pts',(72.145844283983,-10.7852334354015,12.));
#54180=CARTESIAN_POINT('Ctrl Pts',(72.1208856415171,-10.7911906386027,12.));
#54181=CARTESIAN_POINT('Ctrl Pts',(72.095959174012,-10.7971153394168,12.));
#54182=CARTESIAN_POINT('Ctrl Pts',(72.0710649929214,-10.8030075660811,12.));
#54183=CARTESIAN_POINT('Ctrl Pts',(72.0462032100828,-10.8088673470187,12.));
#54184=CARTESIAN_POINT('Ctrl Pts',(72.0213739377231,-10.8146947108376,12.));
#54185=CARTESIAN_POINT('Ctrl Pts',(71.996577288462,-10.8204896863328,12.));
#54186=CARTESIAN_POINT('Ctrl Pts',(71.971813375312,-10.8262523024897,12.));
#54187=CARTESIAN_POINT('Ctrl Pts',(71.9470823116777,-10.8319825884917,12.));
#54188=CARTESIAN_POINT('Ctrl Pts',(71.9223842113622,-10.8376805737158,12.));
#54189=CARTESIAN_POINT('Ctrl Pts',(71.8977191885726,-10.8433462877312,12.));
#54190=CARTESIAN_POINT('Ctrl Pts',(71.8730873579226,-10.8489797602998,12.));
#54191=CARTESIAN_POINT('Ctrl Pts',(71.8484888344335,-10.8545810213799,12.));
#54192=CARTESIAN_POINT('Ctrl Pts',(71.8239237335318,-10.860150101133,12.));
#54193=CARTESIAN_POINT('Ctrl Pts',(71.7993921710546,-10.8656870299218,12.));
#54194=CARTESIAN_POINT('Ctrl Pts',(71.7748942632578,-10.8711918383071,12.));
#54195=CARTESIAN_POINT('Ctrl Pts',(71.7504301268177,-10.8766645570496,12.));
#54196=CARTESIAN_POINT('Ctrl Pts',(71.7259998788337,-10.8821052171122,12.));
#54197=CARTESIAN_POINT('Ctrl Pts',(71.7016036368254,-10.8875138496674,12.));
#54198=CARTESIAN_POINT('Ctrl Pts',(71.6772415187382,-10.8928904860967,12.));
#54199=CARTESIAN_POINT('Ctrl Pts',(71.6529136429515,-10.8982351579872,12.));
#54200=CARTESIAN_POINT('Ctrl Pts',(71.6286201282815,-10.9035478971329,12.));
#54201=CARTESIAN_POINT('Ctrl Pts',(71.604361093983,-10.9088287355364,12.));
#54202=CARTESIAN_POINT('Ctrl Pts',(71.5801366597479,-10.9140777054169,12.));
#54203=CARTESIAN_POINT('Ctrl Pts',(71.5559469457082,-10.9192948392099,12.));
#54204=CARTESIAN_POINT('Ctrl Pts',(71.5317920724453,-10.9244801695642,12.));
#54205=CARTESIAN_POINT('Ctrl Pts',(71.5076721609936,-10.9296337293425,12.));
#54206=CARTESIAN_POINT('Ctrl Pts',(71.4835873328425,-10.9347555516236,12.));
#54207=CARTESIAN_POINT('Ctrl Pts',(71.4595377099352,-10.9398456697095,12.));
#54208=CARTESIAN_POINT('Ctrl Pts',(71.4355234146718,-10.9449041171269,12.));
#54209=CARTESIAN_POINT('Ctrl Pts',(71.411544569919,-10.9499309276235,12.));
#54210=CARTESIAN_POINT('Ctrl Pts',(71.3876012990135,-10.954926135169,12.));
#54211=CARTESIAN_POINT('Ctrl Pts',(71.3636937257651,-10.9598897739565,12.));
#54212=CARTESIAN_POINT('Ctrl Pts',(71.3398219744547,-10.96482187841,12.));
#54213=CARTESIAN_POINT('Ctrl Pts',(71.3159861698368,-10.9697224831862,12.));
#54214=CARTESIAN_POINT('Ctrl Pts',(71.2921864371499,-10.9745916231711,12.));
#54215=CARTESIAN_POINT('Ctrl Pts',(71.2684229021209,-10.9794293334806,12.));
#54216=CARTESIAN_POINT('Ctrl Pts',(71.2446956909685,-10.9842356494627,12.));
#54217=CARTESIAN_POINT('Ctrl Pts',(71.221004930401,-10.9890106067038,12.));
#54218=CARTESIAN_POINT('Ctrl Pts',(71.1973507476188,-10.993754241032,12.));
#54219=CARTESIAN_POINT('Ctrl Pts',(71.1737332703248,-10.9984665885127,12.));
#54220=CARTESIAN_POINT('Ctrl Pts',(71.1501526267288,-11.0031476854503,12.));
#54221=CARTESIAN_POINT('Ctrl Pts',(71.1266089455517,-11.0077975683895,12.));
#54222=CARTESIAN_POINT('Ctrl Pts',(71.1031023560243,-11.0124162741223,12.));
#54223=CARTESIAN_POINT('Ctrl Pts',(71.0796329878896,-11.0170038396913,12.));
#54224=CARTESIAN_POINT('Ctrl Pts',(71.0562009714125,-11.0215603023854,12.));
#54225=CARTESIAN_POINT('Ctrl Pts',(71.0328064373849,-11.0260856997414,12.));
#54226=CARTESIAN_POINT('Ctrl Pts',(71.0094495171295,-11.0305800695457,12.));
#54227=CARTESIAN_POINT('Ctrl Pts',(70.9861303424989,-11.0350434498408,12.));
#54228=CARTESIAN_POINT('Ctrl Pts',(70.9628490458779,-11.039475878929,12.));
#54229=CARTESIAN_POINT('Ctrl Pts',(70.9396057601953,-11.0438773953686,12.));
#54230=CARTESIAN_POINT('Ctrl Pts',(70.9164006189283,-11.0482480379752,12.));
#54231=CARTESIAN_POINT('Ctrl Pts',(70.8932337561078,-11.0525878458242,12.));
#54232=CARTESIAN_POINT('Ctrl Pts',(70.8701053063158,-11.0568968582566,12.));
#54233=CARTESIAN_POINT('Ctrl Pts',(70.847015404688,-11.061175114883,12.));
#54234=CARTESIAN_POINT('Ctrl Pts',(70.8239641869266,-11.0654226555798,12.));
#54235=CARTESIAN_POINT('Ctrl Pts',(70.8009517893042,-11.0696395204908,12.));
#54236=CARTESIAN_POINT('Ctrl Pts',(70.7779783486689,-11.0738257500292,12.));
#54237=CARTESIAN_POINT('Ctrl Pts',(70.7550440024422,-11.0779813848851,12.));
#54238=CARTESIAN_POINT('Ctrl Pts',(70.7321488886229,-11.0821064660276,12.));
#54239=CARTESIAN_POINT('Ctrl Pts',(70.7092931457996,-11.0862010347022,12.));
#54240=CARTESIAN_POINT('Ctrl Pts',(70.686476913156,-11.0902651324325,12.));
#54241=CARTESIAN_POINT('Ctrl Pts',(70.6637003304768,-11.0942988010231,12.));
#54242=CARTESIAN_POINT('Ctrl Pts',(70.6409635381446,-11.0983020825662,12.));
#54243=CARTESIAN_POINT('Ctrl Pts',(70.6182666771441,-11.1022750194439,12.));
#54244=CARTESIAN_POINT('Ctrl Pts',(70.5956098890744,-11.1062176543257,12.));
#54245=CARTESIAN_POINT('Ctrl Pts',(70.5729933161538,-11.11013003017,12.));
#54246=CARTESIAN_POINT('Ctrl Pts',(70.5504171012247,-11.1140121902274,12.));
#54247=CARTESIAN_POINT('Ctrl Pts',(70.5278813877519,-11.117864178048,12.));
#54248=CARTESIAN_POINT('Ctrl Pts',(70.5053863198306,-11.121686037483,12.));
#54249=CARTESIAN_POINT('Ctrl Pts',(70.4829320421973,-11.1254778126824,12.));
#54250=CARTESIAN_POINT('Ctrl Pts',(70.4605187002356,-11.1292395480975,12.));
#54251=CARTESIAN_POINT('Ctrl Pts',(70.438146439981,-11.1329712884845,12.));
#54252=CARTESIAN_POINT('Ctrl Pts',(70.415815408119,-11.1366730789122,12.));
#54253=CARTESIAN_POINT('Ctrl Pts',(70.3935257519945,-11.1403449647622,12.));
#54254=CARTESIAN_POINT('Ctrl Pts',(70.3712776196216,-11.1439869917269,12.));
#54255=CARTESIAN_POINT('Ctrl Pts',(70.3490711596882,-11.1475992058124,12.));
#54256=CARTESIAN_POINT('Ctrl Pts',(70.3269065215591,-11.1511816533422,12.));
#54257=CARTESIAN_POINT('Ctrl Pts',(70.3047838552758,-11.1547343809647,12.));
#54258=CARTESIAN_POINT('Ctrl Pts',(70.2827033115662,-11.1582574356522,12.));
#54259=CARTESIAN_POINT('Ctrl Pts',(70.2606650418589,-11.1617508647017,12.));
#54260=CARTESIAN_POINT('Ctrl Pts',(70.2386691982902,-11.1652147157383,12.));
#54261=CARTESIAN_POINT('Ctrl Pts',(70.2167159337095,-11.168649036721,12.));
#54262=CARTESIAN_POINT('Ctrl Pts',(70.1948054016817,-11.1720538759499,12.));
#54263=CARTESIAN_POINT('Ctrl Pts',(70.1729377564956,-11.1754292820631,12.));
#54264=CARTESIAN_POINT('Ctrl Pts',(70.1511131531674,-11.1787753040363,12.));
#54265=CARTESIAN_POINT('Ctrl Pts',(70.1293317474432,-11.1820919911846,12.));
#54266=CARTESIAN_POINT('Ctrl Pts',(70.1075936957968,-11.185379393167,12.));
#54267=CARTESIAN_POINT('Ctrl Pts',(70.0858991554283,-11.1886375599914,12.));
#54268=CARTESIAN_POINT('Ctrl Pts',(70.0642482842928,-11.1918665420166,12.));
#54269=CARTESIAN_POINT('Ctrl Pts',(70.0426412411185,-11.1950663899576,12.));
#54270=CARTESIAN_POINT('Ctrl Pts',(70.0210781854243,-11.1982371548919,12.));
#54271=CARTESIAN_POINT('Ctrl Pts',(69.9995592775343,-11.2013788882714,12.));
#54272=CARTESIAN_POINT('Ctrl Pts',(69.97808467858,-11.2044916419244,12.));
#54273=CARTESIAN_POINT('Ctrl Pts',(69.9566545504837,-11.2075754680449,12.));
#54274=CARTESIAN_POINT('Ctrl Pts',(69.9352690559405,-11.2106304191882,12.));
#54275=CARTESIAN_POINT('Ctrl Pts',(69.9139283584022,-11.2136565482678,12.));
#54276=CARTESIAN_POINT('Ctrl Pts',(69.8926326220385,-11.2166539085523,12.));
#54277=CARTESIAN_POINT('Ctrl Pts',(69.871382011789,-11.219622553679,12.));
#54278=CARTESIAN_POINT('Ctrl Pts',(69.8501766934428,-11.2225625376736,12.));
#54279=CARTESIAN_POINT('Ctrl Pts',(69.8290168337076,-11.225473914972,12.));
#54280=CARTESIAN_POINT('Ctrl Pts',(69.8079026002768,-11.2283567404437,12.));
#54281=CARTESIAN_POINT('Ctrl Pts',(69.7868341618954,-11.2312110694187,12.));
#54282=CARTESIAN_POINT('Ctrl Pts',(69.7658116882324,-11.2340369576456,12.));
#54283=CARTESIAN_POINT('Ctrl Pts',(69.7448353497408,-11.2368344612472,12.));
#54284=CARTESIAN_POINT('Ctrl Pts',(69.7239053175356,-11.239603636686,12.));
#54285=CARTESIAN_POINT('Ctrl Pts',(69.7030217632164,-11.2423445407166,12.));
#54286=CARTESIAN_POINT('Ctrl Pts',(69.6821848588457,-11.2450572303841,12.));
#54287=CARTESIAN_POINT('Ctrl Pts',(69.6613947773534,-11.2477417631386,12.));
#54288=CARTESIAN_POINT('Ctrl Pts',(69.6406516928891,-11.2503981969412,12.));
#54289=CARTESIAN_POINT('Ctrl Pts',(69.6199557811245,-11.2530265903557,12.));
#54290=CARTESIAN_POINT('Ctrl Pts',(69.599307219739,-11.2556270027016,12.));
#54291=CARTESIAN_POINT('Ctrl Pts',(69.5787061880857,-11.2581994939541,12.));
#54292=CARTESIAN_POINT('Ctrl Pts',(69.5581528662877,-11.2607441244703,12.));
#54293=CARTESIAN_POINT('Ctrl Pts',(69.5376474344771,-11.263260954763,12.));
#54294=CARTESIAN_POINT('Ctrl Pts',(69.5171900720158,-11.2657500452716,12.));
#54295=CARTESIAN_POINT('Ctrl Pts',(69.4967809565929,-11.2682114561008,12.));
#54296=CARTESIAN_POINT('Ctrl Pts',(69.4764202659397,-11.270645247528,12.));
#54297=CARTESIAN_POINT('Ctrl Pts',(69.456108179879,-11.2730514806139,12.));
#54298=CARTESIAN_POINT('Ctrl Pts',(69.4358448819967,-11.2754302177021,12.));
#54299=CARTESIAN_POINT('Ctrl Pts',(69.4156305620593,-11.2777815231469,12.));
#54300=CARTESIAN_POINT('Ctrl Pts',(69.3954654162281,-11.2801054633816,12.));
#54301=CARTESIAN_POINT('Ctrl Pts',(69.3753496420039,-11.2824021054045,12.));
#54302=CARTESIAN_POINT('Ctrl Pts',(69.3552834337784,-11.2846715154524,12.));
#54303=CARTESIAN_POINT('Ctrl Pts',(69.3352669789587,-11.2869137578459,12.));
#54304=CARTESIAN_POINT('Ctrl Pts',(69.3153004517783,-11.2891288931517,12.));
#54305=CARTESIAN_POINT('Ctrl Pts',(69.295384019272,-11.2913169799628,12.));
#54306=CARTESIAN_POINT('Ctrl Pts',(69.275517853148,-11.2934780784351,12.));
#54307=CARTESIAN_POINT('Ctrl Pts',(69.255702139335,-11.2956122531375,12.));
#54308=CARTESIAN_POINT('Ctrl Pts',(69.2359370894907,-11.2977195764852,12.));
#54309=CARTESIAN_POINT('Ctrl Pts',(69.2162229488531,-11.2998001310964,12.));
#54310=CARTESIAN_POINT('Ctrl Pts',(69.1965599718914,-11.3018540025638,12.));
#54311=CARTESIAN_POINT('Ctrl Pts',(69.1769483991721,-11.3038812726292,12.));
#54312=CARTESIAN_POINT('Ctrl Pts',(69.1573884361,-11.3058820128307,12.));
#54313=CARTESIAN_POINT('Ctrl Pts',(69.1378802251711,-11.3078562764384,12.));
#54314=CARTESIAN_POINT('Ctrl Pts',(69.118423844466,-11.3098040973713,12.));
#54315=CARTESIAN_POINT('Ctrl Pts',(69.1029002322118,-11.3113412156661,12.));
#54316=CARTESIAN_POINT('Ctrl Pts',(69.0912808656811,-11.3124821678798,12.));
#54317=CARTESIAN_POINT('Ctrl Pts',(69.0835449954396,-11.3132375200165,12.));
#54318=CARTESIAN_POINT('Ctrl Pts',(69.079679653846,-11.3136138754165,12.));
#54319=CARTESIAN_POINT('Ctrl Pts',(73.664078719806,-8.93459554657863,0.));
#54320=CARTESIAN_POINT('Ctrl Pts',(73.664078719806,-8.93459554657863,4.));
#54321=CARTESIAN_POINT('Ctrl Pts',(73.664078719806,-8.93459554657865,8.));
#54322=CARTESIAN_POINT('Ctrl Pts',(73.664078719806,-8.93459554657865,12.));
#54323=CARTESIAN_POINT('Ctrl Pts',(73.7581053903597,-8.99145626777918,0.));
#54324=CARTESIAN_POINT('Ctrl Pts',(73.7581053903597,-8.99145626777918,4.));
#54325=CARTESIAN_POINT('Ctrl Pts',(73.7581053903597,-8.9914562677792,8.00000000000001));
#54326=CARTESIAN_POINT('Ctrl Pts',(73.7581053903597,-8.9914562677792,12.));
#54327=CARTESIAN_POINT('Ctrl Pts',(73.8880618019208,-9.14696952162308,0.));
#54328=CARTESIAN_POINT('Ctrl Pts',(73.8880618019208,-9.14696952162308,4.));
#54329=CARTESIAN_POINT('Ctrl Pts',(73.8880618019208,-9.1469695216231,7.99999999999999));
#54330=CARTESIAN_POINT('Ctrl Pts',(73.8880618019208,-9.1469695216231,12.));
#54331=CARTESIAN_POINT('Ctrl Pts',(73.9117532086772,-9.34395683490516,0.));
#54332=CARTESIAN_POINT('Ctrl Pts',(73.9117532086772,-9.34395683490516,4.));
#54333=CARTESIAN_POINT('Ctrl Pts',(73.9117532086772,-9.34395683490517,8.00000000000001));
#54334=CARTESIAN_POINT('Ctrl Pts',(73.9117532086772,-9.34395683490517,12.));
#54335=CARTESIAN_POINT('Ctrl Pts',(73.9013264985864,-9.4257064323754,0.));
#54336=CARTESIAN_POINT('Ctrl Pts',(73.9013264985864,-9.4257064323754,4.));
#54337=CARTESIAN_POINT('Ctrl Pts',(73.9013264985864,-9.4257064323754,8.));
#54338=CARTESIAN_POINT('Ctrl Pts',(73.9013264985864,-9.4257064323754,12.));
#54339=CARTESIAN_POINT('',(73.664078719806,-8.93459554657863,0.));
#54340=CARTESIAN_POINT('',(73.9013264985865,-9.4257064323754,0.));
#54341=CARTESIAN_POINT('Ctrl Pts',(73.664078719806,-8.93459554657863,6.97125684381022E-35));
#54342=CARTESIAN_POINT('Ctrl Pts',(73.7581053903597,-8.99145626777918,6.97125684381022E-35));
#54343=CARTESIAN_POINT('Ctrl Pts',(73.832366196966,-9.08032098426141,6.97125684381023E-35));
#54344=CARTESIAN_POINT('Ctrl Pts',(73.8719282264933,-9.18272825076427,6.97125684381023E-35));
#54345=CARTESIAN_POINT('Ctrl Pts',(73.9015997486387,-9.25953370064141,6.97125684381022E-35));
#54346=CARTESIAN_POINT('Ctrl Pts',(73.9117532086772,-9.34395683490516,6.97125684381022E-35));
#54347=CARTESIAN_POINT('Ctrl Pts',(73.9013264985864,-9.4257064323754,6.97125684381022E-35));
#54348=CARTESIAN_POINT('',(73.9013264985865,-9.4257064323754,12.));
#54349=CARTESIAN_POINT('Ctrl Pts',(73.9013264985864,-9.4257064323754,0.));
#54350=CARTESIAN_POINT('Ctrl Pts',(73.9013264985864,-9.4257064323754,4.));
#54351=CARTESIAN_POINT('Ctrl Pts',(73.9013264985864,-9.4257064323754,8.));
#54352=CARTESIAN_POINT('Ctrl Pts',(73.9013264985864,-9.4257064323754,12.));
#54353=CARTESIAN_POINT('',(73.664078719806,-8.93459554657865,12.));
#54354=CARTESIAN_POINT('Ctrl Pts',(73.9013264985864,-9.4257064323754,12.));
#54355=CARTESIAN_POINT('Ctrl Pts',(73.9117532086772,-9.34395683490517,12.));
#54356=CARTESIAN_POINT('Ctrl Pts',(73.9015997486387,-9.25953370064143,12.));
#54357=CARTESIAN_POINT('Ctrl Pts',(73.8719282264933,-9.18272825076428,12.));
#54358=CARTESIAN_POINT('Ctrl Pts',(73.832366196966,-9.08032098426143,12.));
#54359=CARTESIAN_POINT('Ctrl Pts',(73.7581053903597,-8.9914562677792,12.));
#54360=CARTESIAN_POINT('Ctrl Pts',(73.664078719806,-8.93459554657865,12.));
#54361=CARTESIAN_POINT('Ctrl Pts',(73.664078719806,-8.93459554657865,12.));
#54362=CARTESIAN_POINT('Ctrl Pts',(73.664078719806,-8.93459554657865,8.));
#54363=CARTESIAN_POINT('Ctrl Pts',(73.664078719806,-8.93459554657863,4.));
#54364=CARTESIAN_POINT('Ctrl Pts',(73.664078719806,-8.93459554657863,0.));
#54365=CARTESIAN_POINT('Origin',(3.71649880366789E-10,-4.88285199465431E-11,
0.));
#54366=CARTESIAN_POINT('Origin',(3.71649880366789E-10,-4.88285199465431E-11,
12.));
#54367=CARTESIAN_POINT('Origin',(3.71649880366789E-10,-4.88285199465431E-11,
0.));
#54368=CARTESIAN_POINT('Ctrl Pts',(72.6683126419592,-16.4184755008033,-5.55111512312578E-16));
#54369=CARTESIAN_POINT('Ctrl Pts',(72.6683126419592,-16.4184755008033,4.));
#54370=CARTESIAN_POINT('Ctrl Pts',(72.6683126419592,-16.4184755008033,8.));
#54371=CARTESIAN_POINT('Ctrl Pts',(72.6683126419592,-16.4184755008033,12.));
#54372=CARTESIAN_POINT('Ctrl Pts',(72.644096499941,-16.5256563519777,-5.55111512312578E-16));
#54373=CARTESIAN_POINT('Ctrl Pts',(72.644096499941,-16.5256563519777,4.));
#54374=CARTESIAN_POINT('Ctrl Pts',(72.644096499941,-16.5256563519777,8.00000000000001));
#54375=CARTESIAN_POINT('Ctrl Pts',(72.644096499941,-16.5256563519777,12.));
#54376=CARTESIAN_POINT('Ctrl Pts',(72.5376471652845,-16.6981133841325,-5.55111512312578E-16));
#54377=CARTESIAN_POINT('Ctrl Pts',(72.5376471652845,-16.6981133841325,4.));
#54378=CARTESIAN_POINT('Ctrl Pts',(72.5376471652845,-16.6981133841324,7.99999999999999));
#54379=CARTESIAN_POINT('Ctrl Pts',(72.5376471652845,-16.6981133841324,12.));
#54380=CARTESIAN_POINT('Ctrl Pts',(72.3582555997247,-16.7828708182973,-5.55111512312578E-16));
#54381=CARTESIAN_POINT('Ctrl Pts',(72.3582555997247,-16.7828708182973,4.));
#54382=CARTESIAN_POINT('Ctrl Pts',(72.3582555997247,-16.7828708182972,8.00000000000001));
#54383=CARTESIAN_POINT('Ctrl Pts',(72.3582555997247,-16.7828708182972,12.));
#54384=CARTESIAN_POINT('Ctrl Pts',(72.2774028393488,-16.7988252568804,-5.55111512312578E-16));
#54385=CARTESIAN_POINT('Ctrl Pts',(72.2774028393488,-16.7988252568804,4.));
#54386=CARTESIAN_POINT('Ctrl Pts',(72.2774028393488,-16.7988252568804,8.));
#54387=CARTESIAN_POINT('Ctrl Pts',(72.2774028393488,-16.7988252568804,12.));
#54388=CARTESIAN_POINT('',(72.6683126419592,-16.4184755008033,2.77555756156289E-16));
#54389=CARTESIAN_POINT('',(72.2774028393488,-16.7988252568806,0.));
#54390=CARTESIAN_POINT('Ctrl Pts',(72.6683126419592,-16.4184755008033,1.02909569064144E-17));
#54391=CARTESIAN_POINT('Ctrl Pts',(72.644096499941,-16.5256563519777,1.02909569064142E-17));
#54392=CARTESIAN_POINT('Ctrl Pts',(72.5832683087087,-16.6242032274947,1.02909569064147E-17));
#54393=CARTESIAN_POINT('Ctrl Pts',(72.4986222461611,-16.6941134995864,1.02909569064145E-17));
#54394=CARTESIAN_POINT('Ctrl Pts',(72.4351376992503,-16.7465462036552,1.02909569064144E-17));
#54395=CARTESIAN_POINT('Ctrl Pts',(72.3582555997247,-16.7828708182973,1.0290956906414E-17));
#54396=CARTESIAN_POINT('Ctrl Pts',(72.2774028393488,-16.7988252568804,1.02909569064144E-17));
#54397=CARTESIAN_POINT('',(72.2774028393489,-16.7988252568806,12.));
#54398=CARTESIAN_POINT('Ctrl Pts',(72.2774028393488,-16.7988252568804,-5.55111512312578E-16));
#54399=CARTESIAN_POINT('Ctrl Pts',(72.2774028393488,-16.7988252568804,4.));
#54400=CARTESIAN_POINT('Ctrl Pts',(72.2774028393488,-16.7988252568804,8.));
#54401=CARTESIAN_POINT('Ctrl Pts',(72.2774028393488,-16.7988252568804,12.));
#54402=CARTESIAN_POINT('',(72.6683126419592,-16.4184755008033,12.));
#54403=CARTESIAN_POINT('Ctrl Pts',(72.2774028393488,-16.7988252568804,12.));
#54404=CARTESIAN_POINT('Ctrl Pts',(72.3582555997247,-16.7828708182972,12.));
#54405=CARTESIAN_POINT('Ctrl Pts',(72.4351376992503,-16.7465462036552,12.));
#54406=CARTESIAN_POINT('Ctrl Pts',(72.4986222461611,-16.6941134995864,12.));
#54407=CARTESIAN_POINT('Ctrl Pts',(72.5832683087087,-16.6242032274947,12.));
#54408=CARTESIAN_POINT('Ctrl Pts',(72.644096499941,-16.5256563519777,12.));
#54409=CARTESIAN_POINT('Ctrl Pts',(72.6683126419592,-16.4184755008033,12.));
#54410=CARTESIAN_POINT('Ctrl Pts',(72.6683126419592,-16.4184755008033,12.));
#54411=CARTESIAN_POINT('Ctrl Pts',(72.6683126419592,-16.4184755008033,8.));
#54412=CARTESIAN_POINT('Ctrl Pts',(72.6683126419592,-16.4184755008033,4.));
#54413=CARTESIAN_POINT('Ctrl Pts',(72.6683126419592,-16.4184755008033,-5.55111512312578E-16));
#54414=CARTESIAN_POINT('Ctrl Pts',(67.8307641965655,-17.2912529479484,0.));
#54415=CARTESIAN_POINT('Ctrl Pts',(67.8307641965655,-17.2912529479484,12.));
#54416=CARTESIAN_POINT('Ctrl Pts',(67.8346476309018,-17.2912149114119,0.));
#54417=CARTESIAN_POINT('Ctrl Pts',(67.8346476309018,-17.2912149114119,12.));
#54418=CARTESIAN_POINT('Ctrl Pts',(67.842419897098,-17.2911366591348,0.));
#54419=CARTESIAN_POINT('Ctrl Pts',(67.842419897098,-17.2911366591348,12.));
#54420=CARTESIAN_POINT('Ctrl Pts',(67.8540944889687,-17.291012743109,0.));
#54421=CARTESIAN_POINT('Ctrl Pts',(67.8540944889687,-17.291012743109,12.));
#54422=CARTESIAN_POINT('Ctrl Pts',(67.8696929978782,-17.2908344459694,0.));
#54423=CARTESIAN_POINT('Ctrl Pts',(67.8696929978782,-17.2908344459694,12.));
#54424=CARTESIAN_POINT('Ctrl Pts',(67.8892451049608,-17.2905897723948,0.));
#54425=CARTESIAN_POINT('Ctrl Pts',(67.8892451049608,-17.2905897723948,12.));
#54426=CARTESIAN_POINT('Ctrl Pts',(67.9088511496686,-17.2903232740694,0.));
#54427=CARTESIAN_POINT('Ctrl Pts',(67.9088511496686,-17.2903232740694,12.));
#54428=CARTESIAN_POINT('Ctrl Pts',(67.9285110571741,-17.2900349103981,0.));
#54429=CARTESIAN_POINT('Ctrl Pts',(67.9285110571741,-17.2900349103981,12.));
#54430=CARTESIAN_POINT('Ctrl Pts',(67.9482246901667,-17.2897246158941,0.));
#54431=CARTESIAN_POINT('Ctrl Pts',(67.9482246901667,-17.2897246158941,12.));
#54432=CARTESIAN_POINT('Ctrl Pts',(67.9679918502579,-17.2893923013894,0.));
#54433=CARTESIAN_POINT('Ctrl Pts',(67.9679918502579,-17.2893923013894,12.));
#54434=CARTESIAN_POINT('Ctrl Pts',(67.987812304921,-17.2890378644866,0.));
#54435=CARTESIAN_POINT('Ctrl Pts',(67.987812304921,-17.2890378644866,12.));
#54436=CARTESIAN_POINT('Ctrl Pts',(68.007685808115,-17.28866119774,0.));
#54437=CARTESIAN_POINT('Ctrl Pts',(68.007685808115,-17.28866119774,12.));
#54438=CARTESIAN_POINT('Ctrl Pts',(68.0276121227356,-17.2882621974721,0.));
#54439=CARTESIAN_POINT('Ctrl Pts',(68.0276121227356,-17.2882621974721,12.));
#54440=CARTESIAN_POINT('Ctrl Pts',(68.0475910442424,-17.2878407730961,0.));
#54441=CARTESIAN_POINT('Ctrl Pts',(68.0475910442424,-17.2878407730961,12.));
#54442=CARTESIAN_POINT('Ctrl Pts',(68.0676223930412,-17.2873968440839,0.));
#54443=CARTESIAN_POINT('Ctrl Pts',(68.0676223930412,-17.2873968440839,12.));
#54444=CARTESIAN_POINT('Ctrl Pts',(68.0877060033205,-17.2869303355432,0.));
#54445=CARTESIAN_POINT('Ctrl Pts',(68.0877060033205,-17.2869303355432,12.));
#54446=CARTESIAN_POINT('Ctrl Pts',(68.1078417137877,-17.2864411745459,0.));
#54447=CARTESIAN_POINT('Ctrl Pts',(68.1078417137877,-17.2864411745459,12.));
#54448=CARTESIAN_POINT('Ctrl Pts',(68.1280293561511,-17.2859292855705,0.));
#54449=CARTESIAN_POINT('Ctrl Pts',(68.1280293561511,-17.2859292855705,12.));
#54450=CARTESIAN_POINT('Ctrl Pts',(68.1482687493226,-17.2853945882072,0.));
#54451=CARTESIAN_POINT('Ctrl Pts',(68.1482687493226,-17.2853945882072,12.));
#54452=CARTESIAN_POINT('Ctrl Pts',(68.1685597054232,-17.2848369995293,0.));
#54453=CARTESIAN_POINT('Ctrl Pts',(68.1685597054232,-17.2848369995293,12.));
#54454=CARTESIAN_POINT('Ctrl Pts',(68.1889020335427,-17.2842564355799,0.));
#54455=CARTESIAN_POINT('Ctrl Pts',(68.1889020335427,-17.2842564355799,12.));
#54456=CARTESIAN_POINT('Ctrl Pts',(68.2092955440567,-17.2836528130819,0.));
#54457=CARTESIAN_POINT('Ctrl Pts',(68.2092955440567,-17.2836528130819,12.));
#54458=CARTESIAN_POINT('Ctrl Pts',(68.2297400535294,-17.2830260513867,0.));
#54459=CARTESIAN_POINT('Ctrl Pts',(68.2297400535294,-17.2830260513867,12.));
#54460=CARTESIAN_POINT('Ctrl Pts',(68.2502353845071,-17.2823760723874,0.));
#54461=CARTESIAN_POINT('Ctrl Pts',(68.2502353845071,-17.2823760723874,12.));
#54462=CARTESIAN_POINT('Ctrl Pts',(68.2707813631731,-17.2817027995831,0.));
#54463=CARTESIAN_POINT('Ctrl Pts',(68.2707813631731,-17.2817027995831,12.));
#54464=CARTESIAN_POINT('Ctrl Pts',(68.2913778177261,-17.2810061574353,0.));
#54465=CARTESIAN_POINT('Ctrl Pts',(68.2913778177261,-17.2810061574353,12.));
#54466=CARTESIAN_POINT('Ctrl Pts',(68.3120245763914,-17.2802860705815,0.));
#54467=CARTESIAN_POINT('Ctrl Pts',(68.3120245763914,-17.2802860705815,12.));
#54468=CARTESIAN_POINT('Ctrl Pts',(68.3327214657575,-17.2795424631799,0.));
#54469=CARTESIAN_POINT('Ctrl Pts',(68.3327214657575,-17.2795424631799,12.));
#54470=CARTESIAN_POINT('Ctrl Pts',(68.3534683116515,-17.2787752592484,0.));
#54471=CARTESIAN_POINT('Ctrl Pts',(68.3534683116515,-17.2787752592484,12.));
#54472=CARTESIAN_POINT('Ctrl Pts',(68.3742649398964,-17.2779843829608,0.));
#54473=CARTESIAN_POINT('Ctrl Pts',(68.3742649398964,-17.2779843829608,12.));
#54474=CARTESIAN_POINT('Ctrl Pts',(68.3951111770487,-17.2771697589384,0.));
#54475=CARTESIAN_POINT('Ctrl Pts',(68.3951111770487,-17.2771697589384,12.));
#54476=CARTESIAN_POINT('Ctrl Pts',(68.4160068512753,-17.2763313126018,0.));
#54477=CARTESIAN_POINT('Ctrl Pts',(68.4160068512753,-17.2763313126018,12.));
#54478=CARTESIAN_POINT('Ctrl Pts',(68.436951792677,-17.2754689702992,0.));
#54479=CARTESIAN_POINT('Ctrl Pts',(68.436951792677,-17.2754689702992,12.));
#54480=CARTESIAN_POINT('Ctrl Pts',(68.4579458328185,-17.2745826591119,0.));
#54481=CARTESIAN_POINT('Ctrl Pts',(68.4579458328185,-17.2745826591119,12.));
#54482=CARTESIAN_POINT('Ctrl Pts',(68.4789888044351,-17.2736723067365,0.));
#54483=CARTESIAN_POINT('Ctrl Pts',(68.4789888044351,-17.2736723067365,12.));
#54484=CARTESIAN_POINT('Ctrl Pts',(68.5000805410911,-17.2727378413489,0.));
#54485=CARTESIAN_POINT('Ctrl Pts',(68.5000805410911,-17.2727378413489,12.));
#54486=CARTESIAN_POINT('Ctrl Pts',(68.521220876786,-17.2717791914544,0.));
#54487=CARTESIAN_POINT('Ctrl Pts',(68.521220876786,-17.2717791914544,12.));
#54488=CARTESIAN_POINT('Ctrl Pts',(68.5424096459772,-17.2707962858919,0.));
#54489=CARTESIAN_POINT('Ctrl Pts',(68.5424096459772,-17.2707962858919,12.));
#54490=CARTESIAN_POINT('Ctrl Pts',(68.5636466837517,-17.269789053896,0.));
#54491=CARTESIAN_POINT('Ctrl Pts',(68.5636466837517,-17.269789053896,12.));
#54492=CARTESIAN_POINT('Ctrl Pts',(68.5849318259449,-17.2687574251428,0.));
#54493=CARTESIAN_POINT('Ctrl Pts',(68.5849318259449,-17.2687574251428,12.));
#54494=CARTESIAN_POINT('Ctrl Pts',(68.6062649092764,-17.2677013298057,0.));
#54495=CARTESIAN_POINT('Ctrl Pts',(68.6062649092764,-17.2677013298057,12.));
#54496=CARTESIAN_POINT('Ctrl Pts',(68.6276457714729,-17.2666206986084,0.));
#54497=CARTESIAN_POINT('Ctrl Pts',(68.6276457714729,-17.2666206986084,12.));
#54498=CARTESIAN_POINT('Ctrl Pts',(68.6490742512057,-17.2655154627928,0.));
#54499=CARTESIAN_POINT('Ctrl Pts',(68.6490742512057,-17.2655154627928,12.));
#54500=CARTESIAN_POINT('Ctrl Pts',(68.6705501880249,-17.2643855540892,0.));
#54501=CARTESIAN_POINT('Ctrl Pts',(68.6705501880249,-17.2643855540892,12.));
#54502=CARTESIAN_POINT('Ctrl Pts',(68.6920734222938,-17.2632309046892,0.));
#54503=CARTESIAN_POINT('Ctrl Pts',(68.6920734222938,-17.2632309046892,12.));
#54504=CARTESIAN_POINT('Ctrl Pts',(68.7136437951097,-17.2620514472182,0.));
#54505=CARTESIAN_POINT('Ctrl Pts',(68.7136437951097,-17.2620514472182,12.));
#54506=CARTESIAN_POINT('Ctrl Pts',(68.7352611482547,-17.2608471147185,0.));
#54507=CARTESIAN_POINT('Ctrl Pts',(68.7352611482547,-17.2608471147185,12.));
#54508=CARTESIAN_POINT('Ctrl Pts',(68.7569253242333,-17.259617840655,0.));
#54509=CARTESIAN_POINT('Ctrl Pts',(68.7569253242333,-17.259617840655,12.));
#54510=CARTESIAN_POINT('Ctrl Pts',(68.7786361662882,-17.2583635589198,0.));
#54511=CARTESIAN_POINT('Ctrl Pts',(68.7786361662882,-17.2583635589198,12.));
#54512=CARTESIAN_POINT('Ctrl Pts',(68.8003935184184,-17.2570842038383,0.));
#54513=CARTESIAN_POINT('Ctrl Pts',(68.8003935184184,-17.2570842038383,12.));
#54514=CARTESIAN_POINT('Ctrl Pts',(68.8221972253941,-17.2557797101812,0.));
#54515=CARTESIAN_POINT('Ctrl Pts',(68.8221972253941,-17.2557797101812,12.));
#54516=CARTESIAN_POINT('Ctrl Pts',(68.844047132755,-17.2544500131624,0.));
#54517=CARTESIAN_POINT('Ctrl Pts',(68.844047132755,-17.2544500131624,12.));
#54518=CARTESIAN_POINT('Ctrl Pts',(68.8659430867972,-17.2530950484258,0.));
#54519=CARTESIAN_POINT('Ctrl Pts',(68.8659430867972,-17.2530950484258,12.));
#54520=CARTESIAN_POINT('Ctrl Pts',(68.8878849345557,-17.2517147520376,0.));
#54521=CARTESIAN_POINT('Ctrl Pts',(68.8878849345557,-17.2517147520376,12.));
#54522=CARTESIAN_POINT('Ctrl Pts',(68.909872523787,-17.2503090604792,0.));
#54523=CARTESIAN_POINT('Ctrl Pts',(68.909872523787,-17.2503090604792,12.));
#54524=CARTESIAN_POINT('Ctrl Pts',(68.9319057029409,-17.248877910643,0.));
#54525=CARTESIAN_POINT('Ctrl Pts',(68.9319057029409,-17.248877910643,12.));
#54526=CARTESIAN_POINT('Ctrl Pts',(68.9539843211619,-17.2474212398275,0.));
#54527=CARTESIAN_POINT('Ctrl Pts',(68.9539843211619,-17.2474212398275,12.));
#54528=CARTESIAN_POINT('Ctrl Pts',(68.9761082282922,-17.2459389857327,0.));
#54529=CARTESIAN_POINT('Ctrl Pts',(68.9761082282922,-17.2459389857327,12.));
#54530=CARTESIAN_POINT('Ctrl Pts',(68.9982772748694,-17.2444310864585,0.));
#54531=CARTESIAN_POINT('Ctrl Pts',(68.9982772748694,-17.2444310864585,12.));
#54532=CARTESIAN_POINT('Ctrl Pts',(69.0204913121225,-17.2428974805044,0.));
#54533=CARTESIAN_POINT('Ctrl Pts',(69.0204913121225,-17.2428974805044,12.));
#54534=CARTESIAN_POINT('Ctrl Pts',(69.0427501919636,-17.2413381067723,0.));
#54535=CARTESIAN_POINT('Ctrl Pts',(69.0427501919636,-17.2413381067723,12.));
#54536=CARTESIAN_POINT('Ctrl Pts',(69.065053766986,-17.2397529045589,0.));
#54537=CARTESIAN_POINT('Ctrl Pts',(69.065053766986,-17.2397529045589,12.));
#54538=CARTESIAN_POINT('Ctrl Pts',(69.0874018904599,-17.2381418135491,0.));
#54539=CARTESIAN_POINT('Ctrl Pts',(69.0874018904599,-17.2381418135491,12.));
#54540=CARTESIAN_POINT('Ctrl Pts',(69.1097944163245,-17.2365047738125,0.));
#54541=CARTESIAN_POINT('Ctrl Pts',(69.1097944163245,-17.2365047738125,12.));
#54542=CARTESIAN_POINT('Ctrl Pts',(69.1322311991752,-17.2348417258015,0.));
#54543=CARTESIAN_POINT('Ctrl Pts',(69.1322311991752,-17.2348417258015,12.));
#54544=CARTESIAN_POINT('Ctrl Pts',(69.1547120942527,-17.2331526103506,0.));
#54545=CARTESIAN_POINT('Ctrl Pts',(69.1547120942527,-17.2331526103506,12.));
#54546=CARTESIAN_POINT('Ctrl Pts',(69.1772369574447,-17.23143736867,0.));
#54547=CARTESIAN_POINT('Ctrl Pts',(69.1772369574447,-17.23143736867,12.));
#54548=CARTESIAN_POINT('Ctrl Pts',(69.1998056452828,-17.2296959423407,0.));
#54549=CARTESIAN_POINT('Ctrl Pts',(69.1998056452828,-17.2296959423407,12.));
#54550=CARTESIAN_POINT('Ctrl Pts',(69.222418014938,-17.227928273312,0.));
#54551=CARTESIAN_POINT('Ctrl Pts',(69.222418014938,-17.227928273312,12.));
#54552=CARTESIAN_POINT('Ctrl Pts',(69.2450739242109,-17.226134303902,0.));
#54553=CARTESIAN_POINT('Ctrl Pts',(69.2450739242109,-17.226134303902,12.));
#54554=CARTESIAN_POINT('Ctrl Pts',(69.2677732315224,-17.224313976797,0.));
#54555=CARTESIAN_POINT('Ctrl Pts',(69.2677732315224,-17.224313976797,12.));
#54556=CARTESIAN_POINT('Ctrl Pts',(69.2905157959166,-17.2224672350438,0.));
#54557=CARTESIAN_POINT('Ctrl Pts',(69.2905157959166,-17.2224672350438,12.));
#54558=CARTESIAN_POINT('Ctrl Pts',(69.3133014770555,-17.2205940220459,0.));
#54559=CARTESIAN_POINT('Ctrl Pts',(69.3133014770555,-17.2205940220459,12.));
#54560=CARTESIAN_POINT('Ctrl Pts',(69.3361301352141,-17.2186942815602,0.));
#54561=CARTESIAN_POINT('Ctrl Pts',(69.3361301352141,-17.2186942815602,12.));
#54562=CARTESIAN_POINT('Ctrl Pts',(69.3590016312692,-17.2167679576984,0.));
#54563=CARTESIAN_POINT('Ctrl Pts',(69.3590016312692,-17.2167679576984,12.));
#54564=CARTESIAN_POINT('Ctrl Pts',(69.3819158266916,-17.2148149949252,0.));
#54565=CARTESIAN_POINT('Ctrl Pts',(69.3819158266916,-17.2148149949252,12.));
#54566=CARTESIAN_POINT('Ctrl Pts',(69.404872583548,-17.2128353380502,0.));
#54567=CARTESIAN_POINT('Ctrl Pts',(69.404872583548,-17.2128353380502,12.));
#54568=CARTESIAN_POINT('Ctrl Pts',(69.4278717644973,-17.2108289322254,0.));
#54569=CARTESIAN_POINT('Ctrl Pts',(69.4278717644973,-17.2108289322254,12.));
#54570=CARTESIAN_POINT('Ctrl Pts',(69.450913232785,-17.2087957229423,0.));
#54571=CARTESIAN_POINT('Ctrl Pts',(69.450913232785,-17.2087957229423,12.));
#54572=CARTESIAN_POINT('Ctrl Pts',(69.4739968522313,-17.2067356560336,0.));
#54573=CARTESIAN_POINT('Ctrl Pts',(69.4739968522313,-17.2067356560336,12.));
#54574=CARTESIAN_POINT('Ctrl Pts',(69.4971224872269,-17.2046486776708,0.));
#54575=CARTESIAN_POINT('Ctrl Pts',(69.4971224872269,-17.2046486776708,12.));
#54576=CARTESIAN_POINT('Ctrl Pts',(69.5202900027367,-17.2025347343577,0.));
#54577=CARTESIAN_POINT('Ctrl Pts',(69.5202900027367,-17.2025347343577,12.));
#54578=CARTESIAN_POINT('Ctrl Pts',(69.5434992642944,-17.2003937729268,0.));
#54579=CARTESIAN_POINT('Ctrl Pts',(69.5434992642944,-17.2003937729268,12.));
#54580=CARTESIAN_POINT('Ctrl Pts',(69.5667501379969,-17.1982257405377,0.));
#54581=CARTESIAN_POINT('Ctrl Pts',(69.5667501379969,-17.1982257405377,12.));
#54582=CARTESIAN_POINT('Ctrl Pts',(69.5900424904921,-17.196030584678,0.));
#54583=CARTESIAN_POINT('Ctrl Pts',(69.5900424904921,-17.196030584678,12.));
#54584=CARTESIAN_POINT('Ctrl Pts',(69.6133761889749,-17.1938082531612,0.));
#54585=CARTESIAN_POINT('Ctrl Pts',(69.6133761889749,-17.1938082531612,12.));
#54586=CARTESIAN_POINT('Ctrl Pts',(69.6367511011898,-17.1915586941192,0.));
#54587=CARTESIAN_POINT('Ctrl Pts',(69.6367511011898,-17.1915586941192,12.));
#54588=CARTESIAN_POINT('Ctrl Pts',(69.6601670954269,-17.1892818560002,0.));
#54589=CARTESIAN_POINT('Ctrl Pts',(69.6601670954269,-17.1892818560002,12.));
#54590=CARTESIAN_POINT('Ctrl Pts',(69.6836240405164,-17.1869776875666,0.));
#54591=CARTESIAN_POINT('Ctrl Pts',(69.6836240405164,-17.1869776875666,12.));
#54592=CARTESIAN_POINT('Ctrl Pts',(69.7071218058178,-17.1846461378973,0.));
#54593=CARTESIAN_POINT('Ctrl Pts',(69.7071218058178,-17.1846461378973,12.));
#54594=CARTESIAN_POINT('Ctrl Pts',(69.7306602612155,-17.1822871563842,0.));
#54595=CARTESIAN_POINT('Ctrl Pts',(69.7306602612155,-17.1822871563842,12.));
#54596=CARTESIAN_POINT('Ctrl Pts',(69.7542392771234,-17.179900692726,0.));
#54597=CARTESIAN_POINT('Ctrl Pts',(69.7542392771234,-17.179900692726,12.));
#54598=CARTESIAN_POINT('Ctrl Pts',(69.777858724479,-17.1774866969256,0.));
#54599=CARTESIAN_POINT('Ctrl Pts',(69.777858724479,-17.1774866969256,12.));
#54600=CARTESIAN_POINT('Ctrl Pts',(69.8015184747398,-17.1750451192885,0.));
#54601=CARTESIAN_POINT('Ctrl Pts',(69.8015184747398,-17.1750451192885,12.));
#54602=CARTESIAN_POINT('Ctrl Pts',(69.8252183998702,-17.1725759104252,0.));
#54603=CARTESIAN_POINT('Ctrl Pts',(69.8252183998702,-17.1725759104252,12.));
#54604=CARTESIAN_POINT('Ctrl Pts',(69.8489583723407,-17.1700790212473,0.));
#54605=CARTESIAN_POINT('Ctrl Pts',(69.8489583723407,-17.1700790212473,12.));
#54606=CARTESIAN_POINT('Ctrl Pts',(69.8727382651286,-17.167554402962,0.));
#54607=CARTESIAN_POINT('Ctrl Pts',(69.8727382651286,-17.167554402962,12.));
#54608=CARTESIAN_POINT('Ctrl Pts',(69.8965579517147,-17.1650020070686,0.));
#54609=CARTESIAN_POINT('Ctrl Pts',(69.8965579517147,-17.1650020070686,12.));
#54610=CARTESIAN_POINT('Ctrl Pts',(69.9204173060781,-17.1624217853578,0.));
#54611=CARTESIAN_POINT('Ctrl Pts',(69.9204173060781,-17.1624217853578,12.));
#54612=CARTESIAN_POINT('Ctrl Pts',(69.9443162026865,-17.1598136899144,0.));
#54613=CARTESIAN_POINT('Ctrl Pts',(69.9443162026865,-17.1598136899144,12.));
#54614=CARTESIAN_POINT('Ctrl Pts',(69.9682545164939,-17.157177673114,0.));
#54615=CARTESIAN_POINT('Ctrl Pts',(69.9682545164939,-17.157177673114,12.));
#54616=CARTESIAN_POINT('Ctrl Pts',(69.9922321229424,-17.154513687616,0.));
#54617=CARTESIAN_POINT('Ctrl Pts',(69.9922321229424,-17.154513687616,12.));
#54618=CARTESIAN_POINT('Ctrl Pts',(70.0162488979584,-17.1518216863623,0.));
#54619=CARTESIAN_POINT('Ctrl Pts',(70.0162488979584,-17.1518216863623,12.));
#54620=CARTESIAN_POINT('Ctrl Pts',(70.0403047179483,-17.1491016225749,0.));
#54621=CARTESIAN_POINT('Ctrl Pts',(70.0403047179483,-17.1491016225749,12.));
#54622=CARTESIAN_POINT('Ctrl Pts',(70.0643994597873,-17.1463534497594,0.));
#54623=CARTESIAN_POINT('Ctrl Pts',(70.0643994597873,-17.1463534497594,12.));
#54624=CARTESIAN_POINT('Ctrl Pts',(70.0885330008179,-17.1435771217018,0.));
#54625=CARTESIAN_POINT('Ctrl Pts',(70.0885330008179,-17.1435771217018,12.));
#54626=CARTESIAN_POINT('Ctrl Pts',(70.1127052188522,-17.1407725924617,0.));
#54627=CARTESIAN_POINT('Ctrl Pts',(70.1127052188522,-17.1407725924617,12.));
#54628=CARTESIAN_POINT('Ctrl Pts',(70.1369159921687,-17.1379398163709,0.));
#54629=CARTESIAN_POINT('Ctrl Pts',(70.1369159921687,-17.1379398163709,12.));
#54630=CARTESIAN_POINT('Ctrl Pts',(70.1611651995083,-17.1350787480312,0.));
#54631=CARTESIAN_POINT('Ctrl Pts',(70.1611651995083,-17.1350787480312,12.));
#54632=CARTESIAN_POINT('Ctrl Pts',(70.1854527200631,-17.1321893423182,0.));
#54633=CARTESIAN_POINT('Ctrl Pts',(70.1854527200631,-17.1321893423182,12.));
#54634=CARTESIAN_POINT('Ctrl Pts',(70.2097784334747,-17.1292715543778,0.));
#54635=CARTESIAN_POINT('Ctrl Pts',(70.2097784334747,-17.1292715543778,12.));
#54636=CARTESIAN_POINT('Ctrl Pts',(70.2341422198363,-17.1263253396202,0.));
#54637=CARTESIAN_POINT('Ctrl Pts',(70.2341422198363,-17.1263253396202,12.));
#54638=CARTESIAN_POINT('Ctrl Pts',(70.2585439596901,-17.1233506537176,0.));
#54639=CARTESIAN_POINT('Ctrl Pts',(70.2585439596901,-17.1233506537176,12.));
#54640=CARTESIAN_POINT('Ctrl Pts',(70.2829835340238,-17.1203474526031,0.));
#54641=CARTESIAN_POINT('Ctrl Pts',(70.2829835340238,-17.1203474526031,12.));
#54642=CARTESIAN_POINT('Ctrl Pts',(70.3074608242608,-17.1173156924733,0.));
#54643=CARTESIAN_POINT('Ctrl Pts',(70.3074608242608,-17.1173156924733,12.));
#54644=CARTESIAN_POINT('Ctrl Pts',(70.3319757122568,-17.1142553297867,0.));
#54645=CARTESIAN_POINT('Ctrl Pts',(70.3319757122568,-17.1142553297867,12.));
#54646=CARTESIAN_POINT('Ctrl Pts',(70.3565280803022,-17.1111663212568,0.));
#54647=CARTESIAN_POINT('Ctrl Pts',(70.3565280803022,-17.1111663212568,12.));
#54648=CARTESIAN_POINT('Ctrl Pts',(70.3811178111201,-17.1080486238499,0.));
#54649=CARTESIAN_POINT('Ctrl Pts',(70.3811178111201,-17.1080486238499,12.));
#54650=CARTESIAN_POINT('Ctrl Pts',(70.4057447878624,-17.1049021947834,0.));
#54651=CARTESIAN_POINT('Ctrl Pts',(70.4057447878624,-17.1049021947834,12.));
#54652=CARTESIAN_POINT('Ctrl Pts',(70.430408894101,-17.1017269915292,0.));
#54653=CARTESIAN_POINT('Ctrl Pts',(70.430408894101,-17.1017269915292,12.));
#54654=CARTESIAN_POINT('Ctrl Pts',(70.4551100138238,-17.0985229718124,0.));
#54655=CARTESIAN_POINT('Ctrl Pts',(70.4551100138238,-17.0985229718124,12.));
#54656=CARTESIAN_POINT('Ctrl Pts',(70.4798480314381,-17.0952900936048,0.));
#54657=CARTESIAN_POINT('Ctrl Pts',(70.4798480314381,-17.0952900936048,12.));
#54658=CARTESIAN_POINT('Ctrl Pts',(70.5046228317677,-17.0920283151219,0.));
#54659=CARTESIAN_POINT('Ctrl Pts',(70.5046228317677,-17.0920283151219,12.));
#54660=CARTESIAN_POINT('Ctrl Pts',(70.5294343000513,-17.088737594822,0.));
#54661=CARTESIAN_POINT('Ctrl Pts',(70.5294343000513,-17.088737594822,12.));
#54662=CARTESIAN_POINT('Ctrl Pts',(70.5542823219331,-17.0854178914087,0.));
#54663=CARTESIAN_POINT('Ctrl Pts',(70.5542823219331,-17.0854178914087,12.));
#54664=CARTESIAN_POINT('Ctrl Pts',(70.5791667834582,-17.082069163831,0.));
#54665=CARTESIAN_POINT('Ctrl Pts',(70.5791667834582,-17.082069163831,12.));
#54666=CARTESIAN_POINT('Ctrl Pts',(70.6040875710749,-17.0786913712763,0.));
#54667=CARTESIAN_POINT('Ctrl Pts',(70.6040875710749,-17.0786913712763,12.));
#54668=CARTESIAN_POINT('Ctrl Pts',(70.6290445716337,-17.0752844731678,0.));
#54669=CARTESIAN_POINT('Ctrl Pts',(70.6290445716337,-17.0752844731678,12.));
#54670=CARTESIAN_POINT('Ctrl Pts',(70.6540376723841,-17.0718484291624,0.));
#54671=CARTESIAN_POINT('Ctrl Pts',(70.6540376723841,-17.0718484291624,12.));
#54672=CARTESIAN_POINT('Ctrl Pts',(70.6790667609679,-17.0683831991532,0.));
#54673=CARTESIAN_POINT('Ctrl Pts',(70.6790667609679,-17.0683831991532,12.));
#54674=CARTESIAN_POINT('Ctrl Pts',(70.7041317254125,-17.0648887432713,0.));
#54675=CARTESIAN_POINT('Ctrl Pts',(70.7041317254125,-17.0648887432713,12.));
#54676=CARTESIAN_POINT('Ctrl Pts',(70.7292324541341,-17.0613650218787,0.));
#54677=CARTESIAN_POINT('Ctrl Pts',(70.7292324541341,-17.0613650218787,12.));
#54678=CARTESIAN_POINT('Ctrl Pts',(70.7543688359374,-17.0578119955649,0.));
#54679=CARTESIAN_POINT('Ctrl Pts',(70.7543688359374,-17.0578119955649,12.));
#54680=CARTESIAN_POINT('Ctrl Pts',(70.7795407600127,-17.0542296251462,0.));
#54681=CARTESIAN_POINT('Ctrl Pts',(70.7795407600127,-17.0542296251462,12.));
#54682=CARTESIAN_POINT('Ctrl Pts',(70.8047481159306,-17.0506178716664,0.));
#54683=CARTESIAN_POINT('Ctrl Pts',(70.8047481159306,-17.0506178716664,12.));
#54684=CARTESIAN_POINT('Ctrl Pts',(70.8299907936346,-17.0469766964005,0.));
#54685=CARTESIAN_POINT('Ctrl Pts',(70.8299907936346,-17.0469766964005,12.));
#54686=CARTESIAN_POINT('Ctrl Pts',(70.8552686834435,-17.0433060608478,0.));
#54687=CARTESIAN_POINT('Ctrl Pts',(70.8552686834435,-17.0433060608478,12.));
#54688=CARTESIAN_POINT('Ctrl Pts',(70.8805816760507,-17.0396059267279,0.));
#54689=CARTESIAN_POINT('Ctrl Pts',(70.8805816760507,-17.0396059267279,12.));
#54690=CARTESIAN_POINT('Ctrl Pts',(70.9059296625214,-17.0358762559786,0.));
#54691=CARTESIAN_POINT('Ctrl Pts',(70.9059296625214,-17.0358762559786,12.));
#54692=CARTESIAN_POINT('Ctrl Pts',(70.9313125342872,-17.0321170107562,0.));
#54693=CARTESIAN_POINT('Ctrl Pts',(70.9313125342872,-17.0321170107562,12.));
#54694=CARTESIAN_POINT('Ctrl Pts',(70.9567301831355,-17.028328153439,0.));
#54695=CARTESIAN_POINT('Ctrl Pts',(70.9567301831355,-17.028328153439,12.));
#54696=CARTESIAN_POINT('Ctrl Pts',(70.9821825012134,-17.0245096466228,0.));
#54697=CARTESIAN_POINT('Ctrl Pts',(70.9821825012134,-17.0245096466228,12.));
#54698=CARTESIAN_POINT('Ctrl Pts',(71.0076693810303,-17.0206614531165,0.));
#54699=CARTESIAN_POINT('Ctrl Pts',(71.0076693810303,-17.0206614531165,12.));
#54700=CARTESIAN_POINT('Ctrl Pts',(71.0331907154575,-17.0167835359419,0.));
#54701=CARTESIAN_POINT('Ctrl Pts',(71.0331907154575,-17.0167835359419,12.));
#54702=CARTESIAN_POINT('Ctrl Pts',(71.0587463977266,-17.0128758583335,0.));
#54703=CARTESIAN_POINT('Ctrl Pts',(71.0587463977266,-17.0128758583335,12.));
#54704=CARTESIAN_POINT('Ctrl Pts',(71.0843363214216,-17.0089383837437,0.));
#54705=CARTESIAN_POINT('Ctrl Pts',(71.0843363214216,-17.0089383837437,12.));
#54706=CARTESIAN_POINT('Ctrl Pts',(71.1099603804779,-17.0049710758393,0.));
#54707=CARTESIAN_POINT('Ctrl Pts',(71.1099603804779,-17.0049710758393,12.));
#54708=CARTESIAN_POINT('Ctrl Pts',(71.1356184691799,-17.0009738984935,0.));
#54709=CARTESIAN_POINT('Ctrl Pts',(71.1356184691799,-17.0009738984935,12.));
#54710=CARTESIAN_POINT('Ctrl Pts',(71.1613104821565,-16.9969468157824,0.));
#54711=CARTESIAN_POINT('Ctrl Pts',(71.1613104821565,-16.9969468157824,12.));
#54712=CARTESIAN_POINT('Ctrl Pts',(71.1870363143742,-16.9928897919829,0.));
#54713=CARTESIAN_POINT('Ctrl Pts',(71.1870363143742,-16.9928897919829,12.));
#54714=CARTESIAN_POINT('Ctrl Pts',(71.2127958611248,-16.9888027915743,0.));
#54715=CARTESIAN_POINT('Ctrl Pts',(71.2127958611248,-16.9888027915743,12.));
#54716=CARTESIAN_POINT('Ctrl Pts',(71.2385890180233,-16.9846857792385,0.));
#54717=CARTESIAN_POINT('Ctrl Pts',(71.2385890180233,-16.9846857792385,12.));
#54718=CARTESIAN_POINT('Ctrl Pts',(71.2644156810209,-16.9805387198573,0.));
#54719=CARTESIAN_POINT('Ctrl Pts',(71.2644156810209,-16.9805387198573,12.));
#54720=CARTESIAN_POINT('Ctrl Pts',(71.2902757464127,-16.9763615785138,0.));
#54721=CARTESIAN_POINT('Ctrl Pts',(71.2902757464127,-16.9763615785138,12.));
#54722=CARTESIAN_POINT('Ctrl Pts',(71.3161691108425,-16.9721543204951,0.));
#54723=CARTESIAN_POINT('Ctrl Pts',(71.3161691108425,-16.9721543204951,12.));
#54724=CARTESIAN_POINT('Ctrl Pts',(71.3420956713072,-16.9679169112993,0.));
#54725=CARTESIAN_POINT('Ctrl Pts',(71.3420956713072,-16.9679169112993,12.));
#54726=CARTESIAN_POINT('Ctrl Pts',(71.3680553251548,-16.9636493166395,0.));
#54727=CARTESIAN_POINT('Ctrl Pts',(71.3680553251548,-16.9636493166395,12.));
#54728=CARTESIAN_POINT('Ctrl Pts',(71.3940479700663,-16.9593515024274,0.));
#54729=CARTESIAN_POINT('Ctrl Pts',(71.3940479700663,-16.9593515024274,12.));
#54730=CARTESIAN_POINT('Ctrl Pts',(71.4200735040374,-16.9550234347619,0.));
#54731=CARTESIAN_POINT('Ctrl Pts',(71.4200735040374,-16.9550234347619,12.));
#54732=CARTESIAN_POINT('Ctrl Pts',(71.4461318253561,-16.9506650799188,0.));
#54733=CARTESIAN_POINT('Ctrl Pts',(71.4461318253561,-16.9506650799188,12.));
#54734=CARTESIAN_POINT('Ctrl Pts',(71.4722228325805,-16.9462764043445,0.));
#54735=CARTESIAN_POINT('Ctrl Pts',(71.4722228325805,-16.9462764043445,12.));
#54736=CARTESIAN_POINT('Ctrl Pts',(71.498346424507,-16.9418573746492,0.));
#54737=CARTESIAN_POINT('Ctrl Pts',(71.498346424507,-16.9418573746492,12.));
#54738=CARTESIAN_POINT('Ctrl Pts',(71.5245025002154,-16.9374079576204,0.));
#54739=CARTESIAN_POINT('Ctrl Pts',(71.5245025002154,-16.9374079576204,12.));
#54740=CARTESIAN_POINT('Ctrl Pts',(71.5506909591139,-16.9329281202379,0.));
#54741=CARTESIAN_POINT('Ctrl Pts',(71.5506909591139,-16.9329281202379,12.));
#54742=CARTESIAN_POINT('Ctrl Pts',(71.5769117009844,-16.9284178296934,0.));
#54743=CARTESIAN_POINT('Ctrl Pts',(71.5769117009844,-16.9284178296934,12.));
#54744=CARTESIAN_POINT('Ctrl Pts',(71.6031646260169,-16.923877053407,0.));
#54745=CARTESIAN_POINT('Ctrl Pts',(71.6031646260169,-16.923877053407,12.));
#54746=CARTESIAN_POINT('Ctrl Pts',(71.6294496348644,-16.9193057590605,0.));
#54747=CARTESIAN_POINT('Ctrl Pts',(71.6294496348644,-16.9193057590605,12.));
#54748=CARTESIAN_POINT('Ctrl Pts',(71.6557666285908,-16.9147039145715,0.));
#54749=CARTESIAN_POINT('Ctrl Pts',(71.6557666285908,-16.9147039145715,12.));
#54750=CARTESIAN_POINT('Ctrl Pts',(71.6821155085605,-16.9100714880367,0.));
#54751=CARTESIAN_POINT('Ctrl Pts',(71.6821155085605,-16.9100714880367,12.));
#54752=CARTESIAN_POINT('Ctrl Pts',(71.7084961763355,-16.9054084476847,0.));
#54753=CARTESIAN_POINT('Ctrl Pts',(71.7084961763355,-16.9054084476847,12.));
#54754=CARTESIAN_POINT('Ctrl Pts',(71.7349085335796,-16.9007147618344,0.));
#54755=CARTESIAN_POINT('Ctrl Pts',(71.7349085335796,-16.9007147618344,12.));
#54756=CARTESIAN_POINT('Ctrl Pts',(71.761352481924,-16.8959903988411,0.));
#54757=CARTESIAN_POINT('Ctrl Pts',(71.761352481924,-16.8959903988411,12.));
#54758=CARTESIAN_POINT('Ctrl Pts',(71.7878279229556,-16.8912353270944,0.));
#54759=CARTESIAN_POINT('Ctrl Pts',(71.7878279229556,-16.8912353270944,12.));
#54760=CARTESIAN_POINT('Ctrl Pts',(71.8143347584977,-16.8864495151347,0.));
#54761=CARTESIAN_POINT('Ctrl Pts',(71.8143347584977,-16.8864495151347,12.));
#54762=CARTESIAN_POINT('Ctrl Pts',(71.8408728908269,-16.8816329317473,0.));
#54763=CARTESIAN_POINT('Ctrl Pts',(71.8408728908269,-16.8816329317473,12.));
#54764=CARTESIAN_POINT('Ctrl Pts',(71.8674422229151,-16.87678554607,0.));
#54765=CARTESIAN_POINT('Ctrl Pts',(71.8674422229151,-16.87678554607,12.));
#54766=CARTESIAN_POINT('Ctrl Pts',(71.8940426586521,-16.8719073276967,0.));
#54767=CARTESIAN_POINT('Ctrl Pts',(71.8940426586521,-16.8719073276967,12.));
#54768=CARTESIAN_POINT('Ctrl Pts',(71.920674103086,-16.8669982467915,0.));
#54769=CARTESIAN_POINT('Ctrl Pts',(71.920674103086,-16.8669982467915,12.));
#54770=CARTESIAN_POINT('Ctrl Pts',(71.9473364618889,-16.8620582738431,0.));
#54771=CARTESIAN_POINT('Ctrl Pts',(71.9473364618889,-16.8620582738431,12.));
#54772=CARTESIAN_POINT('Ctrl Pts',(71.9740296408319,-16.8570873794264,0.));
#54773=CARTESIAN_POINT('Ctrl Pts',(71.9740296408319,-16.8570873794264,12.));
#54774=CARTESIAN_POINT('Ctrl Pts',(72.0007535452071,-16.8520855339444,0.));
#54775=CARTESIAN_POINT('Ctrl Pts',(72.0007535452071,-16.8520855339444,12.));
#54776=CARTESIAN_POINT('Ctrl Pts',(72.0275080793742,-16.8470527074278,0.));
#54777=CARTESIAN_POINT('Ctrl Pts',(72.0275080793742,-16.8470527074278,12.));
#54778=CARTESIAN_POINT('Ctrl Pts',(72.0542931459865,-16.8419888691984,0.));
#54779=CARTESIAN_POINT('Ctrl Pts',(72.0542931459865,-16.8419888691984,12.));
#54780=CARTESIAN_POINT('Ctrl Pts',(72.0811086466177,-16.8368939881457,0.));
#54781=CARTESIAN_POINT('Ctrl Pts',(72.0811086466177,-16.8368939881457,12.));
#54782=CARTESIAN_POINT('Ctrl Pts',(72.1079544831569,-16.8317680333415,0.));
#54783=CARTESIAN_POINT('Ctrl Pts',(72.1079544831569,-16.8317680333415,12.));
#54784=CARTESIAN_POINT('Ctrl Pts',(72.1348305590233,-16.8266109745801,0.));
#54785=CARTESIAN_POINT('Ctrl Pts',(72.1348305590233,-16.8266109745801,12.));
#54786=CARTESIAN_POINT('Ctrl Pts',(72.1617367803226,-16.8214227828941,0.));
#54787=CARTESIAN_POINT('Ctrl Pts',(72.1617367803226,-16.8214227828941,12.));
#54788=CARTESIAN_POINT('Ctrl Pts',(72.1886730573389,-16.8162034312257,0.));
#54789=CARTESIAN_POINT('Ctrl Pts',(72.1886730573389,-16.8162034312257,12.));
#54790=CARTESIAN_POINT('Ctrl Pts',(72.2156393048868,-16.8109528945876,0.));
#54791=CARTESIAN_POINT('Ctrl Pts',(72.2156393048868,-16.8109528945876,12.));
#54792=CARTESIAN_POINT('Ctrl Pts',(72.242635439009,-16.8056711485797,0.));
#54793=CARTESIAN_POINT('Ctrl Pts',(72.242635439009,-16.8056711485797,12.));
#54794=CARTESIAN_POINT('Ctrl Pts',(72.2696613743687,-16.800358168223,0.));
#54795=CARTESIAN_POINT('Ctrl Pts',(72.2696613743687,-16.800358168223,12.));
#54796=CARTESIAN_POINT('Ctrl Pts',(72.2967170212331,-16.7950139266117,0.));
#54797=CARTESIAN_POINT('Ctrl Pts',(72.2967170212331,-16.7950139266117,12.));
#54798=CARTESIAN_POINT('Ctrl Pts',(72.323802282931,-16.7896383937839,0.));
#54799=CARTESIAN_POINT('Ctrl Pts',(72.323802282931,-16.7896383937839,12.));
#54800=CARTESIAN_POINT('Ctrl Pts',(72.3509170523038,-16.7842315351401,0.));
#54801=CARTESIAN_POINT('Ctrl Pts',(72.3509170523038,-16.7842315351401,12.));
#54802=CARTESIAN_POINT('Ctrl Pts',(72.3780612168057,-16.7787933137551,0.));
#54803=CARTESIAN_POINT('Ctrl Pts',(72.3780612168057,-16.7787933137551,12.));
#54804=CARTESIAN_POINT('Ctrl Pts',(72.4052346648058,-16.7733236932185,0.));
#54805=CARTESIAN_POINT('Ctrl Pts',(72.4052346648058,-16.7733236932185,12.));
#54806=CARTESIAN_POINT('Ctrl Pts',(72.4324372916884,-16.7678226404189,0.));
#54807=CARTESIAN_POINT('Ctrl Pts',(72.4324372916884,-16.7678226404189,12.));
#54808=CARTESIAN_POINT('Ctrl Pts',(72.4596690055347,-16.7622901280741,0.));
#54809=CARTESIAN_POINT('Ctrl Pts',(72.4596690055347,-16.7622901280741,12.));
#54810=CARTESIAN_POINT('Ctrl Pts',(72.4869297342051,-16.7567261380614,0.));
#54811=CARTESIAN_POINT('Ctrl Pts',(72.4869297342051,-16.7567261380614,12.));
#54812=CARTESIAN_POINT('Ctrl Pts',(72.5142194273203,-16.7511306618793,0.));
#54813=CARTESIAN_POINT('Ctrl Pts',(72.5142194273203,-16.7511306618793,12.));
#54814=CARTESIAN_POINT('Ctrl Pts',(72.5415380515905,-16.7455036973724,0.));
#54815=CARTESIAN_POINT('Ctrl Pts',(72.5415380515905,-16.7455036973724,12.));
#54816=CARTESIAN_POINT('Ctrl Pts',(72.563416080574,-16.7409769365953,0.));
#54817=CARTESIAN_POINT('Ctrl Pts',(72.563416080574,-16.7409769365953,12.));
#54818=CARTESIAN_POINT('Ctrl Pts',(72.5798376087406,-16.7375676985272,0.));
#54819=CARTESIAN_POINT('Ctrl Pts',(72.5798376087406,-16.7375676985272,12.));
#54820=CARTESIAN_POINT('Ctrl Pts',(72.5907910745874,-16.7352885767459,0.));
#54821=CARTESIAN_POINT('Ctrl Pts',(72.5907910745874,-16.7352885767459,12.));
#54822=CARTESIAN_POINT('Ctrl Pts',(72.5962692526112,-16.7341474417544,0.));
#54823=CARTESIAN_POINT('Ctrl Pts',(72.5962692526112,-16.7341474417544,12.));
#54824=CARTESIAN_POINT('',(67.8307641965655,-17.2912529479484,0.));
#54825=CARTESIAN_POINT('Ctrl Pts',(67.8307641965655,-17.2912529479484,0.));
#54826=CARTESIAN_POINT('Ctrl Pts',(67.8346476309018,-17.2912149114119,0.));
#54827=CARTESIAN_POINT('Ctrl Pts',(67.842419897098,-17.2911366591348,0.));
#54828=CARTESIAN_POINT('Ctrl Pts',(67.8540944889687,-17.291012743109,0.));
#54829=CARTESIAN_POINT('Ctrl Pts',(67.8696929978782,-17.2908344459694,0.));
#54830=CARTESIAN_POINT('Ctrl Pts',(67.8892451049608,-17.2905897723948,0.));
#54831=CARTESIAN_POINT('Ctrl Pts',(67.9088511496686,-17.2903232740694,0.));
#54832=CARTESIAN_POINT('Ctrl Pts',(67.9285110571741,-17.2900349103981,0.));
#54833=CARTESIAN_POINT('Ctrl Pts',(67.9482246901667,-17.2897246158941,0.));
#54834=CARTESIAN_POINT('Ctrl Pts',(67.9679918502579,-17.2893923013894,0.));
#54835=CARTESIAN_POINT('Ctrl Pts',(67.987812304921,-17.2890378644866,0.));
#54836=CARTESIAN_POINT('Ctrl Pts',(68.007685808115,-17.28866119774,0.));
#54837=CARTESIAN_POINT('Ctrl Pts',(68.0276121227356,-17.2882621974721,0.));
#54838=CARTESIAN_POINT('Ctrl Pts',(68.0475910442424,-17.2878407730961,0.));
#54839=CARTESIAN_POINT('Ctrl Pts',(68.0676223930412,-17.2873968440839,0.));
#54840=CARTESIAN_POINT('Ctrl Pts',(68.0877060033205,-17.2869303355432,0.));
#54841=CARTESIAN_POINT('Ctrl Pts',(68.1078417137877,-17.2864411745459,0.));
#54842=CARTESIAN_POINT('Ctrl Pts',(68.1280293561511,-17.2859292855705,0.));
#54843=CARTESIAN_POINT('Ctrl Pts',(68.1482687493226,-17.2853945882072,0.));
#54844=CARTESIAN_POINT('Ctrl Pts',(68.1685597054232,-17.2848369995293,0.));
#54845=CARTESIAN_POINT('Ctrl Pts',(68.1889020335427,-17.2842564355799,0.));
#54846=CARTESIAN_POINT('Ctrl Pts',(68.2092955440567,-17.2836528130819,0.));
#54847=CARTESIAN_POINT('Ctrl Pts',(68.2297400535294,-17.2830260513867,0.));
#54848=CARTESIAN_POINT('Ctrl Pts',(68.2502353845071,-17.2823760723874,0.));
#54849=CARTESIAN_POINT('Ctrl Pts',(68.2707813631731,-17.2817027995831,0.));
#54850=CARTESIAN_POINT('Ctrl Pts',(68.2913778177261,-17.2810061574353,0.));
#54851=CARTESIAN_POINT('Ctrl Pts',(68.3120245763914,-17.2802860705815,0.));
#54852=CARTESIAN_POINT('Ctrl Pts',(68.3327214657575,-17.2795424631799,0.));
#54853=CARTESIAN_POINT('Ctrl Pts',(68.3534683116515,-17.2787752592484,0.));
#54854=CARTESIAN_POINT('Ctrl Pts',(68.3742649398964,-17.2779843829608,0.));
#54855=CARTESIAN_POINT('Ctrl Pts',(68.3951111770487,-17.2771697589384,0.));
#54856=CARTESIAN_POINT('Ctrl Pts',(68.4160068512753,-17.2763313126018,0.));
#54857=CARTESIAN_POINT('Ctrl Pts',(68.436951792677,-17.2754689702992,0.));
#54858=CARTESIAN_POINT('Ctrl Pts',(68.4579458328185,-17.2745826591119,0.));
#54859=CARTESIAN_POINT('Ctrl Pts',(68.4789888044351,-17.2736723067365,0.));
#54860=CARTESIAN_POINT('Ctrl Pts',(68.5000805410911,-17.2727378413489,0.));
#54861=CARTESIAN_POINT('Ctrl Pts',(68.521220876786,-17.2717791914544,0.));
#54862=CARTESIAN_POINT('Ctrl Pts',(68.5424096459772,-17.2707962858919,0.));
#54863=CARTESIAN_POINT('Ctrl Pts',(68.5636466837517,-17.269789053896,0.));
#54864=CARTESIAN_POINT('Ctrl Pts',(68.5849318259449,-17.2687574251428,0.));
#54865=CARTESIAN_POINT('Ctrl Pts',(68.6062649092764,-17.2677013298057,0.));
#54866=CARTESIAN_POINT('Ctrl Pts',(68.6276457714729,-17.2666206986084,0.));
#54867=CARTESIAN_POINT('Ctrl Pts',(68.6490742512057,-17.2655154627928,0.));
#54868=CARTESIAN_POINT('Ctrl Pts',(68.6705501880249,-17.2643855540892,0.));
#54869=CARTESIAN_POINT('Ctrl Pts',(68.6920734222938,-17.2632309046892,0.));
#54870=CARTESIAN_POINT('Ctrl Pts',(68.7136437951097,-17.2620514472182,0.));
#54871=CARTESIAN_POINT('Ctrl Pts',(68.7352611482547,-17.2608471147185,0.));
#54872=CARTESIAN_POINT('Ctrl Pts',(68.7569253242333,-17.259617840655,0.));
#54873=CARTESIAN_POINT('Ctrl Pts',(68.7786361662882,-17.2583635589198,0.));
#54874=CARTESIAN_POINT('Ctrl Pts',(68.8003935184184,-17.2570842038383,0.));
#54875=CARTESIAN_POINT('Ctrl Pts',(68.8221972253941,-17.2557797101812,0.));
#54876=CARTESIAN_POINT('Ctrl Pts',(68.844047132755,-17.2544500131624,0.));
#54877=CARTESIAN_POINT('Ctrl Pts',(68.8659430867972,-17.2530950484258,0.));
#54878=CARTESIAN_POINT('Ctrl Pts',(68.8878849345557,-17.2517147520376,0.));
#54879=CARTESIAN_POINT('Ctrl Pts',(68.909872523787,-17.2503090604792,0.));
#54880=CARTESIAN_POINT('Ctrl Pts',(68.9319057029409,-17.248877910643,0.));
#54881=CARTESIAN_POINT('Ctrl Pts',(68.9539843211619,-17.2474212398275,0.));
#54882=CARTESIAN_POINT('Ctrl Pts',(68.9761082282922,-17.2459389857327,0.));
#54883=CARTESIAN_POINT('Ctrl Pts',(68.9982772748694,-17.2444310864585,0.));
#54884=CARTESIAN_POINT('Ctrl Pts',(69.0204913121225,-17.2428974805044,0.));
#54885=CARTESIAN_POINT('Ctrl Pts',(69.0427501919636,-17.2413381067723,0.));
#54886=CARTESIAN_POINT('Ctrl Pts',(69.065053766986,-17.2397529045589,0.));
#54887=CARTESIAN_POINT('Ctrl Pts',(69.0874018904599,-17.2381418135491,0.));
#54888=CARTESIAN_POINT('Ctrl Pts',(69.1097944163245,-17.2365047738125,0.));
#54889=CARTESIAN_POINT('Ctrl Pts',(69.1322311991752,-17.2348417258015,0.));
#54890=CARTESIAN_POINT('Ctrl Pts',(69.1547120942527,-17.2331526103506,0.));
#54891=CARTESIAN_POINT('Ctrl Pts',(69.1772369574447,-17.23143736867,0.));
#54892=CARTESIAN_POINT('Ctrl Pts',(69.1998056452828,-17.2296959423407,0.));
#54893=CARTESIAN_POINT('Ctrl Pts',(69.222418014938,-17.227928273312,0.));
#54894=CARTESIAN_POINT('Ctrl Pts',(69.2450739242109,-17.226134303902,0.));
#54895=CARTESIAN_POINT('Ctrl Pts',(69.2677732315224,-17.224313976797,0.));
#54896=CARTESIAN_POINT('Ctrl Pts',(69.2905157959166,-17.2224672350438,0.));
#54897=CARTESIAN_POINT('Ctrl Pts',(69.3133014770555,-17.2205940220459,0.));
#54898=CARTESIAN_POINT('Ctrl Pts',(69.3361301352141,-17.2186942815602,0.));
#54899=CARTESIAN_POINT('Ctrl Pts',(69.3590016312692,-17.2167679576984,0.));
#54900=CARTESIAN_POINT('Ctrl Pts',(69.3819158266916,-17.2148149949252,0.));
#54901=CARTESIAN_POINT('Ctrl Pts',(69.404872583548,-17.2128353380502,0.));
#54902=CARTESIAN_POINT('Ctrl Pts',(69.4278717644973,-17.2108289322254,0.));
#54903=CARTESIAN_POINT('Ctrl Pts',(69.450913232785,-17.2087957229423,0.));
#54904=CARTESIAN_POINT('Ctrl Pts',(69.4739968522313,-17.2067356560336,0.));
#54905=CARTESIAN_POINT('Ctrl Pts',(69.4971224872269,-17.2046486776708,0.));
#54906=CARTESIAN_POINT('Ctrl Pts',(69.5202900027367,-17.2025347343577,0.));
#54907=CARTESIAN_POINT('Ctrl Pts',(69.5434992642944,-17.2003937729268,0.));
#54908=CARTESIAN_POINT('Ctrl Pts',(69.5667501379969,-17.1982257405377,0.));
#54909=CARTESIAN_POINT('Ctrl Pts',(69.5900424904921,-17.196030584678,0.));
#54910=CARTESIAN_POINT('Ctrl Pts',(69.6133761889749,-17.1938082531612,0.));
#54911=CARTESIAN_POINT('Ctrl Pts',(69.6367511011898,-17.1915586941192,0.));
#54912=CARTESIAN_POINT('Ctrl Pts',(69.6601670954269,-17.1892818560002,0.));
#54913=CARTESIAN_POINT('Ctrl Pts',(69.6836240405164,-17.1869776875666,0.));
#54914=CARTESIAN_POINT('Ctrl Pts',(69.7071218058178,-17.1846461378973,0.));
#54915=CARTESIAN_POINT('Ctrl Pts',(69.7306602612155,-17.1822871563842,0.));
#54916=CARTESIAN_POINT('Ctrl Pts',(69.7542392771234,-17.179900692726,0.));
#54917=CARTESIAN_POINT('Ctrl Pts',(69.777858724479,-17.1774866969256,0.));
#54918=CARTESIAN_POINT('Ctrl Pts',(69.8015184747398,-17.1750451192885,0.));
#54919=CARTESIAN_POINT('Ctrl Pts',(69.8252183998702,-17.1725759104252,0.));
#54920=CARTESIAN_POINT('Ctrl Pts',(69.8489583723407,-17.1700790212473,0.));
#54921=CARTESIAN_POINT('Ctrl Pts',(69.8727382651286,-17.167554402962,0.));
#54922=CARTESIAN_POINT('Ctrl Pts',(69.8965579517147,-17.1650020070686,0.));
#54923=CARTESIAN_POINT('Ctrl Pts',(69.9204173060781,-17.1624217853578,0.));
#54924=CARTESIAN_POINT('Ctrl Pts',(69.9443162026865,-17.1598136899144,0.));
#54925=CARTESIAN_POINT('Ctrl Pts',(69.9682545164939,-17.157177673114,0.));
#54926=CARTESIAN_POINT('Ctrl Pts',(69.9922321229424,-17.154513687616,0.));
#54927=CARTESIAN_POINT('Ctrl Pts',(70.0162488979584,-17.1518216863623,0.));
#54928=CARTESIAN_POINT('Ctrl Pts',(70.0403047179483,-17.1491016225749,0.));
#54929=CARTESIAN_POINT('Ctrl Pts',(70.0643994597873,-17.1463534497594,0.));
#54930=CARTESIAN_POINT('Ctrl Pts',(70.0885330008179,-17.1435771217018,0.));
#54931=CARTESIAN_POINT('Ctrl Pts',(70.1127052188522,-17.1407725924617,0.));
#54932=CARTESIAN_POINT('Ctrl Pts',(70.1369159921687,-17.1379398163709,0.));
#54933=CARTESIAN_POINT('Ctrl Pts',(70.1611651995083,-17.1350787480312,0.));
#54934=CARTESIAN_POINT('Ctrl Pts',(70.1854527200631,-17.1321893423182,0.));
#54935=CARTESIAN_POINT('Ctrl Pts',(70.2097784334747,-17.1292715543778,0.));
#54936=CARTESIAN_POINT('Ctrl Pts',(70.2341422198363,-17.1263253396202,0.));
#54937=CARTESIAN_POINT('Ctrl Pts',(70.2585439596901,-17.1233506537176,0.));
#54938=CARTESIAN_POINT('Ctrl Pts',(70.2829835340238,-17.1203474526031,0.));
#54939=CARTESIAN_POINT('Ctrl Pts',(70.3074608242608,-17.1173156924733,0.));
#54940=CARTESIAN_POINT('Ctrl Pts',(70.3319757122568,-17.1142553297867,0.));
#54941=CARTESIAN_POINT('Ctrl Pts',(70.3565280803022,-17.1111663212568,0.));
#54942=CARTESIAN_POINT('Ctrl Pts',(70.3811178111201,-17.1080486238499,0.));
#54943=CARTESIAN_POINT('Ctrl Pts',(70.4057447878624,-17.1049021947834,0.));
#54944=CARTESIAN_POINT('Ctrl Pts',(70.430408894101,-17.1017269915292,0.));
#54945=CARTESIAN_POINT('Ctrl Pts',(70.4551100138238,-17.0985229718124,0.));
#54946=CARTESIAN_POINT('Ctrl Pts',(70.4798480314381,-17.0952900936048,0.));
#54947=CARTESIAN_POINT('Ctrl Pts',(70.5046228317677,-17.0920283151219,0.));
#54948=CARTESIAN_POINT('Ctrl Pts',(70.5294343000513,-17.088737594822,0.));
#54949=CARTESIAN_POINT('Ctrl Pts',(70.5542823219331,-17.0854178914087,0.));
#54950=CARTESIAN_POINT('Ctrl Pts',(70.5791667834582,-17.082069163831,0.));
#54951=CARTESIAN_POINT('Ctrl Pts',(70.6040875710749,-17.0786913712763,0.));
#54952=CARTESIAN_POINT('Ctrl Pts',(70.6290445716337,-17.0752844731678,0.));
#54953=CARTESIAN_POINT('Ctrl Pts',(70.6540376723841,-17.0718484291624,0.));
#54954=CARTESIAN_POINT('Ctrl Pts',(70.6790667609679,-17.0683831991532,0.));
#54955=CARTESIAN_POINT('Ctrl Pts',(70.7041317254125,-17.0648887432713,0.));
#54956=CARTESIAN_POINT('Ctrl Pts',(70.7292324541341,-17.0613650218787,0.));
#54957=CARTESIAN_POINT('Ctrl Pts',(70.7543688359374,-17.0578119955649,0.));
#54958=CARTESIAN_POINT('Ctrl Pts',(70.7795407600127,-17.0542296251462,0.));
#54959=CARTESIAN_POINT('Ctrl Pts',(70.8047481159306,-17.0506178716664,0.));
#54960=CARTESIAN_POINT('Ctrl Pts',(70.8299907936346,-17.0469766964005,0.));
#54961=CARTESIAN_POINT('Ctrl Pts',(70.8552686834435,-17.0433060608478,0.));
#54962=CARTESIAN_POINT('Ctrl Pts',(70.8805816760507,-17.0396059267279,0.));
#54963=CARTESIAN_POINT('Ctrl Pts',(70.9059296625214,-17.0358762559786,0.));
#54964=CARTESIAN_POINT('Ctrl Pts',(70.9313125342872,-17.0321170107562,0.));
#54965=CARTESIAN_POINT('Ctrl Pts',(70.9567301831355,-17.028328153439,0.));
#54966=CARTESIAN_POINT('Ctrl Pts',(70.9821825012134,-17.0245096466228,0.));
#54967=CARTESIAN_POINT('Ctrl Pts',(71.0076693810303,-17.0206614531165,0.));
#54968=CARTESIAN_POINT('Ctrl Pts',(71.0331907154575,-17.0167835359419,0.));
#54969=CARTESIAN_POINT('Ctrl Pts',(71.0587463977266,-17.0128758583335,0.));
#54970=CARTESIAN_POINT('Ctrl Pts',(71.0843363214216,-17.0089383837437,0.));
#54971=CARTESIAN_POINT('Ctrl Pts',(71.1099603804779,-17.0049710758393,0.));
#54972=CARTESIAN_POINT('Ctrl Pts',(71.1356184691799,-17.0009738984935,0.));
#54973=CARTESIAN_POINT('Ctrl Pts',(71.1613104821565,-16.9969468157824,0.));
#54974=CARTESIAN_POINT('Ctrl Pts',(71.1870363143742,-16.9928897919829,0.));
#54975=CARTESIAN_POINT('Ctrl Pts',(71.2127958611248,-16.9888027915743,0.));
#54976=CARTESIAN_POINT('Ctrl Pts',(71.2385890180233,-16.9846857792385,0.));
#54977=CARTESIAN_POINT('Ctrl Pts',(71.2644156810209,-16.9805387198573,0.));
#54978=CARTESIAN_POINT('Ctrl Pts',(71.2902757464127,-16.9763615785138,0.));
#54979=CARTESIAN_POINT('Ctrl Pts',(71.3161691108425,-16.9721543204951,0.));
#54980=CARTESIAN_POINT('Ctrl Pts',(71.3420956713072,-16.9679169112993,0.));
#54981=CARTESIAN_POINT('Ctrl Pts',(71.3680553251548,-16.9636493166395,0.));
#54982=CARTESIAN_POINT('Ctrl Pts',(71.3940479700663,-16.9593515024274,0.));
#54983=CARTESIAN_POINT('Ctrl Pts',(71.4200735040374,-16.9550234347619,0.));
#54984=CARTESIAN_POINT('Ctrl Pts',(71.4461318253561,-16.9506650799188,0.));
#54985=CARTESIAN_POINT('Ctrl Pts',(71.4722228325805,-16.9462764043445,0.));
#54986=CARTESIAN_POINT('Ctrl Pts',(71.498346424507,-16.9418573746492,0.));
#54987=CARTESIAN_POINT('Ctrl Pts',(71.5245025002154,-16.9374079576204,0.));
#54988=CARTESIAN_POINT('Ctrl Pts',(71.5506909591139,-16.9329281202379,0.));
#54989=CARTESIAN_POINT('Ctrl Pts',(71.5769117009844,-16.9284178296934,0.));
#54990=CARTESIAN_POINT('Ctrl Pts',(71.6031646260169,-16.923877053407,0.));
#54991=CARTESIAN_POINT('Ctrl Pts',(71.6294496348644,-16.9193057590605,0.));
#54992=CARTESIAN_POINT('Ctrl Pts',(71.6557666285908,-16.9147039145715,0.));
#54993=CARTESIAN_POINT('Ctrl Pts',(71.6821155085605,-16.9100714880367,0.));
#54994=CARTESIAN_POINT('Ctrl Pts',(71.7084961763355,-16.9054084476847,0.));
#54995=CARTESIAN_POINT('Ctrl Pts',(71.7349085335796,-16.9007147618344,0.));
#54996=CARTESIAN_POINT('Ctrl Pts',(71.761352481924,-16.8959903988411,0.));
#54997=CARTESIAN_POINT('Ctrl Pts',(71.7878279229556,-16.8912353270944,0.));
#54998=CARTESIAN_POINT('Ctrl Pts',(71.8143347584977,-16.8864495151347,0.));
#54999=CARTESIAN_POINT('Ctrl Pts',(71.8408728908269,-16.8816329317473,0.));
#55000=CARTESIAN_POINT('Ctrl Pts',(71.8674422229151,-16.87678554607,0.));
#55001=CARTESIAN_POINT('Ctrl Pts',(71.8940426586521,-16.8719073276967,0.));
#55002=CARTESIAN_POINT('Ctrl Pts',(71.920674103086,-16.8669982467915,0.));
#55003=CARTESIAN_POINT('Ctrl Pts',(71.9473364618889,-16.8620582738431,0.));
#55004=CARTESIAN_POINT('Ctrl Pts',(71.9740296408319,-16.8570873794264,0.));
#55005=CARTESIAN_POINT('Ctrl Pts',(72.0007535452071,-16.8520855339444,0.));
#55006=CARTESIAN_POINT('Ctrl Pts',(72.0275080793742,-16.8470527074278,0.));
#55007=CARTESIAN_POINT('Ctrl Pts',(72.0542931459865,-16.8419888691984,0.));
#55008=CARTESIAN_POINT('Ctrl Pts',(72.0811086466177,-16.8368939881457,0.));
#55009=CARTESIAN_POINT('Ctrl Pts',(72.1079544831569,-16.8317680333415,0.));
#55010=CARTESIAN_POINT('Ctrl Pts',(72.1348305590233,-16.8266109745801,0.));
#55011=CARTESIAN_POINT('Ctrl Pts',(72.1617367803226,-16.8214227828941,0.));
#55012=CARTESIAN_POINT('Ctrl Pts',(72.1886730573389,-16.8162034312257,0.));
#55013=CARTESIAN_POINT('Ctrl Pts',(72.2156393048868,-16.8109528945876,0.));
#55014=CARTESIAN_POINT('Ctrl Pts',(72.2387802230664,-16.8064254147766,0.));
#55015=CARTESIAN_POINT('Ctrl Pts',(72.2565380035009,-16.8029374213801,0.));
#55016=CARTESIAN_POINT('Ctrl Pts',(72.2688994294962,-16.8005027425888,0.));
#55017=CARTESIAN_POINT('Ctrl Pts',(72.2758557890971,-16.7991305317792,0.));
#55018=CARTESIAN_POINT('Ctrl Pts',(72.2774028393488,-16.7988252568806,0.));
#55019=CARTESIAN_POINT('',(67.8307641965655,-17.2912529479484,12.));
#55020=CARTESIAN_POINT('',(67.8307641965655,-17.2912529479484,0.));
#55021=CARTESIAN_POINT('Ctrl Pts',(72.2774028393489,-16.7988252568806,12.));
#55022=CARTESIAN_POINT('Ctrl Pts',(72.2758557890971,-16.7991305317792,12.));
#55023=CARTESIAN_POINT('Ctrl Pts',(72.2688994294962,-16.8005027425888,12.));
#55024=CARTESIAN_POINT('Ctrl Pts',(72.2565380035009,-16.8029374213801,12.));
#55025=CARTESIAN_POINT('Ctrl Pts',(72.2387802230664,-16.8064254147766,12.));
#55026=CARTESIAN_POINT('Ctrl Pts',(72.2156393048868,-16.8109528945876,12.));
#55027=CARTESIAN_POINT('Ctrl Pts',(72.1886730573389,-16.8162034312257,12.));
#55028=CARTESIAN_POINT('Ctrl Pts',(72.1617367803226,-16.8214227828941,12.));
#55029=CARTESIAN_POINT('Ctrl Pts',(72.1348305590233,-16.8266109745801,12.));
#55030=CARTESIAN_POINT('Ctrl Pts',(72.1079544831569,-16.8317680333415,12.));
#55031=CARTESIAN_POINT('Ctrl Pts',(72.0811086466177,-16.8368939881457,12.));
#55032=CARTESIAN_POINT('Ctrl Pts',(72.0542931459865,-16.8419888691984,12.));
#55033=CARTESIAN_POINT('Ctrl Pts',(72.0275080793742,-16.8470527074278,12.));
#55034=CARTESIAN_POINT('Ctrl Pts',(72.0007535452071,-16.8520855339444,12.));
#55035=CARTESIAN_POINT('Ctrl Pts',(71.9740296408319,-16.8570873794264,12.));
#55036=CARTESIAN_POINT('Ctrl Pts',(71.9473364618889,-16.8620582738431,12.));
#55037=CARTESIAN_POINT('Ctrl Pts',(71.920674103086,-16.8669982467915,12.));
#55038=CARTESIAN_POINT('Ctrl Pts',(71.8940426586521,-16.8719073276967,12.));
#55039=CARTESIAN_POINT('Ctrl Pts',(71.8674422229151,-16.87678554607,12.));
#55040=CARTESIAN_POINT('Ctrl Pts',(71.8408728908269,-16.8816329317473,12.));
#55041=CARTESIAN_POINT('Ctrl Pts',(71.8143347584977,-16.8864495151347,12.));
#55042=CARTESIAN_POINT('Ctrl Pts',(71.7878279229556,-16.8912353270944,12.));
#55043=CARTESIAN_POINT('Ctrl Pts',(71.761352481924,-16.8959903988411,12.));
#55044=CARTESIAN_POINT('Ctrl Pts',(71.7349085335796,-16.9007147618344,12.));
#55045=CARTESIAN_POINT('Ctrl Pts',(71.7084961763355,-16.9054084476847,12.));
#55046=CARTESIAN_POINT('Ctrl Pts',(71.6821155085605,-16.9100714880367,12.));
#55047=CARTESIAN_POINT('Ctrl Pts',(71.6557666285908,-16.9147039145715,12.));
#55048=CARTESIAN_POINT('Ctrl Pts',(71.6294496348644,-16.9193057590605,12.));
#55049=CARTESIAN_POINT('Ctrl Pts',(71.6031646260169,-16.923877053407,12.));
#55050=CARTESIAN_POINT('Ctrl Pts',(71.5769117009844,-16.9284178296934,12.));
#55051=CARTESIAN_POINT('Ctrl Pts',(71.5506909591139,-16.9329281202379,12.));
#55052=CARTESIAN_POINT('Ctrl Pts',(71.5245025002154,-16.9374079576204,12.));
#55053=CARTESIAN_POINT('Ctrl Pts',(71.498346424507,-16.9418573746492,12.));
#55054=CARTESIAN_POINT('Ctrl Pts',(71.4722228325805,-16.9462764043445,12.));
#55055=CARTESIAN_POINT('Ctrl Pts',(71.4461318253561,-16.9506650799188,12.));
#55056=CARTESIAN_POINT('Ctrl Pts',(71.4200735040374,-16.9550234347619,12.));
#55057=CARTESIAN_POINT('Ctrl Pts',(71.3940479700663,-16.9593515024274,12.));
#55058=CARTESIAN_POINT('Ctrl Pts',(71.3680553251548,-16.9636493166395,12.));
#55059=CARTESIAN_POINT('Ctrl Pts',(71.3420956713072,-16.9679169112993,12.));
#55060=CARTESIAN_POINT('Ctrl Pts',(71.3161691108425,-16.9721543204951,12.));
#55061=CARTESIAN_POINT('Ctrl Pts',(71.2902757464127,-16.9763615785138,12.));
#55062=CARTESIAN_POINT('Ctrl Pts',(71.2644156810209,-16.9805387198573,12.));
#55063=CARTESIAN_POINT('Ctrl Pts',(71.2385890180233,-16.9846857792385,12.));
#55064=CARTESIAN_POINT('Ctrl Pts',(71.2127958611248,-16.9888027915743,12.));
#55065=CARTESIAN_POINT('Ctrl Pts',(71.1870363143742,-16.9928897919829,12.));
#55066=CARTESIAN_POINT('Ctrl Pts',(71.1613104821565,-16.9969468157824,12.));
#55067=CARTESIAN_POINT('Ctrl Pts',(71.1356184691799,-17.0009738984935,12.));
#55068=CARTESIAN_POINT('Ctrl Pts',(71.1099603804779,-17.0049710758393,12.));
#55069=CARTESIAN_POINT('Ctrl Pts',(71.0843363214216,-17.0089383837437,12.));
#55070=CARTESIAN_POINT('Ctrl Pts',(71.0587463977266,-17.0128758583335,12.));
#55071=CARTESIAN_POINT('Ctrl Pts',(71.0331907154575,-17.0167835359419,12.));
#55072=CARTESIAN_POINT('Ctrl Pts',(71.0076693810303,-17.0206614531165,12.));
#55073=CARTESIAN_POINT('Ctrl Pts',(70.9821825012134,-17.0245096466228,12.));
#55074=CARTESIAN_POINT('Ctrl Pts',(70.9567301831355,-17.028328153439,12.));
#55075=CARTESIAN_POINT('Ctrl Pts',(70.9313125342872,-17.0321170107562,12.));
#55076=CARTESIAN_POINT('Ctrl Pts',(70.9059296625214,-17.0358762559786,12.));
#55077=CARTESIAN_POINT('Ctrl Pts',(70.8805816760507,-17.0396059267279,12.));
#55078=CARTESIAN_POINT('Ctrl Pts',(70.8552686834435,-17.0433060608478,12.));
#55079=CARTESIAN_POINT('Ctrl Pts',(70.8299907936346,-17.0469766964005,12.));
#55080=CARTESIAN_POINT('Ctrl Pts',(70.8047481159306,-17.0506178716664,12.));
#55081=CARTESIAN_POINT('Ctrl Pts',(70.7795407600127,-17.0542296251462,12.));
#55082=CARTESIAN_POINT('Ctrl Pts',(70.7543688359374,-17.0578119955649,12.));
#55083=CARTESIAN_POINT('Ctrl Pts',(70.7292324541341,-17.0613650218787,12.));
#55084=CARTESIAN_POINT('Ctrl Pts',(70.7041317254125,-17.0648887432713,12.));
#55085=CARTESIAN_POINT('Ctrl Pts',(70.6790667609679,-17.0683831991532,12.));
#55086=CARTESIAN_POINT('Ctrl Pts',(70.6540376723841,-17.0718484291624,12.));
#55087=CARTESIAN_POINT('Ctrl Pts',(70.6290445716337,-17.0752844731678,12.));
#55088=CARTESIAN_POINT('Ctrl Pts',(70.6040875710749,-17.0786913712763,12.));
#55089=CARTESIAN_POINT('Ctrl Pts',(70.5791667834582,-17.082069163831,12.));
#55090=CARTESIAN_POINT('Ctrl Pts',(70.5542823219331,-17.0854178914087,12.));
#55091=CARTESIAN_POINT('Ctrl Pts',(70.5294343000513,-17.088737594822,12.));
#55092=CARTESIAN_POINT('Ctrl Pts',(70.5046228317677,-17.0920283151219,12.));
#55093=CARTESIAN_POINT('Ctrl Pts',(70.4798480314381,-17.0952900936048,12.));
#55094=CARTESIAN_POINT('Ctrl Pts',(70.4551100138238,-17.0985229718124,12.));
#55095=CARTESIAN_POINT('Ctrl Pts',(70.430408894101,-17.1017269915292,12.));
#55096=CARTESIAN_POINT('Ctrl Pts',(70.4057447878624,-17.1049021947834,12.));
#55097=CARTESIAN_POINT('Ctrl Pts',(70.3811178111201,-17.1080486238499,12.));
#55098=CARTESIAN_POINT('Ctrl Pts',(70.3565280803022,-17.1111663212568,12.));
#55099=CARTESIAN_POINT('Ctrl Pts',(70.3319757122568,-17.1142553297867,12.));
#55100=CARTESIAN_POINT('Ctrl Pts',(70.3074608242608,-17.1173156924733,12.));
#55101=CARTESIAN_POINT('Ctrl Pts',(70.2829835340238,-17.1203474526031,12.));
#55102=CARTESIAN_POINT('Ctrl Pts',(70.2585439596901,-17.1233506537176,12.));
#55103=CARTESIAN_POINT('Ctrl Pts',(70.2341422198363,-17.1263253396202,12.));
#55104=CARTESIAN_POINT('Ctrl Pts',(70.2097784334747,-17.1292715543778,12.));
#55105=CARTESIAN_POINT('Ctrl Pts',(70.1854527200631,-17.1321893423182,12.));
#55106=CARTESIAN_POINT('Ctrl Pts',(70.1611651995083,-17.1350787480312,12.));
#55107=CARTESIAN_POINT('Ctrl Pts',(70.1369159921687,-17.1379398163709,12.));
#55108=CARTESIAN_POINT('Ctrl Pts',(70.1127052188522,-17.1407725924617,12.));
#55109=CARTESIAN_POINT('Ctrl Pts',(70.0885330008179,-17.1435771217018,12.));
#55110=CARTESIAN_POINT('Ctrl Pts',(70.0643994597873,-17.1463534497594,12.));
#55111=CARTESIAN_POINT('Ctrl Pts',(70.0403047179483,-17.1491016225749,12.));
#55112=CARTESIAN_POINT('Ctrl Pts',(70.0162488979584,-17.1518216863623,12.));
#55113=CARTESIAN_POINT('Ctrl Pts',(69.9922321229424,-17.154513687616,12.));
#55114=CARTESIAN_POINT('Ctrl Pts',(69.9682545164939,-17.157177673114,12.));
#55115=CARTESIAN_POINT('Ctrl Pts',(69.9443162026865,-17.1598136899144,12.));
#55116=CARTESIAN_POINT('Ctrl Pts',(69.9204173060781,-17.1624217853578,12.));
#55117=CARTESIAN_POINT('Ctrl Pts',(69.8965579517147,-17.1650020070686,12.));
#55118=CARTESIAN_POINT('Ctrl Pts',(69.8727382651286,-17.167554402962,12.));
#55119=CARTESIAN_POINT('Ctrl Pts',(69.8489583723407,-17.1700790212473,12.));
#55120=CARTESIAN_POINT('Ctrl Pts',(69.8252183998702,-17.1725759104252,12.));
#55121=CARTESIAN_POINT('Ctrl Pts',(69.8015184747398,-17.1750451192885,12.));
#55122=CARTESIAN_POINT('Ctrl Pts',(69.777858724479,-17.1774866969256,12.));
#55123=CARTESIAN_POINT('Ctrl Pts',(69.7542392771234,-17.179900692726,12.));
#55124=CARTESIAN_POINT('Ctrl Pts',(69.7306602612155,-17.1822871563842,12.));
#55125=CARTESIAN_POINT('Ctrl Pts',(69.7071218058178,-17.1846461378973,12.));
#55126=CARTESIAN_POINT('Ctrl Pts',(69.6836240405164,-17.1869776875666,12.));
#55127=CARTESIAN_POINT('Ctrl Pts',(69.6601670954269,-17.1892818560002,12.));
#55128=CARTESIAN_POINT('Ctrl Pts',(69.6367511011898,-17.1915586941192,12.));
#55129=CARTESIAN_POINT('Ctrl Pts',(69.6133761889749,-17.1938082531612,12.));
#55130=CARTESIAN_POINT('Ctrl Pts',(69.5900424904921,-17.196030584678,12.));
#55131=CARTESIAN_POINT('Ctrl Pts',(69.5667501379969,-17.1982257405377,12.));
#55132=CARTESIAN_POINT('Ctrl Pts',(69.5434992642944,-17.2003937729268,12.));
#55133=CARTESIAN_POINT('Ctrl Pts',(69.5202900027367,-17.2025347343577,12.));
#55134=CARTESIAN_POINT('Ctrl Pts',(69.4971224872269,-17.2046486776708,12.));
#55135=CARTESIAN_POINT('Ctrl Pts',(69.4739968522313,-17.2067356560336,12.));
#55136=CARTESIAN_POINT('Ctrl Pts',(69.450913232785,-17.2087957229423,12.));
#55137=CARTESIAN_POINT('Ctrl Pts',(69.4278717644973,-17.2108289322254,12.));
#55138=CARTESIAN_POINT('Ctrl Pts',(69.404872583548,-17.2128353380502,12.));
#55139=CARTESIAN_POINT('Ctrl Pts',(69.3819158266916,-17.2148149949252,12.));
#55140=CARTESIAN_POINT('Ctrl Pts',(69.3590016312692,-17.2167679576984,12.));
#55141=CARTESIAN_POINT('Ctrl Pts',(69.3361301352141,-17.2186942815602,12.));
#55142=CARTESIAN_POINT('Ctrl Pts',(69.3133014770555,-17.2205940220459,12.));
#55143=CARTESIAN_POINT('Ctrl Pts',(69.2905157959166,-17.2224672350438,12.));
#55144=CARTESIAN_POINT('Ctrl Pts',(69.2677732315224,-17.224313976797,12.));
#55145=CARTESIAN_POINT('Ctrl Pts',(69.2450739242109,-17.226134303902,12.));
#55146=CARTESIAN_POINT('Ctrl Pts',(69.222418014938,-17.227928273312,12.));
#55147=CARTESIAN_POINT('Ctrl Pts',(69.1998056452828,-17.2296959423407,12.));
#55148=CARTESIAN_POINT('Ctrl Pts',(69.1772369574447,-17.23143736867,12.));
#55149=CARTESIAN_POINT('Ctrl Pts',(69.1547120942527,-17.2331526103506,12.));
#55150=CARTESIAN_POINT('Ctrl Pts',(69.1322311991752,-17.2348417258015,12.));
#55151=CARTESIAN_POINT('Ctrl Pts',(69.1097944163245,-17.2365047738125,12.));
#55152=CARTESIAN_POINT('Ctrl Pts',(69.0874018904599,-17.2381418135491,12.));
#55153=CARTESIAN_POINT('Ctrl Pts',(69.065053766986,-17.2397529045589,12.));
#55154=CARTESIAN_POINT('Ctrl Pts',(69.0427501919636,-17.2413381067723,12.));
#55155=CARTESIAN_POINT('Ctrl Pts',(69.0204913121225,-17.2428974805044,12.));
#55156=CARTESIAN_POINT('Ctrl Pts',(68.9982772748694,-17.2444310864585,12.));
#55157=CARTESIAN_POINT('Ctrl Pts',(68.9761082282922,-17.2459389857327,12.));
#55158=CARTESIAN_POINT('Ctrl Pts',(68.9539843211619,-17.2474212398275,12.));
#55159=CARTESIAN_POINT('Ctrl Pts',(68.9319057029409,-17.248877910643,12.));
#55160=CARTESIAN_POINT('Ctrl Pts',(68.909872523787,-17.2503090604792,12.));
#55161=CARTESIAN_POINT('Ctrl Pts',(68.8878849345557,-17.2517147520376,12.));
#55162=CARTESIAN_POINT('Ctrl Pts',(68.8659430867972,-17.2530950484258,12.));
#55163=CARTESIAN_POINT('Ctrl Pts',(68.844047132755,-17.2544500131624,12.));
#55164=CARTESIAN_POINT('Ctrl Pts',(68.8221972253941,-17.2557797101812,12.));
#55165=CARTESIAN_POINT('Ctrl Pts',(68.8003935184184,-17.2570842038383,12.));
#55166=CARTESIAN_POINT('Ctrl Pts',(68.7786361662882,-17.2583635589198,12.));
#55167=CARTESIAN_POINT('Ctrl Pts',(68.7569253242333,-17.259617840655,12.));
#55168=CARTESIAN_POINT('Ctrl Pts',(68.7352611482547,-17.2608471147185,12.));
#55169=CARTESIAN_POINT('Ctrl Pts',(68.7136437951097,-17.2620514472182,12.));
#55170=CARTESIAN_POINT('Ctrl Pts',(68.6920734222938,-17.2632309046892,12.));
#55171=CARTESIAN_POINT('Ctrl Pts',(68.6705501880249,-17.2643855540892,12.));
#55172=CARTESIAN_POINT('Ctrl Pts',(68.6490742512057,-17.2655154627928,12.));
#55173=CARTESIAN_POINT('Ctrl Pts',(68.6276457714729,-17.2666206986084,12.));
#55174=CARTESIAN_POINT('Ctrl Pts',(68.6062649092764,-17.2677013298057,12.));
#55175=CARTESIAN_POINT('Ctrl Pts',(68.5849318259449,-17.2687574251428,12.));
#55176=CARTESIAN_POINT('Ctrl Pts',(68.5636466837517,-17.269789053896,12.));
#55177=CARTESIAN_POINT('Ctrl Pts',(68.5424096459772,-17.2707962858919,12.));
#55178=CARTESIAN_POINT('Ctrl Pts',(68.521220876786,-17.2717791914544,12.));
#55179=CARTESIAN_POINT('Ctrl Pts',(68.5000805410911,-17.2727378413489,12.));
#55180=CARTESIAN_POINT('Ctrl Pts',(68.4789888044351,-17.2736723067365,12.));
#55181=CARTESIAN_POINT('Ctrl Pts',(68.4579458328185,-17.2745826591119,12.));
#55182=CARTESIAN_POINT('Ctrl Pts',(68.436951792677,-17.2754689702992,12.));
#55183=CARTESIAN_POINT('Ctrl Pts',(68.4160068512753,-17.2763313126018,12.));
#55184=CARTESIAN_POINT('Ctrl Pts',(68.3951111770487,-17.2771697589384,12.));
#55185=CARTESIAN_POINT('Ctrl Pts',(68.3742649398964,-17.2779843829608,12.));
#55186=CARTESIAN_POINT('Ctrl Pts',(68.3534683116515,-17.2787752592484,12.));
#55187=CARTESIAN_POINT('Ctrl Pts',(68.3327214657575,-17.2795424631799,12.));
#55188=CARTESIAN_POINT('Ctrl Pts',(68.3120245763914,-17.2802860705815,12.));
#55189=CARTESIAN_POINT('Ctrl Pts',(68.2913778177261,-17.2810061574353,12.));
#55190=CARTESIAN_POINT('Ctrl Pts',(68.2707813631731,-17.2817027995831,12.));
#55191=CARTESIAN_POINT('Ctrl Pts',(68.2502353845071,-17.2823760723874,12.));
#55192=CARTESIAN_POINT('Ctrl Pts',(68.2297400535294,-17.2830260513867,12.));
#55193=CARTESIAN_POINT('Ctrl Pts',(68.2092955440567,-17.2836528130819,12.));
#55194=CARTESIAN_POINT('Ctrl Pts',(68.1889020335427,-17.2842564355799,12.));
#55195=CARTESIAN_POINT('Ctrl Pts',(68.1685597054232,-17.2848369995293,12.));
#55196=CARTESIAN_POINT('Ctrl Pts',(68.1482687493226,-17.2853945882072,12.));
#55197=CARTESIAN_POINT('Ctrl Pts',(68.1280293561511,-17.2859292855705,12.));
#55198=CARTESIAN_POINT('Ctrl Pts',(68.1078417137877,-17.2864411745459,12.));
#55199=CARTESIAN_POINT('Ctrl Pts',(68.0877060033205,-17.2869303355432,12.));
#55200=CARTESIAN_POINT('Ctrl Pts',(68.0676223930412,-17.2873968440839,12.));
#55201=CARTESIAN_POINT('Ctrl Pts',(68.0475910442424,-17.2878407730961,12.));
#55202=CARTESIAN_POINT('Ctrl Pts',(68.0276121227356,-17.2882621974721,12.));
#55203=CARTESIAN_POINT('Ctrl Pts',(68.007685808115,-17.28866119774,12.));
#55204=CARTESIAN_POINT('Ctrl Pts',(67.987812304921,-17.2890378644866,12.));
#55205=CARTESIAN_POINT('Ctrl Pts',(67.9679918502579,-17.2893923013894,12.));
#55206=CARTESIAN_POINT('Ctrl Pts',(67.9482246901667,-17.2897246158941,12.));
#55207=CARTESIAN_POINT('Ctrl Pts',(67.9285110571741,-17.2900349103981,12.));
#55208=CARTESIAN_POINT('Ctrl Pts',(67.9088511496686,-17.2903232740694,12.));
#55209=CARTESIAN_POINT('Ctrl Pts',(67.8892451049608,-17.2905897723948,12.));
#55210=CARTESIAN_POINT('Ctrl Pts',(67.8696929978782,-17.2908344459694,12.));
#55211=CARTESIAN_POINT('Ctrl Pts',(67.8540944889687,-17.291012743109,12.));
#55212=CARTESIAN_POINT('Ctrl Pts',(67.842419897098,-17.2911366591348,12.));
#55213=CARTESIAN_POINT('Ctrl Pts',(67.8346476309018,-17.2912149114119,12.));
#55214=CARTESIAN_POINT('Ctrl Pts',(67.8307641965655,-17.2912529479484,12.));
#55215=CARTESIAN_POINT('Ctrl Pts',(72.6050633494717,-15.3208442077424,-5.55111512312578E-16));
#55216=CARTESIAN_POINT('Ctrl Pts',(72.6050633494717,-15.3208442077424,4.));
#55217=CARTESIAN_POINT('Ctrl Pts',(72.6050633494717,-15.3208442077424,8.));
#55218=CARTESIAN_POINT('Ctrl Pts',(72.6050633494717,-15.3208442077424,12.));
#55219=CARTESIAN_POINT('Ctrl Pts',(72.6937764817671,-15.3856835210422,-5.55111512312578E-16));
#55220=CARTESIAN_POINT('Ctrl Pts',(72.6937764817671,-15.3856835210422,3.99999999999999));
#55221=CARTESIAN_POINT('Ctrl Pts',(72.6937764817672,-15.3856835210423,8.));
#55222=CARTESIAN_POINT('Ctrl Pts',(72.6937764817672,-15.3856835210423,12.));
#55223=CARTESIAN_POINT('Ctrl Pts',(72.8096834307711,-15.5519317750289,-5.55111512312578E-16));
#55224=CARTESIAN_POINT('Ctrl Pts',(72.8096834307711,-15.5519317750289,4.00000000000001));
#55225=CARTESIAN_POINT('Ctrl Pts',(72.8096834307711,-15.551931775029,8.));
#55226=CARTESIAN_POINT('Ctrl Pts',(72.8096834307711,-15.551931775029,12.));
#55227=CARTESIAN_POINT('Ctrl Pts',(72.8161171750016,-15.7502340068145,-5.55111512312578E-16));
#55228=CARTESIAN_POINT('Ctrl Pts',(72.8161171750016,-15.7502340068145,3.99999999999999));
#55229=CARTESIAN_POINT('Ctrl Pts',(72.8161171750016,-15.7502340068145,8.00000000000001));
#55230=CARTESIAN_POINT('Ctrl Pts',(72.8161171750016,-15.7502340068145,12.));
#55231=CARTESIAN_POINT('Ctrl Pts',(72.7986051948038,-15.8307637747231,-5.55111512312578E-16));
#55232=CARTESIAN_POINT('Ctrl Pts',(72.7986051948038,-15.8307637747231,4.));
#55233=CARTESIAN_POINT('Ctrl Pts',(72.7986051948038,-15.8307637747231,8.));
#55234=CARTESIAN_POINT('Ctrl Pts',(72.7986051948038,-15.8307637747231,12.));
#55235=CARTESIAN_POINT('',(72.6050633494717,-15.3208442077424,-2.77555756156289E-16));
#55236=CARTESIAN_POINT('',(72.7986051948038,-15.8307637747231,2.77555756156289E-16));
#55237=CARTESIAN_POINT('Ctrl Pts',(72.6050633494717,-15.3208442077424,-5.55111512312578E-16));
#55238=CARTESIAN_POINT('Ctrl Pts',(72.6937764817671,-15.3856835210422,-5.55111512312578E-16));
#55239=CARTESIAN_POINT('Ctrl Pts',(72.7600090240551,-15.4806825233204,-5.55111512312578E-16));
#55240=CARTESIAN_POINT('Ctrl Pts',(72.790495213764,-15.586148130594,-5.55111512312578E-16));
#55241=CARTESIAN_POINT('Ctrl Pts',(72.8133598560457,-15.6652473360493,-5.55111512312578E-16));
#55242=CARTESIAN_POINT('Ctrl Pts',(72.8161171750016,-15.7502340068145,-5.55111512312578E-16));
#55243=CARTESIAN_POINT('Ctrl Pts',(72.7986051948038,-15.8307637747231,-5.55111512312578E-16));
#55244=CARTESIAN_POINT('',(72.7986051948038,-15.8307637747231,12.));
#55245=CARTESIAN_POINT('Ctrl Pts',(72.7986051948038,-15.8307637747231,-5.55111512312578E-16));
#55246=CARTESIAN_POINT('Ctrl Pts',(72.7986051948038,-15.8307637747231,4.));
#55247=CARTESIAN_POINT('Ctrl Pts',(72.7986051948038,-15.8307637747231,8.));
#55248=CARTESIAN_POINT('Ctrl Pts',(72.7986051948038,-15.8307637747231,12.));
#55249=CARTESIAN_POINT('',(72.6050633494717,-15.3208442077424,12.));
#55250=CARTESIAN_POINT('Ctrl Pts',(72.7986051948038,-15.8307637747231,12.));
#55251=CARTESIAN_POINT('Ctrl Pts',(72.8161171750016,-15.7502340068145,12.));
#55252=CARTESIAN_POINT('Ctrl Pts',(72.8133598560457,-15.6652473360493,12.));
#55253=CARTESIAN_POINT('Ctrl Pts',(72.790495213764,-15.5861481305941,12.));
#55254=CARTESIAN_POINT('Ctrl Pts',(72.7600090240551,-15.4806825233204,12.));
#55255=CARTESIAN_POINT('Ctrl Pts',(72.6937764817672,-15.3856835210423,12.));
#55256=CARTESIAN_POINT('Ctrl Pts',(72.6050633494717,-15.3208442077424,12.));
#55257=CARTESIAN_POINT('Ctrl Pts',(72.6050633494717,-15.3208442077424,12.));
#55258=CARTESIAN_POINT('Ctrl Pts',(72.6050633494717,-15.3208442077424,8.));
#55259=CARTESIAN_POINT('Ctrl Pts',(72.6050633494717,-15.3208442077424,4.));
#55260=CARTESIAN_POINT('Ctrl Pts',(72.6050633494717,-15.3208442077424,-5.55111512312578E-16));
#55261=CARTESIAN_POINT('Origin',(3.65979954444617E-10,-8.10341340518591E-11,
0.));
#55262=CARTESIAN_POINT('Origin',(3.65979954444617E-10,-8.10341340518591E-11,
12.));
#55263=CARTESIAN_POINT('Origin',(3.65979954444617E-10,-8.10341340518591E-11,
0.));
#55264=CARTESIAN_POINT('Ctrl Pts',(70.9608233461364,-22.6894590071785,0.));
#55265=CARTESIAN_POINT('Ctrl Pts',(70.9608233461364,-22.6894590071785,4.));
#55266=CARTESIAN_POINT('Ctrl Pts',(70.9608233461364,-22.6894590071785,8.));
#55267=CARTESIAN_POINT('Ctrl Pts',(70.9608233461364,-22.6894590071785,12.));
#55268=CARTESIAN_POINT('Ctrl Pts',(70.9273579271571,-22.7941214270113,0.));
#55269=CARTESIAN_POINT('Ctrl Pts',(70.9273579271571,-22.7941214270113,4.));
#55270=CARTESIAN_POINT('Ctrl Pts',(70.9273579271571,-22.7941214270113,8.00000000000001));
#55271=CARTESIAN_POINT('Ctrl Pts',(70.9273579271571,-22.7941214270113,12.));
#55272=CARTESIAN_POINT('Ctrl Pts',(70.8062825417802,-22.9566438338674,0.));
#55273=CARTESIAN_POINT('Ctrl Pts',(70.8062825417802,-22.9566438338674,4.));
#55274=CARTESIAN_POINT('Ctrl Pts',(70.8062825417802,-22.9566438338674,7.99999999999999));
#55275=CARTESIAN_POINT('Ctrl Pts',(70.8062825417802,-22.9566438338674,12.));
#55276=CARTESIAN_POINT('Ctrl Pts',(70.6201870200063,-23.0254444386654,0.));
#55277=CARTESIAN_POINT('Ctrl Pts',(70.6201870200063,-23.0254444386654,4.));
#55278=CARTESIAN_POINT('Ctrl Pts',(70.6201870200063,-23.0254444386654,8.00000000000001));
#55279=CARTESIAN_POINT('Ctrl Pts',(70.6201870200063,-23.0254444386654,12.));
#55280=CARTESIAN_POINT('Ctrl Pts',(70.5382514078489,-23.0342913834092,0.));
#55281=CARTESIAN_POINT('Ctrl Pts',(70.5382514078489,-23.0342913834092,4.));
#55282=CARTESIAN_POINT('Ctrl Pts',(70.5382514078489,-23.0342913834092,8.));
#55283=CARTESIAN_POINT('Ctrl Pts',(70.5382514078489,-23.0342913834092,12.));
#55284=CARTESIAN_POINT('',(70.9608233461364,-22.6894590071785,0.));
#55285=CARTESIAN_POINT('',(70.5382514078489,-23.0342913834093,0.));
#55286=CARTESIAN_POINT('Ctrl Pts',(70.9608233461364,-22.6894590071785,0.));
#55287=CARTESIAN_POINT('Ctrl Pts',(70.9273579271571,-22.7941214270113,0.));
#55288=CARTESIAN_POINT('Ctrl Pts',(70.858171992656,-22.8869913737862,0.));
#55289=CARTESIAN_POINT('Ctrl Pts',(70.767754993209,-22.9492582831544,0.));
#55290=CARTESIAN_POINT('Ctrl Pts',(70.6999422436237,-22.9959584651805,0.));
#55291=CARTESIAN_POINT('Ctrl Pts',(70.6201870200063,-23.0254444386654,0.));
#55292=CARTESIAN_POINT('Ctrl Pts',(70.5382514078489,-23.0342913834092,0.));
#55293=CARTESIAN_POINT('',(70.5382514078489,-23.0342913834093,12.));
#55294=CARTESIAN_POINT('Ctrl Pts',(70.5382514078489,-23.0342913834092,0.));
#55295=CARTESIAN_POINT('Ctrl Pts',(70.5382514078489,-23.0342913834092,4.));
#55296=CARTESIAN_POINT('Ctrl Pts',(70.5382514078489,-23.0342913834092,8.));
#55297=CARTESIAN_POINT('Ctrl Pts',(70.5382514078489,-23.0342913834092,12.));
#55298=CARTESIAN_POINT('',(70.9608233461364,-22.6894590071785,12.));
#55299=CARTESIAN_POINT('Ctrl Pts',(70.5382514078489,-23.0342913834092,12.));
#55300=CARTESIAN_POINT('Ctrl Pts',(70.6201870200063,-23.0254444386654,12.));
#55301=CARTESIAN_POINT('Ctrl Pts',(70.6999422436237,-22.9959584651805,12.));
#55302=CARTESIAN_POINT('Ctrl Pts',(70.767754993209,-22.9492582831544,12.));
#55303=CARTESIAN_POINT('Ctrl Pts',(70.858171992656,-22.8869913737862,12.));
#55304=CARTESIAN_POINT('Ctrl Pts',(70.9273579271571,-22.7941214270113,12.));
#55305=CARTESIAN_POINT('Ctrl Pts',(70.9608233461364,-22.6894590071785,12.));
#55306=CARTESIAN_POINT('Ctrl Pts',(70.9608233461364,-22.6894590071785,12.));
#55307=CARTESIAN_POINT('Ctrl Pts',(70.9608233461364,-22.6894590071785,8.));
#55308=CARTESIAN_POINT('Ctrl Pts',(70.9608233461364,-22.6894590071785,4.));
#55309=CARTESIAN_POINT('Ctrl Pts',(70.9608233461364,-22.6894590071785,0.));
#55310=CARTESIAN_POINT('Ctrl Pts',(66.0656156664138,-23.1372951448024,0.));
#55311=CARTESIAN_POINT('Ctrl Pts',(66.0656156664138,-23.1372951448024,12.));
#55312=CARTESIAN_POINT('Ctrl Pts',(66.0694876382126,-23.1375957166104,0.));
#55313=CARTESIAN_POINT('Ctrl Pts',(66.0694876382126,-23.1375957166104,12.));
#55314=CARTESIAN_POINT('Ctrl Pts',(66.0772371487248,-23.13819515974,0.));
#55315=CARTESIAN_POINT('Ctrl Pts',(66.0772371487248,-23.13819515974,12.));
#55316=CARTESIAN_POINT('Ctrl Pts',(66.088878115242,-23.1390892229779,0.));
#55317=CARTESIAN_POINT('Ctrl Pts',(66.088878115242,-23.1390892229779,12.));
#55318=CARTESIAN_POINT('Ctrl Pts',(66.1044328067355,-23.1402711039425,0.));
#55319=CARTESIAN_POINT('Ctrl Pts',(66.1044328067355,-23.1402711039425,12.));
#55320=CARTESIAN_POINT('Ctrl Pts',(66.1239318368548,-23.1417314398398,0.));
#55321=CARTESIAN_POINT('Ctrl Pts',(66.1239318368548,-23.1417314398398,12.));
#55322=CARTESIAN_POINT('Ctrl Pts',(66.1434865015027,-23.1431747350098,0.));
#55323=CARTESIAN_POINT('Ctrl Pts',(66.1434865015027,-23.1431747350098,12.));
#55324=CARTESIAN_POINT('Ctrl Pts',(66.1630967296747,-23.1446009424903,0.));
#55325=CARTESIAN_POINT('Ctrl Pts',(66.1630967296747,-23.1446009424903,12.));
#55326=CARTESIAN_POINT('Ctrl Pts',(66.1827623902899,-23.1460099850763,0.));
#55327=CARTESIAN_POINT('Ctrl Pts',(66.1827623902899,-23.1460099850763,12.));
#55328=CARTESIAN_POINT('Ctrl Pts',(66.2024832934866,-23.1474017566484,0.));
